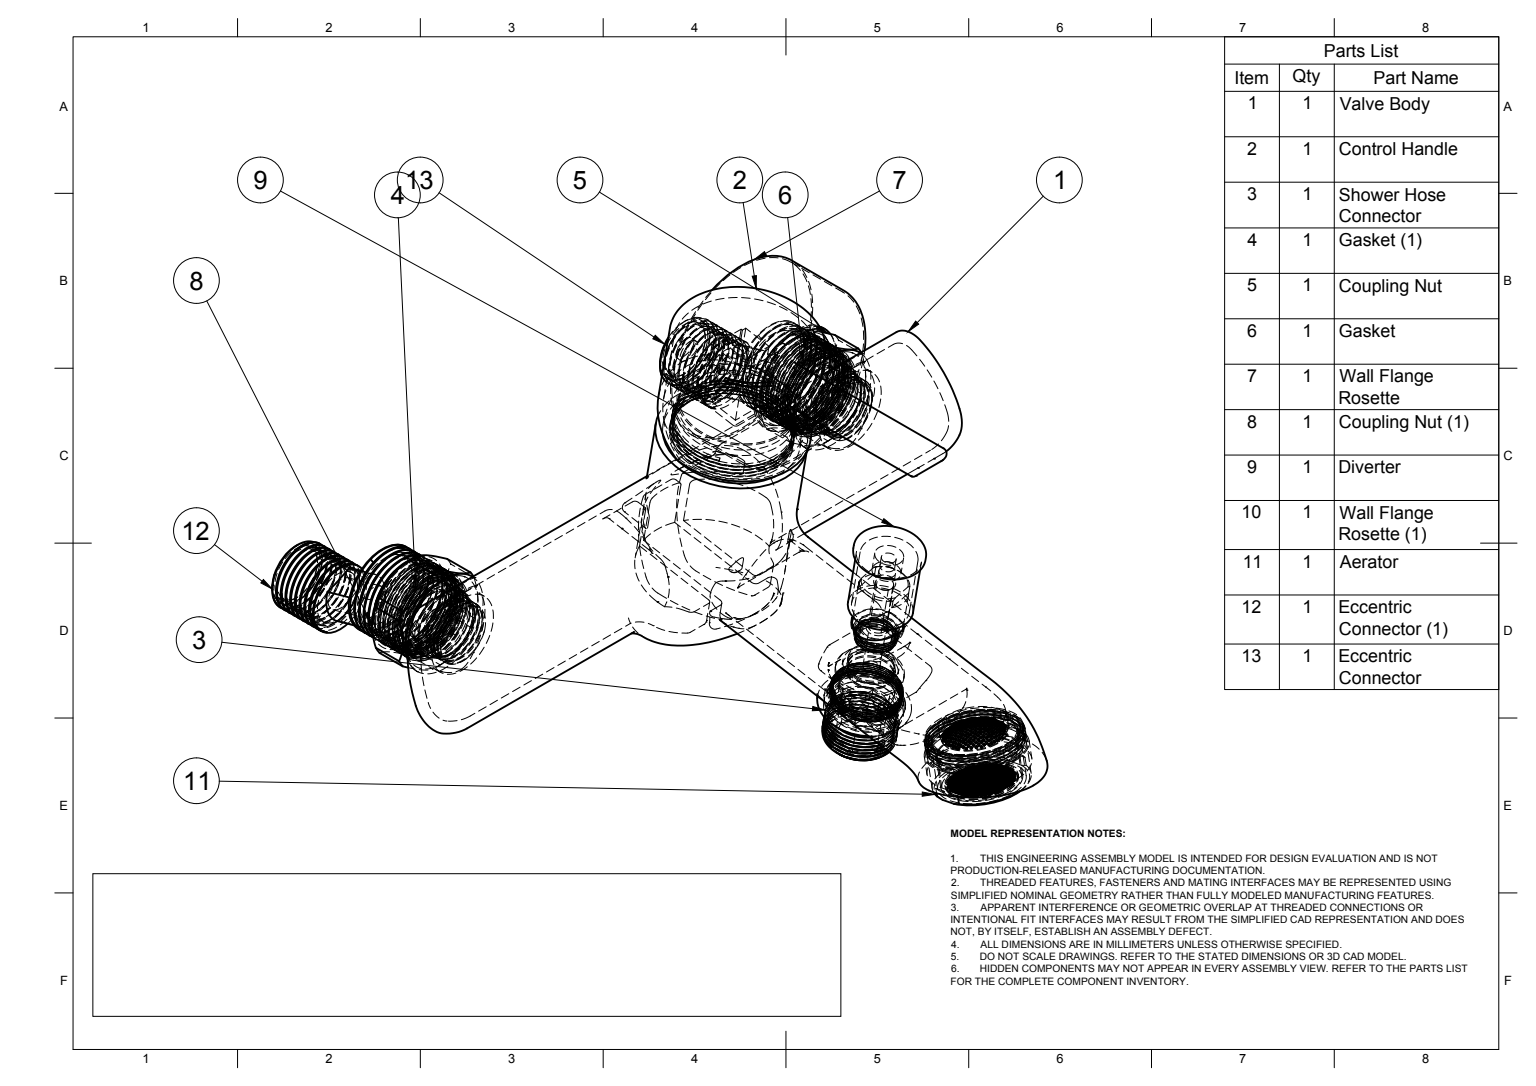
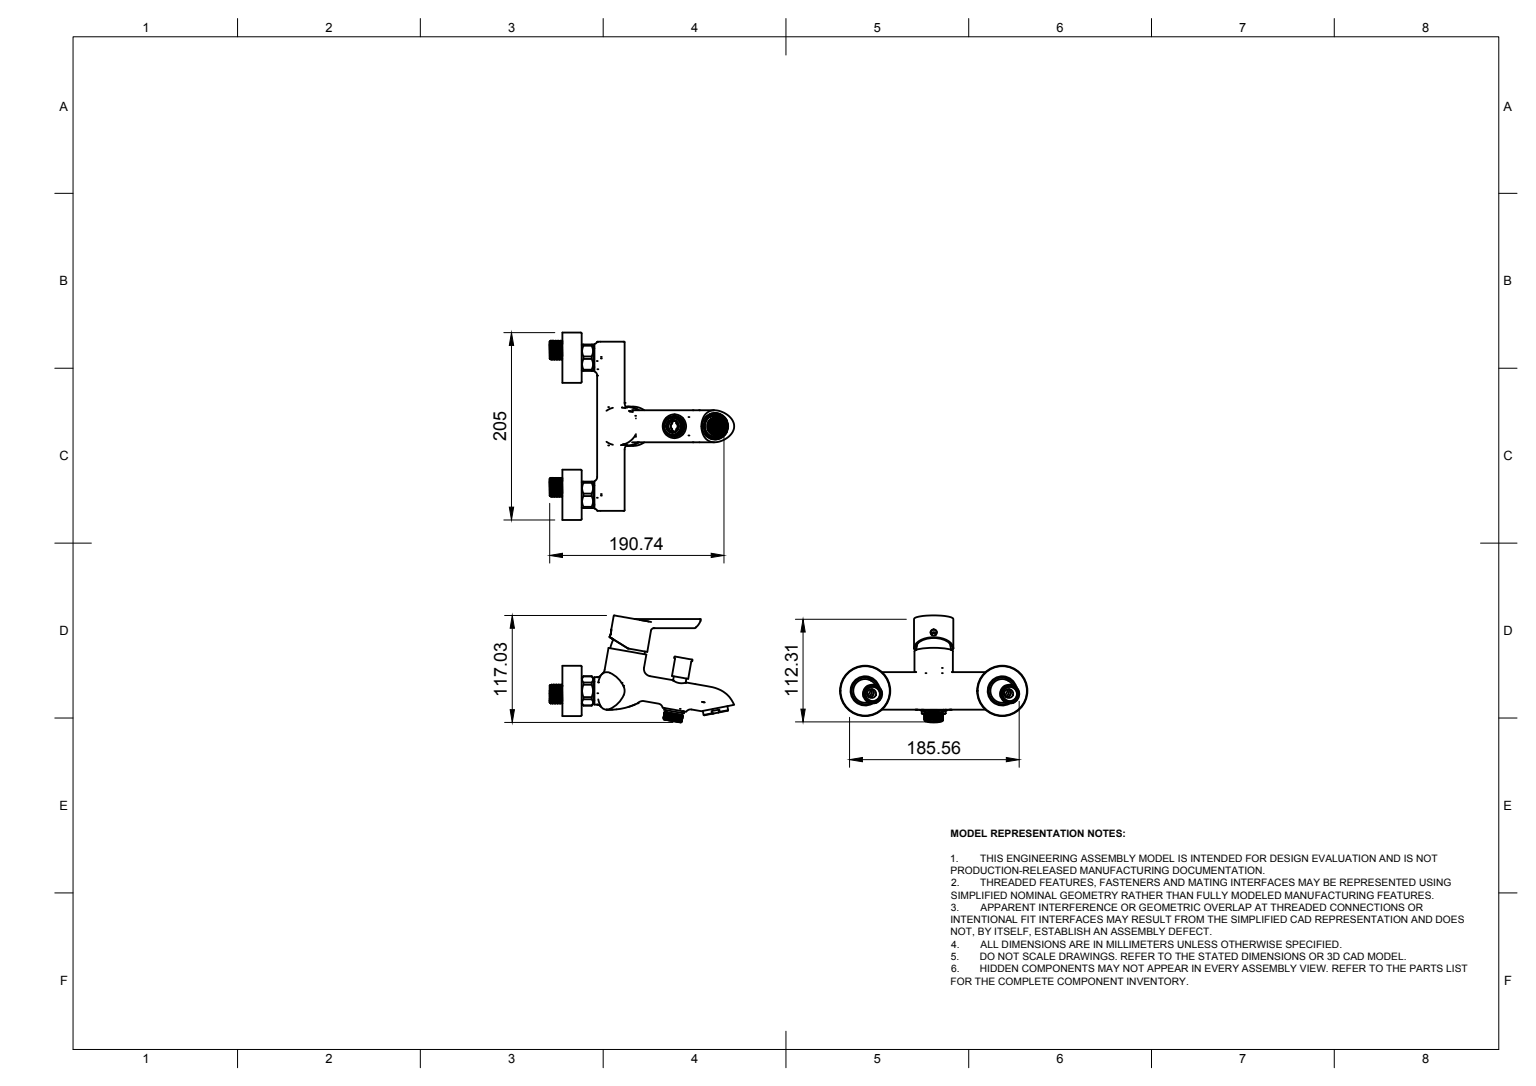
ISO-10303-21;
HEADER;
/* Generated by software containing ST-Developer
 * from STEP Tools, Inc. (www.steptools.com) 
 */

FILE_DESCRIPTION(
/* description */ ('STEP AP214'),
/* implementation_level */ '2;1');

FILE_NAME(
/* name */ 'MAS-607',
/* time_stamp */ '2026-10-05T23:18:41-07:00',
/* author */ (''),
/* organization */ (''),
/* preprocessor_version */ 'ST-DEVELOPER v20.2',
/* originating_system */ 'Autodesk Translation Framework v15.15.0.0',
/* authorisation */ '');

FILE_SCHEMA (('AUTOMOTIVE_DESIGN { 1 0 10303 214 3 1 1 }'));
ENDSEC;

DATA;
#10=MECHANICAL_DESIGN_GEOMETRIC_PRESENTATION_REPRESENTATION('',(#100,#101,
#102,#103,#104,#105,#106,#107,#108,#109,#110,#111,#112),#221662);
#11=ITEM_DEFINED_TRANSFORMATION($,$,#79483,#86151);
#12=ITEM_DEFINED_TRANSFORMATION($,$,#80379,#86152);
#13=ITEM_DEFINED_TRANSFORMATION($,$,#80522,#86153);
#14=ITEM_DEFINED_TRANSFORMATION($,$,#80620,#86154);
#15=ITEM_DEFINED_TRANSFORMATION($,$,#80667,#86155);
#16=ITEM_DEFINED_TRANSFORMATION($,$,#80719,#86156);
#17=ITEM_DEFINED_TRANSFORMATION($,$,#80766,#86157);
#18=ITEM_DEFINED_TRANSFORMATION($,$,#80796,#86158);
#19=ITEM_DEFINED_TRANSFORMATION($,$,#80848,#86159);
#20=ITEM_DEFINED_TRANSFORMATION($,$,#80951,#86160);
#21=ITEM_DEFINED_TRANSFORMATION($,$,#80981,#86161);
#22=ITEM_DEFINED_TRANSFORMATION($,$,#85967,#86162);
#23=ITEM_DEFINED_TRANSFORMATION($,$,#86059,#86163);
#24=(
REPRESENTATION_RELATIONSHIP($,$,#221709,#221708)
REPRESENTATION_RELATIONSHIP_WITH_TRANSFORMATION(#11)
SHAPE_REPRESENTATION_RELATIONSHIP()
);
#25=(
REPRESENTATION_RELATIONSHIP($,$,#221710,#221708)
REPRESENTATION_RELATIONSHIP_WITH_TRANSFORMATION(#12)
SHAPE_REPRESENTATION_RELATIONSHIP()
);
#26=(
REPRESENTATION_RELATIONSHIP($,$,#221711,#221708)
REPRESENTATION_RELATIONSHIP_WITH_TRANSFORMATION(#13)
SHAPE_REPRESENTATION_RELATIONSHIP()
);
#27=(
REPRESENTATION_RELATIONSHIP($,$,#221712,#221708)
REPRESENTATION_RELATIONSHIP_WITH_TRANSFORMATION(#14)
SHAPE_REPRESENTATION_RELATIONSHIP()
);
#28=(
REPRESENTATION_RELATIONSHIP($,$,#221713,#221708)
REPRESENTATION_RELATIONSHIP_WITH_TRANSFORMATION(#15)
SHAPE_REPRESENTATION_RELATIONSHIP()
);
#29=(
REPRESENTATION_RELATIONSHIP($,$,#221714,#221708)
REPRESENTATION_RELATIONSHIP_WITH_TRANSFORMATION(#16)
SHAPE_REPRESENTATION_RELATIONSHIP()
);
#30=(
REPRESENTATION_RELATIONSHIP($,$,#221715,#221708)
REPRESENTATION_RELATIONSHIP_WITH_TRANSFORMATION(#17)
SHAPE_REPRESENTATION_RELATIONSHIP()
);
#31=(
REPRESENTATION_RELATIONSHIP($,$,#221716,#221708)
REPRESENTATION_RELATIONSHIP_WITH_TRANSFORMATION(#18)
SHAPE_REPRESENTATION_RELATIONSHIP()
);
#32=(
REPRESENTATION_RELATIONSHIP($,$,#221717,#221708)
REPRESENTATION_RELATIONSHIP_WITH_TRANSFORMATION(#19)
SHAPE_REPRESENTATION_RELATIONSHIP()
);
#33=(
REPRESENTATION_RELATIONSHIP($,$,#221718,#221708)
REPRESENTATION_RELATIONSHIP_WITH_TRANSFORMATION(#20)
SHAPE_REPRESENTATION_RELATIONSHIP()
);
#34=(
REPRESENTATION_RELATIONSHIP($,$,#221719,#221708)
REPRESENTATION_RELATIONSHIP_WITH_TRANSFORMATION(#21)
SHAPE_REPRESENTATION_RELATIONSHIP()
);
#35=(
REPRESENTATION_RELATIONSHIP($,$,#221720,#221708)
REPRESENTATION_RELATIONSHIP_WITH_TRANSFORMATION(#22)
SHAPE_REPRESENTATION_RELATIONSHIP()
);
#36=(
REPRESENTATION_RELATIONSHIP($,$,#221721,#221708)
REPRESENTATION_RELATIONSHIP_WITH_TRANSFORMATION(#23)
SHAPE_REPRESENTATION_RELATIONSHIP()
);
#37=CONTEXT_DEPENDENT_SHAPE_REPRESENTATION(#24,#221695);
#38=CONTEXT_DEPENDENT_SHAPE_REPRESENTATION(#25,#221696);
#39=CONTEXT_DEPENDENT_SHAPE_REPRESENTATION(#26,#221697);
#40=CONTEXT_DEPENDENT_SHAPE_REPRESENTATION(#27,#221698);
#41=CONTEXT_DEPENDENT_SHAPE_REPRESENTATION(#28,#221699);
#42=CONTEXT_DEPENDENT_SHAPE_REPRESENTATION(#29,#221700);
#43=CONTEXT_DEPENDENT_SHAPE_REPRESENTATION(#30,#221701);
#44=CONTEXT_DEPENDENT_SHAPE_REPRESENTATION(#31,#221702);
#45=CONTEXT_DEPENDENT_SHAPE_REPRESENTATION(#32,#221703);
#46=CONTEXT_DEPENDENT_SHAPE_REPRESENTATION(#33,#221704);
#47=CONTEXT_DEPENDENT_SHAPE_REPRESENTATION(#34,#221705);
#48=CONTEXT_DEPENDENT_SHAPE_REPRESENTATION(#35,#221706);
#49=CONTEXT_DEPENDENT_SHAPE_REPRESENTATION(#36,#221707);
#50=NEXT_ASSEMBLY_USAGE_OCCURRENCE('Valve Body:1','Valve Body:1',
'Valve Body:1',#221723,#221724,'Valve Body:1');
#51=NEXT_ASSEMBLY_USAGE_OCCURRENCE('Control Handle:1',
'Control Handle:1','Control Handle:1',#221723,#221725,
'Control Handle:1');
#52=NEXT_ASSEMBLY_USAGE_OCCURRENCE('Shower Hose Connector:1',
'Shower Hose Connector:1','Shower Hose Connector:1',#221723,#221726,
'Shower Hose Connector:1');
#53=NEXT_ASSEMBLY_USAGE_OCCURRENCE('Gasket (1):1','Gasket (1):1',
'Gasket (1):1',#221723,#221727,'Gasket (1):1');
#54=NEXT_ASSEMBLY_USAGE_OCCURRENCE('Coupling Nut:1','Coupling Nut:1',
'Coupling Nut:1',#221723,#221728,'Coupling Nut:1');
#55=NEXT_ASSEMBLY_USAGE_OCCURRENCE('Gasket:1','Gasket:1','Gasket:1',#221723,
#221729,'Gasket:1');
#56=NEXT_ASSEMBLY_USAGE_OCCURRENCE('Wall Flange Rosette:1',
'Wall Flange Rosette:1','Wall Flange Rosette:1',#221723,#221730,
'Wall Flange Rosette:1');
#57=NEXT_ASSEMBLY_USAGE_OCCURRENCE('Coupling Nut (1):1',
'Coupling Nut (1):1','Coupling Nut (1):1',#221723,#221731,
'Coupling Nut (1):1');
#58=NEXT_ASSEMBLY_USAGE_OCCURRENCE('Diverter:1','Diverter:1',
'Diverter:1',#221723,#221732,'Diverter:1');
#59=NEXT_ASSEMBLY_USAGE_OCCURRENCE('Wall Flange Rosette (1):1',
'Wall Flange Rosette (1):1','Wall Flange Rosette (1):1',#221723,#221733,
'Wall Flange Rosette (1):1');
#60=NEXT_ASSEMBLY_USAGE_OCCURRENCE('Aerator:1','Aerator:1','Aerator:1',
#221723,#221734,'Aerator:1');
#61=NEXT_ASSEMBLY_USAGE_OCCURRENCE('Eccentric Connector (1):1',
'Eccentric Connector (1):1','Eccentric Connector (1):1',#221723,#221735,
'Eccentric Connector (1):1');
#62=NEXT_ASSEMBLY_USAGE_OCCURRENCE('Eccentric Connector:1',
'Eccentric Connector:1','Eccentric Connector:1',#221723,#221736,
'Eccentric Connector:1');
#63=MANIFOLD_SOLID_BREP('Body1',#79323);
#64=MANIFOLD_SOLID_BREP('Body1',#79324);
#65=MANIFOLD_SOLID_BREP('Body1',#79325);
#66=MANIFOLD_SOLID_BREP('Body1',#79326);
#67=MANIFOLD_SOLID_BREP('Body1',#79327);
#68=MANIFOLD_SOLID_BREP('Body1',#79328);
#69=MANIFOLD_SOLID_BREP('Body1',#79329);
#70=MANIFOLD_SOLID_BREP('Body1',#79332);
#71=MANIFOLD_SOLID_BREP('Body1',#79333);
#72=MANIFOLD_SOLID_BREP('Body1',#79334);
#73=MANIFOLD_SOLID_BREP('Body1',#79335);
#74=SHAPE_REPRESENTATION_RELATIONSHIP('SRR','None',#221709,#87);
#75=SHAPE_REPRESENTATION_RELATIONSHIP('SRR','None',#221710,#88);
#76=SHAPE_REPRESENTATION_RELATIONSHIP('SRR','None',#221711,#89);
#77=SHAPE_REPRESENTATION_RELATIONSHIP('SRR','None',#221712,#90);
#78=SHAPE_REPRESENTATION_RELATIONSHIP('SRR','None',#221713,#91);
#79=SHAPE_REPRESENTATION_RELATIONSHIP('SRR','None',#221714,#92);
#80=SHAPE_REPRESENTATION_RELATIONSHIP('SRR','None',#221715,#93);
#81=SHAPE_REPRESENTATION_RELATIONSHIP('SRR','None',#221716,#94);
#82=SHAPE_REPRESENTATION_RELATIONSHIP('SRR','None',#221717,#95);
#83=SHAPE_REPRESENTATION_RELATIONSHIP('SRR','None',#221718,#96);
#84=SHAPE_REPRESENTATION_RELATIONSHIP('SRR','None',#221719,#97);
#85=SHAPE_REPRESENTATION_RELATIONSHIP('SRR','None',#221720,#98);
#86=SHAPE_REPRESENTATION_RELATIONSHIP('SRR','None',#221721,#99);
#87=ADVANCED_BREP_SHAPE_REPRESENTATION('',(#79336),#221649);
#88=ADVANCED_BREP_SHAPE_REPRESENTATION('',(#63),#221650);
#89=ADVANCED_BREP_SHAPE_REPRESENTATION('',(#64),#221651);
#90=ADVANCED_BREP_SHAPE_REPRESENTATION('',(#65),#221652);
#91=ADVANCED_BREP_SHAPE_REPRESENTATION('',(#66),#221653);
#92=ADVANCED_BREP_SHAPE_REPRESENTATION('',(#67),#221654);
#93=ADVANCED_BREP_SHAPE_REPRESENTATION('',(#68),#221655);
#94=ADVANCED_BREP_SHAPE_REPRESENTATION('',(#69),#221656);
#95=ADVANCED_BREP_SHAPE_REPRESENTATION('',(#79337),#221657);
#96=ADVANCED_BREP_SHAPE_REPRESENTATION('',(#70),#221658);
#97=ADVANCED_BREP_SHAPE_REPRESENTATION('',(#71),#221659);
#98=ADVANCED_BREP_SHAPE_REPRESENTATION('',(#72),#221660);
#99=ADVANCED_BREP_SHAPE_REPRESENTATION('',(#73),#221661);
#100=STYLED_ITEM('',(#221783),#79336);
#101=STYLED_ITEM('',(#221783),#63);
#102=STYLED_ITEM('',(#221783),#64);
#103=STYLED_ITEM('',(#221783),#65);
#104=STYLED_ITEM('',(#221783),#66);
#105=STYLED_ITEM('',(#221783),#67);
#106=STYLED_ITEM('',(#221783),#68);
#107=STYLED_ITEM('',(#221783),#69);
#108=STYLED_ITEM('',(#221783),#79337);
#109=STYLED_ITEM('',(#221783),#70);
#110=STYLED_ITEM('',(#221783),#71);
#111=STYLED_ITEM('',(#221783),#72);
#112=STYLED_ITEM('',(#221783),#73);
#113=B_SPLINE_SURFACE_WITH_KNOTS('',3,3,((#122040,#122041,#122042,#122043,
#122044,#122045,#122046,#122047,#122048,#122049,#122050),(#122051,#122052,
#122053,#122054,#122055,#122056,#122057,#122058,#122059,#122060,#122061),
(#122062,#122063,#122064,#122065,#122066,#122067,#122068,#122069,#122070,
#122071,#122072),(#122073,#122074,#122075,#122076,#122077,#122078,#122079,
#122080,#122081,#122082,#122083)),.UNSPECIFIED.,.F.,.F.,.F.,(4,4),(4,1,
1,1,1,1,1,1,4),(0.,1.),(0.,0.125,0.249999999999986,0.374999999999913,0.499999999999809,
0.625000000000008,0.749999999999904,0.8749999999998,1.),.UNSPECIFIED.);
#114=B_SPLINE_SURFACE_WITH_KNOTS('',3,3,((#122246,#122247,#122248,#122249,
#122250,#122251,#122252,#122253,#122254,#122255,#122256),(#122257,#122258,
#122259,#122260,#122261,#122262,#122263,#122264,#122265,#122266,#122267),
(#122268,#122269,#122270,#122271,#122272,#122273,#122274,#122275,#122276,
#122277,#122278),(#122279,#122280,#122281,#122282,#122283,#122284,#122285,
#122286,#122287,#122288,#122289),(#122290,#122291,#122292,#122293,#122294,
#122295,#122296,#122297,#122298,#122299,#122300),(#122301,#122302,#122303,
#122304,#122305,#122306,#122307,#122308,#122309,#122310,#122311),(#122312,
#122313,#122314,#122315,#122316,#122317,#122318,#122319,#122320,#122321,
#122322),(#122323,#122324,#122325,#122326,#122327,#122328,#122329,#122330,
#122331,#122332,#122333),(#122334,#122335,#122336,#122337,#122338,#122339,
#122340,#122341,#122342,#122343,#122344),(#122345,#122346,#122347,#122348,
#122349,#122350,#122351,#122352,#122353,#122354,#122355)),.UNSPECIFIED.,
 .F.,.F.,.F.,(4,3,3,4),(4,1,1,1,1,1,1,1,4),(-0.01,0.,0.978175299313866,
1.),(0.,0.125000000000015,0.25000000000002,0.374999999999975,0.500000000000081,
0.625000000000188,0.750000000000041,0.875000000000148,1.),.UNSPECIFIED.);
#115=B_SPLINE_SURFACE_WITH_KNOTS('',3,3,((#122432,#122433,#122434,#122435,
#122436,#122437,#122438,#122439,#122440,#122441,#122442,#122443,#122444,
#122445,#122446,#122447,#122448,#122449,#122450),(#122451,#122452,#122453,
#122454,#122455,#122456,#122457,#122458,#122459,#122460,#122461,#122462,
#122463,#122464,#122465,#122466,#122467,#122468,#122469),(#122470,#122471,
#122472,#122473,#122474,#122475,#122476,#122477,#122478,#122479,#122480,
#122481,#122482,#122483,#122484,#122485,#122486,#122487,#122488),(#122489,
#122490,#122491,#122492,#122493,#122494,#122495,#122496,#122497,#122498,
#122499,#122500,#122501,#122502,#122503,#122504,#122505,#122506,#122507)),
 .UNSPECIFIED.,.F.,.F.,.F.,(4,4),(4,1,1,1,1,1,1,1,1,1,1,1,1,1,1,1,4),(0.,
1.),(0.,0.0625000000000019,0.12499999999999,0.187499999999977,0.249999999999904,
0.312500000000014,0.37499999999992,0.43750000000003,0.499999999999936,0.562500000000046,
0.624999999999952,0.687499999999859,0.749999999999968,0.812499999999875,
0.874999999999984,0.937499999999891,1.),.UNSPECIFIED.);
#116=B_SPLINE_SURFACE_WITH_KNOTS('',3,3,((#122509,#122510,#122511,#122512,
#122513,#122514,#122515,#122516,#122517,#122518,#122519,#122520,#122521,
#122522,#122523,#122524,#122525,#122526,#122527,#122528,#122529,#122530,
#122531,#122532,#122533,#122534,#122535,#122536,#122537,#122538,#122539,
#122540,#122541,#122542,#122543),(#122544,#122545,#122546,#122547,#122548,
#122549,#122550,#122551,#122552,#122553,#122554,#122555,#122556,#122557,
#122558,#122559,#122560,#122561,#122562,#122563,#122564,#122565,#122566,
#122567,#122568,#122569,#122570,#122571,#122572,#122573,#122574,#122575,
#122576,#122577,#122578),(#122579,#122580,#122581,#122582,#122583,#122584,
#122585,#122586,#122587,#122588,#122589,#122590,#122591,#122592,#122593,
#122594,#122595,#122596,#122597,#122598,#122599,#122600,#122601,#122602,
#122603,#122604,#122605,#122606,#122607,#122608,#122609,#122610,#122611,
#122612,#122613),(#122614,#122615,#122616,#122617,#122618,#122619,#122620,
#122621,#122622,#122623,#122624,#122625,#122626,#122627,#122628,#122629,
#122630,#122631,#122632,#122633,#122634,#122635,#122636,#122637,#122638,
#122639,#122640,#122641,#122642,#122643,#122644,#122645,#122646,#122647,
#122648)),.UNSPECIFIED.,.F.,.F.,.F.,(4,4),(4,1,1,1,1,1,1,1,1,1,1,1,1,1,
1,1,1,1,1,1,1,1,1,1,1,1,1,1,1,1,1,1,4),(0.,1.),(0.,0.031249999999986,0.0625000000000033,
0.0937499999999268,0.124999999999954,0.156249999999982,0.187499999999906,
0.218749999999933,0.249999999999961,0.281249999999885,0.312499999999912,
0.343749999999836,0.374999999999863,0.406249999999891,0.437499999999815,
0.468749999999842,0.49999999999987,0.531249999999794,0.562499999999821,
0.593749999999849,0.624999999999772,0.6562499999998,0.687499999999724,0.718749999999751,
0.749999999999779,0.781249999999703,0.81249999999973,0.843749999999758,
0.874999999999681,0.906249999999709,0.937499999999633,0.96874999999966,
1.),.UNSPECIFIED.);
#117=B_SPLINE_SURFACE_WITH_KNOTS('',3,3,((#122930,#122931,#122932,#122933,
#122934,#122935,#122936,#122937,#122938,#122939,#122940,#122941,#122942,
#122943,#122944,#122945,#122946,#122947,#122948,#122949,#122950,#122951,
#122952,#122953,#122954,#122955,#122956,#122957,#122958,#122959,#122960,
#122961,#122962,#122963,#122964),(#122965,#122966,#122967,#122968,#122969,
#122970,#122971,#122972,#122973,#122974,#122975,#122976,#122977,#122978,
#122979,#122980,#122981,#122982,#122983,#122984,#122985,#122986,#122987,
#122988,#122989,#122990,#122991,#122992,#122993,#122994,#122995,#122996,
#122997,#122998,#122999),(#123000,#123001,#123002,#123003,#123004,#123005,
#123006,#123007,#123008,#123009,#123010,#123011,#123012,#123013,#123014,
#123015,#123016,#123017,#123018,#123019,#123020,#123021,#123022,#123023,
#123024,#123025,#123026,#123027,#123028,#123029,#123030,#123031,#123032,
#123033,#123034),(#123035,#123036,#123037,#123038,#123039,#123040,#123041,
#123042,#123043,#123044,#123045,#123046,#123047,#123048,#123049,#123050,
#123051,#123052,#123053,#123054,#123055,#123056,#123057,#123058,#123059,
#123060,#123061,#123062,#123063,#123064,#123065,#123066,#123067,#123068,
#123069)),.UNSPECIFIED.,.F.,.F.,.F.,(4,4),(4,1,1,1,1,1,1,1,1,1,1,1,1,1,
1,1,1,1,1,1,1,1,1,1,1,1,1,1,1,1,1,1,4),(0.,1.),(0.,0.0312499999999875,0.0624999999999539,
0.0937500000000046,0.12499999999995,0.15625,0.187499999999946,0.218749999999891,
0.249999999999942,0.281249999999887,0.312499999999938,0.343749999999883,
0.374999999999934,0.40624999999988,0.43749999999993,0.468749999999876,0.499999999999821,
0.531249999999872,0.562499999999817,0.593749999999868,0.624999999999813,
0.656249999999864,0.687499999999809,0.71874999999986,0.749999999999805,
0.781249999999751,0.812499999999801,0.843749999999747,0.874999999999797,
0.906249999999743,0.937499999999793,0.968749999999739,1.),.UNSPECIFIED.);
#118=B_SPLINE_SURFACE_WITH_KNOTS('',3,3,((#123453,#123454,#123455,#123456,
#123457,#123458,#123459,#123460,#123461,#123462,#123463,#123464,#123465,
#123466,#123467,#123468,#123469,#123470,#123471,#123472,#123473,#123474,
#123475,#123476,#123477,#123478,#123479,#123480,#123481,#123482,#123483,
#123484,#123485),(#123486,#123487,#123488,#123489,#123490,#123491,#123492,
#123493,#123494,#123495,#123496,#123497,#123498,#123499,#123500,#123501,
#123502,#123503,#123504,#123505,#123506,#123507,#123508,#123509,#123510,
#123511,#123512,#123513,#123514,#123515,#123516,#123517,#123518),(#123519,
#123520,#123521,#123522,#123523,#123524,#123525,#123526,#123527,#123528,
#123529,#123530,#123531,#123532,#123533,#123534,#123535,#123536,#123537,
#123538,#123539,#123540,#123541,#123542,#123543,#123544,#123545,#123546,
#123547,#123548,#123549,#123550,#123551),(#123552,#123553,#123554,#123555,
#123556,#123557,#123558,#123559,#123560,#123561,#123562,#123563,#123564,
#123565,#123566,#123567,#123568,#123569,#123570,#123571,#123572,#123573,
#123574,#123575,#123576,#123577,#123578,#123579,#123580,#123581,#123582,
#123583,#123584)),.UNSPECIFIED.,.F.,.F.,.F.,(4,4),(4,1,1,1,1,1,1,1,1,1,
1,1,1,1,1,1,1,1,1,1,1,1,1,1,1,1,1,1,1,1,4),(0.,1.),(0.,0.0624999999999647,
0.0937499999999471,0.125000000000042,0.156250000000025,0.187500000000007,
0.218749999999989,0.249999999999972,0.281249999999954,0.312499999999937,
0.343750000000032,0.375000000000014,0.40625,0.437499999999979,0.468749999999961,
0.499999999999944,0.531250000000039,0.562500000000021,0.59375,0.624999999999986,
0.656249999999968,0.687499999999951,0.718749999999933,0.750000000000028,
0.781250000000011,0.8125,0.843749999999975,0.874999999999958,0.90624999999994,
0.937499999999923,1.),.UNSPECIFIED.);
#119=B_SPLINE_SURFACE_WITH_KNOTS('',3,3,((#128648,#128649,#128650,#128651,
#128652,#128653,#128654,#128655,#128656,#128657,#128658),(#128659,#128660,
#128661,#128662,#128663,#128664,#128665,#128666,#128667,#128668,#128669),
(#128670,#128671,#128672,#128673,#128674,#128675,#128676,#128677,#128678,
#128679,#128680),(#128681,#128682,#128683,#128684,#128685,#128686,#128687,
#128688,#128689,#128690,#128691)),.UNSPECIFIED.,.F.,.F.,.F.,(4,4),(4,1,
1,1,1,1,1,1,4),(0.,1.),(0.,0.125,0.249999999999986,0.374999999999913,0.499999999999809,
0.625000000000008,0.749999999999904,0.8749999999998,1.),.UNSPECIFIED.);
#120=B_SPLINE_SURFACE_WITH_KNOTS('',3,3,((#128722,#128723,#128724,#128725,
#128726,#128727,#128728,#128729,#128730,#128731,#128732,#128733,#128734,
#128735,#128736,#128737,#128738,#128739,#128740),(#128741,#128742,#128743,
#128744,#128745,#128746,#128747,#128748,#128749,#128750,#128751,#128752,
#128753,#128754,#128755,#128756,#128757,#128758,#128759),(#128760,#128761,
#128762,#128763,#128764,#128765,#128766,#128767,#128768,#128769,#128770,
#128771,#128772,#128773,#128774,#128775,#128776,#128777,#128778),(#128779,
#128780,#128781,#128782,#128783,#128784,#128785,#128786,#128787,#128788,
#128789,#128790,#128791,#128792,#128793,#128794,#128795,#128796,#128797)),
 .UNSPECIFIED.,.F.,.F.,.F.,(4,4),(4,1,1,1,1,1,1,1,1,1,1,1,1,1,1,1,4),(0.,
1.),(0.,0.0625000000000019,0.12499999999999,0.187499999999977,0.249999999999904,
0.312500000000014,0.37499999999992,0.43750000000003,0.499999999999936,0.562500000000046,
0.624999999999952,0.687499999999859,0.749999999999968,0.812499999999875,
0.874999999999984,0.937499999999891,1.),.UNSPECIFIED.);
#121=B_SPLINE_SURFACE_WITH_KNOTS('',3,3,((#128874,#128875,#128876,#128877,
#128878,#128879,#128880,#128881,#128882,#128883,#128884),(#128885,#128886,
#128887,#128888,#128889,#128890,#128891,#128892,#128893,#128894,#128895),
(#128896,#128897,#128898,#128899,#128900,#128901,#128902,#128903,#128904,
#128905,#128906),(#128907,#128908,#128909,#128910,#128911,#128912,#128913,
#128914,#128915,#128916,#128917),(#128918,#128919,#128920,#128921,#128922,
#128923,#128924,#128925,#128926,#128927,#128928),(#128929,#128930,#128931,
#128932,#128933,#128934,#128935,#128936,#128937,#128938,#128939),(#128940,
#128941,#128942,#128943,#128944,#128945,#128946,#128947,#128948,#128949,
#128950)),.UNSPECIFIED.,.F.,.F.,.F.,(4,3,4),(4,1,1,1,1,1,1,1,4),(0.,0.978284469703565,
1.),(0.,0.125000000000015,0.25000000000002,0.374999999999975,0.500000000000081,
0.625000000000188,0.750000000000041,0.875000000000148,1.),.UNSPECIFIED.);
#122=B_SPLINE_SURFACE_WITH_KNOTS('',3,3,((#128952,#128953,#128954,#128955,
#128956,#128957,#128958,#128959,#128960,#128961,#128962,#128963,#128964,
#128965,#128966,#128967,#128968,#128969,#128970,#128971,#128972,#128973,
#128974,#128975,#128976,#128977,#128978,#128979,#128980,#128981,#128982,
#128983,#128984,#128985,#128986),(#128987,#128988,#128989,#128990,#128991,
#128992,#128993,#128994,#128995,#128996,#128997,#128998,#128999,#129000,
#129001,#129002,#129003,#129004,#129005,#129006,#129007,#129008,#129009,
#129010,#129011,#129012,#129013,#129014,#129015,#129016,#129017,#129018,
#129019,#129020,#129021),(#129022,#129023,#129024,#129025,#129026,#129027,
#129028,#129029,#129030,#129031,#129032,#129033,#129034,#129035,#129036,
#129037,#129038,#129039,#129040,#129041,#129042,#129043,#129044,#129045,
#129046,#129047,#129048,#129049,#129050,#129051,#129052,#129053,#129054,
#129055,#129056),(#129057,#129058,#129059,#129060,#129061,#129062,#129063,
#129064,#129065,#129066,#129067,#129068,#129069,#129070,#129071,#129072,
#129073,#129074,#129075,#129076,#129077,#129078,#129079,#129080,#129081,
#129082,#129083,#129084,#129085,#129086,#129087,#129088,#129089,#129090,
#129091)),.UNSPECIFIED.,.F.,.F.,.F.,(4,4),(4,1,1,1,1,1,1,1,1,1,1,1,1,1,
1,1,1,1,1,1,1,1,1,1,1,1,1,1,1,1,1,1,4),(0.,1.),(0.,0.031249999999986,0.0625000000000033,
0.0937499999999268,0.124999999999954,0.156249999999982,0.187499999999906,
0.218749999999933,0.249999999999961,0.281249999999885,0.312499999999912,
0.343749999999836,0.374999999999863,0.406249999999891,0.437499999999815,
0.468749999999842,0.49999999999987,0.531249999999794,0.562499999999821,
0.593749999999849,0.624999999999772,0.6562499999998,0.687499999999724,0.718749999999751,
0.749999999999779,0.781249999999703,0.81249999999973,0.843749999999758,
0.874999999999681,0.906249999999709,0.937499999999633,0.96874999999966,
1.),.UNSPECIFIED.);
#123=B_SPLINE_SURFACE_WITH_KNOTS('',3,3,((#129371,#129372,#129373,#129374,
#129375,#129376,#129377,#129378,#129379,#129380,#129381,#129382,#129383,
#129384,#129385,#129386,#129387,#129388,#129389,#129390,#129391,#129392,
#129393,#129394,#129395,#129396,#129397,#129398,#129399,#129400,#129401,
#129402,#129403),(#129404,#129405,#129406,#129407,#129408,#129409,#129410,
#129411,#129412,#129413,#129414,#129415,#129416,#129417,#129418,#129419,
#129420,#129421,#129422,#129423,#129424,#129425,#129426,#129427,#129428,
#129429,#129430,#129431,#129432,#129433,#129434,#129435,#129436),(#129437,
#129438,#129439,#129440,#129441,#129442,#129443,#129444,#129445,#129446,
#129447,#129448,#129449,#129450,#129451,#129452,#129453,#129454,#129455,
#129456,#129457,#129458,#129459,#129460,#129461,#129462,#129463,#129464,
#129465,#129466,#129467,#129468,#129469),(#129470,#129471,#129472,#129473,
#129474,#129475,#129476,#129477,#129478,#129479,#129480,#129481,#129482,
#129483,#129484,#129485,#129486,#129487,#129488,#129489,#129490,#129491,
#129492,#129493,#129494,#129495,#129496,#129497,#129498,#129499,#129500,
#129501,#129502)),.UNSPECIFIED.,.F.,.F.,.F.,(4,4),(4,1,1,1,1,1,1,1,1,1,
1,1,1,1,1,1,1,1,1,1,1,1,1,1,1,1,1,1,1,1,4),(0.,1.),(0.,0.0624999999999647,
0.0937499999999471,0.125000000000042,0.156250000000025,0.187500000000007,
0.218749999999989,0.249999999999972,0.281249999999954,0.312499999999937,
0.343750000000032,0.375000000000014,0.40625,0.437499999999979,0.468749999999961,
0.499999999999944,0.531250000000039,0.562500000000021,0.59375,0.624999999999986,
0.656249999999968,0.687499999999951,0.718749999999933,0.750000000000028,
0.781250000000011,0.8125,0.843749999999975,0.874999999999958,0.90624999999994,
0.937499999999923,1.),.UNSPECIFIED.);
#124=B_SPLINE_SURFACE_WITH_KNOTS('',3,3,((#129824,#129825,#129826,#129827,
#129828,#129829,#129830,#129831,#129832,#129833,#129834,#129835,#129836,
#129837,#129838,#129839,#129840,#129841,#129842,#129843,#129844,#129845,
#129846,#129847,#129848,#129849,#129850,#129851,#129852,#129853,#129854,
#129855,#129856,#129857,#129858),(#129859,#129860,#129861,#129862,#129863,
#129864,#129865,#129866,#129867,#129868,#129869,#129870,#129871,#129872,
#129873,#129874,#129875,#129876,#129877,#129878,#129879,#129880,#129881,
#129882,#129883,#129884,#129885,#129886,#129887,#129888,#129889,#129890,
#129891,#129892,#129893),(#129894,#129895,#129896,#129897,#129898,#129899,
#129900,#129901,#129902,#129903,#129904,#129905,#129906,#129907,#129908,
#129909,#129910,#129911,#129912,#129913,#129914,#129915,#129916,#129917,
#129918,#129919,#129920,#129921,#129922,#129923,#129924,#129925,#129926,
#129927,#129928),(#129929,#129930,#129931,#129932,#129933,#129934,#129935,
#129936,#129937,#129938,#129939,#129940,#129941,#129942,#129943,#129944,
#129945,#129946,#129947,#129948,#129949,#129950,#129951,#129952,#129953,
#129954,#129955,#129956,#129957,#129958,#129959,#129960,#129961,#129962,
#129963)),.UNSPECIFIED.,.F.,.F.,.F.,(4,4),(4,1,1,1,1,1,1,1,1,1,1,1,1,1,
1,1,1,1,1,1,1,1,1,1,1,1,1,1,1,1,1,1,4),(0.,1.),(0.,0.0312499999999977,0.0624999999999638,
0.0937500000000142,0.124999999999959,0.15625000000001,0.187499999999955,
0.2187499999999,0.24999999999995,0.281249999999895,0.312499999999945,0.34374999999989,
0.374999999999941,0.406249999999886,0.437499999999936,0.468749999999881,
0.499999999999826,0.531249999999877,0.562499999999822,0.593749999999872,
0.624999999999817,0.656249999999867,0.687499999999812,0.718749999999863,
0.749999999999808,0.781249999999753,0.812499999999803,0.843749999999749,
0.874999999999799,0.906249999999744,0.937499999999794,0.968749999999739,
1.),.UNSPECIFIED.);
#125=B_SPLINE_SURFACE_WITH_KNOTS('',1,3,((#129975,#129976,#129977,#129978,
#129979,#129980,#129981,#129982,#129983,#129984,#129985,#129986,#129987,
#129988,#129989,#129990,#129991,#129992,#129993,#129994,#129995,#129996,
#129997,#129998,#129999,#130000,#130001,#130002,#130003,#130004,#130005,
#130006,#130007,#130008,#130009,#130010,#130011,#130012,#130013,#130014,
#130015,#130016,#130017,#130018,#130019,#130020,#130021,#130022,#130023,
#130024,#130025,#130026,#130027,#130028,#130029,#130030,#130031,#130032,
#130033,#130034,#130035,#130036,#130037,#130038,#130039,#130040,#130041,
#130042,#130043,#130044,#130045,#130046,#130047,#130048,#130049,#130050,
#130051,#130052,#130053,#130054,#130055,#130056,#130057,#130058,#130059),
(#130060,#130061,#130062,#130063,#130064,#130065,#130066,#130067,#130068,
#130069,#130070,#130071,#130072,#130073,#130074,#130075,#130076,#130077,
#130078,#130079,#130080,#130081,#130082,#130083,#130084,#130085,#130086,
#130087,#130088,#130089,#130090,#130091,#130092,#130093,#130094,#130095,
#130096,#130097,#130098,#130099,#130100,#130101,#130102,#130103,#130104,
#130105,#130106,#130107,#130108,#130109,#130110,#130111,#130112,#130113,
#130114,#130115,#130116,#130117,#130118,#130119,#130120,#130121,#130122,
#130123,#130124,#130125,#130126,#130127,#130128,#130129,#130130,#130131,
#130132,#130133,#130134,#130135,#130136,#130137,#130138,#130139,#130140,
#130141,#130142,#130143,#130144)),.UNSPECIFIED.,.F.,.F.,.F.,(2,2),(4,1,
1,1,1,1,1,1,1,1,1,1,1,1,1,1,1,1,1,1,1,1,1,1,1,1,1,1,1,1,1,1,1,1,1,1,1,1,
1,1,1,1,1,1,1,1,1,1,1,1,1,1,1,1,1,1,1,1,1,1,1,1,1,1,1,1,1,1,1,1,1,1,1,1,
1,1,1,1,1,1,1,1,4),(0.,1.),(0.,0.0122851866641497,0.0245703733282994,0.0368555599924492,
0.0491407466565989,0.0614259333207486,0.0737111199848983,0.085996306649048,
0.0982814933131977,0.110566679977347,0.122851866641497,0.135137053305647,
0.147422239969797,0.159707426633946,0.171992613298096,0.184277799962246,
0.196562986626395,0.208848173290545,0.221133359954695,0.233418546618845,
0.245703733282994,0.257988919947144,0.270274106611294,0.282559293275443,
0.294844479939593,0.307129666603743,0.319414853267893,0.331700039932042,
0.343985226596192,0.356270413260342,0.368555599924492,0.380840786588641,
0.393125973252791,0.405411159916941,0.41769634658109,0.42998153324524,0.44226671990939,
0.45455190657354,0.466837093237689,0.479122279901839,0.491407466565989,
0.503692653230138,0.515977839894288,0.528263026558438,0.540548213222588,
0.552833399886737,0.565118586550887,0.577403773215037,0.589688959879186,
0.601974146543336,0.614259333207486,0.626544519871636,0.638829706535785,
0.651114893199935,0.663400079864085,0.675685266528234,0.687970453192384,
0.700255639856534,0.712540826520684,0.724826013184833,0.737111199848983,
0.749396386513133,0.761681573177282,0.773966759841432,0.786251946505582,
0.798537133169732,0.810822319833881,0.823107506498031,0.835392693162181,
0.847677879826331,0.85996306649048,0.87224825315463,0.88453343981878,0.896818626482929,
0.909103813147079,0.921388999811229,0.933674186475379,0.945959373139528,
0.958244559803678,0.970529746467828,0.982814933131977,0.995100119796127,
1.),.UNSPECIFIED.);
#126=B_SPLINE_SURFACE_WITH_KNOTS('',1,3,((#130146,#130147,#130148,#130149,
#130150,#130151,#130152,#130153,#130154,#130155,#130156,#130157,#130158,
#130159,#130160,#130161,#130162,#130163,#130164,#130165,#130166,#130167,
#130168,#130169,#130170,#130171,#130172,#130173,#130174,#130175,#130176,
#130177,#130178,#130179,#130180,#130181,#130182,#130183,#130184,#130185,
#130186,#130187,#130188,#130189,#130190,#130191,#130192,#130193,#130194,
#130195,#130196,#130197,#130198,#130199,#130200,#130201,#130202,#130203,
#130204,#130205,#130206,#130207,#130208,#130209,#130210,#130211,#130212,
#130213,#130214,#130215,#130216,#130217,#130218,#130219,#130220,#130221,
#130222,#130223,#130224,#130225,#130226,#130227,#130228,#130229,#130230),
(#130231,#130232,#130233,#130234,#130235,#130236,#130237,#130238,#130239,
#130240,#130241,#130242,#130243,#130244,#130245,#130246,#130247,#130248,
#130249,#130250,#130251,#130252,#130253,#130254,#130255,#130256,#130257,
#130258,#130259,#130260,#130261,#130262,#130263,#130264,#130265,#130266,
#130267,#130268,#130269,#130270,#130271,#130272,#130273,#130274,#130275,
#130276,#130277,#130278,#130279,#130280,#130281,#130282,#130283,#130284,
#130285,#130286,#130287,#130288,#130289,#130290,#130291,#130292,#130293,
#130294,#130295,#130296,#130297,#130298,#130299,#130300,#130301,#130302,
#130303,#130304,#130305,#130306,#130307,#130308,#130309,#130310,#130311,
#130312,#130313,#130314,#130315)),.UNSPECIFIED.,.F.,.F.,.F.,(2,2),(4,1,
1,1,1,1,1,1,1,1,1,1,1,1,1,1,1,1,1,1,1,1,1,1,1,1,1,1,1,1,1,1,1,1,1,1,1,1,
1,1,1,1,1,1,1,1,1,1,1,1,1,1,1,1,1,1,1,1,1,1,1,1,1,1,1,1,1,1,1,1,1,1,1,1,
1,1,1,1,1,1,1,1,4),(0.,1.),(0.,0.0122851866641497,0.0245703733282994,0.0368555599924492,
0.0491407466565989,0.0614259333207486,0.0737111199848983,0.085996306649048,
0.0982814933131977,0.110566679977347,0.122851866641497,0.135137053305647,
0.147422239969797,0.159707426633946,0.171992613298096,0.184277799962246,
0.196562986626395,0.208848173290545,0.221133359954695,0.233418546618845,
0.245703733282994,0.257988919947144,0.270274106611294,0.282559293275443,
0.294844479939593,0.307129666603743,0.319414853267893,0.331700039932042,
0.343985226596192,0.356270413260342,0.368555599924492,0.380840786588641,
0.393125973252791,0.405411159916941,0.41769634658109,0.42998153324524,0.44226671990939,
0.45455190657354,0.466837093237689,0.479122279901839,0.491407466565989,
0.503692653230138,0.515977839894288,0.528263026558438,0.540548213222588,
0.552833399886737,0.565118586550887,0.577403773215037,0.589688959879186,
0.601974146543336,0.614259333207486,0.626544519871636,0.638829706535785,
0.651114893199935,0.663400079864085,0.675685266528234,0.687970453192384,
0.700255639856534,0.712540826520684,0.724826013184833,0.737111199848983,
0.749396386513133,0.761681573177282,0.773966759841432,0.786251946505582,
0.798537133169732,0.810822319833881,0.823107506498031,0.835392693162181,
0.847677879826331,0.85996306649048,0.87224825315463,0.88453343981878,0.896818626482929,
0.909103813147079,0.921388999811229,0.933674186475379,0.945959373139528,
0.958244559803678,0.970529746467828,0.982814933131977,0.995100119796127,
1.),.UNSPECIFIED.);
#127=B_SPLINE_SURFACE_WITH_KNOTS('',3,3,((#132433,#132434,#132435,#132436,
#132437,#132438,#132439,#132440,#132441),(#132442,#132443,#132444,#132445,
#132446,#132447,#132448,#132449,#132450),(#132451,#132452,#132453,#132454,
#132455,#132456,#132457,#132458,#132459),(#132460,#132461,#132462,#132463,
#132464,#132465,#132466,#132467,#132468),(#132469,#132470,#132471,#132472,
#132473,#132474,#132475,#132476,#132477),(#132478,#132479,#132480,#132481,
#132482,#132483,#132484,#132485,#132486)),.UNSPECIFIED.,.F.,.F.,.F.,(4,
2,4),(4,2,3,4),(0.,0.5,1.),(-0.00320679271163163,1.21084430265805,2.42168860531611,
6.01951071788134),.UNSPECIFIED.);
#128=B_SPLINE_SURFACE_WITH_KNOTS('',3,3,((#136533,#136534,#136535,#136536,
#136537,#136538,#136539,#136540,#136541,#136542,#136543,#136544,#136545,
#136546,#136547,#136548,#136549,#136550,#136551,#136552,#136553,#136554),
(#136555,#136556,#136557,#136558,#136559,#136560,#136561,#136562,#136563,
#136564,#136565,#136566,#136567,#136568,#136569,#136570,#136571,#136572,
#136573,#136574,#136575,#136576),(#136577,#136578,#136579,#136580,#136581,
#136582,#136583,#136584,#136585,#136586,#136587,#136588,#136589,#136590,
#136591,#136592,#136593,#136594,#136595,#136596,#136597,#136598),(#136599,
#136600,#136601,#136602,#136603,#136604,#136605,#136606,#136607,#136608,
#136609,#136610,#136611,#136612,#136613,#136614,#136615,#136616,#136617,
#136618,#136619,#136620),(#136621,#136622,#136623,#136624,#136625,#136626,
#136627,#136628,#136629,#136630,#136631,#136632,#136633,#136634,#136635,
#136636,#136637,#136638,#136639,#136640,#136641,#136642),(#136643,#136644,
#136645,#136646,#136647,#136648,#136649,#136650,#136651,#136652,#136653,
#136654,#136655,#136656,#136657,#136658,#136659,#136660,#136661,#136662,
#136663,#136664),(#136665,#136666,#136667,#136668,#136669,#136670,#136671,
#136672,#136673,#136674,#136675,#136676,#136677,#136678,#136679,#136680,
#136681,#136682,#136683,#136684,#136685,#136686),(#136687,#136688,#136689,
#136690,#136691,#136692,#136693,#136694,#136695,#136696,#136697,#136698,
#136699,#136700,#136701,#136702,#136703,#136704,#136705,#136706,#136707,
#136708),(#136709,#136710,#136711,#136712,#136713,#136714,#136715,#136716,
#136717,#136718,#136719,#136720,#136721,#136722,#136723,#136724,#136725,
#136726,#136727,#136728,#136729,#136730),(#136731,#136732,#136733,#136734,
#136735,#136736,#136737,#136738,#136739,#136740,#136741,#136742,#136743,
#136744,#136745,#136746,#136747,#136748,#136749,#136750,#136751,#136752),
(#136753,#136754,#136755,#136756,#136757,#136758,#136759,#136760,#136761,
#136762,#136763,#136764,#136765,#136766,#136767,#136768,#136769,#136770,
#136771,#136772,#136773,#136774),(#136775,#136776,#136777,#136778,#136779,
#136780,#136781,#136782,#136783,#136784,#136785,#136786,#136787,#136788,
#136789,#136790,#136791,#136792,#136793,#136794,#136795,#136796),(#136797,
#136798,#136799,#136800,#136801,#136802,#136803,#136804,#136805,#136806,
#136807,#136808,#136809,#136810,#136811,#136812,#136813,#136814,#136815,
#136816,#136817,#136818)),.UNSPECIFIED.,.F.,.F.,.F.,(4,1,1,1,1,1,1,1,1,
1,4),(4,1,1,1,1,1,1,1,1,1,1,1,1,1,1,1,1,1,1,4),(0.,0.0709766854731603,0.132271619181511,
0.254861486598212,0.377451354014914,0.500041221431615,0.622631088848316,
0.745220956265018,0.867810823681719,0.92910575739007,1.),(0.,0.13235257180777,
0.254901630119635,0.316176159275667,0.346813423853634,0.354472739998076,
0.358302398070297,0.362132056142617,0.369791372287059,0.3774506884316,0.438725217587533,
0.499999746743466,0.622548805055332,0.683823334211265,0.745097863367198,
0.80637239252323,0.867646921679163,0.928921450835096,0.990195979991028,
1.),.UNSPECIFIED.);
#129=B_SPLINE_SURFACE_WITH_KNOTS('',3,3,((#136902,#136903,#136904,#136905,
#136906,#136907,#136908,#136909,#136910,#136911,#136912,#136913,#136914,
#136915,#136916,#136917,#136918,#136919,#136920,#136921,#136922,#136923),
(#136924,#136925,#136926,#136927,#136928,#136929,#136930,#136931,#136932,
#136933,#136934,#136935,#136936,#136937,#136938,#136939,#136940,#136941,
#136942,#136943,#136944,#136945),(#136946,#136947,#136948,#136949,#136950,
#136951,#136952,#136953,#136954,#136955,#136956,#136957,#136958,#136959,
#136960,#136961,#136962,#136963,#136964,#136965,#136966,#136967),(#136968,
#136969,#136970,#136971,#136972,#136973,#136974,#136975,#136976,#136977,
#136978,#136979,#136980,#136981,#136982,#136983,#136984,#136985,#136986,
#136987,#136988,#136989),(#136990,#136991,#136992,#136993,#136994,#136995,
#136996,#136997,#136998,#136999,#137000,#137001,#137002,#137003,#137004,
#137005,#137006,#137007,#137008,#137009,#137010,#137011),(#137012,#137013,
#137014,#137015,#137016,#137017,#137018,#137019,#137020,#137021,#137022,
#137023,#137024,#137025,#137026,#137027,#137028,#137029,#137030,#137031,
#137032,#137033),(#137034,#137035,#137036,#137037,#137038,#137039,#137040,
#137041,#137042,#137043,#137044,#137045,#137046,#137047,#137048,#137049,
#137050,#137051,#137052,#137053,#137054,#137055),(#137056,#137057,#137058,
#137059,#137060,#137061,#137062,#137063,#137064,#137065,#137066,#137067,
#137068,#137069,#137070,#137071,#137072,#137073,#137074,#137075,#137076,
#137077),(#137078,#137079,#137080,#137081,#137082,#137083,#137084,#137085,
#137086,#137087,#137088,#137089,#137090,#137091,#137092,#137093,#137094,
#137095,#137096,#137097,#137098,#137099),(#137100,#137101,#137102,#137103,
#137104,#137105,#137106,#137107,#137108,#137109,#137110,#137111,#137112,
#137113,#137114,#137115,#137116,#137117,#137118,#137119,#137120,#137121),
(#137122,#137123,#137124,#137125,#137126,#137127,#137128,#137129,#137130,
#137131,#137132,#137133,#137134,#137135,#137136,#137137,#137138,#137139,
#137140,#137141,#137142,#137143),(#137144,#137145,#137146,#137147,#137148,
#137149,#137150,#137151,#137152,#137153,#137154,#137155,#137156,#137157,
#137158,#137159,#137160,#137161,#137162,#137163,#137164,#137165),(#137166,
#137167,#137168,#137169,#137170,#137171,#137172,#137173,#137174,#137175,
#137176,#137177,#137178,#137179,#137180,#137181,#137182,#137183,#137184,
#137185,#137186,#137187)),.UNSPECIFIED.,.F.,.F.,.F.,(4,1,1,1,1,1,1,1,1,
1,4),(4,1,1,1,1,1,1,1,1,1,1,1,1,1,1,1,1,1,1,4),(0.,0.0709778601999125,0.132273968651597,
0.254866185554966,0.377458402458335,0.500050619361704,0.622642836265073,
0.745235053168442,0.86782727007181,0.929123378523495,1.),(0.,0.132351844415717,
0.254900175335541,0.316174340795552,0.346811423525508,0.354470694207947,
0.358300329549167,0.362129964890486,0.369789235572925,0.377448506255464,
0.438722671715376,0.499996837175288,0.622545168095112,0.683819333555024,
0.745093499014936,0.806367664474947,0.867641829934859,0.928915995394771,
0.990190160854683,1.),.UNSPECIFIED.);
#130=B_SPLINE_SURFACE_WITH_KNOTS('',3,3,((#137610,#137611,#137612,#137613,
#137614,#137615,#137616,#137617,#137618,#137619,#137620,#137621,#137622,
#137623,#137624,#137625),(#137626,#137627,#137628,#137629,#137630,#137631,
#137632,#137633,#137634,#137635,#137636,#137637,#137638,#137639,#137640,
#137641),(#137642,#137643,#137644,#137645,#137646,#137647,#137648,#137649,
#137650,#137651,#137652,#137653,#137654,#137655,#137656,#137657),(#137658,
#137659,#137660,#137661,#137662,#137663,#137664,#137665,#137666,#137667,
#137668,#137669,#137670,#137671,#137672,#137673),(#137674,#137675,#137676,
#137677,#137678,#137679,#137680,#137681,#137682,#137683,#137684,#137685,
#137686,#137687,#137688,#137689),(#137690,#137691,#137692,#137693,#137694,
#137695,#137696,#137697,#137698,#137699,#137700,#137701,#137702,#137703,
#137704,#137705),(#137706,#137707,#137708,#137709,#137710,#137711,#137712,
#137713,#137714,#137715,#137716,#137717,#137718,#137719,#137720,#137721),
(#137722,#137723,#137724,#137725,#137726,#137727,#137728,#137729,#137730,
#137731,#137732,#137733,#137734,#137735,#137736,#137737),(#137738,#137739,
#137740,#137741,#137742,#137743,#137744,#137745,#137746,#137747,#137748,
#137749,#137750,#137751,#137752,#137753),(#137754,#137755,#137756,#137757,
#137758,#137759,#137760,#137761,#137762,#137763,#137764,#137765,#137766,
#137767,#137768,#137769),(#137770,#137771,#137772,#137773,#137774,#137775,
#137776,#137777,#137778,#137779,#137780,#137781,#137782,#137783,#137784,
#137785),(#137786,#137787,#137788,#137789,#137790,#137791,#137792,#137793,
#137794,#137795,#137796,#137797,#137798,#137799,#137800,#137801),(#137802,
#137803,#137804,#137805,#137806,#137807,#137808,#137809,#137810,#137811,
#137812,#137813,#137814,#137815,#137816,#137817),(#137818,#137819,#137820,
#137821,#137822,#137823,#137824,#137825,#137826,#137827,#137828,#137829,
#137830,#137831,#137832,#137833)),.UNSPECIFIED.,.F.,.F.,.F.,(4,1,1,1,1,
1,1,1,1,1,1,4),(4,1,1,1,1,1,1,1,1,1,1,1,1,4),(0.,0.134085205134682,0.255951223187441,
0.3778172412402,0.499683259292959,0.621549277345718,0.682482286372097,0.743415295398476,
0.804348304424856,0.865281313451235,0.926214322477615,1.),(0.,0.132446393239555,
0.193720576817934,0.254994760396314,0.316268943974693,0.377543127553072,
0.408180219342262,0.438817311131451,0.469454402920641,0.500091494709831,
0.56136567828821,0.622639861866589,0.745188229023347,1.),.UNSPECIFIED.);
#131=B_SPLINE_SURFACE_WITH_KNOTS('',3,3,((#138125,#138126,#138127,#138128,
#138129,#138130,#138131,#138132,#138133),(#138134,#138135,#138136,#138137,
#138138,#138139,#138140,#138141,#138142),(#138143,#138144,#138145,#138146,
#138147,#138148,#138149,#138150,#138151),(#138152,#138153,#138154,#138155,
#138156,#138157,#138158,#138159,#138160),(#138161,#138162,#138163,#138164,
#138165,#138166,#138167,#138168,#138169),(#138170,#138171,#138172,#138173,
#138174,#138175,#138176,#138177,#138178),(#138179,#138180,#138181,#138182,
#138183,#138184,#138185,#138186,#138187),(#138188,#138189,#138190,#138191,
#138192,#138193,#138194,#138195,#138196),(#138197,#138198,#138199,#138200,
#138201,#138202,#138203,#138204,#138205),(#138206,#138207,#138208,#138209,
#138210,#138211,#138212,#138213,#138214),(#138215,#138216,#138217,#138218,
#138219,#138220,#138221,#138222,#138223),(#138224,#138225,#138226,#138227,
#138228,#138229,#138230,#138231,#138232)),.UNSPECIFIED.,.F.,.F.,.F.,(4,
1,1,1,1,1,1,1,1,4),(4,1,1,1,1,1,4),(0.,0.133433046999215,0.194394733712586,
0.255356420425957,0.316318107139328,0.377279793852699,0.499203167279441,
0.621126540706183,0.743049914132925,1.),(0.,0.267979296737124,0.384002950769135,
0.500026604801238,0.616050258833249,0.73207391286526,1.),.UNSPECIFIED.);
#132=B_SPLINE_SURFACE_WITH_KNOTS('',3,3,((#138251,#138252,#138253,#138254,
#138255,#138256,#138257,#138258,#138259),(#138260,#138261,#138262,#138263,
#138264,#138265,#138266,#138267,#138268),(#138269,#138270,#138271,#138272,
#138273,#138274,#138275,#138276,#138277),(#138278,#138279,#138280,#138281,
#138282,#138283,#138284,#138285,#138286),(#138287,#138288,#138289,#138290,
#138291,#138292,#138293,#138294,#138295),(#138296,#138297,#138298,#138299,
#138300,#138301,#138302,#138303,#138304),(#138305,#138306,#138307,#138308,
#138309,#138310,#138311,#138312,#138313),(#138314,#138315,#138316,#138317,
#138318,#138319,#138320,#138321,#138322),(#138323,#138324,#138325,#138326,
#138327,#138328,#138329,#138330,#138331),(#138332,#138333,#138334,#138335,
#138336,#138337,#138338,#138339,#138340),(#138341,#138342,#138343,#138344,
#138345,#138346,#138347,#138348,#138349),(#138350,#138351,#138352,#138353,
#138354,#138355,#138356,#138357,#138358),(#138359,#138360,#138361,#138362,
#138363,#138364,#138365,#138366,#138367)),.UNSPECIFIED.,.F.,.F.,.F.,(4,
1,1,1,1,1,1,1,1,1,4),(4,1,1,1,1,1,4),(0.,0.133046842649236,0.255715309974117,
0.378383777298997,0.501052244623878,0.623720711948759,0.746389179273639,
0.807723412936079,0.86905764659852,0.93039188026096,1.),(0.,0.268199906405258,
0.384249094355361,0.500298282305557,0.61634747025566,0.732396658205762,
1.),.UNSPECIFIED.);
#133=B_SPLINE_SURFACE_WITH_KNOTS('',3,3,((#138412,#138413,#138414,#138415,
#138416,#138417,#138418,#138419,#138420),(#138421,#138422,#138423,#138424,
#138425,#138426,#138427,#138428,#138429),(#138430,#138431,#138432,#138433,
#138434,#138435,#138436,#138437,#138438),(#138439,#138440,#138441,#138442,
#138443,#138444,#138445,#138446,#138447),(#138448,#138449,#138450,#138451,
#138452,#138453,#138454,#138455,#138456),(#138457,#138458,#138459,#138460,
#138461,#138462,#138463,#138464,#138465),(#138466,#138467,#138468,#138469,
#138470,#138471,#138472,#138473,#138474),(#138475,#138476,#138477,#138478,
#138479,#138480,#138481,#138482,#138483),(#138484,#138485,#138486,#138487,
#138488,#138489,#138490,#138491,#138492),(#138493,#138494,#138495,#138496,
#138497,#138498,#138499,#138500,#138501),(#138502,#138503,#138504,#138505,
#138506,#138507,#138508,#138509,#138510),(#138511,#138512,#138513,#138514,
#138515,#138516,#138517,#138518,#138519),(#138520,#138521,#138522,#138523,
#138524,#138525,#138526,#138527,#138528),(#138529,#138530,#138531,#138532,
#138533,#138534,#138535,#138536,#138537),(#138538,#138539,#138540,#138541,
#138542,#138543,#138544,#138545,#138546),(#138547,#138548,#138549,#138550,
#138551,#138552,#138553,#138554,#138555)),.UNSPECIFIED.,.F.,.F.,.F.,(4,
1,1,1,1,1,1,1,1,1,1,1,1,4),(4,1,1,1,1,1,4),(0.,0.130820538487595,0.192157288159239,
0.253494037830883,0.314830787502527,0.376167537174171,0.437504286845815,
0.498841036517459,0.560177786189103,0.621514535860747,0.682851285532391,
0.744188035204036,0.866861534547324,1.),(0.,0.268122375620859,0.384109336577756,
0.500096297534654,0.616083258491645,0.732070219448542,1.),.UNSPECIFIED.);
#134=B_SPLINE_SURFACE_WITH_KNOTS('',3,3,((#138565,#138566,#138567,#138568,
#138569,#138570,#138571),(#138572,#138573,#138574,#138575,#138576,#138577,
#138578),(#138579,#138580,#138581,#138582,#138583,#138584,#138585),(#138586,
#138587,#138588,#138589,#138590,#138591,#138592),(#138593,#138594,#138595,
#138596,#138597,#138598,#138599),(#138600,#138601,#138602,#138603,#138604,
#138605,#138606),(#138607,#138608,#138609,#138610,#138611,#138612,#138613),
(#138614,#138615,#138616,#138617,#138618,#138619,#138620),(#138621,#138622,
#138623,#138624,#138625,#138626,#138627),(#138628,#138629,#138630,#138631,
#138632,#138633,#138634),(#138635,#138636,#138637,#138638,#138639,#138640,
#138641),(#138642,#138643,#138644,#138645,#138646,#138647,#138648)),
 .UNSPECIFIED.,.F.,.F.,.F.,(4,1,1,1,1,1,1,1,1,4),(4,1,1,1,4),(0.,0.25699883636701,
0.378859719476966,0.500720602586923,0.561651044141901,0.622581485696879,
0.683511927251857,0.744442368806835,0.866303251916792,1.),(0.,0.268023493710597,
0.500050957704942,0.732078421699288,1.),.UNSPECIFIED.);
#135=B_SPLINE_SURFACE_WITH_KNOTS('',3,3,((#138716,#138717,#138718,#138719,
#138720,#138721,#138722,#138723,#138724,#138725,#138726,#138727,#138728,
#138729,#138730,#138731),(#138732,#138733,#138734,#138735,#138736,#138737,
#138738,#138739,#138740,#138741,#138742,#138743,#138744,#138745,#138746,
#138747),(#138748,#138749,#138750,#138751,#138752,#138753,#138754,#138755,
#138756,#138757,#138758,#138759,#138760,#138761,#138762,#138763),(#138764,
#138765,#138766,#138767,#138768,#138769,#138770,#138771,#138772,#138773,
#138774,#138775,#138776,#138777,#138778,#138779),(#138780,#138781,#138782,
#138783,#138784,#138785,#138786,#138787,#138788,#138789,#138790,#138791,
#138792,#138793,#138794,#138795),(#138796,#138797,#138798,#138799,#138800,
#138801,#138802,#138803,#138804,#138805,#138806,#138807,#138808,#138809,
#138810,#138811),(#138812,#138813,#138814,#138815,#138816,#138817,#138818,
#138819,#138820,#138821,#138822,#138823,#138824,#138825,#138826,#138827),
(#138828,#138829,#138830,#138831,#138832,#138833,#138834,#138835,#138836,
#138837,#138838,#138839,#138840,#138841,#138842,#138843),(#138844,#138845,
#138846,#138847,#138848,#138849,#138850,#138851,#138852,#138853,#138854,
#138855,#138856,#138857,#138858,#138859),(#138860,#138861,#138862,#138863,
#138864,#138865,#138866,#138867,#138868,#138869,#138870,#138871,#138872,
#138873,#138874,#138875),(#138876,#138877,#138878,#138879,#138880,#138881,
#138882,#138883,#138884,#138885,#138886,#138887,#138888,#138889,#138890,
#138891),(#138892,#138893,#138894,#138895,#138896,#138897,#138898,#138899,
#138900,#138901,#138902,#138903,#138904,#138905,#138906,#138907),(#138908,
#138909,#138910,#138911,#138912,#138913,#138914,#138915,#138916,#138917,
#138918,#138919,#138920,#138921,#138922,#138923),(#138924,#138925,#138926,
#138927,#138928,#138929,#138930,#138931,#138932,#138933,#138934,#138935,
#138936,#138937,#138938,#138939)),.UNSPECIFIED.,.F.,.F.,.F.,(4,1,1,1,1,
1,1,1,1,1,1,4),(4,1,1,1,1,1,1,1,1,1,1,1,1,4),(0.,0.134085205130259,0.25595122318364,
0.377817241237021,0.499683259290403,0.621549277343784,0.682482286370475,
0.743415295397166,0.804348304423856,0.865281313450547,0.926214322477238,
1.),(0.,0.132425037814215,0.193700746780136,0.254976455746057,0.316252164711979,
0.3775278736779,0.40816572816086,0.438803582643821,0.469441437126781,0.500079291609742,
0.561355000575663,0.622630709541584,0.745182127473427,1.),.UNSPECIFIED.);
#136=B_SPLINE_SURFACE_WITH_KNOTS('',3,3,((#140502,#140503,#140504,#140505,
#140506,#140507),(#140508,#140509,#140510,#140511,#140512,#140513),(#140514,
#140515,#140516,#140517,#140518,#140519),(#140520,#140521,#140522,#140523,
#140524,#140525),(#140526,#140527,#140528,#140529,#140530,#140531)),
 .UNSPECIFIED.,.F.,.F.,.F.,(4,1,4),(4,1,1,4),(0.,0.369957079162583,1.),
(0.,0.342988625591935,0.659504826702446,1.),.UNSPECIFIED.);
#137=B_SPLINE_SURFACE_WITH_KNOTS('',3,3,((#141306,#141307,#141308,#141309,
#141310,#141311,#141312,#141313),(#141314,#141315,#141316,#141317,#141318,
#141319,#141320,#141321),(#141322,#141323,#141324,#141325,#141326,#141327,
#141328,#141329),(#141330,#141331,#141332,#141333,#141334,#141335,#141336,
#141337),(#141338,#141339,#141340,#141341,#141342,#141343,#141344,#141345),
(#141346,#141347,#141348,#141349,#141350,#141351,#141352,#141353),(#141354,
#141355,#141356,#141357,#141358,#141359,#141360,#141361),(#141362,#141363,
#141364,#141365,#141366,#141367,#141368,#141369),(#141370,#141371,#141372,
#141373,#141374,#141375,#141376,#141377),(#141378,#141379,#141380,#141381,
#141382,#141383,#141384,#141385),(#141386,#141387,#141388,#141389,#141390,
#141391,#141392,#141393),(#141394,#141395,#141396,#141397,#141398,#141399,
#141400,#141401)),.UNSPECIFIED.,.F.,.F.,.F.,(4,1,1,1,1,1,1,1,1,4),(4,1,
1,1,1,4),(0.,0.132237188173058,0.254692642818978,0.499603552110817,0.622059006756737,
0.744514461402656,0.805742188725616,0.866969916048576,0.928197643371536,
1.),(0.,0.368244530951745,0.72001943774428,0.807963164442414,0.895906891140547,
1.),.UNSPECIFIED.);
#138=B_SPLINE_SURFACE_WITH_KNOTS('',3,3,((#142290,#142291,#142292,#142293,
#142294,#142295,#142296,#142297,#142298,#142299,#142300,#142301,#142302,
#142303,#142304,#142305,#142306),(#142307,#142308,#142309,#142310,#142311,
#142312,#142313,#142314,#142315,#142316,#142317,#142318,#142319,#142320,
#142321,#142322,#142323),(#142324,#142325,#142326,#142327,#142328,#142329,
#142330,#142331,#142332,#142333,#142334,#142335,#142336,#142337,#142338,
#142339,#142340),(#142341,#142342,#142343,#142344,#142345,#142346,#142347,
#142348,#142349,#142350,#142351,#142352,#142353,#142354,#142355,#142356,
#142357),(#142358,#142359,#142360,#142361,#142362,#142363,#142364,#142365,
#142366,#142367,#142368,#142369,#142370,#142371,#142372,#142373,#142374),
(#142375,#142376,#142377,#142378,#142379,#142380,#142381,#142382,#142383,
#142384,#142385,#142386,#142387,#142388,#142389,#142390,#142391),(#142392,
#142393,#142394,#142395,#142396,#142397,#142398,#142399,#142400,#142401,
#142402,#142403,#142404,#142405,#142406,#142407,#142408),(#142409,#142410,
#142411,#142412,#142413,#142414,#142415,#142416,#142417,#142418,#142419,
#142420,#142421,#142422,#142423,#142424,#142425),(#142426,#142427,#142428,
#142429,#142430,#142431,#142432,#142433,#142434,#142435,#142436,#142437,
#142438,#142439,#142440,#142441,#142442),(#142443,#142444,#142445,#142446,
#142447,#142448,#142449,#142450,#142451,#142452,#142453,#142454,#142455,
#142456,#142457,#142458,#142459),(#142460,#142461,#142462,#142463,#142464,
#142465,#142466,#142467,#142468,#142469,#142470,#142471,#142472,#142473,
#142474,#142475,#142476)),.UNSPECIFIED.,.F.,.F.,.F.,(4,1,1,1,1,1,1,1,4),
(4,1,1,1,1,1,1,1,1,1,1,1,1,1,4),(0.,0.0889679837912601,0.269044155127216,
0.449120326463171,0.629196497799126,0.719234583467104,0.809272669135082,
0.899313189025203,1.),(0.,0.0299186510352439,0.0465421302688725,0.0548538698856868,
0.0631656095025011,0.0714773491193154,0.0797890887361297,0.0964125679697582,
0.113036047203387,0.146283005670644,0.212776922605158,0.279270839539673,
0.412258673408701,0.678234341146759,1.),.UNSPECIFIED.);
#139=B_SPLINE_SURFACE_WITH_KNOTS('',3,3,((#142494,#142495,#142496,#142497,
#142498,#142499,#142500,#142501,#142502,#142503,#142504,#142505,#142506,
#142507,#142508,#142509,#142510),(#142511,#142512,#142513,#142514,#142515,
#142516,#142517,#142518,#142519,#142520,#142521,#142522,#142523,#142524,
#142525,#142526,#142527),(#142528,#142529,#142530,#142531,#142532,#142533,
#142534,#142535,#142536,#142537,#142538,#142539,#142540,#142541,#142542,
#142543,#142544),(#142545,#142546,#142547,#142548,#142549,#142550,#142551,
#142552,#142553,#142554,#142555,#142556,#142557,#142558,#142559,#142560,
#142561),(#142562,#142563,#142564,#142565,#142566,#142567,#142568,#142569,
#142570,#142571,#142572,#142573,#142574,#142575,#142576,#142577,#142578),
(#142579,#142580,#142581,#142582,#142583,#142584,#142585,#142586,#142587,
#142588,#142589,#142590,#142591,#142592,#142593,#142594,#142595),(#142596,
#142597,#142598,#142599,#142600,#142601,#142602,#142603,#142604,#142605,
#142606,#142607,#142608,#142609,#142610,#142611,#142612),(#142613,#142614,
#142615,#142616,#142617,#142618,#142619,#142620,#142621,#142622,#142623,
#142624,#142625,#142626,#142627,#142628,#142629),(#142630,#142631,#142632,
#142633,#142634,#142635,#142636,#142637,#142638,#142639,#142640,#142641,
#142642,#142643,#142644,#142645,#142646),(#142647,#142648,#142649,#142650,
#142651,#142652,#142653,#142654,#142655,#142656,#142657,#142658,#142659,
#142660,#142661,#142662,#142663),(#142664,#142665,#142666,#142667,#142668,
#142669,#142670,#142671,#142672,#142673,#142674,#142675,#142676,#142677,
#142678,#142679,#142680)),.UNSPECIFIED.,.F.,.F.,.F.,(4,1,1,1,1,1,1,1,4),
(4,1,1,1,1,1,1,1,1,1,1,1,1,1,4),(0.,0.100847834071465,0.1908968616028,0.280915298912381,
0.370933736221962,0.550970610841123,0.731007485460285,0.911044360079447,
1.),(0.,0.0299179598037716,0.0465410175397665,0.054852546407764,0.0631640752757615,
0.0714756041437589,0.0797871330117564,0.0964101907477513,0.113033248483746,
0.146279363955736,0.212771594899716,0.279263825843695,0.412248287731655,
0.678217211507574,1.),.UNSPECIFIED.);
#140=B_SPLINE_SURFACE_WITH_KNOTS('',3,3,((#142692,#142693,#142694,#142695,
#142696,#142697,#142698,#142699),(#142700,#142701,#142702,#142703,#142704,
#142705,#142706,#142707),(#142708,#142709,#142710,#142711,#142712,#142713,
#142714,#142715),(#142716,#142717,#142718,#142719,#142720,#142721,#142722,
#142723),(#142724,#142725,#142726,#142727,#142728,#142729,#142730,#142731),
(#142732,#142733,#142734,#142735,#142736,#142737,#142738,#142739),(#142740,
#142741,#142742,#142743,#142744,#142745,#142746,#142747),(#142748,#142749,
#142750,#142751,#142752,#142753,#142754,#142755),(#142756,#142757,#142758,
#142759,#142760,#142761,#142762,#142763),(#142764,#142765,#142766,#142767,
#142768,#142769,#142770,#142771),(#142772,#142773,#142774,#142775,#142776,
#142777,#142778,#142779),(#142780,#142781,#142782,#142783,#142784,#142785,
#142786,#142787)),.UNSPECIFIED.,.F.,.F.,.F.,(4,1,1,1,1,1,1,1,1,4),(4,1,
1,1,1,4),(0.,0.0720826203636762,0.133291887827124,0.194500937409253,0.255709986991381,
0.378128086155638,0.500546185319895,0.745382383648409,0.867800482812665,
1.),(0.,0.368244531554185,0.720019439162548,0.807963166064639,0.895906892966729,
1.),.UNSPECIFIED.);
#141=B_SPLINE_SURFACE_WITH_KNOTS('',3,3,((#144028,#144029,#144030,#144031),
(#144032,#144033,#144034,#144035),(#144036,#144037,#144038,#144039),(#144040,
#144041,#144042,#144043),(#144044,#144045,#144046,#144047),(#144048,#144049,
#144050,#144051),(#144052,#144053,#144054,#144055)),.UNSPECIFIED.,.F.,.F.,
 .F.,(4,1,1,1,4),(4,4),(0.,0.244135329830522,0.48749215556374,0.730848981296959,
1.),(0.,1.),.UNSPECIFIED.);
#142=B_SPLINE_SURFACE_WITH_KNOTS('',3,3,((#144080,#144081,#144082,#144083),
(#144084,#144085,#144086,#144087),(#144088,#144089,#144090,#144091),(#144092,
#144093,#144094,#144095)),.UNSPECIFIED.,.F.,.F.,.F.,(4,4),(4,4),(0.,1.),
(0.,1.),.UNSPECIFIED.);
#143=B_SPLINE_SURFACE_WITH_KNOTS('',3,3,((#144143,#144144,#144145,#144146),
(#144147,#144148,#144149,#144150),(#144151,#144152,#144153,#144154),(#144155,
#144156,#144157,#144158)),.UNSPECIFIED.,.F.,.F.,.F.,(4,4),(4,4),(0.,1.),
(0.,1.),.UNSPECIFIED.);
#144=B_SPLINE_SURFACE_WITH_KNOTS('',3,3,((#144194,#144195,#144196,#144197),
(#144198,#144199,#144200,#144201),(#144202,#144203,#144204,#144205),(#144206,
#144207,#144208,#144209)),.UNSPECIFIED.,.F.,.F.,.F.,(4,4),(4,4),(0.,1.),
(0.,1.),.UNSPECIFIED.);
#145=B_SPLINE_SURFACE_WITH_KNOTS('',3,3,((#144342,#144343,#144344,#144345,
#144346,#144347),(#144348,#144349,#144350,#144351,#144352,#144353),(#144354,
#144355,#144356,#144357,#144358,#144359),(#144360,#144361,#144362,#144363,
#144364,#144365),(#144366,#144367,#144368,#144369,#144370,#144371)),
 .UNSPECIFIED.,.F.,.F.,.F.,(4,1,4),(4,1,1,4),(0.,0.697012231186303,1.),
(0.,0.257158083013883,0.500013148495854,1.),.UNSPECIFIED.);
#146=B_SPLINE_SURFACE_WITH_KNOTS('',3,3,((#144608,#144609,#144610,#144611,
#144612,#144613,#144614,#144615,#144616),(#144617,#144618,#144619,#144620,
#144621,#144622,#144623,#144624,#144625),(#144626,#144627,#144628,#144629,
#144630,#144631,#144632,#144633,#144634),(#144635,#144636,#144637,#144638,
#144639,#144640,#144641,#144642,#144643),(#144644,#144645,#144646,#144647,
#144648,#144649,#144650,#144651,#144652),(#144653,#144654,#144655,#144656,
#144657,#144658,#144659,#144660,#144661)),.UNSPECIFIED.,.F.,.F.,.F.,(4,
1,1,4),(4,1,1,1,1,1,4),(0.,0.131537245772329,0.300810603491857,1.),(0.,
0.135760677797667,0.257212789613593,0.378664901429518,0.500117013245444,
0.743021236877295,1.),.UNSPECIFIED.);
#147=B_SPLINE_SURFACE_WITH_KNOTS('',3,3,((#144666,#144667,#144668,#144669),
(#144670,#144671,#144672,#144673),(#144674,#144675,#144676,#144677),(#144678,
#144679,#144680,#144681)),.UNSPECIFIED.,.F.,.F.,.F.,(4,4),(4,4),(0.,1.),
(0.,1.),.UNSPECIFIED.);
#148=B_SPLINE_SURFACE_WITH_KNOTS('',3,3,((#144814,#144815,#144816,#144817,
#144818,#144819,#144820),(#144821,#144822,#144823,#144824,#144825,#144826,
#144827),(#144828,#144829,#144830,#144831,#144832,#144833,#144834),(#144835,
#144836,#144837,#144838,#144839,#144840,#144841),(#144842,#144843,#144844,
#144845,#144846,#144847,#144848)),.UNSPECIFIED.,.F.,.F.,.F.,(4,1,4),(4,
1,1,1,4),(0.,0.434785331173339,1.),(0.,0.317132125632511,0.510431545616903,
0.703730965601296,1.),.UNSPECIFIED.);
#149=B_SPLINE_SURFACE_WITH_KNOTS('',3,3,((#145067,#145068,#145069,#145070,
#145071,#145072,#145073),(#145074,#145075,#145076,#145077,#145078,#145079,
#145080),(#145081,#145082,#145083,#145084,#145085,#145086,#145087),(#145088,
#145089,#145090,#145091,#145092,#145093,#145094)),.UNSPECIFIED.,.F.,.F.,
 .F.,(4,4),(4,1,1,1,4),(0.,1.),(0.,0.317106921791329,0.510285028193446,
0.703322658299063,1.),.UNSPECIFIED.);
#150=B_SPLINE_SURFACE_WITH_KNOTS('',3,3,((#145106,#145107,#145108,#145109,
#145110,#145111),(#145112,#145113,#145114,#145115,#145116,#145117),(#145118,
#145119,#145120,#145121,#145122,#145123),(#145124,#145125,#145126,#145127,
#145128,#145129)),.UNSPECIFIED.,.F.,.F.,.F.,(4,4),(4,1,1,4),(0.,1.),(0.,
0.342987585047177,0.659504136375237,1.),.UNSPECIFIED.);
#151=B_SPLINE_SURFACE_WITH_KNOTS('',3,3,((#145239,#145240,#145241,#145242),
(#145243,#145244,#145245,#145246),(#145247,#145248,#145249,#145250),(#145251,
#145252,#145253,#145254)),.UNSPECIFIED.,.F.,.F.,.F.,(4,4),(4,4),(0.,1.),
(0.,1.),.UNSPECIFIED.);
#152=B_SPLINE_SURFACE_WITH_KNOTS('',3,3,((#147022,#147023,#147024,#147025,
#147026),(#147027,#147028,#147029,#147030,#147031),(#147032,#147033,#147034,
#147035,#147036),(#147037,#147038,#147039,#147040,#147041),(#147042,#147043,
#147044,#147045,#147046),(#147047,#147048,#147049,#147050,#147051),(#147052,
#147053,#147054,#147055,#147056),(#147057,#147058,#147059,#147060,#147061),
(#147062,#147063,#147064,#147065,#147066),(#147067,#147068,#147069,#147070,
#147071),(#147072,#147073,#147074,#147075,#147076),(#147077,#147078,#147079,
#147080,#147081),(#147082,#147083,#147084,#147085,#147086),(#147087,#147088,
#147089,#147090,#147091),(#147092,#147093,#147094,#147095,#147096)),
 .UNSPECIFIED.,.F.,.F.,.F.,(4,1,1,1,1,1,1,1,1,1,1,1,4),(4,1,4),(0.,0.132758396201778,
0.255171695067938,0.316378344501018,0.377584993934098,0.438791643367178,
0.499998292800258,0.561204942233338,0.622411591666418,0.683618241099498,
0.744824890532579,0.867238189398739,1.),(0.,0.579456290792951,1.),
 .UNSPECIFIED.);
#153=B_SPLINE_SURFACE_WITH_KNOTS('',3,3,((#148668,#148669,#148670,#148671,
#148672,#148673,#148674),(#148675,#148676,#148677,#148678,#148679,#148680,
#148681),(#148682,#148683,#148684,#148685,#148686,#148687,#148688),(#148689,
#148690,#148691,#148692,#148693,#148694,#148695),(#148696,#148697,#148698,
#148699,#148700,#148701,#148702),(#148703,#148704,#148705,#148706,#148707,
#148708,#148709),(#148710,#148711,#148712,#148713,#148714,#148715,#148716),
(#148717,#148718,#148719,#148720,#148721,#148722,#148723),(#148724,#148725,
#148726,#148727,#148728,#148729,#148730)),.UNSPECIFIED.,.F.,.F.,.F.,(4,
1,1,1,1,1,4),(4,1,1,1,4),(0.,0.132239664806569,0.254822586974579,0.4999884313106,
0.62257135347861,0.74515427564662,1.),(0.,0.263399375189117,0.5001298925661,
0.736860409943177,1.),.UNSPECIFIED.);
#154=B_SPLINE_SURFACE_WITH_KNOTS('',3,3,((#149012,#149013,#149014,#149015,
#149016,#149017,#149018),(#149019,#149020,#149021,#149022,#149023,#149024,
#149025),(#149026,#149027,#149028,#149029,#149030,#149031,#149032),(#149033,
#149034,#149035,#149036,#149037,#149038,#149039),(#149040,#149041,#149042,
#149043,#149044,#149045,#149046),(#149047,#149048,#149049,#149050,#149051,
#149052,#149053),(#149054,#149055,#149056,#149057,#149058,#149059,#149060),
(#149061,#149062,#149063,#149064,#149065,#149066,#149067),(#149068,#149069,
#149070,#149071,#149072,#149073,#149074),(#149075,#149076,#149077,#149078,
#149079,#149080,#149081),(#149082,#149083,#149084,#149085,#149086,#149087,
#149088),(#149089,#149090,#149091,#149092,#149093,#149094,#149095),(#149096,
#149097,#149098,#149099,#149100,#149101,#149102),(#149103,#149104,#149105,
#149106,#149107,#149108,#149109),(#149110,#149111,#149112,#149113,#149114,
#149115,#149116)),.UNSPECIFIED.,.F.,.F.,.F.,(4,1,1,1,1,1,1,1,1,1,1,1,4),
(4,1,1,1,4),(0.,0.132202892489769,0.193512430520198,0.254821968550627,0.316131506581056,
0.377441044611485,0.438750582641914,0.500060120672344,0.561369658702773,
0.622679196733201,0.74529827279406,0.867917348854918,1.),(0.,0.262289949012551,
0.500131074192934,0.737972199373412,1.),.UNSPECIFIED.);
#155=B_SPLINE_SURFACE_WITH_KNOTS('',3,3,((#149465,#149466,#149467,#149468,
#149469,#149470,#149471),(#149472,#149473,#149474,#149475,#149476,#149477,
#149478),(#149479,#149480,#149481,#149482,#149483,#149484,#149485),(#149486,
#149487,#149488,#149489,#149490,#149491,#149492),(#149493,#149494,#149495,
#149496,#149497,#149498,#149499),(#149500,#149501,#149502,#149503,#149504,
#149505,#149506),(#149507,#149508,#149509,#149510,#149511,#149512,#149513),
(#149514,#149515,#149516,#149517,#149518,#149519,#149520),(#149521,#149522,
#149523,#149524,#149525,#149526,#149527)),.UNSPECIFIED.,.F.,.F.,.F.,(4,
1,1,1,1,1,4),(4,1,1,1,4),(0.,0.132239677404676,0.254822595509748,0.499988431719892,
0.622571349824964,0.745154267930036,1.),(0.,0.263425190538822,0.500155220443197,
0.736885250347666,1.),.UNSPECIFIED.);
#156=B_SPLINE_SURFACE_WITH_KNOTS('',3,3,((#149635,#149636,#149637,#149638,
#149639,#149640,#149641),(#149642,#149643,#149644,#149645,#149646,#149647,
#149648),(#149649,#149650,#149651,#149652,#149653,#149654,#149655),(#149656,
#149657,#149658,#149659,#149660,#149661,#149662),(#149663,#149664,#149665,
#149666,#149667,#149668,#149669),(#149670,#149671,#149672,#149673,#149674,
#149675,#149676),(#149677,#149678,#149679,#149680,#149681,#149682,#149683),
(#149684,#149685,#149686,#149687,#149688,#149689,#149690),(#149691,#149692,
#149693,#149694,#149695,#149696,#149697),(#149698,#149699,#149700,#149701,
#149702,#149703,#149704),(#149705,#149706,#149707,#149708,#149709,#149710,
#149711),(#149712,#149713,#149714,#149715,#149716,#149717,#149718),(#149719,
#149720,#149721,#149722,#149723,#149724,#149725)),.UNSPECIFIED.,.F.,.F.,
 .F.,(4,1,1,1,1,1,1,1,1,1,4),(4,1,1,1,4),(0.,0.132545826215179,0.255032336533119,
0.377518846851059,0.438762102010029,0.500005357168999,0.561248612327969,
0.622491867486939,0.744978377804879,0.867464888122819,1.),(0.,0.262900516152029,
0.500175417475005,0.737450318797982,1.),.UNSPECIFIED.);
#157=B_SPLINE_SURFACE_WITH_KNOTS('',3,3,((#150344,#150345,#150346,#150347,
#150348,#150349,#150350),(#150351,#150352,#150353,#150354,#150355,#150356,
#150357),(#150358,#150359,#150360,#150361,#150362,#150363,#150364),(#150365,
#150366,#150367,#150368,#150369,#150370,#150371),(#150372,#150373,#150374,
#150375,#150376,#150377,#150378),(#150379,#150380,#150381,#150382,#150383,
#150384,#150385),(#150386,#150387,#150388,#150389,#150390,#150391,#150392),
(#150393,#150394,#150395,#150396,#150397,#150398,#150399),(#150400,#150401,
#150402,#150403,#150404,#150405,#150406)),.UNSPECIFIED.,.F.,.F.,.F.,(4,
1,1,1,1,1,4),(4,1,1,1,4),(0.,0.132239677404625,0.254822595509704,0.499988431719863,
0.622571349824942,0.745154267930021,1.),(0.,0.26342519053886,0.500155220443287,
0.736885250347713,1.),.UNSPECIFIED.);
#158=B_SPLINE_SURFACE_WITH_KNOTS('',3,3,((#150712,#150713,#150714,#150715,
#150716,#150717,#150718),(#150719,#150720,#150721,#150722,#150723,#150724,
#150725),(#150726,#150727,#150728,#150729,#150730,#150731,#150732),(#150733,
#150734,#150735,#150736,#150737,#150738,#150739),(#150740,#150741,#150742,
#150743,#150744,#150745,#150746),(#150747,#150748,#150749,#150750,#150751,
#150752,#150753),(#150754,#150755,#150756,#150757,#150758,#150759,#150760),
(#150761,#150762,#150763,#150764,#150765,#150766,#150767),(#150768,#150769,
#150770,#150771,#150772,#150773,#150774),(#150775,#150776,#150777,#150778,
#150779,#150780,#150781),(#150782,#150783,#150784,#150785,#150786,#150787,
#150788),(#150789,#150790,#150791,#150792,#150793,#150794,#150795),(#150796,
#150797,#150798,#150799,#150800,#150801,#150802)),.UNSPECIFIED.,.F.,.F.,
 .F.,(4,1,1,1,1,1,1,1,1,1,4),(4,1,1,1,4),(0.,0.132545826214933,0.255032336532908,
0.377518846850882,0.43876210200987,0.500005357168857,0.561248612327844,
0.622491867486832,0.744978377804806,0.867464888122781,1.),(0.,0.262905612958216,
0.500178847936523,0.737452082914831,1.),.UNSPECIFIED.);
#159=B_SPLINE_SURFACE_WITH_KNOTS('',3,3,((#150892,#150893,#150894,#150895,
#150896,#150897,#150898),(#150899,#150900,#150901,#150902,#150903,#150904,
#150905),(#150906,#150907,#150908,#150909,#150910,#150911,#150912),(#150913,
#150914,#150915,#150916,#150917,#150918,#150919),(#150920,#150921,#150922,
#150923,#150924,#150925,#150926),(#150927,#150928,#150929,#150930,#150931,
#150932,#150933),(#150934,#150935,#150936,#150937,#150938,#150939,#150940),
(#150941,#150942,#150943,#150944,#150945,#150946,#150947),(#150948,#150949,
#150950,#150951,#150952,#150953,#150954)),.UNSPECIFIED.,.F.,.F.,.F.,(4,
1,1,1,1,1,4),(4,1,1,1,4),(0.,0.132239664806391,0.254822586974288,0.499988431310081,
0.622571353477978,0.745154275645875,1.),(0.,0.263399375189117,0.5001298925661,
0.736860409943082,1.),.UNSPECIFIED.);
#160=B_SPLINE_SURFACE_WITH_KNOTS('',3,3,((#151226,#151227,#151228,#151229,
#151230,#151231,#151232),(#151233,#151234,#151235,#151236,#151237,#151238,
#151239),(#151240,#151241,#151242,#151243,#151244,#151245,#151246),(#151247,
#151248,#151249,#151250,#151251,#151252,#151253),(#151254,#151255,#151256,
#151257,#151258,#151259,#151260),(#151261,#151262,#151263,#151264,#151265,
#151266,#151267),(#151268,#151269,#151270,#151271,#151272,#151273,#151274),
(#151275,#151276,#151277,#151278,#151279,#151280,#151281),(#151282,#151283,
#151284,#151285,#151286,#151287,#151288),(#151289,#151290,#151291,#151292,
#151293,#151294,#151295),(#151296,#151297,#151298,#151299,#151300,#151301,
#151302),(#151303,#151304,#151305,#151306,#151307,#151308,#151309),(#151310,
#151311,#151312,#151313,#151314,#151315,#151316),(#151317,#151318,#151319,
#151320,#151321,#151322,#151323),(#151324,#151325,#151326,#151327,#151328,
#151329,#151330)),.UNSPECIFIED.,.F.,.F.,.F.,(4,1,1,1,1,1,1,1,1,1,1,1,4),
(4,1,1,1,4),(0.,0.132202892489662,0.193512430520099,0.254821968550535,0.316131506580972,
0.377441044611408,0.438750582641845,0.500060120672282,0.561369658702718,
0.622679196733155,0.745298272794028,0.867917348854901,1.),(0.,0.262289949012583,
0.500131074192996,0.737972199373408,1.),.UNSPECIFIED.);
#161=B_SPLINE_SURFACE_WITH_KNOTS('',3,3,((#151468,#151469,#151470,#151471,
#151472,#151473,#151474,#151475,#151476,#151477,#151478),(#151479,#151480,
#151481,#151482,#151483,#151484,#151485,#151486,#151487,#151488,#151489),
(#151490,#151491,#151492,#151493,#151494,#151495,#151496,#151497,#151498,
#151499,#151500),(#151501,#151502,#151503,#151504,#151505,#151506,#151507,
#151508,#151509,#151510,#151511),(#151512,#151513,#151514,#151515,#151516,
#151517,#151518,#151519,#151520,#151521,#151522),(#151523,#151524,#151525,
#151526,#151527,#151528,#151529,#151530,#151531,#151532,#151533),(#151534,
#151535,#151536,#151537,#151538,#151539,#151540,#151541,#151542,#151543,
#151544),(#151545,#151546,#151547,#151548,#151549,#151550,#151551,#151552,
#151553,#151554,#151555),(#151556,#151557,#151558,#151559,#151560,#151561,
#151562,#151563,#151564,#151565,#151566)),.UNSPECIFIED.,.F.,.F.,.F.,(4,
1,1,1,1,1,4),(4,1,1,1,1,1,1,1,4),(0.,0.254208751460181,0.499694013842769,
0.622436645034063,0.745179276225357,0.86792190741665,1.),(0.,0.138828491142032,
0.259244177039013,0.379659862935897,0.500075548832782,0.620491234729763,
0.740906920626647,0.861322606523628,1.),.UNSPECIFIED.);
#162=B_SPLINE_SURFACE_WITH_KNOTS('',3,3,((#151636,#151637,#151638,#151639,
#151640,#151641,#151642),(#151643,#151644,#151645,#151646,#151647,#151648,
#151649),(#151650,#151651,#151652,#151653,#151654,#151655,#151656),(#151657,
#151658,#151659,#151660,#151661,#151662,#151663),(#151664,#151665,#151666,
#151667,#151668,#151669,#151670),(#151671,#151672,#151673,#151674,#151675,
#151676,#151677),(#151678,#151679,#151680,#151681,#151682,#151683,#151684)),
 .UNSPECIFIED.,.F.,.F.,.F.,(4,1,1,1,4),(4,1,1,1,4),(0.,0.257623699974245,
0.499835655335243,0.742047610696241,1.),(0.,0.259937323174334,0.500055099785869,
0.740172876397403,1.),.UNSPECIFIED.);
#163=B_SPLINE_SURFACE_WITH_KNOTS('',3,3,((#151804,#151805,#151806,#151807,
#151808,#151809,#151810,#151811,#151812,#151813,#151814),(#151815,#151816,
#151817,#151818,#151819,#151820,#151821,#151822,#151823,#151824,#151825),
(#151826,#151827,#151828,#151829,#151830,#151831,#151832,#151833,#151834,
#151835,#151836),(#151837,#151838,#151839,#151840,#151841,#151842,#151843,
#151844,#151845,#151846,#151847),(#151848,#151849,#151850,#151851,#151852,
#151853,#151854,#151855,#151856,#151857,#151858),(#151859,#151860,#151861,
#151862,#151863,#151864,#151865,#151866,#151867,#151868,#151869),(#151870,
#151871,#151872,#151873,#151874,#151875,#151876,#151877,#151878,#151879,
#151880)),.UNSPECIFIED.,.F.,.F.,.F.,(4,1,1,1,4),(4,1,1,1,1,1,1,1,4),(0.,
0.258806803182955,0.500771503994781,0.742736204806219,1.),(0.,0.146126082968561,
0.264104099863688,0.382082116758815,0.500060133653942,0.618038150549069,
0.736016167444196,0.853994184339323,1.),.UNSPECIFIED.);
#164=B_SPLINE_SURFACE_WITH_KNOTS('',3,3,((#151953,#151954,#151955,#151956,
#151957,#151958,#151959),(#151960,#151961,#151962,#151963,#151964,#151965,
#151966),(#151967,#151968,#151969,#151970,#151971,#151972,#151973),(#151974,
#151975,#151976,#151977,#151978,#151979,#151980),(#151981,#151982,#151983,
#151984,#151985,#151986,#151987),(#151988,#151989,#151990,#151991,#151992,
#151993,#151994),(#151995,#151996,#151997,#151998,#151999,#152000,#152001),
(#152002,#152003,#152004,#152005,#152006,#152007,#152008),(#152009,#152010,
#152011,#152012,#152013,#152014,#152015),(#152016,#152017,#152018,#152019,
#152020,#152021,#152022),(#152023,#152024,#152025,#152026,#152027,#152028,
#152029),(#152030,#152031,#152032,#152033,#152034,#152035,#152036),(#152037,
#152038,#152039,#152040,#152041,#152042,#152043),(#152044,#152045,#152046,
#152047,#152048,#152049,#152050),(#152051,#152052,#152053,#152054,#152055,
#152056,#152057),(#152058,#152059,#152060,#152061,#152062,#152063,#152064),
(#152065,#152066,#152067,#152068,#152069,#152070,#152071),(#152072,#152073,
#152074,#152075,#152076,#152077,#152078),(#152079,#152080,#152081,#152082,
#152083,#152084,#152085),(#152086,#152087,#152088,#152089,#152090,#152091,
#152092),(#152093,#152094,#152095,#152096,#152097,#152098,#152099),(#152100,
#152101,#152102,#152103,#152104,#152105,#152106),(#152107,#152108,#152109,
#152110,#152111,#152112,#152113),(#152114,#152115,#152116,#152117,#152118,
#152119,#152120),(#152121,#152122,#152123,#152124,#152125,#152126,#152127),
(#152128,#152129,#152130,#152131,#152132,#152133,#152134),(#152135,#152136,
#152137,#152138,#152139,#152140,#152141),(#152142,#152143,#152144,#152145,
#152146,#152147,#152148),(#152149,#152150,#152151,#152152,#152153,#152154,
#152155),(#152156,#152157,#152158,#152159,#152160,#152161,#152162),(#152163,
#152164,#152165,#152166,#152167,#152168,#152169),(#152170,#152171,#152172,
#152173,#152174,#152175,#152176),(#152177,#152178,#152179,#152180,#152181,
#152182,#152183)),.UNSPECIFIED.,.F.,.F.,.F.,(4,1,1,1,1,1,1,1,1,1,1,1,1,
1,1,1,1,1,1,1,1,1,1,1,1,1,1,1,1,1,4),(4,1,1,1,4),(0.,0.0658304936520168,
0.0968410489872127,0.127851604322409,0.158862159657605,0.1898727149928,
0.220883270327996,0.251893825663192,0.313914936333584,0.34492549166878,
0.375936047003976,0.391441324671574,0.406946602339172,0.437957157674368,
0.468967713009564,0.49997826834476,0.530988823679956,0.561999379015152,
0.593009934350347,0.608515212017945,0.624020489685543,0.655031045020739,
0.686041600355935,0.748062711026327,0.779073266361523,0.810083821696719,
0.841094377031915,0.872104932367111,0.903115487702307,0.934126043037503,
1.),(0.,0.336621216511749,0.510184141880342,0.683747067249001,1.),
 .UNSPECIFIED.);
#165=B_SPLINE_SURFACE_WITH_KNOTS('',3,3,((#152443,#152444,#152445,#152446,
#152447,#152448,#152449,#152450,#152451,#152452,#152453),(#152454,#152455,
#152456,#152457,#152458,#152459,#152460,#152461,#152462,#152463,#152464),
(#152465,#152466,#152467,#152468,#152469,#152470,#152471,#152472,#152473,
#152474,#152475),(#152476,#152477,#152478,#152479,#152480,#152481,#152482,
#152483,#152484,#152485,#152486),(#152487,#152488,#152489,#152490,#152491,
#152492,#152493,#152494,#152495,#152496,#152497),(#152498,#152499,#152500,
#152501,#152502,#152503,#152504,#152505,#152506,#152507,#152508),(#152509,
#152510,#152511,#152512,#152513,#152514,#152515,#152516,#152517,#152518,
#152519),(#152520,#152521,#152522,#152523,#152524,#152525,#152526,#152527,
#152528,#152529,#152530),(#152531,#152532,#152533,#152534,#152535,#152536,
#152537,#152538,#152539,#152540,#152541),(#152542,#152543,#152544,#152545,
#152546,#152547,#152548,#152549,#152550,#152551,#152552),(#152553,#152554,
#152555,#152556,#152557,#152558,#152559,#152560,#152561,#152562,#152563),
(#152564,#152565,#152566,#152567,#152568,#152569,#152570,#152571,#152572,
#152573,#152574),(#152575,#152576,#152577,#152578,#152579,#152580,#152581,
#152582,#152583,#152584,#152585),(#152586,#152587,#152588,#152589,#152590,
#152591,#152592,#152593,#152594,#152595,#152596),(#152597,#152598,#152599,
#152600,#152601,#152602,#152603,#152604,#152605,#152606,#152607),(#152608,
#152609,#152610,#152611,#152612,#152613,#152614,#152615,#152616,#152617,
#152618),(#152619,#152620,#152621,#152622,#152623,#152624,#152625,#152626,
#152627,#152628,#152629),(#152630,#152631,#152632,#152633,#152634,#152635,
#152636,#152637,#152638,#152639,#152640),(#152641,#152642,#152643,#152644,
#152645,#152646,#152647,#152648,#152649,#152650,#152651),(#152652,#152653,
#152654,#152655,#152656,#152657,#152658,#152659,#152660,#152661,#152662)),
 .UNSPECIFIED.,.F.,.F.,.F.,(4,1,1,1,1,1,1,1,1,1,1,1,1,1,1,1,1,4),(4,1,1,
1,1,1,1,1,4),(0.,0.0708680261420804,0.132162830392948,0.254752438894683,
0.316047243145551,0.377342047396419,0.438636851647286,0.46928425377272,
0.499931655898154,0.530579058023588,0.561226460149022,0.622521264399889,
0.683816068650757,0.745110872901625,0.806405677152492,0.86770048140336,
0.928995285654228,1.),(0.,0.136846366314673,0.257938577852228,0.379030789389783,
0.500123000927338,0.621215212464893,0.742307424002448,0.863399635540003,
1.),.UNSPECIFIED.);
#166=B_SPLINE_SURFACE_WITH_KNOTS('',3,3,((#152674,#152675,#152676,#152677,
#152678,#152679,#152680,#152681,#152682,#152683,#152684),(#152685,#152686,
#152687,#152688,#152689,#152690,#152691,#152692,#152693,#152694,#152695),
(#152696,#152697,#152698,#152699,#152700,#152701,#152702,#152703,#152704,
#152705,#152706),(#152707,#152708,#152709,#152710,#152711,#152712,#152713,
#152714,#152715,#152716,#152717),(#152718,#152719,#152720,#152721,#152722,
#152723,#152724,#152725,#152726,#152727,#152728),(#152729,#152730,#152731,
#152732,#152733,#152734,#152735,#152736,#152737,#152738,#152739),(#152740,
#152741,#152742,#152743,#152744,#152745,#152746,#152747,#152748,#152749,
#152750),(#152751,#152752,#152753,#152754,#152755,#152756,#152757,#152758,
#152759,#152760,#152761),(#152762,#152763,#152764,#152765,#152766,#152767,
#152768,#152769,#152770,#152771,#152772),(#152773,#152774,#152775,#152776,
#152777,#152778,#152779,#152780,#152781,#152782,#152783)),.UNSPECIFIED.,
 .F.,.F.,.F.,(4,1,1,1,1,1,1,4),(4,1,1,1,1,1,1,1,4),(0.,0.132043267539266,
0.254787356474467,0.377531445409669,0.500275534344871,0.623019623280073,
0.745763712215274,1.),(0.,0.138828554116791,0.259244178532127,0.379659802947559,
0.500075427362895,0.620491051778231,0.740906676193567,0.861322300609,1.),
 .UNSPECIFIED.);
#167=B_SPLINE_SURFACE_WITH_KNOTS('',3,3,((#153064,#153065,#153066,#153067,
#153068,#153069,#153070,#153071,#153072),(#153073,#153074,#153075,#153076,
#153077,#153078,#153079,#153080,#153081),(#153082,#153083,#153084,#153085,
#153086,#153087,#153088,#153089,#153090),(#153091,#153092,#153093,#153094,
#153095,#153096,#153097,#153098,#153099),(#153100,#153101,#153102,#153103,
#153104,#153105,#153106,#153107,#153108),(#153109,#153110,#153111,#153112,
#153113,#153114,#153115,#153116,#153117),(#153118,#153119,#153120,#153121,
#153122,#153123,#153124,#153125,#153126)),.UNSPECIFIED.,.F.,.F.,.F.,(4,
1,1,1,4),(4,1,1,1,1,1,4),(0.,0.257122326414864,0.49891834990865,0.740714373402823,
1.),(0.,0.264098460225707,0.382080501845444,0.500062543465087,0.618044585084824,
0.736026626704467,1.),.UNSPECIFIED.);
#168=B_SPLINE_SURFACE_WITH_KNOTS('',3,3,((#153186,#153187,#153188,#153189,
#153190,#153191,#153192),(#153193,#153194,#153195,#153196,#153197,#153198,
#153199),(#153200,#153201,#153202,#153203,#153204,#153205,#153206),(#153207,
#153208,#153209,#153210,#153211,#153212,#153213),(#153214,#153215,#153216,
#153217,#153218,#153219,#153220),(#153221,#153222,#153223,#153224,#153225,
#153226,#153227),(#153228,#153229,#153230,#153231,#153232,#153233,#153234)),
 .UNSPECIFIED.,.F.,.F.,.F.,(4,1,1,1,4),(4,1,1,1,4),(0.,0.257735074161703,
0.499844908300334,0.741954742438964,1.),(0.,0.259940639367695,0.500057872218097,
0.740175105068594,1.),.UNSPECIFIED.);
#169=B_SPLINE_SURFACE_WITH_KNOTS('',3,3,((#153359,#153360,#153361,#153362,
#153363,#153364,#153365),(#153366,#153367,#153368,#153369,#153370,#153371,
#153372),(#153373,#153374,#153375,#153376,#153377,#153378,#153379),(#153380,
#153381,#153382,#153383,#153384,#153385,#153386),(#153387,#153388,#153389,
#153390,#153391,#153392,#153393),(#153394,#153395,#153396,#153397,#153398,
#153399,#153400),(#153401,#153402,#153403,#153404,#153405,#153406,#153407),
(#153408,#153409,#153410,#153411,#153412,#153413,#153414),(#153415,#153416,
#153417,#153418,#153419,#153420,#153421),(#153422,#153423,#153424,#153425,
#153426,#153427,#153428),(#153429,#153430,#153431,#153432,#153433,#153434,
#153435),(#153436,#153437,#153438,#153439,#153440,#153441,#153442)),
 .UNSPECIFIED.,.F.,.F.,.F.,(4,1,1,1,1,1,1,1,1,4),(4,1,1,1,4),(0.,0.131942207186592,
0.254618794764067,0.377295382341543,0.499971969919018,0.561310263707756,
0.622648557496493,0.745325145073969,0.868001732651444,1.),(0.,0.257681345106317,
0.499753140798927,0.741824936491634,1.),.UNSPECIFIED.);
#170=B_SPLINE_SURFACE_WITH_KNOTS('',3,3,((#153886,#153887,#153888,#153889,
#153890,#153891,#153892),(#153893,#153894,#153895,#153896,#153897,#153898,
#153899),(#153900,#153901,#153902,#153903,#153904,#153905,#153906),(#153907,
#153908,#153909,#153910,#153911,#153912,#153913),(#153914,#153915,#153916,
#153917,#153918,#153919,#153920),(#153921,#153922,#153923,#153924,#153925,
#153926,#153927),(#153928,#153929,#153930,#153931,#153932,#153933,#153934),
(#153935,#153936,#153937,#153938,#153939,#153940,#153941),(#153942,#153943,
#153944,#153945,#153946,#153947,#153948),(#153949,#153950,#153951,#153952,
#153953,#153954,#153955),(#153956,#153957,#153958,#153959,#153960,#153961,
#153962),(#153963,#153964,#153965,#153966,#153967,#153968,#153969),(#153970,
#153971,#153972,#153973,#153974,#153975,#153976),(#153977,#153978,#153979,
#153980,#153981,#153982,#153983)),.UNSPECIFIED.,.F.,.F.,.F.,(4,1,1,1,1,
1,1,1,1,1,1,4),(4,1,1,1,4),(0.,0.132195054850011,0.254794129835051,0.316093667327571,
0.377393204820091,0.438692742312611,0.499992279805131,0.561291817297652,
0.622591354790172,0.745190429775212,0.867789504760252,1.),(0.,0.261340468241408,
0.500099147644516,0.738857827047623,1.),.UNSPECIFIED.);
#171=B_SPLINE_SURFACE_WITH_KNOTS('',3,3,((#154202,#154203,#154204,#154205,
#154206),(#154207,#154208,#154209,#154210,#154211),(#154212,#154213,#154214,
#154215,#154216),(#154217,#154218,#154219,#154220,#154221)),
 .UNSPECIFIED.,.F.,.F.,.F.,(4,4),(4,1,4),(0.,1.),(0.,0.50287827766393,1.),
 .UNSPECIFIED.);
#172=B_SPLINE_SURFACE_WITH_KNOTS('',3,3,((#154416,#154417,#154418,#154419,
#154420,#154421,#154422),(#154423,#154424,#154425,#154426,#154427,#154428,
#154429),(#154430,#154431,#154432,#154433,#154434,#154435,#154436),(#154437,
#154438,#154439,#154440,#154441,#154442,#154443),(#154444,#154445,#154446,
#154447,#154448,#154449,#154450),(#154451,#154452,#154453,#154454,#154455,
#154456,#154457),(#154458,#154459,#154460,#154461,#154462,#154463,#154464),
(#154465,#154466,#154467,#154468,#154469,#154470,#154471),(#154472,#154473,
#154474,#154475,#154476,#154477,#154478),(#154479,#154480,#154481,#154482,
#154483,#154484,#154485),(#154486,#154487,#154488,#154489,#154490,#154491,
#154492),(#154493,#154494,#154495,#154496,#154497,#154498,#154499),(#154500,
#154501,#154502,#154503,#154504,#154505,#154506),(#154507,#154508,#154509,
#154510,#154511,#154512,#154513)),.UNSPECIFIED.,.F.,.F.,.F.,(4,1,1,1,1,
1,1,1,1,1,1,4),(4,1,1,1,4),(0.,0.132195054849916,0.25479412983497,0.316093667327497,
0.377393204820023,0.43869274231255,0.499992279805077,0.561291817297604,
0.622591354790131,0.745190429775184,0.867789504760238,1.),(0.,0.261340468241415,
0.50009914764452,0.738857827047626,1.),.UNSPECIFIED.);
#173=B_SPLINE_SURFACE_WITH_KNOTS('',3,3,((#154716,#154717,#154718,#154719,
#154720,#154721,#154722),(#154723,#154724,#154725,#154726,#154727,#154728,
#154729),(#154730,#154731,#154732,#154733,#154734,#154735,#154736),(#154737,
#154738,#154739,#154740,#154741,#154742,#154743),(#154744,#154745,#154746,
#154747,#154748,#154749,#154750),(#154751,#154752,#154753,#154754,#154755,
#154756,#154757),(#154758,#154759,#154760,#154761,#154762,#154763,#154764),
(#154765,#154766,#154767,#154768,#154769,#154770,#154771),(#154772,#154773,
#154774,#154775,#154776,#154777,#154778),(#154779,#154780,#154781,#154782,
#154783,#154784,#154785),(#154786,#154787,#154788,#154789,#154790,#154791,
#154792),(#154793,#154794,#154795,#154796,#154797,#154798,#154799),(#154800,
#154801,#154802,#154803,#154804,#154805,#154806)),.UNSPECIFIED.,.F.,.F.,
 .F.,(4,1,1,1,1,1,1,1,1,1,4),(4,1,1,1,4),(0.,0.132030874480919,0.19336634824744,
0.254701822013961,0.316037295780482,0.377372769547002,0.500043717080044,
0.622714664613086,0.745385612146127,0.868056559679169,1.),(0.,0.260567545092337,
0.500088901308193,0.73961025752405,1.),.UNSPECIFIED.);
#174=B_SPLINE_SURFACE_WITH_KNOTS('',3,3,((#155084,#155085,#155086,#155087),
(#155088,#155089,#155090,#155091),(#155092,#155093,#155094,#155095),(#155096,
#155097,#155098,#155099),(#155100,#155101,#155102,#155103),(#155104,#155105,
#155106,#155107),(#155108,#155109,#155110,#155111),(#155112,#155113,#155114,
#155115),(#155116,#155117,#155118,#155119),(#155120,#155121,#155122,#155123),
(#155124,#155125,#155126,#155127),(#155128,#155129,#155130,#155131),(#155132,
#155133,#155134,#155135),(#155136,#155137,#155138,#155139),(#155140,#155141,
#155142,#155143),(#155144,#155145,#155146,#155147)),.UNSPECIFIED.,.F.,.F.,
 .F.,(4,1,1,1,1,1,1,1,1,1,1,1,1,4),(4,4),(0.,0.131636988977778,0.193017807710131,
0.254398626442485,0.315779445174839,0.377160263907192,0.499921901371899,
0.561302720104253,0.622683538836606,0.68406435756896,0.745445176301313,
0.806825995033667,0.86820681376602,1.),(0.,1.),.UNSPECIFIED.);
#175=B_SPLINE_SURFACE_WITH_KNOTS('',3,3,((#155542,#155543,#155544,#155545,
#155546),(#155547,#155548,#155549,#155550,#155551),(#155552,#155553,#155554,
#155555,#155556),(#155557,#155558,#155559,#155560,#155561),(#155562,#155563,
#155564,#155565,#155566),(#155567,#155568,#155569,#155570,#155571),(#155572,
#155573,#155574,#155575,#155576),(#155577,#155578,#155579,#155580,#155581),
(#155582,#155583,#155584,#155585,#155586),(#155587,#155588,#155589,#155590,
#155591),(#155592,#155593,#155594,#155595,#155596),(#155597,#155598,#155599,
#155600,#155601),(#155602,#155603,#155604,#155605,#155606),(#155607,#155608,
#155609,#155610,#155611),(#155612,#155613,#155614,#155615,#155616)),
 .UNSPECIFIED.,.F.,.F.,.F.,(4,1,1,1,1,1,1,1,1,1,1,1,4),(4,1,4),(0.,0.132758396228893,
0.255171695213975,0.316378344706517,0.377584994199058,0.438791643691599,
0.49999829318414,0.561204942676681,0.622411592169222,0.683618241661764,
0.744824891154305,0.867238190139387,1.),(0.,0.579500129312416,1.),
 .UNSPECIFIED.);
#176=B_SPLINE_SURFACE_WITH_KNOTS('',3,3,((#159336,#159337,#159338,#159339),
(#159340,#159341,#159342,#159343),(#159344,#159345,#159346,#159347),(#159348,
#159349,#159350,#159351),(#159352,#159353,#159354,#159355),(#159356,#159357,
#159358,#159359),(#159360,#159361,#159362,#159363),(#159364,#159365,#159366,
#159367),(#159368,#159369,#159370,#159371),(#159372,#159373,#159374,#159375),
(#159376,#159377,#159378,#159379),(#159380,#159381,#159382,#159383),(#159384,
#159385,#159386,#159387),(#159388,#159389,#159390,#159391),(#159392,#159393,
#159394,#159395),(#159396,#159397,#159398,#159399)),.UNSPECIFIED.,.F.,.F.,
 .F.,(4,1,1,1,1,1,1,1,1,1,1,1,1,4),(4,4),(0.,0.0631871049823428,0.143694780613763,
0.224202456245058,0.304710131876457,0.385217807507856,0.465725483139255,
0.54623315877055,0.626740834401949,0.707248510033348,0.787756185664748,
0.868263861296042,0.948771536927442,1.),(0.,1.),.UNSPECIFIED.);
#177=B_SPLINE_SURFACE_WITH_KNOTS('',3,3,((#159424,#159425,#159426,#159427),
(#159428,#159429,#159430,#159431),(#159432,#159433,#159434,#159435),(#159436,
#159437,#159438,#159439),(#159440,#159441,#159442,#159443),(#159444,#159445,
#159446,#159447),(#159448,#159449,#159450,#159451),(#159452,#159453,#159454,
#159455),(#159456,#159457,#159458,#159459),(#159460,#159461,#159462,#159463),
(#159464,#159465,#159466,#159467),(#159468,#159469,#159470,#159471),(#159472,
#159473,#159474,#159475),(#159476,#159477,#159478,#159479),(#159480,#159481,
#159482,#159483),(#159484,#159485,#159486,#159487)),.UNSPECIFIED.,.F.,.F.,
 .F.,(4,1,1,1,1,1,1,1,1,1,1,1,1,4),(4,4),(0.,0.063187150036898,0.143694817475814,
0.224202484914604,0.304710152353498,0.385217819792393,0.465725487231287,
0.546233154670077,0.626740822108972,0.707248489547867,0.787756156986761,
0.868263824425551,0.948771491864446,1.),(0.,1.),.UNSPECIFIED.);
#178=B_SPLINE_SURFACE_WITH_KNOTS('',3,1,((#159815,#159816),(#159817,#159818),
(#159819,#159820),(#159821,#159822)),.UNSPECIFIED.,.F.,.F.,.F.,(4,4),(2,
2),(0.00340538980800498,1.),(0.,1.18214433782264),.UNSPECIFIED.);
#179=B_SPLINE_SURFACE_WITH_KNOTS('',1,3,((#174040,#174041,#174042,#174043,
#174044,#174045,#174046,#174047,#174048,#174049,#174050,#174051,#174052,
#174053,#174054,#174055,#174056,#174057,#174058,#174059,#174060,#174061,
#174062,#174063,#174064,#174065,#174066,#174067,#174068,#174069,#174070,
#174071,#174072,#174073,#174074,#174075,#174076,#174077,#174078,#174079,
#174080,#174081,#174082,#174083,#174084,#174085,#174086,#174087,#174088,
#174089,#174090,#174091,#174092,#174093,#174094,#174095,#174096,#174097,
#174098,#174099,#174100,#174101,#174102,#174103,#174104,#174105,#174106),
(#174107,#174108,#174109,#174110,#174111,#174112,#174113,#174114,#174115,
#174116,#174117,#174118,#174119,#174120,#174121,#174122,#174123,#174124,
#174125,#174126,#174127,#174128,#174129,#174130,#174131,#174132,#174133,
#174134,#174135,#174136,#174137,#174138,#174139,#174140,#174141,#174142,
#174143,#174144,#174145,#174146,#174147,#174148,#174149,#174150,#174151,
#174152,#174153,#174154,#174155,#174156,#174157,#174158,#174159,#174160,
#174161,#174162,#174163,#174164,#174165,#174166,#174167,#174168,#174169,
#174170,#174171,#174172,#174173)),.UNSPECIFIED.,.F.,.F.,.F.,(2,2),(4,1,
1,1,1,1,1,1,1,1,1,1,1,1,1,1,1,1,1,1,1,1,1,1,1,1,1,1,1,1,1,1,1,1,1,1,1,1,
1,1,1,1,1,1,1,1,1,1,1,1,1,1,1,1,1,1,1,1,1,1,1,1,1,1,4),(0.,1.),(0.,0.0157026587679609,
0.0314053175359218,0.0471079763038827,0.0628106350718436,0.0785132938398045,
0.0942159526077654,0.109918611375726,0.125621270143687,0.141323928911648,
0.157026587679609,0.17272924644757,0.188431905215531,0.204134563983492,
0.219837222751453,0.235539881519413,0.251242540287374,0.266945199055335,
0.282647857823296,0.298350516591257,0.314053175359218,0.329755834127179,
0.34545849289514,0.361161151663101,0.376863810431061,0.392566469199022,
0.408269127966983,0.423971786734944,0.439674445502905,0.455377104270866,
0.471079763038827,0.486782421806788,0.502485080574749,0.518187739342709,
0.53389039811067,0.549593056878631,0.565295715646592,0.580998374414553,
0.596701033182514,0.612403691950475,0.628106350718436,0.643809009486397,
0.659511668254358,0.675214327022318,0.690916985790279,0.70661964455824,
0.722322303326201,0.738024962094162,0.753727620862123,0.769430279630084,
0.785132938398045,0.800835597166006,0.816538255933966,0.832240914701927,
0.847943573469888,0.863646232237849,0.87934889100581,0.895051549773771,
0.910754208541732,0.926456867309693,0.942159526077654,0.957862184845615,
0.973564843613575,0.989267502381536,1.),.UNSPECIFIED.);
#180=B_SPLINE_SURFACE_WITH_KNOTS('',1,3,((#174174,#174175,#174176,#174177,
#174178,#174179,#174180,#174181,#174182,#174183,#174184,#174185,#174186,
#174187,#174188,#174189,#174190,#174191,#174192,#174193,#174194,#174195,
#174196,#174197,#174198,#174199,#174200,#174201,#174202,#174203,#174204,
#174205,#174206,#174207,#174208,#174209,#174210,#174211,#174212,#174213,
#174214,#174215,#174216,#174217,#174218,#174219,#174220,#174221,#174222,
#174223,#174224,#174225,#174226,#174227,#174228,#174229,#174230,#174231,
#174232,#174233,#174234,#174235,#174236,#174237,#174238,#174239,#174240),
(#174241,#174242,#174243,#174244,#174245,#174246,#174247,#174248,#174249,
#174250,#174251,#174252,#174253,#174254,#174255,#174256,#174257,#174258,
#174259,#174260,#174261,#174262,#174263,#174264,#174265,#174266,#174267,
#174268,#174269,#174270,#174271,#174272,#174273,#174274,#174275,#174276,
#174277,#174278,#174279,#174280,#174281,#174282,#174283,#174284,#174285,
#174286,#174287,#174288,#174289,#174290,#174291,#174292,#174293,#174294,
#174295,#174296,#174297,#174298,#174299,#174300,#174301,#174302,#174303,
#174304,#174305,#174306,#174307)),.UNSPECIFIED.,.F.,.F.,.F.,(2,2),(4,1,
1,1,1,1,1,1,1,1,1,1,1,1,1,1,1,1,1,1,1,1,1,1,1,1,1,1,1,1,1,1,1,1,1,1,1,1,
1,1,1,1,1,1,1,1,1,1,1,1,1,1,1,1,1,1,1,1,1,1,1,1,1,1,4),(0.,1.),(0.,0.0157026587679609,
0.0314053175359218,0.0471079763038827,0.0628106350718436,0.0785132938398045,
0.0942159526077654,0.109918611375726,0.125621270143687,0.141323928911648,
0.157026587679609,0.17272924644757,0.188431905215531,0.204134563983492,
0.219837222751453,0.235539881519413,0.251242540287374,0.266945199055335,
0.282647857823296,0.298350516591257,0.314053175359218,0.329755834127179,
0.34545849289514,0.361161151663101,0.376863810431061,0.392566469199022,
0.408269127966983,0.423971786734944,0.439674445502905,0.455377104270866,
0.471079763038827,0.486782421806788,0.502485080574749,0.518187739342709,
0.53389039811067,0.549593056878631,0.565295715646592,0.580998374414553,
0.596701033182514,0.612403691950475,0.628106350718436,0.643809009486397,
0.659511668254358,0.675214327022318,0.690916985790279,0.70661964455824,
0.722322303326201,0.738024962094162,0.753727620862123,0.769430279630084,
0.785132938398045,0.800835597166006,0.816538255933966,0.832240914701927,
0.847943573469888,0.863646232237849,0.87934889100581,0.895051549773771,
0.910754208541732,0.926456867309693,0.942159526077654,0.957862184845615,
0.973564843613575,0.989267502381536,1.),.UNSPECIFIED.);
#181=B_SPLINE_SURFACE_WITH_KNOTS('',1,3,((#174308,#174309,#174310,#174311,
#174312,#174313,#174314,#174315,#174316,#174317,#174318,#174319,#174320,
#174321,#174322,#174323,#174324,#174325,#174326,#174327,#174328,#174329,
#174330,#174331,#174332,#174333,#174334,#174335,#174336,#174337,#174338,
#174339,#174340,#174341,#174342,#174343,#174344,#174345,#174346,#174347,
#174348,#174349,#174350,#174351,#174352,#174353,#174354,#174355,#174356,
#174357,#174358,#174359,#174360,#174361,#174362,#174363,#174364,#174365,
#174366,#174367,#174368,#174369,#174370,#174371,#174372,#174373,#174374,
#174375,#174376,#174377,#174378,#174379,#174380,#174381,#174382,#174383,
#174384),(#174385,#174386,#174387,#174388,#174389,#174390,#174391,#174392,
#174393,#174394,#174395,#174396,#174397,#174398,#174399,#174400,#174401,
#174402,#174403,#174404,#174405,#174406,#174407,#174408,#174409,#174410,
#174411,#174412,#174413,#174414,#174415,#174416,#174417,#174418,#174419,
#174420,#174421,#174422,#174423,#174424,#174425,#174426,#174427,#174428,
#174429,#174430,#174431,#174432,#174433,#174434,#174435,#174436,#174437,
#174438,#174439,#174440,#174441,#174442,#174443,#174444,#174445,#174446,
#174447,#174448,#174449,#174450,#174451,#174452,#174453,#174454,#174455,
#174456,#174457,#174458,#174459,#174460,#174461)),.UNSPECIFIED.,.F.,.F.,
 .F.,(2,2),(4,1,1,1,1,1,1,1,1,1,1,1,1,1,1,1,1,1,1,1,1,1,1,1,1,1,1,1,1,1,
1,1,1,1,1,1,1,1,1,1,1,1,1,1,1,1,1,1,1,1,1,1,1,1,1,1,1,1,1,1,1,1,1,1,1,1,
1,1,1,1,1,1,1,1,4),(0.,1.),(0.,0.0135337770704249,0.0270675541408498,0.0406013312112747,
0.0541351082816996,0.0676688853521246,0.0812026624225494,0.0947364394929744,
0.108270216563399,0.121803993633824,0.135337770704249,0.148871547774674,
0.162405324845099,0.175939101915524,0.189472878985949,0.203006656056374,
0.216540433126799,0.230074210197223,0.243607987267648,0.257141764338073,
0.270675541408498,0.284209318478923,0.297743095549348,0.311276872619773,
0.324810649690198,0.338344426760623,0.351878203831048,0.365411980901473,
0.378945757971897,0.392479535042322,0.406013312112747,0.419547089183172,
0.433080866253597,0.446614643324022,0.460148420394447,0.473682197464872,
0.487215974535297,0.500749751605722,0.514283528676147,0.527817305746571,
0.541351082816996,0.554884859887421,0.568418636957846,0.581952414028271,
0.595486191098696,0.609019968169121,0.622553745239546,0.636087522309971,
0.649621299380396,0.663155076450821,0.676688853521245,0.69022263059167,
0.703756407662095,0.71729018473252,0.730823961802945,0.74435773887337,0.757891515943795,
0.77142529301422,0.784959070084645,0.79849284715507,0.812026624225495,0.825560401295919,
0.839094178366344,0.852627955436769,0.866161732507194,0.879695509577619,
0.893229286648044,0.906763063718469,0.920296840788894,0.933830617859319,
0.947364394929744,0.960898172000169,0.974431949070593,0.987965726141018,
1.),.UNSPECIFIED.);
#182=B_SPLINE_SURFACE_WITH_KNOTS('',1,3,((#174462,#174463,#174464,#174465,
#174466,#174467,#174468,#174469,#174470,#174471,#174472,#174473,#174474,
#174475,#174476,#174477,#174478,#174479,#174480,#174481,#174482,#174483,
#174484,#174485,#174486,#174487,#174488,#174489,#174490,#174491,#174492,
#174493,#174494,#174495,#174496,#174497,#174498,#174499,#174500,#174501,
#174502,#174503,#174504,#174505,#174506,#174507,#174508,#174509,#174510,
#174511,#174512,#174513,#174514,#174515,#174516,#174517,#174518,#174519,
#174520,#174521,#174522,#174523,#174524,#174525,#174526,#174527,#174528,
#174529,#174530,#174531,#174532,#174533,#174534,#174535,#174536,#174537,
#174538),(#174539,#174540,#174541,#174542,#174543,#174544,#174545,#174546,
#174547,#174548,#174549,#174550,#174551,#174552,#174553,#174554,#174555,
#174556,#174557,#174558,#174559,#174560,#174561,#174562,#174563,#174564,
#174565,#174566,#174567,#174568,#174569,#174570,#174571,#174572,#174573,
#174574,#174575,#174576,#174577,#174578,#174579,#174580,#174581,#174582,
#174583,#174584,#174585,#174586,#174587,#174588,#174589,#174590,#174591,
#174592,#174593,#174594,#174595,#174596,#174597,#174598,#174599,#174600,
#174601,#174602,#174603,#174604,#174605,#174606,#174607,#174608,#174609,
#174610,#174611,#174612,#174613,#174614,#174615)),.UNSPECIFIED.,.F.,.F.,
 .F.,(2,2),(4,1,1,1,1,1,1,1,1,1,1,1,1,1,1,1,1,1,1,1,1,1,1,1,1,1,1,1,1,1,
1,1,1,1,1,1,1,1,1,1,1,1,1,1,1,1,1,1,1,1,1,1,1,1,1,1,1,1,1,1,1,1,1,1,1,1,
1,1,1,1,1,1,1,1,4),(0.,1.),(0.,0.0135337770704249,0.0270675541408498,0.0406013312112747,
0.0541351082816996,0.0676688853521246,0.0812026624225494,0.0947364394929744,
0.108270216563399,0.121803993633824,0.135337770704249,0.148871547774674,
0.162405324845099,0.175939101915524,0.189472878985949,0.203006656056374,
0.216540433126799,0.230074210197223,0.243607987267648,0.257141764338073,
0.270675541408498,0.284209318478923,0.297743095549348,0.311276872619773,
0.324810649690198,0.338344426760623,0.351878203831048,0.365411980901473,
0.378945757971897,0.392479535042322,0.406013312112747,0.419547089183172,
0.433080866253597,0.446614643324022,0.460148420394447,0.473682197464872,
0.487215974535297,0.500749751605722,0.514283528676147,0.527817305746571,
0.541351082816996,0.554884859887421,0.568418636957846,0.581952414028271,
0.595486191098696,0.609019968169121,0.622553745239546,0.636087522309971,
0.649621299380396,0.663155076450821,0.676688853521245,0.69022263059167,
0.703756407662095,0.71729018473252,0.730823961802945,0.74435773887337,0.757891515943795,
0.77142529301422,0.784959070084645,0.79849284715507,0.812026624225495,0.825560401295919,
0.839094178366344,0.852627955436769,0.866161732507194,0.879695509577619,
0.893229286648044,0.906763063718469,0.920296840788894,0.933830617859319,
0.947364394929744,0.960898172000169,0.974431949070593,0.987965726141018,
1.),.UNSPECIFIED.);
#183=B_SPLINE_SURFACE_WITH_KNOTS('',3,3,((#176366,#176367,#176368,#176369,
#176370,#176371,#176372,#176373,#176374,#176375,#176376,#176377,#176378,
#176379,#176380,#176381,#176382,#176383,#176384,#176385,#176386,#176387,
#176388,#176389,#176390,#176391,#176392,#176393,#176394,#176395,#176396,
#176397,#176398,#176399,#176400),(#176401,#176402,#176403,#176404,#176405,
#176406,#176407,#176408,#176409,#176410,#176411,#176412,#176413,#176414,
#176415,#176416,#176417,#176418,#176419,#176420,#176421,#176422,#176423,
#176424,#176425,#176426,#176427,#176428,#176429,#176430,#176431,#176432,
#176433,#176434,#176435),(#176436,#176437,#176438,#176439,#176440,#176441,
#176442,#176443,#176444,#176445,#176446,#176447,#176448,#176449,#176450,
#176451,#176452,#176453,#176454,#176455,#176456,#176457,#176458,#176459,
#176460,#176461,#176462,#176463,#176464,#176465,#176466,#176467,#176468,
#176469,#176470),(#176471,#176472,#176473,#176474,#176475,#176476,#176477,
#176478,#176479,#176480,#176481,#176482,#176483,#176484,#176485,#176486,
#176487,#176488,#176489,#176490,#176491,#176492,#176493,#176494,#176495,
#176496,#176497,#176498,#176499,#176500,#176501,#176502,#176503,#176504,
#176505)),.UNSPECIFIED.,.F.,.F.,.F.,(4,4),(4,1,1,1,1,1,1,1,1,1,1,1,1,1,
1,1,1,1,1,1,1,1,1,1,1,1,1,1,1,1,1,1,4),(0.,1.),(0.,0.031249999999992,0.062499999999984,
0.0937500000001036,0.125000000000096,0.156250000000088,0.187500000000079,
0.218750000000072,0.250000000000191,0.281250000000183,0.312500000000176,
0.343750000000167,0.375000000000159,0.406250000000151,0.437500000000271,
0.468750000000263,0.500000000000255,0.531250000000247,0.562500000000239,
0.593750000000231,0.62500000000035,0.656250000000342,0.687500000000335,
0.718750000000326,0.750000000000319,0.781250000000438,0.81250000000043,
0.843750000000422,0.875000000000414,0.906250000000406,0.937500000000398,
0.968750000000518,1.),.UNSPECIFIED.);
#184=B_SPLINE_SURFACE_WITH_KNOTS('',3,3,((#176773,#176774,#176775,#176776,
#176777,#176778,#176779,#176780,#176781,#176782,#176783,#176784,#176785,
#176786,#176787,#176788,#176789,#176790,#176791,#176792,#176793,#176794,
#176795,#176796,#176797,#176798,#176799,#176800,#176801,#176802,#176803,
#176804,#176805,#176806,#176807),(#176808,#176809,#176810,#176811,#176812,
#176813,#176814,#176815,#176816,#176817,#176818,#176819,#176820,#176821,
#176822,#176823,#176824,#176825,#176826,#176827,#176828,#176829,#176830,
#176831,#176832,#176833,#176834,#176835,#176836,#176837,#176838,#176839,
#176840,#176841,#176842),(#176843,#176844,#176845,#176846,#176847,#176848,
#176849,#176850,#176851,#176852,#176853,#176854,#176855,#176856,#176857,
#176858,#176859,#176860,#176861,#176862,#176863,#176864,#176865,#176866,
#176867,#176868,#176869,#176870,#176871,#176872,#176873,#176874,#176875,
#176876,#176877),(#176878,#176879,#176880,#176881,#176882,#176883,#176884,
#176885,#176886,#176887,#176888,#176889,#176890,#176891,#176892,#176893,
#176894,#176895,#176896,#176897,#176898,#176899,#176900,#176901,#176902,
#176903,#176904,#176905,#176906,#176907,#176908,#176909,#176910,#176911,
#176912)),.UNSPECIFIED.,.F.,.F.,.F.,(4,4),(4,1,1,1,1,1,1,1,1,1,1,1,1,1,
1,1,1,1,1,1,1,1,1,1,1,1,1,1,1,1,1,1,4),(0.,1.),(0.,0.031250000000078,0.0625000000000372,
0.0937500000001152,0.125000000000074,0.156250000000034,0.187500000000111,
0.218750000000071,0.250000000000148,0.281250000000108,0.312500000000186,
0.343750000000145,0.375000000000104,0.406250000000182,0.437500000000141,
0.468750000000219,0.500000000000178,0.531250000000256,0.562500000000216,
0.593750000000175,0.625000000000253,0.656250000000212,0.68750000000029,
0.718750000000249,0.750000000000208,0.781250000000286,0.812500000000245,
0.843750000000323,0.875000000000282,0.90625000000036,0.93750000000032,0.968750000000279,
1.),.UNSPECIFIED.);
#185=B_SPLINE_SURFACE_WITH_KNOTS('',3,3,((#176995,#176996,#176997,#176998,
#176999,#177000,#177001,#177002,#177003,#177004,#177005,#177006,#177007,
#177008,#177009,#177010,#177011,#177012,#177013,#177014,#177015,#177016,
#177017,#177018,#177019,#177020,#177021,#177022,#177023,#177024,#177025,
#177026,#177027,#177028,#177029,#177030,#177031,#177032,#177033,#177034,
#177035,#177036,#177037,#177038,#177039,#177040,#177041,#177042,#177043,
#177044,#177045,#177046,#177047,#177048,#177049,#177050,#177051,#177052,
#177053,#177054,#177055,#177056,#177057,#177058,#177059,#177060,#177061),
(#177062,#177063,#177064,#177065,#177066,#177067,#177068,#177069,#177070,
#177071,#177072,#177073,#177074,#177075,#177076,#177077,#177078,#177079,
#177080,#177081,#177082,#177083,#177084,#177085,#177086,#177087,#177088,
#177089,#177090,#177091,#177092,#177093,#177094,#177095,#177096,#177097,
#177098,#177099,#177100,#177101,#177102,#177103,#177104,#177105,#177106,
#177107,#177108,#177109,#177110,#177111,#177112,#177113,#177114,#177115,
#177116,#177117,#177118,#177119,#177120,#177121,#177122,#177123,#177124,
#177125,#177126,#177127,#177128),(#177129,#177130,#177131,#177132,#177133,
#177134,#177135,#177136,#177137,#177138,#177139,#177140,#177141,#177142,
#177143,#177144,#177145,#177146,#177147,#177148,#177149,#177150,#177151,
#177152,#177153,#177154,#177155,#177156,#177157,#177158,#177159,#177160,
#177161,#177162,#177163,#177164,#177165,#177166,#177167,#177168,#177169,
#177170,#177171,#177172,#177173,#177174,#177175,#177176,#177177,#177178,
#177179,#177180,#177181,#177182,#177183,#177184,#177185,#177186,#177187,
#177188,#177189,#177190,#177191,#177192,#177193,#177194,#177195),(#177196,
#177197,#177198,#177199,#177200,#177201,#177202,#177203,#177204,#177205,
#177206,#177207,#177208,#177209,#177210,#177211,#177212,#177213,#177214,
#177215,#177216,#177217,#177218,#177219,#177220,#177221,#177222,#177223,
#177224,#177225,#177226,#177227,#177228,#177229,#177230,#177231,#177232,
#177233,#177234,#177235,#177236,#177237,#177238,#177239,#177240,#177241,
#177242,#177243,#177244,#177245,#177246,#177247,#177248,#177249,#177250,
#177251,#177252,#177253,#177254,#177255,#177256,#177257,#177258,#177259,
#177260,#177261,#177262)),.UNSPECIFIED.,.F.,.F.,.F.,(4,4),(4,1,1,1,1,1,
1,1,1,1,1,1,1,1,1,1,1,1,1,1,1,1,1,1,1,1,1,1,1,1,1,1,1,1,1,1,1,1,1,1,1,1,
1,1,1,1,1,1,1,1,1,1,1,1,1,1,1,1,1,1,1,1,1,1,4),(0.,1.),(0.,0.015625,0.03125,
0.046875,0.0625,0.078125,0.09375,0.109375,0.125,0.140625,0.15625,0.171875,
0.1875,0.203125,0.21875,0.234375,0.25,0.265625,0.28125,0.296875,0.3125,
0.328125,0.34375,0.359375,0.375,0.390625,0.40625,0.421875,0.4375,0.453125,
0.46875,0.484375,0.5,0.515625,0.53125,0.546875,0.5625,0.578125,0.59375,
0.609375,0.625,0.640625,0.65625,0.671875,0.6875,0.703125,0.71875,0.734375,
0.75,0.765625,0.78125,0.796875,0.8125,0.828125,0.84375,0.859375,0.875,0.890625,
0.90625,0.921875,0.9375,0.953125,0.96875,0.984375,1.),.UNSPECIFIED.);
#186=B_SPLINE_SURFACE_WITH_KNOTS('',3,3,((#177270,#177271,#177272,#177273,
#177274),(#177275,#177276,#177277,#177278,#177279),(#177280,#177281,#177282,
#177283,#177284),(#177285,#177286,#177287,#177288,#177289)),
 .UNSPECIFIED.,.F.,.F.,.F.,(4,4),(4,1,4),(0.,1.),(0.,0.500000000000012,
1.),.UNSPECIFIED.);
#187=B_SPLINE_SURFACE_WITH_KNOTS('',3,1,((#177348,#177349),(#177350,#177351),
(#177352,#177353),(#177354,#177355),(#177356,#177357),(#177358,#177359),
(#177360,#177361),(#177362,#177363),(#177364,#177365),(#177366,#177367),
(#177368,#177369),(#177370,#177371)),.UNSPECIFIED.,.F.,.F.,.F.,(4,2,2,2,
2,4),(2,2),(0.0140497253938099,0.25,0.5,0.75,0.875,0.987103459251385),(0.,
0.071789856256767),.UNSPECIFIED.);
#188=B_SPLINE_SURFACE_WITH_KNOTS('',3,3,((#177430,#177431,#177432,#177433,
#177434),(#177435,#177436,#177437,#177438,#177439),(#177440,#177441,#177442,
#177443,#177444),(#177445,#177446,#177447,#177448,#177449)),
 .UNSPECIFIED.,.F.,.F.,.F.,(4,4),(4,1,4),(0.,1.),(0.,0.500000000000012,
1.),.UNSPECIFIED.);
#189=B_SPLINE_SURFACE_WITH_KNOTS('',3,3,((#177456,#177457,#177458,#177459,
#177460,#177461,#177462,#177463,#177464,#177465,#177466,#177467,#177468,
#177469,#177470,#177471,#177472,#177473,#177474,#177475,#177476,#177477,
#177478,#177479,#177480,#177481,#177482,#177483,#177484,#177485,#177486,
#177487,#177488,#177489,#177490,#177491,#177492,#177493,#177494,#177495,
#177496,#177497,#177498,#177499,#177500,#177501,#177502,#177503,#177504,
#177505,#177506,#177507,#177508,#177509,#177510,#177511,#177512,#177513,
#177514,#177515,#177516,#177517,#177518,#177519,#177520,#177521,#177522),
(#177523,#177524,#177525,#177526,#177527,#177528,#177529,#177530,#177531,
#177532,#177533,#177534,#177535,#177536,#177537,#177538,#177539,#177540,
#177541,#177542,#177543,#177544,#177545,#177546,#177547,#177548,#177549,
#177550,#177551,#177552,#177553,#177554,#177555,#177556,#177557,#177558,
#177559,#177560,#177561,#177562,#177563,#177564,#177565,#177566,#177567,
#177568,#177569,#177570,#177571,#177572,#177573,#177574,#177575,#177576,
#177577,#177578,#177579,#177580,#177581,#177582,#177583,#177584,#177585,
#177586,#177587,#177588,#177589),(#177590,#177591,#177592,#177593,#177594,
#177595,#177596,#177597,#177598,#177599,#177600,#177601,#177602,#177603,
#177604,#177605,#177606,#177607,#177608,#177609,#177610,#177611,#177612,
#177613,#177614,#177615,#177616,#177617,#177618,#177619,#177620,#177621,
#177622,#177623,#177624,#177625,#177626,#177627,#177628,#177629,#177630,
#177631,#177632,#177633,#177634,#177635,#177636,#177637,#177638,#177639,
#177640,#177641,#177642,#177643,#177644,#177645,#177646,#177647,#177648,
#177649,#177650,#177651,#177652,#177653,#177654,#177655,#177656),(#177657,
#177658,#177659,#177660,#177661,#177662,#177663,#177664,#177665,#177666,
#177667,#177668,#177669,#177670,#177671,#177672,#177673,#177674,#177675,
#177676,#177677,#177678,#177679,#177680,#177681,#177682,#177683,#177684,
#177685,#177686,#177687,#177688,#177689,#177690,#177691,#177692,#177693,
#177694,#177695,#177696,#177697,#177698,#177699,#177700,#177701,#177702,
#177703,#177704,#177705,#177706,#177707,#177708,#177709,#177710,#177711,
#177712,#177713,#177714,#177715,#177716,#177717,#177718,#177719,#177720,
#177721,#177722,#177723)),.UNSPECIFIED.,.F.,.F.,.F.,(4,4),(4,1,1,1,1,1,
1,1,1,1,1,1,1,1,1,1,1,1,1,1,1,1,1,1,1,1,1,1,1,1,1,1,1,1,1,1,1,1,1,1,1,1,
1,1,1,1,1,1,1,1,1,1,1,1,1,1,1,1,1,1,1,1,1,1,4),(0.,1.),(0.,0.015625,0.03125,
0.046875,0.0625,0.078125,0.09375,0.109375,0.125,0.140625,0.15625,0.171875,
0.1875,0.203125,0.21875,0.234375,0.25,0.265625,0.28125,0.296875,0.3125,
0.328125,0.34375,0.359375,0.375,0.390625,0.40625,0.421875,0.4375,0.453125,
0.46875,0.484375,0.5,0.515625,0.53125,0.546875,0.5625,0.578125,0.59375,
0.609375,0.625,0.640625,0.65625,0.671875,0.6875,0.703125,0.71875,0.734375,
0.75,0.765625,0.78125,0.796875,0.8125,0.828125,0.84375,0.859375,0.875,0.890625,
0.90625,0.921875,0.9375,0.953125,0.96875,0.984375,1.),.UNSPECIFIED.);
#190=B_SPLINE_SURFACE_WITH_KNOTS('',3,3,((#177724,#177725,#177726,#177727,
#177728,#177729,#177730,#177731,#177732,#177733,#177734,#177735,#177736,
#177737,#177738,#177739,#177740,#177741,#177742,#177743,#177744,#177745,
#177746,#177747,#177748,#177749,#177750,#177751,#177752,#177753,#177754,
#177755,#177756,#177757,#177758),(#177759,#177760,#177761,#177762,#177763,
#177764,#177765,#177766,#177767,#177768,#177769,#177770,#177771,#177772,
#177773,#177774,#177775,#177776,#177777,#177778,#177779,#177780,#177781,
#177782,#177783,#177784,#177785,#177786,#177787,#177788,#177789,#177790,
#177791,#177792,#177793),(#177794,#177795,#177796,#177797,#177798,#177799,
#177800,#177801,#177802,#177803,#177804,#177805,#177806,#177807,#177808,
#177809,#177810,#177811,#177812,#177813,#177814,#177815,#177816,#177817,
#177818,#177819,#177820,#177821,#177822,#177823,#177824,#177825,#177826,
#177827,#177828),(#177829,#177830,#177831,#177832,#177833,#177834,#177835,
#177836,#177837,#177838,#177839,#177840,#177841,#177842,#177843,#177844,
#177845,#177846,#177847,#177848,#177849,#177850,#177851,#177852,#177853,
#177854,#177855,#177856,#177857,#177858,#177859,#177860,#177861,#177862,
#177863)),.UNSPECIFIED.,.F.,.F.,.F.,(4,4),(4,1,1,1,1,1,1,1,1,1,1,1,1,1,
1,1,1,1,1,1,1,1,1,1,1,1,1,1,1,1,1,1,4),(0.,1.),(0.,0.031250000000078,0.0625000000000372,
0.0937500000001152,0.125000000000074,0.156250000000034,0.187500000000111,
0.218750000000071,0.250000000000148,0.281250000000108,0.312500000000186,
0.343750000000145,0.375000000000104,0.406250000000182,0.437500000000141,
0.468750000000219,0.500000000000178,0.531250000000256,0.562500000000216,
0.593750000000175,0.625000000000253,0.656250000000212,0.68750000000029,
0.718750000000249,0.750000000000208,0.781250000000286,0.812500000000245,
0.843750000000323,0.875000000000282,0.90625000000036,0.93750000000032,0.968750000000279,
1.),.UNSPECIFIED.);
#191=B_SPLINE_SURFACE_WITH_KNOTS('',3,3,((#179610,#179611,#179612,#179613,
#179614,#179615,#179616,#179617,#179618,#179619,#179620,#179621,#179622,
#179623,#179624,#179625,#179626,#179627,#179628,#179629,#179630,#179631,
#179632,#179633,#179634,#179635,#179636,#179637,#179638,#179639,#179640,
#179641,#179642,#179643,#179644),(#179645,#179646,#179647,#179648,#179649,
#179650,#179651,#179652,#179653,#179654,#179655,#179656,#179657,#179658,
#179659,#179660,#179661,#179662,#179663,#179664,#179665,#179666,#179667,
#179668,#179669,#179670,#179671,#179672,#179673,#179674,#179675,#179676,
#179677,#179678,#179679),(#179680,#179681,#179682,#179683,#179684,#179685,
#179686,#179687,#179688,#179689,#179690,#179691,#179692,#179693,#179694,
#179695,#179696,#179697,#179698,#179699,#179700,#179701,#179702,#179703,
#179704,#179705,#179706,#179707,#179708,#179709,#179710,#179711,#179712,
#179713,#179714),(#179715,#179716,#179717,#179718,#179719,#179720,#179721,
#179722,#179723,#179724,#179725,#179726,#179727,#179728,#179729,#179730,
#179731,#179732,#179733,#179734,#179735,#179736,#179737,#179738,#179739,
#179740,#179741,#179742,#179743,#179744,#179745,#179746,#179747,#179748,
#179749)),.UNSPECIFIED.,.F.,.F.,.F.,(4,4),(4,1,1,1,1,1,1,1,1,1,1,1,1,1,
1,1,1,1,1,1,1,1,1,1,1,1,1,1,1,1,1,1,4),(0.,1.),(0.,0.031249999999992,0.062499999999984,
0.0937500000001036,0.125000000000096,0.156250000000088,0.187500000000079,
0.218750000000072,0.250000000000191,0.281250000000183,0.312500000000176,
0.343750000000167,0.375000000000159,0.406250000000151,0.437500000000271,
0.468750000000263,0.500000000000255,0.531250000000247,0.562500000000239,
0.593750000000231,0.62500000000035,0.656250000000342,0.687500000000335,
0.718750000000326,0.750000000000319,0.781250000000438,0.81250000000043,
0.843750000000422,0.875000000000414,0.906250000000406,0.937500000000398,
0.968750000000518,1.),.UNSPECIFIED.);
#192=B_SPLINE_SURFACE_WITH_KNOTS('',3,3,((#180017,#180018,#180019,#180020,
#180021,#180022,#180023,#180024,#180025,#180026,#180027,#180028,#180029,
#180030,#180031,#180032,#180033,#180034,#180035,#180036,#180037,#180038,
#180039,#180040,#180041,#180042,#180043,#180044,#180045,#180046,#180047,
#180048,#180049,#180050,#180051),(#180052,#180053,#180054,#180055,#180056,
#180057,#180058,#180059,#180060,#180061,#180062,#180063,#180064,#180065,
#180066,#180067,#180068,#180069,#180070,#180071,#180072,#180073,#180074,
#180075,#180076,#180077,#180078,#180079,#180080,#180081,#180082,#180083,
#180084,#180085,#180086),(#180087,#180088,#180089,#180090,#180091,#180092,
#180093,#180094,#180095,#180096,#180097,#180098,#180099,#180100,#180101,
#180102,#180103,#180104,#180105,#180106,#180107,#180108,#180109,#180110,
#180111,#180112,#180113,#180114,#180115,#180116,#180117,#180118,#180119,
#180120,#180121),(#180122,#180123,#180124,#180125,#180126,#180127,#180128,
#180129,#180130,#180131,#180132,#180133,#180134,#180135,#180136,#180137,
#180138,#180139,#180140,#180141,#180142,#180143,#180144,#180145,#180146,
#180147,#180148,#180149,#180150,#180151,#180152,#180153,#180154,#180155,
#180156)),.UNSPECIFIED.,.F.,.F.,.F.,(4,4),(4,1,1,1,1,1,1,1,1,1,1,1,1,1,
1,1,1,1,1,1,1,1,1,1,1,1,1,1,1,1,1,1,4),(0.,1.),(0.,0.031250000000078,0.0625000000000372,
0.0937500000001152,0.125000000000074,0.156250000000034,0.187500000000111,
0.218750000000071,0.250000000000148,0.281250000000108,0.312500000000186,
0.343750000000145,0.375000000000104,0.406250000000182,0.437500000000141,
0.468750000000219,0.500000000000178,0.531250000000256,0.562500000000216,
0.593750000000175,0.625000000000253,0.656250000000212,0.68750000000029,
0.718750000000249,0.750000000000208,0.781250000000286,0.812500000000245,
0.843750000000323,0.875000000000282,0.90625000000036,0.93750000000032,0.968750000000279,
1.),.UNSPECIFIED.);
#193=B_SPLINE_SURFACE_WITH_KNOTS('',3,3,((#180239,#180240,#180241,#180242,
#180243,#180244,#180245,#180246,#180247,#180248,#180249,#180250,#180251,
#180252,#180253,#180254,#180255,#180256,#180257,#180258,#180259,#180260,
#180261,#180262,#180263,#180264,#180265,#180266,#180267,#180268,#180269,
#180270,#180271,#180272,#180273,#180274,#180275,#180276,#180277,#180278,
#180279,#180280,#180281,#180282,#180283,#180284,#180285,#180286,#180287,
#180288,#180289,#180290,#180291,#180292,#180293,#180294,#180295,#180296,
#180297,#180298,#180299,#180300,#180301,#180302,#180303,#180304,#180305),
(#180306,#180307,#180308,#180309,#180310,#180311,#180312,#180313,#180314,
#180315,#180316,#180317,#180318,#180319,#180320,#180321,#180322,#180323,
#180324,#180325,#180326,#180327,#180328,#180329,#180330,#180331,#180332,
#180333,#180334,#180335,#180336,#180337,#180338,#180339,#180340,#180341,
#180342,#180343,#180344,#180345,#180346,#180347,#180348,#180349,#180350,
#180351,#180352,#180353,#180354,#180355,#180356,#180357,#180358,#180359,
#180360,#180361,#180362,#180363,#180364,#180365,#180366,#180367,#180368,
#180369,#180370,#180371,#180372),(#180373,#180374,#180375,#180376,#180377,
#180378,#180379,#180380,#180381,#180382,#180383,#180384,#180385,#180386,
#180387,#180388,#180389,#180390,#180391,#180392,#180393,#180394,#180395,
#180396,#180397,#180398,#180399,#180400,#180401,#180402,#180403,#180404,
#180405,#180406,#180407,#180408,#180409,#180410,#180411,#180412,#180413,
#180414,#180415,#180416,#180417,#180418,#180419,#180420,#180421,#180422,
#180423,#180424,#180425,#180426,#180427,#180428,#180429,#180430,#180431,
#180432,#180433,#180434,#180435,#180436,#180437,#180438,#180439),(#180440,
#180441,#180442,#180443,#180444,#180445,#180446,#180447,#180448,#180449,
#180450,#180451,#180452,#180453,#180454,#180455,#180456,#180457,#180458,
#180459,#180460,#180461,#180462,#180463,#180464,#180465,#180466,#180467,
#180468,#180469,#180470,#180471,#180472,#180473,#180474,#180475,#180476,
#180477,#180478,#180479,#180480,#180481,#180482,#180483,#180484,#180485,
#180486,#180487,#180488,#180489,#180490,#180491,#180492,#180493,#180494,
#180495,#180496,#180497,#180498,#180499,#180500,#180501,#180502,#180503,
#180504,#180505,#180506)),.UNSPECIFIED.,.F.,.F.,.F.,(4,4),(4,1,1,1,1,1,
1,1,1,1,1,1,1,1,1,1,1,1,1,1,1,1,1,1,1,1,1,1,1,1,1,1,1,1,1,1,1,1,1,1,1,1,
1,1,1,1,1,1,1,1,1,1,1,1,1,1,1,1,1,1,1,1,1,1,4),(0.,1.),(0.,0.015625,0.03125,
0.046875,0.0625,0.078125,0.09375,0.109375,0.125,0.140625,0.15625,0.171875,
0.1875,0.203125,0.21875,0.234375,0.25,0.265625,0.28125,0.296875,0.3125,
0.328125,0.34375,0.359375,0.375,0.390625,0.40625,0.421875,0.4375,0.453125,
0.46875,0.484375,0.5,0.515625,0.53125,0.546875,0.5625,0.578125,0.59375,
0.609375,0.625,0.640625,0.65625,0.671875,0.6875,0.703125,0.71875,0.734375,
0.75,0.765625,0.78125,0.796875,0.8125,0.828125,0.84375,0.859375,0.875,0.890625,
0.90625,0.921875,0.9375,0.953125,0.96875,0.984375,1.),.UNSPECIFIED.);
#194=B_SPLINE_SURFACE_WITH_KNOTS('',3,3,((#180514,#180515,#180516,#180517,
#180518),(#180519,#180520,#180521,#180522,#180523),(#180524,#180525,#180526,
#180527,#180528),(#180529,#180530,#180531,#180532,#180533)),
 .UNSPECIFIED.,.F.,.F.,.F.,(4,4),(4,1,4),(0.,1.),(0.,0.500000000000012,
1.),.UNSPECIFIED.);
#195=B_SPLINE_SURFACE_WITH_KNOTS('',3,1,((#180592,#180593),(#180594,#180595),
(#180596,#180597),(#180598,#180599),(#180600,#180601),(#180602,#180603),
(#180604,#180605),(#180606,#180607),(#180608,#180609),(#180610,#180611),
(#180612,#180613),(#180614,#180615)),.UNSPECIFIED.,.F.,.F.,.F.,(4,2,2,2,
2,4),(2,2),(0.0140497253938089,0.25,0.5,0.75,0.875,0.987103459251385),(0.,
0.0717898562567659),.UNSPECIFIED.);
#196=B_SPLINE_SURFACE_WITH_KNOTS('',3,3,((#180674,#180675,#180676,#180677,
#180678),(#180679,#180680,#180681,#180682,#180683),(#180684,#180685,#180686,
#180687,#180688),(#180689,#180690,#180691,#180692,#180693)),
 .UNSPECIFIED.,.F.,.F.,.F.,(4,4),(4,1,4),(0.,1.),(0.,0.500000000000012,
1.),.UNSPECIFIED.);
#197=B_SPLINE_SURFACE_WITH_KNOTS('',3,3,((#180700,#180701,#180702,#180703,
#180704,#180705,#180706,#180707,#180708,#180709,#180710,#180711,#180712,
#180713,#180714,#180715,#180716,#180717,#180718,#180719,#180720,#180721,
#180722,#180723,#180724,#180725,#180726,#180727,#180728,#180729,#180730,
#180731,#180732,#180733,#180734,#180735,#180736,#180737,#180738,#180739,
#180740,#180741,#180742,#180743,#180744,#180745,#180746,#180747,#180748,
#180749,#180750,#180751,#180752,#180753,#180754,#180755,#180756,#180757,
#180758,#180759,#180760,#180761,#180762,#180763,#180764,#180765,#180766),
(#180767,#180768,#180769,#180770,#180771,#180772,#180773,#180774,#180775,
#180776,#180777,#180778,#180779,#180780,#180781,#180782,#180783,#180784,
#180785,#180786,#180787,#180788,#180789,#180790,#180791,#180792,#180793,
#180794,#180795,#180796,#180797,#180798,#180799,#180800,#180801,#180802,
#180803,#180804,#180805,#180806,#180807,#180808,#180809,#180810,#180811,
#180812,#180813,#180814,#180815,#180816,#180817,#180818,#180819,#180820,
#180821,#180822,#180823,#180824,#180825,#180826,#180827,#180828,#180829,
#180830,#180831,#180832,#180833),(#180834,#180835,#180836,#180837,#180838,
#180839,#180840,#180841,#180842,#180843,#180844,#180845,#180846,#180847,
#180848,#180849,#180850,#180851,#180852,#180853,#180854,#180855,#180856,
#180857,#180858,#180859,#180860,#180861,#180862,#180863,#180864,#180865,
#180866,#180867,#180868,#180869,#180870,#180871,#180872,#180873,#180874,
#180875,#180876,#180877,#180878,#180879,#180880,#180881,#180882,#180883,
#180884,#180885,#180886,#180887,#180888,#180889,#180890,#180891,#180892,
#180893,#180894,#180895,#180896,#180897,#180898,#180899,#180900),(#180901,
#180902,#180903,#180904,#180905,#180906,#180907,#180908,#180909,#180910,
#180911,#180912,#180913,#180914,#180915,#180916,#180917,#180918,#180919,
#180920,#180921,#180922,#180923,#180924,#180925,#180926,#180927,#180928,
#180929,#180930,#180931,#180932,#180933,#180934,#180935,#180936,#180937,
#180938,#180939,#180940,#180941,#180942,#180943,#180944,#180945,#180946,
#180947,#180948,#180949,#180950,#180951,#180952,#180953,#180954,#180955,
#180956,#180957,#180958,#180959,#180960,#180961,#180962,#180963,#180964,
#180965,#180966,#180967)),.UNSPECIFIED.,.F.,.F.,.F.,(4,4),(4,1,1,1,1,1,
1,1,1,1,1,1,1,1,1,1,1,1,1,1,1,1,1,1,1,1,1,1,1,1,1,1,1,1,1,1,1,1,1,1,1,1,
1,1,1,1,1,1,1,1,1,1,1,1,1,1,1,1,1,1,1,1,1,1,4),(0.,1.),(0.,0.015625,0.03125,
0.046875,0.0625,0.078125,0.09375,0.109375,0.125,0.140625,0.15625,0.171875,
0.1875,0.203125,0.21875,0.234375,0.25,0.265625,0.28125,0.296875,0.3125,
0.328125,0.34375,0.359375,0.375,0.390625,0.40625,0.421875,0.4375,0.453125,
0.46875,0.484375,0.5,0.515625,0.53125,0.546875,0.5625,0.578125,0.59375,
0.609375,0.625,0.640625,0.65625,0.671875,0.6875,0.703125,0.71875,0.734375,
0.75,0.765625,0.78125,0.796875,0.8125,0.828125,0.84375,0.859375,0.875,0.890625,
0.90625,0.921875,0.9375,0.953125,0.96875,0.984375,1.),.UNSPECIFIED.);
#198=B_SPLINE_SURFACE_WITH_KNOTS('',3,3,((#180968,#180969,#180970,#180971,
#180972,#180973,#180974,#180975,#180976,#180977,#180978,#180979,#180980,
#180981,#180982,#180983,#180984,#180985,#180986,#180987,#180988,#180989,
#180990,#180991,#180992,#180993,#180994,#180995,#180996,#180997,#180998,
#180999,#181000,#181001,#181002),(#181003,#181004,#181005,#181006,#181007,
#181008,#181009,#181010,#181011,#181012,#181013,#181014,#181015,#181016,
#181017,#181018,#181019,#181020,#181021,#181022,#181023,#181024,#181025,
#181026,#181027,#181028,#181029,#181030,#181031,#181032,#181033,#181034,
#181035,#181036,#181037),(#181038,#181039,#181040,#181041,#181042,#181043,
#181044,#181045,#181046,#181047,#181048,#181049,#181050,#181051,#181052,
#181053,#181054,#181055,#181056,#181057,#181058,#181059,#181060,#181061,
#181062,#181063,#181064,#181065,#181066,#181067,#181068,#181069,#181070,
#181071,#181072),(#181073,#181074,#181075,#181076,#181077,#181078,#181079,
#181080,#181081,#181082,#181083,#181084,#181085,#181086,#181087,#181088,
#181089,#181090,#181091,#181092,#181093,#181094,#181095,#181096,#181097,
#181098,#181099,#181100,#181101,#181102,#181103,#181104,#181105,#181106,
#181107)),.UNSPECIFIED.,.F.,.F.,.F.,(4,4),(4,1,1,1,1,1,1,1,1,1,1,1,1,1,
1,1,1,1,1,1,1,1,1,1,1,1,1,1,1,1,1,1,4),(0.,1.),(0.,0.031250000000078,0.0625000000000372,
0.0937500000001152,0.125000000000074,0.156250000000034,0.187500000000111,
0.218750000000071,0.250000000000148,0.281250000000108,0.312500000000186,
0.343750000000145,0.375000000000104,0.406250000000182,0.437500000000141,
0.468750000000219,0.500000000000178,0.531250000000256,0.562500000000216,
0.593750000000175,0.625000000000253,0.656250000000212,0.68750000000029,
0.718750000000249,0.750000000000208,0.781250000000286,0.812500000000245,
0.843750000000323,0.875000000000282,0.90625000000036,0.93750000000032,0.968750000000279,
1.),.UNSPECIFIED.);
#199=B_SPLINE_SURFACE_WITH_KNOTS('',1,3,((#183512,#183513,#183514,#183515,
#183516,#183517,#183518,#183519,#183520,#183521,#183522,#183523,#183524,
#183525,#183526,#183527,#183528,#183529,#183530,#183531,#183532,#183533,
#183534,#183535,#183536,#183537,#183538,#183539,#183540,#183541,#183542,
#183543,#183544,#183545,#183546,#183547,#183548,#183549,#183550,#183551,
#183552,#183553,#183554,#183555,#183556,#183557,#183558,#183559,#183560,
#183561,#183562,#183563,#183564,#183565),(#183566,#183567,#183568,#183569,
#183570,#183571,#183572,#183573,#183574,#183575,#183576,#183577,#183578,
#183579,#183580,#183581,#183582,#183583,#183584,#183585,#183586,#183587,
#183588,#183589,#183590,#183591,#183592,#183593,#183594,#183595,#183596,
#183597,#183598,#183599,#183600,#183601,#183602,#183603,#183604,#183605,
#183606,#183607,#183608,#183609,#183610,#183611,#183612,#183613,#183614,
#183615,#183616,#183617,#183618,#183619)),.UNSPECIFIED.,.F.,.F.,.F.,(2,
2),(4,1,1,1,1,1,1,1,1,1,1,1,1,1,1,1,1,1,1,1,1,1,1,1,1,1,1,1,1,1,1,1,1,1,
1,1,1,1,1,1,1,1,1,1,1,1,1,1,1,1,1,4),(0.,1.),(0.,0.0198373427721521,0.0396746855443041,
0.0595120283164562,0.0793493710886083,0.0991867138607603,0.119024056632912,
0.138861399405064,0.158698742177217,0.178536084949369,0.198373427721521,
0.218210770493673,0.238048113265825,0.257885456037977,0.277722798810129,
0.297560141582281,0.317397484354433,0.337234827126585,0.357072169898737,
0.376909512670889,0.396746855443041,0.416584198215193,0.436421540987345,
0.456258883759498,0.47609622653165,0.495933569303802,0.515770912075954,
0.535608254848106,0.555445597620258,0.57528294039241,0.595120283164562,
0.614957625936714,0.634794968708866,0.654632311481018,0.67446965425317,
0.694306997025322,0.714144339797474,0.733981682569626,0.753819025341778,
0.773656368113931,0.793493710886083,0.813331053658235,0.833168396430387,
0.853005739202539,0.872843081974691,0.892680424746843,0.912517767518995,
0.932355110291147,0.952192453063299,0.972029795835451,0.991867138607603,
1.),.UNSPECIFIED.);
#200=B_SPLINE_SURFACE_WITH_KNOTS('',1,3,((#183620,#183621,#183622,#183623,
#183624,#183625,#183626,#183627,#183628,#183629,#183630,#183631,#183632,
#183633,#183634,#183635,#183636,#183637,#183638,#183639,#183640,#183641,
#183642,#183643,#183644,#183645,#183646,#183647,#183648,#183649,#183650,
#183651,#183652,#183653,#183654,#183655,#183656,#183657,#183658,#183659,
#183660,#183661,#183662,#183663,#183664,#183665,#183666,#183667,#183668,
#183669,#183670,#183671,#183672,#183673),(#183674,#183675,#183676,#183677,
#183678,#183679,#183680,#183681,#183682,#183683,#183684,#183685,#183686,
#183687,#183688,#183689,#183690,#183691,#183692,#183693,#183694,#183695,
#183696,#183697,#183698,#183699,#183700,#183701,#183702,#183703,#183704,
#183705,#183706,#183707,#183708,#183709,#183710,#183711,#183712,#183713,
#183714,#183715,#183716,#183717,#183718,#183719,#183720,#183721,#183722,
#183723,#183724,#183725,#183726,#183727)),.UNSPECIFIED.,.F.,.F.,.F.,(2,
2),(4,1,1,1,1,1,1,1,1,1,1,1,1,1,1,1,1,1,1,1,1,1,1,1,1,1,1,1,1,1,1,1,1,1,
1,1,1,1,1,1,1,1,1,1,1,1,1,1,1,1,1,4),(0.,1.),(0.,0.0198373427721521,0.0396746855443041,
0.0595120283164562,0.0793493710886083,0.0991867138607603,0.119024056632912,
0.138861399405064,0.158698742177217,0.178536084949369,0.198373427721521,
0.218210770493673,0.238048113265825,0.257885456037977,0.277722798810129,
0.297560141582281,0.317397484354433,0.337234827126585,0.357072169898737,
0.376909512670889,0.396746855443041,0.416584198215193,0.436421540987345,
0.456258883759498,0.47609622653165,0.495933569303802,0.515770912075954,
0.535608254848106,0.555445597620258,0.57528294039241,0.595120283164562,
0.614957625936714,0.634794968708866,0.654632311481018,0.67446965425317,
0.694306997025322,0.714144339797474,0.733981682569626,0.753819025341778,
0.773656368113931,0.793493710886083,0.813331053658235,0.833168396430387,
0.853005739202539,0.872843081974691,0.892680424746843,0.912517767518995,
0.932355110291147,0.952192453063299,0.972029795835451,0.991867138607603,
1.),.UNSPECIFIED.);
#201=B_SPLINE_SURFACE_WITH_KNOTS('',3,3,((#184914,#184915,#184916,#184917,
#184918,#184919,#184920,#184921,#184922,#184923,#184924,#184925,#184926,
#184927,#184928,#184929,#184930,#184931,#184932,#184933,#184934,#184935,
#184936,#184937,#184938,#184939,#184940,#184941,#184942,#184943,#184944,
#184945,#184946,#184947,#184948),(#184949,#184950,#184951,#184952,#184953,
#184954,#184955,#184956,#184957,#184958,#184959,#184960,#184961,#184962,
#184963,#184964,#184965,#184966,#184967,#184968,#184969,#184970,#184971,
#184972,#184973,#184974,#184975,#184976,#184977,#184978,#184979,#184980,
#184981,#184982,#184983),(#184984,#184985,#184986,#184987,#184988,#184989,
#184990,#184991,#184992,#184993,#184994,#184995,#184996,#184997,#184998,
#184999,#185000,#185001,#185002,#185003,#185004,#185005,#185006,#185007,
#185008,#185009,#185010,#185011,#185012,#185013,#185014,#185015,#185016,
#185017,#185018),(#185019,#185020,#185021,#185022,#185023,#185024,#185025,
#185026,#185027,#185028,#185029,#185030,#185031,#185032,#185033,#185034,
#185035,#185036,#185037,#185038,#185039,#185040,#185041,#185042,#185043,
#185044,#185045,#185046,#185047,#185048,#185049,#185050,#185051,#185052,
#185053)),.UNSPECIFIED.,.F.,.F.,.F.,(4,4),(4,1,1,1,1,1,1,1,1,1,1,1,1,1,
1,1,1,1,1,1,1,1,1,1,1,1,1,1,1,1,1,1,4),(0.,1.),(0.,0.0312500000000065,0.0625000000000025,
0.0937500000000037,0.125000000000005,0.156250000000045,0.187500000000073,
0.218749999999969,0.249999999999997,0.281250000000024,0.312500000000052,
0.343750000000079,0.374999999999975,0.40625,0.43750000000003,0.468750000000058,
0.500000000000085,0.531249999999982,0.562500000000009,0.593750000000036,
0.625000000000064,0.656250000000091,0.687499999999988,0.718750000000015,
0.750000000000043,0.78125000000007,0.812500000000097,0.84375,0.875000000000021,
0.906250000000049,0.937500000000076,0.968750000000104,1.),.UNSPECIFIED.);
#202=B_SPLINE_SURFACE_WITH_KNOTS('',3,3,((#185513,#185514,#185515,#185516,
#185517,#185518,#185519,#185520,#185521,#185522,#185523,#185524,#185525,
#185526,#185527,#185528,#185529,#185530,#185531),(#185532,#185533,#185534,
#185535,#185536,#185537,#185538,#185539,#185540,#185541,#185542,#185543,
#185544,#185545,#185546,#185547,#185548,#185549,#185550),(#185551,#185552,
#185553,#185554,#185555,#185556,#185557,#185558,#185559,#185560,#185561,
#185562,#185563,#185564,#185565,#185566,#185567,#185568,#185569),(#185570,
#185571,#185572,#185573,#185574,#185575,#185576,#185577,#185578,#185579,
#185580,#185581,#185582,#185583,#185584,#185585,#185586,#185587,#185588)),
 .UNSPECIFIED.,.F.,.F.,.F.,(4,4),(4,1,1,1,1,1,1,1,1,1,1,1,1,1,1,1,4),(0.,
1.),(0.,0.0625000000000177,0.124999999999754,0.187499999999772,0.249999999999789,
0.312499999999525,0.374999999999543,0.437499999999561,0.499999999999297,
0.562499999999315,0.624999999999332,0.687499999999069,0.749999999999086,
0.812499999998822,0.87499999999884,0.937499999998858,1.),.UNSPECIFIED.);
#203=B_SPLINE_SURFACE_WITH_KNOTS('',3,3,((#185868,#185869,#185870,#185871,
#185872,#185873,#185874,#185875,#185876,#185877,#185878,#185879,#185880,
#185881,#185882,#185883,#185884,#185885,#185886,#185887,#185888,#185889,
#185890,#185891,#185892,#185893,#185894,#185895,#185896,#185897,#185898,
#185899,#185900,#185901,#185902),(#185903,#185904,#185905,#185906,#185907,
#185908,#185909,#185910,#185911,#185912,#185913,#185914,#185915,#185916,
#185917,#185918,#185919,#185920,#185921,#185922,#185923,#185924,#185925,
#185926,#185927,#185928,#185929,#185930,#185931,#185932,#185933,#185934,
#185935,#185936,#185937),(#185938,#185939,#185940,#185941,#185942,#185943,
#185944,#185945,#185946,#185947,#185948,#185949,#185950,#185951,#185952,
#185953,#185954,#185955,#185956,#185957,#185958,#185959,#185960,#185961,
#185962,#185963,#185964,#185965,#185966,#185967,#185968,#185969,#185970,
#185971,#185972),(#185973,#185974,#185975,#185976,#185977,#185978,#185979,
#185980,#185981,#185982,#185983,#185984,#185985,#185986,#185987,#185988,
#185989,#185990,#185991,#185992,#185993,#185994,#185995,#185996,#185997,
#185998,#185999,#186000,#186001,#186002,#186003,#186004,#186005,#186006,
#186007)),.UNSPECIFIED.,.F.,.F.,.F.,(4,4),(4,1,1,1,1,1,1,1,1,1,1,1,1,1,
1,1,1,1,1,1,1,1,1,1,1,1,1,1,1,1,1,1,4),(0.,1.),(0.,0.0312499999999954,0.0624999999999932,
0.0937499999999958,0.124999999999998,0.15625,0.187500000000028,0.218750000000055,
0.249999999999961,0.281249999999988,0.312500000000014,0.343750000000041,
0.375000000000068,0.406249999999974,0.4375,0.468750000000028,0.500000000000054,
0.531250000000081,0.562499999999987,0.593750000000014,0.625000000000041,
0.656250000000068,0.687499999999974,0.71875,0.750000000000027,0.781250000000054,
0.812500000000081,0.843749999999987,0.875000000000014,0.90625000000004,
0.937500000000067,0.968750000000094,1.),.UNSPECIFIED.);
#204=B_SPLINE_SURFACE_WITH_KNOTS('',3,3,((#186635,#186636,#186637,#186638,
#186639,#186640,#186641,#186642,#186643,#186644,#186645,#186646,#186647,
#186648,#186649,#186650,#186651,#186652,#186653,#186654,#186655,#186656,
#186657,#186658,#186659,#186660,#186661,#186662,#186663,#186664,#186665,
#186666,#186667,#186668,#186669,#186670,#186671,#186672,#186673,#186674,
#186675,#186676,#186677,#186678,#186679,#186680,#186681,#186682,#186683,
#186684,#186685,#186686,#186687,#186688,#186689,#186690,#186691,#186692,
#186693,#186694,#186695,#186696,#186697,#186698,#186699,#186700,#186701),
(#186702,#186703,#186704,#186705,#186706,#186707,#186708,#186709,#186710,
#186711,#186712,#186713,#186714,#186715,#186716,#186717,#186718,#186719,
#186720,#186721,#186722,#186723,#186724,#186725,#186726,#186727,#186728,
#186729,#186730,#186731,#186732,#186733,#186734,#186735,#186736,#186737,
#186738,#186739,#186740,#186741,#186742,#186743,#186744,#186745,#186746,
#186747,#186748,#186749,#186750,#186751,#186752,#186753,#186754,#186755,
#186756,#186757,#186758,#186759,#186760,#186761,#186762,#186763,#186764,
#186765,#186766,#186767,#186768),(#186769,#186770,#186771,#186772,#186773,
#186774,#186775,#186776,#186777,#186778,#186779,#186780,#186781,#186782,
#186783,#186784,#186785,#186786,#186787,#186788,#186789,#186790,#186791,
#186792,#186793,#186794,#186795,#186796,#186797,#186798,#186799,#186800,
#186801,#186802,#186803,#186804,#186805,#186806,#186807,#186808,#186809,
#186810,#186811,#186812,#186813,#186814,#186815,#186816,#186817,#186818,
#186819,#186820,#186821,#186822,#186823,#186824,#186825,#186826,#186827,
#186828,#186829,#186830,#186831,#186832,#186833,#186834,#186835),(#186836,
#186837,#186838,#186839,#186840,#186841,#186842,#186843,#186844,#186845,
#186846,#186847,#186848,#186849,#186850,#186851,#186852,#186853,#186854,
#186855,#186856,#186857,#186858,#186859,#186860,#186861,#186862,#186863,
#186864,#186865,#186866,#186867,#186868,#186869,#186870,#186871,#186872,
#186873,#186874,#186875,#186876,#186877,#186878,#186879,#186880,#186881,
#186882,#186883,#186884,#186885,#186886,#186887,#186888,#186889,#186890,
#186891,#186892,#186893,#186894,#186895,#186896,#186897,#186898,#186899,
#186900,#186901,#186902)),.UNSPECIFIED.,.F.,.F.,.F.,(4,4),(4,1,1,1,1,1,
1,1,1,1,1,1,1,1,1,1,1,1,1,1,1,1,1,1,1,1,1,1,1,1,1,1,1,1,1,1,1,1,1,1,1,1,
1,1,1,1,1,1,1,1,1,1,1,1,1,1,1,1,1,1,1,1,1,1,4),(0.,1.),(0.,0.0156250000000016,
0.031250000000001,0.0468750000000015,0.062500000000002,0.0781250000000025,
0.093750000000003,0.109375000000004,0.125000000000004,0.140625000000026,
0.156249999999973,0.171875000000027,0.187499999999974,0.203125000000028,
0.218749999999975,0.234375000000029,0.249999999999976,0.26562500000003,
0.281249999999977,0.296875000000031,0.312499999999978,0.328125000000032,
0.343749999999979,0.359375000000033,0.37499999999998,0.390625000000034,
0.406249999999981,0.421875000000035,0.437499999999982,0.453125000000036,
0.468749999999983,0.484375000000037,0.499999999999984,0.515625000000038,
0.531249999999985,0.546875000000039,0.562499999999986,0.57812500000004,
0.593749999999987,0.609375000000041,0.624999999999988,0.640625000000042,
0.656249999999989,0.671875000000043,0.68749999999999,0.703125000000044,
0.718749999999991,0.734375000000045,0.749999999999992,0.765625000000046,
0.78125,0.796875000000047,0.8125,0.828125000000048,0.84375,0.859374999999941,
0.875,0.890624999999943,0.90625,0.921874999999943,0.9375,0.953124999999945,
0.96875,0.984374999999945,1.),.UNSPECIFIED.);
#205=B_SPLINE_SURFACE_WITH_KNOTS('',3,3,((#186905,#186906,#186907,#186908,
#186909,#186910,#186911,#186912,#186913,#186914,#186915,#186916,#186917,
#186918,#186919,#186920,#186921,#186922,#186923),(#186924,#186925,#186926,
#186927,#186928,#186929,#186930,#186931,#186932,#186933,#186934,#186935,
#186936,#186937,#186938,#186939,#186940,#186941,#186942),(#186943,#186944,
#186945,#186946,#186947,#186948,#186949,#186950,#186951,#186952,#186953,
#186954,#186955,#186956,#186957,#186958,#186959,#186960,#186961),(#186962,
#186963,#186964,#186965,#186966,#186967,#186968,#186969,#186970,#186971,
#186972,#186973,#186974,#186975,#186976,#186977,#186978,#186979,#186980)),
 .UNSPECIFIED.,.F.,.F.,.F.,(4,4),(4,1,1,1,1,1,1,1,1,1,1,1,1,1,1,1,4),(0.,
1.),(0.,0.062499999999931,0.124999999999862,0.187500000000069,0.25,0.312499999999931,
0.374999999999862,0.437499999999793,0.499999999999724,0.562499999999931,
0.624999999999862,0.687499999999793,0.749999999999724,0.812499999999656,
0.874999999999587,0.937499999999793,1.),.UNSPECIFIED.);
#206=B_SPLINE_SURFACE_WITH_KNOTS('',3,3,((#186987,#186988,#186989,#186990,
#186991,#186992,#186993,#186994,#186995,#186996,#186997,#186998,#186999,
#187000,#187001,#187002,#187003,#187004,#187005),(#187006,#187007,#187008,
#187009,#187010,#187011,#187012,#187013,#187014,#187015,#187016,#187017,
#187018,#187019,#187020,#187021,#187022,#187023,#187024),(#187025,#187026,
#187027,#187028,#187029,#187030,#187031,#187032,#187033,#187034,#187035,
#187036,#187037,#187038,#187039,#187040,#187041,#187042,#187043),(#187044,
#187045,#187046,#187047,#187048,#187049,#187050,#187051,#187052,#187053,
#187054,#187055,#187056,#187057,#187058,#187059,#187060,#187061,#187062)),
 .UNSPECIFIED.,.F.,.F.,.F.,(4,4),(4,1,1,1,1,1,1,1,1,1,1,1,1,1,1,1,4),(0.,
1.),(0.,0.0625000000000641,0.125000000000129,0.18749999999985,0.249999999999914,
0.312499999999979,0.3749999999997,0.437499999999764,0.499999999999828,0.562499999999549,
0.624999999999614,0.687499999999335,0.749999999999399,0.812499999999464,
0.874999999999185,0.937499999999249,1.),.UNSPECIFIED.);
#207=B_SPLINE_SURFACE_WITH_KNOTS('',3,3,((#208963,#208964,#208965,#208966,
#208967,#208968,#208969),(#208970,#208971,#208972,#208973,#208974,#208975,
#208976),(#208977,#208978,#208979,#208980,#208981,#208982,#208983),(#208984,
#208985,#208986,#208987,#208988,#208989,#208990)),.UNSPECIFIED.,.F.,.F.,
 .F.,(4,4),(4,1,1,1,4),(0.,1.),(0.,0.25,0.5,0.75,1.),.UNSPECIFIED.);
#208=B_SPLINE_SURFACE_WITH_KNOTS('',3,3,((#209027,#209028,#209029,#209030,
#209031,#209032,#209033,#209034,#209035,#209036,#209037,#209038,#209039,
#209040,#209041,#209042,#209043,#209044,#209045,#209046,#209047,#209048,
#209049,#209050,#209051,#209052,#209053,#209054,#209055,#209056,#209057,
#209058,#209059,#209060,#209061,#209062,#209063,#209064,#209065,#209066,
#209067,#209068,#209069,#209070,#209071,#209072,#209073,#209074,#209075,
#209076,#209077,#209078,#209079,#209080,#209081,#209082,#209083,#209084,
#209085,#209086,#209087,#209088,#209089,#209090,#209091,#209092,#209093),
(#209094,#209095,#209096,#209097,#209098,#209099,#209100,#209101,#209102,
#209103,#209104,#209105,#209106,#209107,#209108,#209109,#209110,#209111,
#209112,#209113,#209114,#209115,#209116,#209117,#209118,#209119,#209120,
#209121,#209122,#209123,#209124,#209125,#209126,#209127,#209128,#209129,
#209130,#209131,#209132,#209133,#209134,#209135,#209136,#209137,#209138,
#209139,#209140,#209141,#209142,#209143,#209144,#209145,#209146,#209147,
#209148,#209149,#209150,#209151,#209152,#209153,#209154,#209155,#209156,
#209157,#209158,#209159,#209160),(#209161,#209162,#209163,#209164,#209165,
#209166,#209167,#209168,#209169,#209170,#209171,#209172,#209173,#209174,
#209175,#209176,#209177,#209178,#209179,#209180,#209181,#209182,#209183,
#209184,#209185,#209186,#209187,#209188,#209189,#209190,#209191,#209192,
#209193,#209194,#209195,#209196,#209197,#209198,#209199,#209200,#209201,
#209202,#209203,#209204,#209205,#209206,#209207,#209208,#209209,#209210,
#209211,#209212,#209213,#209214,#209215,#209216,#209217,#209218,#209219,
#209220,#209221,#209222,#209223,#209224,#209225,#209226,#209227),(#209228,
#209229,#209230,#209231,#209232,#209233,#209234,#209235,#209236,#209237,
#209238,#209239,#209240,#209241,#209242,#209243,#209244,#209245,#209246,
#209247,#209248,#209249,#209250,#209251,#209252,#209253,#209254,#209255,
#209256,#209257,#209258,#209259,#209260,#209261,#209262,#209263,#209264,
#209265,#209266,#209267,#209268,#209269,#209270,#209271,#209272,#209273,
#209274,#209275,#209276,#209277,#209278,#209279,#209280,#209281,#209282,
#209283,#209284,#209285,#209286,#209287,#209288,#209289,#209290,#209291,
#209292,#209293,#209294)),.UNSPECIFIED.,.F.,.F.,.F.,(4,4),(4,1,1,1,1,1,
1,1,1,1,1,1,1,1,1,1,1,1,1,1,1,1,1,1,1,1,1,1,1,1,1,1,1,1,1,1,1,1,1,1,1,1,
1,1,1,1,1,1,1,1,1,1,1,1,1,1,1,1,1,1,1,1,1,1,4),(0.,1.),(0.,0.0156250000000022,
0.0312500000000006,0.0468750000000009,0.0625000000000012,0.0781250000000015,
0.0937500000000018,0.109375000000002,0.124999999999983,0.140624999999983,
0.156249999999984,0.171874999999984,0.187499999999984,0.203124999999984,
0.218749999999985,0.234374999999986,0.249999999999986,0.265624999999986,
0.281249999999986,0.296874999999986,0.312499999999987,0.328124999999987,
0.343749999999987,0.359374999999987,0.374999999999988,0.390624999999988,
0.406249999999988,0.421874999999989,0.437499999999989,0.45312499999999,
0.46874999999999,0.48437499999999,0.49999999999999,0.515624999999991,0.531249999999991,
0.546874999999991,0.562499999999992,0.578124999999992,0.593749999999992,
0.609374999999993,0.624999999999993,0.640624999999993,0.65625,0.671875,
0.6875,0.703125,0.71875,0.734375,0.75,0.765625,0.78125,0.796875,0.8125,
0.828125,0.84375,0.859375,0.875,0.890625,0.90625,0.921875,0.9375,0.953125,
0.96875,0.984375,1.),.UNSPECIFIED.);
#209=B_SPLINE_SURFACE_WITH_KNOTS('',3,3,((#209336,#209337,#209338,#209339,
#209340,#209341,#209342,#209343,#209344,#209345,#209346,#209347,#209348,
#209349,#209350,#209351,#209352,#209353,#209354,#209355,#209356,#209357,
#209358,#209359,#209360,#209361,#209362,#209363,#209364,#209365,#209366,
#209367,#209368,#209369,#209370,#209371,#209372,#209373,#209374,#209375,
#209376,#209377,#209378,#209379,#209380,#209381,#209382,#209383,#209384,
#209385,#209386,#209387,#209388,#209389,#209390,#209391,#209392,#209393,
#209394,#209395,#209396,#209397,#209398,#209399,#209400,#209401,#209402),
(#209403,#209404,#209405,#209406,#209407,#209408,#209409,#209410,#209411,
#209412,#209413,#209414,#209415,#209416,#209417,#209418,#209419,#209420,
#209421,#209422,#209423,#209424,#209425,#209426,#209427,#209428,#209429,
#209430,#209431,#209432,#209433,#209434,#209435,#209436,#209437,#209438,
#209439,#209440,#209441,#209442,#209443,#209444,#209445,#209446,#209447,
#209448,#209449,#209450,#209451,#209452,#209453,#209454,#209455,#209456,
#209457,#209458,#209459,#209460,#209461,#209462,#209463,#209464,#209465,
#209466,#209467,#209468,#209469),(#209470,#209471,#209472,#209473,#209474,
#209475,#209476,#209477,#209478,#209479,#209480,#209481,#209482,#209483,
#209484,#209485,#209486,#209487,#209488,#209489,#209490,#209491,#209492,
#209493,#209494,#209495,#209496,#209497,#209498,#209499,#209500,#209501,
#209502,#209503,#209504,#209505,#209506,#209507,#209508,#209509,#209510,
#209511,#209512,#209513,#209514,#209515,#209516,#209517,#209518,#209519,
#209520,#209521,#209522,#209523,#209524,#209525,#209526,#209527,#209528,
#209529,#209530,#209531,#209532,#209533,#209534,#209535,#209536),(#209537,
#209538,#209539,#209540,#209541,#209542,#209543,#209544,#209545,#209546,
#209547,#209548,#209549,#209550,#209551,#209552,#209553,#209554,#209555,
#209556,#209557,#209558,#209559,#209560,#209561,#209562,#209563,#209564,
#209565,#209566,#209567,#209568,#209569,#209570,#209571,#209572,#209573,
#209574,#209575,#209576,#209577,#209578,#209579,#209580,#209581,#209582,
#209583,#209584,#209585,#209586,#209587,#209588,#209589,#209590,#209591,
#209592,#209593,#209594,#209595,#209596,#209597,#209598,#209599,#209600,
#209601,#209602,#209603)),.UNSPECIFIED.,.F.,.F.,.F.,(4,4),(4,1,1,1,1,1,
1,1,1,1,1,1,1,1,1,1,1,1,1,1,1,1,1,1,1,1,1,1,1,1,1,1,1,1,1,1,1,1,1,1,1,1,
1,1,1,1,1,1,1,1,1,1,1,1,1,1,1,1,1,1,1,1,1,1,4),(0.,1.),(0.,0.0156250000000031,
0.03125,0.046875,0.0625,0.078125,0.09375,0.109375,0.124999999999992,0.140624999999992,
0.156249999999992,0.171874999999992,0.187499999999992,0.203124999999992,
0.218749999999993,0.234374999999993,0.249999999999993,0.265624999999993,
0.281249999999993,0.296874999999993,0.312499999999993,0.328124999999993,
0.343749999999994,0.359374999999994,0.374999999999994,0.390624999999994,
0.406249999999994,0.421874999999994,0.437499999999994,0.453125,0.46875,
0.484375,0.5,0.515625,0.53125,0.546875,0.5625,0.578125,0.59375,0.609375,
0.625,0.640625,0.65625,0.671875,0.6875,0.703125,0.71875,0.734375,0.75,0.765625,
0.78125,0.796875,0.8125,0.828125,0.84375,0.859375,0.875,0.890625,0.90625,
0.921875,0.9375,0.953125,0.96875,0.984375,1.),.UNSPECIFIED.);
#210=B_SPLINE_SURFACE_WITH_KNOTS('',3,3,((#209610,#209611,#209612,#209613,
#209614,#209615,#209616),(#209617,#209618,#209619,#209620,#209621,#209622,
#209623),(#209624,#209625,#209626,#209627,#209628,#209629,#209630),(#209631,
#209632,#209633,#209634,#209635,#209636,#209637)),.UNSPECIFIED.,.F.,.F.,
 .F.,(4,4),(4,1,1,1,4),(0.,1.),(0.,0.250000000000029,0.500000000000019,
0.75000000000001,1.),.UNSPECIFIED.);
#211=B_SPLINE_SURFACE_WITH_KNOTS('',3,3,((#209651,#209652,#209653,#209654,
#209655,#209656,#209657),(#209658,#209659,#209660,#209661,#209662,#209663,
#209664),(#209665,#209666,#209667,#209668,#209669,#209670,#209671),(#209672,
#209673,#209674,#209675,#209676,#209677,#209678)),.UNSPECIFIED.,.F.,.F.,
 .F.,(4,4),(4,1,1,1,4),(0.,1.),(0.,0.25,0.5,0.75,1.),.UNSPECIFIED.);
#212=B_SPLINE_SURFACE_WITH_KNOTS('',3,3,((#209685,#209686,#209687,#209688,
#209689,#209690,#209691,#209692,#209693,#209694,#209695,#209696,#209697,
#209698,#209699,#209700,#209701,#209702,#209703,#209704,#209705,#209706,
#209707,#209708,#209709,#209710,#209711,#209712,#209713,#209714,#209715,
#209716,#209717,#209718,#209719,#209720,#209721,#209722,#209723,#209724,
#209725,#209726,#209727,#209728,#209729,#209730,#209731,#209732,#209733,
#209734,#209735,#209736,#209737,#209738,#209739,#209740,#209741,#209742,
#209743,#209744,#209745,#209746,#209747,#209748,#209749,#209750,#209751),
(#209752,#209753,#209754,#209755,#209756,#209757,#209758,#209759,#209760,
#209761,#209762,#209763,#209764,#209765,#209766,#209767,#209768,#209769,
#209770,#209771,#209772,#209773,#209774,#209775,#209776,#209777,#209778,
#209779,#209780,#209781,#209782,#209783,#209784,#209785,#209786,#209787,
#209788,#209789,#209790,#209791,#209792,#209793,#209794,#209795,#209796,
#209797,#209798,#209799,#209800,#209801,#209802,#209803,#209804,#209805,
#209806,#209807,#209808,#209809,#209810,#209811,#209812,#209813,#209814,
#209815,#209816,#209817,#209818),(#209819,#209820,#209821,#209822,#209823,
#209824,#209825,#209826,#209827,#209828,#209829,#209830,#209831,#209832,
#209833,#209834,#209835,#209836,#209837,#209838,#209839,#209840,#209841,
#209842,#209843,#209844,#209845,#209846,#209847,#209848,#209849,#209850,
#209851,#209852,#209853,#209854,#209855,#209856,#209857,#209858,#209859,
#209860,#209861,#209862,#209863,#209864,#209865,#209866,#209867,#209868,
#209869,#209870,#209871,#209872,#209873,#209874,#209875,#209876,#209877,
#209878,#209879,#209880,#209881,#209882,#209883,#209884,#209885),(#209886,
#209887,#209888,#209889,#209890,#209891,#209892,#209893,#209894,#209895,
#209896,#209897,#209898,#209899,#209900,#209901,#209902,#209903,#209904,
#209905,#209906,#209907,#209908,#209909,#209910,#209911,#209912,#209913,
#209914,#209915,#209916,#209917,#209918,#209919,#209920,#209921,#209922,
#209923,#209924,#209925,#209926,#209927,#209928,#209929,#209930,#209931,
#209932,#209933,#209934,#209935,#209936,#209937,#209938,#209939,#209940,
#209941,#209942,#209943,#209944,#209945,#209946,#209947,#209948,#209949,
#209950,#209951,#209952)),.UNSPECIFIED.,.F.,.F.,.F.,(4,4),(4,1,1,1,1,1,
1,1,1,1,1,1,1,1,1,1,1,1,1,1,1,1,1,1,1,1,1,1,1,1,1,1,1,1,1,1,1,1,1,1,1,1,
1,1,1,1,1,1,1,1,1,1,1,1,1,1,1,1,1,1,1,1,1,1,4),(0.,1.),(0.,0.0156250000000031,
0.03125,0.046875,0.0625,0.078125,0.09375,0.109375,0.124999999999992,0.140624999999992,
0.156249999999992,0.171874999999992,0.187499999999992,0.203124999999992,
0.218749999999993,0.234374999999993,0.249999999999993,0.265624999999993,
0.281249999999993,0.296874999999993,0.312499999999993,0.328124999999993,
0.343749999999994,0.359374999999994,0.374999999999994,0.390624999999994,
0.406249999999994,0.421874999999994,0.437499999999994,0.453125,0.46875,
0.484375,0.5,0.515625,0.53125,0.546875,0.5625,0.578125,0.59375,0.609375,
0.625,0.640625,0.65625,0.671875,0.6875,0.703125,0.71875,0.734375,0.75,0.765625,
0.78125,0.796875,0.8125,0.828125,0.84375,0.859375,0.875,0.890625,0.90625,
0.921875,0.9375,0.953125,0.96875,0.984375,1.),.UNSPECIFIED.);
#213=B_SPLINE_SURFACE_WITH_KNOTS('',3,3,((#209954,#209955,#209956,#209957,
#209958,#209959,#209960,#209961,#209962,#209963,#209964,#209965,#209966,
#209967,#209968,#209969,#209970,#209971,#209972,#209973,#209974,#209975,
#209976,#209977,#209978,#209979,#209980,#209981,#209982,#209983,#209984,
#209985,#209986,#209987,#209988,#209989,#209990,#209991,#209992,#209993,
#209994,#209995,#209996,#209997,#209998,#209999,#210000,#210001,#210002,
#210003,#210004,#210005,#210006,#210007,#210008,#210009,#210010,#210011,
#210012,#210013,#210014,#210015,#210016,#210017,#210018,#210019,#210020),
(#210021,#210022,#210023,#210024,#210025,#210026,#210027,#210028,#210029,
#210030,#210031,#210032,#210033,#210034,#210035,#210036,#210037,#210038,
#210039,#210040,#210041,#210042,#210043,#210044,#210045,#210046,#210047,
#210048,#210049,#210050,#210051,#210052,#210053,#210054,#210055,#210056,
#210057,#210058,#210059,#210060,#210061,#210062,#210063,#210064,#210065,
#210066,#210067,#210068,#210069,#210070,#210071,#210072,#210073,#210074,
#210075,#210076,#210077,#210078,#210079,#210080,#210081,#210082,#210083,
#210084,#210085,#210086,#210087),(#210088,#210089,#210090,#210091,#210092,
#210093,#210094,#210095,#210096,#210097,#210098,#210099,#210100,#210101,
#210102,#210103,#210104,#210105,#210106,#210107,#210108,#210109,#210110,
#210111,#210112,#210113,#210114,#210115,#210116,#210117,#210118,#210119,
#210120,#210121,#210122,#210123,#210124,#210125,#210126,#210127,#210128,
#210129,#210130,#210131,#210132,#210133,#210134,#210135,#210136,#210137,
#210138,#210139,#210140,#210141,#210142,#210143,#210144,#210145,#210146,
#210147,#210148,#210149,#210150,#210151,#210152,#210153,#210154),(#210155,
#210156,#210157,#210158,#210159,#210160,#210161,#210162,#210163,#210164,
#210165,#210166,#210167,#210168,#210169,#210170,#210171,#210172,#210173,
#210174,#210175,#210176,#210177,#210178,#210179,#210180,#210181,#210182,
#210183,#210184,#210185,#210186,#210187,#210188,#210189,#210190,#210191,
#210192,#210193,#210194,#210195,#210196,#210197,#210198,#210199,#210200,
#210201,#210202,#210203,#210204,#210205,#210206,#210207,#210208,#210209,
#210210,#210211,#210212,#210213,#210214,#210215,#210216,#210217,#210218,
#210219,#210220,#210221)),.UNSPECIFIED.,.F.,.F.,.F.,(4,4),(4,1,1,1,1,1,
1,1,1,1,1,1,1,1,1,1,1,1,1,1,1,1,1,1,1,1,1,1,1,1,1,1,1,1,1,1,1,1,1,1,1,1,
1,1,1,1,1,1,1,1,1,1,1,1,1,1,1,1,1,1,1,1,1,1,4),(0.,1.),(0.,0.0156250000000022,
0.0312500000000006,0.0468750000000009,0.0625000000000012,0.0781250000000015,
0.0937500000000018,0.109375000000002,0.124999999999983,0.140624999999983,
0.156249999999984,0.171874999999984,0.187499999999984,0.203124999999984,
0.218749999999985,0.234374999999986,0.249999999999986,0.265624999999986,
0.281249999999986,0.296874999999986,0.312499999999987,0.328124999999987,
0.343749999999987,0.359374999999987,0.374999999999988,0.390624999999988,
0.406249999999988,0.421874999999989,0.437499999999989,0.45312499999999,
0.46874999999999,0.48437499999999,0.49999999999999,0.515624999999991,0.531249999999991,
0.546874999999991,0.562499999999992,0.578124999999992,0.593749999999992,
0.609374999999993,0.624999999999993,0.640624999999993,0.65625,0.671875,
0.6875,0.703125,0.71875,0.734375,0.75,0.765625,0.78125,0.796875,0.8125,
0.828125,0.84375,0.859375,0.875,0.890625,0.90625,0.921875,0.9375,0.953125,
0.96875,0.984375,1.),.UNSPECIFIED.);
#214=B_SPLINE_SURFACE_WITH_KNOTS('',3,3,((#210223,#210224,#210225,#210226,
#210227,#210228,#210229,#210230,#210231,#210232,#210233,#210234,#210235,
#210236,#210237,#210238,#210239,#210240,#210241),(#210242,#210243,#210244,
#210245,#210246,#210247,#210248,#210249,#210250,#210251,#210252,#210253,
#210254,#210255,#210256,#210257,#210258,#210259,#210260),(#210261,#210262,
#210263,#210264,#210265,#210266,#210267,#210268,#210269,#210270,#210271,
#210272,#210273,#210274,#210275,#210276,#210277,#210278,#210279),(#210280,
#210281,#210282,#210283,#210284,#210285,#210286,#210287,#210288,#210289,
#210290,#210291,#210292,#210293,#210294,#210295,#210296,#210297,#210298)),
 .UNSPECIFIED.,.F.,.F.,.F.,(4,4),(4,1,1,1,1,1,1,1,1,1,1,1,1,1,1,1,4),(0.,
1.),(0.,0.0624999999999738,0.124999999999948,0.187499999999503,0.249999999999477,
0.312499999999451,0.374999999999424,0.437499999999398,0.499999999999372,
0.562499999999346,0.62499999999932,0.687499999998875,0.749999999998849,
0.812499999998822,0.874999999998796,0.93749999999877,1.),.UNSPECIFIED.);
#215=B_SPLINE_SURFACE_WITH_KNOTS('',3,3,((#210340,#210341,#210342,#210343,
#210344,#210345,#210346),(#210347,#210348,#210349,#210350,#210351,#210352,
#210353),(#210354,#210355,#210356,#210357,#210358,#210359,#210360),(#210361,
#210362,#210363,#210364,#210365,#210366,#210367)),.UNSPECIFIED.,.F.,.F.,
 .F.,(4,4),(4,1,1,1,4),(0.,1.),(0.,0.25,0.5,0.75,1.),.UNSPECIFIED.);
#216=B_SPLINE_SURFACE_WITH_KNOTS('',3,3,((#210404,#210405,#210406,#210407,
#210408,#210409,#210410,#210411,#210412,#210413,#210414,#210415,#210416,
#210417,#210418,#210419,#210420,#210421,#210422,#210423,#210424,#210425,
#210426,#210427,#210428,#210429,#210430,#210431,#210432,#210433,#210434,
#210435,#210436,#210437,#210438),(#210439,#210440,#210441,#210442,#210443,
#210444,#210445,#210446,#210447,#210448,#210449,#210450,#210451,#210452,
#210453,#210454,#210455,#210456,#210457,#210458,#210459,#210460,#210461,
#210462,#210463,#210464,#210465,#210466,#210467,#210468,#210469,#210470,
#210471,#210472,#210473),(#210474,#210475,#210476,#210477,#210478,#210479,
#210480,#210481,#210482,#210483,#210484,#210485,#210486,#210487,#210488,
#210489,#210490,#210491,#210492,#210493,#210494,#210495,#210496,#210497,
#210498,#210499,#210500,#210501,#210502,#210503,#210504,#210505,#210506,
#210507,#210508),(#210509,#210510,#210511,#210512,#210513,#210514,#210515,
#210516,#210517,#210518,#210519,#210520,#210521,#210522,#210523,#210524,
#210525,#210526,#210527,#210528,#210529,#210530,#210531,#210532,#210533,
#210534,#210535,#210536,#210537,#210538,#210539,#210540,#210541,#210542,
#210543)),.UNSPECIFIED.,.F.,.F.,.F.,(4,4),(4,1,1,1,1,1,1,1,1,1,1,1,1,1,
1,1,1,1,1,1,1,1,1,1,1,1,1,1,1,1,1,1,4),(0.,1.),(0.,0.0312500000000088,0.0625000000000175,
0.0937500000000263,0.125000000000035,0.156250000000044,0.187500000000053,
0.218750000000062,0.25000000000007,0.281250000000078,0.312500000000087,
0.343750000000096,0.375000000000105,0.406250000000114,0.437500000000123,
0.468750000000131,0.50000000000014,0.531250000000149,0.562500000000157,
0.593750000000166,0.625000000000175,0.656250000000184,0.687500000000192,
0.718750000000201,0.75000000000021,0.781250000000079,0.812500000000087,
0.843750000000096,0.875000000000105,0.906250000000114,0.937500000000122,
0.968750000000131,1.),.UNSPECIFIED.);
#217=B_SPLINE_SURFACE_WITH_KNOTS('',3,3,((#211020,#211021,#211022,#211023,
#211024,#211025,#211026,#211027,#211028,#211029,#211030,#211031,#211032,
#211033,#211034,#211035,#211036,#211037,#211038,#211039,#211040,#211041,
#211042,#211043,#211044,#211045,#211046,#211047,#211048,#211049,#211050,
#211051,#211052,#211053,#211054,#211055,#211056,#211057,#211058,#211059,
#211060,#211061,#211062,#211063,#211064,#211065,#211066,#211067,#211068,
#211069,#211070,#211071,#211072,#211073,#211074,#211075,#211076,#211077,
#211078,#211079,#211080,#211081,#211082,#211083,#211084,#211085,#211086),
(#211087,#211088,#211089,#211090,#211091,#211092,#211093,#211094,#211095,
#211096,#211097,#211098,#211099,#211100,#211101,#211102,#211103,#211104,
#211105,#211106,#211107,#211108,#211109,#211110,#211111,#211112,#211113,
#211114,#211115,#211116,#211117,#211118,#211119,#211120,#211121,#211122,
#211123,#211124,#211125,#211126,#211127,#211128,#211129,#211130,#211131,
#211132,#211133,#211134,#211135,#211136,#211137,#211138,#211139,#211140,
#211141,#211142,#211143,#211144,#211145,#211146,#211147,#211148,#211149,
#211150,#211151,#211152,#211153),(#211154,#211155,#211156,#211157,#211158,
#211159,#211160,#211161,#211162,#211163,#211164,#211165,#211166,#211167,
#211168,#211169,#211170,#211171,#211172,#211173,#211174,#211175,#211176,
#211177,#211178,#211179,#211180,#211181,#211182,#211183,#211184,#211185,
#211186,#211187,#211188,#211189,#211190,#211191,#211192,#211193,#211194,
#211195,#211196,#211197,#211198,#211199,#211200,#211201,#211202,#211203,
#211204,#211205,#211206,#211207,#211208,#211209,#211210,#211211,#211212,
#211213,#211214,#211215,#211216,#211217,#211218,#211219,#211220),(#211221,
#211222,#211223,#211224,#211225,#211226,#211227,#211228,#211229,#211230,
#211231,#211232,#211233,#211234,#211235,#211236,#211237,#211238,#211239,
#211240,#211241,#211242,#211243,#211244,#211245,#211246,#211247,#211248,
#211249,#211250,#211251,#211252,#211253,#211254,#211255,#211256,#211257,
#211258,#211259,#211260,#211261,#211262,#211263,#211264,#211265,#211266,
#211267,#211268,#211269,#211270,#211271,#211272,#211273,#211274,#211275,
#211276,#211277,#211278,#211279,#211280,#211281,#211282,#211283,#211284,
#211285,#211286,#211287)),.UNSPECIFIED.,.F.,.F.,.F.,(4,4),(4,1,1,1,1,1,
1,1,1,1,1,1,1,1,1,1,1,1,1,1,1,1,1,1,1,1,1,1,1,1,1,1,1,1,1,1,1,1,1,1,1,1,
1,1,1,1,1,1,1,1,1,1,1,1,1,1,1,1,1,1,1,1,1,1,4),(0.,1.),(0.,0.015625,0.03125,
0.046875,0.0625,0.078125,0.09375,0.109375,0.125,0.140625,0.15625,0.171875,
0.1875,0.203125,0.21875,0.234375,0.25,0.265625,0.28125,0.296875,0.3125,
0.328125,0.34375,0.359375,0.375,0.390625,0.40625,0.421875,0.4375,0.453125,
0.46875,0.484375,0.5,0.515625,0.53125,0.546875,0.5625,0.578125,0.59375,
0.609375,0.625,0.640625,0.65625,0.671875,0.6875,0.703125,0.71875,0.734375,
0.75,0.765625,0.78125,0.796875,0.8125,0.828125,0.84375,0.859375,0.875,0.890625,
0.90625,0.921875,0.9375,0.953125,0.96875,0.984375,1.),.UNSPECIFIED.);
#218=B_SPLINE_SURFACE_WITH_KNOTS('',3,3,((#211354,#211355,#211356,#211357,
#211358,#211359,#211360),(#211361,#211362,#211363,#211364,#211365,#211366,
#211367),(#211368,#211369,#211370,#211371,#211372,#211373,#211374),(#211375,
#211376,#211377,#211378,#211379,#211380,#211381)),.UNSPECIFIED.,.F.,.F.,
 .F.,(4,4),(4,1,1,1,4),(0.,1.),(0.,0.250000000000007,0.5,0.75,1.),
 .UNSPECIFIED.);
#219=B_SPLINE_SURFACE_WITH_KNOTS('',3,3,((#211409,#211410,#211411,#211412,
#211413,#211414,#211415),(#211416,#211417,#211418,#211419,#211420,#211421,
#211422),(#211423,#211424,#211425,#211426,#211427,#211428,#211429),(#211430,
#211431,#211432,#211433,#211434,#211435,#211436)),.UNSPECIFIED.,.F.,.F.,
 .F.,(4,4),(4,1,1,1,4),(0.,1.),(0.,0.25,0.5,0.75,1.),.UNSPECIFIED.);
#220=B_SPLINE_SURFACE_WITH_KNOTS('',3,3,((#211443,#211444,#211445,#211446,
#211447,#211448,#211449,#211450,#211451,#211452,#211453,#211454,#211455,
#211456,#211457,#211458,#211459,#211460,#211461,#211462,#211463,#211464,
#211465,#211466,#211467,#211468,#211469,#211470,#211471,#211472,#211473,
#211474,#211475,#211476,#211477,#211478,#211479,#211480,#211481,#211482,
#211483,#211484,#211485,#211486,#211487,#211488,#211489,#211490,#211491,
#211492,#211493,#211494,#211495,#211496,#211497,#211498,#211499,#211500,
#211501,#211502,#211503,#211504,#211505,#211506,#211507,#211508,#211509),
(#211510,#211511,#211512,#211513,#211514,#211515,#211516,#211517,#211518,
#211519,#211520,#211521,#211522,#211523,#211524,#211525,#211526,#211527,
#211528,#211529,#211530,#211531,#211532,#211533,#211534,#211535,#211536,
#211537,#211538,#211539,#211540,#211541,#211542,#211543,#211544,#211545,
#211546,#211547,#211548,#211549,#211550,#211551,#211552,#211553,#211554,
#211555,#211556,#211557,#211558,#211559,#211560,#211561,#211562,#211563,
#211564,#211565,#211566,#211567,#211568,#211569,#211570,#211571,#211572,
#211573,#211574,#211575,#211576),(#211577,#211578,#211579,#211580,#211581,
#211582,#211583,#211584,#211585,#211586,#211587,#211588,#211589,#211590,
#211591,#211592,#211593,#211594,#211595,#211596,#211597,#211598,#211599,
#211600,#211601,#211602,#211603,#211604,#211605,#211606,#211607,#211608,
#211609,#211610,#211611,#211612,#211613,#211614,#211615,#211616,#211617,
#211618,#211619,#211620,#211621,#211622,#211623,#211624,#211625,#211626,
#211627,#211628,#211629,#211630,#211631,#211632,#211633,#211634,#211635,
#211636,#211637,#211638,#211639,#211640,#211641,#211642,#211643),(#211644,
#211645,#211646,#211647,#211648,#211649,#211650,#211651,#211652,#211653,
#211654,#211655,#211656,#211657,#211658,#211659,#211660,#211661,#211662,
#211663,#211664,#211665,#211666,#211667,#211668,#211669,#211670,#211671,
#211672,#211673,#211674,#211675,#211676,#211677,#211678,#211679,#211680,
#211681,#211682,#211683,#211684,#211685,#211686,#211687,#211688,#211689,
#211690,#211691,#211692,#211693,#211694,#211695,#211696,#211697,#211698,
#211699,#211700,#211701,#211702,#211703,#211704,#211705,#211706,#211707,
#211708,#211709,#211710)),.UNSPECIFIED.,.F.,.F.,.F.,(4,4),(4,1,1,1,1,1,
1,1,1,1,1,1,1,1,1,1,1,1,1,1,1,1,1,1,1,1,1,1,1,1,1,1,1,1,1,1,1,1,1,1,1,1,
1,1,1,1,1,1,1,1,1,1,1,1,1,1,1,1,1,1,1,1,1,1,4),(0.,1.),(0.,0.015625,0.03125,
0.046875,0.0625,0.078125,0.09375,0.109375,0.125,0.140625,0.15625,0.171875,
0.1875,0.203125,0.21875,0.234375,0.25,0.265625,0.28125,0.296875,0.3125,
0.328125,0.34375,0.359375,0.375,0.390625,0.40625,0.421875,0.4375,0.453125,
0.46875,0.484375,0.5,0.515625,0.53125,0.546875,0.5625,0.578125,0.59375,
0.609375,0.625,0.640625,0.65625,0.671875,0.6875,0.703125,0.71875,0.734375,
0.75,0.765625,0.78125,0.796875,0.8125,0.828125,0.84375,0.859375,0.875,0.890625,
0.90625,0.921875,0.9375,0.953125,0.96875,0.984375,1.),.UNSPECIFIED.);
#221=B_SPLINE_SURFACE_WITH_KNOTS('',3,3,((#211790,#211791,#211792,#211793,
#211794,#211795,#211796,#211797,#211798,#211799,#211800,#211801,#211802,
#211803,#211804,#211805,#211806,#211807,#211808,#211809,#211810,#211811,
#211812,#211813,#211814,#211815,#211816,#211817,#211818,#211819,#211820,
#211821,#211822,#211823,#211824,#211825,#211826,#211827,#211828,#211829,
#211830,#211831,#211832,#211833,#211834,#211835,#211836,#211837,#211838,
#211839,#211840,#211841,#211842,#211843,#211844,#211845,#211846,#211847,
#211848,#211849,#211850,#211851,#211852,#211853,#211854,#211855,#211856),
(#211857,#211858,#211859,#211860,#211861,#211862,#211863,#211864,#211865,
#211866,#211867,#211868,#211869,#211870,#211871,#211872,#211873,#211874,
#211875,#211876,#211877,#211878,#211879,#211880,#211881,#211882,#211883,
#211884,#211885,#211886,#211887,#211888,#211889,#211890,#211891,#211892,
#211893,#211894,#211895,#211896,#211897,#211898,#211899,#211900,#211901,
#211902,#211903,#211904,#211905,#211906,#211907,#211908,#211909,#211910,
#211911,#211912,#211913,#211914,#211915,#211916,#211917,#211918,#211919,
#211920,#211921,#211922,#211923),(#211924,#211925,#211926,#211927,#211928,
#211929,#211930,#211931,#211932,#211933,#211934,#211935,#211936,#211937,
#211938,#211939,#211940,#211941,#211942,#211943,#211944,#211945,#211946,
#211947,#211948,#211949,#211950,#211951,#211952,#211953,#211954,#211955,
#211956,#211957,#211958,#211959,#211960,#211961,#211962,#211963,#211964,
#211965,#211966,#211967,#211968,#211969,#211970,#211971,#211972,#211973,
#211974,#211975,#211976,#211977,#211978,#211979,#211980,#211981,#211982,
#211983,#211984,#211985,#211986,#211987,#211988,#211989,#211990),(#211991,
#211992,#211993,#211994,#211995,#211996,#211997,#211998,#211999,#212000,
#212001,#212002,#212003,#212004,#212005,#212006,#212007,#212008,#212009,
#212010,#212011,#212012,#212013,#212014,#212015,#212016,#212017,#212018,
#212019,#212020,#212021,#212022,#212023,#212024,#212025,#212026,#212027,
#212028,#212029,#212030,#212031,#212032,#212033,#212034,#212035,#212036,
#212037,#212038,#212039,#212040,#212041,#212042,#212043,#212044,#212045,
#212046,#212047,#212048,#212049,#212050,#212051,#212052,#212053,#212054,
#212055,#212056,#212057)),.UNSPECIFIED.,.F.,.F.,.F.,(4,4),(4,1,1,1,1,1,
1,1,1,1,1,1,1,1,1,1,1,1,1,1,1,1,1,1,1,1,1,1,1,1,1,1,1,1,1,1,1,1,1,1,1,1,
1,1,1,1,1,1,1,1,1,1,1,1,1,1,1,1,1,1,1,1,1,1,4),(0.,1.),(0.,0.015625,0.03125,
0.046875,0.0625,0.078125,0.09375,0.109375,0.125,0.140625,0.15625,0.171875,
0.1875,0.203125,0.21875,0.234375,0.25,0.265625,0.28125,0.296875,0.3125,
0.328125,0.34375,0.359375,0.375,0.390625,0.40625,0.421875,0.4375,0.453125,
0.46875,0.484375,0.5,0.515625,0.53125,0.546875,0.5625,0.578125,0.59375,
0.609375,0.625,0.640625,0.65625,0.671875,0.6875,0.703125,0.71875,0.734375,
0.75,0.765625,0.78125,0.796875,0.8125,0.828125,0.84375,0.859375,0.875,0.890625,
0.90625,0.921875,0.9375,0.953125,0.96875,0.984375,1.),.UNSPECIFIED.);
#222=B_SPLINE_SURFACE_WITH_KNOTS('',3,3,((#212059,#212060,#212061,#212062,
#212063,#212064,#212065,#212066,#212067,#212068,#212069,#212070,#212071,
#212072,#212073,#212074,#212075,#212076,#212077,#212078,#212079,#212080,
#212081,#212082,#212083,#212084,#212085,#212086,#212087,#212088,#212089,
#212090,#212091,#212092,#212093),(#212094,#212095,#212096,#212097,#212098,
#212099,#212100,#212101,#212102,#212103,#212104,#212105,#212106,#212107,
#212108,#212109,#212110,#212111,#212112,#212113,#212114,#212115,#212116,
#212117,#212118,#212119,#212120,#212121,#212122,#212123,#212124,#212125,
#212126,#212127,#212128),(#212129,#212130,#212131,#212132,#212133,#212134,
#212135,#212136,#212137,#212138,#212139,#212140,#212141,#212142,#212143,
#212144,#212145,#212146,#212147,#212148,#212149,#212150,#212151,#212152,
#212153,#212154,#212155,#212156,#212157,#212158,#212159,#212160,#212161,
#212162,#212163),(#212164,#212165,#212166,#212167,#212168,#212169,#212170,
#212171,#212172,#212173,#212174,#212175,#212176,#212177,#212178,#212179,
#212180,#212181,#212182,#212183,#212184,#212185,#212186,#212187,#212188,
#212189,#212190,#212191,#212192,#212193,#212194,#212195,#212196,#212197,
#212198)),.UNSPECIFIED.,.F.,.F.,.F.,(4,4),(4,1,1,1,1,1,1,1,1,1,1,1,1,1,
1,1,1,1,1,1,1,1,1,1,1,1,1,1,1,1,1,1,4),(0.,1.),(0.,0.0312499999999743,0.0624999999999486,
0.0937499999999229,0.125000000000034,0.156250000000008,0.187499999999983,
0.218749999999957,0.249999999999932,0.281250000000043,0.312500000000017,
0.343749999999991,0.374999999999966,0.406250000000077,0.437500000000052,
0.468750000000026,0.5,0.531249999999974,0.562500000000086,0.59375000000006,
0.625000000000034,0.656250000000009,0.687499999999983,0.718750000000095,
0.750000000000069,0.781250000000043,0.812500000000017,0.843750000000129,
0.875000000000103,0.906250000000077,0.937500000000052,0.968750000000026,
1.),.UNSPECIFIED.);
#223=B_SPLINE_SURFACE_WITH_KNOTS('',3,3,((#212211,#212212,#212213,#212214,
#212215,#212216,#212217,#212218,#212219,#212220,#212221,#212222,#212223,
#212224,#212225,#212226,#212227,#212228,#212229,#212230,#212231,#212232,
#212233,#212234,#212235,#212236,#212237,#212238,#212239,#212240,#212241,
#212242,#212243,#212244,#212245,#212246,#212247,#212248,#212249,#212250,
#212251,#212252,#212253,#212254,#212255,#212256,#212257,#212258,#212259,
#212260,#212261,#212262,#212263,#212264,#212265,#212266,#212267,#212268,
#212269,#212270,#212271,#212272,#212273,#212274,#212275,#212276,#212277),
(#212278,#212279,#212280,#212281,#212282,#212283,#212284,#212285,#212286,
#212287,#212288,#212289,#212290,#212291,#212292,#212293,#212294,#212295,
#212296,#212297,#212298,#212299,#212300,#212301,#212302,#212303,#212304,
#212305,#212306,#212307,#212308,#212309,#212310,#212311,#212312,#212313,
#212314,#212315,#212316,#212317,#212318,#212319,#212320,#212321,#212322,
#212323,#212324,#212325,#212326,#212327,#212328,#212329,#212330,#212331,
#212332,#212333,#212334,#212335,#212336,#212337,#212338,#212339,#212340,
#212341,#212342,#212343,#212344),(#212345,#212346,#212347,#212348,#212349,
#212350,#212351,#212352,#212353,#212354,#212355,#212356,#212357,#212358,
#212359,#212360,#212361,#212362,#212363,#212364,#212365,#212366,#212367,
#212368,#212369,#212370,#212371,#212372,#212373,#212374,#212375,#212376,
#212377,#212378,#212379,#212380,#212381,#212382,#212383,#212384,#212385,
#212386,#212387,#212388,#212389,#212390,#212391,#212392,#212393,#212394,
#212395,#212396,#212397,#212398,#212399,#212400,#212401,#212402,#212403,
#212404,#212405,#212406,#212407,#212408,#212409,#212410,#212411),(#212412,
#212413,#212414,#212415,#212416,#212417,#212418,#212419,#212420,#212421,
#212422,#212423,#212424,#212425,#212426,#212427,#212428,#212429,#212430,
#212431,#212432,#212433,#212434,#212435,#212436,#212437,#212438,#212439,
#212440,#212441,#212442,#212443,#212444,#212445,#212446,#212447,#212448,
#212449,#212450,#212451,#212452,#212453,#212454,#212455,#212456,#212457,
#212458,#212459,#212460,#212461,#212462,#212463,#212464,#212465,#212466,
#212467,#212468,#212469,#212470,#212471,#212472,#212473,#212474,#212475,
#212476,#212477,#212478)),.UNSPECIFIED.,.F.,.F.,.F.,(4,4),(4,1,1,1,1,1,
1,1,1,1,1,1,1,1,1,1,1,1,1,1,1,1,1,1,1,1,1,1,1,1,1,1,1,1,1,1,1,1,1,1,1,1,
1,1,1,1,1,1,1,1,1,1,1,1,1,1,1,1,1,1,1,1,1,1,4),(0.,1.),(0.,0.015625,0.03125,
0.046875,0.0625,0.078125,0.09375,0.109375,0.125,0.140625,0.15625,0.171875,
0.1875,0.203125,0.21875,0.234375,0.25,0.265625,0.28125,0.296875,0.3125,
0.328125,0.34375,0.359375,0.375,0.390625,0.40625,0.421875,0.4375,0.453125,
0.46875,0.484375,0.5,0.515625,0.53125,0.546875,0.5625,0.578125,0.59375,
0.609375,0.625,0.640625,0.65625,0.671875,0.6875,0.703125,0.71875,0.734375,
0.75,0.765625,0.78125,0.796875,0.8125,0.828125,0.84375,0.859375,0.875,0.890625,
0.90625,0.921875,0.9375,0.953125,0.96875,0.984375,1.),.UNSPECIFIED.);
#224=B_SPLINE_SURFACE_WITH_KNOTS('',3,3,((#212480,#212481,#212482,#212483,
#212484,#212485,#212486,#212487,#212488,#212489,#212490,#212491,#212492,
#212493,#212494,#212495,#212496,#212497,#212498,#212499,#212500,#212501,
#212502,#212503,#212504,#212505,#212506,#212507,#212508,#212509,#212510,
#212511,#212512,#212513,#212514),(#212515,#212516,#212517,#212518,#212519,
#212520,#212521,#212522,#212523,#212524,#212525,#212526,#212527,#212528,
#212529,#212530,#212531,#212532,#212533,#212534,#212535,#212536,#212537,
#212538,#212539,#212540,#212541,#212542,#212543,#212544,#212545,#212546,
#212547,#212548,#212549),(#212550,#212551,#212552,#212553,#212554,#212555,
#212556,#212557,#212558,#212559,#212560,#212561,#212562,#212563,#212564,
#212565,#212566,#212567,#212568,#212569,#212570,#212571,#212572,#212573,
#212574,#212575,#212576,#212577,#212578,#212579,#212580,#212581,#212582,
#212583,#212584),(#212585,#212586,#212587,#212588,#212589,#212590,#212591,
#212592,#212593,#212594,#212595,#212596,#212597,#212598,#212599,#212600,
#212601,#212602,#212603,#212604,#212605,#212606,#212607,#212608,#212609,
#212610,#212611,#212612,#212613,#212614,#212615,#212616,#212617,#212618,
#212619)),.UNSPECIFIED.,.F.,.F.,.F.,(4,4),(4,1,1,1,1,1,1,1,1,1,1,1,1,1,
1,1,1,1,1,1,1,1,1,1,1,1,1,1,1,1,1,1,4),(0.,1.),(0.,0.031249999999901,0.0624999999999529,
0.0937500000000048,0.125000000000057,0.156250000000109,0.187500000000009,
0.218750000000062,0.250000000000113,0.281250000000165,0.312500000000066,
0.343750000000118,0.37500000000017,0.406250000000221,0.437500000000123,
0.468750000000175,0.500000000000226,0.531250000000278,0.562500000000179,
0.593750000000231,0.625000000000283,0.656250000000335,0.687500000000236,
0.718750000000288,0.75000000000034,0.781250000000392,0.812500000000292,
0.843750000000344,0.875000000000396,0.906250000000448,0.937500000000349,
0.968750000000401,1.),.UNSPECIFIED.);
#225=B_SPLINE_SURFACE_WITH_KNOTS('',3,3,((#212696,#212697,#212698,#212699,
#212700,#212701,#212702,#212703,#212704,#212705,#212706,#212707,#212708,
#212709,#212710,#212711,#212712,#212713,#212714),(#212715,#212716,#212717,
#212718,#212719,#212720,#212721,#212722,#212723,#212724,#212725,#212726,
#212727,#212728,#212729,#212730,#212731,#212732,#212733),(#212734,#212735,
#212736,#212737,#212738,#212739,#212740,#212741,#212742,#212743,#212744,
#212745,#212746,#212747,#212748,#212749,#212750,#212751,#212752),(#212753,
#212754,#212755,#212756,#212757,#212758,#212759,#212760,#212761,#212762,
#212763,#212764,#212765,#212766,#212767,#212768,#212769,#212770,#212771)),
 .UNSPECIFIED.,.F.,.F.,.F.,(4,4),(4,1,1,1,1,1,1,1,1,1,1,1,1,1,1,1,4),(0.,
1.),(0.,0.0625,0.124999999999643,0.187499999999643,0.249999999999643,0.312499999999286,
0.374999999999286,0.437499999999286,0.499999999999286,0.562499999998929,
0.624999999998929,0.687499999998929,0.749999999998572,0.812499999998572,
0.874999999998572,0.937499999998572,1.),.UNSPECIFIED.);
#226=B_SPLINE_SURFACE_WITH_KNOTS('',3,3,((#217794,#217795,#217796,#217797,
#217798,#217799,#217800),(#217801,#217802,#217803,#217804,#217805,#217806,
#217807),(#217808,#217809,#217810,#217811,#217812,#217813,#217814),(#217815,
#217816,#217817,#217818,#217819,#217820,#217821)),.UNSPECIFIED.,.F.,.F.,
 .F.,(4,4),(4,1,1,1,4),(0.,1.),(0.,0.25,0.5,0.75,1.),.UNSPECIFIED.);
#227=B_SPLINE_SURFACE_WITH_KNOTS('',3,3,((#217858,#217859,#217860,#217861,
#217862,#217863,#217864,#217865,#217866,#217867,#217868,#217869,#217870,
#217871,#217872,#217873,#217874,#217875,#217876,#217877,#217878,#217879,
#217880,#217881,#217882,#217883,#217884,#217885,#217886,#217887,#217888,
#217889,#217890,#217891,#217892,#217893,#217894,#217895,#217896,#217897,
#217898,#217899,#217900,#217901,#217902,#217903,#217904,#217905,#217906,
#217907,#217908,#217909,#217910,#217911,#217912,#217913,#217914,#217915,
#217916,#217917,#217918,#217919,#217920,#217921,#217922,#217923,#217924),
(#217925,#217926,#217927,#217928,#217929,#217930,#217931,#217932,#217933,
#217934,#217935,#217936,#217937,#217938,#217939,#217940,#217941,#217942,
#217943,#217944,#217945,#217946,#217947,#217948,#217949,#217950,#217951,
#217952,#217953,#217954,#217955,#217956,#217957,#217958,#217959,#217960,
#217961,#217962,#217963,#217964,#217965,#217966,#217967,#217968,#217969,
#217970,#217971,#217972,#217973,#217974,#217975,#217976,#217977,#217978,
#217979,#217980,#217981,#217982,#217983,#217984,#217985,#217986,#217987,
#217988,#217989,#217990,#217991),(#217992,#217993,#217994,#217995,#217996,
#217997,#217998,#217999,#218000,#218001,#218002,#218003,#218004,#218005,
#218006,#218007,#218008,#218009,#218010,#218011,#218012,#218013,#218014,
#218015,#218016,#218017,#218018,#218019,#218020,#218021,#218022,#218023,
#218024,#218025,#218026,#218027,#218028,#218029,#218030,#218031,#218032,
#218033,#218034,#218035,#218036,#218037,#218038,#218039,#218040,#218041,
#218042,#218043,#218044,#218045,#218046,#218047,#218048,#218049,#218050,
#218051,#218052,#218053,#218054,#218055,#218056,#218057,#218058),(#218059,
#218060,#218061,#218062,#218063,#218064,#218065,#218066,#218067,#218068,
#218069,#218070,#218071,#218072,#218073,#218074,#218075,#218076,#218077,
#218078,#218079,#218080,#218081,#218082,#218083,#218084,#218085,#218086,
#218087,#218088,#218089,#218090,#218091,#218092,#218093,#218094,#218095,
#218096,#218097,#218098,#218099,#218100,#218101,#218102,#218103,#218104,
#218105,#218106,#218107,#218108,#218109,#218110,#218111,#218112,#218113,
#218114,#218115,#218116,#218117,#218118,#218119,#218120,#218121,#218122,
#218123,#218124,#218125)),.UNSPECIFIED.,.F.,.F.,.F.,(4,4),(4,1,1,1,1,1,
1,1,1,1,1,1,1,1,1,1,1,1,1,1,1,1,1,1,1,1,1,1,1,1,1,1,1,1,1,1,1,1,1,1,1,1,
1,1,1,1,1,1,1,1,1,1,1,1,1,1,1,1,1,1,1,1,1,1,4),(0.,1.),(0.,0.0156250000000022,
0.0312500000000006,0.0468750000000009,0.0625000000000012,0.0781250000000015,
0.0937500000000018,0.109375000000002,0.124999999999983,0.140624999999983,
0.156249999999984,0.171874999999984,0.187499999999984,0.203124999999984,
0.218749999999985,0.234374999999986,0.249999999999986,0.265624999999986,
0.281249999999986,0.296874999999986,0.312499999999987,0.328124999999987,
0.343749999999987,0.359374999999987,0.374999999999988,0.390624999999988,
0.406249999999988,0.421874999999989,0.437499999999989,0.45312499999999,
0.46874999999999,0.48437499999999,0.49999999999999,0.515624999999991,0.531249999999991,
0.546874999999991,0.562499999999992,0.578124999999992,0.593749999999992,
0.609374999999993,0.624999999999993,0.640624999999993,0.65625,0.671875,
0.6875,0.703125,0.71875,0.734375,0.75,0.765625,0.78125,0.796875,0.8125,
0.828125,0.84375,0.859375,0.875,0.890625,0.90625,0.921875,0.9375,0.953125,
0.96875,0.984375,1.),.UNSPECIFIED.);
#228=B_SPLINE_SURFACE_WITH_KNOTS('',3,3,((#218167,#218168,#218169,#218170,
#218171,#218172,#218173,#218174,#218175,#218176,#218177,#218178,#218179,
#218180,#218181,#218182,#218183,#218184,#218185,#218186,#218187,#218188,
#218189,#218190,#218191,#218192,#218193,#218194,#218195,#218196,#218197,
#218198,#218199,#218200,#218201,#218202,#218203,#218204,#218205,#218206,
#218207,#218208,#218209,#218210,#218211,#218212,#218213,#218214,#218215,
#218216,#218217,#218218,#218219,#218220,#218221,#218222,#218223,#218224,
#218225,#218226,#218227,#218228,#218229,#218230,#218231,#218232,#218233),
(#218234,#218235,#218236,#218237,#218238,#218239,#218240,#218241,#218242,
#218243,#218244,#218245,#218246,#218247,#218248,#218249,#218250,#218251,
#218252,#218253,#218254,#218255,#218256,#218257,#218258,#218259,#218260,
#218261,#218262,#218263,#218264,#218265,#218266,#218267,#218268,#218269,
#218270,#218271,#218272,#218273,#218274,#218275,#218276,#218277,#218278,
#218279,#218280,#218281,#218282,#218283,#218284,#218285,#218286,#218287,
#218288,#218289,#218290,#218291,#218292,#218293,#218294,#218295,#218296,
#218297,#218298,#218299,#218300),(#218301,#218302,#218303,#218304,#218305,
#218306,#218307,#218308,#218309,#218310,#218311,#218312,#218313,#218314,
#218315,#218316,#218317,#218318,#218319,#218320,#218321,#218322,#218323,
#218324,#218325,#218326,#218327,#218328,#218329,#218330,#218331,#218332,
#218333,#218334,#218335,#218336,#218337,#218338,#218339,#218340,#218341,
#218342,#218343,#218344,#218345,#218346,#218347,#218348,#218349,#218350,
#218351,#218352,#218353,#218354,#218355,#218356,#218357,#218358,#218359,
#218360,#218361,#218362,#218363,#218364,#218365,#218366,#218367),(#218368,
#218369,#218370,#218371,#218372,#218373,#218374,#218375,#218376,#218377,
#218378,#218379,#218380,#218381,#218382,#218383,#218384,#218385,#218386,
#218387,#218388,#218389,#218390,#218391,#218392,#218393,#218394,#218395,
#218396,#218397,#218398,#218399,#218400,#218401,#218402,#218403,#218404,
#218405,#218406,#218407,#218408,#218409,#218410,#218411,#218412,#218413,
#218414,#218415,#218416,#218417,#218418,#218419,#218420,#218421,#218422,
#218423,#218424,#218425,#218426,#218427,#218428,#218429,#218430,#218431,
#218432,#218433,#218434)),.UNSPECIFIED.,.F.,.F.,.F.,(4,4),(4,1,1,1,1,1,
1,1,1,1,1,1,1,1,1,1,1,1,1,1,1,1,1,1,1,1,1,1,1,1,1,1,1,1,1,1,1,1,1,1,1,1,
1,1,1,1,1,1,1,1,1,1,1,1,1,1,1,1,1,1,1,1,1,1,4),(0.,1.),(0.,0.0156250000000031,
0.03125,0.046875,0.0625,0.078125,0.09375,0.109375,0.124999999999992,0.140624999999992,
0.156249999999992,0.171874999999992,0.187499999999992,0.203124999999992,
0.218749999999993,0.234374999999993,0.249999999999993,0.265624999999993,
0.281249999999993,0.296874999999993,0.312499999999993,0.328124999999993,
0.343749999999994,0.359374999999994,0.374999999999994,0.390624999999994,
0.406249999999994,0.421874999999994,0.437499999999994,0.453125,0.46875,
0.484375,0.5,0.515625,0.53125,0.546875,0.5625,0.578125,0.59375,0.609375,
0.625,0.640625,0.65625,0.671875,0.6875,0.703125,0.71875,0.734375,0.75,0.765625,
0.78125,0.796875,0.8125,0.828125,0.84375,0.859375,0.875,0.890625,0.90625,
0.921875,0.9375,0.953125,0.96875,0.984375,1.),.UNSPECIFIED.);
#229=B_SPLINE_SURFACE_WITH_KNOTS('',3,3,((#218441,#218442,#218443,#218444,
#218445,#218446,#218447),(#218448,#218449,#218450,#218451,#218452,#218453,
#218454),(#218455,#218456,#218457,#218458,#218459,#218460,#218461),(#218462,
#218463,#218464,#218465,#218466,#218467,#218468)),.UNSPECIFIED.,.F.,.F.,
 .F.,(4,4),(4,1,1,1,4),(0.,1.),(0.,0.250000000000029,0.500000000000019,
0.75000000000001,1.),.UNSPECIFIED.);
#230=B_SPLINE_SURFACE_WITH_KNOTS('',3,3,((#218482,#218483,#218484,#218485,
#218486,#218487,#218488),(#218489,#218490,#218491,#218492,#218493,#218494,
#218495),(#218496,#218497,#218498,#218499,#218500,#218501,#218502),(#218503,
#218504,#218505,#218506,#218507,#218508,#218509)),.UNSPECIFIED.,.F.,.F.,
 .F.,(4,4),(4,1,1,1,4),(0.,1.),(0.,0.25,0.5,0.75,1.),.UNSPECIFIED.);
#231=B_SPLINE_SURFACE_WITH_KNOTS('',3,3,((#218516,#218517,#218518,#218519,
#218520,#218521,#218522,#218523,#218524,#218525,#218526,#218527,#218528,
#218529,#218530,#218531,#218532,#218533,#218534,#218535,#218536,#218537,
#218538,#218539,#218540,#218541,#218542,#218543,#218544,#218545,#218546,
#218547,#218548,#218549,#218550,#218551,#218552,#218553,#218554,#218555,
#218556,#218557,#218558,#218559,#218560,#218561,#218562,#218563,#218564,
#218565,#218566,#218567,#218568,#218569,#218570,#218571,#218572,#218573,
#218574,#218575,#218576,#218577,#218578,#218579,#218580,#218581,#218582),
(#218583,#218584,#218585,#218586,#218587,#218588,#218589,#218590,#218591,
#218592,#218593,#218594,#218595,#218596,#218597,#218598,#218599,#218600,
#218601,#218602,#218603,#218604,#218605,#218606,#218607,#218608,#218609,
#218610,#218611,#218612,#218613,#218614,#218615,#218616,#218617,#218618,
#218619,#218620,#218621,#218622,#218623,#218624,#218625,#218626,#218627,
#218628,#218629,#218630,#218631,#218632,#218633,#218634,#218635,#218636,
#218637,#218638,#218639,#218640,#218641,#218642,#218643,#218644,#218645,
#218646,#218647,#218648,#218649),(#218650,#218651,#218652,#218653,#218654,
#218655,#218656,#218657,#218658,#218659,#218660,#218661,#218662,#218663,
#218664,#218665,#218666,#218667,#218668,#218669,#218670,#218671,#218672,
#218673,#218674,#218675,#218676,#218677,#218678,#218679,#218680,#218681,
#218682,#218683,#218684,#218685,#218686,#218687,#218688,#218689,#218690,
#218691,#218692,#218693,#218694,#218695,#218696,#218697,#218698,#218699,
#218700,#218701,#218702,#218703,#218704,#218705,#218706,#218707,#218708,
#218709,#218710,#218711,#218712,#218713,#218714,#218715,#218716),(#218717,
#218718,#218719,#218720,#218721,#218722,#218723,#218724,#218725,#218726,
#218727,#218728,#218729,#218730,#218731,#218732,#218733,#218734,#218735,
#218736,#218737,#218738,#218739,#218740,#218741,#218742,#218743,#218744,
#218745,#218746,#218747,#218748,#218749,#218750,#218751,#218752,#218753,
#218754,#218755,#218756,#218757,#218758,#218759,#218760,#218761,#218762,
#218763,#218764,#218765,#218766,#218767,#218768,#218769,#218770,#218771,
#218772,#218773,#218774,#218775,#218776,#218777,#218778,#218779,#218780,
#218781,#218782,#218783)),.UNSPECIFIED.,.F.,.F.,.F.,(4,4),(4,1,1,1,1,1,
1,1,1,1,1,1,1,1,1,1,1,1,1,1,1,1,1,1,1,1,1,1,1,1,1,1,1,1,1,1,1,1,1,1,1,1,
1,1,1,1,1,1,1,1,1,1,1,1,1,1,1,1,1,1,1,1,1,1,4),(0.,1.),(0.,0.0156250000000031,
0.03125,0.046875,0.0625,0.078125,0.09375,0.109375,0.124999999999992,0.140624999999992,
0.156249999999992,0.171874999999992,0.187499999999992,0.203124999999992,
0.218749999999993,0.234374999999993,0.249999999999993,0.265624999999993,
0.281249999999993,0.296874999999993,0.312499999999993,0.328124999999993,
0.343749999999994,0.359374999999994,0.374999999999994,0.390624999999994,
0.406249999999994,0.421874999999994,0.437499999999994,0.453125,0.46875,
0.484375,0.5,0.515625,0.53125,0.546875,0.5625,0.578125,0.59375,0.609375,
0.625,0.640625,0.65625,0.671875,0.6875,0.703125,0.71875,0.734375,0.75,0.765625,
0.78125,0.796875,0.8125,0.828125,0.84375,0.859375,0.875,0.890625,0.90625,
0.921875,0.9375,0.953125,0.96875,0.984375,1.),.UNSPECIFIED.);
#232=B_SPLINE_SURFACE_WITH_KNOTS('',3,3,((#218785,#218786,#218787,#218788,
#218789,#218790,#218791,#218792,#218793,#218794,#218795,#218796,#218797,
#218798,#218799,#218800,#218801,#218802,#218803,#218804,#218805,#218806,
#218807,#218808,#218809,#218810,#218811,#218812,#218813,#218814,#218815,
#218816,#218817,#218818,#218819,#218820,#218821,#218822,#218823,#218824,
#218825,#218826,#218827,#218828,#218829,#218830,#218831,#218832,#218833,
#218834,#218835,#218836,#218837,#218838,#218839,#218840,#218841,#218842,
#218843,#218844,#218845,#218846,#218847,#218848,#218849,#218850,#218851),
(#218852,#218853,#218854,#218855,#218856,#218857,#218858,#218859,#218860,
#218861,#218862,#218863,#218864,#218865,#218866,#218867,#218868,#218869,
#218870,#218871,#218872,#218873,#218874,#218875,#218876,#218877,#218878,
#218879,#218880,#218881,#218882,#218883,#218884,#218885,#218886,#218887,
#218888,#218889,#218890,#218891,#218892,#218893,#218894,#218895,#218896,
#218897,#218898,#218899,#218900,#218901,#218902,#218903,#218904,#218905,
#218906,#218907,#218908,#218909,#218910,#218911,#218912,#218913,#218914,
#218915,#218916,#218917,#218918),(#218919,#218920,#218921,#218922,#218923,
#218924,#218925,#218926,#218927,#218928,#218929,#218930,#218931,#218932,
#218933,#218934,#218935,#218936,#218937,#218938,#218939,#218940,#218941,
#218942,#218943,#218944,#218945,#218946,#218947,#218948,#218949,#218950,
#218951,#218952,#218953,#218954,#218955,#218956,#218957,#218958,#218959,
#218960,#218961,#218962,#218963,#218964,#218965,#218966,#218967,#218968,
#218969,#218970,#218971,#218972,#218973,#218974,#218975,#218976,#218977,
#218978,#218979,#218980,#218981,#218982,#218983,#218984,#218985),(#218986,
#218987,#218988,#218989,#218990,#218991,#218992,#218993,#218994,#218995,
#218996,#218997,#218998,#218999,#219000,#219001,#219002,#219003,#219004,
#219005,#219006,#219007,#219008,#219009,#219010,#219011,#219012,#219013,
#219014,#219015,#219016,#219017,#219018,#219019,#219020,#219021,#219022,
#219023,#219024,#219025,#219026,#219027,#219028,#219029,#219030,#219031,
#219032,#219033,#219034,#219035,#219036,#219037,#219038,#219039,#219040,
#219041,#219042,#219043,#219044,#219045,#219046,#219047,#219048,#219049,
#219050,#219051,#219052)),.UNSPECIFIED.,.F.,.F.,.F.,(4,4),(4,1,1,1,1,1,
1,1,1,1,1,1,1,1,1,1,1,1,1,1,1,1,1,1,1,1,1,1,1,1,1,1,1,1,1,1,1,1,1,1,1,1,
1,1,1,1,1,1,1,1,1,1,1,1,1,1,1,1,1,1,1,1,1,1,4),(0.,1.),(0.,0.0156250000000022,
0.0312500000000006,0.0468750000000009,0.0625000000000012,0.0781250000000015,
0.0937500000000018,0.109375000000002,0.124999999999983,0.140624999999983,
0.156249999999984,0.171874999999984,0.187499999999984,0.203124999999984,
0.218749999999985,0.234374999999986,0.249999999999986,0.265624999999986,
0.281249999999986,0.296874999999986,0.312499999999987,0.328124999999987,
0.343749999999987,0.359374999999987,0.374999999999988,0.390624999999988,
0.406249999999988,0.421874999999989,0.437499999999989,0.45312499999999,
0.46874999999999,0.48437499999999,0.49999999999999,0.515624999999991,0.531249999999991,
0.546874999999991,0.562499999999992,0.578124999999992,0.593749999999992,
0.609374999999993,0.624999999999993,0.640624999999993,0.65625,0.671875,
0.6875,0.703125,0.71875,0.734375,0.75,0.765625,0.78125,0.796875,0.8125,
0.828125,0.84375,0.859375,0.875,0.890625,0.90625,0.921875,0.9375,0.953125,
0.96875,0.984375,1.),.UNSPECIFIED.);
#233=B_SPLINE_SURFACE_WITH_KNOTS('',3,3,((#219054,#219055,#219056,#219057,
#219058,#219059,#219060,#219061,#219062,#219063,#219064,#219065,#219066,
#219067,#219068,#219069,#219070,#219071,#219072),(#219073,#219074,#219075,
#219076,#219077,#219078,#219079,#219080,#219081,#219082,#219083,#219084,
#219085,#219086,#219087,#219088,#219089,#219090,#219091),(#219092,#219093,
#219094,#219095,#219096,#219097,#219098,#219099,#219100,#219101,#219102,
#219103,#219104,#219105,#219106,#219107,#219108,#219109,#219110),(#219111,
#219112,#219113,#219114,#219115,#219116,#219117,#219118,#219119,#219120,
#219121,#219122,#219123,#219124,#219125,#219126,#219127,#219128,#219129)),
 .UNSPECIFIED.,.F.,.F.,.F.,(4,4),(4,1,1,1,1,1,1,1,1,1,1,1,1,1,1,1,4),(0.,
1.),(0.,0.0624999999999738,0.124999999999948,0.187499999999503,0.249999999999477,
0.312499999999451,0.374999999999424,0.437499999999398,0.499999999999372,
0.562499999999346,0.62499999999932,0.687499999998875,0.749999999998849,
0.812499999998822,0.874999999998796,0.93749999999877,1.),.UNSPECIFIED.);
#234=B_SPLINE_SURFACE_WITH_KNOTS('',3,3,((#219171,#219172,#219173,#219174,
#219175,#219176,#219177),(#219178,#219179,#219180,#219181,#219182,#219183,
#219184),(#219185,#219186,#219187,#219188,#219189,#219190,#219191),(#219192,
#219193,#219194,#219195,#219196,#219197,#219198)),.UNSPECIFIED.,.F.,.F.,
 .F.,(4,4),(4,1,1,1,4),(0.,1.),(0.,0.25,0.5,0.75,1.),.UNSPECIFIED.);
#235=B_SPLINE_SURFACE_WITH_KNOTS('',3,3,((#219235,#219236,#219237,#219238,
#219239,#219240,#219241,#219242,#219243,#219244,#219245,#219246,#219247,
#219248,#219249,#219250,#219251,#219252,#219253,#219254,#219255,#219256,
#219257,#219258,#219259,#219260,#219261,#219262,#219263,#219264,#219265,
#219266,#219267,#219268,#219269),(#219270,#219271,#219272,#219273,#219274,
#219275,#219276,#219277,#219278,#219279,#219280,#219281,#219282,#219283,
#219284,#219285,#219286,#219287,#219288,#219289,#219290,#219291,#219292,
#219293,#219294,#219295,#219296,#219297,#219298,#219299,#219300,#219301,
#219302,#219303,#219304),(#219305,#219306,#219307,#219308,#219309,#219310,
#219311,#219312,#219313,#219314,#219315,#219316,#219317,#219318,#219319,
#219320,#219321,#219322,#219323,#219324,#219325,#219326,#219327,#219328,
#219329,#219330,#219331,#219332,#219333,#219334,#219335,#219336,#219337,
#219338,#219339),(#219340,#219341,#219342,#219343,#219344,#219345,#219346,
#219347,#219348,#219349,#219350,#219351,#219352,#219353,#219354,#219355,
#219356,#219357,#219358,#219359,#219360,#219361,#219362,#219363,#219364,
#219365,#219366,#219367,#219368,#219369,#219370,#219371,#219372,#219373,
#219374)),.UNSPECIFIED.,.F.,.F.,.F.,(4,4),(4,1,1,1,1,1,1,1,1,1,1,1,1,1,
1,1,1,1,1,1,1,1,1,1,1,1,1,1,1,1,1,1,4),(0.,1.),(0.,0.0312500000000088,0.0625000000000175,
0.0937500000000263,0.125000000000035,0.156250000000044,0.187500000000053,
0.218750000000062,0.25000000000007,0.281250000000078,0.312500000000087,
0.343750000000096,0.375000000000105,0.406250000000114,0.437500000000123,
0.468750000000131,0.50000000000014,0.531250000000149,0.562500000000157,
0.593750000000166,0.625000000000175,0.656250000000184,0.687500000000192,
0.718750000000201,0.75000000000021,0.781250000000079,0.812500000000087,
0.843750000000096,0.875000000000105,0.906250000000114,0.937500000000122,
0.968750000000131,1.),.UNSPECIFIED.);
#236=B_SPLINE_SURFACE_WITH_KNOTS('',3,3,((#219849,#219850,#219851,#219852,
#219853,#219854,#219855,#219856,#219857,#219858,#219859,#219860,#219861,
#219862,#219863,#219864,#219865,#219866,#219867,#219868,#219869,#219870,
#219871,#219872,#219873,#219874,#219875,#219876,#219877,#219878,#219879,
#219880,#219881,#219882,#219883,#219884,#219885,#219886,#219887,#219888,
#219889,#219890,#219891,#219892,#219893,#219894,#219895,#219896,#219897,
#219898,#219899,#219900,#219901,#219902,#219903,#219904,#219905,#219906,
#219907,#219908,#219909,#219910,#219911,#219912,#219913,#219914,#219915),
(#219916,#219917,#219918,#219919,#219920,#219921,#219922,#219923,#219924,
#219925,#219926,#219927,#219928,#219929,#219930,#219931,#219932,#219933,
#219934,#219935,#219936,#219937,#219938,#219939,#219940,#219941,#219942,
#219943,#219944,#219945,#219946,#219947,#219948,#219949,#219950,#219951,
#219952,#219953,#219954,#219955,#219956,#219957,#219958,#219959,#219960,
#219961,#219962,#219963,#219964,#219965,#219966,#219967,#219968,#219969,
#219970,#219971,#219972,#219973,#219974,#219975,#219976,#219977,#219978,
#219979,#219980,#219981,#219982),(#219983,#219984,#219985,#219986,#219987,
#219988,#219989,#219990,#219991,#219992,#219993,#219994,#219995,#219996,
#219997,#219998,#219999,#220000,#220001,#220002,#220003,#220004,#220005,
#220006,#220007,#220008,#220009,#220010,#220011,#220012,#220013,#220014,
#220015,#220016,#220017,#220018,#220019,#220020,#220021,#220022,#220023,
#220024,#220025,#220026,#220027,#220028,#220029,#220030,#220031,#220032,
#220033,#220034,#220035,#220036,#220037,#220038,#220039,#220040,#220041,
#220042,#220043,#220044,#220045,#220046,#220047,#220048,#220049),(#220050,
#220051,#220052,#220053,#220054,#220055,#220056,#220057,#220058,#220059,
#220060,#220061,#220062,#220063,#220064,#220065,#220066,#220067,#220068,
#220069,#220070,#220071,#220072,#220073,#220074,#220075,#220076,#220077,
#220078,#220079,#220080,#220081,#220082,#220083,#220084,#220085,#220086,
#220087,#220088,#220089,#220090,#220091,#220092,#220093,#220094,#220095,
#220096,#220097,#220098,#220099,#220100,#220101,#220102,#220103,#220104,
#220105,#220106,#220107,#220108,#220109,#220110,#220111,#220112,#220113,
#220114,#220115,#220116)),.UNSPECIFIED.,.F.,.F.,.F.,(4,4),(4,1,1,1,1,1,
1,1,1,1,1,1,1,1,1,1,1,1,1,1,1,1,1,1,1,1,1,1,1,1,1,1,1,1,1,1,1,1,1,1,1,1,
1,1,1,1,1,1,1,1,1,1,1,1,1,1,1,1,1,1,1,1,1,1,4),(0.,1.),(0.,0.015625,0.03125,
0.046875,0.0625,0.078125,0.09375,0.109375,0.125,0.140625,0.15625,0.171875,
0.1875,0.203125,0.21875,0.234375,0.25,0.265625,0.28125,0.296875,0.3125,
0.328125,0.34375,0.359375,0.375,0.390625,0.40625,0.421875,0.4375,0.453125,
0.46875,0.484375,0.5,0.515625,0.53125,0.546875,0.5625,0.578125,0.59375,
0.609375,0.625,0.640625,0.65625,0.671875,0.6875,0.703125,0.71875,0.734375,
0.75,0.765625,0.78125,0.796875,0.8125,0.828125,0.84375,0.859375,0.875,0.890625,
0.90625,0.921875,0.9375,0.953125,0.96875,0.984375,1.),.UNSPECIFIED.);
#237=B_SPLINE_SURFACE_WITH_KNOTS('',3,3,((#220185,#220186,#220187,#220188,
#220189,#220190,#220191),(#220192,#220193,#220194,#220195,#220196,#220197,
#220198),(#220199,#220200,#220201,#220202,#220203,#220204,#220205),(#220206,
#220207,#220208,#220209,#220210,#220211,#220212)),.UNSPECIFIED.,.F.,.F.,
 .F.,(4,4),(4,1,1,1,4),(0.,1.),(0.,0.250000000000007,0.5,0.75,1.),
 .UNSPECIFIED.);
#238=B_SPLINE_SURFACE_WITH_KNOTS('',3,3,((#220240,#220241,#220242,#220243,
#220244,#220245,#220246),(#220247,#220248,#220249,#220250,#220251,#220252,
#220253),(#220254,#220255,#220256,#220257,#220258,#220259,#220260),(#220261,
#220262,#220263,#220264,#220265,#220266,#220267)),.UNSPECIFIED.,.F.,.F.,
 .F.,(4,4),(4,1,1,1,4),(0.,1.),(0.,0.25,0.5,0.75,1.),.UNSPECIFIED.);
#239=B_SPLINE_SURFACE_WITH_KNOTS('',3,3,((#220274,#220275,#220276,#220277,
#220278,#220279,#220280,#220281,#220282,#220283,#220284,#220285,#220286,
#220287,#220288,#220289,#220290,#220291,#220292,#220293,#220294,#220295,
#220296,#220297,#220298,#220299,#220300,#220301,#220302,#220303,#220304,
#220305,#220306,#220307,#220308,#220309,#220310,#220311,#220312,#220313,
#220314,#220315,#220316,#220317,#220318,#220319,#220320,#220321,#220322,
#220323,#220324,#220325,#220326,#220327,#220328,#220329,#220330,#220331,
#220332,#220333,#220334,#220335,#220336,#220337,#220338,#220339,#220340),
(#220341,#220342,#220343,#220344,#220345,#220346,#220347,#220348,#220349,
#220350,#220351,#220352,#220353,#220354,#220355,#220356,#220357,#220358,
#220359,#220360,#220361,#220362,#220363,#220364,#220365,#220366,#220367,
#220368,#220369,#220370,#220371,#220372,#220373,#220374,#220375,#220376,
#220377,#220378,#220379,#220380,#220381,#220382,#220383,#220384,#220385,
#220386,#220387,#220388,#220389,#220390,#220391,#220392,#220393,#220394,
#220395,#220396,#220397,#220398,#220399,#220400,#220401,#220402,#220403,
#220404,#220405,#220406,#220407),(#220408,#220409,#220410,#220411,#220412,
#220413,#220414,#220415,#220416,#220417,#220418,#220419,#220420,#220421,
#220422,#220423,#220424,#220425,#220426,#220427,#220428,#220429,#220430,
#220431,#220432,#220433,#220434,#220435,#220436,#220437,#220438,#220439,
#220440,#220441,#220442,#220443,#220444,#220445,#220446,#220447,#220448,
#220449,#220450,#220451,#220452,#220453,#220454,#220455,#220456,#220457,
#220458,#220459,#220460,#220461,#220462,#220463,#220464,#220465,#220466,
#220467,#220468,#220469,#220470,#220471,#220472,#220473,#220474),(#220475,
#220476,#220477,#220478,#220479,#220480,#220481,#220482,#220483,#220484,
#220485,#220486,#220487,#220488,#220489,#220490,#220491,#220492,#220493,
#220494,#220495,#220496,#220497,#220498,#220499,#220500,#220501,#220502,
#220503,#220504,#220505,#220506,#220507,#220508,#220509,#220510,#220511,
#220512,#220513,#220514,#220515,#220516,#220517,#220518,#220519,#220520,
#220521,#220522,#220523,#220524,#220525,#220526,#220527,#220528,#220529,
#220530,#220531,#220532,#220533,#220534,#220535,#220536,#220537,#220538,
#220539,#220540,#220541)),.UNSPECIFIED.,.F.,.F.,.F.,(4,4),(4,1,1,1,1,1,
1,1,1,1,1,1,1,1,1,1,1,1,1,1,1,1,1,1,1,1,1,1,1,1,1,1,1,1,1,1,1,1,1,1,1,1,
1,1,1,1,1,1,1,1,1,1,1,1,1,1,1,1,1,1,1,1,1,1,4),(0.,1.),(0.,0.015625,0.03125,
0.046875,0.0625,0.078125,0.09375,0.109375,0.125,0.140625,0.15625,0.171875,
0.1875,0.203125,0.21875,0.234375,0.25,0.265625,0.28125,0.296875,0.3125,
0.328125,0.34375,0.359375,0.375,0.390625,0.40625,0.421875,0.4375,0.453125,
0.46875,0.484375,0.5,0.515625,0.53125,0.546875,0.5625,0.578125,0.59375,
0.609375,0.625,0.640625,0.65625,0.671875,0.6875,0.703125,0.71875,0.734375,
0.75,0.765625,0.78125,0.796875,0.8125,0.828125,0.84375,0.859375,0.875,0.890625,
0.90625,0.921875,0.9375,0.953125,0.96875,0.984375,1.),.UNSPECIFIED.);
#240=B_SPLINE_SURFACE_WITH_KNOTS('',3,3,((#220621,#220622,#220623,#220624,
#220625,#220626,#220627,#220628,#220629,#220630,#220631,#220632,#220633,
#220634,#220635,#220636,#220637,#220638,#220639,#220640,#220641,#220642,
#220643,#220644,#220645,#220646,#220647,#220648,#220649,#220650,#220651,
#220652,#220653,#220654,#220655,#220656,#220657,#220658,#220659,#220660,
#220661,#220662,#220663,#220664,#220665,#220666,#220667,#220668,#220669,
#220670,#220671,#220672,#220673,#220674,#220675,#220676,#220677,#220678,
#220679,#220680,#220681,#220682,#220683,#220684,#220685,#220686,#220687),
(#220688,#220689,#220690,#220691,#220692,#220693,#220694,#220695,#220696,
#220697,#220698,#220699,#220700,#220701,#220702,#220703,#220704,#220705,
#220706,#220707,#220708,#220709,#220710,#220711,#220712,#220713,#220714,
#220715,#220716,#220717,#220718,#220719,#220720,#220721,#220722,#220723,
#220724,#220725,#220726,#220727,#220728,#220729,#220730,#220731,#220732,
#220733,#220734,#220735,#220736,#220737,#220738,#220739,#220740,#220741,
#220742,#220743,#220744,#220745,#220746,#220747,#220748,#220749,#220750,
#220751,#220752,#220753,#220754),(#220755,#220756,#220757,#220758,#220759,
#220760,#220761,#220762,#220763,#220764,#220765,#220766,#220767,#220768,
#220769,#220770,#220771,#220772,#220773,#220774,#220775,#220776,#220777,
#220778,#220779,#220780,#220781,#220782,#220783,#220784,#220785,#220786,
#220787,#220788,#220789,#220790,#220791,#220792,#220793,#220794,#220795,
#220796,#220797,#220798,#220799,#220800,#220801,#220802,#220803,#220804,
#220805,#220806,#220807,#220808,#220809,#220810,#220811,#220812,#220813,
#220814,#220815,#220816,#220817,#220818,#220819,#220820,#220821),(#220822,
#220823,#220824,#220825,#220826,#220827,#220828,#220829,#220830,#220831,
#220832,#220833,#220834,#220835,#220836,#220837,#220838,#220839,#220840,
#220841,#220842,#220843,#220844,#220845,#220846,#220847,#220848,#220849,
#220850,#220851,#220852,#220853,#220854,#220855,#220856,#220857,#220858,
#220859,#220860,#220861,#220862,#220863,#220864,#220865,#220866,#220867,
#220868,#220869,#220870,#220871,#220872,#220873,#220874,#220875,#220876,
#220877,#220878,#220879,#220880,#220881,#220882,#220883,#220884,#220885,
#220886,#220887,#220888)),.UNSPECIFIED.,.F.,.F.,.F.,(4,4),(4,1,1,1,1,1,
1,1,1,1,1,1,1,1,1,1,1,1,1,1,1,1,1,1,1,1,1,1,1,1,1,1,1,1,1,1,1,1,1,1,1,1,
1,1,1,1,1,1,1,1,1,1,1,1,1,1,1,1,1,1,1,1,1,1,4),(0.,1.),(0.,0.015625,0.03125,
0.046875,0.0625,0.078125,0.09375,0.109375,0.125,0.140625,0.15625,0.171875,
0.1875,0.203125,0.21875,0.234375,0.25,0.265625,0.28125,0.296875,0.3125,
0.328125,0.34375,0.359375,0.375,0.390625,0.40625,0.421875,0.4375,0.453125,
0.46875,0.484375,0.5,0.515625,0.53125,0.546875,0.5625,0.578125,0.59375,
0.609375,0.625,0.640625,0.65625,0.671875,0.6875,0.703125,0.71875,0.734375,
0.75,0.765625,0.78125,0.796875,0.8125,0.828125,0.84375,0.859375,0.875,0.890625,
0.90625,0.921875,0.9375,0.953125,0.96875,0.984375,1.),.UNSPECIFIED.);
#241=B_SPLINE_SURFACE_WITH_KNOTS('',3,3,((#220890,#220891,#220892,#220893,
#220894,#220895,#220896,#220897,#220898,#220899,#220900,#220901,#220902,
#220903,#220904,#220905,#220906,#220907,#220908,#220909,#220910,#220911,
#220912,#220913,#220914,#220915,#220916,#220917,#220918,#220919,#220920,
#220921,#220922,#220923,#220924),(#220925,#220926,#220927,#220928,#220929,
#220930,#220931,#220932,#220933,#220934,#220935,#220936,#220937,#220938,
#220939,#220940,#220941,#220942,#220943,#220944,#220945,#220946,#220947,
#220948,#220949,#220950,#220951,#220952,#220953,#220954,#220955,#220956,
#220957,#220958,#220959),(#220960,#220961,#220962,#220963,#220964,#220965,
#220966,#220967,#220968,#220969,#220970,#220971,#220972,#220973,#220974,
#220975,#220976,#220977,#220978,#220979,#220980,#220981,#220982,#220983,
#220984,#220985,#220986,#220987,#220988,#220989,#220990,#220991,#220992,
#220993,#220994),(#220995,#220996,#220997,#220998,#220999,#221000,#221001,
#221002,#221003,#221004,#221005,#221006,#221007,#221008,#221009,#221010,
#221011,#221012,#221013,#221014,#221015,#221016,#221017,#221018,#221019,
#221020,#221021,#221022,#221023,#221024,#221025,#221026,#221027,#221028,
#221029)),.UNSPECIFIED.,.F.,.F.,.F.,(4,4),(4,1,1,1,1,1,1,1,1,1,1,1,1,1,
1,1,1,1,1,1,1,1,1,1,1,1,1,1,1,1,1,1,4),(0.,1.),(0.,0.0312499999999743,0.0624999999999486,
0.0937499999999229,0.125000000000034,0.156250000000008,0.187499999999983,
0.218749999999957,0.249999999999932,0.281250000000043,0.312500000000017,
0.343749999999991,0.374999999999966,0.406250000000077,0.437500000000052,
0.468750000000026,0.5,0.531249999999974,0.562500000000086,0.59375000000006,
0.625000000000034,0.656250000000009,0.687499999999983,0.718750000000095,
0.750000000000069,0.781250000000043,0.812500000000017,0.843750000000129,
0.875000000000103,0.906250000000077,0.937500000000052,0.968750000000026,
1.),.UNSPECIFIED.);
#242=B_SPLINE_SURFACE_WITH_KNOTS('',3,3,((#221042,#221043,#221044,#221045,
#221046,#221047,#221048,#221049,#221050,#221051,#221052,#221053,#221054,
#221055,#221056,#221057,#221058,#221059,#221060,#221061,#221062,#221063,
#221064,#221065,#221066,#221067,#221068,#221069,#221070,#221071,#221072,
#221073,#221074,#221075,#221076,#221077,#221078,#221079,#221080,#221081,
#221082,#221083,#221084,#221085,#221086,#221087,#221088,#221089,#221090,
#221091,#221092,#221093,#221094,#221095,#221096,#221097,#221098,#221099,
#221100,#221101,#221102,#221103,#221104,#221105,#221106,#221107,#221108),
(#221109,#221110,#221111,#221112,#221113,#221114,#221115,#221116,#221117,
#221118,#221119,#221120,#221121,#221122,#221123,#221124,#221125,#221126,
#221127,#221128,#221129,#221130,#221131,#221132,#221133,#221134,#221135,
#221136,#221137,#221138,#221139,#221140,#221141,#221142,#221143,#221144,
#221145,#221146,#221147,#221148,#221149,#221150,#221151,#221152,#221153,
#221154,#221155,#221156,#221157,#221158,#221159,#221160,#221161,#221162,
#221163,#221164,#221165,#221166,#221167,#221168,#221169,#221170,#221171,
#221172,#221173,#221174,#221175),(#221176,#221177,#221178,#221179,#221180,
#221181,#221182,#221183,#221184,#221185,#221186,#221187,#221188,#221189,
#221190,#221191,#221192,#221193,#221194,#221195,#221196,#221197,#221198,
#221199,#221200,#221201,#221202,#221203,#221204,#221205,#221206,#221207,
#221208,#221209,#221210,#221211,#221212,#221213,#221214,#221215,#221216,
#221217,#221218,#221219,#221220,#221221,#221222,#221223,#221224,#221225,
#221226,#221227,#221228,#221229,#221230,#221231,#221232,#221233,#221234,
#221235,#221236,#221237,#221238,#221239,#221240,#221241,#221242),(#221243,
#221244,#221245,#221246,#221247,#221248,#221249,#221250,#221251,#221252,
#221253,#221254,#221255,#221256,#221257,#221258,#221259,#221260,#221261,
#221262,#221263,#221264,#221265,#221266,#221267,#221268,#221269,#221270,
#221271,#221272,#221273,#221274,#221275,#221276,#221277,#221278,#221279,
#221280,#221281,#221282,#221283,#221284,#221285,#221286,#221287,#221288,
#221289,#221290,#221291,#221292,#221293,#221294,#221295,#221296,#221297,
#221298,#221299,#221300,#221301,#221302,#221303,#221304,#221305,#221306,
#221307,#221308,#221309)),.UNSPECIFIED.,.F.,.F.,.F.,(4,4),(4,1,1,1,1,1,
1,1,1,1,1,1,1,1,1,1,1,1,1,1,1,1,1,1,1,1,1,1,1,1,1,1,1,1,1,1,1,1,1,1,1,1,
1,1,1,1,1,1,1,1,1,1,1,1,1,1,1,1,1,1,1,1,1,1,4),(0.,1.),(0.,0.015625,0.03125,
0.046875,0.0625,0.078125,0.09375,0.109375,0.125,0.140625,0.15625,0.171875,
0.1875,0.203125,0.21875,0.234375,0.25,0.265625,0.28125,0.296875,0.3125,
0.328125,0.34375,0.359375,0.375,0.390625,0.40625,0.421875,0.4375,0.453125,
0.46875,0.484375,0.5,0.515625,0.53125,0.546875,0.5625,0.578125,0.59375,
0.609375,0.625,0.640625,0.65625,0.671875,0.6875,0.703125,0.71875,0.734375,
0.75,0.765625,0.78125,0.796875,0.8125,0.828125,0.84375,0.859375,0.875,0.890625,
0.90625,0.921875,0.9375,0.953125,0.96875,0.984375,1.),.UNSPECIFIED.);
#243=B_SPLINE_SURFACE_WITH_KNOTS('',3,3,((#221311,#221312,#221313,#221314,
#221315,#221316,#221317,#221318,#221319,#221320,#221321,#221322,#221323,
#221324,#221325,#221326,#221327,#221328,#221329,#221330,#221331,#221332,
#221333,#221334,#221335,#221336,#221337,#221338,#221339,#221340,#221341,
#221342,#221343,#221344,#221345),(#221346,#221347,#221348,#221349,#221350,
#221351,#221352,#221353,#221354,#221355,#221356,#221357,#221358,#221359,
#221360,#221361,#221362,#221363,#221364,#221365,#221366,#221367,#221368,
#221369,#221370,#221371,#221372,#221373,#221374,#221375,#221376,#221377,
#221378,#221379,#221380),(#221381,#221382,#221383,#221384,#221385,#221386,
#221387,#221388,#221389,#221390,#221391,#221392,#221393,#221394,#221395,
#221396,#221397,#221398,#221399,#221400,#221401,#221402,#221403,#221404,
#221405,#221406,#221407,#221408,#221409,#221410,#221411,#221412,#221413,
#221414,#221415),(#221416,#221417,#221418,#221419,#221420,#221421,#221422,
#221423,#221424,#221425,#221426,#221427,#221428,#221429,#221430,#221431,
#221432,#221433,#221434,#221435,#221436,#221437,#221438,#221439,#221440,
#221441,#221442,#221443,#221444,#221445,#221446,#221447,#221448,#221449,
#221450)),.UNSPECIFIED.,.F.,.F.,.F.,(4,4),(4,1,1,1,1,1,1,1,1,1,1,1,1,1,
1,1,1,1,1,1,1,1,1,1,1,1,1,1,1,1,1,1,4),(0.,1.),(0.,0.031249999999901,0.0624999999999529,
0.0937500000000048,0.125000000000057,0.156250000000109,0.187500000000009,
0.218750000000062,0.250000000000113,0.281250000000165,0.312500000000066,
0.343750000000118,0.37500000000017,0.406250000000221,0.437500000000123,
0.468750000000175,0.500000000000226,0.531250000000278,0.562500000000179,
0.593750000000231,0.625000000000283,0.656250000000335,0.687500000000236,
0.718750000000288,0.75000000000034,0.781250000000392,0.812500000000292,
0.843750000000344,0.875000000000396,0.906250000000448,0.937500000000349,
0.968750000000401,1.),.UNSPECIFIED.);
#244=B_SPLINE_SURFACE_WITH_KNOTS('',3,3,((#221527,#221528,#221529,#221530,
#221531,#221532,#221533,#221534,#221535,#221536,#221537,#221538,#221539,
#221540,#221541,#221542,#221543,#221544,#221545),(#221546,#221547,#221548,
#221549,#221550,#221551,#221552,#221553,#221554,#221555,#221556,#221557,
#221558,#221559,#221560,#221561,#221562,#221563,#221564),(#221565,#221566,
#221567,#221568,#221569,#221570,#221571,#221572,#221573,#221574,#221575,
#221576,#221577,#221578,#221579,#221580,#221581,#221582,#221583),(#221584,
#221585,#221586,#221587,#221588,#221589,#221590,#221591,#221592,#221593,
#221594,#221595,#221596,#221597,#221598,#221599,#221600,#221601,#221602)),
 .UNSPECIFIED.,.F.,.F.,.F.,(4,4),(4,1,1,1,1,1,1,1,1,1,1,1,1,1,1,1,4),(0.,
1.),(0.,0.0625,0.124999999999643,0.187499999999643,0.249999999999643,0.312499999999286,
0.374999999999286,0.437499999999286,0.499999999999286,0.562499999998929,
0.624999999998929,0.687499999998929,0.749999999998572,0.812499999998572,
0.874999999998572,0.937499999998572,1.),.UNSPECIFIED.);
#245=FACE_BOUND('',#23999,.T.);
#246=FACE_BOUND('',#24007,.T.);
#247=FACE_BOUND('',#24009,.T.);
#248=FACE_BOUND('',#24078,.T.);
#249=FACE_BOUND('',#24086,.T.);
#250=FACE_BOUND('',#24088,.T.);
#251=FACE_BOUND('',#24096,.T.);
#252=FACE_BOUND('',#24098,.T.);
#253=FACE_BOUND('',#24167,.T.);
#254=FACE_BOUND('',#24175,.T.);
#255=FACE_BOUND('',#24180,.T.);
#256=FACE_BOUND('',#24242,.T.);
#257=FACE_BOUND('',#24244,.T.);
#258=FACE_BOUND('',#24267,.T.);
#259=FACE_BOUND('',#24269,.T.);
#260=FACE_BOUND('',#24271,.T.);
#261=FACE_BOUND('',#24339,.T.);
#262=FACE_BOUND('',#24341,.T.);
#263=FACE_BOUND('',#24394,.T.);
#264=FACE_BOUND('',#24425,.T.);
#265=FACE_BOUND('',#24455,.T.);
#266=FACE_BOUND('',#24474,.T.);
#267=FACE_BOUND('',#24478,.T.);
#268=FACE_BOUND('',#24480,.T.);
#269=FACE_BOUND('',#24594,.T.);
#270=FACE_BOUND('',#24605,.T.);
#271=FACE_BOUND('',#24611,.T.);
#272=FACE_BOUND('',#24616,.T.);
#273=FACE_BOUND('',#24644,.T.);
#274=FACE_BOUND('',#24645,.T.);
#275=FACE_BOUND('',#24701,.T.);
#276=FACE_BOUND('',#24703,.T.);
#277=FACE_BOUND('',#24705,.T.);
#278=FACE_BOUND('',#24713,.T.);
#279=FACE_BOUND('',#24715,.T.);
#280=FACE_BOUND('',#24717,.T.);
#281=FACE_BOUND('',#24719,.T.);
#282=FACE_BOUND('',#24733,.T.);
#283=FACE_BOUND('',#24735,.T.);
#284=FACE_BOUND('',#24737,.T.);
#285=FACE_BOUND('',#24739,.T.);
#286=FACE_BOUND('',#24741,.T.);
#287=FACE_BOUND('',#24743,.T.);
#288=FACE_BOUND('',#24771,.T.);
#289=FACE_BOUND('',#24781,.T.);
#290=FACE_BOUND('',#24783,.T.);
#291=FACE_BOUND('',#24797,.T.);
#292=FACE_BOUND('',#24799,.T.);
#293=FACE_BOUND('',#24801,.T.);
#294=FACE_BOUND('',#24803,.T.);
#295=FACE_BOUND('',#24805,.T.);
#296=FACE_BOUND('',#24807,.T.);
#297=FACE_BOUND('',#24816,.T.);
#298=FACE_BOUND('',#24818,.T.);
#299=FACE_BOUND('',#24820,.T.);
#300=FACE_BOUND('',#24823,.T.);
#301=FACE_BOUND('',#24825,.T.);
#302=FACE_BOUND('',#24853,.T.);
#303=FACE_BOUND('',#24863,.T.);
#304=FACE_BOUND('',#24865,.T.);
#305=FACE_BOUND('',#24899,.T.);
#306=FACE_BOUND('',#24901,.T.);
#307=FACE_BOUND('',#24903,.T.);
#308=FACE_BOUND('',#24906,.T.);
#309=FACE_BOUND('',#24909,.T.);
#310=FACE_BOUND('',#24917,.T.);
#311=FACE_BOUND('',#24919,.T.);
#312=FACE_BOUND('',#24921,.T.);
#313=FACE_BOUND('',#24924,.T.);
#314=FACE_BOUND('',#24933,.T.);
#315=FACE_BOUND('',#24935,.T.);
#316=FACE_BOUND('',#24937,.T.);
#317=FACE_BOUND('',#24940,.T.);
#318=FACE_BOUND('',#24942,.T.);
#319=FACE_BOUND('',#24953,.T.);
#320=FACE_BOUND('',#24954,.T.);
#321=FACE_BOUND('',#24955,.T.);
#322=FACE_BOUND('',#24959,.T.);
#323=FACE_BOUND('',#24960,.T.);
#324=FACE_BOUND('',#24961,.T.);
#325=FACE_BOUND('',#24984,.T.);
#326=FACE_BOUND('',#24986,.T.);
#327=FACE_BOUND('',#24992,.T.);
#328=FACE_BOUND('',#24994,.T.);
#329=FACE_BOUND('',#24996,.T.);
#330=FACE_BOUND('',#26056,.T.);
#331=FACE_BOUND('',#27802,.T.);
#332=FACE_BOUND('',#27804,.T.);
#333=FACE_BOUND('',#27805,.T.);
#334=FACE_BOUND('',#27806,.T.);
#335=FACE_BOUND('',#27807,.T.);
#336=FACE_BOUND('',#27808,.T.);
#337=FACE_BOUND('',#27809,.T.);
#338=FACE_BOUND('',#27810,.T.);
#339=FACE_BOUND('',#27811,.T.);
#340=FACE_BOUND('',#27812,.T.);
#341=FACE_BOUND('',#27813,.T.);
#342=FACE_BOUND('',#27814,.T.);
#343=FACE_BOUND('',#27815,.T.);
#344=FACE_BOUND('',#27816,.T.);
#345=FACE_BOUND('',#27817,.T.);
#346=FACE_BOUND('',#27818,.T.);
#347=FACE_BOUND('',#27819,.T.);
#348=FACE_BOUND('',#27820,.T.);
#349=FACE_BOUND('',#27821,.T.);
#350=FACE_BOUND('',#27822,.T.);
#351=FACE_BOUND('',#27823,.T.);
#352=FACE_BOUND('',#27824,.T.);
#353=FACE_BOUND('',#27825,.T.);
#354=FACE_BOUND('',#27826,.T.);
#355=FACE_BOUND('',#27827,.T.);
#356=FACE_BOUND('',#27828,.T.);
#357=FACE_BOUND('',#27829,.T.);
#358=FACE_BOUND('',#27830,.T.);
#359=FACE_BOUND('',#27831,.T.);
#360=FACE_BOUND('',#27832,.T.);
#361=FACE_BOUND('',#27833,.T.);
#362=FACE_BOUND('',#27834,.T.);
#363=FACE_BOUND('',#27835,.T.);
#364=FACE_BOUND('',#27836,.T.);
#365=FACE_BOUND('',#27837,.T.);
#366=FACE_BOUND('',#27838,.T.);
#367=FACE_BOUND('',#27839,.T.);
#368=FACE_BOUND('',#27840,.T.);
#369=FACE_BOUND('',#27841,.T.);
#370=FACE_BOUND('',#27842,.T.);
#371=FACE_BOUND('',#27843,.T.);
#372=FACE_BOUND('',#27844,.T.);
#373=FACE_BOUND('',#27845,.T.);
#374=FACE_BOUND('',#27846,.T.);
#375=FACE_BOUND('',#27847,.T.);
#376=FACE_BOUND('',#27848,.T.);
#377=FACE_BOUND('',#27849,.T.);
#378=FACE_BOUND('',#27850,.T.);
#379=FACE_BOUND('',#27851,.T.);
#380=FACE_BOUND('',#27852,.T.);
#381=FACE_BOUND('',#27853,.T.);
#382=FACE_BOUND('',#27854,.T.);
#383=FACE_BOUND('',#27855,.T.);
#384=FACE_BOUND('',#27856,.T.);
#385=FACE_BOUND('',#27857,.T.);
#386=FACE_BOUND('',#27858,.T.);
#387=FACE_BOUND('',#27859,.T.);
#388=FACE_BOUND('',#27860,.T.);
#389=FACE_BOUND('',#27861,.T.);
#390=FACE_BOUND('',#27862,.T.);
#391=FACE_BOUND('',#27863,.T.);
#392=FACE_BOUND('',#27864,.T.);
#393=FACE_BOUND('',#27865,.T.);
#394=FACE_BOUND('',#27866,.T.);
#395=FACE_BOUND('',#27867,.T.);
#396=FACE_BOUND('',#27868,.T.);
#397=FACE_BOUND('',#27869,.T.);
#398=FACE_BOUND('',#27870,.T.);
#399=FACE_BOUND('',#27871,.T.);
#400=FACE_BOUND('',#27872,.T.);
#401=FACE_BOUND('',#27873,.T.);
#402=FACE_BOUND('',#27874,.T.);
#403=FACE_BOUND('',#27875,.T.);
#404=FACE_BOUND('',#27876,.T.);
#405=FACE_BOUND('',#27877,.T.);
#406=FACE_BOUND('',#27878,.T.);
#407=FACE_BOUND('',#27879,.T.);
#408=FACE_BOUND('',#27880,.T.);
#409=FACE_BOUND('',#27881,.T.);
#410=FACE_BOUND('',#27882,.T.);
#411=FACE_BOUND('',#27883,.T.);
#412=FACE_BOUND('',#27884,.T.);
#413=FACE_BOUND('',#27885,.T.);
#414=FACE_BOUND('',#27886,.T.);
#415=FACE_BOUND('',#27887,.T.);
#416=FACE_BOUND('',#27888,.T.);
#417=FACE_BOUND('',#27889,.T.);
#418=FACE_BOUND('',#27890,.T.);
#419=FACE_BOUND('',#27891,.T.);
#420=FACE_BOUND('',#27892,.T.);
#421=FACE_BOUND('',#27893,.T.);
#422=FACE_BOUND('',#27894,.T.);
#423=FACE_BOUND('',#27895,.T.);
#424=FACE_BOUND('',#27896,.T.);
#425=FACE_BOUND('',#27897,.T.);
#426=FACE_BOUND('',#27898,.T.);
#427=FACE_BOUND('',#27899,.T.);
#428=FACE_BOUND('',#27900,.T.);
#429=FACE_BOUND('',#27901,.T.);
#430=FACE_BOUND('',#27902,.T.);
#431=FACE_BOUND('',#27903,.T.);
#432=FACE_BOUND('',#27904,.T.);
#433=FACE_BOUND('',#27905,.T.);
#434=FACE_BOUND('',#27906,.T.);
#435=FACE_BOUND('',#27907,.T.);
#436=FACE_BOUND('',#27908,.T.);
#437=FACE_BOUND('',#27909,.T.);
#438=FACE_BOUND('',#27910,.T.);
#439=FACE_BOUND('',#27911,.T.);
#440=FACE_BOUND('',#27912,.T.);
#441=FACE_BOUND('',#27913,.T.);
#442=FACE_BOUND('',#27914,.T.);
#443=FACE_BOUND('',#27915,.T.);
#444=FACE_BOUND('',#27916,.T.);
#445=FACE_BOUND('',#27917,.T.);
#446=FACE_BOUND('',#27918,.T.);
#447=FACE_BOUND('',#27919,.T.);
#448=FACE_BOUND('',#27920,.T.);
#449=FACE_BOUND('',#27921,.T.);
#450=FACE_BOUND('',#27922,.T.);
#451=FACE_BOUND('',#27923,.T.);
#452=FACE_BOUND('',#27924,.T.);
#453=FACE_BOUND('',#27925,.T.);
#454=FACE_BOUND('',#27926,.T.);
#455=FACE_BOUND('',#27927,.T.);
#456=FACE_BOUND('',#27928,.T.);
#457=FACE_BOUND('',#27929,.T.);
#458=FACE_BOUND('',#27930,.T.);
#459=FACE_BOUND('',#27931,.T.);
#460=FACE_BOUND('',#27932,.T.);
#461=FACE_BOUND('',#27933,.T.);
#462=FACE_BOUND('',#27934,.T.);
#463=FACE_BOUND('',#27935,.T.);
#464=FACE_BOUND('',#27936,.T.);
#465=FACE_BOUND('',#27937,.T.);
#466=FACE_BOUND('',#27938,.T.);
#467=FACE_BOUND('',#27939,.T.);
#468=FACE_BOUND('',#27940,.T.);
#469=FACE_BOUND('',#27941,.T.);
#470=FACE_BOUND('',#27942,.T.);
#471=FACE_BOUND('',#27943,.T.);
#472=FACE_BOUND('',#27944,.T.);
#473=FACE_BOUND('',#27945,.T.);
#474=FACE_BOUND('',#27946,.T.);
#475=FACE_BOUND('',#27947,.T.);
#476=FACE_BOUND('',#27948,.T.);
#477=FACE_BOUND('',#27949,.T.);
#478=FACE_BOUND('',#27950,.T.);
#479=FACE_BOUND('',#27951,.T.);
#480=FACE_BOUND('',#27952,.T.);
#481=FACE_BOUND('',#27953,.T.);
#482=FACE_BOUND('',#27954,.T.);
#483=FACE_BOUND('',#27955,.T.);
#484=FACE_BOUND('',#27956,.T.);
#485=FACE_BOUND('',#27957,.T.);
#486=FACE_BOUND('',#27958,.T.);
#487=FACE_BOUND('',#27959,.T.);
#488=FACE_BOUND('',#27960,.T.);
#489=FACE_BOUND('',#27961,.T.);
#490=FACE_BOUND('',#27962,.T.);
#491=FACE_BOUND('',#27963,.T.);
#492=FACE_BOUND('',#27964,.T.);
#493=FACE_BOUND('',#27965,.T.);
#494=FACE_BOUND('',#27966,.T.);
#495=FACE_BOUND('',#27967,.T.);
#496=FACE_BOUND('',#27968,.T.);
#497=FACE_BOUND('',#27969,.T.);
#498=FACE_BOUND('',#27970,.T.);
#499=FACE_BOUND('',#27971,.T.);
#500=FACE_BOUND('',#27972,.T.);
#501=FACE_BOUND('',#27973,.T.);
#502=FACE_BOUND('',#27974,.T.);
#503=FACE_BOUND('',#27975,.T.);
#504=FACE_BOUND('',#27976,.T.);
#505=FACE_BOUND('',#27977,.T.);
#506=FACE_BOUND('',#27978,.T.);
#507=FACE_BOUND('',#27979,.T.);
#508=FACE_BOUND('',#27980,.T.);
#509=FACE_BOUND('',#27981,.T.);
#510=FACE_BOUND('',#27982,.T.);
#511=FACE_BOUND('',#27983,.T.);
#512=FACE_BOUND('',#27984,.T.);
#513=FACE_BOUND('',#27985,.T.);
#514=FACE_BOUND('',#27986,.T.);
#515=FACE_BOUND('',#27987,.T.);
#516=FACE_BOUND('',#27988,.T.);
#517=FACE_BOUND('',#27989,.T.);
#518=FACE_BOUND('',#27990,.T.);
#519=FACE_BOUND('',#27991,.T.);
#520=FACE_BOUND('',#27992,.T.);
#521=FACE_BOUND('',#27993,.T.);
#522=FACE_BOUND('',#27994,.T.);
#523=FACE_BOUND('',#27995,.T.);
#524=FACE_BOUND('',#27996,.T.);
#525=FACE_BOUND('',#27997,.T.);
#526=FACE_BOUND('',#27998,.T.);
#527=FACE_BOUND('',#27999,.T.);
#528=FACE_BOUND('',#28000,.T.);
#529=FACE_BOUND('',#28001,.T.);
#530=FACE_BOUND('',#28002,.T.);
#531=FACE_BOUND('',#28003,.T.);
#532=FACE_BOUND('',#28004,.T.);
#533=FACE_BOUND('',#28005,.T.);
#534=FACE_BOUND('',#28006,.T.);
#535=FACE_BOUND('',#28007,.T.);
#536=FACE_BOUND('',#28008,.T.);
#537=FACE_BOUND('',#28009,.T.);
#538=FACE_BOUND('',#28010,.T.);
#539=FACE_BOUND('',#28011,.T.);
#540=FACE_BOUND('',#28012,.T.);
#541=FACE_BOUND('',#28013,.T.);
#542=FACE_BOUND('',#28014,.T.);
#543=FACE_BOUND('',#28015,.T.);
#544=FACE_BOUND('',#28016,.T.);
#545=FACE_BOUND('',#28017,.T.);
#546=FACE_BOUND('',#28018,.T.);
#547=FACE_BOUND('',#28019,.T.);
#548=FACE_BOUND('',#28020,.T.);
#549=FACE_BOUND('',#28021,.T.);
#550=FACE_BOUND('',#28022,.T.);
#551=FACE_BOUND('',#28023,.T.);
#552=FACE_BOUND('',#28024,.T.);
#553=FACE_BOUND('',#28025,.T.);
#554=FACE_BOUND('',#28026,.T.);
#555=FACE_BOUND('',#28027,.T.);
#556=FACE_BOUND('',#28028,.T.);
#557=FACE_BOUND('',#28029,.T.);
#558=FACE_BOUND('',#28030,.T.);
#559=FACE_BOUND('',#28031,.T.);
#560=FACE_BOUND('',#28032,.T.);
#561=FACE_BOUND('',#28033,.T.);
#562=FACE_BOUND('',#28034,.T.);
#563=FACE_BOUND('',#28035,.T.);
#564=FACE_BOUND('',#28036,.T.);
#565=FACE_BOUND('',#28037,.T.);
#566=FACE_BOUND('',#28038,.T.);
#567=FACE_BOUND('',#28039,.T.);
#568=FACE_BOUND('',#28040,.T.);
#569=FACE_BOUND('',#28041,.T.);
#570=FACE_BOUND('',#28042,.T.);
#571=FACE_BOUND('',#28043,.T.);
#572=FACE_BOUND('',#28044,.T.);
#573=FACE_BOUND('',#28045,.T.);
#574=FACE_BOUND('',#28046,.T.);
#575=FACE_BOUND('',#28047,.T.);
#576=FACE_BOUND('',#28048,.T.);
#577=FACE_BOUND('',#28049,.T.);
#578=FACE_BOUND('',#28050,.T.);
#579=FACE_BOUND('',#28051,.T.);
#580=FACE_BOUND('',#28052,.T.);
#581=FACE_BOUND('',#28053,.T.);
#582=FACE_BOUND('',#28054,.T.);
#583=FACE_BOUND('',#28055,.T.);
#584=FACE_BOUND('',#28056,.T.);
#585=FACE_BOUND('',#28057,.T.);
#586=FACE_BOUND('',#28058,.T.);
#587=FACE_BOUND('',#28059,.T.);
#588=FACE_BOUND('',#28060,.T.);
#589=FACE_BOUND('',#28061,.T.);
#590=FACE_BOUND('',#28062,.T.);
#591=FACE_BOUND('',#28063,.T.);
#592=FACE_BOUND('',#28064,.T.);
#593=FACE_BOUND('',#28065,.T.);
#594=FACE_BOUND('',#28066,.T.);
#595=FACE_BOUND('',#28067,.T.);
#596=FACE_BOUND('',#28068,.T.);
#597=FACE_BOUND('',#28069,.T.);
#598=FACE_BOUND('',#28070,.T.);
#599=FACE_BOUND('',#28071,.T.);
#600=FACE_BOUND('',#28072,.T.);
#601=FACE_BOUND('',#28073,.T.);
#602=FACE_BOUND('',#28074,.T.);
#603=FACE_BOUND('',#28075,.T.);
#604=FACE_BOUND('',#28076,.T.);
#605=FACE_BOUND('',#28077,.T.);
#606=FACE_BOUND('',#28078,.T.);
#607=FACE_BOUND('',#28079,.T.);
#608=FACE_BOUND('',#28080,.T.);
#609=FACE_BOUND('',#28081,.T.);
#610=FACE_BOUND('',#28082,.T.);
#611=FACE_BOUND('',#28083,.T.);
#612=FACE_BOUND('',#28084,.T.);
#613=FACE_BOUND('',#28085,.T.);
#614=FACE_BOUND('',#28086,.T.);
#615=FACE_BOUND('',#28087,.T.);
#616=FACE_BOUND('',#28088,.T.);
#617=FACE_BOUND('',#28089,.T.);
#618=FACE_BOUND('',#28090,.T.);
#619=FACE_BOUND('',#28091,.T.);
#620=FACE_BOUND('',#28092,.T.);
#621=FACE_BOUND('',#28093,.T.);
#622=FACE_BOUND('',#28094,.T.);
#623=FACE_BOUND('',#28095,.T.);
#624=FACE_BOUND('',#28096,.T.);
#625=FACE_BOUND('',#28097,.T.);
#626=FACE_BOUND('',#28098,.T.);
#627=FACE_BOUND('',#28099,.T.);
#628=FACE_BOUND('',#28100,.T.);
#629=FACE_BOUND('',#28101,.T.);
#630=FACE_BOUND('',#28102,.T.);
#631=FACE_BOUND('',#28103,.T.);
#632=FACE_BOUND('',#28104,.T.);
#633=FACE_BOUND('',#28105,.T.);
#634=FACE_BOUND('',#28106,.T.);
#635=FACE_BOUND('',#28107,.T.);
#636=FACE_BOUND('',#28108,.T.);
#637=FACE_BOUND('',#28109,.T.);
#638=FACE_BOUND('',#28110,.T.);
#639=FACE_BOUND('',#28111,.T.);
#640=FACE_BOUND('',#28112,.T.);
#641=FACE_BOUND('',#28113,.T.);
#642=FACE_BOUND('',#28114,.T.);
#643=FACE_BOUND('',#28115,.T.);
#644=FACE_BOUND('',#28116,.T.);
#645=FACE_BOUND('',#28117,.T.);
#646=FACE_BOUND('',#28118,.T.);
#647=FACE_BOUND('',#28119,.T.);
#648=FACE_BOUND('',#28120,.T.);
#649=FACE_BOUND('',#28121,.T.);
#650=FACE_BOUND('',#28122,.T.);
#651=FACE_BOUND('',#28123,.T.);
#652=FACE_BOUND('',#28124,.T.);
#653=FACE_BOUND('',#28125,.T.);
#654=FACE_BOUND('',#28126,.T.);
#655=FACE_BOUND('',#28127,.T.);
#656=FACE_BOUND('',#28128,.T.);
#657=FACE_BOUND('',#28129,.T.);
#658=FACE_BOUND('',#28130,.T.);
#659=FACE_BOUND('',#28131,.T.);
#660=FACE_BOUND('',#28132,.T.);
#661=FACE_BOUND('',#28133,.T.);
#662=FACE_BOUND('',#28134,.T.);
#663=FACE_BOUND('',#28135,.T.);
#664=FACE_BOUND('',#28136,.T.);
#665=FACE_BOUND('',#28137,.T.);
#666=FACE_BOUND('',#28138,.T.);
#667=FACE_BOUND('',#28139,.T.);
#668=FACE_BOUND('',#28140,.T.);
#669=FACE_BOUND('',#28141,.T.);
#670=FACE_BOUND('',#28142,.T.);
#671=FACE_BOUND('',#28143,.T.);
#672=FACE_BOUND('',#28144,.T.);
#673=FACE_BOUND('',#28145,.T.);
#674=FACE_BOUND('',#28146,.T.);
#675=FACE_BOUND('',#28147,.T.);
#676=FACE_BOUND('',#28148,.T.);
#677=FACE_BOUND('',#28149,.T.);
#678=FACE_BOUND('',#28150,.T.);
#679=FACE_BOUND('',#28151,.T.);
#680=FACE_BOUND('',#28152,.T.);
#681=FACE_BOUND('',#28153,.T.);
#682=FACE_BOUND('',#28154,.T.);
#683=FACE_BOUND('',#28155,.T.);
#684=FACE_BOUND('',#28156,.T.);
#685=FACE_BOUND('',#28157,.T.);
#686=FACE_BOUND('',#28158,.T.);
#687=FACE_BOUND('',#28159,.T.);
#688=FACE_BOUND('',#28160,.T.);
#689=FACE_BOUND('',#28161,.T.);
#690=FACE_BOUND('',#28162,.T.);
#691=FACE_BOUND('',#28163,.T.);
#692=FACE_BOUND('',#28164,.T.);
#693=FACE_BOUND('',#28165,.T.);
#694=FACE_BOUND('',#28166,.T.);
#695=FACE_BOUND('',#28167,.T.);
#696=FACE_BOUND('',#28168,.T.);
#697=FACE_BOUND('',#28169,.T.);
#698=FACE_BOUND('',#28170,.T.);
#699=FACE_BOUND('',#28171,.T.);
#700=FACE_BOUND('',#28172,.T.);
#701=FACE_BOUND('',#28173,.T.);
#702=FACE_BOUND('',#28174,.T.);
#703=FACE_BOUND('',#28175,.T.);
#704=FACE_BOUND('',#28176,.T.);
#705=FACE_BOUND('',#28177,.T.);
#706=FACE_BOUND('',#28178,.T.);
#707=FACE_BOUND('',#28179,.T.);
#708=FACE_BOUND('',#28180,.T.);
#709=FACE_BOUND('',#28181,.T.);
#710=FACE_BOUND('',#28182,.T.);
#711=FACE_BOUND('',#28183,.T.);
#712=FACE_BOUND('',#28184,.T.);
#713=FACE_BOUND('',#28185,.T.);
#714=FACE_BOUND('',#28186,.T.);
#715=FACE_BOUND('',#28187,.T.);
#716=FACE_BOUND('',#28188,.T.);
#717=FACE_BOUND('',#28189,.T.);
#718=FACE_BOUND('',#28190,.T.);
#719=FACE_BOUND('',#28191,.T.);
#720=FACE_BOUND('',#28192,.T.);
#721=FACE_BOUND('',#28193,.T.);
#722=FACE_BOUND('',#28194,.T.);
#723=FACE_BOUND('',#28195,.T.);
#724=FACE_BOUND('',#28196,.T.);
#725=FACE_BOUND('',#28197,.T.);
#726=FACE_BOUND('',#28198,.T.);
#727=FACE_BOUND('',#28199,.T.);
#728=FACE_BOUND('',#28200,.T.);
#729=FACE_BOUND('',#28201,.T.);
#730=FACE_BOUND('',#28202,.T.);
#731=FACE_BOUND('',#28203,.T.);
#732=FACE_BOUND('',#28204,.T.);
#733=FACE_BOUND('',#28205,.T.);
#734=FACE_BOUND('',#28206,.T.);
#735=FACE_BOUND('',#28207,.T.);
#736=FACE_BOUND('',#28208,.T.);
#737=FACE_BOUND('',#28209,.T.);
#738=FACE_BOUND('',#28210,.T.);
#739=FACE_BOUND('',#28211,.T.);
#740=FACE_BOUND('',#28212,.T.);
#741=FACE_BOUND('',#28213,.T.);
#742=FACE_BOUND('',#28214,.T.);
#743=FACE_BOUND('',#28215,.T.);
#744=FACE_BOUND('',#28216,.T.);
#745=FACE_BOUND('',#28217,.T.);
#746=FACE_BOUND('',#28218,.T.);
#747=FACE_BOUND('',#28219,.T.);
#748=FACE_BOUND('',#28220,.T.);
#749=FACE_BOUND('',#28221,.T.);
#750=FACE_BOUND('',#28222,.T.);
#751=FACE_BOUND('',#28223,.T.);
#752=FACE_BOUND('',#28224,.T.);
#753=FACE_BOUND('',#28225,.T.);
#754=FACE_BOUND('',#28226,.T.);
#755=FACE_BOUND('',#28227,.T.);
#756=FACE_BOUND('',#28228,.T.);
#757=FACE_BOUND('',#28229,.T.);
#758=FACE_BOUND('',#28230,.T.);
#759=FACE_BOUND('',#28231,.T.);
#760=FACE_BOUND('',#28232,.T.);
#761=FACE_BOUND('',#28233,.T.);
#762=FACE_BOUND('',#28234,.T.);
#763=FACE_BOUND('',#28235,.T.);
#764=FACE_BOUND('',#28236,.T.);
#765=FACE_BOUND('',#28237,.T.);
#766=FACE_BOUND('',#28238,.T.);
#767=FACE_BOUND('',#28239,.T.);
#768=FACE_BOUND('',#28240,.T.);
#769=FACE_BOUND('',#28246,.T.);
#770=FACE_BOUND('',#28247,.T.);
#771=FACE_BOUND('',#28248,.T.);
#772=FACE_BOUND('',#28249,.T.);
#773=FACE_BOUND('',#28250,.T.);
#774=FACE_BOUND('',#28251,.T.);
#775=FACE_BOUND('',#28252,.T.);
#776=FACE_BOUND('',#28253,.T.);
#777=FACE_BOUND('',#28254,.T.);
#778=FACE_BOUND('',#28255,.T.);
#779=FACE_BOUND('',#28256,.T.);
#780=FACE_BOUND('',#28257,.T.);
#781=FACE_BOUND('',#28258,.T.);
#782=FACE_BOUND('',#28259,.T.);
#783=FACE_BOUND('',#28260,.T.);
#784=FACE_BOUND('',#28261,.T.);
#785=FACE_BOUND('',#28262,.T.);
#786=FACE_BOUND('',#28263,.T.);
#787=FACE_BOUND('',#28264,.T.);
#788=FACE_BOUND('',#28265,.T.);
#789=FACE_BOUND('',#28266,.T.);
#790=FACE_BOUND('',#28267,.T.);
#791=FACE_BOUND('',#28268,.T.);
#792=FACE_BOUND('',#28269,.T.);
#793=FACE_BOUND('',#28270,.T.);
#794=FACE_BOUND('',#28271,.T.);
#795=FACE_BOUND('',#28272,.T.);
#796=FACE_BOUND('',#28273,.T.);
#797=FACE_BOUND('',#28274,.T.);
#798=FACE_BOUND('',#28275,.T.);
#799=FACE_BOUND('',#28276,.T.);
#800=FACE_BOUND('',#28277,.T.);
#801=FACE_BOUND('',#28278,.T.);
#802=FACE_BOUND('',#28279,.T.);
#803=FACE_BOUND('',#28280,.T.);
#804=FACE_BOUND('',#28281,.T.);
#805=FACE_BOUND('',#28282,.T.);
#806=FACE_BOUND('',#28283,.T.);
#807=FACE_BOUND('',#28284,.T.);
#808=FACE_BOUND('',#28285,.T.);
#809=FACE_BOUND('',#28286,.T.);
#810=FACE_BOUND('',#28287,.T.);
#811=FACE_BOUND('',#28288,.T.);
#812=FACE_BOUND('',#28289,.T.);
#813=FACE_BOUND('',#28290,.T.);
#814=FACE_BOUND('',#28291,.T.);
#815=FACE_BOUND('',#28292,.T.);
#816=FACE_BOUND('',#28293,.T.);
#817=FACE_BOUND('',#28294,.T.);
#818=FACE_BOUND('',#28295,.T.);
#819=FACE_BOUND('',#28296,.T.);
#820=FACE_BOUND('',#28297,.T.);
#821=FACE_BOUND('',#28298,.T.);
#822=FACE_BOUND('',#28299,.T.);
#823=FACE_BOUND('',#28300,.T.);
#824=FACE_BOUND('',#28301,.T.);
#825=FACE_BOUND('',#28302,.T.);
#826=FACE_BOUND('',#28303,.T.);
#827=FACE_BOUND('',#28304,.T.);
#828=FACE_BOUND('',#28305,.T.);
#829=FACE_BOUND('',#28306,.T.);
#830=FACE_BOUND('',#28307,.T.);
#831=FACE_BOUND('',#28308,.T.);
#832=FACE_BOUND('',#28309,.T.);
#833=FACE_BOUND('',#28310,.T.);
#834=FACE_BOUND('',#28311,.T.);
#835=FACE_BOUND('',#28312,.T.);
#836=FACE_BOUND('',#28313,.T.);
#837=FACE_BOUND('',#28314,.T.);
#838=FACE_BOUND('',#28315,.T.);
#839=FACE_BOUND('',#28316,.T.);
#840=FACE_BOUND('',#28317,.T.);
#841=FACE_BOUND('',#28318,.T.);
#842=FACE_BOUND('',#28319,.T.);
#843=FACE_BOUND('',#28320,.T.);
#844=FACE_BOUND('',#28321,.T.);
#845=FACE_BOUND('',#28322,.T.);
#846=FACE_BOUND('',#28323,.T.);
#847=FACE_BOUND('',#28324,.T.);
#848=FACE_BOUND('',#28325,.T.);
#849=FACE_BOUND('',#28326,.T.);
#850=FACE_BOUND('',#28327,.T.);
#851=FACE_BOUND('',#28328,.T.);
#852=FACE_BOUND('',#28329,.T.);
#853=FACE_BOUND('',#28330,.T.);
#854=FACE_BOUND('',#28331,.T.);
#855=FACE_BOUND('',#28332,.T.);
#856=FACE_BOUND('',#28333,.T.);
#857=FACE_BOUND('',#28334,.T.);
#858=FACE_BOUND('',#28335,.T.);
#859=FACE_BOUND('',#28336,.T.);
#860=FACE_BOUND('',#28337,.T.);
#861=FACE_BOUND('',#28338,.T.);
#862=FACE_BOUND('',#28339,.T.);
#863=FACE_BOUND('',#28340,.T.);
#864=FACE_BOUND('',#28341,.T.);
#865=FACE_BOUND('',#28342,.T.);
#866=FACE_BOUND('',#28343,.T.);
#867=FACE_BOUND('',#28344,.T.);
#868=FACE_BOUND('',#28345,.T.);
#869=FACE_BOUND('',#28346,.T.);
#870=FACE_BOUND('',#28347,.T.);
#871=FACE_BOUND('',#28348,.T.);
#872=FACE_BOUND('',#28349,.T.);
#873=FACE_BOUND('',#28350,.T.);
#874=FACE_BOUND('',#28351,.T.);
#875=FACE_BOUND('',#28352,.T.);
#876=FACE_BOUND('',#28353,.T.);
#877=FACE_BOUND('',#28354,.T.);
#878=FACE_BOUND('',#28355,.T.);
#879=FACE_BOUND('',#28356,.T.);
#880=FACE_BOUND('',#28357,.T.);
#881=FACE_BOUND('',#28358,.T.);
#882=FACE_BOUND('',#28359,.T.);
#883=FACE_BOUND('',#28360,.T.);
#884=FACE_BOUND('',#28361,.T.);
#885=FACE_BOUND('',#28362,.T.);
#886=FACE_BOUND('',#28363,.T.);
#887=FACE_BOUND('',#28364,.T.);
#888=FACE_BOUND('',#28365,.T.);
#889=FACE_BOUND('',#28366,.T.);
#890=FACE_BOUND('',#28367,.T.);
#891=FACE_BOUND('',#28368,.T.);
#892=FACE_BOUND('',#28369,.T.);
#893=FACE_BOUND('',#28370,.T.);
#894=FACE_BOUND('',#28371,.T.);
#895=FACE_BOUND('',#28372,.T.);
#896=FACE_BOUND('',#28373,.T.);
#897=FACE_BOUND('',#28374,.T.);
#898=FACE_BOUND('',#28375,.T.);
#899=FACE_BOUND('',#28376,.T.);
#900=FACE_BOUND('',#28377,.T.);
#901=FACE_BOUND('',#28378,.T.);
#902=FACE_BOUND('',#28379,.T.);
#903=FACE_BOUND('',#28380,.T.);
#904=FACE_BOUND('',#28381,.T.);
#905=FACE_BOUND('',#28382,.T.);
#906=FACE_BOUND('',#28383,.T.);
#907=FACE_BOUND('',#28384,.T.);
#908=FACE_BOUND('',#28385,.T.);
#909=FACE_BOUND('',#28386,.T.);
#910=FACE_BOUND('',#28387,.T.);
#911=FACE_BOUND('',#28388,.T.);
#912=FACE_BOUND('',#28389,.T.);
#913=FACE_BOUND('',#28390,.T.);
#914=FACE_BOUND('',#28391,.T.);
#915=FACE_BOUND('',#28392,.T.);
#916=FACE_BOUND('',#28393,.T.);
#917=FACE_BOUND('',#28394,.T.);
#918=FACE_BOUND('',#28395,.T.);
#919=FACE_BOUND('',#28396,.T.);
#920=FACE_BOUND('',#28397,.T.);
#921=FACE_BOUND('',#28398,.T.);
#922=FACE_BOUND('',#28399,.T.);
#923=FACE_BOUND('',#28400,.T.);
#924=FACE_BOUND('',#28401,.T.);
#925=FACE_BOUND('',#28402,.T.);
#926=FACE_BOUND('',#28403,.T.);
#927=FACE_BOUND('',#28404,.T.);
#928=FACE_BOUND('',#28405,.T.);
#929=FACE_BOUND('',#28406,.T.);
#930=FACE_BOUND('',#28407,.T.);
#931=FACE_BOUND('',#28408,.T.);
#932=FACE_BOUND('',#28409,.T.);
#933=FACE_BOUND('',#28410,.T.);
#934=FACE_BOUND('',#28411,.T.);
#935=FACE_BOUND('',#28412,.T.);
#936=FACE_BOUND('',#28413,.T.);
#937=FACE_BOUND('',#28414,.T.);
#938=FACE_BOUND('',#28415,.T.);
#939=FACE_BOUND('',#28416,.T.);
#940=FACE_BOUND('',#28417,.T.);
#941=FACE_BOUND('',#28418,.T.);
#942=FACE_BOUND('',#28419,.T.);
#943=FACE_BOUND('',#28420,.T.);
#944=FACE_BOUND('',#28421,.T.);
#945=FACE_BOUND('',#28422,.T.);
#946=FACE_BOUND('',#28423,.T.);
#947=FACE_BOUND('',#28424,.T.);
#948=FACE_BOUND('',#28425,.T.);
#949=FACE_BOUND('',#28426,.T.);
#950=FACE_BOUND('',#28427,.T.);
#951=FACE_BOUND('',#28428,.T.);
#952=FACE_BOUND('',#28429,.T.);
#953=FACE_BOUND('',#28430,.T.);
#954=FACE_BOUND('',#28431,.T.);
#955=FACE_BOUND('',#28432,.T.);
#956=FACE_BOUND('',#28433,.T.);
#957=FACE_BOUND('',#28434,.T.);
#958=FACE_BOUND('',#28435,.T.);
#959=FACE_BOUND('',#28436,.T.);
#960=FACE_BOUND('',#28437,.T.);
#961=FACE_BOUND('',#28438,.T.);
#962=FACE_BOUND('',#28439,.T.);
#963=FACE_BOUND('',#28440,.T.);
#964=FACE_BOUND('',#28441,.T.);
#965=FACE_BOUND('',#28442,.T.);
#966=FACE_BOUND('',#28443,.T.);
#967=FACE_BOUND('',#28444,.T.);
#968=FACE_BOUND('',#28445,.T.);
#969=FACE_BOUND('',#28446,.T.);
#970=FACE_BOUND('',#28447,.T.);
#971=FACE_BOUND('',#28448,.T.);
#972=FACE_BOUND('',#28449,.T.);
#973=FACE_BOUND('',#28450,.T.);
#974=FACE_BOUND('',#28451,.T.);
#975=FACE_BOUND('',#28452,.T.);
#976=FACE_BOUND('',#28453,.T.);
#977=FACE_BOUND('',#28454,.T.);
#978=FACE_BOUND('',#28455,.T.);
#979=FACE_BOUND('',#28456,.T.);
#980=FACE_BOUND('',#28457,.T.);
#981=FACE_BOUND('',#28458,.T.);
#982=FACE_BOUND('',#28459,.T.);
#983=FACE_BOUND('',#28460,.T.);
#984=FACE_BOUND('',#28461,.T.);
#985=FACE_BOUND('',#28462,.T.);
#986=FACE_BOUND('',#28463,.T.);
#987=FACE_BOUND('',#28464,.T.);
#988=FACE_BOUND('',#28465,.T.);
#989=FACE_BOUND('',#28466,.T.);
#990=FACE_BOUND('',#28467,.T.);
#991=FACE_BOUND('',#28468,.T.);
#992=FACE_BOUND('',#28469,.T.);
#993=FACE_BOUND('',#28470,.T.);
#994=FACE_BOUND('',#28471,.T.);
#995=FACE_BOUND('',#28472,.T.);
#996=FACE_BOUND('',#28473,.T.);
#997=FACE_BOUND('',#28474,.T.);
#998=FACE_BOUND('',#28475,.T.);
#999=FACE_BOUND('',#28476,.T.);
#1000=FACE_BOUND('',#28477,.T.);
#1001=FACE_BOUND('',#28478,.T.);
#1002=FACE_BOUND('',#28479,.T.);
#1003=FACE_BOUND('',#28480,.T.);
#1004=FACE_BOUND('',#28481,.T.);
#1005=FACE_BOUND('',#28482,.T.);
#1006=FACE_BOUND('',#28483,.T.);
#1007=FACE_BOUND('',#28484,.T.);
#1008=FACE_BOUND('',#28485,.T.);
#1009=FACE_BOUND('',#28486,.T.);
#1010=FACE_BOUND('',#28487,.T.);
#1011=FACE_BOUND('',#28488,.T.);
#1012=FACE_BOUND('',#28489,.T.);
#1013=FACE_BOUND('',#28490,.T.);
#1014=FACE_BOUND('',#28491,.T.);
#1015=FACE_BOUND('',#28492,.T.);
#1016=FACE_BOUND('',#28493,.T.);
#1017=FACE_BOUND('',#28494,.T.);
#1018=FACE_BOUND('',#28495,.T.);
#1019=FACE_BOUND('',#28496,.T.);
#1020=FACE_BOUND('',#28497,.T.);
#1021=FACE_BOUND('',#28498,.T.);
#1022=FACE_BOUND('',#28499,.T.);
#1023=FACE_BOUND('',#28500,.T.);
#1024=FACE_BOUND('',#28501,.T.);
#1025=FACE_BOUND('',#28502,.T.);
#1026=FACE_BOUND('',#28503,.T.);
#1027=FACE_BOUND('',#28504,.T.);
#1028=FACE_BOUND('',#28505,.T.);
#1029=FACE_BOUND('',#28506,.T.);
#1030=FACE_BOUND('',#28507,.T.);
#1031=FACE_BOUND('',#28508,.T.);
#1032=FACE_BOUND('',#28509,.T.);
#1033=FACE_BOUND('',#28510,.T.);
#1034=FACE_BOUND('',#28511,.T.);
#1035=FACE_BOUND('',#28512,.T.);
#1036=FACE_BOUND('',#28513,.T.);
#1037=FACE_BOUND('',#28514,.T.);
#1038=FACE_BOUND('',#28515,.T.);
#1039=FACE_BOUND('',#28516,.T.);
#1040=FACE_BOUND('',#28517,.T.);
#1041=FACE_BOUND('',#28518,.T.);
#1042=FACE_BOUND('',#28519,.T.);
#1043=FACE_BOUND('',#28520,.T.);
#1044=FACE_BOUND('',#28521,.T.);
#1045=FACE_BOUND('',#28522,.T.);
#1046=FACE_BOUND('',#28523,.T.);
#1047=FACE_BOUND('',#28524,.T.);
#1048=FACE_BOUND('',#28525,.T.);
#1049=FACE_BOUND('',#28526,.T.);
#1050=FACE_BOUND('',#28527,.T.);
#1051=FACE_BOUND('',#28528,.T.);
#1052=FACE_BOUND('',#28529,.T.);
#1053=FACE_BOUND('',#28530,.T.);
#1054=FACE_BOUND('',#28531,.T.);
#1055=FACE_BOUND('',#28532,.T.);
#1056=FACE_BOUND('',#28533,.T.);
#1057=FACE_BOUND('',#28534,.T.);
#1058=FACE_BOUND('',#28535,.T.);
#1059=FACE_BOUND('',#28536,.T.);
#1060=FACE_BOUND('',#28537,.T.);
#1061=FACE_BOUND('',#28538,.T.);
#1062=FACE_BOUND('',#28539,.T.);
#1063=FACE_BOUND('',#28540,.T.);
#1064=FACE_BOUND('',#28541,.T.);
#1065=FACE_BOUND('',#28542,.T.);
#1066=FACE_BOUND('',#28543,.T.);
#1067=FACE_BOUND('',#28544,.T.);
#1068=FACE_BOUND('',#28545,.T.);
#1069=FACE_BOUND('',#28546,.T.);
#1070=FACE_BOUND('',#28547,.T.);
#1071=FACE_BOUND('',#28548,.T.);
#1072=FACE_BOUND('',#28549,.T.);
#1073=FACE_BOUND('',#28550,.T.);
#1074=FACE_BOUND('',#28551,.T.);
#1075=FACE_BOUND('',#28552,.T.);
#1076=FACE_BOUND('',#28553,.T.);
#1077=FACE_BOUND('',#28554,.T.);
#1078=FACE_BOUND('',#28555,.T.);
#1079=FACE_BOUND('',#28556,.T.);
#1080=FACE_BOUND('',#28557,.T.);
#1081=FACE_BOUND('',#28558,.T.);
#1082=FACE_BOUND('',#28559,.T.);
#1083=FACE_BOUND('',#28560,.T.);
#1084=FACE_BOUND('',#28561,.T.);
#1085=FACE_BOUND('',#28562,.T.);
#1086=FACE_BOUND('',#28563,.T.);
#1087=FACE_BOUND('',#28564,.T.);
#1088=FACE_BOUND('',#28565,.T.);
#1089=FACE_BOUND('',#28566,.T.);
#1090=FACE_BOUND('',#28567,.T.);
#1091=FACE_BOUND('',#28568,.T.);
#1092=FACE_BOUND('',#28569,.T.);
#1093=FACE_BOUND('',#28570,.T.);
#1094=FACE_BOUND('',#28571,.T.);
#1095=FACE_BOUND('',#28572,.T.);
#1096=FACE_BOUND('',#28573,.T.);
#1097=FACE_BOUND('',#28574,.T.);
#1098=FACE_BOUND('',#28575,.T.);
#1099=FACE_BOUND('',#28576,.T.);
#1100=FACE_BOUND('',#28577,.T.);
#1101=FACE_BOUND('',#28578,.T.);
#1102=FACE_BOUND('',#28579,.T.);
#1103=FACE_BOUND('',#28580,.T.);
#1104=FACE_BOUND('',#28581,.T.);
#1105=FACE_BOUND('',#28582,.T.);
#1106=FACE_BOUND('',#28583,.T.);
#1107=FACE_BOUND('',#28584,.T.);
#1108=FACE_BOUND('',#28585,.T.);
#1109=FACE_BOUND('',#28586,.T.);
#1110=FACE_BOUND('',#28587,.T.);
#1111=FACE_BOUND('',#28588,.T.);
#1112=FACE_BOUND('',#28589,.T.);
#1113=FACE_BOUND('',#28590,.T.);
#1114=FACE_BOUND('',#28591,.T.);
#1115=FACE_BOUND('',#28592,.T.);
#1116=FACE_BOUND('',#28593,.T.);
#1117=FACE_BOUND('',#28594,.T.);
#1118=FACE_BOUND('',#28595,.T.);
#1119=FACE_BOUND('',#28596,.T.);
#1120=FACE_BOUND('',#28597,.T.);
#1121=FACE_BOUND('',#28598,.T.);
#1122=FACE_BOUND('',#28599,.T.);
#1123=FACE_BOUND('',#28600,.T.);
#1124=FACE_BOUND('',#28601,.T.);
#1125=FACE_BOUND('',#28602,.T.);
#1126=FACE_BOUND('',#28603,.T.);
#1127=FACE_BOUND('',#28604,.T.);
#1128=FACE_BOUND('',#28605,.T.);
#1129=FACE_BOUND('',#28606,.T.);
#1130=FACE_BOUND('',#28607,.T.);
#1131=FACE_BOUND('',#28608,.T.);
#1132=FACE_BOUND('',#28609,.T.);
#1133=FACE_BOUND('',#28610,.T.);
#1134=FACE_BOUND('',#28611,.T.);
#1135=FACE_BOUND('',#28612,.T.);
#1136=FACE_BOUND('',#28613,.T.);
#1137=FACE_BOUND('',#28614,.T.);
#1138=FACE_BOUND('',#28615,.T.);
#1139=FACE_BOUND('',#28616,.T.);
#1140=FACE_BOUND('',#28617,.T.);
#1141=FACE_BOUND('',#28618,.T.);
#1142=FACE_BOUND('',#28619,.T.);
#1143=FACE_BOUND('',#28620,.T.);
#1144=FACE_BOUND('',#28621,.T.);
#1145=FACE_BOUND('',#28622,.T.);
#1146=FACE_BOUND('',#28623,.T.);
#1147=FACE_BOUND('',#28624,.T.);
#1148=FACE_BOUND('',#28625,.T.);
#1149=FACE_BOUND('',#28626,.T.);
#1150=FACE_BOUND('',#28627,.T.);
#1151=FACE_BOUND('',#28628,.T.);
#1152=FACE_BOUND('',#28629,.T.);
#1153=FACE_BOUND('',#28630,.T.);
#1154=FACE_BOUND('',#28631,.T.);
#1155=FACE_BOUND('',#28632,.T.);
#1156=FACE_BOUND('',#28633,.T.);
#1157=FACE_BOUND('',#28634,.T.);
#1158=FACE_BOUND('',#28635,.T.);
#1159=FACE_BOUND('',#28636,.T.);
#1160=FACE_BOUND('',#28637,.T.);
#1161=FACE_BOUND('',#28638,.T.);
#1162=FACE_BOUND('',#28639,.T.);
#1163=FACE_BOUND('',#28640,.T.);
#1164=FACE_BOUND('',#28641,.T.);
#1165=FACE_BOUND('',#28642,.T.);
#1166=FACE_BOUND('',#28643,.T.);
#1167=FACE_BOUND('',#28644,.T.);
#1168=FACE_BOUND('',#28645,.T.);
#1169=FACE_BOUND('',#28646,.T.);
#1170=FACE_BOUND('',#28647,.T.);
#1171=FACE_BOUND('',#28648,.T.);
#1172=FACE_BOUND('',#28649,.T.);
#1173=FACE_BOUND('',#28650,.T.);
#1174=FACE_BOUND('',#28651,.T.);
#1175=FACE_BOUND('',#28652,.T.);
#1176=FACE_BOUND('',#28653,.T.);
#1177=FACE_BOUND('',#28654,.T.);
#1178=FACE_BOUND('',#28655,.T.);
#1179=FACE_BOUND('',#28656,.T.);
#1180=FACE_BOUND('',#28657,.T.);
#1181=FACE_BOUND('',#28658,.T.);
#1182=FACE_BOUND('',#28659,.T.);
#1183=FACE_BOUND('',#28660,.T.);
#1184=FACE_BOUND('',#28661,.T.);
#1185=FACE_BOUND('',#28662,.T.);
#1186=FACE_BOUND('',#28663,.T.);
#1187=FACE_BOUND('',#28664,.T.);
#1188=FACE_BOUND('',#28665,.T.);
#1189=FACE_BOUND('',#28666,.T.);
#1190=FACE_BOUND('',#28667,.T.);
#1191=FACE_BOUND('',#28668,.T.);
#1192=FACE_BOUND('',#28669,.T.);
#1193=FACE_BOUND('',#28670,.T.);
#1194=FACE_BOUND('',#28671,.T.);
#1195=FACE_BOUND('',#28672,.T.);
#1196=FACE_BOUND('',#28673,.T.);
#1197=FACE_BOUND('',#28674,.T.);
#1198=FACE_BOUND('',#28675,.T.);
#1199=FACE_BOUND('',#28676,.T.);
#1200=FACE_BOUND('',#28677,.T.);
#1201=FACE_BOUND('',#28678,.T.);
#1202=FACE_BOUND('',#28679,.T.);
#1203=FACE_BOUND('',#28680,.T.);
#1204=FACE_BOUND('',#28681,.T.);
#1205=FACE_BOUND('',#28682,.T.);
#1206=FACE_BOUND('',#28684,.T.);
#1207=FACE_BOUND('',#28698,.T.);
#1208=FACE_BOUND('',#28700,.T.);
#1209=FACE_BOUND('',#28701,.T.);
#1210=FACE_BOUND('',#28702,.T.);
#1211=FACE_BOUND('',#28703,.T.);
#1212=FACE_BOUND('',#28704,.T.);
#1213=FACE_BOUND('',#28705,.T.);
#1214=FACE_BOUND('',#28706,.T.);
#1215=FACE_BOUND('',#28707,.T.);
#1216=FACE_BOUND('',#28708,.T.);
#1217=FACE_BOUND('',#28709,.T.);
#1218=FACE_BOUND('',#28710,.T.);
#1219=FACE_BOUND('',#28711,.T.);
#1220=FACE_BOUND('',#28712,.T.);
#1221=FACE_BOUND('',#28713,.T.);
#1222=FACE_BOUND('',#28714,.T.);
#1223=FACE_BOUND('',#28715,.T.);
#1224=FACE_BOUND('',#28716,.T.);
#1225=FACE_BOUND('',#28717,.T.);
#1226=FACE_BOUND('',#28718,.T.);
#1227=FACE_BOUND('',#28719,.T.);
#1228=FACE_BOUND('',#28720,.T.);
#1229=FACE_BOUND('',#28721,.T.);
#1230=FACE_BOUND('',#28722,.T.);
#1231=FACE_BOUND('',#28723,.T.);
#1232=FACE_BOUND('',#28724,.T.);
#1233=FACE_BOUND('',#28725,.T.);
#1234=FACE_BOUND('',#28726,.T.);
#1235=FACE_BOUND('',#28727,.T.);
#1236=FACE_BOUND('',#28728,.T.);
#1237=FACE_BOUND('',#28729,.T.);
#1238=FACE_BOUND('',#28730,.T.);
#1239=FACE_BOUND('',#28731,.T.);
#1240=FACE_BOUND('',#28732,.T.);
#1241=FACE_BOUND('',#28733,.T.);
#1242=FACE_BOUND('',#28734,.T.);
#1243=FACE_BOUND('',#28735,.T.);
#1244=FACE_BOUND('',#28736,.T.);
#1245=FACE_BOUND('',#28737,.T.);
#1246=FACE_BOUND('',#28738,.T.);
#1247=FACE_BOUND('',#28739,.T.);
#1248=FACE_BOUND('',#28740,.T.);
#1249=FACE_BOUND('',#28741,.T.);
#1250=FACE_BOUND('',#28742,.T.);
#1251=FACE_BOUND('',#28743,.T.);
#1252=FACE_BOUND('',#28744,.T.);
#1253=FACE_BOUND('',#28745,.T.);
#1254=FACE_BOUND('',#28746,.T.);
#1255=FACE_BOUND('',#28747,.T.);
#1256=FACE_BOUND('',#28748,.T.);
#1257=FACE_BOUND('',#28749,.T.);
#1258=FACE_BOUND('',#28750,.T.);
#1259=FACE_BOUND('',#28751,.T.);
#1260=FACE_BOUND('',#28752,.T.);
#1261=FACE_BOUND('',#28753,.T.);
#1262=FACE_BOUND('',#28754,.T.);
#1263=FACE_BOUND('',#28755,.T.);
#1264=FACE_BOUND('',#28756,.T.);
#1265=FACE_BOUND('',#28757,.T.);
#1266=FACE_BOUND('',#28758,.T.);
#1267=FACE_BOUND('',#28759,.T.);
#1268=FACE_BOUND('',#28760,.T.);
#1269=FACE_BOUND('',#28761,.T.);
#1270=FACE_BOUND('',#28762,.T.);
#1271=FACE_BOUND('',#28763,.T.);
#1272=FACE_BOUND('',#28764,.T.);
#1273=FACE_BOUND('',#28765,.T.);
#1274=FACE_BOUND('',#28766,.T.);
#1275=FACE_BOUND('',#28767,.T.);
#1276=FACE_BOUND('',#28768,.T.);
#1277=FACE_BOUND('',#28769,.T.);
#1278=FACE_BOUND('',#28770,.T.);
#1279=FACE_BOUND('',#28771,.T.);
#1280=FACE_BOUND('',#28772,.T.);
#1281=FACE_BOUND('',#28773,.T.);
#1282=FACE_BOUND('',#28774,.T.);
#1283=FACE_BOUND('',#28775,.T.);
#1284=FACE_BOUND('',#28776,.T.);
#1285=FACE_BOUND('',#28777,.T.);
#1286=FACE_BOUND('',#28778,.T.);
#1287=FACE_BOUND('',#28779,.T.);
#1288=FACE_BOUND('',#28780,.T.);
#1289=FACE_BOUND('',#28781,.T.);
#1290=FACE_BOUND('',#28782,.T.);
#1291=FACE_BOUND('',#28783,.T.);
#1292=FACE_BOUND('',#28784,.T.);
#1293=FACE_BOUND('',#28785,.T.);
#1294=FACE_BOUND('',#28786,.T.);
#1295=FACE_BOUND('',#28787,.T.);
#1296=FACE_BOUND('',#28788,.T.);
#1297=FACE_BOUND('',#28789,.T.);
#1298=FACE_BOUND('',#28790,.T.);
#1299=FACE_BOUND('',#28791,.T.);
#1300=FACE_BOUND('',#28792,.T.);
#1301=FACE_BOUND('',#28793,.T.);
#1302=FACE_BOUND('',#28794,.T.);
#1303=FACE_BOUND('',#28795,.T.);
#1304=FACE_BOUND('',#28796,.T.);
#1305=FACE_BOUND('',#28797,.T.);
#1306=FACE_BOUND('',#28798,.T.);
#1307=FACE_BOUND('',#28799,.T.);
#1308=FACE_BOUND('',#28800,.T.);
#1309=FACE_BOUND('',#28801,.T.);
#1310=FACE_BOUND('',#28802,.T.);
#1311=FACE_BOUND('',#28803,.T.);
#1312=FACE_BOUND('',#28804,.T.);
#1313=FACE_BOUND('',#28805,.T.);
#1314=FACE_BOUND('',#28806,.T.);
#1315=FACE_BOUND('',#28807,.T.);
#1316=FACE_BOUND('',#28808,.T.);
#1317=FACE_BOUND('',#28809,.T.);
#1318=FACE_BOUND('',#28810,.T.);
#1319=FACE_BOUND('',#28811,.T.);
#1320=FACE_BOUND('',#28812,.T.);
#1321=FACE_BOUND('',#28813,.T.);
#1322=FACE_BOUND('',#28814,.T.);
#1323=FACE_BOUND('',#28815,.T.);
#1324=FACE_BOUND('',#28816,.T.);
#1325=FACE_BOUND('',#28817,.T.);
#1326=FACE_BOUND('',#28818,.T.);
#1327=FACE_BOUND('',#28819,.T.);
#1328=FACE_BOUND('',#28820,.T.);
#1329=FACE_BOUND('',#28821,.T.);
#1330=FACE_BOUND('',#28822,.T.);
#1331=FACE_BOUND('',#28823,.T.);
#1332=FACE_BOUND('',#28824,.T.);
#1333=FACE_BOUND('',#28825,.T.);
#1334=FACE_BOUND('',#28826,.T.);
#1335=FACE_BOUND('',#28827,.T.);
#1336=FACE_BOUND('',#28828,.T.);
#1337=FACE_BOUND('',#28829,.T.);
#1338=FACE_BOUND('',#28830,.T.);
#1339=FACE_BOUND('',#28831,.T.);
#1340=FACE_BOUND('',#28832,.T.);
#1341=FACE_BOUND('',#28833,.T.);
#1342=FACE_BOUND('',#28834,.T.);
#1343=FACE_BOUND('',#28835,.T.);
#1344=FACE_BOUND('',#28836,.T.);
#1345=FACE_BOUND('',#28837,.T.);
#1346=FACE_BOUND('',#28838,.T.);
#1347=FACE_BOUND('',#28839,.T.);
#1348=FACE_BOUND('',#28840,.T.);
#1349=FACE_BOUND('',#28841,.T.);
#1350=FACE_BOUND('',#28842,.T.);
#1351=FACE_BOUND('',#28843,.T.);
#1352=FACE_BOUND('',#28844,.T.);
#1353=FACE_BOUND('',#28845,.T.);
#1354=FACE_BOUND('',#28846,.T.);
#1355=FACE_BOUND('',#28847,.T.);
#1356=FACE_BOUND('',#28848,.T.);
#1357=FACE_BOUND('',#28849,.T.);
#1358=FACE_BOUND('',#28850,.T.);
#1359=FACE_BOUND('',#28851,.T.);
#1360=FACE_BOUND('',#28852,.T.);
#1361=FACE_BOUND('',#28853,.T.);
#1362=FACE_BOUND('',#28854,.T.);
#1363=FACE_BOUND('',#28855,.T.);
#1364=FACE_BOUND('',#28856,.T.);
#1365=FACE_BOUND('',#28857,.T.);
#1366=FACE_BOUND('',#28858,.T.);
#1367=FACE_BOUND('',#28859,.T.);
#1368=FACE_BOUND('',#28860,.T.);
#1369=FACE_BOUND('',#28861,.T.);
#1370=FACE_BOUND('',#28862,.T.);
#1371=FACE_BOUND('',#28863,.T.);
#1372=FACE_BOUND('',#28864,.T.);
#1373=FACE_BOUND('',#28865,.T.);
#1374=FACE_BOUND('',#28866,.T.);
#1375=FACE_BOUND('',#28867,.T.);
#1376=FACE_BOUND('',#28868,.T.);
#1377=FACE_BOUND('',#28869,.T.);
#1378=FACE_BOUND('',#28870,.T.);
#1379=FACE_BOUND('',#28871,.T.);
#1380=FACE_BOUND('',#28872,.T.);
#1381=FACE_BOUND('',#28873,.T.);
#1382=FACE_BOUND('',#28874,.T.);
#1383=FACE_BOUND('',#28875,.T.);
#1384=FACE_BOUND('',#28876,.T.);
#1385=FACE_BOUND('',#28877,.T.);
#1386=FACE_BOUND('',#28878,.T.);
#1387=FACE_BOUND('',#28879,.T.);
#1388=FACE_BOUND('',#28880,.T.);
#1389=FACE_BOUND('',#28881,.T.);
#1390=FACE_BOUND('',#28882,.T.);
#1391=FACE_BOUND('',#28883,.T.);
#1392=FACE_BOUND('',#28884,.T.);
#1393=FACE_BOUND('',#28885,.T.);
#1394=FACE_BOUND('',#28886,.T.);
#1395=FACE_BOUND('',#28887,.T.);
#1396=FACE_BOUND('',#28888,.T.);
#1397=FACE_BOUND('',#28889,.T.);
#1398=FACE_BOUND('',#28890,.T.);
#1399=FACE_BOUND('',#28891,.T.);
#1400=FACE_BOUND('',#28892,.T.);
#1401=FACE_BOUND('',#28893,.T.);
#1402=FACE_BOUND('',#28894,.T.);
#1403=FACE_BOUND('',#28895,.T.);
#1404=FACE_BOUND('',#28896,.T.);
#1405=FACE_BOUND('',#28897,.T.);
#1406=FACE_BOUND('',#28898,.T.);
#1407=FACE_BOUND('',#28899,.T.);
#1408=FACE_BOUND('',#28900,.T.);
#1409=FACE_BOUND('',#28901,.T.);
#1410=FACE_BOUND('',#28902,.T.);
#1411=FACE_BOUND('',#28903,.T.);
#1412=FACE_BOUND('',#28904,.T.);
#1413=FACE_BOUND('',#28905,.T.);
#1414=FACE_BOUND('',#28906,.T.);
#1415=FACE_BOUND('',#28907,.T.);
#1416=FACE_BOUND('',#28908,.T.);
#1417=FACE_BOUND('',#28909,.T.);
#1418=FACE_BOUND('',#28910,.T.);
#1419=FACE_BOUND('',#28911,.T.);
#1420=FACE_BOUND('',#28912,.T.);
#1421=FACE_BOUND('',#28913,.T.);
#1422=FACE_BOUND('',#28914,.T.);
#1423=FACE_BOUND('',#28915,.T.);
#1424=FACE_BOUND('',#28916,.T.);
#1425=FACE_BOUND('',#28917,.T.);
#1426=FACE_BOUND('',#28918,.T.);
#1427=FACE_BOUND('',#28919,.T.);
#1428=FACE_BOUND('',#28920,.T.);
#1429=FACE_BOUND('',#28921,.T.);
#1430=FACE_BOUND('',#28922,.T.);
#1431=FACE_BOUND('',#28923,.T.);
#1432=FACE_BOUND('',#28924,.T.);
#1433=FACE_BOUND('',#28925,.T.);
#1434=FACE_BOUND('',#28926,.T.);
#1435=FACE_BOUND('',#28927,.T.);
#1436=FACE_BOUND('',#28928,.T.);
#1437=FACE_BOUND('',#28929,.T.);
#1438=FACE_BOUND('',#28930,.T.);
#1439=FACE_BOUND('',#28931,.T.);
#1440=FACE_BOUND('',#28932,.T.);
#1441=FACE_BOUND('',#28933,.T.);
#1442=FACE_BOUND('',#28934,.T.);
#1443=FACE_BOUND('',#28935,.T.);
#1444=FACE_BOUND('',#28936,.T.);
#1445=FACE_BOUND('',#28937,.T.);
#1446=FACE_BOUND('',#28938,.T.);
#1447=FACE_BOUND('',#28939,.T.);
#1448=FACE_BOUND('',#28940,.T.);
#1449=FACE_BOUND('',#28941,.T.);
#1450=FACE_BOUND('',#28942,.T.);
#1451=FACE_BOUND('',#28943,.T.);
#1452=FACE_BOUND('',#28944,.T.);
#1453=FACE_BOUND('',#28945,.T.);
#1454=FACE_BOUND('',#28946,.T.);
#1455=FACE_BOUND('',#28947,.T.);
#1456=FACE_BOUND('',#28948,.T.);
#1457=FACE_BOUND('',#28949,.T.);
#1458=FACE_BOUND('',#28950,.T.);
#1459=FACE_BOUND('',#28951,.T.);
#1460=FACE_BOUND('',#28952,.T.);
#1461=FACE_BOUND('',#28953,.T.);
#1462=FACE_BOUND('',#28954,.T.);
#1463=FACE_BOUND('',#28955,.T.);
#1464=FACE_BOUND('',#28961,.T.);
#1465=FACE_BOUND('',#28962,.T.);
#1466=FACE_BOUND('',#28963,.T.);
#1467=FACE_BOUND('',#28964,.T.);
#1468=FACE_BOUND('',#28965,.T.);
#1469=FACE_BOUND('',#28966,.T.);
#1470=FACE_BOUND('',#28967,.T.);
#1471=FACE_BOUND('',#28968,.T.);
#1472=FACE_BOUND('',#28969,.T.);
#1473=FACE_BOUND('',#28970,.T.);
#1474=FACE_BOUND('',#28971,.T.);
#1475=FACE_BOUND('',#28972,.T.);
#1476=FACE_BOUND('',#28973,.T.);
#1477=FACE_BOUND('',#28974,.T.);
#1478=FACE_BOUND('',#28975,.T.);
#1479=FACE_BOUND('',#28976,.T.);
#1480=FACE_BOUND('',#28977,.T.);
#1481=FACE_BOUND('',#28978,.T.);
#1482=FACE_BOUND('',#28979,.T.);
#1483=FACE_BOUND('',#28980,.T.);
#1484=FACE_BOUND('',#28981,.T.);
#1485=FACE_BOUND('',#28982,.T.);
#1486=FACE_BOUND('',#28983,.T.);
#1487=FACE_BOUND('',#28984,.T.);
#1488=FACE_BOUND('',#28985,.T.);
#1489=FACE_BOUND('',#28986,.T.);
#1490=FACE_BOUND('',#28987,.T.);
#1491=FACE_BOUND('',#28988,.T.);
#1492=FACE_BOUND('',#28989,.T.);
#1493=FACE_BOUND('',#28990,.T.);
#1494=FACE_BOUND('',#28991,.T.);
#1495=FACE_BOUND('',#28992,.T.);
#1496=FACE_BOUND('',#28993,.T.);
#1497=FACE_BOUND('',#28994,.T.);
#1498=FACE_BOUND('',#28995,.T.);
#1499=FACE_BOUND('',#28996,.T.);
#1500=FACE_BOUND('',#28997,.T.);
#1501=FACE_BOUND('',#28998,.T.);
#1502=FACE_BOUND('',#28999,.T.);
#1503=FACE_BOUND('',#29000,.T.);
#1504=FACE_BOUND('',#29001,.T.);
#1505=FACE_BOUND('',#29002,.T.);
#1506=FACE_BOUND('',#29003,.T.);
#1507=FACE_BOUND('',#29004,.T.);
#1508=FACE_BOUND('',#29005,.T.);
#1509=FACE_BOUND('',#29006,.T.);
#1510=FACE_BOUND('',#29007,.T.);
#1511=FACE_BOUND('',#29008,.T.);
#1512=FACE_BOUND('',#29009,.T.);
#1513=FACE_BOUND('',#29010,.T.);
#1514=FACE_BOUND('',#29011,.T.);
#1515=FACE_BOUND('',#29012,.T.);
#1516=FACE_BOUND('',#29013,.T.);
#1517=FACE_BOUND('',#29014,.T.);
#1518=FACE_BOUND('',#29015,.T.);
#1519=FACE_BOUND('',#29016,.T.);
#1520=FACE_BOUND('',#29017,.T.);
#1521=FACE_BOUND('',#29018,.T.);
#1522=FACE_BOUND('',#29019,.T.);
#1523=FACE_BOUND('',#29020,.T.);
#1524=FACE_BOUND('',#29021,.T.);
#1525=FACE_BOUND('',#29022,.T.);
#1526=FACE_BOUND('',#29023,.T.);
#1527=FACE_BOUND('',#29024,.T.);
#1528=FACE_BOUND('',#29025,.T.);
#1529=FACE_BOUND('',#29026,.T.);
#1530=FACE_BOUND('',#29027,.T.);
#1531=FACE_BOUND('',#29028,.T.);
#1532=FACE_BOUND('',#29029,.T.);
#1533=FACE_BOUND('',#29030,.T.);
#1534=FACE_BOUND('',#29031,.T.);
#1535=FACE_BOUND('',#29032,.T.);
#1536=FACE_BOUND('',#29033,.T.);
#1537=FACE_BOUND('',#29034,.T.);
#1538=FACE_BOUND('',#29035,.T.);
#1539=FACE_BOUND('',#29036,.T.);
#1540=FACE_BOUND('',#29037,.T.);
#1541=FACE_BOUND('',#29038,.T.);
#1542=FACE_BOUND('',#29039,.T.);
#1543=FACE_BOUND('',#29040,.T.);
#1544=FACE_BOUND('',#29041,.T.);
#1545=FACE_BOUND('',#29042,.T.);
#1546=FACE_BOUND('',#29043,.T.);
#1547=FACE_BOUND('',#29044,.T.);
#1548=FACE_BOUND('',#29045,.T.);
#1549=FACE_BOUND('',#29046,.T.);
#1550=FACE_BOUND('',#29047,.T.);
#1551=FACE_BOUND('',#29048,.T.);
#1552=FACE_BOUND('',#29049,.T.);
#1553=FACE_BOUND('',#29050,.T.);
#1554=FACE_BOUND('',#29051,.T.);
#1555=FACE_BOUND('',#29052,.T.);
#1556=FACE_BOUND('',#29053,.T.);
#1557=FACE_BOUND('',#29054,.T.);
#1558=FACE_BOUND('',#29055,.T.);
#1559=FACE_BOUND('',#29056,.T.);
#1560=FACE_BOUND('',#29057,.T.);
#1561=FACE_BOUND('',#29058,.T.);
#1562=FACE_BOUND('',#29059,.T.);
#1563=FACE_BOUND('',#29060,.T.);
#1564=FACE_BOUND('',#29061,.T.);
#1565=FACE_BOUND('',#29062,.T.);
#1566=FACE_BOUND('',#29063,.T.);
#1567=FACE_BOUND('',#29064,.T.);
#1568=FACE_BOUND('',#29065,.T.);
#1569=FACE_BOUND('',#29066,.T.);
#1570=FACE_BOUND('',#29067,.T.);
#1571=FACE_BOUND('',#29068,.T.);
#1572=FACE_BOUND('',#29069,.T.);
#1573=FACE_BOUND('',#29070,.T.);
#1574=FACE_BOUND('',#29071,.T.);
#1575=FACE_BOUND('',#29072,.T.);
#1576=FACE_BOUND('',#29073,.T.);
#1577=FACE_BOUND('',#29074,.T.);
#1578=FACE_BOUND('',#29075,.T.);
#1579=FACE_BOUND('',#29076,.T.);
#1580=FACE_BOUND('',#29077,.T.);
#1581=FACE_BOUND('',#29078,.T.);
#1582=FACE_BOUND('',#29079,.T.);
#1583=FACE_BOUND('',#29080,.T.);
#1584=FACE_BOUND('',#29081,.T.);
#1585=FACE_BOUND('',#29082,.T.);
#1586=FACE_BOUND('',#29083,.T.);
#1587=FACE_BOUND('',#29084,.T.);
#1588=FACE_BOUND('',#29085,.T.);
#1589=FACE_BOUND('',#29086,.T.);
#1590=FACE_BOUND('',#29087,.T.);
#1591=FACE_BOUND('',#29088,.T.);
#1592=FACE_BOUND('',#29089,.T.);
#1593=FACE_BOUND('',#29090,.T.);
#1594=FACE_BOUND('',#29091,.T.);
#1595=FACE_BOUND('',#29092,.T.);
#1596=FACE_BOUND('',#29093,.T.);
#1597=FACE_BOUND('',#29094,.T.);
#1598=FACE_BOUND('',#29095,.T.);
#1599=FACE_BOUND('',#29096,.T.);
#1600=FACE_BOUND('',#29097,.T.);
#1601=FACE_BOUND('',#29098,.T.);
#1602=FACE_BOUND('',#29099,.T.);
#1603=FACE_BOUND('',#29100,.T.);
#1604=FACE_BOUND('',#29101,.T.);
#1605=FACE_BOUND('',#29102,.T.);
#1606=FACE_BOUND('',#29103,.T.);
#1607=FACE_BOUND('',#29104,.T.);
#1608=FACE_BOUND('',#29105,.T.);
#1609=FACE_BOUND('',#29106,.T.);
#1610=FACE_BOUND('',#29107,.T.);
#1611=FACE_BOUND('',#29108,.T.);
#1612=FACE_BOUND('',#29109,.T.);
#1613=FACE_BOUND('',#29110,.T.);
#1614=FACE_BOUND('',#29111,.T.);
#1615=FACE_BOUND('',#29112,.T.);
#1616=FACE_BOUND('',#29113,.T.);
#1617=FACE_BOUND('',#29114,.T.);
#1618=FACE_BOUND('',#29115,.T.);
#1619=FACE_BOUND('',#29116,.T.);
#1620=FACE_BOUND('',#29117,.T.);
#1621=FACE_BOUND('',#29118,.T.);
#1622=FACE_BOUND('',#29119,.T.);
#1623=FACE_BOUND('',#29120,.T.);
#1624=FACE_BOUND('',#29121,.T.);
#1625=FACE_BOUND('',#29122,.T.);
#1626=FACE_BOUND('',#29123,.T.);
#1627=FACE_BOUND('',#29124,.T.);
#1628=FACE_BOUND('',#29125,.T.);
#1629=FACE_BOUND('',#29126,.T.);
#1630=FACE_BOUND('',#29127,.T.);
#1631=FACE_BOUND('',#29128,.T.);
#1632=FACE_BOUND('',#29129,.T.);
#1633=FACE_BOUND('',#29130,.T.);
#1634=FACE_BOUND('',#29131,.T.);
#1635=FACE_BOUND('',#29132,.T.);
#1636=FACE_BOUND('',#29133,.T.);
#1637=FACE_BOUND('',#29134,.T.);
#1638=FACE_BOUND('',#29135,.T.);
#1639=FACE_BOUND('',#29136,.T.);
#1640=FACE_BOUND('',#29137,.T.);
#1641=FACE_BOUND('',#29138,.T.);
#1642=FACE_BOUND('',#29139,.T.);
#1643=FACE_BOUND('',#29140,.T.);
#1644=FACE_BOUND('',#29141,.T.);
#1645=FACE_BOUND('',#29142,.T.);
#1646=FACE_BOUND('',#29143,.T.);
#1647=FACE_BOUND('',#29144,.T.);
#1648=FACE_BOUND('',#29145,.T.);
#1649=FACE_BOUND('',#29146,.T.);
#1650=FACE_BOUND('',#29147,.T.);
#1651=FACE_BOUND('',#29148,.T.);
#1652=FACE_BOUND('',#29149,.T.);
#1653=FACE_BOUND('',#29150,.T.);
#1654=FACE_BOUND('',#29151,.T.);
#1655=FACE_BOUND('',#29152,.T.);
#1656=FACE_BOUND('',#29153,.T.);
#1657=FACE_BOUND('',#29154,.T.);
#1658=FACE_BOUND('',#29155,.T.);
#1659=FACE_BOUND('',#29156,.T.);
#1660=FACE_BOUND('',#29157,.T.);
#1661=FACE_BOUND('',#29158,.T.);
#1662=FACE_BOUND('',#29159,.T.);
#1663=FACE_BOUND('',#29160,.T.);
#1664=FACE_BOUND('',#29161,.T.);
#1665=FACE_BOUND('',#29162,.T.);
#1666=FACE_BOUND('',#29163,.T.);
#1667=FACE_BOUND('',#29164,.T.);
#1668=FACE_BOUND('',#29165,.T.);
#1669=FACE_BOUND('',#29166,.T.);
#1670=FACE_BOUND('',#29167,.T.);
#1671=FACE_BOUND('',#29168,.T.);
#1672=FACE_BOUND('',#29169,.T.);
#1673=FACE_BOUND('',#29170,.T.);
#1674=FACE_BOUND('',#29171,.T.);
#1675=FACE_BOUND('',#29172,.T.);
#1676=FACE_BOUND('',#29173,.T.);
#1677=FACE_BOUND('',#29174,.T.);
#1678=FACE_BOUND('',#29175,.T.);
#1679=FACE_BOUND('',#29176,.T.);
#1680=FACE_BOUND('',#29177,.T.);
#1681=FACE_BOUND('',#29178,.T.);
#1682=FACE_BOUND('',#29179,.T.);
#1683=FACE_BOUND('',#29180,.T.);
#1684=FACE_BOUND('',#29181,.T.);
#1685=FACE_BOUND('',#29182,.T.);
#1686=FACE_BOUND('',#29183,.T.);
#1687=FACE_BOUND('',#29184,.T.);
#1688=FACE_BOUND('',#29185,.T.);
#1689=FACE_BOUND('',#29186,.T.);
#1690=FACE_BOUND('',#29187,.T.);
#1691=FACE_BOUND('',#29188,.T.);
#1692=FACE_BOUND('',#29189,.T.);
#1693=FACE_BOUND('',#29190,.T.);
#1694=FACE_BOUND('',#29191,.T.);
#1695=FACE_BOUND('',#29192,.T.);
#1696=FACE_BOUND('',#29193,.T.);
#1697=FACE_BOUND('',#29194,.T.);
#1698=FACE_BOUND('',#29195,.T.);
#1699=FACE_BOUND('',#29196,.T.);
#1700=FACE_BOUND('',#29197,.T.);
#1701=FACE_BOUND('',#29198,.T.);
#1702=FACE_BOUND('',#29199,.T.);
#1703=FACE_BOUND('',#29200,.T.);
#1704=FACE_BOUND('',#29201,.T.);
#1705=FACE_BOUND('',#29202,.T.);
#1706=FACE_BOUND('',#29203,.T.);
#1707=FACE_BOUND('',#29204,.T.);
#1708=FACE_BOUND('',#29205,.T.);
#1709=FACE_BOUND('',#29206,.T.);
#1710=FACE_BOUND('',#29207,.T.);
#1711=FACE_BOUND('',#29208,.T.);
#1712=FACE_BOUND('',#29209,.T.);
#1713=FACE_BOUND('',#29210,.T.);
#1714=FACE_BOUND('',#29211,.T.);
#1715=FACE_BOUND('',#29212,.T.);
#1716=FACE_BOUND('',#29213,.T.);
#1717=FACE_BOUND('',#29214,.T.);
#1718=FACE_BOUND('',#29215,.T.);
#1719=FACE_BOUND('',#29216,.T.);
#1720=FACE_BOUND('',#29218,.T.);
#1721=FACE_BOUND('',#29289,.T.);
#1722=FACE_BOUND('',#29291,.T.);
#1723=FACE_BOUND('',#29293,.T.);
#1724=FACE_BOUND('',#29297,.T.);
#1725=FACE_BOUND('',#29373,.T.);
#1726=FACE_BOUND('',#29375,.T.);
#1727=FACE_BOUND('',#29377,.T.);
#1728=FACE_BOUND('',#29381,.T.);
#1729=(
BOUNDED_CURVE()
B_SPLINE_CURVE(3,(#113475,#113476,#113477,#113478,#113479,#113480,#113481,
#113482,#113483,#113484,#113485,#113486,#113487,#113488,#113489,#113490),
 .UNSPECIFIED.,.F.,.F.)
B_SPLINE_CURVE_WITH_KNOTS((4,1,1,1,1,1,1,1,1,1,1,1,1,4),(0.,0.060042788247584,
0.141371222377395,0.225595544932924,0.308864429207092,0.38816486004432,
0.463257434984739,0.536512885135913,0.611617817006763,0.691030118817633,
0.774478150226589,0.858703197204449,0.940023204544441,1.),.UNSPECIFIED.)
CURVE()
GEOMETRIC_REPRESENTATION_ITEM()
RATIONAL_B_SPLINE_CURVE((1.00001389582334,1.00001389582334,1.00001389582334,
1.00001389582334,1.00001389582334,1.00001389582334,1.00001389582334,1.00001389582334,
1.00001389582334,1.00001389582334,1.00001389582334,1.00001389582334,1.00001389582334,
1.00001389582334,1.00001389582334,1.00001389582334))
REPRESENTATION_ITEM('')
);
#1730=(
BOUNDED_CURVE()
B_SPLINE_CURVE(3,(#113496,#113497,#113498,#113499,#113500,#113501,#113502,
#113503,#113504,#113505,#113506,#113507,#113508,#113509,#113510,#113511),
 .UNSPECIFIED.,.F.,.F.)
B_SPLINE_CURVE_WITH_KNOTS((4,1,1,1,1,1,1,1,1,1,1,1,1,4),(0.,0.0613883734612031,
0.142549216299429,0.226569566267063,0.309514053988871,0.388483661117508,
0.463334217441732,0.536400941313595,0.611266764348142,0.690361351445686,
0.773496593681541,0.857520919530913,0.93867542130663,1.),.UNSPECIFIED.)
CURVE()
GEOMETRIC_REPRESENTATION_ITEM()
RATIONAL_B_SPLINE_CURVE((1.00001399653248,1.00001399653248,1.00001399653248,
1.00001399653248,1.00001399653248,1.00001399653248,1.00001399653248,1.00001399653248,
1.00001399653248,1.00001399653248,1.00001399653248,1.00001399653248,1.00001399653248,
1.00001399653248,1.00001399653248,1.00001399653248))
REPRESENTATION_ITEM('')
);
#1731=(
BOUNDED_CURVE()
B_SPLINE_CURVE(2,(#115636,#115637,#115638),.UNSPECIFIED.,.F.,.F.)
B_SPLINE_CURVE_WITH_KNOTS((3,3),(-1.23975190889131,-0.413328514141033),
 .UNSPECIFIED.)
CURVE()
GEOMETRIC_REPRESENTATION_ITEM()
RATIONAL_B_SPLINE_CURVE((1.30231782319316,1.50378709162254,1.30231782319316))
REPRESENTATION_ITEM('')
);
#1732=(
BOUNDED_CURVE()
B_SPLINE_CURVE(2,(#115640,#115641,#115642),.UNSPECIFIED.,.F.,.F.)
B_SPLINE_CURVE_WITH_KNOTS((3,3),(-1.23975190893748,-0.413328514094878),
 .UNSPECIFIED.)
CURVE()
GEOMETRIC_REPRESENTATION_ITEM()
RATIONAL_B_SPLINE_CURVE((1.30231782317067,1.50378709164506,1.30231782317066))
REPRESENTATION_ITEM('')
);
#1733=(
BOUNDED_CURVE()
B_SPLINE_CURVE(2,(#115644,#115645,#115646),.UNSPECIFIED.,.F.,.F.)
B_SPLINE_CURVE_WITH_KNOTS((3,3),(-1.23975190893749,-0.413328514094885),
 .UNSPECIFIED.)
CURVE()
GEOMETRIC_REPRESENTATION_ITEM()
RATIONAL_B_SPLINE_CURVE((1.30231782317067,1.50378709164507,1.30231782317067))
REPRESENTATION_ITEM('')
);
#1734=(
BOUNDED_CURVE()
B_SPLINE_CURVE(2,(#115648,#115649,#115650),.UNSPECIFIED.,.F.,.F.)
B_SPLINE_CURVE_WITH_KNOTS((3,3),(0.413328514141046,0.826540211516179),
 .UNSPECIFIED.)
CURVE()
GEOMETRIC_REPRESENTATION_ITEM()
RATIONAL_B_SPLINE_CURVE((1.30231782319316,1.40305245740785,1.40305245740785))
REPRESENTATION_ITEM('')
);
#1735=(
BOUNDED_CURVE()
B_SPLINE_CURVE(2,(#115653,#115654,#115655),.UNSPECIFIED.,.F.,.F.)
B_SPLINE_CURVE_WITH_KNOTS((3,3),(0.826540211516179,1.23975190889131),
 .UNSPECIFIED.)
CURVE()
GEOMETRIC_REPRESENTATION_ITEM()
RATIONAL_B_SPLINE_CURVE((1.40305245740785,1.40305245740785,1.30231782319316))
REPRESENTATION_ITEM('')
);
#1736=(
BOUNDED_CURVE()
B_SPLINE_CURVE(2,(#115657,#115658,#115659),.UNSPECIFIED.,.F.,.F.)
B_SPLINE_CURVE_WITH_KNOTS((3,3),(0.413328514094879,1.23975190893749),
 .UNSPECIFIED.)
CURVE()
GEOMETRIC_REPRESENTATION_ITEM()
RATIONAL_B_SPLINE_CURVE((1.30231782317066,1.50378709164507,1.30231782317066))
REPRESENTATION_ITEM('')
);
#1737=(
BOUNDED_CURVE()
B_SPLINE_CURVE(2,(#115660,#115661,#115662),.UNSPECIFIED.,.F.,.F.)
B_SPLINE_CURVE_WITH_KNOTS((3,3),(0.413328514094884,1.23975190893748),
 .UNSPECIFIED.)
CURVE()
GEOMETRIC_REPRESENTATION_ITEM()
RATIONAL_B_SPLINE_CURVE((1.30231782317066,1.50378709164505,1.30231782317065))
REPRESENTATION_ITEM('')
);
#1738=(
BOUNDED_CURVE()
B_SPLINE_CURVE(3,(#116718,#116719,#116720,#116721,#116722,#116723,#116724,
#116725,#116726),.UNSPECIFIED.,.F.,.F.)
B_SPLINE_CURVE_WITH_KNOTS((4,1,1,1,1,1,4),(0.498245638802688,0.561105453430608,
0.658744313843059,0.756748145426417,0.857662812773838,0.964062246408474,
1.),.UNSPECIFIED.)
CURVE()
GEOMETRIC_REPRESENTATION_ITEM()
RATIONAL_B_SPLINE_CURVE((1.1080784066728,1.1080784066728,1.1080784066728,
1.1080784066728,1.1080784066728,1.1080784066728,1.1080784066728,1.1080784066728,
1.1080784066728))
REPRESENTATION_ITEM('')
);
#1739=(
BOUNDED_CURVE()
B_SPLINE_CURVE(2,(#116783,#116784,#116785),.UNSPECIFIED.,.F.,.F.)
B_SPLINE_CURVE_WITH_KNOTS((3,3),(-1.23975190889132,-0.413328514141037),
 .UNSPECIFIED.)
CURVE()
GEOMETRIC_REPRESENTATION_ITEM()
RATIONAL_B_SPLINE_CURVE((1.30231782319316,1.50378709162254,1.30231782319316))
REPRESENTATION_ITEM('')
);
#1740=(
BOUNDED_CURVE()
B_SPLINE_CURVE(2,(#116787,#116788,#116789),.UNSPECIFIED.,.F.,.F.)
B_SPLINE_CURVE_WITH_KNOTS((3,3),(-1.23975190893749,-0.413328514094873),
 .UNSPECIFIED.)
CURVE()
GEOMETRIC_REPRESENTATION_ITEM()
RATIONAL_B_SPLINE_CURVE((1.30231782317066,1.50378709164507,1.30231782317066))
REPRESENTATION_ITEM('')
);
#1741=(
BOUNDED_CURVE()
B_SPLINE_CURVE(2,(#116791,#116792,#116793),.UNSPECIFIED.,.F.,.F.)
B_SPLINE_CURVE_WITH_KNOTS((3,3),(-1.23975190893748,-0.413328514094879),
 .UNSPECIFIED.)
CURVE()
GEOMETRIC_REPRESENTATION_ITEM()
RATIONAL_B_SPLINE_CURVE((1.30231782317065,1.50378709164505,1.30231782317066))
REPRESENTATION_ITEM('')
);
#1742=(
BOUNDED_CURVE()
B_SPLINE_CURVE(2,(#116795,#116796,#116797),.UNSPECIFIED.,.F.,.F.)
B_SPLINE_CURVE_WITH_KNOTS((3,3),(0.413328514141045,0.826540211516179),
 .UNSPECIFIED.)
CURVE()
GEOMETRIC_REPRESENTATION_ITEM()
RATIONAL_B_SPLINE_CURVE((1.30231782319316,1.40305245740785,1.40305245740785))
REPRESENTATION_ITEM('')
);
#1743=(
BOUNDED_CURVE()
B_SPLINE_CURVE(2,(#116800,#116801,#116802),.UNSPECIFIED.,.F.,.F.)
B_SPLINE_CURVE_WITH_KNOTS((3,3),(0.826540211516179,1.23975190889132),
 .UNSPECIFIED.)
CURVE()
GEOMETRIC_REPRESENTATION_ITEM()
RATIONAL_B_SPLINE_CURVE((1.40305245740785,1.40305245740785,1.30231782319316))
REPRESENTATION_ITEM('')
);
#1744=(
BOUNDED_CURVE()
B_SPLINE_CURVE(2,(#116804,#116805,#116806),.UNSPECIFIED.,.F.,.F.)
B_SPLINE_CURVE_WITH_KNOTS((3,3),(0.41332851409488,1.23975190893749),
 .UNSPECIFIED.)
CURVE()
GEOMETRIC_REPRESENTATION_ITEM()
RATIONAL_B_SPLINE_CURVE((1.30231782317066,1.50378709164506,1.30231782317066))
REPRESENTATION_ITEM('')
);
#1745=(
BOUNDED_CURVE()
B_SPLINE_CURVE(2,(#116807,#116808,#116809),.UNSPECIFIED.,.F.,.F.)
B_SPLINE_CURVE_WITH_KNOTS((3,3),(0.413328514094886,1.23975190893748),
 .UNSPECIFIED.)
CURVE()
GEOMETRIC_REPRESENTATION_ITEM()
RATIONAL_B_SPLINE_CURVE((1.30231782317066,1.50378709164505,1.30231782317066))
REPRESENTATION_ITEM('')
);
#1746=(
BOUNDED_CURVE()
B_SPLINE_CURVE(3,(#117409,#117410,#117411,#117412,#117413,#117414,#117415,
#117416,#117417),.UNSPECIFIED.,.F.,.F.)
B_SPLINE_CURVE_WITH_KNOTS((4,1,1,1,1,1,4),(0.,0.135223490006101,0.368372760690441,
0.577807692760591,0.764911637581468,0.932796326685917,1.),.UNSPECIFIED.)
CURVE()
GEOMETRIC_REPRESENTATION_ITEM()
RATIONAL_B_SPLINE_CURVE((1.17156684956244,1.17156684956244,1.17156684956244,
1.17156684956244,1.17156684956244,1.17156684956244,1.17156684956244,1.17156684956244,
1.17156684956244))
REPRESENTATION_ITEM('')
);
#1747=(
BOUNDED_CURVE()
B_SPLINE_CURVE(3,(#117607,#117608,#117609,#117610,#117611,#117612,#117613),
 .UNSPECIFIED.,.F.,.F.)
B_SPLINE_CURVE_WITH_KNOTS((4,1,1,1,4),(0.,0.291641690547774,0.569344832932309,
0.824487948659488,0.999999966448407),.UNSPECIFIED.)
CURVE()
GEOMETRIC_REPRESENTATION_ITEM()
RATIONAL_B_SPLINE_CURVE((1.14438518125604,1.14438518125604,1.14438518125604,
1.14438518125604,1.14438518125604,1.14438518125604,1.14438518125604))
REPRESENTATION_ITEM('')
);
#1748=(
BOUNDED_CURVE()
B_SPLINE_CURVE(3,(#118540,#118541,#118542,#118543),.UNSPECIFIED.,.F.,.F.)
B_SPLINE_CURVE_WITH_KNOTS((4,4),(0.,1.),.UNSPECIFIED.)
CURVE()
GEOMETRIC_REPRESENTATION_ITEM()
RATIONAL_B_SPLINE_CURVE((1.02979156448796,0.990068747199373,0.990069478517477,
1.02979375844227))
REPRESENTATION_ITEM('')
);
#1749=(
BOUNDED_CURVE()
B_SPLINE_CURVE(3,(#120387,#120388,#120389,#120390),.UNSPECIFIED.,.F.,.F.)
B_SPLINE_CURVE_WITH_KNOTS((4,4),(0.,1.),.UNSPECIFIED.)
CURVE()
GEOMETRIC_REPRESENTATION_ITEM()
RATIONAL_B_SPLINE_CURVE((1.0350339969107,0.988321903155915,0.988322001030004,
1.03503429053297))
REPRESENTATION_ITEM('')
);
#1750=(
BOUNDED_CURVE()
B_SPLINE_CURVE(3,(#125894,#125895,#125896,#125897),.UNSPECIFIED.,.F.,.F.)
B_SPLINE_CURVE_WITH_KNOTS((4,4),(0.,1.),.UNSPECIFIED.)
CURVE()
GEOMETRIC_REPRESENTATION_ITEM()
RATIONAL_B_SPLINE_CURVE((1.1194923501161,1.03775180012471,0.997948145087754,
1.00008138500524))
REPRESENTATION_ITEM('')
);
#1751=(
BOUNDED_CURVE()
B_SPLINE_CURVE(3,(#125956,#125957,#125958,#125959,#125960,#125961),
 .UNSPECIFIED.,.F.,.F.)
B_SPLINE_CURVE_WITH_KNOTS((4,1,1,4),(0.,0.0439726678853666,0.554904538801605,
1.),.UNSPECIFIED.)
CURVE()
GEOMETRIC_REPRESENTATION_ITEM()
RATIONAL_B_SPLINE_CURVE((1.11949037511337,1.11949037511337,1.11949037511337,
1.11949037511337,1.11949037511337,1.11949037511337))
REPRESENTATION_ITEM('')
);
#1752=(
BOUNDED_CURVE()
B_SPLINE_CURVE(3,(#126614,#126615,#126616,#126617),.UNSPECIFIED.,.F.,.F.)
B_SPLINE_CURVE_WITH_KNOTS((4,4),(0.,0.999999993839391),.UNSPECIFIED.)
CURVE()
GEOMETRIC_REPRESENTATION_ITEM()
RATIONAL_B_SPLINE_CURVE((1.03503360228858,0.988322081496627,0.988322132570662,
1.03503375551068))
REPRESENTATION_ITEM('')
);
#1753=(
BOUNDED_CURVE()
B_SPLINE_CURVE(3,(#126731,#126732,#126733,#126734),.UNSPECIFIED.,.F.,.F.)
B_SPLINE_CURVE_WITH_KNOTS((4,4),(0.,1.),.UNSPECIFIED.)
CURVE()
GEOMETRIC_REPRESENTATION_ITEM()
RATIONAL_B_SPLINE_CURVE((1.03503398156237,0.988321878442041,0.988322006146192,
1.03503436467482))
REPRESENTATION_ITEM('')
);
#1754=(
BOUNDED_CURVE()
B_SPLINE_CURVE(3,(#131531,#131532,#131533,#131534),.UNSPECIFIED.,.F.,.F.)
B_SPLINE_CURVE_WITH_KNOTS((4,4),(2.53618980579517E-5,1.),.UNSPECIFIED.)
CURVE()
GEOMETRIC_REPRESENTATION_ITEM()
RATIONAL_B_SPLINE_CURVE((1.00144258776943,0.992211728886904,1.02728082050576,
1.10664986262599))
REPRESENTATION_ITEM('')
);
#1755=(
BOUNDED_CURVE()
B_SPLINE_CURVE(3,(#131667,#131668,#131669,#131670),.UNSPECIFIED.,.F.,.F.)
B_SPLINE_CURVE_WITH_KNOTS((4,4),(0.,0.99998151481627),.UNSPECIFIED.)
CURVE()
GEOMETRIC_REPRESENTATION_ITEM()
RATIONAL_B_SPLINE_CURVE((1.10666105100836,1.05697038096492,1.02464192514604,
1.00967568355171))
REPRESENTATION_ITEM('')
);
#1756=(
BOUNDED_CURVE()
B_SPLINE_CURVE(3,(#135216,#135217,#135218,#135219),.UNSPECIFIED.,.F.,.F.)
B_SPLINE_CURVE_WITH_KNOTS((4,4),(0.,1.),.UNSPECIFIED.)
CURVE()
GEOMETRIC_REPRESENTATION_ITEM()
RATIONAL_B_SPLINE_CURVE((1.1715918217896,0.942817810547867,0.942802727064813,
1.17154657134044))
REPRESENTATION_ITEM('')
);
#1757=(
BOUNDED_CURVE()
B_SPLINE_CURVE(3,(#139977,#139978,#139979,#139980),.UNSPECIFIED.,.F.,.F.)
B_SPLINE_CURVE_WITH_KNOTS((4,4),(0.,1.),.UNSPECIFIED.)
CURVE()
GEOMETRIC_REPRESENTATION_ITEM()
RATIONAL_B_SPLINE_CURVE((1.1728399592297,0.86224977517439,0.970253168357341,
1.49685013877855))
REPRESENTATION_ITEM('')
);
#1758=(
BOUNDED_CURVE()
B_SPLINE_CURVE(3,(#145857,#145858,#145859,#145860,#145861,#145862,#145863,
#145864,#145865,#145866,#145867,#145868,#145869),.UNSPECIFIED.,.F.,.F.)
B_SPLINE_CURVE_WITH_KNOTS((4,1,1,1,1,1,1,1,1,1,4),(0.,0.0361770017020252,
0.110322638446908,0.191341394631034,0.279299595253617,0.374729923390192,
0.478819817310066,0.592531700959653,0.717431194571663,0.855542845896087,
1.),.UNSPECIFIED.)
CURVE()
GEOMETRIC_REPRESENTATION_ITEM()
RATIONAL_B_SPLINE_CURVE((1.17157173846247,1.17157173846247,1.17157173846247,
1.17157173846247,1.17157173846247,1.17157173846247,1.17157173846247,1.17157173846247,
1.17157173846247,1.17157173846247,1.17157173846247,1.17157173846247,1.17157173846247))
REPRESENTATION_ITEM('')
);
#1759=(
BOUNDED_CURVE()
B_SPLINE_CURVE(3,(#146006,#146007,#146008,#146009),.UNSPECIFIED.,.F.,.F.)
B_SPLINE_CURVE_WITH_KNOTS((4,4),(0.,0.999997706678458),.UNSPECIFIED.)
CURVE()
GEOMETRIC_REPRESENTATION_ITEM()
RATIONAL_B_SPLINE_CURVE((1.17153882871445,0.942808335086217,0.942820391063934,
1.1715749966476))
REPRESENTATION_ITEM('')
);
#1760=(
BOUNDED_CURVE()
B_SPLINE_CURVE(3,(#146190,#146191,#146192,#146193),.UNSPECIFIED.,.F.,.F.)
B_SPLINE_CURVE_WITH_KNOTS((4,4),(0.,1.),.UNSPECIFIED.)
CURVE()
GEOMETRIC_REPRESENTATION_ITEM()
RATIONAL_B_SPLINE_CURVE((1.07476116149506,0.975082344906196,0.975079612909692,
1.07475296550555))
REPRESENTATION_ITEM('')
);
#1761=(
BOUNDED_CURVE()
B_SPLINE_CURVE(3,(#148249,#148250,#148251,#148252),.UNSPECIFIED.,.F.,.F.)
B_SPLINE_CURVE_WITH_KNOTS((4,4),(0.,1.),.UNSPECIFIED.)
CURVE()
GEOMETRIC_REPRESENTATION_ITEM()
RATIONAL_B_SPLINE_CURVE((1.06562254279167,0.920748224239219,1.01575223807641,
1.35063458430324))
REPRESENTATION_ITEM('')
);
#1762=(
BOUNDED_CURVE()
B_SPLINE_CURVE(3,(#155076,#155077,#155078,#155079),.UNSPECIFIED.,.F.,.F.)
B_SPLINE_CURVE_WITH_KNOTS((4,4),(0.,1.),.UNSPECIFIED.)
CURVE()
GEOMETRIC_REPRESENTATION_ITEM()
RATIONAL_B_SPLINE_CURVE((1.00307588690503,1.01543948096341,1.06507487566662,
1.15198207101464))
REPRESENTATION_ITEM('')
);
#1763=(
BOUNDED_CURVE()
B_SPLINE_CURVE(3,(#155449,#155450,#155451,#155452),.UNSPECIFIED.,.F.,.F.)
B_SPLINE_CURVE_WITH_KNOTS((4,4),(0.,1.),.UNSPECIFIED.)
CURVE()
GEOMETRIC_REPRESENTATION_ITEM()
RATIONAL_B_SPLINE_CURVE((1.02461141564327,0.991255872256879,0.991805091524064,
1.02625907344483))
REPRESENTATION_ITEM('')
);
#1764=(
BOUNDED_CURVE()
B_SPLINE_CURVE(3,(#156152,#156153,#156154,#156155),.UNSPECIFIED.,.F.,.F.)
B_SPLINE_CURVE_WITH_KNOTS((4,4),(1.38694351006516E-5,1.),.UNSPECIFIED.)
CURVE()
GEOMETRIC_REPRESENTATION_ITEM()
RATIONAL_B_SPLINE_CURVE((1.12701103586907,0.957656401969315,0.957662988299714,
1.12703079486027))
REPRESENTATION_ITEM('')
);
#1765=(
BOUNDED_CURVE()
B_SPLINE_CURVE(3,(#156811,#156812,#156813,#156814,#156815,#156816,#156817,
#156818,#156819,#156820),.UNSPECIFIED.,.F.,.F.)
B_SPLINE_CURVE_WITH_KNOTS((4,1,1,1,1,1,1,4),(0.,0.137093559948487,0.289586259168106,
0.458249167268145,0.635927168939495,0.81211997438687,0.983002488738192,
0.999999802202788),.UNSPECIFIED.)
CURVE()
GEOMETRIC_REPRESENTATION_ITEM()
RATIONAL_B_SPLINE_CURVE((1.17111220952591,1.17111220952591,1.17111220952591,
1.17111220952591,1.17111220952591,1.17111220952591,1.17111220952591,1.17111220952591,
1.17111220952591,1.17111220952591))
REPRESENTATION_ITEM('')
);
#1766=(
BOUNDED_CURVE()
B_SPLINE_CURVE(3,(#159803,#159804,#159805,#159806,#159807,#159808,#159809,
#159810,#159811,#159812,#159813),.UNSPECIFIED.,.F.,.F.)
B_SPLINE_CURVE_WITH_KNOTS((4,1,1,1,1,1,1,1,4),(0.,0.141779774422697,0.288564186808889,
0.419637721811095,0.537332459847568,0.657407795649981,0.783847578789506,
0.908572898255855,1.),.UNSPECIFIED.)
CURVE()
GEOMETRIC_REPRESENTATION_ITEM()
RATIONAL_B_SPLINE_CURVE((1.03357883859121,1.03357883859121,1.03357883859121,
1.03357883859121,1.03357883859121,1.03357883859121,1.03357883859121,1.03357883859121,
1.03357883859121,1.03357883859121,1.03357883859121))
REPRESENTATION_ITEM('')
);
#1767=(
BOUNDED_CURVE()
B_SPLINE_CURVE(3,(#159870,#159871,#159872,#159873,#159874,#159875,#159876),
 .UNSPECIFIED.,.F.,.F.)
B_SPLINE_CURVE_WITH_KNOTS((4,1,1,1,4),(0.,0.224667526957694,0.481948378364901,
0.749503179488002,1.),.UNSPECIFIED.)
CURVE()
GEOMETRIC_REPRESENTATION_ITEM()
RATIONAL_B_SPLINE_CURVE((1.24731983145218,1.24731983145218,1.24731983145218,
1.24731983145218,1.24731983145218,1.24731983145218,1.24731983145218))
REPRESENTATION_ITEM('')
);
#1768=(
BOUNDED_CURVE()
B_SPLINE_CURVE(3,(#159878,#159879,#159880,#159881,#159882,#159883,#159884,
#159885,#159886,#159887),.UNSPECIFIED.,.F.,.F.)
B_SPLINE_CURVE_WITH_KNOTS((4,1,1,1,1,1,1,4),(0.,0.122671457527971,0.275186389436719,
0.426161388513612,0.576657904418794,0.727651491077518,0.880206170558277,
1.),.UNSPECIFIED.)
CURVE()
GEOMETRIC_REPRESENTATION_ITEM()
RATIONAL_B_SPLINE_CURVE((1.26434380601904,1.26434380601904,1.26434380601904,
1.26434380601904,1.26434380601904,1.26434380601904,1.26434380601904,1.26434380601904,
1.26434380601904,1.26434380601904))
REPRESENTATION_ITEM('')
);
#1769=(
BOUNDED_CURVE()
B_SPLINE_CURVE(3,(#159888,#159889,#159890,#159891,#159892,#159893,#159894),
 .UNSPECIFIED.,.F.,.F.)
B_SPLINE_CURVE_WITH_KNOTS((4,1,1,1,4),(0.,0.253269801031687,0.52066383235046,
0.77788908313976,0.999999610731203),.UNSPECIFIED.)
CURVE()
GEOMETRIC_REPRESENTATION_ITEM()
RATIONAL_B_SPLINE_CURVE((1.24732214149726,1.24732214149726,1.24732214149726,
1.24732214149726,1.24732214149726,1.24732214149726,1.24732214149726))
REPRESENTATION_ITEM('')
);
#1770=(
BOUNDED_CURVE()
B_SPLINE_CURVE(2,(#173205,#173206,#173207),.UNSPECIFIED.,.F.,.F.)
B_SPLINE_CURVE_WITH_KNOTS((3,3),(-1.84750056124993,-0.734340623816359),
 .UNSPECIFIED.)
CURVE()
GEOMETRIC_REPRESENTATION_ITEM()
RATIONAL_B_SPLINE_CURVE((1.51230430780121,1.74625859842863,1.51230430780121))
REPRESENTATION_ITEM('')
);
#1771=(
BOUNDED_CURVE()
B_SPLINE_CURVE(2,(#173209,#173210,#173211),.UNSPECIFIED.,.F.,.F.)
B_SPLINE_CURVE_WITH_KNOTS((3,3),(-1.84750056124992,-0.734340623816352),
 .UNSPECIFIED.)
CURVE()
GEOMETRIC_REPRESENTATION_ITEM()
RATIONAL_B_SPLINE_CURVE((1.51230430780122,1.74625859842863,1.51230430780121))
REPRESENTATION_ITEM('')
);
#1772=(
BOUNDED_CURVE()
B_SPLINE_CURVE(2,(#173213,#173214,#173215),.UNSPECIFIED.,.F.,.F.)
B_SPLINE_CURVE_WITH_KNOTS((3,3),(-1.84750056124992,-0.734340623816351),
 .UNSPECIFIED.)
CURVE()
GEOMETRIC_REPRESENTATION_ITEM()
RATIONAL_B_SPLINE_CURVE((1.51230430780122,1.74625859842864,1.51230430780121))
REPRESENTATION_ITEM('')
);
#1773=(
BOUNDED_CURVE()
B_SPLINE_CURVE(2,(#173220,#173221,#173222),.UNSPECIFIED.,.F.,.F.)
B_SPLINE_CURVE_WITH_KNOTS((3,3),(0.734340623816355,1.8475005612499),
 .UNSPECIFIED.)
CURVE()
GEOMETRIC_REPRESENTATION_ITEM()
RATIONAL_B_SPLINE_CURVE((1.5123043078012,1.7462585984286,1.5123043078012))
REPRESENTATION_ITEM('')
);
#1774=(
BOUNDED_CURVE()
B_SPLINE_CURVE(2,(#173224,#173225,#173226),.UNSPECIFIED.,.F.,.F.)
B_SPLINE_CURVE_WITH_KNOTS((3,3),(0.734340623816354,1.84750056124992),
 .UNSPECIFIED.)
CURVE()
GEOMETRIC_REPRESENTATION_ITEM()
RATIONAL_B_SPLINE_CURVE((1.51230430780121,1.74625859842862,1.51230430780121))
REPRESENTATION_ITEM('')
);
#1775=(
BOUNDED_CURVE()
B_SPLINE_CURVE(2,(#173227,#173228,#173229),.UNSPECIFIED.,.F.,.F.)
B_SPLINE_CURVE_WITH_KNOTS((3,3),(0.734340623816358,1.84750056124993),
 .UNSPECIFIED.)
CURVE()
GEOMETRIC_REPRESENTATION_ITEM()
RATIONAL_B_SPLINE_CURVE((1.51230430780122,1.74625859842864,1.51230430780122))
REPRESENTATION_ITEM('')
);
#1776=(
BOUNDED_CURVE()
B_SPLINE_CURVE(2,(#176260,#176261,#176262),.UNSPECIFIED.,.F.,.F.)
B_SPLINE_CURVE_WITH_KNOTS((3,3),(1.60808462077175,3.73981215786375),
 .UNSPECIFIED.)
CURVE()
GEOMETRIC_REPRESENTATION_ITEM()
RATIONAL_B_SPLINE_CURVE((1.37704917963476,1.5195025430206,1.37704917962903))
REPRESENTATION_ITEM('')
);
#1777=(
BOUNDED_CURVE()
B_SPLINE_CURVE(2,(#176266,#176267,#176268),.UNSPECIFIED.,.F.,.F.)
B_SPLINE_CURVE_WITH_KNOTS((3,3),(1.60809643499364,3.73983031850846),
 .UNSPECIFIED.)
CURVE()
GEOMETRIC_REPRESENTATION_ITEM()
RATIONAL_B_SPLINE_CURVE((1.37705242397036,1.51950612297573,1.37705242396606))
REPRESENTATION_ITEM('')
);
#1778=(
BOUNDED_CURVE()
B_SPLINE_CURVE(2,(#176272,#176273,#176274),.UNSPECIFIED.,.F.,.F.)
B_SPLINE_CURVE_WITH_KNOTS((3,3),(-3.73983031850955,-1.60809643499435),
 .UNSPECIFIED.)
CURVE()
GEOMETRIC_REPRESENTATION_ITEM()
RATIONAL_B_SPLINE_CURVE((1.37705242396626,1.51950612297595,1.37705242397056))
REPRESENTATION_ITEM('')
);
#1779=(
BOUNDED_CURVE()
B_SPLINE_CURVE(2,(#176278,#176279,#176280),.UNSPECIFIED.,.F.,.F.)
B_SPLINE_CURVE_WITH_KNOTS((3,3),(1.60808462077176,3.73981215785305),
 .UNSPECIFIED.)
CURVE()
GEOMETRIC_REPRESENTATION_ITEM()
RATIONAL_B_SPLINE_CURVE((1.37704917963477,1.51950254301989,1.37704917963046))
REPRESENTATION_ITEM('')
);
#1780=(
BOUNDED_CURVE()
B_SPLINE_CURVE(2,(#176284,#176285,#176286),.UNSPECIFIED.,.F.,.F.)
B_SPLINE_CURVE_WITH_KNOTS((3,3),(1.6080964349947,3.73983031851011),
 .UNSPECIFIED.)
CURVE()
GEOMETRIC_REPRESENTATION_ITEM()
RATIONAL_B_SPLINE_CURVE((1.37705242397066,1.51950612297606,1.37705242396636))
REPRESENTATION_ITEM('')
);
#1781=(
BOUNDED_CURVE()
B_SPLINE_CURVE(2,(#176295,#176296,#176297),.UNSPECIFIED.,.F.,.F.)
B_SPLINE_CURVE_WITH_KNOTS((3,3),(1.60809643499431,3.73983031850951),
 .UNSPECIFIED.)
CURVE()
GEOMETRIC_REPRESENTATION_ITEM()
RATIONAL_B_SPLINE_CURVE((1.37705242397056,1.51950612297595,1.37705242396626))
REPRESENTATION_ITEM('')
);
#1782=(
BOUNDED_CURVE()
B_SPLINE_CURVE(2,(#176302,#176303,#176304),.UNSPECIFIED.,.F.,.F.)
B_SPLINE_CURVE_WITH_KNOTS((3,3),(1.76947846838518,3.98831685496983),
 .UNSPECIFIED.)
CURVE()
GEOMETRIC_REPRESENTATION_ITEM()
RATIONAL_B_SPLINE_CURVE((1.42161885175909,1.56868287088003,1.4216188517602))
REPRESENTATION_ITEM('')
);
#1783=(
BOUNDED_CURVE()
B_SPLINE_CURVE(2,(#176308,#176309,#176310),.UNSPECIFIED.,.F.,.F.)
B_SPLINE_CURVE_WITH_KNOTS((3,3),(-3.98831685495251,-1.76947846838545),
 .UNSPECIFIED.)
CURVE()
GEOMETRIC_REPRESENTATION_ITEM()
RATIONAL_B_SPLINE_CURVE((1.42161885176135,1.56868287087821,1.42161885175878))
REPRESENTATION_ITEM('')
);
#1784=(
BOUNDED_CURVE()
B_SPLINE_CURVE(2,(#176314,#176315,#176316),.UNSPECIFIED.,.F.,.F.)
B_SPLINE_CURVE_WITH_KNOTS((3,3),(1.76947846838546,3.98831685495253),
 .UNSPECIFIED.)
CURVE()
GEOMETRIC_REPRESENTATION_ITEM()
RATIONAL_B_SPLINE_CURVE((1.42161885175877,1.56868287087821,1.42161885176135))
REPRESENTATION_ITEM('')
);
#1785=(
BOUNDED_CURVE()
B_SPLINE_CURVE(2,(#176320,#176321,#176322),.UNSPECIFIED.,.F.,.F.)
B_SPLINE_CURVE_WITH_KNOTS((3,3),(1.76947846838366,3.98831685496745),
 .UNSPECIFIED.)
CURVE()
GEOMETRIC_REPRESENTATION_ITEM()
RATIONAL_B_SPLINE_CURVE((1.42161885175867,1.56868287087957,1.42161885175978))
REPRESENTATION_ITEM('')
);
#1786=(
BOUNDED_CURVE()
B_SPLINE_CURVE(2,(#176326,#176327,#176328),.UNSPECIFIED.,.F.,.F.)
B_SPLINE_CURVE_WITH_KNOTS((3,3),(-3.98831685495252,-1.76947846838541),
 .UNSPECIFIED.)
CURVE()
GEOMETRIC_REPRESENTATION_ITEM()
RATIONAL_B_SPLINE_CURVE((1.42161885176135,1.56868287087821,1.42161885175877))
REPRESENTATION_ITEM('')
);
#1787=(
BOUNDED_CURVE()
B_SPLINE_CURVE(2,(#176337,#176338,#176339),.UNSPECIFIED.,.F.,.F.)
B_SPLINE_CURVE_WITH_KNOTS((3,3),(-3.98831685495253,-1.7694784683854),
 .UNSPECIFIED.)
CURVE()
GEOMETRIC_REPRESENTATION_ITEM()
RATIONAL_B_SPLINE_CURVE((1.42161885176135,1.56868287087822,1.42161885175877))
REPRESENTATION_ITEM('')
);
#1788=(
BOUNDED_CURVE()
B_SPLINE_CURVE(2,(#179504,#179505,#179506),.UNSPECIFIED.,.F.,.F.)
B_SPLINE_CURVE_WITH_KNOTS((3,3),(1.60808462077176,3.73981215786377),
 .UNSPECIFIED.)
CURVE()
GEOMETRIC_REPRESENTATION_ITEM()
RATIONAL_B_SPLINE_CURVE((1.37704917963476,1.51950254302061,1.37704917962903))
REPRESENTATION_ITEM('')
);
#1789=(
BOUNDED_CURVE()
B_SPLINE_CURVE(2,(#179510,#179511,#179512),.UNSPECIFIED.,.F.,.F.)
B_SPLINE_CURVE_WITH_KNOTS((3,3),(1.608096434994,3.73983031850901),
 .UNSPECIFIED.)
CURVE()
GEOMETRIC_REPRESENTATION_ITEM()
RATIONAL_B_SPLINE_CURVE((1.37705242397046,1.51950612297584,1.37705242396616))
REPRESENTATION_ITEM('')
);
#1790=(
BOUNDED_CURVE()
B_SPLINE_CURVE(2,(#179516,#179517,#179518),.UNSPECIFIED.,.F.,.F.)
B_SPLINE_CURVE_WITH_KNOTS((3,3),(-3.73983031850899,-1.60809643499399),
 .UNSPECIFIED.)
CURVE()
GEOMETRIC_REPRESENTATION_ITEM()
RATIONAL_B_SPLINE_CURVE((1.37705242396616,1.51950612297584,1.37705242397046))
REPRESENTATION_ITEM('')
);
#1791=(
BOUNDED_CURVE()
B_SPLINE_CURVE(2,(#179522,#179523,#179524),.UNSPECIFIED.,.F.,.F.)
B_SPLINE_CURVE_WITH_KNOTS((3,3),(1.60808462077176,3.73981215785304),
 .UNSPECIFIED.)
CURVE()
GEOMETRIC_REPRESENTATION_ITEM()
RATIONAL_B_SPLINE_CURVE((1.37704917963476,1.51950254301988,1.37704917963046))
REPRESENTATION_ITEM('')
);
#1792=(
BOUNDED_CURVE()
B_SPLINE_CURVE(2,(#179528,#179529,#179530),.UNSPECIFIED.,.F.,.F.)
B_SPLINE_CURVE_WITH_KNOTS((3,3),(1.60809643499362,3.73983031850844),
 .UNSPECIFIED.)
CURVE()
GEOMETRIC_REPRESENTATION_ITEM()
RATIONAL_B_SPLINE_CURVE((1.37705242397036,1.51950612297573,1.37705242396606))
REPRESENTATION_ITEM('')
);
#1793=(
BOUNDED_CURVE()
B_SPLINE_CURVE(2,(#179539,#179540,#179541),.UNSPECIFIED.,.F.,.F.)
B_SPLINE_CURVE_WITH_KNOTS((3,3),(1.60809643499432,3.73983031850951),
 .UNSPECIFIED.)
CURVE()
GEOMETRIC_REPRESENTATION_ITEM()
RATIONAL_B_SPLINE_CURVE((1.37705242397056,1.51950612297595,1.37705242396626))
REPRESENTATION_ITEM('')
);
#1794=(
BOUNDED_CURVE()
B_SPLINE_CURVE(2,(#179546,#179547,#179548),.UNSPECIFIED.,.F.,.F.)
B_SPLINE_CURVE_WITH_KNOTS((3,3),(1.76947846838519,3.98831685496984),
 .UNSPECIFIED.)
CURVE()
GEOMETRIC_REPRESENTATION_ITEM()
RATIONAL_B_SPLINE_CURVE((1.4216188517591,1.56868287088004,1.4216188517602))
REPRESENTATION_ITEM('')
);
#1795=(
BOUNDED_CURVE()
B_SPLINE_CURVE(2,(#179552,#179553,#179554),.UNSPECIFIED.,.F.,.F.)
B_SPLINE_CURVE_WITH_KNOTS((3,3),(-3.98831685495251,-1.76947846838546),
 .UNSPECIFIED.)
CURVE()
GEOMETRIC_REPRESENTATION_ITEM()
RATIONAL_B_SPLINE_CURVE((1.42161885176135,1.56868287087821,1.42161885175877))
REPRESENTATION_ITEM('')
);
#1796=(
BOUNDED_CURVE()
B_SPLINE_CURVE(2,(#179558,#179559,#179560),.UNSPECIFIED.,.F.,.F.)
B_SPLINE_CURVE_WITH_KNOTS((3,3),(1.76947846838545,3.98831685495252),
 .UNSPECIFIED.)
CURVE()
GEOMETRIC_REPRESENTATION_ITEM()
RATIONAL_B_SPLINE_CURVE((1.42161885175877,1.56868287087821,1.42161885176135))
REPRESENTATION_ITEM('')
);
#1797=(
BOUNDED_CURVE()
B_SPLINE_CURVE(2,(#179564,#179565,#179566),.UNSPECIFIED.,.F.,.F.)
B_SPLINE_CURVE_WITH_KNOTS((3,3),(1.76947846838366,3.98831685496743),
 .UNSPECIFIED.)
CURVE()
GEOMETRIC_REPRESENTATION_ITEM()
RATIONAL_B_SPLINE_CURVE((1.42161885175867,1.56868287087956,1.42161885175977))
REPRESENTATION_ITEM('')
);
#1798=(
BOUNDED_CURVE()
B_SPLINE_CURVE(2,(#179570,#179571,#179572),.UNSPECIFIED.,.F.,.F.)
B_SPLINE_CURVE_WITH_KNOTS((3,3),(-3.98831685495253,-1.76947846838542),
 .UNSPECIFIED.)
CURVE()
GEOMETRIC_REPRESENTATION_ITEM()
RATIONAL_B_SPLINE_CURVE((1.42161885176134,1.56868287087821,1.42161885175876))
REPRESENTATION_ITEM('')
);
#1799=(
BOUNDED_CURVE()
B_SPLINE_CURVE(2,(#179581,#179582,#179583),.UNSPECIFIED.,.F.,.F.)
B_SPLINE_CURVE_WITH_KNOTS((3,3),(-3.98831685495253,-1.76947846838542),
 .UNSPECIFIED.)
CURVE()
GEOMETRIC_REPRESENTATION_ITEM()
RATIONAL_B_SPLINE_CURVE((1.42161885176135,1.56868287087821,1.42161885175877))
REPRESENTATION_ITEM('')
);
#1800=(
BOUNDED_CURVE()
B_SPLINE_CURVE(2,(#182624,#182625,#182626),.UNSPECIFIED.,.F.,.F.)
B_SPLINE_CURVE_WITH_KNOTS((3,3),(0.462569328702153,0.587652141350747),
 .UNSPECIFIED.)
CURVE()
GEOMETRIC_REPRESENTATION_ITEM()
RATIONAL_B_SPLINE_CURVE((1.3055338176145,1.33529904244958,1.35882091219323))
REPRESENTATION_ITEM('')
);
#1801=(
BOUNDED_CURVE()
B_SPLINE_CURVE(2,(#183748,#183749,#183750),.UNSPECIFIED.,.F.,.F.)
B_SPLINE_CURVE_WITH_KNOTS((3,3),(-1.97427612804245,-1.83367684633348),
 .UNSPECIFIED.)
CURVE()
GEOMETRIC_REPRESENTATION_ITEM()
RATIONAL_B_SPLINE_CURVE((1.43398246254344,1.46667622338746,1.49251235895387))
REPRESENTATION_ITEM('')
);
#1802=(
BOUNDED_CURVE()
B_SPLINE_CURVE(2,(#186587,#186588,#186589),.UNSPECIFIED.,.F.,.F.)
B_SPLINE_CURVE_WITH_KNOTS((3,3),(1.17484908943589,1.45283332058119),
 .UNSPECIFIED.)
CURVE()
GEOMETRIC_REPRESENTATION_ITEM()
RATIONAL_B_SPLINE_CURVE((1.26057059861676,1.27619589726591,1.28462728942758))
REPRESENTATION_ITEM('')
);
#1803=(
BOUNDED_CURVE()
B_SPLINE_CURVE(2,(#186592,#186593,#186594),.UNSPECIFIED.,.F.,.F.)
B_SPLINE_CURVE_WITH_KNOTS((3,3),(1.81320048054135,2.07306669608502),
 .UNSPECIFIED.)
CURVE()
GEOMETRIC_REPRESENTATION_ITEM()
RATIONAL_B_SPLINE_CURVE((1.22106645430084,1.21305223086313,1.19820004130138))
REPRESENTATION_ITEM('')
);
#1804=(
BOUNDED_CURVE()
B_SPLINE_CURVE(2,(#186598,#186599,#186600),.UNSPECIFIED.,.F.,.F.)
B_SPLINE_CURVE_WITH_KNOTS((3,3),(-1.45283332058118,-1.17484908943588),
 .UNSPECIFIED.)
CURVE()
GEOMETRIC_REPRESENTATION_ITEM()
RATIONAL_B_SPLINE_CURVE((1.28462728942758,1.27619589726592,1.26057059861677))
REPRESENTATION_ITEM('')
);
#1805=(
BOUNDED_CURVE()
B_SPLINE_CURVE(2,(#186604,#186605,#186606),.UNSPECIFIED.,.F.,.F.)
B_SPLINE_CURVE_WITH_KNOTS((3,3),(-2.07306669608501,-1.81320048054134),
 .UNSPECIFIED.)
CURVE()
GEOMETRIC_REPRESENTATION_ITEM()
RATIONAL_B_SPLINE_CURVE((1.19820004130138,1.21305223086313,1.22106645430084))
REPRESENTATION_ITEM('')
);
#1806=TOROIDAL_SURFACE('',#79562,11.,0.5);
#1807=TOROIDAL_SURFACE('',#79569,11.75,0.5);
#1808=TOROIDAL_SURFACE('',#79572,10.5,0.5);
#1809=TOROIDAL_SURFACE('',#79582,10.5,0.5);
#1810=TOROIDAL_SURFACE('',#79596,8.25,0.5);
#1811=TOROIDAL_SURFACE('',#79627,7.,0.5);
#1812=TOROIDAL_SURFACE('',#79657,10.,0.5);
#1813=TOROIDAL_SURFACE('',#79691,10.,0.5);
#1814=TOROIDAL_SURFACE('',#79762,26.,1.5);
#1815=TOROIDAL_SURFACE('',#79767,7.,1.5);
#1816=TOROIDAL_SURFACE('',#79770,26.,1.5);
#1817=TOROIDAL_SURFACE('',#79776,66.,1.5);
#1818=TOROIDAL_SURFACE('',#79792,4.,1.5);
#1819=TOROIDAL_SURFACE('',#79796,4.,1.5);
#1820=TOROIDAL_SURFACE('',#79803,4.,1.5);
#1821=TOROIDAL_SURFACE('',#79808,4.,1.5);
#1822=TOROIDAL_SURFACE('',#79811,36.,1.5);
#1823=TOROIDAL_SURFACE('',#79813,36.,1.5);
#1824=TOROIDAL_SURFACE('',#79817,36.,1.5);
#1825=TOROIDAL_SURFACE('',#79885,66.,1.5);
#1826=TOROIDAL_SURFACE('',#79890,26.,1.5);
#1827=TOROIDAL_SURFACE('',#79895,7.,1.5);
#1828=TOROIDAL_SURFACE('',#79898,26.,1.5);
#1829=TOROIDAL_SURFACE('',#79903,4.,1.5);
#1830=TOROIDAL_SURFACE('',#79906,36.,1.5);
#1831=TOROIDAL_SURFACE('',#79908,36.,1.5);
#1832=TOROIDAL_SURFACE('',#79910,4.,1.5);
#1833=TOROIDAL_SURFACE('',#79914,4.,1.5);
#1834=TOROIDAL_SURFACE('',#79921,4.,1.5);
#1835=TOROIDAL_SURFACE('',#79928,36.,1.5);
#1836=TOROIDAL_SURFACE('',#80002,36.5,1.);
#1837=TOROIDAL_SURFACE('',#80005,66.5,1.);
#1838=TOROIDAL_SURFACE('',#80008,4.5,1.);
#1839=TOROIDAL_SURFACE('',#80012,4.5,1.);
#1840=TOROIDAL_SURFACE('',#80022,14.,1.5);
#1841=TOROIDAL_SURFACE('',#80027,14.,1.5);
#1842=TOROIDAL_SURFACE('',#80031,8.016437378118,1.5);
#1843=TOROIDAL_SURFACE('',#80089,4.498378496899,1.);
#1844=TOROIDAL_SURFACE('',#80091,14.5,1.);
#1845=TOROIDAL_SURFACE('',#80097,14.5,1.);
#1846=TOROIDAL_SURFACE('',#80104,14.5,1.);
#1847=TOROIDAL_SURFACE('',#80111,14.5,1.);
#1848=TOROIDAL_SURFACE('',#80114,4.498378496898,1.);
#1849=TOROIDAL_SURFACE('',#80131,26.64683059909,1.);
#1850=TOROIDAL_SURFACE('',#80154,10.5,1.);
#1851=TOROIDAL_SURFACE('',#80169,10.5,1.);
#1852=TOROIDAL_SURFACE('',#80170,10.55051025722,1.);
#1853=TOROIDAL_SURFACE('',#80173,2.449489742783,1.);
#1854=TOROIDAL_SURFACE('',#80182,2.449489742783,1.);
#1855=TOROIDAL_SURFACE('',#80184,10.55051025722,1.);
#1856=TOROIDAL_SURFACE('',#80186,13.,1.5);
#1857=TOROIDAL_SURFACE('',#80197,3.998378496899,1.5);
#1858=TOROIDAL_SURFACE('',#80227,39.5,0.5);
#1859=TOROIDAL_SURFACE('',#80239,39.5,0.5);
#1860=TOROIDAL_SURFACE('',#80264,7.5,0.5);
#1861=TOROIDAL_SURFACE('',#80267,29.5,0.5);
#1862=TOROIDAL_SURFACE('',#80270,29.5,0.5);
#1863=TOROIDAL_SURFACE('',#80276,7.5,0.5);
#1864=TOROIDAL_SURFACE('',#80284,29.5,0.5);
#1865=TOROIDAL_SURFACE('',#80287,29.5,0.5);
#1866=TOROIDAL_SURFACE('',#80290,7.5,0.5);
#1867=TOROIDAL_SURFACE('',#80294,7.5,0.5);
#1868=TOROIDAL_SURFACE('',#80326,3.998378496898,1.5);
#1869=TOROIDAL_SURFACE('',#80333,13.,1.5);
#1870=TOROIDAL_SURFACE('',#80345,3.,1.5);
#1871=TOROIDAL_SURFACE('',#80355,3.,1.5);
#1872=TOROIDAL_SURFACE('',#80359,36.5,1.);
#1873=TOROIDAL_SURFACE('',#80360,66.5,1.);
#1874=TOROIDAL_SURFACE('',#80367,14.,1.5);
#1875=TOROIDAL_SURFACE('',#80370,14.,1.5);
#1876=TOROIDAL_SURFACE('',#80371,26.6468278765,1.);
#1877=TOROIDAL_SURFACE('',#80375,8.,1.5);
#1878=TOROIDAL_SURFACE('',#80380,21.,0.5);
#1879=TOROIDAL_SURFACE('',#80400,18.5,1.5);
#1880=TOROIDAL_SURFACE('',#80403,2.866784855558,1.5);
#1881=TOROIDAL_SURFACE('',#80406,2.866784855558,1.5);
#1882=TOROIDAL_SURFACE('',#80441,2.866784855558,1.5);
#1883=TOROIDAL_SURFACE('',#80446,2.866784855558,1.5);
#1884=TOROIDAL_SURFACE('',#80451,2.866784855558,1.5);
#1885=TOROIDAL_SURFACE('',#80473,2.866784855558,1.5);
#1886=TOROIDAL_SURFACE('',#80583,6.75,0.25);
#1887=TOROIDAL_SURFACE('',#80586,8.25,0.5);
#1888=TOROIDAL_SURFACE('',#80621,9.75,0.25);
#1889=TOROIDAL_SURFACE('',#80625,11.25,0.25);
#1890=TOROIDAL_SURFACE('',#80638,11.25,0.25);
#1891=TOROIDAL_SURFACE('',#80642,9.75,0.25);
#1892=TOROIDAL_SURFACE('',#80720,9.75,0.25);
#1893=TOROIDAL_SURFACE('',#80724,11.25,0.25);
#1894=TOROIDAL_SURFACE('',#80737,11.25,0.25);
#1895=TOROIDAL_SURFACE('',#80741,9.75,0.25);
#1896=TOROIDAL_SURFACE('',#80767,26.5,1.);
#1897=TOROIDAL_SURFACE('',#80779,26.5,0.5);
#1898=TOROIDAL_SURFACE('',#80902,5.84208667428926,0.959420631745662);
#1899=TOROIDAL_SURFACE('',#80915,9.5,0.5);
#1900=TOROIDAL_SURFACE('',#80918,9.5,0.5);
#1901=TOROIDAL_SURFACE('',#80921,9.5,0.5);
#1902=TOROIDAL_SURFACE('',#80926,7.5,0.5);
#1903=TOROIDAL_SURFACE('',#80952,26.5,1.);
#1904=TOROIDAL_SURFACE('',#80964,26.5,0.5);
#1905=TOROIDAL_SURFACE('',#80993,10.88886271061,0.7);
#1906=TOROIDAL_SURFACE('',#80996,12.35,1.3);
#1907=TOROIDAL_SURFACE('',#81028,10.85,0.5);
#1908=TOROIDAL_SURFACE('',#81037,12.35,1.);
#1909=TOROIDAL_SURFACE('',#81040,10.88886271061,1.);
#1910=CONICAL_SURFACE('',#79555,9.799780026165,0.785375619840672);
#1911=CONICAL_SURFACE('',#79616,13.79977495601,0.785381825805275);
#1912=CONICAL_SURFACE('',#79634,5.799851372624,0.785372339464152);
#1913=CONICAL_SURFACE('',#79652,16.375,0.21711131448682);
#1914=CONICAL_SURFACE('',#79653,17.175,0.7853981625);
#1915=CONICAL_SURFACE('',#79664,8.699805279292,0.785376526397671);
#1916=CONICAL_SURFACE('',#79681,11.25,0.7853981625);
#1917=CONICAL_SURFACE('',#79688,7.75000000000001,1.04719755);
#1918=CONICAL_SURFACE('',#79689,7.95,0.7853981625);
#1919=CONICAL_SURFACE('',#79698,8.699805279292,0.785376526397671);
#1920=CONICAL_SURFACE('',#79716,11.25,0.7853981625);
#1921=CONICAL_SURFACE('',#79723,7.75000000000001,1.04719755);
#1922=CONICAL_SURFACE('',#79724,7.95,0.7853981625);
#1923=CONICAL_SURFACE('',#80315,9.79989529474,0.785387399312301);
#1924=CONICAL_SURFACE('',#80396,20.37470056578,0.174533028825274);
#1925=CONICAL_SURFACE('',#80430,1.183506656857,0.0174532924999985);
#1926=CONICAL_SURFACE('',#80434,1.183506656857,0.0174532924999985);
#1927=CONICAL_SURFACE('',#80455,1.183506656857,0.0174532924999985);
#1928=CONICAL_SURFACE('',#80460,0.816493292676001,0.0174532924999985);
#1929=CONICAL_SURFACE('',#80464,1.189214422822,0.0174532924999985);
#1930=CONICAL_SURFACE('',#80467,1.189214422821,0.0174532924999985);
#1931=CONICAL_SURFACE('',#80476,1.183506656857,0.0174532924999985);
#1932=CONICAL_SURFACE('',#80479,0.816493289244397,0.0174532924999985);
#1933=CONICAL_SURFACE('',#80540,9.49999999999999,0.7853981625);
#1934=CONICAL_SURFACE('',#80555,7.25,1.04719755);
#1935=CONICAL_SURFACE('',#80571,10.25,1.04719755);
#1936=CONICAL_SURFACE('',#80573,9.99999999999999,1.04719755);
#1937=CONICAL_SURFACE('',#80592,9.49999999999999,0.7853981625);
#1938=CONICAL_SURFACE('',#80594,10.25,0.7853981625);
#1939=CONICAL_SURFACE('',#80684,12.750003108,0.785398266415682);
#1940=CONICAL_SURFACE('',#80686,15.,0.7853981625);
#1941=CONICAL_SURFACE('',#80695,15.,0.7853981625);
#1942=CONICAL_SURFACE('',#80785,15.31367390024,0.849141474959914);
#1943=CONICAL_SURFACE('',#80792,15.125,0.849141474959914);
#1944=CONICAL_SURFACE('',#80813,12.750003108,0.785398266415682);
#1945=CONICAL_SURFACE('',#80815,15.,0.7853981625);
#1946=CONICAL_SURFACE('',#80824,15.,0.7853981625);
#1947=CONICAL_SURFACE('',#80853,2.05,1.0297442575);
#1948=CONICAL_SURFACE('',#80859,5.5,0.7853981625);
#1949=CONICAL_SURFACE('',#80871,7.,0.7853981625);
#1950=CONICAL_SURFACE('',#80878,6.,1.04719755);
#1951=CONICAL_SURFACE('',#80890,2.55,0.7853981625);
#1952=CONICAL_SURFACE('',#80892,3.05,0.7853981625);
#1953=CONICAL_SURFACE('',#80894,5.5,0.7853981625);
#1954=CONICAL_SURFACE('',#80896,4.9,0.7853981625);
#1955=CONICAL_SURFACE('',#80948,7.,0.7853981625);
#1956=CONICAL_SURFACE('',#80970,15.31367390024,0.849141474959914);
#1957=CONICAL_SURFACE('',#80977,15.125,0.849141474959914);
#1958=CONICAL_SURFACE('',#80989,11.64412671312,0.0349065849999998);
#1959=CONICAL_SURFACE('',#81044,11.94412676881,0.0349065849999998);
#1960=CONICAL_SURFACE('',#81062,13.65,0.7853981625);
#1961=CONICAL_SURFACE('',#81068,13.45,0.7853981625);
#1962=CONICAL_SURFACE('',#81070,13.45,0.7853981625);
#1963=CONICAL_SURFACE('',#85991,12.87032685775,0.785398346845167);
#1964=CONICAL_SURFACE('',#86011,9.75000242976401,0.785398331532869);
#1965=CONICAL_SURFACE('',#86014,9.75000242976401,0.785398331532869);
#1966=CONICAL_SURFACE('',#86035,12.87032685775,0.785398346845167);
#1967=CONICAL_SURFACE('',#86042,10.75000319972,0.785398446953936);
#1968=CONICAL_SURFACE('',#86050,7.999997663262,0.785397845123046);
#1969=CONICAL_SURFACE('',#86083,12.87032685775,0.785398346845167);
#1970=CONICAL_SURFACE('',#86103,9.75000242976401,0.785398331532869);
#1971=CONICAL_SURFACE('',#86106,9.75000242976401,0.785398331532869);
#1972=CONICAL_SURFACE('',#86127,12.87032685775,0.785398346845167);
#1973=CONICAL_SURFACE('',#86134,10.75000319972,0.785398446953936);
#1974=CONICAL_SURFACE('',#86142,7.999997663262,0.785397845123046);
#1975=ORIENTED_CLOSED_SHELL('',*,#79318,.F.);
#1976=ORIENTED_CLOSED_SHELL('',*,#79319,.F.);
#1977=ORIENTED_CLOSED_SHELL('',*,#79320,.F.);
#1978=ORIENTED_CLOSED_SHELL('',*,#79321,.F.);
#1979=ORIENTED_CLOSED_SHELL('',*,#79330,.F.);
#1980=CYLINDRICAL_SURFACE('',#79490,1.5);
#1981=CYLINDRICAL_SURFACE('',#79491,20.5);
#1982=CYLINDRICAL_SURFACE('',#79498,1.5);
#1983=CYLINDRICAL_SURFACE('',#79499,20.5);
#1984=CYLINDRICAL_SURFACE('',#79500,20.5);
#1985=CYLINDRICAL_SURFACE('',#79503,1.5);
#1986=CYLINDRICAL_SURFACE('',#79507,20.5);
#1987=CYLINDRICAL_SURFACE('',#79512,1.5);
#1988=CYLINDRICAL_SURFACE('',#79515,8.4);
#1989=CYLINDRICAL_SURFACE('',#79517,8.4);
#1990=CYLINDRICAL_SURFACE('',#79518,8.4);
#1991=CYLINDRICAL_SURFACE('',#79519,8.4);
#1992=CYLINDRICAL_SURFACE('',#79521,8.4);
#1993=CYLINDRICAL_SURFACE('',#79522,8.4);
#1994=CYLINDRICAL_SURFACE('',#79524,17.);
#1995=CYLINDRICAL_SURFACE('',#79525,17.);
#1996=CYLINDRICAL_SURFACE('',#79526,17.);
#1997=CYLINDRICAL_SURFACE('',#79527,17.);
#1998=CYLINDRICAL_SURFACE('',#79528,17.);
#1999=CYLINDRICAL_SURFACE('',#79530,16.375);
#2000=CYLINDRICAL_SURFACE('',#79533,16.375);
#2001=CYLINDRICAL_SURFACE('',#79534,16.375);
#2002=CYLINDRICAL_SURFACE('',#79539,20.5);
#2003=CYLINDRICAL_SURFACE('',#79549,11.);
#2004=CYLINDRICAL_SURFACE('',#79558,10.5);
#2005=CYLINDRICAL_SURFACE('',#79565,11.25);
#2006=CYLINDRICAL_SURFACE('',#79577,11.);
#2007=CYLINDRICAL_SURFACE('',#79578,21.);
#2008=CYLINDRICAL_SURFACE('',#79586,40.);
#2009=CYLINDRICAL_SURFACE('',#79593,9.500000000001);
#2010=CYLINDRICAL_SURFACE('',#79601,7.75);
#2011=CYLINDRICAL_SURFACE('',#79603,6.5);
#2012=CYLINDRICAL_SURFACE('',#79607,9.5);
#2013=CYLINDRICAL_SURFACE('',#79612,13.5);
#2014=CYLINDRICAL_SURFACE('',#79618,14.5);
#2015=CYLINDRICAL_SURFACE('',#79621,7.25);
#2016=CYLINDRICAL_SURFACE('',#79632,6.5);
#2017=CYLINDRICAL_SURFACE('',#79638,5.5);
#2018=CYLINDRICAL_SURFACE('',#79641,9.50000000000001);
#2019=CYLINDRICAL_SURFACE('',#79644,37.5);
#2020=CYLINDRICAL_SURFACE('',#79647,16.375);
#2021=CYLINDRICAL_SURFACE('',#79648,16.);
#2022=CYLINDRICAL_SURFACE('',#79656,17.);
#2023=CYLINDRICAL_SURFACE('',#79662,9.49999999999999);
#2024=CYLINDRICAL_SURFACE('',#79666,8.4);
#2025=CYLINDRICAL_SURFACE('',#79667,12.);
#2026=CYLINDRICAL_SURFACE('',#79669,37.5);
#2027=CYLINDRICAL_SURFACE('',#79672,8.5);
#2028=CYLINDRICAL_SURFACE('',#79674,10.25);
#2029=CYLINDRICAL_SURFACE('',#79677,11.75);
#2030=CYLINDRICAL_SURFACE('',#79683,7.75000000000001);
#2031=CYLINDRICAL_SURFACE('',#79696,9.49999999999999);
#2032=CYLINDRICAL_SURFACE('',#79700,8.4);
#2033=CYLINDRICAL_SURFACE('',#79702,12.);
#2034=CYLINDRICAL_SURFACE('',#79704,37.5);
#2035=CYLINDRICAL_SURFACE('',#79707,8.5);
#2036=CYLINDRICAL_SURFACE('',#79709,10.25);
#2037=CYLINDRICAL_SURFACE('',#79712,11.75);
#2038=CYLINDRICAL_SURFACE('',#79718,7.75000000000001);
#2039=CYLINDRICAL_SURFACE('',#79735,1.5);
#2040=CYLINDRICAL_SURFACE('',#79740,18.5);
#2041=CYLINDRICAL_SURFACE('',#79748,0.999999999999999);
#2042=CYLINDRICAL_SURFACE('',#79753,1.5);
#2043=CYLINDRICAL_SURFACE('',#79755,20.5);
#2044=CYLINDRICAL_SURFACE('',#79757,0.999999999999999);
#2045=CYLINDRICAL_SURFACE('',#79775,1.5);
#2046=CYLINDRICAL_SURFACE('',#79795,27.5);
#2047=CYLINDRICAL_SURFACE('',#79806,27.5);
#2048=CYLINDRICAL_SURFACE('',#79807,67.5);
#2049=CYLINDRICAL_SURFACE('',#79812,1.5);
#2050=CYLINDRICAL_SURFACE('',#79814,5.5);
#2051=CYLINDRICAL_SURFACE('',#79815,37.5);
#2052=CYLINDRICAL_SURFACE('',#79819,37.5);
#2053=CYLINDRICAL_SURFACE('',#79820,5.5);
#2054=CYLINDRICAL_SURFACE('',#79844,1.5);
#2055=CYLINDRICAL_SURFACE('',#79848,1.);
#2056=CYLINDRICAL_SURFACE('',#79851,0.999999999999999);
#2057=CYLINDRICAL_SURFACE('',#79853,1.5);
#2058=CYLINDRICAL_SURFACE('',#79861,18.5);
#2059=CYLINDRICAL_SURFACE('',#79865,20.5);
#2060=CYLINDRICAL_SURFACE('',#79888,1.5);
#2061=CYLINDRICAL_SURFACE('',#79902,27.5);
#2062=CYLINDRICAL_SURFACE('',#79907,1.5);
#2063=CYLINDRICAL_SURFACE('',#79912,67.5);
#2064=CYLINDRICAL_SURFACE('',#79913,27.5);
#2065=CYLINDRICAL_SURFACE('',#79924,5.5);
#2066=CYLINDRICAL_SURFACE('',#79925,5.5);
#2067=CYLINDRICAL_SURFACE('',#79926,37.5);
#2068=CYLINDRICAL_SURFACE('',#79930,37.5);
#2069=CYLINDRICAL_SURFACE('',#79963,1.5);
#2070=CYLINDRICAL_SURFACE('',#79968,15.5);
#2071=CYLINDRICAL_SURFACE('',#79971,15.5);
#2072=CYLINDRICAL_SURFACE('',#79974,5.498378496899);
#2073=CYLINDRICAL_SURFACE('',#79976,5.498378496898);
#2074=CYLINDRICAL_SURFACE('',#79979,1.);
#2075=CYLINDRICAL_SURFACE('',#79981,1.);
#2076=CYLINDRICAL_SURFACE('',#79985,1.5);
#2077=CYLINDRICAL_SURFACE('',#79986,1.5);
#2078=CYLINDRICAL_SURFACE('',#80010,5.5);
#2079=CYLINDRICAL_SURFACE('',#80018,1.5);
#2080=CYLINDRICAL_SURFACE('',#80024,15.5);
#2081=CYLINDRICAL_SURFACE('',#80035,9.51643737811801);
#2082=CYLINDRICAL_SURFACE('',#80039,9.51643737811801);
#2083=CYLINDRICAL_SURFACE('',#80049,12.);
#2084=CYLINDRICAL_SURFACE('',#80053,12.);
#2085=CYLINDRICAL_SURFACE('',#80057,18.);
#2086=CYLINDRICAL_SURFACE('',#80062,18.);
#2087=CYLINDRICAL_SURFACE('',#80064,8.);
#2088=CYLINDRICAL_SURFACE('',#80066,8.);
#2089=CYLINDRICAL_SURFACE('',#80079,1.5);
#2090=CYLINDRICAL_SURFACE('',#80082,15.5);
#2091=CYLINDRICAL_SURFACE('',#80087,5.498378496899);
#2092=CYLINDRICAL_SURFACE('',#80094,0.999999999999999);
#2093=CYLINDRICAL_SURFACE('',#80100,0.999999999999999);
#2094=CYLINDRICAL_SURFACE('',#80101,1.5);
#2095=CYLINDRICAL_SURFACE('',#80108,0.999999999999999);
#2096=CYLINDRICAL_SURFACE('',#80116,5.498378496898);
#2097=CYLINDRICAL_SURFACE('',#80117,27.6468278765);
#2098=CYLINDRICAL_SURFACE('',#80122,27.64683059909);
#2099=CYLINDRICAL_SURFACE('',#80135,1.5);
#2100=CYLINDRICAL_SURFACE('',#80137,1.5);
#2101=CYLINDRICAL_SURFACE('',#80142,1.5);
#2102=CYLINDRICAL_SURFACE('',#80143,9.500000000001);
#2103=CYLINDRICAL_SURFACE('',#80159,11.5);
#2104=CYLINDRICAL_SURFACE('',#80160,11.5);
#2105=CYLINDRICAL_SURFACE('',#80162,1.);
#2106=CYLINDRICAL_SURFACE('',#80165,1.);
#2107=CYLINDRICAL_SURFACE('',#80174,1.5);
#2108=CYLINDRICAL_SURFACE('',#80176,1.);
#2109=CYLINDRICAL_SURFACE('',#80188,1.5);
#2110=CYLINDRICAL_SURFACE('',#80192,1.5);
#2111=CYLINDRICAL_SURFACE('',#80202,27.49622463646);
#2112=CYLINDRICAL_SURFACE('',#80205,1.5);
#2113=CYLINDRICAL_SURFACE('',#80206,18.5);
#2114=CYLINDRICAL_SURFACE('',#80207,18.5);
#2115=CYLINDRICAL_SURFACE('',#80219,15.);
#2116=CYLINDRICAL_SURFACE('',#80223,15.);
#2117=CYLINDRICAL_SURFACE('',#80233,40.);
#2118=CYLINDRICAL_SURFACE('',#80234,8.);
#2119=CYLINDRICAL_SURFACE('',#80237,40.);
#2120=CYLINDRICAL_SURFACE('',#80244,40.);
#2121=CYLINDRICAL_SURFACE('',#80245,8.);
#2122=CYLINDRICAL_SURFACE('',#80261,15.);
#2123=CYLINDRICAL_SURFACE('',#80262,15.);
#2124=CYLINDRICAL_SURFACE('',#80263,40.);
#2125=CYLINDRICAL_SURFACE('',#80277,30.);
#2126=CYLINDRICAL_SURFACE('',#80279,30.);
#2127=CYLINDRICAL_SURFACE('',#80281,30.);
#2128=CYLINDRICAL_SURFACE('',#80297,30.);
#2129=CYLINDRICAL_SURFACE('',#80301,30.);
#2130=CYLINDRICAL_SURFACE('',#80304,30.);
#2131=CYLINDRICAL_SURFACE('',#80310,13.);
#2132=CYLINDRICAL_SURFACE('',#80311,13.);
#2133=CYLINDRICAL_SURFACE('',#80316,1.5);
#2134=CYLINDRICAL_SURFACE('',#80331,1.5);
#2135=CYLINDRICAL_SURFACE('',#80332,1.5);
#2136=CYLINDRICAL_SURFACE('',#80334,1.5);
#2137=CYLINDRICAL_SURFACE('',#80340,1.5);
#2138=CYLINDRICAL_SURFACE('',#80341,70.);
#2139=CYLINDRICAL_SURFACE('',#80342,30.);
#2140=CYLINDRICAL_SURFACE('',#80343,1.5);
#2141=CYLINDRICAL_SURFACE('',#80347,67.5);
#2142=CYLINDRICAL_SURFACE('',#80349,1.5);
#2143=CYLINDRICAL_SURFACE('',#80352,1.5);
#2144=CYLINDRICAL_SURFACE('',#80357,1.5);
#2145=CYLINDRICAL_SURFACE('',#80361,1.5);
#2146=CYLINDRICAL_SURFACE('',#80368,1.5);
#2147=CYLINDRICAL_SURFACE('',#80369,1.5);
#2148=CYLINDRICAL_SURFACE('',#80373,0.999999999999999);
#2149=CYLINDRICAL_SURFACE('',#80378,20.5);
#2150=CYLINDRICAL_SURFACE('',#80384,21.5);
#2151=CYLINDRICAL_SURFACE('',#80388,15.00000000001);
#2152=CYLINDRICAL_SURFACE('',#80389,20.);
#2153=CYLINDRICAL_SURFACE('',#80395,3.40000000000001);
#2154=CYLINDRICAL_SURFACE('',#80409,2.15);
#2155=CYLINDRICAL_SURFACE('',#80412,19.);
#2156=CYLINDRICAL_SURFACE('',#80417,17.5);
#2157=CYLINDRICAL_SURFACE('',#80423,19.);
#2158=CYLINDRICAL_SURFACE('',#80426,17.5);
#2159=CYLINDRICAL_SURFACE('',#80438,1.50000000000001);
#2160=CYLINDRICAL_SURFACE('',#80444,1.50000000000001);
#2161=CYLINDRICAL_SURFACE('',#80449,1.50000000000001);
#2162=CYLINDRICAL_SURFACE('',#80458,1.50000000000001);
#2163=CYLINDRICAL_SURFACE('',#80469,1.50000000000001);
#2164=CYLINDRICAL_SURFACE('',#80471,1.50000000000001);
#2165=CYLINDRICAL_SURFACE('',#80500,2.50000000000001);
#2166=CYLINDRICAL_SURFACE('',#80503,2.50000000000001);
#2167=CYLINDRICAL_SURFACE('',#80507,10.);
#2168=CYLINDRICAL_SURFACE('',#80512,10.);
#2169=CYLINDRICAL_SURFACE('',#80514,4.00000000000099);
#2170=CYLINDRICAL_SURFACE('',#80523,9.35);
#2171=CYLINDRICAL_SURFACE('',#80525,9.35);
#2172=CYLINDRICAL_SURFACE('',#80526,9.35);
#2173=CYLINDRICAL_SURFACE('',#80527,9.35);
#2174=CYLINDRICAL_SURFACE('',#80528,9.35);
#2175=CYLINDRICAL_SURFACE('',#80529,9.35);
#2176=CYLINDRICAL_SURFACE('',#80530,9.35);
#2177=CYLINDRICAL_SURFACE('',#80532,9.50000000000001);
#2178=CYLINDRICAL_SURFACE('',#80534,9.50000000000001);
#2179=CYLINDRICAL_SURFACE('',#80535,9.50000000000001);
#2180=CYLINDRICAL_SURFACE('',#80536,9.50000000000001);
#2181=CYLINDRICAL_SURFACE('',#80537,9.50000000000001);
#2182=CYLINDRICAL_SURFACE('',#80538,9.50000000000001);
#2183=CYLINDRICAL_SURFACE('',#80539,9.50000000000001);
#2184=CYLINDRICAL_SURFACE('',#80542,10.);
#2185=CYLINDRICAL_SURFACE('',#80544,10.);
#2186=CYLINDRICAL_SURFACE('',#80545,10.);
#2187=CYLINDRICAL_SURFACE('',#80546,10.);
#2188=CYLINDRICAL_SURFACE('',#80547,10.);
#2189=CYLINDRICAL_SURFACE('',#80548,10.25);
#2190=CYLINDRICAL_SURFACE('',#80550,10.25);
#2191=CYLINDRICAL_SURFACE('',#80551,10.25);
#2192=CYLINDRICAL_SURFACE('',#80552,10.25);
#2193=CYLINDRICAL_SURFACE('',#80553,10.25);
#2194=CYLINDRICAL_SURFACE('',#80554,10.25);
#2195=CYLINDRICAL_SURFACE('',#80557,10.25);
#2196=CYLINDRICAL_SURFACE('',#80559,9.25);
#2197=CYLINDRICAL_SURFACE('',#80563,11.);
#2198=CYLINDRICAL_SURFACE('',#80566,9.15);
#2199=CYLINDRICAL_SURFACE('',#80569,10.);
#2200=CYLINDRICAL_SURFACE('',#80576,7.75);
#2201=CYLINDRICAL_SURFACE('',#80580,6.5);
#2202=CYLINDRICAL_SURFACE('',#80589,4.);
#2203=CYLINDRICAL_SURFACE('',#80596,9.50000000000001);
#2204=CYLINDRICAL_SURFACE('',#80597,9.35);
#2205=CYLINDRICAL_SURFACE('',#80601,4.);
#2206=CYLINDRICAL_SURFACE('',#80629,12.1);
#2207=CYLINDRICAL_SURFACE('',#80646,7.50000000000001);
#2208=CYLINDRICAL_SURFACE('',#80649,1.5);
#2209=CYLINDRICAL_SURFACE('',#80652,1.5);
#2210=CYLINDRICAL_SURFACE('',#80658,1.5);
#2211=CYLINDRICAL_SURFACE('',#80668,13.0486498132185);
#2212=CYLINDRICAL_SURFACE('',#80669,13.0486498132185);
#2213=CYLINDRICAL_SURFACE('',#80670,13.0486498132185);
#2214=CYLINDRICAL_SURFACE('',#80671,12.25);
#2215=CYLINDRICAL_SURFACE('',#80673,12.25);
#2216=CYLINDRICAL_SURFACE('',#80674,12.25);
#2217=CYLINDRICAL_SURFACE('',#80675,12.25);
#2218=CYLINDRICAL_SURFACE('',#80676,12.25);
#2219=CYLINDRICAL_SURFACE('',#80678,10.5);
#2220=CYLINDRICAL_SURFACE('',#80681,12.25);
#2221=CYLINDRICAL_SURFACE('',#80683,13.0486498132185);
#2222=CYLINDRICAL_SURFACE('',#80704,16.);
#2223=CYLINDRICAL_SURFACE('',#80708,16.);
#2224=CYLINDRICAL_SURFACE('',#80709,16.);
#2225=CYLINDRICAL_SURFACE('',#80712,16.);
#2226=CYLINDRICAL_SURFACE('',#80713,16.);
#2227=CYLINDRICAL_SURFACE('',#80714,16.);
#2228=CYLINDRICAL_SURFACE('',#80728,12.1);
#2229=CYLINDRICAL_SURFACE('',#80745,7.50000000000001);
#2230=CYLINDRICAL_SURFACE('',#80748,1.5);
#2231=CYLINDRICAL_SURFACE('',#80751,1.5);
#2232=CYLINDRICAL_SURFACE('',#80757,1.5);
#2233=CYLINDRICAL_SURFACE('',#80771,27.5);
#2234=CYLINDRICAL_SURFACE('',#80773,12.4);
#2235=CYLINDRICAL_SURFACE('',#80776,2.00000000000001);
#2236=CYLINDRICAL_SURFACE('',#80783,27.);
#2237=CYLINDRICAL_SURFACE('',#80797,13.0486498132185);
#2238=CYLINDRICAL_SURFACE('',#80798,13.0486498132185);
#2239=CYLINDRICAL_SURFACE('',#80799,13.0486498132185);
#2240=CYLINDRICAL_SURFACE('',#80800,12.25);
#2241=CYLINDRICAL_SURFACE('',#80802,12.25);
#2242=CYLINDRICAL_SURFACE('',#80803,12.25);
#2243=CYLINDRICAL_SURFACE('',#80804,12.25);
#2244=CYLINDRICAL_SURFACE('',#80805,12.25);
#2245=CYLINDRICAL_SURFACE('',#80807,10.5);
#2246=CYLINDRICAL_SURFACE('',#80810,12.25);
#2247=CYLINDRICAL_SURFACE('',#80812,13.0486498132185);
#2248=CYLINDRICAL_SURFACE('',#80833,16.);
#2249=CYLINDRICAL_SURFACE('',#80837,16.);
#2250=CYLINDRICAL_SURFACE('',#80838,16.);
#2251=CYLINDRICAL_SURFACE('',#80841,16.);
#2252=CYLINDRICAL_SURFACE('',#80842,16.);
#2253=CYLINDRICAL_SURFACE('',#80843,16.);
#2254=CYLINDRICAL_SURFACE('',#80849,2.05);
#2255=CYLINDRICAL_SURFACE('',#80855,5.5);
#2256=CYLINDRICAL_SURFACE('',#80857,5.5);
#2257=CYLINDRICAL_SURFACE('',#80858,5.5);
#2258=CYLINDRICAL_SURFACE('',#80861,6.);
#2259=CYLINDRICAL_SURFACE('',#80863,6.);
#2260=CYLINDRICAL_SURFACE('',#80864,7.);
#2261=CYLINDRICAL_SURFACE('',#80873,5.25);
#2262=CYLINDRICAL_SURFACE('',#80876,6.);
#2263=CYLINDRICAL_SURFACE('',#80881,4.4);
#2264=CYLINDRICAL_SURFACE('',#80885,2.55);
#2265=CYLINDRICAL_SURFACE('',#80898,5.5);
#2266=CYLINDRICAL_SURFACE('',#80899,6.47238979616114);
#2267=CYLINDRICAL_SURFACE('',#80905,6.47238979616113);
#2268=CYLINDRICAL_SURFACE('',#80907,9.);
#2269=CYLINDRICAL_SURFACE('',#80911,9.99999999999999);
#2270=CYLINDRICAL_SURFACE('',#80923,7.99999999999999);
#2271=CYLINDRICAL_SURFACE('',#80929,4.);
#2272=CYLINDRICAL_SURFACE('',#80932,2.30850939467147);
#2273=CYLINDRICAL_SURFACE('',#80956,27.5);
#2274=CYLINDRICAL_SURFACE('',#80958,12.4);
#2275=CYLINDRICAL_SURFACE('',#80961,2.00000000000001);
#2276=CYLINDRICAL_SURFACE('',#80968,27.);
#2277=CYLINDRICAL_SURFACE('',#80982,13.9);
#2278=CYLINDRICAL_SURFACE('',#80984,13.9);
#2279=CYLINDRICAL_SURFACE('',#80986,13.9);
#2280=CYLINDRICAL_SURFACE('',#80987,13.9);
#2281=CYLINDRICAL_SURFACE('',#80999,0.75);
#2282=CYLINDRICAL_SURFACE('',#81000,0.75);
#2283=CYLINDRICAL_SURFACE('',#81001,11.05);
#2284=CYLINDRICAL_SURFACE('',#81013,0.75);
#2285=CYLINDRICAL_SURFACE('',#81014,0.75);
#2286=CYLINDRICAL_SURFACE('',#81015,11.35);
#2287=CYLINDRICAL_SURFACE('',#81031,9.85);
#2288=CYLINDRICAL_SURFACE('',#81034,10.15);
#2289=CYLINDRICAL_SURFACE('',#81046,12.25);
#2290=CYLINDRICAL_SURFACE('',#81049,12.75);
#2291=CYLINDRICAL_SURFACE('',#81052,13.1);
#2292=CYLINDRICAL_SURFACE('',#81055,13.7);
#2293=CYLINDRICAL_SURFACE('',#81064,12.75);
#2294=CYLINDRICAL_SURFACE('',#81078,13.9);
#2295=CYLINDRICAL_SURFACE('',#85941,0.75);
#2296=CYLINDRICAL_SURFACE('',#85942,0.75);
#2297=CYLINDRICAL_SURFACE('',#85947,0.75);
#2298=CYLINDRICAL_SURFACE('',#85948,0.75);
#2299=CYLINDRICAL_SURFACE('',#85968,10.25);
#2300=CYLINDRICAL_SURFACE('',#85971,10.25);
#2301=CYLINDRICAL_SURFACE('',#85972,10.25);
#2302=CYLINDRICAL_SURFACE('',#85973,10.25);
#2303=CYLINDRICAL_SURFACE('',#85974,10.25);
#2304=CYLINDRICAL_SURFACE('',#85975,10.25);
#2305=CYLINDRICAL_SURFACE('',#85976,10.25);
#2306=CYLINDRICAL_SURFACE('',#85977,10.25);
#2307=CYLINDRICAL_SURFACE('',#85978,13.);
#2308=CYLINDRICAL_SURFACE('',#85980,13.);
#2309=CYLINDRICAL_SURFACE('',#85982,13.);
#2310=CYLINDRICAL_SURFACE('',#85983,13.);
#2311=CYLINDRICAL_SURFACE('',#85984,13.);
#2312=CYLINDRICAL_SURFACE('',#85985,13.);
#2313=CYLINDRICAL_SURFACE('',#85986,13.);
#2314=CYLINDRICAL_SURFACE('',#85987,13.);
#2315=CYLINDRICAL_SURFACE('',#85988,13.);
#2316=CYLINDRICAL_SURFACE('',#85993,9.09006752601109);
#2317=CYLINDRICAL_SURFACE('',#85994,9.09006752601109);
#2318=CYLINDRICAL_SURFACE('',#85995,9.09006752601109);
#2319=CYLINDRICAL_SURFACE('',#85996,9.09006752601109);
#2320=CYLINDRICAL_SURFACE('',#85997,9.0900675260086);
#2321=CYLINDRICAL_SURFACE('',#85998,9.0900675260086);
#2322=CYLINDRICAL_SURFACE('',#85999,9.0900675260086);
#2323=CYLINDRICAL_SURFACE('',#86000,9.0900675260086);
#2324=CYLINDRICAL_SURFACE('',#86001,9.08769033371916);
#2325=CYLINDRICAL_SURFACE('',#86003,11.8397710119949);
#2326=CYLINDRICAL_SURFACE('',#86005,11.8397710119949);
#2327=CYLINDRICAL_SURFACE('',#86006,11.8397710119949);
#2328=CYLINDRICAL_SURFACE('',#86007,11.8397710119877);
#2329=CYLINDRICAL_SURFACE('',#86008,11.8397710119877);
#2330=CYLINDRICAL_SURFACE('',#86009,11.8397710119877);
#2331=CYLINDRICAL_SURFACE('',#86010,11.8397710119877);
#2332=CYLINDRICAL_SURFACE('',#86016,4.75);
#2333=CYLINDRICAL_SURFACE('',#86019,11.8397710119877);
#2334=CYLINDRICAL_SURFACE('',#86020,11.8397710119949);
#2335=CYLINDRICAL_SURFACE('',#86022,10.3625);
#2336=CYLINDRICAL_SURFACE('',#86023,9.08769033371916);
#2337=CYLINDRICAL_SURFACE('',#86025,9.0900675260086);
#2338=CYLINDRICAL_SURFACE('',#86026,9.09006752601109);
#2339=CYLINDRICAL_SURFACE('',#86037,13.);
#2340=CYLINDRICAL_SURFACE('',#86038,10.5);
#2341=CYLINDRICAL_SURFACE('',#86048,7.75);
#2342=CYLINDRICAL_SURFACE('',#86053,10.25);
#2343=CYLINDRICAL_SURFACE('',#86058,10.3625);
#2344=CYLINDRICAL_SURFACE('',#86060,10.25);
#2345=CYLINDRICAL_SURFACE('',#86063,10.25);
#2346=CYLINDRICAL_SURFACE('',#86064,10.25);
#2347=CYLINDRICAL_SURFACE('',#86065,10.25);
#2348=CYLINDRICAL_SURFACE('',#86066,10.25);
#2349=CYLINDRICAL_SURFACE('',#86067,10.25);
#2350=CYLINDRICAL_SURFACE('',#86068,10.25);
#2351=CYLINDRICAL_SURFACE('',#86069,10.25);
#2352=CYLINDRICAL_SURFACE('',#86070,13.);
#2353=CYLINDRICAL_SURFACE('',#86072,13.);
#2354=CYLINDRICAL_SURFACE('',#86074,13.);
#2355=CYLINDRICAL_SURFACE('',#86075,13.);
#2356=CYLINDRICAL_SURFACE('',#86076,13.);
#2357=CYLINDRICAL_SURFACE('',#86077,13.);
#2358=CYLINDRICAL_SURFACE('',#86078,13.);
#2359=CYLINDRICAL_SURFACE('',#86079,13.);
#2360=CYLINDRICAL_SURFACE('',#86080,13.);
#2361=CYLINDRICAL_SURFACE('',#86085,9.09006752601109);
#2362=CYLINDRICAL_SURFACE('',#86086,9.09006752601109);
#2363=CYLINDRICAL_SURFACE('',#86087,9.09006752601109);
#2364=CYLINDRICAL_SURFACE('',#86088,9.09006752601109);
#2365=CYLINDRICAL_SURFACE('',#86089,9.0900675260086);
#2366=CYLINDRICAL_SURFACE('',#86090,9.0900675260086);
#2367=CYLINDRICAL_SURFACE('',#86091,9.0900675260086);
#2368=CYLINDRICAL_SURFACE('',#86092,9.0900675260086);
#2369=CYLINDRICAL_SURFACE('',#86093,9.08769033371916);
#2370=CYLINDRICAL_SURFACE('',#86095,11.8397710119949);
#2371=CYLINDRICAL_SURFACE('',#86097,11.8397710119949);
#2372=CYLINDRICAL_SURFACE('',#86098,11.8397710119949);
#2373=CYLINDRICAL_SURFACE('',#86099,11.8397710119877);
#2374=CYLINDRICAL_SURFACE('',#86100,11.8397710119877);
#2375=CYLINDRICAL_SURFACE('',#86101,11.8397710119877);
#2376=CYLINDRICAL_SURFACE('',#86102,11.8397710119877);
#2377=CYLINDRICAL_SURFACE('',#86108,4.75);
#2378=CYLINDRICAL_SURFACE('',#86111,11.8397710119877);
#2379=CYLINDRICAL_SURFACE('',#86112,11.8397710119949);
#2380=CYLINDRICAL_SURFACE('',#86114,10.3625);
#2381=CYLINDRICAL_SURFACE('',#86115,9.08769033371916);
#2382=CYLINDRICAL_SURFACE('',#86117,9.0900675260086);
#2383=CYLINDRICAL_SURFACE('',#86118,9.09006752601109);
#2384=CYLINDRICAL_SURFACE('',#86129,13.);
#2385=CYLINDRICAL_SURFACE('',#86130,10.5);
#2386=CYLINDRICAL_SURFACE('',#86140,7.75);
#2387=CYLINDRICAL_SURFACE('',#86145,10.25);
#2388=CYLINDRICAL_SURFACE('',#86150,10.3625);
#2389=(
BOUNDED_SURFACE()
B_SPLINE_SURFACE(3,3,((#106617,#106618,#106619,#106620,#106621,#106622,
#106623,#106624,#106625),(#106626,#106627,#106628,#106629,#106630,#106631,
#106632,#106633,#106634),(#106635,#106636,#106637,#106638,#106639,#106640,
#106641,#106642,#106643),(#106644,#106645,#106646,#106647,#106648,#106649,
#106650,#106651,#106652)),.UNSPECIFIED.,.F.,.F.,.F.)
B_SPLINE_SURFACE_WITH_KNOTS((4,4),(4,1,1,1,1,1,4),(0.,1.),(0.,0.170731713964461,
0.369331369271742,0.571283666971615,0.772321449964879,0.980780822111612,
1.),.UNSPECIFIED.)
GEOMETRIC_REPRESENTATION_ITEM()
RATIONAL_B_SPLINE_SURFACE(((1.469253866242,1.469253866242,1.469253866242,
1.469253866242,1.469253866242,1.469253866242,1.469253866242,1.469253866242,
1.469253866242),(0.843582044586,0.843582044586,0.843582044586,0.843582044586,
0.843582044586,0.843582044586,0.843582044586,0.843582044586,0.843582044586),
(0.843582044586,0.843582044586,0.843582044586,0.843582044586,0.843582044586,
0.843582044586,0.843582044586,0.843582044586,0.843582044586),(1.469253866242,
1.469253866242,1.469253866242,1.469253866242,1.469253866242,1.469253866242,
1.469253866242,1.469253866242,1.469253866242)))
REPRESENTATION_ITEM('')
SURFACE()
);
#2390=(
BOUNDED_SURFACE()
B_SPLINE_SURFACE(3,3,((#106672,#106673,#106674,#106675,#106676,#106677,
#106678,#106679,#106680,#106681,#106682,#106683,#106684,#106685,#106686,
#106687,#106688,#106689,#106690,#106691),(#106692,#106693,#106694,#106695,
#106696,#106697,#106698,#106699,#106700,#106701,#106702,#106703,#106704,
#106705,#106706,#106707,#106708,#106709,#106710,#106711),(#106712,#106713,
#106714,#106715,#106716,#106717,#106718,#106719,#106720,#106721,#106722,
#106723,#106724,#106725,#106726,#106727,#106728,#106729,#106730,#106731),
(#106732,#106733,#106734,#106735,#106736,#106737,#106738,#106739,#106740,
#106741,#106742,#106743,#106744,#106745,#106746,#106747,#106748,#106749,
#106750,#106751)),.UNSPECIFIED.,.F.,.F.,.F.)
B_SPLINE_SURFACE_WITH_KNOTS((4,4),(4,1,1,1,1,1,1,1,1,1,1,1,1,1,1,1,1,4),
(0.,1.),(0.,0.0396611801962909,0.0991280080993822,0.158967060305227,0.213500355613908,
0.265743805592041,0.31877970559442,0.372320929804579,0.42550049560743,0.477326879186013,
0.531755535132276,0.594383860510548,0.661759309442457,0.728996536779342,
0.791903310438717,0.857857310969531,0.931521029517504,1.),.UNSPECIFIED.)
GEOMETRIC_REPRESENTATION_ITEM()
RATIONAL_B_SPLINE_SURFACE(((1.186027134151,1.186027134151,1.186027134151,
1.186027134151,1.186027134151,1.186027134151,1.186027134151,1.186027134151,
1.186027134151,1.186027134151,1.186027134151,1.186027134151,1.186027134151,
1.186027134151,1.186027134151,1.186027134151,1.186027134151,1.186027134151,
1.186027134151,1.186027134151),(0.9379909552829,0.9379909552829,0.9379909552829,
0.9379909552829,0.9379909552829,0.9379909552829,0.9379909552829,0.9379909552829,
0.9379909552829,0.9379909552829,0.9379909552829,0.9379909552829,0.9379909552829,
0.9379909552829,0.9379909552829,0.9379909552829,0.9379909552829,0.9379909552829,
0.9379909552829,0.9379909552829),(0.9379909552829,0.9379909552829,0.9379909552829,
0.9379909552829,0.9379909552829,0.9379909552829,0.9379909552829,0.9379909552829,
0.9379909552829,0.9379909552829,0.9379909552829,0.9379909552829,0.9379909552829,
0.9379909552829,0.9379909552829,0.9379909552829,0.9379909552829,0.9379909552829,
0.9379909552829,0.9379909552829),(1.186027134151,1.186027134151,1.186027134151,
1.186027134151,1.186027134151,1.186027134151,1.186027134151,1.186027134151,
1.186027134151,1.186027134151,1.186027134151,1.186027134151,1.186027134151,
1.186027134151,1.186027134151,1.186027134151,1.186027134151,1.186027134151,
1.186027134151,1.186027134151)))
REPRESENTATION_ITEM('')
SURFACE()
);
#2391=(
BOUNDED_SURFACE()
B_SPLINE_SURFACE(3,3,((#106769,#106770,#106771,#106772,#106773,#106774,
#106775,#106776,#106777,#106778,#106779,#106780,#106781,#106782,#106783,
#106784,#106785,#106786,#106787,#106788),(#106789,#106790,#106791,#106792,
#106793,#106794,#106795,#106796,#106797,#106798,#106799,#106800,#106801,
#106802,#106803,#106804,#106805,#106806,#106807,#106808),(#106809,#106810,
#106811,#106812,#106813,#106814,#106815,#106816,#106817,#106818,#106819,
#106820,#106821,#106822,#106823,#106824,#106825,#106826,#106827,#106828),
(#106829,#106830,#106831,#106832,#106833,#106834,#106835,#106836,#106837,
#106838,#106839,#106840,#106841,#106842,#106843,#106844,#106845,#106846,
#106847,#106848)),.UNSPECIFIED.,.F.,.F.,.F.)
B_SPLINE_SURFACE_WITH_KNOTS((4,4),(4,1,1,1,1,1,1,1,1,1,1,1,1,1,1,1,1,4),
(0.,1.),(0.,0.0294841287779505,0.0658109628884052,0.105749498424659,0.149530724255755,
0.197388379273207,0.249559161241624,0.306281102763413,0.367810676903299,
0.434427999245631,0.506607662324375,0.585506710794748,0.670705086525465,
0.75370766324414,0.832219267034226,0.905244950763814,0.970572923362877,
1.),.UNSPECIFIED.)
GEOMETRIC_REPRESENTATION_ITEM()
RATIONAL_B_SPLINE_SURFACE(((1.204673293213,1.204673293213,1.204673293213,
1.204673293213,1.204673293213,1.204673293213,1.204673293213,1.204673293213,
1.204673293213,1.204673293213,1.204673293213,1.204673293213,1.204673293213,
1.204673293213,1.204673293213,1.204673293213,1.204673293213,1.204673293213,
1.204673293213,1.204673293213),(0.931775568929,0.931775568929,0.931775568929,
0.931775568929,0.931775568929,0.931775568929,0.931775568929,0.931775568929,
0.931775568929,0.931775568929,0.931775568929,0.931775568929,0.931775568929,
0.931775568929,0.931775568929,0.931775568929,0.931775568929,0.931775568929,
0.931775568929,0.931775568929),(0.931775568929,0.931775568929,0.931775568929,
0.931775568929,0.931775568929,0.931775568929,0.931775568929,0.931775568929,
0.931775568929,0.931775568929,0.931775568929,0.931775568929,0.931775568929,
0.931775568929,0.931775568929,0.931775568929,0.931775568929,0.931775568929,
0.931775568929,0.931775568929),(1.204673293213,1.204673293213,1.204673293213,
1.204673293213,1.204673293213,1.204673293213,1.204673293213,1.204673293213,
1.204673293213,1.204673293213,1.204673293213,1.204673293213,1.204673293213,
1.204673293213,1.204673293213,1.204673293213,1.204673293213,1.204673293213,
1.204673293213,1.204673293213)))
REPRESENTATION_ITEM('')
SURFACE()
);
#2392=(
BOUNDED_SURFACE()
B_SPLINE_SURFACE(3,3,((#106891,#106892,#106893,#106894,#106895,#106896,
#106897,#106898,#106899),(#106900,#106901,#106902,#106903,#106904,#106905,
#106906,#106907,#106908),(#106909,#106910,#106911,#106912,#106913,#106914,
#106915,#106916,#106917),(#106918,#106919,#106920,#106921,#106922,#106923,
#106924,#106925,#106926)),.UNSPECIFIED.,.F.,.F.,.F.)
B_SPLINE_SURFACE_WITH_KNOTS((4,4),(4,1,1,1,1,1,4),(0.,1.),(0.,0.0142463491922952,
0.215979712627769,0.410391612199461,0.611571691500493,0.81768157648455,
1.),.UNSPECIFIED.)
GEOMETRIC_REPRESENTATION_ITEM()
RATIONAL_B_SPLINE_SURFACE(((1.469254032395,1.469254032395,1.469254032395,
1.469254032395,1.469254032395,1.469254032395,1.469254032395,1.469254032395,
1.469254032395),(0.8435819892018,0.8435819892018,0.8435819892018,0.8435819892018,
0.8435819892018,0.8435819892018,0.8435819892018,0.8435819892018,0.8435819892018),
(0.8435819892018,0.8435819892018,0.8435819892018,0.8435819892018,0.8435819892018,
0.8435819892018,0.8435819892018,0.8435819892018,0.8435819892018),(1.469254032395,
1.469254032395,1.469254032395,1.469254032395,1.469254032395,1.469254032395,
1.469254032395,1.469254032395,1.469254032395)))
REPRESENTATION_ITEM('')
SURFACE()
);
#2393=(
BOUNDED_SURFACE()
B_SPLINE_SURFACE(3,3,((#106952,#106953,#106954,#106955,#106956,#106957,
#106958,#106959,#106960,#106961,#106962,#106963,#106964,#106965,#106966,
#106967,#106968,#106969,#106970),(#106971,#106972,#106973,#106974,#106975,
#106976,#106977,#106978,#106979,#106980,#106981,#106982,#106983,#106984,
#106985,#106986,#106987,#106988,#106989),(#106990,#106991,#106992,#106993,
#106994,#106995,#106996,#106997,#106998,#106999,#107000,#107001,#107002,
#107003,#107004,#107005,#107006,#107007,#107008),(#107009,#107010,#107011,
#107012,#107013,#107014,#107015,#107016,#107017,#107018,#107019,#107020,
#107021,#107022,#107023,#107024,#107025,#107026,#107027)),.UNSPECIFIED.,
 .F.,.F.,.F.)
B_SPLINE_SURFACE_WITH_KNOTS((4,4),(4,1,1,1,1,1,1,1,1,1,1,1,1,1,1,1,4),(0.,
1.),(0.,0.036181255324217,0.099722007940329,0.168833416481539,0.243160050304141,
0.324333552794184,0.412835986179286,0.500211138210296,0.582010035481769,
0.656172226852367,0.722805119287517,0.782471486007149,0.835893769847624,
0.883837058018828,0.927058268252567,0.966313597455318,1.),.UNSPECIFIED.)
GEOMETRIC_REPRESENTATION_ITEM()
RATIONAL_B_SPLINE_SURFACE(((1.204709660399,1.204709660399,1.204709660399,
1.204709660399,1.204709660399,1.204709660399,1.204709660399,1.204709660399,
1.204709660399,1.204709660399,1.204709660399,1.204709660399,1.204709660399,
1.204709660399,1.204709660399,1.204709660399,1.204709660399,1.204709660399,
1.204709660399),(0.9317634465338,0.9317634465338,0.9317634465338,0.9317634465338,
0.9317634465338,0.9317634465338,0.9317634465338,0.9317634465338,0.9317634465338,
0.9317634465338,0.9317634465338,0.9317634465338,0.9317634465338,0.9317634465338,
0.9317634465338,0.9317634465338,0.9317634465338,0.9317634465338,0.9317634465338),
(0.9317634465338,0.9317634465338,0.9317634465338,0.9317634465338,0.9317634465338,
0.9317634465338,0.9317634465338,0.9317634465338,0.9317634465338,0.9317634465338,
0.9317634465338,0.9317634465338,0.9317634465338,0.9317634465338,0.9317634465338,
0.9317634465338,0.9317634465338,0.9317634465338,0.9317634465338),(1.204709660399,
1.204709660399,1.204709660399,1.204709660399,1.204709660399,1.204709660399,
1.204709660399,1.204709660399,1.204709660399,1.204709660399,1.204709660399,
1.204709660399,1.204709660399,1.204709660399,1.204709660399,1.204709660399,
1.204709660399,1.204709660399,1.204709660399)))
REPRESENTATION_ITEM('')
SURFACE()
);
#2394=(
BOUNDED_SURFACE()
B_SPLINE_SURFACE(3,3,((#107055,#107056,#107057,#107058,#107059,#107060,
#107061,#107062,#107063,#107064,#107065,#107066,#107067,#107068,#107069,
#107070,#107071,#107072,#107073,#107074),(#107075,#107076,#107077,#107078,
#107079,#107080,#107081,#107082,#107083,#107084,#107085,#107086,#107087,
#107088,#107089,#107090,#107091,#107092,#107093,#107094),(#107095,#107096,
#107097,#107098,#107099,#107100,#107101,#107102,#107103,#107104,#107105,
#107106,#107107,#107108,#107109,#107110,#107111,#107112,#107113,#107114),
(#107115,#107116,#107117,#107118,#107119,#107120,#107121,#107122,#107123,
#107124,#107125,#107126,#107127,#107128,#107129,#107130,#107131,#107132,
#107133,#107134)),.UNSPECIFIED.,.F.,.F.,.F.)
B_SPLINE_SURFACE_WITH_KNOTS((4,4),(4,1,1,1,1,1,1,1,1,1,1,1,1,1,1,1,1,4),
(0.,1.),(0.,0.0634473073458767,0.137474475480583,0.203439315591922,0.266070813426101,
0.333494447777073,0.401437472430427,0.464401084256882,0.51858368764375,
0.569769560865856,0.622221496328389,0.67514181525029,0.727526446084146,
0.778774499915783,0.832231436034466,0.891640084181608,0.951727885385323,
1.),.UNSPECIFIED.)
GEOMETRIC_REPRESENTATION_ITEM()
RATIONAL_B_SPLINE_SURFACE(((1.186029185783,1.186029185783,1.186029185783,
1.186029185783,1.186029185783,1.186029185783,1.186029185783,1.186029185783,
1.186029185783,1.186029185783,1.186029185783,1.186029185783,1.186029185783,
1.186029185783,1.186029185783,1.186029185783,1.186029185783,1.186029185783,
1.186029185783,1.186029185783),(0.9379902714058,0.9379902714058,0.9379902714058,
0.9379902714058,0.9379902714058,0.9379902714058,0.9379902714058,0.9379902714058,
0.9379902714058,0.9379902714058,0.9379902714058,0.9379902714058,0.9379902714058,
0.9379902714058,0.9379902714058,0.9379902714058,0.9379902714058,0.9379902714058,
0.9379902714058,0.9379902714058),(0.9379902714058,0.9379902714058,0.9379902714058,
0.9379902714058,0.9379902714058,0.9379902714058,0.9379902714058,0.9379902714058,
0.9379902714058,0.9379902714058,0.9379902714058,0.9379902714058,0.9379902714058,
0.9379902714058,0.9379902714058,0.9379902714058,0.9379902714058,0.9379902714058,
0.9379902714058,0.9379902714058),(1.186029185783,1.186029185783,1.186029185783,
1.186029185783,1.186029185783,1.186029185783,1.186029185783,1.186029185783,
1.186029185783,1.186029185783,1.186029185783,1.186029185783,1.186029185783,
1.186029185783,1.186029185783,1.186029185783,1.186029185783,1.186029185783,
1.186029185783,1.186029185783)))
REPRESENTATION_ITEM('')
SURFACE()
);
#2395=(
BOUNDED_SURFACE()
B_SPLINE_SURFACE(3,3,((#107227,#107228,#107229,#107230,#107231,#107232,
#107233,#107234,#107235,#107236,#107237,#107238,#107239,#107240,#107241,
#107242,#107243,#107244),(#107245,#107246,#107247,#107248,#107249,#107250,
#107251,#107252,#107253,#107254,#107255,#107256,#107257,#107258,#107259,
#107260,#107261,#107262),(#107263,#107264,#107265,#107266,#107267,#107268,
#107269,#107270,#107271,#107272,#107273,#107274,#107275,#107276,#107277,
#107278,#107279,#107280),(#107281,#107282,#107283,#107284,#107285,#107286,
#107287,#107288,#107289,#107290,#107291,#107292,#107293,#107294,#107295,
#107296,#107297,#107298)),.UNSPECIFIED.,.F.,.F.,.F.)
B_SPLINE_SURFACE_WITH_KNOTS((4,4),(4,1,1,1,1,1,1,1,1,1,1,1,1,1,1,4),(0.,
1.),(0.,0.10132397085951,0.219927044777174,0.32793320705097,0.424979133082566,
0.511366209904966,0.588468326001569,0.657700207042955,0.720289724582783,
0.776922704267249,0.828179553385519,0.874662083720489,0.91698653274977,
0.955782383375446,0.991693741530312,1.),.UNSPECIFIED.)
GEOMETRIC_REPRESENTATION_ITEM()
RATIONAL_B_SPLINE_SURFACE(((1.284279766139,1.284279766139,1.284279766139,
1.284279766139,1.284279766139,1.284279766139,1.284279766139,1.284279766139,
1.284279766139,1.284279766139,1.284279766139,1.284279766139,1.284279766139,
1.284279766139,1.284279766139,1.284279766139,1.284279766139,1.284279766139),
(0.9052400779535,0.9052400779535,0.9052400779535,0.9052400779535,0.9052400779535,
0.9052400779535,0.9052400779535,0.9052400779535,0.9052400779535,0.9052400779535,
0.9052400779535,0.9052400779535,0.9052400779535,0.9052400779535,0.9052400779535,
0.9052400779535,0.9052400779535,0.9052400779535),(0.9052400779535,0.9052400779535,
0.9052400779535,0.9052400779535,0.9052400779535,0.9052400779535,0.9052400779535,
0.9052400779535,0.9052400779535,0.9052400779535,0.9052400779535,0.9052400779535,
0.9052400779535,0.9052400779535,0.9052400779535,0.9052400779535,0.9052400779535,
0.9052400779535),(1.284279766139,1.284279766139,1.284279766139,1.284279766139,
1.284279766139,1.284279766139,1.284279766139,1.284279766139,1.284279766139,
1.284279766139,1.284279766139,1.284279766139,1.284279766139,1.284279766139,
1.284279766139,1.284279766139,1.284279766139,1.284279766139)))
REPRESENTATION_ITEM('')
SURFACE()
);
#2396=(
BOUNDED_SURFACE()
B_SPLINE_SURFACE(3,3,((#107767,#107768,#107769,#107770,#107771,#107772,
#107773,#107774,#107775,#107776,#107777,#107778,#107779,#107780,#107781,
#107782,#107783,#107784,#107785,#107786,#107787,#107788,#107789,#107790,
#107791,#107792,#107793,#107794,#107795,#107796,#107797,#107798,#107799),
(#107800,#107801,#107802,#107803,#107804,#107805,#107806,#107807,#107808,
#107809,#107810,#107811,#107812,#107813,#107814,#107815,#107816,#107817,
#107818,#107819,#107820,#107821,#107822,#107823,#107824,#107825,#107826,
#107827,#107828,#107829,#107830,#107831,#107832),(#107833,#107834,#107835,
#107836,#107837,#107838,#107839,#107840,#107841,#107842,#107843,#107844,
#107845,#107846,#107847,#107848,#107849,#107850,#107851,#107852,#107853,
#107854,#107855,#107856,#107857,#107858,#107859,#107860,#107861,#107862,
#107863,#107864,#107865),(#107866,#107867,#107868,#107869,#107870,#107871,
#107872,#107873,#107874,#107875,#107876,#107877,#107878,#107879,#107880,
#107881,#107882,#107883,#107884,#107885,#107886,#107887,#107888,#107889,
#107890,#107891,#107892,#107893,#107894,#107895,#107896,#107897,#107898)),
 .UNSPECIFIED.,.F.,.F.,.F.)
B_SPLINE_SURFACE_WITH_KNOTS((4,4),(4,1,1,1,1,1,1,1,1,1,1,1,1,1,1,1,1,1,
1,1,1,1,1,1,1,1,1,1,1,1,4),(0.,1.),(0.,0.0644716348476169,0.137167075810373,
0.211054732176919,0.283781237138607,0.353003626042113,0.416381685205945,
0.471964431181103,0.521223312478128,0.565576440751156,0.605617803352698,
0.641934173237287,0.675008141068028,0.705215849646144,0.732928243655327,
0.758516244890887,0.78233549305937,0.804479039034365,0.824836899490745,
0.843461996593347,0.860503635413291,0.876112967850447,0.890506098780472,
0.904021603335236,0.917013597842901,0.930049136530003,0.944066490933434,
0.959054067042945,0.973766036233171,0.986879426257445,1.),.UNSPECIFIED.)
GEOMETRIC_REPRESENTATION_ITEM()
RATIONAL_B_SPLINE_SURFACE(((1.095545407101,1.095545407101,1.095545407101,
1.095545407101,1.095545407101,1.095545407101,1.095545407101,1.095545407101,
1.095545407101,1.095545407101,1.095545407101,1.095545407101,1.095545407101,
1.095545407101,1.095545407101,1.095545407101,1.095545407101,1.095545407101,
1.095545407101,1.095545407101,1.095545407101,1.095545407101,1.095545407101,
1.095545407101,1.095545407101,1.095545407101,1.095545407101,1.095545407101,
1.095545407101,1.095545407101,1.095545407101,1.095545407101,1.095545407101),
(0.9681515309662,0.9681515309662,0.9681515309662,0.9681515309662,0.9681515309662,
0.9681515309662,0.9681515309662,0.9681515309662,0.9681515309662,0.9681515309662,
0.9681515309662,0.9681515309662,0.9681515309662,0.9681515309662,0.9681515309662,
0.9681515309662,0.9681515309662,0.9681515309662,0.9681515309662,0.9681515309662,
0.9681515309662,0.9681515309662,0.9681515309662,0.9681515309662,0.9681515309662,
0.9681515309662,0.9681515309662,0.9681515309662,0.9681515309662,0.9681515309662,
0.9681515309662,0.9681515309662,0.9681515309662),(0.9681515309662,0.9681515309662,
0.9681515309662,0.9681515309662,0.9681515309662,0.9681515309662,0.9681515309662,
0.9681515309662,0.9681515309662,0.9681515309662,0.9681515309662,0.9681515309662,
0.9681515309662,0.9681515309662,0.9681515309662,0.9681515309662,0.9681515309662,
0.9681515309662,0.9681515309662,0.9681515309662,0.9681515309662,0.9681515309662,
0.9681515309662,0.9681515309662,0.9681515309662,0.9681515309662,0.9681515309662,
0.9681515309662,0.9681515309662,0.9681515309662,0.9681515309662,0.9681515309662,
0.9681515309662),(1.095545407101,1.095545407101,1.095545407101,1.095545407101,
1.095545407101,1.095545407101,1.095545407101,1.095545407101,1.095545407101,
1.095545407101,1.095545407101,1.095545407101,1.095545407101,1.095545407101,
1.095545407101,1.095545407101,1.095545407101,1.095545407101,1.095545407101,
1.095545407101,1.095545407101,1.095545407101,1.095545407101,1.095545407101,
1.095545407101,1.095545407101,1.095545407101,1.095545407101,1.095545407101,
1.095545407101,1.095545407101,1.095545407101,1.095545407101)))
REPRESENTATION_ITEM('')
SURFACE()
);
#2397=(
BOUNDED_SURFACE()
B_SPLINE_SURFACE(3,3,((#107915,#107916,#107917,#107918,#107919,#107920,
#107921,#107922,#107923,#107924,#107925,#107926,#107927,#107928,#107929,
#107930,#107931),(#107932,#107933,#107934,#107935,#107936,#107937,#107938,
#107939,#107940,#107941,#107942,#107943,#107944,#107945,#107946,#107947,
#107948),(#107949,#107950,#107951,#107952,#107953,#107954,#107955,#107956,
#107957,#107958,#107959,#107960,#107961,#107962,#107963,#107964,#107965),
(#107966,#107967,#107968,#107969,#107970,#107971,#107972,#107973,#107974,
#107975,#107976,#107977,#107978,#107979,#107980,#107981,#107982)),
 .UNSPECIFIED.,.F.,.F.,.F.)
B_SPLINE_SURFACE_WITH_KNOTS((4,4),(4,1,1,1,1,1,1,1,1,1,1,1,1,1,4),(0.,1.),
(0.,0.0956146431540125,0.200570336486981,0.29617085639003,0.382446369780954,
0.459533334763256,0.527981368507571,0.590340486919798,0.649866246025106,
0.709565784246277,0.769912468560832,0.830222740675431,0.890369247895391,
0.9504555950694,1.),.UNSPECIFIED.)
GEOMETRIC_REPRESENTATION_ITEM()
RATIONAL_B_SPLINE_SURFACE(((1.220899632035,1.220899632035,1.220899632035,
1.220899632035,1.220899632035,1.220899632035,1.220899632035,1.220899632035,
1.220899632035,1.220899632035,1.220899632035,1.220899632035,1.220899632035,
1.220899632035,1.220899632035,1.220899632035,1.220899632035),(0.9263667893217,
0.9263667893217,0.9263667893217,0.9263667893217,0.9263667893217,0.9263667893217,
0.9263667893217,0.9263667893217,0.9263667893217,0.9263667893217,0.9263667893217,
0.9263667893217,0.9263667893217,0.9263667893217,0.9263667893217,0.9263667893217,
0.9263667893217),(0.9263667893217,0.9263667893217,0.9263667893217,0.9263667893217,
0.9263667893217,0.9263667893217,0.9263667893217,0.9263667893217,0.9263667893217,
0.9263667893217,0.9263667893217,0.9263667893217,0.9263667893217,0.9263667893217,
0.9263667893217,0.9263667893217,0.9263667893217),(1.220899632035,1.220899632035,
1.220899632035,1.220899632035,1.220899632035,1.220899632035,1.220899632035,
1.220899632035,1.220899632035,1.220899632035,1.220899632035,1.220899632035,
1.220899632035,1.220899632035,1.220899632035,1.220899632035,1.220899632035)))
REPRESENTATION_ITEM('')
SURFACE()
);
#2398=(
BOUNDED_SURFACE()
B_SPLINE_SURFACE(3,3,((#107984,#107985,#107986,#107987,#107988,#107989,
#107990,#107991,#107992,#107993,#107994,#107995,#107996,#107997),(#107998,
#107999,#108000,#108001,#108002,#108003,#108004,#108005,#108006,#108007,
#108008,#108009,#108010,#108011),(#108012,#108013,#108014,#108015,#108016,
#108017,#108018,#108019,#108020,#108021,#108022,#108023,#108024,#108025),
(#108026,#108027,#108028,#108029,#108030,#108031,#108032,#108033,#108034,
#108035,#108036,#108037,#108038,#108039),(#108040,#108041,#108042,#108043,
#108044,#108045,#108046,#108047,#108048,#108049,#108050,#108051,#108052,
#108053),(#108054,#108055,#108056,#108057,#108058,#108059,#108060,#108061,
#108062,#108063,#108064,#108065,#108066,#108067),(#108068,#108069,#108070,
#108071,#108072,#108073,#108074,#108075,#108076,#108077,#108078,#108079,
#108080,#108081)),.UNSPECIFIED.,.F.,.F.,.F.)
B_SPLINE_SURFACE_WITH_KNOTS((4,3,4),(4,1,1,1,1,1,1,1,1,1,1,4),(0.,0.5,1.),
(0.,0.0583353807888762,0.12799724109847,0.204577536604604,0.288006073180643,
0.378737316341168,0.478075810040363,0.587386075028147,0.707620337333203,
0.838547292329974,0.975947862327006,1.),.UNSPECIFIED.)
GEOMETRIC_REPRESENTATION_ITEM()
RATIONAL_B_SPLINE_SURFACE(((1.174660538235,1.174660538235,1.174660538235,
1.174660538235,1.174660538235,1.174660538235,1.174660538235,1.174660538235,
1.174660538235,1.174660538235,1.174660538235,1.174660538235,1.174660538235,
1.174660538235),(0.9417798205884,0.9417798205884,0.9417798205884,0.9417798205884,
0.9417798205884,0.9417798205884,0.9417798205884,0.9417798205884,0.9417798205884,
0.9417798205884,0.9417798205884,0.9417798205884,0.9417798205884,0.9417798205884),
(0.9417798205884,0.9417798205884,0.9417798205884,0.9417798205884,0.9417798205884,
0.9417798205884,0.9417798205884,0.9417798205884,0.9417798205884,0.9417798205884,
0.9417798205884,0.9417798205884,0.9417798205884,0.9417798205884),(1.174660538235,
1.174660538235,1.174660538235,1.174660538235,1.174660538235,1.174660538235,
1.174660538235,1.174660538235,1.174660538235,1.174660538235,1.174660538235,
1.174660538235,1.174660538235,1.174660538235),(0.9417798205884,0.9417798205884,
0.9417798205884,0.9417798205884,0.9417798205884,0.9417798205884,0.9417798205884,
0.9417798205884,0.9417798205884,0.9417798205884,0.9417798205884,0.9417798205884,
0.9417798205884,0.9417798205884),(0.9417798205884,0.9417798205884,0.9417798205884,
0.9417798205884,0.9417798205884,0.9417798205884,0.9417798205884,0.9417798205884,
0.9417798205884,0.9417798205884,0.9417798205884,0.9417798205884,0.9417798205884,
0.9417798205884),(1.174660538235,1.174660538235,1.174660538235,1.174660538235,
1.174660538235,1.174660538235,1.174660538235,1.174660538235,1.174660538235,
1.174660538235,1.174660538235,1.174660538235,1.174660538235,1.174660538235)))
REPRESENTATION_ITEM('')
SURFACE()
);
#2399=(
BOUNDED_SURFACE()
B_SPLINE_SURFACE(3,3,((#108137,#108138,#108139,#108140,#108141,#108142,
#108143,#108144,#108145,#108146,#108147,#108148,#108149,#108150,#108151,
#108152,#108153),(#108154,#108155,#108156,#108157,#108158,#108159,#108160,
#108161,#108162,#108163,#108164,#108165,#108166,#108167,#108168,#108169,
#108170),(#108171,#108172,#108173,#108174,#108175,#108176,#108177,#108178,
#108179,#108180,#108181,#108182,#108183,#108184,#108185,#108186,#108187),
(#108188,#108189,#108190,#108191,#108192,#108193,#108194,#108195,#108196,
#108197,#108198,#108199,#108200,#108201,#108202,#108203,#108204)),
 .UNSPECIFIED.,.F.,.F.,.F.)
B_SPLINE_SURFACE_WITH_KNOTS((4,4),(4,1,1,1,1,1,1,1,1,1,1,1,1,1,4),(0.,1.),
(0.,0.0421741349720486,0.122382017207444,0.194203536901675,0.257534399271218,
0.321534135544779,0.38726227689901,0.452657895941669,0.516567929355648,
0.579748305445392,0.647421910672303,0.723873761459194,0.810175603109662,
0.905570261612151,1.),.UNSPECIFIED.)
GEOMETRIC_REPRESENTATION_ITEM()
RATIONAL_B_SPLINE_SURFACE(((1.219577374139,1.219577374139,1.219577374139,
1.219577374139,1.219577374139,1.219577374139,1.219577374139,1.219577374139,
1.219577374139,1.219577374139,1.219577374139,1.219577374139,1.219577374139,
1.219577374139,1.219577374139,1.219577374139,1.219577374139),(0.9268075419537,
0.9268075419537,0.9268075419537,0.9268075419537,0.9268075419537,0.9268075419537,
0.9268075419537,0.9268075419537,0.9268075419537,0.9268075419537,0.9268075419537,
0.9268075419537,0.9268075419537,0.9268075419537,0.9268075419537,0.9268075419537,
0.9268075419537),(0.9268075419537,0.9268075419537,0.9268075419537,0.9268075419537,
0.9268075419537,0.9268075419537,0.9268075419537,0.9268075419537,0.9268075419537,
0.9268075419537,0.9268075419537,0.9268075419537,0.9268075419537,0.9268075419537,
0.9268075419537,0.9268075419537,0.9268075419537),(1.219577374139,1.219577374139,
1.219577374139,1.219577374139,1.219577374139,1.219577374139,1.219577374139,
1.219577374139,1.219577374139,1.219577374139,1.219577374139,1.219577374139,
1.219577374139,1.219577374139,1.219577374139,1.219577374139,1.219577374139)))
REPRESENTATION_ITEM('')
SURFACE()
);
#2400=(
BOUNDED_SURFACE()
B_SPLINE_SURFACE(3,3,((#108545,#108546,#108547,#108548,#108549,#108550,
#108551,#108552,#108553,#108554,#108555,#108556,#108557,#108558,#108559,
#108560,#108561,#108562),(#108563,#108564,#108565,#108566,#108567,#108568,
#108569,#108570,#108571,#108572,#108573,#108574,#108575,#108576,#108577,
#108578,#108579,#108580),(#108581,#108582,#108583,#108584,#108585,#108586,
#108587,#108588,#108589,#108590,#108591,#108592,#108593,#108594,#108595,
#108596,#108597,#108598),(#108599,#108600,#108601,#108602,#108603,#108604,
#108605,#108606,#108607,#108608,#108609,#108610,#108611,#108612,#108613,
#108614,#108615,#108616)),.UNSPECIFIED.,.F.,.F.,.F.)
B_SPLINE_SURFACE_WITH_KNOTS((4,4),(4,1,1,1,1,1,1,1,1,1,1,1,1,1,1,4),(0.,
1.),(0.,0.00785484539651376,0.0438075231225187,0.0829336925491939,0.125798873740089,
0.172955219979332,0.224941148148525,0.282279526175794,0.345470718132813,
0.415012619574855,0.491463209282815,0.575434444650706,0.667777195884821,
0.770833971303908,0.887651863786679,1.),.UNSPECIFIED.)
GEOMETRIC_REPRESENTATION_ITEM()
RATIONAL_B_SPLINE_SURFACE(((1.284338682996,1.284338682996,1.284338682996,
1.284338682996,1.284338682996,1.284338682996,1.284338682996,1.284338682996,
1.284338682996,1.284338682996,1.284338682996,1.284338682996,1.284338682996,
1.284338682996,1.284338682996,1.284338682996,1.284338682996,1.284338682996),
(0.9052204390014,0.9052204390014,0.9052204390014,0.9052204390014,0.9052204390014,
0.9052204390014,0.9052204390014,0.9052204390014,0.9052204390014,0.9052204390014,
0.9052204390014,0.9052204390014,0.9052204390014,0.9052204390014,0.9052204390014,
0.9052204390014,0.9052204390014,0.9052204390014),(0.9052204390014,0.9052204390014,
0.9052204390014,0.9052204390014,0.9052204390014,0.9052204390014,0.9052204390014,
0.9052204390014,0.9052204390014,0.9052204390014,0.9052204390014,0.9052204390014,
0.9052204390014,0.9052204390014,0.9052204390014,0.9052204390014,0.9052204390014,
0.9052204390014),(1.284338682996,1.284338682996,1.284338682996,1.284338682996,
1.284338682996,1.284338682996,1.284338682996,1.284338682996,1.284338682996,
1.284338682996,1.284338682996,1.284338682996,1.284338682996,1.284338682996,
1.284338682996,1.284338682996,1.284338682996,1.284338682996)))
REPRESENTATION_ITEM('')
SURFACE()
);
#2401=(
BOUNDED_SURFACE()
B_SPLINE_SURFACE(3,3,((#108761,#108762,#108763,#108764,#108765,#108766,
#108767),(#108768,#108769,#108770,#108771,#108772,#108773,#108774),(#108775,
#108776,#108777,#108778,#108779,#108780,#108781),(#108782,#108783,#108784,
#108785,#108786,#108787,#108788)),.UNSPECIFIED.,.F.,.F.,.F.)
B_SPLINE_SURFACE_WITH_KNOTS((4,4),(4,1,1,1,4),(0.173609205866266,0.826397151609457),
(0.734662338499708,0.745916192959342,0.809036419626865,0.87313299624406,
0.92104874395541),.UNSPECIFIED.)
GEOMETRIC_REPRESENTATION_ITEM()
RATIONAL_B_SPLINE_SURFACE(((1.0407131654991,1.0407131654991,1.0407131654991,
1.0407131654991,1.0407131654991,1.0407131654991,1.0407131654991),(0.98642841615643,
0.98642841615643,0.98642841615643,0.98642841615643,0.98642841615643,0.98642841615643,
0.98642841615643),(0.986428944838583,0.986428944838583,0.986428944838583,
0.986428944838583,0.986428944838583,0.986428944838583,0.986428944838583),
(1.04071475154556,1.04071475154556,1.04071475154556,1.04071475154556,1.04071475154556,
1.04071475154556,1.04071475154556)))
REPRESENTATION_ITEM('')
SURFACE()
);
#2402=(
BOUNDED_SURFACE()
B_SPLINE_SURFACE(3,3,((#108828,#108829,#108830,#108831,#108832,#108833,
#108834,#108835,#108836,#108837,#108838,#108839,#108840,#108841,#108842,
#108843,#108844),(#108845,#108846,#108847,#108848,#108849,#108850,#108851,
#108852,#108853,#108854,#108855,#108856,#108857,#108858,#108859,#108860,
#108861),(#108862,#108863,#108864,#108865,#108866,#108867,#108868,#108869,
#108870,#108871,#108872,#108873,#108874,#108875,#108876,#108877,#108878),
(#108879,#108880,#108881,#108882,#108883,#108884,#108885,#108886,#108887,
#108888,#108889,#108890,#108891,#108892,#108893,#108894,#108895)),
 .UNSPECIFIED.,.F.,.F.,.F.)
B_SPLINE_SURFACE_WITH_KNOTS((4,4),(4,1,1,1,1,1,1,1,1,1,1,1,1,1,4),(0.,1.),
(0.,0.0494607190127907,0.109552090730043,0.169758737534662,0.230148354533949,
0.290560261854406,0.350306525877549,0.40987255925942,0.472274987329372,
0.540774950770296,0.617873523590501,0.704101656323432,0.799618934750072,
0.904474902078167,1.),.UNSPECIFIED.)
GEOMETRIC_REPRESENTATION_ITEM()
RATIONAL_B_SPLINE_SURFACE(((1.220899718882,1.220899718882,1.220899718882,
1.220899718882,1.220899718882,1.220899718882,1.220899718882,1.220899718882,
1.220899718882,1.220899718882,1.220899718882,1.220899718882,1.220899718882,
1.220899718882,1.220899718882,1.220899718882,1.220899718882),(0.9263667603727,
0.9263667603727,0.9263667603727,0.9263667603727,0.9263667603727,0.9263667603727,
0.9263667603727,0.9263667603727,0.9263667603727,0.9263667603727,0.9263667603727,
0.9263667603727,0.9263667603727,0.9263667603727,0.9263667603727,0.9263667603727,
0.9263667603727),(0.9263667603727,0.9263667603727,0.9263667603727,0.9263667603727,
0.9263667603727,0.9263667603727,0.9263667603727,0.9263667603727,0.9263667603727,
0.9263667603727,0.9263667603727,0.9263667603727,0.9263667603727,0.9263667603727,
0.9263667603727,0.9263667603727,0.9263667603727),(1.220899718882,1.220899718882,
1.220899718882,1.220899718882,1.220899718882,1.220899718882,1.220899718882,
1.220899718882,1.220899718882,1.220899718882,1.220899718882,1.220899718882,
1.220899718882,1.220899718882,1.220899718882,1.220899718882,1.220899718882)))
REPRESENTATION_ITEM('')
SURFACE()
);
#2403=(
BOUNDED_SURFACE()
B_SPLINE_SURFACE(3,3,((#108897,#108898,#108899,#108900,#108901,#108902,
#108903,#108904,#108905,#108906,#108907,#108908,#108909,#108910,#108911,
#108912,#108913),(#108914,#108915,#108916,#108917,#108918,#108919,#108920,
#108921,#108922,#108923,#108924,#108925,#108926,#108927,#108928,#108929,
#108930),(#108931,#108932,#108933,#108934,#108935,#108936,#108937,#108938,
#108939,#108940,#108941,#108942,#108943,#108944,#108945,#108946,#108947),
(#108948,#108949,#108950,#108951,#108952,#108953,#108954,#108955,#108956,
#108957,#108958,#108959,#108960,#108961,#108962,#108963,#108964)),
 .UNSPECIFIED.,.F.,.F.,.F.)
B_SPLINE_SURFACE_WITH_KNOTS((4,4),(4,1,1,1,1,1,1,1,1,1,1,1,1,1,4),(0.,1.),
(0.,0.0934555018707438,0.190098316562109,0.277412276927369,0.35430591142789,
0.422006518582467,0.485074288423762,0.548771616802643,0.613848873864871,
0.679223443651306,0.742843206526981,0.805944165791561,0.877524725574254,
0.957638281560363,1.),.UNSPECIFIED.)
GEOMETRIC_REPRESENTATION_ITEM()
RATIONAL_B_SPLINE_SURFACE(((1.219577491546,1.219577491546,1.219577491546,
1.219577491546,1.219577491546,1.219577491546,1.219577491546,1.219577491546,
1.219577491546,1.219577491546,1.219577491546,1.219577491546,1.219577491546,
1.219577491546,1.219577491546,1.219577491546,1.219577491546),(0.9268075028179,
0.9268075028179,0.9268075028179,0.9268075028179,0.9268075028179,0.9268075028179,
0.9268075028179,0.9268075028179,0.9268075028179,0.9268075028179,0.9268075028179,
0.9268075028179,0.9268075028179,0.9268075028179,0.9268075028179,0.9268075028179,
0.9268075028179),(0.9268075028179,0.9268075028179,0.9268075028179,0.9268075028179,
0.9268075028179,0.9268075028179,0.9268075028179,0.9268075028179,0.9268075028179,
0.9268075028179,0.9268075028179,0.9268075028179,0.9268075028179,0.9268075028179,
0.9268075028179,0.9268075028179,0.9268075028179),(1.219577491546,1.219577491546,
1.219577491546,1.219577491546,1.219577491546,1.219577491546,1.219577491546,
1.219577491546,1.219577491546,1.219577491546,1.219577491546,1.219577491546,
1.219577491546,1.219577491546,1.219577491546,1.219577491546,1.219577491546)))
REPRESENTATION_ITEM('')
SURFACE()
);
#2404=(
BOUNDED_SURFACE()
B_SPLINE_SURFACE(3,3,((#108983,#108984,#108985,#108986,#108987,#108988,
#108989,#108990,#108991,#108992,#108993,#108994,#108995,#108996),(#108997,
#108998,#108999,#109000,#109001,#109002,#109003,#109004,#109005,#109006,
#109007,#109008,#109009,#109010),(#109011,#109012,#109013,#109014,#109015,
#109016,#109017,#109018,#109019,#109020,#109021,#109022,#109023,#109024),
(#109025,#109026,#109027,#109028,#109029,#109030,#109031,#109032,#109033,
#109034,#109035,#109036,#109037,#109038),(#109039,#109040,#109041,#109042,
#109043,#109044,#109045,#109046,#109047,#109048,#109049,#109050,#109051,
#109052),(#109053,#109054,#109055,#109056,#109057,#109058,#109059,#109060,
#109061,#109062,#109063,#109064,#109065,#109066),(#109067,#109068,#109069,
#109070,#109071,#109072,#109073,#109074,#109075,#109076,#109077,#109078,
#109079,#109080)),.UNSPECIFIED.,.F.,.F.,.F.)
B_SPLINE_SURFACE_WITH_KNOTS((4,3,4),(4,1,1,1,1,1,1,1,1,1,1,4),(0.,0.5,1.),
(0.,0.0457158190500442,0.186722884538372,0.317871899774413,0.436483936855332,
0.542898565175996,0.638400280945175,0.724959173697019,0.804412779028879,
0.877341467334142,0.943792148331645,1.),.UNSPECIFIED.)
GEOMETRIC_REPRESENTATION_ITEM()
RATIONAL_B_SPLINE_SURFACE(((1.174644569129,1.174644569129,1.174644569129,
1.174644569129,1.174644569129,1.174644569129,1.174644569129,1.174644569129,
1.174644569129,1.174644569129,1.174644569129,1.174644569129,1.174644569129,
1.174644569129),(0.9417851436237,0.9417851436237,0.9417851436237,0.9417851436237,
0.9417851436237,0.9417851436237,0.9417851436237,0.9417851436237,0.9417851436237,
0.9417851436237,0.9417851436237,0.9417851436237,0.9417851436237,0.9417851436237),
(0.9417851436237,0.9417851436237,0.9417851436237,0.9417851436237,0.9417851436237,
0.9417851436237,0.9417851436237,0.9417851436237,0.9417851436237,0.9417851436237,
0.9417851436237,0.9417851436237,0.9417851436237,0.9417851436237),(1.174644569129,
1.174644569129,1.174644569129,1.174644569129,1.174644569129,1.174644569129,
1.174644569129,1.174644569129,1.174644569129,1.174644569129,1.174644569129,
1.174644569129,1.174644569129,1.174644569129),(0.9417851436237,0.9417851436237,
0.9417851436237,0.9417851436237,0.9417851436237,0.9417851436237,0.9417851436237,
0.9417851436237,0.9417851436237,0.9417851436237,0.9417851436237,0.9417851436237,
0.9417851436237,0.9417851436237),(0.9417851436237,0.9417851436237,0.9417851436237,
0.9417851436237,0.9417851436237,0.9417851436237,0.9417851436237,0.9417851436237,
0.9417851436237,0.9417851436237,0.9417851436237,0.9417851436237,0.9417851436237,
0.9417851436237),(1.174644569129,1.174644569129,1.174644569129,1.174644569129,
1.174644569129,1.174644569129,1.174644569129,1.174644569129,1.174644569129,
1.174644569129,1.174644569129,1.174644569129,1.174644569129,1.174644569129)))
REPRESENTATION_ITEM('')
SURFACE()
);
#2405=(
BOUNDED_SURFACE()
B_SPLINE_SURFACE(2,2,((#111271,#111272,#111273,#111274,#111275,#111276,
#111277,#111278,#111279),(#111280,#111281,#111282,#111283,#111284,#111285,
#111286,#111287,#111288),(#111289,#111290,#111291,#111292,#111293,#111294,
#111295,#111296,#111297)),.UNSPECIFIED.,.F.,.T.,.F.)
B_SPLINE_SURFACE_WITH_KNOTS((3,3),(3,2,2,2,3),(-0.000347234788822782,0.411138013168365),
(-3.14159265358979,-1.5707963267949,0.,1.5707963267949,3.14159265358979),
 .UNSPECIFIED.)
GEOMETRIC_REPRESENTATION_ITEM()
RATIONAL_B_SPLINE_SURFACE(((1.,0.707106781186548,1.,0.707106781186548,1.,
0.707106781186548,1.,0.707106781186548,1.),(0.978909540707877,0.692193574402748,
0.978909540707877,0.692193574402748,0.978909540707877,0.692193574402748,
0.978909540707877,0.692193574402748,0.978909540707877),(1.,0.707106781186548,
1.,0.707106781186548,1.,0.707106781186548,1.,0.707106781186548,1.)))
REPRESENTATION_ITEM('')
SURFACE()
);
#2406=(
BOUNDED_SURFACE()
B_SPLINE_SURFACE(3,3,((#116850,#116851,#116852,#116853,#116854,#116855,
#116856,#116857),(#116858,#116859,#116860,#116861,#116862,#116863,#116864,
#116865),(#116866,#116867,#116868,#116869,#116870,#116871,#116872,#116873),
(#116874,#116875,#116876,#116877,#116878,#116879,#116880,#116881)),
 .UNSPECIFIED.,.F.,.F.,.F.)
B_SPLINE_SURFACE_WITH_KNOTS((4,4),(4,1,1,1,1,4),(0.,1.),(0.,0.029644668996018,
0.295068368107701,0.594721077667762,0.933272474288206,1.),.UNSPECIFIED.)
GEOMETRIC_REPRESENTATION_ITEM()
RATIONAL_B_SPLINE_SURFACE(((1.155703625555,1.155703625555,1.155703625555,
1.155703625555,1.155703625555,1.155703625555,1.155703625555,1.155703625555),
(0.9480987914817,0.9480987914817,0.9480987914817,0.9480987914817,0.9480987914817,
0.9480987914817,0.9480987914817,0.9480987914817),(0.9480987914817,0.9480987914817,
0.9480987914817,0.9480987914817,0.9480987914817,0.9480987914817,0.9480987914817,
0.9480987914817),(1.155703625555,1.155703625555,1.155703625555,1.155703625555,
1.155703625555,1.155703625555,1.155703625555,1.155703625555)))
REPRESENTATION_ITEM('')
SURFACE()
);
#2407=(
BOUNDED_SURFACE()
B_SPLINE_SURFACE(3,3,((#116993,#116994,#116995,#116996,#116997,#116998,
#116999,#117000,#117001,#117002,#117003,#117004,#117005,#117006),(#117007,
#117008,#117009,#117010,#117011,#117012,#117013,#117014,#117015,#117016,
#117017,#117018,#117019,#117020),(#117021,#117022,#117023,#117024,#117025,
#117026,#117027,#117028,#117029,#117030,#117031,#117032,#117033,#117034),
(#117035,#117036,#117037,#117038,#117039,#117040,#117041,#117042,#117043,
#117044,#117045,#117046,#117047,#117048)),.UNSPECIFIED.,.F.,.F.,.F.)
B_SPLINE_SURFACE_WITH_KNOTS((4,4),(4,1,1,1,1,1,1,1,1,1,1,4),(0.,1.),(0.,
0.0973878961741514,0.197407551664285,0.282741541036489,0.368602466936746,
0.462528035468287,0.558082759241583,0.651875585473768,0.746019006514905,
0.842958604322709,0.945166921256564,1.),.UNSPECIFIED.)
GEOMETRIC_REPRESENTATION_ITEM()
RATIONAL_B_SPLINE_SURFACE(((1.120036296291,1.120036296291,1.120036296291,
1.120036296291,1.120036296291,1.120036296291,1.120036296291,1.120036296291,
1.120036296291,1.120036296291,1.120036296291,1.120036296291,1.120036296291,
1.120036296291),(0.9599879012363,0.9599879012363,0.9599879012363,0.9599879012363,
0.9599879012363,0.9599879012363,0.9599879012363,0.9599879012363,0.9599879012363,
0.9599879012363,0.9599879012363,0.9599879012363,0.9599879012363,0.9599879012363),
(0.9599879012363,0.9599879012363,0.9599879012363,0.9599879012363,0.9599879012363,
0.9599879012363,0.9599879012363,0.9599879012363,0.9599879012363,0.9599879012363,
0.9599879012363,0.9599879012363,0.9599879012363,0.9599879012363),(1.120036296291,
1.120036296291,1.120036296291,1.120036296291,1.120036296291,1.120036296291,
1.120036296291,1.120036296291,1.120036296291,1.120036296291,1.120036296291,
1.120036296291,1.120036296291,1.120036296291)))
REPRESENTATION_ITEM('')
SURFACE()
);
#2408=(
BOUNDED_SURFACE()
B_SPLINE_SURFACE(3,3,((#117119,#117120,#117121,#117122,#117123,#117124,
#117125,#117126,#117127,#117128,#117129,#117130,#117131),(#117132,#117133,
#117134,#117135,#117136,#117137,#117138,#117139,#117140,#117141,#117142,
#117143,#117144),(#117145,#117146,#117147,#117148,#117149,#117150,#117151,
#117152,#117153,#117154,#117155,#117156,#117157),(#117158,#117159,#117160,
#117161,#117162,#117163,#117164,#117165,#117166,#117167,#117168,#117169,
#117170)),.UNSPECIFIED.,.F.,.F.,.F.)
B_SPLINE_SURFACE_WITH_KNOTS((4,4),(4,1,1,1,1,1,1,1,1,1,4),(0.,1.),(0.,0.0998120955522525,
0.242016858642978,0.370462774661701,0.48666884032665,0.592130131858907,
0.688274163622353,0.775605045484402,0.855250354769886,0.929728823459487,
1.),.UNSPECIFIED.)
GEOMETRIC_REPRESENTATION_ITEM()
RATIONAL_B_SPLINE_SURFACE(((1.293938747545,1.293938747545,1.293938747545,
1.293938747545,1.293938747545,1.293938747545,1.293938747545,1.293938747545,
1.293938747545,1.293938747545,1.293938747545,1.293938747545,1.293938747545),
(0.9020204174849,0.9020204174849,0.9020204174849,0.9020204174849,0.9020204174849,
0.9020204174849,0.9020204174849,0.9020204174849,0.9020204174849,0.9020204174849,
0.9020204174849,0.9020204174849,0.9020204174849),(0.9020204174849,0.9020204174849,
0.9020204174849,0.9020204174849,0.9020204174849,0.9020204174849,0.9020204174849,
0.9020204174849,0.9020204174849,0.9020204174849,0.9020204174849,0.9020204174849,
0.9020204174849),(1.293938747545,1.293938747545,1.293938747545,1.293938747545,
1.293938747545,1.293938747545,1.293938747545,1.293938747545,1.293938747545,
1.293938747545,1.293938747545,1.293938747545,1.293938747545)))
REPRESENTATION_ITEM('')
SURFACE()
);
#2409=(
BOUNDED_SURFACE()
B_SPLINE_SURFACE(3,3,((#117275,#117276,#117277,#117278,#117279,#117280),
(#117281,#117282,#117283,#117284,#117285,#117286),(#117287,#117288,#117289,
#117290,#117291,#117292),(#117293,#117294,#117295,#117296,#117297,#117298)),
 .UNSPECIFIED.,.F.,.F.,.F.)
B_SPLINE_SURFACE_WITH_KNOTS((4,4),(4,1,1,4),(0.,1.),(0.,0.285815104154731,
0.750510867666097,1.),.UNSPECIFIED.)
GEOMETRIC_REPRESENTATION_ITEM()
RATIONAL_B_SPLINE_SURFACE(((1.365416124288,1.365416124288,1.365416124288,
1.365416124288,1.365416124288,1.365416124288),(0.8781946252374,0.8781946252374,
0.8781946252374,0.8781946252374,0.8781946252374,0.8781946252374),(0.8781946252374,
0.8781946252374,0.8781946252374,0.8781946252374,0.8781946252374,0.8781946252374),
(1.365416124288,1.365416124288,1.365416124288,1.365416124288,1.365416124288,
1.365416124288)))
REPRESENTATION_ITEM('')
SURFACE()
);
#2410=(
BOUNDED_SURFACE()
B_SPLINE_SURFACE(3,3,((#117370,#117371,#117372,#117373,#117374,#117375,
#117376,#117377,#117378),(#117379,#117380,#117381,#117382,#117383,#117384,
#117385,#117386,#117387),(#117388,#117389,#117390,#117391,#117392,#117393,
#117394,#117395,#117396),(#117397,#117398,#117399,#117400,#117401,#117402,
#117403,#117404,#117405)),.UNSPECIFIED.,.F.,.F.,.F.)
B_SPLINE_SURFACE_WITH_KNOTS((4,4),(4,1,1,1,1,1,4),(0.,1.),(0.,0.16964553092277,
0.380015263105082,0.568987634495723,0.737810837959708,0.889292577451102,
1.),.UNSPECIFIED.)
GEOMETRIC_REPRESENTATION_ITEM()
RATIONAL_B_SPLINE_SURFACE(((1.365402191724,1.365402191724,1.365402191724,
1.365402191724,1.365402191724,1.365402191724,1.365402191724,1.365402191724,
1.365402191724),(0.8781992694255,0.8781992694255,0.8781992694255,0.8781992694255,
0.8781992694255,0.8781992694255,0.8781992694255,0.8781992694255,0.8781992694255),
(0.8781992694255,0.8781992694255,0.8781992694255,0.8781992694255,0.8781992694255,
0.8781992694255,0.8781992694255,0.8781992694255,0.8781992694255),(1.365402191724,
1.365402191724,1.365402191724,1.365402191724,1.365402191724,1.365402191724,
1.365402191724,1.365402191724,1.365402191724)))
REPRESENTATION_ITEM('')
SURFACE()
);
#2411=(
BOUNDED_SURFACE()
B_SPLINE_SURFACE(3,3,((#117540,#117541,#117542,#117543,#117544,#117545,
#117546,#117547,#117548,#117549,#117550,#117551,#117552,#117553,#117554),
(#117555,#117556,#117557,#117558,#117559,#117560,#117561,#117562,#117563,
#117564,#117565,#117566,#117567,#117568,#117569),(#117570,#117571,#117572,
#117573,#117574,#117575,#117576,#117577,#117578,#117579,#117580,#117581,
#117582,#117583,#117584),(#117585,#117586,#117587,#117588,#117589,#117590,
#117591,#117592,#117593,#117594,#117595,#117596,#117597,#117598,#117599)),
 .UNSPECIFIED.,.F.,.F.,.F.)
B_SPLINE_SURFACE_WITH_KNOTS((4,4),(4,1,1,1,1,1,1,1,1,1,1,1,4),(0.,1.),(0.,
0.0133121513771896,0.155629666020943,0.286186478435823,0.406137126501649,
0.515333723729991,0.614145412195474,0.703320557553204,0.783598098684785,
0.855708888389128,0.920381450070005,0.978344668750669,1.),.UNSPECIFIED.)
GEOMETRIC_REPRESENTATION_ITEM()
RATIONAL_B_SPLINE_SURFACE(((1.250202018407,1.250202018407,1.250202018407,
1.250202018407,1.250202018407,1.250202018407,1.250202018407,1.250202018407,
1.250202018407,1.250202018407,1.250202018407,1.250202018407,1.250202018407,
1.250202018407,1.250202018407),(0.9165993271976,0.9165993271976,0.9165993271976,
0.9165993271976,0.9165993271976,0.9165993271976,0.9165993271976,0.9165993271976,
0.9165993271976,0.9165993271976,0.9165993271976,0.9165993271976,0.9165993271976,
0.9165993271976,0.9165993271976),(0.9165993271976,0.9165993271976,0.9165993271976,
0.9165993271976,0.9165993271976,0.9165993271976,0.9165993271976,0.9165993271976,
0.9165993271976,0.9165993271976,0.9165993271976,0.9165993271976,0.9165993271976,
0.9165993271976,0.9165993271976),(1.250202018407,1.250202018407,1.250202018407,
1.250202018407,1.250202018407,1.250202018407,1.250202018407,1.250202018407,
1.250202018407,1.250202018407,1.250202018407,1.250202018407,1.250202018407,
1.250202018407,1.250202018407)))
REPRESENTATION_ITEM('')
SURFACE()
);
#2412=(
BOUNDED_SURFACE()
B_SPLINE_SURFACE(3,3,((#117620,#117621,#117622,#117623,#117624,#117625,
#117626,#117627,#117628,#117629,#117630,#117631,#117632,#117633,#117634),
(#117635,#117636,#117637,#117638,#117639,#117640,#117641,#117642,#117643,
#117644,#117645,#117646,#117647,#117648,#117649),(#117650,#117651,#117652,
#117653,#117654,#117655,#117656,#117657,#117658,#117659,#117660,#117661,
#117662,#117663,#117664),(#117665,#117666,#117667,#117668,#117669,#117670,
#117671,#117672,#117673,#117674,#117675,#117676,#117677,#117678,#117679)),
 .UNSPECIFIED.,.F.,.F.,.F.)
B_SPLINE_SURFACE_WITH_KNOTS((4,4),(4,1,1,1,1,1,1,1,1,1,1,1,4),(0.,1.),(0.,
0.0993304258737296,0.195288926245669,0.279764193611795,0.357478306071918,
0.437884275258005,0.519144483225908,0.599505042528899,0.680729928008849,
0.764271760028651,0.850469396333162,0.939451116239952,1.),.UNSPECIFIED.)
GEOMETRIC_REPRESENTATION_ITEM()
RATIONAL_B_SPLINE_SURFACE(((1.519035604992,1.519035604992,1.519035604992,
1.519035604992,1.519035604992,1.519035604992,1.519035604992,1.519035604992,
1.519035604992,1.519035604992,1.519035604992,1.519035604992,1.519035604992,
1.519035604992,1.519035604992),(0.8269881316694,0.8269881316694,0.8269881316694,
0.8269881316694,0.8269881316694,0.8269881316694,0.8269881316694,0.8269881316694,
0.8269881316694,0.8269881316694,0.8269881316694,0.8269881316694,0.8269881316694,
0.8269881316694,0.8269881316694),(0.8269881316694,0.8269881316694,0.8269881316694,
0.8269881316694,0.8269881316694,0.8269881316694,0.8269881316694,0.8269881316694,
0.8269881316694,0.8269881316694,0.8269881316694,0.8269881316694,0.8269881316694,
0.8269881316694,0.8269881316694),(1.519035604992,1.519035604992,1.519035604992,
1.519035604992,1.519035604992,1.519035604992,1.519035604992,1.519035604992,
1.519035604992,1.519035604992,1.519035604992,1.519035604992,1.519035604992,
1.519035604992,1.519035604992)))
REPRESENTATION_ITEM('')
SURFACE()
);
#2413=(
BOUNDED_SURFACE()
B_SPLINE_SURFACE(3,3,((#117877,#117878,#117879,#117880,#117881,#117882,
#117883,#117884,#117885),(#117886,#117887,#117888,#117889,#117890,#117891,
#117892,#117893,#117894),(#117895,#117896,#117897,#117898,#117899,#117900,
#117901,#117902,#117903),(#117904,#117905,#117906,#117907,#117908,#117909,
#117910,#117911,#117912)),.UNSPECIFIED.,.F.,.F.,.F.)
B_SPLINE_SURFACE_WITH_KNOTS((4,4),(4,1,1,1,1,1,4),(0.,1.),(0.,0.192791195394506,
0.411717423884289,0.621651126749646,0.812473561049781,0.973652979997317,
1.),.UNSPECIFIED.)
GEOMETRIC_REPRESENTATION_ITEM()
RATIONAL_B_SPLINE_SURFACE(((1.365114458785,1.365114458785,1.365114458785,
1.365114458785,1.365114458785,1.365114458785,1.365114458785,1.365114458785,
1.365114458785),(0.878295180405,0.878295180405,0.878295180405,0.878295180405,
0.878295180405,0.878295180405,0.878295180405,0.878295180405,0.878295180405),
(0.878295180405,0.878295180405,0.878295180405,0.878295180405,0.878295180405,
0.878295180405,0.878295180405,0.878295180405,0.878295180405),(1.365114458785,
1.365114458785,1.365114458785,1.365114458785,1.365114458785,1.365114458785,
1.365114458785,1.365114458785,1.365114458785)))
REPRESENTATION_ITEM('')
SURFACE()
);
#2414=(
BOUNDED_SURFACE()
B_SPLINE_SURFACE(3,3,((#117949,#117950,#117951,#117952,#117953,#117954,
#117955,#117956,#117957,#117958,#117959,#117960,#117961,#117962,#117963,
#117964,#117965),(#117966,#117967,#117968,#117969,#117970,#117971,#117972,
#117973,#117974,#117975,#117976,#117977,#117978,#117979,#117980,#117981,
#117982),(#117983,#117984,#117985,#117986,#117987,#117988,#117989,#117990,
#117991,#117992,#117993,#117994,#117995,#117996,#117997,#117998,#117999),
(#118000,#118001,#118002,#118003,#118004,#118005,#118006,#118007,#118008,
#118009,#118010,#118011,#118012,#118013,#118014,#118015,#118016)),
 .UNSPECIFIED.,.F.,.F.,.F.)
B_SPLINE_SURFACE_WITH_KNOTS((4,4),(4,1,1,1,1,1,1,1,1,1,1,1,1,1,4),(0.,1.),
(0.,0.0494607190127907,0.109552090730043,0.169758737534662,0.230148354533949,
0.290560261854406,0.350306525877549,0.40987255925942,0.472274987329372,
0.540774950770296,0.617873523590501,0.704101656323432,0.799618934750072,
0.904474902078167,1.),.UNSPECIFIED.)
GEOMETRIC_REPRESENTATION_ITEM()
RATIONAL_B_SPLINE_SURFACE(((1.220899718882,1.220899718882,1.220899718882,
1.220899718882,1.220899718882,1.220899718882,1.220899718882,1.220899718882,
1.220899718882,1.220899718882,1.220899718882,1.220899718882,1.220899718882,
1.220899718882,1.220899718882,1.220899718882,1.220899718882),(0.9263667603727,
0.9263667603727,0.9263667603727,0.9263667603727,0.9263667603727,0.9263667603727,
0.9263667603727,0.9263667603727,0.9263667603727,0.9263667603727,0.9263667603727,
0.9263667603727,0.9263667603727,0.9263667603727,0.9263667603727,0.9263667603727,
0.9263667603727),(0.9263667603727,0.9263667603727,0.9263667603727,0.9263667603727,
0.9263667603727,0.9263667603727,0.9263667603727,0.9263667603727,0.9263667603727,
0.9263667603727,0.9263667603727,0.9263667603727,0.9263667603727,0.9263667603727,
0.9263667603727,0.9263667603727,0.9263667603727),(1.220899718882,1.220899718882,
1.220899718882,1.220899718882,1.220899718882,1.220899718882,1.220899718882,
1.220899718882,1.220899718882,1.220899718882,1.220899718882,1.220899718882,
1.220899718882,1.220899718882,1.220899718882,1.220899718882,1.220899718882)))
REPRESENTATION_ITEM('')
SURFACE()
);
#2415=(
BOUNDED_SURFACE()
B_SPLINE_SURFACE(3,3,((#118215,#118216,#118217,#118218,#118219,#118220),
(#118221,#118222,#118223,#118224,#118225,#118226),(#118227,#118228,#118229,
#118230,#118231,#118232),(#118233,#118234,#118235,#118236,#118237,#118238)),
 .UNSPECIFIED.,.F.,.F.,.F.)
B_SPLINE_SURFACE_WITH_KNOTS((4,4),(4,1,1,4),(0.,1.),(0.,0.447612208701937,
0.9386901437205,1.),.UNSPECIFIED.)
GEOMETRIC_REPRESENTATION_ITEM()
RATIONAL_B_SPLINE_SURFACE(((1.132184188967,1.132184188967,1.132184188967,
1.132184188967,1.132184188967,1.132184188967),(0.9559386036777,0.9559386036777,
0.9559386036777,0.9559386036777,0.9559386036777,0.9559386036777),(0.9559386036777,
0.9559386036777,0.9559386036777,0.9559386036777,0.9559386036777,0.9559386036777),
(1.132184188967,1.132184188967,1.132184188967,1.132184188967,1.132184188967,
1.132184188967)))
REPRESENTATION_ITEM('')
SURFACE()
);
#2416=(
BOUNDED_SURFACE()
B_SPLINE_SURFACE(3,3,((#118311,#118312,#118313,#118314,#118315,#118316,
#118317,#118318,#118319,#118320,#118321,#118322,#118323),(#118324,#118325,
#118326,#118327,#118328,#118329,#118330,#118331,#118332,#118333,#118334,
#118335,#118336),(#118337,#118338,#118339,#118340,#118341,#118342,#118343,
#118344,#118345,#118346,#118347,#118348,#118349),(#118350,#118351,#118352,
#118353,#118354,#118355,#118356,#118357,#118358,#118359,#118360,#118361,
#118362)),.UNSPECIFIED.,.F.,.F.,.F.)
B_SPLINE_SURFACE_WITH_KNOTS((4,4),(4,1,1,1,1,1,1,1,1,1,4),(0.,1.),(0.,0.0726579731238688,
0.165540666880435,0.265778081450179,0.365083883521996,0.460784315560169,
0.55478726880033,0.657326573221902,0.774847166279867,0.904679558230862,
1.),.UNSPECIFIED.)
GEOMETRIC_REPRESENTATION_ITEM()
RATIONAL_B_SPLINE_SURFACE(((1.132183962178,1.132183962178,1.132183962178,
1.132183962178,1.132183962178,1.132183962178,1.132183962178,1.132183962178,
1.132183962178,1.132183962178,1.132183962178,1.132183962178,1.132183962178),
(0.955938679274,0.955938679274,0.955938679274,0.955938679274,0.955938679274,
0.955938679274,0.955938679274,0.955938679274,0.955938679274,0.955938679274,
0.955938679274,0.955938679274,0.955938679274),(0.955938679274,0.955938679274,
0.955938679274,0.955938679274,0.955938679274,0.955938679274,0.955938679274,
0.955938679274,0.955938679274,0.955938679274,0.955938679274,0.955938679274,
0.955938679274),(1.132183962178,1.132183962178,1.132183962178,1.132183962178,
1.132183962178,1.132183962178,1.132183962178,1.132183962178,1.132183962178,
1.132183962178,1.132183962178,1.132183962178,1.132183962178)))
REPRESENTATION_ITEM('')
SURFACE()
);
#2417=(
BOUNDED_SURFACE()
B_SPLINE_SURFACE(3,3,((#118632,#118633,#118634,#118635,#118636,#118637,
#118638,#118639,#118640,#118641,#118642,#118643,#118644,#118645,#118646,
#118647,#118648,#118649,#118650,#118651,#118652,#118653),(#118654,#118655,
#118656,#118657,#118658,#118659,#118660,#118661,#118662,#118663,#118664,
#118665,#118666,#118667,#118668,#118669,#118670,#118671,#118672,#118673,
#118674,#118675),(#118676,#118677,#118678,#118679,#118680,#118681,#118682,
#118683,#118684,#118685,#118686,#118687,#118688,#118689,#118690,#118691,
#118692,#118693,#118694,#118695,#118696,#118697),(#118698,#118699,#118700,
#118701,#118702,#118703,#118704,#118705,#118706,#118707,#118708,#118709,
#118710,#118711,#118712,#118713,#118714,#118715,#118716,#118717,#118718,
#118719)),.UNSPECIFIED.,.F.,.F.,.F.)
B_SPLINE_SURFACE_WITH_KNOTS((4,4),(4,1,1,1,1,1,1,1,1,1,1,1,1,1,1,1,1,1,
1,4),(0.,1.),(0.,0.00179852648676455,0.0684134361341035,0.138569448512766,
0.212049560253872,0.281023409010827,0.341871044231178,0.39611355557608,
0.444140369343199,0.487339341535663,0.530585789342856,0.575339323721559,
0.620494040055896,0.664485227938823,0.706756351680787,0.752682439877936,
0.80459823145977,0.863065026247903,0.928980423200659,1.),.UNSPECIFIED.)
GEOMETRIC_REPRESENTATION_ITEM()
RATIONAL_B_SPLINE_SURFACE(((1.255321138723,1.255321138723,1.255321138723,
1.255321138723,1.255321138723,1.255321138723,1.255321138723,1.255321138723,
1.255321138723,1.255321138723,1.255321138723,1.255321138723,1.255321138723,
1.255321138723,1.255321138723,1.255321138723,1.255321138723,1.255321138723,
1.255321138723,1.255321138723,1.255321138723,1.255321138723),(0.914892953759,
0.914892953759,0.914892953759,0.914892953759,0.914892953759,0.914892953759,
0.914892953759,0.914892953759,0.914892953759,0.914892953759,0.914892953759,
0.914892953759,0.914892953759,0.914892953759,0.914892953759,0.914892953759,
0.914892953759,0.914892953759,0.914892953759,0.914892953759,0.914892953759,
0.914892953759),(0.914892953759,0.914892953759,0.914892953759,0.914892953759,
0.914892953759,0.914892953759,0.914892953759,0.914892953759,0.914892953759,
0.914892953759,0.914892953759,0.914892953759,0.914892953759,0.914892953759,
0.914892953759,0.914892953759,0.914892953759,0.914892953759,0.914892953759,
0.914892953759,0.914892953759,0.914892953759),(1.255321138723,1.255321138723,
1.255321138723,1.255321138723,1.255321138723,1.255321138723,1.255321138723,
1.255321138723,1.255321138723,1.255321138723,1.255321138723,1.255321138723,
1.255321138723,1.255321138723,1.255321138723,1.255321138723,1.255321138723,
1.255321138723,1.255321138723,1.255321138723,1.255321138723,1.255321138723)))
REPRESENTATION_ITEM('')
SURFACE()
);
#2418=(
BOUNDED_SURFACE()
B_SPLINE_SURFACE(3,3,((#118976,#118977,#118978,#118979,#118980),(#118981,
#118982,#118983,#118984,#118985),(#118986,#118987,#118988,#118989,#118990),
(#118991,#118992,#118993,#118994,#118995)),.UNSPECIFIED.,.F.,.F.,.F.)
B_SPLINE_SURFACE_WITH_KNOTS((4,4),(4,1,4),(0.,1.),(0.,0.469552763526497,
1.),.UNSPECIFIED.)
GEOMETRIC_REPRESENTATION_ITEM()
RATIONAL_B_SPLINE_SURFACE(((1.365422134914,1.365422134914,1.365422134914,
1.365422134914,1.365422134914),(0.8781926216954,0.8781926216954,0.8781926216954,
0.8781926216954,0.8781926216954),(0.8781926216954,0.8781926216954,0.8781926216954,
0.8781926216954,0.8781926216954),(1.365422134914,1.365422134914,1.365422134914,
1.365422134914,1.365422134914)))
REPRESENTATION_ITEM('')
SURFACE()
);
#2419=(
BOUNDED_SURFACE()
B_SPLINE_SURFACE(3,3,((#119003,#119004,#119005,#119006,#119007,#119008,
#119009,#119010,#119011,#119012,#119013,#119014,#119015,#119016,#119017),
(#119018,#119019,#119020,#119021,#119022,#119023,#119024,#119025,#119026,
#119027,#119028,#119029,#119030,#119031,#119032),(#119033,#119034,#119035,
#119036,#119037,#119038,#119039,#119040,#119041,#119042,#119043,#119044,
#119045,#119046,#119047),(#119048,#119049,#119050,#119051,#119052,#119053,
#119054,#119055,#119056,#119057,#119058,#119059,#119060,#119061,#119062)),
 .UNSPECIFIED.,.F.,.F.,.F.)
B_SPLINE_SURFACE_WITH_KNOTS((4,4),(4,1,1,1,1,1,1,1,1,1,1,1,4),(0.,1.),(0.,
0.0436634499300064,0.166198886318839,0.276683120299012,0.375301849455497,
0.46256216640866,0.540611125333518,0.612179050794216,0.680223368266989,
0.748962133643248,0.825081182648611,0.91081093482415,1.),.UNSPECIFIED.)
GEOMETRIC_REPRESENTATION_ITEM()
RATIONAL_B_SPLINE_SURFACE(((1.351003587175,1.351003587175,1.351003587175,
1.351003587175,1.351003587175,1.351003587175,1.351003587175,1.351003587175,
1.351003587175,1.351003587175,1.351003587175,1.351003587175,1.351003587175,
1.351003587175,1.351003587175),(0.882998804275,0.882998804275,0.882998804275,
0.882998804275,0.882998804275,0.882998804275,0.882998804275,0.882998804275,
0.882998804275,0.882998804275,0.882998804275,0.882998804275,0.882998804275,
0.882998804275,0.882998804275),(0.882998804275,0.882998804275,0.882998804275,
0.882998804275,0.882998804275,0.882998804275,0.882998804275,0.882998804275,
0.882998804275,0.882998804275,0.882998804275,0.882998804275,0.882998804275,
0.882998804275,0.882998804275),(1.351003587175,1.351003587175,1.351003587175,
1.351003587175,1.351003587175,1.351003587175,1.351003587175,1.351003587175,
1.351003587175,1.351003587175,1.351003587175,1.351003587175,1.351003587175,
1.351003587175,1.351003587175)))
REPRESENTATION_ITEM('')
SURFACE()
);
#2420=(
BOUNDED_SURFACE()
B_SPLINE_SURFACE(3,3,((#119272,#119273,#119274,#119275,#119276,#119277,
#119278,#119279,#119280,#119281,#119282,#119283,#119284,#119285,#119286,
#119287,#119288),(#119289,#119290,#119291,#119292,#119293,#119294,#119295,
#119296,#119297,#119298,#119299,#119300,#119301,#119302,#119303,#119304,
#119305),(#119306,#119307,#119308,#119309,#119310,#119311,#119312,#119313,
#119314,#119315,#119316,#119317,#119318,#119319,#119320,#119321,#119322),
(#119323,#119324,#119325,#119326,#119327,#119328,#119329,#119330,#119331,
#119332,#119333,#119334,#119335,#119336,#119337,#119338,#119339)),
 .UNSPECIFIED.,.F.,.F.,.F.)
B_SPLINE_SURFACE_WITH_KNOTS((4,4),(4,1,1,1,1,1,1,1,1,1,1,1,1,1,4),(0.,1.),
(0.,0.0934555018707438,0.190098316562109,0.277412276927369,0.35430591142789,
0.422006518582467,0.485074288423762,0.548771616802643,0.613848873864871,
0.679223443651306,0.742843206526981,0.805944165791561,0.877524725574254,
0.957638281560363,1.),.UNSPECIFIED.)
GEOMETRIC_REPRESENTATION_ITEM()
RATIONAL_B_SPLINE_SURFACE(((1.219577491546,1.219577491546,1.219577491546,
1.219577491546,1.219577491546,1.219577491546,1.219577491546,1.219577491546,
1.219577491546,1.219577491546,1.219577491546,1.219577491546,1.219577491546,
1.219577491546,1.219577491546,1.219577491546,1.219577491546),(0.9268075028179,
0.9268075028179,0.9268075028179,0.9268075028179,0.9268075028179,0.9268075028179,
0.9268075028179,0.9268075028179,0.9268075028179,0.9268075028179,0.9268075028179,
0.9268075028179,0.9268075028179,0.9268075028179,0.9268075028179,0.9268075028179,
0.9268075028179),(0.9268075028179,0.9268075028179,0.9268075028179,0.9268075028179,
0.9268075028179,0.9268075028179,0.9268075028179,0.9268075028179,0.9268075028179,
0.9268075028179,0.9268075028179,0.9268075028179,0.9268075028179,0.9268075028179,
0.9268075028179,0.9268075028179,0.9268075028179),(1.219577491546,1.219577491546,
1.219577491546,1.219577491546,1.219577491546,1.219577491546,1.219577491546,
1.219577491546,1.219577491546,1.219577491546,1.219577491546,1.219577491546,
1.219577491546,1.219577491546,1.219577491546,1.219577491546,1.219577491546)))
REPRESENTATION_ITEM('')
SURFACE()
);
#2421=(
BOUNDED_SURFACE()
B_SPLINE_SURFACE(3,3,((#119374,#119375,#119376,#119377,#119378,#119379,
#119380,#119381,#119382,#119383,#119384,#119385),(#119386,#119387,#119388,
#119389,#119390,#119391,#119392,#119393,#119394,#119395,#119396,#119397),
(#119398,#119399,#119400,#119401,#119402,#119403,#119404,#119405,#119406,
#119407,#119408,#119409),(#119410,#119411,#119412,#119413,#119414,#119415,
#119416,#119417,#119418,#119419,#119420,#119421)),.UNSPECIFIED.,.F.,.F.,
 .F.)
B_SPLINE_SURFACE_WITH_KNOTS((4,4),(4,1,1,1,1,1,1,1,1,4),(0.,1.),(0.,0.0491574788676924,
0.219592918841423,0.374383193798209,0.513141463206398,0.639408605121616,
0.757222110220193,0.870630976300795,0.983497613603143,1.),.UNSPECIFIED.)
GEOMETRIC_REPRESENTATION_ITEM()
RATIONAL_B_SPLINE_SURFACE(((1.035729017359,1.035729017359,1.035729017359,
1.035729017359,1.035729017359,1.035729017359,1.035729017359,1.035729017359,
1.035729017359,1.035729017359,1.035729017359,1.035729017359),(0.988090327547,
0.988090327547,0.988090327547,0.988090327547,0.988090327547,0.988090327547,
0.988090327547,0.988090327547,0.988090327547,0.988090327547,0.988090327547,
0.988090327547),(0.988090327547,0.988090327547,0.988090327547,0.988090327547,
0.988090327547,0.988090327547,0.988090327547,0.988090327547,0.988090327547,
0.988090327547,0.988090327547,0.988090327547),(1.035729017359,1.035729017359,
1.035729017359,1.035729017359,1.035729017359,1.035729017359,1.035729017359,
1.035729017359,1.035729017359,1.035729017359,1.035729017359,1.035729017359)))
REPRESENTATION_ITEM('')
SURFACE()
);
#2422=(
BOUNDED_SURFACE()
B_SPLINE_SURFACE(3,3,((#119834,#119835,#119836,#119837,#119838,#119839,
#119840,#119841,#119842),(#119843,#119844,#119845,#119846,#119847,#119848,
#119849,#119850,#119851),(#119852,#119853,#119854,#119855,#119856,#119857,
#119858,#119859,#119860),(#119861,#119862,#119863,#119864,#119865,#119866,
#119867,#119868,#119869)),.UNSPECIFIED.,.F.,.F.,.F.)
B_SPLINE_SURFACE_WITH_KNOTS((4,4),(4,1,1,1,1,1,4),(0.,1.),(0.,0.124217072598013,
0.310755649966071,0.499972699325182,0.689255533447521,0.875770604197989,
1.),.UNSPECIFIED.)
GEOMETRIC_REPRESENTATION_ITEM()
RATIONAL_B_SPLINE_SURFACE(((1.043303594112,1.043303594112,1.043303594112,
1.043303594112,1.043303594112,1.043303594112,1.043303594112,1.043303594112,
1.043303594112),(0.9855654686295,0.9855654686295,0.9855654686295,0.9855654686295,
0.9855654686295,0.9855654686295,0.9855654686295,0.9855654686295,0.9855654686295),
(0.9855654686295,0.9855654686295,0.9855654686295,0.9855654686295,0.9855654686295,
0.9855654686295,0.9855654686295,0.9855654686295,0.9855654686295),(1.043303594112,
1.043303594112,1.043303594112,1.043303594112,1.043303594112,1.043303594112,
1.043303594112,1.043303594112,1.043303594112)))
REPRESENTATION_ITEM('')
SURFACE()
);
#2423=(
BOUNDED_SURFACE()
B_SPLINE_SURFACE(3,3,((#119949,#119950,#119951,#119952,#119953,#119954),
(#119955,#119956,#119957,#119958,#119959,#119960),(#119961,#119962,#119963,
#119964,#119965,#119966),(#119967,#119968,#119969,#119970,#119971,#119972)),
 .UNSPECIFIED.,.F.,.F.,.F.)
B_SPLINE_SURFACE_WITH_KNOTS((4,4),(4,1,1,4),(0.,1.),(0.,0.290351630545127,
0.6856968431484,1.),.UNSPECIFIED.)
GEOMETRIC_REPRESENTATION_ITEM()
RATIONAL_B_SPLINE_SURFACE(((1.04998815347,1.04998815347,1.04998815347,1.04998815347,
1.04998815347,1.04998815347),(0.9833372821767,0.9833372821767,0.9833372821767,
0.9833372821767,0.9833372821767,0.9833372821767),(0.9833372821767,0.9833372821767,
0.9833372821767,0.9833372821767,0.9833372821767,0.9833372821767),(1.04998815347,
1.04998815347,1.04998815347,1.04998815347,1.04998815347,1.04998815347)))
REPRESENTATION_ITEM('')
SURFACE()
);
#2424=(
BOUNDED_SURFACE()
B_SPLINE_SURFACE(3,3,((#119986,#119987,#119988,#119989,#119990,#119991,
#119992,#119993,#119994,#119995,#119996,#119997,#119998,#119999,#120000,
#120001,#120002,#120003,#120004,#120005,#120006,#120007,#120008,#120009,
#120010,#120011),(#120012,#120013,#120014,#120015,#120016,#120017,#120018,
#120019,#120020,#120021,#120022,#120023,#120024,#120025,#120026,#120027,
#120028,#120029,#120030,#120031,#120032,#120033,#120034,#120035,#120036,
#120037),(#120038,#120039,#120040,#120041,#120042,#120043,#120044,#120045,
#120046,#120047,#120048,#120049,#120050,#120051,#120052,#120053,#120054,
#120055,#120056,#120057,#120058,#120059,#120060,#120061,#120062,#120063),
(#120064,#120065,#120066,#120067,#120068,#120069,#120070,#120071,#120072,
#120073,#120074,#120075,#120076,#120077,#120078,#120079,#120080,#120081,
#120082,#120083,#120084,#120085,#120086,#120087,#120088,#120089)),
 .UNSPECIFIED.,.F.,.F.,.F.)
B_SPLINE_SURFACE_WITH_KNOTS((4,4),(4,1,1,1,1,1,1,1,1,1,1,1,1,1,1,1,1,1,
1,1,1,1,1,4),(0.,1.),(0.,0.0604690860171424,0.125750773183185,0.184471262697933,
0.23763259918399,0.285727129729686,0.328587237304838,0.367339669645258,
0.404193671801395,0.441150852354512,0.478525964786371,0.515930821440246,
0.552912972270284,0.589583703038061,0.62782560752874,0.669834379167559,
0.716144402441833,0.760844285447638,0.806281350038666,0.853281683657045,
0.900484124800725,0.947112731733202,0.993172991216528,1.),.UNSPECIFIED.)
GEOMETRIC_REPRESENTATION_ITEM()
RATIONAL_B_SPLINE_SURFACE(((1.050211534691,1.050211534691,1.050211534691,
1.050211534691,1.050211534691,1.050211534691,1.050211534691,1.050211534691,
1.050211534691,1.050211534691,1.050211534691,1.050211534691,1.050211534691,
1.050211534691,1.050211534691,1.050211534691,1.050211534691,1.050211534691,
1.050211534691,1.050211534691,1.050211534691,1.050211534691,1.050211534691,
1.050211534691,1.050211534691,1.050211534691),(0.9832628217698,0.9832628217698,
0.9832628217698,0.9832628217698,0.9832628217698,0.9832628217698,0.9832628217698,
0.9832628217698,0.9832628217698,0.9832628217698,0.9832628217698,0.9832628217698,
0.9832628217698,0.9832628217698,0.9832628217698,0.9832628217698,0.9832628217698,
0.9832628217698,0.9832628217698,0.9832628217698,0.9832628217698,0.9832628217698,
0.9832628217698,0.9832628217698,0.9832628217698,0.9832628217698),(0.9832628217698,
0.9832628217698,0.9832628217698,0.9832628217698,0.9832628217698,0.9832628217698,
0.9832628217698,0.9832628217698,0.9832628217698,0.9832628217698,0.9832628217698,
0.9832628217698,0.9832628217698,0.9832628217698,0.9832628217698,0.9832628217698,
0.9832628217698,0.9832628217698,0.9832628217698,0.9832628217698,0.9832628217698,
0.9832628217698,0.9832628217698,0.9832628217698,0.9832628217698,0.9832628217698),
(1.050211534691,1.050211534691,1.050211534691,1.050211534691,1.050211534691,
1.050211534691,1.050211534691,1.050211534691,1.050211534691,1.050211534691,
1.050211534691,1.050211534691,1.050211534691,1.050211534691,1.050211534691,
1.050211534691,1.050211534691,1.050211534691,1.050211534691,1.050211534691,
1.050211534691,1.050211534691,1.050211534691,1.050211534691,1.050211534691,
1.050211534691)))
REPRESENTATION_ITEM('')
SURFACE()
);
#2425=(
BOUNDED_SURFACE()
B_SPLINE_SURFACE(3,3,((#120354,#120355,#120356,#120357,#120358,#120359,
#120360,#120361),(#120362,#120363,#120364,#120365,#120366,#120367,#120368,
#120369),(#120370,#120371,#120372,#120373,#120374,#120375,#120376,#120377),
(#120378,#120379,#120380,#120381,#120382,#120383,#120384,#120385)),
 .UNSPECIFIED.,.F.,.F.,.F.)
B_SPLINE_SURFACE_WITH_KNOTS((4,4),(4,1,1,1,1,4),(0.,1.),(0.,0.115906347737713,
0.324457197714345,0.557614394200552,0.816082473111432,1.),.UNSPECIFIED.)
GEOMETRIC_REPRESENTATION_ITEM()
RATIONAL_B_SPLINE_SURFACE(((1.04998793531,1.04998793531,1.04998793531,1.04998793531,
1.04998793531,1.04998793531,1.04998793531,1.04998793531),(0.9833373548966,
0.9833373548966,0.9833373548966,0.9833373548966,0.9833373548966,0.9833373548966,
0.9833373548966,0.9833373548966),(0.9833373548966,0.9833373548966,0.9833373548966,
0.9833373548966,0.9833373548966,0.9833373548966,0.9833373548966,0.9833373548966),
(1.04998793531,1.04998793531,1.04998793531,1.04998793531,1.04998793531,
1.04998793531,1.04998793531,1.04998793531)))
REPRESENTATION_ITEM('')
SURFACE()
);
#2426=(
BOUNDED_SURFACE()
B_SPLINE_SURFACE(3,3,((#120428,#120429,#120430,#120431,#120432,#120433),
(#120434,#120435,#120436,#120437,#120438,#120439),(#120440,#120441,#120442,
#120443,#120444,#120445),(#120446,#120447,#120448,#120449,#120450,#120451)),
 .UNSPECIFIED.,.F.,.F.,.F.)
B_SPLINE_SURFACE_WITH_KNOTS((4,4),(4,1,1,4),(0.,1.),(0.,0.261439365657105,
0.646008272416107,1.),.UNSPECIFIED.)
GEOMETRIC_REPRESENTATION_ITEM()
RATIONAL_B_SPLINE_SURFACE(((1.043303932823,1.043303932823,1.043303932823,
1.043303932823,1.043303932823,1.043303932823),(0.9855653557257,0.9855653557257,
0.9855653557257,0.9855653557257,0.9855653557257,0.9855653557257),(0.9855653557257,
0.9855653557257,0.9855653557257,0.9855653557257,0.9855653557257,0.9855653557257),
(1.043303932823,1.043303932823,1.043303932823,1.043303932823,1.043303932823,
1.043303932823)))
REPRESENTATION_ITEM('')
SURFACE()
);
#2427=(
BOUNDED_SURFACE()
B_SPLINE_SURFACE(3,3,((#120512,#120513,#120514,#120515,#120516,#120517),
(#120518,#120519,#120520,#120521,#120522,#120523),(#120524,#120525,#120526,
#120527,#120528,#120529),(#120530,#120531,#120532,#120533,#120534,#120535)),
 .UNSPECIFIED.,.F.,.F.,.F.)
B_SPLINE_SURFACE_WITH_KNOTS((4,4),(4,1,1,4),(0.,1.),(0.,0.338411219840004,
0.730847710170391,1.),.UNSPECIFIED.)
GEOMETRIC_REPRESENTATION_ITEM()
RATIONAL_B_SPLINE_SURFACE(((1.043304304122,1.043304304122,1.043304304122,
1.043304304122,1.043304304122,1.043304304122),(0.9855652319594,0.9855652319594,
0.9855652319594,0.9855652319594,0.9855652319594,0.9855652319594),(0.9855652319594,
0.9855652319594,0.9855652319594,0.9855652319594,0.9855652319594,0.9855652319594),
(1.043304304122,1.043304304122,1.043304304122,1.043304304122,1.043304304122,
1.043304304122)))
REPRESENTATION_ITEM('')
SURFACE()
);
#2428=(
BOUNDED_SURFACE()
B_SPLINE_SURFACE(3,3,((#120599,#120600,#120601,#120602,#120603,#120604,
#120605,#120606,#120607),(#120608,#120609,#120610,#120611,#120612,#120613,
#120614,#120615,#120616),(#120617,#120618,#120619,#120620,#120621,#120622,
#120623,#120624,#120625),(#120626,#120627,#120628,#120629,#120630,#120631,
#120632,#120633,#120634)),.UNSPECIFIED.,.F.,.F.,.F.)
B_SPLINE_SURFACE_WITH_KNOTS((4,4),(4,1,1,1,1,1,4),(0.,1.),(0.,0.145600865509264,
0.314399883400269,0.481396351840591,0.652048510615264,0.82890573043304,
1.),.UNSPECIFIED.)
GEOMETRIC_REPRESENTATION_ITEM()
RATIONAL_B_SPLINE_SURFACE(((1.057416537047,1.057416537047,1.057416537047,
1.057416537047,1.057416537047,1.057416537047,1.057416537047,1.057416537047,
1.057416537047),(0.9808611543175,0.9808611543175,0.9808611543175,0.9808611543175,
0.9808611543175,0.9808611543175,0.9808611543175,0.9808611543175,0.9808611543175),
(0.9808611543175,0.9808611543175,0.9808611543175,0.9808611543175,0.9808611543175,
0.9808611543175,0.9808611543175,0.9808611543175,0.9808611543175),(1.057416537047,
1.057416537047,1.057416537047,1.057416537047,1.057416537047,1.057416537047,
1.057416537047,1.057416537047,1.057416537047)))
REPRESENTATION_ITEM('')
SURFACE()
);
#2429=(
BOUNDED_SURFACE()
B_SPLINE_SURFACE(3,3,((#120749,#120750,#120751,#120752,#120753,#120754,
#120755,#120756,#120757),(#120758,#120759,#120760,#120761,#120762,#120763,
#120764,#120765,#120766),(#120767,#120768,#120769,#120770,#120771,#120772,
#120773,#120774,#120775),(#120776,#120777,#120778,#120779,#120780,#120781,
#120782,#120783,#120784)),.UNSPECIFIED.,.F.,.F.,.F.)
B_SPLINE_SURFACE_WITH_KNOTS((4,4),(4,1,1,1,1,1,4),(0.,1.),(0.,0.145967497811959,
0.326469868263455,0.503631939312401,0.67673102833901,0.85125569646002,1.),
 .UNSPECIFIED.)
GEOMETRIC_REPRESENTATION_ITEM()
RATIONAL_B_SPLINE_SURFACE(((1.057410488177,1.057410488177,1.057410488177,
1.057410488177,1.057410488177,1.057410488177,1.057410488177,1.057410488177,
1.057410488177),(0.9808631706077,0.9808631706077,0.9808631706077,0.9808631706077,
0.9808631706077,0.9808631706077,0.9808631706077,0.9808631706077,0.9808631706077),
(0.9808631706077,0.9808631706077,0.9808631706077,0.9808631706077,0.9808631706077,
0.9808631706077,0.9808631706077,0.9808631706077,0.9808631706077),(1.057410488177,
1.057410488177,1.057410488177,1.057410488177,1.057410488177,1.057410488177,
1.057410488177,1.057410488177,1.057410488177)))
REPRESENTATION_ITEM('')
SURFACE()
);
#2430=(
BOUNDED_SURFACE()
B_SPLINE_SURFACE(3,3,((#120879,#120880,#120881,#120882,#120883,#120884,
#120885,#120886,#120887,#120888),(#120889,#120890,#120891,#120892,#120893,
#120894,#120895,#120896,#120897,#120898),(#120899,#120900,#120901,#120902,
#120903,#120904,#120905,#120906,#120907,#120908),(#120909,#120910,#120911,
#120912,#120913,#120914,#120915,#120916,#120917,#120918),(#120919,#120920,
#120921,#120922,#120923,#120924,#120925,#120926,#120927,#120928),(#120929,
#120930,#120931,#120932,#120933,#120934,#120935,#120936,#120937,#120938),
(#120939,#120940,#120941,#120942,#120943,#120944,#120945,#120946,#120947,
#120948)),.UNSPECIFIED.,.F.,.F.,.F.)
B_SPLINE_SURFACE_WITH_KNOTS((4,3,4),(4,1,1,1,1,1,1,4),(0.,0.5,1.),(0.,0.161025004538591,
0.369602103221435,0.554126466977726,0.718053106645468,0.864942898489644,
0.996691241096418,1.),.UNSPECIFIED.)
GEOMETRIC_REPRESENTATION_ITEM()
RATIONAL_B_SPLINE_SURFACE(((1.201213809876,1.201213809876,1.201213809876,
1.201213809876,1.201213809876,1.201213809876,1.201213809876,1.201213809876,
1.201213809876,1.201213809876),(0.9329287300413,0.9329287300413,0.9329287300413,
0.9329287300413,0.9329287300413,0.9329287300413,0.9329287300413,0.9329287300413,
0.9329287300413,0.9329287300413),(0.9329287300413,0.9329287300413,0.9329287300413,
0.9329287300413,0.9329287300413,0.9329287300413,0.9329287300413,0.9329287300413,
0.9329287300413,0.9329287300413),(1.201213809876,1.201213809876,1.201213809876,
1.201213809876,1.201213809876,1.201213809876,1.201213809876,1.201213809876,
1.201213809876,1.201213809876),(0.9329287300413,0.9329287300413,0.9329287300413,
0.9329287300413,0.9329287300413,0.9329287300413,0.9329287300413,0.9329287300413,
0.9329287300413,0.9329287300413),(0.9329287300413,0.9329287300413,0.9329287300413,
0.9329287300413,0.9329287300413,0.9329287300413,0.9329287300413,0.9329287300413,
0.9329287300413,0.9329287300413),(1.201213809876,1.201213809876,1.201213809876,
1.201213809876,1.201213809876,1.201213809876,1.201213809876,1.201213809876,
1.201213809876,1.201213809876)))
REPRESENTATION_ITEM('')
SURFACE()
);
#2431=(
BOUNDED_SURFACE()
B_SPLINE_SURFACE(3,3,((#121035,#121036,#121037,#121038,#121039,#121040,
#121041,#121042,#121043,#121044),(#121045,#121046,#121047,#121048,#121049,
#121050,#121051,#121052,#121053,#121054),(#121055,#121056,#121057,#121058,
#121059,#121060,#121061,#121062,#121063,#121064),(#121065,#121066,#121067,
#121068,#121069,#121070,#121071,#121072,#121073,#121074),(#121075,#121076,
#121077,#121078,#121079,#121080,#121081,#121082,#121083,#121084),(#121085,
#121086,#121087,#121088,#121089,#121090,#121091,#121092,#121093,#121094),
(#121095,#121096,#121097,#121098,#121099,#121100,#121101,#121102,#121103,
#121104)),.UNSPECIFIED.,.F.,.F.,.F.)
B_SPLINE_SURFACE_WITH_KNOTS((4,3,4),(4,1,1,1,1,1,1,4),(0.,0.5,1.),(0.,0.00259132042105358,
0.133683284416713,0.278707201971115,0.438527579442401,0.616079075546092,
0.815708952652196,1.),.UNSPECIFIED.)
GEOMETRIC_REPRESENTATION_ITEM()
RATIONAL_B_SPLINE_SURFACE(((1.201171733823,1.201171733823,1.201171733823,
1.201171733823,1.201171733823,1.201171733823,1.201171733823,1.201171733823,
1.201171733823,1.201171733823),(0.9329427553922,0.9329427553922,0.9329427553922,
0.9329427553922,0.9329427553922,0.9329427553922,0.9329427553922,0.9329427553922,
0.9329427553922,0.9329427553922),(0.9329427553922,0.9329427553922,0.9329427553922,
0.9329427553922,0.9329427553922,0.9329427553922,0.9329427553922,0.9329427553922,
0.9329427553922,0.9329427553922),(1.201171733823,1.201171733823,1.201171733823,
1.201171733823,1.201171733823,1.201171733823,1.201171733823,1.201171733823,
1.201171733823,1.201171733823),(0.9329427553922,0.9329427553922,0.9329427553922,
0.9329427553922,0.9329427553922,0.9329427553922,0.9329427553922,0.9329427553922,
0.9329427553922,0.9329427553922),(0.9329427553922,0.9329427553922,0.9329427553922,
0.9329427553922,0.9329427553922,0.9329427553922,0.9329427553922,0.9329427553922,
0.9329427553922,0.9329427553922),(1.201171733823,1.201171733823,1.201171733823,
1.201171733823,1.201171733823,1.201171733823,1.201171733823,1.201171733823,
1.201171733823,1.201171733823)))
REPRESENTATION_ITEM('')
SURFACE()
);
#2432=(
BOUNDED_SURFACE()
B_SPLINE_SURFACE(3,3,((#121106,#121107,#121108,#121109,#121110,#121111,
#121112,#121113,#121114,#121115,#121116,#121117),(#121118,#121119,#121120,
#121121,#121122,#121123,#121124,#121125,#121126,#121127,#121128,#121129),
(#121130,#121131,#121132,#121133,#121134,#121135,#121136,#121137,#121138,
#121139,#121140,#121141),(#121142,#121143,#121144,#121145,#121146,#121147,
#121148,#121149,#121150,#121151,#121152,#121153),(#121154,#121155,#121156,
#121157,#121158,#121159,#121160,#121161,#121162,#121163,#121164,#121165),
(#121166,#121167,#121168,#121169,#121170,#121171,#121172,#121173,#121174,
#121175,#121176,#121177),(#121178,#121179,#121180,#121181,#121182,#121183,
#121184,#121185,#121186,#121187,#121188,#121189)),.UNSPECIFIED.,.F.,.F.,
 .F.)
B_SPLINE_SURFACE_WITH_KNOTS((4,3,4),(4,1,1,1,1,1,1,1,1,4),(0.,0.5,1.),(0.,
0.000255491591619197,0.127239783683594,0.253487500080297,0.379079641346161,
0.504106145120676,0.628664885620248,0.752853160032759,0.87675838090237,
1.),.UNSPECIFIED.)
GEOMETRIC_REPRESENTATION_ITEM()
RATIONAL_B_SPLINE_SURFACE(((1.193844362293,1.193844362293,1.193844362293,
1.193844362293,1.193844362293,1.193844362293,1.193844362293,1.193844362293,
1.193844362293,1.193844362293,1.193844362293,1.193844362293),(0.9353852125691,
0.9353852125691,0.9353852125691,0.9353852125691,0.9353852125691,0.9353852125691,
0.9353852125691,0.9353852125691,0.9353852125691,0.9353852125691,0.9353852125691,
0.9353852125691),(0.9353852125691,0.9353852125691,0.9353852125691,0.9353852125691,
0.9353852125691,0.9353852125691,0.9353852125691,0.9353852125691,0.9353852125691,
0.9353852125691,0.9353852125691,0.9353852125691),(1.193844362293,1.193844362293,
1.193844362293,1.193844362293,1.193844362293,1.193844362293,1.193844362293,
1.193844362293,1.193844362293,1.193844362293,1.193844362293,1.193844362293),
(0.9353852125691,0.9353852125691,0.9353852125691,0.9353852125691,0.9353852125691,
0.9353852125691,0.9353852125691,0.9353852125691,0.9353852125691,0.9353852125691,
0.9353852125691,0.9353852125691),(0.9353852125691,0.9353852125691,0.9353852125691,
0.9353852125691,0.9353852125691,0.9353852125691,0.9353852125691,0.9353852125691,
0.9353852125691,0.9353852125691,0.9353852125691,0.9353852125691),(1.193844362293,
1.193844362293,1.193844362293,1.193844362293,1.193844362293,1.193844362293,
1.193844362293,1.193844362293,1.193844362293,1.193844362293,1.193844362293,
1.193844362293)))
REPRESENTATION_ITEM('')
SURFACE()
);
#2433=(
BOUNDED_SURFACE()
B_SPLINE_SURFACE(3,3,((#121191,#121192,#121193,#121194,#121195,#121196,
#121197,#121198,#121199,#121200,#121201,#121202,#121203,#121204,#121205,
#121206,#121207,#121208,#121209,#121210,#121211,#121212,#121213,#121214,
#121215,#121216,#121217,#121218,#121219,#121220,#121221,#121222,#121223,
#121224),(#121225,#121226,#121227,#121228,#121229,#121230,#121231,#121232,
#121233,#121234,#121235,#121236,#121237,#121238,#121239,#121240,#121241,
#121242,#121243,#121244,#121245,#121246,#121247,#121248,#121249,#121250,
#121251,#121252,#121253,#121254,#121255,#121256,#121257,#121258),(#121259,
#121260,#121261,#121262,#121263,#121264,#121265,#121266,#121267,#121268,
#121269,#121270,#121271,#121272,#121273,#121274,#121275,#121276,#121277,
#121278,#121279,#121280,#121281,#121282,#121283,#121284,#121285,#121286,
#121287,#121288,#121289,#121290,#121291,#121292),(#121293,#121294,#121295,
#121296,#121297,#121298,#121299,#121300,#121301,#121302,#121303,#121304,
#121305,#121306,#121307,#121308,#121309,#121310,#121311,#121312,#121313,
#121314,#121315,#121316,#121317,#121318,#121319,#121320,#121321,#121322,
#121323,#121324,#121325,#121326),(#121327,#121328,#121329,#121330,#121331,
#121332,#121333,#121334,#121335,#121336,#121337,#121338,#121339,#121340,
#121341,#121342,#121343,#121344,#121345,#121346,#121347,#121348,#121349,
#121350,#121351,#121352,#121353,#121354,#121355,#121356,#121357,#121358,
#121359,#121360),(#121361,#121362,#121363,#121364,#121365,#121366,#121367,
#121368,#121369,#121370,#121371,#121372,#121373,#121374,#121375,#121376,
#121377,#121378,#121379,#121380,#121381,#121382,#121383,#121384,#121385,
#121386,#121387,#121388,#121389,#121390,#121391,#121392,#121393,#121394),
(#121395,#121396,#121397,#121398,#121399,#121400,#121401,#121402,#121403,
#121404,#121405,#121406,#121407,#121408,#121409,#121410,#121411,#121412,
#121413,#121414,#121415,#121416,#121417,#121418,#121419,#121420,#121421,
#121422,#121423,#121424,#121425,#121426,#121427,#121428)),.UNSPECIFIED.,
 .F.,.F.,.F.)
B_SPLINE_SURFACE_WITH_KNOTS((4,3,4),(4,1,1,1,1,1,1,1,1,1,1,1,1,1,1,1,1,
1,1,1,1,1,1,1,1,1,1,1,1,1,1,4),(0.,0.5,1.),(0.,0.00390411019570353,0.0280798877427953,
0.0549594760925253,0.084482057830751,0.116603170427511,0.15129817037668,
0.188488834966683,0.227507129809145,0.267411106706363,0.307272885523456,
0.346360547263377,0.385850664440005,0.42467066457681,0.461154766662463,
0.495850904898193,0.529827873260416,0.564306064772395,0.600347337077154,
0.637306063447508,0.674154674464573,0.71211198969174,0.750908172946504,
0.789490910831634,0.826793915174607,0.861784930834985,0.894042278866944,
0.923582402081779,0.950408852900018,0.974512143542049,0.995871943984923,
1.),.UNSPECIFIED.)
GEOMETRIC_REPRESENTATION_ITEM()
RATIONAL_B_SPLINE_SURFACE(((1.182964165402,1.182964165402,1.182964165402,
1.182964165402,1.182964165402,1.182964165402,1.182964165402,1.182964165402,
1.182964165402,1.182964165402,1.182964165402,1.182964165402,1.182964165402,
1.182964165402,1.182964165402,1.182964165402,1.182964165402,1.182964165402,
1.182964165402,1.182964165402,1.182964165402,1.182964165402,1.182964165402,
1.182964165402,1.182964165402,1.182964165402,1.182964165402,1.182964165402,
1.182964165402,1.182964165402,1.182964165402,1.182964165402,1.182964165402,
1.182964165402),(0.9390119448661,0.9390119448661,0.9390119448661,0.9390119448661,
0.9390119448661,0.9390119448661,0.9390119448661,0.9390119448661,0.9390119448661,
0.9390119448661,0.9390119448661,0.9390119448661,0.9390119448661,0.9390119448661,
0.9390119448661,0.9390119448661,0.9390119448661,0.9390119448661,0.9390119448661,
0.9390119448661,0.9390119448661,0.9390119448661,0.9390119448661,0.9390119448661,
0.9390119448661,0.9390119448661,0.9390119448661,0.9390119448661,0.9390119448661,
0.9390119448661,0.9390119448661,0.9390119448661,0.9390119448661,0.9390119448661),
(0.9390119448661,0.9390119448661,0.9390119448661,0.9390119448661,0.9390119448661,
0.9390119448661,0.9390119448661,0.9390119448661,0.9390119448661,0.9390119448661,
0.9390119448661,0.9390119448661,0.9390119448661,0.9390119448661,0.9390119448661,
0.9390119448661,0.9390119448661,0.9390119448661,0.9390119448661,0.9390119448661,
0.9390119448661,0.9390119448661,0.9390119448661,0.9390119448661,0.9390119448661,
0.9390119448661,0.9390119448661,0.9390119448661,0.9390119448661,0.9390119448661,
0.9390119448661,0.9390119448661,0.9390119448661,0.9390119448661),(1.182964165402,
1.182964165402,1.182964165402,1.182964165402,1.182964165402,1.182964165402,
1.182964165402,1.182964165402,1.182964165402,1.182964165402,1.182964165402,
1.182964165402,1.182964165402,1.182964165402,1.182964165402,1.182964165402,
1.182964165402,1.182964165402,1.182964165402,1.182964165402,1.182964165402,
1.182964165402,1.182964165402,1.182964165402,1.182964165402,1.182964165402,
1.182964165402,1.182964165402,1.182964165402,1.182964165402,1.182964165402,
1.182964165402,1.182964165402,1.182964165402),(0.9390119448661,0.9390119448661,
0.9390119448661,0.9390119448661,0.9390119448661,0.9390119448661,0.9390119448661,
0.9390119448661,0.9390119448661,0.9390119448661,0.9390119448661,0.9390119448661,
0.9390119448661,0.9390119448661,0.9390119448661,0.9390119448661,0.9390119448661,
0.9390119448661,0.9390119448661,0.9390119448661,0.9390119448661,0.9390119448661,
0.9390119448661,0.9390119448661,0.9390119448661,0.9390119448661,0.9390119448661,
0.9390119448661,0.9390119448661,0.9390119448661,0.9390119448661,0.9390119448661,
0.9390119448661,0.9390119448661),(0.9390119448661,0.9390119448661,0.9390119448661,
0.9390119448661,0.9390119448661,0.9390119448661,0.9390119448661,0.9390119448661,
0.9390119448661,0.9390119448661,0.9390119448661,0.9390119448661,0.9390119448661,
0.9390119448661,0.9390119448661,0.9390119448661,0.9390119448661,0.9390119448661,
0.9390119448661,0.9390119448661,0.9390119448661,0.9390119448661,0.9390119448661,
0.9390119448661,0.9390119448661,0.9390119448661,0.9390119448661,0.9390119448661,
0.9390119448661,0.9390119448661,0.9390119448661,0.9390119448661,0.9390119448661,
0.9390119448661),(1.182964165402,1.182964165402,1.182964165402,1.182964165402,
1.182964165402,1.182964165402,1.182964165402,1.182964165402,1.182964165402,
1.182964165402,1.182964165402,1.182964165402,1.182964165402,1.182964165402,
1.182964165402,1.182964165402,1.182964165402,1.182964165402,1.182964165402,
1.182964165402,1.182964165402,1.182964165402,1.182964165402,1.182964165402,
1.182964165402,1.182964165402,1.182964165402,1.182964165402,1.182964165402,
1.182964165402,1.182964165402,1.182964165402,1.182964165402,1.182964165402)))
REPRESENTATION_ITEM('')
SURFACE()
);
#2434=(
BOUNDED_SURFACE()
B_SPLINE_SURFACE(3,3,((#121430,#121431,#121432,#121433,#121434,#121435,
#121436,#121437,#121438,#121439,#121440,#121441),(#121442,#121443,#121444,
#121445,#121446,#121447,#121448,#121449,#121450,#121451,#121452,#121453),
(#121454,#121455,#121456,#121457,#121458,#121459,#121460,#121461,#121462,
#121463,#121464,#121465),(#121466,#121467,#121468,#121469,#121470,#121471,
#121472,#121473,#121474,#121475,#121476,#121477),(#121478,#121479,#121480,
#121481,#121482,#121483,#121484,#121485,#121486,#121487,#121488,#121489),
(#121490,#121491,#121492,#121493,#121494,#121495,#121496,#121497,#121498,
#121499,#121500,#121501),(#121502,#121503,#121504,#121505,#121506,#121507,
#121508,#121509,#121510,#121511,#121512,#121513)),.UNSPECIFIED.,.F.,.F.,
 .F.)
B_SPLINE_SURFACE_WITH_KNOTS((4,3,4),(4,1,1,1,1,1,1,1,1,4),(0.,0.5,1.),(0.,
0.121577744739987,0.2454785297075,0.369661120308666,0.494217098932518,0.61923924716235,
0.744819531284461,0.871051615748787,0.998028327089304,1.),.UNSPECIFIED.)
GEOMETRIC_REPRESENTATION_ITEM()
RATIONAL_B_SPLINE_SURFACE(((1.193843399739,1.193843399739,1.193843399739,
1.193843399739,1.193843399739,1.193843399739,1.193843399739,1.193843399739,
1.193843399739,1.193843399739,1.193843399739,1.193843399739),(0.9353855334202,
0.9353855334202,0.9353855334202,0.9353855334202,0.9353855334202,0.9353855334202,
0.9353855334202,0.9353855334202,0.9353855334202,0.9353855334202,0.9353855334202,
0.9353855334202),(0.9353855334202,0.9353855334202,0.9353855334202,0.9353855334202,
0.9353855334202,0.9353855334202,0.9353855334202,0.9353855334202,0.9353855334202,
0.9353855334202,0.9353855334202,0.9353855334202),(1.193843399739,1.193843399739,
1.193843399739,1.193843399739,1.193843399739,1.193843399739,1.193843399739,
1.193843399739,1.193843399739,1.193843399739,1.193843399739,1.193843399739),
(0.9353855334202,0.9353855334202,0.9353855334202,0.9353855334202,0.9353855334202,
0.9353855334202,0.9353855334202,0.9353855334202,0.9353855334202,0.9353855334202,
0.9353855334202,0.9353855334202),(0.9353855334202,0.9353855334202,0.9353855334202,
0.9353855334202,0.9353855334202,0.9353855334202,0.9353855334202,0.9353855334202,
0.9353855334202,0.9353855334202,0.9353855334202,0.9353855334202),(1.193843399739,
1.193843399739,1.193843399739,1.193843399739,1.193843399739,1.193843399739,
1.193843399739,1.193843399739,1.193843399739,1.193843399739,1.193843399739,
1.193843399739)))
REPRESENTATION_ITEM('')
SURFACE()
);
#2435=(
BOUNDED_SURFACE()
B_SPLINE_SURFACE(3,3,((#121515,#121516,#121517,#121518,#121519,#121520,
#121521,#121522,#121523,#121524),(#121525,#121526,#121527,#121528,#121529,
#121530,#121531,#121532,#121533,#121534),(#121535,#121536,#121537,#121538,
#121539,#121540,#121541,#121542,#121543,#121544),(#121545,#121546,#121547,
#121548,#121549,#121550,#121551,#121552,#121553,#121554),(#121555,#121556,
#121557,#121558,#121559,#121560,#121561,#121562,#121563,#121564),(#121565,
#121566,#121567,#121568,#121569,#121570,#121571,#121572,#121573,#121574),
(#121575,#121576,#121577,#121578,#121579,#121580,#121581,#121582,#121583,
#121584)),.UNSPECIFIED.,.F.,.F.,.F.)
B_SPLINE_SURFACE_WITH_KNOTS((4,3,4),(4,1,1,1,1,1,1,4),(0.,0.5,1.),(0.,0.213585163989469,
0.405450323624376,0.577282704132798,0.731642183256355,0.871392511498999,
0.997433055266827,1.),.UNSPECIFIED.)
GEOMETRIC_REPRESENTATION_ITEM()
RATIONAL_B_SPLINE_SURFACE(((1.201113977633,1.201113977633,1.201113977633,
1.201113977633,1.201113977633,1.201113977633,1.201113977633,1.201113977633,
1.201113977633,1.201113977633),(0.9329620074556,0.9329620074556,0.9329620074556,
0.9329620074556,0.9329620074556,0.9329620074556,0.9329620074556,0.9329620074556,
0.9329620074556,0.9329620074556),(0.9329620074556,0.9329620074556,0.9329620074556,
0.9329620074556,0.9329620074556,0.9329620074556,0.9329620074556,0.9329620074556,
0.9329620074556,0.9329620074556),(1.201113977633,1.201113977633,1.201113977633,
1.201113977633,1.201113977633,1.201113977633,1.201113977633,1.201113977633,
1.201113977633,1.201113977633),(0.9329620074556,0.9329620074556,0.9329620074556,
0.9329620074556,0.9329620074556,0.9329620074556,0.9329620074556,0.9329620074556,
0.9329620074556,0.9329620074556),(0.9329620074556,0.9329620074556,0.9329620074556,
0.9329620074556,0.9329620074556,0.9329620074556,0.9329620074556,0.9329620074556,
0.9329620074556,0.9329620074556),(1.201113977633,1.201113977633,1.201113977633,
1.201113977633,1.201113977633,1.201113977633,1.201113977633,1.201113977633,
1.201113977633,1.201113977633)))
REPRESENTATION_ITEM('')
SURFACE()
);
#2436=(
BOUNDED_SURFACE()
B_SPLINE_SURFACE(3,3,((#121603,#121604,#121605,#121606,#121607,#121608,
#121609,#121610,#121611,#121612,#121613),(#121614,#121615,#121616,#121617,
#121618,#121619,#121620,#121621,#121622,#121623,#121624),(#121625,#121626,
#121627,#121628,#121629,#121630,#121631,#121632,#121633,#121634,#121635),
(#121636,#121637,#121638,#121639,#121640,#121641,#121642,#121643,#121644,
#121645,#121646),(#121647,#121648,#121649,#121650,#121651,#121652,#121653,
#121654,#121655,#121656,#121657),(#121658,#121659,#121660,#121661,#121662,
#121663,#121664,#121665,#121666,#121667,#121668),(#121669,#121670,#121671,
#121672,#121673,#121674,#121675,#121676,#121677,#121678,#121679)),
 .UNSPECIFIED.,.F.,.F.,.F.)
B_SPLINE_SURFACE_WITH_KNOTS((4,3,4),(4,1,1,1,1,1,1,1,4),(0.,0.5,1.),(0.,
0.00181797331928698,0.105490767602339,0.219958045817536,0.345909152683817,
0.484805134723122,0.638614040911334,0.809850477822227,1.),.UNSPECIFIED.)
GEOMETRIC_REPRESENTATION_ITEM()
RATIONAL_B_SPLINE_SURFACE(((1.201132896331,1.201132896331,1.201132896331,
1.201132896331,1.201132896331,1.201132896331,1.201132896331,1.201132896331,
1.201132896331,1.201132896331,1.201132896331),(0.932955701223,0.932955701223,
0.932955701223,0.932955701223,0.932955701223,0.932955701223,0.932955701223,
0.932955701223,0.932955701223,0.932955701223,0.932955701223),(0.932955701223,
0.932955701223,0.932955701223,0.932955701223,0.932955701223,0.932955701223,
0.932955701223,0.932955701223,0.932955701223,0.932955701223,0.932955701223),
(1.201132896331,1.201132896331,1.201132896331,1.201132896331,1.201132896331,
1.201132896331,1.201132896331,1.201132896331,1.201132896331,1.201132896331,
1.201132896331),(0.932955701223,0.932955701223,0.932955701223,0.932955701223,
0.932955701223,0.932955701223,0.932955701223,0.932955701223,0.932955701223,
0.932955701223,0.932955701223),(0.932955701223,0.932955701223,0.932955701223,
0.932955701223,0.932955701223,0.932955701223,0.932955701223,0.932955701223,
0.932955701223,0.932955701223,0.932955701223),(1.201132896331,1.201132896331,
1.201132896331,1.201132896331,1.201132896331,1.201132896331,1.201132896331,
1.201132896331,1.201132896331,1.201132896331,1.201132896331)))
REPRESENTATION_ITEM('')
SURFACE()
);
#2437=(
BOUNDED_SURFACE()
B_SPLINE_SURFACE(3,3,((#121681,#121682,#121683,#121684,#121685,#121686,
#121687,#121688,#121689),(#121690,#121691,#121692,#121693,#121694,#121695,
#121696,#121697,#121698),(#121699,#121700,#121701,#121702,#121703,#121704,
#121705,#121706,#121707),(#121708,#121709,#121710,#121711,#121712,#121713,
#121714,#121715,#121716),(#121717,#121718,#121719,#121720,#121721,#121722,
#121723,#121724,#121725),(#121726,#121727,#121728,#121729,#121730,#121731,
#121732,#121733,#121734),(#121735,#121736,#121737,#121738,#121739,#121740,
#121741,#121742,#121743)),.UNSPECIFIED.,.F.,.F.,.F.)
B_SPLINE_SURFACE_WITH_KNOTS((4,3,4),(4,1,1,1,1,1,4),(0.,0.5,1.),(0.,0.146812258466779,
0.312562551467087,0.499888765632735,0.688675725217384,0.852980904228354,
1.),.UNSPECIFIED.)
GEOMETRIC_REPRESENTATION_ITEM()
RATIONAL_B_SPLINE_SURFACE(((1.193840868885,1.193840868885,1.193840868885,
1.193840868885,1.193840868885,1.193840868885,1.193840868885,1.193840868885,
1.193840868885),(0.9353863770384,0.9353863770384,0.9353863770384,0.9353863770384,
0.9353863770384,0.9353863770384,0.9353863770384,0.9353863770384,0.9353863770384),
(0.9353863770384,0.9353863770384,0.9353863770384,0.9353863770384,0.9353863770384,
0.9353863770384,0.9353863770384,0.9353863770384,0.9353863770384),(1.193840868885,
1.193840868885,1.193840868885,1.193840868885,1.193840868885,1.193840868885,
1.193840868885,1.193840868885,1.193840868885),(0.9353863770384,0.9353863770384,
0.9353863770384,0.9353863770384,0.9353863770384,0.9353863770384,0.9353863770384,
0.9353863770384,0.9353863770384),(0.9353863770384,0.9353863770384,0.9353863770384,
0.9353863770384,0.9353863770384,0.9353863770384,0.9353863770384,0.9353863770384,
0.9353863770384),(1.193840868885,1.193840868885,1.193840868885,1.193840868885,
1.193840868885,1.193840868885,1.193840868885,1.193840868885,1.193840868885)))
REPRESENTATION_ITEM('')
SURFACE()
);
#2438=(
BOUNDED_SURFACE()
B_SPLINE_SURFACE(3,3,((#121820,#121821,#121822,#121823,#121824,#121825,
#121826,#121827,#121828,#121829,#121830,#121831),(#121832,#121833,#121834,
#121835,#121836,#121837,#121838,#121839,#121840,#121841,#121842,#121843),
(#121844,#121845,#121846,#121847,#121848,#121849,#121850,#121851,#121852,
#121853,#121854,#121855),(#121856,#121857,#121858,#121859,#121860,#121861,
#121862,#121863,#121864,#121865,#121866,#121867),(#121868,#121869,#121870,
#121871,#121872,#121873,#121874,#121875,#121876,#121877,#121878,#121879),
(#121880,#121881,#121882,#121883,#121884,#121885,#121886,#121887,#121888,
#121889,#121890,#121891),(#121892,#121893,#121894,#121895,#121896,#121897,
#121898,#121899,#121900,#121901,#121902,#121903)),.UNSPECIFIED.,.F.,.F.,
 .F.)
B_SPLINE_SURFACE_WITH_KNOTS((4,3,4),(4,1,1,1,1,1,1,1,1,4),(0.,0.5,1.),(0.,
0.1150816828504,0.247731000070067,0.394496984674143,0.542441014806786,0.677432974789258,
0.797298327727755,0.903511214341264,0.999875262137635,1.),.UNSPECIFIED.)
GEOMETRIC_REPRESENTATION_ITEM()
RATIONAL_B_SPLINE_SURFACE(((1.193841606841,1.193841606841,1.193841606841,
1.193841606841,1.193841606841,1.193841606841,1.193841606841,1.193841606841,
1.193841606841,1.193841606841,1.193841606841,1.193841606841),(0.9353861310531,
0.9353861310531,0.9353861310531,0.9353861310531,0.9353861310531,0.9353861310531,
0.9353861310531,0.9353861310531,0.9353861310531,0.9353861310531,0.9353861310531,
0.9353861310531),(0.9353861310531,0.9353861310531,0.9353861310531,0.9353861310531,
0.9353861310531,0.9353861310531,0.9353861310531,0.9353861310531,0.9353861310531,
0.9353861310531,0.9353861310531,0.9353861310531),(1.193841606841,1.193841606841,
1.193841606841,1.193841606841,1.193841606841,1.193841606841,1.193841606841,
1.193841606841,1.193841606841,1.193841606841,1.193841606841,1.193841606841),
(0.9353861310531,0.9353861310531,0.9353861310531,0.9353861310531,0.9353861310531,
0.9353861310531,0.9353861310531,0.9353861310531,0.9353861310531,0.9353861310531,
0.9353861310531,0.9353861310531),(0.9353861310531,0.9353861310531,0.9353861310531,
0.9353861310531,0.9353861310531,0.9353861310531,0.9353861310531,0.9353861310531,
0.9353861310531,0.9353861310531,0.9353861310531,0.9353861310531),(1.193841606841,
1.193841606841,1.193841606841,1.193841606841,1.193841606841,1.193841606841,
1.193841606841,1.193841606841,1.193841606841,1.193841606841,1.193841606841,
1.193841606841)))
REPRESENTATION_ITEM('')
SURFACE()
);
#2439=(
BOUNDED_SURFACE()
B_SPLINE_SURFACE(3,3,((#123619,#123620,#123621,#123622,#123623,#123624,
#123625,#123626),(#123627,#123628,#123629,#123630,#123631,#123632,#123633,
#123634),(#123635,#123636,#123637,#123638,#123639,#123640,#123641,#123642),
(#123643,#123644,#123645,#123646,#123647,#123648,#123649,#123650)),
 .UNSPECIFIED.,.F.,.F.,.F.)
B_SPLINE_SURFACE_WITH_KNOTS((4,4),(4,1,1,1,1,4),(0.,1.),(0.,0.0246171264152833,
0.291238908164661,0.592562353394222,0.933298045148062,1.),.UNSPECIFIED.)
GEOMETRIC_REPRESENTATION_ITEM()
RATIONAL_B_SPLINE_SURFACE(((1.155702096291,1.155702096291,1.155702096291,
1.155702096291,1.155702096291,1.155702096291,1.155702096291,1.155702096291),
(0.9480993012362,0.9480993012362,0.9480993012362,0.9480993012362,0.9480993012362,
0.9480993012362,0.9480993012362,0.9480993012362),(0.9480993012362,0.9480993012362,
0.9480993012362,0.9480993012362,0.9480993012362,0.9480993012362,0.9480993012362,
0.9480993012362),(1.155702096291,1.155702096291,1.155702096291,1.155702096291,
1.155702096291,1.155702096291,1.155702096291,1.155702096291)))
REPRESENTATION_ITEM('')
SURFACE()
);
#2440=(
BOUNDED_SURFACE()
B_SPLINE_SURFACE(3,3,((#123749,#123750,#123751,#123752,#123753,#123754,
#123755,#123756,#123757,#123758,#123759,#123760,#123761,#123762,#123763),
(#123764,#123765,#123766,#123767,#123768,#123769,#123770,#123771,#123772,
#123773,#123774,#123775,#123776,#123777,#123778),(#123779,#123780,#123781,
#123782,#123783,#123784,#123785,#123786,#123787,#123788,#123789,#123790,
#123791,#123792,#123793),(#123794,#123795,#123796,#123797,#123798,#123799,
#123800,#123801,#123802,#123803,#123804,#123805,#123806,#123807,#123808)),
 .UNSPECIFIED.,.F.,.F.,.F.)
B_SPLINE_SURFACE_WITH_KNOTS((4,4),(4,1,1,1,1,1,1,1,1,1,1,1,4),(0.,1.),(0.,
0.0727177819492164,0.16359452595188,0.250961907386609,0.334788546033315,
0.415442620198573,0.49511203377138,0.575859115958059,0.655273963838798,
0.731996243944222,0.814480068027282,0.906324996644106,1.),.UNSPECIFIED.)
GEOMETRIC_REPRESENTATION_ITEM()
RATIONAL_B_SPLINE_SURFACE(((1.519033843966,1.519033843966,1.519033843966,
1.519033843966,1.519033843966,1.519033843966,1.519033843966,1.519033843966,
1.519033843966,1.519033843966,1.519033843966,1.519033843966,1.519033843966,
1.519033843966,1.519033843966),(0.8269887186781,0.8269887186781,0.8269887186781,
0.8269887186781,0.8269887186781,0.8269887186781,0.8269887186781,0.8269887186781,
0.8269887186781,0.8269887186781,0.8269887186781,0.8269887186781,0.8269887186781,
0.8269887186781,0.8269887186781),(0.8269887186781,0.8269887186781,0.8269887186781,
0.8269887186781,0.8269887186781,0.8269887186781,0.8269887186781,0.8269887186781,
0.8269887186781,0.8269887186781,0.8269887186781,0.8269887186781,0.8269887186781,
0.8269887186781,0.8269887186781),(1.519033843966,1.519033843966,1.519033843966,
1.519033843966,1.519033843966,1.519033843966,1.519033843966,1.519033843966,
1.519033843966,1.519033843966,1.519033843966,1.519033843966,1.519033843966,
1.519033843966,1.519033843966)))
REPRESENTATION_ITEM('')
SURFACE()
);
#2441=(
BOUNDED_SURFACE()
B_SPLINE_SURFACE(3,3,((#124103,#124104,#124105,#124106,#124107,#124108,
#124109,#124110,#124111,#124112),(#124113,#124114,#124115,#124116,#124117,
#124118,#124119,#124120,#124121,#124122),(#124123,#124124,#124125,#124126,
#124127,#124128,#124129,#124130,#124131,#124132),(#124133,#124134,#124135,
#124136,#124137,#124138,#124139,#124140,#124141,#124142)),.UNSPECIFIED.,
 .F.,.F.,.F.)
B_SPLINE_SURFACE_WITH_KNOTS((4,4),(4,1,1,1,1,1,1,4),(0.,1.),(0.,0.0442218692304281,
0.265842058411036,0.466113430548006,0.645383516910958,0.805695668205441,
0.948933238513881,1.),.UNSPECIFIED.)
GEOMETRIC_REPRESENTATION_ITEM()
RATIONAL_B_SPLINE_SURFACE(((1.365422972509,1.365422972509,1.365422972509,
1.365422972509,1.365422972509,1.365422972509,1.365422972509,1.365422972509,
1.365422972509,1.365422972509),(0.878192342497,0.878192342497,0.878192342497,
0.878192342497,0.878192342497,0.878192342497,0.878192342497,0.878192342497,
0.878192342497,0.878192342497),(0.878192342497,0.878192342497,0.878192342497,
0.878192342497,0.878192342497,0.878192342497,0.878192342497,0.878192342497,
0.878192342497,0.878192342497),(1.365422972509,1.365422972509,1.365422972509,
1.365422972509,1.365422972509,1.365422972509,1.365422972509,1.365422972509,
1.365422972509,1.365422972509)))
REPRESENTATION_ITEM('')
SURFACE()
);
#2442=(
BOUNDED_SURFACE()
B_SPLINE_SURFACE(3,3,((#124201,#124202,#124203,#124204,#124205,#124206,
#124207,#124208,#124209,#124210,#124211,#124212,#124213,#124214,#124215),
(#124216,#124217,#124218,#124219,#124220,#124221,#124222,#124223,#124224,
#124225,#124226,#124227,#124228,#124229,#124230),(#124231,#124232,#124233,
#124234,#124235,#124236,#124237,#124238,#124239,#124240,#124241,#124242,
#124243,#124244,#124245),(#124246,#124247,#124248,#124249,#124250,#124251,
#124252,#124253,#124254,#124255,#124256,#124257,#124258,#124259,#124260)),
 .UNSPECIFIED.,.F.,.F.,.F.)
B_SPLINE_SURFACE_WITH_KNOTS((4,4),(4,1,1,1,1,1,1,1,1,1,1,1,4),(0.,1.),(0.,
0.0084168370653201,0.153296921706747,0.285251477789455,0.405485980176222,
0.5143437021125,0.612495974405379,0.700795271015088,0.780077840916837,0.851172072538887,
0.914904276103888,0.972101275929351,1.),.UNSPECIFIED.)
GEOMETRIC_REPRESENTATION_ITEM()
RATIONAL_B_SPLINE_SURFACE(((1.250208738268,1.250208738268,1.250208738268,
1.250208738268,1.250208738268,1.250208738268,1.250208738268,1.250208738268,
1.250208738268,1.250208738268,1.250208738268,1.250208738268,1.250208738268,
1.250208738268,1.250208738268),(0.916597087244,0.916597087244,0.916597087244,
0.916597087244,0.916597087244,0.916597087244,0.916597087244,0.916597087244,
0.916597087244,0.916597087244,0.916597087244,0.916597087244,0.916597087244,
0.916597087244,0.916597087244),(0.916597087244,0.916597087244,0.916597087244,
0.916597087244,0.916597087244,0.916597087244,0.916597087244,0.916597087244,
0.916597087244,0.916597087244,0.916597087244,0.916597087244,0.916597087244,
0.916597087244,0.916597087244),(1.250208738268,1.250208738268,1.250208738268,
1.250208738268,1.250208738268,1.250208738268,1.250208738268,1.250208738268,
1.250208738268,1.250208738268,1.250208738268,1.250208738268,1.250208738268,
1.250208738268,1.250208738268)))
REPRESENTATION_ITEM('')
SURFACE()
);
#2443=(
BOUNDED_SURFACE()
B_SPLINE_SURFACE(3,3,((#124437,#124438,#124439,#124440,#124441,#124442),
(#124443,#124444,#124445,#124446,#124447,#124448),(#124449,#124450,#124451,
#124452,#124453,#124454),(#124455,#124456,#124457,#124458,#124459,#124460)),
 .UNSPECIFIED.,.F.,.F.,.F.)
B_SPLINE_SURFACE_WITH_KNOTS((4,4),(4,1,1,4),(0.,1.),(0.,0.0668296872169646,
0.628269522946755,1.),.UNSPECIFIED.)
GEOMETRIC_REPRESENTATION_ITEM()
RATIONAL_B_SPLINE_SURFACE(((1.365416977784,1.365416977784,1.365416977784,
1.365416977784,1.365416977784,1.365416977784),(0.8781943407385,0.8781943407385,
0.8781943407385,0.8781943407385,0.8781943407385,0.8781943407385),(0.8781943407385,
0.8781943407385,0.8781943407385,0.8781943407385,0.8781943407385,0.8781943407385),
(1.365416977784,1.365416977784,1.365416977784,1.365416977784,1.365416977784,
1.365416977784)))
REPRESENTATION_ITEM('')
SURFACE()
);
#2444=(
BOUNDED_SURFACE()
B_SPLINE_SURFACE(3,3,((#124474,#124475,#124476,#124477,#124478,#124479,
#124480,#124481,#124482,#124483,#124484,#124485,#124486,#124487,#124488),
(#124489,#124490,#124491,#124492,#124493,#124494,#124495,#124496,#124497,
#124498,#124499,#124500,#124501,#124502,#124503),(#124504,#124505,#124506,
#124507,#124508,#124509,#124510,#124511,#124512,#124513,#124514,#124515,
#124516,#124517,#124518),(#124519,#124520,#124521,#124522,#124523,#124524,
#124525,#124526,#124527,#124528,#124529,#124530,#124531,#124532,#124533)),
 .UNSPECIFIED.,.F.,.F.,.F.)
B_SPLINE_SURFACE_WITH_KNOTS((4,4),(4,1,1,1,1,1,1,1,1,1,1,1,4),(0.,1.),(0.,
0.100036646536872,0.223693703070815,0.335641994831635,0.437371524654234,
0.529770444704687,0.614003043110945,0.692082215426747,0.767474713817308,
0.84177692890213,0.916098301259391,0.991595887369207,1.),.UNSPECIFIED.)
GEOMETRIC_REPRESENTATION_ITEM()
RATIONAL_B_SPLINE_SURFACE(((1.293938210524,1.293938210524,1.293938210524,
1.293938210524,1.293938210524,1.293938210524,1.293938210524,1.293938210524,
1.293938210524,1.293938210524,1.293938210524,1.293938210524,1.293938210524,
1.293938210524,1.293938210524),(0.9020205964919,0.9020205964919,0.9020205964919,
0.9020205964919,0.9020205964919,0.9020205964919,0.9020205964919,0.9020205964919,
0.9020205964919,0.9020205964919,0.9020205964919,0.9020205964919,0.9020205964919,
0.9020205964919,0.9020205964919),(0.9020205964919,0.9020205964919,0.9020205964919,
0.9020205964919,0.9020205964919,0.9020205964919,0.9020205964919,0.9020205964919,
0.9020205964919,0.9020205964919,0.9020205964919,0.9020205964919,0.9020205964919,
0.9020205964919,0.9020205964919),(1.293938210524,1.293938210524,1.293938210524,
1.293938210524,1.293938210524,1.293938210524,1.293938210524,1.293938210524,
1.293938210524,1.293938210524,1.293938210524,1.293938210524,1.293938210524,
1.293938210524,1.293938210524)))
REPRESENTATION_ITEM('')
SURFACE()
);
#2445=(
BOUNDED_SURFACE()
B_SPLINE_SURFACE(3,3,((#124740,#124741,#124742,#124743,#124744,#124745,
#124746,#124747),(#124748,#124749,#124750,#124751,#124752,#124753,#124754,
#124755),(#124756,#124757,#124758,#124759,#124760,#124761,#124762,#124763),
(#124764,#124765,#124766,#124767,#124768,#124769,#124770,#124771)),
 .UNSPECIFIED.,.F.,.F.,.F.)
B_SPLINE_SURFACE_WITH_KNOTS((4,4),(4,1,1,1,1,4),(0.,1.),(0.,0.156651639089242,
0.358591440264207,0.564674709448518,0.789411493920748,1.),.UNSPECIFIED.)
GEOMETRIC_REPRESENTATION_ITEM()
RATIONAL_B_SPLINE_SURFACE(((1.12003765321,1.12003765321,1.12003765321,1.12003765321,
1.12003765321,1.12003765321,1.12003765321,1.12003765321),(0.9599874489302,
0.9599874489302,0.9599874489302,0.9599874489302,0.9599874489302,0.9599874489302,
0.9599874489302,0.9599874489302),(0.9599874489302,0.9599874489302,0.9599874489302,
0.9599874489302,0.9599874489302,0.9599874489302,0.9599874489302,0.9599874489302),
(1.12003765321,1.12003765321,1.12003765321,1.12003765321,1.12003765321,
1.12003765321,1.12003765321,1.12003765321)))
REPRESENTATION_ITEM('')
SURFACE()
);
#2446=(
BOUNDED_SURFACE()
B_SPLINE_SURFACE(3,3,((#124774,#124775,#124776,#124777,#124778,#124779,
#124780,#124781,#124782,#124783,#124784,#124785,#124786,#124787,#124788,
#124789,#124790),(#124791,#124792,#124793,#124794,#124795,#124796,#124797,
#124798,#124799,#124800,#124801,#124802,#124803,#124804,#124805,#124806,
#124807),(#124808,#124809,#124810,#124811,#124812,#124813,#124814,#124815,
#124816,#124817,#124818,#124819,#124820,#124821,#124822,#124823,#124824),
(#124825,#124826,#124827,#124828,#124829,#124830,#124831,#124832,#124833,
#124834,#124835,#124836,#124837,#124838,#124839,#124840,#124841)),
 .UNSPECIFIED.,.F.,.F.,.F.)
B_SPLINE_SURFACE_WITH_KNOTS((4,4),(4,1,1,1,1,1,1,1,1,1,1,1,1,1,4),(0.,1.),
(0.,0.0956146431540125,0.200570336486981,0.29617085639003,0.382446369780954,
0.459533334763256,0.527981368507571,0.590340486919798,0.649866246025106,
0.709565784246277,0.769912468560832,0.830222740675431,0.890369247895391,
0.9504555950694,1.),.UNSPECIFIED.)
GEOMETRIC_REPRESENTATION_ITEM()
RATIONAL_B_SPLINE_SURFACE(((1.220899632035,1.220899632035,1.220899632035,
1.220899632035,1.220899632035,1.220899632035,1.220899632035,1.220899632035,
1.220899632035,1.220899632035,1.220899632035,1.220899632035,1.220899632035,
1.220899632035,1.220899632035,1.220899632035,1.220899632035),(0.9263667893217,
0.9263667893217,0.9263667893217,0.9263667893217,0.9263667893217,0.9263667893217,
0.9263667893217,0.9263667893217,0.9263667893217,0.9263667893217,0.9263667893217,
0.9263667893217,0.9263667893217,0.9263667893217,0.9263667893217,0.9263667893217,
0.9263667893217),(0.9263667893217,0.9263667893217,0.9263667893217,0.9263667893217,
0.9263667893217,0.9263667893217,0.9263667893217,0.9263667893217,0.9263667893217,
0.9263667893217,0.9263667893217,0.9263667893217,0.9263667893217,0.9263667893217,
0.9263667893217,0.9263667893217,0.9263667893217),(1.220899632035,1.220899632035,
1.220899632035,1.220899632035,1.220899632035,1.220899632035,1.220899632035,
1.220899632035,1.220899632035,1.220899632035,1.220899632035,1.220899632035,
1.220899632035,1.220899632035,1.220899632035,1.220899632035,1.220899632035)))
REPRESENTATION_ITEM('')
SURFACE()
);
#2447=(
BOUNDED_SURFACE()
B_SPLINE_SURFACE(3,3,((#125007,#125008,#125009,#125010,#125011,#125012,
#125013,#125014,#125015,#125016),(#125017,#125018,#125019,#125020,#125021,
#125022,#125023,#125024,#125025,#125026),(#125027,#125028,#125029,#125030,
#125031,#125032,#125033,#125034,#125035,#125036),(#125037,#125038,#125039,
#125040,#125041,#125042,#125043,#125044,#125045,#125046)),.UNSPECIFIED.,
 .F.,.F.,.F.)
B_SPLINE_SURFACE_WITH_KNOTS((4,4),(4,1,1,1,1,1,1,4),(0.,1.),(0.,0.0291077785832009,
0.175697498314966,0.342920964150671,0.52427955765036,0.713524484672767,
0.905557751001572,1.),.UNSPECIFIED.)
GEOMETRIC_REPRESENTATION_ITEM()
RATIONAL_B_SPLINE_SURFACE(((1.365112687886,1.365112687886,1.365112687886,
1.365112687886,1.365112687886,1.365112687886,1.365112687886,1.365112687886,
1.365112687886,1.365112687886),(0.8782957707048,0.8782957707048,0.8782957707048,
0.8782957707048,0.8782957707048,0.8782957707048,0.8782957707048,0.8782957707048,
0.8782957707048,0.8782957707048),(0.8782957707048,0.8782957707048,0.8782957707048,
0.8782957707048,0.8782957707048,0.8782957707048,0.8782957707048,0.8782957707048,
0.8782957707048,0.8782957707048),(1.365112687886,1.365112687886,1.365112687886,
1.365112687886,1.365112687886,1.365112687886,1.365112687886,1.365112687886,
1.365112687886,1.365112687886)))
REPRESENTATION_ITEM('')
SURFACE()
);
#2448=(
BOUNDED_SURFACE()
B_SPLINE_SURFACE(3,3,((#125089,#125090,#125091,#125092,#125093),(#125094,
#125095,#125096,#125097,#125098),(#125099,#125100,#125101,#125102,#125103),
(#125104,#125105,#125106,#125107,#125108)),.UNSPECIFIED.,.F.,.F.,.F.)
B_SPLINE_SURFACE_WITH_KNOTS((4,4),(4,1,4),(0.,1.),(0.,0.328690768122142,
1.),.UNSPECIFIED.)
GEOMETRIC_REPRESENTATION_ITEM()
RATIONAL_B_SPLINE_SURFACE(((1.365414096237,1.365414096237,1.365414096237,
1.365414096237,1.365414096237),(0.8781953012543,0.8781953012543,0.8781953012543,
0.8781953012543,0.8781953012543),(0.8781953012543,0.8781953012543,0.8781953012543,
0.8781953012543,0.8781953012543),(1.365414096237,1.365414096237,1.365414096237,
1.365414096237,1.365414096237)))
REPRESENTATION_ITEM('')
SURFACE()
);
#2449=(
BOUNDED_SURFACE()
B_SPLINE_SURFACE(3,3,((#125118,#125119,#125120,#125121,#125122,#125123,
#125124,#125125,#125126,#125127,#125128,#125129,#125130,#125131,#125132,
#125133,#125134,#125135,#125136,#125137),(#125138,#125139,#125140,#125141,
#125142,#125143,#125144,#125145,#125146,#125147,#125148,#125149,#125150,
#125151,#125152,#125153,#125154,#125155,#125156,#125157),(#125158,#125159,
#125160,#125161,#125162,#125163,#125164,#125165,#125166,#125167,#125168,
#125169,#125170,#125171,#125172,#125173,#125174,#125175,#125176,#125177),
(#125178,#125179,#125180,#125181,#125182,#125183,#125184,#125185,#125186,
#125187,#125188,#125189,#125190,#125191,#125192,#125193,#125194,#125195,
#125196,#125197)),.UNSPECIFIED.,.F.,.F.,.F.)
B_SPLINE_SURFACE_WITH_KNOTS((4,4),(4,1,1,1,1,1,1,1,1,1,1,1,1,1,1,1,1,4),
(0.,1.),(0.,0.0437810757388625,0.14954997921505,0.246647238721872,0.335632768061324,
0.417102216875795,0.491694466527586,0.560145818346898,0.623130978563885,
0.681070799832575,0.734496942850944,0.783914635620664,0.829348379595357,
0.870873757986737,0.909008250330309,0.944496730233535,0.978199195579797,
1.),.UNSPECIFIED.)
GEOMETRIC_REPRESENTATION_ITEM()
RATIONAL_B_SPLINE_SURFACE(((1.350953897201,1.350953897201,1.350953897201,
1.350953897201,1.350953897201,1.350953897201,1.350953897201,1.350953897201,
1.350953897201,1.350953897201,1.350953897201,1.350953897201,1.350953897201,
1.350953897201,1.350953897201,1.350953897201,1.350953897201,1.350953897201,
1.350953897201,1.350953897201),(0.8830153675996,0.8830153675996,0.8830153675996,
0.8830153675996,0.8830153675996,0.8830153675996,0.8830153675996,0.8830153675996,
0.8830153675996,0.8830153675996,0.8830153675996,0.8830153675996,0.8830153675996,
0.8830153675996,0.8830153675996,0.8830153675996,0.8830153675996,0.8830153675996,
0.8830153675996,0.8830153675996),(0.8830153675996,0.8830153675996,0.8830153675996,
0.8830153675996,0.8830153675996,0.8830153675996,0.8830153675996,0.8830153675996,
0.8830153675996,0.8830153675996,0.8830153675996,0.8830153675996,0.8830153675996,
0.8830153675996,0.8830153675996,0.8830153675996,0.8830153675996,0.8830153675996,
0.8830153675996,0.8830153675996),(1.350953897201,1.350953897201,1.350953897201,
1.350953897201,1.350953897201,1.350953897201,1.350953897201,1.350953897201,
1.350953897201,1.350953897201,1.350953897201,1.350953897201,1.350953897201,
1.350953897201,1.350953897201,1.350953897201,1.350953897201,1.350953897201,
1.350953897201,1.350953897201)))
REPRESENTATION_ITEM('')
SURFACE()
);
#2450=(
BOUNDED_SURFACE()
B_SPLINE_SURFACE(3,3,((#125421,#125422,#125423,#125424,#125425,#125426,
#125427,#125428,#125429,#125430,#125431,#125432,#125433,#125434,#125435,
#125436,#125437,#125438,#125439,#125440,#125441,#125442),(#125443,#125444,
#125445,#125446,#125447,#125448,#125449,#125450,#125451,#125452,#125453,
#125454,#125455,#125456,#125457,#125458,#125459,#125460,#125461,#125462,
#125463,#125464),(#125465,#125466,#125467,#125468,#125469,#125470,#125471,
#125472,#125473,#125474,#125475,#125476,#125477,#125478,#125479,#125480,
#125481,#125482,#125483,#125484,#125485,#125486),(#125487,#125488,#125489,
#125490,#125491,#125492,#125493,#125494,#125495,#125496,#125497,#125498,
#125499,#125500,#125501,#125502,#125503,#125504,#125505,#125506,#125507,
#125508)),.UNSPECIFIED.,.F.,.F.,.F.)
B_SPLINE_SURFACE_WITH_KNOTS((4,4),(4,1,1,1,1,1,1,1,1,1,1,1,1,1,1,1,1,1,
1,4),(0.,1.),(0.,0.0711383255328258,0.137163359302248,0.195720435393546,
0.247715273019436,0.293698370802659,0.336008737306656,0.380005256943101,
0.425168878602564,0.469947554154179,0.513213820955286,0.55641075188751,
0.604436817371917,0.658671873052936,0.719515049298376,0.788488856663347,
0.862062739446009,0.932266724631227,0.998927768427254,1.),.UNSPECIFIED.)
GEOMETRIC_REPRESENTATION_ITEM()
RATIONAL_B_SPLINE_SURFACE(((1.255321345493,1.255321345493,1.255321345493,
1.255321345493,1.255321345493,1.255321345493,1.255321345493,1.255321345493,
1.255321345493,1.255321345493,1.255321345493,1.255321345493,1.255321345493,
1.255321345493,1.255321345493,1.255321345493,1.255321345493,1.255321345493,
1.255321345493,1.255321345493,1.255321345493,1.255321345493),(0.9148928848357,
0.9148928848357,0.9148928848357,0.9148928848357,0.9148928848357,0.9148928848357,
0.9148928848357,0.9148928848357,0.9148928848357,0.9148928848357,0.9148928848357,
0.9148928848357,0.9148928848357,0.9148928848357,0.9148928848357,0.9148928848357,
0.9148928848357,0.9148928848357,0.9148928848357,0.9148928848357,0.9148928848357,
0.9148928848357),(0.9148928848357,0.9148928848357,0.9148928848357,0.9148928848357,
0.9148928848357,0.9148928848357,0.9148928848357,0.9148928848357,0.9148928848357,
0.9148928848357,0.9148928848357,0.9148928848357,0.9148928848357,0.9148928848357,
0.9148928848357,0.9148928848357,0.9148928848357,0.9148928848357,0.9148928848357,
0.9148928848357,0.9148928848357,0.9148928848357),(1.255321345493,1.255321345493,
1.255321345493,1.255321345493,1.255321345493,1.255321345493,1.255321345493,
1.255321345493,1.255321345493,1.255321345493,1.255321345493,1.255321345493,
1.255321345493,1.255321345493,1.255321345493,1.255321345493,1.255321345493,
1.255321345493,1.255321345493,1.255321345493,1.255321345493,1.255321345493)))
REPRESENTATION_ITEM('')
SURFACE()
);
#2451=(
BOUNDED_SURFACE()
B_SPLINE_SURFACE(3,3,((#125841,#125842,#125843,#125844,#125845,#125846,
#125847,#125848,#125849,#125850,#125851,#125852,#125853),(#125854,#125855,
#125856,#125857,#125858,#125859,#125860,#125861,#125862,#125863,#125864,
#125865,#125866),(#125867,#125868,#125869,#125870,#125871,#125872,#125873,
#125874,#125875,#125876,#125877,#125878,#125879),(#125880,#125881,#125882,
#125883,#125884,#125885,#125886,#125887,#125888,#125889,#125890,#125891,
#125892)),.UNSPECIFIED.,.F.,.F.,.F.)
B_SPLINE_SURFACE_WITH_KNOTS((4,4),(4,1,1,1,1,1,1,1,1,1,4),(0.,1.),(0.,0.0952638051529656,
0.22509444570554,0.342634254506935,0.445180680757504,0.539182519786869,
0.634901504810863,0.734230912844932,0.834482617338388,0.927390396537817,
1.),.UNSPECIFIED.)
GEOMETRIC_REPRESENTATION_ITEM()
RATIONAL_B_SPLINE_SURFACE(((1.132183978984,1.132183978984,1.132183978984,
1.132183978984,1.132183978984,1.132183978984,1.132183978984,1.132183978984,
1.132183978984,1.132183978984,1.132183978984,1.132183978984,1.132183978984),
(0.9559386736722,0.9559386736722,0.9559386736722,0.9559386736722,0.9559386736722,
0.9559386736722,0.9559386736722,0.9559386736722,0.9559386736722,0.9559386736722,
0.9559386736722,0.9559386736722,0.9559386736722),(0.9559386736722,0.9559386736722,
0.9559386736722,0.9559386736722,0.9559386736722,0.9559386736722,0.9559386736722,
0.9559386736722,0.9559386736722,0.9559386736722,0.9559386736722,0.9559386736722,
0.9559386736722),(1.132183978984,1.132183978984,1.132183978984,1.132183978984,
1.132183978984,1.132183978984,1.132183978984,1.132183978984,1.132183978984,
1.132183978984,1.132183978984,1.132183978984,1.132183978984)))
REPRESENTATION_ITEM('')
SURFACE()
);
#2452=(
BOUNDED_SURFACE()
B_SPLINE_SURFACE(3,3,((#125932,#125933,#125934,#125935,#125936,#125937),
(#125938,#125939,#125940,#125941,#125942,#125943),(#125944,#125945,#125946,
#125947,#125948,#125949),(#125950,#125951,#125952,#125953,#125954,#125955)),
 .UNSPECIFIED.,.F.,.F.,.F.)
B_SPLINE_SURFACE_WITH_KNOTS((4,4),(4,1,1,4),(0.,1.),(0.,0.0615355941999108,
0.552403092261162,1.),.UNSPECIFIED.)
GEOMETRIC_REPRESENTATION_ITEM()
RATIONAL_B_SPLINE_SURFACE(((1.132184177625,1.132184177625,1.132184177625,
1.132184177625,1.132184177625,1.132184177625),(0.9559386074585,0.9559386074585,
0.9559386074585,0.9559386074585,0.9559386074585,0.9559386074585),(0.9559386074585,
0.9559386074585,0.9559386074585,0.9559386074585,0.9559386074585,0.9559386074585),
(1.132184177625,1.132184177625,1.132184177625,1.132184177625,1.132184177625,
1.132184177625)))
REPRESENTATION_ITEM('')
SURFACE()
);
#2453=(
BOUNDED_SURFACE()
B_SPLINE_SURFACE(3,3,((#125982,#125983,#125984,#125985,#125986,#125987,
#125988,#125989,#125990,#125991,#125992,#125993,#125994,#125995,#125996,
#125997,#125998),(#125999,#126000,#126001,#126002,#126003,#126004,#126005,
#126006,#126007,#126008,#126009,#126010,#126011,#126012,#126013,#126014,
#126015),(#126016,#126017,#126018,#126019,#126020,#126021,#126022,#126023,
#126024,#126025,#126026,#126027,#126028,#126029,#126030,#126031,#126032),
(#126033,#126034,#126035,#126036,#126037,#126038,#126039,#126040,#126041,
#126042,#126043,#126044,#126045,#126046,#126047,#126048,#126049)),
 .UNSPECIFIED.,.F.,.F.,.F.)
B_SPLINE_SURFACE_WITH_KNOTS((4,4),(4,1,1,1,1,1,1,1,1,1,1,1,1,1,4),(0.,1.),
(0.,0.0421741349720486,0.122382017207444,0.194203536901675,0.257534399271218,
0.321534135544779,0.38726227689901,0.452657895941669,0.516567929355648,
0.579748305445392,0.647421910672303,0.723873761459194,0.810175603109662,
0.905570261612151,1.),.UNSPECIFIED.)
GEOMETRIC_REPRESENTATION_ITEM()
RATIONAL_B_SPLINE_SURFACE(((1.219577374139,1.219577374139,1.219577374139,
1.219577374139,1.219577374139,1.219577374139,1.219577374139,1.219577374139,
1.219577374139,1.219577374139,1.219577374139,1.219577374139,1.219577374139,
1.219577374139,1.219577374139,1.219577374139,1.219577374139),(0.9268075419537,
0.9268075419537,0.9268075419537,0.9268075419537,0.9268075419537,0.9268075419537,
0.9268075419537,0.9268075419537,0.9268075419537,0.9268075419537,0.9268075419537,
0.9268075419537,0.9268075419537,0.9268075419537,0.9268075419537,0.9268075419537,
0.9268075419537),(0.9268075419537,0.9268075419537,0.9268075419537,0.9268075419537,
0.9268075419537,0.9268075419537,0.9268075419537,0.9268075419537,0.9268075419537,
0.9268075419537,0.9268075419537,0.9268075419537,0.9268075419537,0.9268075419537,
0.9268075419537,0.9268075419537,0.9268075419537),(1.219577374139,1.219577374139,
1.219577374139,1.219577374139,1.219577374139,1.219577374139,1.219577374139,
1.219577374139,1.219577374139,1.219577374139,1.219577374139,1.219577374139,
1.219577374139,1.219577374139,1.219577374139,1.219577374139,1.219577374139)))
REPRESENTATION_ITEM('')
SURFACE()
);
#2454=(
BOUNDED_SURFACE()
B_SPLINE_SURFACE(3,3,((#126077,#126078,#126079,#126080,#126081,#126082,
#126083,#126084,#126085,#126086,#126087,#126088),(#126089,#126090,#126091,
#126092,#126093,#126094,#126095,#126096,#126097,#126098,#126099,#126100),
(#126101,#126102,#126103,#126104,#126105,#126106,#126107,#126108,#126109,
#126110,#126111,#126112),(#126113,#126114,#126115,#126116,#126117,#126118,
#126119,#126120,#126121,#126122,#126123,#126124)),.UNSPECIFIED.,.F.,.F.,
 .F.)
B_SPLINE_SURFACE_WITH_KNOTS((4,4),(4,1,1,1,1,1,1,1,1,4),(0.,1.),(0.,0.0164345215705728,
0.129301162013314,0.242710853927909,0.360524593523248,0.486789420086521,
0.625540658542323,0.780319654457662,0.950754978076216,1.),.UNSPECIFIED.)
GEOMETRIC_REPRESENTATION_ITEM()
RATIONAL_B_SPLINE_SURFACE(((1.03572903915,1.03572903915,1.03572903915,1.03572903915,
1.03572903915,1.03572903915,1.03572903915,1.03572903915,1.03572903915,1.03572903915,
1.03572903915,1.03572903915),(0.9880903202835,0.9880903202835,0.9880903202835,
0.9880903202835,0.9880903202835,0.9880903202835,0.9880903202835,0.9880903202835,
0.9880903202835,0.9880903202835,0.9880903202835,0.9880903202835),(0.9880903202835,
0.9880903202835,0.9880903202835,0.9880903202835,0.9880903202835,0.9880903202835,
0.9880903202835,0.9880903202835,0.9880903202835,0.9880903202835,0.9880903202835,
0.9880903202835),(1.03572903915,1.03572903915,1.03572903915,1.03572903915,
1.03572903915,1.03572903915,1.03572903915,1.03572903915,1.03572903915,1.03572903915,
1.03572903915,1.03572903915)))
REPRESENTATION_ITEM('')
SURFACE()
);
#2455=(
BOUNDED_SURFACE()
B_SPLINE_SURFACE(3,3,((#126575,#126576,#126577,#126578,#126579,#126580,
#126581,#126582,#126583),(#126584,#126585,#126586,#126587,#126588,#126589,
#126590,#126591,#126592),(#126593,#126594,#126595,#126596,#126597,#126598,
#126599,#126600,#126601),(#126602,#126603,#126604,#126605,#126606,#126607,
#126608,#126609,#126610)),.UNSPECIFIED.,.F.,.F.,.F.)
B_SPLINE_SURFACE_WITH_KNOTS((4,4),(4,1,1,1,1,1,4),(0.,1.),(0.,0.124217072386526,
0.310755650559109,0.499972700734522,0.689255535673335,0.875770607228338,
1.),.UNSPECIFIED.)
GEOMETRIC_REPRESENTATION_ITEM()
RATIONAL_B_SPLINE_SURFACE(((1.04330354939,1.04330354939,1.04330354939,1.04330354939,
1.04330354939,1.04330354939,1.04330354939,1.04330354939,1.04330354939),
(0.9855654835368,0.9855654835368,0.9855654835368,0.9855654835368,0.9855654835368,
0.9855654835368,0.9855654835368,0.9855654835368,0.9855654835368),(0.9855654835368,
0.9855654835368,0.9855654835368,0.9855654835368,0.9855654835368,0.9855654835368,
0.9855654835368,0.9855654835368,0.9855654835368),(1.04330354939,1.04330354939,
1.04330354939,1.04330354939,1.04330354939,1.04330354939,1.04330354939,1.04330354939,
1.04330354939)))
REPRESENTATION_ITEM('')
SURFACE()
);
#2456=(
BOUNDED_SURFACE()
B_SPLINE_SURFACE(3,3,((#126654,#126655,#126656,#126657,#126658,#126659,
#126660,#126661,#126662,#126663,#126664,#126665,#126666,#126667,#126668,
#126669,#126670,#126671,#126672),(#126673,#126674,#126675,#126676,#126677,
#126678,#126679,#126680,#126681,#126682,#126683,#126684,#126685,#126686,
#126687,#126688,#126689,#126690,#126691),(#126692,#126693,#126694,#126695,
#126696,#126697,#126698,#126699,#126700,#126701,#126702,#126703,#126704,
#126705,#126706,#126707,#126708,#126709,#126710),(#126711,#126712,#126713,
#126714,#126715,#126716,#126717,#126718,#126719,#126720,#126721,#126722,
#126723,#126724,#126725,#126726,#126727,#126728,#126729)),.UNSPECIFIED.,
 .F.,.F.,.F.)
B_SPLINE_SURFACE_WITH_KNOTS((4,4),(4,1,1,1,1,1,1,1,1,1,1,1,1,1,1,1,4),(0.,
1.),(0.,0.0799280122799653,0.16360439135842,0.238188789720562,0.304013208895698,
0.361552441990052,0.412607959769593,0.462371825350478,0.513679071869309,
0.566147489952465,0.617336562641754,0.665597869256093,0.718768591516355,
0.778520204495205,0.846090350205214,0.922943284356756,1.),.UNSPECIFIED.)
GEOMETRIC_REPRESENTATION_ITEM()
RATIONAL_B_SPLINE_SURFACE(((1.057421706335,1.057421706335,1.057421706335,
1.057421706335,1.057421706335,1.057421706335,1.057421706335,1.057421706335,
1.057421706335,1.057421706335,1.057421706335,1.057421706335,1.057421706335,
1.057421706335,1.057421706335,1.057421706335,1.057421706335,1.057421706335,
1.057421706335),(0.9808594312216,0.9808594312216,0.9808594312216,0.9808594312216,
0.9808594312216,0.9808594312216,0.9808594312216,0.9808594312216,0.9808594312216,
0.9808594312216,0.9808594312216,0.9808594312216,0.9808594312216,0.9808594312216,
0.9808594312216,0.9808594312216,0.9808594312216,0.9808594312216,0.9808594312216),
(0.9808594312216,0.9808594312216,0.9808594312216,0.9808594312216,0.9808594312216,
0.9808594312216,0.9808594312216,0.9808594312216,0.9808594312216,0.9808594312216,
0.9808594312216,0.9808594312216,0.9808594312216,0.9808594312216,0.9808594312216,
0.9808594312216,0.9808594312216,0.9808594312216,0.9808594312216),(1.057421706335,
1.057421706335,1.057421706335,1.057421706335,1.057421706335,1.057421706335,
1.057421706335,1.057421706335,1.057421706335,1.057421706335,1.057421706335,
1.057421706335,1.057421706335,1.057421706335,1.057421706335,1.057421706335,
1.057421706335,1.057421706335,1.057421706335)))
REPRESENTATION_ITEM('')
SURFACE()
);
#2457=(
BOUNDED_SURFACE()
B_SPLINE_SURFACE(3,3,((#126949,#126950,#126951,#126952,#126953,#126954),
(#126955,#126956,#126957,#126958,#126959,#126960),(#126961,#126962,#126963,
#126964,#126965,#126966),(#126967,#126968,#126969,#126970,#126971,#126972)),
 .UNSPECIFIED.,.F.,.F.,.F.)
B_SPLINE_SURFACE_WITH_KNOTS((4,4),(4,1,1,4),(0.,1.),(0.,0.261439365399046,
0.646008272605236,1.),.UNSPECIFIED.)
GEOMETRIC_REPRESENTATION_ITEM()
RATIONAL_B_SPLINE_SURFACE(((1.043303915571,1.043303915571,1.043303915571,
1.043303915571,1.043303915571,1.043303915571),(0.9855653614763,0.9855653614763,
0.9855653614763,0.9855653614763,0.9855653614763,0.9855653614763),(0.9855653614763,
0.9855653614763,0.9855653614763,0.9855653614763,0.9855653614763,0.9855653614763),
(1.043303915571,1.043303915571,1.043303915571,1.043303915571,1.043303915571,
1.043303915571)))
REPRESENTATION_ITEM('')
SURFACE()
);
#2458=(
BOUNDED_SURFACE()
B_SPLINE_SURFACE(3,3,((#127033,#127034,#127035,#127036,#127037,#127038),
(#127039,#127040,#127041,#127042,#127043,#127044),(#127045,#127046,#127047,
#127048,#127049,#127050),(#127051,#127052,#127053,#127054,#127055,#127056)),
 .UNSPECIFIED.,.F.,.F.,.F.)
B_SPLINE_SURFACE_WITH_KNOTS((4,4),(4,1,1,4),(0.,1.),(0.,0.338411218706876,
0.730847706276313,1.),.UNSPECIFIED.)
GEOMETRIC_REPRESENTATION_ITEM()
RATIONAL_B_SPLINE_SURFACE(((1.043304339832,1.043304339832,1.043304339832,
1.043304339832,1.043304339832,1.043304339832),(0.9855652200561,0.9855652200561,
0.9855652200561,0.9855652200561,0.9855652200561,0.9855652200561),(0.9855652200561,
0.9855652200561,0.9855652200561,0.9855652200561,0.9855652200561,0.9855652200561),
(1.043304339832,1.043304339832,1.043304339832,1.043304339832,1.043304339832,
1.043304339832)))
REPRESENTATION_ITEM('')
SURFACE()
);
#2459=(
BOUNDED_SURFACE()
B_SPLINE_SURFACE(3,3,((#127120,#127121,#127122,#127123,#127124,#127125),
(#127126,#127127,#127128,#127129,#127130,#127131),(#127132,#127133,#127134,
#127135,#127136,#127137),(#127138,#127139,#127140,#127141,#127142,#127143)),
 .UNSPECIFIED.,.F.,.F.,.F.)
B_SPLINE_SURFACE_WITH_KNOTS((4,4),(4,1,1,4),(0.,1.),(0.,0.29605416480998,
0.688995950644091,1.),.UNSPECIFIED.)
GEOMETRIC_REPRESENTATION_ITEM()
RATIONAL_B_SPLINE_SURFACE(((1.049988055972,1.049988055972,1.049988055972,
1.049988055972,1.049988055972,1.049988055972),(0.983337314676,0.983337314676,
0.983337314676,0.983337314676,0.983337314676,0.983337314676),(0.983337314676,
0.983337314676,0.983337314676,0.983337314676,0.983337314676,0.983337314676),
(1.049988055972,1.049988055972,1.049988055972,1.049988055972,1.049988055972,
1.049988055972)))
REPRESENTATION_ITEM('')
SURFACE()
);
#2460=(
BOUNDED_SURFACE()
B_SPLINE_SURFACE(3,3,((#127157,#127158,#127159,#127160,#127161,#127162,
#127163,#127164,#127165,#127166,#127167,#127168),(#127169,#127170,#127171,
#127172,#127173,#127174,#127175,#127176,#127177,#127178,#127179,#127180),
(#127181,#127182,#127183,#127184,#127185,#127186,#127187,#127188,#127189,
#127190,#127191,#127192),(#127193,#127194,#127195,#127196,#127197,#127198,
#127199,#127200,#127201,#127202,#127203,#127204)),.UNSPECIFIED.,.F.,.F.,
 .F.)
B_SPLINE_SURFACE_WITH_KNOTS((4,4),(4,1,1,1,1,1,1,1,1,4),(0.,1.),(0.,0.0415070947502971,
0.154210972284995,0.269286157242448,0.38315843713789,0.490653949298758,
0.603397292452659,0.728418373951416,0.867462240539534,1.),.UNSPECIFIED.)
GEOMETRIC_REPRESENTATION_ITEM()
RATIONAL_B_SPLINE_SURFACE(((1.050209251113,1.050209251113,1.050209251113,
1.050209251113,1.050209251113,1.050209251113,1.050209251113,1.050209251113,
1.050209251113,1.050209251113,1.050209251113,1.050209251113),(0.9832635829624,
0.9832635829624,0.9832635829624,0.9832635829624,0.9832635829624,0.9832635829624,
0.9832635829624,0.9832635829624,0.9832635829624,0.9832635829624,0.9832635829624,
0.9832635829624),(0.9832635829624,0.9832635829624,0.9832635829624,0.9832635829624,
0.9832635829624,0.9832635829624,0.9832635829624,0.9832635829624,0.9832635829624,
0.9832635829624,0.9832635829624,0.9832635829624),(1.050209251113,1.050209251113,
1.050209251113,1.050209251113,1.050209251113,1.050209251113,1.050209251113,
1.050209251113,1.050209251113,1.050209251113,1.050209251113,1.050209251113)))
REPRESENTATION_ITEM('')
SURFACE()
);
#2461=(
BOUNDED_SURFACE()
B_SPLINE_SURFACE(3,3,((#127358,#127359,#127360,#127361,#127362,#127363,
#127364,#127365),(#127366,#127367,#127368,#127369,#127370,#127371,#127372,
#127373),(#127374,#127375,#127376,#127377,#127378,#127379,#127380,#127381),
(#127382,#127383,#127384,#127385,#127386,#127387,#127388,#127389)),
 .UNSPECIFIED.,.F.,.F.,.F.)
B_SPLINE_SURFACE_WITH_KNOTS((4,4),(4,1,1,1,1,4),(0.,1.),(0.,0.20131167769844,
0.447511967106375,0.696970531427775,0.944927146503993,1.),.UNSPECIFIED.)
GEOMETRIC_REPRESENTATION_ITEM()
RATIONAL_B_SPLINE_SURFACE(((1.050193937179,1.050193937179,1.050193937179,
1.050193937179,1.050193937179,1.050193937179,1.050193937179,1.050193937179),
(0.9832686876072,0.9832686876072,0.9832686876072,0.9832686876072,0.9832686876071,
0.9832686876072,0.9832686876072,0.9832686876072),(0.9832686876072,0.9832686876072,
0.9832686876072,0.9832686876072,0.9832686876071,0.9832686876072,0.9832686876072,
0.9832686876072),(1.050193937179,1.050193937179,1.050193937179,1.050193937179,
1.050193937179,1.050193937179,1.050193937179,1.050193937179)))
REPRESENTATION_ITEM('')
SURFACE()
);
#2462=(
BOUNDED_SURFACE()
B_SPLINE_SURFACE(3,3,((#127425,#127426,#127427,#127428,#127429,#127430),
(#127431,#127432,#127433,#127434,#127435,#127436),(#127437,#127438,#127439,
#127440,#127441,#127442),(#127443,#127444,#127445,#127446,#127447,#127448)),
 .UNSPECIFIED.,.F.,.F.,.F.)
B_SPLINE_SURFACE_WITH_KNOTS((4,4),(4,1,1,4),(0.,1.),(0.,0.314367621060507,
0.711949844500348,1.),.UNSPECIFIED.)
GEOMETRIC_REPRESENTATION_ITEM()
RATIONAL_B_SPLINE_SURFACE(((1.049987137241,1.049987137241,1.049987137241,
1.049987137241,1.049987137241,1.049987137241),(0.9833376209197,0.9833376209197,
0.9833376209197,0.9833376209197,0.9833376209197,0.9833376209197),(0.9833376209197,
0.9833376209197,0.9833376209197,0.9833376209197,0.9833376209197,0.9833376209197),
(1.049987137241,1.049987137241,1.049987137241,1.049987137241,1.049987137241,
1.049987137241)))
REPRESENTATION_ITEM('')
SURFACE()
);
#2463=(
BOUNDED_SURFACE()
B_SPLINE_SURFACE(3,3,((#127489,#127490,#127491,#127492,#127493,#127494,
#127495,#127496,#127497,#127498),(#127499,#127500,#127501,#127502,#127503,
#127504,#127505,#127506,#127507,#127508),(#127509,#127510,#127511,#127512,
#127513,#127514,#127515,#127516,#127517,#127518),(#127519,#127520,#127521,
#127522,#127523,#127524,#127525,#127526,#127527,#127528),(#127529,#127530,
#127531,#127532,#127533,#127534,#127535,#127536,#127537,#127538),(#127539,
#127540,#127541,#127542,#127543,#127544,#127545,#127546,#127547,#127548),
(#127549,#127550,#127551,#127552,#127553,#127554,#127555,#127556,#127557,
#127558)),.UNSPECIFIED.,.F.,.F.,.F.)
B_SPLINE_SURFACE_WITH_KNOTS((4,3,4),(4,1,1,1,1,1,1,4),(0.,0.5,1.),(0.,0.161024836461119,
0.369601718395748,0.554125890569757,0.718052359943506,0.864941999117123,
0.996690204747089,1.),.UNSPECIFIED.)
GEOMETRIC_REPRESENTATION_ITEM()
RATIONAL_B_SPLINE_SURFACE(((1.201213809875,1.201213809875,1.201213809875,
1.201213809875,1.201213809875,1.201213809875,1.201213809875,1.201213809875,
1.201213809875,1.201213809875),(0.9329287300417,0.9329287300417,0.9329287300417,
0.9329287300417,0.9329287300417,0.9329287300417,0.9329287300417,0.9329287300417,
0.9329287300417,0.9329287300417),(0.9329287300417,0.9329287300417,0.9329287300417,
0.9329287300417,0.9329287300417,0.9329287300417,0.9329287300417,0.9329287300417,
0.9329287300417,0.9329287300417),(1.201213809875,1.201213809875,1.201213809875,
1.201213809875,1.201213809875,1.201213809875,1.201213809875,1.201213809875,
1.201213809875,1.201213809875),(0.9329287300417,0.9329287300417,0.9329287300417,
0.9329287300417,0.9329287300417,0.9329287300417,0.9329287300417,0.9329287300417,
0.9329287300417,0.9329287300417),(0.9329287300417,0.9329287300417,0.9329287300417,
0.9329287300417,0.9329287300417,0.9329287300417,0.9329287300417,0.9329287300417,
0.9329287300417,0.9329287300417),(1.201213809875,1.201213809875,1.201213809875,
1.201213809875,1.201213809875,1.201213809875,1.201213809875,1.201213809875,
1.201213809875,1.201213809875)))
REPRESENTATION_ITEM('')
SURFACE()
);
#2464=(
BOUNDED_SURFACE()
B_SPLINE_SURFACE(3,3,((#127645,#127646,#127647,#127648,#127649,#127650,
#127651,#127652,#127653,#127654),(#127655,#127656,#127657,#127658,#127659,
#127660,#127661,#127662,#127663,#127664),(#127665,#127666,#127667,#127668,
#127669,#127670,#127671,#127672,#127673,#127674),(#127675,#127676,#127677,
#127678,#127679,#127680,#127681,#127682,#127683,#127684),(#127685,#127686,
#127687,#127688,#127689,#127690,#127691,#127692,#127693,#127694),(#127695,
#127696,#127697,#127698,#127699,#127700,#127701,#127702,#127703,#127704),
(#127705,#127706,#127707,#127708,#127709,#127710,#127711,#127712,#127713,
#127714)),.UNSPECIFIED.,.F.,.F.,.F.)
B_SPLINE_SURFACE_WITH_KNOTS((4,3,4),(4,1,1,1,1,1,1,4),(0.,0.5,1.),(0.,0.0025907538636228,
0.133682793303005,0.278706793926935,0.438527262608492,0.616078859653579,
0.815708849792895,1.),.UNSPECIFIED.)
GEOMETRIC_REPRESENTATION_ITEM()
RATIONAL_B_SPLINE_SURFACE(((1.201171733822,1.201171733822,1.201171733822,
1.201171733822,1.201171733822,1.201171733822,1.201171733822,1.201171733822,
1.201171733822,1.201171733822),(0.9329427553926,0.9329427553926,0.9329427553926,
0.9329427553926,0.9329427553926,0.9329427553926,0.9329427553926,0.9329427553926,
0.9329427553926,0.9329427553926),(0.9329427553926,0.9329427553926,0.9329427553926,
0.9329427553926,0.9329427553926,0.9329427553926,0.9329427553926,0.9329427553926,
0.9329427553926,0.9329427553926),(1.201171733822,1.201171733822,1.201171733822,
1.201171733822,1.201171733822,1.201171733822,1.201171733822,1.201171733822,
1.201171733822,1.201171733822),(0.9329427553926,0.9329427553926,0.9329427553926,
0.9329427553926,0.9329427553926,0.9329427553926,0.9329427553926,0.9329427553926,
0.9329427553926,0.9329427553926),(0.9329427553926,0.9329427553926,0.9329427553926,
0.9329427553926,0.9329427553926,0.9329427553926,0.9329427553926,0.9329427553926,
0.9329427553926,0.9329427553926),(1.201171733822,1.201171733822,1.201171733822,
1.201171733822,1.201171733822,1.201171733822,1.201171733822,1.201171733822,
1.201171733822,1.201171733822)))
REPRESENTATION_ITEM('')
SURFACE()
);
#2465=(
BOUNDED_SURFACE()
B_SPLINE_SURFACE(3,3,((#127716,#127717,#127718,#127719,#127720,#127721,
#127722,#127723,#127724,#127725,#127726,#127727,#127728,#127729,#127730,
#127731,#127732,#127733,#127734,#127735,#127736,#127737,#127738,#127739,
#127740,#127741),(#127742,#127743,#127744,#127745,#127746,#127747,#127748,
#127749,#127750,#127751,#127752,#127753,#127754,#127755,#127756,#127757,
#127758,#127759,#127760,#127761,#127762,#127763,#127764,#127765,#127766,
#127767),(#127768,#127769,#127770,#127771,#127772,#127773,#127774,#127775,
#127776,#127777,#127778,#127779,#127780,#127781,#127782,#127783,#127784,
#127785,#127786,#127787,#127788,#127789,#127790,#127791,#127792,#127793),
(#127794,#127795,#127796,#127797,#127798,#127799,#127800,#127801,#127802,
#127803,#127804,#127805,#127806,#127807,#127808,#127809,#127810,#127811,
#127812,#127813,#127814,#127815,#127816,#127817,#127818,#127819),(#127820,
#127821,#127822,#127823,#127824,#127825,#127826,#127827,#127828,#127829,
#127830,#127831,#127832,#127833,#127834,#127835,#127836,#127837,#127838,
#127839,#127840,#127841,#127842,#127843,#127844,#127845),(#127846,#127847,
#127848,#127849,#127850,#127851,#127852,#127853,#127854,#127855,#127856,
#127857,#127858,#127859,#127860,#127861,#127862,#127863,#127864,#127865,
#127866,#127867,#127868,#127869,#127870,#127871),(#127872,#127873,#127874,
#127875,#127876,#127877,#127878,#127879,#127880,#127881,#127882,#127883,
#127884,#127885,#127886,#127887,#127888,#127889,#127890,#127891,#127892,
#127893,#127894,#127895,#127896,#127897)),.UNSPECIFIED.,.F.,.F.,.F.)
B_SPLINE_SURFACE_WITH_KNOTS((4,3,4),(4,1,1,1,1,1,1,1,1,1,1,1,1,1,1,1,1,
1,1,1,1,1,1,4),(0.,0.5,1.),(0.,0.00338709104151123,0.0292031644766076,0.0596169482905785,
0.0941190289168756,0.132291998012268,0.173832504660512,0.218910698019246,
0.268547982014753,0.323764747156882,0.385760267159764,0.456177213623959,
0.530980523979295,0.603593295594907,0.667945269850854,0.724945053578612,
0.775984643286146,0.822177899369198,0.864653703764676,0.903649038429262,
0.93888404941214,0.969960836451304,0.99638734008221,1.),.UNSPECIFIED.)
GEOMETRIC_REPRESENTATION_ITEM()
RATIONAL_B_SPLINE_SURFACE(((1.193841844068,1.193841844068,1.193841844068,
1.193841844068,1.193841844068,1.193841844068,1.193841844068,1.193841844068,
1.193841844068,1.193841844068,1.193841844068,1.193841844068,1.193841844068,
1.193841844068,1.193841844068,1.193841844068,1.193841844068,1.193841844068,
1.193841844068,1.193841844068,1.193841844068,1.193841844068,1.193841844068,
1.193841844068,1.193841844068,1.193841844068),(0.9353860519774,0.9353860519774,
0.9353860519774,0.9353860519774,0.9353860519774,0.9353860519774,0.9353860519774,
0.9353860519774,0.9353860519774,0.9353860519774,0.9353860519774,0.9353860519774,
0.9353860519774,0.9353860519774,0.9353860519774,0.9353860519774,0.9353860519774,
0.9353860519774,0.9353860519774,0.9353860519774,0.9353860519774,0.9353860519774,
0.9353860519774,0.9353860519774,0.9353860519774,0.9353860519774),(0.9353860519774,
0.9353860519774,0.9353860519774,0.9353860519774,0.9353860519774,0.9353860519774,
0.9353860519774,0.9353860519774,0.9353860519774,0.9353860519774,0.9353860519774,
0.9353860519774,0.9353860519774,0.9353860519774,0.9353860519774,0.9353860519774,
0.9353860519774,0.9353860519774,0.9353860519774,0.9353860519774,0.9353860519774,
0.9353860519774,0.9353860519774,0.9353860519774,0.9353860519774,0.9353860519774),
(1.193841844068,1.193841844068,1.193841844068,1.193841844068,1.193841844068,
1.193841844068,1.193841844068,1.193841844068,1.193841844068,1.193841844068,
1.193841844068,1.193841844068,1.193841844068,1.193841844068,1.193841844068,
1.193841844068,1.193841844068,1.193841844068,1.193841844068,1.193841844068,
1.193841844068,1.193841844068,1.193841844068,1.193841844068,1.193841844068,
1.193841844068),(0.9353860519774,0.9353860519774,0.9353860519774,0.9353860519774,
0.9353860519774,0.9353860519774,0.9353860519774,0.9353860519774,0.9353860519774,
0.9353860519774,0.9353860519774,0.9353860519774,0.9353860519774,0.9353860519774,
0.9353860519774,0.9353860519774,0.9353860519774,0.9353860519774,0.9353860519774,
0.9353860519774,0.9353860519774,0.9353860519774,0.9353860519774,0.9353860519774,
0.9353860519774,0.9353860519774),(0.9353860519774,0.9353860519774,0.9353860519774,
0.9353860519774,0.9353860519774,0.9353860519774,0.9353860519774,0.9353860519774,
0.9353860519774,0.9353860519774,0.9353860519774,0.9353860519774,0.9353860519774,
0.9353860519774,0.9353860519774,0.9353860519774,0.9353860519774,0.9353860519774,
0.9353860519774,0.9353860519774,0.9353860519774,0.9353860519774,0.9353860519774,
0.9353860519774,0.9353860519774,0.9353860519774),(1.193841844068,1.193841844068,
1.193841844068,1.193841844068,1.193841844068,1.193841844068,1.193841844068,
1.193841844068,1.193841844068,1.193841844068,1.193841844068,1.193841844068,
1.193841844068,1.193841844068,1.193841844068,1.193841844068,1.193841844068,
1.193841844068,1.193841844068,1.193841844068,1.193841844068,1.193841844068,
1.193841844068,1.193841844068,1.193841844068,1.193841844068)))
REPRESENTATION_ITEM('')
SURFACE()
);
#2466=(
BOUNDED_SURFACE()
B_SPLINE_SURFACE(3,3,((#127899,#127900,#127901,#127902,#127903,#127904,
#127905,#127906,#127907,#127908),(#127909,#127910,#127911,#127912,#127913,
#127914,#127915,#127916,#127917,#127918),(#127919,#127920,#127921,#127922,
#127923,#127924,#127925,#127926,#127927,#127928),(#127929,#127930,#127931,
#127932,#127933,#127934,#127935,#127936,#127937,#127938),(#127939,#127940,
#127941,#127942,#127943,#127944,#127945,#127946,#127947,#127948),(#127949,
#127950,#127951,#127952,#127953,#127954,#127955,#127956,#127957,#127958),
(#127959,#127960,#127961,#127962,#127963,#127964,#127965,#127966,#127967,
#127968)),.UNSPECIFIED.,.F.,.F.,.F.)
B_SPLINE_SURFACE_WITH_KNOTS((4,3,4),(4,1,1,1,1,1,1,4),(0.,0.5,1.),(0.,0.213585283551531,
0.4054505508447,0.577283027769576,0.731642593504136,0.871393000159704,0.997433614646813,
1.),.UNSPECIFIED.)
GEOMETRIC_REPRESENTATION_ITEM()
RATIONAL_B_SPLINE_SURFACE(((1.201113977633,1.201113977633,1.201113977633,
1.201113977633,1.201113977633,1.201113977633,1.201113977633,1.201113977633,
1.201113977633,1.201113977633),(0.9329620074556,0.9329620074556,0.9329620074556,
0.9329620074556,0.9329620074556,0.9329620074556,0.9329620074556,0.9329620074556,
0.9329620074556,0.9329620074556),(0.9329620074556,0.9329620074556,0.9329620074556,
0.9329620074556,0.9329620074556,0.9329620074556,0.9329620074556,0.9329620074556,
0.9329620074556,0.9329620074556),(1.201113977633,1.201113977633,1.201113977633,
1.201113977633,1.201113977633,1.201113977633,1.201113977633,1.201113977633,
1.201113977633,1.201113977633),(0.9329620074556,0.9329620074556,0.9329620074556,
0.9329620074556,0.9329620074556,0.9329620074556,0.9329620074556,0.9329620074556,
0.9329620074556,0.9329620074556),(0.9329620074556,0.9329620074556,0.9329620074556,
0.9329620074556,0.9329620074556,0.9329620074556,0.9329620074556,0.9329620074556,
0.9329620074556,0.9329620074556),(1.201113977633,1.201113977633,1.201113977633,
1.201113977633,1.201113977633,1.201113977633,1.201113977633,1.201113977633,
1.201113977633,1.201113977633)))
REPRESENTATION_ITEM('')
SURFACE()
);
#2467=(
BOUNDED_SURFACE()
B_SPLINE_SURFACE(3,3,((#127987,#127988,#127989,#127990,#127991,#127992,
#127993,#127994,#127995,#127996,#127997),(#127998,#127999,#128000,#128001,
#128002,#128003,#128004,#128005,#128006,#128007,#128008),(#128009,#128010,
#128011,#128012,#128013,#128014,#128015,#128016,#128017,#128018,#128019),
(#128020,#128021,#128022,#128023,#128024,#128025,#128026,#128027,#128028,
#128029,#128030),(#128031,#128032,#128033,#128034,#128035,#128036,#128037,
#128038,#128039,#128040,#128041),(#128042,#128043,#128044,#128045,#128046,
#128047,#128048,#128049,#128050,#128051,#128052),(#128053,#128054,#128055,
#128056,#128057,#128058,#128059,#128060,#128061,#128062,#128063)),
 .UNSPECIFIED.,.F.,.F.,.F.)
B_SPLINE_SURFACE_WITH_KNOTS((4,3,4),(4,1,1,1,1,1,1,1,4),(0.,0.5,1.),(0.,
0.00181835876594797,0.105491111993237,0.219958345253759,0.345909403004321,
0.484805331232095,0.638614178236773,0.80985054968314,1.),.UNSPECIFIED.)
GEOMETRIC_REPRESENTATION_ITEM()
RATIONAL_B_SPLINE_SURFACE(((1.201132896331,1.201132896331,1.201132896331,
1.201132896331,1.201132896331,1.201132896331,1.201132896331,1.201132896331,
1.201132896331,1.201132896331,1.201132896331),(0.9329557012229,0.9329557012229,
0.9329557012229,0.9329557012229,0.9329557012229,0.9329557012229,0.9329557012229,
0.9329557012229,0.9329557012229,0.9329557012229,0.9329557012229),(0.9329557012229,
0.9329557012229,0.9329557012229,0.9329557012229,0.9329557012229,0.9329557012229,
0.9329557012229,0.9329557012229,0.9329557012229,0.9329557012229,0.9329557012229),
(1.201132896331,1.201132896331,1.201132896331,1.201132896331,1.201132896331,
1.201132896331,1.201132896331,1.201132896331,1.201132896331,1.201132896331,
1.201132896331),(0.9329557012229,0.9329557012229,0.9329557012229,0.9329557012229,
0.9329557012229,0.9329557012229,0.9329557012229,0.9329557012229,0.9329557012229,
0.9329557012229,0.9329557012229),(0.9329557012229,0.9329557012229,0.9329557012229,
0.9329557012229,0.9329557012229,0.9329557012229,0.9329557012229,0.9329557012229,
0.9329557012229,0.9329557012229,0.9329557012229),(1.201132896331,1.201132896331,
1.201132896331,1.201132896331,1.201132896331,1.201132896331,1.201132896331,
1.201132896331,1.201132896331,1.201132896331,1.201132896331)))
REPRESENTATION_ITEM('')
SURFACE()
);
#2468=(
BOUNDED_SURFACE()
B_SPLINE_SURFACE(3,3,((#128065,#128066,#128067,#128068,#128069,#128070,
#128071,#128072,#128073,#128074,#128075,#128076),(#128077,#128078,#128079,
#128080,#128081,#128082,#128083,#128084,#128085,#128086,#128087,#128088),
(#128089,#128090,#128091,#128092,#128093,#128094,#128095,#128096,#128097,
#128098,#128099,#128100),(#128101,#128102,#128103,#128104,#128105,#128106,
#128107,#128108,#128109,#128110,#128111,#128112),(#128113,#128114,#128115,
#128116,#128117,#128118,#128119,#128120,#128121,#128122,#128123,#128124),
(#128125,#128126,#128127,#128128,#128129,#128130,#128131,#128132,#128133,
#128134,#128135,#128136),(#128137,#128138,#128139,#128140,#128141,#128142,
#128143,#128144,#128145,#128146,#128147,#128148)),.UNSPECIFIED.,.F.,.F.,
 .F.)
B_SPLINE_SURFACE_WITH_KNOTS((4,3,4),(4,1,1,1,1,1,1,1,1,4),(0.,0.5,1.),(0.,
0.000255346721705583,0.127238168179912,0.25348490093621,0.379076505598381,
0.504103162940652,0.628662748636027,0.752852442580265,0.876759085909055,
1.),.UNSPECIFIED.)
GEOMETRIC_REPRESENTATION_ITEM()
RATIONAL_B_SPLINE_SURFACE(((1.193842470635,1.193842470635,1.193842470635,
1.193842470635,1.193842470635,1.193842470635,1.193842470635,1.193842470635,
1.193842470635,1.193842470635,1.193842470635,1.193842470635),(0.9353858431218,
0.9353858431218,0.9353858431218,0.9353858431218,0.9353858431218,0.9353858431218,
0.9353858431218,0.9353858431218,0.9353858431218,0.9353858431218,0.9353858431218,
0.9353858431218),(0.9353858431218,0.9353858431218,0.9353858431218,0.9353858431218,
0.9353858431218,0.9353858431218,0.9353858431218,0.9353858431218,0.9353858431218,
0.9353858431218,0.9353858431218,0.9353858431218),(1.193842470635,1.193842470635,
1.193842470635,1.193842470635,1.193842470635,1.193842470635,1.193842470635,
1.193842470635,1.193842470635,1.193842470635,1.193842470635,1.193842470635),
(0.9353858431218,0.9353858431218,0.9353858431218,0.9353858431218,0.9353858431218,
0.9353858431218,0.9353858431218,0.9353858431218,0.9353858431218,0.9353858431218,
0.9353858431218,0.9353858431218),(0.9353858431218,0.9353858431218,0.9353858431218,
0.9353858431218,0.9353858431218,0.9353858431218,0.9353858431218,0.9353858431218,
0.9353858431218,0.9353858431218,0.9353858431218,0.9353858431218),(1.193842470635,
1.193842470635,1.193842470635,1.193842470635,1.193842470635,1.193842470635,
1.193842470635,1.193842470635,1.193842470635,1.193842470635,1.193842470635,
1.193842470635)))
REPRESENTATION_ITEM('')
SURFACE()
);
#2469=(
BOUNDED_SURFACE()
B_SPLINE_SURFACE(3,3,((#128150,#128151,#128152,#128153,#128154,#128155,
#128156,#128157,#128158,#128159,#128160,#128161,#128162,#128163,#128164,
#128165,#128166,#128167,#128168,#128169),(#128170,#128171,#128172,#128173,
#128174,#128175,#128176,#128177,#128178,#128179,#128180,#128181,#128182,
#128183,#128184,#128185,#128186,#128187,#128188,#128189),(#128190,#128191,
#128192,#128193,#128194,#128195,#128196,#128197,#128198,#128199,#128200,
#128201,#128202,#128203,#128204,#128205,#128206,#128207,#128208,#128209),
(#128210,#128211,#128212,#128213,#128214,#128215,#128216,#128217,#128218,
#128219,#128220,#128221,#128222,#128223,#128224,#128225,#128226,#128227,
#128228,#128229),(#128230,#128231,#128232,#128233,#128234,#128235,#128236,
#128237,#128238,#128239,#128240,#128241,#128242,#128243,#128244,#128245,
#128246,#128247,#128248,#128249),(#128250,#128251,#128252,#128253,#128254,
#128255,#128256,#128257,#128258,#128259,#128260,#128261,#128262,#128263,
#128264,#128265,#128266,#128267,#128268,#128269),(#128270,#128271,#128272,
#128273,#128274,#128275,#128276,#128277,#128278,#128279,#128280,#128281,
#128282,#128283,#128284,#128285,#128286,#128287,#128288,#128289)),
 .UNSPECIFIED.,.F.,.F.,.F.)
B_SPLINE_SURFACE_WITH_KNOTS((4,3,4),(4,1,1,1,1,1,1,1,1,1,1,1,1,1,1,1,1,
4),(0.,0.5,1.),(0.,0.0489590947384862,0.106545697307053,0.169926417435894,
0.240019733012254,0.317744348497442,0.399711066482656,0.479868307731546,
0.557020357792415,0.630152704112907,0.698243580475678,0.760671732039233,
0.81767991258728,0.869583135240796,0.916669699502804,0.959206322109519,
0.997448988846953,1.),.UNSPECIFIED.)
GEOMETRIC_REPRESENTATION_ITEM()
RATIONAL_B_SPLINE_SURFACE(((1.182965384822,1.182965384822,1.182965384822,
1.182965384822,1.182965384822,1.182965384822,1.182965384822,1.182965384822,
1.182965384822,1.182965384822,1.182965384822,1.182965384822,1.182965384822,
1.182965384822,1.182965384822,1.182965384822,1.182965384822,1.182965384822,
1.182965384822,1.182965384822),(0.9390115383926,0.9390115383926,0.9390115383926,
0.9390115383926,0.9390115383926,0.9390115383926,0.9390115383926,0.9390115383926,
0.9390115383926,0.9390115383926,0.9390115383926,0.9390115383926,0.9390115383926,
0.9390115383926,0.9390115383926,0.9390115383926,0.9390115383926,0.9390115383926,
0.9390115383926,0.9390115383926),(0.9390115383926,0.9390115383926,0.9390115383926,
0.9390115383926,0.9390115383926,0.9390115383926,0.9390115383926,0.9390115383926,
0.9390115383926,0.9390115383926,0.9390115383926,0.9390115383926,0.9390115383926,
0.9390115383926,0.9390115383926,0.9390115383926,0.9390115383926,0.9390115383926,
0.9390115383926,0.9390115383926),(1.182965384822,1.182965384822,1.182965384822,
1.182965384822,1.182965384822,1.182965384822,1.182965384822,1.182965384822,
1.182965384822,1.182965384822,1.182965384822,1.182965384822,1.182965384822,
1.182965384822,1.182965384822,1.182965384822,1.182965384822,1.182965384822,
1.182965384822,1.182965384822),(0.9390115383926,0.9390115383926,0.9390115383926,
0.9390115383926,0.9390115383926,0.9390115383926,0.9390115383926,0.9390115383926,
0.9390115383926,0.9390115383926,0.9390115383926,0.9390115383926,0.9390115383926,
0.9390115383926,0.9390115383926,0.9390115383926,0.9390115383926,0.9390115383926,
0.9390115383926,0.9390115383926),(0.9390115383926,0.9390115383926,0.9390115383926,
0.9390115383926,0.9390115383926,0.9390115383926,0.9390115383926,0.9390115383926,
0.9390115383926,0.9390115383926,0.9390115383926,0.9390115383926,0.9390115383926,
0.9390115383926,0.9390115383926,0.9390115383926,0.9390115383926,0.9390115383926,
0.9390115383926,0.9390115383926),(1.182965384822,1.182965384822,1.182965384822,
1.182965384822,1.182965384822,1.182965384822,1.182965384822,1.182965384822,
1.182965384822,1.182965384822,1.182965384822,1.182965384822,1.182965384822,
1.182965384822,1.182965384822,1.182965384822,1.182965384822,1.182965384822,
1.182965384822,1.182965384822)))
REPRESENTATION_ITEM('')
SURFACE()
);
#2470=(
BOUNDED_SURFACE()
B_SPLINE_SURFACE(3,3,((#128308,#128309,#128310,#128311,#128312,#128313,
#128314,#128315,#128316,#128317,#128318,#128319,#128320,#128321,#128322,
#128323,#128324,#128325,#128326),(#128327,#128328,#128329,#128330,#128331,
#128332,#128333,#128334,#128335,#128336,#128337,#128338,#128339,#128340,
#128341,#128342,#128343,#128344,#128345),(#128346,#128347,#128348,#128349,
#128350,#128351,#128352,#128353,#128354,#128355,#128356,#128357,#128358,
#128359,#128360,#128361,#128362,#128363,#128364),(#128365,#128366,#128367,
#128368,#128369,#128370,#128371,#128372,#128373,#128374,#128375,#128376,
#128377,#128378,#128379,#128380,#128381,#128382,#128383),(#128384,#128385,
#128386,#128387,#128388,#128389,#128390,#128391,#128392,#128393,#128394,
#128395,#128396,#128397,#128398,#128399,#128400,#128401,#128402),(#128403,
#128404,#128405,#128406,#128407,#128408,#128409,#128410,#128411,#128412,
#128413,#128414,#128415,#128416,#128417,#128418,#128419,#128420,#128421),
(#128422,#128423,#128424,#128425,#128426,#128427,#128428,#128429,#128430,
#128431,#128432,#128433,#128434,#128435,#128436,#128437,#128438,#128439,
#128440)),.UNSPECIFIED.,.F.,.F.,.F.)
B_SPLINE_SURFACE_WITH_KNOTS((4,3,4),(4,1,1,1,1,1,1,1,1,1,1,1,1,1,1,1,4),
(0.,0.5,1.),(0.,0.00198169918793633,0.0506821482100691,0.105488478666356,
0.16376961522165,0.222938538024466,0.281407831568016,0.339150728322178,
0.397207423178538,0.457726780737408,0.522920886388937,0.594978378611854,
0.675924491902483,0.762809530116442,0.849642958155992,0.931396381678324,
1.),.UNSPECIFIED.)
GEOMETRIC_REPRESENTATION_ITEM()
RATIONAL_B_SPLINE_SURFACE(((1.18298561069,1.18298561069,1.18298561069,1.18298561069,
1.18298561069,1.18298561069,1.18298561069,1.18298561069,1.18298561069,1.18298561069,
1.18298561069,1.18298561069,1.18298561069,1.18298561069,1.18298561069,1.18298561069,
1.18298561069,1.18298561069,1.18298561069),(0.9390047964366,0.9390047964366,
0.9390047964366,0.9390047964366,0.9390047964366,0.9390047964366,0.9390047964366,
0.9390047964366,0.9390047964366,0.9390047964366,0.9390047964366,0.9390047964366,
0.9390047964366,0.9390047964366,0.9390047964366,0.9390047964366,0.9390047964366,
0.9390047964366,0.9390047964366),(0.9390047964366,0.9390047964366,0.9390047964366,
0.9390047964366,0.9390047964366,0.9390047964366,0.9390047964366,0.9390047964366,
0.9390047964366,0.9390047964366,0.9390047964366,0.9390047964366,0.9390047964366,
0.9390047964366,0.9390047964366,0.9390047964366,0.9390047964366,0.9390047964366,
0.9390047964366),(1.18298561069,1.18298561069,1.18298561069,1.18298561069,
1.18298561069,1.18298561069,1.18298561069,1.18298561069,1.18298561069,1.18298561069,
1.18298561069,1.18298561069,1.18298561069,1.18298561069,1.18298561069,1.18298561069,
1.18298561069,1.18298561069,1.18298561069),(0.9390047964366,0.9390047964366,
0.9390047964366,0.9390047964366,0.9390047964366,0.9390047964366,0.9390047964366,
0.9390047964366,0.9390047964366,0.9390047964366,0.9390047964366,0.9390047964366,
0.9390047964366,0.9390047964366,0.9390047964366,0.9390047964366,0.9390047964366,
0.9390047964366,0.9390047964366),(0.9390047964366,0.9390047964366,0.9390047964366,
0.9390047964366,0.9390047964366,0.9390047964366,0.9390047964366,0.9390047964366,
0.9390047964366,0.9390047964366,0.9390047964366,0.9390047964366,0.9390047964366,
0.9390047964366,0.9390047964366,0.9390047964366,0.9390047964366,0.9390047964366,
0.9390047964366),(1.18298561069,1.18298561069,1.18298561069,1.18298561069,
1.18298561069,1.18298561069,1.18298561069,1.18298561069,1.18298561069,1.18298561069,
1.18298561069,1.18298561069,1.18298561069,1.18298561069,1.18298561069,1.18298561069,
1.18298561069,1.18298561069,1.18298561069)))
REPRESENTATION_ITEM('')
SURFACE()
);
#2471=(
BOUNDED_SURFACE()
B_SPLINE_SURFACE(3,3,((#128523,#128524,#128525,#128526,#128527,#128528,
#128529,#128530,#128531,#128532,#128533,#128534),(#128535,#128536,#128537,
#128538,#128539,#128540,#128541,#128542,#128543,#128544,#128545,#128546),
(#128547,#128548,#128549,#128550,#128551,#128552,#128553,#128554,#128555,
#128556,#128557,#128558),(#128559,#128560,#128561,#128562,#128563,#128564,
#128565,#128566,#128567,#128568,#128569,#128570),(#128571,#128572,#128573,
#128574,#128575,#128576,#128577,#128578,#128579,#128580,#128581,#128582),
(#128583,#128584,#128585,#128586,#128587,#128588,#128589,#128590,#128591,
#128592,#128593,#128594),(#128595,#128596,#128597,#128598,#128599,#128600,
#128601,#128602,#128603,#128604,#128605,#128606)),.UNSPECIFIED.,.F.,.F.,
 .F.)
B_SPLINE_SURFACE_WITH_KNOTS((4,3,4),(4,1,1,1,1,1,1,1,1,4),(0.,0.5,1.),(0.,
0.121564102375813,0.245468926981195,0.369653809053026,0.494206194236183,
0.619223276452004,0.744802842314215,0.871034840780298,0.998000117655881,
1.),.UNSPECIFIED.)
GEOMETRIC_REPRESENTATION_ITEM()
RATIONAL_B_SPLINE_SURFACE(((1.193853494575,1.193853494575,1.193853494575,
1.193853494575,1.193853494575,1.193853494575,1.193853494575,1.193853494575,
1.193853494575,1.193853494575,1.193853494575,1.193853494575),(0.9353821684751,
0.9353821684751,0.9353821684751,0.9353821684751,0.9353821684751,0.9353821684751,
0.9353821684751,0.9353821684751,0.9353821684751,0.9353821684751,0.9353821684751,
0.9353821684751),(0.9353821684751,0.9353821684751,0.9353821684751,0.9353821684751,
0.9353821684751,0.9353821684751,0.9353821684751,0.9353821684751,0.9353821684751,
0.9353821684751,0.9353821684751,0.9353821684751),(1.193853494575,1.193853494575,
1.193853494575,1.193853494575,1.193853494575,1.193853494575,1.193853494575,
1.193853494575,1.193853494575,1.193853494575,1.193853494575,1.193853494575),
(0.9353821684751,0.9353821684751,0.9353821684751,0.9353821684751,0.9353821684751,
0.9353821684751,0.9353821684751,0.9353821684751,0.9353821684751,0.9353821684751,
0.9353821684751,0.9353821684751),(0.9353821684751,0.9353821684751,0.9353821684751,
0.9353821684751,0.9353821684751,0.9353821684751,0.9353821684751,0.9353821684751,
0.9353821684751,0.9353821684751,0.9353821684751,0.9353821684751),(1.193853494575,
1.193853494575,1.193853494575,1.193853494575,1.193853494575,1.193853494575,
1.193853494575,1.193853494575,1.193853494575,1.193853494575,1.193853494575,
1.193853494575)))
REPRESENTATION_ITEM('')
SURFACE()
);
#2472=(
BOUNDED_SURFACE()
B_SPLINE_SURFACE(3,3,((#130378,#130379,#130380,#130381,#130382),(#130383,
#130384,#130385,#130386,#130387),(#130388,#130389,#130390,#130391,#130392),
(#130393,#130394,#130395,#130396,#130397)),.UNSPECIFIED.,.F.,.F.,.F.)
B_SPLINE_SURFACE_WITH_KNOTS((4,4),(4,1,4),(0.,1.),(0.,0.0723197122150453,
1.),.UNSPECIFIED.)
GEOMETRIC_REPRESENTATION_ITEM()
RATIONAL_B_SPLINE_SURFACE(((1.229651833258,1.229651833258,1.229651833258,
1.229651833258,1.229651833258),(0.9234493889141,0.9234493889141,0.9234493889141,
0.9234493889141,0.9234493889141),(0.9234493889141,0.9234493889141,0.9234493889141,
0.9234493889141,0.9234493889141),(1.229651833258,1.229651833258,1.229651833258,
1.229651833258,1.229651833258)))
REPRESENTATION_ITEM('')
SURFACE()
);
#2473=(
BOUNDED_SURFACE()
B_SPLINE_SURFACE(3,3,((#130463,#130464,#130465,#130466,#130467,#130468,
#130469,#130470,#130471,#130472,#130473,#130474,#130475,#130476,#130477,
#130478,#130479,#130480,#130481,#130482),(#130483,#130484,#130485,#130486,
#130487,#130488,#130489,#130490,#130491,#130492,#130493,#130494,#130495,
#130496,#130497,#130498,#130499,#130500,#130501,#130502),(#130503,#130504,
#130505,#130506,#130507,#130508,#130509,#130510,#130511,#130512,#130513,
#130514,#130515,#130516,#130517,#130518,#130519,#130520,#130521,#130522),
(#130523,#130524,#130525,#130526,#130527,#130528,#130529,#130530,#130531,
#130532,#130533,#130534,#130535,#130536,#130537,#130538,#130539,#130540,
#130541,#130542)),.UNSPECIFIED.,.F.,.F.,.F.)
B_SPLINE_SURFACE_WITH_KNOTS((4,4),(4,1,1,1,1,1,1,1,1,1,1,1,1,1,1,1,1,4),
(0.,1.),(0.,0.0396611801962909,0.0991280080993822,0.158967060305227,0.213500355613908,
0.265743805592041,0.31877970559442,0.372320929804579,0.42550049560743,0.477326879186013,
0.531755535132276,0.594383860510548,0.661759309442457,0.728996536779342,
0.791903310438717,0.857857310969531,0.931521029517504,1.),.UNSPECIFIED.)
GEOMETRIC_REPRESENTATION_ITEM()
RATIONAL_B_SPLINE_SURFACE(((1.186027134151,1.186027134151,1.186027134151,
1.186027134151,1.186027134151,1.186027134151,1.186027134151,1.186027134151,
1.186027134151,1.186027134151,1.186027134151,1.186027134151,1.186027134151,
1.186027134151,1.186027134151,1.186027134151,1.186027134151,1.186027134151,
1.186027134151,1.186027134151),(0.9379909552829,0.9379909552829,0.9379909552829,
0.9379909552829,0.9379909552829,0.9379909552829,0.9379909552829,0.9379909552829,
0.9379909552829,0.9379909552829,0.9379909552829,0.9379909552829,0.9379909552829,
0.9379909552829,0.9379909552829,0.9379909552829,0.9379909552829,0.9379909552829,
0.9379909552829,0.9379909552829),(0.9379909552829,0.9379909552829,0.9379909552829,
0.9379909552829,0.9379909552829,0.9379909552829,0.9379909552829,0.9379909552829,
0.9379909552829,0.9379909552829,0.9379909552829,0.9379909552829,0.9379909552829,
0.9379909552829,0.9379909552829,0.9379909552829,0.9379909552829,0.9379909552829,
0.9379909552829,0.9379909552829),(1.186027134151,1.186027134151,1.186027134151,
1.186027134151,1.186027134151,1.186027134151,1.186027134151,1.186027134151,
1.186027134151,1.186027134151,1.186027134151,1.186027134151,1.186027134151,
1.186027134151,1.186027134151,1.186027134151,1.186027134151,1.186027134151,
1.186027134151,1.186027134151)))
REPRESENTATION_ITEM('')
SURFACE()
);
#2474=(
BOUNDED_SURFACE()
B_SPLINE_SURFACE(3,3,((#131452,#131453,#131454,#131455,#131456,#131457,
#131458,#131459,#131460,#131461,#131462,#131463,#131464,#131465,#131466,
#131467,#131468,#131469),(#131470,#131471,#131472,#131473,#131474,#131475,
#131476,#131477,#131478,#131479,#131480,#131481,#131482,#131483,#131484,
#131485,#131486,#131487),(#131488,#131489,#131490,#131491,#131492,#131493,
#131494,#131495,#131496,#131497,#131498,#131499,#131500,#131501,#131502,
#131503,#131504,#131505),(#131506,#131507,#131508,#131509,#131510,#131511,
#131512,#131513,#131514,#131515,#131516,#131517,#131518,#131519,#131520,
#131521,#131522,#131523)),.UNSPECIFIED.,.F.,.F.,.F.)
B_SPLINE_SURFACE_WITH_KNOTS((4,4),(4,1,1,1,1,1,1,1,1,1,1,1,1,1,1,4),(0.,
1.),(0.,0.0565664707614419,0.138737193301063,0.216966583065079,0.292764930742884,
0.367550058790166,0.442396912571936,0.51714275336354,0.591290850026512,
0.664372024038177,0.735878178033487,0.805267355840292,0.8719728304485,0.935407611159442,
0.994981558271123,1.),.UNSPECIFIED.)
GEOMETRIC_REPRESENTATION_ITEM()
RATIONAL_B_SPLINE_SURFACE(((1.117361802752,1.117361802752,1.117361802752,
1.117361802752,1.117361802752,1.117361802752,1.117361802752,1.117361802752,
1.117361802752,1.117361802752,1.117361802752,1.117361802752,1.117361802752,
1.117361802752,1.117361802752,1.117361802752,1.117361802752,1.117361802752),
(0.9608793990826,0.9608793990826,0.9608793990826,0.9608793990826,0.9608793990826,
0.9608793990826,0.9608793990826,0.9608793990826,0.9608793990826,0.9608793990826,
0.9608793990826,0.9608793990826,0.9608793990826,0.9608793990826,0.9608793990826,
0.9608793990826,0.9608793990826,0.9608793990826),(0.9608793990826,0.9608793990826,
0.9608793990826,0.9608793990826,0.9608793990826,0.9608793990826,0.9608793990826,
0.9608793990826,0.9608793990826,0.9608793990826,0.9608793990826,0.9608793990826,
0.9608793990826,0.9608793990826,0.9608793990826,0.9608793990826,0.9608793990826,
0.9608793990826),(1.117361802752,1.117361802752,1.117361802752,1.117361802752,
1.117361802752,1.117361802752,1.117361802752,1.117361802752,1.117361802752,
1.117361802752,1.117361802752,1.117361802752,1.117361802752,1.117361802752,
1.117361802752,1.117361802752,1.117361802752,1.117361802752)))
REPRESENTATION_ITEM('')
SURFACE()
);
#2475=(
BOUNDED_SURFACE()
B_SPLINE_SURFACE(3,3,((#131671,#131672,#131673,#131674,#131675,#131676,
#131677,#131678,#131679,#131680,#131681,#131682,#131683,#131684,#131685),
(#131686,#131687,#131688,#131689,#131690,#131691,#131692,#131693,#131694,
#131695,#131696,#131697,#131698,#131699,#131700),(#131701,#131702,#131703,
#131704,#131705,#131706,#131707,#131708,#131709,#131710,#131711,#131712,
#131713,#131714,#131715),(#131716,#131717,#131718,#131719,#131720,#131721,
#131722,#131723,#131724,#131725,#131726,#131727,#131728,#131729,#131730)),
 .UNSPECIFIED.,.F.,.F.,.F.)
B_SPLINE_SURFACE_WITH_KNOTS((4,4),(4,1,1,1,1,1,1,1,1,1,1,1,4),(0.,1.),(0.,
0.00433344281298221,0.0666934882632817,0.132801776489929,0.205016366496403,
0.284357715917161,0.370665202265106,0.46484948769096,0.568277692564041,
0.682614773264253,0.810064514841178,0.952973196107536,1.),.UNSPECIFIED.)
GEOMETRIC_REPRESENTATION_ITEM()
RATIONAL_B_SPLINE_SURFACE(((1.116717554521,1.116717554521,1.116717554521,
1.116717554521,1.116717554521,1.116717554521,1.116717554521,1.116717554521,
1.116717554521,1.116717554521,1.116717554521,1.116717554521,1.116717554521,
1.116717554521,1.116717554521),(0.9610941484931,0.9610941484931,0.9610941484931,
0.9610941484931,0.9610941484931,0.9610941484931,0.9610941484931,0.9610941484931,
0.9610941484931,0.9610941484931,0.9610941484931,0.9610941484931,0.9610941484931,
0.9610941484931,0.9610941484931),(0.9610941484931,0.9610941484931,0.9610941484931,
0.9610941484931,0.9610941484931,0.9610941484931,0.9610941484931,0.9610941484931,
0.9610941484931,0.9610941484931,0.9610941484931,0.9610941484931,0.9610941484931,
0.9610941484931,0.9610941484931),(1.116717554521,1.116717554521,1.116717554521,
1.116717554521,1.116717554521,1.116717554521,1.116717554521,1.116717554521,
1.116717554521,1.116717554521,1.116717554521,1.116717554521,1.116717554521,
1.116717554521,1.116717554521)))
REPRESENTATION_ITEM('')
SURFACE()
);
#2476=(
BOUNDED_SURFACE()
B_SPLINE_SURFACE(3,3,((#131768,#131769,#131770,#131771),(#131772,#131773,
#131774,#131775),(#131776,#131777,#131778,#131779),(#131780,#131781,#131782,
#131783)),.UNSPECIFIED.,.F.,.F.,.F.)
B_SPLINE_SURFACE_WITH_KNOTS((4,4),(4,4),(0.,1.),(0.,1.),.UNSPECIFIED.)
GEOMETRIC_REPRESENTATION_ITEM()
RATIONAL_B_SPLINE_SURFACE(((1.1173473569,1.1173473569,1.1173473569,1.1173473569),
(0.9608842143667,0.9608842143667,0.9608842143667,0.9608842143667),(0.9608842143667,
0.9608842143667,0.9608842143667,0.9608842143667),(1.1173473569,1.1173473569,
1.1173473569,1.1173473569)))
REPRESENTATION_ITEM('')
SURFACE()
);
#2477=(
BOUNDED_SURFACE()
B_SPLINE_SURFACE(3,3,((#131784,#131785,#131786,#131787,#131788,#131789,
#131790,#131791,#131792,#131793,#131794,#131795,#131796,#131797,#131798,
#131799,#131800,#131801,#131802,#131803),(#131804,#131805,#131806,#131807,
#131808,#131809,#131810,#131811,#131812,#131813,#131814,#131815,#131816,
#131817,#131818,#131819,#131820,#131821,#131822,#131823),(#131824,#131825,
#131826,#131827,#131828,#131829,#131830,#131831,#131832,#131833,#131834,
#131835,#131836,#131837,#131838,#131839,#131840,#131841,#131842,#131843),
(#131844,#131845,#131846,#131847,#131848,#131849,#131850,#131851,#131852,
#131853,#131854,#131855,#131856,#131857,#131858,#131859,#131860,#131861,
#131862,#131863)),.UNSPECIFIED.,.F.,.F.,.F.)
B_SPLINE_SURFACE_WITH_KNOTS((4,4),(4,1,1,1,1,1,1,1,1,1,1,1,1,1,1,1,1,4),
(0.,1.),(0.,0.0634473073458767,0.137474475480583,0.203439315591922,0.266070813426101,
0.333494447777073,0.401437472430427,0.464401084256882,0.51858368764375,
0.569769560865856,0.622221496328389,0.67514181525029,0.727526446084146,
0.778774499915783,0.832231436034466,0.891640084181608,0.951727885385323,
1.),.UNSPECIFIED.)
GEOMETRIC_REPRESENTATION_ITEM()
RATIONAL_B_SPLINE_SURFACE(((1.186029185783,1.186029185783,1.186029185783,
1.186029185783,1.186029185783,1.186029185783,1.186029185783,1.186029185783,
1.186029185783,1.186029185783,1.186029185783,1.186029185783,1.186029185783,
1.186029185783,1.186029185783,1.186029185783,1.186029185783,1.186029185783,
1.186029185783,1.186029185783),(0.9379902714058,0.9379902714058,0.9379902714058,
0.9379902714058,0.9379902714058,0.9379902714058,0.9379902714058,0.9379902714058,
0.9379902714058,0.9379902714058,0.9379902714058,0.9379902714058,0.9379902714058,
0.9379902714058,0.9379902714058,0.9379902714058,0.9379902714058,0.9379902714058,
0.9379902714058,0.9379902714058),(0.9379902714058,0.9379902714058,0.9379902714058,
0.9379902714058,0.9379902714058,0.9379902714058,0.9379902714058,0.9379902714058,
0.9379902714058,0.9379902714058,0.9379902714058,0.9379902714058,0.9379902714058,
0.9379902714058,0.9379902714058,0.9379902714058,0.9379902714058,0.9379902714058,
0.9379902714058,0.9379902714058),(1.186029185783,1.186029185783,1.186029185783,
1.186029185783,1.186029185783,1.186029185783,1.186029185783,1.186029185783,
1.186029185783,1.186029185783,1.186029185783,1.186029185783,1.186029185783,
1.186029185783,1.186029185783,1.186029185783,1.186029185783,1.186029185783,
1.186029185783,1.186029185783)))
REPRESENTATION_ITEM('')
SURFACE()
);
#2478=(
BOUNDED_SURFACE()
B_SPLINE_SURFACE(3,3,((#131894,#131895,#131896,#131897,#131898,#131899,
#131900,#131901,#131902,#131903,#131904,#131905,#131906,#131907),(#131908,
#131909,#131910,#131911,#131912,#131913,#131914,#131915,#131916,#131917,
#131918,#131919,#131920,#131921),(#131922,#131923,#131924,#131925,#131926,
#131927,#131928,#131929,#131930,#131931,#131932,#131933,#131934,#131935),
(#131936,#131937,#131938,#131939,#131940,#131941,#131942,#131943,#131944,
#131945,#131946,#131947,#131948,#131949)),.UNSPECIFIED.,.F.,.F.,.F.)
B_SPLINE_SURFACE_WITH_KNOTS((4,4),(4,1,1,1,1,1,1,1,1,1,1,4),(0.,1.),(0.,
0.025958376473271,0.179859171762141,0.318182203672271,0.441108132212019,
0.551634708740777,0.651710515506557,0.743010369069283,0.826230829945666,
0.901572688650554,0.970015580606343,1.),.UNSPECIFIED.)
GEOMETRIC_REPRESENTATION_ITEM()
RATIONAL_B_SPLINE_SURFACE(((1.116719050321,1.116719050321,1.116719050321,
1.116719050321,1.116719050321,1.116719050321,1.116719050321,1.116719050321,
1.116719050321,1.116719050321,1.116719050321,1.116719050321,1.116719050321,
1.116719050321),(0.961093649893,0.961093649893,0.961093649893,0.961093649893,
0.961093649893,0.961093649893,0.961093649893,0.961093649893,0.961093649893,
0.961093649893,0.961093649893,0.961093649893,0.961093649893,0.961093649893),
(0.961093649893,0.961093649893,0.961093649893,0.961093649893,0.961093649893,
0.961093649893,0.961093649893,0.961093649893,0.961093649893,0.961093649893,
0.961093649893,0.961093649893,0.961093649893,0.961093649893),(1.116719050321,
1.116719050321,1.116719050321,1.116719050321,1.116719050321,1.116719050321,
1.116719050321,1.116719050321,1.116719050321,1.116719050321,1.116719050321,
1.116719050321,1.116719050321,1.116719050321)))
REPRESENTATION_ITEM('')
SURFACE()
);
#2479=(
BOUNDED_SURFACE()
B_SPLINE_SURFACE(3,3,((#131951,#131952,#131953,#131954),(#131955,#131956,
#131957,#131958),(#131959,#131960,#131961,#131962),(#131963,#131964,#131965,
#131966)),.UNSPECIFIED.,.F.,.F.,.F.)
B_SPLINE_SURFACE_WITH_KNOTS((4,4),(4,4),(0.,1.),(0.,1.),.UNSPECIFIED.)
GEOMETRIC_REPRESENTATION_ITEM()
RATIONAL_B_SPLINE_SURFACE(((1.117354081969,1.117354081969,1.117354081969,
1.117354081969),(0.9608819726769,0.9608819726769,0.9608819726769,0.9608819726769),
(0.9608819726769,0.9608819726769,0.9608819726769,0.9608819726769),(1.117354081969,
1.117354081969,1.117354081969,1.117354081969)))
REPRESENTATION_ITEM('')
SURFACE()
);
#2480=(
BOUNDED_SURFACE()
B_SPLINE_SURFACE(3,3,((#131977,#131978,#131979,#131980,#131981,#131982,
#131983,#131984,#131985,#131986,#131987,#131988,#131989,#131990,#131991,
#131992,#131993,#131994),(#131995,#131996,#131997,#131998,#131999,#132000,
#132001,#132002,#132003,#132004,#132005,#132006,#132007,#132008,#132009,
#132010,#132011,#132012),(#132013,#132014,#132015,#132016,#132017,#132018,
#132019,#132020,#132021,#132022,#132023,#132024,#132025,#132026,#132027,
#132028,#132029,#132030),(#132031,#132032,#132033,#132034,#132035,#132036,
#132037,#132038,#132039,#132040,#132041,#132042,#132043,#132044,#132045,
#132046,#132047,#132048)),.UNSPECIFIED.,.F.,.F.,.F.)
B_SPLINE_SURFACE_WITH_KNOTS((4,4),(4,1,1,1,1,1,1,1,1,1,1,1,1,1,1,4),(0.,
1.),(0.,0.000242963129974397,0.0605980029967337,0.126012042753347,0.195352701343378,
0.267486808827858,0.341302963992409,0.415716209072041,0.489674476326956,
0.56246465276733,0.634611827570827,0.706994977225878,0.780514441156784,
0.856110535001656,0.934799701636564,1.),.UNSPECIFIED.)
GEOMETRIC_REPRESENTATION_ITEM()
RATIONAL_B_SPLINE_SURFACE(((1.117353920691,1.117353920691,1.117353920691,
1.117353920691,1.117353920691,1.117353920691,1.117353920691,1.117353920691,
1.117353920691,1.117353920691,1.117353920691,1.117353920691,1.117353920691,
1.117353920691,1.117353920691,1.117353920691,1.117353920691,1.117353920691),
(0.9608820264364,0.9608820264364,0.9608820264364,0.9608820264364,0.9608820264364,
0.9608820264364,0.9608820264364,0.9608820264364,0.9608820264364,0.9608820264364,
0.9608820264364,0.9608820264364,0.9608820264364,0.9608820264364,0.9608820264364,
0.9608820264364,0.9608820264364,0.9608820264364),(0.9608820264364,0.9608820264364,
0.9608820264364,0.9608820264364,0.9608820264364,0.9608820264364,0.9608820264364,
0.9608820264364,0.9608820264364,0.9608820264364,0.9608820264364,0.9608820264364,
0.9608820264364,0.9608820264364,0.9608820264364,0.9608820264364,0.9608820264364,
0.9608820264364),(1.117353920691,1.117353920691,1.117353920691,1.117353920691,
1.117353920691,1.117353920691,1.117353920691,1.117353920691,1.117353920691,
1.117353920691,1.117353920691,1.117353920691,1.117353920691,1.117353920691,
1.117353920691,1.117353920691,1.117353920691,1.117353920691)))
REPRESENTATION_ITEM('')
SURFACE()
);
#2481=(
BOUNDED_SURFACE()
B_SPLINE_SURFACE(3,3,((#132299,#132300,#132301,#132302,#132303,#132304,
#132305,#132306),(#132307,#132308,#132309,#132310,#132311,#132312,#132313,
#132314),(#132315,#132316,#132317,#132318,#132319,#132320,#132321,#132322),
(#132323,#132324,#132325,#132326,#132327,#132328,#132329,#132330)),
 .UNSPECIFIED.,.F.,.F.,.F.)
B_SPLINE_SURFACE_WITH_KNOTS((4,4),(4,1,1,1,1,4),(0.,1.),(0.,0.120712626123964,
0.331920437096621,0.562126515133101,0.816265604424358,1.),.UNSPECIFIED.)
GEOMETRIC_REPRESENTATION_ITEM()
RATIONAL_B_SPLINE_SURFACE(((1.229639485543,1.229639485543,1.229639485543,
1.229639485543,1.229639485543,1.229639485543,1.229639485543,1.229639485543),
(0.9234535048188,0.9234535048188,0.9234535048188,0.9234535048188,0.9234535048188,
0.9234535048188,0.9234535048188,0.9234535048188),(0.9234535048188,0.9234535048188,
0.9234535048188,0.9234535048188,0.9234535048188,0.9234535048188,0.9234535048188,
0.9234535048188),(1.229639485543,1.229639485543,1.229639485543,1.229639485543,
1.229639485543,1.229639485543,1.229639485543,1.229639485543)))
REPRESENTATION_ITEM('')
SURFACE()
);
#2482=(
BOUNDED_SURFACE()
B_SPLINE_SURFACE(3,3,((#132549,#132550,#132551,#132552,#132553,#132554,
#132555,#132556,#132557),(#132558,#132559,#132560,#132561,#132562,#132563,
#132564,#132565,#132566),(#132567,#132568,#132569,#132570,#132571,#132572,
#132573,#132574,#132575),(#132576,#132577,#132578,#132579,#132580,#132581,
#132582,#132583,#132584)),.UNSPECIFIED.,.F.,.F.,.F.)
B_SPLINE_SURFACE_WITH_KNOTS((4,4),(4,1,1,1,1,1,4),(0.,1.),(0.,0.0837316477041681,
0.294311209377657,0.486443539434301,0.667285087674737,0.84576890430481,
1.),.UNSPECIFIED.)
GEOMETRIC_REPRESENTATION_ITEM()
RATIONAL_B_SPLINE_SURFACE(((1.00893514375611,1.00893514375611,1.00893514375611,
1.00893514375611,1.00893514375611,1.00893514375611,1.00893514375611,1.00893514375611,
1.00893514375611),(1.01179069517864,1.01179069517864,1.01179069517864,1.01179069517864,
1.01179069517864,1.01179069517864,1.01179069517864,1.01179069517864,1.01179069517864),
(1.01533069338925,1.01533069338925,1.01533069338925,1.01533069338925,1.01533069338925,
1.01533069338925,1.01533069338925,1.01533069338925,1.01533069338925),(1.01955513838796,
1.01955513838796,1.01955513838796,1.01955513838796,1.01955513838796,1.01955513838796,
1.01955513838796,1.01955513838796,1.01955513838796)))
REPRESENTATION_ITEM('')
SURFACE()
);
#2483=(
BOUNDED_SURFACE()
B_SPLINE_SURFACE(3,3,((#132594,#132595,#132596,#132597,#132598,#132599,
#132600,#132601,#132602),(#132603,#132604,#132605,#132606,#132607,#132608,
#132609,#132610,#132611),(#132612,#132613,#132614,#132615,#132616,#132617,
#132618,#132619,#132620),(#132621,#132622,#132623,#132624,#132625,#132626,
#132627,#132628,#132629)),.UNSPECIFIED.,.F.,.F.,.F.)
B_SPLINE_SURFACE_WITH_KNOTS((4,4),(4,1,1,1,1,1,4),(0.,1.),(0.,0.0837316477041681,
0.294311209377657,0.486443539434301,0.667285087674737,0.84576890430481,
1.),.UNSPECIFIED.)
GEOMETRIC_REPRESENTATION_ITEM()
RATIONAL_B_SPLINE_SURFACE(((1.01955513838796,1.01955513838796,1.01955513838796,
1.01955513838796,1.01955513838796,1.01955513838796,1.01955513838796,1.01955513838796,
1.01955513838796),(1.03766231011378,1.03766231011378,1.03766231011378,1.03766231011378,
1.03766231011378,1.03766231011378,1.03766231011378,1.03766231011378,1.03766231011378),
(1.06834429701362,1.06834429701362,1.06834429701362,1.06834429701362,1.06834429701362,
1.06834429701362,1.06834429701362,1.06834429701362,1.06834429701362),(1.11160109908747,
1.11160109908747,1.11160109908747,1.11160109908747,1.11160109908747,1.11160109908747,
1.11160109908747,1.11160109908747,1.11160109908747)))
REPRESENTATION_ITEM('')
SURFACE()
);
#2484=(
BOUNDED_SURFACE()
B_SPLINE_SURFACE(3,3,((#132643,#132644,#132645,#132646,#132647,#132648,
#132649,#132650,#132651,#132652,#132653,#132654,#132655,#132656,#132657,
#132658,#132659,#132660,#132661,#132662,#132663),(#132664,#132665,#132666,
#132667,#132668,#132669,#132670,#132671,#132672,#132673,#132674,#132675,
#132676,#132677,#132678,#132679,#132680,#132681,#132682,#132683,#132684),
(#132685,#132686,#132687,#132688,#132689,#132690,#132691,#132692,#132693,
#132694,#132695,#132696,#132697,#132698,#132699,#132700,#132701,#132702,
#132703,#132704,#132705),(#132706,#132707,#132708,#132709,#132710,#132711,
#132712,#132713,#132714,#132715,#132716,#132717,#132718,#132719,#132720,
#132721,#132722,#132723,#132724,#132725,#132726)),.UNSPECIFIED.,.F.,.F.,
 .F.)
B_SPLINE_SURFACE_WITH_KNOTS((4,4),(4,1,1,1,1,1,1,1,1,1,1,1,1,1,1,1,1,1,
4),(0.,1.),(0.,0.0546624749950295,0.160757685575355,0.256729617165409,0.343735196321369,
0.422731592898268,0.494638559250071,0.560248549174547,0.620252323655667,
0.6753431121518,0.726138185608107,0.772911121896331,0.815853204906754,0.855219379345603,
0.891312858927466,0.92449329904142,0.955123399607878,0.983429063756098,
1.),.UNSPECIFIED.)
GEOMETRIC_REPRESENTATION_ITEM()
RATIONAL_B_SPLINE_SURFACE(((1.11300250285163,1.11300250285163,1.11300250285163,
1.11300250285163,1.11300250285163,1.11300250285163,1.11300250285163,1.11300250285163,
1.11300250285163,1.11300250285163,1.11300250285163,1.11300250285163,1.11300250285163,
1.11300250285163,1.11300250285163,1.11300250285163,1.11300250285163,1.11300250285163,
1.11300250285163,1.11300250285163,1.11300250285163),(1.04579493402343,1.04579493402343,
1.04579493402343,1.04579493402343,1.04579493402343,1.04579493402343,1.04579493402343,
1.04579493402343,1.04579493402343,1.04579493402343,1.04579493402343,1.04579493402343,
1.04579493402343,1.04579493402343,1.04579493402343,1.04579493402343,1.04579493402343,
1.04579493402343,1.04579493402343,1.04579493402343,1.04579493402343),(1.00856584262147,
1.00856584262147,1.00856584262147,1.00856584262147,1.00856584262147,1.00856584262147,
1.00856584262147,1.00856584262147,1.00856584262147,1.00856584262147,1.00856584262147,
1.00856584262147,1.00856584262147,1.00856584262147,1.00856584262147,1.00856584262147,
1.00856584262147,1.00856584262147,1.00856584262147,1.00856584262147,1.00856584262147),
(1.00131522864575,1.00131522864575,1.00131522864575,1.00131522864575,1.00131522864575,
1.00131522864575,1.00131522864575,1.00131522864575,1.00131522864575,1.00131522864575,
1.00131522864575,1.00131522864575,1.00131522864575,1.00131522864575,1.00131522864575,
1.00131522864575,1.00131522864575,1.00131522864575,1.00131522864575,1.00131522864575,
1.00131522864575)))
REPRESENTATION_ITEM('')
SURFACE()
);
#2485=(
BOUNDED_SURFACE()
B_SPLINE_SURFACE(3,3,((#132823,#132824,#132825,#132826,#132827,#132828),
(#132829,#132830,#132831,#132832,#132833,#132834),(#132835,#132836,#132837,
#132838,#132839,#132840),(#132841,#132842,#132843,#132844,#132845,#132846)),
 .UNSPECIFIED.,.F.,.F.,.F.)
B_SPLINE_SURFACE_WITH_KNOTS((4,4),(4,1,1,4),(0.,1.),(0.,0.0270381251289528,
0.669758370381433,1.),.UNSPECIFIED.)
GEOMETRIC_REPRESENTATION_ITEM()
RATIONAL_B_SPLINE_SURFACE(((1.02521912049085,1.02521912049085,1.02521912049085,
1.02521912049085,1.02521912049085,1.02521912049085),(1.01907532458687,1.01907532458687,
1.01907532458687,1.01907532458687,1.01907532458687,1.01907532458687),(1.0140540765962,
1.0140540765962,1.0140540765962,1.0140540765962,1.0140540765962,1.0140540765962),
(1.01015537651883,1.01015537651883,1.01015537651883,1.01015537651883,1.01015537651883,
1.01015537651883)))
REPRESENTATION_ITEM('')
SURFACE()
);
#2486=(
BOUNDED_SURFACE()
B_SPLINE_SURFACE(3,3,((#132883,#132884,#132885,#132886,#132887,#132888,
#132889,#132890),(#132891,#132892,#132893,#132894,#132895,#132896,#132897,
#132898),(#132899,#132900,#132901,#132902,#132903,#132904,#132905,#132906),
(#132907,#132908,#132909,#132910,#132911,#132912,#132913,#132914)),
 .UNSPECIFIED.,.F.,.F.,.F.)
B_SPLINE_SURFACE_WITH_KNOTS((4,4),(4,1,1,1,1,4),(0.,1.),(0.,0.105738953419075,
0.324437351992926,0.56483220773929,0.829287264033599,1.),.UNSPECIFIED.)
GEOMETRIC_REPRESENTATION_ITEM()
RATIONAL_B_SPLINE_SURFACE(((1.01015537651883,1.01015537651883,1.01015537651883,
1.01015537651883,1.01015537651883,1.01015537651883,1.01015537651883,1.01015537651883),
(1.00780920781131,1.00780920781131,1.00780920781131,1.00780920781131,1.00780920781131,
1.00780920781131,1.00780920781131,1.00780920781131),(1.00586956078178,1.00586956078178,
1.00586956078178,1.00586956078178,1.00586956078178,1.00586956078178,1.00586956078178,
1.00586956078178),(1.00433643543025,1.00433643543025,1.00433643543025,1.00433643543025,
1.00433643543025,1.00433643543025,1.00433643543025,1.00433643543025)))
REPRESENTATION_ITEM('')
SURFACE()
);
#2487=(
BOUNDED_SURFACE()
B_SPLINE_SURFACE(3,3,((#132933,#132934,#132935,#132936,#132937,#132938,
#132939,#132940),(#132941,#132942,#132943,#132944,#132945,#132946,#132947,
#132948),(#132949,#132950,#132951,#132952,#132953,#132954,#132955,#132956),
(#132957,#132958,#132959,#132960,#132961,#132962,#132963,#132964)),
 .UNSPECIFIED.,.F.,.F.,.F.)
B_SPLINE_SURFACE_WITH_KNOTS((4,4),(4,1,1,1,1,4),(0.,1.),(0.,0.105738953419075,
0.324437351992926,0.56483220773929,0.829287264033599,1.),.UNSPECIFIED.)
GEOMETRIC_REPRESENTATION_ITEM()
RATIONAL_B_SPLINE_SURFACE(((1.02521912049085,1.02521912049085,1.02521912049085,
1.02521912049085,1.02521912049085,1.02521912049085,1.02521912049085,1.02521912049085),
(1.01907532458687,1.01907532458687,1.01907532458687,1.01907532458687,1.01907532458687,
1.01907532458687,1.01907532458687,1.01907532458687),(1.0140540765962,1.0140540765962,
1.0140540765962,1.0140540765962,1.0140540765962,1.0140540765962,1.0140540765962,
1.0140540765962),(1.01015537651883,1.01015537651883,1.01015537651883,1.01015537651883,
1.01015537651883,1.01015537651883,1.01015537651883,1.01015537651883)))
REPRESENTATION_ITEM('')
SURFACE()
);
#2488=(
BOUNDED_SURFACE()
B_SPLINE_SURFACE(3,3,((#132996,#132997,#132998,#132999,#133000,#133001,
#133002,#133003,#133004,#133005,#133006,#133007,#133008,#133009,#133010,
#133011),(#133012,#133013,#133014,#133015,#133016,#133017,#133018,#133019,
#133020,#133021,#133022,#133023,#133024,#133025,#133026,#133027),(#133028,
#133029,#133030,#133031,#133032,#133033,#133034,#133035,#133036,#133037,
#133038,#133039,#133040,#133041,#133042,#133043),(#133044,#133045,#133046,
#133047,#133048,#133049,#133050,#133051,#133052,#133053,#133054,#133055,
#133056,#133057,#133058,#133059)),.UNSPECIFIED.,.F.,.F.,.F.)
B_SPLINE_SURFACE_WITH_KNOTS((4,4),(4,1,1,1,1,1,1,1,1,1,1,1,1,4),(0.,1.),
(0.,0.0186503236401621,0.0681861826858635,0.122274864726643,0.181134794327188,
0.244976288689619,0.314185121458223,0.389489559305443,0.47162927932211,
0.561313355930194,0.659220518921088,0.766025144246682,0.882569333512905,
1.),.UNSPECIFIED.)
GEOMETRIC_REPRESENTATION_ITEM()
RATIONAL_B_SPLINE_SURFACE(((1.00001053115096,1.00001053115096,1.00001053115096,
1.00001053115096,1.00001053115096,1.00001053115096,1.00001053115096,1.00001053115096,
1.00001053115096,1.00001053115096,1.00001053115096,1.00001053115096,1.00001053115096,
1.00001053115096,1.00001053115096,1.00001053115096),(0.999657107718199,
0.999657107718199,0.999657107718199,0.999657107718199,0.999657107718199,
0.999657107718199,0.999657107718199,0.999657107718199,0.999657107718199,
0.999657107718199,0.999657107718199,0.999657107718199,0.999657107718199,
0.999657107718199,0.999657107718199,0.999657107718199),(1.0081993019117,
1.0081993019117,1.0081993019117,1.0081993019117,1.0081993019117,1.0081993019117,
1.0081993019117,1.0081993019117,1.0081993019117,1.0081993019117,1.0081993019117,
1.0081993019117,1.0081993019117,1.0081993019117,1.0081993019117,1.0081993019117),
(1.02563711373146,1.02563711373146,1.02563711373146,1.02563711373146,1.02563711373146,
1.02563711373146,1.02563711373146,1.02563711373146,1.02563711373146,1.02563711373146,
1.02563711373146,1.02563711373146,1.02563711373146,1.02563711373146,1.02563711373146,
1.02563711373146)))
REPRESENTATION_ITEM('')
SURFACE()
);
#2489=(
BOUNDED_SURFACE()
B_SPLINE_SURFACE(3,3,((#133129,#133130,#133131,#133132,#133133,#133134),
(#133135,#133136,#133137,#133138,#133139,#133140),(#133141,#133142,#133143,
#133144,#133145,#133146),(#133147,#133148,#133149,#133150,#133151,#133152)),
 .UNSPECIFIED.,.F.,.F.,.F.)
B_SPLINE_SURFACE_WITH_KNOTS((4,4),(4,1,1,4),(0.,1.),(0.,0.0271721067421099,
0.646141430958428,1.),.UNSPECIFIED.)
GEOMETRIC_REPRESENTATION_ITEM()
RATIONAL_B_SPLINE_SURFACE(((1.00945321541545,1.00945321541545,1.00945321541545,
1.00945321541545,1.00945321541545,1.00945321541545),(1.01344341494481,1.01344341494481,
1.01344341494481,1.01344341494481,1.01344341494481,1.01344341494481),(1.01869681103622,
1.01869681103622,1.01869681103622,1.01869681103622,1.01869681103622,1.01869681103622),
(1.02521340368968,1.02521340368968,1.02521340368968,1.02521340368968,1.02521340368968,
1.02521340368968)))
REPRESENTATION_ITEM('')
SURFACE()
);
#2490=(
BOUNDED_SURFACE()
B_SPLINE_SURFACE(3,3,((#133174,#133175,#133176,#133177,#133178,#133179,
#133180,#133181),(#133182,#133183,#133184,#133185,#133186,#133187,#133188,
#133189),(#133190,#133191,#133192,#133193,#133194,#133195,#133196,#133197),
(#133198,#133199,#133200,#133201,#133202,#133203,#133204,#133205)),
 .UNSPECIFIED.,.F.,.F.,.F.)
B_SPLINE_SURFACE_WITH_KNOTS((4,4),(4,1,1,1,1,4),(0.,1.),(-0.00146608837293589,
0.0970814361513046,0.317736262577814,0.559494757859586,0.822645521844187,
1.00146608855681),.UNSPECIFIED.)
GEOMETRIC_REPRESENTATION_ITEM()
RATIONAL_B_SPLINE_SURFACE(((1.00945321541545,1.00945321541545,1.00945321541545,
1.00945321541545,1.00945321541545,1.00945321541545,1.00945321541545,1.00945321541545),
(1.01344341494481,1.01344341494481,1.01344341494481,1.01344341494481,1.01344341494481,
1.01344341494481,1.01344341494481,1.01344341494481),(1.01869681103622,1.01869681103622,
1.01869681103622,1.01869681103622,1.01869681103622,1.01869681103622,1.01869681103622,
1.01869681103622),(1.02521340368968,1.02521340368968,1.02521340368968,1.02521340368968,
1.02521340368968,1.02521340368968,1.02521340368968,1.02521340368968)))
REPRESENTATION_ITEM('')
SURFACE()
);
#2491=(
BOUNDED_SURFACE()
B_SPLINE_SURFACE(3,3,((#133216,#133217,#133218,#133219,#133220,#133221,
#133222,#133223),(#133224,#133225,#133226,#133227,#133228,#133229,#133230,
#133231),(#133232,#133233,#133234,#133235,#133236,#133237,#133238,#133239),
(#133240,#133241,#133242,#133243,#133244,#133245,#133246,#133247)),
 .UNSPECIFIED.,.F.,.F.,.F.)
B_SPLINE_SURFACE_WITH_KNOTS((4,4),(4,1,1,1,1,4),(0.,1.),(0.,0.0970814361513046,
0.317736262577814,0.559494757859586,0.822645521844187,1.),.UNSPECIFIED.)
GEOMETRIC_REPRESENTATION_ITEM()
RATIONAL_B_SPLINE_SURFACE(((1.00417423477067,1.00417423477067,1.00417423477067,
1.00417423477067,1.00417423477067,1.00417423477067,1.00417423477067,1.00417423477067),
(1.00557922143849,1.00557922143849,1.00557922143849,1.00557922143849,1.00557922143849,
1.00557922143849,1.00557922143849,1.00557922143849),(1.00733888165342,1.00733888165342,
1.00733888165342,1.00733888165342,1.00733888165342,1.00733888165342,1.00733888165342,
1.00733888165342),(1.00945321541545,1.00945321541545,1.00945321541545,1.00945321541545,
1.00945321541545,1.00945321541545,1.00945321541545,1.00945321541545)))
REPRESENTATION_ITEM('')
SURFACE()
);
#2492=(
BOUNDED_SURFACE()
B_SPLINE_SURFACE(3,3,((#133254,#133255,#133256,#133257,#133258,#133259,
#133260,#133261,#133262,#133263,#133264,#133265,#133266,#133267,#133268,
#133269,#133270),(#133271,#133272,#133273,#133274,#133275,#133276,#133277,
#133278,#133279,#133280,#133281,#133282,#133283,#133284,#133285,#133286,
#133287),(#133288,#133289,#133290,#133291,#133292,#133293,#133294,#133295,
#133296,#133297,#133298,#133299,#133300,#133301,#133302,#133303,#133304),
(#133305,#133306,#133307,#133308,#133309,#133310,#133311,#133312,#133313,
#133314,#133315,#133316,#133317,#133318,#133319,#133320,#133321)),
 .UNSPECIFIED.,.F.,.F.,.F.)
B_SPLINE_SURFACE_WITH_KNOTS((4,4),(4,1,1,1,1,1,1,1,1,1,1,1,1,1,4),(0.,1.),
(0.,0.0169119460810613,0.0654242130848353,0.118166345404895,0.175802236516308,
0.238929210760529,0.307690566088615,0.381894800562219,0.461375561007429,
0.546721723948187,0.639112945312709,0.739719346812922,0.849650913359874,
0.96995594614347,1.),.UNSPECIFIED.)
GEOMETRIC_REPRESENTATION_ITEM()
RATIONAL_B_SPLINE_SURFACE(((1.00000962163611,1.00000962163611,1.00000962163611,
1.00000962163611,1.00000962163611,1.00000962163611,1.00000962163611,1.00000962163611,
1.00000962163611,1.00000962163611,1.00000962163611,1.00000962163611,1.00000962163611,
1.00000962163611,1.00000962163611,1.00000962163611,1.00000962163611),(1.00033430815833,
1.00033430815833,1.00033430815833,1.00033430815833,1.00033430815833,1.00033430815833,
1.00033430815833,1.00033430815833,1.00033430815833,1.00033430815833,1.00033430815833,
1.00033430815833,1.00033430815833,1.00033430815833,1.00033430815833,1.00033430815833,
1.00033430815833),(1.00887651633456,1.00887651633456,1.00887651633456,1.00887651633456,
1.00887651633456,1.00887651633456,1.00887651633456,1.00887651633456,1.00887651633456,
1.00887651633456,1.00887651633456,1.00887651633456,1.00887651633456,1.00887651633456,
1.00887651633456,1.00887651633456,1.00887651633456),(1.02563624616481,1.02563624616481,
1.02563624616481,1.02563624616481,1.02563624616481,1.02563624616481,1.02563624616481,
1.02563624616481,1.02563624616481,1.02563624616481,1.02563624616481,1.02563624616481,
1.02563624616481,1.02563624616481,1.02563624616481,1.02563624616481,1.02563624616481)))
REPRESENTATION_ITEM('')
SURFACE()
);
#2493=(
BOUNDED_SURFACE()
B_SPLINE_SURFACE(3,3,((#133528,#133529,#133530,#133531,#133532,#133533,
#133534,#133535,#133536,#133537,#133538,#133539,#133540,#133541,#133542,
#133543,#133544,#133545,#133546,#133547),(#133548,#133549,#133550,#133551,
#133552,#133553,#133554,#133555,#133556,#133557,#133558,#133559,#133560,
#133561,#133562,#133563,#133564,#133565,#133566,#133567),(#133568,#133569,
#133570,#133571,#133572,#133573,#133574,#133575,#133576,#133577,#133578,
#133579,#133580,#133581,#133582,#133583,#133584,#133585,#133586,#133587),
(#133588,#133589,#133590,#133591,#133592,#133593,#133594,#133595,#133596,
#133597,#133598,#133599,#133600,#133601,#133602,#133603,#133604,#133605,
#133606,#133607)),.UNSPECIFIED.,.F.,.F.,.F.)
B_SPLINE_SURFACE_WITH_KNOTS((4,4),(4,1,1,1,1,1,1,1,1,1,1,1,1,1,1,1,1,4),
(0.,1.),(0.,0.0396611801962909,0.0991280080993822,0.158967060305227,0.213500355613908,
0.265743805592041,0.31877970559442,0.372320929804579,0.42550049560743,0.477326879186013,
0.531755535132276,0.594383860510548,0.661759309442457,0.728996536779342,
0.791903310438717,0.857857310969531,0.931521029517504,1.),.UNSPECIFIED.)
GEOMETRIC_REPRESENTATION_ITEM()
RATIONAL_B_SPLINE_SURFACE(((1.186027134151,1.186027134151,1.186027134151,
1.186027134151,1.186027134151,1.186027134151,1.186027134151,1.186027134151,
1.186027134151,1.186027134151,1.186027134151,1.186027134151,1.186027134151,
1.186027134151,1.186027134151,1.186027134151,1.186027134151,1.186027134151,
1.186027134151,1.186027134151),(0.9379909552829,0.9379909552829,0.9379909552829,
0.9379909552829,0.9379909552829,0.9379909552829,0.9379909552829,0.9379909552829,
0.9379909552829,0.9379909552829,0.9379909552829,0.9379909552829,0.9379909552829,
0.9379909552829,0.9379909552829,0.9379909552829,0.9379909552829,0.9379909552829,
0.9379909552829,0.9379909552829),(0.9379909552829,0.9379909552829,0.9379909552829,
0.9379909552829,0.9379909552829,0.9379909552829,0.9379909552829,0.9379909552829,
0.9379909552829,0.9379909552829,0.9379909552829,0.9379909552829,0.9379909552829,
0.9379909552829,0.9379909552829,0.9379909552829,0.9379909552829,0.9379909552829,
0.9379909552829,0.9379909552829),(1.186027134151,1.186027134151,1.186027134151,
1.186027134151,1.186027134151,1.186027134151,1.186027134151,1.186027134151,
1.186027134151,1.186027134151,1.186027134151,1.186027134151,1.186027134151,
1.186027134151,1.186027134151,1.186027134151,1.186027134151,1.186027134151,
1.186027134151,1.186027134151)))
REPRESENTATION_ITEM('')
SURFACE()
);
#2494=(
BOUNDED_SURFACE()
B_SPLINE_SURFACE(3,3,((#133731,#133732,#133733,#133734,#133735,#133736,
#133737,#133738,#133739,#133740),(#133741,#133742,#133743,#133744,#133745,
#133746,#133747,#133748,#133749,#133750),(#133751,#133752,#133753,#133754,
#133755,#133756,#133757,#133758,#133759,#133760),(#133761,#133762,#133763,
#133764,#133765,#133766,#133767,#133768,#133769,#133770)),.UNSPECIFIED.,
 .F.,.F.,.F.)
B_SPLINE_SURFACE_WITH_KNOTS((4,4),(4,1,1,1,1,1,1,4),(0.,1.),(0.,0.180483144409011,
0.376627636825192,0.555380925262604,0.717719202974124,0.864187978201653,
0.995189047099047,1.),.UNSPECIFIED.)
GEOMETRIC_REPRESENTATION_ITEM()
RATIONAL_B_SPLINE_SURFACE(((1.543563279584,1.543563279584,1.543563279584,
1.543563279584,1.543563279584,1.543563279584,1.543563279584,1.543563279584,
1.543563279584,1.543563279584),(0.8188122401388,0.8188122401388,0.8188122401388,
0.8188122401388,0.8188122401388,0.8188122401388,0.8188122401388,0.8188122401388,
0.8188122401388,0.8188122401388),(0.8188122401388,0.8188122401388,0.8188122401388,
0.8188122401388,0.8188122401388,0.8188122401388,0.8188122401388,0.8188122401388,
0.8188122401388,0.8188122401388),(1.543563279584,1.543563279584,1.543563279584,
1.543563279584,1.543563279584,1.543563279584,1.543563279584,1.543563279584,
1.543563279584,1.543563279584)))
REPRESENTATION_ITEM('')
SURFACE()
);
#2495=(
BOUNDED_SURFACE()
B_SPLINE_SURFACE(3,3,((#134090,#134091,#134092,#134093,#134094,#134095,
#134096,#134097,#134098,#134099),(#134100,#134101,#134102,#134103,#134104,
#134105,#134106,#134107,#134108,#134109),(#134110,#134111,#134112,#134113,
#134114,#134115,#134116,#134117,#134118,#134119),(#134120,#134121,#134122,
#134123,#134124,#134125,#134126,#134127,#134128,#134129)),.UNSPECIFIED.,
 .F.,.F.,.F.)
B_SPLINE_SURFACE_WITH_KNOTS((4,4),(4,1,1,1,1,1,1,4),(0.,1.),(0.,0.0801033777080447,
0.269947183593058,0.444907444701882,0.606049850917101,0.757247797830559,
0.903019663307709,1.),.UNSPECIFIED.)
GEOMETRIC_REPRESENTATION_ITEM()
RATIONAL_B_SPLINE_SURFACE(((1.289190167752,1.289190167752,1.289190167752,
1.289190167752,1.289190167752,1.289190167752,1.289190167752,1.289190167752,
1.289190167752,1.289190167752),(0.9036032774159,0.9036032774159,0.9036032774159,
0.9036032774159,0.9036032774159,0.9036032774159,0.9036032774159,0.9036032774159,
0.9036032774159,0.9036032774159),(0.9036032774159,0.9036032774159,0.9036032774159,
0.9036032774159,0.9036032774159,0.9036032774159,0.9036032774159,0.9036032774159,
0.9036032774159,0.9036032774159),(1.289190167752,1.289190167752,1.289190167752,
1.289190167752,1.289190167752,1.289190167752,1.289190167752,1.289190167752,
1.289190167752,1.289190167752)))
REPRESENTATION_ITEM('')
SURFACE()
);
#2496=(
BOUNDED_SURFACE()
B_SPLINE_SURFACE(3,3,((#134254,#134255,#134256,#134257,#134258,#134259,
#134260,#134261,#134262,#134263,#134264,#134265,#134266,#134267,#134268,
#134269,#134270,#134271,#134272,#134273,#134274,#134275,#134276),(#134277,
#134278,#134279,#134280,#134281,#134282,#134283,#134284,#134285,#134286,
#134287,#134288,#134289,#134290,#134291,#134292,#134293,#134294,#134295,
#134296,#134297,#134298,#134299),(#134300,#134301,#134302,#134303,#134304,
#134305,#134306,#134307,#134308,#134309,#134310,#134311,#134312,#134313,
#134314,#134315,#134316,#134317,#134318,#134319,#134320,#134321,#134322),
(#134323,#134324,#134325,#134326,#134327,#134328,#134329,#134330,#134331,
#134332,#134333,#134334,#134335,#134336,#134337,#134338,#134339,#134340,
#134341,#134342,#134343,#134344,#134345)),.UNSPECIFIED.,.F.,.F.,.F.)
B_SPLINE_SURFACE_WITH_KNOTS((4,4),(4,3,1,1,1,1,1,1,1,1,1,1,1,1,1,1,1,1,
4),(0.,1.),(-0.0877127999650316,0.,0.0438526529104932,0.0936371717010089,
0.147143943539872,0.203180298908346,0.261023062007613,0.320175420604179,
0.380280116633112,0.441075199270649,0.502372544364654,0.564033875272927,
0.62595494019857,0.68805881886387,0.75029079479597,0.812614800050668,0.875010812287183,
0.937472218801071,1.),.UNSPECIFIED.)
GEOMETRIC_REPRESENTATION_ITEM()
RATIONAL_B_SPLINE_SURFACE(((1.,1.,1.,1.,1.,1.,1.,1.,1.,1.,1.,1.,1.,1.,1.,
1.,1.,1.,1.,1.,1.,1.,1.),(0.776946963780595,0.776946963780595,0.776946963780595,
0.776946963780595,0.776946963780595,0.776946963780595,0.776946963780595,
0.776946963780595,0.776946963780595,0.776946963780595,0.776946963780596,
0.776946963780595,0.776946963780595,0.776946963780595,0.776946963780595,
0.776946963780595,0.776946963780595,0.776946963780595,0.776946963780595,
0.776946963780595,0.776946963780595,0.776946963780595,0.776946963780595),
(0.776946963780595,0.776946963780595,0.776946963780595,0.776946963780595,
0.776946963780595,0.776946963780595,0.776946963780595,0.776946963780595,
0.776946963780595,0.776946963780595,0.776946963780596,0.776946963780595,
0.776946963780595,0.776946963780595,0.776946963780595,0.776946963780595,
0.776946963780595,0.776946963780595,0.776946963780595,0.776946963780595,
0.776946963780595,0.776946963780595,0.776946963780595),(1.,1.,1.,1.,1.,
1.,1.,1.,1.,1.,1.,1.,1.,1.,1.,1.,1.,1.,1.,1.,1.,1.,1.)))
REPRESENTATION_ITEM('')
SURFACE()
);
#2497=(
BOUNDED_SURFACE()
B_SPLINE_SURFACE(3,3,((#134718,#134719,#134720,#134721,#134722,#134723),
(#134724,#134725,#134726,#134727,#134728,#134729),(#134730,#134731,#134732,
#134733,#134734,#134735),(#134736,#134737,#134738,#134739,#134740,#134741)),
 .UNSPECIFIED.,.F.,.F.,.F.)
B_SPLINE_SURFACE_WITH_KNOTS((4,4),(4,1,1,4),(0.,1.),(0.,0.291618855427959,
0.679839163052527,1.),.UNSPECIFIED.)
GEOMETRIC_REPRESENTATION_ITEM()
RATIONAL_B_SPLINE_SURFACE(((1.268105254047,1.268105254047,1.268105254047,
1.268105254047,1.268105254047,1.268105254047),(0.9106315819844,0.9106315819844,
0.9106315819844,0.9106315819844,0.9106315819844,0.9106315819844),(0.9106315819844,
0.9106315819844,0.9106315819844,0.9106315819844,0.9106315819844,0.9106315819844),
(1.268105254047,1.268105254047,1.268105254047,1.268105254047,1.268105254047,
1.268105254047)))
REPRESENTATION_ITEM('')
SURFACE()
);
#2498=(
BOUNDED_SURFACE()
B_SPLINE_SURFACE(3,3,((#134864,#134865,#134866,#134867,#134868,#134869,
#134870,#134871,#134872,#134873),(#134874,#134875,#134876,#134877,#134878,
#134879,#134880,#134881,#134882,#134883),(#134884,#134885,#134886,#134887,
#134888,#134889,#134890,#134891,#134892,#134893),(#134894,#134895,#134896,
#134897,#134898,#134899,#134900,#134901,#134902,#134903)),.UNSPECIFIED.,
 .F.,.F.,.F.)
B_SPLINE_SURFACE_WITH_KNOTS((4,4),(4,1,1,1,1,1,1,4),(0.,1.),(0.,0.0598844757860275,
0.21530560800185,0.388152655537293,0.569077055547832,0.736795344088362,
0.884453290136092,1.),.UNSPECIFIED.)
GEOMETRIC_REPRESENTATION_ITEM()
RATIONAL_B_SPLINE_SURFACE(((1.625548306272,1.625548306272,1.625548306272,
1.625548306272,1.625548306272,1.625548306272,1.625548306272,1.625548306272,
1.625548306272,1.625548306272),(0.7914838979093,0.7914838979093,0.7914838979093,
0.7914838979093,0.7914838979093,0.7914838979093,0.7914838979093,0.7914838979093,
0.7914838979093,0.7914838979093),(0.7914838979093,0.7914838979093,0.7914838979093,
0.7914838979093,0.7914838979093,0.7914838979093,0.7914838979093,0.7914838979093,
0.7914838979093,0.7914838979093),(1.625548306272,1.625548306272,1.625548306272,
1.625548306272,1.625548306272,1.625548306272,1.625548306272,1.625548306272,
1.625548306272,1.625548306272)))
REPRESENTATION_ITEM('')
SURFACE()
);
#2499=(
BOUNDED_SURFACE()
B_SPLINE_SURFACE(3,3,((#134994,#134995,#134996,#134997,#134998,#134999,
#135000,#135001,#135002,#135003),(#135004,#135005,#135006,#135007,#135008,
#135009,#135010,#135011,#135012,#135013),(#135014,#135015,#135016,#135017,
#135018,#135019,#135020,#135021,#135022,#135023),(#135024,#135025,#135026,
#135027,#135028,#135029,#135030,#135031,#135032,#135033)),.UNSPECIFIED.,
 .F.,.F.,.F.)
B_SPLINE_SURFACE_WITH_KNOTS((4,4),(4,1,1,1,1,1,1,4),(0.,1.),(0.,0.118544207568657,
0.266810022823391,0.435219131927487,0.616475909576636,0.78883439689268,
0.943447617027774,1.),.UNSPECIFIED.)
GEOMETRIC_REPRESENTATION_ITEM()
RATIONAL_B_SPLINE_SURFACE(((1.62577582512,1.62577582512,1.62577582512,1.62577582512,
1.62577582512,1.62577582512,1.62577582512,1.62577582512,1.62577582512,1.62577582512),
(0.7914080582935,0.7914080582935,0.7914080582935,0.7914080582935,0.7914080582935,
0.7914080582935,0.7914080582935,0.7914080582935,0.7914080582935,0.7914080582935),
(0.7914080582935,0.7914080582935,0.7914080582935,0.7914080582935,0.7914080582935,
0.7914080582935,0.7914080582935,0.7914080582935,0.7914080582935,0.7914080582935),
(1.62577582512,1.62577582512,1.62577582512,1.62577582512,1.62577582512,
1.62577582512,1.62577582512,1.62577582512,1.62577582512,1.62577582512)))
REPRESENTATION_ITEM('')
SURFACE()
);
#2500=(
BOUNDED_SURFACE()
B_SPLINE_SURFACE(3,3,((#135155,#135156,#135157,#135158,#135159,#135160,
#135161,#135162,#135163,#135164,#135165,#135166,#135167,#135168,#135169),
(#135170,#135171,#135172,#135173,#135174,#135175,#135176,#135177,#135178,
#135179,#135180,#135181,#135182,#135183,#135184),(#135185,#135186,#135187,
#135188,#135189,#135190,#135191,#135192,#135193,#135194,#135195,#135196,
#135197,#135198,#135199),(#135200,#135201,#135202,#135203,#135204,#135205,
#135206,#135207,#135208,#135209,#135210,#135211,#135212,#135213,#135214)),
 .UNSPECIFIED.,.F.,.F.,.F.)
B_SPLINE_SURFACE_WITH_KNOTS((4,4),(4,1,1,1,1,1,1,1,1,1,1,1,4),(0.,1.),(0.,
0.0167135648045114,0.156510702717728,0.290602098832967,0.41291935039186,
0.522243745128064,0.620141294857168,0.708532612403636,0.788779269412781,
0.861957662054057,0.928247897390154,0.98772116750503,1.),.UNSPECIFIED.)
GEOMETRIC_REPRESENTATION_ITEM()
RATIONAL_B_SPLINE_SURFACE(((1.289190114461,1.289190114461,1.289190114461,
1.289190114461,1.289190114461,1.289190114461,1.289190114461,1.289190114461,
1.289190114461,1.289190114461,1.289190114461,1.289190114461,1.289190114461,
1.289190114461,1.289190114461),(0.9036032951798,0.9036032951798,0.9036032951798,
0.9036032951798,0.9036032951798,0.9036032951798,0.9036032951798,0.9036032951798,
0.9036032951798,0.9036032951798,0.9036032951798,0.9036032951798,0.9036032951798,
0.9036032951798,0.9036032951798),(0.9036032951798,0.9036032951798,0.9036032951798,
0.9036032951798,0.9036032951798,0.9036032951798,0.9036032951798,0.9036032951798,
0.9036032951798,0.9036032951798,0.9036032951798,0.9036032951798,0.9036032951798,
0.9036032951798,0.9036032951798),(1.289190114461,1.289190114461,1.289190114461,
1.289190114461,1.289190114461,1.289190114461,1.289190114461,1.289190114461,
1.289190114461,1.289190114461,1.289190114461,1.289190114461,1.289190114461,
1.289190114461,1.289190114461)))
REPRESENTATION_ITEM('')
SURFACE()
);
#2501=(
BOUNDED_SURFACE()
B_SPLINE_SURFACE(3,3,((#135581,#135582,#135583,#135584,#135585,#135586),
(#135587,#135588,#135589,#135590,#135591,#135592),(#135593,#135594,#135595,
#135596,#135597,#135598),(#135599,#135600,#135601,#135602,#135603,#135604)),
 .UNSPECIFIED.,.F.,.F.,.F.)
B_SPLINE_SURFACE_WITH_KNOTS((4,4),(4,1,1,4),(0.,1.),(0.,0.235053155447178,
0.807846173326003,1.),.UNSPECIFIED.)
GEOMETRIC_REPRESENTATION_ITEM()
RATIONAL_B_SPLINE_SURFACE(((1.190144115645,1.190144115645,1.190144115645,
1.190144115645,1.190144115645,1.190144115645),(0.9366186281184,0.9366186281184,
0.9366186281184,0.9366186281184,0.9366186281184,0.9366186281184),(0.9366186281184,
0.9366186281184,0.9366186281184,0.9366186281184,0.9366186281184,0.9366186281184),
(1.190144115645,1.190144115645,1.190144115645,1.190144115645,1.190144115645,
1.190144115645)))
REPRESENTATION_ITEM('')
SURFACE()
);
#2502=(
BOUNDED_SURFACE()
B_SPLINE_SURFACE(3,3,((#135839,#135840,#135841,#135842,#135843,#135844,
#135845,#135846,#135847,#135848,#135849,#135850,#135851,#135852,#135853,
#135854),(#135855,#135856,#135857,#135858,#135859,#135860,#135861,#135862,
#135863,#135864,#135865,#135866,#135867,#135868,#135869,#135870),(#135871,
#135872,#135873,#135874,#135875,#135876,#135877,#135878,#135879,#135880,
#135881,#135882,#135883,#135884,#135885,#135886),(#135887,#135888,#135889,
#135890,#135891,#135892,#135893,#135894,#135895,#135896,#135897,#135898,
#135899,#135900,#135901,#135902),(#135903,#135904,#135905,#135906,#135907,
#135908,#135909,#135910,#135911,#135912,#135913,#135914,#135915,#135916,
#135917,#135918),(#135919,#135920,#135921,#135922,#135923,#135924,#135925,
#135926,#135927,#135928,#135929,#135930,#135931,#135932,#135933,#135934),
(#135935,#135936,#135937,#135938,#135939,#135940,#135941,#135942,#135943,
#135944,#135945,#135946,#135947,#135948,#135949,#135950)),.UNSPECIFIED.,
 .F.,.F.,.F.)
B_SPLINE_SURFACE_WITH_KNOTS((4,3,4),(4,1,1,1,1,1,1,1,1,1,1,1,1,4),(0.,0.5,
1.),(0.,0.0687092176565791,0.148436322486723,0.231002296681117,0.312631644850041,
0.390370677084989,0.463984704679376,0.535797779848878,0.609423921069924,
0.687272621576965,0.769077589534318,0.851644273887414,0.931363117848373,
1.),.UNSPECIFIED.)
GEOMETRIC_REPRESENTATION_ITEM()
RATIONAL_B_SPLINE_SURFACE(((1.308864936088,1.308864936088,1.308864936088,
1.308864936088,1.308864936088,1.308864936088,1.308864936088,1.308864936088,
1.308864936088,1.308864936088,1.308864936088,1.308864936088,1.308864936088,
1.308864936088,1.308864936088,1.308864936088),(0.8970450213041,0.8970450213041,
0.8970450213041,0.8970450213041,0.8970450213041,0.8970450213041,0.8970450213041,
0.8970450213041,0.8970450213041,0.8970450213041,0.8970450213041,0.8970450213041,
0.8970450213041,0.8970450213041,0.8970450213041,0.8970450213041),(0.8970450213041,
0.8970450213041,0.8970450213041,0.8970450213041,0.8970450213041,0.8970450213041,
0.8970450213041,0.8970450213041,0.8970450213041,0.8970450213041,0.8970450213041,
0.8970450213041,0.8970450213041,0.8970450213041,0.8970450213041,0.8970450213041),
(1.308864936088,1.308864936088,1.308864936088,1.308864936088,1.308864936088,
1.308864936088,1.308864936088,1.308864936088,1.308864936088,1.308864936088,
1.308864936088,1.308864936088,1.308864936088,1.308864936088,1.308864936088,
1.308864936088),(0.8970450213041,0.8970450213041,0.8970450213041,0.8970450213041,
0.8970450213041,0.8970450213041,0.8970450213041,0.8970450213041,0.8970450213041,
0.8970450213041,0.8970450213041,0.8970450213041,0.8970450213041,0.8970450213041,
0.8970450213041,0.8970450213041),(0.8970450213041,0.8970450213041,0.8970450213041,
0.8970450213041,0.8970450213041,0.8970450213041,0.8970450213041,0.8970450213041,
0.8970450213041,0.8970450213041,0.8970450213041,0.8970450213041,0.8970450213041,
0.8970450213041,0.8970450213041,0.8970450213041),(1.308864936088,1.308864936088,
1.308864936088,1.308864936088,1.308864936088,1.308864936088,1.308864936088,
1.308864936088,1.308864936088,1.308864936088,1.308864936088,1.308864936088,
1.308864936088,1.308864936088,1.308864936088,1.308864936088)))
REPRESENTATION_ITEM('')
SURFACE()
);
#2503=(
BOUNDED_SURFACE()
B_SPLINE_SURFACE(3,3,((#135952,#135953,#135954,#135955,#135956,#135957),
(#135958,#135959,#135960,#135961,#135962,#135963),(#135964,#135965,#135966,
#135967,#135968,#135969),(#135970,#135971,#135972,#135973,#135974,#135975)),
 .UNSPECIFIED.,.F.,.F.,.F.)
B_SPLINE_SURFACE_WITH_KNOTS((4,4),(4,1,1,4),(0.,1.),(0.,0.0809027375127101,
0.709349370148383,1.),.UNSPECIFIED.)
GEOMETRIC_REPRESENTATION_ITEM()
RATIONAL_B_SPLINE_SURFACE(((1.190145701779,1.190145701779,1.190145701779,
1.190145701779,1.190145701779,1.190145701779),(0.936618099407,0.936618099407,
0.936618099407,0.936618099407,0.936618099407,0.936618099407),(0.936618099407,
0.936618099407,0.936618099407,0.936618099407,0.936618099407,0.936618099407),
(1.190145701779,1.190145701779,1.190145701779,1.190145701779,1.190145701779,
1.190145701779)))
REPRESENTATION_ITEM('')
SURFACE()
);
#2504=(
BOUNDED_SURFACE()
B_SPLINE_SURFACE(3,3,((#135977,#135978,#135979,#135980,#135981,#135982),
(#135983,#135984,#135985,#135986,#135987,#135988),(#135989,#135990,#135991,
#135992,#135993,#135994),(#135995,#135996,#135997,#135998,#135999,#136000),
(#136001,#136002,#136003,#136004,#136005,#136006),(#136007,#136008,#136009,
#136010,#136011,#136012),(#136013,#136014,#136015,#136016,#136017,#136018)),
 .UNSPECIFIED.,.F.,.F.,.F.)
B_SPLINE_SURFACE_WITH_KNOTS((4,3,4),(4,1,1,4),(0.,0.5,1.),(0.,0.274607544356056,
0.733821408099398,1.),.UNSPECIFIED.)
GEOMETRIC_REPRESENTATION_ITEM()
RATIONAL_B_SPLINE_SURFACE(((1.232615246856,1.232615246856,1.232615246856,
1.232615246856,1.232615246856,1.232615246856),(0.9224615843814,0.9224615843814,
0.9224615843814,0.9224615843814,0.9224615843814,0.9224615843814),(0.9224615843814,
0.9224615843814,0.9224615843814,0.9224615843814,0.9224615843814,0.9224615843814),
(1.232615246856,1.232615246856,1.232615246856,1.232615246856,1.232615246856,
1.232615246856),(0.9224615843814,0.9224615843814,0.9224615843814,0.9224615843814,
0.9224615843814,0.9224615843814),(0.9224615843814,0.9224615843814,0.9224615843814,
0.9224615843814,0.9224615843814,0.9224615843814),(1.232615246856,1.232615246856,
1.232615246856,1.232615246856,1.232615246856,1.232615246856)))
REPRESENTATION_ITEM('')
SURFACE()
);
#2505=(
BOUNDED_SURFACE()
B_SPLINE_SURFACE(3,3,((#136020,#136021,#136022,#136023,#136024,#136025),
(#136026,#136027,#136028,#136029,#136030,#136031),(#136032,#136033,#136034,
#136035,#136036,#136037),(#136038,#136039,#136040,#136041,#136042,#136043)),
 .UNSPECIFIED.,.F.,.F.,.F.)
B_SPLINE_SURFACE_WITH_KNOTS((4,4),(4,1,1,4),(0.,1.),(0.,0.0915158091820991,
0.730870545365667,1.),.UNSPECIFIED.)
GEOMETRIC_REPRESENTATION_ITEM()
RATIONAL_B_SPLINE_SURFACE(((1.190145739571,1.190145739571,1.190145739571,
1.190145739571,1.190145739571,1.190145739571),(0.9366180868096,0.9366180868096,
0.9366180868096,0.9366180868096,0.9366180868096,0.9366180868096),(0.9366180868096,
0.9366180868096,0.9366180868096,0.9366180868096,0.9366180868096,0.9366180868096),
(1.190145739571,1.190145739571,1.190145739571,1.190145739571,1.190145739571,
1.190145739571)))
REPRESENTATION_ITEM('')
SURFACE()
);
#2506=(
BOUNDED_SURFACE()
B_SPLINE_SURFACE(3,3,((#136045,#136046,#136047,#136048,#136049,#136050,
#136051,#136052,#136053,#136054,#136055,#136056,#136057,#136058,#136059,
#136060),(#136061,#136062,#136063,#136064,#136065,#136066,#136067,#136068,
#136069,#136070,#136071,#136072,#136073,#136074,#136075,#136076),(#136077,
#136078,#136079,#136080,#136081,#136082,#136083,#136084,#136085,#136086,
#136087,#136088,#136089,#136090,#136091,#136092),(#136093,#136094,#136095,
#136096,#136097,#136098,#136099,#136100,#136101,#136102,#136103,#136104,
#136105,#136106,#136107,#136108),(#136109,#136110,#136111,#136112,#136113,
#136114,#136115,#136116,#136117,#136118,#136119,#136120,#136121,#136122,
#136123,#136124),(#136125,#136126,#136127,#136128,#136129,#136130,#136131,
#136132,#136133,#136134,#136135,#136136,#136137,#136138,#136139,#136140),
(#136141,#136142,#136143,#136144,#136145,#136146,#136147,#136148,#136149,
#136150,#136151,#136152,#136153,#136154,#136155,#136156)),.UNSPECIFIED.,
 .F.,.F.,.F.)
B_SPLINE_SURFACE_WITH_KNOTS((4,3,4),(4,1,1,1,1,1,1,1,1,1,1,1,1,4),(0.,0.5,
1.),(0.,0.0700282448367935,0.149591065260121,0.231957090335842,0.31326843643496,
0.39068316564619,0.464059946408323,0.535688017619035,0.609079764496469,
0.686617012874269,0.768115357612328,0.85048528028637,0.930041884500008,
1.),.UNSPECIFIED.)
GEOMETRIC_REPRESENTATION_ITEM()
RATIONAL_B_SPLINE_SURFACE(((1.308862041161,1.308862041161,1.308862041161,
1.308862041161,1.308862041161,1.308862041161,1.308862041161,1.308862041161,
1.308862041161,1.308862041161,1.308862041161,1.308862041161,1.308862041161,
1.308862041161,1.308862041161,1.308862041161),(0.8970459862798,0.8970459862798,
0.8970459862798,0.8970459862798,0.8970459862798,0.8970459862798,0.8970459862798,
0.8970459862798,0.8970459862798,0.8970459862798,0.8970459862798,0.8970459862798,
0.8970459862798,0.8970459862798,0.8970459862798,0.8970459862798),(0.8970459862798,
0.8970459862798,0.8970459862798,0.8970459862798,0.8970459862798,0.8970459862798,
0.8970459862798,0.8970459862798,0.8970459862798,0.8970459862798,0.8970459862798,
0.8970459862798,0.8970459862798,0.8970459862798,0.8970459862798,0.8970459862798),
(1.308862041161,1.308862041161,1.308862041161,1.308862041161,1.308862041161,
1.308862041161,1.308862041161,1.308862041161,1.308862041161,1.308862041161,
1.308862041161,1.308862041161,1.308862041161,1.308862041161,1.308862041161,
1.308862041161),(0.8970459862798,0.8970459862798,0.8970459862798,0.8970459862798,
0.8970459862798,0.8970459862798,0.8970459862798,0.8970459862798,0.8970459862798,
0.8970459862798,0.8970459862798,0.8970459862798,0.8970459862798,0.8970459862798,
0.8970459862798,0.8970459862798),(0.8970459862798,0.8970459862798,0.8970459862798,
0.8970459862798,0.8970459862798,0.8970459862798,0.8970459862798,0.8970459862798,
0.8970459862798,0.8970459862798,0.8970459862798,0.8970459862798,0.8970459862798,
0.8970459862798,0.8970459862798,0.8970459862798),(1.308862041161,1.308862041161,
1.308862041161,1.308862041161,1.308862041161,1.308862041161,1.308862041161,
1.308862041161,1.308862041161,1.308862041161,1.308862041161,1.308862041161,
1.308862041161,1.308862041161,1.308862041161,1.308862041161)))
REPRESENTATION_ITEM('')
SURFACE()
);
#2507=(
BOUNDED_SURFACE()
B_SPLINE_SURFACE(3,3,((#138377,#138378,#138379,#138380),(#138381,#138382,
#138383,#138384),(#138385,#138386,#138387,#138388),(#138389,#138390,#138391,
#138392)),.UNSPECIFIED.,.F.,.F.,.F.)
B_SPLINE_SURFACE_WITH_KNOTS((4,4),(4,4),(0.,1.),(0.,1.),.UNSPECIFIED.)
GEOMETRIC_REPRESENTATION_ITEM()
RATIONAL_B_SPLINE_SURFACE(((1.008822121122,0.8033151890331,0.8032831812337,
1.008726097724),(1.008912249556,0.8013058203417,0.8012734855446,1.008815245165),
(1.008912321853,0.8013042085275,0.8012718734681,1.008815316675),(1.008822107526,
0.8033154921495,0.8032834843994,1.008726084276)))
REPRESENTATION_ITEM('')
SURFACE()
);
#2508=(
BOUNDED_SURFACE()
B_SPLINE_SURFACE(3,3,((#139238,#139239,#139240,#139241,#139242,#139243,
#139244,#139245,#139246,#139247,#139248,#139249,#139250,#139251,#139252,
#139253,#139254,#139255,#139256,#139257,#139258,#139259,#139260,#139261,
#139262,#139263,#139264,#139265,#139266,#139267,#139268,#139269,#139270,
#139271,#139272,#139273,#139274,#139275,#139276,#139277,#139278,#139279,
#139280,#139281,#139282,#139283,#139284,#139285,#139286,#139287,#139288,
#139289,#139290,#139291,#139292,#139293,#139294),(#139295,#139296,#139297,
#139298,#139299,#139300,#139301,#139302,#139303,#139304,#139305,#139306,
#139307,#139308,#139309,#139310,#139311,#139312,#139313,#139314,#139315,
#139316,#139317,#139318,#139319,#139320,#139321,#139322,#139323,#139324,
#139325,#139326,#139327,#139328,#139329,#139330,#139331,#139332,#139333,
#139334,#139335,#139336,#139337,#139338,#139339,#139340,#139341,#139342,
#139343,#139344,#139345,#139346,#139347,#139348,#139349,#139350,#139351),
(#139352,#139353,#139354,#139355,#139356,#139357,#139358,#139359,#139360,
#139361,#139362,#139363,#139364,#139365,#139366,#139367,#139368,#139369,
#139370,#139371,#139372,#139373,#139374,#139375,#139376,#139377,#139378,
#139379,#139380,#139381,#139382,#139383,#139384,#139385,#139386,#139387,
#139388,#139389,#139390,#139391,#139392,#139393,#139394,#139395,#139396,
#139397,#139398,#139399,#139400,#139401,#139402,#139403,#139404,#139405,
#139406,#139407,#139408),(#139409,#139410,#139411,#139412,#139413,#139414,
#139415,#139416,#139417,#139418,#139419,#139420,#139421,#139422,#139423,
#139424,#139425,#139426,#139427,#139428,#139429,#139430,#139431,#139432,
#139433,#139434,#139435,#139436,#139437,#139438,#139439,#139440,#139441,
#139442,#139443,#139444,#139445,#139446,#139447,#139448,#139449,#139450,
#139451,#139452,#139453,#139454,#139455,#139456,#139457,#139458,#139459,
#139460,#139461,#139462,#139463,#139464,#139465)),.UNSPECIFIED.,.F.,.F.,
 .F.)
B_SPLINE_SURFACE_WITH_KNOTS((4,4),(4,1,1,1,1,1,1,1,1,1,1,1,1,1,1,1,1,1,
1,1,1,1,1,1,1,1,1,1,1,1,1,1,1,1,1,1,1,1,1,1,1,1,1,1,1,1,1,1,1,1,1,1,1,1,
4),(0.,1.),(0.,0.00436594588687658,0.0182600210166181,0.0336361494826213,
0.0506183732771892,0.0693310885947867,0.0898968700401271,0.112502721901119,
0.137670869409112,0.166010055644541,0.197488961679859,0.231803117837838,
0.269453903656424,0.310997004277211,0.356845197598653,0.407613486217267,
0.459741003658159,0.507079603017427,0.548859184651959,0.586033851963287,
0.619338629530692,0.649347424630681,0.676440228532917,0.701038763414989,
0.723416730015481,0.743823676714273,0.762471787524201,0.779541489745329,
0.795189394601638,0.809554049025702,0.822746458983589,0.834875103495141,
0.846051713912006,0.856380231241817,0.865896925803063,0.874602749195169,
0.88252206935229,0.889825047977363,0.896737634924824,0.903485575835366,
0.910246440119728,0.917100212565293,0.923938121747363,0.930419691089745,
0.936750575754955,0.94324323866504,0.949721357335021,0.955738934700183,
0.961744884998761,0.96808108564707,0.974379967180707,0.981030794925491,
0.98771333105686,0.994327233714889,1.),.UNSPECIFIED.)
GEOMETRIC_REPRESENTATION_ITEM()
RATIONAL_B_SPLINE_SURFACE(((1.753204797659,1.753204797659,1.753204797659,
1.753204797659,1.753204797659,1.753204797659,1.753204797659,1.753204797659,
1.753204797659,1.753204797659,1.753204797659,1.753204797659,1.753204797659,
1.753204797659,1.753204797659,1.753204797659,1.753204797659,1.753204797659,
1.753204797659,1.753204797659,1.753204797659,1.753204797659,1.753204797659,
1.753204797659,1.753204797659,1.753204797659,1.753204797659,1.753204797659,
1.753204797659,1.753204797659,1.753204797659,1.753204797659,1.753204797659,
1.753204797659,1.753204797659,1.753204797659,1.753204797659,1.753204797659,
1.753204797659,1.753204797659,1.753204797659,1.753204797659,1.753204797659,
1.753204797659,1.753204797659,1.753204797659,1.753204797659,1.753204797659,
1.753204797659,1.753204797659,1.753204797659,1.753204797659,1.753204797659,
1.753204797659,1.753204797659,1.753204797659,1.753204797659),(0.7489317341138,
0.7489317341138,0.7489317341138,0.7489317341138,0.7489317341138,0.7489317341138,
0.7489317341138,0.7489317341138,0.7489317341138,0.7489317341138,0.7489317341138,
0.7489317341138,0.7489317341138,0.7489317341138,0.7489317341138,0.7489317341138,
0.7489317341138,0.7489317341138,0.7489317341138,0.7489317341138,0.7489317341138,
0.7489317341138,0.7489317341138,0.7489317341138,0.7489317341138,0.7489317341138,
0.7489317341138,0.7489317341138,0.7489317341138,0.7489317341138,0.7489317341138,
0.7489317341138,0.7489317341138,0.7489317341138,0.7489317341138,0.7489317341138,
0.7489317341138,0.7489317341138,0.7489317341138,0.7489317341138,0.7489317341138,
0.7489317341138,0.7489317341138,0.7489317341138,0.7489317341138,0.7489317341138,
0.7489317341138,0.7489317341138,0.7489317341138,0.7489317341138,0.7489317341138,
0.7489317341138,0.7489317341138,0.7489317341138,0.7489317341138,0.7489317341138,
0.7489317341138),(0.7489317341138,0.7489317341138,0.7489317341138,0.7489317341138,
0.7489317341138,0.7489317341138,0.7489317341138,0.7489317341138,0.7489317341138,
0.7489317341138,0.7489317341138,0.7489317341138,0.7489317341138,0.7489317341138,
0.7489317341138,0.7489317341138,0.7489317341138,0.7489317341138,0.7489317341138,
0.7489317341138,0.7489317341138,0.7489317341138,0.7489317341138,0.7489317341138,
0.7489317341138,0.7489317341138,0.7489317341138,0.7489317341138,0.7489317341138,
0.7489317341138,0.7489317341138,0.7489317341138,0.7489317341138,0.7489317341138,
0.7489317341138,0.7489317341138,0.7489317341138,0.7489317341138,0.7489317341138,
0.7489317341138,0.7489317341138,0.7489317341138,0.7489317341138,0.7489317341138,
0.7489317341138,0.7489317341138,0.7489317341138,0.7489317341138,0.7489317341138,
0.7489317341138,0.7489317341138,0.7489317341138,0.7489317341138,0.7489317341138,
0.7489317341138,0.7489317341138,0.7489317341138),(1.753204797659,1.753204797659,
1.753204797659,1.753204797659,1.753204797659,1.753204797659,1.753204797659,
1.753204797659,1.753204797659,1.753204797659,1.753204797659,1.753204797659,
1.753204797659,1.753204797659,1.753204797659,1.753204797659,1.753204797659,
1.753204797659,1.753204797659,1.753204797659,1.753204797659,1.753204797659,
1.753204797659,1.753204797659,1.753204797659,1.753204797659,1.753204797659,
1.753204797659,1.753204797659,1.753204797659,1.753204797659,1.753204797659,
1.753204797659,1.753204797659,1.753204797659,1.753204797659,1.753204797659,
1.753204797659,1.753204797659,1.753204797659,1.753204797659,1.753204797659,
1.753204797659,1.753204797659,1.753204797659,1.753204797659,1.753204797659,
1.753204797659,1.753204797659,1.753204797659,1.753204797659,1.753204797659,
1.753204797659,1.753204797659,1.753204797659,1.753204797659,1.753204797659)))
REPRESENTATION_ITEM('')
SURFACE()
);
#2509=(
BOUNDED_SURFACE()
B_SPLINE_SURFACE(3,3,((#139981,#139982,#139983,#139984,#139985,#139986,
#139987,#139988,#139989,#139990,#139991,#139992,#139993,#139994,#139995,
#139996,#139997),(#139998,#139999,#140000,#140001,#140002,#140003,#140004,
#140005,#140006,#140007,#140008,#140009,#140010,#140011,#140012,#140013,
#140014),(#140015,#140016,#140017,#140018,#140019,#140020,#140021,#140022,
#140023,#140024,#140025,#140026,#140027,#140028,#140029,#140030,#140031),
(#140032,#140033,#140034,#140035,#140036,#140037,#140038,#140039,#140040,
#140041,#140042,#140043,#140044,#140045,#140046,#140047,#140048)),
 .UNSPECIFIED.,.F.,.F.,.F.)
B_SPLINE_SURFACE_WITH_KNOTS((4,4),(4,1,1,1,1,1,1,1,1,1,1,1,1,1,4),(0.,1.),
(0.,0.0309106984649458,0.0767351380515422,0.126422877856924,0.180395940015139,
0.239061834418011,0.302825261448321,0.372125224244129,0.447415877060644,
0.529151218103455,0.61776396940816,0.713738372609746,0.817824498173652,
0.93084881910144,1.),.UNSPECIFIED.)
GEOMETRIC_REPRESENTATION_ITEM()
RATIONAL_B_SPLINE_SURFACE(((1.477765587143,1.477765587143,1.477765587143,
1.477765587143,1.477765587143,1.477765587143,1.477765587143,1.477765587143,
1.477765587143,1.477765587143,1.477765587143,1.477765587143,1.477765587143,
1.477765587143,1.477765587143,1.477765587143,1.477765587143),(0.8407448042857,
0.8407448042857,0.8407448042857,0.8407448042857,0.8407448042857,0.8407448042857,
0.8407448042857,0.8407448042857,0.8407448042857,0.8407448042857,0.8407448042857,
0.8407448042857,0.8407448042857,0.8407448042857,0.8407448042857,0.8407448042857,
0.8407448042857),(0.8407448042857,0.8407448042857,0.8407448042857,0.8407448042857,
0.8407448042857,0.8407448042857,0.8407448042857,0.8407448042857,0.8407448042857,
0.8407448042857,0.8407448042857,0.8407448042857,0.8407448042857,0.8407448042857,
0.8407448042857,0.8407448042857,0.8407448042857),(1.477765587143,1.477765587143,
1.477765587143,1.477765587143,1.477765587143,1.477765587143,1.477765587143,
1.477765587143,1.477765587143,1.477765587143,1.477765587143,1.477765587143,
1.477765587143,1.477765587143,1.477765587143,1.477765587143,1.477765587143)))
REPRESENTATION_ITEM('')
SURFACE()
);
#2510=(
BOUNDED_SURFACE()
B_SPLINE_SURFACE(3,3,((#140136,#140137,#140138,#140139,#140140,#140141,
#140142,#140143,#140144,#140145),(#140146,#140147,#140148,#140149,#140150,
#140151,#140152,#140153,#140154,#140155),(#140156,#140157,#140158,#140159,
#140160,#140161,#140162,#140163,#140164,#140165),(#140166,#140167,#140168,
#140169,#140170,#140171,#140172,#140173,#140174,#140175)),.UNSPECIFIED.,
 .F.,.F.,.F.)
B_SPLINE_SURFACE_WITH_KNOTS((4,4),(4,1,1,1,1,1,1,4),(0.,1.),(0.,0.128230369083995,
0.280285083819611,0.448824676206344,0.626406055676366,0.804550055721658,
0.977970892840894,1.),.UNSPECIFIED.)
GEOMETRIC_REPRESENTATION_ITEM()
RATIONAL_B_SPLINE_SURFACE(((1.391693969077,1.391693969077,1.391693969077,
1.391693969077,1.391693969077,1.391693969077,1.391693969077,1.391693969077,
1.391693969077,1.391693969077),(0.8694353436408,0.8694353436408,0.8694353436408,
0.8694353436408,0.8694353436408,0.8694353436408,0.8694353436408,0.8694353436408,
0.8694353436408,0.8694353436408),(0.8694353436408,0.8694353436408,0.8694353436408,
0.8694353436408,0.8694353436408,0.8694353436408,0.8694353436408,0.8694353436408,
0.8694353436408,0.8694353436408),(1.391693969077,1.391693969077,1.391693969077,
1.391693969077,1.391693969077,1.391693969077,1.391693969077,1.391693969077,
1.391693969077,1.391693969077)))
REPRESENTATION_ITEM('')
SURFACE()
);
#2511=(
BOUNDED_SURFACE()
B_SPLINE_SURFACE(3,3,((#140424,#140425,#140426,#140427),(#140428,#140429,
#140430,#140431),(#140432,#140433,#140434,#140435),(#140436,#140437,#140438,
#140439)),.UNSPECIFIED.,.F.,.F.,.F.)
B_SPLINE_SURFACE_WITH_KNOTS((4,4),(4,4),(0.,1.),(0.,1.),.UNSPECIFIED.)
GEOMETRIC_REPRESENTATION_ITEM()
RATIONAL_B_SPLINE_SURFACE(((1.292957414843,1.292957414843,1.292957414843,
1.292957414843),(0.9023475283856,0.9023475283856,0.9023475283856,0.9023475283856),
(0.9023475283856,0.9023475283856,0.9023475283856,0.9023475283856),(1.292957414843,
1.292957414843,1.292957414843,1.292957414843)))
REPRESENTATION_ITEM('')
SURFACE()
);
#2512=(
BOUNDED_SURFACE()
B_SPLINE_SURFACE(3,3,((#140565,#140566,#140567,#140568,#140569,#140570,
#140571),(#140572,#140573,#140574,#140575,#140576,#140577,#140578),(#140579,
#140580,#140581,#140582,#140583,#140584,#140585),(#140586,#140587,#140588,
#140589,#140590,#140591,#140592)),.UNSPECIFIED.,.F.,.F.,.F.)
B_SPLINE_SURFACE_WITH_KNOTS((4,4),(4,1,1,1,4),(0.,1.),(0.,0.222752526718504,
0.482252641961039,0.73941984056398,1.),.UNSPECIFIED.)
GEOMETRIC_REPRESENTATION_ITEM()
RATIONAL_B_SPLINE_SURFACE(((1.400806786583,1.400806786583,1.400806786583,
1.400806786583,1.400806786583,1.400806786583,1.400806786583),(0.8663977378056,
0.8663977378056,0.8663977378056,0.8663977378056,0.8663977378056,0.8663977378056,
0.8663977378056),(0.8663977378056,0.8663977378056,0.8663977378056,0.8663977378056,
0.8663977378056,0.8663977378056,0.8663977378056),(1.400806786583,1.400806786583,
1.400806786583,1.400806786583,1.400806786583,1.400806786583,1.400806786583)))
REPRESENTATION_ITEM('')
SURFACE()
);
#2513=(
BOUNDED_SURFACE()
B_SPLINE_SURFACE(3,3,((#141054,#141055,#141056,#141057,#141058,#141059,
#141060,#141061,#141062,#141063),(#141064,#141065,#141066,#141067,#141068,
#141069,#141070,#141071,#141072,#141073),(#141074,#141075,#141076,#141077,
#141078,#141079,#141080,#141081,#141082,#141083),(#141084,#141085,#141086,
#141087,#141088,#141089,#141090,#141091,#141092,#141093)),.UNSPECIFIED.,
 .F.,.F.,.F.)
B_SPLINE_SURFACE_WITH_KNOTS((4,4),(4,1,1,1,1,1,1,4),(0.,1.),(0.,0.0210781168668079,
0.19449715108835,0.372688328304436,0.550339588756535,0.718994260976883,
0.87136168298915,1.),.UNSPECIFIED.)
GEOMETRIC_REPRESENTATION_ITEM()
RATIONAL_B_SPLINE_SURFACE(((1.391693714632,1.391693714632,1.391693714632,
1.391693714632,1.391693714632,1.391693714632,1.391693714632,1.391693714632,
1.391693714632,1.391693714632),(0.8694354284561,0.8694354284561,0.8694354284561,
0.8694354284561,0.8694354284561,0.8694354284561,0.8694354284561,0.8694354284561,
0.8694354284561,0.8694354284561),(0.8694354284561,0.8694354284561,0.8694354284561,
0.8694354284561,0.8694354284561,0.8694354284561,0.8694354284561,0.8694354284561,
0.8694354284561,0.8694354284561),(1.391693714632,1.391693714632,1.391693714632,
1.391693714632,1.391693714632,1.391693714632,1.391693714632,1.391693714632,
1.391693714632,1.391693714632)))
REPRESENTATION_ITEM('')
SURFACE()
);
#2514=(
BOUNDED_SURFACE()
B_SPLINE_SURFACE(3,3,((#141536,#141537,#141538,#141539,#141540,#141541,
#141542,#141543,#141544,#141545,#141546,#141547,#141548,#141549,#141550,
#141551,#141552),(#141553,#141554,#141555,#141556,#141557,#141558,#141559,
#141560,#141561,#141562,#141563,#141564,#141565,#141566,#141567,#141568,
#141569),(#141570,#141571,#141572,#141573,#141574,#141575,#141576,#141577,
#141578,#141579,#141580,#141581,#141582,#141583,#141584,#141585,#141586),
(#141587,#141588,#141589,#141590,#141591,#141592,#141593,#141594,#141595,
#141596,#141597,#141598,#141599,#141600,#141601,#141602,#141603)),
 .UNSPECIFIED.,.F.,.F.,.F.)
B_SPLINE_SURFACE_WITH_KNOTS((4,4),(4,1,1,1,1,1,1,1,1,1,1,1,1,1,4),(0.,1.),
(0.,0.069890317865961,0.183519863377166,0.288095357886999,0.384463811683335,
0.473385027678461,0.555345635364338,0.630785683183373,0.700166793190766,
0.763949567937318,0.82257831309593,0.876462900672047,0.926018168114661,
0.971673401817449,1.),.UNSPECIFIED.)
GEOMETRIC_REPRESENTATION_ITEM()
RATIONAL_B_SPLINE_SURFACE(((1.47776666642,1.47776666642,1.47776666642,1.47776666642,
1.47776666642,1.47776666642,1.47776666642,1.47776666642,1.47776666642,1.47776666642,
1.47776666642,1.47776666642,1.47776666642,1.47776666642,1.47776666642,1.47776666642,
1.47776666642),(0.8407444445268,0.8407444445268,0.8407444445268,0.8407444445268,
0.8407444445268,0.8407444445268,0.8407444445268,0.8407444445268,0.8407444445268,
0.8407444445268,0.8407444445268,0.8407444445268,0.8407444445268,0.8407444445268,
0.8407444445268,0.8407444445268,0.8407444445268),(0.8407444445268,0.8407444445268,
0.8407444445268,0.8407444445268,0.8407444445268,0.8407444445268,0.8407444445268,
0.8407444445268,0.8407444445268,0.8407444445268,0.8407444445268,0.8407444445268,
0.8407444445268,0.8407444445268,0.8407444445268,0.8407444445268,0.8407444445268),
(1.47776666642,1.47776666642,1.47776666642,1.47776666642,1.47776666642,
1.47776666642,1.47776666642,1.47776666642,1.47776666642,1.47776666642,1.47776666642,
1.47776666642,1.47776666642,1.47776666642,1.47776666642,1.47776666642,1.47776666642)))
REPRESENTATION_ITEM('')
SURFACE()
);
#2515=(
BOUNDED_SURFACE()
B_SPLINE_SURFACE(3,3,((#141677,#141678,#141679,#141680,#141681,#141682,
#141683,#141684,#141685,#141686,#141687,#141688,#141689,#141690,#141691,
#141692,#141693,#141694,#141695,#141696,#141697,#141698,#141699,#141700,
#141701,#141702,#141703,#141704,#141705,#141706,#141707,#141708,#141709,
#141710,#141711,#141712,#141713,#141714,#141715,#141716,#141717,#141718,
#141719,#141720,#141721,#141722,#141723,#141724,#141725,#141726,#141727,
#141728,#141729,#141730,#141731,#141732,#141733),(#141734,#141735,#141736,
#141737,#141738,#141739,#141740,#141741,#141742,#141743,#141744,#141745,
#141746,#141747,#141748,#141749,#141750,#141751,#141752,#141753,#141754,
#141755,#141756,#141757,#141758,#141759,#141760,#141761,#141762,#141763,
#141764,#141765,#141766,#141767,#141768,#141769,#141770,#141771,#141772,
#141773,#141774,#141775,#141776,#141777,#141778,#141779,#141780,#141781,
#141782,#141783,#141784,#141785,#141786,#141787,#141788,#141789,#141790),
(#141791,#141792,#141793,#141794,#141795,#141796,#141797,#141798,#141799,
#141800,#141801,#141802,#141803,#141804,#141805,#141806,#141807,#141808,
#141809,#141810,#141811,#141812,#141813,#141814,#141815,#141816,#141817,
#141818,#141819,#141820,#141821,#141822,#141823,#141824,#141825,#141826,
#141827,#141828,#141829,#141830,#141831,#141832,#141833,#141834,#141835,
#141836,#141837,#141838,#141839,#141840,#141841,#141842,#141843,#141844,
#141845,#141846,#141847),(#141848,#141849,#141850,#141851,#141852,#141853,
#141854,#141855,#141856,#141857,#141858,#141859,#141860,#141861,#141862,
#141863,#141864,#141865,#141866,#141867,#141868,#141869,#141870,#141871,
#141872,#141873,#141874,#141875,#141876,#141877,#141878,#141879,#141880,
#141881,#141882,#141883,#141884,#141885,#141886,#141887,#141888,#141889,
#141890,#141891,#141892,#141893,#141894,#141895,#141896,#141897,#141898,
#141899,#141900,#141901,#141902,#141903,#141904)),.UNSPECIFIED.,.F.,.F.,
 .F.)
B_SPLINE_SURFACE_WITH_KNOTS((4,4),(4,1,1,1,1,1,1,1,1,1,1,1,1,1,1,1,1,1,
1,1,1,1,1,1,1,1,1,1,1,1,1,1,1,1,1,1,1,1,1,1,1,1,1,1,1,1,1,1,1,1,1,1,1,1,
4),(0.,1.),(0.,0.00102850105811001,0.00759318438410793,0.0139342463721671,
0.0202721319015908,0.0267573495732106,0.0334153340449433,0.0399168198355134,
0.045663172318244,0.0517104759733391,0.0580362016986109,0.0643601149605132,
0.0709346866883761,0.078010969765109,0.0857264910323804,0.0941395929016807,
0.103307185168012,0.113276381440939,0.124079872938569,0.135753629220017,
0.148375964850575,0.162042755872641,0.176849244103508,0.192893057298682,
0.210287271282822,0.229156444467865,0.249639202539587,0.271887793018783,
0.296073149179171,0.322391880247146,0.351041060424109,0.382305717422001,
0.416405241220516,0.453678246748928,0.494467807818825,0.539245592433777,
0.5885590237456,0.638055262903253,0.681623741762806,0.720070723334701,0.754284171425329,
0.784974928394346,0.812861516420407,0.838339911838843,0.861378440096615,
0.882356404231104,0.901543934509106,0.919072351149281,0.935063242320242,
0.949632381127728,0.962891435925974,0.974950552369462,0.985929151039583,
0.995930274056731,1.),.UNSPECIFIED.)
GEOMETRIC_REPRESENTATION_ITEM()
RATIONAL_B_SPLINE_SURFACE(((1.753204347239,1.753204347239,1.753204347239,
1.753204347239,1.753204347239,1.753204347239,1.753204347239,1.753204347239,
1.753204347239,1.753204347239,1.753204347239,1.753204347239,1.753204347239,
1.753204347239,1.753204347239,1.753204347239,1.753204347239,1.753204347239,
1.753204347239,1.753204347239,1.753204347239,1.753204347239,1.753204347239,
1.753204347239,1.753204347239,1.753204347239,1.753204347239,1.753204347239,
1.753204347239,1.753204347239,1.753204347239,1.753204347239,1.753204347239,
1.753204347239,1.753204347239,1.753204347239,1.753204347239,1.753204347239,
1.753204347239,1.753204347239,1.753204347239,1.753204347239,1.753204347239,
1.753204347239,1.753204347239,1.753204347239,1.753204347239,1.753204347239,
1.753204347239,1.753204347239,1.753204347239,1.753204347239,1.753204347239,
1.753204347239,1.753204347239,1.753204347239,1.753204347239),(0.7489318842535,
0.7489318842535,0.7489318842535,0.7489318842535,0.7489318842535,0.7489318842535,
0.7489318842535,0.7489318842535,0.7489318842535,0.7489318842535,0.7489318842535,
0.7489318842535,0.7489318842535,0.7489318842535,0.7489318842535,0.7489318842535,
0.7489318842535,0.7489318842535,0.7489318842535,0.7489318842535,0.7489318842535,
0.7489318842535,0.7489318842535,0.7489318842535,0.7489318842535,0.7489318842535,
0.7489318842535,0.7489318842535,0.7489318842535,0.7489318842535,0.7489318842535,
0.7489318842535,0.7489318842535,0.7489318842535,0.7489318842535,0.7489318842535,
0.7489318842535,0.7489318842535,0.7489318842535,0.7489318842535,0.7489318842535,
0.7489318842535,0.7489318842535,0.7489318842535,0.7489318842535,0.7489318842535,
0.7489318842535,0.7489318842535,0.7489318842535,0.7489318842535,0.7489318842535,
0.7489318842535,0.7489318842535,0.7489318842535,0.7489318842535,0.7489318842535,
0.7489318842535),(0.7489318842535,0.7489318842535,0.7489318842535,0.7489318842535,
0.7489318842535,0.7489318842535,0.7489318842535,0.7489318842535,0.7489318842535,
0.7489318842535,0.7489318842535,0.7489318842535,0.7489318842535,0.7489318842535,
0.7489318842535,0.7489318842535,0.7489318842535,0.7489318842535,0.7489318842535,
0.7489318842535,0.7489318842535,0.7489318842535,0.7489318842535,0.7489318842535,
0.7489318842535,0.7489318842535,0.7489318842535,0.7489318842535,0.7489318842535,
0.7489318842535,0.7489318842535,0.7489318842535,0.7489318842535,0.7489318842535,
0.7489318842535,0.7489318842535,0.7489318842535,0.7489318842535,0.7489318842535,
0.7489318842535,0.7489318842535,0.7489318842535,0.7489318842535,0.7489318842535,
0.7489318842535,0.7489318842535,0.7489318842535,0.7489318842535,0.7489318842535,
0.7489318842535,0.7489318842535,0.7489318842535,0.7489318842535,0.7489318842535,
0.7489318842535,0.7489318842535,0.7489318842535),(1.753204347239,1.753204347239,
1.753204347239,1.753204347239,1.753204347239,1.753204347239,1.753204347239,
1.753204347239,1.753204347239,1.753204347239,1.753204347239,1.753204347239,
1.753204347239,1.753204347239,1.753204347239,1.753204347239,1.753204347239,
1.753204347239,1.753204347239,1.753204347239,1.753204347239,1.753204347239,
1.753204347239,1.753204347239,1.753204347239,1.753204347239,1.753204347239,
1.753204347239,1.753204347239,1.753204347239,1.753204347239,1.753204347239,
1.753204347239,1.753204347239,1.753204347239,1.753204347239,1.753204347239,
1.753204347239,1.753204347239,1.753204347239,1.753204347239,1.753204347239,
1.753204347239,1.753204347239,1.753204347239,1.753204347239,1.753204347239,
1.753204347239,1.753204347239,1.753204347239,1.753204347239,1.753204347239,
1.753204347239,1.753204347239,1.753204347239,1.753204347239,1.753204347239)))
REPRESENTATION_ITEM('')
SURFACE()
);
#2516=(
BOUNDED_SURFACE()
B_SPLINE_SURFACE(3,3,((#143029,#143030,#143031,#143032,#143033,#143034),
(#143035,#143036,#143037,#143038,#143039,#143040),(#143041,#143042,#143043,
#143044,#143045,#143046),(#143047,#143048,#143049,#143050,#143051,#143052)),
 .UNSPECIFIED.,.F.,.F.,.F.)
B_SPLINE_SURFACE_WITH_KNOTS((4,4),(4,1,1,4),(0.,1.),(0.,0.431751876033485,
0.936198433808859,1.),.UNSPECIFIED.)
GEOMETRIC_REPRESENTATION_ITEM()
RATIONAL_B_SPLINE_SURFACE(((1.289342975298,1.289342975298,1.289342975298,
1.289342975298,1.289342975298,1.289342975298),(0.9035523415674,0.9035523415674,
0.9035523415674,0.9035523415674,0.9035523415674,0.9035523415674),(0.9035523415674,
0.9035523415674,0.9035523415674,0.9035523415674,0.9035523415674,0.9035523415674),
(1.289342975298,1.289342975298,1.289342975298,1.289342975298,1.289342975298,
1.289342975298)))
REPRESENTATION_ITEM('')
SURFACE()
);
#2517=(
BOUNDED_SURFACE()
B_SPLINE_SURFACE(3,3,((#143070,#143071,#143072,#143073,#143074,#143075,
#143076,#143077,#143078,#143079),(#143080,#143081,#143082,#143083,#143084,
#143085,#143086,#143087,#143088,#143089),(#143090,#143091,#143092,#143093,
#143094,#143095,#143096,#143097,#143098,#143099),(#143100,#143101,#143102,
#143103,#143104,#143105,#143106,#143107,#143108,#143109)),.UNSPECIFIED.,
 .F.,.F.,.F.)
B_SPLINE_SURFACE_WITH_KNOTS((4,4),(4,1,1,1,1,1,1,4),(0.,1.),(0.,0.0532774375645769,
0.208329877010428,0.378436697484889,0.575701395918878,0.790211251619391,
0.990473980866038,1.),.UNSPECIFIED.)
GEOMETRIC_REPRESENTATION_ITEM()
RATIONAL_B_SPLINE_SURFACE(((1.478656999093,1.478656999093,1.478656999093,
1.478656999093,1.478656999093,1.478656999093,1.478656999093,1.478656999093,
1.478656999093,1.478656999093),(0.8404476669691,0.8404476669691,0.8404476669691,
0.8404476669691,0.8404476669691,0.8404476669691,0.8404476669691,0.8404476669691,
0.8404476669691,0.8404476669691),(0.8404476669691,0.8404476669691,0.8404476669691,
0.8404476669691,0.8404476669691,0.8404476669691,0.8404476669691,0.8404476669691,
0.8404476669691,0.8404476669691),(1.478656999093,1.478656999093,1.478656999093,
1.478656999093,1.478656999093,1.478656999093,1.478656999093,1.478656999093,
1.478656999093,1.478656999093)))
REPRESENTATION_ITEM('')
SURFACE()
);
#2518=(
BOUNDED_SURFACE()
B_SPLINE_SURFACE(3,3,((#143313,#143314,#143315,#143316,#143317,#143318,
#143319,#143320,#143321,#143322),(#143323,#143324,#143325,#143326,#143327,
#143328,#143329,#143330,#143331,#143332),(#143333,#143334,#143335,#143336,
#143337,#143338,#143339,#143340,#143341,#143342),(#143343,#143344,#143345,
#143346,#143347,#143348,#143349,#143350,#143351,#143352)),.UNSPECIFIED.,
 .F.,.F.,.F.)
B_SPLINE_SURFACE_WITH_KNOTS((4,4),(4,1,1,1,1,1,1,4),(0.,1.),(0.,0.0779252083993214,
0.243678133170507,0.415917299399803,0.596243537777757,0.781438784892872,
0.967855482654964,1.),.UNSPECIFIED.)
GEOMETRIC_REPRESENTATION_ITEM()
RATIONAL_B_SPLINE_SURFACE(((1.474156190063,1.474156190063,1.474156190063,
1.474156190063,1.474156190063,1.474156190063,1.474156190063,1.474156190063,
1.474156190063,1.474156190063),(0.8419479366457,0.8419479366457,0.8419479366457,
0.8419479366457,0.8419479366457,0.8419479366457,0.8419479366457,0.8419479366457,
0.8419479366457,0.8419479366457),(0.8419479366457,0.8419479366457,0.8419479366457,
0.8419479366457,0.8419479366457,0.8419479366457,0.8419479366457,0.8419479366457,
0.8419479366457,0.8419479366457),(1.474156190063,1.474156190063,1.474156190063,
1.474156190063,1.474156190063,1.474156190063,1.474156190063,1.474156190063,
1.474156190063,1.474156190063)))
REPRESENTATION_ITEM('')
SURFACE()
);
#2519=(
BOUNDED_SURFACE()
B_SPLINE_SURFACE(3,3,((#143483,#143484,#143485,#143486,#143487,#143488,
#143489,#143490,#143491,#143492),(#143493,#143494,#143495,#143496,#143497,
#143498,#143499,#143500,#143501,#143502),(#143503,#143504,#143505,#143506,
#143507,#143508,#143509,#143510,#143511,#143512),(#143513,#143514,#143515,
#143516,#143517,#143518,#143519,#143520,#143521,#143522)),.UNSPECIFIED.,
 .F.,.F.,.F.)
B_SPLINE_SURFACE_WITH_KNOTS((4,4),(4,1,1,1,1,1,1,4),(0.,1.),(0.,0.0147775451285446,
0.185822509142439,0.356344875612291,0.525759183537156,0.694014694357844,
0.861570783923705,1.),.UNSPECIFIED.)
GEOMETRIC_REPRESENTATION_ITEM()
RATIONAL_B_SPLINE_SURFACE(((1.474127146691,1.474127146691,1.474127146691,
1.474127146691,1.474127146691,1.474127146691,1.474127146691,1.474127146691,
1.474127146691,1.474127146691),(0.8419576177696,0.8419576177696,0.8419576177696,
0.8419576177696,0.8419576177696,0.8419576177696,0.8419576177696,0.8419576177696,
0.8419576177696,0.8419576177696),(0.8419576177696,0.8419576177696,0.8419576177696,
0.8419576177696,0.8419576177696,0.8419576177696,0.8419576177696,0.8419576177696,
0.8419576177696,0.8419576177696),(1.474127146691,1.474127146691,1.474127146691,
1.474127146691,1.474127146691,1.474127146691,1.474127146691,1.474127146691,
1.474127146691,1.474127146691)))
REPRESENTATION_ITEM('')
SURFACE()
);
#2520=(
BOUNDED_SURFACE()
B_SPLINE_SURFACE(3,3,((#143587,#143588,#143589,#143590,#143591,#143592,
#143593,#143594,#143595),(#143596,#143597,#143598,#143599,#143600,#143601,
#143602,#143603,#143604),(#143605,#143606,#143607,#143608,#143609,#143610,
#143611,#143612,#143613),(#143614,#143615,#143616,#143617,#143618,#143619,
#143620,#143621,#143622)),.UNSPECIFIED.,.F.,.F.,.F.)
B_SPLINE_SURFACE_WITH_KNOTS((4,4),(4,1,1,1,1,1,4),(0.,1.),(0.,0.125272810862783,
0.299863569490546,0.48106636157826,0.670112397030726,0.863600947542818,
1.),.UNSPECIFIED.)
GEOMETRIC_REPRESENTATION_ITEM()
RATIONAL_B_SPLINE_SURFACE(((1.30708297461,1.30708297461,1.30708297461,1.30708297461,
1.30708297461,1.30708297461,1.30708297461,1.30708297461,1.30708297461),
(0.8976390084633,0.8976390084633,0.8976390084633,0.8976390084633,0.8976390084633,
0.8976390084633,0.8976390084633,0.8976390084633,0.8976390084633),(0.8976390084633,
0.8976390084633,0.8976390084633,0.8976390084633,0.8976390084633,0.8976390084633,
0.8976390084633,0.8976390084633,0.8976390084633),(1.30708297461,1.30708297461,
1.30708297461,1.30708297461,1.30708297461,1.30708297461,1.30708297461,1.30708297461,
1.30708297461)))
REPRESENTATION_ITEM('')
SURFACE()
);
#2521=(
BOUNDED_SURFACE()
B_SPLINE_SURFACE(3,3,((#143655,#143656,#143657,#143658,#143659,#143660,
#143661,#143662),(#143663,#143664,#143665,#143666,#143667,#143668,#143669,
#143670),(#143671,#143672,#143673,#143674,#143675,#143676,#143677,#143678),
(#143679,#143680,#143681,#143682,#143683,#143684,#143685,#143686)),
 .UNSPECIFIED.,.F.,.F.,.F.)
B_SPLINE_SURFACE_WITH_KNOTS((4,4),(4,1,1,1,1,4),(0.,1.),(0.,0.0104550154603523,
0.283607455569876,0.586586557478444,0.907836751474964,1.),.UNSPECIFIED.)
GEOMETRIC_REPRESENTATION_ITEM()
RATIONAL_B_SPLINE_SURFACE(((1.053280938608,1.053280938608,1.053280938608,
1.053280938608,1.053280938608,1.053280938608,1.053280938608,1.053280938608),
(0.9822396871305,0.9822396871305,0.9822396871305,0.9822396871305,0.9822396871305,
0.9822396871305,0.9822396871305,0.9822396871305),(0.9822396871305,0.9822396871305,
0.9822396871305,0.9822396871305,0.9822396871305,0.9822396871305,0.9822396871305,
0.9822396871305),(1.053280938608,1.053280938608,1.053280938608,1.053280938608,
1.053280938608,1.053280938608,1.053280938608,1.053280938608)))
REPRESENTATION_ITEM('')
SURFACE()
);
#2522=(
BOUNDED_SURFACE()
B_SPLINE_SURFACE(3,3,((#143709,#143710,#143711,#143712,#143713,#143714,
#143715,#143716,#143717),(#143718,#143719,#143720,#143721,#143722,#143723,
#143724,#143725,#143726),(#143727,#143728,#143729,#143730,#143731,#143732,
#143733,#143734,#143735),(#143736,#143737,#143738,#143739,#143740,#143741,
#143742,#143743,#143744)),.UNSPECIFIED.,.F.,.F.,.F.)
B_SPLINE_SURFACE_WITH_KNOTS((4,4),(4,1,1,1,1,1,4),(0.,1.),(0.,0.142766734134771,
0.334374398032124,0.521585124423469,0.701026212149163,0.873921879053949,
1.),.UNSPECIFIED.)
GEOMETRIC_REPRESENTATION_ITEM()
RATIONAL_B_SPLINE_SURFACE(((1.307082945987,1.307082945987,1.307082945987,
1.307082945987,1.307082945987,1.307082945987,1.307082945987,1.307082945987,
1.307082945987),(0.8976390180043,0.8976390180043,0.8976390180043,0.8976390180043,
0.8976390180043,0.8976390180043,0.8976390180043,0.8976390180043,0.8976390180043),
(0.8976390180043,0.8976390180043,0.8976390180043,0.8976390180043,0.8976390180043,
0.8976390180043,0.8976390180043,0.8976390180043,0.8976390180043),(1.307082945987,
1.307082945987,1.307082945987,1.307082945987,1.307082945987,1.307082945987,
1.307082945987,1.307082945987,1.307082945987)))
REPRESENTATION_ITEM('')
SURFACE()
);
#2523=(
BOUNDED_SURFACE()
B_SPLINE_SURFACE(3,3,((#143751,#143752,#143753,#143754,#143755,#143756,
#143757,#143758,#143759,#143760),(#143761,#143762,#143763,#143764,#143765,
#143766,#143767,#143768,#143769,#143770),(#143771,#143772,#143773,#143774,
#143775,#143776,#143777,#143778,#143779,#143780),(#143781,#143782,#143783,
#143784,#143785,#143786,#143787,#143788,#143789,#143790)),.UNSPECIFIED.,
 .F.,.F.,.F.)
B_SPLINE_SURFACE_WITH_KNOTS((4,4),(4,1,1,1,1,1,1,4),(0.,1.),(0.,0.140512983352509,
0.308388853051919,0.476969773176465,0.646706159656357,0.81755755850554,
0.988926783135651,1.),.UNSPECIFIED.)
GEOMETRIC_REPRESENTATION_ITEM()
RATIONAL_B_SPLINE_SURFACE(((1.474127154187,1.474127154187,1.474127154187,
1.474127154187,1.474127154187,1.474127154187,1.474127154187,1.474127154187,
1.474127154187,1.474127154187),(0.8419576152711,0.8419576152711,0.8419576152711,
0.8419576152711,0.8419576152711,0.8419576152711,0.8419576152711,0.8419576152711,
0.8419576152711,0.8419576152711),(0.8419576152711,0.8419576152711,0.8419576152711,
0.8419576152711,0.8419576152711,0.8419576152711,0.8419576152711,0.8419576152711,
0.8419576152711,0.8419576152711),(1.474127154187,1.474127154187,1.474127154187,
1.474127154187,1.474127154187,1.474127154187,1.474127154187,1.474127154187,
1.474127154187,1.474127154187)))
REPRESENTATION_ITEM('')
SURFACE()
);
#2524=(
BOUNDED_SURFACE()
B_SPLINE_SURFACE(3,3,((#143855,#143856,#143857,#143858,#143859,#143860,
#143861,#143862,#143863,#143864),(#143865,#143866,#143867,#143868,#143869,
#143870,#143871,#143872,#143873,#143874),(#143875,#143876,#143877,#143878,
#143879,#143880,#143881,#143882,#143883,#143884),(#143885,#143886,#143887,
#143888,#143889,#143890,#143891,#143892,#143893,#143894)),.UNSPECIFIED.,
 .F.,.F.,.F.)
B_SPLINE_SURFACE_WITH_KNOTS((4,4),(4,1,1,1,1,1,1,4),(0.,1.),(0.,0.0339830500431831,
0.220389385504102,0.405800841682597,0.58634133762222,0.758214941734974,
0.924667979715977,1.),.UNSPECIFIED.)
GEOMETRIC_REPRESENTATION_ITEM()
RATIONAL_B_SPLINE_SURFACE(((1.474147508313,1.474147508313,1.474147508313,
1.474147508313,1.474147508313,1.474147508313,1.474147508313,1.474147508313,
1.474147508313,1.474147508313),(0.8419508305625,0.8419508305625,0.8419508305625,
0.8419508305625,0.8419508305625,0.8419508305625,0.8419508305625,0.8419508305625,
0.8419508305625,0.8419508305625),(0.8419508305625,0.8419508305625,0.8419508305625,
0.8419508305625,0.8419508305625,0.8419508305625,0.8419508305625,0.8419508305625,
0.8419508305625,0.8419508305625),(1.474147508313,1.474147508313,1.474147508313,
1.474147508313,1.474147508313,1.474147508313,1.474147508313,1.474147508313,
1.474147508313,1.474147508313)))
REPRESENTATION_ITEM('')
SURFACE()
);
#2525=(
BOUNDED_SURFACE()
B_SPLINE_SURFACE(3,3,((#144431,#144432,#144433,#144434,#144435,#144436,
#144437,#144438,#144439,#144440,#144441,#144442),(#144443,#144444,#144445,
#144446,#144447,#144448,#144449,#144450,#144451,#144452,#144453,#144454),
(#144455,#144456,#144457,#144458,#144459,#144460,#144461,#144462,#144463,
#144464,#144465,#144466),(#144467,#144468,#144469,#144470,#144471,#144472,
#144473,#144474,#144475,#144476,#144477,#144478)),.UNSPECIFIED.,.F.,.F.,
 .F.)
B_SPLINE_SURFACE_WITH_KNOTS((4,4),(4,1,1,1,1,1,1,1,1,4),(0.,1.),(0.,0.138818488903363,
0.265940452688414,0.381533804843745,0.48830798531101,0.587709442370304,
0.691765681012883,0.798051585674866,0.902466958148731,1.),.UNSPECIFIED.)
GEOMETRIC_REPRESENTATION_ITEM()
RATIONAL_B_SPLINE_SURFACE(((1.438707812053,1.438707812053,1.438707812053,
1.438707812053,1.438707812053,1.438707812053,1.438707812053,1.438707812053,
1.438707812053,1.438707812053,1.438707812053,1.438707812053),(0.853764062649,
0.853764062649,0.853764062649,0.853764062649,0.853764062649,0.853764062649,
0.853764062649,0.853764062649,0.853764062649,0.853764062649,0.853764062649,
0.853764062649),(0.853764062649,0.853764062649,0.853764062649,0.853764062649,
0.853764062649,0.853764062649,0.853764062649,0.853764062649,0.853764062649,
0.853764062649,0.853764062649,0.853764062649),(1.438707812053,1.438707812053,
1.438707812053,1.438707812053,1.438707812053,1.438707812053,1.438707812053,
1.438707812053,1.438707812053,1.438707812053,1.438707812053,1.438707812053)))
REPRESENTATION_ITEM('')
SURFACE()
);
#2526=(
BOUNDED_SURFACE()
B_SPLINE_SURFACE(3,3,((#144481,#144482,#144483,#144484,#144485,#144486,
#144487,#144488,#144489,#144490,#144491,#144492,#144493,#144494,#144495,
#144496),(#144497,#144498,#144499,#144500,#144501,#144502,#144503,#144504,
#144505,#144506,#144507,#144508,#144509,#144510,#144511,#144512),(#144513,
#144514,#144515,#144516,#144517,#144518,#144519,#144520,#144521,#144522,
#144523,#144524,#144525,#144526,#144527,#144528),(#144529,#144530,#144531,
#144532,#144533,#144534,#144535,#144536,#144537,#144538,#144539,#144540,
#144541,#144542,#144543,#144544)),.UNSPECIFIED.,.F.,.F.,.F.)
B_SPLINE_SURFACE_WITH_KNOTS((4,4),(4,1,1,1,1,1,1,1,1,1,1,1,1,4),(0.,1.),
(0.,0.0400287123538256,0.085970757690431,0.136438109413432,0.191920076265951,
0.252892665741402,0.319816049166386,0.393195571222119,0.473564327244262,
0.561361330336151,0.656626165655672,0.760754425605914,0.875598191304292,
1.),.UNSPECIFIED.)
GEOMETRIC_REPRESENTATION_ITEM()
RATIONAL_B_SPLINE_SURFACE(((1.438707901845,1.438707901845,1.438707901845,
1.438707901845,1.438707901845,1.438707901845,1.438707901845,1.438707901845,
1.438707901845,1.438707901845,1.438707901845,1.438707901845,1.438707901845,
1.438707901845,1.438707901845,1.438707901845),(0.8537640327185,0.8537640327185,
0.8537640327185,0.8537640327185,0.8537640327185,0.8537640327185,0.8537640327185,
0.8537640327185,0.8537640327185,0.8537640327185,0.8537640327185,0.8537640327185,
0.8537640327185,0.8537640327185,0.8537640327185,0.8537640327185),(0.8537640327185,
0.8537640327185,0.8537640327185,0.8537640327185,0.8537640327185,0.8537640327185,
0.8537640327185,0.8537640327185,0.8537640327185,0.8537640327185,0.8537640327185,
0.8537640327185,0.8537640327185,0.8537640327185,0.8537640327185,0.8537640327185),
(1.438707901845,1.438707901845,1.438707901845,1.438707901845,1.438707901845,
1.438707901845,1.438707901845,1.438707901845,1.438707901845,1.438707901845,
1.438707901845,1.438707901845,1.438707901845,1.438707901845,1.438707901845,
1.438707901845)))
REPRESENTATION_ITEM('')
SURFACE()
);
#2527=(
BOUNDED_SURFACE()
B_SPLINE_SURFACE(3,3,((#144697,#144698,#144699,#144700,#144701,#144702,
#144703),(#144704,#144705,#144706,#144707,#144708,#144709,#144710),(#144711,
#144712,#144713,#144714,#144715,#144716,#144717),(#144718,#144719,#144720,
#144721,#144722,#144723,#144724)),.UNSPECIFIED.,.F.,.F.,.F.)
B_SPLINE_SURFACE_WITH_KNOTS((4,4),(4,1,1,1,4),(0.,1.),(0.,0.0527467299113482,
0.354834542652793,0.677277799939644,1.),.UNSPECIFIED.)
GEOMETRIC_REPRESENTATION_ITEM()
RATIONAL_B_SPLINE_SURFACE(((1.416282589503,1.416282589503,1.416282589503,
1.416282589503,1.416282589503,1.416282589503,1.416282589503),(0.8612391368322,
0.8612391368322,0.8612391368322,0.8612391368322,0.8612391368322,0.8612391368322,
0.8612391368322),(0.8612391368322,0.8612391368322,0.8612391368322,0.8612391368322,
0.8612391368322,0.8612391368322,0.8612391368322),(1.416282589503,1.416282589503,
1.416282589503,1.416282589503,1.416282589503,1.416282589503,1.416282589503)))
REPRESENTATION_ITEM('')
SURFACE()
);
#2528=(
BOUNDED_SURFACE()
B_SPLINE_SURFACE(3,3,((#144726,#144727,#144728,#144729,#144730,#144731,
#144732,#144733,#144734,#144735,#144736,#144737),(#144738,#144739,#144740,
#144741,#144742,#144743,#144744,#144745,#144746,#144747,#144748,#144749),
(#144750,#144751,#144752,#144753,#144754,#144755,#144756,#144757,#144758,
#144759,#144760,#144761),(#144762,#144763,#144764,#144765,#144766,#144767,
#144768,#144769,#144770,#144771,#144772,#144773)),.UNSPECIFIED.,.F.,.F.,
 .F.)
B_SPLINE_SURFACE_WITH_KNOTS((4,4),(4,1,1,1,1,1,1,1,1,4),(0.,1.),(0.,0.113647120730493,
0.219125808734348,0.329468109271596,0.439978777291567,0.551628244914102,
0.666572223899566,0.781504772087705,0.893407203154914,1.),.UNSPECIFIED.)
GEOMETRIC_REPRESENTATION_ITEM()
RATIONAL_B_SPLINE_SURFACE(((1.411871186478,1.411871186478,1.411871186478,
1.411871186478,1.411871186478,1.411871186478,1.411871186478,1.411871186478,
1.411871186478,1.411871186478,1.411871186478,1.411871186478),(0.8627096045073,
0.8627096045073,0.8627096045073,0.8627096045073,0.8627096045073,0.8627096045073,
0.8627096045073,0.8627096045073,0.8627096045073,0.8627096045073,0.8627096045073,
0.8627096045073),(0.8627096045073,0.8627096045073,0.8627096045073,0.8627096045073,
0.8627096045073,0.8627096045073,0.8627096045073,0.8627096045073,0.8627096045073,
0.8627096045073,0.8627096045073,0.8627096045073),(1.411871186478,1.411871186478,
1.411871186478,1.411871186478,1.411871186478,1.411871186478,1.411871186478,
1.411871186478,1.411871186478,1.411871186478,1.411871186478,1.411871186478)))
REPRESENTATION_ITEM('')
SURFACE()
);
#2529=(
BOUNDED_SURFACE()
B_SPLINE_SURFACE(3,3,((#144849,#144850,#144851,#144852,#144853,#144854),
(#144855,#144856,#144857,#144858,#144859,#144860),(#144861,#144862,#144863,
#144864,#144865,#144866),(#144867,#144868,#144869,#144870,#144871,#144872)),
 .UNSPECIFIED.,.F.,.F.,.F.)
B_SPLINE_SURFACE_WITH_KNOTS((4,4),(4,1,1,4),(0.,1.),(0.,0.373237854628505,
0.718584603248465,1.),.UNSPECIFIED.)
GEOMETRIC_REPRESENTATION_ITEM()
RATIONAL_B_SPLINE_SURFACE(((1.416338033926,1.416338033926,1.416338033926,
1.416338033926,1.416338033926,1.416338033926),(0.861220655358,0.861220655358,
0.861220655358,0.861220655358,0.861220655358,0.861220655358),(0.861220655358,
0.861220655358,0.861220655358,0.861220655358,0.861220655358,0.861220655358),
(1.416338033926,1.416338033926,1.416338033926,1.416338033926,1.416338033926,
1.416338033926)))
REPRESENTATION_ITEM('')
SURFACE()
);
#2530=(
BOUNDED_SURFACE()
B_SPLINE_SURFACE(3,3,((#144894,#144895,#144896,#144897,#144898,#144899,
#144900,#144901,#144902,#144903,#144904,#144905,#144906,#144907),(#144908,
#144909,#144910,#144911,#144912,#144913,#144914,#144915,#144916,#144917,
#144918,#144919,#144920,#144921),(#144922,#144923,#144924,#144925,#144926,
#144927,#144928,#144929,#144930,#144931,#144932,#144933,#144934,#144935),
(#144936,#144937,#144938,#144939,#144940,#144941,#144942,#144943,#144944,
#144945,#144946,#144947,#144948,#144949)),.UNSPECIFIED.,.F.,.F.,.F.)
B_SPLINE_SURFACE_WITH_KNOTS((4,4),(4,1,1,1,1,1,1,1,1,1,1,4),(0.,1.),(0.,
0.0189196969648684,0.123026245101233,0.22799245863482,0.333423755560677,
0.4381783971276,0.543725879883426,0.653238579359784,0.762171136752647,0.869991259904252,
0.976017729140831,1.),.UNSPECIFIED.)
GEOMETRIC_REPRESENTATION_ITEM()
RATIONAL_B_SPLINE_SURFACE(((1.411894266579,1.411894266579,1.411894266579,
1.411894266579,1.411894266579,1.411894266579,1.411894266579,1.411894266579,
1.411894266579,1.411894266579,1.411894266579,1.411894266579,1.411894266579,
1.411894266579),(0.8627019111402,0.8627019111402,0.8627019111402,0.8627019111402,
0.8627019111402,0.8627019111402,0.8627019111402,0.8627019111402,0.8627019111402,
0.8627019111402,0.8627019111402,0.8627019111402,0.8627019111402,0.8627019111402),
(0.8627019111402,0.8627019111402,0.8627019111402,0.8627019111402,0.8627019111402,
0.8627019111402,0.8627019111402,0.8627019111402,0.8627019111402,0.8627019111402,
0.8627019111402,0.8627019111402,0.8627019111402,0.8627019111402),(1.411894266579,
1.411894266579,1.411894266579,1.411894266579,1.411894266579,1.411894266579,
1.411894266579,1.411894266579,1.411894266579,1.411894266579,1.411894266579,
1.411894266579,1.411894266579,1.411894266579)))
REPRESENTATION_ITEM('')
SURFACE()
);
#2531=(
BOUNDED_SURFACE()
B_SPLINE_SURFACE(3,3,((#145190,#145191,#145192,#145193,#145194,#145195,
#145196,#145197),(#145198,#145199,#145200,#145201,#145202,#145203,#145204,
#145205),(#145206,#145207,#145208,#145209,#145210,#145211,#145212,#145213),
(#145214,#145215,#145216,#145217,#145218,#145219,#145220,#145221)),
 .UNSPECIFIED.,.F.,.F.,.F.)
B_SPLINE_SURFACE_WITH_KNOTS((4,4),(4,1,1,1,1,4),(0.,1.),(0.,0.0014184679519637,
0.26748144230672,0.529910202206513,0.793736319541623,1.),.UNSPECIFIED.)
GEOMETRIC_REPRESENTATION_ITEM()
RATIONAL_B_SPLINE_SURFACE(((1.400814311523,1.400814311523,1.400814311523,
1.400814311523,1.400814311523,1.400814311523,1.400814311523,1.400814311523),
(0.8663952294922,0.8663952294922,0.8663952294922,0.8663952294922,0.8663952294922,
0.8663952294922,0.8663952294922,0.8663952294922),(0.8663952294922,0.8663952294922,
0.8663952294922,0.8663952294922,0.8663952294922,0.8663952294922,0.8663952294922,
0.8663952294922),(1.400814311523,1.400814311523,1.400814311523,1.400814311523,
1.400814311523,1.400814311523,1.400814311523,1.400814311523)))
REPRESENTATION_ITEM('')
SURFACE()
);
#2532=(
BOUNDED_SURFACE()
B_SPLINE_SURFACE(3,3,((#145223,#145224,#145225,#145226),(#145227,#145228,
#145229,#145230),(#145231,#145232,#145233,#145234),(#145235,#145236,#145237,
#145238)),.UNSPECIFIED.,.F.,.F.,.F.)
B_SPLINE_SURFACE_WITH_KNOTS((4,4),(4,4),(0.,1.),(0.,1.),.UNSPECIFIED.)
GEOMETRIC_REPRESENTATION_ITEM()
RATIONAL_B_SPLINE_SURFACE(((1.292992000439,1.292992000439,1.292992000439,
1.292992000439),(0.9023359998537,0.9023359998537,0.9023359998537,0.9023359998537),
(0.9023359998537,0.9023359998537,0.9023359998537,0.9023359998537),(1.292992000439,
1.292992000439,1.292992000439,1.292992000439)))
REPRESENTATION_ITEM('')
SURFACE()
);
#2533=(
BOUNDED_SURFACE()
B_SPLINE_SURFACE(3,3,((#145638,#145639,#145640,#145641,#145642,#145643,
#145644,#145645,#145646,#145647,#145648,#145649,#145650,#145651,#145652,
#145653),(#145654,#145655,#145656,#145657,#145658,#145659,#145660,#145661,
#145662,#145663,#145664,#145665,#145666,#145667,#145668,#145669),(#145670,
#145671,#145672,#145673,#145674,#145675,#145676,#145677,#145678,#145679,
#145680,#145681,#145682,#145683,#145684,#145685),(#145686,#145687,#145688,
#145689,#145690,#145691,#145692,#145693,#145694,#145695,#145696,#145697,
#145698,#145699,#145700,#145701)),.UNSPECIFIED.,.F.,.F.,.F.)
B_SPLINE_SURFACE_WITH_KNOTS((4,4),(4,1,1,1,1,1,1,1,1,1,1,1,1,4),(0.,1.),
(0.,0.0559219040610143,0.119566494393519,0.185306102594679,0.252047391027673,
0.319960693178036,0.38890975610616,0.458498614355498,0.530499085950225,
0.608940039864404,0.696077429834816,0.792156237533156,0.898636382678449,
1.),.UNSPECIFIED.)
GEOMETRIC_REPRESENTATION_ITEM()
RATIONAL_B_SPLINE_SURFACE(((1.307002971129,1.307002971129,1.307002971129,
1.307002971129,1.307002971129,1.307002971129,1.307002971129,1.307002971129,
1.307002971129,1.307002971129,1.307002971129,1.307002971129,1.307002971129,
1.307002971129,1.307002971129,1.307002971129),(0.8976656762905,0.8976656762905,
0.8976656762905,0.8976656762905,0.8976656762905,0.8976656762905,0.8976656762905,
0.8976656762905,0.8976656762905,0.8976656762905,0.8976656762905,0.8976656762905,
0.8976656762905,0.8976656762905,0.8976656762905,0.8976656762905),(0.8976656762905,
0.8976656762905,0.8976656762905,0.8976656762905,0.8976656762905,0.8976656762905,
0.8976656762905,0.8976656762905,0.8976656762905,0.8976656762905,0.8976656762905,
0.8976656762905,0.8976656762905,0.8976656762905,0.8976656762905,0.8976656762905),
(1.307002971129,1.307002971129,1.307002971129,1.307002971129,1.307002971129,
1.307002971129,1.307002971129,1.307002971129,1.307002971129,1.307002971129,
1.307002971129,1.307002971129,1.307002971129,1.307002971129,1.307002971129,
1.307002971129)))
REPRESENTATION_ITEM('')
SURFACE()
);
#2534=(
BOUNDED_SURFACE()
B_SPLINE_SURFACE(3,3,((#145952,#145953,#145954,#145955,#145956,#145957,
#145958,#145959,#145960,#145961,#145962,#145963,#145964),(#145965,#145966,
#145967,#145968,#145969,#145970,#145971,#145972,#145973,#145974,#145975,
#145976,#145977),(#145978,#145979,#145980,#145981,#145982,#145983,#145984,
#145985,#145986,#145987,#145988,#145989,#145990),(#145991,#145992,#145993,
#145994,#145995,#145996,#145997,#145998,#145999,#146000,#146001,#146002,
#146003)),.UNSPECIFIED.,.F.,.F.,.F.)
B_SPLINE_SURFACE_WITH_KNOTS((4,4),(4,1,1,1,1,1,1,1,1,1,4),(0.,1.),(0.,0.0361770017020252,
0.110322638446908,0.191341394631034,0.279299595253617,0.374729923390192,
0.478819817310066,0.592531700959653,0.717431194571663,0.855542845896087,
1.),.UNSPECIFIED.)
GEOMETRIC_REPRESENTATION_ITEM()
RATIONAL_B_SPLINE_SURFACE(((1.17157330090261,1.17157330090261,1.17157330090261,
1.17157330090261,1.17157330090261,1.17157330090261,1.17157330090261,1.17157330090261,
1.17157330090261,1.17157330090261,1.17157330090261,1.17157330090261,1.17157330090261),
(0.942808938970757,0.942808938970757,0.942808938970757,0.942808938970757,
0.942808938970757,0.942808938970757,0.942808938970757,0.942808938970757,
0.942808938970757,0.942808938970757,0.942808938970757,0.942808938970757,
0.942808938970757),(0.942808899699103,0.942808899699103,0.942808899699103,
0.942808899699103,0.942808899699103,0.942808899699103,0.942808899699103,
0.942808899699103,0.942808899699103,0.942808899699103,0.942808899699103,
0.942808899699103,0.942808899699103),(1.17157318308765,1.17157318308765,
1.17157318308765,1.17157318308765,1.17157318308765,1.17157318308765,1.17157318308765,
1.17157318308765,1.17157318308765,1.17157318308765,1.17157318308765,1.17157318308765,
1.17157318308765)))
REPRESENTATION_ITEM('')
SURFACE()
);
#2535=(
BOUNDED_SURFACE()
B_SPLINE_SURFACE(3,3,((#146010,#146011,#146012,#146013,#146014,#146015),
(#146016,#146017,#146018,#146019,#146020,#146021),(#146022,#146023,#146024,
#146025,#146026,#146027),(#146028,#146029,#146030,#146031,#146032,#146033)),
 .UNSPECIFIED.,.F.,.F.,.F.)
B_SPLINE_SURFACE_WITH_KNOTS((4,4),(4,1,1,4),(0.,1.),(0.,0.143192077928725,
0.593387555486125,1.),.UNSPECIFIED.)
GEOMETRIC_REPRESENTATION_ITEM()
RATIONAL_B_SPLINE_SURFACE(((1.365448016002,1.365448016002,1.365448016002,
1.365448016002,1.365448016002,1.365448016002),(0.878183994666,0.878183994666,
0.878183994666,0.878183994666,0.878183994666,0.878183994666),(0.878183994666,
0.878183994666,0.878183994666,0.878183994666,0.878183994666,0.878183994666),
(1.365448016002,1.365448016002,1.365448016002,1.365448016002,1.365448016002,
1.365448016002)))
REPRESENTATION_ITEM('')
SURFACE()
);
#2536=(
BOUNDED_SURFACE()
B_SPLINE_SURFACE(3,3,((#146131,#146132,#146133,#146134,#146135,#146136,
#146137,#146138,#146139),(#146140,#146141,#146142,#146143,#146144,#146145,
#146146,#146147,#146148),(#146149,#146150,#146151,#146152,#146153,#146154,
#146155,#146156,#146157),(#146158,#146159,#146160,#146161,#146162,#146163,
#146164,#146165,#146166)),.UNSPECIFIED.,.F.,.F.,.F.)
B_SPLINE_SURFACE_WITH_KNOTS((4,4),(4,1,1,1,1,1,4),(0.,1.),(0.,0.210945365171019,
0.440528327664717,0.642835784013808,0.823409899665082,0.985793689031676,
1.),.UNSPECIFIED.)
GEOMETRIC_REPRESENTATION_ITEM()
RATIONAL_B_SPLINE_SURFACE(((1.289189279229,1.289189279229,1.289189279229,
1.289189279229,1.289189279229,1.289189279229,1.289189279229,1.289189279229,
1.289189279229),(0.9036035735905,0.9036035735905,0.9036035735905,0.9036035735905,
0.9036035735905,0.9036035735905,0.9036035735905,0.9036035735905,0.9036035735905),
(0.9036035735905,0.9036035735905,0.9036035735905,0.9036035735905,0.9036035735905,
0.9036035735905,0.9036035735905,0.9036035735905,0.9036035735905),(1.289189279229,
1.289189279229,1.289189279229,1.289189279229,1.289189279229,1.289189279229,
1.289189279229,1.289189279229,1.289189279229)))
REPRESENTATION_ITEM('')
SURFACE()
);
#2537=(
BOUNDED_SURFACE()
B_SPLINE_SURFACE(3,3,((#146194,#146195,#146196,#146197,#146198,#146199,
#146200,#146201),(#146202,#146203,#146204,#146205,#146206,#146207,#146208,
#146209),(#146210,#146211,#146212,#146213,#146214,#146215,#146216,#146217),
(#146218,#146219,#146220,#146221,#146222,#146223,#146224,#146225)),
 .UNSPECIFIED.,.F.,.F.,.F.)
B_SPLINE_SURFACE_WITH_KNOTS((4,4),(4,1,1,1,1,4),(0.,1.),(0.,0.0487760373381725,
0.313271775641559,0.605696041835668,0.929388134239699,1.),.UNSPECIFIED.)
GEOMETRIC_REPRESENTATION_ITEM()
RATIONAL_B_SPLINE_SURFACE(((1.19718919652,1.19718919652,1.19718919652,1.19718919652,
1.19718919652,1.19718919652,1.19718919652,1.19718919652),(0.9342702678265,
0.9342702678265,0.9342702678265,0.9342702678265,0.9342702678265,0.9342702678265,
0.9342702678265,0.9342702678265),(0.9342702678265,0.9342702678265,0.9342702678265,
0.9342702678265,0.9342702678265,0.9342702678265,0.9342702678265,0.9342702678265),
(1.19718919652,1.19718919652,1.19718919652,1.19718919652,1.19718919652,
1.19718919652,1.19718919652,1.19718919652)))
REPRESENTATION_ITEM('')
SURFACE()
);
#2538=(
BOUNDED_SURFACE()
B_SPLINE_SURFACE(3,3,((#146429,#146430,#146431,#146432,#146433,#146434,
#146435,#146436),(#146437,#146438,#146439,#146440,#146441,#146442,#146443,
#146444),(#146445,#146446,#146447,#146448,#146449,#146450,#146451,#146452),
(#146453,#146454,#146455,#146456,#146457,#146458,#146459,#146460)),
 .UNSPECIFIED.,.F.,.F.,.F.)
B_SPLINE_SURFACE_WITH_KNOTS((4,4),(4,1,1,1,1,4),(0.,1.),(0.,0.218953851268331,
0.474954346235349,0.702206697993898,0.905113568673651,1.),.UNSPECIFIED.)
GEOMETRIC_REPRESENTATION_ITEM()
RATIONAL_B_SPLINE_SURFACE(((1.289211918215,1.289211918215,1.289211918215,
1.289211918215,1.289211918215,1.289211918215,1.289211918215,1.289211918215),
(0.9035960272617,0.9035960272617,0.9035960272617,0.9035960272617,0.9035960272617,
0.9035960272617,0.9035960272617,0.9035960272617),(0.9035960272617,0.9035960272617,
0.9035960272617,0.9035960272617,0.9035960272617,0.9035960272617,0.9035960272617,
0.9035960272617),(1.289211918215,1.289211918215,1.289211918215,1.289211918215,
1.289211918215,1.289211918215,1.289211918215,1.289211918215)))
REPRESENTATION_ITEM('')
SURFACE()
);
#2539=(
BOUNDED_SURFACE()
B_SPLINE_SURFACE(3,3,((#146696,#146697,#146698,#146699,#146700,#146701,
#146702,#146703,#146704,#146705,#146706,#146707,#146708),(#146709,#146710,
#146711,#146712,#146713,#146714,#146715,#146716,#146717,#146718,#146719,
#146720,#146721),(#146722,#146723,#146724,#146725,#146726,#146727,#146728,
#146729,#146730,#146731,#146732,#146733,#146734),(#146735,#146736,#146737,
#146738,#146739,#146740,#146741,#146742,#146743,#146744,#146745,#146746,
#146747)),.UNSPECIFIED.,.F.,.F.,.F.)
B_SPLINE_SURFACE_WITH_KNOTS((4,4),(4,1,1,1,1,1,1,1,1,1,4),(0.,1.),(0.,0.0617308889043711,
0.222967927738356,0.364574399931382,0.491340784341846,0.605251267138888,
0.708180598151713,0.801277211250371,0.885526519088398,0.96089518018748,
1.),.UNSPECIFIED.)
GEOMETRIC_REPRESENTATION_ITEM()
RATIONAL_B_SPLINE_SURFACE(((1.225181244217,1.225181244217,1.225181244217,
1.225181244217,1.225181244217,1.225181244217,1.225181244217,1.225181244217,
1.225181244217,1.225181244217,1.225181244217,1.225181244217,1.225181244217),
(0.9249395852609,0.9249395852609,0.9249395852609,0.9249395852609,0.9249395852609,
0.9249395852609,0.9249395852609,0.9249395852609,0.9249395852609,0.9249395852609,
0.9249395852609,0.9249395852609,0.9249395852609),(0.9249395852609,0.9249395852609,
0.9249395852609,0.9249395852609,0.9249395852609,0.9249395852609,0.9249395852609,
0.9249395852609,0.9249395852609,0.9249395852609,0.9249395852609,0.9249395852609,
0.9249395852609),(1.225181244217,1.225181244217,1.225181244217,1.225181244217,
1.225181244217,1.225181244217,1.225181244217,1.225181244217,1.225181244217,
1.225181244217,1.225181244217,1.225181244217,1.225181244217)))
REPRESENTATION_ITEM('')
SURFACE()
);
#2540=(
BOUNDED_SURFACE()
B_SPLINE_SURFACE(3,3,((#146837,#146838,#146839,#146840,#146841,#146842,
#146843,#146844,#146845,#146846,#146847,#146848,#146849,#146850,#146851,
#146852,#146853),(#146854,#146855,#146856,#146857,#146858,#146859,#146860,
#146861,#146862,#146863,#146864,#146865,#146866,#146867,#146868,#146869,
#146870),(#146871,#146872,#146873,#146874,#146875,#146876,#146877,#146878,
#146879,#146880,#146881,#146882,#146883,#146884,#146885,#146886,#146887),
(#146888,#146889,#146890,#146891,#146892,#146893,#146894,#146895,#146896,
#146897,#146898,#146899,#146900,#146901,#146902,#146903,#146904)),
 .UNSPECIFIED.,.F.,.F.,.F.)
B_SPLINE_SURFACE_WITH_KNOTS((4,4),(4,1,1,1,1,1,1,1,1,1,1,1,1,1,4),(0.,1.),
(0.,0.0169119460810613,0.0654242130848353,0.118166345404895,0.175802236516308,
0.238929210760529,0.307690566088615,0.381894800562219,0.461375561007429,
0.546721723948187,0.639112945312709,0.739719346812922,0.849650913359874,
0.96995594614347,1.),.UNSPECIFIED.)
GEOMETRIC_REPRESENTATION_ITEM()
RATIONAL_B_SPLINE_SURFACE(((1.02563715093864,1.02563715093864,1.02563715093864,
1.02563715093864,1.02563715093864,1.02563715093864,1.02563715093864,1.02563715093864,
1.02563715093864,1.02563715093864,1.02563715093864,1.02563715093864,1.02563715093864,
1.02563715093864,1.02563715093864,1.02563715093864,1.02563715093864),(1.00821461019054,
1.00821461019054,1.00821461019054,1.00821461019054,1.00821461019054,1.00821461019054,
1.00821461019054,1.00821461019054,1.00821461019054,1.00821461019054,1.00821461019054,
1.00821461019054,1.00821461019054,1.00821461019054,1.00821461019054,1.00821461019054,
1.00821461019054),(0.999672100423032,0.999672100423032,0.999672100423032,
0.999672100423032,0.999672100423032,0.999672100423032,0.999672100423032,
0.999672100423032,0.999672100423032,0.999672100423032,0.999672100423032,
0.999672100423032,0.999672100423032,0.999672100423032,0.999672100423032,
0.999672100423032,0.999672100423032),(1.00000962163611,1.00000962163611,
1.00000962163611,1.00000962163611,1.00000962163611,1.00000962163611,1.00000962163611,
1.00000962163611,1.00000962163611,1.00000962163611,1.00000962163611,1.00000962163611,
1.00000962163611,1.00000962163611,1.00000962163611,1.00000962163611,1.00000962163611)))
REPRESENTATION_ITEM('')
SURFACE()
);
#2541=(
BOUNDED_SURFACE()
B_SPLINE_SURFACE(3,3,((#146935,#146936,#146937,#146938,#146939,#146940),
(#146941,#146942,#146943,#146944,#146945,#146946),(#146947,#146948,#146949,
#146950,#146951,#146952),(#146953,#146954,#146955,#146956,#146957,#146958)),
 .UNSPECIFIED.,.F.,.F.,.F.)
B_SPLINE_SURFACE_WITH_KNOTS((4,4),(4,1,1,4),(0.,1.),(0.,0.330743299833935,
0.694013975265241,1.),.UNSPECIFIED.)
GEOMETRIC_REPRESENTATION_ITEM()
RATIONAL_B_SPLINE_SURFACE(((1.289433315103,1.289433315103,1.289433315103,
1.289433315103,1.289433315103,1.289433315103),(0.9035222282991,0.9035222282991,
0.9035222282991,0.9035222282991,0.9035222282991,0.9035222282991),(0.9035222282991,
0.9035222282991,0.9035222282991,0.9035222282991,0.9035222282991,0.9035222282991),
(1.289433315103,1.289433315103,1.289433315103,1.289433315103,1.289433315103,
1.289433315103)))
REPRESENTATION_ITEM('')
SURFACE()
);
#2542=(
BOUNDED_SURFACE()
B_SPLINE_SURFACE(3,3,((#147219,#147220,#147221,#147222,#147223,#147224,
#147225,#147226,#147227,#147228,#147229),(#147230,#147231,#147232,#147233,
#147234,#147235,#147236,#147237,#147238,#147239,#147240),(#147241,#147242,
#147243,#147244,#147245,#147246,#147247,#147248,#147249,#147250,#147251),
(#147252,#147253,#147254,#147255,#147256,#147257,#147258,#147259,#147260,
#147261,#147262)),.UNSPECIFIED.,.F.,.F.,.F.)
B_SPLINE_SURFACE_WITH_KNOTS((4,4),(4,1,1,1,1,1,1,1,4),(0.,1.),(0.,0.09718625494397,
0.209222889679937,0.33412363069135,0.473952091224752,0.627037941696765,
0.768578301480889,0.892964492195342,1.),.UNSPECIFIED.)
GEOMETRIC_REPRESENTATION_ITEM()
RATIONAL_B_SPLINE_SURFACE(((1.155039452605,1.155039452605,1.155039452605,
1.155039452605,1.155039452605,1.155039452605,1.155039452605,1.155039452605,
1.155039452605,1.155039452605,1.155039452605),(0.9483201824649,0.9483201824649,
0.9483201824649,0.9483201824649,0.9483201824649,0.9483201824649,0.9483201824649,
0.9483201824649,0.9483201824649,0.9483201824649,0.9483201824649),(0.9483201824649,
0.9483201824649,0.9483201824649,0.9483201824649,0.9483201824649,0.9483201824649,
0.9483201824649,0.9483201824649,0.9483201824649,0.9483201824649,0.9483201824649),
(1.155039452605,1.155039452605,1.155039452605,1.155039452605,1.155039452605,
1.155039452605,1.155039452605,1.155039452605,1.155039452605,1.155039452605,
1.155039452605)))
REPRESENTATION_ITEM('')
SURFACE()
);
#2543=(
BOUNDED_SURFACE()
B_SPLINE_SURFACE(3,3,((#147376,#147377,#147378,#147379,#147380,#147381),
(#147382,#147383,#147384,#147385,#147386,#147387),(#147388,#147389,#147390,
#147391,#147392,#147393),(#147394,#147395,#147396,#147397,#147398,#147399)),
 .UNSPECIFIED.,.F.,.F.,.F.)
B_SPLINE_SURFACE_WITH_KNOTS((4,4),(4,1,1,4),(0.,1.),(0.,0.335198257973395,
0.677912136352372,1.),.UNSPECIFIED.)
GEOMETRIC_REPRESENTATION_ITEM()
RATIONAL_B_SPLINE_SURFACE(((1.097833560248,1.097833560248,1.097833560248,
1.097833560248,1.097833560248,1.097833560248),(0.9673888132507,0.9673888132507,
0.9673888132507,0.9673888132507,0.9673888132507,0.9673888132507),(0.9673888132507,
0.9673888132507,0.9673888132507,0.9673888132507,0.9673888132507,0.9673888132507),
(1.097833560248,1.097833560248,1.097833560248,1.097833560248,1.097833560248,
1.097833560248)))
REPRESENTATION_ITEM('')
SURFACE()
);
#2544=(
BOUNDED_SURFACE()
B_SPLINE_SURFACE(3,3,((#147427,#147428,#147429,#147430),(#147431,#147432,
#147433,#147434),(#147435,#147436,#147437,#147438),(#147439,#147440,#147441,
#147442)),.UNSPECIFIED.,.F.,.F.,.F.)
B_SPLINE_SURFACE_WITH_KNOTS((4,4),(4,4),(0.,1.),(0.,1.),.UNSPECIFIED.)
GEOMETRIC_REPRESENTATION_ITEM()
RATIONAL_B_SPLINE_SURFACE(((1.007258252712,0.8716678894048,0.857683274695,
0.9653044085823),(1.006827278554,0.879287880805,0.8661336322704,0.9673645329503),
(1.00640304118,0.8867887601249,0.8744518978764,0.9693924544342),(1.006012840932,
0.8936878339527,0.882102778005,0.971257673089)))
REPRESENTATION_ITEM('')
SURFACE()
);
#2545=(
BOUNDED_SURFACE()
B_SPLINE_SURFACE(3,3,((#147485,#147486,#147487,#147488,#147489,#147490,
#147491,#147492,#147493,#147494,#147495,#147496,#147497,#147498,#147499,
#147500,#147501,#147502,#147503,#147504,#147505,#147506),(#147507,#147508,
#147509,#147510,#147511,#147512,#147513,#147514,#147515,#147516,#147517,
#147518,#147519,#147520,#147521,#147522,#147523,#147524,#147525,#147526,
#147527,#147528),(#147529,#147530,#147531,#147532,#147533,#147534,#147535,
#147536,#147537,#147538,#147539,#147540,#147541,#147542,#147543,#147544,
#147545,#147546,#147547,#147548,#147549,#147550),(#147551,#147552,#147553,
#147554,#147555,#147556,#147557,#147558,#147559,#147560,#147561,#147562,
#147563,#147564,#147565,#147566,#147567,#147568,#147569,#147570,#147571,
#147572)),.UNSPECIFIED.,.F.,.F.,.F.)
B_SPLINE_SURFACE_WITH_KNOTS((4,4),(4,1,1,1,1,1,1,1,1,1,1,1,1,1,1,1,1,1,
1,4),(0.,1.),(0.,0.0711383255328258,0.137163359302248,0.195720435393546,
0.247715273019436,0.293698370802659,0.336008737306656,0.380005256943101,
0.425168878602564,0.469947554154179,0.513213820955286,0.55641075188751,
0.604436817371917,0.658671873052936,0.719515049298376,0.788488856663347,
0.862062739446009,0.932266724631227,0.998927768427254,1.),.UNSPECIFIED.)
GEOMETRIC_REPRESENTATION_ITEM()
RATIONAL_B_SPLINE_SURFACE(((1.255321345493,1.255321345493,1.255321345493,
1.255321345493,1.255321345493,1.255321345493,1.255321345493,1.255321345493,
1.255321345493,1.255321345493,1.255321345493,1.255321345493,1.255321345493,
1.255321345493,1.255321345493,1.255321345493,1.255321345493,1.255321345493,
1.255321345493,1.255321345493,1.255321345493,1.255321345493),(0.9148928848357,
0.9148928848357,0.9148928848357,0.9148928848357,0.9148928848357,0.9148928848357,
0.9148928848357,0.9148928848357,0.9148928848357,0.9148928848357,0.9148928848357,
0.9148928848357,0.9148928848357,0.9148928848357,0.9148928848357,0.9148928848357,
0.9148928848357,0.9148928848357,0.9148928848357,0.9148928848357,0.9148928848357,
0.9148928848357),(0.9148928848357,0.9148928848357,0.9148928848357,0.9148928848357,
0.9148928848357,0.9148928848357,0.9148928848357,0.9148928848357,0.9148928848357,
0.9148928848357,0.9148928848357,0.9148928848357,0.9148928848357,0.9148928848357,
0.9148928848357,0.9148928848357,0.9148928848357,0.9148928848357,0.9148928848357,
0.9148928848357,0.9148928848357,0.9148928848357),(1.255321345493,1.255321345493,
1.255321345493,1.255321345493,1.255321345493,1.255321345493,1.255321345493,
1.255321345493,1.255321345493,1.255321345493,1.255321345493,1.255321345493,
1.255321345493,1.255321345493,1.255321345493,1.255321345493,1.255321345493,
1.255321345493,1.255321345493,1.255321345493,1.255321345493,1.255321345493)))
REPRESENTATION_ITEM('')
SURFACE()
);
#2546=(
BOUNDED_SURFACE()
B_SPLINE_SURFACE(3,3,((#147722,#147723,#147724,#147725,#147726,#147727,
#147728,#147729,#147730,#147731,#147732,#147733,#147734,#147735,#147736),
(#147737,#147738,#147739,#147740,#147741,#147742,#147743,#147744,#147745,
#147746,#147747,#147748,#147749,#147750,#147751),(#147752,#147753,#147754,
#147755,#147756,#147757,#147758,#147759,#147760,#147761,#147762,#147763,
#147764,#147765,#147766),(#147767,#147768,#147769,#147770,#147771,#147772,
#147773,#147774,#147775,#147776,#147777,#147778,#147779,#147780,#147781)),
 .UNSPECIFIED.,.F.,.F.,.F.)
B_SPLINE_SURFACE_WITH_KNOTS((4,4),(4,1,1,1,1,1,1,1,1,1,1,1,4),(0.,1.),(0.,
0.00433344281298221,0.0666934882632817,0.132801776489929,0.205016366496403,
0.284357715917161,0.370665202265106,0.46484948769096,0.568277692564041,
0.682614773264253,0.810064514841178,0.952973196107536,1.),.UNSPECIFIED.)
GEOMETRIC_REPRESENTATION_ITEM()
RATIONAL_B_SPLINE_SURFACE(((1.116717554521,1.116717554521,1.116717554521,
1.116717554521,1.116717554521,1.116717554521,1.116717554521,1.116717554521,
1.116717554521,1.116717554521,1.116717554521,1.116717554521,1.116717554521,
1.116717554521,1.116717554521),(0.9610941484931,0.9610941484931,0.9610941484931,
0.9610941484931,0.9610941484931,0.9610941484931,0.9610941484931,0.9610941484931,
0.9610941484931,0.9610941484931,0.9610941484931,0.9610941484931,0.9610941484931,
0.9610941484931,0.9610941484931),(0.9610941484931,0.9610941484931,0.9610941484931,
0.9610941484931,0.9610941484931,0.9610941484931,0.9610941484931,0.9610941484931,
0.9610941484931,0.9610941484931,0.9610941484931,0.9610941484931,0.9610941484931,
0.9610941484931,0.9610941484931),(1.116717554521,1.116717554521,1.116717554521,
1.116717554521,1.116717554521,1.116717554521,1.116717554521,1.116717554521,
1.116717554521,1.116717554521,1.116717554521,1.116717554521,1.116717554521,
1.116717554521,1.116717554521)))
REPRESENTATION_ITEM('')
SURFACE()
);
#2547=(
BOUNDED_SURFACE()
B_SPLINE_SURFACE(3,3,((#147835,#147836,#147837,#147838,#147839,#147840,
#147841,#147842,#147843,#147844,#147845,#147846,#147847,#147848,#147849,
#147850,#147851,#147852,#147853,#147854,#147855,#147856,#147857,#147858,
#147859,#147860,#147861,#147862,#147863,#147864,#147865,#147866),(#147867,
#147868,#147869,#147870,#147871,#147872,#147873,#147874,#147875,#147876,
#147877,#147878,#147879,#147880,#147881,#147882,#147883,#147884,#147885,
#147886,#147887,#147888,#147889,#147890,#147891,#147892,#147893,#147894,
#147895,#147896,#147897,#147898),(#147899,#147900,#147901,#147902,#147903,
#147904,#147905,#147906,#147907,#147908,#147909,#147910,#147911,#147912,
#147913,#147914,#147915,#147916,#147917,#147918,#147919,#147920,#147921,
#147922,#147923,#147924,#147925,#147926,#147927,#147928,#147929,#147930),
(#147931,#147932,#147933,#147934,#147935,#147936,#147937,#147938,#147939,
#147940,#147941,#147942,#147943,#147944,#147945,#147946,#147947,#147948,
#147949,#147950,#147951,#147952,#147953,#147954,#147955,#147956,#147957,
#147958,#147959,#147960,#147961,#147962)),.UNSPECIFIED.,.F.,.F.,.F.)
B_SPLINE_SURFACE_WITH_KNOTS((4,4),(4,1,1,1,1,1,1,1,1,1,1,1,1,1,1,1,1,1,
1,1,1,1,1,1,1,1,1,1,1,4),(0.,1.),(0.,0.00739679806268109,0.0171434919654321,
0.0278671486052808,0.0396906394914082,0.0527364856978208,0.0671005283054457,
0.0828041080432213,0.09991535616353,0.118571172417619,0.13891405612076,
0.161058401251212,0.185059763604759,0.211052408434658,0.23922330365136,
0.269821407003499,0.303084978001006,0.338803301575319,0.377356136968251,
0.419277131157154,0.465109562725025,0.515198516585569,0.569694099550452,
0.628581626647206,0.692308097186769,0.762043150357223,0.838144940217723,
0.913367566845421,0.976864842465518,1.),.UNSPECIFIED.)
GEOMETRIC_REPRESENTATION_ITEM()
RATIONAL_B_SPLINE_SURFACE(((1.778014213746,1.778014213746,1.778014213746,
1.778014213746,1.778014213746,1.778014213746,1.778014213746,1.778014213746,
1.778014213746,1.778014213746,1.778014213746,1.778014213746,1.778014213746,
1.778014213746,1.778014213746,1.778014213746,1.778014213746,1.778014213746,
1.778014213746,1.778014213746,1.778014213746,1.778014213746,1.778014213746,
1.778014213746,1.778014213746,1.778014213746,1.778014213746,1.778014213746,
1.778014213746,1.778014213746,1.778014213746,1.778014213746),(0.7406619287514,
0.7406619287514,0.7406619287514,0.7406619287514,0.7406619287514,0.7406619287514,
0.7406619287514,0.7406619287514,0.7406619287514,0.7406619287514,0.7406619287514,
0.7406619287514,0.7406619287514,0.7406619287514,0.7406619287514,0.7406619287514,
0.7406619287514,0.7406619287514,0.7406619287514,0.7406619287514,0.7406619287514,
0.7406619287514,0.7406619287514,0.7406619287514,0.7406619287514,0.7406619287514,
0.7406619287514,0.7406619287514,0.7406619287514,0.7406619287514,0.7406619287514,
0.7406619287514),(0.7406619287514,0.7406619287514,0.7406619287514,0.7406619287514,
0.7406619287514,0.7406619287514,0.7406619287514,0.7406619287514,0.7406619287514,
0.7406619287514,0.7406619287514,0.7406619287514,0.7406619287514,0.7406619287514,
0.7406619287514,0.7406619287514,0.7406619287514,0.7406619287514,0.7406619287514,
0.7406619287514,0.7406619287514,0.7406619287514,0.7406619287514,0.7406619287514,
0.7406619287514,0.7406619287514,0.7406619287514,0.7406619287514,0.7406619287514,
0.7406619287514,0.7406619287514,0.7406619287514),(1.778014213746,1.778014213746,
1.778014213746,1.778014213746,1.778014213746,1.778014213746,1.778014213746,
1.778014213746,1.778014213746,1.778014213746,1.778014213746,1.778014213746,
1.778014213746,1.778014213746,1.778014213746,1.778014213746,1.778014213746,
1.778014213746,1.778014213746,1.778014213746,1.778014213746,1.778014213746,
1.778014213746,1.778014213746,1.778014213746,1.778014213746,1.778014213746,
1.778014213746,1.778014213746,1.778014213746,1.778014213746,1.778014213746)))
REPRESENTATION_ITEM('')
SURFACE()
);
#2548=(
BOUNDED_SURFACE()
B_SPLINE_SURFACE(3,3,((#147977,#147978,#147979,#147980),(#147981,#147982,
#147983,#147984),(#147985,#147986,#147987,#147988),(#147989,#147990,#147991,
#147992)),.UNSPECIFIED.,.F.,.F.,.F.)
B_SPLINE_SURFACE_WITH_KNOTS((4,4),(4,4),(0.,1.),(0.,1.),.UNSPECIFIED.)
GEOMETRIC_REPRESENTATION_ITEM()
RATIONAL_B_SPLINE_SURFACE(((1.1173473569,1.1173473569,1.1173473569,1.1173473569),
(0.9608842143667,0.9608842143667,0.9608842143667,0.9608842143667),(0.9608842143667,
0.9608842143667,0.9608842143667,0.9608842143667),(1.1173473569,1.1173473569,
1.1173473569,1.1173473569)))
REPRESENTATION_ITEM('')
SURFACE()
);
#2549=(
BOUNDED_SURFACE()
B_SPLINE_SURFACE(3,3,((#147999,#148000,#148001,#148002,#148003,#148004,
#148005,#148006,#148007,#148008,#148009,#148010,#148011,#148012,#148013,
#148014,#148015,#148016,#148017,#148018),(#148019,#148020,#148021,#148022,
#148023,#148024,#148025,#148026,#148027,#148028,#148029,#148030,#148031,
#148032,#148033,#148034,#148035,#148036,#148037,#148038),(#148039,#148040,
#148041,#148042,#148043,#148044,#148045,#148046,#148047,#148048,#148049,
#148050,#148051,#148052,#148053,#148054,#148055,#148056,#148057,#148058),
(#148059,#148060,#148061,#148062,#148063,#148064,#148065,#148066,#148067,
#148068,#148069,#148070,#148071,#148072,#148073,#148074,#148075,#148076,
#148077,#148078)),.UNSPECIFIED.,.F.,.F.,.F.)
B_SPLINE_SURFACE_WITH_KNOTS((4,4),(4,1,1,1,1,1,1,1,1,1,1,1,1,1,1,1,1,4),
(0.,1.),(0.,0.0634473073458767,0.137474475480583,0.203439315591922,0.266070813426101,
0.333494447777073,0.401437472430427,0.464401084256882,0.51858368764375,
0.569769560865856,0.622221496328389,0.67514181525029,0.727526446084146,
0.778774499915783,0.832231436034466,0.891640084181608,0.951727885385323,
1.),.UNSPECIFIED.)
GEOMETRIC_REPRESENTATION_ITEM()
RATIONAL_B_SPLINE_SURFACE(((1.186029185783,1.186029185783,1.186029185783,
1.186029185783,1.186029185783,1.186029185783,1.186029185783,1.186029185783,
1.186029185783,1.186029185783,1.186029185783,1.186029185783,1.186029185783,
1.186029185783,1.186029185783,1.186029185783,1.186029185783,1.186029185783,
1.186029185783,1.186029185783),(0.9379902714058,0.9379902714058,0.9379902714058,
0.9379902714058,0.9379902714058,0.9379902714058,0.9379902714058,0.9379902714058,
0.9379902714058,0.9379902714058,0.9379902714058,0.9379902714058,0.9379902714058,
0.9379902714058,0.9379902714058,0.9379902714058,0.9379902714058,0.9379902714058,
0.9379902714058,0.9379902714058),(0.9379902714058,0.9379902714058,0.9379902714058,
0.9379902714058,0.9379902714058,0.9379902714058,0.9379902714058,0.9379902714058,
0.9379902714058,0.9379902714058,0.9379902714058,0.9379902714058,0.9379902714058,
0.9379902714058,0.9379902714058,0.9379902714058,0.9379902714058,0.9379902714058,
0.9379902714058,0.9379902714058),(1.186029185783,1.186029185783,1.186029185783,
1.186029185783,1.186029185783,1.186029185783,1.186029185783,1.186029185783,
1.186029185783,1.186029185783,1.186029185783,1.186029185783,1.186029185783,
1.186029185783,1.186029185783,1.186029185783,1.186029185783,1.186029185783,
1.186029185783,1.186029185783)))
REPRESENTATION_ITEM('')
SURFACE()
);
#2550=(
BOUNDED_SURFACE()
B_SPLINE_SURFACE(3,3,((#148208,#148209,#148210,#148211,#148212,#148213,
#148214,#148215,#148216,#148217),(#148218,#148219,#148220,#148221,#148222,
#148223,#148224,#148225,#148226,#148227),(#148228,#148229,#148230,#148231,
#148232,#148233,#148234,#148235,#148236,#148237),(#148238,#148239,#148240,
#148241,#148242,#148243,#148244,#148245,#148246,#148247)),.UNSPECIFIED.,
 .F.,.F.,.F.)
B_SPLINE_SURFACE_WITH_KNOTS((4,4),(4,1,1,1,1,1,1,4),(0.,1.),(0.,0.00515718315225492,
0.135375072417774,0.281251016648657,0.443276496267116,0.622074124477441,
0.818604636422717,1.),.UNSPECIFIED.)
GEOMETRIC_REPRESENTATION_ITEM()
RATIONAL_B_SPLINE_SURFACE(((1.54356298079,1.54356298079,1.54356298079,1.54356298079,
1.54356298079,1.54356298079,1.54356298079,1.54356298079,1.54356298079,1.54356298079),
(0.8188123397367,0.8188123397367,0.8188123397367,0.8188123397367,0.8188123397367,
0.8188123397367,0.8188123397367,0.8188123397367,0.8188123397367,0.8188123397367),
(0.8188123397367,0.8188123397367,0.8188123397367,0.8188123397367,0.8188123397367,
0.8188123397367,0.8188123397367,0.8188123397367,0.8188123397367,0.8188123397367),
(1.54356298079,1.54356298079,1.54356298079,1.54356298079,1.54356298079,
1.54356298079,1.54356298079,1.54356298079,1.54356298079,1.54356298079)))
REPRESENTATION_ITEM('')
SURFACE()
);
#2551=(
BOUNDED_SURFACE()
B_SPLINE_SURFACE(3,3,((#148418,#148419,#148420,#148421,#148422,#148423,
#148424,#148425),(#148426,#148427,#148428,#148429,#148430,#148431,#148432,
#148433),(#148434,#148435,#148436,#148437,#148438,#148439,#148440,#148441),
(#148442,#148443,#148444,#148445,#148446,#148447,#148448,#148449)),
 .UNSPECIFIED.,.F.,.F.,.F.)
B_SPLINE_SURFACE_WITH_KNOTS((4,4),(4,1,1,1,1,4),(0.,1.),(0.,0.018056873287542,
0.345151041851993,0.669351068431515,0.992791000152672,1.),.UNSPECIFIED.)
GEOMETRIC_REPRESENTATION_ITEM()
RATIONAL_B_SPLINE_SURFACE(((1.546274274408,1.546274274408,1.546274274408,
1.546274274408,1.546274274408,1.546274274408,1.546274274408,1.546274274408),
(0.8179085751973,0.8179085751973,0.8179085751973,0.8179085751973,0.8179085751973,
0.8179085751973,0.8179085751973,0.8179085751973),(0.8179085751973,0.8179085751973,
0.8179085751973,0.8179085751973,0.8179085751973,0.8179085751973,0.8179085751973,
0.8179085751973),(1.546274274408,1.546274274408,1.546274274408,1.546274274408,
1.546274274408,1.546274274408,1.546274274408,1.546274274408)))
REPRESENTATION_ITEM('')
SURFACE()
);
#2552=(
BOUNDED_SURFACE()
B_SPLINE_SURFACE(3,3,((#148459,#148460,#148461,#148462,#148463,#148464),
(#148465,#148466,#148467,#148468,#148469,#148470),(#148471,#148472,#148473,
#148474,#148475,#148476),(#148477,#148478,#148479,#148480,#148481,#148482)),
 .UNSPECIFIED.,.F.,.F.,.F.)
B_SPLINE_SURFACE_WITH_KNOTS((4,4),(4,1,1,4),(0.,1.),(0.,0.31080225069139,
0.761591972733954,1.),.UNSPECIFIED.)
GEOMETRIC_REPRESENTATION_ITEM()
RATIONAL_B_SPLINE_SURFACE(((1.187262794735,1.187262794735,1.187262794735,
1.187262794735,1.187262794735,1.187262794735),(0.9375790684218,0.9375790684218,
0.9375790684218,0.9375790684218,0.9375790684218,0.9375790684218),(0.9375790684218,
0.9375790684218,0.9375790684218,0.9375790684218,0.9375790684218,0.9375790684218),
(1.187262794735,1.187262794735,1.187262794735,1.187262794735,1.187262794735,
1.187262794735)))
REPRESENTATION_ITEM('')
SURFACE()
);
#2553=(
BOUNDED_SURFACE()
B_SPLINE_SURFACE(3,3,((#148542,#148543,#148544,#148545),(#148546,#148547,
#148548,#148549),(#148550,#148551,#148552,#148553),(#148554,#148555,#148556,
#148557)),.UNSPECIFIED.,.F.,.F.,.F.)
B_SPLINE_SURFACE_WITH_KNOTS((4,4),(4,4),(0.,1.),(0.,1.),.UNSPECIFIED.)
GEOMETRIC_REPRESENTATION_ITEM()
RATIONAL_B_SPLINE_SURFACE(((1.011180720188,0.8618966200521,0.8618556159516,
1.011057707886),(1.011640235655,0.8562207209891,0.8561780316645,1.011512167682),
(1.01213768218,0.8500763004794,0.8500317868227,1.01200414121),(1.012657343954,
0.8436574789567,0.8436110594958,1.012518085571)))
REPRESENTATION_ITEM('')
SURFACE()
);
#2554=(
BOUNDED_SURFACE()
B_SPLINE_SURFACE(3,3,((#148566,#148567,#148568,#148569),(#148570,#148571,
#148572,#148573),(#148574,#148575,#148576,#148577),(#148578,#148579,#148580,
#148581)),.UNSPECIFIED.,.F.,.F.,.F.)
B_SPLINE_SURFACE_WITH_KNOTS((4,4),(4,4),(0.,1.),(0.,1.),.UNSPECIFIED.)
GEOMETRIC_REPRESENTATION_ITEM()
RATIONAL_B_SPLINE_SURFACE(((1.010409839248,0.8769632993351,0.8769431939423,
1.010349523069),(1.01120923021,0.8675150817268,0.8674934324034,1.01114428224),
(1.012237722807,0.8553590500252,0.8553354142881,1.012166815596),(1.013244124764,
0.8434641135782,0.8434385340929,1.013167386308)))
REPRESENTATION_ITEM('')
SURFACE()
);
#2555=(
BOUNDED_SURFACE()
B_SPLINE_SURFACE(3,3,((#148995,#148996,#148997,#148998),(#148999,#149000,
#149001,#149002),(#149003,#149004,#149005,#149006),(#149007,#149008,#149009,
#149010)),.UNSPECIFIED.,.F.,.F.,.F.)
B_SPLINE_SURFACE_WITH_KNOTS((4,4),(4,4),(0.,1.),(0.,1.),.UNSPECIFIED.)
GEOMETRIC_REPRESENTATION_ITEM()
RATIONAL_B_SPLINE_SURFACE(((1.013235612141,0.8434362301637,0.8434372659622,
1.013238719536),(1.012229953762,0.8553321413794,0.8553330984767,1.012232825054),
(1.011193573923,0.867591456086,0.8675923320778,1.011196201899),(1.010402717632,
0.8769464780539,0.8769472921545,1.010405159934)))
REPRESENTATION_ITEM('')
SURFACE()
);
#2556=(
BOUNDED_SURFACE()
B_SPLINE_SURFACE(3,3,((#149118,#149119,#149120,#149121),(#149122,#149123,
#149124,#149125),(#149126,#149127,#149128,#149129),(#149130,#149131,#149132,
#149133)),.UNSPECIFIED.,.F.,.F.,.F.)
B_SPLINE_SURFACE_WITH_KNOTS((4,4),(4,4),(0.,1.),(0.,1.),.UNSPECIFIED.)
GEOMETRIC_REPRESENTATION_ITEM()
RATIONAL_B_SPLINE_SURFACE(((1.010400602958,0.8769605371814,0.8769497680482,
1.010368295558),(1.011189967337,0.8676223315438,0.8676107450762,1.011155207934),
(1.012219596932,0.8554417807797,0.8554291281992,1.012181639191),(1.01323329396,
0.8434497127943,0.8434360105978,1.013192187371)))
REPRESENTATION_ITEM('')
SURFACE()
);
#2557=(
BOUNDED_SURFACE()
B_SPLINE_SURFACE(3,3,((#149564,#149565,#149566,#149567),(#149568,#149569,
#149570,#149571),(#149572,#149573,#149574,#149575),(#149576,#149577,#149578,
#149579)),.UNSPECIFIED.,.F.,.F.,.F.)
B_SPLINE_SURFACE_WITH_KNOTS((4,4),(4,4),(0.,1.),(0.,1.),.UNSPECIFIED.)
GEOMETRIC_REPRESENTATION_ITEM()
RATIONAL_B_SPLINE_SURFACE(((1.013249647536,0.8434881174035,0.8434387387947,
1.01310151171),(1.012238397043,0.8554335459903,0.8553879360963,1.012101567361),
(1.0112206302,0.8674559491715,0.8674141322774,1.011095179517),(1.01041429526,
0.8769808062689,0.876941994413,1.010297859693)))
REPRESENTATION_ITEM('')
SURFACE()
);
#2558=(
BOUNDED_SURFACE()
B_SPLINE_SURFACE(3,3,((#149607,#149608,#149609,#149610),(#149611,#149612,
#149613,#149614),(#149615,#149616,#149617,#149618),(#149619,#149620,#149621,
#149622)),.UNSPECIFIED.,.F.,.F.,.F.)
B_SPLINE_SURFACE_WITH_KNOTS((4,4),(4,4),(0.,1.),(0.,1.),.UNSPECIFIED.)
GEOMETRIC_REPRESENTATION_ITEM()
RATIONAL_B_SPLINE_SURFACE(((1.012658416243,0.843652975638,0.8436063190053,
1.012518446345),(1.012143467457,0.850013227104,0.8499684684794,1.012009191583),
(1.011645124798,0.8561683724535,0.8561254506298,1.011516359326),(1.011180895029,
0.8619021816099,0.8618609708532,1.011057262759)))
REPRESENTATION_ITEM('')
SURFACE()
);
#2559=(
BOUNDED_SURFACE()
B_SPLINE_SURFACE(3,3,((#150260,#150261,#150262,#150263),(#150264,#150265,
#150266,#150267),(#150268,#150269,#150270,#150271),(#150272,#150273,#150274,
#150275)),.UNSPECIFIED.,.F.,.F.,.F.)
B_SPLINE_SURFACE_WITH_KNOTS((4,4),(4,4),(0.,1.),(0.,1.),.UNSPECIFIED.)
GEOMETRIC_REPRESENTATION_ITEM()
RATIONAL_B_SPLINE_SURFACE(((1.013249647536,0.8434881174035,0.8434387387948,
1.01310151171),(1.012238397043,0.8554335459903,0.8553879360964,1.012101567361),
(1.0112206302,0.8674559491716,0.8674141322775,1.011095179517),(1.01041429526,
0.876980806269,0.8769419944131,1.010297859693)))
REPRESENTATION_ITEM('')
SURFACE()
);
#2560=(
BOUNDED_SURFACE()
B_SPLINE_SURFACE(3,3,((#150602,#150603,#150604,#150605),(#150606,#150607,
#150608,#150609),(#150610,#150611,#150612,#150613),(#150614,#150615,#150616,
#150617)),.UNSPECIFIED.,.F.,.F.,.F.)
B_SPLINE_SURFACE_WITH_KNOTS((4,4),(4,4),(0.,1.),(0.,1.),.UNSPECIFIED.)
GEOMETRIC_REPRESENTATION_ITEM()
RATIONAL_B_SPLINE_SURFACE(((1.010400602958,0.8769605371815,0.8769497680483,
1.010368295558),(1.011189967337,0.8676223315439,0.8676107450763,1.011155207934),
(1.012219596932,0.8554417807799,0.8554291281992,1.01218163919),(1.01323329396,
0.8434497127945,0.8434360105979,1.01319218737)))
REPRESENTATION_ITEM('')
SURFACE()
);
#2561=(
BOUNDED_SURFACE()
B_SPLINE_SURFACE(3,3,((#150690,#150691,#150692,#150693),(#150694,#150695,
#150696,#150697),(#150698,#150699,#150700,#150701),(#150702,#150703,#150704,
#150705)),.UNSPECIFIED.,.F.,.F.,.F.)
B_SPLINE_SURFACE_WITH_KNOTS((4,4),(4,4),(0.,1.),(0.,1.),.UNSPECIFIED.)
GEOMETRIC_REPRESENTATION_ITEM()
RATIONAL_B_SPLINE_SURFACE(((1.011180720188,0.8618966200521,0.8618556159514,
1.011057707886),(1.011640235656,0.8562207209891,0.8561780316643,1.011512167682),
(1.012137682181,0.8500763004794,0.8500317868225,1.01200414121),(1.012657343955,
0.8436574789567,0.8436110594956,1.012518085571)))
REPRESENTATION_ITEM('')
SURFACE()
);
#2562=(
BOUNDED_SURFACE()
B_SPLINE_SURFACE(3,3,((#150815,#150816,#150817,#150818),(#150819,#150820,
#150821,#150822),(#150823,#150824,#150825,#150826),(#150827,#150828,#150829,
#150830)),.UNSPECIFIED.,.F.,.F.,.F.)
B_SPLINE_SURFACE_WITH_KNOTS((4,4),(4,4),(0.,1.),(0.,1.),.UNSPECIFIED.)
GEOMETRIC_REPRESENTATION_ITEM()
RATIONAL_B_SPLINE_SURFACE(((1.012658416244,0.8436529756379,0.843606319005,
1.012518446345),(1.012143467457,0.850013227104,0.8499684684792,1.012009191583),
(1.011645124798,0.8561683724535,0.8561254506296,1.011516359326),(1.011180895029,
0.8619021816099,0.861860970853,1.011057262759)))
REPRESENTATION_ITEM('')
SURFACE()
);
#2563=(
BOUNDED_SURFACE()
B_SPLINE_SURFACE(3,3,((#150837,#150838,#150839,#150840),(#150841,#150842,
#150843,#150844),(#150845,#150846,#150847,#150848),(#150849,#150850,#150851,
#150852)),.UNSPECIFIED.,.F.,.F.,.F.)
B_SPLINE_SURFACE_WITH_KNOTS((4,4),(4,4),(0.,1.),(0.,1.),.UNSPECIFIED.)
GEOMETRIC_REPRESENTATION_ITEM()
RATIONAL_B_SPLINE_SURFACE(((1.01323561214,0.8434362301639,0.8434372659623,
1.013238719536),(1.012229953762,0.8553321413796,0.8553330984767,1.012232825053),
(1.011193573923,0.8675914560862,0.8675923320778,1.011196201898),(1.010402717632,
0.8769464780541,0.8769472921545,1.010405159933)))
REPRESENTATION_ITEM('')
SURFACE()
);
#2564=(
BOUNDED_SURFACE()
B_SPLINE_SURFACE(3,3,((#151147,#151148,#151149,#151150),(#151151,#151152,
#151153,#151154),(#151155,#151156,#151157,#151158),(#151159,#151160,#151161,
#151162)),.UNSPECIFIED.,.F.,.F.,.F.)
B_SPLINE_SURFACE_WITH_KNOTS((4,4),(4,4),(0.,1.),(0.,1.),.UNSPECIFIED.)
GEOMETRIC_REPRESENTATION_ITEM()
RATIONAL_B_SPLINE_SURFACE(((1.010409839247,0.8769632993348,0.8769431939425,
1.01034952307),(1.011209230209,0.8675150817265,0.8674934324036,1.01114428224),
(1.012237722807,0.8553590500249,0.8553354142882,1.012166815597),(1.013244124763,
0.8434641135779,0.8434385340931,1.013167386309)))
REPRESENTATION_ITEM('')
SURFACE()
);
#2565=(
BOUNDED_SURFACE()
B_SPLINE_SURFACE(3,3,((#151686,#151687,#151688,#151689),(#151690,#151691,
#151692,#151693),(#151694,#151695,#151696,#151697),(#151698,#151699,#151700,
#151701)),.UNSPECIFIED.,.F.,.F.,.F.)
B_SPLINE_SURFACE_WITH_KNOTS((4,4),(4,4),(0.,1.),(0.,1.),.UNSPECIFIED.)
GEOMETRIC_REPRESENTATION_ITEM()
RATIONAL_B_SPLINE_SURFACE(((1.010417420083,0.8327746891999,0.8327405236387,
1.0103149234),(1.008972082557,0.855975924729,0.8559464993787,1.008883806506),
(1.007744072525,0.8756885174588,0.8756631195597,1.007667878827),(1.007061933964,
0.8866385254159,0.8866153646972,1.006992451808)))
REPRESENTATION_ITEM('')
SURFACE()
);
#2566=(
BOUNDED_SURFACE()
B_SPLINE_SURFACE(3,3,((#151933,#151934,#151935,#151936),(#151937,#151938,
#151939,#151940),(#151941,#151942,#151943,#151944),(#151945,#151946,#151947,
#151948)),.UNSPECIFIED.,.F.,.F.,.F.)
B_SPLINE_SURFACE_WITH_KNOTS((4,4),(4,4),(0.,1.),(0.,1.),.UNSPECIFIED.)
GEOMETRIC_REPRESENTATION_ITEM()
RATIONAL_B_SPLINE_SURFACE(((1.,1.,1.,1.),(0.9999761823555,1.000244831856,
1.000245109353,0.9999770148458),(1.001594007107,0.9836145123668,0.983595940764,
1.001538292299),(1.005023743582,0.9483587695743,0.9483002384861,1.004848150317)))
REPRESENTATION_ITEM('')
SURFACE()
);
#2567=(
BOUNDED_SURFACE()
B_SPLINE_SURFACE(3,3,((#153169,#153170,#153171,#153172),(#153173,#153174,
#153175,#153176),(#153177,#153178,#153179,#153180),(#153181,#153182,#153183,
#153184)),.UNSPECIFIED.,.F.,.F.,.F.)
B_SPLINE_SURFACE_WITH_KNOTS((4,4),(4,4),(0.,1.),(0.,1.),.UNSPECIFIED.)
GEOMETRIC_REPRESENTATION_ITEM()
RATIONAL_B_SPLINE_SURFACE(((1.007042941756,0.8866336160624,0.8866223630418,
1.007009182694),(1.00772434029,0.8756655162888,0.8756531745481,1.007687315068),
(1.008958893915,0.8557935813658,0.8557792670889,1.008915951085),(1.010389488669,
0.832766079544,0.8327494795017,1.010339688542)))
REPRESENTATION_ITEM('')
SURFACE()
);
#2568=(
BOUNDED_SURFACE()
B_SPLINE_SURFACE(3,3,((#153235,#153236,#153237,#153238),(#153239,#153240,
#153241,#153242),(#153243,#153244,#153245,#153246),(#153247,#153248,#153249,
#153250)),.UNSPECIFIED.,.F.,.F.,.F.)
B_SPLINE_SURFACE_WITH_KNOTS((4,4),(4,4),(0.,1.),(0.,1.),.UNSPECIFIED.)
GEOMETRIC_REPRESENTATION_ITEM()
RATIONAL_B_SPLINE_SURFACE(((1.,1.,1.,1.),(0.9999865607556,1.000144735869,
1.000144432799,0.999985651546),(1.001528719443,0.9835362368208,0.9835707111406,
1.001632142403),(1.004804655344,0.9482555755455,0.9483639258552,1.005129706273)))
REPRESENTATION_ITEM('')
SURFACE()
);
#2569=(
BOUNDED_SURFACE()
B_SPLINE_SURFACE(3,3,((#153265,#153266,#153267,#153268),(#153269,#153270,
#153271,#153272),(#153273,#153274,#153275,#153276),(#153277,#153278,#153279,
#153280)),.UNSPECIFIED.,.F.,.F.,.F.)
B_SPLINE_SURFACE_WITH_KNOTS((4,4),(4,4),(0.,1.),(0.,1.),.UNSPECIFIED.)
GEOMETRIC_REPRESENTATION_ITEM()
RATIONAL_B_SPLINE_SURFACE(((1.007751232385,0.8441927077371,0.8441759670975,
1.007701010467),(1.007532711944,0.8485851806412,0.8485689119488,1.007483905867),
(1.00730599456,0.8531424200671,0.8531266410251,1.007258657434),(1.00707431254,
0.8577994534751,0.8577841748059,1.007028476532)))
REPRESENTATION_ITEM('')
SURFACE()
);
#2570=(
BOUNDED_SURFACE()
B_SPLINE_SURFACE(3,3,((#153653,#153654,#153655,#153656),(#153657,#153658,
#153659,#153660),(#153661,#153662,#153663,#153664),(#153665,#153666,#153667,
#153668)),.UNSPECIFIED.,.F.,.F.,.F.)
B_SPLINE_SURFACE_WITH_KNOTS((4,4),(4,4),(0.,1.),(0.,1.),.UNSPECIFIED.)
GEOMETRIC_REPRESENTATION_ITEM()
RATIONAL_B_SPLINE_SURFACE(((1.007074258056,0.8577963970444,0.8577811874664,
1.007028629322),(1.007304418006,0.8531698236429,0.8531541192235,1.007257304748),
(1.007532328373,0.8485884703757,0.8485722759515,1.0074837451),(1.007750873574,
0.8441953715068,0.8441787072129,1.007700880692)))
REPRESENTATION_ITEM('')
SURFACE()
);
#2571=(
BOUNDED_SURFACE()
B_SPLINE_SURFACE(3,3,((#153847,#153848,#153849,#153850),(#153851,#153852,
#153853,#153854),(#153855,#153856,#153857,#153858),(#153859,#153860,#153861,
#153862)),.UNSPECIFIED.,.F.,.F.,.F.)
B_SPLINE_SURFACE_WITH_KNOTS((4,4),(4,4),(0.,1.),(0.,1.),.UNSPECIFIED.)
GEOMETRIC_REPRESENTATION_ITEM()
RATIONAL_B_SPLINE_SURFACE(((1.008509940924,0.8799663128153,0.8799421151717,
1.008437347994),(1.009061509065,0.8721863812946,0.8721606152913,1.008984211055),
(1.009661139189,0.8637285300159,0.8637010589907,1.009578726113),(1.010270334951,
0.8551357543165,0.8551065510698,1.010182725211)))
REPRESENTATION_ITEM('')
SURFACE()
);
#2572=(
BOUNDED_SURFACE()
B_SPLINE_SURFACE(3,3,((#154082,#154083,#154084,#154085),(#154086,#154087,
#154088,#154089),(#154090,#154091,#154092,#154093),(#154094,#154095,#154096,
#154097)),.UNSPECIFIED.,.F.,.F.,.F.)
B_SPLINE_SURFACE_WITH_KNOTS((4,4),(4,4),(0.,1.),(0.,1.),.UNSPECIFIED.)
GEOMETRIC_REPRESENTATION_ITEM()
RATIONAL_B_SPLINE_SURFACE(((1.010270521476,0.855133113183,0.8551039195422,
1.010182940553),(1.009662767308,0.863705555624,0.8636780895057,1.009580368953),
(1.009062759899,0.8721687291531,0.8721429685373,1.008985478052),(1.008509452897,
0.8799731880642,0.8799490002066,1.008436889324)))
REPRESENTATION_ITEM('')
SURFACE()
);
#2573=(
BOUNDED_SURFACE()
B_SPLINE_SURFACE(3,3,((#154178,#154179,#154180,#154181),(#154182,#154183,
#154184,#154185),(#154186,#154187,#154188,#154189),(#154190,#154191,#154192,
#154193)),.UNSPECIFIED.,.F.,.F.,.F.)
B_SPLINE_SURFACE_WITH_KNOTS((4,4),(4,4),(0.,1.),(0.,1.),.UNSPECIFIED.)
GEOMETRIC_REPRESENTATION_ITEM()
RATIONAL_B_SPLINE_SURFACE(((1.010390527686,0.8555764834497,0.8555484358643,
1.01030638493),(1.009638708354,0.8660264235414,0.8660004053733,1.009560653849),
(1.008824865687,0.8773384592094,0.8773146378808,1.008753401701),(1.008356067081,
0.8838545424531,0.8838319865722,1.008288399438)))
REPRESENTATION_ITEM('')
SURFACE()
);
#2574=(
BOUNDED_SURFACE()
B_SPLINE_SURFACE(3,3,((#154234,#154235,#154236,#154237),(#154238,#154239,
#154240,#154241),(#154242,#154243,#154244,#154245),(#154246,#154247,#154248,
#154249)),.UNSPECIFIED.,.F.,.F.,.F.)
B_SPLINE_SURFACE_WITH_KNOTS((4,4),(4,4),(0.,1.),(0.,1.),.UNSPECIFIED.)
GEOMETRIC_REPRESENTATION_ITEM()
RATIONAL_B_SPLINE_SURFACE(((1.008132395777,0.8893233508291,0.8892957763681,
1.008049672393),(1.008118961572,0.8895061816728,0.889478652763,1.008036374842),
(1.008279269408,0.8873244956603,0.8872964231958,1.008195052014),(1.008608872932,
0.8828388047798,0.8828096147308,1.008521302784)))
REPRESENTATION_ITEM('')
SURFACE()
);
#2575=(
BOUNDED_SURFACE()
B_SPLINE_SURFACE(3,3,((#154315,#154316,#154317,#154318),(#154319,#154320,
#154321,#154322),(#154323,#154324,#154325,#154326),(#154327,#154328,#154329,
#154330)),.UNSPECIFIED.,.F.,.F.,.F.)
B_SPLINE_SURFACE_WITH_KNOTS((4,4),(4,4),(0.,1.),(0.,1.),.UNSPECIFIED.)
GEOMETRIC_REPRESENTATION_ITEM()
RATIONAL_B_SPLINE_SURFACE(((1.008356913351,0.8838612339881,0.8838315240827,
1.008267783634),(1.008831957538,0.8772593890908,0.877227990342,1.008737761292),
(1.009633148898,0.8661249699641,0.8660907228766,1.009530407636),(1.010391558546,
0.8555851023152,0.8555481589836,1.010280728551)))
REPRESENTATION_ITEM('')
SURFACE()
);
#2576=(
BOUNDED_SURFACE()
B_SPLINE_SURFACE(3,3,((#154388,#154389,#154390,#154391),(#154392,#154393,
#154394,#154395),(#154396,#154397,#154398,#154399),(#154400,#154401,#154402,
#154403)),.UNSPECIFIED.,.F.,.F.,.F.)
B_SPLINE_SURFACE_WITH_KNOTS((4,4),(4,4),(0.,1.),(0.,1.),.UNSPECIFIED.)
GEOMETRIC_REPRESENTATION_ITEM()
RATIONAL_B_SPLINE_SURFACE(((1.008509940924,0.8799663128153,0.8799421151718,
1.008437347994),(1.009061509065,0.8721863812947,0.8721606152913,1.008984211055),
(1.009661139189,0.863728530016,0.8637010589907,1.009578726113),(1.010270334951,
0.8551357543165,0.8551065510698,1.010182725211)))
REPRESENTATION_ITEM('')
SURFACE()
);
#2577=(
BOUNDED_SURFACE()
B_SPLINE_SURFACE(3,3,((#154612,#154613,#154614,#154615),(#154616,#154617,
#154618,#154619),(#154620,#154621,#154622,#154623),(#154624,#154625,#154626,
#154627)),.UNSPECIFIED.,.F.,.F.,.F.)
B_SPLINE_SURFACE_WITH_KNOTS((4,4),(4,4),(0.,1.),(0.,1.),.UNSPECIFIED.)
GEOMETRIC_REPRESENTATION_ITEM()
RATIONAL_B_SPLINE_SURFACE(((1.010270521476,0.8551331131831,0.8551039195422,
1.010182940553),(1.009662767308,0.863705555624,0.8636780895057,1.009580368953),
(1.009062759899,0.8721687291531,0.8721429685373,1.008985478051),(1.008509452897,
0.8799731880642,0.8799490002065,1.008436889324)))
REPRESENTATION_ITEM('')
SURFACE()
);
#2578=(
BOUNDED_SURFACE()
B_SPLINE_SURFACE(3,3,((#154979,#154980,#154981,#154982,#154983,#154984),
(#154985,#154986,#154987,#154988,#154989,#154990),(#154991,#154992,#154993,
#154994,#154995,#154996),(#154997,#154998,#154999,#155000,#155001,#155002)),
 .UNSPECIFIED.,.F.,.F.,.F.)
B_SPLINE_SURFACE_WITH_KNOTS((4,4),(4,1,1,4),(0.,1.),(0.,0.380343625085213,
0.838543336801836,1.),.UNSPECIFIED.)
GEOMETRIC_REPRESENTATION_ITEM()
RATIONAL_B_SPLINE_SURFACE(((1.097838297065,1.097838297065,1.097838297065,
1.097838297065,1.097838297065,1.097838297065),(0.9673872343117,0.9673872343117,
0.9673872343117,0.9673872343117,0.9673872343117,0.9673872343117),(0.9673872343117,
0.9673872343117,0.9673872343117,0.9673872343117,0.9673872343117,0.9673872343117),
(1.097838297065,1.097838297065,1.097838297065,1.097838297065,1.097838297065,
1.097838297065)))
REPRESENTATION_ITEM('')
SURFACE()
);
#2579=(
BOUNDED_SURFACE()
B_SPLINE_SURFACE(3,3,((#155006,#155007,#155008,#155009),(#155010,#155011,
#155012,#155013),(#155014,#155015,#155016,#155017),(#155018,#155019,#155020,
#155021)),.UNSPECIFIED.,.F.,.F.,.F.)
B_SPLINE_SURFACE_WITH_KNOTS((4,4),(4,4),(0.,1.),(0.,1.),.UNSPECIFIED.)
GEOMETRIC_REPRESENTATION_ITEM()
RATIONAL_B_SPLINE_SURFACE(((1.,0.8932355607724,0.8836489357959,0.9712401250704),
(1.,0.8866507841162,0.8764728968729,0.9694663382699),(1.,0.8795406937193,
0.868724375078,0.9675510440761),(1.,0.8723221998445,0.8608577160073,0.9656065484883)))
REPRESENTATION_ITEM('')
SURFACE()
);
#2580=(
BOUNDED_SURFACE()
B_SPLINE_SURFACE(3,3,((#155029,#155030,#155031,#155032,#155033,#155034),
(#155035,#155036,#155037,#155038,#155039,#155040),(#155041,#155042,#155043,
#155044,#155045,#155046),(#155047,#155048,#155049,#155050,#155051,#155052)),
 .UNSPECIFIED.,.F.,.F.,.F.)
B_SPLINE_SURFACE_WITH_KNOTS((4,4),(4,1,1,4),(0.,1.),(0.,0.048792228532537,
0.607299349828058,1.),.UNSPECIFIED.)
GEOMETRIC_REPRESENTATION_ITEM()
RATIONAL_B_SPLINE_SURFACE(((1.227394348186,1.227394348186,1.227394348186,
1.227394348186,1.227394348186,1.227394348186),(0.9242018839379,0.9242018839379,
0.9242018839379,0.9242018839379,0.9242018839379,0.9242018839379),(0.9242018839379,
0.9242018839379,0.9242018839379,0.9242018839379,0.9242018839379,0.9242018839379),
(1.227394348186,1.227394348186,1.227394348186,1.227394348186,1.227394348186,
1.227394348186)))
REPRESENTATION_ITEM('')
SURFACE()
);
#2581=(
BOUNDED_SURFACE()
B_SPLINE_SURFACE(3,3,((#155055,#155056,#155057,#155058,#155059),(#155060,
#155061,#155062,#155063,#155064),(#155065,#155066,#155067,#155068,#155069),
(#155070,#155071,#155072,#155073,#155074)),.UNSPECIFIED.,.F.,.F.,.F.)
B_SPLINE_SURFACE_WITH_KNOTS((4,4),(4,1,4),(0.,1.),(0.,0.724305737931071,
1.),.UNSPECIFIED.)
GEOMETRIC_REPRESENTATION_ITEM()
RATIONAL_B_SPLINE_SURFACE(((1.071521449038,1.071521449038,1.071521449038,
1.071521449038,1.071521449038),(0.9761595169872,0.9761595169872,0.9761595169872,
0.9761595169872,0.9761595169872),(0.9761595169872,0.9761595169872,0.9761595169872,
0.9761595169872,0.9761595169872),(1.071521449038,1.071521449038,1.071521449038,
1.071521449038,1.071521449038)))
REPRESENTATION_ITEM('')
SURFACE()
);
#2582=(
BOUNDED_SURFACE()
B_SPLINE_SURFACE(3,3,((#155429,#155430,#155431,#155432,#155433),(#155434,
#155435,#155436,#155437,#155438),(#155439,#155440,#155441,#155442,#155443),
(#155444,#155445,#155446,#155447,#155448)),.UNSPECIFIED.,.F.,.F.,.F.)
B_SPLINE_SURFACE_WITH_KNOTS((4,4),(4,1,4),(0.,1.),(0.,0.294824597653245,
1.),.UNSPECIFIED.)
GEOMETRIC_REPRESENTATION_ITEM()
RATIONAL_B_SPLINE_SURFACE(((1.071512049094,1.071512049094,1.071512049094,
1.071512049094,1.071512049094),(0.9761626503021,0.9761626503021,0.9761626503021,
0.9761626503021,0.9761626503021),(0.9761626503021,0.9761626503021,0.9761626503021,
0.9761626503021,0.9761626503021),(1.071512049094,1.071512049094,1.071512049094,
1.071512049094,1.071512049094)))
REPRESENTATION_ITEM('')
SURFACE()
);
#2583=(
BOUNDED_SURFACE()
B_SPLINE_SURFACE(3,3,((#155459,#155460,#155461,#155462,#155463,#155464),
(#155465,#155466,#155467,#155468,#155469,#155470),(#155471,#155472,#155473,
#155474,#155475,#155476),(#155477,#155478,#155479,#155480,#155481,#155482)),
 .UNSPECIFIED.,.F.,.F.,.F.)
B_SPLINE_SURFACE_WITH_KNOTS((4,4),(4,1,1,4),(0.,1.),(0.,0.313954312956168,
0.656504260785239,1.),.UNSPECIFIED.)
GEOMETRIC_REPRESENTATION_ITEM()
RATIONAL_B_SPLINE_SURFACE(((1.097834676065,1.097834676065,1.097834676065,
1.097834676065,1.097834676065,1.097834676065),(0.9673884413118,0.9673884413118,
0.9673884413118,0.9673884413118,0.9673884413118,0.9673884413118),(0.9673884413118,
0.9673884413118,0.9673884413118,0.9673884413118,0.9673884413118,0.9673884413118),
(1.097834676065,1.097834676065,1.097834676065,1.097834676065,1.097834676065,
1.097834676065)))
REPRESENTATION_ITEM('')
SURFACE()
);
#2584=(
BOUNDED_SURFACE()
B_SPLINE_SURFACE(3,3,((#155501,#155502,#155503,#155504),(#155505,#155506,
#155507,#155508),(#155509,#155510,#155511,#155512),(#155513,#155514,#155515,
#155516)),.UNSPECIFIED.,.F.,.F.,.F.)
B_SPLINE_SURFACE_WITH_KNOTS((4,4),(4,4),(0.,1.),(0.,1.),.UNSPECIFIED.)
GEOMETRIC_REPRESENTATION_ITEM()
RATIONAL_B_SPLINE_SURFACE(((1.006012832044,0.8936858019092,0.8821005665622,
0.9712571260029),(1.006404088946,0.8867679030724,0.87442881276,0.9693868180087),
(1.00682837482,0.8792660117647,0.866109427854,0.9673586230877),(1.00725810598,
0.8716678411682,0.8576832719446,0.9653043983088)))
REPRESENTATION_ITEM('')
SURFACE()
);
#2585=(
BOUNDED_SURFACE()
B_SPLINE_SURFACE(3,3,((#155742,#155743,#155744,#155745,#155746,#155747),
(#155748,#155749,#155750,#155751,#155752,#155753),(#155754,#155755,#155756,
#155757,#155758,#155759),(#155760,#155761,#155762,#155763,#155764,#155765)),
 .UNSPECIFIED.,.F.,.F.,.F.)
B_SPLINE_SURFACE_WITH_KNOTS((4,4),(4,1,1,4),(0.,1.),(0.,0.305886131949221,
0.66938588399328,1.),.UNSPECIFIED.)
GEOMETRIC_REPRESENTATION_ITEM()
RATIONAL_B_SPLINE_SURFACE(((1.289432719618,1.289432719618,1.289432719618,
1.289432719618,1.289432719618,1.289432719618),(0.9035224267941,0.9035224267941,
0.9035224267941,0.9035224267941,0.9035224267941,0.9035224267941),(0.9035224267941,
0.9035224267941,0.9035224267941,0.9035224267941,0.9035224267941,0.9035224267941),
(1.289432719618,1.289432719618,1.289432719618,1.289432719618,1.289432719618,
1.289432719618)))
REPRESENTATION_ITEM('')
SURFACE()
);
#2586=(
BOUNDED_SURFACE()
B_SPLINE_SURFACE(3,3,((#155940,#155941,#155942,#155943,#155944,#155945,
#155946,#155947,#155948,#155949),(#155950,#155951,#155952,#155953,#155954,
#155955,#155956,#155957,#155958,#155959),(#155960,#155961,#155962,#155963,
#155964,#155965,#155966,#155967,#155968,#155969),(#155970,#155971,#155972,
#155973,#155974,#155975,#155976,#155977,#155978,#155979)),.UNSPECIFIED.,
 .F.,.F.,.F.)
B_SPLINE_SURFACE_WITH_KNOTS((4,4),(4,1,1,1,1,1,1,4),(0.,1.),(0.,0.00407814944862078,
0.20628932018066,0.424188287120768,0.621485607426675,0.792206769446229,
0.94764413919974,1.),.UNSPECIFIED.)
GEOMETRIC_REPRESENTATION_ITEM()
RATIONAL_B_SPLINE_SURFACE(((1.478660809567,1.478660809567,1.478660809567,
1.478660809567,1.478660809567,1.478660809567,1.478660809567,1.478660809567,
1.478660809567,1.478660809567),(0.840446396811,0.840446396811,0.840446396811,
0.840446396811,0.840446396811,0.840446396811,0.840446396811,0.840446396811,
0.840446396811,0.840446396811),(0.840446396811,0.840446396811,0.840446396811,
0.840446396811,0.840446396811,0.840446396811,0.840446396811,0.840446396811,
0.840446396811,0.840446396811),(1.478660809567,1.478660809567,1.478660809567,
1.478660809567,1.478660809567,1.478660809567,1.478660809567,1.478660809567,
1.478660809567,1.478660809567)))
REPRESENTATION_ITEM('')
SURFACE()
);
#2587=(
BOUNDED_SURFACE()
B_SPLINE_SURFACE(3,3,((#156025,#156026,#156027,#156028,#156029,#156030),
(#156031,#156032,#156033,#156034,#156035,#156036),(#156037,#156038,#156039,
#156040,#156041,#156042),(#156043,#156044,#156045,#156046,#156047,#156048)),
 .UNSPECIFIED.,.F.,.F.,.F.)
B_SPLINE_SURFACE_WITH_KNOTS((4,4),(4,1,1,4),(0.,1.),(0.,0.0564405642465865,
0.555415182027201,1.),.UNSPECIFIED.)
GEOMETRIC_REPRESENTATION_ITEM()
RATIONAL_B_SPLINE_SURFACE(((1.289342804764,1.289342804764,1.289342804764,
1.289342804764,1.289342804764,1.289342804764),(0.9035523984119,0.9035523984119,
0.9035523984119,0.9035523984119,0.9035523984119,0.9035523984119),(0.9035523984119,
0.9035523984119,0.9035523984119,0.9035523984119,0.9035523984119,0.9035523984119),
(1.289342804764,1.289342804764,1.289342804764,1.289342804764,1.289342804764,
1.289342804764)))
REPRESENTATION_ITEM('')
SURFACE()
);
#2588=(
BOUNDED_SURFACE()
B_SPLINE_SURFACE(3,3,((#156100,#156101,#156102,#156103,#156104,#156105,
#156106,#156107,#156108,#156109,#156110,#156111,#156112),(#156113,#156114,
#156115,#156116,#156117,#156118,#156119,#156120,#156121,#156122,#156123,
#156124,#156125),(#156126,#156127,#156128,#156129,#156130,#156131,#156132,
#156133,#156134,#156135,#156136,#156137,#156138),(#156139,#156140,#156141,
#156142,#156143,#156144,#156145,#156146,#156147,#156148,#156149,#156150,
#156151)),.UNSPECIFIED.,.F.,.F.,.F.)
B_SPLINE_SURFACE_WITH_KNOTS((4,4),(4,1,1,1,1,1,1,1,1,1,4),(0.,1.),(0.,0.0392950764212505,
0.11457615782262,0.1986935009597,0.291671866982471,0.394461000807193,0.508210508879651,
0.634800597831141,0.77592091339028,0.937113831440419,1.),.UNSPECIFIED.)
GEOMETRIC_REPRESENTATION_ITEM()
RATIONAL_B_SPLINE_SURFACE(((1.225183392518,1.225183392518,1.225183392518,
1.225183392518,1.225183392518,1.225183392518,1.225183392518,1.225183392518,
1.225183392518,1.225183392518,1.225183392518,1.225183392518,1.225183392518),
(0.9249388691606,0.9249388691606,0.9249388691606,0.9249388691606,0.9249388691606,
0.9249388691606,0.9249388691606,0.9249388691606,0.9249388691606,0.9249388691606,
0.9249388691606,0.9249388691606,0.9249388691606),(0.9249388691606,0.9249388691606,
0.9249388691606,0.9249388691606,0.9249388691606,0.9249388691606,0.9249388691606,
0.9249388691606,0.9249388691606,0.9249388691606,0.9249388691606,0.9249388691606,
0.9249388691606),(1.225183392518,1.225183392518,1.225183392518,1.225183392518,
1.225183392518,1.225183392518,1.225183392518,1.225183392518,1.225183392518,
1.225183392518,1.225183392518,1.225183392518,1.225183392518)))
REPRESENTATION_ITEM('')
SURFACE()
);
#2589=(
BOUNDED_SURFACE()
B_SPLINE_SURFACE(3,3,((#156160,#156161,#156162,#156163,#156164,#156165,
#156166,#156167,#156168,#156169,#156170,#156171,#156172,#156173,#156174,
#156175),(#156176,#156177,#156178,#156179,#156180,#156181,#156182,#156183,
#156184,#156185,#156186,#156187,#156188,#156189,#156190,#156191),(#156192,
#156193,#156194,#156195,#156196,#156197,#156198,#156199,#156200,#156201,
#156202,#156203,#156204,#156205,#156206,#156207),(#156208,#156209,#156210,
#156211,#156212,#156213,#156214,#156215,#156216,#156217,#156218,#156219,
#156220,#156221,#156222,#156223)),.UNSPECIFIED.,.F.,.F.,.F.)
B_SPLINE_SURFACE_WITH_KNOTS((4,4),(4,1,1,1,1,1,1,1,1,1,1,1,1,4),(0.,1.),
(0.,0.0186503236401621,0.0681861826858635,0.122274864726643,0.181134794327188,
0.244976288689619,0.314185121458223,0.389489559305443,0.47162927932211,
0.561313355930194,0.659220518921088,0.766025144246682,0.882569333512905,
1.),.UNSPECIFIED.)
GEOMETRIC_REPRESENTATION_ITEM()
RATIONAL_B_SPLINE_SURFACE(((1.02563369563202,1.02563369563202,1.02563369563202,
1.02563369563202,1.02563369563202,1.02563369563202,1.02563369563202,1.02563369563202,
1.02563369563202,1.02563369563202,1.02563369563202,1.02563369563202,1.02563369563202,
1.02563369563202,1.02563369563202,1.02563369563202),(1.00889094478308,1.00889094478308,
1.00889094478308,1.00889094478308,1.00889094478308,1.00889094478308,1.00889094478308,
1.00889094478308,1.00889094478308,1.00889094478308,1.00889094478308,1.00889094478308,
1.00889094478308,1.00889094478308,1.00889094478308,1.00889094478308),(1.00034988995606,
1.00034988995606,1.00034988995606,1.00034988995606,1.00034988995606,1.00034988995606,
1.00034988995606,1.00034988995606,1.00034988995606,1.00034988995606,1.00034988995606,
1.00034988995606,1.00034988995606,1.00034988995606,1.00034988995606,1.00034988995606),
(1.00001053115096,1.00001053115096,1.00001053115096,1.00001053115096,1.00001053115096,
1.00001053115096,1.00001053115096,1.00001053115096,1.00001053115096,1.00001053115096,
1.00001053115096,1.00001053115096,1.00001053115096,1.00001053115096,1.00001053115096,
1.00001053115096)))
REPRESENTATION_ITEM('')
SURFACE()
);
#2590=(
BOUNDED_SURFACE()
B_SPLINE_SURFACE(3,3,((#156226,#156227,#156228,#156229,#156230,#156231),
(#156232,#156233,#156234,#156235,#156236,#156237),(#156238,#156239,#156240,
#156241,#156242,#156243),(#156244,#156245,#156246,#156247,#156248,#156249)),
 .UNSPECIFIED.,.F.,.F.,.F.)
B_SPLINE_SURFACE_WITH_KNOTS((4,4),(4,1,1,4),(0.,1.),(0.,0.422272978047247,
0.965778076451582,1.),.UNSPECIFIED.)
GEOMETRIC_REPRESENTATION_ITEM()
RATIONAL_B_SPLINE_SURFACE(((1.227394458612,1.227394458612,1.227394458612,
1.227394458612,1.227394458612,1.227394458612),(0.9242018471293,0.9242018471293,
0.9242018471293,0.9242018471293,0.9242018471293,0.9242018471293),(0.9242018471293,
0.9242018471293,0.9242018471293,0.9242018471293,0.9242018471293,0.9242018471293),
(1.227394458612,1.227394458612,1.227394458612,1.227394458612,1.227394458612,
1.227394458612)))
REPRESENTATION_ITEM('')
SURFACE()
);
#2591=(
BOUNDED_SURFACE()
B_SPLINE_SURFACE(3,3,((#156259,#156260,#156261,#156262),(#156263,#156264,
#156265,#156266),(#156267,#156268,#156269,#156270),(#156271,#156272,#156273,
#156274)),.UNSPECIFIED.,.F.,.F.,.F.)
B_SPLINE_SURFACE_WITH_KNOTS((4,4),(4,4),(0.,1.),(0.,1.),.UNSPECIFIED.)
GEOMETRIC_REPRESENTATION_ITEM()
RATIONAL_B_SPLINE_SURFACE(((1.,0.8723221998447,0.8608577160075,0.9656065484883),
(1.,0.8795681296753,0.8687542745717,0.9675584346892),(1.,0.8866850345386,
0.8765102227196,0.9694755645429),(1.,0.8932587951734,0.8836742564673,0.9712463838817)))
REPRESENTATION_ITEM('')
SURFACE()
);
#2592=(
BOUNDED_SURFACE()
B_SPLINE_SURFACE(3,3,((#156276,#156277,#156278,#156279,#156280,#156281),
(#156282,#156283,#156284,#156285,#156286,#156287),(#156288,#156289,#156290,
#156291,#156292,#156293),(#156294,#156295,#156296,#156297,#156298,#156299)),
 .UNSPECIFIED.,.F.,.F.,.F.)
B_SPLINE_SURFACE_WITH_KNOTS((4,4),(4,1,1,4),(0.,1.),(0.,0.148909102857252,
0.594712811487906,1.),.UNSPECIFIED.)
GEOMETRIC_REPRESENTATION_ITEM()
RATIONAL_B_SPLINE_SURFACE(((1.097837209174,1.097837209174,1.097837209174,
1.097837209174,1.097837209174,1.097837209174),(0.9673875969419,0.9673875969419,
0.9673875969419,0.9673875969419,0.9673875969419,0.9673875969419),(0.9673875969419,
0.9673875969419,0.9673875969419,0.9673875969419,0.9673875969419,0.9673875969419),
(1.097837209174,1.097837209174,1.097837209174,1.097837209174,1.097837209174,
1.097837209174)))
REPRESENTATION_ITEM('')
SURFACE()
);
#2593=(
BOUNDED_SURFACE()
B_SPLINE_SURFACE(3,3,((#156303,#156304,#156305,#156306,#156307,#156308,
#156309,#156310,#156311,#156312,#156313),(#156314,#156315,#156316,#156317,
#156318,#156319,#156320,#156321,#156322,#156323,#156324),(#156325,#156326,
#156327,#156328,#156329,#156330,#156331,#156332,#156333,#156334,#156335),
(#156336,#156337,#156338,#156339,#156340,#156341,#156342,#156343,#156344,
#156345,#156346)),.UNSPECIFIED.,.F.,.F.,.F.)
B_SPLINE_SURFACE_WITH_KNOTS((4,4),(4,1,1,1,1,1,1,1,4),(0.,1.),(0.,0.0971862194548168,
0.209222881559132,0.334123661442517,0.473952177526924,0.627038064857414,
0.768578420172363,0.89296459914939,1.),.UNSPECIFIED.)
GEOMETRIC_REPRESENTATION_ITEM()
RATIONAL_B_SPLINE_SURFACE(((1.155039451457,1.155039451457,1.155039451457,
1.155039451457,1.155039451457,1.155039451457,1.155039451457,1.155039451457,
1.155039451457,1.155039451457,1.155039451457),(0.9483201828478,0.9483201828478,
0.9483201828478,0.9483201828478,0.9483201828478,0.9483201828478,0.9483201828478,
0.9483201828478,0.9483201828478,0.9483201828478,0.9483201828478),(0.9483201828478,
0.9483201828478,0.9483201828478,0.9483201828478,0.9483201828478,0.9483201828478,
0.9483201828478,0.9483201828478,0.9483201828478,0.9483201828478,0.9483201828478),
(1.155039451457,1.155039451457,1.155039451457,1.155039451457,1.155039451457,
1.155039451457,1.155039451457,1.155039451457,1.155039451457,1.155039451457,
1.155039451457)))
REPRESENTATION_ITEM('')
SURFACE()
);
#2594=(
BOUNDED_SURFACE()
B_SPLINE_SURFACE(3,3,((#156347,#156348,#156349,#156350,#156351,#156352,
#156353,#156354,#156355,#156356,#156357,#156358,#156359,#156360,#156361,
#156362,#156363,#156364,#156365,#156366,#156367,#156368,#156369,#156370,
#156371,#156372,#156373),(#156374,#156375,#156376,#156377,#156378,#156379,
#156380,#156381,#156382,#156383,#156384,#156385,#156386,#156387,#156388,
#156389,#156390,#156391,#156392,#156393,#156394,#156395,#156396,#156397,
#156398,#156399,#156400),(#156401,#156402,#156403,#156404,#156405,#156406,
#156407,#156408,#156409,#156410,#156411,#156412,#156413,#156414,#156415,
#156416,#156417,#156418,#156419,#156420,#156421,#156422,#156423,#156424,
#156425,#156426,#156427),(#156428,#156429,#156430,#156431,#156432,#156433,
#156434,#156435,#156436,#156437,#156438,#156439,#156440,#156441,#156442,
#156443,#156444,#156445,#156446,#156447,#156448,#156449,#156450,#156451,
#156452,#156453,#156454)),.UNSPECIFIED.,.F.,.F.,.F.)
B_SPLINE_SURFACE_WITH_KNOTS((4,4),(4,1,1,1,1,1,1,1,1,1,1,1,1,1,1,1,1,1,
1,1,1,1,1,1,4),(0.,1.),(0.,0.0133790708609555,0.0453329796627258,0.0807388003454147,
0.119840389730795,0.163002464189262,0.208524978632734,0.255893607883244,
0.304895617468101,0.352488053627177,0.399297953204769,0.44670582741306,
0.495059060800077,0.544318051162291,0.593648529667453,0.642243067504499,
0.69097472016604,0.740534478000938,0.788178737579007,0.834198656035311,
0.878796199450591,0.918860483820039,0.954457386043452,0.986512936409789,
1.),.UNSPECIFIED.)
GEOMETRIC_REPRESENTATION_ITEM()
RATIONAL_B_SPLINE_SURFACE(((1.261104736243,1.261104736243,1.261104736243,
1.261104736243,1.261104736243,1.261104736243,1.261104736243,1.261104736243,
1.261104736243,1.261104736243,1.261104736243,1.261104736243,1.261104736243,
1.261104736243,1.261104736243,1.261104736243,1.261104736243,1.261104736243,
1.261104736243,1.261104736243,1.261104736243,1.261104736243,1.261104736243,
1.261104736243,1.261104736243,1.261104736243,1.261104736243),(0.912965087919,
0.912965087919,0.912965087919,0.912965087919,0.912965087919,0.912965087919,
0.912965087919,0.912965087919,0.912965087919,0.912965087919,0.912965087919,
0.912965087919,0.912965087919,0.912965087919,0.912965087919,0.912965087919,
0.912965087919,0.912965087919,0.912965087919,0.912965087919,0.912965087919,
0.912965087919,0.912965087919,0.912965087919,0.912965087919,0.912965087919,
0.912965087919),(0.912965087919,0.912965087919,0.912965087919,0.912965087919,
0.912965087919,0.912965087919,0.912965087919,0.912965087919,0.912965087919,
0.912965087919,0.912965087919,0.912965087919,0.912965087919,0.912965087919,
0.912965087919,0.912965087919,0.912965087919,0.912965087919,0.912965087919,
0.912965087919,0.912965087919,0.912965087919,0.912965087919,0.912965087919,
0.912965087919,0.912965087919,0.912965087919),(1.261104736243,1.261104736243,
1.261104736243,1.261104736243,1.261104736243,1.261104736243,1.261104736243,
1.261104736243,1.261104736243,1.261104736243,1.261104736243,1.261104736243,
1.261104736243,1.261104736243,1.261104736243,1.261104736243,1.261104736243,
1.261104736243,1.261104736243,1.261104736243,1.261104736243,1.261104736243,
1.261104736243,1.261104736243,1.261104736243,1.261104736243,1.261104736243)))
REPRESENTATION_ITEM('')
SURFACE()
);
#2595=(
BOUNDED_SURFACE()
B_SPLINE_SURFACE(3,3,((#156684,#156685,#156686,#156687,#156688,#156689,
#156690,#156691,#156692,#156693,#156694,#156695,#156696,#156697,#156698,
#156699,#156700,#156701,#156702,#156703,#156704,#156705),(#156706,#156707,
#156708,#156709,#156710,#156711,#156712,#156713,#156714,#156715,#156716,
#156717,#156718,#156719,#156720,#156721,#156722,#156723,#156724,#156725,
#156726,#156727),(#156728,#156729,#156730,#156731,#156732,#156733,#156734,
#156735,#156736,#156737,#156738,#156739,#156740,#156741,#156742,#156743,
#156744,#156745,#156746,#156747,#156748,#156749),(#156750,#156751,#156752,
#156753,#156754,#156755,#156756,#156757,#156758,#156759,#156760,#156761,
#156762,#156763,#156764,#156765,#156766,#156767,#156768,#156769,#156770,
#156771)),.UNSPECIFIED.,.F.,.F.,.F.)
B_SPLINE_SURFACE_WITH_KNOTS((4,4),(4,1,1,1,1,1,1,1,1,1,1,1,1,1,1,1,1,1,
1,4),(0.,1.),(0.,0.00179852648676455,0.0684134361341035,0.138569448512766,
0.212049560253872,0.281023409010827,0.341871044231178,0.39611355557608,
0.444140369343199,0.487339341535663,0.530585789342856,0.575339323721559,
0.620494040055896,0.664485227938823,0.706756351680787,0.752682439877936,
0.80459823145977,0.863065026247903,0.928980423200659,1.),.UNSPECIFIED.)
GEOMETRIC_REPRESENTATION_ITEM()
RATIONAL_B_SPLINE_SURFACE(((1.255321138723,1.255321138723,1.255321138723,
1.255321138723,1.255321138723,1.255321138723,1.255321138723,1.255321138723,
1.255321138723,1.255321138723,1.255321138723,1.255321138723,1.255321138723,
1.255321138723,1.255321138723,1.255321138723,1.255321138723,1.255321138723,
1.255321138723,1.255321138723,1.255321138723,1.255321138723),(0.914892953759,
0.914892953759,0.914892953759,0.914892953759,0.914892953759,0.914892953759,
0.914892953759,0.914892953759,0.914892953759,0.914892953759,0.914892953759,
0.914892953759,0.914892953759,0.914892953759,0.914892953759,0.914892953759,
0.914892953759,0.914892953759,0.914892953759,0.914892953759,0.914892953759,
0.914892953759),(0.914892953759,0.914892953759,0.914892953759,0.914892953759,
0.914892953759,0.914892953759,0.914892953759,0.914892953759,0.914892953759,
0.914892953759,0.914892953759,0.914892953759,0.914892953759,0.914892953759,
0.914892953759,0.914892953759,0.914892953759,0.914892953759,0.914892953759,
0.914892953759,0.914892953759,0.914892953759),(1.255321138723,1.255321138723,
1.255321138723,1.255321138723,1.255321138723,1.255321138723,1.255321138723,
1.255321138723,1.255321138723,1.255321138723,1.255321138723,1.255321138723,
1.255321138723,1.255321138723,1.255321138723,1.255321138723,1.255321138723,
1.255321138723,1.255321138723,1.255321138723,1.255321138723,1.255321138723)))
REPRESENTATION_ITEM('')
SURFACE()
);
#2596=(
BOUNDED_SURFACE()
B_SPLINE_SURFACE(3,3,((#156821,#156822,#156823,#156824,#156825,#156826,
#156827,#156828,#156829,#156830,#156831),(#156832,#156833,#156834,#156835,
#156836,#156837,#156838,#156839,#156840,#156841,#156842),(#156843,#156844,
#156845,#156846,#156847,#156848,#156849,#156850,#156851,#156852,#156853),
(#156854,#156855,#156856,#156857,#156858,#156859,#156860,#156861,#156862,
#156863,#156864)),.UNSPECIFIED.,.F.,.F.,.F.)
B_SPLINE_SURFACE_WITH_KNOTS((4,4),(4,1,1,1,1,1,1,1,4),(0.,1.),(0.,0.0185293626863753,
0.146534230162969,0.288917342557819,0.446398650999111,0.612297392457084,
0.77680939958634,0.936363164269577,1.),.UNSPECIFIED.)
GEOMETRIC_REPRESENTATION_ITEM()
RATIONAL_B_SPLINE_SURFACE(((1.366220667592,1.366220667592,1.366220667592,
1.366220667592,1.366220667592,1.366220667592,1.366220667592,1.366220667592,
1.366220667592,1.366220667592,1.366220667592),(0.8779264441361,0.8779264441361,
0.8779264441361,0.8779264441361,0.8779264441361,0.8779264441361,0.8779264441361,
0.8779264441361,0.8779264441361,0.8779264441361,0.8779264441361),(0.8779264441361,
0.8779264441361,0.8779264441361,0.8779264441361,0.8779264441361,0.8779264441361,
0.8779264441361,0.8779264441361,0.8779264441361,0.8779264441361,0.8779264441361),
(1.366220667592,1.366220667592,1.366220667592,1.366220667592,1.366220667592,
1.366220667592,1.366220667592,1.366220667592,1.366220667592,1.366220667592,
1.366220667592)))
REPRESENTATION_ITEM('')
SURFACE()
);
#2597=(
BOUNDED_SURFACE()
B_SPLINE_SURFACE(2,2,((#157031,#157032,#157033),(#157034,#157035,#157036),
(#157037,#157038,#157039),(#157040,#157041,#157042),(#157043,#157044,#157045)),
 .UNSPECIFIED.,.F.,.F.,.F.)
B_SPLINE_SURFACE_WITH_KNOTS((3,2,3),(3,3),(5.17583184338056E-13,0.78540290201525,
1.57080580402998),(-0.715662500296765,0.715662500296765),.UNSPECIFIED.)
GEOMETRIC_REPRESENTATION_ITEM()
RATIONAL_B_SPLINE_SURFACE(((1.,0.754658728802486,1.),(0.923878625813598,
0.697213069324277,0.923878625813598),(1.,0.754658728802486,1.),(0.923878625813414,
0.697213069324138,0.923878625813414),(1.,0.754658728802486,1.)))
REPRESENTATION_ITEM('')
SURFACE()
);
#2598=(
BOUNDED_SURFACE()
B_SPLINE_SURFACE(3,3,((#157065,#157066,#157067,#157068,#157069,#157070,
#157071,#157072,#157073,#157074),(#157075,#157076,#157077,#157078,#157079,
#157080,#157081,#157082,#157083,#157084),(#157085,#157086,#157087,#157088,
#157089,#157090,#157091,#157092,#157093,#157094),(#157095,#157096,#157097,
#157098,#157099,#157100,#157101,#157102,#157103,#157104)),.UNSPECIFIED.,
 .F.,.F.,.F.)
B_SPLINE_SURFACE_WITH_KNOTS((4,4),(4,1,1,1,1,1,1,4),(0.,1.),(0.,0.0918892366120133,
0.277217977594551,0.468937582524931,0.657129296434973,0.829336528589428,
0.981429132764797,1.),.UNSPECIFIED.)
GEOMETRIC_REPRESENTATION_ITEM()
RATIONAL_B_SPLINE_SURFACE(((1.367123648823,1.367123648823,1.367123648823,
1.367123648823,1.367123648823,1.367123648823,1.367123648823,1.367123648823,
1.367123648823,1.367123648823),(0.8776254503924,0.8776254503924,0.8776254503924,
0.8776254503924,0.8776254503924,0.8776254503924,0.8776254503924,0.8776254503924,
0.8776254503924,0.8776254503924),(0.8776254503924,0.8776254503924,0.8776254503924,
0.8776254503924,0.8776254503924,0.8776254503924,0.8776254503924,0.8776254503924,
0.8776254503924,0.8776254503924),(1.367123648823,1.367123648823,1.367123648823,
1.367123648823,1.367123648823,1.367123648823,1.367123648823,1.367123648823,
1.367123648823,1.367123648823)))
REPRESENTATION_ITEM('')
SURFACE()
);
#2599=(
BOUNDED_SURFACE()
B_SPLINE_SURFACE(2,2,((#157106,#157107,#157108),(#157109,#157110,#157111),
(#157112,#157113,#157114),(#157115,#157116,#157117),(#157118,#157119,#157120)),
 .UNSPECIFIED.,.F.,.F.,.F.)
B_SPLINE_SURFACE_WITH_KNOTS((3,2,3),(3,3),(-1.57080581687637,-0.785402908437997,
3.76899203758591E-13),(-0.715662500299626,0.715662500299626),
 .UNSPECIFIED.)
GEOMETRIC_REPRESENTATION_ITEM()
RATIONAL_B_SPLINE_SURFACE(((1.,0.754658728800609,1.),(0.923878624584496,
0.69721306839499,0.923878624584496),(1.,0.754658728800609,1.),(0.923878624584344,
0.697213068394876,0.923878624584344),(1.,0.754658728800609,1.)))
REPRESENTATION_ITEM('')
SURFACE()
);
#2600=(
BOUNDED_SURFACE()
B_SPLINE_SURFACE(3,3,((#157126,#157127,#157128,#157129,#157130,#157131,
#157132,#157133,#157134,#157135,#157136,#157137,#157138,#157139,#157140,
#157141,#157142,#157143,#157144,#157145,#157146,#157147,#157148,#157149,
#157150,#157151,#157152,#157153,#157154,#157155,#157156,#157157),(#157158,
#157159,#157160,#157161,#157162,#157163,#157164,#157165,#157166,#157167,
#157168,#157169,#157170,#157171,#157172,#157173,#157174,#157175,#157176,
#157177,#157178,#157179,#157180,#157181,#157182,#157183,#157184,#157185,
#157186,#157187,#157188,#157189),(#157190,#157191,#157192,#157193,#157194,
#157195,#157196,#157197,#157198,#157199,#157200,#157201,#157202,#157203,
#157204,#157205,#157206,#157207,#157208,#157209,#157210,#157211,#157212,
#157213,#157214,#157215,#157216,#157217,#157218,#157219,#157220,#157221),
(#157222,#157223,#157224,#157225,#157226,#157227,#157228,#157229,#157230,
#157231,#157232,#157233,#157234,#157235,#157236,#157237,#157238,#157239,
#157240,#157241,#157242,#157243,#157244,#157245,#157246,#157247,#157248,
#157249,#157250,#157251,#157252,#157253)),.UNSPECIFIED.,.F.,.F.,.F.)
B_SPLINE_SURFACE_WITH_KNOTS((4,4),(4,1,1,1,1,1,1,1,1,1,1,1,1,1,1,1,1,1,
1,1,1,1,1,1,1,1,1,1,1,4),(0.,1.),(0.,0.022976135501356,0.0695598229222624,
0.121692586326365,0.178900115493456,0.240694690781884,0.30610330870727,
0.373471747186216,0.440686754218971,0.501942919989092,0.555359583174251,
0.602908392139393,0.6457512695131,0.684704926133708,0.720523567288128,0.753147804956652,
0.782813392672435,0.809944931270991,0.834840676715807,0.857737986813372,
0.878754366287739,0.898008224113769,0.915646640643435,0.931806303451426,
0.946546912483728,0.959896478233652,0.971957268367346,0.982857205461103,
0.992730071740333,1.),.UNSPECIFIED.)
GEOMETRIC_REPRESENTATION_ITEM()
RATIONAL_B_SPLINE_SURFACE(((1.777949029729,1.777949029729,1.777949029729,
1.777949029729,1.777949029729,1.777949029729,1.777949029729,1.777949029729,
1.777949029729,1.777949029729,1.777949029729,1.777949029729,1.777949029729,
1.777949029729,1.777949029729,1.777949029729,1.777949029729,1.777949029729,
1.777949029729,1.777949029729,1.777949029729,1.777949029729,1.777949029729,
1.777949029729,1.777949029729,1.777949029729,1.777949029729,1.777949029729,
1.777949029729,1.777949029729,1.777949029729,1.777949029729),(0.740683656757,
0.740683656757,0.740683656757,0.740683656757,0.740683656757,0.740683656757,
0.740683656757,0.740683656757,0.740683656757,0.740683656757,0.740683656757,
0.740683656757,0.740683656757,0.740683656757,0.740683656757,0.740683656757,
0.740683656757,0.740683656757,0.740683656757,0.740683656757,0.740683656757,
0.740683656757,0.740683656757,0.740683656757,0.740683656757,0.740683656757,
0.740683656757,0.740683656757,0.740683656757,0.740683656757,0.740683656757,
0.740683656757),(0.740683656757,0.740683656757,0.740683656757,0.740683656757,
0.740683656757,0.740683656757,0.740683656757,0.740683656757,0.740683656757,
0.740683656757,0.740683656757,0.740683656757,0.740683656757,0.740683656757,
0.740683656757,0.740683656757,0.740683656757,0.740683656757,0.740683656757,
0.740683656757,0.740683656757,0.740683656757,0.740683656757,0.740683656757,
0.740683656757,0.740683656757,0.740683656757,0.740683656757,0.740683656757,
0.740683656757,0.740683656757,0.740683656757),(1.777949029729,1.777949029729,
1.777949029729,1.777949029729,1.777949029729,1.777949029729,1.777949029729,
1.777949029729,1.777949029729,1.777949029729,1.777949029729,1.777949029729,
1.777949029729,1.777949029729,1.777949029729,1.777949029729,1.777949029729,
1.777949029729,1.777949029729,1.777949029729,1.777949029729,1.777949029729,
1.777949029729,1.777949029729,1.777949029729,1.777949029729,1.777949029729,
1.777949029729,1.777949029729,1.777949029729,1.777949029729,1.777949029729)))
REPRESENTATION_ITEM('')
SURFACE()
);
#2601=(
BOUNDED_SURFACE()
B_SPLINE_SURFACE(3,3,((#157306,#157307,#157308,#157309,#157310,#157311,
#157312,#157313,#157314,#157315,#157316,#157317,#157318,#157319),(#157320,
#157321,#157322,#157323,#157324,#157325,#157326,#157327,#157328,#157329,
#157330,#157331,#157332,#157333),(#157334,#157335,#157336,#157337,#157338,
#157339,#157340,#157341,#157342,#157343,#157344,#157345,#157346,#157347),
(#157348,#157349,#157350,#157351,#157352,#157353,#157354,#157355,#157356,
#157357,#157358,#157359,#157360,#157361)),.UNSPECIFIED.,.F.,.F.,.F.)
B_SPLINE_SURFACE_WITH_KNOTS((4,4),(4,1,1,1,1,1,1,1,1,1,1,4),(0.,1.),(0.,
0.025958376473271,0.179859171762141,0.318182203672271,0.441108132212019,
0.551634708740777,0.651710515506557,0.743010369069283,0.826230829945666,
0.901572688650554,0.970015580606343,1.),.UNSPECIFIED.)
GEOMETRIC_REPRESENTATION_ITEM()
RATIONAL_B_SPLINE_SURFACE(((1.116719050321,1.116719050321,1.116719050321,
1.116719050321,1.116719050321,1.116719050321,1.116719050321,1.116719050321,
1.116719050321,1.116719050321,1.116719050321,1.116719050321,1.116719050321,
1.116719050321),(0.961093649893,0.961093649893,0.961093649893,0.961093649893,
0.961093649893,0.961093649893,0.961093649893,0.961093649893,0.961093649893,
0.961093649893,0.961093649893,0.961093649893,0.961093649893,0.961093649893),
(0.961093649893,0.961093649893,0.961093649893,0.961093649893,0.961093649893,
0.961093649893,0.961093649893,0.961093649893,0.961093649893,0.961093649893,
0.961093649893,0.961093649893,0.961093649893,0.961093649893),(1.116719050321,
1.116719050321,1.116719050321,1.116719050321,1.116719050321,1.116719050321,
1.116719050321,1.116719050321,1.116719050321,1.116719050321,1.116719050321,
1.116719050321,1.116719050321,1.116719050321)))
REPRESENTATION_ITEM('')
SURFACE()
);
#2602=(
BOUNDED_SURFACE()
B_SPLINE_SURFACE(3,3,((#157370,#157371,#157372,#157373),(#157374,#157375,
#157376,#157377),(#157378,#157379,#157380,#157381),(#157382,#157383,#157384,
#157385)),.UNSPECIFIED.,.F.,.F.,.F.)
B_SPLINE_SURFACE_WITH_KNOTS((4,4),(4,4),(0.,1.),(0.,1.),.UNSPECIFIED.)
GEOMETRIC_REPRESENTATION_ITEM()
RATIONAL_B_SPLINE_SURFACE(((1.117354081969,1.117354081969,1.117354081969,
1.117354081969),(0.9608819726769,0.9608819726769,0.9608819726769,0.9608819726769),
(0.9608819726769,0.9608819726769,0.9608819726769,0.9608819726769),(1.117354081969,
1.117354081969,1.117354081969,1.117354081969)))
REPRESENTATION_ITEM('')
SURFACE()
);
#2603=(
BOUNDED_SURFACE()
B_SPLINE_SURFACE(3,3,((#157392,#157393,#157394,#157395,#157396,#157397),
(#157398,#157399,#157400,#157401,#157402,#157403),(#157404,#157405,#157406,
#157407,#157408,#157409),(#157410,#157411,#157412,#157413,#157414,#157415)),
 .UNSPECIFIED.,.F.,.F.,.F.)
B_SPLINE_SURFACE_WITH_KNOTS((4,4),(4,1,1,4),(0.,1.),(0.,0.131075263192113,
0.624369556415442,1.),.UNSPECIFIED.)
GEOMETRIC_REPRESENTATION_ITEM()
RATIONAL_B_SPLINE_SURFACE(((1.187262830589,1.187262830589,1.187262830589,
1.187262830589,1.187262830589,1.187262830589),(0.9375790564704,0.9375790564704,
0.9375790564704,0.9375790564704,0.9375790564704,0.9375790564704),(0.9375790564704,
0.9375790564704,0.9375790564704,0.9375790564704,0.9375790564704,0.9375790564704),
(1.187262830589,1.187262830589,1.187262830589,1.187262830589,1.187262830589,
1.187262830589)))
REPRESENTATION_ITEM('')
SURFACE()
);
#2604=(
BOUNDED_SURFACE()
B_SPLINE_SURFACE(3,3,((#157417,#157418,#157419,#157420,#157421,#157422,
#157423,#157424),(#157425,#157426,#157427,#157428,#157429,#157430,#157431,
#157432),(#157433,#157434,#157435,#157436,#157437,#157438,#157439,#157440),
(#157441,#157442,#157443,#157444,#157445,#157446,#157447,#157448)),
 .UNSPECIFIED.,.F.,.F.,.F.)
B_SPLINE_SURFACE_WITH_KNOTS((4,4),(4,1,1,1,1,4),(0.,1.),(0.,0.0123570293092027,
0.272651924312037,0.542654748910529,0.824134468225905,1.),.UNSPECIFIED.)
GEOMETRIC_REPRESENTATION_ITEM()
RATIONAL_B_SPLINE_SURFACE(((1.546267699181,1.546267699181,1.546267699181,
1.546267699181,1.546267699181,1.546267699181,1.546267699181,1.546267699181),
(0.8179107669398,0.8179107669398,0.8179107669398,0.8179107669398,0.8179107669398,
0.8179107669398,0.8179107669398,0.8179107669398),(0.8179107669398,0.8179107669398,
0.8179107669398,0.8179107669398,0.8179107669398,0.8179107669398,0.8179107669398,
0.8179107669398),(1.546267699181,1.546267699181,1.546267699181,1.546267699181,
1.546267699181,1.546267699181,1.546267699181,1.546267699181)))
REPRESENTATION_ITEM('')
SURFACE()
);
#2605=(
BOUNDED_SURFACE()
B_SPLINE_SURFACE(3,3,((#157456,#157457,#157458,#157459,#157460,#157461,
#157462,#157463,#157464,#157465),(#157466,#157467,#157468,#157469,#157470,
#157471,#157472,#157473,#157474,#157475),(#157476,#157477,#157478,#157479,
#157480,#157481,#157482,#157483,#157484,#157485),(#157486,#157487,#157488,
#157489,#157490,#157491,#157492,#157493,#157494,#157495)),.UNSPECIFIED.,
 .F.,.F.,.F.)
B_SPLINE_SURFACE_WITH_KNOTS((4,4),(4,1,1,1,1,1,1,4),(0.,1.),(0.,0.0912471898348692,
0.237776614561094,0.390267328672513,0.55260360700317,0.728899321816043,
0.920187339345513,1.),.UNSPECIFIED.)
GEOMETRIC_REPRESENTATION_ITEM()
RATIONAL_B_SPLINE_SURFACE(((1.289680320997,1.289680320997,1.289680320997,
1.289680320997,1.289680320997,1.289680320997,1.289680320997,1.289680320997,
1.289680320997,1.289680320997),(0.9034398930009,0.9034398930009,0.9034398930009,
0.9034398930009,0.9034398930009,0.9034398930009,0.9034398930009,0.9034398930009,
0.9034398930009,0.9034398930009),(0.9034398930009,0.9034398930009,0.9034398930009,
0.9034398930009,0.9034398930009,0.9034398930009,0.9034398930009,0.9034398930009,
0.9034398930009,0.9034398930009),(1.289680320997,1.289680320997,1.289680320997,
1.289680320997,1.289680320997,1.289680320997,1.289680320997,1.289680320997,
1.289680320997,1.289680320997)))
REPRESENTATION_ITEM('')
SURFACE()
);
#2606=(
BOUNDED_SURFACE()
B_SPLINE_SURFACE(3,3,((#157621,#157622,#157623,#157624,#157625,#157626,
#157627,#157628,#157629,#157630,#157631,#157632,#157633,#157634,#157635,
#157636,#157637,#157638,#157639,#157640,#157641),(#157642,#157643,#157644,
#157645,#157646,#157647,#157648,#157649,#157650,#157651,#157652,#157653,
#157654,#157655,#157656,#157657,#157658,#157659,#157660,#157661,#157662),
(#157663,#157664,#157665,#157666,#157667,#157668,#157669,#157670,#157671,
#157672,#157673,#157674,#157675,#157676,#157677,#157678,#157679,#157680,
#157681,#157682,#157683),(#157684,#157685,#157686,#157687,#157688,#157689,
#157690,#157691,#157692,#157693,#157694,#157695,#157696,#157697,#157698,
#157699,#157700,#157701,#157702,#157703,#157704)),.UNSPECIFIED.,.F.,.F.,
 .F.)
B_SPLINE_SURFACE_WITH_KNOTS((4,4),(4,1,1,1,1,1,1,1,1,1,1,1,1,1,1,1,1,1,
4),(0.,1.),(0.,0.0546624749950295,0.160757685575355,0.256729617165409,0.343735196321369,
0.422731592898268,0.494638559250071,0.560248549174547,0.620252323655667,
0.6753431121518,0.726138185608107,0.772911121896331,0.815853204906754,0.855219379345603,
0.891312858927466,0.92449329904142,0.955123399607878,0.983429063756098,
1.),.UNSPECIFIED.)
GEOMETRIC_REPRESENTATION_ITEM()
RATIONAL_B_SPLINE_SURFACE(((1.00131522864575,1.00131522864575,1.00131522864575,
1.00131522864575,1.00131522864575,1.00131522864575,1.00131522864575,1.00131522864575,
1.00131522864575,1.00131522864575,1.00131522864575,1.00131522864575,1.00131522864575,
1.00131522864575,1.00131522864575,1.00131522864575,1.00131522864575,1.00131522864575,
1.00131522864575,1.00131522864575,1.00131522864575),(0.992301531113087,
0.992301531113087,0.992301531113087,0.992301531113087,0.992301531113087,
0.992301531113087,0.992301531113087,0.992301531113087,0.992301531113087,
0.992301531113087,0.992301531113087,0.992301531113087,0.992301531113087,
0.992301531113087,0.992301531113087,0.992301531113087,0.992301531113087,
0.992301531113087,0.992301531113087,0.992301531113087,0.992301531113087),
(1.02961822457532,1.02961822457532,1.02961822457532,1.02961822457532,1.02961822457532,
1.02961822457532,1.02961822457532,1.02961822457532,1.02961822457532,1.02961822457532,
1.02961822457532,1.02961822457532,1.02961822457532,1.02961822457532,1.02961822457532,
1.02961822457532,1.02961822457532,1.02961822457532,1.02961822457532,1.02961822457532,
1.02961822457532),(1.11326530903245,1.11326530903245,1.11326530903245,1.11326530903245,
1.11326530903245,1.11326530903245,1.11326530903245,1.11326530903245,1.11326530903245,
1.11326530903245,1.11326530903245,1.11326530903245,1.11326530903245,1.11326530903245,
1.11326530903245,1.11326530903245,1.11326530903245,1.11326530903245,1.11326530903245,
1.11326530903245,1.11326530903245)))
REPRESENTATION_ITEM('')
SURFACE()
);
#2607=(
BOUNDED_SURFACE()
B_SPLINE_SURFACE(3,3,((#157707,#157708,#157709,#157710,#157711,#157712,
#157713,#157714,#157715,#157716),(#157717,#157718,#157719,#157720,#157721,
#157722,#157723,#157724,#157725,#157726),(#157727,#157728,#157729,#157730,
#157731,#157732,#157733,#157734,#157735,#157736),(#157737,#157738,#157739,
#157740,#157741,#157742,#157743,#157744,#157745,#157746)),.UNSPECIFIED.,
 .F.,.F.,.F.)
B_SPLINE_SURFACE_WITH_KNOTS((4,4),(4,1,1,1,1,1,1,4),(0.,1.),(0.,0.100889583131889,
0.31750308787695,0.513050576898124,0.689879175955297,0.85048492065676,0.997565294800237,
1.),.UNSPECIFIED.)
GEOMETRIC_REPRESENTATION_ITEM()
RATIONAL_B_SPLINE_SURFACE(((1.365423084219,1.365423084219,1.365423084219,
1.365423084219,1.365423084219,1.365423084219,1.365423084219,1.365423084219,
1.365423084219,1.365423084219),(0.8781923052603,0.8781923052603,0.8781923052603,
0.8781923052603,0.8781923052603,0.8781923052603,0.8781923052603,0.8781923052603,
0.8781923052603,0.8781923052603),(0.8781923052603,0.8781923052603,0.8781923052603,
0.8781923052603,0.8781923052603,0.8781923052603,0.8781923052603,0.8781923052603,
0.8781923052603,0.8781923052603),(1.365423084219,1.365423084219,1.365423084219,
1.365423084219,1.365423084219,1.365423084219,1.365423084219,1.365423084219,
1.365423084219,1.365423084219)))
REPRESENTATION_ITEM('')
SURFACE()
);
#2608=(
BOUNDED_SURFACE()
B_SPLINE_SURFACE(3,3,((#157765,#157766,#157767,#157768,#157769,#157770,
#157771,#157772),(#157773,#157774,#157775,#157776,#157777,#157778,#157779,
#157780),(#157781,#157782,#157783,#157784,#157785,#157786,#157787,#157788),
(#157789,#157790,#157791,#157792,#157793,#157794,#157795,#157796)),
 .UNSPECIFIED.,.F.,.F.,.F.)
B_SPLINE_SURFACE_WITH_KNOTS((4,4),(4,1,1,1,1,4),(0.,1.),(0.,0.157697040801397,
0.393079047435905,0.650027565804429,0.931370132469644,1.),.UNSPECIFIED.)
GEOMETRIC_REPRESENTATION_ITEM()
RATIONAL_B_SPLINE_SURFACE(((1.197148182303,1.197148182303,1.197148182303,
1.197148182303,1.197148182303,1.197148182303,1.197148182303,1.197148182303),
(0.9342839392322,0.9342839392322,0.9342839392322,0.9342839392322,0.9342839392322,
0.9342839392322,0.9342839392322,0.9342839392322),(0.9342839392322,0.9342839392322,
0.9342839392322,0.9342839392322,0.9342839392322,0.9342839392322,0.9342839392322,
0.9342839392322),(1.197148182303,1.197148182303,1.197148182303,1.197148182303,
1.197148182303,1.197148182303,1.197148182303,1.197148182303)))
REPRESENTATION_ITEM('')
SURFACE()
);
#2609=(
BOUNDED_SURFACE()
B_SPLINE_SURFACE(3,3,((#157809,#157810,#157811,#157812,#157813,#157814,
#157815,#157816),(#157817,#157818,#157819,#157820,#157821,#157822,#157823,
#157824),(#157825,#157826,#157827,#157828,#157829,#157830,#157831,#157832),
(#157833,#157834,#157835,#157836,#157837,#157838,#157839,#157840)),
 .UNSPECIFIED.,.F.,.F.,.F.)
B_SPLINE_SURFACE_WITH_KNOTS((4,4),(4,1,1,1,1,4),(0.,1.),(0.,0.245592378959836,
0.46830203940624,0.669594909978842,0.852727601618965,1.),.UNSPECIFIED.)
GEOMETRIC_REPRESENTATION_ITEM()
RATIONAL_B_SPLINE_SURFACE(((1.57495749403,1.57495749403,1.57495749403,1.57495749403,
1.57495749403,1.57495749403,1.57495749403,1.57495749403),(0.80834750199,
0.80834750199,0.80834750199,0.80834750199,0.80834750199,0.80834750199,0.80834750199,
0.80834750199),(0.80834750199,0.80834750199,0.80834750199,0.80834750199,
0.80834750199,0.80834750199,0.80834750199,0.80834750199),(1.57495749403,
1.57495749403,1.57495749403,1.57495749403,1.57495749403,1.57495749403,1.57495749403,
1.57495749403)))
REPRESENTATION_ITEM('')
SURFACE()
);
#2610=(
BOUNDED_SURFACE()
B_SPLINE_SURFACE(3,3,((#157908,#157909,#157910,#157911,#157912,#157913),
(#157914,#157915,#157916,#157917,#157918,#157919),(#157920,#157921,#157922,
#157923,#157924,#157925),(#157926,#157927,#157928,#157929,#157930,#157931)),
 .UNSPECIFIED.,.F.,.F.,.F.)
B_SPLINE_SURFACE_WITH_KNOTS((4,4),(4,1,1,4),(0.,1.),(0.,0.315996242763536,
0.651612786416777,1.),.UNSPECIFIED.)
GEOMETRIC_REPRESENTATION_ITEM()
RATIONAL_B_SPLINE_SURFACE(((1.618973394811,1.618973394811,1.618973394811,
1.618973394811,1.618973394811,1.618973394811),(0.7936755350628,0.7936755350628,
0.7936755350628,0.7936755350628,0.7936755350628,0.7936755350628),(0.7936755350628,
0.7936755350628,0.7936755350628,0.7936755350628,0.7936755350628,0.7936755350628),
(1.618973394811,1.618973394811,1.618973394811,1.618973394811,1.618973394811,
1.618973394811)))
REPRESENTATION_ITEM('')
SURFACE()
);
#2611=(
BOUNDED_SURFACE()
B_SPLINE_SURFACE(3,3,((#157933,#157934,#157935,#157936,#157937,#157938),
(#157939,#157940,#157941,#157942,#157943,#157944),(#157945,#157946,#157947,
#157948,#157949,#157950),(#157951,#157952,#157953,#157954,#157955,#157956)),
 .UNSPECIFIED.,.F.,.F.,.F.)
B_SPLINE_SURFACE_WITH_KNOTS((4,4),(4,1,1,4),(0.,1.),(0.,0.353278343182746,
0.688996150200427,1.),.UNSPECIFIED.)
GEOMETRIC_REPRESENTATION_ITEM()
RATIONAL_B_SPLINE_SURFACE(((1.61897754235,1.61897754235,1.61897754235,1.61897754235,
1.61897754235,1.61897754235),(0.7936741525501,0.7936741525501,0.7936741525501,
0.7936741525501,0.7936741525501,0.7936741525501),(0.7936741525501,0.7936741525501,
0.7936741525501,0.7936741525501,0.7936741525501,0.7936741525501),(1.61897754235,
1.61897754235,1.61897754235,1.61897754235,1.61897754235,1.61897754235)))
REPRESENTATION_ITEM('')
SURFACE()
);
#2612=(
BOUNDED_SURFACE()
B_SPLINE_SURFACE(3,3,((#158024,#158025,#158026,#158027,#158028,#158029,
#158030),(#158031,#158032,#158033,#158034,#158035,#158036,#158037),(#158038,
#158039,#158040,#158041,#158042,#158043,#158044),(#158045,#158046,#158047,
#158048,#158049,#158050,#158051)),.UNSPECIFIED.,.F.,.F.,.F.)
B_SPLINE_SURFACE_WITH_KNOTS((4,4),(4,1,1,1,4),(0.,1.),(0.,0.238209296182581,
0.514853671561738,0.773063557579565,1.),.UNSPECIFIED.)
GEOMETRIC_REPRESENTATION_ITEM()
RATIONAL_B_SPLINE_SURFACE(((1.574963454954,1.574963454954,1.574963454954,
1.574963454954,1.574963454954,1.574963454954,1.574963454954),(0.8083455150155,
0.8083455150155,0.8083455150155,0.8083455150155,0.8083455150155,0.8083455150155,
0.8083455150155),(0.8083455150155,0.8083455150155,0.8083455150155,0.8083455150155,
0.8083455150155,0.8083455150155,0.8083455150155),(1.574963454954,1.574963454954,
1.574963454954,1.574963454954,1.574963454954,1.574963454954,1.574963454954)))
REPRESENTATION_ITEM('')
SURFACE()
);
#2613=(
BOUNDED_SURFACE()
B_SPLINE_SURFACE(3,3,((#158059,#158060,#158061,#158062,#158063,#158064,
#158065,#158066),(#158067,#158068,#158069,#158070,#158071,#158072,#158073,
#158074),(#158075,#158076,#158077,#158078,#158079,#158080,#158081,#158082),
(#158083,#158084,#158085,#158086,#158087,#158088,#158089,#158090)),
 .UNSPECIFIED.,.F.,.F.,.F.)
B_SPLINE_SURFACE_WITH_KNOTS((4,4),(4,1,1,1,1,4),(0.,1.),(0.,0.0910089094295778,
0.411981715642662,0.714695138546929,0.987601458405524,1.),.UNSPECIFIED.)
GEOMETRIC_REPRESENTATION_ITEM()
RATIONAL_B_SPLINE_SURFACE(((1.053281584436,1.053281584436,1.053281584436,
1.053281584436,1.053281584436,1.053281584436,1.053281584436,1.053281584436),
(0.9822394718546,0.9822394718546,0.9822394718546,0.9822394718546,0.9822394718546,
0.9822394718546,0.9822394718546,0.9822394718546),(0.9822394718546,0.9822394718546,
0.9822394718546,0.9822394718546,0.9822394718546,0.9822394718546,0.9822394718546,
0.9822394718546),(1.053281584436,1.053281584436,1.053281584436,1.053281584436,
1.053281584436,1.053281584436,1.053281584436,1.053281584436)))
REPRESENTATION_ITEM('')
SURFACE()
);
#2614=(
BOUNDED_SURFACE()
B_SPLINE_SURFACE(3,3,((#158092,#158093,#158094,#158095,#158096,#158097,
#158098,#158099,#158100,#158101,#158102,#158103,#158104,#158105,#158106),
(#158107,#158108,#158109,#158110,#158111,#158112,#158113,#158114,#158115,
#158116,#158117,#158118,#158119,#158120,#158121),(#158122,#158123,#158124,
#158125,#158126,#158127,#158128,#158129,#158130,#158131,#158132,#158133,
#158134,#158135,#158136),(#158137,#158138,#158139,#158140,#158141,#158142,
#158143,#158144,#158145,#158146,#158147,#158148,#158149,#158150,#158151)),
 .UNSPECIFIED.,.F.,.F.,.F.)
B_SPLINE_SURFACE_WITH_KNOTS((4,4),(4,1,1,1,1,1,1,1,1,1,1,1,4),(0.,1.),(0.,
0.0156422110548145,0.0753559354221289,0.141207904238176,0.214058894202432,
0.294186759104291,0.382332029305939,0.47906197419899,0.584630248561368,
0.699064662214264,0.825987217014722,0.963692456243815,1.),.UNSPECIFIED.)
GEOMETRIC_REPRESENTATION_ITEM()
RATIONAL_B_SPLINE_SURFACE(((1.289195161833,1.289195161833,1.289195161833,
1.289195161833,1.289195161833,1.289195161833,1.289195161833,1.289195161833,
1.289195161833,1.289195161833,1.289195161833,1.289195161833,1.289195161833,
1.289195161833,1.289195161833),(0.9036016127224,0.9036016127224,0.9036016127224,
0.9036016127224,0.9036016127224,0.9036016127224,0.9036016127224,0.9036016127224,
0.9036016127224,0.9036016127224,0.9036016127224,0.9036016127224,0.9036016127224,
0.9036016127224,0.9036016127224),(0.9036016127224,0.9036016127224,0.9036016127224,
0.9036016127224,0.9036016127224,0.9036016127224,0.9036016127224,0.9036016127224,
0.9036016127224,0.9036016127224,0.9036016127224,0.9036016127224,0.9036016127224,
0.9036016127224,0.9036016127224),(1.289195161833,1.289195161833,1.289195161833,
1.289195161833,1.289195161833,1.289195161833,1.289195161833,1.289195161833,
1.289195161833,1.289195161833,1.289195161833,1.289195161833,1.289195161833,
1.289195161833,1.289195161833)))
REPRESENTATION_ITEM('')
SURFACE()
);
#2615=(
BOUNDED_SURFACE()
B_SPLINE_SURFACE(3,3,((#159279,#159280,#159281,#159282,#159283,#159284,
#159285,#159286,#159287,#159288,#159289,#159290,#159291),(#159292,#159293,
#159294,#159295,#159296,#159297,#159298,#159299,#159300,#159301,#159302,
#159303,#159304),(#159305,#159306,#159307,#159308,#159309,#159310,#159311,
#159312,#159313,#159314,#159315,#159316,#159317),(#159318,#159319,#159320,
#159321,#159322,#159323,#159324,#159325,#159326,#159327,#159328,#159329,
#159330)),.UNSPECIFIED.,.F.,.F.,.F.)
B_SPLINE_SURFACE_WITH_KNOTS((4,4),(4,1,1,1,1,1,1,1,1,1,4),(0.,1.),(0.,0.0348134269562723,
0.158608211677217,0.280646015430893,0.400635489137686,0.518375328151176,
0.633927632286859,0.74698660160379,0.85748053072882,0.966231997819705,1.),
 .UNSPECIFIED.)
GEOMETRIC_REPRESENTATION_ITEM()
RATIONAL_B_SPLINE_SURFACE(((1.216775993711,1.216775993711,1.216775993711,
1.216775993711,1.216775993711,1.216775993711,1.216775993711,1.216775993711,
1.216775993711,1.216775993711,1.216775993711,1.216775993711,1.216775993711),
(0.9277413354296,0.9277413354296,0.9277413354296,0.9277413354296,0.9277413354296,
0.9277413354296,0.9277413354296,0.9277413354296,0.9277413354296,0.9277413354296,
0.9277413354296,0.9277413354296,0.9277413354296),(0.9277413354296,0.9277413354296,
0.9277413354296,0.9277413354296,0.9277413354296,0.9277413354296,0.9277413354296,
0.9277413354296,0.9277413354296,0.9277413354296,0.9277413354296,0.9277413354296,
0.9277413354296),(1.216775993711,1.216775993711,1.216775993711,1.216775993711,
1.216775993711,1.216775993711,1.216775993711,1.216775993711,1.216775993711,
1.216775993711,1.216775993711,1.216775993711,1.216775993711)))
REPRESENTATION_ITEM('')
SURFACE()
);
#2616=(
BOUNDED_SURFACE()
B_SPLINE_SURFACE(3,3,((#159523,#159524,#159525,#159526,#159527,#159528,
#159529,#159530,#159531,#159532,#159533,#159534,#159535),(#159536,#159537,
#159538,#159539,#159540,#159541,#159542,#159543,#159544,#159545,#159546,
#159547,#159548),(#159549,#159550,#159551,#159552,#159553,#159554,#159555,
#159556,#159557,#159558,#159559,#159560,#159561),(#159562,#159563,#159564,
#159565,#159566,#159567,#159568,#159569,#159570,#159571,#159572,#159573,
#159574)),.UNSPECIFIED.,.F.,.F.,.F.)
B_SPLINE_SURFACE_WITH_KNOTS((4,4),(4,1,1,1,1,1,1,1,1,1,4),(0.,1.),(0.,0.0348134437205886,
0.158607302135055,0.280647732326047,0.400637496360499,0.518378147625292,
0.633929635661477,0.746988357647408,0.857493579740769,0.966231987897078,
1.),.UNSPECIFIED.)
GEOMETRIC_REPRESENTATION_ITEM()
RATIONAL_B_SPLINE_SURFACE(((1.216775996933,1.216775996933,1.216775996933,
1.216775996933,1.216775996933,1.216775996933,1.216775996933,1.216775996933,
1.216775996933,1.216775996933,1.216775996933,1.216775996933,1.216775996933),
(0.9277413343557,0.9277413343557,0.9277413343557,0.9277413343557,0.9277413343557,
0.9277413343557,0.9277413343557,0.9277413343557,0.9277413343557,0.9277413343557,
0.9277413343557,0.9277413343557,0.9277413343557),(0.9277413343557,0.9277413343557,
0.9277413343557,0.9277413343557,0.9277413343557,0.9277413343557,0.9277413343557,
0.9277413343557,0.9277413343557,0.9277413343557,0.9277413343557,0.9277413343557,
0.9277413343557),(1.216775996933,1.216775996933,1.216775996933,1.216775996933,
1.216775996933,1.216775996933,1.216775996933,1.216775996933,1.216775996933,
1.216775996933,1.216775996933,1.216775996933,1.216775996933)))
REPRESENTATION_ITEM('')
SURFACE()
);
#2617=(
BOUNDED_SURFACE()
B_SPLINE_SURFACE(3,3,((#159756,#159757,#159758,#159759,#159760,#159761,
#159762,#159763,#159764,#159765,#159766),(#159767,#159768,#159769,#159770,
#159771,#159772,#159773,#159774,#159775,#159776,#159777),(#159778,#159779,
#159780,#159781,#159782,#159783,#159784,#159785,#159786,#159787,#159788),
(#159789,#159790,#159791,#159792,#159793,#159794,#159795,#159796,#159797,
#159798,#159799)),.UNSPECIFIED.,.F.,.F.,.F.)
B_SPLINE_SURFACE_WITH_KNOTS((4,4),(4,1,1,1,1,1,1,1,4),(0.,1.),(0.,0.148763869419657,
0.292686130252006,0.421203860344306,0.536603666842246,0.654337651793038,
0.778311983622731,0.900605282133238,1.),.UNSPECIFIED.)
GEOMETRIC_REPRESENTATION_ITEM()
RATIONAL_B_SPLINE_SURFACE(((1.068703746667,1.068703746667,1.068703746667,
1.068703746667,1.068703746667,1.068703746667,1.068703746667,1.068703746667,
1.068703746667,1.068703746667,1.068703746667),(0.9770987511109,0.9770987511109,
0.9770987511109,0.9770987511109,0.9770987511109,0.9770987511109,0.9770987511109,
0.9770987511109,0.9770987511109,0.9770987511109,0.9770987511109),(0.9770987511109,
0.9770987511109,0.9770987511109,0.9770987511109,0.9770987511109,0.9770987511109,
0.9770987511109,0.9770987511109,0.9770987511109,0.9770987511109,0.9770987511109),
(1.068703746667,1.068703746667,1.068703746667,1.068703746667,1.068703746667,
1.068703746667,1.068703746667,1.068703746667,1.068703746667,1.068703746667,
1.068703746667)))
REPRESENTATION_ITEM('')
SURFACE()
);
#2618=(
BOUNDED_SURFACE()
B_SPLINE_SURFACE(3,3,((#159895,#159896,#159897,#159898,#159899,#159900,
#159901,#159902,#159903,#159904),(#159905,#159906,#159907,#159908,#159909,
#159910,#159911,#159912,#159913,#159914),(#159915,#159916,#159917,#159918,
#159919,#159920,#159921,#159922,#159923,#159924),(#159925,#159926,#159927,
#159928,#159929,#159930,#159931,#159932,#159933,#159934)),.UNSPECIFIED.,
 .F.,.F.,.F.)
B_SPLINE_SURFACE_WITH_KNOTS((4,4),(4,1,1,1,1,1,1,4),(0.,1.),(0.,0.0982957502815311,
0.222717520122402,0.361997328765986,0.517413543628817,0.685998740299415,
0.858955544446863,1.),.UNSPECIFIED.)
GEOMETRIC_REPRESENTATION_ITEM()
RATIONAL_B_SPLINE_SURFACE(((1.298412003099,1.298412003099,1.298412003099,
1.298412003099,1.298412003099,1.298412003099,1.298412003099,1.298412003099,
1.298412003099,1.298412003099),(0.9005293323002,0.9005293323002,0.9005293323002,
0.9005293323002,0.9005293323002,0.9005293323002,0.9005293323002,0.9005293323002,
0.9005293323002,0.9005293323002),(0.9005293323002,0.9005293323002,0.9005293323002,
0.9005293323002,0.9005293323002,0.9005293323002,0.9005293323002,0.9005293323002,
0.9005293323002,0.9005293323002),(1.298412003099,1.298412003099,1.298412003099,
1.298412003099,1.298412003099,1.298412003099,1.298412003099,1.298412003099,
1.298412003099,1.298412003099)))
REPRESENTATION_ITEM('')
SURFACE()
);
#2619=(
BOUNDED_SURFACE()
B_SPLINE_SURFACE(3,3,((#160037,#160038,#160039,#160040,#160041,#160042,
#160043,#160044,#160045,#160046,#160047),(#160048,#160049,#160050,#160051,
#160052,#160053,#160054,#160055,#160056,#160057,#160058),(#160059,#160060,
#160061,#160062,#160063,#160064,#160065,#160066,#160067,#160068,#160069),
(#160070,#160071,#160072,#160073,#160074,#160075,#160076,#160077,#160078,
#160079,#160080)),.UNSPECIFIED.,.F.,.F.,.F.)
B_SPLINE_SURFACE_WITH_KNOTS((4,4),(4,1,1,1,1,1,1,1,4),(0.,1.),(0.,0.113847052245463,
0.256880770340595,0.393447274181346,0.529715276691642,0.664740251429543,
0.79675578013572,0.925830065497239,1.),.UNSPECIFIED.)
GEOMETRIC_REPRESENTATION_ITEM()
RATIONAL_B_SPLINE_SURFACE(((1.14428616678,1.14428616678,1.14428616678,1.14428616678,
1.14428616678,1.14428616678,1.14428616678,1.14428616678,1.14428616678,1.14428616678,
1.14428616678),(0.9519046110735,0.9519046110735,0.9519046110735,0.9519046110735,
0.9519046110735,0.9519046110735,0.9519046110735,0.9519046110735,0.9519046110735,
0.9519046110735,0.9519046110735),(0.9519046110735,0.9519046110735,0.9519046110735,
0.9519046110735,0.9519046110735,0.9519046110735,0.9519046110735,0.9519046110735,
0.9519046110735,0.9519046110735,0.9519046110735),(1.14428616678,1.14428616678,
1.14428616678,1.14428616678,1.14428616678,1.14428616678,1.14428616678,1.14428616678,
1.14428616678,1.14428616678,1.14428616678)))
REPRESENTATION_ITEM('')
SURFACE()
);
#2620=(
BOUNDED_SURFACE()
B_SPLINE_SURFACE(3,3,((#160180,#160181,#160182,#160183,#160184,#160185,
#160186,#160187,#160188,#160189,#160190),(#160191,#160192,#160193,#160194,
#160195,#160196,#160197,#160198,#160199,#160200,#160201),(#160202,#160203,
#160204,#160205,#160206,#160207,#160208,#160209,#160210,#160211,#160212),
(#160213,#160214,#160215,#160216,#160217,#160218,#160219,#160220,#160221,
#160222,#160223)),.UNSPECIFIED.,.F.,.F.,.F.)
B_SPLINE_SURFACE_WITH_KNOTS((4,4),(4,1,1,1,1,1,1,1,4),(0.,1.),(0.,0.0944145406001002,
0.22382893510453,0.356121659603939,0.491296333098967,0.627233999913856,
0.763922934472171,0.907653635910875,1.),.UNSPECIFIED.)
GEOMETRIC_REPRESENTATION_ITEM()
RATIONAL_B_SPLINE_SURFACE(((1.144284885867,1.144284885867,1.144284885867,
1.144284885867,1.144284885867,1.144284885867,1.144284885867,1.144284885867,
1.144284885867,1.144284885867,1.144284885867),(0.9519050380443,0.9519050380443,
0.9519050380443,0.9519050380443,0.9519050380443,0.9519050380443,0.9519050380443,
0.9519050380443,0.9519050380443,0.9519050380443,0.9519050380443),(0.9519050380443,
0.9519050380443,0.9519050380443,0.9519050380443,0.9519050380443,0.9519050380443,
0.9519050380443,0.9519050380443,0.9519050380443,0.9519050380443,0.9519050380443),
(1.144284885867,1.144284885867,1.144284885867,1.144284885867,1.144284885867,
1.144284885867,1.144284885867,1.144284885867,1.144284885867,1.144284885867,
1.144284885867)))
REPRESENTATION_ITEM('')
SURFACE()
);
#2621=(
BOUNDED_SURFACE()
B_SPLINE_SURFACE(3,3,((#160430,#160431,#160432,#160433,#160434,#160435,
#160436,#160437,#160438,#160439),(#160440,#160441,#160442,#160443,#160444,
#160445,#160446,#160447,#160448,#160449),(#160450,#160451,#160452,#160453,
#160454,#160455,#160456,#160457,#160458,#160459),(#160460,#160461,#160462,
#160463,#160464,#160465,#160466,#160467,#160468,#160469)),.UNSPECIFIED.,
 .F.,.F.,.F.)
B_SPLINE_SURFACE_WITH_KNOTS((4,4),(4,1,1,1,1,1,1,4),(0.,1.),(0.,0.146101495488384,
0.319452627218425,0.487967212214235,0.642996851728068,0.781791002263477,
0.905806643913708,1.),.UNSPECIFIED.)
GEOMETRIC_REPRESENTATION_ITEM()
RATIONAL_B_SPLINE_SURFACE(((1.298413325381,1.298413325381,1.298413325381,
1.298413325381,1.298413325381,1.298413325381,1.298413325381,1.298413325381,
1.298413325381,1.298413325381),(0.9005288915396,0.9005288915396,0.9005288915396,
0.9005288915396,0.9005288915396,0.9005288915396,0.9005288915396,0.9005288915396,
0.9005288915396,0.9005288915396),(0.9005288915396,0.9005288915396,0.9005288915396,
0.9005288915396,0.9005288915396,0.9005288915396,0.9005288915396,0.9005288915396,
0.9005288915396,0.9005288915396),(1.298413325381,1.298413325381,1.298413325381,
1.298413325381,1.298413325381,1.298413325381,1.298413325381,1.298413325381,
1.298413325381,1.298413325381)))
REPRESENTATION_ITEM('')
SURFACE()
);
#2622=(
BOUNDED_SURFACE()
B_SPLINE_SURFACE(3,3,((#160471,#160472,#160473,#160474,#160475,#160476,
#160477),(#160478,#160479,#160480,#160481,#160482,#160483,#160484),(#160485,
#160486,#160487,#160488,#160489,#160490,#160491),(#160492,#160493,#160494,
#160495,#160496,#160497,#160498)),.UNSPECIFIED.,.F.,.F.,.F.)
B_SPLINE_SURFACE_WITH_KNOTS((4,4),(4,1,1,1,4),(0.,1.),(0.,0.230593160213399,
0.482348490956705,0.744157121798399,1.),.UNSPECIFIED.)
GEOMETRIC_REPRESENTATION_ITEM()
RATIONAL_B_SPLINE_SURFACE(((1.353838625123,1.353838625123,1.353838625123,
1.353838625123,1.353838625123,1.353838625123,1.353838625123),(0.8820537916258,
0.8820537916258,0.8820537916258,0.8820537916258,0.8820537916258,0.8820537916258,
0.8820537916258),(0.8820537916258,0.8820537916258,0.8820537916258,0.8820537916258,
0.8820537916258,0.8820537916258,0.8820537916258),(1.353838625123,1.353838625123,
1.353838625123,1.353838625123,1.353838625123,1.353838625123,1.353838625123)))
REPRESENTATION_ITEM('')
SURFACE()
);
#2623=(
BOUNDED_SURFACE()
B_SPLINE_SURFACE(3,3,((#160516,#160517,#160518,#160519,#160520,#160521,
#160522,#160523,#160524,#160525),(#160526,#160527,#160528,#160529,#160530,
#160531,#160532,#160533,#160534,#160535),(#160536,#160537,#160538,#160539,
#160540,#160541,#160542,#160543,#160544,#160545),(#160546,#160547,#160548,
#160549,#160550,#160551,#160552,#160553,#160554,#160555)),.UNSPECIFIED.,
 .F.,.F.,.F.)
B_SPLINE_SURFACE_WITH_KNOTS((4,4),(4,1,1,1,1,1,1,4),(0.,1.),(0.,0.13457163316798,
0.282274649724905,0.428486319030034,0.574234601524777,0.720464271965091,
0.868205782040083,1.),.UNSPECIFIED.)
GEOMETRIC_REPRESENTATION_ITEM()
RATIONAL_B_SPLINE_SURFACE(((1.375941287385,1.375941287385,1.375941287385,
1.375941287385,1.375941287385,1.375941287385,1.375941287385,1.375941287385,
1.375941287385,1.375941287385),(0.8746862375382,0.8746862375382,0.8746862375382,
0.8746862375382,0.8746862375382,0.8746862375382,0.8746862375382,0.8746862375382,
0.8746862375382,0.8746862375382),(0.8746862375382,0.8746862375382,0.8746862375382,
0.8746862375382,0.8746862375382,0.8746862375382,0.8746862375382,0.8746862375382,
0.8746862375382,0.8746862375382),(1.375941287385,1.375941287385,1.375941287385,
1.375941287385,1.375941287385,1.375941287385,1.375941287385,1.375941287385,
1.375941287385,1.375941287385)))
REPRESENTATION_ITEM('')
SURFACE()
);
#2624=(
BOUNDED_SURFACE()
B_SPLINE_SURFACE(3,3,((#160619,#160620,#160621,#160622,#160623,#160624,
#160625),(#160626,#160627,#160628,#160629,#160630,#160631,#160632),(#160633,
#160634,#160635,#160636,#160637,#160638,#160639),(#160640,#160641,#160642,
#160643,#160644,#160645,#160646)),.UNSPECIFIED.,.F.,.F.,.F.)
B_SPLINE_SURFACE_WITH_KNOTS((4,4),(4,1,1,1,4),(0.,1.),(0.,0.266221048065604,
0.525168076403688,0.774267556960161,1.),.UNSPECIFIED.)
GEOMETRIC_REPRESENTATION_ITEM()
RATIONAL_B_SPLINE_SURFACE(((1.35383923737,1.35383923737,1.35383923737,1.35383923737,
1.35383923737,1.35383923737,1.35383923737),(0.8820535875433,0.8820535875433,
0.8820535875433,0.8820535875433,0.8820535875433,0.8820535875433,0.8820535875433),
(0.8820535875433,0.8820535875433,0.8820535875433,0.8820535875433,0.8820535875433,
0.8820535875433,0.8820535875433),(1.35383923737,1.35383923737,1.35383923737,
1.35383923737,1.35383923737,1.35383923737,1.35383923737)))
REPRESENTATION_ITEM('')
SURFACE()
);
#2625=(
BOUNDED_SURFACE()
B_SPLINE_SURFACE(3,3,((#160766,#160767,#160768,#160769,#160770,#160771),
(#160772,#160773,#160774,#160775,#160776,#160777),(#160778,#160779,#160780,
#160781,#160782,#160783),(#160784,#160785,#160786,#160787,#160788,#160789)),
 .UNSPECIFIED.,.F.,.F.,.F.)
B_SPLINE_SURFACE_WITH_KNOTS((4,4),(4,1,1,4),(0.,1.),(0.,0.343001553297945,
0.735822721578711,1.),.UNSPECIFIED.)
GEOMETRIC_REPRESENTATION_ITEM()
RATIONAL_B_SPLINE_SURFACE(((1.133911518843,1.133911518843,1.133911518843,
1.133911518843,1.133911518843,1.133911518843),(0.9553628270522,0.9553628270522,
0.9553628270522,0.9553628270522,0.9553628270522,0.9553628270522),(0.9553628270522,
0.9553628270522,0.9553628270522,0.9553628270522,0.9553628270522,0.9553628270522),
(1.133911518843,1.133911518843,1.133911518843,1.133911518843,1.133911518843,
1.133911518843)))
REPRESENTATION_ITEM('')
SURFACE()
);
#2626=(
BOUNDED_SURFACE()
B_SPLINE_SURFACE(3,3,((#160791,#160792,#160793,#160794,#160795,#160796),
(#160797,#160798,#160799,#160800,#160801,#160802),(#160803,#160804,#160805,
#160806,#160807,#160808),(#160809,#160810,#160811,#160812,#160813,#160814)),
 .UNSPECIFIED.,.F.,.F.,.F.)
B_SPLINE_SURFACE_WITH_KNOTS((4,4),(4,1,1,4),(0.,1.),(0.,0.326783840018485,
0.677637015410791,1.),.UNSPECIFIED.)
GEOMETRIC_REPRESENTATION_ITEM()
RATIONAL_B_SPLINE_SURFACE(((1.154127816646,1.154127816646,1.154127816646,
1.154127816646,1.154127816646,1.154127816646),(0.948624061118,0.948624061118,
0.948624061118,0.948624061118,0.948624061118,0.948624061118),(0.948624061118,
0.948624061118,0.948624061118,0.948624061118,0.948624061118,0.948624061118),
(1.154127816646,1.154127816646,1.154127816646,1.154127816646,1.154127816646,
1.154127816646)))
REPRESENTATION_ITEM('')
SURFACE()
);
#2627=(
BOUNDED_SURFACE()
B_SPLINE_SURFACE(3,3,((#160816,#160817,#160818,#160819,#160820,#160821),
(#160822,#160823,#160824,#160825,#160826,#160827),(#160828,#160829,#160830,
#160831,#160832,#160833),(#160834,#160835,#160836,#160837,#160838,#160839)),
 .UNSPECIFIED.,.F.,.F.,.F.)
B_SPLINE_SURFACE_WITH_KNOTS((4,4),(4,1,1,4),(0.,1.),(0.,0.325921012985495,
0.684444108359778,1.),.UNSPECIFIED.)
GEOMETRIC_REPRESENTATION_ITEM()
RATIONAL_B_SPLINE_SURFACE(((1.154128041374,1.154128041374,1.154128041374,
1.154128041374,1.154128041374,1.154128041374),(0.9486239862088,0.9486239862088,
0.9486239862088,0.9486239862088,0.9486239862088,0.9486239862088),(0.9486239862088,
0.9486239862088,0.9486239862088,0.9486239862088,0.9486239862088,0.9486239862088),
(1.154128041374,1.154128041374,1.154128041374,1.154128041374,1.154128041374,
1.154128041374)))
REPRESENTATION_ITEM('')
SURFACE()
);
#2628=(
BOUNDED_SURFACE()
B_SPLINE_SURFACE(3,3,((#160840,#160841,#160842,#160843,#160844,#160845),
(#160846,#160847,#160848,#160849,#160850,#160851),(#160852,#160853,#160854,
#160855,#160856,#160857),(#160858,#160859,#160860,#160861,#160862,#160863)),
 .UNSPECIFIED.,.F.,.F.,.F.)
B_SPLINE_SURFACE_WITH_KNOTS((4,4),(4,1,1,4),(0.,1.),(0.,0.298212289448515,
0.67415586424402,1.),.UNSPECIFIED.)
GEOMETRIC_REPRESENTATION_ITEM()
RATIONAL_B_SPLINE_SURFACE(((1.133911518295,1.133911518295,1.133911518295,
1.133911518295,1.133911518295,1.133911518295),(0.955362827235,0.955362827235,
0.955362827235,0.955362827235,0.955362827235,0.955362827235),(0.955362827235,
0.955362827235,0.955362827235,0.955362827235,0.955362827235,0.955362827235),
(1.133911518295,1.133911518295,1.133911518295,1.133911518295,1.133911518295,
1.133911518295)))
REPRESENTATION_ITEM('')
SURFACE()
);
#2629=(
BOUNDED_SURFACE()
B_SPLINE_SURFACE(3,3,((#161268,#161269,#161270,#161271,#161272,#161273,
#161274,#161275,#161276,#161277,#161278,#161279,#161280,#161281,#161282,
#161283,#161284,#161285,#161286,#161287,#161288,#161289,#161290,#161291,
#161292,#161293,#161294,#161295,#161296,#161297,#161298,#161299,#161300,
#161301,#161302,#161303,#161304,#161305,#161306,#161307),(#161308,#161309,
#161310,#161311,#161312,#161313,#161314,#161315,#161316,#161317,#161318,
#161319,#161320,#161321,#161322,#161323,#161324,#161325,#161326,#161327,
#161328,#161329,#161330,#161331,#161332,#161333,#161334,#161335,#161336,
#161337,#161338,#161339,#161340,#161341,#161342,#161343,#161344,#161345,
#161346,#161347),(#161348,#161349,#161350,#161351,#161352,#161353,#161354,
#161355,#161356,#161357,#161358,#161359,#161360,#161361,#161362,#161363,
#161364,#161365,#161366,#161367,#161368,#161369,#161370,#161371,#161372,
#161373,#161374,#161375,#161376,#161377,#161378,#161379,#161380,#161381,
#161382,#161383,#161384,#161385,#161386,#161387),(#161388,#161389,#161390,
#161391,#161392,#161393,#161394,#161395,#161396,#161397,#161398,#161399,
#161400,#161401,#161402,#161403,#161404,#161405,#161406,#161407,#161408,
#161409,#161410,#161411,#161412,#161413,#161414,#161415,#161416,#161417,
#161418,#161419,#161420,#161421,#161422,#161423,#161424,#161425,#161426,
#161427)),.UNSPECIFIED.,.F.,.F.,.F.)
B_SPLINE_SURFACE_WITH_KNOTS((4,4),(4,1,1,1,1,1,1,1,1,1,1,1,1,1,1,1,1,1,
1,1,1,1,1,1,1,1,1,1,1,1,1,1,1,1,1,1,1,4),(0.,1.),(0.,0.0080855657193485,
0.0596218558242468,0.106852501388389,0.150184164955898,0.19003235366263,
0.226816246755187,0.260884487830858,0.292377213220895,0.321411667226958,
0.348115402080392,0.372633477126632,0.395157121664735,0.415908415220206,
0.434997267820443,0.452409696784467,0.468313480733662,0.482712550753752,
0.495419214437213,0.507133333503985,0.519448003687265,0.533357648922,0.548832281415337,
0.566241232560042,0.585544933168279,0.606300542403394,0.628001557637231,
0.650281261920833,0.673235965567153,0.698456243264167,0.725991202217506,
0.755882932612454,0.78864738633083,0.824762418308521,0.864558914403212,
0.908348167961349,0.956921864249176,1.),.UNSPECIFIED.)
GEOMETRIC_REPRESENTATION_ITEM()
RATIONAL_B_SPLINE_SURFACE(((1.046091568931,1.046091568931,1.046091568931,
1.046091568931,1.046091568931,1.046091568931,1.046091568931,1.046091568931,
1.046091568931,1.046091568931,1.046091568931,1.046091568931,1.046091568931,
1.046091568931,1.046091568931,1.046091568931,1.046091568931,1.046091568931,
1.046091568931,1.046091568931,1.046091568931,1.046091568931,1.046091568931,
1.046091568931,1.046091568931,1.046091568931,1.046091568931,1.046091568931,
1.046091568931,1.046091568931,1.046091568931,1.046091568931,1.046091568931,
1.046091568931,1.046091568931,1.046091568931,1.046091568931,1.046091568931,
1.046091568931,1.046091568931),(0.9846361436895,0.9846361436895,0.9846361436895,
0.9846361436895,0.9846361436895,0.9846361436895,0.9846361436895,0.9846361436895,
0.9846361436895,0.9846361436895,0.9846361436895,0.9846361436895,0.9846361436895,
0.9846361436895,0.9846361436895,0.9846361436895,0.9846361436895,0.9846361436895,
0.9846361436895,0.9846361436895,0.9846361436895,0.9846361436895,0.9846361436895,
0.9846361436895,0.9846361436895,0.9846361436895,0.9846361436895,0.9846361436895,
0.9846361436895,0.9846361436895,0.9846361436895,0.9846361436895,0.9846361436895,
0.9846361436895,0.9846361436895,0.9846361436895,0.9846361436895,0.9846361436895,
0.9846361436895,0.9846361436895),(0.9846361436895,0.9846361436895,0.9846361436895,
0.9846361436895,0.9846361436895,0.9846361436895,0.9846361436895,0.9846361436895,
0.9846361436895,0.9846361436895,0.9846361436895,0.9846361436895,0.9846361436895,
0.9846361436895,0.9846361436895,0.9846361436895,0.9846361436895,0.9846361436895,
0.9846361436895,0.9846361436895,0.9846361436895,0.9846361436895,0.9846361436895,
0.9846361436895,0.9846361436895,0.9846361436895,0.9846361436895,0.9846361436895,
0.9846361436895,0.9846361436895,0.9846361436895,0.9846361436895,0.9846361436895,
0.9846361436895,0.9846361436895,0.9846361436895,0.9846361436895,0.9846361436895,
0.9846361436895,0.9846361436895),(1.046091568931,1.046091568931,1.046091568931,
1.046091568931,1.046091568931,1.046091568931,1.046091568931,1.046091568931,
1.046091568931,1.046091568931,1.046091568931,1.046091568931,1.046091568931,
1.046091568931,1.046091568931,1.046091568931,1.046091568931,1.046091568931,
1.046091568931,1.046091568931,1.046091568931,1.046091568931,1.046091568931,
1.046091568931,1.046091568931,1.046091568931,1.046091568931,1.046091568931,
1.046091568931,1.046091568931,1.046091568931,1.046091568931,1.046091568931,
1.046091568931,1.046091568931,1.046091568931,1.046091568931,1.046091568931,
1.046091568931,1.046091568931)))
REPRESENTATION_ITEM('')
SURFACE()
);
#2630=(
BOUNDED_SURFACE()
B_SPLINE_SURFACE(3,3,((#161772,#161773,#161774,#161775,#161776,#161777),
(#161778,#161779,#161780,#161781,#161782,#161783),(#161784,#161785,#161786,
#161787,#161788,#161789),(#161790,#161791,#161792,#161793,#161794,#161795)),
 .UNSPECIFIED.,.F.,.F.,.F.)
B_SPLINE_SURFACE_WITH_KNOTS((4,4),(4,1,1,4),(0.,1.),(0.,0.297847735602895,
0.685768611894679,1.),.UNSPECIFIED.)
GEOMETRIC_REPRESENTATION_ITEM()
RATIONAL_B_SPLINE_SURFACE(((1.064510917442,1.064510917442,1.064510917442,
1.064510917442,1.064510917442,1.064510917442),(0.9784963608528,0.9784963608528,
0.9784963608528,0.9784963608528,0.9784963608528,0.9784963608528),(0.9784963608528,
0.9784963608528,0.9784963608528,0.9784963608528,0.9784963608528,0.9784963608528),
(1.064510917442,1.064510917442,1.064510917442,1.064510917442,1.064510917442,
1.064510917442)))
REPRESENTATION_ITEM('')
SURFACE()
);
#2631=(
BOUNDED_SURFACE()
B_SPLINE_SURFACE(3,3,((#161798,#161799,#161800,#161801,#161802,#161803,
#161804,#161805,#161806,#161807,#161808,#161809,#161810,#161811),(#161812,
#161813,#161814,#161815,#161816,#161817,#161818,#161819,#161820,#161821,
#161822,#161823,#161824,#161825),(#161826,#161827,#161828,#161829,#161830,
#161831,#161832,#161833,#161834,#161835,#161836,#161837,#161838,#161839),
(#161840,#161841,#161842,#161843,#161844,#161845,#161846,#161847,#161848,
#161849,#161850,#161851,#161852,#161853)),.UNSPECIFIED.,.F.,.F.,.F.)
B_SPLINE_SURFACE_WITH_KNOTS((4,4),(4,1,1,1,1,1,1,1,1,1,1,4),(0.,1.),(0.,
0.0507109297548065,0.123516716092259,0.193792769620065,0.266862729149513,
0.34659901892772,0.435171212264714,0.53358024119019,0.644372653483454,0.767724369233791,
0.895033447798833,1.),.UNSPECIFIED.)
GEOMETRIC_REPRESENTATION_ITEM()
RATIONAL_B_SPLINE_SURFACE(((1.133915806589,1.133915806589,1.133915806589,
1.133915806589,1.133915806589,1.133915806589,1.133915806589,1.133915806589,
1.133915806589,1.133915806589,1.133915806589,1.133915806589,1.133915806589,
1.133915806589),(0.9553613978037,0.9553613978037,0.9553613978037,0.9553613978037,
0.9553613978037,0.9553613978037,0.9553613978037,0.9553613978037,0.9553613978037,
0.9553613978037,0.9553613978037,0.9553613978037,0.9553613978037,0.9553613978037),
(0.9553613978037,0.9553613978037,0.9553613978037,0.9553613978037,0.9553613978037,
0.9553613978037,0.9553613978037,0.9553613978037,0.9553613978037,0.9553613978037,
0.9553613978037,0.9553613978037,0.9553613978037,0.9553613978037),(1.133915806589,
1.133915806589,1.133915806589,1.133915806589,1.133915806589,1.133915806589,
1.133915806589,1.133915806589,1.133915806589,1.133915806589,1.133915806589,
1.133915806589,1.133915806589,1.133915806589)))
REPRESENTATION_ITEM('')
SURFACE()
);
#2632=(
BOUNDED_SURFACE()
B_SPLINE_SURFACE(3,3,((#161854,#161855,#161856,#161857,#161858,#161859,
#161860,#161861,#161862,#161863,#161864,#161865,#161866,#161867),(#161868,
#161869,#161870,#161871,#161872,#161873,#161874,#161875,#161876,#161877,
#161878,#161879,#161880,#161881),(#161882,#161883,#161884,#161885,#161886,
#161887,#161888,#161889,#161890,#161891,#161892,#161893,#161894,#161895),
(#161896,#161897,#161898,#161899,#161900,#161901,#161902,#161903,#161904,
#161905,#161906,#161907,#161908,#161909)),.UNSPECIFIED.,.F.,.F.,.F.)
B_SPLINE_SURFACE_WITH_KNOTS((4,4),(4,1,1,1,1,1,1,1,1,1,1,4),(0.,1.),(0.,
0.104814911231639,0.230943732857245,0.351656664711374,0.461900769684698,
0.561079572404948,0.649863357676646,0.729556548498204,0.802369461782467,
0.872320141269624,0.94477376676948,1.),.UNSPECIFIED.)
GEOMETRIC_REPRESENTATION_ITEM()
RATIONAL_B_SPLINE_SURFACE(((1.133915819794,1.133915819794,1.133915819794,
1.133915819794,1.133915819794,1.133915819794,1.133915819794,1.133915819794,
1.133915819794,1.133915819794,1.133915819794,1.133915819794,1.133915819794,
1.133915819794),(0.955361393402,0.955361393402,0.955361393402,0.955361393402,
0.955361393402,0.955361393402,0.955361393402,0.955361393402,0.955361393402,
0.955361393402,0.955361393402,0.955361393402,0.955361393402,0.955361393402),
(0.955361393402,0.955361393402,0.955361393402,0.955361393402,0.955361393402,
0.955361393402,0.955361393402,0.955361393402,0.955361393402,0.955361393402,
0.955361393402,0.955361393402,0.955361393402,0.955361393402),(1.133915819794,
1.133915819794,1.133915819794,1.133915819794,1.133915819794,1.133915819794,
1.133915819794,1.133915819794,1.133915819794,1.133915819794,1.133915819794,
1.133915819794,1.133915819794,1.133915819794)))
REPRESENTATION_ITEM('')
SURFACE()
);
#2633=(
BOUNDED_SURFACE()
B_SPLINE_SURFACE(3,3,((#161911,#161912,#161913,#161914,#161915,#161916),
(#161917,#161918,#161919,#161920,#161921,#161922),(#161923,#161924,#161925,
#161926,#161927,#161928),(#161929,#161930,#161931,#161932,#161933,#161934)),
 .UNSPECIFIED.,.F.,.F.,.F.)
B_SPLINE_SURFACE_WITH_KNOTS((4,4),(4,1,1,4),(0.,1.),(0.,0.325174256189807,
0.72869537342957,1.),.UNSPECIFIED.)
GEOMETRIC_REPRESENTATION_ITEM()
RATIONAL_B_SPLINE_SURFACE(((1.064511164288,1.064511164288,1.064511164288,
1.064511164288,1.064511164288,1.064511164288),(0.9784962785707,0.9784962785707,
0.9784962785707,0.9784962785707,0.9784962785707,0.9784962785707),(0.9784962785707,
0.9784962785707,0.9784962785707,0.9784962785707,0.9784962785707,0.9784962785707),
(1.064511164288,1.064511164288,1.064511164288,1.064511164288,1.064511164288,
1.064511164288)))
REPRESENTATION_ITEM('')
SURFACE()
);
#2634=ELLIPSE('',#79489,7.3350975987285,0.32648194728831);
#2635=ELLIPSE('',#79497,7.83636103876833,0.373161200194601);
#2636=ELLIPSE('',#79579,12.7157342481197,10.9354621733428);
#2637=ELLIPSE('',#79581,12.7157342481197,10.9354621733428);
#2638=ELLIPSE('',#79623,8.41787972385908,7.11051334783377);
#2639=ELLIPSE('',#79624,9.74678054815318,7.6569975264341);
#2640=ELLIPSE('',#79625,8.32808509851651,7.07191618373715);
#2641=ELLIPSE('',#79626,9.18146121407547,7.43010531309855);
#2642=ELLIPSE('',#79642,14.1342891289832,8.17227711305746);
#2643=ELLIPSE('',#79746,0.448239149373515,0.327540749333151);
#2644=ELLIPSE('',#79856,0.537354784288396,0.471561563563283);
#2645=ELLIPSE('',#79960,3.55794038290777,3.09770950143825);
#2646=ELLIPSE('',#79962,3.55430359086793,3.0925288495517);
#2647=ELLIPSE('',#79989,0.230877359575232,0.0439685216321683);
#2648=ELLIPSE('',#79992,0.999999440004323,0.999956206655532);
#2649=ELLIPSE('',#79993,0.58212397125333,0.288222735668278);
#2650=ELLIPSE('',#79994,1.00000913814908,1.00000372087532);
#2651=ELLIPSE('',#79996,0.99999751649857,0.999949952913826);
#2652=ELLIPSE('',#79997,0.461878026571497,0.20445740323273);
#2653=ELLIPSE('',#79999,0.570625652506482,0.279442134038595);
#2654=ELLIPSE('',#80000,1.00000820510229,1.00000324016541);
#2655=ELLIPSE('',#80036,5.77975652153566,1.73376523826803);
#2656=ELLIPSE('',#80037,5.77975702315866,1.73376510670019);
#2657=ELLIPSE('',#80040,7.98766575140942,6.54138279610246);
#2658=ELLIPSE('',#80041,7.89479656652042,6.50286203782701);
#2659=ELLIPSE('',#80048,6.68093268230233,6.48391619812492);
#2660=ELLIPSE('',#80050,17.8204676442288,10.8665310134287);
#2661=ELLIPSE('',#80054,17.8216755759407,10.8669283569276);
#2662=ELLIPSE('',#80055,13.7004973761119,10.3996515308452);
#2663=ELLIPSE('',#80056,17.8213078488318,10.8675975589238);
#2664=ELLIPSE('',#80058,0.300578905254033,0.300169332845296);
#2665=ELLIPSE('',#80061,0.300501638187859,0.300145087153444);
#2666=ELLIPSE('',#80063,26.0448166050072,22.5188326364935);
#2667=ELLIPSE('',#80067,26.0445282577398,22.5188288456468);
#2668=ELLIPSE('',#80075,1.16678567996192,0.984956908240673);
#2669=ELLIPSE('',#80080,2.02790772505133,1.32306037298937);
#2670=ELLIPSE('',#80086,1.50087549620214,1.50024072486622);
#2671=ELLIPSE('',#80109,1.00000429582904,0.999959765461321);
#2672=ELLIPSE('',#80119,7.36743767248193,6.31153366741115);
#2673=ELLIPSE('',#80120,7.3643766184232,6.30732810291296);
#2674=ELLIPSE('',#80121,7.36683820377045,6.30652372661992);
#2675=ELLIPSE('',#80198,6.01936442072139,4.02510096151128);
#2676=ELLIPSE('',#80199,1.50007989461004,1.49835565329252);
#2677=ELLIPSE('',#80201,7.45835235668087,6.38816819337483);
#2678=ELLIPSE('',#80203,14.4207325249774,8.05921542126747);
#2679=ELLIPSE('',#80210,7.92572203798161,6.57522559953783);
#2680=ELLIPSE('',#80324,1.50007991586928,1.49835521240408);
#2681=ELLIPSE('',#80325,6.01990921502876,4.02545539685083);
#2682=ELLIPSE('',#80364,7.9772978335424,6.59922188838911);
#2683=ELLIPSE('',#80385,23.1884969675686,21.5);
#2684=ELLIPSE('',#80387,23.1884969675686,21.5);
#2685=ELLIPSE('',#80391,21.5706948535507,20.0000000000001);
#2686=ELLIPSE('',#80394,21.5706948535507,20.0000000000001);
#2687=ELLIPSE('',#80397,22.4931093186433,20.8022577124141);
#2688=ELLIPSE('',#80399,22.4931093186513,20.8022577124259);
#2689=ELLIPSE('',#80461,1.38995187870583,0.982694699824574);
#2690=ELLIPSE('',#80465,1.42205238917504,1.00538969185979);
#2691=ELLIPSE('',#80468,1.42205238916912,1.00538969185822);
#2692=ELLIPSE('',#80480,1.38995186236733,0.982694649787225);
#2693=ELLIPSE('',#80508,57.0184616553497,7.46584982016915);
#2694=ELLIPSE('',#80513,64.4723561020752,8.58068888240209);
#2695=ELLIPSE('',#80518,60.7406503949971,10.3416271531119);
#2696=ELLIPSE('',#80520,62.3232622923384,10.641597160497);
#2697=ELLIPSE('',#86017,4.91756185694802,4.75000000000025);
#2698=ELLIPSE('',#86018,4.91756185694662,4.74999999999883);
#2699=ELLIPSE('',#86109,4.91756185694817,4.75000000000039);
#2700=ELLIPSE('',#86110,4.91756185694847,4.75000000000065);
#2701=LINE('',#106613,#9768);
#2702=LINE('',#106615,#9769);
#2703=LINE('',#106950,#9770);
#2704=LINE('',#106951,#9771);
#2705=LINE('',#107207,#9772);
#2706=LINE('',#107758,#9773);
#2707=LINE('',#107759,#9774);
#2708=LINE('',#108267,#9775);
#2709=LINE('',#108825,#9776);
#2710=LINE('',#108827,#9777);
#2711=LINE('',#109125,#9778);
#2712=LINE('',#109254,#9779);
#2713=LINE('',#109326,#9780);
#2714=LINE('',#109441,#9781);
#2715=LINE('',#109491,#9782);
#2716=LINE('',#109604,#9783);
#2717=LINE('',#109681,#9784);
#2718=LINE('',#109724,#9785);
#2719=LINE('',#109768,#9786);
#2720=LINE('',#109996,#9787);
#2721=LINE('',#110222,#9788);
#2722=LINE('',#110454,#9789);
#2723=LINE('',#110486,#9790);
#2724=LINE('',#110567,#9791);
#2725=LINE('',#110648,#9792);
#2726=LINE('',#110787,#9793);
#2727=LINE('',#111047,#9794);
#2728=LINE('',#111463,#9795);
#2729=LINE('',#111492,#9796);
#2730=LINE('',#111578,#9797);
#2731=LINE('',#111581,#9798);
#2732=LINE('',#111587,#9799);
#2733=LINE('',#111599,#9800);
#2734=LINE('',#111650,#9801);
#2735=LINE('',#111651,#9802);
#2736=LINE('',#112256,#9803);
#2737=LINE('',#113128,#9804);
#2738=LINE('',#113325,#9805);
#2739=LINE('',#113362,#9806);
#2740=LINE('',#113388,#9807);
#2741=LINE('',#113394,#9808);
#2742=LINE('',#113431,#9809);
#2743=LINE('',#113453,#9810);
#2744=LINE('',#113459,#9811);
#2745=LINE('',#113465,#9812);
#2746=LINE('',#113471,#9813);
#2747=LINE('',#113524,#9814);
#2748=LINE('',#113530,#9815);
#2749=LINE('',#113538,#9816);
#2750=LINE('',#113664,#9817);
#2751=LINE('',#113667,#9818);
#2752=LINE('',#113930,#9819);
#2753=LINE('',#113934,#9820);
#2754=LINE('',#113960,#9821);
#2755=LINE('',#114235,#9822);
#2756=LINE('',#114914,#9823);
#2757=LINE('',#115280,#9824);
#2758=LINE('',#115284,#9825);
#2759=LINE('',#115455,#9826);
#2760=LINE('',#115461,#9827);
#2761=LINE('',#115604,#9828);
#2762=LINE('',#115609,#9829);
#2763=LINE('',#115616,#9830);
#2764=LINE('',#115621,#9831);
#2765=LINE('',#115628,#9832);
#2766=LINE('',#115651,#9833);
#2767=LINE('',#115665,#9834);
#2768=LINE('',#115678,#9835);
#2769=LINE('',#116093,#9836);
#2770=LINE('',#116707,#9837);
#2771=LINE('',#116711,#9838);
#2772=LINE('',#116714,#9839);
#2773=LINE('',#116748,#9840);
#2774=LINE('',#116751,#9841);
#2775=LINE('',#116756,#9842);
#2776=LINE('',#116763,#9843);
#2777=LINE('',#116768,#9844);
#2778=LINE('',#116775,#9845);
#2779=LINE('',#116798,#9846);
#2780=LINE('',#116812,#9847);
#2781=LINE('',#116817,#9848);
#2782=LINE('',#116819,#9849);
#2783=LINE('',#116821,#9850);
#2784=LINE('',#116823,#9851);
#2785=LINE('',#116825,#9852);
#2786=LINE('',#116826,#9853);
#2787=LINE('',#116828,#9854);
#2788=LINE('',#116829,#9855);
#2789=LINE('',#116831,#9856);
#2790=LINE('',#116833,#9857);
#2791=LINE('',#116835,#9858);
#2792=LINE('',#116837,#9859);
#2793=LINE('',#116844,#9860);
#2794=LINE('',#116848,#9861);
#2795=LINE('',#117113,#9862);
#2796=LINE('',#117115,#9863);
#2797=LINE('',#117118,#9864);
#2798=LINE('',#117357,#9865);
#2799=LINE('',#117369,#9866);
#2800=LINE('',#117504,#9867);
#2801=LINE('',#117507,#9868);
#2802=LINE('',#117509,#9869);
#2803=LINE('',#117618,#9870);
#2804=LINE('',#117619,#9871);
#2805=LINE('',#118955,#9872);
#2806=LINE('',#118971,#9873);
#2807=LINE('',#119357,#9874);
#2808=LINE('',#119373,#9875);
#2809=LINE('',#119490,#9876);
#2810=LINE('',#119623,#9877);
#2811=LINE('',#119803,#9878);
#2812=LINE('',#122245,#9879);
#2813=LINE('',#122357,#9880);
#2814=LINE('',#122508,#9881);
#2815=LINE('',#123595,#9882);
#2816=LINE('',#123597,#9883);
#2817=LINE('',#123599,#9884);
#2818=LINE('',#123601,#9885);
#2819=LINE('',#123603,#9886);
#2820=LINE('',#123604,#9887);
#2821=LINE('',#123606,#9888);
#2822=LINE('',#123607,#9889);
#2823=LINE('',#123609,#9890);
#2824=LINE('',#123611,#9891);
#2825=LINE('',#123613,#9892);
#2826=LINE('',#123615,#9893);
#2827=LINE('',#123743,#9894);
#2828=LINE('',#123747,#9895);
#2829=LINE('',#124100,#9896);
#2830=LINE('',#124102,#9897);
#2831=LINE('',#124362,#9898);
#2832=LINE('',#124433,#9899);
#2833=LINE('',#124436,#9900);
#2834=LINE('',#124472,#9901);
#2835=LINE('',#124473,#9902);
#2836=LINE('',#124716,#9903);
#2837=LINE('',#124739,#9904);
#2838=LINE('',#125405,#9905);
#2839=LINE('',#125420,#9906);
#2840=LINE('',#125981,#9907);
#2841=LINE('',#126076,#9908);
#2842=LINE('',#126214,#9909);
#2843=LINE('',#126231,#9910);
#2844=LINE('',#126387,#9911);
#2845=LINE('',#128721,#9912);
#2846=LINE('',#128799,#9913);
#2847=LINE('',#128951,#9914);
#2848=LINE('',#130145,#9915);
#2849=LINE('',#130316,#9916);
#2850=LINE('',#130323,#9917);
#2851=LINE('',#130325,#9918);
#2852=LINE('',#130327,#9919);
#2853=LINE('',#130329,#9920);
#2854=LINE('',#130342,#9921);
#2855=LINE('',#130344,#9922);
#2856=LINE('',#130346,#9923);
#2857=LINE('',#130357,#9924);
#2858=LINE('',#130360,#9925);
#2859=LINE('',#130362,#9926);
#2860=LINE('',#130366,#9927);
#2861=LINE('',#130368,#9928);
#2862=LINE('',#130376,#9929);
#2863=LINE('',#130405,#9930);
#2864=LINE('',#130459,#9931);
#2865=LINE('',#130461,#9932);
#2866=LINE('',#130462,#9933);
#2867=LINE('',#130599,#9934);
#2868=LINE('',#130809,#9935);
#2869=LINE('',#131031,#9936);
#2870=LINE('',#131158,#9937);
#2871=LINE('',#131190,#9938);
#2872=LINE('',#131323,#9939);
#2873=LINE('',#131351,#9940);
#2874=LINE('',#131878,#9941);
#2875=LINE('',#131892,#9942);
#2876=LINE('',#132386,#9943);
#2877=LINE('',#133459,#9944);
#2878=LINE('',#133466,#9945);
#2879=LINE('',#133470,#9946);
#2880=LINE('',#133472,#9947);
#2881=LINE('',#133473,#9948);
#2882=LINE('',#133475,#9949);
#2883=LINE('',#134436,#9950);
#2884=LINE('',#134583,#9951);
#2885=LINE('',#134694,#9952);
#2886=LINE('',#134712,#9953);
#2887=LINE('',#135396,#9954);
#2888=LINE('',#135398,#9955);
#2889=LINE('',#135577,#9956);
#2890=LINE('',#135578,#9957);
#2891=LINE('',#135614,#9958);
#2892=LINE('',#135619,#9959);
#2893=LINE('',#135625,#9960);
#2894=LINE('',#135629,#9961);
#2895=LINE('',#135644,#9962);
#2896=LINE('',#136522,#9963);
#2897=LINE('',#137848,#9964);
#2898=LINE('',#137895,#9965);
#2899=LINE('',#137934,#9966);
#2900=LINE('',#138666,#9967);
#2901=LINE('',#138705,#9968);
#2902=LINE('',#139066,#9969);
#2903=LINE('',#141026,#9970);
#2904=LINE('',#142940,#9971);
#2905=LINE('',#143028,#9972);
#2906=LINE('',#143481,#9973);
#2907=LINE('',#143689,#9974);
#2908=LINE('',#143853,#9975);
#2909=LINE('',#144373,#9976);
#2910=LINE('',#145397,#9977);
#2911=LINE('',#145399,#9978);
#2912=LINE('',#145401,#9979);
#2913=LINE('',#145402,#9980);
#2914=LINE('',#145404,#9981);
#2915=LINE('',#145411,#9982);
#2916=LINE('',#145415,#9983);
#2917=LINE('',#145500,#9984);
#2918=LINE('',#145576,#9985);
#2919=LINE('',#145595,#9986);
#2920=LINE('',#145631,#9987);
#2921=LINE('',#145831,#9988);
#2922=LINE('',#145834,#9989);
#2923=LINE('',#145881,#9990);
#2924=LINE('',#145883,#9991);
#2925=LINE('',#145885,#9992);
#2926=LINE('',#145948,#9993);
#2927=LINE('',#146296,#9994);
#2928=LINE('',#146299,#9995);
#2929=LINE('',#146333,#9996);
#2930=LINE('',#146364,#9997);
#2931=LINE('',#146366,#9998);
#2932=LINE('',#146367,#9999);
#2933=LINE('',#146906,#10000);
#2934=LINE('',#146909,#10001);
#2935=LINE('',#146910,#10002);
#2936=LINE('',#146914,#10003);
#2937=LINE('',#146916,#10004);
#2938=LINE('',#146917,#10005);
#2939=LINE('',#147574,#10006);
#2940=LINE('',#147714,#10007);
#2941=LINE('',#147721,#10008);
#2942=LINE('',#149827,#10009);
#2943=LINE('',#149867,#10010);
#2944=LINE('',#149954,#10011);
#2945=LINE('',#149957,#10012);
#2946=LINE('',#150111,#10013);
#2947=LINE('',#150150,#10014);
#2948=LINE('',#150202,#10015);
#2949=LINE('',#150257,#10016);
#2950=LINE('',#150259,#10017);
#2951=LINE('',#154828,#10018);
#2952=LINE('',#154832,#10019);
#2953=LINE('',#154966,#10020);
#2954=LINE('',#156808,#10021);
#2955=LINE('',#156999,#10022);
#2956=LINE('',#158442,#10023);
#2957=LINE('',#158463,#10024);
#2958=LINE('',#158665,#10025);
#2959=LINE('',#158710,#10026);
#2960=LINE('',#158718,#10027);
#2961=LINE('',#158739,#10028);
#2962=LINE('',#158764,#10029);
#2963=LINE('',#159026,#10030);
#2964=LINE('',#159059,#10031);
#2965=LINE('',#159061,#10032);
#2966=LINE('',#159063,#10033);
#2967=LINE('',#159064,#10034);
#2968=LINE('',#159070,#10035);
#2969=LINE('',#159074,#10036);
#2970=LINE('',#159078,#10037);
#2971=LINE('',#159080,#10038);
#2972=LINE('',#159086,#10039);
#2973=LINE('',#159089,#10040);
#2974=LINE('',#159092,#10041);
#2975=LINE('',#159094,#10042);
#2976=LINE('',#159098,#10043);
#2977=LINE('',#159099,#10044);
#2978=LINE('',#159102,#10045);
#2979=LINE('',#159105,#10046);
#2980=LINE('',#159109,#10047);
#2981=LINE('',#159111,#10048);
#2982=LINE('',#159113,#10049);
#2983=LINE('',#159114,#10050);
#2984=LINE('',#159119,#10051);
#2985=LINE('',#159123,#10052);
#2986=LINE('',#159125,#10053);
#2987=LINE('',#159126,#10054);
#2988=LINE('',#159131,#10055);
#2989=LINE('',#159135,#10056);
#2990=LINE('',#159137,#10057);
#2991=LINE('',#159138,#10058);
#2992=LINE('',#159144,#10059);
#2993=LINE('',#159152,#10060);
#2994=LINE('',#159160,#10061);
#2995=LINE('',#159169,#10062);
#2996=LINE('',#159173,#10063);
#2997=LINE('',#159175,#10064);
#2998=LINE('',#159176,#10065);
#2999=LINE('',#159334,#10066);
#3000=LINE('',#159510,#10067);
#3001=LINE('',#159512,#10068);
#3002=LINE('',#159516,#10069);
#3003=LINE('',#159517,#10070);
#3004=LINE('',#159518,#10071);
#3005=LINE('',#159522,#10072);
#3006=LINE('',#159685,#10073);
#3007=LINE('',#159692,#10074);
#3008=LINE('',#159695,#10075);
#3009=LINE('',#159696,#10076);
#3010=LINE('',#159700,#10077);
#3011=LINE('',#159704,#10078);
#3012=LINE('',#159706,#10079);
#3013=LINE('',#159708,#10080);
#3014=LINE('',#159710,#10081);
#3015=LINE('',#159712,#10082);
#3016=LINE('',#159714,#10083);
#3017=LINE('',#159716,#10084);
#3018=LINE('',#159717,#10085);
#3019=LINE('',#159720,#10086);
#3020=LINE('',#159722,#10087);
#3021=LINE('',#159723,#10088);
#3022=LINE('',#159726,#10089);
#3023=LINE('',#159727,#10090);
#3024=LINE('',#159730,#10091);
#3025=LINE('',#159731,#10092);
#3026=LINE('',#159734,#10093);
#3027=LINE('',#159735,#10094);
#3028=LINE('',#159738,#10095);
#3029=LINE('',#159739,#10096);
#3030=LINE('',#159742,#10097);
#3031=LINE('',#159743,#10098);
#3032=LINE('',#159746,#10099);
#3033=LINE('',#159747,#10100);
#3034=LINE('',#159749,#10101);
#3035=LINE('',#159753,#10102);
#3036=LINE('',#159754,#10103);
#3037=LINE('',#160179,#10104);
#3038=LINE('',#160332,#10105);
#3039=LINE('',#160675,#10106);
#3040=LINE('',#160980,#10107);
#3041=LINE('',#161941,#10108);
#3042=LINE('',#162330,#10109);
#3043=LINE('',#162956,#10110);
#3044=LINE('',#163166,#10111);
#3045=LINE('',#163572,#10112);
#3046=LINE('',#163993,#10113);
#3047=LINE('',#164421,#10114);
#3048=LINE('',#164833,#10115);
#3049=LINE('',#165106,#10116);
#3050=LINE('',#165636,#10117);
#3051=LINE('',#166150,#10118);
#3052=LINE('',#166686,#10119);
#3053=LINE('',#167210,#10120);
#3054=LINE('',#167730,#10121);
#3055=LINE('',#168256,#10122);
#3056=LINE('',#168283,#10123);
#3057=LINE('',#168630,#10124);
#3058=LINE('',#169158,#10125);
#3059=LINE('',#169674,#10126);
#3060=LINE('',#170192,#10127);
#3061=LINE('',#170718,#10128);
#3062=LINE('',#171017,#10129);
#3063=LINE('',#171447,#10130);
#3064=LINE('',#171891,#10131);
#3065=LINE('',#172549,#10132);
#3066=LINE('',#172769,#10133);
#3067=LINE('',#173217,#10134);
#3068=LINE('',#173296,#10135);
#3069=LINE('',#173304,#10136);
#3070=LINE('',#173310,#10137);
#3071=LINE('',#173726,#10138);
#3072=LINE('',#173793,#10139);
#3073=LINE('',#173799,#10140);
#3074=LINE('',#173806,#10141);
#3075=LINE('',#173821,#10142);
#3076=LINE('',#173824,#10143);
#3077=LINE('',#173948,#10144);
#3078=LINE('',#174618,#10145);
#3079=LINE('',#174620,#10146);
#3080=LINE('',#174621,#10147);
#3081=LINE('',#174624,#10148);
#3082=LINE('',#174626,#10149);
#3083=LINE('',#174627,#10150);
#3084=LINE('',#174630,#10151);
#3085=LINE('',#174632,#10152);
#3086=LINE('',#174633,#10153);
#3087=LINE('',#174638,#10154);
#3088=LINE('',#174642,#10155);
#3089=LINE('',#174644,#10156);
#3090=LINE('',#174645,#10157);
#3091=LINE('',#174648,#10158);
#3092=LINE('',#174650,#10159);
#3093=LINE('',#174651,#10160);
#3094=LINE('',#174653,#10161);
#3095=LINE('',#174654,#10162);
#3096=LINE('',#174660,#10163);
#3097=LINE('',#174662,#10164);
#3098=LINE('',#174664,#10165);
#3099=LINE('',#174666,#10166);
#3100=LINE('',#174668,#10167);
#3101=LINE('',#174669,#10168);
#3102=LINE('',#174671,#10169);
#3103=LINE('',#174672,#10170);
#3104=LINE('',#174674,#10171);
#3105=LINE('',#174676,#10172);
#3106=LINE('',#174678,#10173);
#3107=LINE('',#174680,#10174);
#3108=LINE('',#174703,#10175);
#3109=LINE('',#174707,#10176);
#3110=LINE('',#174711,#10177);
#3111=LINE('',#174715,#10178);
#3112=LINE('',#174719,#10179);
#3113=LINE('',#174723,#10180);
#3114=LINE('',#174727,#10181);
#3115=LINE('',#174745,#10182);
#3116=LINE('',#174769,#10183);
#3117=LINE('',#174847,#10184);
#3118=LINE('',#174927,#10185);
#3119=LINE('',#175093,#10186);
#3120=LINE('',#175123,#10187);
#3121=LINE('',#175188,#10188);
#3122=LINE('',#175253,#10189);
#3123=LINE('',#175334,#10190);
#3124=LINE('',#175494,#10191);
#3125=LINE('',#175659,#10192);
#3126=LINE('',#175816,#10193);
#3127=LINE('',#175831,#10194);
#3128=LINE('',#176150,#10195);
#3129=LINE('',#176290,#10196);
#3130=LINE('',#176332,#10197);
#3131=LINE('',#176342,#10198);
#3132=LINE('',#176343,#10199);
#3133=LINE('',#176345,#10200);
#3134=LINE('',#176346,#10201);
#3135=LINE('',#176348,#10202);
#3136=LINE('',#176350,#10203);
#3137=LINE('',#176352,#10204);
#3138=LINE('',#176354,#10205);
#3139=LINE('',#176356,#10206);
#3140=LINE('',#176358,#10207);
#3141=LINE('',#176359,#10208);
#3142=LINE('',#176362,#10209);
#3143=LINE('',#176772,#10210);
#3144=LINE('',#177269,#10211);
#3145=LINE('',#177883,#10212);
#3146=LINE('',#177887,#10213);
#3147=LINE('',#177891,#10214);
#3148=LINE('',#177895,#10215);
#3149=LINE('',#177899,#10216);
#3150=LINE('',#177903,#10217);
#3151=LINE('',#177907,#10218);
#3152=LINE('',#177925,#10219);
#3153=LINE('',#177954,#10220);
#3154=LINE('',#177961,#10221);
#3155=LINE('',#177964,#10222);
#3156=LINE('',#177977,#10223);
#3157=LINE('',#177982,#10224);
#3158=LINE('',#177991,#10225);
#3159=LINE('',#177999,#10226);
#3160=LINE('',#178079,#10227);
#3161=LINE('',#178155,#10228);
#3162=LINE('',#178321,#10229);
#3163=LINE('',#178351,#10230);
#3164=LINE('',#178420,#10231);
#3165=LINE('',#178487,#10232);
#3166=LINE('',#178570,#10233);
#3167=LINE('',#178736,#10234);
#3168=LINE('',#178905,#10235);
#3169=LINE('',#179064,#10236);
#3170=LINE('',#179079,#10237);
#3171=LINE('',#179394,#10238);
#3172=LINE('',#179534,#10239);
#3173=LINE('',#179576,#10240);
#3174=LINE('',#179586,#10241);
#3175=LINE('',#179587,#10242);
#3176=LINE('',#179589,#10243);
#3177=LINE('',#179590,#10244);
#3178=LINE('',#179592,#10245);
#3179=LINE('',#179594,#10246);
#3180=LINE('',#179596,#10247);
#3181=LINE('',#179598,#10248);
#3182=LINE('',#179600,#10249);
#3183=LINE('',#179602,#10250);
#3184=LINE('',#179603,#10251);
#3185=LINE('',#179606,#10252);
#3186=LINE('',#180016,#10253);
#3187=LINE('',#180513,#10254);
#3188=LINE('',#181115,#10255);
#3189=LINE('',#181121,#10256);
#3190=LINE('',#181126,#10257);
#3191=LINE('',#181319,#10258);
#3192=LINE('',#181683,#10259);
#3193=LINE('',#182045,#10260);
#3194=LINE('',#182068,#10261);
#3195=LINE('',#182209,#10262);
#3196=LINE('',#182592,#10263);
#3197=LINE('',#182596,#10264);
#3198=LINE('',#182600,#10265);
#3199=LINE('',#182604,#10266);
#3200=LINE('',#182608,#10267);
#3201=LINE('',#182631,#10268);
#3202=LINE('',#183011,#10269);
#3203=LINE('',#183017,#10270);
#3204=LINE('',#183027,#10271);
#3205=LINE('',#183032,#10272);
#3206=LINE('',#183043,#10273);
#3207=LINE('',#183054,#10274);
#3208=LINE('',#183187,#10275);
#3209=LINE('',#183448,#10276);
#3210=LINE('',#183456,#10277);
#3211=LINE('',#183463,#10278);
#3212=LINE('',#183470,#10279);
#3213=LINE('',#183488,#10280);
#3214=LINE('',#183498,#10281);
#3215=LINE('',#183504,#10282);
#3216=LINE('',#183729,#10283);
#3217=LINE('',#183742,#10284);
#3218=LINE('',#183744,#10285);
#3219=LINE('',#183747,#10286);
#3220=LINE('',#183766,#10287);
#3221=LINE('',#183773,#10288);
#3222=LINE('',#183776,#10289);
#3223=LINE('',#183789,#10290);
#3224=LINE('',#183794,#10291);
#3225=LINE('',#183803,#10292);
#3226=LINE('',#183811,#10293);
#3227=LINE('',#183825,#10294);
#3228=LINE('',#183967,#10295);
#3229=LINE('',#184165,#10296);
#3230=LINE('',#184353,#10297);
#3231=LINE('',#184386,#10298);
#3232=LINE('',#184406,#10299);
#3233=LINE('',#184429,#10300);
#3234=LINE('',#184449,#10301);
#3235=LINE('',#184452,#10302);
#3236=LINE('',#184478,#10303);
#3237=LINE('',#184612,#10304);
#3238=LINE('',#184613,#10305);
#3239=LINE('',#184616,#10306);
#3240=LINE('',#184636,#10307);
#3241=LINE('',#184641,#10308);
#3242=LINE('',#184667,#10309);
#3243=LINE('',#184748,#10310);
#3244=LINE('',#184754,#10311);
#3245=LINE('',#184769,#10312);
#3246=LINE('',#184774,#10313);
#3247=LINE('',#184780,#10314);
#3248=LINE('',#184786,#10315);
#3249=LINE('',#184793,#10316);
#3250=LINE('',#184797,#10317);
#3251=LINE('',#184801,#10318);
#3252=LINE('',#184805,#10319);
#3253=LINE('',#184809,#10320);
#3254=LINE('',#184912,#10321);
#3255=LINE('',#185512,#10322);
#3256=LINE('',#185590,#10323);
#3257=LINE('',#186590,#10324);
#3258=LINE('',#186595,#10325);
#3259=LINE('',#186609,#10326);
#3260=LINE('',#186610,#10327);
#3261=LINE('',#186903,#10328);
#3262=LINE('',#187082,#10329);
#3263=LINE('',#187084,#10330);
#3264=LINE('',#187085,#10331);
#3265=LINE('',#187088,#10332);
#3266=LINE('',#187092,#10333);
#3267=LINE('',#187099,#10334);
#3268=LINE('',#187104,#10335);
#3269=LINE('',#187112,#10336);
#3270=LINE('',#187114,#10337);
#3271=LINE('',#187115,#10338);
#3272=LINE('',#187121,#10339);
#3273=LINE('',#187123,#10340);
#3274=LINE('',#187129,#10341);
#3275=LINE('',#187134,#10342);
#3276=LINE('',#187140,#10343);
#3277=LINE('',#187144,#10344);
#3278=LINE('',#187149,#10345);
#3279=LINE('',#187150,#10346);
#3280=LINE('',#187155,#10347);
#3281=LINE('',#187156,#10348);
#3282=LINE('',#187161,#10349);
#3283=LINE('',#187168,#10350);
#3284=LINE('',#187172,#10351);
#3285=LINE('',#187177,#10352);
#3286=LINE('',#187183,#10353);
#3287=LINE('',#187192,#10354);
#3288=LINE('',#187196,#10355);
#3289=LINE('',#187201,#10356);
#3290=LINE('',#187207,#10357);
#3291=LINE('',#187216,#10358);
#3292=LINE('',#187220,#10359);
#3293=LINE('',#187225,#10360);
#3294=LINE('',#187231,#10361);
#3295=LINE('',#187240,#10362);
#3296=LINE('',#187244,#10363);
#3297=LINE('',#187249,#10364);
#3298=LINE('',#187255,#10365);
#3299=LINE('',#187266,#10366);
#3300=LINE('',#187268,#10367);
#3301=LINE('',#187269,#10368);
#3302=LINE('',#187275,#10369);
#3303=LINE('',#187277,#10370);
#3304=LINE('',#187283,#10371);
#3305=LINE('',#187288,#10372);
#3306=LINE('',#187294,#10373);
#3307=LINE('',#187298,#10374);
#3308=LINE('',#187303,#10375);
#3309=LINE('',#187305,#10376);
#3310=LINE('',#187311,#10377);
#3311=LINE('',#187312,#10378);
#3312=LINE('',#187317,#10379);
#3313=LINE('',#187324,#10380);
#3314=LINE('',#187328,#10381);
#3315=LINE('',#187333,#10382);
#3316=LINE('',#187335,#10383);
#3317=LINE('',#187341,#10384);
#3318=LINE('',#187342,#10385);
#3319=LINE('',#187347,#10386);
#3320=LINE('',#187354,#10387);
#3321=LINE('',#187358,#10388);
#3322=LINE('',#187363,#10389);
#3323=LINE('',#187369,#10390);
#3324=LINE('',#187371,#10391);
#3325=LINE('',#187377,#10392);
#3326=LINE('',#187384,#10393);
#3327=LINE('',#187388,#10394);
#3328=LINE('',#187393,#10395);
#3329=LINE('',#187399,#10396);
#3330=LINE('',#187408,#10397);
#3331=LINE('',#187412,#10398);
#3332=LINE('',#187417,#10399);
#3333=LINE('',#187419,#10400);
#3334=LINE('',#187425,#10401);
#3335=LINE('',#187426,#10402);
#3336=LINE('',#187431,#10403);
#3337=LINE('',#187438,#10404);
#3338=LINE('',#187442,#10405);
#3339=LINE('',#187447,#10406);
#3340=LINE('',#187449,#10407);
#3341=LINE('',#187455,#10408);
#3342=LINE('',#187456,#10409);
#3343=LINE('',#187461,#10410);
#3344=LINE('',#187468,#10411);
#3345=LINE('',#187472,#10412);
#3346=LINE('',#187477,#10413);
#3347=LINE('',#187479,#10414);
#3348=LINE('',#187485,#10415);
#3349=LINE('',#187486,#10416);
#3350=LINE('',#187491,#10417);
#3351=LINE('',#187498,#10418);
#3352=LINE('',#187502,#10419);
#3353=LINE('',#187507,#10420);
#3354=LINE('',#187509,#10421);
#3355=LINE('',#187515,#10422);
#3356=LINE('',#187516,#10423);
#3357=LINE('',#187521,#10424);
#3358=LINE('',#187528,#10425);
#3359=LINE('',#187532,#10426);
#3360=LINE('',#187537,#10427);
#3361=LINE('',#187543,#10428);
#3362=LINE('',#187552,#10429);
#3363=LINE('',#187556,#10430);
#3364=LINE('',#187561,#10431);
#3365=LINE('',#187567,#10432);
#3366=LINE('',#187576,#10433);
#3367=LINE('',#187580,#10434);
#3368=LINE('',#187585,#10435);
#3369=LINE('',#187591,#10436);
#3370=LINE('',#187600,#10437);
#3371=LINE('',#187604,#10438);
#3372=LINE('',#187609,#10439);
#3373=LINE('',#187615,#10440);
#3374=LINE('',#187624,#10441);
#3375=LINE('',#187628,#10442);
#3376=LINE('',#187633,#10443);
#3377=LINE('',#187639,#10444);
#3378=LINE('',#187648,#10445);
#3379=LINE('',#187652,#10446);
#3380=LINE('',#187657,#10447);
#3381=LINE('',#187663,#10448);
#3382=LINE('',#187674,#10449);
#3383=LINE('',#187677,#10450);
#3384=LINE('',#187682,#10451);
#3385=LINE('',#187687,#10452);
#3386=LINE('',#187691,#10453);
#3387=LINE('',#187696,#10454);
#3388=LINE('',#187702,#10455);
#3389=LINE('',#187706,#10456);
#3390=LINE('',#187711,#10457);
#3391=LINE('',#187713,#10458);
#3392=LINE('',#187719,#10459);
#3393=LINE('',#187720,#10460);
#3394=LINE('',#187725,#10461);
#3395=LINE('',#187732,#10462);
#3396=LINE('',#187736,#10463);
#3397=LINE('',#187741,#10464);
#3398=LINE('',#187747,#10465);
#3399=LINE('',#187756,#10466);
#3400=LINE('',#187760,#10467);
#3401=LINE('',#187765,#10468);
#3402=LINE('',#187771,#10469);
#3403=LINE('',#187780,#10470);
#3404=LINE('',#187784,#10471);
#3405=LINE('',#187789,#10472);
#3406=LINE('',#187795,#10473);
#3407=LINE('',#187804,#10474);
#3408=LINE('',#187808,#10475);
#3409=LINE('',#187813,#10476);
#3410=LINE('',#187819,#10477);
#3411=LINE('',#187828,#10478);
#3412=LINE('',#187832,#10479);
#3413=LINE('',#187837,#10480);
#3414=LINE('',#187843,#10481);
#3415=LINE('',#187852,#10482);
#3416=LINE('',#187856,#10483);
#3417=LINE('',#187861,#10484);
#3418=LINE('',#187867,#10485);
#3419=LINE('',#187876,#10486);
#3420=LINE('',#187880,#10487);
#3421=LINE('',#187885,#10488);
#3422=LINE('',#187891,#10489);
#3423=LINE('',#187900,#10490);
#3424=LINE('',#187904,#10491);
#3425=LINE('',#187909,#10492);
#3426=LINE('',#187915,#10493);
#3427=LINE('',#187924,#10494);
#3428=LINE('',#187928,#10495);
#3429=LINE('',#187933,#10496);
#3430=LINE('',#187935,#10497);
#3431=LINE('',#187941,#10498);
#3432=LINE('',#187942,#10499);
#3433=LINE('',#187947,#10500);
#3434=LINE('',#187954,#10501);
#3435=LINE('',#187958,#10502);
#3436=LINE('',#187963,#10503);
#3437=LINE('',#187965,#10504);
#3438=LINE('',#187971,#10505);
#3439=LINE('',#187972,#10506);
#3440=LINE('',#187977,#10507);
#3441=LINE('',#187984,#10508);
#3442=LINE('',#187988,#10509);
#3443=LINE('',#187993,#10510);
#3444=LINE('',#187999,#10511);
#3445=LINE('',#188008,#10512);
#3446=LINE('',#188012,#10513);
#3447=LINE('',#188017,#10514);
#3448=LINE('',#188023,#10515);
#3449=LINE('',#188032,#10516);
#3450=LINE('',#188036,#10517);
#3451=LINE('',#188041,#10518);
#3452=LINE('',#188047,#10519);
#3453=LINE('',#188056,#10520);
#3454=LINE('',#188060,#10521);
#3455=LINE('',#188065,#10522);
#3456=LINE('',#188071,#10523);
#3457=LINE('',#188080,#10524);
#3458=LINE('',#188084,#10525);
#3459=LINE('',#188089,#10526);
#3460=LINE('',#188095,#10527);
#3461=LINE('',#188104,#10528);
#3462=LINE('',#188108,#10529);
#3463=LINE('',#188113,#10530);
#3464=LINE('',#188119,#10531);
#3465=LINE('',#188128,#10532);
#3466=LINE('',#188132,#10533);
#3467=LINE('',#188137,#10534);
#3468=LINE('',#188143,#10535);
#3469=LINE('',#188152,#10536);
#3470=LINE('',#188156,#10537);
#3471=LINE('',#188161,#10538);
#3472=LINE('',#188167,#10539);
#3473=LINE('',#188176,#10540);
#3474=LINE('',#188180,#10541);
#3475=LINE('',#188185,#10542);
#3476=LINE('',#188191,#10543);
#3477=LINE('',#188200,#10544);
#3478=LINE('',#188204,#10545);
#3479=LINE('',#188209,#10546);
#3480=LINE('',#188215,#10547);
#3481=LINE('',#188224,#10548);
#3482=LINE('',#188226,#10549);
#3483=LINE('',#188231,#10550);
#3484=LINE('',#188235,#10551);
#3485=LINE('',#188240,#10552);
#3486=LINE('',#188245,#10553);
#3487=LINE('',#188254,#10554);
#3488=LINE('',#188258,#10555);
#3489=LINE('',#188263,#10556);
#3490=LINE('',#188269,#10557);
#3491=LINE('',#188278,#10558);
#3492=LINE('',#188282,#10559);
#3493=LINE('',#188287,#10560);
#3494=LINE('',#188293,#10561);
#3495=LINE('',#188302,#10562);
#3496=LINE('',#188306,#10563);
#3497=LINE('',#188311,#10564);
#3498=LINE('',#188317,#10565);
#3499=LINE('',#188326,#10566);
#3500=LINE('',#188330,#10567);
#3501=LINE('',#188335,#10568);
#3502=LINE('',#188341,#10569);
#3503=LINE('',#188350,#10570);
#3504=LINE('',#188354,#10571);
#3505=LINE('',#188359,#10572);
#3506=LINE('',#188365,#10573);
#3507=LINE('',#188374,#10574);
#3508=LINE('',#188378,#10575);
#3509=LINE('',#188383,#10576);
#3510=LINE('',#188389,#10577);
#3511=LINE('',#188398,#10578);
#3512=LINE('',#188402,#10579);
#3513=LINE('',#188407,#10580);
#3514=LINE('',#188413,#10581);
#3515=LINE('',#188422,#10582);
#3516=LINE('',#188426,#10583);
#3517=LINE('',#188431,#10584);
#3518=LINE('',#188437,#10585);
#3519=LINE('',#188446,#10586);
#3520=LINE('',#188450,#10587);
#3521=LINE('',#188455,#10588);
#3522=LINE('',#188461,#10589);
#3523=LINE('',#188470,#10590);
#3524=LINE('',#188474,#10591);
#3525=LINE('',#188479,#10592);
#3526=LINE('',#188485,#10593);
#3527=LINE('',#188494,#10594);
#3528=LINE('',#188498,#10595);
#3529=LINE('',#188503,#10596);
#3530=LINE('',#188509,#10597);
#3531=LINE('',#188511,#10598);
#3532=LINE('',#188517,#10599);
#3533=LINE('',#188524,#10600);
#3534=LINE('',#188528,#10601);
#3535=LINE('',#188533,#10602);
#3536=LINE('',#188539,#10603);
#3537=LINE('',#188541,#10604);
#3538=LINE('',#188547,#10605);
#3539=LINE('',#188554,#10606);
#3540=LINE('',#188558,#10607);
#3541=LINE('',#188563,#10608);
#3542=LINE('',#188569,#10609);
#3543=LINE('',#188578,#10610);
#3544=LINE('',#188582,#10611);
#3545=LINE('',#188587,#10612);
#3546=LINE('',#188593,#10613);
#3547=LINE('',#188602,#10614);
#3548=LINE('',#188606,#10615);
#3549=LINE('',#188611,#10616);
#3550=LINE('',#188617,#10617);
#3551=LINE('',#188626,#10618);
#3552=LINE('',#188630,#10619);
#3553=LINE('',#188635,#10620);
#3554=LINE('',#188641,#10621);
#3555=LINE('',#188650,#10622);
#3556=LINE('',#188654,#10623);
#3557=LINE('',#188659,#10624);
#3558=LINE('',#188665,#10625);
#3559=LINE('',#188674,#10626);
#3560=LINE('',#188678,#10627);
#3561=LINE('',#188683,#10628);
#3562=LINE('',#188689,#10629);
#3563=LINE('',#188698,#10630);
#3564=LINE('',#188702,#10631);
#3565=LINE('',#188707,#10632);
#3566=LINE('',#188713,#10633);
#3567=LINE('',#188722,#10634);
#3568=LINE('',#188726,#10635);
#3569=LINE('',#188731,#10636);
#3570=LINE('',#188737,#10637);
#3571=LINE('',#188746,#10638);
#3572=LINE('',#188750,#10639);
#3573=LINE('',#188755,#10640);
#3574=LINE('',#188761,#10641);
#3575=LINE('',#188770,#10642);
#3576=LINE('',#188774,#10643);
#3577=LINE('',#188779,#10644);
#3578=LINE('',#188785,#10645);
#3579=LINE('',#188794,#10646);
#3580=LINE('',#188798,#10647);
#3581=LINE('',#188803,#10648);
#3582=LINE('',#188809,#10649);
#3583=LINE('',#188818,#10650);
#3584=LINE('',#188822,#10651);
#3585=LINE('',#188827,#10652);
#3586=LINE('',#188833,#10653);
#3587=LINE('',#188842,#10654);
#3588=LINE('',#188846,#10655);
#3589=LINE('',#188851,#10656);
#3590=LINE('',#188857,#10657);
#3591=LINE('',#188866,#10658);
#3592=LINE('',#188870,#10659);
#3593=LINE('',#188875,#10660);
#3594=LINE('',#188881,#10661);
#3595=LINE('',#188890,#10662);
#3596=LINE('',#188894,#10663);
#3597=LINE('',#188899,#10664);
#3598=LINE('',#188905,#10665);
#3599=LINE('',#188914,#10666);
#3600=LINE('',#188918,#10667);
#3601=LINE('',#188923,#10668);
#3602=LINE('',#188929,#10669);
#3603=LINE('',#188938,#10670);
#3604=LINE('',#188942,#10671);
#3605=LINE('',#188947,#10672);
#3606=LINE('',#188953,#10673);
#3607=LINE('',#188962,#10674);
#3608=LINE('',#188966,#10675);
#3609=LINE('',#188971,#10676);
#3610=LINE('',#188977,#10677);
#3611=LINE('',#188986,#10678);
#3612=LINE('',#188990,#10679);
#3613=LINE('',#188995,#10680);
#3614=LINE('',#189001,#10681);
#3615=LINE('',#189010,#10682);
#3616=LINE('',#189014,#10683);
#3617=LINE('',#189019,#10684);
#3618=LINE('',#189025,#10685);
#3619=LINE('',#189034,#10686);
#3620=LINE('',#189038,#10687);
#3621=LINE('',#189043,#10688);
#3622=LINE('',#189049,#10689);
#3623=LINE('',#189058,#10690);
#3624=LINE('',#189062,#10691);
#3625=LINE('',#189067,#10692);
#3626=LINE('',#189073,#10693);
#3627=LINE('',#189082,#10694);
#3628=LINE('',#189086,#10695);
#3629=LINE('',#189091,#10696);
#3630=LINE('',#189097,#10697);
#3631=LINE('',#189106,#10698);
#3632=LINE('',#189110,#10699);
#3633=LINE('',#189115,#10700);
#3634=LINE('',#189121,#10701);
#3635=LINE('',#189130,#10702);
#3636=LINE('',#189134,#10703);
#3637=LINE('',#189139,#10704);
#3638=LINE('',#189145,#10705);
#3639=LINE('',#189154,#10706);
#3640=LINE('',#189158,#10707);
#3641=LINE('',#189163,#10708);
#3642=LINE('',#189169,#10709);
#3643=LINE('',#189178,#10710);
#3644=LINE('',#189182,#10711);
#3645=LINE('',#189187,#10712);
#3646=LINE('',#189193,#10713);
#3647=LINE('',#189202,#10714);
#3648=LINE('',#189206,#10715);
#3649=LINE('',#189211,#10716);
#3650=LINE('',#189217,#10717);
#3651=LINE('',#189226,#10718);
#3652=LINE('',#189230,#10719);
#3653=LINE('',#189235,#10720);
#3654=LINE('',#189241,#10721);
#3655=LINE('',#189250,#10722);
#3656=LINE('',#189254,#10723);
#3657=LINE('',#189259,#10724);
#3658=LINE('',#189265,#10725);
#3659=LINE('',#189274,#10726);
#3660=LINE('',#189278,#10727);
#3661=LINE('',#189283,#10728);
#3662=LINE('',#189289,#10729);
#3663=LINE('',#189298,#10730);
#3664=LINE('',#189302,#10731);
#3665=LINE('',#189307,#10732);
#3666=LINE('',#189313,#10733);
#3667=LINE('',#189322,#10734);
#3668=LINE('',#189326,#10735);
#3669=LINE('',#189331,#10736);
#3670=LINE('',#189337,#10737);
#3671=LINE('',#189346,#10738);
#3672=LINE('',#189350,#10739);
#3673=LINE('',#189355,#10740);
#3674=LINE('',#189361,#10741);
#3675=LINE('',#189370,#10742);
#3676=LINE('',#189374,#10743);
#3677=LINE('',#189379,#10744);
#3678=LINE('',#189385,#10745);
#3679=LINE('',#189394,#10746);
#3680=LINE('',#189398,#10747);
#3681=LINE('',#189403,#10748);
#3682=LINE('',#189409,#10749);
#3683=LINE('',#189418,#10750);
#3684=LINE('',#189422,#10751);
#3685=LINE('',#189427,#10752);
#3686=LINE('',#189433,#10753);
#3687=LINE('',#189442,#10754);
#3688=LINE('',#189446,#10755);
#3689=LINE('',#189451,#10756);
#3690=LINE('',#189457,#10757);
#3691=LINE('',#189466,#10758);
#3692=LINE('',#189470,#10759);
#3693=LINE('',#189475,#10760);
#3694=LINE('',#189481,#10761);
#3695=LINE('',#189490,#10762);
#3696=LINE('',#189494,#10763);
#3697=LINE('',#189499,#10764);
#3698=LINE('',#189505,#10765);
#3699=LINE('',#189514,#10766);
#3700=LINE('',#189518,#10767);
#3701=LINE('',#189523,#10768);
#3702=LINE('',#189529,#10769);
#3703=LINE('',#189538,#10770);
#3704=LINE('',#189542,#10771);
#3705=LINE('',#189547,#10772);
#3706=LINE('',#189553,#10773);
#3707=LINE('',#189562,#10774);
#3708=LINE('',#189566,#10775);
#3709=LINE('',#189571,#10776);
#3710=LINE('',#189577,#10777);
#3711=LINE('',#189586,#10778);
#3712=LINE('',#189590,#10779);
#3713=LINE('',#189595,#10780);
#3714=LINE('',#189601,#10781);
#3715=LINE('',#189610,#10782);
#3716=LINE('',#189614,#10783);
#3717=LINE('',#189619,#10784);
#3718=LINE('',#189625,#10785);
#3719=LINE('',#189634,#10786);
#3720=LINE('',#189638,#10787);
#3721=LINE('',#189643,#10788);
#3722=LINE('',#189649,#10789);
#3723=LINE('',#189658,#10790);
#3724=LINE('',#189662,#10791);
#3725=LINE('',#189667,#10792);
#3726=LINE('',#189673,#10793);
#3727=LINE('',#189682,#10794);
#3728=LINE('',#189686,#10795);
#3729=LINE('',#189691,#10796);
#3730=LINE('',#189697,#10797);
#3731=LINE('',#189706,#10798);
#3732=LINE('',#189710,#10799);
#3733=LINE('',#189715,#10800);
#3734=LINE('',#189721,#10801);
#3735=LINE('',#189730,#10802);
#3736=LINE('',#189734,#10803);
#3737=LINE('',#189739,#10804);
#3738=LINE('',#189745,#10805);
#3739=LINE('',#189754,#10806);
#3740=LINE('',#189758,#10807);
#3741=LINE('',#189763,#10808);
#3742=LINE('',#189769,#10809);
#3743=LINE('',#189778,#10810);
#3744=LINE('',#189782,#10811);
#3745=LINE('',#189787,#10812);
#3746=LINE('',#189793,#10813);
#3747=LINE('',#189802,#10814);
#3748=LINE('',#189806,#10815);
#3749=LINE('',#189811,#10816);
#3750=LINE('',#189817,#10817);
#3751=LINE('',#189826,#10818);
#3752=LINE('',#189830,#10819);
#3753=LINE('',#189835,#10820);
#3754=LINE('',#189841,#10821);
#3755=LINE('',#189850,#10822);
#3756=LINE('',#189854,#10823);
#3757=LINE('',#189859,#10824);
#3758=LINE('',#189865,#10825);
#3759=LINE('',#189874,#10826);
#3760=LINE('',#189878,#10827);
#3761=LINE('',#189883,#10828);
#3762=LINE('',#189889,#10829);
#3763=LINE('',#189898,#10830);
#3764=LINE('',#189902,#10831);
#3765=LINE('',#189907,#10832);
#3766=LINE('',#189913,#10833);
#3767=LINE('',#189922,#10834);
#3768=LINE('',#189926,#10835);
#3769=LINE('',#189931,#10836);
#3770=LINE('',#189937,#10837);
#3771=LINE('',#189946,#10838);
#3772=LINE('',#189950,#10839);
#3773=LINE('',#189955,#10840);
#3774=LINE('',#189961,#10841);
#3775=LINE('',#189970,#10842);
#3776=LINE('',#189974,#10843);
#3777=LINE('',#189979,#10844);
#3778=LINE('',#189985,#10845);
#3779=LINE('',#189994,#10846);
#3780=LINE('',#189998,#10847);
#3781=LINE('',#190003,#10848);
#3782=LINE('',#190009,#10849);
#3783=LINE('',#190018,#10850);
#3784=LINE('',#190022,#10851);
#3785=LINE('',#190027,#10852);
#3786=LINE('',#190033,#10853);
#3787=LINE('',#190042,#10854);
#3788=LINE('',#190046,#10855);
#3789=LINE('',#190051,#10856);
#3790=LINE('',#190057,#10857);
#3791=LINE('',#190066,#10858);
#3792=LINE('',#190070,#10859);
#3793=LINE('',#190075,#10860);
#3794=LINE('',#190081,#10861);
#3795=LINE('',#190090,#10862);
#3796=LINE('',#190094,#10863);
#3797=LINE('',#190099,#10864);
#3798=LINE('',#190105,#10865);
#3799=LINE('',#190114,#10866);
#3800=LINE('',#190118,#10867);
#3801=LINE('',#190123,#10868);
#3802=LINE('',#190129,#10869);
#3803=LINE('',#190138,#10870);
#3804=LINE('',#190142,#10871);
#3805=LINE('',#190147,#10872);
#3806=LINE('',#190153,#10873);
#3807=LINE('',#190162,#10874);
#3808=LINE('',#190166,#10875);
#3809=LINE('',#190171,#10876);
#3810=LINE('',#190177,#10877);
#3811=LINE('',#190186,#10878);
#3812=LINE('',#190190,#10879);
#3813=LINE('',#190195,#10880);
#3814=LINE('',#190201,#10881);
#3815=LINE('',#190210,#10882);
#3816=LINE('',#190214,#10883);
#3817=LINE('',#190219,#10884);
#3818=LINE('',#190225,#10885);
#3819=LINE('',#190234,#10886);
#3820=LINE('',#190238,#10887);
#3821=LINE('',#190243,#10888);
#3822=LINE('',#190245,#10889);
#3823=LINE('',#190251,#10890);
#3824=LINE('',#190252,#10891);
#3825=LINE('',#190255,#10892);
#3826=LINE('',#190262,#10893);
#3827=LINE('',#190266,#10894);
#3828=LINE('',#190271,#10895);
#3829=LINE('',#190273,#10896);
#3830=LINE('',#190279,#10897);
#3831=LINE('',#190280,#10898);
#3832=LINE('',#190285,#10899);
#3833=LINE('',#190292,#10900);
#3834=LINE('',#190296,#10901);
#3835=LINE('',#190301,#10902);
#3836=LINE('',#190303,#10903);
#3837=LINE('',#190309,#10904);
#3838=LINE('',#190310,#10905);
#3839=LINE('',#190315,#10906);
#3840=LINE('',#190322,#10907);
#3841=LINE('',#190326,#10908);
#3842=LINE('',#190331,#10909);
#3843=LINE('',#190333,#10910);
#3844=LINE('',#190339,#10911);
#3845=LINE('',#190340,#10912);
#3846=LINE('',#190345,#10913);
#3847=LINE('',#190352,#10914);
#3848=LINE('',#190356,#10915);
#3849=LINE('',#190361,#10916);
#3850=LINE('',#190363,#10917);
#3851=LINE('',#190369,#10918);
#3852=LINE('',#190370,#10919);
#3853=LINE('',#190375,#10920);
#3854=LINE('',#190382,#10921);
#3855=LINE('',#190384,#10922);
#3856=LINE('',#190388,#10923);
#3857=LINE('',#190393,#10924);
#3858=LINE('',#190394,#10925);
#3859=LINE('',#190399,#10926);
#3860=LINE('',#190400,#10927);
#3861=LINE('',#190405,#10928);
#3862=LINE('',#190412,#10929);
#3863=LINE('',#190414,#10930);
#3864=LINE('',#190418,#10931);
#3865=LINE('',#190423,#10932);
#3866=LINE('',#190424,#10933);
#3867=LINE('',#190429,#10934);
#3868=LINE('',#190430,#10935);
#3869=LINE('',#190435,#10936);
#3870=LINE('',#190442,#10937);
#3871=LINE('',#190446,#10938);
#3872=LINE('',#190451,#10939);
#3873=LINE('',#190453,#10940);
#3874=LINE('',#190459,#10941);
#3875=LINE('',#190460,#10942);
#3876=LINE('',#190465,#10943);
#3877=LINE('',#190472,#10944);
#3878=LINE('',#190476,#10945);
#3879=LINE('',#190481,#10946);
#3880=LINE('',#190483,#10947);
#3881=LINE('',#190489,#10948);
#3882=LINE('',#190490,#10949);
#3883=LINE('',#190495,#10950);
#3884=LINE('',#190502,#10951);
#3885=LINE('',#190506,#10952);
#3886=LINE('',#190511,#10953);
#3887=LINE('',#190513,#10954);
#3888=LINE('',#190519,#10955);
#3889=LINE('',#190520,#10956);
#3890=LINE('',#190525,#10957);
#3891=LINE('',#190532,#10958);
#3892=LINE('',#190536,#10959);
#3893=LINE('',#190541,#10960);
#3894=LINE('',#190547,#10961);
#3895=LINE('',#190556,#10962);
#3896=LINE('',#190560,#10963);
#3897=LINE('',#190565,#10964);
#3898=LINE('',#190571,#10965);
#3899=LINE('',#190580,#10966);
#3900=LINE('',#190584,#10967);
#3901=LINE('',#190589,#10968);
#3902=LINE('',#190595,#10969);
#3903=LINE('',#190604,#10970);
#3904=LINE('',#190608,#10971);
#3905=LINE('',#190613,#10972);
#3906=LINE('',#190619,#10973);
#3907=LINE('',#190628,#10974);
#3908=LINE('',#190632,#10975);
#3909=LINE('',#190637,#10976);
#3910=LINE('',#190643,#10977);
#3911=LINE('',#190652,#10978);
#3912=LINE('',#190656,#10979);
#3913=LINE('',#190661,#10980);
#3914=LINE('',#190667,#10981);
#3915=LINE('',#190676,#10982);
#3916=LINE('',#190680,#10983);
#3917=LINE('',#190685,#10984);
#3918=LINE('',#190691,#10985);
#3919=LINE('',#190700,#10986);
#3920=LINE('',#190704,#10987);
#3921=LINE('',#190709,#10988);
#3922=LINE('',#190715,#10989);
#3923=LINE('',#190724,#10990);
#3924=LINE('',#190726,#10991);
#3925=LINE('',#190730,#10992);
#3926=LINE('',#190735,#10993);
#3927=LINE('',#190736,#10994);
#3928=LINE('',#190741,#10995);
#3929=LINE('',#190742,#10996);
#3930=LINE('',#190747,#10997);
#3931=LINE('',#190754,#10998);
#3932=LINE('',#190756,#10999);
#3933=LINE('',#190760,#11000);
#3934=LINE('',#190765,#11001);
#3935=LINE('',#190766,#11002);
#3936=LINE('',#190771,#11003);
#3937=LINE('',#190772,#11004);
#3938=LINE('',#190777,#11005);
#3939=LINE('',#190784,#11006);
#3940=LINE('',#190788,#11007);
#3941=LINE('',#190793,#11008);
#3942=LINE('',#190799,#11009);
#3943=LINE('',#190808,#11010);
#3944=LINE('',#190812,#11011);
#3945=LINE('',#190817,#11012);
#3946=LINE('',#190823,#11013);
#3947=LINE('',#190832,#11014);
#3948=LINE('',#190836,#11015);
#3949=LINE('',#190841,#11016);
#3950=LINE('',#190847,#11017);
#3951=LINE('',#190856,#11018);
#3952=LINE('',#190860,#11019);
#3953=LINE('',#190865,#11020);
#3954=LINE('',#190871,#11021);
#3955=LINE('',#190880,#11022);
#3956=LINE('',#190884,#11023);
#3957=LINE('',#190889,#11024);
#3958=LINE('',#190895,#11025);
#3959=LINE('',#190897,#11026);
#3960=LINE('',#190903,#11027);
#3961=LINE('',#190910,#11028);
#3962=LINE('',#190914,#11029);
#3963=LINE('',#190919,#11030);
#3964=LINE('',#190921,#11031);
#3965=LINE('',#190927,#11032);
#3966=LINE('',#190928,#11033);
#3967=LINE('',#190933,#11034);
#3968=LINE('',#190940,#11035);
#3969=LINE('',#190944,#11036);
#3970=LINE('',#190949,#11037);
#3971=LINE('',#190951,#11038);
#3972=LINE('',#190957,#11039);
#3973=LINE('',#190958,#11040);
#3974=LINE('',#190963,#11041);
#3975=LINE('',#190970,#11042);
#3976=LINE('',#190974,#11043);
#3977=LINE('',#190979,#11044);
#3978=LINE('',#190985,#11045);
#3979=LINE('',#190987,#11046);
#3980=LINE('',#190993,#11047);
#3981=LINE('',#191000,#11048);
#3982=LINE('',#191004,#11049);
#3983=LINE('',#191009,#11050);
#3984=LINE('',#191015,#11051);
#3985=LINE('',#191024,#11052);
#3986=LINE('',#191028,#11053);
#3987=LINE('',#191033,#11054);
#3988=LINE('',#191039,#11055);
#3989=LINE('',#191048,#11056);
#3990=LINE('',#191052,#11057);
#3991=LINE('',#191057,#11058);
#3992=LINE('',#191063,#11059);
#3993=LINE('',#191072,#11060);
#3994=LINE('',#191076,#11061);
#3995=LINE('',#191081,#11062);
#3996=LINE('',#191087,#11063);
#3997=LINE('',#191096,#11064);
#3998=LINE('',#191100,#11065);
#3999=LINE('',#191105,#11066);
#4000=LINE('',#191111,#11067);
#4001=LINE('',#191120,#11068);
#4002=LINE('',#191124,#11069);
#4003=LINE('',#191129,#11070);
#4004=LINE('',#191135,#11071);
#4005=LINE('',#191144,#11072);
#4006=LINE('',#191148,#11073);
#4007=LINE('',#191153,#11074);
#4008=LINE('',#191159,#11075);
#4009=LINE('',#191168,#11076);
#4010=LINE('',#191172,#11077);
#4011=LINE('',#191177,#11078);
#4012=LINE('',#191183,#11079);
#4013=LINE('',#191192,#11080);
#4014=LINE('',#191196,#11081);
#4015=LINE('',#191201,#11082);
#4016=LINE('',#191207,#11083);
#4017=LINE('',#191216,#11084);
#4018=LINE('',#191220,#11085);
#4019=LINE('',#191225,#11086);
#4020=LINE('',#191231,#11087);
#4021=LINE('',#191240,#11088);
#4022=LINE('',#191244,#11089);
#4023=LINE('',#191249,#11090);
#4024=LINE('',#191255,#11091);
#4025=LINE('',#191257,#11092);
#4026=LINE('',#191263,#11093);
#4027=LINE('',#191270,#11094);
#4028=LINE('',#191274,#11095);
#4029=LINE('',#191279,#11096);
#4030=LINE('',#191285,#11097);
#4031=LINE('',#191287,#11098);
#4032=LINE('',#191293,#11099);
#4033=LINE('',#191300,#11100);
#4034=LINE('',#191304,#11101);
#4035=LINE('',#191309,#11102);
#4036=LINE('',#191315,#11103);
#4037=LINE('',#191324,#11104);
#4038=LINE('',#191328,#11105);
#4039=LINE('',#191333,#11106);
#4040=LINE('',#191339,#11107);
#4041=LINE('',#191348,#11108);
#4042=LINE('',#191352,#11109);
#4043=LINE('',#191357,#11110);
#4044=LINE('',#191363,#11111);
#4045=LINE('',#191372,#11112);
#4046=LINE('',#191376,#11113);
#4047=LINE('',#191381,#11114);
#4048=LINE('',#191387,#11115);
#4049=LINE('',#191396,#11116);
#4050=LINE('',#191400,#11117);
#4051=LINE('',#191405,#11118);
#4052=LINE('',#191411,#11119);
#4053=LINE('',#191420,#11120);
#4054=LINE('',#191424,#11121);
#4055=LINE('',#191429,#11122);
#4056=LINE('',#191435,#11123);
#4057=LINE('',#191444,#11124);
#4058=LINE('',#191448,#11125);
#4059=LINE('',#191453,#11126);
#4060=LINE('',#191459,#11127);
#4061=LINE('',#191468,#11128);
#4062=LINE('',#191472,#11129);
#4063=LINE('',#191477,#11130);
#4064=LINE('',#191483,#11131);
#4065=LINE('',#191492,#11132);
#4066=LINE('',#191496,#11133);
#4067=LINE('',#191501,#11134);
#4068=LINE('',#191507,#11135);
#4069=LINE('',#191516,#11136);
#4070=LINE('',#191520,#11137);
#4071=LINE('',#191525,#11138);
#4072=LINE('',#191527,#11139);
#4073=LINE('',#191533,#11140);
#4074=LINE('',#191534,#11141);
#4075=LINE('',#191539,#11142);
#4076=LINE('',#191546,#11143);
#4077=LINE('',#191550,#11144);
#4078=LINE('',#191555,#11145);
#4079=LINE('',#191561,#11146);
#4080=LINE('',#191563,#11147);
#4081=LINE('',#191569,#11148);
#4082=LINE('',#191576,#11149);
#4083=LINE('',#191580,#11150);
#4084=LINE('',#191585,#11151);
#4085=LINE('',#191591,#11152);
#4086=LINE('',#191600,#11153);
#4087=LINE('',#191604,#11154);
#4088=LINE('',#191609,#11155);
#4089=LINE('',#191615,#11156);
#4090=LINE('',#191624,#11157);
#4091=LINE('',#191628,#11158);
#4092=LINE('',#191633,#11159);
#4093=LINE('',#191639,#11160);
#4094=LINE('',#191648,#11161);
#4095=LINE('',#191652,#11162);
#4096=LINE('',#191657,#11163);
#4097=LINE('',#191663,#11164);
#4098=LINE('',#191672,#11165);
#4099=LINE('',#191676,#11166);
#4100=LINE('',#191681,#11167);
#4101=LINE('',#191687,#11168);
#4102=LINE('',#191696,#11169);
#4103=LINE('',#191700,#11170);
#4104=LINE('',#191705,#11171);
#4105=LINE('',#191711,#11172);
#4106=LINE('',#191720,#11173);
#4107=LINE('',#191724,#11174);
#4108=LINE('',#191729,#11175);
#4109=LINE('',#191735,#11176);
#4110=LINE('',#191744,#11177);
#4111=LINE('',#191748,#11178);
#4112=LINE('',#191753,#11179);
#4113=LINE('',#191759,#11180);
#4114=LINE('',#191768,#11181);
#4115=LINE('',#191772,#11182);
#4116=LINE('',#191777,#11183);
#4117=LINE('',#191783,#11184);
#4118=LINE('',#191792,#11185);
#4119=LINE('',#191796,#11186);
#4120=LINE('',#191801,#11187);
#4121=LINE('',#191807,#11188);
#4122=LINE('',#191816,#11189);
#4123=LINE('',#191820,#11190);
#4124=LINE('',#191825,#11191);
#4125=LINE('',#191831,#11192);
#4126=LINE('',#191840,#11193);
#4127=LINE('',#191844,#11194);
#4128=LINE('',#191849,#11195);
#4129=LINE('',#191855,#11196);
#4130=LINE('',#191864,#11197);
#4131=LINE('',#191868,#11198);
#4132=LINE('',#191873,#11199);
#4133=LINE('',#191879,#11200);
#4134=LINE('',#191888,#11201);
#4135=LINE('',#191892,#11202);
#4136=LINE('',#191897,#11203);
#4137=LINE('',#191903,#11204);
#4138=LINE('',#191912,#11205);
#4139=LINE('',#191916,#11206);
#4140=LINE('',#191921,#11207);
#4141=LINE('',#191927,#11208);
#4142=LINE('',#191936,#11209);
#4143=LINE('',#191940,#11210);
#4144=LINE('',#191945,#11211);
#4145=LINE('',#191951,#11212);
#4146=LINE('',#191960,#11213);
#4147=LINE('',#191964,#11214);
#4148=LINE('',#191969,#11215);
#4149=LINE('',#191975,#11216);
#4150=LINE('',#191984,#11217);
#4151=LINE('',#191988,#11218);
#4152=LINE('',#191993,#11219);
#4153=LINE('',#191999,#11220);
#4154=LINE('',#192008,#11221);
#4155=LINE('',#192012,#11222);
#4156=LINE('',#192017,#11223);
#4157=LINE('',#192023,#11224);
#4158=LINE('',#192032,#11225);
#4159=LINE('',#192036,#11226);
#4160=LINE('',#192041,#11227);
#4161=LINE('',#192047,#11228);
#4162=LINE('',#192056,#11229);
#4163=LINE('',#192060,#11230);
#4164=LINE('',#192065,#11231);
#4165=LINE('',#192071,#11232);
#4166=LINE('',#192080,#11233);
#4167=LINE('',#192084,#11234);
#4168=LINE('',#192089,#11235);
#4169=LINE('',#192095,#11236);
#4170=LINE('',#192104,#11237);
#4171=LINE('',#192108,#11238);
#4172=LINE('',#192113,#11239);
#4173=LINE('',#192119,#11240);
#4174=LINE('',#192128,#11241);
#4175=LINE('',#192132,#11242);
#4176=LINE('',#192137,#11243);
#4177=LINE('',#192143,#11244);
#4178=LINE('',#192152,#11245);
#4179=LINE('',#192156,#11246);
#4180=LINE('',#192161,#11247);
#4181=LINE('',#192167,#11248);
#4182=LINE('',#192176,#11249);
#4183=LINE('',#192180,#11250);
#4184=LINE('',#192185,#11251);
#4185=LINE('',#192191,#11252);
#4186=LINE('',#192200,#11253);
#4187=LINE('',#192204,#11254);
#4188=LINE('',#192209,#11255);
#4189=LINE('',#192215,#11256);
#4190=LINE('',#192224,#11257);
#4191=LINE('',#192228,#11258);
#4192=LINE('',#192233,#11259);
#4193=LINE('',#192239,#11260);
#4194=LINE('',#192248,#11261);
#4195=LINE('',#192252,#11262);
#4196=LINE('',#192257,#11263);
#4197=LINE('',#192263,#11264);
#4198=LINE('',#192272,#11265);
#4199=LINE('',#192276,#11266);
#4200=LINE('',#192281,#11267);
#4201=LINE('',#192287,#11268);
#4202=LINE('',#192296,#11269);
#4203=LINE('',#192300,#11270);
#4204=LINE('',#192305,#11271);
#4205=LINE('',#192311,#11272);
#4206=LINE('',#192320,#11273);
#4207=LINE('',#192324,#11274);
#4208=LINE('',#192329,#11275);
#4209=LINE('',#192335,#11276);
#4210=LINE('',#192344,#11277);
#4211=LINE('',#192348,#11278);
#4212=LINE('',#192353,#11279);
#4213=LINE('',#192359,#11280);
#4214=LINE('',#192368,#11281);
#4215=LINE('',#192372,#11282);
#4216=LINE('',#192377,#11283);
#4217=LINE('',#192383,#11284);
#4218=LINE('',#192392,#11285);
#4219=LINE('',#192396,#11286);
#4220=LINE('',#192401,#11287);
#4221=LINE('',#192407,#11288);
#4222=LINE('',#192416,#11289);
#4223=LINE('',#192420,#11290);
#4224=LINE('',#192425,#11291);
#4225=LINE('',#192431,#11292);
#4226=LINE('',#192440,#11293);
#4227=LINE('',#192444,#11294);
#4228=LINE('',#192449,#11295);
#4229=LINE('',#192455,#11296);
#4230=LINE('',#192464,#11297);
#4231=LINE('',#192468,#11298);
#4232=LINE('',#192473,#11299);
#4233=LINE('',#192479,#11300);
#4234=LINE('',#192488,#11301);
#4235=LINE('',#192492,#11302);
#4236=LINE('',#192497,#11303);
#4237=LINE('',#192503,#11304);
#4238=LINE('',#192512,#11305);
#4239=LINE('',#192516,#11306);
#4240=LINE('',#192521,#11307);
#4241=LINE('',#192527,#11308);
#4242=LINE('',#192536,#11309);
#4243=LINE('',#192540,#11310);
#4244=LINE('',#192545,#11311);
#4245=LINE('',#192551,#11312);
#4246=LINE('',#192560,#11313);
#4247=LINE('',#192564,#11314);
#4248=LINE('',#192569,#11315);
#4249=LINE('',#192575,#11316);
#4250=LINE('',#192584,#11317);
#4251=LINE('',#192588,#11318);
#4252=LINE('',#192593,#11319);
#4253=LINE('',#192599,#11320);
#4254=LINE('',#192608,#11321);
#4255=LINE('',#192612,#11322);
#4256=LINE('',#192617,#11323);
#4257=LINE('',#192623,#11324);
#4258=LINE('',#192632,#11325);
#4259=LINE('',#192636,#11326);
#4260=LINE('',#192641,#11327);
#4261=LINE('',#192647,#11328);
#4262=LINE('',#192656,#11329);
#4263=LINE('',#192660,#11330);
#4264=LINE('',#192665,#11331);
#4265=LINE('',#192671,#11332);
#4266=LINE('',#192680,#11333);
#4267=LINE('',#192684,#11334);
#4268=LINE('',#192689,#11335);
#4269=LINE('',#192695,#11336);
#4270=LINE('',#192704,#11337);
#4271=LINE('',#192708,#11338);
#4272=LINE('',#192713,#11339);
#4273=LINE('',#192719,#11340);
#4274=LINE('',#192728,#11341);
#4275=LINE('',#192732,#11342);
#4276=LINE('',#192737,#11343);
#4277=LINE('',#192743,#11344);
#4278=LINE('',#192752,#11345);
#4279=LINE('',#192756,#11346);
#4280=LINE('',#192761,#11347);
#4281=LINE('',#192767,#11348);
#4282=LINE('',#192776,#11349);
#4283=LINE('',#192780,#11350);
#4284=LINE('',#192785,#11351);
#4285=LINE('',#192791,#11352);
#4286=LINE('',#192800,#11353);
#4287=LINE('',#192804,#11354);
#4288=LINE('',#192809,#11355);
#4289=LINE('',#192815,#11356);
#4290=LINE('',#192824,#11357);
#4291=LINE('',#192828,#11358);
#4292=LINE('',#192833,#11359);
#4293=LINE('',#192839,#11360);
#4294=LINE('',#192848,#11361);
#4295=LINE('',#192852,#11362);
#4296=LINE('',#192857,#11363);
#4297=LINE('',#192863,#11364);
#4298=LINE('',#192872,#11365);
#4299=LINE('',#192876,#11366);
#4300=LINE('',#192881,#11367);
#4301=LINE('',#192887,#11368);
#4302=LINE('',#192896,#11369);
#4303=LINE('',#192900,#11370);
#4304=LINE('',#192905,#11371);
#4305=LINE('',#192911,#11372);
#4306=LINE('',#192920,#11373);
#4307=LINE('',#192924,#11374);
#4308=LINE('',#192929,#11375);
#4309=LINE('',#192935,#11376);
#4310=LINE('',#192944,#11377);
#4311=LINE('',#192948,#11378);
#4312=LINE('',#192953,#11379);
#4313=LINE('',#192959,#11380);
#4314=LINE('',#192968,#11381);
#4315=LINE('',#192972,#11382);
#4316=LINE('',#192977,#11383);
#4317=LINE('',#192983,#11384);
#4318=LINE('',#192992,#11385);
#4319=LINE('',#192996,#11386);
#4320=LINE('',#193001,#11387);
#4321=LINE('',#193007,#11388);
#4322=LINE('',#193016,#11389);
#4323=LINE('',#193020,#11390);
#4324=LINE('',#193025,#11391);
#4325=LINE('',#193031,#11392);
#4326=LINE('',#193040,#11393);
#4327=LINE('',#193044,#11394);
#4328=LINE('',#193049,#11395);
#4329=LINE('',#193055,#11396);
#4330=LINE('',#193064,#11397);
#4331=LINE('',#193068,#11398);
#4332=LINE('',#193073,#11399);
#4333=LINE('',#193079,#11400);
#4334=LINE('',#193088,#11401);
#4335=LINE('',#193092,#11402);
#4336=LINE('',#193097,#11403);
#4337=LINE('',#193103,#11404);
#4338=LINE('',#193112,#11405);
#4339=LINE('',#193116,#11406);
#4340=LINE('',#193121,#11407);
#4341=LINE('',#193127,#11408);
#4342=LINE('',#193136,#11409);
#4343=LINE('',#193140,#11410);
#4344=LINE('',#193145,#11411);
#4345=LINE('',#193151,#11412);
#4346=LINE('',#193160,#11413);
#4347=LINE('',#193164,#11414);
#4348=LINE('',#193169,#11415);
#4349=LINE('',#193175,#11416);
#4350=LINE('',#193184,#11417);
#4351=LINE('',#193188,#11418);
#4352=LINE('',#193193,#11419);
#4353=LINE('',#193199,#11420);
#4354=LINE('',#193208,#11421);
#4355=LINE('',#193212,#11422);
#4356=LINE('',#193217,#11423);
#4357=LINE('',#193223,#11424);
#4358=LINE('',#193232,#11425);
#4359=LINE('',#193236,#11426);
#4360=LINE('',#193241,#11427);
#4361=LINE('',#193247,#11428);
#4362=LINE('',#193256,#11429);
#4363=LINE('',#193260,#11430);
#4364=LINE('',#193265,#11431);
#4365=LINE('',#193271,#11432);
#4366=LINE('',#193280,#11433);
#4367=LINE('',#193284,#11434);
#4368=LINE('',#193289,#11435);
#4369=LINE('',#193295,#11436);
#4370=LINE('',#193304,#11437);
#4371=LINE('',#193308,#11438);
#4372=LINE('',#193313,#11439);
#4373=LINE('',#193319,#11440);
#4374=LINE('',#193328,#11441);
#4375=LINE('',#193332,#11442);
#4376=LINE('',#193337,#11443);
#4377=LINE('',#193343,#11444);
#4378=LINE('',#193352,#11445);
#4379=LINE('',#193356,#11446);
#4380=LINE('',#193361,#11447);
#4381=LINE('',#193367,#11448);
#4382=LINE('',#193376,#11449);
#4383=LINE('',#193380,#11450);
#4384=LINE('',#193385,#11451);
#4385=LINE('',#193391,#11452);
#4386=LINE('',#193400,#11453);
#4387=LINE('',#193404,#11454);
#4388=LINE('',#193409,#11455);
#4389=LINE('',#193415,#11456);
#4390=LINE('',#193425,#11457);
#4391=LINE('',#193427,#11458);
#4392=LINE('',#193429,#11459);
#4393=LINE('',#193430,#11460);
#4394=LINE('',#193434,#11461);
#4395=LINE('',#193435,#11462);
#4396=LINE('',#193436,#11463);
#4397=LINE('',#193440,#11464);
#4398=LINE('',#193441,#11465);
#4399=LINE('',#193442,#11466);
#4400=LINE('',#193444,#11467);
#4401=LINE('',#193445,#11468);
#4402=LINE('',#193449,#11469);
#4403=LINE('',#193451,#11470);
#4404=LINE('',#193453,#11471);
#4405=LINE('',#193454,#11472);
#4406=LINE('',#193458,#11473);
#4407=LINE('',#193459,#11474);
#4408=LINE('',#193460,#11475);
#4409=LINE('',#193464,#11476);
#4410=LINE('',#193465,#11477);
#4411=LINE('',#193466,#11478);
#4412=LINE('',#193468,#11479);
#4413=LINE('',#193469,#11480);
#4414=LINE('',#193473,#11481);
#4415=LINE('',#193475,#11482);
#4416=LINE('',#193477,#11483);
#4417=LINE('',#193478,#11484);
#4418=LINE('',#193482,#11485);
#4419=LINE('',#193483,#11486);
#4420=LINE('',#193484,#11487);
#4421=LINE('',#193488,#11488);
#4422=LINE('',#193489,#11489);
#4423=LINE('',#193490,#11490);
#4424=LINE('',#193492,#11491);
#4425=LINE('',#193493,#11492);
#4426=LINE('',#193497,#11493);
#4427=LINE('',#193499,#11494);
#4428=LINE('',#193501,#11495);
#4429=LINE('',#193502,#11496);
#4430=LINE('',#193506,#11497);
#4431=LINE('',#193507,#11498);
#4432=LINE('',#193508,#11499);
#4433=LINE('',#193512,#11500);
#4434=LINE('',#193513,#11501);
#4435=LINE('',#193514,#11502);
#4436=LINE('',#193516,#11503);
#4437=LINE('',#193517,#11504);
#4438=LINE('',#193521,#11505);
#4439=LINE('',#193523,#11506);
#4440=LINE('',#193525,#11507);
#4441=LINE('',#193526,#11508);
#4442=LINE('',#193530,#11509);
#4443=LINE('',#193531,#11510);
#4444=LINE('',#193532,#11511);
#4445=LINE('',#193536,#11512);
#4446=LINE('',#193537,#11513);
#4447=LINE('',#193538,#11514);
#4448=LINE('',#193540,#11515);
#4449=LINE('',#193541,#11516);
#4450=LINE('',#193545,#11517);
#4451=LINE('',#193547,#11518);
#4452=LINE('',#193549,#11519);
#4453=LINE('',#193550,#11520);
#4454=LINE('',#193554,#11521);
#4455=LINE('',#193555,#11522);
#4456=LINE('',#193556,#11523);
#4457=LINE('',#193560,#11524);
#4458=LINE('',#193561,#11525);
#4459=LINE('',#193562,#11526);
#4460=LINE('',#193564,#11527);
#4461=LINE('',#193565,#11528);
#4462=LINE('',#193569,#11529);
#4463=LINE('',#193571,#11530);
#4464=LINE('',#193573,#11531);
#4465=LINE('',#193574,#11532);
#4466=LINE('',#193578,#11533);
#4467=LINE('',#193579,#11534);
#4468=LINE('',#193580,#11535);
#4469=LINE('',#193584,#11536);
#4470=LINE('',#193585,#11537);
#4471=LINE('',#193586,#11538);
#4472=LINE('',#193588,#11539);
#4473=LINE('',#193589,#11540);
#4474=LINE('',#193593,#11541);
#4475=LINE('',#193595,#11542);
#4476=LINE('',#193597,#11543);
#4477=LINE('',#193598,#11544);
#4478=LINE('',#193602,#11545);
#4479=LINE('',#193603,#11546);
#4480=LINE('',#193604,#11547);
#4481=LINE('',#193608,#11548);
#4482=LINE('',#193609,#11549);
#4483=LINE('',#193610,#11550);
#4484=LINE('',#193612,#11551);
#4485=LINE('',#193613,#11552);
#4486=LINE('',#193617,#11553);
#4487=LINE('',#193619,#11554);
#4488=LINE('',#193621,#11555);
#4489=LINE('',#193622,#11556);
#4490=LINE('',#193626,#11557);
#4491=LINE('',#193627,#11558);
#4492=LINE('',#193628,#11559);
#4493=LINE('',#193632,#11560);
#4494=LINE('',#193633,#11561);
#4495=LINE('',#193634,#11562);
#4496=LINE('',#193636,#11563);
#4497=LINE('',#193637,#11564);
#4498=LINE('',#193641,#11565);
#4499=LINE('',#193643,#11566);
#4500=LINE('',#193645,#11567);
#4501=LINE('',#193646,#11568);
#4502=LINE('',#193650,#11569);
#4503=LINE('',#193651,#11570);
#4504=LINE('',#193652,#11571);
#4505=LINE('',#193656,#11572);
#4506=LINE('',#193657,#11573);
#4507=LINE('',#193658,#11574);
#4508=LINE('',#193660,#11575);
#4509=LINE('',#193661,#11576);
#4510=LINE('',#193665,#11577);
#4511=LINE('',#193667,#11578);
#4512=LINE('',#193669,#11579);
#4513=LINE('',#193670,#11580);
#4514=LINE('',#193674,#11581);
#4515=LINE('',#193675,#11582);
#4516=LINE('',#193676,#11583);
#4517=LINE('',#193680,#11584);
#4518=LINE('',#193681,#11585);
#4519=LINE('',#193682,#11586);
#4520=LINE('',#193684,#11587);
#4521=LINE('',#193685,#11588);
#4522=LINE('',#193689,#11589);
#4523=LINE('',#193691,#11590);
#4524=LINE('',#193693,#11591);
#4525=LINE('',#193694,#11592);
#4526=LINE('',#193698,#11593);
#4527=LINE('',#193699,#11594);
#4528=LINE('',#193700,#11595);
#4529=LINE('',#193704,#11596);
#4530=LINE('',#193705,#11597);
#4531=LINE('',#193706,#11598);
#4532=LINE('',#193708,#11599);
#4533=LINE('',#193709,#11600);
#4534=LINE('',#193713,#11601);
#4535=LINE('',#193715,#11602);
#4536=LINE('',#193717,#11603);
#4537=LINE('',#193718,#11604);
#4538=LINE('',#193722,#11605);
#4539=LINE('',#193723,#11606);
#4540=LINE('',#193724,#11607);
#4541=LINE('',#193728,#11608);
#4542=LINE('',#193729,#11609);
#4543=LINE('',#193730,#11610);
#4544=LINE('',#193732,#11611);
#4545=LINE('',#193733,#11612);
#4546=LINE('',#193737,#11613);
#4547=LINE('',#193739,#11614);
#4548=LINE('',#193741,#11615);
#4549=LINE('',#193742,#11616);
#4550=LINE('',#193746,#11617);
#4551=LINE('',#193747,#11618);
#4552=LINE('',#193748,#11619);
#4553=LINE('',#193752,#11620);
#4554=LINE('',#193753,#11621);
#4555=LINE('',#193754,#11622);
#4556=LINE('',#193756,#11623);
#4557=LINE('',#193757,#11624);
#4558=LINE('',#193761,#11625);
#4559=LINE('',#193763,#11626);
#4560=LINE('',#193765,#11627);
#4561=LINE('',#193766,#11628);
#4562=LINE('',#193770,#11629);
#4563=LINE('',#193771,#11630);
#4564=LINE('',#193772,#11631);
#4565=LINE('',#193776,#11632);
#4566=LINE('',#193777,#11633);
#4567=LINE('',#193778,#11634);
#4568=LINE('',#193780,#11635);
#4569=LINE('',#193781,#11636);
#4570=LINE('',#193785,#11637);
#4571=LINE('',#193787,#11638);
#4572=LINE('',#193789,#11639);
#4573=LINE('',#193790,#11640);
#4574=LINE('',#193794,#11641);
#4575=LINE('',#193795,#11642);
#4576=LINE('',#193796,#11643);
#4577=LINE('',#193800,#11644);
#4578=LINE('',#193801,#11645);
#4579=LINE('',#193802,#11646);
#4580=LINE('',#193804,#11647);
#4581=LINE('',#193805,#11648);
#4582=LINE('',#193809,#11649);
#4583=LINE('',#193811,#11650);
#4584=LINE('',#193813,#11651);
#4585=LINE('',#193814,#11652);
#4586=LINE('',#193818,#11653);
#4587=LINE('',#193819,#11654);
#4588=LINE('',#193820,#11655);
#4589=LINE('',#193824,#11656);
#4590=LINE('',#193825,#11657);
#4591=LINE('',#193826,#11658);
#4592=LINE('',#193828,#11659);
#4593=LINE('',#193829,#11660);
#4594=LINE('',#193833,#11661);
#4595=LINE('',#193835,#11662);
#4596=LINE('',#193837,#11663);
#4597=LINE('',#193838,#11664);
#4598=LINE('',#193842,#11665);
#4599=LINE('',#193843,#11666);
#4600=LINE('',#193844,#11667);
#4601=LINE('',#193848,#11668);
#4602=LINE('',#193849,#11669);
#4603=LINE('',#193850,#11670);
#4604=LINE('',#193852,#11671);
#4605=LINE('',#193853,#11672);
#4606=LINE('',#193857,#11673);
#4607=LINE('',#193859,#11674);
#4608=LINE('',#193861,#11675);
#4609=LINE('',#193862,#11676);
#4610=LINE('',#193866,#11677);
#4611=LINE('',#193867,#11678);
#4612=LINE('',#193868,#11679);
#4613=LINE('',#193872,#11680);
#4614=LINE('',#193873,#11681);
#4615=LINE('',#193874,#11682);
#4616=LINE('',#193876,#11683);
#4617=LINE('',#193877,#11684);
#4618=LINE('',#193881,#11685);
#4619=LINE('',#193883,#11686);
#4620=LINE('',#193885,#11687);
#4621=LINE('',#193886,#11688);
#4622=LINE('',#193890,#11689);
#4623=LINE('',#193891,#11690);
#4624=LINE('',#193892,#11691);
#4625=LINE('',#193896,#11692);
#4626=LINE('',#193897,#11693);
#4627=LINE('',#193898,#11694);
#4628=LINE('',#193900,#11695);
#4629=LINE('',#193901,#11696);
#4630=LINE('',#193905,#11697);
#4631=LINE('',#193907,#11698);
#4632=LINE('',#193909,#11699);
#4633=LINE('',#193910,#11700);
#4634=LINE('',#193914,#11701);
#4635=LINE('',#193915,#11702);
#4636=LINE('',#193916,#11703);
#4637=LINE('',#193920,#11704);
#4638=LINE('',#193921,#11705);
#4639=LINE('',#193922,#11706);
#4640=LINE('',#193924,#11707);
#4641=LINE('',#193925,#11708);
#4642=LINE('',#193929,#11709);
#4643=LINE('',#193931,#11710);
#4644=LINE('',#193933,#11711);
#4645=LINE('',#193934,#11712);
#4646=LINE('',#193938,#11713);
#4647=LINE('',#193939,#11714);
#4648=LINE('',#193940,#11715);
#4649=LINE('',#193944,#11716);
#4650=LINE('',#193945,#11717);
#4651=LINE('',#193946,#11718);
#4652=LINE('',#193948,#11719);
#4653=LINE('',#193949,#11720);
#4654=LINE('',#193953,#11721);
#4655=LINE('',#193955,#11722);
#4656=LINE('',#193957,#11723);
#4657=LINE('',#193958,#11724);
#4658=LINE('',#193962,#11725);
#4659=LINE('',#193963,#11726);
#4660=LINE('',#193964,#11727);
#4661=LINE('',#193968,#11728);
#4662=LINE('',#193969,#11729);
#4663=LINE('',#193970,#11730);
#4664=LINE('',#193972,#11731);
#4665=LINE('',#193973,#11732);
#4666=LINE('',#193977,#11733);
#4667=LINE('',#193979,#11734);
#4668=LINE('',#193981,#11735);
#4669=LINE('',#193982,#11736);
#4670=LINE('',#193986,#11737);
#4671=LINE('',#193987,#11738);
#4672=LINE('',#193988,#11739);
#4673=LINE('',#193992,#11740);
#4674=LINE('',#193993,#11741);
#4675=LINE('',#193994,#11742);
#4676=LINE('',#193996,#11743);
#4677=LINE('',#193997,#11744);
#4678=LINE('',#194001,#11745);
#4679=LINE('',#194003,#11746);
#4680=LINE('',#194005,#11747);
#4681=LINE('',#194006,#11748);
#4682=LINE('',#194010,#11749);
#4683=LINE('',#194011,#11750);
#4684=LINE('',#194012,#11751);
#4685=LINE('',#194016,#11752);
#4686=LINE('',#194017,#11753);
#4687=LINE('',#194018,#11754);
#4688=LINE('',#194020,#11755);
#4689=LINE('',#194021,#11756);
#4690=LINE('',#194025,#11757);
#4691=LINE('',#194027,#11758);
#4692=LINE('',#194029,#11759);
#4693=LINE('',#194030,#11760);
#4694=LINE('',#194034,#11761);
#4695=LINE('',#194035,#11762);
#4696=LINE('',#194036,#11763);
#4697=LINE('',#194040,#11764);
#4698=LINE('',#194041,#11765);
#4699=LINE('',#194042,#11766);
#4700=LINE('',#194044,#11767);
#4701=LINE('',#194045,#11768);
#4702=LINE('',#194049,#11769);
#4703=LINE('',#194051,#11770);
#4704=LINE('',#194053,#11771);
#4705=LINE('',#194054,#11772);
#4706=LINE('',#194058,#11773);
#4707=LINE('',#194059,#11774);
#4708=LINE('',#194060,#11775);
#4709=LINE('',#194064,#11776);
#4710=LINE('',#194065,#11777);
#4711=LINE('',#194066,#11778);
#4712=LINE('',#194068,#11779);
#4713=LINE('',#194069,#11780);
#4714=LINE('',#194073,#11781);
#4715=LINE('',#194075,#11782);
#4716=LINE('',#194077,#11783);
#4717=LINE('',#194078,#11784);
#4718=LINE('',#194082,#11785);
#4719=LINE('',#194083,#11786);
#4720=LINE('',#194084,#11787);
#4721=LINE('',#194088,#11788);
#4722=LINE('',#194089,#11789);
#4723=LINE('',#194090,#11790);
#4724=LINE('',#194092,#11791);
#4725=LINE('',#194093,#11792);
#4726=LINE('',#194097,#11793);
#4727=LINE('',#194099,#11794);
#4728=LINE('',#194101,#11795);
#4729=LINE('',#194102,#11796);
#4730=LINE('',#194106,#11797);
#4731=LINE('',#194107,#11798);
#4732=LINE('',#194108,#11799);
#4733=LINE('',#194112,#11800);
#4734=LINE('',#194113,#11801);
#4735=LINE('',#194114,#11802);
#4736=LINE('',#194116,#11803);
#4737=LINE('',#194117,#11804);
#4738=LINE('',#194121,#11805);
#4739=LINE('',#194123,#11806);
#4740=LINE('',#194125,#11807);
#4741=LINE('',#194126,#11808);
#4742=LINE('',#194130,#11809);
#4743=LINE('',#194131,#11810);
#4744=LINE('',#194132,#11811);
#4745=LINE('',#194136,#11812);
#4746=LINE('',#194137,#11813);
#4747=LINE('',#194138,#11814);
#4748=LINE('',#194140,#11815);
#4749=LINE('',#194141,#11816);
#4750=LINE('',#194145,#11817);
#4751=LINE('',#194147,#11818);
#4752=LINE('',#194149,#11819);
#4753=LINE('',#194150,#11820);
#4754=LINE('',#194154,#11821);
#4755=LINE('',#194155,#11822);
#4756=LINE('',#194156,#11823);
#4757=LINE('',#194160,#11824);
#4758=LINE('',#194161,#11825);
#4759=LINE('',#194162,#11826);
#4760=LINE('',#194164,#11827);
#4761=LINE('',#194165,#11828);
#4762=LINE('',#194169,#11829);
#4763=LINE('',#194171,#11830);
#4764=LINE('',#194173,#11831);
#4765=LINE('',#194174,#11832);
#4766=LINE('',#194178,#11833);
#4767=LINE('',#194179,#11834);
#4768=LINE('',#194180,#11835);
#4769=LINE('',#194184,#11836);
#4770=LINE('',#194185,#11837);
#4771=LINE('',#194186,#11838);
#4772=LINE('',#194188,#11839);
#4773=LINE('',#194189,#11840);
#4774=LINE('',#194193,#11841);
#4775=LINE('',#194195,#11842);
#4776=LINE('',#194197,#11843);
#4777=LINE('',#194198,#11844);
#4778=LINE('',#194202,#11845);
#4779=LINE('',#194203,#11846);
#4780=LINE('',#194204,#11847);
#4781=LINE('',#194208,#11848);
#4782=LINE('',#194209,#11849);
#4783=LINE('',#194210,#11850);
#4784=LINE('',#194212,#11851);
#4785=LINE('',#194213,#11852);
#4786=LINE('',#194217,#11853);
#4787=LINE('',#194219,#11854);
#4788=LINE('',#194221,#11855);
#4789=LINE('',#194222,#11856);
#4790=LINE('',#194226,#11857);
#4791=LINE('',#194227,#11858);
#4792=LINE('',#194228,#11859);
#4793=LINE('',#194232,#11860);
#4794=LINE('',#194233,#11861);
#4795=LINE('',#194234,#11862);
#4796=LINE('',#194236,#11863);
#4797=LINE('',#194237,#11864);
#4798=LINE('',#194241,#11865);
#4799=LINE('',#194243,#11866);
#4800=LINE('',#194245,#11867);
#4801=LINE('',#194246,#11868);
#4802=LINE('',#194250,#11869);
#4803=LINE('',#194251,#11870);
#4804=LINE('',#194252,#11871);
#4805=LINE('',#194256,#11872);
#4806=LINE('',#194257,#11873);
#4807=LINE('',#194258,#11874);
#4808=LINE('',#194260,#11875);
#4809=LINE('',#194261,#11876);
#4810=LINE('',#194265,#11877);
#4811=LINE('',#194267,#11878);
#4812=LINE('',#194269,#11879);
#4813=LINE('',#194270,#11880);
#4814=LINE('',#194274,#11881);
#4815=LINE('',#194275,#11882);
#4816=LINE('',#194276,#11883);
#4817=LINE('',#194280,#11884);
#4818=LINE('',#194281,#11885);
#4819=LINE('',#194282,#11886);
#4820=LINE('',#194284,#11887);
#4821=LINE('',#194285,#11888);
#4822=LINE('',#194289,#11889);
#4823=LINE('',#194291,#11890);
#4824=LINE('',#194293,#11891);
#4825=LINE('',#194294,#11892);
#4826=LINE('',#194298,#11893);
#4827=LINE('',#194299,#11894);
#4828=LINE('',#194300,#11895);
#4829=LINE('',#194304,#11896);
#4830=LINE('',#194305,#11897);
#4831=LINE('',#194306,#11898);
#4832=LINE('',#194308,#11899);
#4833=LINE('',#194309,#11900);
#4834=LINE('',#194313,#11901);
#4835=LINE('',#194315,#11902);
#4836=LINE('',#194317,#11903);
#4837=LINE('',#194318,#11904);
#4838=LINE('',#194322,#11905);
#4839=LINE('',#194323,#11906);
#4840=LINE('',#194324,#11907);
#4841=LINE('',#194328,#11908);
#4842=LINE('',#194329,#11909);
#4843=LINE('',#194330,#11910);
#4844=LINE('',#194332,#11911);
#4845=LINE('',#194333,#11912);
#4846=LINE('',#194337,#11913);
#4847=LINE('',#194339,#11914);
#4848=LINE('',#194341,#11915);
#4849=LINE('',#194342,#11916);
#4850=LINE('',#194346,#11917);
#4851=LINE('',#194347,#11918);
#4852=LINE('',#194348,#11919);
#4853=LINE('',#194352,#11920);
#4854=LINE('',#194353,#11921);
#4855=LINE('',#194354,#11922);
#4856=LINE('',#194356,#11923);
#4857=LINE('',#194357,#11924);
#4858=LINE('',#194361,#11925);
#4859=LINE('',#194363,#11926);
#4860=LINE('',#194365,#11927);
#4861=LINE('',#194366,#11928);
#4862=LINE('',#194370,#11929);
#4863=LINE('',#194371,#11930);
#4864=LINE('',#194372,#11931);
#4865=LINE('',#194376,#11932);
#4866=LINE('',#194377,#11933);
#4867=LINE('',#194378,#11934);
#4868=LINE('',#194380,#11935);
#4869=LINE('',#194381,#11936);
#4870=LINE('',#194385,#11937);
#4871=LINE('',#194387,#11938);
#4872=LINE('',#194389,#11939);
#4873=LINE('',#194390,#11940);
#4874=LINE('',#194394,#11941);
#4875=LINE('',#194395,#11942);
#4876=LINE('',#194396,#11943);
#4877=LINE('',#194400,#11944);
#4878=LINE('',#194401,#11945);
#4879=LINE('',#194402,#11946);
#4880=LINE('',#194404,#11947);
#4881=LINE('',#194405,#11948);
#4882=LINE('',#194409,#11949);
#4883=LINE('',#194411,#11950);
#4884=LINE('',#194413,#11951);
#4885=LINE('',#194414,#11952);
#4886=LINE('',#194418,#11953);
#4887=LINE('',#194419,#11954);
#4888=LINE('',#194420,#11955);
#4889=LINE('',#194424,#11956);
#4890=LINE('',#194425,#11957);
#4891=LINE('',#194426,#11958);
#4892=LINE('',#194428,#11959);
#4893=LINE('',#194429,#11960);
#4894=LINE('',#194433,#11961);
#4895=LINE('',#194435,#11962);
#4896=LINE('',#194437,#11963);
#4897=LINE('',#194438,#11964);
#4898=LINE('',#194442,#11965);
#4899=LINE('',#194443,#11966);
#4900=LINE('',#194444,#11967);
#4901=LINE('',#194448,#11968);
#4902=LINE('',#194449,#11969);
#4903=LINE('',#194450,#11970);
#4904=LINE('',#194452,#11971);
#4905=LINE('',#194453,#11972);
#4906=LINE('',#194457,#11973);
#4907=LINE('',#194459,#11974);
#4908=LINE('',#194461,#11975);
#4909=LINE('',#194462,#11976);
#4910=LINE('',#194466,#11977);
#4911=LINE('',#194467,#11978);
#4912=LINE('',#194468,#11979);
#4913=LINE('',#194472,#11980);
#4914=LINE('',#194473,#11981);
#4915=LINE('',#194474,#11982);
#4916=LINE('',#194476,#11983);
#4917=LINE('',#194477,#11984);
#4918=LINE('',#194481,#11985);
#4919=LINE('',#194483,#11986);
#4920=LINE('',#194485,#11987);
#4921=LINE('',#194486,#11988);
#4922=LINE('',#194490,#11989);
#4923=LINE('',#194491,#11990);
#4924=LINE('',#194492,#11991);
#4925=LINE('',#194496,#11992);
#4926=LINE('',#194497,#11993);
#4927=LINE('',#194498,#11994);
#4928=LINE('',#194500,#11995);
#4929=LINE('',#194501,#11996);
#4930=LINE('',#194505,#11997);
#4931=LINE('',#194507,#11998);
#4932=LINE('',#194509,#11999);
#4933=LINE('',#194510,#12000);
#4934=LINE('',#194514,#12001);
#4935=LINE('',#194515,#12002);
#4936=LINE('',#194516,#12003);
#4937=LINE('',#194520,#12004);
#4938=LINE('',#194521,#12005);
#4939=LINE('',#194522,#12006);
#4940=LINE('',#194524,#12007);
#4941=LINE('',#194525,#12008);
#4942=LINE('',#194529,#12009);
#4943=LINE('',#194531,#12010);
#4944=LINE('',#194533,#12011);
#4945=LINE('',#194534,#12012);
#4946=LINE('',#194538,#12013);
#4947=LINE('',#194539,#12014);
#4948=LINE('',#194540,#12015);
#4949=LINE('',#194544,#12016);
#4950=LINE('',#194545,#12017);
#4951=LINE('',#194546,#12018);
#4952=LINE('',#194548,#12019);
#4953=LINE('',#194549,#12020);
#4954=LINE('',#194553,#12021);
#4955=LINE('',#194555,#12022);
#4956=LINE('',#194557,#12023);
#4957=LINE('',#194558,#12024);
#4958=LINE('',#194562,#12025);
#4959=LINE('',#194563,#12026);
#4960=LINE('',#194564,#12027);
#4961=LINE('',#194568,#12028);
#4962=LINE('',#194569,#12029);
#4963=LINE('',#194570,#12030);
#4964=LINE('',#194572,#12031);
#4965=LINE('',#194573,#12032);
#4966=LINE('',#194577,#12033);
#4967=LINE('',#194579,#12034);
#4968=LINE('',#194581,#12035);
#4969=LINE('',#194582,#12036);
#4970=LINE('',#194586,#12037);
#4971=LINE('',#194587,#12038);
#4972=LINE('',#194588,#12039);
#4973=LINE('',#194592,#12040);
#4974=LINE('',#194593,#12041);
#4975=LINE('',#194594,#12042);
#4976=LINE('',#194596,#12043);
#4977=LINE('',#194597,#12044);
#4978=LINE('',#194601,#12045);
#4979=LINE('',#194603,#12046);
#4980=LINE('',#194605,#12047);
#4981=LINE('',#194606,#12048);
#4982=LINE('',#194610,#12049);
#4983=LINE('',#194611,#12050);
#4984=LINE('',#194612,#12051);
#4985=LINE('',#194616,#12052);
#4986=LINE('',#194617,#12053);
#4987=LINE('',#194618,#12054);
#4988=LINE('',#194620,#12055);
#4989=LINE('',#194621,#12056);
#4990=LINE('',#194625,#12057);
#4991=LINE('',#194627,#12058);
#4992=LINE('',#194629,#12059);
#4993=LINE('',#194630,#12060);
#4994=LINE('',#194634,#12061);
#4995=LINE('',#194635,#12062);
#4996=LINE('',#194636,#12063);
#4997=LINE('',#194640,#12064);
#4998=LINE('',#194641,#12065);
#4999=LINE('',#194642,#12066);
#5000=LINE('',#194644,#12067);
#5001=LINE('',#194645,#12068);
#5002=LINE('',#194649,#12069);
#5003=LINE('',#194651,#12070);
#5004=LINE('',#194653,#12071);
#5005=LINE('',#194654,#12072);
#5006=LINE('',#194658,#12073);
#5007=LINE('',#194659,#12074);
#5008=LINE('',#194660,#12075);
#5009=LINE('',#194664,#12076);
#5010=LINE('',#194665,#12077);
#5011=LINE('',#194666,#12078);
#5012=LINE('',#194668,#12079);
#5013=LINE('',#194669,#12080);
#5014=LINE('',#194673,#12081);
#5015=LINE('',#194675,#12082);
#5016=LINE('',#194677,#12083);
#5017=LINE('',#194678,#12084);
#5018=LINE('',#194682,#12085);
#5019=LINE('',#194683,#12086);
#5020=LINE('',#194684,#12087);
#5021=LINE('',#194688,#12088);
#5022=LINE('',#194689,#12089);
#5023=LINE('',#194690,#12090);
#5024=LINE('',#194692,#12091);
#5025=LINE('',#194693,#12092);
#5026=LINE('',#194697,#12093);
#5027=LINE('',#194699,#12094);
#5028=LINE('',#194701,#12095);
#5029=LINE('',#194702,#12096);
#5030=LINE('',#194706,#12097);
#5031=LINE('',#194707,#12098);
#5032=LINE('',#194708,#12099);
#5033=LINE('',#194712,#12100);
#5034=LINE('',#194713,#12101);
#5035=LINE('',#194714,#12102);
#5036=LINE('',#194716,#12103);
#5037=LINE('',#194717,#12104);
#5038=LINE('',#194721,#12105);
#5039=LINE('',#194723,#12106);
#5040=LINE('',#194725,#12107);
#5041=LINE('',#194726,#12108);
#5042=LINE('',#194730,#12109);
#5043=LINE('',#194731,#12110);
#5044=LINE('',#194732,#12111);
#5045=LINE('',#194736,#12112);
#5046=LINE('',#194737,#12113);
#5047=LINE('',#194738,#12114);
#5048=LINE('',#194740,#12115);
#5049=LINE('',#194741,#12116);
#5050=LINE('',#194745,#12117);
#5051=LINE('',#194747,#12118);
#5052=LINE('',#194749,#12119);
#5053=LINE('',#194750,#12120);
#5054=LINE('',#194754,#12121);
#5055=LINE('',#194755,#12122);
#5056=LINE('',#194756,#12123);
#5057=LINE('',#194760,#12124);
#5058=LINE('',#194761,#12125);
#5059=LINE('',#194762,#12126);
#5060=LINE('',#194764,#12127);
#5061=LINE('',#194765,#12128);
#5062=LINE('',#194769,#12129);
#5063=LINE('',#194771,#12130);
#5064=LINE('',#194773,#12131);
#5065=LINE('',#194774,#12132);
#5066=LINE('',#194778,#12133);
#5067=LINE('',#194779,#12134);
#5068=LINE('',#194780,#12135);
#5069=LINE('',#194784,#12136);
#5070=LINE('',#194785,#12137);
#5071=LINE('',#194786,#12138);
#5072=LINE('',#194788,#12139);
#5073=LINE('',#194789,#12140);
#5074=LINE('',#194793,#12141);
#5075=LINE('',#194795,#12142);
#5076=LINE('',#194797,#12143);
#5077=LINE('',#194798,#12144);
#5078=LINE('',#194802,#12145);
#5079=LINE('',#194803,#12146);
#5080=LINE('',#194804,#12147);
#5081=LINE('',#194808,#12148);
#5082=LINE('',#194809,#12149);
#5083=LINE('',#194810,#12150);
#5084=LINE('',#194812,#12151);
#5085=LINE('',#194813,#12152);
#5086=LINE('',#194817,#12153);
#5087=LINE('',#194819,#12154);
#5088=LINE('',#194821,#12155);
#5089=LINE('',#194822,#12156);
#5090=LINE('',#194826,#12157);
#5091=LINE('',#194827,#12158);
#5092=LINE('',#194828,#12159);
#5093=LINE('',#194832,#12160);
#5094=LINE('',#194833,#12161);
#5095=LINE('',#194834,#12162);
#5096=LINE('',#194836,#12163);
#5097=LINE('',#194837,#12164);
#5098=LINE('',#194841,#12165);
#5099=LINE('',#194843,#12166);
#5100=LINE('',#194845,#12167);
#5101=LINE('',#194846,#12168);
#5102=LINE('',#194850,#12169);
#5103=LINE('',#194851,#12170);
#5104=LINE('',#194852,#12171);
#5105=LINE('',#194856,#12172);
#5106=LINE('',#194857,#12173);
#5107=LINE('',#194858,#12174);
#5108=LINE('',#194860,#12175);
#5109=LINE('',#194861,#12176);
#5110=LINE('',#194865,#12177);
#5111=LINE('',#194867,#12178);
#5112=LINE('',#194869,#12179);
#5113=LINE('',#194870,#12180);
#5114=LINE('',#194874,#12181);
#5115=LINE('',#194875,#12182);
#5116=LINE('',#194876,#12183);
#5117=LINE('',#194880,#12184);
#5118=LINE('',#194881,#12185);
#5119=LINE('',#194882,#12186);
#5120=LINE('',#194884,#12187);
#5121=LINE('',#194885,#12188);
#5122=LINE('',#194889,#12189);
#5123=LINE('',#194891,#12190);
#5124=LINE('',#194893,#12191);
#5125=LINE('',#194894,#12192);
#5126=LINE('',#194898,#12193);
#5127=LINE('',#194899,#12194);
#5128=LINE('',#194900,#12195);
#5129=LINE('',#194904,#12196);
#5130=LINE('',#194905,#12197);
#5131=LINE('',#194906,#12198);
#5132=LINE('',#194908,#12199);
#5133=LINE('',#194909,#12200);
#5134=LINE('',#194913,#12201);
#5135=LINE('',#194915,#12202);
#5136=LINE('',#194917,#12203);
#5137=LINE('',#194918,#12204);
#5138=LINE('',#194922,#12205);
#5139=LINE('',#194923,#12206);
#5140=LINE('',#194924,#12207);
#5141=LINE('',#194928,#12208);
#5142=LINE('',#194929,#12209);
#5143=LINE('',#194930,#12210);
#5144=LINE('',#194932,#12211);
#5145=LINE('',#194933,#12212);
#5146=LINE('',#194937,#12213);
#5147=LINE('',#194939,#12214);
#5148=LINE('',#194941,#12215);
#5149=LINE('',#194942,#12216);
#5150=LINE('',#194946,#12217);
#5151=LINE('',#194947,#12218);
#5152=LINE('',#194948,#12219);
#5153=LINE('',#194952,#12220);
#5154=LINE('',#194953,#12221);
#5155=LINE('',#194954,#12222);
#5156=LINE('',#194956,#12223);
#5157=LINE('',#194957,#12224);
#5158=LINE('',#194961,#12225);
#5159=LINE('',#194963,#12226);
#5160=LINE('',#194965,#12227);
#5161=LINE('',#194966,#12228);
#5162=LINE('',#194970,#12229);
#5163=LINE('',#194971,#12230);
#5164=LINE('',#194972,#12231);
#5165=LINE('',#194976,#12232);
#5166=LINE('',#194977,#12233);
#5167=LINE('',#194978,#12234);
#5168=LINE('',#194980,#12235);
#5169=LINE('',#194981,#12236);
#5170=LINE('',#194985,#12237);
#5171=LINE('',#194987,#12238);
#5172=LINE('',#194989,#12239);
#5173=LINE('',#194990,#12240);
#5174=LINE('',#194994,#12241);
#5175=LINE('',#194995,#12242);
#5176=LINE('',#194996,#12243);
#5177=LINE('',#195000,#12244);
#5178=LINE('',#195001,#12245);
#5179=LINE('',#195002,#12246);
#5180=LINE('',#195004,#12247);
#5181=LINE('',#195005,#12248);
#5182=LINE('',#195009,#12249);
#5183=LINE('',#195011,#12250);
#5184=LINE('',#195013,#12251);
#5185=LINE('',#195014,#12252);
#5186=LINE('',#195018,#12253);
#5187=LINE('',#195019,#12254);
#5188=LINE('',#195020,#12255);
#5189=LINE('',#195024,#12256);
#5190=LINE('',#195025,#12257);
#5191=LINE('',#195026,#12258);
#5192=LINE('',#195028,#12259);
#5193=LINE('',#195029,#12260);
#5194=LINE('',#195033,#12261);
#5195=LINE('',#195035,#12262);
#5196=LINE('',#195037,#12263);
#5197=LINE('',#195038,#12264);
#5198=LINE('',#195042,#12265);
#5199=LINE('',#195043,#12266);
#5200=LINE('',#195044,#12267);
#5201=LINE('',#195048,#12268);
#5202=LINE('',#195049,#12269);
#5203=LINE('',#195050,#12270);
#5204=LINE('',#195052,#12271);
#5205=LINE('',#195053,#12272);
#5206=LINE('',#195057,#12273);
#5207=LINE('',#195059,#12274);
#5208=LINE('',#195061,#12275);
#5209=LINE('',#195062,#12276);
#5210=LINE('',#195066,#12277);
#5211=LINE('',#195067,#12278);
#5212=LINE('',#195068,#12279);
#5213=LINE('',#195072,#12280);
#5214=LINE('',#195073,#12281);
#5215=LINE('',#195074,#12282);
#5216=LINE('',#195076,#12283);
#5217=LINE('',#195077,#12284);
#5218=LINE('',#195081,#12285);
#5219=LINE('',#195083,#12286);
#5220=LINE('',#195085,#12287);
#5221=LINE('',#195086,#12288);
#5222=LINE('',#195090,#12289);
#5223=LINE('',#195091,#12290);
#5224=LINE('',#195092,#12291);
#5225=LINE('',#195096,#12292);
#5226=LINE('',#195097,#12293);
#5227=LINE('',#195098,#12294);
#5228=LINE('',#195100,#12295);
#5229=LINE('',#195101,#12296);
#5230=LINE('',#195105,#12297);
#5231=LINE('',#195107,#12298);
#5232=LINE('',#195109,#12299);
#5233=LINE('',#195110,#12300);
#5234=LINE('',#195114,#12301);
#5235=LINE('',#195115,#12302);
#5236=LINE('',#195116,#12303);
#5237=LINE('',#195120,#12304);
#5238=LINE('',#195121,#12305);
#5239=LINE('',#195122,#12306);
#5240=LINE('',#195124,#12307);
#5241=LINE('',#195125,#12308);
#5242=LINE('',#195129,#12309);
#5243=LINE('',#195131,#12310);
#5244=LINE('',#195133,#12311);
#5245=LINE('',#195134,#12312);
#5246=LINE('',#195138,#12313);
#5247=LINE('',#195139,#12314);
#5248=LINE('',#195140,#12315);
#5249=LINE('',#195144,#12316);
#5250=LINE('',#195145,#12317);
#5251=LINE('',#195146,#12318);
#5252=LINE('',#195148,#12319);
#5253=LINE('',#195149,#12320);
#5254=LINE('',#195153,#12321);
#5255=LINE('',#195155,#12322);
#5256=LINE('',#195157,#12323);
#5257=LINE('',#195158,#12324);
#5258=LINE('',#195162,#12325);
#5259=LINE('',#195163,#12326);
#5260=LINE('',#195164,#12327);
#5261=LINE('',#195168,#12328);
#5262=LINE('',#195169,#12329);
#5263=LINE('',#195170,#12330);
#5264=LINE('',#195172,#12331);
#5265=LINE('',#195173,#12332);
#5266=LINE('',#195177,#12333);
#5267=LINE('',#195179,#12334);
#5268=LINE('',#195181,#12335);
#5269=LINE('',#195182,#12336);
#5270=LINE('',#195186,#12337);
#5271=LINE('',#195187,#12338);
#5272=LINE('',#195188,#12339);
#5273=LINE('',#195192,#12340);
#5274=LINE('',#195193,#12341);
#5275=LINE('',#195194,#12342);
#5276=LINE('',#195196,#12343);
#5277=LINE('',#195197,#12344);
#5278=LINE('',#195201,#12345);
#5279=LINE('',#195203,#12346);
#5280=LINE('',#195205,#12347);
#5281=LINE('',#195206,#12348);
#5282=LINE('',#195210,#12349);
#5283=LINE('',#195211,#12350);
#5284=LINE('',#195212,#12351);
#5285=LINE('',#195216,#12352);
#5286=LINE('',#195217,#12353);
#5287=LINE('',#195218,#12354);
#5288=LINE('',#195220,#12355);
#5289=LINE('',#195221,#12356);
#5290=LINE('',#195225,#12357);
#5291=LINE('',#195227,#12358);
#5292=LINE('',#195229,#12359);
#5293=LINE('',#195230,#12360);
#5294=LINE('',#195234,#12361);
#5295=LINE('',#195235,#12362);
#5296=LINE('',#195236,#12363);
#5297=LINE('',#195240,#12364);
#5298=LINE('',#195241,#12365);
#5299=LINE('',#195242,#12366);
#5300=LINE('',#195244,#12367);
#5301=LINE('',#195245,#12368);
#5302=LINE('',#195249,#12369);
#5303=LINE('',#195251,#12370);
#5304=LINE('',#195253,#12371);
#5305=LINE('',#195254,#12372);
#5306=LINE('',#195258,#12373);
#5307=LINE('',#195259,#12374);
#5308=LINE('',#195260,#12375);
#5309=LINE('',#195264,#12376);
#5310=LINE('',#195265,#12377);
#5311=LINE('',#195266,#12378);
#5312=LINE('',#195268,#12379);
#5313=LINE('',#195269,#12380);
#5314=LINE('',#195273,#12381);
#5315=LINE('',#195275,#12382);
#5316=LINE('',#195277,#12383);
#5317=LINE('',#195278,#12384);
#5318=LINE('',#195282,#12385);
#5319=LINE('',#195283,#12386);
#5320=LINE('',#195284,#12387);
#5321=LINE('',#195288,#12388);
#5322=LINE('',#195289,#12389);
#5323=LINE('',#195290,#12390);
#5324=LINE('',#195292,#12391);
#5325=LINE('',#195293,#12392);
#5326=LINE('',#195297,#12393);
#5327=LINE('',#195299,#12394);
#5328=LINE('',#195301,#12395);
#5329=LINE('',#195302,#12396);
#5330=LINE('',#195306,#12397);
#5331=LINE('',#195307,#12398);
#5332=LINE('',#195308,#12399);
#5333=LINE('',#195312,#12400);
#5334=LINE('',#195313,#12401);
#5335=LINE('',#195314,#12402);
#5336=LINE('',#195316,#12403);
#5337=LINE('',#195317,#12404);
#5338=LINE('',#195321,#12405);
#5339=LINE('',#195323,#12406);
#5340=LINE('',#195325,#12407);
#5341=LINE('',#195326,#12408);
#5342=LINE('',#195330,#12409);
#5343=LINE('',#195331,#12410);
#5344=LINE('',#195332,#12411);
#5345=LINE('',#195336,#12412);
#5346=LINE('',#195337,#12413);
#5347=LINE('',#195338,#12414);
#5348=LINE('',#195340,#12415);
#5349=LINE('',#195341,#12416);
#5350=LINE('',#195345,#12417);
#5351=LINE('',#195347,#12418);
#5352=LINE('',#195349,#12419);
#5353=LINE('',#195350,#12420);
#5354=LINE('',#195354,#12421);
#5355=LINE('',#195355,#12422);
#5356=LINE('',#195356,#12423);
#5357=LINE('',#195360,#12424);
#5358=LINE('',#195361,#12425);
#5359=LINE('',#195362,#12426);
#5360=LINE('',#195364,#12427);
#5361=LINE('',#195365,#12428);
#5362=LINE('',#195369,#12429);
#5363=LINE('',#195371,#12430);
#5364=LINE('',#195373,#12431);
#5365=LINE('',#195374,#12432);
#5366=LINE('',#195378,#12433);
#5367=LINE('',#195379,#12434);
#5368=LINE('',#195380,#12435);
#5369=LINE('',#195384,#12436);
#5370=LINE('',#195385,#12437);
#5371=LINE('',#195386,#12438);
#5372=LINE('',#195388,#12439);
#5373=LINE('',#195389,#12440);
#5374=LINE('',#195393,#12441);
#5375=LINE('',#195395,#12442);
#5376=LINE('',#195397,#12443);
#5377=LINE('',#195398,#12444);
#5378=LINE('',#195402,#12445);
#5379=LINE('',#195403,#12446);
#5380=LINE('',#195404,#12447);
#5381=LINE('',#195408,#12448);
#5382=LINE('',#195409,#12449);
#5383=LINE('',#195410,#12450);
#5384=LINE('',#195412,#12451);
#5385=LINE('',#195413,#12452);
#5386=LINE('',#195417,#12453);
#5387=LINE('',#195419,#12454);
#5388=LINE('',#195421,#12455);
#5389=LINE('',#195422,#12456);
#5390=LINE('',#195426,#12457);
#5391=LINE('',#195427,#12458);
#5392=LINE('',#195428,#12459);
#5393=LINE('',#195432,#12460);
#5394=LINE('',#195433,#12461);
#5395=LINE('',#195434,#12462);
#5396=LINE('',#195436,#12463);
#5397=LINE('',#195437,#12464);
#5398=LINE('',#195441,#12465);
#5399=LINE('',#195443,#12466);
#5400=LINE('',#195445,#12467);
#5401=LINE('',#195446,#12468);
#5402=LINE('',#195450,#12469);
#5403=LINE('',#195451,#12470);
#5404=LINE('',#195452,#12471);
#5405=LINE('',#195456,#12472);
#5406=LINE('',#195457,#12473);
#5407=LINE('',#195458,#12474);
#5408=LINE('',#195460,#12475);
#5409=LINE('',#195461,#12476);
#5410=LINE('',#195465,#12477);
#5411=LINE('',#195467,#12478);
#5412=LINE('',#195469,#12479);
#5413=LINE('',#195470,#12480);
#5414=LINE('',#195474,#12481);
#5415=LINE('',#195475,#12482);
#5416=LINE('',#195476,#12483);
#5417=LINE('',#195480,#12484);
#5418=LINE('',#195481,#12485);
#5419=LINE('',#195482,#12486);
#5420=LINE('',#195484,#12487);
#5421=LINE('',#195485,#12488);
#5422=LINE('',#195489,#12489);
#5423=LINE('',#195491,#12490);
#5424=LINE('',#195493,#12491);
#5425=LINE('',#195494,#12492);
#5426=LINE('',#195498,#12493);
#5427=LINE('',#195499,#12494);
#5428=LINE('',#195500,#12495);
#5429=LINE('',#195504,#12496);
#5430=LINE('',#195505,#12497);
#5431=LINE('',#195506,#12498);
#5432=LINE('',#195508,#12499);
#5433=LINE('',#195509,#12500);
#5434=LINE('',#195513,#12501);
#5435=LINE('',#195515,#12502);
#5436=LINE('',#195517,#12503);
#5437=LINE('',#195518,#12504);
#5438=LINE('',#195522,#12505);
#5439=LINE('',#195523,#12506);
#5440=LINE('',#195524,#12507);
#5441=LINE('',#195528,#12508);
#5442=LINE('',#195529,#12509);
#5443=LINE('',#195530,#12510);
#5444=LINE('',#195532,#12511);
#5445=LINE('',#195533,#12512);
#5446=LINE('',#195537,#12513);
#5447=LINE('',#195539,#12514);
#5448=LINE('',#195541,#12515);
#5449=LINE('',#195542,#12516);
#5450=LINE('',#195546,#12517);
#5451=LINE('',#195547,#12518);
#5452=LINE('',#195548,#12519);
#5453=LINE('',#195552,#12520);
#5454=LINE('',#195553,#12521);
#5455=LINE('',#195554,#12522);
#5456=LINE('',#195556,#12523);
#5457=LINE('',#195557,#12524);
#5458=LINE('',#195561,#12525);
#5459=LINE('',#195563,#12526);
#5460=LINE('',#195565,#12527);
#5461=LINE('',#195566,#12528);
#5462=LINE('',#195570,#12529);
#5463=LINE('',#195571,#12530);
#5464=LINE('',#195572,#12531);
#5465=LINE('',#195576,#12532);
#5466=LINE('',#195577,#12533);
#5467=LINE('',#195578,#12534);
#5468=LINE('',#195580,#12535);
#5469=LINE('',#195581,#12536);
#5470=LINE('',#195585,#12537);
#5471=LINE('',#195587,#12538);
#5472=LINE('',#195589,#12539);
#5473=LINE('',#195590,#12540);
#5474=LINE('',#195594,#12541);
#5475=LINE('',#195595,#12542);
#5476=LINE('',#195596,#12543);
#5477=LINE('',#195600,#12544);
#5478=LINE('',#195601,#12545);
#5479=LINE('',#195602,#12546);
#5480=LINE('',#195604,#12547);
#5481=LINE('',#195605,#12548);
#5482=LINE('',#195609,#12549);
#5483=LINE('',#195611,#12550);
#5484=LINE('',#195613,#12551);
#5485=LINE('',#195614,#12552);
#5486=LINE('',#195618,#12553);
#5487=LINE('',#195619,#12554);
#5488=LINE('',#195620,#12555);
#5489=LINE('',#195624,#12556);
#5490=LINE('',#195625,#12557);
#5491=LINE('',#195626,#12558);
#5492=LINE('',#195628,#12559);
#5493=LINE('',#195629,#12560);
#5494=LINE('',#195633,#12561);
#5495=LINE('',#195635,#12562);
#5496=LINE('',#195637,#12563);
#5497=LINE('',#195638,#12564);
#5498=LINE('',#195642,#12565);
#5499=LINE('',#195643,#12566);
#5500=LINE('',#195644,#12567);
#5501=LINE('',#195648,#12568);
#5502=LINE('',#195649,#12569);
#5503=LINE('',#195650,#12570);
#5504=LINE('',#195652,#12571);
#5505=LINE('',#195653,#12572);
#5506=LINE('',#195657,#12573);
#5507=LINE('',#195659,#12574);
#5508=LINE('',#195661,#12575);
#5509=LINE('',#195662,#12576);
#5510=LINE('',#195666,#12577);
#5511=LINE('',#195667,#12578);
#5512=LINE('',#195668,#12579);
#5513=LINE('',#195672,#12580);
#5514=LINE('',#195673,#12581);
#5515=LINE('',#195674,#12582);
#5516=LINE('',#195676,#12583);
#5517=LINE('',#195677,#12584);
#5518=LINE('',#195681,#12585);
#5519=LINE('',#195683,#12586);
#5520=LINE('',#195685,#12587);
#5521=LINE('',#195686,#12588);
#5522=LINE('',#195690,#12589);
#5523=LINE('',#195691,#12590);
#5524=LINE('',#195692,#12591);
#5525=LINE('',#195696,#12592);
#5526=LINE('',#195697,#12593);
#5527=LINE('',#195698,#12594);
#5528=LINE('',#195700,#12595);
#5529=LINE('',#195701,#12596);
#5530=LINE('',#195705,#12597);
#5531=LINE('',#195707,#12598);
#5532=LINE('',#195709,#12599);
#5533=LINE('',#195710,#12600);
#5534=LINE('',#195714,#12601);
#5535=LINE('',#195715,#12602);
#5536=LINE('',#195716,#12603);
#5537=LINE('',#195720,#12604);
#5538=LINE('',#195721,#12605);
#5539=LINE('',#195722,#12606);
#5540=LINE('',#195724,#12607);
#5541=LINE('',#195725,#12608);
#5542=LINE('',#195729,#12609);
#5543=LINE('',#195731,#12610);
#5544=LINE('',#195733,#12611);
#5545=LINE('',#195734,#12612);
#5546=LINE('',#195738,#12613);
#5547=LINE('',#195739,#12614);
#5548=LINE('',#195740,#12615);
#5549=LINE('',#195744,#12616);
#5550=LINE('',#195745,#12617);
#5551=LINE('',#195746,#12618);
#5552=LINE('',#195748,#12619);
#5553=LINE('',#195749,#12620);
#5554=LINE('',#195753,#12621);
#5555=LINE('',#195755,#12622);
#5556=LINE('',#195757,#12623);
#5557=LINE('',#195758,#12624);
#5558=LINE('',#195762,#12625);
#5559=LINE('',#195763,#12626);
#5560=LINE('',#195764,#12627);
#5561=LINE('',#195768,#12628);
#5562=LINE('',#195769,#12629);
#5563=LINE('',#195770,#12630);
#5564=LINE('',#195772,#12631);
#5565=LINE('',#195773,#12632);
#5566=LINE('',#195777,#12633);
#5567=LINE('',#195779,#12634);
#5568=LINE('',#195781,#12635);
#5569=LINE('',#195782,#12636);
#5570=LINE('',#195786,#12637);
#5571=LINE('',#195787,#12638);
#5572=LINE('',#195788,#12639);
#5573=LINE('',#195792,#12640);
#5574=LINE('',#195793,#12641);
#5575=LINE('',#195794,#12642);
#5576=LINE('',#195796,#12643);
#5577=LINE('',#195797,#12644);
#5578=LINE('',#195801,#12645);
#5579=LINE('',#195803,#12646);
#5580=LINE('',#195805,#12647);
#5581=LINE('',#195806,#12648);
#5582=LINE('',#195810,#12649);
#5583=LINE('',#195811,#12650);
#5584=LINE('',#195812,#12651);
#5585=LINE('',#195816,#12652);
#5586=LINE('',#195817,#12653);
#5587=LINE('',#195818,#12654);
#5588=LINE('',#195820,#12655);
#5589=LINE('',#195821,#12656);
#5590=LINE('',#195825,#12657);
#5591=LINE('',#195827,#12658);
#5592=LINE('',#195829,#12659);
#5593=LINE('',#195830,#12660);
#5594=LINE('',#195834,#12661);
#5595=LINE('',#195835,#12662);
#5596=LINE('',#195836,#12663);
#5597=LINE('',#195840,#12664);
#5598=LINE('',#195841,#12665);
#5599=LINE('',#195842,#12666);
#5600=LINE('',#195844,#12667);
#5601=LINE('',#195845,#12668);
#5602=LINE('',#195849,#12669);
#5603=LINE('',#195851,#12670);
#5604=LINE('',#195853,#12671);
#5605=LINE('',#195854,#12672);
#5606=LINE('',#195858,#12673);
#5607=LINE('',#195859,#12674);
#5608=LINE('',#195860,#12675);
#5609=LINE('',#195864,#12676);
#5610=LINE('',#195865,#12677);
#5611=LINE('',#195866,#12678);
#5612=LINE('',#195868,#12679);
#5613=LINE('',#195869,#12680);
#5614=LINE('',#195873,#12681);
#5615=LINE('',#195875,#12682);
#5616=LINE('',#195877,#12683);
#5617=LINE('',#195878,#12684);
#5618=LINE('',#195882,#12685);
#5619=LINE('',#195883,#12686);
#5620=LINE('',#195884,#12687);
#5621=LINE('',#195888,#12688);
#5622=LINE('',#195889,#12689);
#5623=LINE('',#195890,#12690);
#5624=LINE('',#195892,#12691);
#5625=LINE('',#195893,#12692);
#5626=LINE('',#195897,#12693);
#5627=LINE('',#195899,#12694);
#5628=LINE('',#195901,#12695);
#5629=LINE('',#195902,#12696);
#5630=LINE('',#195906,#12697);
#5631=LINE('',#195907,#12698);
#5632=LINE('',#195908,#12699);
#5633=LINE('',#195912,#12700);
#5634=LINE('',#195913,#12701);
#5635=LINE('',#195914,#12702);
#5636=LINE('',#195916,#12703);
#5637=LINE('',#195917,#12704);
#5638=LINE('',#195921,#12705);
#5639=LINE('',#195923,#12706);
#5640=LINE('',#195925,#12707);
#5641=LINE('',#195926,#12708);
#5642=LINE('',#195930,#12709);
#5643=LINE('',#195931,#12710);
#5644=LINE('',#195932,#12711);
#5645=LINE('',#195936,#12712);
#5646=LINE('',#195937,#12713);
#5647=LINE('',#195938,#12714);
#5648=LINE('',#195940,#12715);
#5649=LINE('',#195941,#12716);
#5650=LINE('',#195945,#12717);
#5651=LINE('',#195947,#12718);
#5652=LINE('',#195949,#12719);
#5653=LINE('',#195950,#12720);
#5654=LINE('',#195954,#12721);
#5655=LINE('',#195955,#12722);
#5656=LINE('',#195956,#12723);
#5657=LINE('',#195960,#12724);
#5658=LINE('',#195961,#12725);
#5659=LINE('',#195962,#12726);
#5660=LINE('',#195964,#12727);
#5661=LINE('',#195965,#12728);
#5662=LINE('',#195969,#12729);
#5663=LINE('',#195971,#12730);
#5664=LINE('',#195973,#12731);
#5665=LINE('',#195974,#12732);
#5666=LINE('',#195978,#12733);
#5667=LINE('',#195979,#12734);
#5668=LINE('',#195980,#12735);
#5669=LINE('',#195984,#12736);
#5670=LINE('',#195985,#12737);
#5671=LINE('',#195986,#12738);
#5672=LINE('',#195988,#12739);
#5673=LINE('',#195989,#12740);
#5674=LINE('',#195993,#12741);
#5675=LINE('',#195995,#12742);
#5676=LINE('',#195997,#12743);
#5677=LINE('',#195998,#12744);
#5678=LINE('',#196002,#12745);
#5679=LINE('',#196003,#12746);
#5680=LINE('',#196004,#12747);
#5681=LINE('',#196008,#12748);
#5682=LINE('',#196009,#12749);
#5683=LINE('',#196010,#12750);
#5684=LINE('',#196012,#12751);
#5685=LINE('',#196013,#12752);
#5686=LINE('',#196017,#12753);
#5687=LINE('',#196019,#12754);
#5688=LINE('',#196021,#12755);
#5689=LINE('',#196022,#12756);
#5690=LINE('',#196026,#12757);
#5691=LINE('',#196027,#12758);
#5692=LINE('',#196028,#12759);
#5693=LINE('',#196032,#12760);
#5694=LINE('',#196033,#12761);
#5695=LINE('',#196034,#12762);
#5696=LINE('',#196036,#12763);
#5697=LINE('',#196037,#12764);
#5698=LINE('',#196041,#12765);
#5699=LINE('',#196043,#12766);
#5700=LINE('',#196045,#12767);
#5701=LINE('',#196046,#12768);
#5702=LINE('',#196050,#12769);
#5703=LINE('',#196051,#12770);
#5704=LINE('',#196052,#12771);
#5705=LINE('',#196056,#12772);
#5706=LINE('',#196057,#12773);
#5707=LINE('',#196058,#12774);
#5708=LINE('',#196060,#12775);
#5709=LINE('',#196061,#12776);
#5710=LINE('',#196065,#12777);
#5711=LINE('',#196067,#12778);
#5712=LINE('',#196069,#12779);
#5713=LINE('',#196070,#12780);
#5714=LINE('',#196074,#12781);
#5715=LINE('',#196075,#12782);
#5716=LINE('',#196076,#12783);
#5717=LINE('',#196080,#12784);
#5718=LINE('',#196081,#12785);
#5719=LINE('',#196082,#12786);
#5720=LINE('',#196084,#12787);
#5721=LINE('',#196085,#12788);
#5722=LINE('',#196089,#12789);
#5723=LINE('',#196091,#12790);
#5724=LINE('',#196093,#12791);
#5725=LINE('',#196094,#12792);
#5726=LINE('',#196098,#12793);
#5727=LINE('',#196099,#12794);
#5728=LINE('',#196100,#12795);
#5729=LINE('',#196104,#12796);
#5730=LINE('',#196105,#12797);
#5731=LINE('',#196106,#12798);
#5732=LINE('',#196108,#12799);
#5733=LINE('',#196109,#12800);
#5734=LINE('',#196113,#12801);
#5735=LINE('',#196115,#12802);
#5736=LINE('',#196117,#12803);
#5737=LINE('',#196118,#12804);
#5738=LINE('',#196122,#12805);
#5739=LINE('',#196123,#12806);
#5740=LINE('',#196124,#12807);
#5741=LINE('',#196128,#12808);
#5742=LINE('',#196129,#12809);
#5743=LINE('',#196130,#12810);
#5744=LINE('',#196132,#12811);
#5745=LINE('',#196133,#12812);
#5746=LINE('',#196137,#12813);
#5747=LINE('',#196139,#12814);
#5748=LINE('',#196141,#12815);
#5749=LINE('',#196142,#12816);
#5750=LINE('',#196146,#12817);
#5751=LINE('',#196147,#12818);
#5752=LINE('',#196148,#12819);
#5753=LINE('',#196152,#12820);
#5754=LINE('',#196153,#12821);
#5755=LINE('',#196154,#12822);
#5756=LINE('',#196156,#12823);
#5757=LINE('',#196157,#12824);
#5758=LINE('',#196161,#12825);
#5759=LINE('',#196163,#12826);
#5760=LINE('',#196165,#12827);
#5761=LINE('',#196166,#12828);
#5762=LINE('',#196170,#12829);
#5763=LINE('',#196171,#12830);
#5764=LINE('',#196172,#12831);
#5765=LINE('',#196176,#12832);
#5766=LINE('',#196177,#12833);
#5767=LINE('',#196178,#12834);
#5768=LINE('',#196180,#12835);
#5769=LINE('',#196181,#12836);
#5770=LINE('',#196185,#12837);
#5771=LINE('',#196187,#12838);
#5772=LINE('',#196189,#12839);
#5773=LINE('',#196190,#12840);
#5774=LINE('',#196194,#12841);
#5775=LINE('',#196195,#12842);
#5776=LINE('',#196196,#12843);
#5777=LINE('',#196200,#12844);
#5778=LINE('',#196201,#12845);
#5779=LINE('',#196202,#12846);
#5780=LINE('',#196204,#12847);
#5781=LINE('',#196205,#12848);
#5782=LINE('',#196209,#12849);
#5783=LINE('',#196211,#12850);
#5784=LINE('',#196213,#12851);
#5785=LINE('',#196214,#12852);
#5786=LINE('',#196218,#12853);
#5787=LINE('',#196219,#12854);
#5788=LINE('',#196220,#12855);
#5789=LINE('',#196224,#12856);
#5790=LINE('',#196225,#12857);
#5791=LINE('',#196226,#12858);
#5792=LINE('',#196228,#12859);
#5793=LINE('',#196229,#12860);
#5794=LINE('',#196233,#12861);
#5795=LINE('',#196235,#12862);
#5796=LINE('',#196237,#12863);
#5797=LINE('',#196238,#12864);
#5798=LINE('',#196242,#12865);
#5799=LINE('',#196243,#12866);
#5800=LINE('',#196244,#12867);
#5801=LINE('',#196248,#12868);
#5802=LINE('',#196249,#12869);
#5803=LINE('',#196250,#12870);
#5804=LINE('',#196252,#12871);
#5805=LINE('',#196253,#12872);
#5806=LINE('',#196257,#12873);
#5807=LINE('',#196259,#12874);
#5808=LINE('',#196261,#12875);
#5809=LINE('',#196262,#12876);
#5810=LINE('',#196266,#12877);
#5811=LINE('',#196267,#12878);
#5812=LINE('',#196268,#12879);
#5813=LINE('',#196272,#12880);
#5814=LINE('',#196273,#12881);
#5815=LINE('',#196274,#12882);
#5816=LINE('',#196276,#12883);
#5817=LINE('',#196277,#12884);
#5818=LINE('',#196281,#12885);
#5819=LINE('',#196283,#12886);
#5820=LINE('',#196285,#12887);
#5821=LINE('',#196286,#12888);
#5822=LINE('',#196290,#12889);
#5823=LINE('',#196291,#12890);
#5824=LINE('',#196292,#12891);
#5825=LINE('',#196296,#12892);
#5826=LINE('',#196297,#12893);
#5827=LINE('',#196298,#12894);
#5828=LINE('',#196300,#12895);
#5829=LINE('',#196301,#12896);
#5830=LINE('',#196305,#12897);
#5831=LINE('',#196307,#12898);
#5832=LINE('',#196309,#12899);
#5833=LINE('',#196310,#12900);
#5834=LINE('',#196314,#12901);
#5835=LINE('',#196315,#12902);
#5836=LINE('',#196316,#12903);
#5837=LINE('',#196320,#12904);
#5838=LINE('',#196321,#12905);
#5839=LINE('',#196322,#12906);
#5840=LINE('',#196324,#12907);
#5841=LINE('',#196325,#12908);
#5842=LINE('',#196329,#12909);
#5843=LINE('',#196331,#12910);
#5844=LINE('',#196333,#12911);
#5845=LINE('',#196334,#12912);
#5846=LINE('',#196338,#12913);
#5847=LINE('',#196339,#12914);
#5848=LINE('',#196340,#12915);
#5849=LINE('',#196344,#12916);
#5850=LINE('',#196345,#12917);
#5851=LINE('',#196346,#12918);
#5852=LINE('',#196348,#12919);
#5853=LINE('',#196349,#12920);
#5854=LINE('',#196353,#12921);
#5855=LINE('',#196355,#12922);
#5856=LINE('',#196357,#12923);
#5857=LINE('',#196358,#12924);
#5858=LINE('',#196362,#12925);
#5859=LINE('',#196363,#12926);
#5860=LINE('',#196364,#12927);
#5861=LINE('',#196368,#12928);
#5862=LINE('',#196369,#12929);
#5863=LINE('',#196370,#12930);
#5864=LINE('',#196372,#12931);
#5865=LINE('',#196373,#12932);
#5866=LINE('',#196377,#12933);
#5867=LINE('',#196379,#12934);
#5868=LINE('',#196381,#12935);
#5869=LINE('',#196382,#12936);
#5870=LINE('',#196386,#12937);
#5871=LINE('',#196387,#12938);
#5872=LINE('',#196388,#12939);
#5873=LINE('',#196392,#12940);
#5874=LINE('',#196393,#12941);
#5875=LINE('',#196394,#12942);
#5876=LINE('',#196396,#12943);
#5877=LINE('',#196397,#12944);
#5878=LINE('',#196401,#12945);
#5879=LINE('',#196403,#12946);
#5880=LINE('',#196405,#12947);
#5881=LINE('',#196406,#12948);
#5882=LINE('',#196410,#12949);
#5883=LINE('',#196411,#12950);
#5884=LINE('',#196412,#12951);
#5885=LINE('',#196416,#12952);
#5886=LINE('',#196417,#12953);
#5887=LINE('',#196418,#12954);
#5888=LINE('',#196420,#12955);
#5889=LINE('',#196421,#12956);
#5890=LINE('',#196425,#12957);
#5891=LINE('',#196427,#12958);
#5892=LINE('',#196429,#12959);
#5893=LINE('',#196430,#12960);
#5894=LINE('',#196434,#12961);
#5895=LINE('',#196435,#12962);
#5896=LINE('',#196436,#12963);
#5897=LINE('',#196440,#12964);
#5898=LINE('',#196441,#12965);
#5899=LINE('',#196442,#12966);
#5900=LINE('',#196444,#12967);
#5901=LINE('',#196445,#12968);
#5902=LINE('',#196449,#12969);
#5903=LINE('',#196451,#12970);
#5904=LINE('',#196453,#12971);
#5905=LINE('',#196454,#12972);
#5906=LINE('',#196458,#12973);
#5907=LINE('',#196459,#12974);
#5908=LINE('',#196460,#12975);
#5909=LINE('',#196464,#12976);
#5910=LINE('',#196465,#12977);
#5911=LINE('',#196466,#12978);
#5912=LINE('',#196468,#12979);
#5913=LINE('',#196469,#12980);
#5914=LINE('',#196473,#12981);
#5915=LINE('',#196475,#12982);
#5916=LINE('',#196477,#12983);
#5917=LINE('',#196478,#12984);
#5918=LINE('',#196482,#12985);
#5919=LINE('',#196483,#12986);
#5920=LINE('',#196484,#12987);
#5921=LINE('',#196488,#12988);
#5922=LINE('',#196489,#12989);
#5923=LINE('',#196490,#12990);
#5924=LINE('',#196492,#12991);
#5925=LINE('',#196493,#12992);
#5926=LINE('',#196497,#12993);
#5927=LINE('',#196499,#12994);
#5928=LINE('',#196501,#12995);
#5929=LINE('',#196502,#12996);
#5930=LINE('',#196506,#12997);
#5931=LINE('',#196507,#12998);
#5932=LINE('',#196508,#12999);
#5933=LINE('',#196512,#13000);
#5934=LINE('',#196513,#13001);
#5935=LINE('',#196514,#13002);
#5936=LINE('',#196516,#13003);
#5937=LINE('',#196517,#13004);
#5938=LINE('',#196521,#13005);
#5939=LINE('',#196523,#13006);
#5940=LINE('',#196525,#13007);
#5941=LINE('',#196526,#13008);
#5942=LINE('',#196530,#13009);
#5943=LINE('',#196531,#13010);
#5944=LINE('',#196532,#13011);
#5945=LINE('',#196536,#13012);
#5946=LINE('',#196537,#13013);
#5947=LINE('',#196538,#13014);
#5948=LINE('',#196540,#13015);
#5949=LINE('',#196541,#13016);
#5950=LINE('',#196545,#13017);
#5951=LINE('',#196547,#13018);
#5952=LINE('',#196549,#13019);
#5953=LINE('',#196550,#13020);
#5954=LINE('',#196554,#13021);
#5955=LINE('',#196555,#13022);
#5956=LINE('',#196556,#13023);
#5957=LINE('',#196560,#13024);
#5958=LINE('',#196561,#13025);
#5959=LINE('',#196562,#13026);
#5960=LINE('',#196564,#13027);
#5961=LINE('',#196565,#13028);
#5962=LINE('',#196569,#13029);
#5963=LINE('',#196571,#13030);
#5964=LINE('',#196573,#13031);
#5965=LINE('',#196574,#13032);
#5966=LINE('',#196578,#13033);
#5967=LINE('',#196579,#13034);
#5968=LINE('',#196580,#13035);
#5969=LINE('',#196584,#13036);
#5970=LINE('',#196585,#13037);
#5971=LINE('',#196586,#13038);
#5972=LINE('',#196588,#13039);
#5973=LINE('',#196589,#13040);
#5974=LINE('',#196593,#13041);
#5975=LINE('',#196595,#13042);
#5976=LINE('',#196597,#13043);
#5977=LINE('',#196598,#13044);
#5978=LINE('',#196602,#13045);
#5979=LINE('',#196603,#13046);
#5980=LINE('',#196604,#13047);
#5981=LINE('',#196608,#13048);
#5982=LINE('',#196609,#13049);
#5983=LINE('',#196610,#13050);
#5984=LINE('',#196612,#13051);
#5985=LINE('',#196613,#13052);
#5986=LINE('',#196617,#13053);
#5987=LINE('',#196619,#13054);
#5988=LINE('',#196621,#13055);
#5989=LINE('',#196622,#13056);
#5990=LINE('',#196626,#13057);
#5991=LINE('',#196627,#13058);
#5992=LINE('',#196628,#13059);
#5993=LINE('',#196632,#13060);
#5994=LINE('',#196633,#13061);
#5995=LINE('',#196634,#13062);
#5996=LINE('',#196636,#13063);
#5997=LINE('',#196637,#13064);
#5998=LINE('',#196641,#13065);
#5999=LINE('',#196643,#13066);
#6000=LINE('',#196645,#13067);
#6001=LINE('',#196646,#13068);
#6002=LINE('',#196650,#13069);
#6003=LINE('',#196651,#13070);
#6004=LINE('',#196652,#13071);
#6005=LINE('',#196656,#13072);
#6006=LINE('',#196657,#13073);
#6007=LINE('',#196658,#13074);
#6008=LINE('',#196660,#13075);
#6009=LINE('',#196661,#13076);
#6010=LINE('',#196665,#13077);
#6011=LINE('',#196667,#13078);
#6012=LINE('',#196669,#13079);
#6013=LINE('',#196670,#13080);
#6014=LINE('',#196674,#13081);
#6015=LINE('',#196675,#13082);
#6016=LINE('',#196676,#13083);
#6017=LINE('',#196680,#13084);
#6018=LINE('',#196681,#13085);
#6019=LINE('',#196682,#13086);
#6020=LINE('',#196684,#13087);
#6021=LINE('',#196685,#13088);
#6022=LINE('',#196689,#13089);
#6023=LINE('',#196691,#13090);
#6024=LINE('',#196693,#13091);
#6025=LINE('',#196694,#13092);
#6026=LINE('',#196698,#13093);
#6027=LINE('',#196699,#13094);
#6028=LINE('',#196700,#13095);
#6029=LINE('',#196704,#13096);
#6030=LINE('',#196705,#13097);
#6031=LINE('',#196706,#13098);
#6032=LINE('',#196708,#13099);
#6033=LINE('',#196709,#13100);
#6034=LINE('',#196713,#13101);
#6035=LINE('',#196715,#13102);
#6036=LINE('',#196717,#13103);
#6037=LINE('',#196718,#13104);
#6038=LINE('',#196722,#13105);
#6039=LINE('',#196723,#13106);
#6040=LINE('',#196724,#13107);
#6041=LINE('',#196728,#13108);
#6042=LINE('',#196729,#13109);
#6043=LINE('',#196730,#13110);
#6044=LINE('',#196732,#13111);
#6045=LINE('',#196733,#13112);
#6046=LINE('',#196737,#13113);
#6047=LINE('',#196739,#13114);
#6048=LINE('',#196741,#13115);
#6049=LINE('',#196742,#13116);
#6050=LINE('',#196746,#13117);
#6051=LINE('',#196747,#13118);
#6052=LINE('',#196748,#13119);
#6053=LINE('',#196752,#13120);
#6054=LINE('',#196753,#13121);
#6055=LINE('',#196754,#13122);
#6056=LINE('',#196756,#13123);
#6057=LINE('',#196757,#13124);
#6058=LINE('',#196761,#13125);
#6059=LINE('',#196763,#13126);
#6060=LINE('',#196765,#13127);
#6061=LINE('',#196766,#13128);
#6062=LINE('',#196770,#13129);
#6063=LINE('',#196771,#13130);
#6064=LINE('',#196772,#13131);
#6065=LINE('',#196776,#13132);
#6066=LINE('',#196777,#13133);
#6067=LINE('',#196778,#13134);
#6068=LINE('',#196780,#13135);
#6069=LINE('',#196781,#13136);
#6070=LINE('',#196785,#13137);
#6071=LINE('',#196787,#13138);
#6072=LINE('',#196789,#13139);
#6073=LINE('',#196790,#13140);
#6074=LINE('',#196794,#13141);
#6075=LINE('',#196795,#13142);
#6076=LINE('',#196796,#13143);
#6077=LINE('',#196800,#13144);
#6078=LINE('',#196801,#13145);
#6079=LINE('',#196802,#13146);
#6080=LINE('',#196804,#13147);
#6081=LINE('',#196805,#13148);
#6082=LINE('',#196809,#13149);
#6083=LINE('',#196811,#13150);
#6084=LINE('',#196813,#13151);
#6085=LINE('',#196814,#13152);
#6086=LINE('',#196818,#13153);
#6087=LINE('',#196819,#13154);
#6088=LINE('',#196820,#13155);
#6089=LINE('',#196824,#13156);
#6090=LINE('',#196825,#13157);
#6091=LINE('',#196826,#13158);
#6092=LINE('',#196828,#13159);
#6093=LINE('',#196829,#13160);
#6094=LINE('',#196833,#13161);
#6095=LINE('',#196835,#13162);
#6096=LINE('',#196837,#13163);
#6097=LINE('',#196838,#13164);
#6098=LINE('',#196842,#13165);
#6099=LINE('',#196843,#13166);
#6100=LINE('',#196844,#13167);
#6101=LINE('',#196848,#13168);
#6102=LINE('',#196849,#13169);
#6103=LINE('',#196850,#13170);
#6104=LINE('',#196852,#13171);
#6105=LINE('',#196853,#13172);
#6106=LINE('',#196857,#13173);
#6107=LINE('',#196859,#13174);
#6108=LINE('',#196861,#13175);
#6109=LINE('',#196862,#13176);
#6110=LINE('',#196866,#13177);
#6111=LINE('',#196867,#13178);
#6112=LINE('',#196868,#13179);
#6113=LINE('',#196872,#13180);
#6114=LINE('',#196873,#13181);
#6115=LINE('',#196874,#13182);
#6116=LINE('',#196876,#13183);
#6117=LINE('',#196877,#13184);
#6118=LINE('',#196881,#13185);
#6119=LINE('',#196883,#13186);
#6120=LINE('',#196885,#13187);
#6121=LINE('',#196886,#13188);
#6122=LINE('',#196890,#13189);
#6123=LINE('',#196891,#13190);
#6124=LINE('',#196892,#13191);
#6125=LINE('',#196896,#13192);
#6126=LINE('',#196897,#13193);
#6127=LINE('',#196898,#13194);
#6128=LINE('',#196900,#13195);
#6129=LINE('',#196901,#13196);
#6130=LINE('',#196905,#13197);
#6131=LINE('',#196907,#13198);
#6132=LINE('',#196909,#13199);
#6133=LINE('',#196910,#13200);
#6134=LINE('',#196914,#13201);
#6135=LINE('',#196915,#13202);
#6136=LINE('',#196916,#13203);
#6137=LINE('',#196920,#13204);
#6138=LINE('',#196921,#13205);
#6139=LINE('',#196922,#13206);
#6140=LINE('',#196924,#13207);
#6141=LINE('',#196925,#13208);
#6142=LINE('',#196929,#13209);
#6143=LINE('',#196931,#13210);
#6144=LINE('',#196933,#13211);
#6145=LINE('',#196934,#13212);
#6146=LINE('',#196938,#13213);
#6147=LINE('',#196939,#13214);
#6148=LINE('',#196940,#13215);
#6149=LINE('',#196944,#13216);
#6150=LINE('',#196945,#13217);
#6151=LINE('',#196946,#13218);
#6152=LINE('',#196948,#13219);
#6153=LINE('',#196949,#13220);
#6154=LINE('',#196953,#13221);
#6155=LINE('',#196955,#13222);
#6156=LINE('',#196957,#13223);
#6157=LINE('',#196958,#13224);
#6158=LINE('',#196962,#13225);
#6159=LINE('',#196963,#13226);
#6160=LINE('',#196964,#13227);
#6161=LINE('',#196968,#13228);
#6162=LINE('',#196969,#13229);
#6163=LINE('',#196970,#13230);
#6164=LINE('',#196972,#13231);
#6165=LINE('',#196973,#13232);
#6166=LINE('',#196977,#13233);
#6167=LINE('',#196979,#13234);
#6168=LINE('',#196981,#13235);
#6169=LINE('',#196982,#13236);
#6170=LINE('',#196986,#13237);
#6171=LINE('',#196987,#13238);
#6172=LINE('',#196988,#13239);
#6173=LINE('',#196992,#13240);
#6174=LINE('',#196993,#13241);
#6175=LINE('',#196994,#13242);
#6176=LINE('',#196996,#13243);
#6177=LINE('',#196997,#13244);
#6178=LINE('',#197001,#13245);
#6179=LINE('',#197003,#13246);
#6180=LINE('',#197005,#13247);
#6181=LINE('',#197006,#13248);
#6182=LINE('',#197010,#13249);
#6183=LINE('',#197011,#13250);
#6184=LINE('',#197012,#13251);
#6185=LINE('',#197016,#13252);
#6186=LINE('',#197017,#13253);
#6187=LINE('',#197018,#13254);
#6188=LINE('',#197020,#13255);
#6189=LINE('',#197021,#13256);
#6190=LINE('',#197025,#13257);
#6191=LINE('',#197027,#13258);
#6192=LINE('',#197029,#13259);
#6193=LINE('',#197030,#13260);
#6194=LINE('',#197034,#13261);
#6195=LINE('',#197035,#13262);
#6196=LINE('',#197036,#13263);
#6197=LINE('',#197040,#13264);
#6198=LINE('',#197041,#13265);
#6199=LINE('',#197042,#13266);
#6200=LINE('',#197044,#13267);
#6201=LINE('',#197045,#13268);
#6202=LINE('',#197049,#13269);
#6203=LINE('',#197051,#13270);
#6204=LINE('',#197053,#13271);
#6205=LINE('',#197054,#13272);
#6206=LINE('',#197058,#13273);
#6207=LINE('',#197059,#13274);
#6208=LINE('',#197060,#13275);
#6209=LINE('',#197064,#13276);
#6210=LINE('',#197065,#13277);
#6211=LINE('',#197066,#13278);
#6212=LINE('',#197068,#13279);
#6213=LINE('',#197069,#13280);
#6214=LINE('',#197073,#13281);
#6215=LINE('',#197075,#13282);
#6216=LINE('',#197077,#13283);
#6217=LINE('',#197078,#13284);
#6218=LINE('',#197082,#13285);
#6219=LINE('',#197083,#13286);
#6220=LINE('',#197084,#13287);
#6221=LINE('',#197088,#13288);
#6222=LINE('',#197089,#13289);
#6223=LINE('',#197090,#13290);
#6224=LINE('',#197092,#13291);
#6225=LINE('',#197093,#13292);
#6226=LINE('',#197097,#13293);
#6227=LINE('',#197099,#13294);
#6228=LINE('',#197101,#13295);
#6229=LINE('',#197102,#13296);
#6230=LINE('',#197106,#13297);
#6231=LINE('',#197107,#13298);
#6232=LINE('',#197108,#13299);
#6233=LINE('',#197112,#13300);
#6234=LINE('',#197113,#13301);
#6235=LINE('',#197114,#13302);
#6236=LINE('',#197116,#13303);
#6237=LINE('',#197117,#13304);
#6238=LINE('',#197121,#13305);
#6239=LINE('',#197123,#13306);
#6240=LINE('',#197125,#13307);
#6241=LINE('',#197126,#13308);
#6242=LINE('',#197130,#13309);
#6243=LINE('',#197131,#13310);
#6244=LINE('',#197132,#13311);
#6245=LINE('',#197136,#13312);
#6246=LINE('',#197137,#13313);
#6247=LINE('',#197138,#13314);
#6248=LINE('',#197140,#13315);
#6249=LINE('',#197141,#13316);
#6250=LINE('',#197145,#13317);
#6251=LINE('',#197147,#13318);
#6252=LINE('',#197149,#13319);
#6253=LINE('',#197150,#13320);
#6254=LINE('',#197154,#13321);
#6255=LINE('',#197155,#13322);
#6256=LINE('',#197156,#13323);
#6257=LINE('',#197160,#13324);
#6258=LINE('',#197161,#13325);
#6259=LINE('',#197162,#13326);
#6260=LINE('',#197164,#13327);
#6261=LINE('',#197165,#13328);
#6262=LINE('',#197169,#13329);
#6263=LINE('',#197171,#13330);
#6264=LINE('',#197173,#13331);
#6265=LINE('',#197174,#13332);
#6266=LINE('',#197178,#13333);
#6267=LINE('',#197179,#13334);
#6268=LINE('',#197180,#13335);
#6269=LINE('',#197184,#13336);
#6270=LINE('',#197185,#13337);
#6271=LINE('',#197186,#13338);
#6272=LINE('',#197188,#13339);
#6273=LINE('',#197189,#13340);
#6274=LINE('',#197193,#13341);
#6275=LINE('',#197195,#13342);
#6276=LINE('',#197197,#13343);
#6277=LINE('',#197198,#13344);
#6278=LINE('',#197202,#13345);
#6279=LINE('',#197203,#13346);
#6280=LINE('',#197204,#13347);
#6281=LINE('',#197208,#13348);
#6282=LINE('',#197209,#13349);
#6283=LINE('',#197210,#13350);
#6284=LINE('',#197212,#13351);
#6285=LINE('',#197213,#13352);
#6286=LINE('',#197217,#13353);
#6287=LINE('',#197219,#13354);
#6288=LINE('',#197221,#13355);
#6289=LINE('',#197222,#13356);
#6290=LINE('',#197226,#13357);
#6291=LINE('',#197227,#13358);
#6292=LINE('',#197228,#13359);
#6293=LINE('',#197232,#13360);
#6294=LINE('',#197233,#13361);
#6295=LINE('',#197234,#13362);
#6296=LINE('',#197236,#13363);
#6297=LINE('',#197237,#13364);
#6298=LINE('',#197241,#13365);
#6299=LINE('',#197243,#13366);
#6300=LINE('',#197245,#13367);
#6301=LINE('',#197246,#13368);
#6302=LINE('',#197250,#13369);
#6303=LINE('',#197251,#13370);
#6304=LINE('',#197252,#13371);
#6305=LINE('',#197256,#13372);
#6306=LINE('',#197257,#13373);
#6307=LINE('',#197258,#13374);
#6308=LINE('',#197260,#13375);
#6309=LINE('',#197261,#13376);
#6310=LINE('',#197265,#13377);
#6311=LINE('',#197267,#13378);
#6312=LINE('',#197269,#13379);
#6313=LINE('',#197270,#13380);
#6314=LINE('',#197274,#13381);
#6315=LINE('',#197275,#13382);
#6316=LINE('',#197276,#13383);
#6317=LINE('',#197280,#13384);
#6318=LINE('',#197281,#13385);
#6319=LINE('',#197282,#13386);
#6320=LINE('',#197284,#13387);
#6321=LINE('',#197285,#13388);
#6322=LINE('',#197289,#13389);
#6323=LINE('',#197291,#13390);
#6324=LINE('',#197293,#13391);
#6325=LINE('',#197294,#13392);
#6326=LINE('',#197298,#13393);
#6327=LINE('',#197299,#13394);
#6328=LINE('',#197300,#13395);
#6329=LINE('',#197304,#13396);
#6330=LINE('',#197305,#13397);
#6331=LINE('',#197306,#13398);
#6332=LINE('',#197308,#13399);
#6333=LINE('',#197309,#13400);
#6334=LINE('',#197313,#13401);
#6335=LINE('',#197315,#13402);
#6336=LINE('',#197317,#13403);
#6337=LINE('',#197318,#13404);
#6338=LINE('',#197322,#13405);
#6339=LINE('',#197323,#13406);
#6340=LINE('',#197324,#13407);
#6341=LINE('',#197328,#13408);
#6342=LINE('',#197329,#13409);
#6343=LINE('',#197330,#13410);
#6344=LINE('',#197332,#13411);
#6345=LINE('',#197333,#13412);
#6346=LINE('',#197337,#13413);
#6347=LINE('',#197339,#13414);
#6348=LINE('',#197341,#13415);
#6349=LINE('',#197342,#13416);
#6350=LINE('',#197346,#13417);
#6351=LINE('',#197347,#13418);
#6352=LINE('',#197348,#13419);
#6353=LINE('',#197352,#13420);
#6354=LINE('',#197353,#13421);
#6355=LINE('',#197354,#13422);
#6356=LINE('',#197356,#13423);
#6357=LINE('',#197357,#13424);
#6358=LINE('',#197361,#13425);
#6359=LINE('',#197363,#13426);
#6360=LINE('',#197365,#13427);
#6361=LINE('',#197366,#13428);
#6362=LINE('',#197370,#13429);
#6363=LINE('',#197371,#13430);
#6364=LINE('',#197372,#13431);
#6365=LINE('',#197376,#13432);
#6366=LINE('',#197377,#13433);
#6367=LINE('',#197378,#13434);
#6368=LINE('',#197380,#13435);
#6369=LINE('',#197381,#13436);
#6370=LINE('',#197385,#13437);
#6371=LINE('',#197387,#13438);
#6372=LINE('',#197389,#13439);
#6373=LINE('',#197390,#13440);
#6374=LINE('',#197394,#13441);
#6375=LINE('',#197395,#13442);
#6376=LINE('',#197396,#13443);
#6377=LINE('',#197400,#13444);
#6378=LINE('',#197401,#13445);
#6379=LINE('',#197402,#13446);
#6380=LINE('',#197404,#13447);
#6381=LINE('',#197405,#13448);
#6382=LINE('',#197409,#13449);
#6383=LINE('',#197411,#13450);
#6384=LINE('',#197413,#13451);
#6385=LINE('',#197414,#13452);
#6386=LINE('',#197418,#13453);
#6387=LINE('',#197419,#13454);
#6388=LINE('',#197420,#13455);
#6389=LINE('',#197424,#13456);
#6390=LINE('',#197425,#13457);
#6391=LINE('',#197426,#13458);
#6392=LINE('',#197428,#13459);
#6393=LINE('',#197429,#13460);
#6394=LINE('',#197433,#13461);
#6395=LINE('',#197435,#13462);
#6396=LINE('',#197437,#13463);
#6397=LINE('',#197438,#13464);
#6398=LINE('',#197442,#13465);
#6399=LINE('',#197443,#13466);
#6400=LINE('',#197444,#13467);
#6401=LINE('',#197448,#13468);
#6402=LINE('',#197449,#13469);
#6403=LINE('',#197450,#13470);
#6404=LINE('',#197452,#13471);
#6405=LINE('',#197453,#13472);
#6406=LINE('',#197457,#13473);
#6407=LINE('',#197459,#13474);
#6408=LINE('',#197461,#13475);
#6409=LINE('',#197462,#13476);
#6410=LINE('',#197466,#13477);
#6411=LINE('',#197467,#13478);
#6412=LINE('',#197468,#13479);
#6413=LINE('',#197472,#13480);
#6414=LINE('',#197473,#13481);
#6415=LINE('',#197474,#13482);
#6416=LINE('',#197476,#13483);
#6417=LINE('',#197477,#13484);
#6418=LINE('',#197481,#13485);
#6419=LINE('',#197483,#13486);
#6420=LINE('',#197485,#13487);
#6421=LINE('',#197486,#13488);
#6422=LINE('',#197490,#13489);
#6423=LINE('',#197491,#13490);
#6424=LINE('',#197492,#13491);
#6425=LINE('',#197496,#13492);
#6426=LINE('',#197497,#13493);
#6427=LINE('',#197498,#13494);
#6428=LINE('',#197500,#13495);
#6429=LINE('',#197501,#13496);
#6430=LINE('',#197505,#13497);
#6431=LINE('',#197507,#13498);
#6432=LINE('',#197509,#13499);
#6433=LINE('',#197510,#13500);
#6434=LINE('',#197514,#13501);
#6435=LINE('',#197515,#13502);
#6436=LINE('',#197516,#13503);
#6437=LINE('',#197520,#13504);
#6438=LINE('',#197521,#13505);
#6439=LINE('',#197522,#13506);
#6440=LINE('',#197524,#13507);
#6441=LINE('',#197525,#13508);
#6442=LINE('',#197529,#13509);
#6443=LINE('',#197531,#13510);
#6444=LINE('',#197533,#13511);
#6445=LINE('',#197534,#13512);
#6446=LINE('',#197538,#13513);
#6447=LINE('',#197539,#13514);
#6448=LINE('',#197540,#13515);
#6449=LINE('',#197544,#13516);
#6450=LINE('',#197545,#13517);
#6451=LINE('',#197546,#13518);
#6452=LINE('',#197548,#13519);
#6453=LINE('',#197549,#13520);
#6454=LINE('',#197553,#13521);
#6455=LINE('',#197555,#13522);
#6456=LINE('',#197557,#13523);
#6457=LINE('',#197558,#13524);
#6458=LINE('',#197562,#13525);
#6459=LINE('',#197563,#13526);
#6460=LINE('',#197564,#13527);
#6461=LINE('',#197568,#13528);
#6462=LINE('',#197569,#13529);
#6463=LINE('',#197570,#13530);
#6464=LINE('',#197572,#13531);
#6465=LINE('',#197573,#13532);
#6466=LINE('',#197577,#13533);
#6467=LINE('',#197579,#13534);
#6468=LINE('',#197581,#13535);
#6469=LINE('',#197582,#13536);
#6470=LINE('',#197586,#13537);
#6471=LINE('',#197587,#13538);
#6472=LINE('',#197588,#13539);
#6473=LINE('',#197592,#13540);
#6474=LINE('',#197593,#13541);
#6475=LINE('',#197594,#13542);
#6476=LINE('',#197596,#13543);
#6477=LINE('',#197597,#13544);
#6478=LINE('',#197601,#13545);
#6479=LINE('',#197603,#13546);
#6480=LINE('',#197605,#13547);
#6481=LINE('',#197606,#13548);
#6482=LINE('',#197610,#13549);
#6483=LINE('',#197611,#13550);
#6484=LINE('',#197612,#13551);
#6485=LINE('',#197616,#13552);
#6486=LINE('',#197617,#13553);
#6487=LINE('',#197618,#13554);
#6488=LINE('',#197620,#13555);
#6489=LINE('',#197621,#13556);
#6490=LINE('',#197625,#13557);
#6491=LINE('',#197627,#13558);
#6492=LINE('',#197629,#13559);
#6493=LINE('',#197630,#13560);
#6494=LINE('',#197634,#13561);
#6495=LINE('',#197635,#13562);
#6496=LINE('',#197636,#13563);
#6497=LINE('',#197640,#13564);
#6498=LINE('',#197641,#13565);
#6499=LINE('',#197642,#13566);
#6500=LINE('',#197644,#13567);
#6501=LINE('',#197645,#13568);
#6502=LINE('',#197649,#13569);
#6503=LINE('',#197651,#13570);
#6504=LINE('',#197653,#13571);
#6505=LINE('',#197654,#13572);
#6506=LINE('',#197658,#13573);
#6507=LINE('',#197659,#13574);
#6508=LINE('',#197660,#13575);
#6509=LINE('',#197664,#13576);
#6510=LINE('',#197665,#13577);
#6511=LINE('',#197666,#13578);
#6512=LINE('',#197668,#13579);
#6513=LINE('',#197669,#13580);
#6514=LINE('',#197673,#13581);
#6515=LINE('',#197675,#13582);
#6516=LINE('',#197677,#13583);
#6517=LINE('',#197678,#13584);
#6518=LINE('',#197682,#13585);
#6519=LINE('',#197683,#13586);
#6520=LINE('',#197684,#13587);
#6521=LINE('',#197688,#13588);
#6522=LINE('',#197689,#13589);
#6523=LINE('',#197690,#13590);
#6524=LINE('',#197692,#13591);
#6525=LINE('',#197693,#13592);
#6526=LINE('',#197697,#13593);
#6527=LINE('',#197699,#13594);
#6528=LINE('',#197701,#13595);
#6529=LINE('',#197702,#13596);
#6530=LINE('',#197706,#13597);
#6531=LINE('',#197707,#13598);
#6532=LINE('',#197708,#13599);
#6533=LINE('',#197712,#13600);
#6534=LINE('',#197713,#13601);
#6535=LINE('',#197714,#13602);
#6536=LINE('',#197716,#13603);
#6537=LINE('',#197717,#13604);
#6538=LINE('',#197721,#13605);
#6539=LINE('',#197723,#13606);
#6540=LINE('',#197725,#13607);
#6541=LINE('',#197726,#13608);
#6542=LINE('',#197730,#13609);
#6543=LINE('',#197731,#13610);
#6544=LINE('',#197732,#13611);
#6545=LINE('',#197736,#13612);
#6546=LINE('',#197737,#13613);
#6547=LINE('',#197738,#13614);
#6548=LINE('',#197740,#13615);
#6549=LINE('',#197741,#13616);
#6550=LINE('',#197745,#13617);
#6551=LINE('',#197747,#13618);
#6552=LINE('',#197749,#13619);
#6553=LINE('',#197750,#13620);
#6554=LINE('',#197754,#13621);
#6555=LINE('',#197755,#13622);
#6556=LINE('',#197756,#13623);
#6557=LINE('',#197760,#13624);
#6558=LINE('',#197761,#13625);
#6559=LINE('',#197762,#13626);
#6560=LINE('',#197764,#13627);
#6561=LINE('',#197765,#13628);
#6562=LINE('',#197769,#13629);
#6563=LINE('',#197771,#13630);
#6564=LINE('',#197773,#13631);
#6565=LINE('',#197774,#13632);
#6566=LINE('',#197778,#13633);
#6567=LINE('',#197779,#13634);
#6568=LINE('',#197780,#13635);
#6569=LINE('',#197784,#13636);
#6570=LINE('',#197785,#13637);
#6571=LINE('',#197786,#13638);
#6572=LINE('',#197788,#13639);
#6573=LINE('',#197789,#13640);
#6574=LINE('',#197793,#13641);
#6575=LINE('',#197795,#13642);
#6576=LINE('',#197797,#13643);
#6577=LINE('',#197798,#13644);
#6578=LINE('',#197802,#13645);
#6579=LINE('',#197803,#13646);
#6580=LINE('',#197804,#13647);
#6581=LINE('',#197808,#13648);
#6582=LINE('',#197809,#13649);
#6583=LINE('',#197810,#13650);
#6584=LINE('',#197812,#13651);
#6585=LINE('',#197813,#13652);
#6586=LINE('',#197817,#13653);
#6587=LINE('',#197819,#13654);
#6588=LINE('',#197821,#13655);
#6589=LINE('',#197822,#13656);
#6590=LINE('',#197826,#13657);
#6591=LINE('',#197827,#13658);
#6592=LINE('',#197828,#13659);
#6593=LINE('',#197832,#13660);
#6594=LINE('',#197833,#13661);
#6595=LINE('',#197834,#13662);
#6596=LINE('',#197836,#13663);
#6597=LINE('',#197837,#13664);
#6598=LINE('',#197841,#13665);
#6599=LINE('',#197843,#13666);
#6600=LINE('',#197845,#13667);
#6601=LINE('',#197846,#13668);
#6602=LINE('',#197850,#13669);
#6603=LINE('',#197851,#13670);
#6604=LINE('',#197852,#13671);
#6605=LINE('',#197856,#13672);
#6606=LINE('',#197857,#13673);
#6607=LINE('',#197858,#13674);
#6608=LINE('',#197860,#13675);
#6609=LINE('',#197861,#13676);
#6610=LINE('',#197865,#13677);
#6611=LINE('',#197867,#13678);
#6612=LINE('',#197869,#13679);
#6613=LINE('',#197870,#13680);
#6614=LINE('',#197874,#13681);
#6615=LINE('',#197875,#13682);
#6616=LINE('',#197876,#13683);
#6617=LINE('',#197880,#13684);
#6618=LINE('',#197881,#13685);
#6619=LINE('',#197882,#13686);
#6620=LINE('',#197884,#13687);
#6621=LINE('',#197885,#13688);
#6622=LINE('',#197889,#13689);
#6623=LINE('',#197891,#13690);
#6624=LINE('',#197893,#13691);
#6625=LINE('',#197894,#13692);
#6626=LINE('',#197898,#13693);
#6627=LINE('',#197899,#13694);
#6628=LINE('',#197900,#13695);
#6629=LINE('',#197904,#13696);
#6630=LINE('',#197905,#13697);
#6631=LINE('',#197906,#13698);
#6632=LINE('',#197908,#13699);
#6633=LINE('',#197909,#13700);
#6634=LINE('',#197913,#13701);
#6635=LINE('',#197915,#13702);
#6636=LINE('',#197917,#13703);
#6637=LINE('',#197918,#13704);
#6638=LINE('',#197922,#13705);
#6639=LINE('',#197923,#13706);
#6640=LINE('',#197924,#13707);
#6641=LINE('',#197928,#13708);
#6642=LINE('',#197929,#13709);
#6643=LINE('',#197930,#13710);
#6644=LINE('',#197932,#13711);
#6645=LINE('',#197933,#13712);
#6646=LINE('',#197937,#13713);
#6647=LINE('',#197939,#13714);
#6648=LINE('',#197941,#13715);
#6649=LINE('',#197942,#13716);
#6650=LINE('',#197946,#13717);
#6651=LINE('',#197947,#13718);
#6652=LINE('',#197948,#13719);
#6653=LINE('',#197952,#13720);
#6654=LINE('',#197953,#13721);
#6655=LINE('',#197954,#13722);
#6656=LINE('',#197956,#13723);
#6657=LINE('',#197957,#13724);
#6658=LINE('',#197961,#13725);
#6659=LINE('',#197963,#13726);
#6660=LINE('',#197965,#13727);
#6661=LINE('',#197966,#13728);
#6662=LINE('',#197970,#13729);
#6663=LINE('',#197971,#13730);
#6664=LINE('',#197972,#13731);
#6665=LINE('',#197976,#13732);
#6666=LINE('',#197977,#13733);
#6667=LINE('',#197978,#13734);
#6668=LINE('',#197980,#13735);
#6669=LINE('',#197981,#13736);
#6670=LINE('',#197985,#13737);
#6671=LINE('',#197987,#13738);
#6672=LINE('',#197989,#13739);
#6673=LINE('',#197990,#13740);
#6674=LINE('',#197994,#13741);
#6675=LINE('',#197995,#13742);
#6676=LINE('',#197996,#13743);
#6677=LINE('',#198000,#13744);
#6678=LINE('',#198001,#13745);
#6679=LINE('',#198002,#13746);
#6680=LINE('',#198004,#13747);
#6681=LINE('',#198005,#13748);
#6682=LINE('',#198009,#13749);
#6683=LINE('',#198011,#13750);
#6684=LINE('',#198013,#13751);
#6685=LINE('',#198014,#13752);
#6686=LINE('',#198018,#13753);
#6687=LINE('',#198019,#13754);
#6688=LINE('',#198020,#13755);
#6689=LINE('',#198024,#13756);
#6690=LINE('',#198025,#13757);
#6691=LINE('',#198026,#13758);
#6692=LINE('',#198028,#13759);
#6693=LINE('',#198029,#13760);
#6694=LINE('',#198033,#13761);
#6695=LINE('',#198035,#13762);
#6696=LINE('',#198037,#13763);
#6697=LINE('',#198038,#13764);
#6698=LINE('',#198042,#13765);
#6699=LINE('',#198043,#13766);
#6700=LINE('',#198044,#13767);
#6701=LINE('',#198048,#13768);
#6702=LINE('',#198049,#13769);
#6703=LINE('',#198050,#13770);
#6704=LINE('',#198052,#13771);
#6705=LINE('',#198053,#13772);
#6706=LINE('',#198057,#13773);
#6707=LINE('',#198059,#13774);
#6708=LINE('',#198061,#13775);
#6709=LINE('',#198062,#13776);
#6710=LINE('',#198066,#13777);
#6711=LINE('',#198067,#13778);
#6712=LINE('',#198068,#13779);
#6713=LINE('',#198072,#13780);
#6714=LINE('',#198073,#13781);
#6715=LINE('',#198074,#13782);
#6716=LINE('',#198076,#13783);
#6717=LINE('',#198077,#13784);
#6718=LINE('',#198081,#13785);
#6719=LINE('',#198083,#13786);
#6720=LINE('',#198085,#13787);
#6721=LINE('',#198086,#13788);
#6722=LINE('',#198090,#13789);
#6723=LINE('',#198091,#13790);
#6724=LINE('',#198092,#13791);
#6725=LINE('',#198096,#13792);
#6726=LINE('',#198097,#13793);
#6727=LINE('',#198098,#13794);
#6728=LINE('',#198100,#13795);
#6729=LINE('',#198101,#13796);
#6730=LINE('',#198105,#13797);
#6731=LINE('',#198107,#13798);
#6732=LINE('',#198109,#13799);
#6733=LINE('',#198110,#13800);
#6734=LINE('',#198114,#13801);
#6735=LINE('',#198115,#13802);
#6736=LINE('',#198116,#13803);
#6737=LINE('',#198120,#13804);
#6738=LINE('',#198121,#13805);
#6739=LINE('',#198122,#13806);
#6740=LINE('',#198124,#13807);
#6741=LINE('',#198125,#13808);
#6742=LINE('',#198129,#13809);
#6743=LINE('',#198131,#13810);
#6744=LINE('',#198133,#13811);
#6745=LINE('',#198134,#13812);
#6746=LINE('',#198138,#13813);
#6747=LINE('',#198139,#13814);
#6748=LINE('',#198140,#13815);
#6749=LINE('',#198144,#13816);
#6750=LINE('',#198145,#13817);
#6751=LINE('',#198146,#13818);
#6752=LINE('',#198148,#13819);
#6753=LINE('',#198149,#13820);
#6754=LINE('',#198153,#13821);
#6755=LINE('',#198155,#13822);
#6756=LINE('',#198157,#13823);
#6757=LINE('',#198158,#13824);
#6758=LINE('',#198162,#13825);
#6759=LINE('',#198163,#13826);
#6760=LINE('',#198164,#13827);
#6761=LINE('',#198168,#13828);
#6762=LINE('',#198169,#13829);
#6763=LINE('',#198170,#13830);
#6764=LINE('',#198172,#13831);
#6765=LINE('',#198173,#13832);
#6766=LINE('',#198177,#13833);
#6767=LINE('',#198179,#13834);
#6768=LINE('',#198181,#13835);
#6769=LINE('',#198182,#13836);
#6770=LINE('',#198186,#13837);
#6771=LINE('',#198187,#13838);
#6772=LINE('',#198188,#13839);
#6773=LINE('',#198192,#13840);
#6774=LINE('',#198193,#13841);
#6775=LINE('',#198194,#13842);
#6776=LINE('',#198196,#13843);
#6777=LINE('',#198197,#13844);
#6778=LINE('',#198201,#13845);
#6779=LINE('',#198203,#13846);
#6780=LINE('',#198205,#13847);
#6781=LINE('',#198206,#13848);
#6782=LINE('',#198210,#13849);
#6783=LINE('',#198211,#13850);
#6784=LINE('',#198212,#13851);
#6785=LINE('',#198216,#13852);
#6786=LINE('',#198217,#13853);
#6787=LINE('',#198218,#13854);
#6788=LINE('',#198220,#13855);
#6789=LINE('',#198221,#13856);
#6790=LINE('',#198225,#13857);
#6791=LINE('',#198227,#13858);
#6792=LINE('',#198229,#13859);
#6793=LINE('',#198230,#13860);
#6794=LINE('',#198234,#13861);
#6795=LINE('',#198235,#13862);
#6796=LINE('',#198236,#13863);
#6797=LINE('',#198240,#13864);
#6798=LINE('',#198241,#13865);
#6799=LINE('',#198242,#13866);
#6800=LINE('',#198244,#13867);
#6801=LINE('',#198245,#13868);
#6802=LINE('',#198249,#13869);
#6803=LINE('',#198251,#13870);
#6804=LINE('',#198253,#13871);
#6805=LINE('',#198254,#13872);
#6806=LINE('',#198258,#13873);
#6807=LINE('',#198259,#13874);
#6808=LINE('',#198260,#13875);
#6809=LINE('',#198264,#13876);
#6810=LINE('',#198265,#13877);
#6811=LINE('',#198266,#13878);
#6812=LINE('',#198268,#13879);
#6813=LINE('',#198269,#13880);
#6814=LINE('',#198273,#13881);
#6815=LINE('',#198275,#13882);
#6816=LINE('',#198277,#13883);
#6817=LINE('',#198278,#13884);
#6818=LINE('',#198282,#13885);
#6819=LINE('',#198283,#13886);
#6820=LINE('',#198284,#13887);
#6821=LINE('',#198288,#13888);
#6822=LINE('',#198289,#13889);
#6823=LINE('',#198290,#13890);
#6824=LINE('',#198292,#13891);
#6825=LINE('',#198293,#13892);
#6826=LINE('',#198297,#13893);
#6827=LINE('',#198299,#13894);
#6828=LINE('',#198301,#13895);
#6829=LINE('',#198302,#13896);
#6830=LINE('',#198306,#13897);
#6831=LINE('',#198307,#13898);
#6832=LINE('',#198308,#13899);
#6833=LINE('',#198312,#13900);
#6834=LINE('',#198313,#13901);
#6835=LINE('',#198314,#13902);
#6836=LINE('',#198316,#13903);
#6837=LINE('',#198317,#13904);
#6838=LINE('',#198321,#13905);
#6839=LINE('',#198323,#13906);
#6840=LINE('',#198325,#13907);
#6841=LINE('',#198326,#13908);
#6842=LINE('',#198330,#13909);
#6843=LINE('',#198331,#13910);
#6844=LINE('',#198332,#13911);
#6845=LINE('',#198336,#13912);
#6846=LINE('',#198337,#13913);
#6847=LINE('',#198338,#13914);
#6848=LINE('',#198340,#13915);
#6849=LINE('',#198341,#13916);
#6850=LINE('',#198345,#13917);
#6851=LINE('',#198347,#13918);
#6852=LINE('',#198349,#13919);
#6853=LINE('',#198350,#13920);
#6854=LINE('',#198354,#13921);
#6855=LINE('',#198355,#13922);
#6856=LINE('',#198356,#13923);
#6857=LINE('',#198360,#13924);
#6858=LINE('',#198361,#13925);
#6859=LINE('',#198362,#13926);
#6860=LINE('',#198364,#13927);
#6861=LINE('',#198365,#13928);
#6862=LINE('',#198369,#13929);
#6863=LINE('',#198371,#13930);
#6864=LINE('',#198373,#13931);
#6865=LINE('',#198374,#13932);
#6866=LINE('',#198378,#13933);
#6867=LINE('',#198379,#13934);
#6868=LINE('',#198380,#13935);
#6869=LINE('',#198384,#13936);
#6870=LINE('',#198385,#13937);
#6871=LINE('',#198386,#13938);
#6872=LINE('',#198388,#13939);
#6873=LINE('',#198389,#13940);
#6874=LINE('',#198393,#13941);
#6875=LINE('',#198395,#13942);
#6876=LINE('',#198397,#13943);
#6877=LINE('',#198398,#13944);
#6878=LINE('',#198402,#13945);
#6879=LINE('',#198403,#13946);
#6880=LINE('',#198404,#13947);
#6881=LINE('',#198408,#13948);
#6882=LINE('',#198409,#13949);
#6883=LINE('',#198410,#13950);
#6884=LINE('',#198412,#13951);
#6885=LINE('',#198413,#13952);
#6886=LINE('',#198417,#13953);
#6887=LINE('',#198419,#13954);
#6888=LINE('',#198421,#13955);
#6889=LINE('',#198422,#13956);
#6890=LINE('',#198426,#13957);
#6891=LINE('',#198427,#13958);
#6892=LINE('',#198428,#13959);
#6893=LINE('',#198432,#13960);
#6894=LINE('',#198433,#13961);
#6895=LINE('',#198434,#13962);
#6896=LINE('',#198436,#13963);
#6897=LINE('',#198437,#13964);
#6898=LINE('',#198441,#13965);
#6899=LINE('',#198443,#13966);
#6900=LINE('',#198445,#13967);
#6901=LINE('',#198446,#13968);
#6902=LINE('',#198450,#13969);
#6903=LINE('',#198451,#13970);
#6904=LINE('',#198452,#13971);
#6905=LINE('',#198456,#13972);
#6906=LINE('',#198457,#13973);
#6907=LINE('',#198458,#13974);
#6908=LINE('',#198460,#13975);
#6909=LINE('',#198461,#13976);
#6910=LINE('',#198465,#13977);
#6911=LINE('',#198467,#13978);
#6912=LINE('',#198469,#13979);
#6913=LINE('',#198470,#13980);
#6914=LINE('',#198474,#13981);
#6915=LINE('',#198475,#13982);
#6916=LINE('',#198476,#13983);
#6917=LINE('',#198480,#13984);
#6918=LINE('',#198481,#13985);
#6919=LINE('',#198482,#13986);
#6920=LINE('',#198484,#13987);
#6921=LINE('',#198485,#13988);
#6922=LINE('',#198489,#13989);
#6923=LINE('',#198491,#13990);
#6924=LINE('',#198493,#13991);
#6925=LINE('',#198494,#13992);
#6926=LINE('',#198498,#13993);
#6927=LINE('',#198499,#13994);
#6928=LINE('',#198500,#13995);
#6929=LINE('',#198504,#13996);
#6930=LINE('',#198505,#13997);
#6931=LINE('',#198506,#13998);
#6932=LINE('',#198508,#13999);
#6933=LINE('',#198509,#14000);
#6934=LINE('',#198513,#14001);
#6935=LINE('',#198515,#14002);
#6936=LINE('',#198517,#14003);
#6937=LINE('',#198518,#14004);
#6938=LINE('',#198522,#14005);
#6939=LINE('',#198523,#14006);
#6940=LINE('',#198524,#14007);
#6941=LINE('',#198528,#14008);
#6942=LINE('',#198529,#14009);
#6943=LINE('',#198530,#14010);
#6944=LINE('',#198532,#14011);
#6945=LINE('',#198533,#14012);
#6946=LINE('',#198537,#14013);
#6947=LINE('',#198539,#14014);
#6948=LINE('',#198541,#14015);
#6949=LINE('',#198542,#14016);
#6950=LINE('',#198546,#14017);
#6951=LINE('',#198547,#14018);
#6952=LINE('',#198548,#14019);
#6953=LINE('',#198552,#14020);
#6954=LINE('',#198553,#14021);
#6955=LINE('',#198554,#14022);
#6956=LINE('',#198556,#14023);
#6957=LINE('',#198557,#14024);
#6958=LINE('',#198561,#14025);
#6959=LINE('',#198563,#14026);
#6960=LINE('',#198565,#14027);
#6961=LINE('',#198566,#14028);
#6962=LINE('',#198570,#14029);
#6963=LINE('',#198571,#14030);
#6964=LINE('',#198572,#14031);
#6965=LINE('',#198576,#14032);
#6966=LINE('',#198577,#14033);
#6967=LINE('',#198578,#14034);
#6968=LINE('',#198580,#14035);
#6969=LINE('',#198581,#14036);
#6970=LINE('',#198585,#14037);
#6971=LINE('',#198587,#14038);
#6972=LINE('',#198589,#14039);
#6973=LINE('',#198590,#14040);
#6974=LINE('',#198594,#14041);
#6975=LINE('',#198595,#14042);
#6976=LINE('',#198596,#14043);
#6977=LINE('',#198600,#14044);
#6978=LINE('',#198601,#14045);
#6979=LINE('',#198602,#14046);
#6980=LINE('',#198604,#14047);
#6981=LINE('',#198605,#14048);
#6982=LINE('',#198609,#14049);
#6983=LINE('',#198611,#14050);
#6984=LINE('',#198613,#14051);
#6985=LINE('',#198614,#14052);
#6986=LINE('',#198618,#14053);
#6987=LINE('',#198619,#14054);
#6988=LINE('',#198620,#14055);
#6989=LINE('',#198624,#14056);
#6990=LINE('',#198625,#14057);
#6991=LINE('',#198626,#14058);
#6992=LINE('',#198628,#14059);
#6993=LINE('',#198629,#14060);
#6994=LINE('',#198633,#14061);
#6995=LINE('',#198635,#14062);
#6996=LINE('',#198637,#14063);
#6997=LINE('',#198638,#14064);
#6998=LINE('',#198642,#14065);
#6999=LINE('',#198643,#14066);
#7000=LINE('',#198644,#14067);
#7001=LINE('',#198648,#14068);
#7002=LINE('',#198649,#14069);
#7003=LINE('',#198650,#14070);
#7004=LINE('',#198652,#14071);
#7005=LINE('',#198653,#14072);
#7006=LINE('',#198657,#14073);
#7007=LINE('',#198659,#14074);
#7008=LINE('',#198661,#14075);
#7009=LINE('',#198662,#14076);
#7010=LINE('',#198666,#14077);
#7011=LINE('',#198667,#14078);
#7012=LINE('',#198668,#14079);
#7013=LINE('',#198672,#14080);
#7014=LINE('',#198673,#14081);
#7015=LINE('',#198674,#14082);
#7016=LINE('',#198676,#14083);
#7017=LINE('',#198677,#14084);
#7018=LINE('',#198681,#14085);
#7019=LINE('',#198683,#14086);
#7020=LINE('',#198685,#14087);
#7021=LINE('',#198686,#14088);
#7022=LINE('',#198690,#14089);
#7023=LINE('',#198691,#14090);
#7024=LINE('',#198692,#14091);
#7025=LINE('',#198696,#14092);
#7026=LINE('',#198697,#14093);
#7027=LINE('',#198698,#14094);
#7028=LINE('',#198700,#14095);
#7029=LINE('',#198701,#14096);
#7030=LINE('',#198705,#14097);
#7031=LINE('',#198707,#14098);
#7032=LINE('',#198709,#14099);
#7033=LINE('',#198710,#14100);
#7034=LINE('',#198714,#14101);
#7035=LINE('',#198715,#14102);
#7036=LINE('',#198716,#14103);
#7037=LINE('',#198720,#14104);
#7038=LINE('',#198721,#14105);
#7039=LINE('',#198722,#14106);
#7040=LINE('',#198724,#14107);
#7041=LINE('',#198725,#14108);
#7042=LINE('',#198729,#14109);
#7043=LINE('',#198731,#14110);
#7044=LINE('',#198733,#14111);
#7045=LINE('',#198734,#14112);
#7046=LINE('',#198738,#14113);
#7047=LINE('',#198739,#14114);
#7048=LINE('',#198740,#14115);
#7049=LINE('',#198744,#14116);
#7050=LINE('',#198745,#14117);
#7051=LINE('',#198746,#14118);
#7052=LINE('',#198748,#14119);
#7053=LINE('',#198749,#14120);
#7054=LINE('',#198753,#14121);
#7055=LINE('',#198755,#14122);
#7056=LINE('',#198757,#14123);
#7057=LINE('',#198758,#14124);
#7058=LINE('',#198762,#14125);
#7059=LINE('',#198763,#14126);
#7060=LINE('',#198764,#14127);
#7061=LINE('',#198768,#14128);
#7062=LINE('',#198769,#14129);
#7063=LINE('',#198770,#14130);
#7064=LINE('',#198772,#14131);
#7065=LINE('',#198773,#14132);
#7066=LINE('',#198777,#14133);
#7067=LINE('',#198779,#14134);
#7068=LINE('',#198781,#14135);
#7069=LINE('',#198782,#14136);
#7070=LINE('',#198786,#14137);
#7071=LINE('',#198787,#14138);
#7072=LINE('',#198788,#14139);
#7073=LINE('',#198792,#14140);
#7074=LINE('',#198793,#14141);
#7075=LINE('',#198794,#14142);
#7076=LINE('',#198796,#14143);
#7077=LINE('',#198797,#14144);
#7078=LINE('',#198801,#14145);
#7079=LINE('',#198803,#14146);
#7080=LINE('',#198805,#14147);
#7081=LINE('',#198806,#14148);
#7082=LINE('',#198810,#14149);
#7083=LINE('',#198811,#14150);
#7084=LINE('',#198812,#14151);
#7085=LINE('',#198816,#14152);
#7086=LINE('',#198817,#14153);
#7087=LINE('',#198818,#14154);
#7088=LINE('',#198820,#14155);
#7089=LINE('',#198821,#14156);
#7090=LINE('',#198825,#14157);
#7091=LINE('',#198827,#14158);
#7092=LINE('',#198829,#14159);
#7093=LINE('',#198830,#14160);
#7094=LINE('',#198834,#14161);
#7095=LINE('',#198835,#14162);
#7096=LINE('',#198836,#14163);
#7097=LINE('',#198840,#14164);
#7098=LINE('',#198841,#14165);
#7099=LINE('',#198842,#14166);
#7100=LINE('',#198844,#14167);
#7101=LINE('',#198845,#14168);
#7102=LINE('',#198849,#14169);
#7103=LINE('',#198851,#14170);
#7104=LINE('',#198853,#14171);
#7105=LINE('',#198854,#14172);
#7106=LINE('',#198858,#14173);
#7107=LINE('',#198859,#14174);
#7108=LINE('',#198860,#14175);
#7109=LINE('',#198864,#14176);
#7110=LINE('',#198865,#14177);
#7111=LINE('',#198866,#14178);
#7112=LINE('',#198868,#14179);
#7113=LINE('',#198869,#14180);
#7114=LINE('',#198873,#14181);
#7115=LINE('',#198875,#14182);
#7116=LINE('',#198877,#14183);
#7117=LINE('',#198878,#14184);
#7118=LINE('',#198882,#14185);
#7119=LINE('',#198883,#14186);
#7120=LINE('',#198884,#14187);
#7121=LINE('',#198888,#14188);
#7122=LINE('',#198889,#14189);
#7123=LINE('',#198890,#14190);
#7124=LINE('',#198892,#14191);
#7125=LINE('',#198893,#14192);
#7126=LINE('',#198897,#14193);
#7127=LINE('',#198899,#14194);
#7128=LINE('',#198901,#14195);
#7129=LINE('',#198902,#14196);
#7130=LINE('',#198906,#14197);
#7131=LINE('',#198907,#14198);
#7132=LINE('',#198908,#14199);
#7133=LINE('',#198912,#14200);
#7134=LINE('',#198913,#14201);
#7135=LINE('',#198914,#14202);
#7136=LINE('',#198916,#14203);
#7137=LINE('',#198917,#14204);
#7138=LINE('',#198921,#14205);
#7139=LINE('',#198923,#14206);
#7140=LINE('',#198925,#14207);
#7141=LINE('',#198926,#14208);
#7142=LINE('',#198930,#14209);
#7143=LINE('',#198931,#14210);
#7144=LINE('',#198932,#14211);
#7145=LINE('',#198936,#14212);
#7146=LINE('',#198937,#14213);
#7147=LINE('',#198938,#14214);
#7148=LINE('',#198940,#14215);
#7149=LINE('',#198941,#14216);
#7150=LINE('',#198945,#14217);
#7151=LINE('',#198947,#14218);
#7152=LINE('',#198949,#14219);
#7153=LINE('',#198950,#14220);
#7154=LINE('',#198954,#14221);
#7155=LINE('',#198955,#14222);
#7156=LINE('',#198956,#14223);
#7157=LINE('',#198960,#14224);
#7158=LINE('',#198961,#14225);
#7159=LINE('',#198962,#14226);
#7160=LINE('',#198964,#14227);
#7161=LINE('',#198965,#14228);
#7162=LINE('',#198969,#14229);
#7163=LINE('',#198971,#14230);
#7164=LINE('',#198973,#14231);
#7165=LINE('',#198974,#14232);
#7166=LINE('',#198978,#14233);
#7167=LINE('',#198979,#14234);
#7168=LINE('',#198980,#14235);
#7169=LINE('',#198984,#14236);
#7170=LINE('',#198985,#14237);
#7171=LINE('',#198986,#14238);
#7172=LINE('',#198988,#14239);
#7173=LINE('',#198989,#14240);
#7174=LINE('',#198993,#14241);
#7175=LINE('',#198995,#14242);
#7176=LINE('',#198997,#14243);
#7177=LINE('',#198998,#14244);
#7178=LINE('',#199002,#14245);
#7179=LINE('',#199003,#14246);
#7180=LINE('',#199004,#14247);
#7181=LINE('',#199008,#14248);
#7182=LINE('',#199009,#14249);
#7183=LINE('',#199010,#14250);
#7184=LINE('',#199012,#14251);
#7185=LINE('',#199013,#14252);
#7186=LINE('',#199017,#14253);
#7187=LINE('',#199019,#14254);
#7188=LINE('',#199021,#14255);
#7189=LINE('',#199022,#14256);
#7190=LINE('',#199026,#14257);
#7191=LINE('',#199027,#14258);
#7192=LINE('',#199028,#14259);
#7193=LINE('',#199032,#14260);
#7194=LINE('',#199033,#14261);
#7195=LINE('',#199034,#14262);
#7196=LINE('',#199036,#14263);
#7197=LINE('',#199037,#14264);
#7198=LINE('',#199041,#14265);
#7199=LINE('',#199043,#14266);
#7200=LINE('',#199045,#14267);
#7201=LINE('',#199046,#14268);
#7202=LINE('',#199050,#14269);
#7203=LINE('',#199051,#14270);
#7204=LINE('',#199052,#14271);
#7205=LINE('',#199056,#14272);
#7206=LINE('',#199057,#14273);
#7207=LINE('',#199058,#14274);
#7208=LINE('',#199060,#14275);
#7209=LINE('',#199061,#14276);
#7210=LINE('',#199065,#14277);
#7211=LINE('',#199067,#14278);
#7212=LINE('',#199069,#14279);
#7213=LINE('',#199070,#14280);
#7214=LINE('',#199074,#14281);
#7215=LINE('',#199075,#14282);
#7216=LINE('',#199076,#14283);
#7217=LINE('',#199080,#14284);
#7218=LINE('',#199081,#14285);
#7219=LINE('',#199082,#14286);
#7220=LINE('',#199084,#14287);
#7221=LINE('',#199085,#14288);
#7222=LINE('',#199089,#14289);
#7223=LINE('',#199091,#14290);
#7224=LINE('',#199093,#14291);
#7225=LINE('',#199094,#14292);
#7226=LINE('',#199098,#14293);
#7227=LINE('',#199099,#14294);
#7228=LINE('',#199100,#14295);
#7229=LINE('',#199104,#14296);
#7230=LINE('',#199105,#14297);
#7231=LINE('',#199106,#14298);
#7232=LINE('',#199108,#14299);
#7233=LINE('',#199109,#14300);
#7234=LINE('',#199113,#14301);
#7235=LINE('',#199115,#14302);
#7236=LINE('',#199117,#14303);
#7237=LINE('',#199118,#14304);
#7238=LINE('',#199122,#14305);
#7239=LINE('',#199123,#14306);
#7240=LINE('',#199124,#14307);
#7241=LINE('',#199128,#14308);
#7242=LINE('',#199129,#14309);
#7243=LINE('',#199130,#14310);
#7244=LINE('',#199132,#14311);
#7245=LINE('',#199133,#14312);
#7246=LINE('',#199137,#14313);
#7247=LINE('',#199139,#14314);
#7248=LINE('',#199141,#14315);
#7249=LINE('',#199142,#14316);
#7250=LINE('',#199146,#14317);
#7251=LINE('',#199147,#14318);
#7252=LINE('',#199148,#14319);
#7253=LINE('',#199152,#14320);
#7254=LINE('',#199153,#14321);
#7255=LINE('',#199154,#14322);
#7256=LINE('',#199156,#14323);
#7257=LINE('',#199157,#14324);
#7258=LINE('',#199161,#14325);
#7259=LINE('',#199163,#14326);
#7260=LINE('',#199165,#14327);
#7261=LINE('',#199166,#14328);
#7262=LINE('',#199170,#14329);
#7263=LINE('',#199171,#14330);
#7264=LINE('',#199172,#14331);
#7265=LINE('',#199176,#14332);
#7266=LINE('',#199177,#14333);
#7267=LINE('',#199178,#14334);
#7268=LINE('',#199180,#14335);
#7269=LINE('',#199181,#14336);
#7270=LINE('',#199185,#14337);
#7271=LINE('',#199187,#14338);
#7272=LINE('',#199189,#14339);
#7273=LINE('',#199190,#14340);
#7274=LINE('',#199194,#14341);
#7275=LINE('',#199195,#14342);
#7276=LINE('',#199196,#14343);
#7277=LINE('',#199200,#14344);
#7278=LINE('',#199201,#14345);
#7279=LINE('',#199202,#14346);
#7280=LINE('',#199204,#14347);
#7281=LINE('',#199205,#14348);
#7282=LINE('',#199209,#14349);
#7283=LINE('',#199211,#14350);
#7284=LINE('',#199213,#14351);
#7285=LINE('',#199214,#14352);
#7286=LINE('',#199218,#14353);
#7287=LINE('',#199219,#14354);
#7288=LINE('',#199220,#14355);
#7289=LINE('',#199224,#14356);
#7290=LINE('',#199225,#14357);
#7291=LINE('',#199226,#14358);
#7292=LINE('',#199228,#14359);
#7293=LINE('',#199229,#14360);
#7294=LINE('',#199233,#14361);
#7295=LINE('',#199235,#14362);
#7296=LINE('',#199237,#14363);
#7297=LINE('',#199238,#14364);
#7298=LINE('',#199242,#14365);
#7299=LINE('',#199243,#14366);
#7300=LINE('',#199244,#14367);
#7301=LINE('',#199248,#14368);
#7302=LINE('',#199249,#14369);
#7303=LINE('',#199250,#14370);
#7304=LINE('',#199252,#14371);
#7305=LINE('',#199253,#14372);
#7306=LINE('',#199257,#14373);
#7307=LINE('',#199259,#14374);
#7308=LINE('',#199261,#14375);
#7309=LINE('',#199262,#14376);
#7310=LINE('',#199266,#14377);
#7311=LINE('',#199267,#14378);
#7312=LINE('',#199268,#14379);
#7313=LINE('',#199272,#14380);
#7314=LINE('',#199273,#14381);
#7315=LINE('',#199274,#14382);
#7316=LINE('',#199276,#14383);
#7317=LINE('',#199277,#14384);
#7318=LINE('',#199281,#14385);
#7319=LINE('',#199283,#14386);
#7320=LINE('',#199285,#14387);
#7321=LINE('',#199286,#14388);
#7322=LINE('',#199290,#14389);
#7323=LINE('',#199291,#14390);
#7324=LINE('',#199292,#14391);
#7325=LINE('',#199296,#14392);
#7326=LINE('',#199297,#14393);
#7327=LINE('',#199298,#14394);
#7328=LINE('',#199300,#14395);
#7329=LINE('',#199301,#14396);
#7330=LINE('',#199305,#14397);
#7331=LINE('',#199307,#14398);
#7332=LINE('',#199309,#14399);
#7333=LINE('',#199310,#14400);
#7334=LINE('',#199314,#14401);
#7335=LINE('',#199315,#14402);
#7336=LINE('',#199316,#14403);
#7337=LINE('',#199320,#14404);
#7338=LINE('',#199321,#14405);
#7339=LINE('',#199322,#14406);
#7340=LINE('',#199324,#14407);
#7341=LINE('',#199325,#14408);
#7342=LINE('',#199329,#14409);
#7343=LINE('',#199331,#14410);
#7344=LINE('',#199333,#14411);
#7345=LINE('',#199334,#14412);
#7346=LINE('',#199338,#14413);
#7347=LINE('',#199339,#14414);
#7348=LINE('',#199340,#14415);
#7349=LINE('',#199344,#14416);
#7350=LINE('',#199345,#14417);
#7351=LINE('',#199346,#14418);
#7352=LINE('',#199348,#14419);
#7353=LINE('',#199349,#14420);
#7354=LINE('',#199353,#14421);
#7355=LINE('',#199355,#14422);
#7356=LINE('',#199357,#14423);
#7357=LINE('',#199358,#14424);
#7358=LINE('',#199362,#14425);
#7359=LINE('',#199363,#14426);
#7360=LINE('',#199364,#14427);
#7361=LINE('',#199368,#14428);
#7362=LINE('',#199369,#14429);
#7363=LINE('',#199370,#14430);
#7364=LINE('',#199372,#14431);
#7365=LINE('',#199373,#14432);
#7366=LINE('',#199377,#14433);
#7367=LINE('',#199379,#14434);
#7368=LINE('',#199381,#14435);
#7369=LINE('',#199382,#14436);
#7370=LINE('',#199386,#14437);
#7371=LINE('',#199387,#14438);
#7372=LINE('',#199388,#14439);
#7373=LINE('',#199392,#14440);
#7374=LINE('',#199393,#14441);
#7375=LINE('',#199394,#14442);
#7376=LINE('',#199396,#14443);
#7377=LINE('',#199397,#14444);
#7378=LINE('',#199401,#14445);
#7379=LINE('',#199403,#14446);
#7380=LINE('',#199405,#14447);
#7381=LINE('',#199406,#14448);
#7382=LINE('',#199410,#14449);
#7383=LINE('',#199411,#14450);
#7384=LINE('',#199412,#14451);
#7385=LINE('',#199416,#14452);
#7386=LINE('',#199417,#14453);
#7387=LINE('',#199418,#14454);
#7388=LINE('',#199420,#14455);
#7389=LINE('',#199421,#14456);
#7390=LINE('',#199425,#14457);
#7391=LINE('',#199427,#14458);
#7392=LINE('',#199429,#14459);
#7393=LINE('',#199430,#14460);
#7394=LINE('',#199434,#14461);
#7395=LINE('',#199435,#14462);
#7396=LINE('',#199436,#14463);
#7397=LINE('',#199440,#14464);
#7398=LINE('',#199441,#14465);
#7399=LINE('',#199442,#14466);
#7400=LINE('',#199444,#14467);
#7401=LINE('',#199445,#14468);
#7402=LINE('',#199449,#14469);
#7403=LINE('',#199451,#14470);
#7404=LINE('',#199453,#14471);
#7405=LINE('',#199454,#14472);
#7406=LINE('',#199458,#14473);
#7407=LINE('',#199459,#14474);
#7408=LINE('',#199460,#14475);
#7409=LINE('',#199464,#14476);
#7410=LINE('',#199465,#14477);
#7411=LINE('',#199466,#14478);
#7412=LINE('',#199468,#14479);
#7413=LINE('',#199469,#14480);
#7414=LINE('',#199473,#14481);
#7415=LINE('',#199475,#14482);
#7416=LINE('',#199477,#14483);
#7417=LINE('',#199478,#14484);
#7418=LINE('',#199482,#14485);
#7419=LINE('',#199483,#14486);
#7420=LINE('',#199484,#14487);
#7421=LINE('',#199488,#14488);
#7422=LINE('',#199489,#14489);
#7423=LINE('',#199490,#14490);
#7424=LINE('',#199492,#14491);
#7425=LINE('',#199493,#14492);
#7426=LINE('',#199497,#14493);
#7427=LINE('',#199499,#14494);
#7428=LINE('',#199501,#14495);
#7429=LINE('',#199502,#14496);
#7430=LINE('',#199506,#14497);
#7431=LINE('',#199507,#14498);
#7432=LINE('',#199508,#14499);
#7433=LINE('',#199512,#14500);
#7434=LINE('',#199513,#14501);
#7435=LINE('',#199514,#14502);
#7436=LINE('',#199516,#14503);
#7437=LINE('',#199517,#14504);
#7438=LINE('',#199521,#14505);
#7439=LINE('',#199523,#14506);
#7440=LINE('',#199525,#14507);
#7441=LINE('',#199526,#14508);
#7442=LINE('',#199530,#14509);
#7443=LINE('',#199531,#14510);
#7444=LINE('',#199532,#14511);
#7445=LINE('',#199536,#14512);
#7446=LINE('',#199537,#14513);
#7447=LINE('',#199538,#14514);
#7448=LINE('',#199540,#14515);
#7449=LINE('',#199541,#14516);
#7450=LINE('',#199545,#14517);
#7451=LINE('',#199547,#14518);
#7452=LINE('',#199549,#14519);
#7453=LINE('',#199550,#14520);
#7454=LINE('',#199554,#14521);
#7455=LINE('',#199555,#14522);
#7456=LINE('',#199556,#14523);
#7457=LINE('',#199560,#14524);
#7458=LINE('',#199561,#14525);
#7459=LINE('',#199562,#14526);
#7460=LINE('',#199564,#14527);
#7461=LINE('',#199565,#14528);
#7462=LINE('',#199569,#14529);
#7463=LINE('',#199571,#14530);
#7464=LINE('',#199573,#14531);
#7465=LINE('',#199574,#14532);
#7466=LINE('',#199578,#14533);
#7467=LINE('',#199579,#14534);
#7468=LINE('',#199580,#14535);
#7469=LINE('',#199584,#14536);
#7470=LINE('',#199585,#14537);
#7471=LINE('',#199586,#14538);
#7472=LINE('',#199588,#14539);
#7473=LINE('',#199589,#14540);
#7474=LINE('',#199593,#14541);
#7475=LINE('',#199595,#14542);
#7476=LINE('',#199597,#14543);
#7477=LINE('',#199598,#14544);
#7478=LINE('',#199602,#14545);
#7479=LINE('',#199603,#14546);
#7480=LINE('',#199604,#14547);
#7481=LINE('',#199608,#14548);
#7482=LINE('',#199609,#14549);
#7483=LINE('',#199610,#14550);
#7484=LINE('',#199612,#14551);
#7485=LINE('',#199613,#14552);
#7486=LINE('',#199617,#14553);
#7487=LINE('',#199619,#14554);
#7488=LINE('',#199621,#14555);
#7489=LINE('',#199622,#14556);
#7490=LINE('',#199626,#14557);
#7491=LINE('',#199627,#14558);
#7492=LINE('',#199628,#14559);
#7493=LINE('',#199632,#14560);
#7494=LINE('',#199633,#14561);
#7495=LINE('',#199634,#14562);
#7496=LINE('',#199636,#14563);
#7497=LINE('',#199637,#14564);
#7498=LINE('',#199641,#14565);
#7499=LINE('',#199643,#14566);
#7500=LINE('',#199645,#14567);
#7501=LINE('',#199646,#14568);
#7502=LINE('',#199650,#14569);
#7503=LINE('',#199651,#14570);
#7504=LINE('',#199652,#14571);
#7505=LINE('',#199656,#14572);
#7506=LINE('',#199657,#14573);
#7507=LINE('',#199658,#14574);
#7508=LINE('',#199660,#14575);
#7509=LINE('',#199661,#14576);
#7510=LINE('',#199665,#14577);
#7511=LINE('',#199667,#14578);
#7512=LINE('',#199669,#14579);
#7513=LINE('',#199670,#14580);
#7514=LINE('',#199674,#14581);
#7515=LINE('',#199675,#14582);
#7516=LINE('',#199676,#14583);
#7517=LINE('',#199680,#14584);
#7518=LINE('',#199681,#14585);
#7519=LINE('',#199682,#14586);
#7520=LINE('',#199684,#14587);
#7521=LINE('',#199685,#14588);
#7522=LINE('',#199689,#14589);
#7523=LINE('',#199691,#14590);
#7524=LINE('',#199693,#14591);
#7525=LINE('',#199694,#14592);
#7526=LINE('',#199698,#14593);
#7527=LINE('',#199699,#14594);
#7528=LINE('',#199700,#14595);
#7529=LINE('',#199704,#14596);
#7530=LINE('',#199705,#14597);
#7531=LINE('',#199706,#14598);
#7532=LINE('',#199708,#14599);
#7533=LINE('',#199709,#14600);
#7534=LINE('',#199713,#14601);
#7535=LINE('',#199715,#14602);
#7536=LINE('',#199717,#14603);
#7537=LINE('',#199718,#14604);
#7538=LINE('',#199722,#14605);
#7539=LINE('',#199723,#14606);
#7540=LINE('',#199724,#14607);
#7541=LINE('',#199728,#14608);
#7542=LINE('',#199729,#14609);
#7543=LINE('',#199730,#14610);
#7544=LINE('',#199732,#14611);
#7545=LINE('',#199733,#14612);
#7546=LINE('',#199737,#14613);
#7547=LINE('',#199739,#14614);
#7548=LINE('',#199741,#14615);
#7549=LINE('',#199742,#14616);
#7550=LINE('',#199746,#14617);
#7551=LINE('',#199747,#14618);
#7552=LINE('',#199748,#14619);
#7553=LINE('',#199752,#14620);
#7554=LINE('',#199753,#14621);
#7555=LINE('',#199754,#14622);
#7556=LINE('',#199756,#14623);
#7557=LINE('',#199757,#14624);
#7558=LINE('',#199761,#14625);
#7559=LINE('',#199763,#14626);
#7560=LINE('',#199765,#14627);
#7561=LINE('',#199766,#14628);
#7562=LINE('',#199770,#14629);
#7563=LINE('',#199771,#14630);
#7564=LINE('',#199772,#14631);
#7565=LINE('',#199776,#14632);
#7566=LINE('',#199777,#14633);
#7567=LINE('',#199778,#14634);
#7568=LINE('',#199780,#14635);
#7569=LINE('',#199781,#14636);
#7570=LINE('',#199785,#14637);
#7571=LINE('',#199787,#14638);
#7572=LINE('',#199789,#14639);
#7573=LINE('',#199790,#14640);
#7574=LINE('',#199794,#14641);
#7575=LINE('',#199795,#14642);
#7576=LINE('',#199796,#14643);
#7577=LINE('',#199800,#14644);
#7578=LINE('',#199801,#14645);
#7579=LINE('',#199802,#14646);
#7580=LINE('',#199804,#14647);
#7581=LINE('',#199805,#14648);
#7582=LINE('',#199809,#14649);
#7583=LINE('',#199811,#14650);
#7584=LINE('',#199813,#14651);
#7585=LINE('',#199814,#14652);
#7586=LINE('',#199818,#14653);
#7587=LINE('',#199819,#14654);
#7588=LINE('',#199820,#14655);
#7589=LINE('',#199824,#14656);
#7590=LINE('',#199825,#14657);
#7591=LINE('',#199826,#14658);
#7592=LINE('',#199828,#14659);
#7593=LINE('',#199829,#14660);
#7594=LINE('',#199833,#14661);
#7595=LINE('',#199835,#14662);
#7596=LINE('',#199837,#14663);
#7597=LINE('',#199838,#14664);
#7598=LINE('',#199842,#14665);
#7599=LINE('',#199843,#14666);
#7600=LINE('',#199844,#14667);
#7601=LINE('',#199848,#14668);
#7602=LINE('',#199849,#14669);
#7603=LINE('',#199850,#14670);
#7604=LINE('',#199852,#14671);
#7605=LINE('',#199853,#14672);
#7606=LINE('',#199857,#14673);
#7607=LINE('',#199859,#14674);
#7608=LINE('',#199861,#14675);
#7609=LINE('',#199862,#14676);
#7610=LINE('',#199866,#14677);
#7611=LINE('',#199867,#14678);
#7612=LINE('',#199868,#14679);
#7613=LINE('',#199872,#14680);
#7614=LINE('',#199873,#14681);
#7615=LINE('',#199874,#14682);
#7616=LINE('',#199876,#14683);
#7617=LINE('',#199877,#14684);
#7618=LINE('',#199881,#14685);
#7619=LINE('',#199883,#14686);
#7620=LINE('',#199885,#14687);
#7621=LINE('',#199886,#14688);
#7622=LINE('',#199890,#14689);
#7623=LINE('',#199891,#14690);
#7624=LINE('',#199892,#14691);
#7625=LINE('',#199896,#14692);
#7626=LINE('',#199897,#14693);
#7627=LINE('',#199898,#14694);
#7628=LINE('',#199900,#14695);
#7629=LINE('',#199901,#14696);
#7630=LINE('',#199905,#14697);
#7631=LINE('',#199907,#14698);
#7632=LINE('',#199909,#14699);
#7633=LINE('',#199910,#14700);
#7634=LINE('',#199914,#14701);
#7635=LINE('',#199915,#14702);
#7636=LINE('',#199916,#14703);
#7637=LINE('',#199920,#14704);
#7638=LINE('',#199921,#14705);
#7639=LINE('',#199922,#14706);
#7640=LINE('',#199924,#14707);
#7641=LINE('',#199925,#14708);
#7642=LINE('',#199929,#14709);
#7643=LINE('',#199931,#14710);
#7644=LINE('',#199933,#14711);
#7645=LINE('',#199934,#14712);
#7646=LINE('',#199938,#14713);
#7647=LINE('',#199939,#14714);
#7648=LINE('',#199940,#14715);
#7649=LINE('',#199944,#14716);
#7650=LINE('',#199945,#14717);
#7651=LINE('',#199946,#14718);
#7652=LINE('',#199948,#14719);
#7653=LINE('',#199949,#14720);
#7654=LINE('',#199953,#14721);
#7655=LINE('',#199955,#14722);
#7656=LINE('',#199957,#14723);
#7657=LINE('',#199958,#14724);
#7658=LINE('',#199962,#14725);
#7659=LINE('',#199963,#14726);
#7660=LINE('',#199964,#14727);
#7661=LINE('',#199968,#14728);
#7662=LINE('',#199969,#14729);
#7663=LINE('',#199970,#14730);
#7664=LINE('',#199972,#14731);
#7665=LINE('',#199973,#14732);
#7666=LINE('',#199977,#14733);
#7667=LINE('',#199979,#14734);
#7668=LINE('',#199981,#14735);
#7669=LINE('',#199982,#14736);
#7670=LINE('',#199986,#14737);
#7671=LINE('',#199987,#14738);
#7672=LINE('',#199988,#14739);
#7673=LINE('',#199992,#14740);
#7674=LINE('',#199993,#14741);
#7675=LINE('',#199994,#14742);
#7676=LINE('',#199996,#14743);
#7677=LINE('',#199997,#14744);
#7678=LINE('',#200001,#14745);
#7679=LINE('',#200003,#14746);
#7680=LINE('',#200005,#14747);
#7681=LINE('',#200006,#14748);
#7682=LINE('',#200010,#14749);
#7683=LINE('',#200011,#14750);
#7684=LINE('',#200012,#14751);
#7685=LINE('',#200016,#14752);
#7686=LINE('',#200017,#14753);
#7687=LINE('',#200018,#14754);
#7688=LINE('',#200020,#14755);
#7689=LINE('',#200021,#14756);
#7690=LINE('',#200025,#14757);
#7691=LINE('',#200027,#14758);
#7692=LINE('',#200029,#14759);
#7693=LINE('',#200030,#14760);
#7694=LINE('',#200034,#14761);
#7695=LINE('',#200035,#14762);
#7696=LINE('',#200036,#14763);
#7697=LINE('',#200040,#14764);
#7698=LINE('',#200041,#14765);
#7699=LINE('',#200042,#14766);
#7700=LINE('',#200044,#14767);
#7701=LINE('',#200045,#14768);
#7702=LINE('',#200049,#14769);
#7703=LINE('',#200051,#14770);
#7704=LINE('',#200053,#14771);
#7705=LINE('',#200054,#14772);
#7706=LINE('',#200058,#14773);
#7707=LINE('',#200059,#14774);
#7708=LINE('',#200060,#14775);
#7709=LINE('',#200064,#14776);
#7710=LINE('',#200065,#14777);
#7711=LINE('',#200066,#14778);
#7712=LINE('',#200068,#14779);
#7713=LINE('',#200069,#14780);
#7714=LINE('',#200073,#14781);
#7715=LINE('',#200075,#14782);
#7716=LINE('',#200077,#14783);
#7717=LINE('',#200078,#14784);
#7718=LINE('',#200082,#14785);
#7719=LINE('',#200083,#14786);
#7720=LINE('',#200084,#14787);
#7721=LINE('',#200088,#14788);
#7722=LINE('',#200089,#14789);
#7723=LINE('',#200090,#14790);
#7724=LINE('',#200092,#14791);
#7725=LINE('',#200093,#14792);
#7726=LINE('',#200097,#14793);
#7727=LINE('',#200099,#14794);
#7728=LINE('',#200101,#14795);
#7729=LINE('',#200102,#14796);
#7730=LINE('',#200106,#14797);
#7731=LINE('',#200107,#14798);
#7732=LINE('',#200108,#14799);
#7733=LINE('',#200112,#14800);
#7734=LINE('',#200113,#14801);
#7735=LINE('',#200114,#14802);
#7736=LINE('',#200116,#14803);
#7737=LINE('',#200117,#14804);
#7738=LINE('',#200121,#14805);
#7739=LINE('',#200123,#14806);
#7740=LINE('',#200125,#14807);
#7741=LINE('',#200126,#14808);
#7742=LINE('',#200130,#14809);
#7743=LINE('',#200131,#14810);
#7744=LINE('',#200132,#14811);
#7745=LINE('',#200136,#14812);
#7746=LINE('',#200137,#14813);
#7747=LINE('',#200138,#14814);
#7748=LINE('',#200140,#14815);
#7749=LINE('',#200141,#14816);
#7750=LINE('',#200145,#14817);
#7751=LINE('',#200147,#14818);
#7752=LINE('',#200149,#14819);
#7753=LINE('',#200150,#14820);
#7754=LINE('',#200154,#14821);
#7755=LINE('',#200155,#14822);
#7756=LINE('',#200156,#14823);
#7757=LINE('',#200160,#14824);
#7758=LINE('',#200161,#14825);
#7759=LINE('',#200162,#14826);
#7760=LINE('',#200164,#14827);
#7761=LINE('',#200165,#14828);
#7762=LINE('',#200169,#14829);
#7763=LINE('',#200171,#14830);
#7764=LINE('',#200173,#14831);
#7765=LINE('',#200174,#14832);
#7766=LINE('',#200178,#14833);
#7767=LINE('',#200179,#14834);
#7768=LINE('',#200180,#14835);
#7769=LINE('',#200184,#14836);
#7770=LINE('',#200185,#14837);
#7771=LINE('',#200186,#14838);
#7772=LINE('',#200188,#14839);
#7773=LINE('',#200189,#14840);
#7774=LINE('',#200193,#14841);
#7775=LINE('',#200195,#14842);
#7776=LINE('',#200197,#14843);
#7777=LINE('',#200198,#14844);
#7778=LINE('',#200202,#14845);
#7779=LINE('',#200203,#14846);
#7780=LINE('',#200204,#14847);
#7781=LINE('',#200208,#14848);
#7782=LINE('',#200209,#14849);
#7783=LINE('',#200210,#14850);
#7784=LINE('',#200212,#14851);
#7785=LINE('',#200213,#14852);
#7786=LINE('',#200217,#14853);
#7787=LINE('',#200219,#14854);
#7788=LINE('',#200221,#14855);
#7789=LINE('',#200222,#14856);
#7790=LINE('',#200226,#14857);
#7791=LINE('',#200227,#14858);
#7792=LINE('',#200228,#14859);
#7793=LINE('',#200232,#14860);
#7794=LINE('',#200233,#14861);
#7795=LINE('',#200234,#14862);
#7796=LINE('',#200236,#14863);
#7797=LINE('',#200237,#14864);
#7798=LINE('',#200241,#14865);
#7799=LINE('',#200243,#14866);
#7800=LINE('',#200245,#14867);
#7801=LINE('',#200246,#14868);
#7802=LINE('',#200250,#14869);
#7803=LINE('',#200251,#14870);
#7804=LINE('',#200252,#14871);
#7805=LINE('',#200256,#14872);
#7806=LINE('',#200257,#14873);
#7807=LINE('',#200258,#14874);
#7808=LINE('',#200260,#14875);
#7809=LINE('',#200261,#14876);
#7810=LINE('',#200265,#14877);
#7811=LINE('',#200267,#14878);
#7812=LINE('',#200269,#14879);
#7813=LINE('',#200270,#14880);
#7814=LINE('',#200274,#14881);
#7815=LINE('',#200275,#14882);
#7816=LINE('',#200276,#14883);
#7817=LINE('',#200280,#14884);
#7818=LINE('',#200281,#14885);
#7819=LINE('',#200282,#14886);
#7820=LINE('',#200284,#14887);
#7821=LINE('',#200285,#14888);
#7822=LINE('',#200289,#14889);
#7823=LINE('',#200291,#14890);
#7824=LINE('',#200293,#14891);
#7825=LINE('',#200294,#14892);
#7826=LINE('',#200298,#14893);
#7827=LINE('',#200299,#14894);
#7828=LINE('',#200300,#14895);
#7829=LINE('',#200304,#14896);
#7830=LINE('',#200305,#14897);
#7831=LINE('',#200306,#14898);
#7832=LINE('',#200308,#14899);
#7833=LINE('',#200309,#14900);
#7834=LINE('',#200313,#14901);
#7835=LINE('',#200315,#14902);
#7836=LINE('',#200317,#14903);
#7837=LINE('',#200318,#14904);
#7838=LINE('',#200322,#14905);
#7839=LINE('',#200323,#14906);
#7840=LINE('',#200324,#14907);
#7841=LINE('',#200328,#14908);
#7842=LINE('',#200329,#14909);
#7843=LINE('',#200330,#14910);
#7844=LINE('',#200332,#14911);
#7845=LINE('',#200333,#14912);
#7846=LINE('',#200337,#14913);
#7847=LINE('',#200339,#14914);
#7848=LINE('',#200341,#14915);
#7849=LINE('',#200342,#14916);
#7850=LINE('',#200346,#14917);
#7851=LINE('',#200347,#14918);
#7852=LINE('',#200348,#14919);
#7853=LINE('',#200352,#14920);
#7854=LINE('',#200353,#14921);
#7855=LINE('',#200354,#14922);
#7856=LINE('',#200356,#14923);
#7857=LINE('',#200357,#14924);
#7858=LINE('',#200361,#14925);
#7859=LINE('',#200363,#14926);
#7860=LINE('',#200365,#14927);
#7861=LINE('',#200366,#14928);
#7862=LINE('',#200370,#14929);
#7863=LINE('',#200371,#14930);
#7864=LINE('',#200372,#14931);
#7865=LINE('',#200376,#14932);
#7866=LINE('',#200377,#14933);
#7867=LINE('',#200378,#14934);
#7868=LINE('',#200380,#14935);
#7869=LINE('',#200381,#14936);
#7870=LINE('',#200385,#14937);
#7871=LINE('',#200387,#14938);
#7872=LINE('',#200389,#14939);
#7873=LINE('',#200390,#14940);
#7874=LINE('',#200394,#14941);
#7875=LINE('',#200395,#14942);
#7876=LINE('',#200396,#14943);
#7877=LINE('',#200400,#14944);
#7878=LINE('',#200401,#14945);
#7879=LINE('',#200402,#14946);
#7880=LINE('',#200404,#14947);
#7881=LINE('',#200405,#14948);
#7882=LINE('',#200409,#14949);
#7883=LINE('',#200411,#14950);
#7884=LINE('',#200413,#14951);
#7885=LINE('',#200414,#14952);
#7886=LINE('',#200418,#14953);
#7887=LINE('',#200419,#14954);
#7888=LINE('',#200420,#14955);
#7889=LINE('',#200424,#14956);
#7890=LINE('',#200425,#14957);
#7891=LINE('',#200426,#14958);
#7892=LINE('',#200428,#14959);
#7893=LINE('',#200429,#14960);
#7894=LINE('',#200433,#14961);
#7895=LINE('',#200435,#14962);
#7896=LINE('',#200437,#14963);
#7897=LINE('',#200438,#14964);
#7898=LINE('',#200442,#14965);
#7899=LINE('',#200443,#14966);
#7900=LINE('',#200444,#14967);
#7901=LINE('',#200448,#14968);
#7902=LINE('',#200449,#14969);
#7903=LINE('',#200450,#14970);
#7904=LINE('',#200452,#14971);
#7905=LINE('',#200453,#14972);
#7906=LINE('',#200457,#14973);
#7907=LINE('',#200459,#14974);
#7908=LINE('',#200461,#14975);
#7909=LINE('',#200462,#14976);
#7910=LINE('',#200466,#14977);
#7911=LINE('',#200467,#14978);
#7912=LINE('',#200468,#14979);
#7913=LINE('',#200472,#14980);
#7914=LINE('',#200473,#14981);
#7915=LINE('',#200474,#14982);
#7916=LINE('',#200476,#14983);
#7917=LINE('',#200477,#14984);
#7918=LINE('',#200481,#14985);
#7919=LINE('',#200483,#14986);
#7920=LINE('',#200485,#14987);
#7921=LINE('',#200486,#14988);
#7922=LINE('',#200490,#14989);
#7923=LINE('',#200491,#14990);
#7924=LINE('',#200492,#14991);
#7925=LINE('',#200496,#14992);
#7926=LINE('',#200497,#14993);
#7927=LINE('',#200498,#14994);
#7928=LINE('',#200500,#14995);
#7929=LINE('',#200501,#14996);
#7930=LINE('',#200505,#14997);
#7931=LINE('',#200507,#14998);
#7932=LINE('',#200509,#14999);
#7933=LINE('',#200510,#15000);
#7934=LINE('',#200514,#15001);
#7935=LINE('',#200515,#15002);
#7936=LINE('',#200516,#15003);
#7937=LINE('',#200520,#15004);
#7938=LINE('',#200521,#15005);
#7939=LINE('',#200522,#15006);
#7940=LINE('',#200524,#15007);
#7941=LINE('',#200525,#15008);
#7942=LINE('',#200529,#15009);
#7943=LINE('',#200531,#15010);
#7944=LINE('',#200533,#15011);
#7945=LINE('',#200534,#15012);
#7946=LINE('',#200538,#15013);
#7947=LINE('',#200539,#15014);
#7948=LINE('',#200540,#15015);
#7949=LINE('',#200544,#15016);
#7950=LINE('',#200545,#15017);
#7951=LINE('',#200546,#15018);
#7952=LINE('',#200548,#15019);
#7953=LINE('',#200549,#15020);
#7954=LINE('',#200553,#15021);
#7955=LINE('',#200555,#15022);
#7956=LINE('',#200557,#15023);
#7957=LINE('',#200558,#15024);
#7958=LINE('',#200562,#15025);
#7959=LINE('',#200563,#15026);
#7960=LINE('',#200564,#15027);
#7961=LINE('',#200568,#15028);
#7962=LINE('',#200569,#15029);
#7963=LINE('',#200570,#15030);
#7964=LINE('',#200572,#15031);
#7965=LINE('',#200573,#15032);
#7966=LINE('',#200577,#15033);
#7967=LINE('',#200579,#15034);
#7968=LINE('',#200581,#15035);
#7969=LINE('',#200582,#15036);
#7970=LINE('',#200586,#15037);
#7971=LINE('',#200587,#15038);
#7972=LINE('',#200588,#15039);
#7973=LINE('',#200592,#15040);
#7974=LINE('',#200593,#15041);
#7975=LINE('',#200594,#15042);
#7976=LINE('',#200596,#15043);
#7977=LINE('',#200597,#15044);
#7978=LINE('',#200601,#15045);
#7979=LINE('',#200603,#15046);
#7980=LINE('',#200605,#15047);
#7981=LINE('',#200606,#15048);
#7982=LINE('',#200610,#15049);
#7983=LINE('',#200611,#15050);
#7984=LINE('',#200612,#15051);
#7985=LINE('',#200616,#15052);
#7986=LINE('',#200617,#15053);
#7987=LINE('',#200618,#15054);
#7988=LINE('',#200620,#15055);
#7989=LINE('',#200621,#15056);
#7990=LINE('',#200625,#15057);
#7991=LINE('',#200627,#15058);
#7992=LINE('',#200629,#15059);
#7993=LINE('',#200630,#15060);
#7994=LINE('',#200634,#15061);
#7995=LINE('',#200635,#15062);
#7996=LINE('',#200636,#15063);
#7997=LINE('',#200640,#15064);
#7998=LINE('',#200641,#15065);
#7999=LINE('',#200642,#15066);
#8000=LINE('',#200644,#15067);
#8001=LINE('',#200645,#15068);
#8002=LINE('',#200649,#15069);
#8003=LINE('',#200651,#15070);
#8004=LINE('',#200653,#15071);
#8005=LINE('',#200654,#15072);
#8006=LINE('',#200658,#15073);
#8007=LINE('',#200659,#15074);
#8008=LINE('',#200660,#15075);
#8009=LINE('',#200664,#15076);
#8010=LINE('',#200665,#15077);
#8011=LINE('',#200666,#15078);
#8012=LINE('',#200668,#15079);
#8013=LINE('',#200669,#15080);
#8014=LINE('',#200673,#15081);
#8015=LINE('',#200675,#15082);
#8016=LINE('',#200677,#15083);
#8017=LINE('',#200678,#15084);
#8018=LINE('',#200682,#15085);
#8019=LINE('',#200683,#15086);
#8020=LINE('',#200684,#15087);
#8021=LINE('',#200688,#15088);
#8022=LINE('',#200689,#15089);
#8023=LINE('',#200690,#15090);
#8024=LINE('',#200692,#15091);
#8025=LINE('',#200693,#15092);
#8026=LINE('',#200697,#15093);
#8027=LINE('',#200699,#15094);
#8028=LINE('',#200701,#15095);
#8029=LINE('',#200702,#15096);
#8030=LINE('',#200706,#15097);
#8031=LINE('',#200707,#15098);
#8032=LINE('',#200708,#15099);
#8033=LINE('',#200712,#15100);
#8034=LINE('',#200713,#15101);
#8035=LINE('',#200714,#15102);
#8036=LINE('',#200716,#15103);
#8037=LINE('',#200717,#15104);
#8038=LINE('',#200721,#15105);
#8039=LINE('',#200723,#15106);
#8040=LINE('',#200725,#15107);
#8041=LINE('',#200726,#15108);
#8042=LINE('',#200730,#15109);
#8043=LINE('',#200731,#15110);
#8044=LINE('',#200732,#15111);
#8045=LINE('',#200736,#15112);
#8046=LINE('',#200737,#15113);
#8047=LINE('',#200738,#15114);
#8048=LINE('',#200740,#15115);
#8049=LINE('',#200741,#15116);
#8050=LINE('',#200745,#15117);
#8051=LINE('',#200747,#15118);
#8052=LINE('',#200749,#15119);
#8053=LINE('',#200750,#15120);
#8054=LINE('',#200754,#15121);
#8055=LINE('',#200755,#15122);
#8056=LINE('',#200756,#15123);
#8057=LINE('',#200760,#15124);
#8058=LINE('',#200761,#15125);
#8059=LINE('',#200762,#15126);
#8060=LINE('',#200764,#15127);
#8061=LINE('',#200765,#15128);
#8062=LINE('',#200769,#15129);
#8063=LINE('',#200771,#15130);
#8064=LINE('',#200773,#15131);
#8065=LINE('',#200774,#15132);
#8066=LINE('',#200778,#15133);
#8067=LINE('',#200779,#15134);
#8068=LINE('',#200780,#15135);
#8069=LINE('',#200784,#15136);
#8070=LINE('',#200785,#15137);
#8071=LINE('',#200786,#15138);
#8072=LINE('',#200788,#15139);
#8073=LINE('',#200789,#15140);
#8074=LINE('',#200793,#15141);
#8075=LINE('',#200795,#15142);
#8076=LINE('',#200797,#15143);
#8077=LINE('',#200798,#15144);
#8078=LINE('',#200802,#15145);
#8079=LINE('',#200803,#15146);
#8080=LINE('',#200804,#15147);
#8081=LINE('',#200808,#15148);
#8082=LINE('',#200809,#15149);
#8083=LINE('',#200810,#15150);
#8084=LINE('',#200812,#15151);
#8085=LINE('',#200813,#15152);
#8086=LINE('',#200817,#15153);
#8087=LINE('',#200819,#15154);
#8088=LINE('',#200821,#15155);
#8089=LINE('',#200822,#15156);
#8090=LINE('',#200826,#15157);
#8091=LINE('',#200827,#15158);
#8092=LINE('',#200828,#15159);
#8093=LINE('',#200832,#15160);
#8094=LINE('',#200833,#15161);
#8095=LINE('',#200834,#15162);
#8096=LINE('',#200836,#15163);
#8097=LINE('',#200837,#15164);
#8098=LINE('',#200841,#15165);
#8099=LINE('',#200843,#15166);
#8100=LINE('',#200845,#15167);
#8101=LINE('',#200846,#15168);
#8102=LINE('',#200850,#15169);
#8103=LINE('',#200851,#15170);
#8104=LINE('',#200852,#15171);
#8105=LINE('',#200856,#15172);
#8106=LINE('',#200857,#15173);
#8107=LINE('',#200858,#15174);
#8108=LINE('',#200860,#15175);
#8109=LINE('',#200861,#15176);
#8110=LINE('',#200865,#15177);
#8111=LINE('',#200867,#15178);
#8112=LINE('',#200869,#15179);
#8113=LINE('',#200870,#15180);
#8114=LINE('',#200874,#15181);
#8115=LINE('',#200875,#15182);
#8116=LINE('',#200876,#15183);
#8117=LINE('',#200880,#15184);
#8118=LINE('',#200881,#15185);
#8119=LINE('',#200882,#15186);
#8120=LINE('',#200884,#15187);
#8121=LINE('',#200885,#15188);
#8122=LINE('',#200889,#15189);
#8123=LINE('',#200891,#15190);
#8124=LINE('',#200893,#15191);
#8125=LINE('',#200894,#15192);
#8126=LINE('',#200898,#15193);
#8127=LINE('',#200899,#15194);
#8128=LINE('',#200900,#15195);
#8129=LINE('',#200904,#15196);
#8130=LINE('',#200905,#15197);
#8131=LINE('',#200906,#15198);
#8132=LINE('',#200908,#15199);
#8133=LINE('',#200909,#15200);
#8134=LINE('',#200913,#15201);
#8135=LINE('',#200915,#15202);
#8136=LINE('',#200917,#15203);
#8137=LINE('',#200918,#15204);
#8138=LINE('',#200922,#15205);
#8139=LINE('',#200923,#15206);
#8140=LINE('',#200924,#15207);
#8141=LINE('',#200928,#15208);
#8142=LINE('',#200929,#15209);
#8143=LINE('',#200930,#15210);
#8144=LINE('',#200932,#15211);
#8145=LINE('',#200933,#15212);
#8146=LINE('',#200937,#15213);
#8147=LINE('',#200939,#15214);
#8148=LINE('',#200941,#15215);
#8149=LINE('',#200942,#15216);
#8150=LINE('',#200946,#15217);
#8151=LINE('',#200947,#15218);
#8152=LINE('',#200948,#15219);
#8153=LINE('',#200952,#15220);
#8154=LINE('',#200953,#15221);
#8155=LINE('',#200954,#15222);
#8156=LINE('',#200956,#15223);
#8157=LINE('',#200957,#15224);
#8158=LINE('',#200961,#15225);
#8159=LINE('',#200963,#15226);
#8160=LINE('',#200965,#15227);
#8161=LINE('',#200966,#15228);
#8162=LINE('',#200970,#15229);
#8163=LINE('',#200971,#15230);
#8164=LINE('',#200972,#15231);
#8165=LINE('',#200976,#15232);
#8166=LINE('',#200977,#15233);
#8167=LINE('',#200978,#15234);
#8168=LINE('',#200980,#15235);
#8169=LINE('',#200981,#15236);
#8170=LINE('',#200985,#15237);
#8171=LINE('',#200987,#15238);
#8172=LINE('',#200989,#15239);
#8173=LINE('',#200990,#15240);
#8174=LINE('',#200994,#15241);
#8175=LINE('',#200995,#15242);
#8176=LINE('',#200996,#15243);
#8177=LINE('',#201000,#15244);
#8178=LINE('',#201001,#15245);
#8179=LINE('',#201002,#15246);
#8180=LINE('',#201004,#15247);
#8181=LINE('',#201005,#15248);
#8182=LINE('',#201009,#15249);
#8183=LINE('',#201011,#15250);
#8184=LINE('',#201013,#15251);
#8185=LINE('',#201014,#15252);
#8186=LINE('',#201018,#15253);
#8187=LINE('',#201019,#15254);
#8188=LINE('',#201020,#15255);
#8189=LINE('',#201024,#15256);
#8190=LINE('',#201025,#15257);
#8191=LINE('',#201026,#15258);
#8192=LINE('',#201028,#15259);
#8193=LINE('',#201029,#15260);
#8194=LINE('',#201033,#15261);
#8195=LINE('',#201035,#15262);
#8196=LINE('',#201037,#15263);
#8197=LINE('',#201038,#15264);
#8198=LINE('',#201042,#15265);
#8199=LINE('',#201043,#15266);
#8200=LINE('',#201044,#15267);
#8201=LINE('',#201048,#15268);
#8202=LINE('',#201049,#15269);
#8203=LINE('',#201050,#15270);
#8204=LINE('',#201052,#15271);
#8205=LINE('',#201053,#15272);
#8206=LINE('',#201057,#15273);
#8207=LINE('',#201059,#15274);
#8208=LINE('',#201061,#15275);
#8209=LINE('',#201062,#15276);
#8210=LINE('',#201066,#15277);
#8211=LINE('',#201067,#15278);
#8212=LINE('',#201068,#15279);
#8213=LINE('',#201072,#15280);
#8214=LINE('',#201073,#15281);
#8215=LINE('',#201074,#15282);
#8216=LINE('',#201076,#15283);
#8217=LINE('',#201077,#15284);
#8218=LINE('',#201081,#15285);
#8219=LINE('',#201083,#15286);
#8220=LINE('',#201085,#15287);
#8221=LINE('',#201086,#15288);
#8222=LINE('',#201090,#15289);
#8223=LINE('',#201091,#15290);
#8224=LINE('',#201092,#15291);
#8225=LINE('',#201096,#15292);
#8226=LINE('',#201097,#15293);
#8227=LINE('',#201098,#15294);
#8228=LINE('',#201100,#15295);
#8229=LINE('',#201101,#15296);
#8230=LINE('',#201105,#15297);
#8231=LINE('',#201107,#15298);
#8232=LINE('',#201109,#15299);
#8233=LINE('',#201110,#15300);
#8234=LINE('',#201114,#15301);
#8235=LINE('',#201115,#15302);
#8236=LINE('',#201116,#15303);
#8237=LINE('',#201120,#15304);
#8238=LINE('',#201121,#15305);
#8239=LINE('',#201122,#15306);
#8240=LINE('',#201124,#15307);
#8241=LINE('',#201125,#15308);
#8242=LINE('',#201129,#15309);
#8243=LINE('',#201131,#15310);
#8244=LINE('',#201133,#15311);
#8245=LINE('',#201134,#15312);
#8246=LINE('',#201138,#15313);
#8247=LINE('',#201139,#15314);
#8248=LINE('',#201140,#15315);
#8249=LINE('',#201144,#15316);
#8250=LINE('',#201145,#15317);
#8251=LINE('',#201146,#15318);
#8252=LINE('',#201148,#15319);
#8253=LINE('',#201149,#15320);
#8254=LINE('',#201153,#15321);
#8255=LINE('',#201155,#15322);
#8256=LINE('',#201157,#15323);
#8257=LINE('',#201158,#15324);
#8258=LINE('',#201162,#15325);
#8259=LINE('',#201163,#15326);
#8260=LINE('',#201164,#15327);
#8261=LINE('',#201168,#15328);
#8262=LINE('',#201169,#15329);
#8263=LINE('',#201170,#15330);
#8264=LINE('',#201172,#15331);
#8265=LINE('',#201173,#15332);
#8266=LINE('',#201177,#15333);
#8267=LINE('',#201179,#15334);
#8268=LINE('',#201181,#15335);
#8269=LINE('',#201182,#15336);
#8270=LINE('',#201186,#15337);
#8271=LINE('',#201187,#15338);
#8272=LINE('',#201188,#15339);
#8273=LINE('',#201192,#15340);
#8274=LINE('',#201193,#15341);
#8275=LINE('',#201194,#15342);
#8276=LINE('',#201196,#15343);
#8277=LINE('',#201197,#15344);
#8278=LINE('',#201201,#15345);
#8279=LINE('',#201203,#15346);
#8280=LINE('',#201205,#15347);
#8281=LINE('',#201206,#15348);
#8282=LINE('',#201210,#15349);
#8283=LINE('',#201211,#15350);
#8284=LINE('',#201212,#15351);
#8285=LINE('',#201216,#15352);
#8286=LINE('',#201217,#15353);
#8287=LINE('',#201218,#15354);
#8288=LINE('',#201220,#15355);
#8289=LINE('',#201221,#15356);
#8290=LINE('',#201225,#15357);
#8291=LINE('',#201227,#15358);
#8292=LINE('',#201229,#15359);
#8293=LINE('',#201230,#15360);
#8294=LINE('',#201234,#15361);
#8295=LINE('',#201235,#15362);
#8296=LINE('',#201236,#15363);
#8297=LINE('',#201240,#15364);
#8298=LINE('',#201241,#15365);
#8299=LINE('',#201242,#15366);
#8300=LINE('',#201244,#15367);
#8301=LINE('',#201245,#15368);
#8302=LINE('',#201249,#15369);
#8303=LINE('',#201251,#15370);
#8304=LINE('',#201253,#15371);
#8305=LINE('',#201254,#15372);
#8306=LINE('',#201258,#15373);
#8307=LINE('',#201259,#15374);
#8308=LINE('',#201260,#15375);
#8309=LINE('',#201264,#15376);
#8310=LINE('',#201265,#15377);
#8311=LINE('',#201266,#15378);
#8312=LINE('',#201268,#15379);
#8313=LINE('',#201269,#15380);
#8314=LINE('',#201273,#15381);
#8315=LINE('',#201275,#15382);
#8316=LINE('',#201277,#15383);
#8317=LINE('',#201278,#15384);
#8318=LINE('',#201282,#15385);
#8319=LINE('',#201283,#15386);
#8320=LINE('',#201284,#15387);
#8321=LINE('',#201288,#15388);
#8322=LINE('',#201289,#15389);
#8323=LINE('',#201290,#15390);
#8324=LINE('',#201292,#15391);
#8325=LINE('',#201293,#15392);
#8326=LINE('',#201297,#15393);
#8327=LINE('',#201299,#15394);
#8328=LINE('',#201301,#15395);
#8329=LINE('',#201302,#15396);
#8330=LINE('',#201306,#15397);
#8331=LINE('',#201307,#15398);
#8332=LINE('',#201308,#15399);
#8333=LINE('',#201312,#15400);
#8334=LINE('',#201313,#15401);
#8335=LINE('',#201314,#15402);
#8336=LINE('',#201316,#15403);
#8337=LINE('',#201317,#15404);
#8338=LINE('',#201321,#15405);
#8339=LINE('',#201323,#15406);
#8340=LINE('',#201325,#15407);
#8341=LINE('',#201326,#15408);
#8342=LINE('',#201330,#15409);
#8343=LINE('',#201331,#15410);
#8344=LINE('',#201332,#15411);
#8345=LINE('',#201336,#15412);
#8346=LINE('',#201337,#15413);
#8347=LINE('',#201338,#15414);
#8348=LINE('',#201340,#15415);
#8349=LINE('',#201341,#15416);
#8350=LINE('',#201345,#15417);
#8351=LINE('',#201347,#15418);
#8352=LINE('',#201349,#15419);
#8353=LINE('',#201350,#15420);
#8354=LINE('',#201354,#15421);
#8355=LINE('',#201355,#15422);
#8356=LINE('',#201356,#15423);
#8357=LINE('',#201360,#15424);
#8358=LINE('',#201361,#15425);
#8359=LINE('',#201362,#15426);
#8360=LINE('',#201364,#15427);
#8361=LINE('',#201365,#15428);
#8362=LINE('',#201369,#15429);
#8363=LINE('',#201371,#15430);
#8364=LINE('',#201373,#15431);
#8365=LINE('',#201374,#15432);
#8366=LINE('',#201378,#15433);
#8367=LINE('',#201379,#15434);
#8368=LINE('',#201380,#15435);
#8369=LINE('',#201384,#15436);
#8370=LINE('',#201385,#15437);
#8371=LINE('',#201386,#15438);
#8372=LINE('',#201388,#15439);
#8373=LINE('',#201389,#15440);
#8374=LINE('',#201393,#15441);
#8375=LINE('',#201395,#15442);
#8376=LINE('',#201397,#15443);
#8377=LINE('',#201398,#15444);
#8378=LINE('',#201402,#15445);
#8379=LINE('',#201403,#15446);
#8380=LINE('',#201404,#15447);
#8381=LINE('',#201408,#15448);
#8382=LINE('',#201409,#15449);
#8383=LINE('',#201410,#15450);
#8384=LINE('',#201412,#15451);
#8385=LINE('',#201413,#15452);
#8386=LINE('',#201417,#15453);
#8387=LINE('',#201419,#15454);
#8388=LINE('',#201421,#15455);
#8389=LINE('',#201422,#15456);
#8390=LINE('',#201426,#15457);
#8391=LINE('',#201427,#15458);
#8392=LINE('',#201428,#15459);
#8393=LINE('',#201432,#15460);
#8394=LINE('',#201433,#15461);
#8395=LINE('',#201434,#15462);
#8396=LINE('',#201436,#15463);
#8397=LINE('',#201437,#15464);
#8398=LINE('',#201441,#15465);
#8399=LINE('',#201443,#15466);
#8400=LINE('',#201445,#15467);
#8401=LINE('',#201446,#15468);
#8402=LINE('',#201450,#15469);
#8403=LINE('',#201451,#15470);
#8404=LINE('',#201452,#15471);
#8405=LINE('',#201456,#15472);
#8406=LINE('',#201457,#15473);
#8407=LINE('',#201458,#15474);
#8408=LINE('',#201460,#15475);
#8409=LINE('',#201461,#15476);
#8410=LINE('',#201465,#15477);
#8411=LINE('',#201467,#15478);
#8412=LINE('',#201469,#15479);
#8413=LINE('',#201470,#15480);
#8414=LINE('',#201474,#15481);
#8415=LINE('',#201475,#15482);
#8416=LINE('',#201476,#15483);
#8417=LINE('',#201480,#15484);
#8418=LINE('',#201481,#15485);
#8419=LINE('',#201482,#15486);
#8420=LINE('',#201484,#15487);
#8421=LINE('',#201485,#15488);
#8422=LINE('',#201489,#15489);
#8423=LINE('',#201491,#15490);
#8424=LINE('',#201493,#15491);
#8425=LINE('',#201494,#15492);
#8426=LINE('',#201498,#15493);
#8427=LINE('',#201499,#15494);
#8428=LINE('',#201500,#15495);
#8429=LINE('',#201504,#15496);
#8430=LINE('',#201505,#15497);
#8431=LINE('',#201506,#15498);
#8432=LINE('',#201508,#15499);
#8433=LINE('',#201509,#15500);
#8434=LINE('',#201513,#15501);
#8435=LINE('',#201515,#15502);
#8436=LINE('',#201517,#15503);
#8437=LINE('',#201518,#15504);
#8438=LINE('',#201522,#15505);
#8439=LINE('',#201523,#15506);
#8440=LINE('',#201524,#15507);
#8441=LINE('',#201528,#15508);
#8442=LINE('',#201529,#15509);
#8443=LINE('',#201530,#15510);
#8444=LINE('',#201532,#15511);
#8445=LINE('',#201533,#15512);
#8446=LINE('',#201537,#15513);
#8447=LINE('',#201539,#15514);
#8448=LINE('',#201541,#15515);
#8449=LINE('',#201542,#15516);
#8450=LINE('',#201546,#15517);
#8451=LINE('',#201547,#15518);
#8452=LINE('',#201548,#15519);
#8453=LINE('',#201552,#15520);
#8454=LINE('',#201553,#15521);
#8455=LINE('',#201554,#15522);
#8456=LINE('',#201556,#15523);
#8457=LINE('',#201557,#15524);
#8458=LINE('',#201561,#15525);
#8459=LINE('',#201563,#15526);
#8460=LINE('',#201565,#15527);
#8461=LINE('',#201566,#15528);
#8462=LINE('',#201570,#15529);
#8463=LINE('',#201571,#15530);
#8464=LINE('',#201572,#15531);
#8465=LINE('',#201576,#15532);
#8466=LINE('',#201577,#15533);
#8467=LINE('',#201578,#15534);
#8468=LINE('',#201580,#15535);
#8469=LINE('',#201581,#15536);
#8470=LINE('',#201585,#15537);
#8471=LINE('',#201587,#15538);
#8472=LINE('',#201589,#15539);
#8473=LINE('',#201590,#15540);
#8474=LINE('',#201594,#15541);
#8475=LINE('',#201595,#15542);
#8476=LINE('',#201596,#15543);
#8477=LINE('',#201600,#15544);
#8478=LINE('',#201601,#15545);
#8479=LINE('',#201602,#15546);
#8480=LINE('',#201604,#15547);
#8481=LINE('',#201605,#15548);
#8482=LINE('',#201609,#15549);
#8483=LINE('',#201611,#15550);
#8484=LINE('',#201613,#15551);
#8485=LINE('',#201614,#15552);
#8486=LINE('',#201618,#15553);
#8487=LINE('',#201619,#15554);
#8488=LINE('',#201620,#15555);
#8489=LINE('',#201624,#15556);
#8490=LINE('',#201625,#15557);
#8491=LINE('',#201626,#15558);
#8492=LINE('',#201628,#15559);
#8493=LINE('',#201629,#15560);
#8494=LINE('',#201633,#15561);
#8495=LINE('',#201635,#15562);
#8496=LINE('',#201637,#15563);
#8497=LINE('',#201638,#15564);
#8498=LINE('',#201642,#15565);
#8499=LINE('',#201643,#15566);
#8500=LINE('',#201644,#15567);
#8501=LINE('',#201648,#15568);
#8502=LINE('',#201649,#15569);
#8503=LINE('',#201650,#15570);
#8504=LINE('',#201652,#15571);
#8505=LINE('',#201653,#15572);
#8506=LINE('',#201657,#15573);
#8507=LINE('',#201659,#15574);
#8508=LINE('',#201661,#15575);
#8509=LINE('',#201662,#15576);
#8510=LINE('',#201666,#15577);
#8511=LINE('',#201667,#15578);
#8512=LINE('',#201668,#15579);
#8513=LINE('',#201672,#15580);
#8514=LINE('',#201673,#15581);
#8515=LINE('',#201674,#15582);
#8516=LINE('',#201676,#15583);
#8517=LINE('',#201677,#15584);
#8518=LINE('',#201681,#15585);
#8519=LINE('',#201683,#15586);
#8520=LINE('',#201685,#15587);
#8521=LINE('',#201686,#15588);
#8522=LINE('',#201690,#15589);
#8523=LINE('',#201691,#15590);
#8524=LINE('',#201692,#15591);
#8525=LINE('',#201696,#15592);
#8526=LINE('',#201697,#15593);
#8527=LINE('',#201698,#15594);
#8528=LINE('',#201700,#15595);
#8529=LINE('',#201701,#15596);
#8530=LINE('',#201705,#15597);
#8531=LINE('',#201707,#15598);
#8532=LINE('',#201709,#15599);
#8533=LINE('',#201710,#15600);
#8534=LINE('',#201714,#15601);
#8535=LINE('',#201715,#15602);
#8536=LINE('',#201716,#15603);
#8537=LINE('',#201720,#15604);
#8538=LINE('',#201721,#15605);
#8539=LINE('',#201722,#15606);
#8540=LINE('',#201724,#15607);
#8541=LINE('',#201725,#15608);
#8542=LINE('',#201729,#15609);
#8543=LINE('',#201731,#15610);
#8544=LINE('',#201733,#15611);
#8545=LINE('',#201734,#15612);
#8546=LINE('',#201738,#15613);
#8547=LINE('',#201739,#15614);
#8548=LINE('',#201740,#15615);
#8549=LINE('',#201744,#15616);
#8550=LINE('',#201745,#15617);
#8551=LINE('',#201746,#15618);
#8552=LINE('',#201748,#15619);
#8553=LINE('',#201749,#15620);
#8554=LINE('',#201753,#15621);
#8555=LINE('',#201755,#15622);
#8556=LINE('',#201757,#15623);
#8557=LINE('',#201758,#15624);
#8558=LINE('',#201762,#15625);
#8559=LINE('',#201763,#15626);
#8560=LINE('',#201764,#15627);
#8561=LINE('',#201768,#15628);
#8562=LINE('',#201769,#15629);
#8563=LINE('',#201770,#15630);
#8564=LINE('',#201772,#15631);
#8565=LINE('',#201773,#15632);
#8566=LINE('',#201777,#15633);
#8567=LINE('',#201779,#15634);
#8568=LINE('',#201781,#15635);
#8569=LINE('',#201782,#15636);
#8570=LINE('',#201786,#15637);
#8571=LINE('',#201787,#15638);
#8572=LINE('',#201788,#15639);
#8573=LINE('',#201792,#15640);
#8574=LINE('',#201793,#15641);
#8575=LINE('',#201794,#15642);
#8576=LINE('',#201796,#15643);
#8577=LINE('',#201797,#15644);
#8578=LINE('',#201801,#15645);
#8579=LINE('',#201803,#15646);
#8580=LINE('',#201805,#15647);
#8581=LINE('',#201806,#15648);
#8582=LINE('',#201810,#15649);
#8583=LINE('',#201811,#15650);
#8584=LINE('',#201812,#15651);
#8585=LINE('',#201816,#15652);
#8586=LINE('',#201817,#15653);
#8587=LINE('',#201818,#15654);
#8588=LINE('',#201820,#15655);
#8589=LINE('',#201821,#15656);
#8590=LINE('',#201825,#15657);
#8591=LINE('',#201827,#15658);
#8592=LINE('',#201829,#15659);
#8593=LINE('',#201830,#15660);
#8594=LINE('',#201834,#15661);
#8595=LINE('',#201835,#15662);
#8596=LINE('',#201836,#15663);
#8597=LINE('',#201840,#15664);
#8598=LINE('',#201841,#15665);
#8599=LINE('',#201842,#15666);
#8600=LINE('',#201844,#15667);
#8601=LINE('',#201845,#15668);
#8602=LINE('',#201849,#15669);
#8603=LINE('',#201851,#15670);
#8604=LINE('',#201853,#15671);
#8605=LINE('',#201854,#15672);
#8606=LINE('',#201858,#15673);
#8607=LINE('',#201859,#15674);
#8608=LINE('',#201860,#15675);
#8609=LINE('',#201864,#15676);
#8610=LINE('',#201865,#15677);
#8611=LINE('',#201866,#15678);
#8612=LINE('',#201868,#15679);
#8613=LINE('',#201869,#15680);
#8614=LINE('',#201873,#15681);
#8615=LINE('',#201875,#15682);
#8616=LINE('',#201877,#15683);
#8617=LINE('',#201878,#15684);
#8618=LINE('',#201882,#15685);
#8619=LINE('',#201883,#15686);
#8620=LINE('',#201884,#15687);
#8621=LINE('',#201888,#15688);
#8622=LINE('',#201889,#15689);
#8623=LINE('',#201890,#15690);
#8624=LINE('',#201892,#15691);
#8625=LINE('',#201893,#15692);
#8626=LINE('',#201897,#15693);
#8627=LINE('',#201899,#15694);
#8628=LINE('',#201901,#15695);
#8629=LINE('',#201902,#15696);
#8630=LINE('',#201906,#15697);
#8631=LINE('',#201907,#15698);
#8632=LINE('',#201908,#15699);
#8633=LINE('',#201912,#15700);
#8634=LINE('',#201913,#15701);
#8635=LINE('',#201914,#15702);
#8636=LINE('',#201916,#15703);
#8637=LINE('',#201917,#15704);
#8638=LINE('',#201921,#15705);
#8639=LINE('',#201923,#15706);
#8640=LINE('',#201925,#15707);
#8641=LINE('',#201926,#15708);
#8642=LINE('',#201930,#15709);
#8643=LINE('',#201931,#15710);
#8644=LINE('',#201932,#15711);
#8645=LINE('',#201936,#15712);
#8646=LINE('',#201937,#15713);
#8647=LINE('',#201938,#15714);
#8648=LINE('',#201940,#15715);
#8649=LINE('',#201941,#15716);
#8650=LINE('',#201945,#15717);
#8651=LINE('',#201947,#15718);
#8652=LINE('',#201949,#15719);
#8653=LINE('',#201950,#15720);
#8654=LINE('',#201954,#15721);
#8655=LINE('',#201955,#15722);
#8656=LINE('',#201956,#15723);
#8657=LINE('',#201960,#15724);
#8658=LINE('',#201961,#15725);
#8659=LINE('',#201962,#15726);
#8660=LINE('',#201964,#15727);
#8661=LINE('',#201965,#15728);
#8662=LINE('',#201969,#15729);
#8663=LINE('',#201971,#15730);
#8664=LINE('',#201973,#15731);
#8665=LINE('',#201974,#15732);
#8666=LINE('',#201978,#15733);
#8667=LINE('',#201979,#15734);
#8668=LINE('',#201980,#15735);
#8669=LINE('',#201984,#15736);
#8670=LINE('',#201985,#15737);
#8671=LINE('',#201986,#15738);
#8672=LINE('',#201988,#15739);
#8673=LINE('',#201989,#15740);
#8674=LINE('',#201993,#15741);
#8675=LINE('',#201995,#15742);
#8676=LINE('',#201997,#15743);
#8677=LINE('',#201998,#15744);
#8678=LINE('',#202002,#15745);
#8679=LINE('',#202003,#15746);
#8680=LINE('',#202004,#15747);
#8681=LINE('',#202008,#15748);
#8682=LINE('',#202009,#15749);
#8683=LINE('',#202010,#15750);
#8684=LINE('',#202012,#15751);
#8685=LINE('',#202013,#15752);
#8686=LINE('',#202017,#15753);
#8687=LINE('',#202019,#15754);
#8688=LINE('',#202021,#15755);
#8689=LINE('',#202022,#15756);
#8690=LINE('',#202026,#15757);
#8691=LINE('',#202027,#15758);
#8692=LINE('',#202028,#15759);
#8693=LINE('',#202032,#15760);
#8694=LINE('',#202033,#15761);
#8695=LINE('',#202034,#15762);
#8696=LINE('',#202036,#15763);
#8697=LINE('',#202037,#15764);
#8698=LINE('',#202041,#15765);
#8699=LINE('',#202043,#15766);
#8700=LINE('',#202045,#15767);
#8701=LINE('',#202046,#15768);
#8702=LINE('',#202050,#15769);
#8703=LINE('',#202051,#15770);
#8704=LINE('',#202052,#15771);
#8705=LINE('',#202056,#15772);
#8706=LINE('',#202057,#15773);
#8707=LINE('',#202058,#15774);
#8708=LINE('',#202060,#15775);
#8709=LINE('',#202061,#15776);
#8710=LINE('',#202065,#15777);
#8711=LINE('',#202067,#15778);
#8712=LINE('',#202069,#15779);
#8713=LINE('',#202070,#15780);
#8714=LINE('',#202074,#15781);
#8715=LINE('',#202075,#15782);
#8716=LINE('',#202076,#15783);
#8717=LINE('',#202080,#15784);
#8718=LINE('',#202081,#15785);
#8719=LINE('',#202082,#15786);
#8720=LINE('',#202084,#15787);
#8721=LINE('',#202085,#15788);
#8722=LINE('',#202089,#15789);
#8723=LINE('',#202091,#15790);
#8724=LINE('',#202093,#15791);
#8725=LINE('',#202094,#15792);
#8726=LINE('',#202098,#15793);
#8727=LINE('',#202099,#15794);
#8728=LINE('',#202100,#15795);
#8729=LINE('',#202104,#15796);
#8730=LINE('',#202105,#15797);
#8731=LINE('',#202106,#15798);
#8732=LINE('',#202108,#15799);
#8733=LINE('',#202109,#15800);
#8734=LINE('',#202113,#15801);
#8735=LINE('',#202115,#15802);
#8736=LINE('',#202117,#15803);
#8737=LINE('',#202118,#15804);
#8738=LINE('',#202122,#15805);
#8739=LINE('',#202123,#15806);
#8740=LINE('',#202124,#15807);
#8741=LINE('',#202128,#15808);
#8742=LINE('',#202129,#15809);
#8743=LINE('',#202130,#15810);
#8744=LINE('',#202132,#15811);
#8745=LINE('',#202133,#15812);
#8746=LINE('',#202137,#15813);
#8747=LINE('',#202139,#15814);
#8748=LINE('',#202141,#15815);
#8749=LINE('',#202142,#15816);
#8750=LINE('',#202146,#15817);
#8751=LINE('',#202147,#15818);
#8752=LINE('',#202148,#15819);
#8753=LINE('',#202152,#15820);
#8754=LINE('',#202153,#15821);
#8755=LINE('',#202154,#15822);
#8756=LINE('',#202156,#15823);
#8757=LINE('',#202157,#15824);
#8758=LINE('',#202161,#15825);
#8759=LINE('',#202163,#15826);
#8760=LINE('',#202165,#15827);
#8761=LINE('',#202166,#15828);
#8762=LINE('',#202170,#15829);
#8763=LINE('',#202171,#15830);
#8764=LINE('',#202172,#15831);
#8765=LINE('',#202176,#15832);
#8766=LINE('',#202177,#15833);
#8767=LINE('',#202178,#15834);
#8768=LINE('',#202180,#15835);
#8769=LINE('',#202181,#15836);
#8770=LINE('',#202185,#15837);
#8771=LINE('',#202187,#15838);
#8772=LINE('',#202189,#15839);
#8773=LINE('',#202190,#15840);
#8774=LINE('',#202194,#15841);
#8775=LINE('',#202195,#15842);
#8776=LINE('',#202196,#15843);
#8777=LINE('',#202200,#15844);
#8778=LINE('',#202201,#15845);
#8779=LINE('',#202202,#15846);
#8780=LINE('',#202204,#15847);
#8781=LINE('',#202205,#15848);
#8782=LINE('',#202209,#15849);
#8783=LINE('',#202211,#15850);
#8784=LINE('',#202213,#15851);
#8785=LINE('',#202214,#15852);
#8786=LINE('',#202218,#15853);
#8787=LINE('',#202219,#15854);
#8788=LINE('',#202220,#15855);
#8789=LINE('',#202224,#15856);
#8790=LINE('',#202225,#15857);
#8791=LINE('',#202226,#15858);
#8792=LINE('',#202228,#15859);
#8793=LINE('',#202229,#15860);
#8794=LINE('',#202233,#15861);
#8795=LINE('',#202235,#15862);
#8796=LINE('',#202237,#15863);
#8797=LINE('',#202238,#15864);
#8798=LINE('',#202242,#15865);
#8799=LINE('',#202243,#15866);
#8800=LINE('',#202244,#15867);
#8801=LINE('',#202248,#15868);
#8802=LINE('',#202249,#15869);
#8803=LINE('',#202250,#15870);
#8804=LINE('',#202252,#15871);
#8805=LINE('',#202253,#15872);
#8806=LINE('',#202257,#15873);
#8807=LINE('',#202259,#15874);
#8808=LINE('',#202261,#15875);
#8809=LINE('',#202262,#15876);
#8810=LINE('',#202266,#15877);
#8811=LINE('',#202267,#15878);
#8812=LINE('',#202268,#15879);
#8813=LINE('',#202272,#15880);
#8814=LINE('',#202273,#15881);
#8815=LINE('',#202274,#15882);
#8816=LINE('',#202276,#15883);
#8817=LINE('',#202277,#15884);
#8818=LINE('',#202281,#15885);
#8819=LINE('',#202283,#15886);
#8820=LINE('',#202285,#15887);
#8821=LINE('',#202286,#15888);
#8822=LINE('',#202290,#15889);
#8823=LINE('',#202291,#15890);
#8824=LINE('',#202292,#15891);
#8825=LINE('',#202296,#15892);
#8826=LINE('',#202297,#15893);
#8827=LINE('',#202298,#15894);
#8828=LINE('',#202300,#15895);
#8829=LINE('',#202301,#15896);
#8830=LINE('',#202305,#15897);
#8831=LINE('',#202307,#15898);
#8832=LINE('',#202309,#15899);
#8833=LINE('',#202310,#15900);
#8834=LINE('',#202314,#15901);
#8835=LINE('',#202315,#15902);
#8836=LINE('',#202316,#15903);
#8837=LINE('',#202320,#15904);
#8838=LINE('',#202321,#15905);
#8839=LINE('',#202322,#15906);
#8840=LINE('',#202324,#15907);
#8841=LINE('',#202325,#15908);
#8842=LINE('',#202329,#15909);
#8843=LINE('',#202331,#15910);
#8844=LINE('',#202333,#15911);
#8845=LINE('',#202334,#15912);
#8846=LINE('',#202338,#15913);
#8847=LINE('',#202339,#15914);
#8848=LINE('',#202340,#15915);
#8849=LINE('',#202344,#15916);
#8850=LINE('',#202345,#15917);
#8851=LINE('',#202346,#15918);
#8852=LINE('',#202348,#15919);
#8853=LINE('',#202349,#15920);
#8854=LINE('',#202353,#15921);
#8855=LINE('',#202355,#15922);
#8856=LINE('',#202357,#15923);
#8857=LINE('',#202358,#15924);
#8858=LINE('',#202362,#15925);
#8859=LINE('',#202363,#15926);
#8860=LINE('',#202364,#15927);
#8861=LINE('',#202368,#15928);
#8862=LINE('',#202369,#15929);
#8863=LINE('',#202370,#15930);
#8864=LINE('',#202372,#15931);
#8865=LINE('',#202373,#15932);
#8866=LINE('',#202377,#15933);
#8867=LINE('',#202379,#15934);
#8868=LINE('',#202381,#15935);
#8869=LINE('',#202382,#15936);
#8870=LINE('',#202386,#15937);
#8871=LINE('',#202387,#15938);
#8872=LINE('',#202388,#15939);
#8873=LINE('',#202392,#15940);
#8874=LINE('',#202393,#15941);
#8875=LINE('',#202394,#15942);
#8876=LINE('',#202396,#15943);
#8877=LINE('',#202397,#15944);
#8878=LINE('',#202401,#15945);
#8879=LINE('',#202403,#15946);
#8880=LINE('',#202405,#15947);
#8881=LINE('',#202406,#15948);
#8882=LINE('',#202410,#15949);
#8883=LINE('',#202411,#15950);
#8884=LINE('',#202412,#15951);
#8885=LINE('',#202416,#15952);
#8886=LINE('',#202417,#15953);
#8887=LINE('',#202418,#15954);
#8888=LINE('',#202420,#15955);
#8889=LINE('',#202421,#15956);
#8890=LINE('',#202425,#15957);
#8891=LINE('',#202427,#15958);
#8892=LINE('',#202429,#15959);
#8893=LINE('',#202430,#15960);
#8894=LINE('',#202434,#15961);
#8895=LINE('',#202435,#15962);
#8896=LINE('',#202436,#15963);
#8897=LINE('',#202440,#15964);
#8898=LINE('',#202441,#15965);
#8899=LINE('',#202442,#15966);
#8900=LINE('',#202444,#15967);
#8901=LINE('',#202445,#15968);
#8902=LINE('',#202449,#15969);
#8903=LINE('',#202451,#15970);
#8904=LINE('',#202453,#15971);
#8905=LINE('',#202454,#15972);
#8906=LINE('',#202458,#15973);
#8907=LINE('',#202459,#15974);
#8908=LINE('',#202460,#15975);
#8909=LINE('',#202464,#15976);
#8910=LINE('',#202465,#15977);
#8911=LINE('',#202466,#15978);
#8912=LINE('',#202468,#15979);
#8913=LINE('',#202469,#15980);
#8914=LINE('',#202473,#15981);
#8915=LINE('',#202475,#15982);
#8916=LINE('',#202477,#15983);
#8917=LINE('',#202478,#15984);
#8918=LINE('',#202482,#15985);
#8919=LINE('',#202483,#15986);
#8920=LINE('',#202484,#15987);
#8921=LINE('',#202488,#15988);
#8922=LINE('',#202489,#15989);
#8923=LINE('',#202490,#15990);
#8924=LINE('',#202492,#15991);
#8925=LINE('',#202493,#15992);
#8926=LINE('',#202497,#15993);
#8927=LINE('',#202499,#15994);
#8928=LINE('',#202501,#15995);
#8929=LINE('',#202502,#15996);
#8930=LINE('',#202506,#15997);
#8931=LINE('',#202507,#15998);
#8932=LINE('',#202508,#15999);
#8933=LINE('',#202512,#16000);
#8934=LINE('',#202513,#16001);
#8935=LINE('',#202514,#16002);
#8936=LINE('',#202516,#16003);
#8937=LINE('',#202517,#16004);
#8938=LINE('',#202521,#16005);
#8939=LINE('',#202523,#16006);
#8940=LINE('',#202525,#16007);
#8941=LINE('',#202526,#16008);
#8942=LINE('',#202530,#16009);
#8943=LINE('',#202531,#16010);
#8944=LINE('',#202532,#16011);
#8945=LINE('',#202536,#16012);
#8946=LINE('',#202537,#16013);
#8947=LINE('',#202538,#16014);
#8948=LINE('',#202540,#16015);
#8949=LINE('',#202541,#16016);
#8950=LINE('',#202545,#16017);
#8951=LINE('',#202547,#16018);
#8952=LINE('',#202549,#16019);
#8953=LINE('',#202550,#16020);
#8954=LINE('',#202554,#16021);
#8955=LINE('',#202555,#16022);
#8956=LINE('',#202556,#16023);
#8957=LINE('',#202560,#16024);
#8958=LINE('',#202561,#16025);
#8959=LINE('',#202562,#16026);
#8960=LINE('',#202564,#16027);
#8961=LINE('',#202565,#16028);
#8962=LINE('',#202569,#16029);
#8963=LINE('',#202571,#16030);
#8964=LINE('',#202573,#16031);
#8965=LINE('',#202574,#16032);
#8966=LINE('',#202578,#16033);
#8967=LINE('',#202579,#16034);
#8968=LINE('',#202580,#16035);
#8969=LINE('',#202584,#16036);
#8970=LINE('',#202585,#16037);
#8971=LINE('',#202586,#16038);
#8972=LINE('',#202588,#16039);
#8973=LINE('',#202589,#16040);
#8974=LINE('',#202593,#16041);
#8975=LINE('',#202595,#16042);
#8976=LINE('',#202597,#16043);
#8977=LINE('',#202598,#16044);
#8978=LINE('',#202602,#16045);
#8979=LINE('',#202603,#16046);
#8980=LINE('',#202604,#16047);
#8981=LINE('',#202608,#16048);
#8982=LINE('',#202609,#16049);
#8983=LINE('',#202610,#16050);
#8984=LINE('',#202612,#16051);
#8985=LINE('',#202613,#16052);
#8986=LINE('',#202617,#16053);
#8987=LINE('',#202619,#16054);
#8988=LINE('',#202621,#16055);
#8989=LINE('',#202622,#16056);
#8990=LINE('',#202626,#16057);
#8991=LINE('',#202627,#16058);
#8992=LINE('',#202628,#16059);
#8993=LINE('',#202632,#16060);
#8994=LINE('',#202633,#16061);
#8995=LINE('',#202634,#16062);
#8996=LINE('',#202636,#16063);
#8997=LINE('',#202637,#16064);
#8998=LINE('',#202641,#16065);
#8999=LINE('',#202643,#16066);
#9000=LINE('',#202645,#16067);
#9001=LINE('',#202646,#16068);
#9002=LINE('',#202650,#16069);
#9003=LINE('',#202651,#16070);
#9004=LINE('',#202652,#16071);
#9005=LINE('',#202656,#16072);
#9006=LINE('',#202657,#16073);
#9007=LINE('',#202658,#16074);
#9008=LINE('',#202660,#16075);
#9009=LINE('',#202661,#16076);
#9010=LINE('',#202665,#16077);
#9011=LINE('',#202667,#16078);
#9012=LINE('',#202669,#16079);
#9013=LINE('',#202670,#16080);
#9014=LINE('',#202674,#16081);
#9015=LINE('',#202675,#16082);
#9016=LINE('',#202676,#16083);
#9017=LINE('',#202680,#16084);
#9018=LINE('',#202681,#16085);
#9019=LINE('',#202682,#16086);
#9020=LINE('',#202684,#16087);
#9021=LINE('',#202685,#16088);
#9022=LINE('',#202689,#16089);
#9023=LINE('',#202691,#16090);
#9024=LINE('',#202693,#16091);
#9025=LINE('',#202694,#16092);
#9026=LINE('',#202698,#16093);
#9027=LINE('',#202699,#16094);
#9028=LINE('',#202700,#16095);
#9029=LINE('',#202704,#16096);
#9030=LINE('',#202705,#16097);
#9031=LINE('',#202706,#16098);
#9032=LINE('',#202708,#16099);
#9033=LINE('',#202709,#16100);
#9034=LINE('',#202713,#16101);
#9035=LINE('',#202715,#16102);
#9036=LINE('',#202717,#16103);
#9037=LINE('',#202718,#16104);
#9038=LINE('',#202722,#16105);
#9039=LINE('',#202723,#16106);
#9040=LINE('',#202724,#16107);
#9041=LINE('',#202728,#16108);
#9042=LINE('',#202729,#16109);
#9043=LINE('',#202730,#16110);
#9044=LINE('',#202732,#16111);
#9045=LINE('',#202733,#16112);
#9046=LINE('',#202737,#16113);
#9047=LINE('',#202739,#16114);
#9048=LINE('',#202741,#16115);
#9049=LINE('',#202742,#16116);
#9050=LINE('',#202746,#16117);
#9051=LINE('',#202747,#16118);
#9052=LINE('',#202748,#16119);
#9053=LINE('',#202752,#16120);
#9054=LINE('',#202753,#16121);
#9055=LINE('',#202754,#16122);
#9056=LINE('',#202756,#16123);
#9057=LINE('',#202757,#16124);
#9058=LINE('',#202761,#16125);
#9059=LINE('',#202763,#16126);
#9060=LINE('',#202765,#16127);
#9061=LINE('',#202766,#16128);
#9062=LINE('',#202770,#16129);
#9063=LINE('',#202771,#16130);
#9064=LINE('',#202772,#16131);
#9065=LINE('',#202776,#16132);
#9066=LINE('',#202777,#16133);
#9067=LINE('',#202778,#16134);
#9068=LINE('',#202780,#16135);
#9069=LINE('',#202781,#16136);
#9070=LINE('',#202785,#16137);
#9071=LINE('',#202787,#16138);
#9072=LINE('',#202789,#16139);
#9073=LINE('',#202790,#16140);
#9074=LINE('',#202794,#16141);
#9075=LINE('',#202795,#16142);
#9076=LINE('',#202796,#16143);
#9077=LINE('',#202800,#16144);
#9078=LINE('',#202801,#16145);
#9079=LINE('',#202802,#16146);
#9080=LINE('',#202804,#16147);
#9081=LINE('',#202805,#16148);
#9082=LINE('',#202809,#16149);
#9083=LINE('',#202811,#16150);
#9084=LINE('',#202813,#16151);
#9085=LINE('',#202814,#16152);
#9086=LINE('',#202818,#16153);
#9087=LINE('',#202819,#16154);
#9088=LINE('',#202820,#16155);
#9089=LINE('',#202824,#16156);
#9090=LINE('',#202825,#16157);
#9091=LINE('',#202826,#16158);
#9092=LINE('',#202828,#16159);
#9093=LINE('',#202829,#16160);
#9094=LINE('',#202833,#16161);
#9095=LINE('',#202835,#16162);
#9096=LINE('',#202837,#16163);
#9097=LINE('',#202838,#16164);
#9098=LINE('',#202842,#16165);
#9099=LINE('',#202843,#16166);
#9100=LINE('',#202844,#16167);
#9101=LINE('',#202848,#16168);
#9102=LINE('',#202849,#16169);
#9103=LINE('',#202850,#16170);
#9104=LINE('',#202852,#16171);
#9105=LINE('',#202853,#16172);
#9106=LINE('',#202857,#16173);
#9107=LINE('',#202859,#16174);
#9108=LINE('',#202861,#16175);
#9109=LINE('',#202862,#16176);
#9110=LINE('',#202866,#16177);
#9111=LINE('',#202867,#16178);
#9112=LINE('',#202868,#16179);
#9113=LINE('',#202872,#16180);
#9114=LINE('',#202873,#16181);
#9115=LINE('',#202874,#16182);
#9116=LINE('',#202876,#16183);
#9117=LINE('',#202877,#16184);
#9118=LINE('',#202881,#16185);
#9119=LINE('',#202883,#16186);
#9120=LINE('',#202885,#16187);
#9121=LINE('',#202886,#16188);
#9122=LINE('',#202890,#16189);
#9123=LINE('',#202891,#16190);
#9124=LINE('',#202892,#16191);
#9125=LINE('',#202896,#16192);
#9126=LINE('',#202897,#16193);
#9127=LINE('',#202898,#16194);
#9128=LINE('',#202900,#16195);
#9129=LINE('',#202901,#16196);
#9130=LINE('',#202905,#16197);
#9131=LINE('',#202907,#16198);
#9132=LINE('',#202909,#16199);
#9133=LINE('',#202910,#16200);
#9134=LINE('',#202914,#16201);
#9135=LINE('',#202915,#16202);
#9136=LINE('',#202916,#16203);
#9137=LINE('',#202920,#16204);
#9138=LINE('',#202921,#16205);
#9139=LINE('',#202922,#16206);
#9140=LINE('',#202924,#16207);
#9141=LINE('',#202925,#16208);
#9142=LINE('',#202929,#16209);
#9143=LINE('',#202931,#16210);
#9144=LINE('',#202933,#16211);
#9145=LINE('',#202934,#16212);
#9146=LINE('',#202938,#16213);
#9147=LINE('',#202939,#16214);
#9148=LINE('',#202940,#16215);
#9149=LINE('',#202944,#16216);
#9150=LINE('',#202945,#16217);
#9151=LINE('',#202946,#16218);
#9152=LINE('',#202948,#16219);
#9153=LINE('',#202949,#16220);
#9154=LINE('',#202953,#16221);
#9155=LINE('',#202955,#16222);
#9156=LINE('',#202957,#16223);
#9157=LINE('',#202958,#16224);
#9158=LINE('',#202962,#16225);
#9159=LINE('',#202963,#16226);
#9160=LINE('',#202964,#16227);
#9161=LINE('',#202968,#16228);
#9162=LINE('',#202969,#16229);
#9163=LINE('',#202970,#16230);
#9164=LINE('',#202972,#16231);
#9165=LINE('',#202973,#16232);
#9166=LINE('',#202977,#16233);
#9167=LINE('',#202979,#16234);
#9168=LINE('',#202981,#16235);
#9169=LINE('',#202982,#16236);
#9170=LINE('',#202986,#16237);
#9171=LINE('',#202987,#16238);
#9172=LINE('',#202988,#16239);
#9173=LINE('',#202992,#16240);
#9174=LINE('',#202993,#16241);
#9175=LINE('',#202994,#16242);
#9176=LINE('',#202996,#16243);
#9177=LINE('',#202997,#16244);
#9178=LINE('',#203001,#16245);
#9179=LINE('',#203003,#16246);
#9180=LINE('',#203005,#16247);
#9181=LINE('',#203006,#16248);
#9182=LINE('',#203010,#16249);
#9183=LINE('',#203011,#16250);
#9184=LINE('',#203012,#16251);
#9185=LINE('',#203016,#16252);
#9186=LINE('',#203017,#16253);
#9187=LINE('',#203018,#16254);
#9188=LINE('',#203020,#16255);
#9189=LINE('',#203021,#16256);
#9190=LINE('',#203025,#16257);
#9191=LINE('',#203027,#16258);
#9192=LINE('',#203029,#16259);
#9193=LINE('',#203030,#16260);
#9194=LINE('',#203034,#16261);
#9195=LINE('',#203035,#16262);
#9196=LINE('',#203036,#16263);
#9197=LINE('',#203040,#16264);
#9198=LINE('',#203041,#16265);
#9199=LINE('',#203042,#16266);
#9200=LINE('',#203044,#16267);
#9201=LINE('',#203045,#16268);
#9202=LINE('',#203049,#16269);
#9203=LINE('',#203051,#16270);
#9204=LINE('',#203053,#16271);
#9205=LINE('',#203054,#16272);
#9206=LINE('',#203058,#16273);
#9207=LINE('',#203059,#16274);
#9208=LINE('',#203060,#16275);
#9209=LINE('',#203064,#16276);
#9210=LINE('',#203065,#16277);
#9211=LINE('',#203066,#16278);
#9212=LINE('',#203068,#16279);
#9213=LINE('',#203069,#16280);
#9214=LINE('',#203073,#16281);
#9215=LINE('',#203075,#16282);
#9216=LINE('',#203077,#16283);
#9217=LINE('',#203078,#16284);
#9218=LINE('',#203082,#16285);
#9219=LINE('',#203083,#16286);
#9220=LINE('',#203084,#16287);
#9221=LINE('',#203088,#16288);
#9222=LINE('',#203089,#16289);
#9223=LINE('',#203090,#16290);
#9224=LINE('',#203092,#16291);
#9225=LINE('',#203093,#16292);
#9226=LINE('',#203097,#16293);
#9227=LINE('',#203099,#16294);
#9228=LINE('',#203101,#16295);
#9229=LINE('',#203102,#16296);
#9230=LINE('',#203106,#16297);
#9231=LINE('',#203107,#16298);
#9232=LINE('',#203108,#16299);
#9233=LINE('',#203112,#16300);
#9234=LINE('',#203113,#16301);
#9235=LINE('',#203114,#16302);
#9236=LINE('',#203116,#16303);
#9237=LINE('',#203117,#16304);
#9238=LINE('',#203121,#16305);
#9239=LINE('',#203123,#16306);
#9240=LINE('',#203125,#16307);
#9241=LINE('',#203126,#16308);
#9242=LINE('',#203130,#16309);
#9243=LINE('',#203131,#16310);
#9244=LINE('',#203132,#16311);
#9245=LINE('',#203136,#16312);
#9246=LINE('',#203137,#16313);
#9247=LINE('',#203138,#16314);
#9248=LINE('',#203140,#16315);
#9249=LINE('',#203141,#16316);
#9250=LINE('',#203145,#16317);
#9251=LINE('',#203147,#16318);
#9252=LINE('',#203149,#16319);
#9253=LINE('',#203150,#16320);
#9254=LINE('',#203154,#16321);
#9255=LINE('',#203155,#16322);
#9256=LINE('',#203156,#16323);
#9257=LINE('',#203160,#16324);
#9258=LINE('',#203161,#16325);
#9259=LINE('',#203162,#16326);
#9260=LINE('',#203164,#16327);
#9261=LINE('',#203165,#16328);
#9262=LINE('',#203169,#16329);
#9263=LINE('',#203171,#16330);
#9264=LINE('',#203173,#16331);
#9265=LINE('',#203174,#16332);
#9266=LINE('',#203178,#16333);
#9267=LINE('',#203179,#16334);
#9268=LINE('',#203180,#16335);
#9269=LINE('',#203184,#16336);
#9270=LINE('',#203185,#16337);
#9271=LINE('',#203186,#16338);
#9272=LINE('',#203188,#16339);
#9273=LINE('',#203189,#16340);
#9274=LINE('',#203193,#16341);
#9275=LINE('',#203195,#16342);
#9276=LINE('',#203197,#16343);
#9277=LINE('',#203198,#16344);
#9278=LINE('',#203202,#16345);
#9279=LINE('',#203203,#16346);
#9280=LINE('',#203204,#16347);
#9281=LINE('',#203208,#16348);
#9282=LINE('',#203209,#16349);
#9283=LINE('',#203210,#16350);
#9284=LINE('',#203212,#16351);
#9285=LINE('',#203213,#16352);
#9286=LINE('',#203217,#16353);
#9287=LINE('',#203219,#16354);
#9288=LINE('',#203221,#16355);
#9289=LINE('',#203222,#16356);
#9290=LINE('',#203226,#16357);
#9291=LINE('',#203227,#16358);
#9292=LINE('',#203228,#16359);
#9293=LINE('',#203232,#16360);
#9294=LINE('',#203233,#16361);
#9295=LINE('',#203234,#16362);
#9296=LINE('',#203236,#16363);
#9297=LINE('',#203237,#16364);
#9298=LINE('',#203241,#16365);
#9299=LINE('',#203243,#16366);
#9300=LINE('',#203245,#16367);
#9301=LINE('',#203246,#16368);
#9302=LINE('',#203250,#16369);
#9303=LINE('',#203251,#16370);
#9304=LINE('',#203252,#16371);
#9305=LINE('',#203256,#16372);
#9306=LINE('',#203257,#16373);
#9307=LINE('',#203258,#16374);
#9308=LINE('',#203260,#16375);
#9309=LINE('',#203261,#16376);
#9310=LINE('',#203265,#16377);
#9311=LINE('',#203267,#16378);
#9312=LINE('',#203269,#16379);
#9313=LINE('',#203270,#16380);
#9314=LINE('',#203274,#16381);
#9315=LINE('',#203275,#16382);
#9316=LINE('',#203276,#16383);
#9317=LINE('',#203280,#16384);
#9318=LINE('',#203281,#16385);
#9319=LINE('',#203282,#16386);
#9320=LINE('',#203284,#16387);
#9321=LINE('',#203285,#16388);
#9322=LINE('',#203289,#16389);
#9323=LINE('',#203291,#16390);
#9324=LINE('',#203293,#16391);
#9325=LINE('',#203294,#16392);
#9326=LINE('',#203298,#16393);
#9327=LINE('',#203299,#16394);
#9328=LINE('',#203300,#16395);
#9329=LINE('',#203304,#16396);
#9330=LINE('',#203305,#16397);
#9331=LINE('',#203306,#16398);
#9332=LINE('',#203308,#16399);
#9333=LINE('',#203309,#16400);
#9334=LINE('',#203313,#16401);
#9335=LINE('',#203315,#16402);
#9336=LINE('',#203317,#16403);
#9337=LINE('',#203318,#16404);
#9338=LINE('',#203322,#16405);
#9339=LINE('',#203323,#16406);
#9340=LINE('',#203324,#16407);
#9341=LINE('',#203328,#16408);
#9342=LINE('',#203329,#16409);
#9343=LINE('',#203330,#16410);
#9344=LINE('',#203332,#16411);
#9345=LINE('',#203333,#16412);
#9346=LINE('',#203337,#16413);
#9347=LINE('',#203339,#16414);
#9348=LINE('',#203341,#16415);
#9349=LINE('',#203342,#16416);
#9350=LINE('',#203346,#16417);
#9351=LINE('',#203347,#16418);
#9352=LINE('',#203348,#16419);
#9353=LINE('',#203352,#16420);
#9354=LINE('',#203353,#16421);
#9355=LINE('',#203354,#16422);
#9356=LINE('',#203356,#16423);
#9357=LINE('',#203357,#16424);
#9358=LINE('',#203361,#16425);
#9359=LINE('',#203363,#16426);
#9360=LINE('',#203365,#16427);
#9361=LINE('',#203366,#16428);
#9362=LINE('',#203370,#16429);
#9363=LINE('',#203371,#16430);
#9364=LINE('',#203372,#16431);
#9365=LINE('',#203376,#16432);
#9366=LINE('',#203377,#16433);
#9367=LINE('',#203378,#16434);
#9368=LINE('',#203380,#16435);
#9369=LINE('',#203381,#16436);
#9370=LINE('',#203385,#16437);
#9371=LINE('',#203387,#16438);
#9372=LINE('',#203389,#16439);
#9373=LINE('',#203390,#16440);
#9374=LINE('',#203394,#16441);
#9375=LINE('',#203395,#16442);
#9376=LINE('',#203396,#16443);
#9377=LINE('',#203400,#16444);
#9378=LINE('',#203401,#16445);
#9379=LINE('',#203402,#16446);
#9380=LINE('',#203404,#16447);
#9381=LINE('',#203405,#16448);
#9382=LINE('',#203409,#16449);
#9383=LINE('',#203411,#16450);
#9384=LINE('',#203413,#16451);
#9385=LINE('',#203414,#16452);
#9386=LINE('',#203418,#16453);
#9387=LINE('',#203419,#16454);
#9388=LINE('',#203420,#16455);
#9389=LINE('',#203424,#16456);
#9390=LINE('',#203425,#16457);
#9391=LINE('',#203426,#16458);
#9392=LINE('',#203428,#16459);
#9393=LINE('',#203429,#16460);
#9394=LINE('',#203433,#16461);
#9395=LINE('',#203435,#16462);
#9396=LINE('',#203437,#16463);
#9397=LINE('',#203438,#16464);
#9398=LINE('',#203442,#16465);
#9399=LINE('',#203443,#16466);
#9400=LINE('',#203444,#16467);
#9401=LINE('',#203448,#16468);
#9402=LINE('',#203449,#16469);
#9403=LINE('',#203450,#16470);
#9404=LINE('',#203452,#16471);
#9405=LINE('',#203453,#16472);
#9406=LINE('',#203457,#16473);
#9407=LINE('',#203459,#16474);
#9408=LINE('',#203461,#16475);
#9409=LINE('',#203462,#16476);
#9410=LINE('',#203466,#16477);
#9411=LINE('',#203467,#16478);
#9412=LINE('',#203468,#16479);
#9413=LINE('',#203472,#16480);
#9414=LINE('',#203473,#16481);
#9415=LINE('',#203474,#16482);
#9416=LINE('',#203476,#16483);
#9417=LINE('',#203477,#16484);
#9418=LINE('',#203481,#16485);
#9419=LINE('',#203483,#16486);
#9420=LINE('',#203485,#16487);
#9421=LINE('',#203486,#16488);
#9422=LINE('',#203490,#16489);
#9423=LINE('',#203491,#16490);
#9424=LINE('',#203492,#16491);
#9425=LINE('',#203496,#16492);
#9426=LINE('',#203497,#16493);
#9427=LINE('',#203498,#16494);
#9428=LINE('',#203500,#16495);
#9429=LINE('',#203501,#16496);
#9430=LINE('',#203505,#16497);
#9431=LINE('',#203507,#16498);
#9432=LINE('',#203509,#16499);
#9433=LINE('',#203510,#16500);
#9434=LINE('',#203514,#16501);
#9435=LINE('',#203515,#16502);
#9436=LINE('',#203516,#16503);
#9437=LINE('',#203520,#16504);
#9438=LINE('',#203521,#16505);
#9439=LINE('',#203522,#16506);
#9440=LINE('',#203524,#16507);
#9441=LINE('',#203525,#16508);
#9442=LINE('',#203529,#16509);
#9443=LINE('',#203531,#16510);
#9444=LINE('',#203533,#16511);
#9445=LINE('',#203534,#16512);
#9446=LINE('',#203538,#16513);
#9447=LINE('',#203539,#16514);
#9448=LINE('',#203540,#16515);
#9449=LINE('',#203544,#16516);
#9450=LINE('',#203545,#16517);
#9451=LINE('',#203546,#16518);
#9452=LINE('',#203548,#16519);
#9453=LINE('',#203549,#16520);
#9454=LINE('',#203553,#16521);
#9455=LINE('',#203555,#16522);
#9456=LINE('',#203557,#16523);
#9457=LINE('',#203558,#16524);
#9458=LINE('',#203562,#16525);
#9459=LINE('',#203563,#16526);
#9460=LINE('',#203564,#16527);
#9461=LINE('',#203568,#16528);
#9462=LINE('',#203569,#16529);
#9463=LINE('',#203570,#16530);
#9464=LINE('',#203572,#16531);
#9465=LINE('',#203573,#16532);
#9466=LINE('',#203577,#16533);
#9467=LINE('',#203579,#16534);
#9468=LINE('',#203581,#16535);
#9469=LINE('',#203582,#16536);
#9470=LINE('',#203586,#16537);
#9471=LINE('',#203587,#16538);
#9472=LINE('',#203588,#16539);
#9473=LINE('',#203592,#16540);
#9474=LINE('',#203593,#16541);
#9475=LINE('',#203594,#16542);
#9476=LINE('',#203596,#16543);
#9477=LINE('',#203597,#16544);
#9478=LINE('',#203601,#16545);
#9479=LINE('',#203603,#16546);
#9480=LINE('',#203605,#16547);
#9481=LINE('',#203606,#16548);
#9482=LINE('',#203610,#16549);
#9483=LINE('',#203611,#16550);
#9484=LINE('',#203612,#16551);
#9485=LINE('',#203616,#16552);
#9486=LINE('',#203617,#16553);
#9487=LINE('',#203618,#16554);
#9488=LINE('',#203620,#16555);
#9489=LINE('',#203621,#16556);
#9490=LINE('',#203625,#16557);
#9491=LINE('',#203627,#16558);
#9492=LINE('',#203629,#16559);
#9493=LINE('',#203630,#16560);
#9494=LINE('',#203634,#16561);
#9495=LINE('',#203635,#16562);
#9496=LINE('',#203636,#16563);
#9497=LINE('',#203640,#16564);
#9498=LINE('',#203641,#16565);
#9499=LINE('',#203642,#16566);
#9500=LINE('',#203644,#16567);
#9501=LINE('',#203645,#16568);
#9502=LINE('',#203649,#16569);
#9503=LINE('',#203651,#16570);
#9504=LINE('',#203653,#16571);
#9505=LINE('',#203654,#16572);
#9506=LINE('',#203658,#16573);
#9507=LINE('',#203659,#16574);
#9508=LINE('',#203660,#16575);
#9509=LINE('',#203664,#16576);
#9510=LINE('',#203665,#16577);
#9511=LINE('',#203666,#16578);
#9512=LINE('',#203668,#16579);
#9513=LINE('',#203669,#16580);
#9514=LINE('',#203673,#16581);
#9515=LINE('',#203675,#16582);
#9516=LINE('',#203677,#16583);
#9517=LINE('',#203678,#16584);
#9518=LINE('',#203682,#16585);
#9519=LINE('',#203683,#16586);
#9520=LINE('',#203684,#16587);
#9521=LINE('',#203688,#16588);
#9522=LINE('',#203689,#16589);
#9523=LINE('',#203690,#16590);
#9524=LINE('',#203692,#16591);
#9525=LINE('',#203693,#16592);
#9526=LINE('',#203697,#16593);
#9527=LINE('',#203699,#16594);
#9528=LINE('',#203701,#16595);
#9529=LINE('',#203702,#16596);
#9530=LINE('',#203706,#16597);
#9531=LINE('',#203707,#16598);
#9532=LINE('',#203708,#16599);
#9533=LINE('',#203712,#16600);
#9534=LINE('',#203713,#16601);
#9535=LINE('',#203714,#16602);
#9536=LINE('',#203716,#16603);
#9537=LINE('',#203717,#16604);
#9538=LINE('',#203721,#16605);
#9539=LINE('',#203723,#16606);
#9540=LINE('',#203725,#16607);
#9541=LINE('',#203726,#16608);
#9542=LINE('',#203730,#16609);
#9543=LINE('',#203731,#16610);
#9544=LINE('',#203732,#16611);
#9545=LINE('',#203736,#16612);
#9546=LINE('',#203737,#16613);
#9547=LINE('',#203738,#16614);
#9548=LINE('',#203740,#16615);
#9549=LINE('',#203741,#16616);
#9550=LINE('',#203745,#16617);
#9551=LINE('',#203747,#16618);
#9552=LINE('',#203749,#16619);
#9553=LINE('',#203750,#16620);
#9554=LINE('',#203754,#16621);
#9555=LINE('',#203755,#16622);
#9556=LINE('',#203756,#16623);
#9557=LINE('',#203760,#16624);
#9558=LINE('',#203761,#16625);
#9559=LINE('',#203762,#16626);
#9560=LINE('',#203764,#16627);
#9561=LINE('',#203765,#16628);
#9562=LINE('',#203769,#16629);
#9563=LINE('',#203771,#16630);
#9564=LINE('',#203773,#16631);
#9565=LINE('',#203774,#16632);
#9566=LINE('',#203778,#16633);
#9567=LINE('',#203779,#16634);
#9568=LINE('',#203780,#16635);
#9569=LINE('',#203784,#16636);
#9570=LINE('',#203785,#16637);
#9571=LINE('',#203786,#16638);
#9572=LINE('',#203788,#16639);
#9573=LINE('',#203789,#16640);
#9574=LINE('',#203793,#16641);
#9575=LINE('',#203795,#16642);
#9576=LINE('',#203797,#16643);
#9577=LINE('',#203798,#16644);
#9578=LINE('',#203802,#16645);
#9579=LINE('',#203803,#16646);
#9580=LINE('',#203804,#16647);
#9581=LINE('',#203808,#16648);
#9582=LINE('',#203809,#16649);
#9583=LINE('',#203810,#16650);
#9584=LINE('',#203812,#16651);
#9585=LINE('',#203813,#16652);
#9586=LINE('',#203817,#16653);
#9587=LINE('',#203819,#16654);
#9588=LINE('',#203821,#16655);
#9589=LINE('',#203822,#16656);
#9590=LINE('',#203826,#16657);
#9591=LINE('',#203827,#16658);
#9592=LINE('',#203828,#16659);
#9593=LINE('',#203832,#16660);
#9594=LINE('',#203833,#16661);
#9595=LINE('',#203834,#16662);
#9596=LINE('',#203836,#16663);
#9597=LINE('',#203837,#16664);
#9598=LINE('',#203841,#16665);
#9599=LINE('',#203843,#16666);
#9600=LINE('',#203845,#16667);
#9601=LINE('',#203846,#16668);
#9602=LINE('',#203850,#16669);
#9603=LINE('',#203851,#16670);
#9604=LINE('',#203852,#16671);
#9605=LINE('',#203856,#16672);
#9606=LINE('',#203857,#16673);
#9607=LINE('',#203858,#16674);
#9608=LINE('',#203860,#16675);
#9609=LINE('',#203861,#16676);
#9610=LINE('',#203865,#16677);
#9611=LINE('',#203867,#16678);
#9612=LINE('',#203869,#16679);
#9613=LINE('',#203870,#16680);
#9614=LINE('',#203874,#16681);
#9615=LINE('',#203875,#16682);
#9616=LINE('',#203876,#16683);
#9617=LINE('',#203880,#16684);
#9618=LINE('',#203881,#16685);
#9619=LINE('',#203882,#16686);
#9620=LINE('',#203884,#16687);
#9621=LINE('',#203885,#16688);
#9622=LINE('',#203890,#16689);
#9623=LINE('',#203892,#16690);
#9624=LINE('',#203894,#16691);
#9625=LINE('',#203895,#16692);
#9626=LINE('',#203898,#16693);
#9627=LINE('',#203900,#16694);
#9628=LINE('',#203901,#16695);
#9629=LINE('',#203904,#16696);
#9630=LINE('',#203905,#16697);
#9631=LINE('',#203908,#16698);
#9632=LINE('',#203909,#16699);
#9633=LINE('',#203911,#16700);
#9634=LINE('',#203915,#16701);
#9635=LINE('',#203917,#16702);
#9636=LINE('',#203919,#16703);
#9637=LINE('',#203921,#16704);
#9638=LINE('',#203925,#16705);
#9639=LINE('',#203927,#16706);
#9640=LINE('',#203929,#16707);
#9641=LINE('',#203931,#16708);
#9642=LINE('',#203948,#16709);
#9643=LINE('',#203950,#16710);
#9644=LINE('',#203954,#16711);
#9645=LINE('',#203958,#16712);
#9646=LINE('',#203970,#16713);
#9647=LINE('',#204037,#16714);
#9648=LINE('',#204089,#16715);
#9649=LINE('',#204141,#16716);
#9650=LINE('',#204283,#16717);
#9651=LINE('',#204417,#16718);
#9652=LINE('',#204554,#16719);
#9653=LINE('',#204693,#16720);
#9654=LINE('',#204831,#16721);
#9655=LINE('',#204967,#16722);
#9656=LINE('',#205096,#16723);
#9657=LINE('',#205110,#16724);
#9658=LINE('',#205244,#16725);
#9659=LINE('',#205387,#16726);
#9660=LINE('',#205552,#16727);
#9661=LINE('',#205712,#16728);
#9662=LINE('',#205879,#16729);
#9663=LINE('',#206044,#16730);
#9664=LINE('',#206207,#16731);
#9665=LINE('',#206216,#16732);
#9666=LINE('',#206225,#16733);
#9667=LINE('',#206303,#16734);
#9668=LINE('',#206419,#16735);
#9669=LINE('',#206439,#16736);
#9670=LINE('',#206521,#16737);
#9671=LINE('',#206589,#16738);
#9672=LINE('',#206737,#16739);
#9673=LINE('',#206881,#16740);
#9674=LINE('',#206897,#16741);
#9675=LINE('',#206975,#16742);
#9676=LINE('',#207043,#16743);
#9677=LINE('',#207171,#16744);
#9678=LINE('',#207317,#16745);
#9679=LINE('',#207334,#16746);
#9680=LINE('',#207487,#16747);
#9681=LINE('',#207645,#16748);
#9682=LINE('',#207803,#16749);
#9683=LINE('',#207835,#16750);
#9684=LINE('',#207937,#16751);
#9685=LINE('',#208019,#16752);
#9686=LINE('',#208181,#16753);
#9687=LINE('',#208339,#16754);
#9688=LINE('',#208471,#16755);
#9689=LINE('',#208573,#16756);
#9690=LINE('',#208591,#16757);
#9691=LINE('',#209012,#16758);
#9692=LINE('',#209296,#16759);
#9693=LINE('',#209335,#16760);
#9694=LINE('',#209953,#16761);
#9695=LINE('',#210222,#16762);
#9696=LINE('',#210314,#16763);
#9697=LINE('',#210389,#16764);
#9698=LINE('',#211295,#16765);
#9699=LINE('',#211789,#16766);
#9700=LINE('',#212058,#16767);
#9701=LINE('',#212479,#16768);
#9702=LINE('',#212636,#16769);
#9703=LINE('',#212641,#16770);
#9704=LINE('',#212650,#16771);
#9705=LINE('',#212654,#16772);
#9706=LINE('',#212787,#16773);
#9707=LINE('',#212793,#16774);
#9708=LINE('',#212860,#16775);
#9709=LINE('',#212912,#16776);
#9710=LINE('',#212962,#16777);
#9711=LINE('',#213102,#16778);
#9712=LINE('',#213238,#16779);
#9713=LINE('',#213381,#16780);
#9714=LINE('',#213518,#16781);
#9715=LINE('',#213654,#16782);
#9716=LINE('',#213790,#16783);
#9717=LINE('',#213917,#16784);
#9718=LINE('',#213931,#16785);
#9719=LINE('',#214065,#16786);
#9720=LINE('',#214206,#16787);
#9721=LINE('',#214371,#16788);
#9722=LINE('',#214529,#16789);
#9723=LINE('',#214696,#16790);
#9724=LINE('',#214861,#16791);
#9725=LINE('',#215024,#16792);
#9726=LINE('',#215033,#16793);
#9727=LINE('',#215042,#16794);
#9728=LINE('',#215120,#16795);
#9729=LINE('',#215236,#16796);
#9730=LINE('',#215256,#16797);
#9731=LINE('',#215342,#16798);
#9732=LINE('',#215414,#16799);
#9733=LINE('',#215564,#16800);
#9734=LINE('',#215710,#16801);
#9735=LINE('',#215726,#16802);
#9736=LINE('',#215804,#16803);
#9737=LINE('',#215878,#16804);
#9738=LINE('',#216014,#16805);
#9739=LINE('',#216152,#16806);
#9740=LINE('',#216169,#16807);
#9741=LINE('',#216322,#16808);
#9742=LINE('',#216480,#16809);
#9743=LINE('',#216638,#16810);
#9744=LINE('',#216670,#16811);
#9745=LINE('',#216774,#16812);
#9746=LINE('',#216856,#16813);
#9747=LINE('',#217016,#16814);
#9748=LINE('',#217176,#16815);
#9749=LINE('',#217308,#16816);
#9750=LINE('',#217410,#16817);
#9751=LINE('',#217428,#16818);
#9752=LINE('',#217843,#16819);
#9753=LINE('',#218127,#16820);
#9754=LINE('',#218166,#16821);
#9755=LINE('',#218784,#16822);
#9756=LINE('',#219053,#16823);
#9757=LINE('',#219145,#16824);
#9758=LINE('',#219220,#16825);
#9759=LINE('',#220124,#16826);
#9760=LINE('',#220620,#16827);
#9761=LINE('',#220889,#16828);
#9762=LINE('',#221310,#16829);
#9763=LINE('',#221467,#16830);
#9764=LINE('',#221472,#16831);
#9765=LINE('',#221481,#16832);
#9766=LINE('',#221485,#16833);
#9767=LINE('',#221618,#16834);
#9768=VECTOR('',#86178,1000.);
#9769=VECTOR('',#86179,1000.);
#9770=VECTOR('',#86198,1000.);
#9771=VECTOR('',#86199,1000.);
#9772=VECTOR('',#86208,1000.);
#9773=VECTOR('',#86213,1000.);
#9774=VECTOR('',#86214,1000.);
#9775=VECTOR('',#86225,1000.);
#9776=VECTOR('',#86232,1000.);
#9777=VECTOR('',#86235,1000.);
#9778=VECTOR('',#86242,8.4);
#9779=VECTOR('',#86247,8.4);
#9780=VECTOR('',#86250,8.4);
#9781=VECTOR('',#86253,8.4);
#9782=VECTOR('',#86258,8.4);
#9783=VECTOR('',#86261,8.4);
#9784=VECTOR('',#86266,17.);
#9785=VECTOR('',#86267,1000.);
#9786=VECTOR('',#86270,17.);
#9787=VECTOR('',#86273,17.);
#9788=VECTOR('',#86276,17.);
#9789=VECTOR('',#86279,17.);
#9790=VECTOR('',#86284,16.375);
#9791=VECTOR('',#86285,1000.);
#9792=VECTOR('',#86286,16.375);
#9793=VECTOR('',#86293,16.375);
#9794=VECTOR('',#86296,16.375);
#9795=VECTOR('',#86329,1000.);
#9796=VECTOR('',#86330,1000.);
#9797=VECTOR('',#86343,10.);
#9798=VECTOR('',#86346,10.);
#9799=VECTOR('',#86351,10.5);
#9800=VECTOR('',#86366,11.25);
#9801=VECTOR('',#86389,1000.);
#9802=VECTOR('',#86390,1000.);
#9803=VECTOR('',#86395,21.);
#9804=VECTOR('',#86410,1000.);
#9805=VECTOR('',#86411,1000.);
#9806=VECTOR('',#86428,9.500000000001);
#9807=VECTOR('',#86443,7.75);
#9808=VECTOR('',#86450,6.5);
#9809=VECTOR('',#86461,9.5);
#9810=VECTOR('',#86470,13.5);
#9811=VECTOR('',#86477,13.79977495601);
#9812=VECTOR('',#86484,14.5);
#9813=VECTOR('',#86491,7.25000000000001);
#9814=VECTOR('',#86514,6.5);
#9815=VECTOR('',#86519,5.799851372624);
#9816=VECTOR('',#86530,5.5);
#9817=VECTOR('',#86541,1000.);
#9818=VECTOR('',#86544,1000.);
#9819=VECTOR('',#86551,16.);
#9820=VECTOR('',#86558,16.375);
#9821=VECTOR('',#86563,17.175);
#9822=VECTOR('',#86580,9.49999999999999);
#9823=VECTOR('',#86591,12.);
#9824=VECTOR('',#86598,1000.);
#9825=VECTOR('',#86601,1000.);
#9826=VECTOR('',#86602,1000.);
#9827=VECTOR('',#86607,1000.);
#9828=VECTOR('',#86608,1000.);
#9829=VECTOR('',#86613,10.25);
#9830=VECTOR('',#86620,11.75);
#9831=VECTOR('',#86627,11.25);
#9832=VECTOR('',#86634,7.75000000000001);
#9833=VECTOR('',#86643,7.75000000000001);
#9834=VECTOR('',#86646,7.95);
#9835=VECTOR('',#86663,9.49999999999999);
#9836=VECTOR('',#86674,12.);
#9837=VECTOR('',#86679,1000.);
#9838=VECTOR('',#86682,1000.);
#9839=VECTOR('',#86685,1000.);
#9840=VECTOR('',#86688,1000.);
#9841=VECTOR('',#86691,1000.);
#9842=VECTOR('',#86696,10.25);
#9843=VECTOR('',#86703,11.75);
#9844=VECTOR('',#86710,11.25);
#9845=VECTOR('',#86717,7.75000000000001);
#9846=VECTOR('',#86726,7.75000000000001);
#9847=VECTOR('',#86729,7.95);
#9848=VECTOR('',#86734,1000.);
#9849=VECTOR('',#86735,1000.);
#9850=VECTOR('',#86736,1000.);
#9851=VECTOR('',#86737,1000.);
#9852=VECTOR('',#86738,1000.);
#9853=VECTOR('',#86739,1000.);
#9854=VECTOR('',#86742,1000.);
#9855=VECTOR('',#86743,1000.);
#9856=VECTOR('',#86746,1000.);
#9857=VECTOR('',#86749,1000.);
#9858=VECTOR('',#86752,1000.);
#9859=VECTOR('',#86755,1000.);
#9860=VECTOR('',#86764,1000.);
#9861=VECTOR('',#86767,1000.);
#9862=VECTOR('',#86786,1000.);
#9863=VECTOR('',#86787,1000.);
#9864=VECTOR('',#86790,1000.);
#9865=VECTOR('',#86795,1000.);
#9866=VECTOR('',#86802,1000.);
#9867=VECTOR('',#86807,1000.);
#9868=VECTOR('',#86810,1000.);
#9869=VECTOR('',#86813,1000.);
#9870=VECTOR('',#86820,1000.);
#9871=VECTOR('',#86821,1000.);
#9872=VECTOR('',#86856,1000.);
#9873=VECTOR('',#86879,1000.);
#9874=VECTOR('',#86898,10.);
#9875=VECTOR('',#86921,10.);
#9876=VECTOR('',#86924,1000.);
#9877=VECTOR('',#86939,1000.);
#9878=VECTOR('',#86950,1000.);
#9879=VECTOR('',#86979,10.);
#9880=VECTOR('',#86980,10.);
#9881=VECTOR('',#86981,10.);
#9882=VECTOR('',#86986,1000.);
#9883=VECTOR('',#86987,1000.);
#9884=VECTOR('',#86988,1000.);
#9885=VECTOR('',#86989,1000.);
#9886=VECTOR('',#86990,1000.);
#9887=VECTOR('',#86991,1000.);
#9888=VECTOR('',#86994,1000.);
#9889=VECTOR('',#86995,1000.);
#9890=VECTOR('',#86998,1000.);
#9891=VECTOR('',#87001,1000.);
#9892=VECTOR('',#87004,1000.);
#9893=VECTOR('',#87007,1000.);
#9894=VECTOR('',#87016,1000.);
#9895=VECTOR('',#87019,1000.);
#9896=VECTOR('',#87028,1000.);
#9897=VECTOR('',#87031,1000.);
#9898=VECTOR('',#87034,1000.);
#9899=VECTOR('',#87039,1000.);
#9900=VECTOR('',#87042,1000.);
#9901=VECTOR('',#87049,1000.);
#9902=VECTOR('',#87050,1000.);
#9903=VECTOR('',#87065,1000.);
#9904=VECTOR('',#87070,1000.);
#9905=VECTOR('',#87093,1000.);
#9906=VECTOR('',#87116,1000.);
#9907=VECTOR('',#87145,10.);
#9908=VECTOR('',#87166,1000.);
#9909=VECTOR('',#87169,10.);
#9910=VECTOR('',#87192,1000.);
#9911=VECTOR('',#87195,1000.);
#9912=VECTOR('',#87230,10.);
#9913=VECTOR('',#87231,10.);
#9914=VECTOR('',#87232,10.);
#9915=VECTOR('',#87235,10.);
#9916=VECTOR('',#87236,10.);
#9917=VECTOR('',#87245,1000.);
#9918=VECTOR('',#87246,1000.);
#9919=VECTOR('',#87247,1000.);
#9920=VECTOR('',#87248,1000.);
#9921=VECTOR('',#87261,1000.);
#9922=VECTOR('',#87262,1000.);
#9923=VECTOR('',#87263,1000.);
#9924=VECTOR('',#87274,1000.);
#9925=VECTOR('',#87277,1000.);
#9926=VECTOR('',#87278,1000.);
#9927=VECTOR('',#87283,1000.);
#9928=VECTOR('',#87284,1000.);
#9929=VECTOR('',#87293,10.);
#9930=VECTOR('',#87298,1000.);
#9931=VECTOR('',#87299,10.);
#9932=VECTOR('',#87300,1000.);
#9933=VECTOR('',#87301,1000.);
#9934=VECTOR('',#87306,10.);
#9935=VECTOR('',#87309,1000.);
#9936=VECTOR('',#87314,10.);
#9937=VECTOR('',#87319,1000.);
#9938=VECTOR('',#87322,10.);
#9939=VECTOR('',#87325,10.);
#9940=VECTOR('',#87328,1000.);
#9941=VECTOR('',#87335,1000.);
#9942=VECTOR('',#87338,1000.);
#9943=VECTOR('',#87351,1000.);
#9944=VECTOR('',#87398,1000.);
#9945=VECTOR('',#87411,1000.);
#9946=VECTOR('',#87414,1000.);
#9947=VECTOR('',#87415,1000.);
#9948=VECTOR('',#87416,1000.);
#9949=VECTOR('',#87417,1000.);
#9950=VECTOR('',#87434,1000.);
#9951=VECTOR('',#87437,1000.);
#9952=VECTOR('',#87438,1000.);
#9953=VECTOR('',#87461,1000.);
#9954=VECTOR('',#87472,1000.);
#9955=VECTOR('',#87473,1000.);
#9956=VECTOR('',#87476,1000.);
#9957=VECTOR('',#87477,1000.);
#9958=VECTOR('',#87492,1000.);
#9959=VECTOR('',#87497,1000.);
#9960=VECTOR('',#87502,1000.);
#9961=VECTOR('',#87505,1000.);
#9962=VECTOR('',#87510,1000.);
#9963=VECTOR('',#87521,1000.);
#9964=VECTOR('',#87522,1000.);
#9965=VECTOR('',#87527,1000.);
#9966=VECTOR('',#87528,1000.);
#9967=VECTOR('',#87533,1000.);
#9968=VECTOR('',#87534,1000.);
#9969=VECTOR('',#87545,1000.);
#9970=VECTOR('',#87560,1000.);
#9971=VECTOR('',#87571,1000.);
#9972=VECTOR('',#87574,1000.);
#9973=VECTOR('',#87595,1000.);
#9974=VECTOR('',#87610,1000.);
#9975=VECTOR('',#87625,1000.);
#9976=VECTOR('',#87656,1000.);
#9977=VECTOR('',#87679,1000.);
#9978=VECTOR('',#87682,1000.);
#9979=VECTOR('',#87685,1000.);
#9980=VECTOR('',#87686,1000.);
#9981=VECTOR('',#87689,1000.);
#9982=VECTOR('',#87698,1000.);
#9983=VECTOR('',#87701,1000.);
#9984=VECTOR('',#87702,1000.);
#9985=VECTOR('',#87703,1000.);
#9986=VECTOR('',#87712,1000.);
#9987=VECTOR('',#87727,1000.);
#9988=VECTOR('',#87740,10.);
#9989=VECTOR('',#87743,10.);
#9990=VECTOR('',#87748,1000.);
#9991=VECTOR('',#87751,1000.);
#9992=VECTOR('',#87754,1000.);
#9993=VECTOR('',#87755,1000.);
#9994=VECTOR('',#87776,1000.);
#9995=VECTOR('',#87779,1000.);
#9996=VECTOR('',#87780,1000.);
#9997=VECTOR('',#87781,1000.);
#9998=VECTOR('',#87782,1000.);
#9999=VECTOR('',#87783,1000.);
#10000=VECTOR('',#87810,1000.);
#10001=VECTOR('',#87813,1000.);
#10002=VECTOR('',#87814,1000.);
#10003=VECTOR('',#87817,1000.);
#10004=VECTOR('',#87818,1000.);
#10005=VECTOR('',#87819,1000.);
#10006=VECTOR('',#87844,10.);
#10007=VECTOR('',#87855,10.);
#10008=VECTOR('',#87856,1000.);
#10009=VECTOR('',#87909,1000.);
#10010=VECTOR('',#87914,1000.);
#10011=VECTOR('',#87915,1000.);
#10012=VECTOR('',#87918,1000.);
#10013=VECTOR('',#87935,1000.);
#10014=VECTOR('',#87940,1000.);
#10015=VECTOR('',#87941,1000.);
#10016=VECTOR('',#87942,1000.);
#10017=VECTOR('',#87945,1000.);
#10018=VECTOR('',#88084,1000.);
#10019=VECTOR('',#88089,1000.);
#10020=VECTOR('',#88092,1000.);
#10021=VECTOR('',#88141,1000.);
#10022=VECTOR('',#88150,1000.);
#10023=VECTOR('',#88225,21.5);
#10024=VECTOR('',#88226,21.5);
#10025=VECTOR('',#88235,10.);
#10026=VECTOR('',#88236,10.);
#10027=VECTOR('',#88243,20.);
#10028=VECTOR('',#88244,20.);
#10029=VECTOR('',#88253,3.40000000000001);
#10030=VECTOR('',#88282,2.15);
#10031=VECTOR('',#88287,1000.);
#10032=VECTOR('',#88288,1000.);
#10033=VECTOR('',#88289,1000.);
#10034=VECTOR('',#88290,1000.);
#10035=VECTOR('',#88297,1000.);
#10036=VECTOR('',#88302,1000.);
#10037=VECTOR('',#88307,1000.);
#10038=VECTOR('',#88310,1000.);
#10039=VECTOR('',#88315,1000.);
#10040=VECTOR('',#88318,1000.);
#10041=VECTOR('',#88321,1000.);
#10042=VECTOR('',#88322,1000.);
#10043=VECTOR('',#88327,1000.);
#10044=VECTOR('',#88328,1000.);
#10045=VECTOR('',#88331,1000.);
#10046=VECTOR('',#88336,1000.);
#10047=VECTOR('',#88339,1000.);
#10048=VECTOR('',#88340,1000.);
#10049=VECTOR('',#88341,1000.);
#10050=VECTOR('',#88342,1000.);
#10051=VECTOR('',#88347,1000.);
#10052=VECTOR('',#88352,1000.);
#10053=VECTOR('',#88353,1000.);
#10054=VECTOR('',#88354,1000.);
#10055=VECTOR('',#88359,1000.);
#10056=VECTOR('',#88364,1000.);
#10057=VECTOR('',#88365,1000.);
#10058=VECTOR('',#88366,1000.);
#10059=VECTOR('',#88373,1000.);
#10060=VECTOR('',#88384,1000.);
#10061=VECTOR('',#88395,1000.);
#10062=VECTOR('',#88406,1000.);
#10063=VECTOR('',#88411,1000.);
#10064=VECTOR('',#88412,1000.);
#10065=VECTOR('',#88413,1000.);
#10066=VECTOR('',#88420,1000.);
#10067=VECTOR('',#88429,1000.);
#10068=VECTOR('',#88430,1000.);
#10069=VECTOR('',#88435,1000.);
#10070=VECTOR('',#88436,1000.);
#10071=VECTOR('',#88437,1000.);
#10072=VECTOR('',#88444,1000.);
#10073=VECTOR('',#88451,1000.);
#10074=VECTOR('',#88462,1000.);
#10075=VECTOR('',#88465,1000.);
#10076=VECTOR('',#88466,1000.);
#10077=VECTOR('',#88473,1000.);
#10078=VECTOR('',#88476,1000.);
#10079=VECTOR('',#88477,1000.);
#10080=VECTOR('',#88478,1000.);
#10081=VECTOR('',#88479,1000.);
#10082=VECTOR('',#88480,1000.);
#10083=VECTOR('',#88481,1000.);
#10084=VECTOR('',#88482,1000.);
#10085=VECTOR('',#88483,1000.);
#10086=VECTOR('',#88486,1000.);
#10087=VECTOR('',#88487,1000.);
#10088=VECTOR('',#88488,1000.);
#10089=VECTOR('',#88491,1000.);
#10090=VECTOR('',#88492,1000.);
#10091=VECTOR('',#88495,1000.);
#10092=VECTOR('',#88496,1000.);
#10093=VECTOR('',#88499,1000.);
#10094=VECTOR('',#88500,1000.);
#10095=VECTOR('',#88503,1000.);
#10096=VECTOR('',#88504,1000.);
#10097=VECTOR('',#88507,1000.);
#10098=VECTOR('',#88508,1000.);
#10099=VECTOR('',#88511,1000.);
#10100=VECTOR('',#88512,1000.);
#10101=VECTOR('',#88515,1000.);
#10102=VECTOR('',#88522,1000.);
#10103=VECTOR('',#88523,1000.);
#10104=VECTOR('',#88538,1000.);
#10105=VECTOR('',#88545,1000.);
#10106=VECTOR('',#88554,1000.);
#10107=VECTOR('',#88567,1000.);
#10108=VECTOR('',#88588,9.35000000000001);
#10109=VECTOR('',#88593,9.35000000000001);
#10110=VECTOR('',#88596,9.35000000000001);
#10111=VECTOR('',#88599,9.35000000000001);
#10112=VECTOR('',#88602,9.35000000000001);
#10113=VECTOR('',#88605,9.35000000000001);
#10114=VECTOR('',#88608,9.35000000000001);
#10115=VECTOR('',#88613,9.50000000000001);
#10116=VECTOR('',#88618,9.50000000000001);
#10117=VECTOR('',#88621,9.50000000000001);
#10118=VECTOR('',#88624,9.50000000000001);
#10119=VECTOR('',#88627,9.50000000000001);
#10120=VECTOR('',#88630,9.50000000000001);
#10121=VECTOR('',#88633,9.50000000000001);
#10122=VECTOR('',#88636,9.5);
#10123=VECTOR('',#88641,10.);
#10124=VECTOR('',#88646,10.);
#10125=VECTOR('',#88649,10.);
#10126=VECTOR('',#88652,10.);
#10127=VECTOR('',#88655,10.);
#10128=VECTOR('',#88658,10.25);
#10129=VECTOR('',#88663,10.25);
#10130=VECTOR('',#88666,10.25);
#10131=VECTOR('',#88669,10.25);
#10132=VECTOR('',#88672,10.25);
#10133=VECTOR('',#88675,10.25);
#10134=VECTOR('',#88678,7.25);
#10135=VECTOR('',#88689,9.25000000000001);
#10136=VECTOR('',#88698,11.);
#10137=VECTOR('',#88705,9.15);
#10138=VECTOR('',#88716,10.25);
#10139=VECTOR('',#88723,9.99999999999999);
#10140=VECTOR('',#88728,7.75);
#10141=VECTOR('',#88737,6.5);
#10142=VECTOR('',#88756,1000.);
#10143=VECTOR('',#88759,1000.);
#10144=VECTOR('',#88766,10.25);
#10145=VECTOR('',#88775,1000.);
#10146=VECTOR('',#88776,1000.);
#10147=VECTOR('',#88777,1000.);
#10148=VECTOR('',#88780,1000.);
#10149=VECTOR('',#88781,1000.);
#10150=VECTOR('',#88782,1000.);
#10151=VECTOR('',#88785,1000.);
#10152=VECTOR('',#88786,1000.);
#10153=VECTOR('',#88787,1000.);
#10154=VECTOR('',#88792,1000.);
#10155=VECTOR('',#88797,1000.);
#10156=VECTOR('',#88798,1000.);
#10157=VECTOR('',#88799,1000.);
#10158=VECTOR('',#88802,1000.);
#10159=VECTOR('',#88803,1000.);
#10160=VECTOR('',#88804,1000.);
#10161=VECTOR('',#88807,1000.);
#10162=VECTOR('',#88808,1000.);
#10163=VECTOR('',#88815,1000.);
#10164=VECTOR('',#88816,1000.);
#10165=VECTOR('',#88817,1000.);
#10166=VECTOR('',#88818,1000.);
#10167=VECTOR('',#88819,1000.);
#10168=VECTOR('',#88820,1000.);
#10169=VECTOR('',#88823,1000.);
#10170=VECTOR('',#88824,1000.);
#10171=VECTOR('',#88827,1000.);
#10172=VECTOR('',#88830,1000.);
#10173=VECTOR('',#88833,1000.);
#10174=VECTOR('',#88836,1000.);
#10175=VECTOR('',#88869,12.1);
#10176=VECTOR('',#88872,1000.);
#10177=VECTOR('',#88875,1000.);
#10178=VECTOR('',#88878,1000.);
#10179=VECTOR('',#88881,1000.);
#10180=VECTOR('',#88884,1000.);
#10181=VECTOR('',#88887,1000.);
#10182=VECTOR('',#88910,7.50000000000001);
#10183=VECTOR('',#88953,13.0486498132185);
#10184=VECTOR('',#88954,10.);
#10185=VECTOR('',#88957,13.0486498132185);
#10186=VECTOR('',#88960,13.0486498132185);
#10187=VECTOR('',#88963,12.25);
#10188=VECTOR('',#88964,10.);
#10189=VECTOR('',#88965,12.25);
#10190=VECTOR('',#88970,12.25);
#10191=VECTOR('',#88973,12.25);
#10192=VECTOR('',#88976,12.25);
#10193=VECTOR('',#88979,12.25);
#10194=VECTOR('',#88986,10.5);
#10195=VECTOR('',#88997,12.750003108);
#10196=VECTOR('',#89012,15.);
#10197=VECTOR('',#89031,15.);
#10198=VECTOR('',#89040,1000.);
#10199=VECTOR('',#89041,1000.);
#10200=VECTOR('',#89044,1000.);
#10201=VECTOR('',#89045,1000.);
#10202=VECTOR('',#89048,1000.);
#10203=VECTOR('',#89051,1000.);
#10204=VECTOR('',#89054,1000.);
#10205=VECTOR('',#89057,1000.);
#10206=VECTOR('',#89060,1000.);
#10207=VECTOR('',#89063,1000.);
#10208=VECTOR('',#89064,1000.);
#10209=VECTOR('',#89069,1000.);
#10210=VECTOR('',#89076,10.);
#10211=VECTOR('',#89077,10.);
#10212=VECTOR('',#89104,12.1);
#10213=VECTOR('',#89107,1000.);
#10214=VECTOR('',#89110,1000.);
#10215=VECTOR('',#89113,1000.);
#10216=VECTOR('',#89116,1000.);
#10217=VECTOR('',#89119,1000.);
#10218=VECTOR('',#89122,1000.);
#10219=VECTOR('',#89145,7.50000000000001);
#10220=VECTOR('',#89196,27.5);
#10221=VECTOR('',#89203,1000.);
#10222=VECTOR('',#89206,1000.);
#10223=VECTOR('',#89225,27.);
#10224=VECTOR('',#89230,15.31367390024);
#10225=VECTOR('',#89243,15.125);
#10226=VECTOR('',#89254,13.0486498132185);
#10227=VECTOR('',#89255,10.);
#10228=VECTOR('',#89258,13.0486498132185);
#10229=VECTOR('',#89261,13.0486498132185);
#10230=VECTOR('',#89264,12.25);
#10231=VECTOR('',#89265,10.);
#10232=VECTOR('',#89266,12.25);
#10233=VECTOR('',#89271,12.25);
#10234=VECTOR('',#89274,12.25);
#10235=VECTOR('',#89277,12.25);
#10236=VECTOR('',#89280,12.25);
#10237=VECTOR('',#89287,10.5);
#10238=VECTOR('',#89298,12.750003108);
#10239=VECTOR('',#89313,15.);
#10240=VECTOR('',#89332,15.);
#10241=VECTOR('',#89341,1000.);
#10242=VECTOR('',#89342,1000.);
#10243=VECTOR('',#89345,1000.);
#10244=VECTOR('',#89346,1000.);
#10245=VECTOR('',#89349,1000.);
#10246=VECTOR('',#89352,1000.);
#10247=VECTOR('',#89355,1000.);
#10248=VECTOR('',#89358,1000.);
#10249=VECTOR('',#89361,1000.);
#10250=VECTOR('',#89364,1000.);
#10251=VECTOR('',#89365,1000.);
#10252=VECTOR('',#89370,1000.);
#10253=VECTOR('',#89377,10.);
#10254=VECTOR('',#89378,10.);
#10255=VECTOR('',#89389,2.05);
#10256=VECTOR('',#89396,2.05);
#10257=VECTOR('',#89401,5.5);
#10258=VECTOR('',#89406,5.5);
#10259=VECTOR('',#89409,5.5);
#10260=VECTOR('',#89412,5.5);
#10261=VECTOR('',#89417,6.);
#10262=VECTOR('',#89422,6.);
#10263=VECTOR('',#89427,7.);
#10264=VECTOR('',#89430,1000.);
#10265=VECTOR('',#89433,1000.);
#10266=VECTOR('',#89436,1000.);
#10267=VECTOR('',#89439,1000.);
#10268=VECTOR('',#89450,5.25);
#10269=VECTOR('',#89463,6.);
#10270=VECTOR('',#89468,4.4);
#10271=VECTOR('',#89479,1000.);
#10272=VECTOR('',#89484,1000.);
#10273=VECTOR('',#89487,2.55);
#10274=VECTOR('',#89492,3.05);
#10275=VECTOR('',#89501,4.9);
#10276=VECTOR('',#89510,6.47238979616114);
#10277=VECTOR('',#89521,6.47238979616113);
#10278=VECTOR('',#89528,9.);
#10279=VECTOR('',#89537,9.99999999999999);
#10280=VECTOR('',#89562,8.);
#10281=VECTOR('',#89575,4.);
#10282=VECTOR('',#89582,2.30850939467147);
#10283=VECTOR('',#89599,1000.);
#10284=VECTOR('',#89602,1000.);
#10285=VECTOR('',#89605,1000.);
#10286=VECTOR('',#89608,1000.);
#10287=VECTOR('',#89633,27.5);
#10288=VECTOR('',#89640,1000.);
#10289=VECTOR('',#89643,1000.);
#10290=VECTOR('',#89662,27.);
#10291=VECTOR('',#89667,15.31367390024);
#10292=VECTOR('',#89680,15.125);
#10293=VECTOR('',#89691,13.9);
#10294=VECTOR('',#89696,13.9);
#10295=VECTOR('',#89701,13.9);
#10296=VECTOR('',#89704,13.9);
#10297=VECTOR('',#89711,11.64412671312);
#10298=VECTOR('',#89730,1000.);
#10299=VECTOR('',#89731,1000.);
#10300=VECTOR('',#89734,1000.);
#10301=VECTOR('',#89735,1000.);
#10302=VECTOR('',#89738,11.05);
#10303=VECTOR('',#89743,11.05);
#10304=VECTOR('',#89764,1000.);
#10305=VECTOR('',#89765,1000.);
#10306=VECTOR('',#89768,1000.);
#10307=VECTOR('',#89769,1000.);
#10308=VECTOR('',#89774,11.35);
#10309=VECTOR('',#89779,11.35);
#10310=VECTOR('',#89808,9.85);
#10311=VECTOR('',#89815,10.15);
#10312=VECTOR('',#89836,11.94412676881);
#10313=VECTOR('',#89841,12.25);
#10314=VECTOR('',#89848,12.75);
#10315=VECTOR('',#89855,13.1);
#10316=VECTOR('',#89862,1000.);
#10317=VECTOR('',#89865,1000.);
#10318=VECTOR('',#89868,1000.);
#10319=VECTOR('',#89871,13.7);
#10320=VECTOR('',#89876,1000.);
#10321=VECTOR('',#89885,12.75);
#10322=VECTOR('',#89888,10.);
#10323=VECTOR('',#89889,10.);
#10324=VECTOR('',#89892,1000.);
#10325=VECTOR('',#89893,1000.);
#10326=VECTOR('',#89904,1000.);
#10327=VECTOR('',#89905,1000.);
#10328=VECTOR('',#89916,10.);
#10329=VECTOR('',#89929,1000.);
#10330=VECTOR('',#89930,1000.);
#10331=VECTOR('',#89931,1000.);
#10332=VECTOR('',#89934,1000.);
#10333=VECTOR('',#89937,1000.);
#10334=VECTOR('',#89946,1000.);
#10335=VECTOR('',#89953,1000.);
#10336=VECTOR('',#89962,1000.);
#10337=VECTOR('',#89963,1000.);
#10338=VECTOR('',#89964,1000.);
#10339=VECTOR('',#89969,1000.);
#10340=VECTOR('',#89972,1000.);
#10341=VECTOR('',#89979,1000.);
#10342=VECTOR('',#89986,1000.);
#10343=VECTOR('',#89993,1000.);
#10344=VECTOR('',#89996,1000.);
#10345=VECTOR('',#90001,1000.);
#10346=VECTOR('',#90002,1000.);
#10347=VECTOR('',#90007,1000.);
#10348=VECTOR('',#90008,1000.);
#10349=VECTOR('',#90015,1000.);
#10350=VECTOR('',#90024,1000.);
#10351=VECTOR('',#90027,1000.);
#10352=VECTOR('',#90032,1000.);
#10353=VECTOR('',#90039,1000.);
#10354=VECTOR('',#90052,1000.);
#10355=VECTOR('',#90055,1000.);
#10356=VECTOR('',#90060,1000.);
#10357=VECTOR('',#90067,1000.);
#10358=VECTOR('',#90080,1000.);
#10359=VECTOR('',#90083,1000.);
#10360=VECTOR('',#90088,1000.);
#10361=VECTOR('',#90095,1000.);
#10362=VECTOR('',#90108,1000.);
#10363=VECTOR('',#90111,1000.);
#10364=VECTOR('',#90116,1000.);
#10365=VECTOR('',#90123,1000.);
#10366=VECTOR('',#90138,1000.);
#10367=VECTOR('',#90139,1000.);
#10368=VECTOR('',#90140,1000.);
#10369=VECTOR('',#90145,1000.);
#10370=VECTOR('',#90148,1000.);
#10371=VECTOR('',#90155,1000.);
#10372=VECTOR('',#90162,1000.);
#10373=VECTOR('',#90169,1000.);
#10374=VECTOR('',#90172,1000.);
#10375=VECTOR('',#90177,1000.);
#10376=VECTOR('',#90178,1000.);
#10377=VECTOR('',#90185,1000.);
#10378=VECTOR('',#90186,1000.);
#10379=VECTOR('',#90193,1000.);
#10380=VECTOR('',#90202,1000.);
#10381=VECTOR('',#90205,1000.);
#10382=VECTOR('',#90210,1000.);
#10383=VECTOR('',#90211,1000.);
#10384=VECTOR('',#90218,1000.);
#10385=VECTOR('',#90219,1000.);
#10386=VECTOR('',#90226,1000.);
#10387=VECTOR('',#90235,1000.);
#10388=VECTOR('',#90238,1000.);
#10389=VECTOR('',#90243,1000.);
#10390=VECTOR('',#90250,1000.);
#10391=VECTOR('',#90251,1000.);
#10392=VECTOR('',#90260,1000.);
#10393=VECTOR('',#90269,1000.);
#10394=VECTOR('',#90272,1000.);
#10395=VECTOR('',#90277,1000.);
#10396=VECTOR('',#90284,1000.);
#10397=VECTOR('',#90297,1000.);
#10398=VECTOR('',#90300,1000.);
#10399=VECTOR('',#90305,1000.);
#10400=VECTOR('',#90306,1000.);
#10401=VECTOR('',#90313,1000.);
#10402=VECTOR('',#90314,1000.);
#10403=VECTOR('',#90321,1000.);
#10404=VECTOR('',#90330,1000.);
#10405=VECTOR('',#90333,1000.);
#10406=VECTOR('',#90338,1000.);
#10407=VECTOR('',#90339,1000.);
#10408=VECTOR('',#90346,1000.);
#10409=VECTOR('',#90347,1000.);
#10410=VECTOR('',#90354,1000.);
#10411=VECTOR('',#90363,1000.);
#10412=VECTOR('',#90366,1000.);
#10413=VECTOR('',#90371,1000.);
#10414=VECTOR('',#90372,1000.);
#10415=VECTOR('',#90379,1000.);
#10416=VECTOR('',#90380,1000.);
#10417=VECTOR('',#90387,1000.);
#10418=VECTOR('',#90396,1000.);
#10419=VECTOR('',#90399,1000.);
#10420=VECTOR('',#90404,1000.);
#10421=VECTOR('',#90405,1000.);
#10422=VECTOR('',#90412,1000.);
#10423=VECTOR('',#90413,1000.);
#10424=VECTOR('',#90420,1000.);
#10425=VECTOR('',#90429,1000.);
#10426=VECTOR('',#90432,1000.);
#10427=VECTOR('',#90437,1000.);
#10428=VECTOR('',#90444,1000.);
#10429=VECTOR('',#90457,1000.);
#10430=VECTOR('',#90460,1000.);
#10431=VECTOR('',#90465,1000.);
#10432=VECTOR('',#90472,1000.);
#10433=VECTOR('',#90485,1000.);
#10434=VECTOR('',#90488,1000.);
#10435=VECTOR('',#90493,1000.);
#10436=VECTOR('',#90500,1000.);
#10437=VECTOR('',#90513,1000.);
#10438=VECTOR('',#90516,1000.);
#10439=VECTOR('',#90521,1000.);
#10440=VECTOR('',#90528,1000.);
#10441=VECTOR('',#90541,1000.);
#10442=VECTOR('',#90544,1000.);
#10443=VECTOR('',#90549,1000.);
#10444=VECTOR('',#90556,1000.);
#10445=VECTOR('',#90569,1000.);
#10446=VECTOR('',#90572,1000.);
#10447=VECTOR('',#90577,1000.);
#10448=VECTOR('',#90584,1000.);
#10449=VECTOR('',#90599,1000.);
#10450=VECTOR('',#90602,1000.);
#10451=VECTOR('',#90607,1000.);
#10452=VECTOR('',#90612,1000.);
#10453=VECTOR('',#90617,1000.);
#10454=VECTOR('',#90624,1000.);
#10455=VECTOR('',#90631,1000.);
#10456=VECTOR('',#90634,1000.);
#10457=VECTOR('',#90639,1000.);
#10458=VECTOR('',#90640,1000.);
#10459=VECTOR('',#90647,1000.);
#10460=VECTOR('',#90648,1000.);
#10461=VECTOR('',#90655,1000.);
#10462=VECTOR('',#90664,1000.);
#10463=VECTOR('',#90667,1000.);
#10464=VECTOR('',#90672,1000.);
#10465=VECTOR('',#90679,1000.);
#10466=VECTOR('',#90692,1000.);
#10467=VECTOR('',#90695,1000.);
#10468=VECTOR('',#90700,1000.);
#10469=VECTOR('',#90707,1000.);
#10470=VECTOR('',#90720,1000.);
#10471=VECTOR('',#90723,1000.);
#10472=VECTOR('',#90728,1000.);
#10473=VECTOR('',#90735,1000.);
#10474=VECTOR('',#90748,1000.);
#10475=VECTOR('',#90751,1000.);
#10476=VECTOR('',#90756,1000.);
#10477=VECTOR('',#90763,1000.);
#10478=VECTOR('',#90776,1000.);
#10479=VECTOR('',#90779,1000.);
#10480=VECTOR('',#90784,1000.);
#10481=VECTOR('',#90791,1000.);
#10482=VECTOR('',#90804,1000.);
#10483=VECTOR('',#90807,1000.);
#10484=VECTOR('',#90812,1000.);
#10485=VECTOR('',#90819,1000.);
#10486=VECTOR('',#90832,1000.);
#10487=VECTOR('',#90835,1000.);
#10488=VECTOR('',#90840,1000.);
#10489=VECTOR('',#90847,1000.);
#10490=VECTOR('',#90860,1000.);
#10491=VECTOR('',#90863,1000.);
#10492=VECTOR('',#90868,1000.);
#10493=VECTOR('',#90875,1000.);
#10494=VECTOR('',#90888,1000.);
#10495=VECTOR('',#90891,1000.);
#10496=VECTOR('',#90896,1000.);
#10497=VECTOR('',#90897,1000.);
#10498=VECTOR('',#90904,1000.);
#10499=VECTOR('',#90905,1000.);
#10500=VECTOR('',#90912,1000.);
#10501=VECTOR('',#90921,1000.);
#10502=VECTOR('',#90924,1000.);
#10503=VECTOR('',#90929,1000.);
#10504=VECTOR('',#90930,1000.);
#10505=VECTOR('',#90937,1000.);
#10506=VECTOR('',#90938,1000.);
#10507=VECTOR('',#90945,1000.);
#10508=VECTOR('',#90954,1000.);
#10509=VECTOR('',#90957,1000.);
#10510=VECTOR('',#90962,1000.);
#10511=VECTOR('',#90969,1000.);
#10512=VECTOR('',#90982,1000.);
#10513=VECTOR('',#90985,1000.);
#10514=VECTOR('',#90990,1000.);
#10515=VECTOR('',#90997,1000.);
#10516=VECTOR('',#91010,1000.);
#10517=VECTOR('',#91013,1000.);
#10518=VECTOR('',#91018,1000.);
#10519=VECTOR('',#91025,1000.);
#10520=VECTOR('',#91038,1000.);
#10521=VECTOR('',#91041,1000.);
#10522=VECTOR('',#91046,1000.);
#10523=VECTOR('',#91053,1000.);
#10524=VECTOR('',#91066,1000.);
#10525=VECTOR('',#91069,1000.);
#10526=VECTOR('',#91074,1000.);
#10527=VECTOR('',#91081,1000.);
#10528=VECTOR('',#91094,1000.);
#10529=VECTOR('',#91097,1000.);
#10530=VECTOR('',#91102,1000.);
#10531=VECTOR('',#91109,1000.);
#10532=VECTOR('',#91122,1000.);
#10533=VECTOR('',#91125,1000.);
#10534=VECTOR('',#91130,1000.);
#10535=VECTOR('',#91137,1000.);
#10536=VECTOR('',#91150,1000.);
#10537=VECTOR('',#91153,1000.);
#10538=VECTOR('',#91158,1000.);
#10539=VECTOR('',#91165,1000.);
#10540=VECTOR('',#91178,1000.);
#10541=VECTOR('',#91181,1000.);
#10542=VECTOR('',#91186,1000.);
#10543=VECTOR('',#91193,1000.);
#10544=VECTOR('',#91206,1000.);
#10545=VECTOR('',#91209,1000.);
#10546=VECTOR('',#91214,1000.);
#10547=VECTOR('',#91221,1000.);
#10548=VECTOR('',#91234,1000.);
#10549=VECTOR('',#91235,1000.);
#10550=VECTOR('',#91240,1000.);
#10551=VECTOR('',#91243,1000.);
#10552=VECTOR('',#91248,1000.);
#10553=VECTOR('',#91255,1000.);
#10554=VECTOR('',#91268,1000.);
#10555=VECTOR('',#91271,1000.);
#10556=VECTOR('',#91276,1000.);
#10557=VECTOR('',#91283,1000.);
#10558=VECTOR('',#91296,1000.);
#10559=VECTOR('',#91299,1000.);
#10560=VECTOR('',#91304,1000.);
#10561=VECTOR('',#91311,1000.);
#10562=VECTOR('',#91324,1000.);
#10563=VECTOR('',#91327,1000.);
#10564=VECTOR('',#91332,1000.);
#10565=VECTOR('',#91339,1000.);
#10566=VECTOR('',#91352,1000.);
#10567=VECTOR('',#91355,1000.);
#10568=VECTOR('',#91360,1000.);
#10569=VECTOR('',#91367,1000.);
#10570=VECTOR('',#91380,1000.);
#10571=VECTOR('',#91383,1000.);
#10572=VECTOR('',#91388,1000.);
#10573=VECTOR('',#91395,1000.);
#10574=VECTOR('',#91408,1000.);
#10575=VECTOR('',#91411,1000.);
#10576=VECTOR('',#91416,1000.);
#10577=VECTOR('',#91423,1000.);
#10578=VECTOR('',#91436,1000.);
#10579=VECTOR('',#91439,1000.);
#10580=VECTOR('',#91444,1000.);
#10581=VECTOR('',#91451,1000.);
#10582=VECTOR('',#91464,1000.);
#10583=VECTOR('',#91467,1000.);
#10584=VECTOR('',#91472,1000.);
#10585=VECTOR('',#91479,1000.);
#10586=VECTOR('',#91492,1000.);
#10587=VECTOR('',#91495,1000.);
#10588=VECTOR('',#91500,1000.);
#10589=VECTOR('',#91507,1000.);
#10590=VECTOR('',#91520,1000.);
#10591=VECTOR('',#91523,1000.);
#10592=VECTOR('',#91528,1000.);
#10593=VECTOR('',#91535,1000.);
#10594=VECTOR('',#91548,1000.);
#10595=VECTOR('',#91551,1000.);
#10596=VECTOR('',#91556,1000.);
#10597=VECTOR('',#91563,1000.);
#10598=VECTOR('',#91564,1000.);
#10599=VECTOR('',#91573,1000.);
#10600=VECTOR('',#91582,1000.);
#10601=VECTOR('',#91585,1000.);
#10602=VECTOR('',#91590,1000.);
#10603=VECTOR('',#91597,1000.);
#10604=VECTOR('',#91598,1000.);
#10605=VECTOR('',#91607,1000.);
#10606=VECTOR('',#91616,1000.);
#10607=VECTOR('',#91619,1000.);
#10608=VECTOR('',#91624,1000.);
#10609=VECTOR('',#91631,1000.);
#10610=VECTOR('',#91644,1000.);
#10611=VECTOR('',#91647,1000.);
#10612=VECTOR('',#91652,1000.);
#10613=VECTOR('',#91659,1000.);
#10614=VECTOR('',#91672,1000.);
#10615=VECTOR('',#91675,1000.);
#10616=VECTOR('',#91680,1000.);
#10617=VECTOR('',#91687,1000.);
#10618=VECTOR('',#91700,1000.);
#10619=VECTOR('',#91703,1000.);
#10620=VECTOR('',#91708,1000.);
#10621=VECTOR('',#91715,1000.);
#10622=VECTOR('',#91728,1000.);
#10623=VECTOR('',#91731,1000.);
#10624=VECTOR('',#91736,1000.);
#10625=VECTOR('',#91743,1000.);
#10626=VECTOR('',#91756,1000.);
#10627=VECTOR('',#91759,1000.);
#10628=VECTOR('',#91764,1000.);
#10629=VECTOR('',#91771,1000.);
#10630=VECTOR('',#91784,1000.);
#10631=VECTOR('',#91787,1000.);
#10632=VECTOR('',#91792,1000.);
#10633=VECTOR('',#91799,1000.);
#10634=VECTOR('',#91812,1000.);
#10635=VECTOR('',#91815,1000.);
#10636=VECTOR('',#91820,1000.);
#10637=VECTOR('',#91827,1000.);
#10638=VECTOR('',#91840,1000.);
#10639=VECTOR('',#91843,1000.);
#10640=VECTOR('',#91848,1000.);
#10641=VECTOR('',#91855,1000.);
#10642=VECTOR('',#91868,1000.);
#10643=VECTOR('',#91871,1000.);
#10644=VECTOR('',#91876,1000.);
#10645=VECTOR('',#91883,1000.);
#10646=VECTOR('',#91896,1000.);
#10647=VECTOR('',#91899,1000.);
#10648=VECTOR('',#91904,1000.);
#10649=VECTOR('',#91911,1000.);
#10650=VECTOR('',#91924,1000.);
#10651=VECTOR('',#91927,1000.);
#10652=VECTOR('',#91932,1000.);
#10653=VECTOR('',#91939,1000.);
#10654=VECTOR('',#91952,1000.);
#10655=VECTOR('',#91955,1000.);
#10656=VECTOR('',#91960,1000.);
#10657=VECTOR('',#91967,1000.);
#10658=VECTOR('',#91980,1000.);
#10659=VECTOR('',#91983,1000.);
#10660=VECTOR('',#91988,1000.);
#10661=VECTOR('',#91995,1000.);
#10662=VECTOR('',#92008,1000.);
#10663=VECTOR('',#92011,1000.);
#10664=VECTOR('',#92016,1000.);
#10665=VECTOR('',#92023,1000.);
#10666=VECTOR('',#92036,1000.);
#10667=VECTOR('',#92039,1000.);
#10668=VECTOR('',#92044,1000.);
#10669=VECTOR('',#92051,1000.);
#10670=VECTOR('',#92064,1000.);
#10671=VECTOR('',#92067,1000.);
#10672=VECTOR('',#92072,1000.);
#10673=VECTOR('',#92079,1000.);
#10674=VECTOR('',#92092,1000.);
#10675=VECTOR('',#92095,1000.);
#10676=VECTOR('',#92100,1000.);
#10677=VECTOR('',#92107,1000.);
#10678=VECTOR('',#92120,1000.);
#10679=VECTOR('',#92123,1000.);
#10680=VECTOR('',#92128,1000.);
#10681=VECTOR('',#92135,1000.);
#10682=VECTOR('',#92148,1000.);
#10683=VECTOR('',#92151,1000.);
#10684=VECTOR('',#92156,1000.);
#10685=VECTOR('',#92163,1000.);
#10686=VECTOR('',#92176,1000.);
#10687=VECTOR('',#92179,1000.);
#10688=VECTOR('',#92184,1000.);
#10689=VECTOR('',#92191,1000.);
#10690=VECTOR('',#92204,1000.);
#10691=VECTOR('',#92207,1000.);
#10692=VECTOR('',#92212,1000.);
#10693=VECTOR('',#92219,1000.);
#10694=VECTOR('',#92232,1000.);
#10695=VECTOR('',#92235,1000.);
#10696=VECTOR('',#92240,1000.);
#10697=VECTOR('',#92247,1000.);
#10698=VECTOR('',#92260,1000.);
#10699=VECTOR('',#92263,1000.);
#10700=VECTOR('',#92268,1000.);
#10701=VECTOR('',#92275,1000.);
#10702=VECTOR('',#92288,1000.);
#10703=VECTOR('',#92291,1000.);
#10704=VECTOR('',#92296,1000.);
#10705=VECTOR('',#92303,1000.);
#10706=VECTOR('',#92316,1000.);
#10707=VECTOR('',#92319,1000.);
#10708=VECTOR('',#92324,1000.);
#10709=VECTOR('',#92331,1000.);
#10710=VECTOR('',#92344,1000.);
#10711=VECTOR('',#92347,1000.);
#10712=VECTOR('',#92352,1000.);
#10713=VECTOR('',#92359,1000.);
#10714=VECTOR('',#92372,1000.);
#10715=VECTOR('',#92375,1000.);
#10716=VECTOR('',#92380,1000.);
#10717=VECTOR('',#92387,1000.);
#10718=VECTOR('',#92400,1000.);
#10719=VECTOR('',#92403,1000.);
#10720=VECTOR('',#92408,1000.);
#10721=VECTOR('',#92415,1000.);
#10722=VECTOR('',#92428,1000.);
#10723=VECTOR('',#92431,1000.);
#10724=VECTOR('',#92436,1000.);
#10725=VECTOR('',#92443,1000.);
#10726=VECTOR('',#92456,1000.);
#10727=VECTOR('',#92459,1000.);
#10728=VECTOR('',#92464,1000.);
#10729=VECTOR('',#92471,1000.);
#10730=VECTOR('',#92484,1000.);
#10731=VECTOR('',#92487,1000.);
#10732=VECTOR('',#92492,1000.);
#10733=VECTOR('',#92499,1000.);
#10734=VECTOR('',#92512,1000.);
#10735=VECTOR('',#92515,1000.);
#10736=VECTOR('',#92520,1000.);
#10737=VECTOR('',#92527,1000.);
#10738=VECTOR('',#92540,1000.);
#10739=VECTOR('',#92543,1000.);
#10740=VECTOR('',#92548,1000.);
#10741=VECTOR('',#92555,1000.);
#10742=VECTOR('',#92568,1000.);
#10743=VECTOR('',#92571,1000.);
#10744=VECTOR('',#92576,1000.);
#10745=VECTOR('',#92583,1000.);
#10746=VECTOR('',#92596,1000.);
#10747=VECTOR('',#92599,1000.);
#10748=VECTOR('',#92604,1000.);
#10749=VECTOR('',#92611,1000.);
#10750=VECTOR('',#92624,1000.);
#10751=VECTOR('',#92627,1000.);
#10752=VECTOR('',#92632,1000.);
#10753=VECTOR('',#92639,1000.);
#10754=VECTOR('',#92652,1000.);
#10755=VECTOR('',#92655,1000.);
#10756=VECTOR('',#92660,1000.);
#10757=VECTOR('',#92667,1000.);
#10758=VECTOR('',#92680,1000.);
#10759=VECTOR('',#92683,1000.);
#10760=VECTOR('',#92688,1000.);
#10761=VECTOR('',#92695,1000.);
#10762=VECTOR('',#92708,1000.);
#10763=VECTOR('',#92711,1000.);
#10764=VECTOR('',#92716,1000.);
#10765=VECTOR('',#92723,1000.);
#10766=VECTOR('',#92736,1000.);
#10767=VECTOR('',#92739,1000.);
#10768=VECTOR('',#92744,1000.);
#10769=VECTOR('',#92751,1000.);
#10770=VECTOR('',#92764,1000.);
#10771=VECTOR('',#92767,1000.);
#10772=VECTOR('',#92772,1000.);
#10773=VECTOR('',#92779,1000.);
#10774=VECTOR('',#92792,1000.);
#10775=VECTOR('',#92795,1000.);
#10776=VECTOR('',#92800,1000.);
#10777=VECTOR('',#92807,1000.);
#10778=VECTOR('',#92820,1000.);
#10779=VECTOR('',#92823,1000.);
#10780=VECTOR('',#92828,1000.);
#10781=VECTOR('',#92835,1000.);
#10782=VECTOR('',#92848,1000.);
#10783=VECTOR('',#92851,1000.);
#10784=VECTOR('',#92856,1000.);
#10785=VECTOR('',#92863,1000.);
#10786=VECTOR('',#92876,1000.);
#10787=VECTOR('',#92879,1000.);
#10788=VECTOR('',#92884,1000.);
#10789=VECTOR('',#92891,1000.);
#10790=VECTOR('',#92904,1000.);
#10791=VECTOR('',#92907,1000.);
#10792=VECTOR('',#92912,1000.);
#10793=VECTOR('',#92919,1000.);
#10794=VECTOR('',#92932,1000.);
#10795=VECTOR('',#92935,1000.);
#10796=VECTOR('',#92940,1000.);
#10797=VECTOR('',#92947,1000.);
#10798=VECTOR('',#92960,1000.);
#10799=VECTOR('',#92963,1000.);
#10800=VECTOR('',#92968,1000.);
#10801=VECTOR('',#92975,1000.);
#10802=VECTOR('',#92988,1000.);
#10803=VECTOR('',#92991,1000.);
#10804=VECTOR('',#92996,1000.);
#10805=VECTOR('',#93003,1000.);
#10806=VECTOR('',#93016,1000.);
#10807=VECTOR('',#93019,1000.);
#10808=VECTOR('',#93024,1000.);
#10809=VECTOR('',#93031,1000.);
#10810=VECTOR('',#93044,1000.);
#10811=VECTOR('',#93047,1000.);
#10812=VECTOR('',#93052,1000.);
#10813=VECTOR('',#93059,1000.);
#10814=VECTOR('',#93072,1000.);
#10815=VECTOR('',#93075,1000.);
#10816=VECTOR('',#93080,1000.);
#10817=VECTOR('',#93087,1000.);
#10818=VECTOR('',#93100,1000.);
#10819=VECTOR('',#93103,1000.);
#10820=VECTOR('',#93108,1000.);
#10821=VECTOR('',#93115,1000.);
#10822=VECTOR('',#93128,1000.);
#10823=VECTOR('',#93131,1000.);
#10824=VECTOR('',#93136,1000.);
#10825=VECTOR('',#93143,1000.);
#10826=VECTOR('',#93156,1000.);
#10827=VECTOR('',#93159,1000.);
#10828=VECTOR('',#93164,1000.);
#10829=VECTOR('',#93171,1000.);
#10830=VECTOR('',#93184,1000.);
#10831=VECTOR('',#93187,1000.);
#10832=VECTOR('',#93192,1000.);
#10833=VECTOR('',#93199,1000.);
#10834=VECTOR('',#93212,1000.);
#10835=VECTOR('',#93215,1000.);
#10836=VECTOR('',#93220,1000.);
#10837=VECTOR('',#93227,1000.);
#10838=VECTOR('',#93240,1000.);
#10839=VECTOR('',#93243,1000.);
#10840=VECTOR('',#93248,1000.);
#10841=VECTOR('',#93255,1000.);
#10842=VECTOR('',#93268,1000.);
#10843=VECTOR('',#93271,1000.);
#10844=VECTOR('',#93276,1000.);
#10845=VECTOR('',#93283,1000.);
#10846=VECTOR('',#93296,1000.);
#10847=VECTOR('',#93299,1000.);
#10848=VECTOR('',#93304,1000.);
#10849=VECTOR('',#93311,1000.);
#10850=VECTOR('',#93324,1000.);
#10851=VECTOR('',#93327,1000.);
#10852=VECTOR('',#93332,1000.);
#10853=VECTOR('',#93339,1000.);
#10854=VECTOR('',#93352,1000.);
#10855=VECTOR('',#93355,1000.);
#10856=VECTOR('',#93360,1000.);
#10857=VECTOR('',#93367,1000.);
#10858=VECTOR('',#93380,1000.);
#10859=VECTOR('',#93383,1000.);
#10860=VECTOR('',#93388,1000.);
#10861=VECTOR('',#93395,1000.);
#10862=VECTOR('',#93408,1000.);
#10863=VECTOR('',#93411,1000.);
#10864=VECTOR('',#93416,1000.);
#10865=VECTOR('',#93423,1000.);
#10866=VECTOR('',#93436,1000.);
#10867=VECTOR('',#93439,1000.);
#10868=VECTOR('',#93444,1000.);
#10869=VECTOR('',#93451,1000.);
#10870=VECTOR('',#93464,1000.);
#10871=VECTOR('',#93467,1000.);
#10872=VECTOR('',#93472,1000.);
#10873=VECTOR('',#93479,1000.);
#10874=VECTOR('',#93492,1000.);
#10875=VECTOR('',#93495,1000.);
#10876=VECTOR('',#93500,1000.);
#10877=VECTOR('',#93507,1000.);
#10878=VECTOR('',#93520,1000.);
#10879=VECTOR('',#93523,1000.);
#10880=VECTOR('',#93528,1000.);
#10881=VECTOR('',#93535,1000.);
#10882=VECTOR('',#93548,1000.);
#10883=VECTOR('',#93551,1000.);
#10884=VECTOR('',#93556,1000.);
#10885=VECTOR('',#93563,1000.);
#10886=VECTOR('',#93576,1000.);
#10887=VECTOR('',#93579,1000.);
#10888=VECTOR('',#93584,1000.);
#10889=VECTOR('',#93585,1000.);
#10890=VECTOR('',#93592,1000.);
#10891=VECTOR('',#93593,1000.);
#10892=VECTOR('',#93598,1000.);
#10893=VECTOR('',#93607,1000.);
#10894=VECTOR('',#93610,1000.);
#10895=VECTOR('',#93615,1000.);
#10896=VECTOR('',#93616,1000.);
#10897=VECTOR('',#93623,1000.);
#10898=VECTOR('',#93624,1000.);
#10899=VECTOR('',#93631,1000.);
#10900=VECTOR('',#93640,1000.);
#10901=VECTOR('',#93643,1000.);
#10902=VECTOR('',#93648,1000.);
#10903=VECTOR('',#93649,1000.);
#10904=VECTOR('',#93656,1000.);
#10905=VECTOR('',#93657,1000.);
#10906=VECTOR('',#93664,1000.);
#10907=VECTOR('',#93673,1000.);
#10908=VECTOR('',#93676,1000.);
#10909=VECTOR('',#93681,1000.);
#10910=VECTOR('',#93682,1000.);
#10911=VECTOR('',#93689,1000.);
#10912=VECTOR('',#93690,1000.);
#10913=VECTOR('',#93697,1000.);
#10914=VECTOR('',#93706,1000.);
#10915=VECTOR('',#93709,1000.);
#10916=VECTOR('',#93714,1000.);
#10917=VECTOR('',#93715,1000.);
#10918=VECTOR('',#93722,1000.);
#10919=VECTOR('',#93723,1000.);
#10920=VECTOR('',#93730,1000.);
#10921=VECTOR('',#93739,1000.);
#10922=VECTOR('',#93740,1000.);
#10923=VECTOR('',#93743,1000.);
#10924=VECTOR('',#93748,1000.);
#10925=VECTOR('',#93749,1000.);
#10926=VECTOR('',#93754,1000.);
#10927=VECTOR('',#93755,1000.);
#10928=VECTOR('',#93762,1000.);
#10929=VECTOR('',#93771,1000.);
#10930=VECTOR('',#93772,1000.);
#10931=VECTOR('',#93775,1000.);
#10932=VECTOR('',#93780,1000.);
#10933=VECTOR('',#93781,1000.);
#10934=VECTOR('',#93786,1000.);
#10935=VECTOR('',#93787,1000.);
#10936=VECTOR('',#93794,1000.);
#10937=VECTOR('',#93803,1000.);
#10938=VECTOR('',#93806,1000.);
#10939=VECTOR('',#93811,1000.);
#10940=VECTOR('',#93812,1000.);
#10941=VECTOR('',#93819,1000.);
#10942=VECTOR('',#93820,1000.);
#10943=VECTOR('',#93827,1000.);
#10944=VECTOR('',#93836,1000.);
#10945=VECTOR('',#93839,1000.);
#10946=VECTOR('',#93844,1000.);
#10947=VECTOR('',#93845,1000.);
#10948=VECTOR('',#93852,1000.);
#10949=VECTOR('',#93853,1000.);
#10950=VECTOR('',#93860,1000.);
#10951=VECTOR('',#93869,1000.);
#10952=VECTOR('',#93872,1000.);
#10953=VECTOR('',#93877,1000.);
#10954=VECTOR('',#93878,1000.);
#10955=VECTOR('',#93885,1000.);
#10956=VECTOR('',#93886,1000.);
#10957=VECTOR('',#93893,1000.);
#10958=VECTOR('',#93902,1000.);
#10959=VECTOR('',#93905,1000.);
#10960=VECTOR('',#93910,1000.);
#10961=VECTOR('',#93917,1000.);
#10962=VECTOR('',#93930,1000.);
#10963=VECTOR('',#93933,1000.);
#10964=VECTOR('',#93938,1000.);
#10965=VECTOR('',#93945,1000.);
#10966=VECTOR('',#93958,1000.);
#10967=VECTOR('',#93961,1000.);
#10968=VECTOR('',#93966,1000.);
#10969=VECTOR('',#93973,1000.);
#10970=VECTOR('',#93986,1000.);
#10971=VECTOR('',#93989,1000.);
#10972=VECTOR('',#93994,1000.);
#10973=VECTOR('',#94001,1000.);
#10974=VECTOR('',#94014,1000.);
#10975=VECTOR('',#94017,1000.);
#10976=VECTOR('',#94022,1000.);
#10977=VECTOR('',#94029,1000.);
#10978=VECTOR('',#94042,1000.);
#10979=VECTOR('',#94045,1000.);
#10980=VECTOR('',#94050,1000.);
#10981=VECTOR('',#94057,1000.);
#10982=VECTOR('',#94070,1000.);
#10983=VECTOR('',#94073,1000.);
#10984=VECTOR('',#94078,1000.);
#10985=VECTOR('',#94085,1000.);
#10986=VECTOR('',#94098,1000.);
#10987=VECTOR('',#94101,1000.);
#10988=VECTOR('',#94106,1000.);
#10989=VECTOR('',#94113,1000.);
#10990=VECTOR('',#94126,1000.);
#10991=VECTOR('',#94127,1000.);
#10992=VECTOR('',#94130,1000.);
#10993=VECTOR('',#94135,1000.);
#10994=VECTOR('',#94136,1000.);
#10995=VECTOR('',#94141,1000.);
#10996=VECTOR('',#94142,1000.);
#10997=VECTOR('',#94149,1000.);
#10998=VECTOR('',#94158,1000.);
#10999=VECTOR('',#94159,1000.);
#11000=VECTOR('',#94162,1000.);
#11001=VECTOR('',#94167,1000.);
#11002=VECTOR('',#94168,1000.);
#11003=VECTOR('',#94173,1000.);
#11004=VECTOR('',#94174,1000.);
#11005=VECTOR('',#94181,1000.);
#11006=VECTOR('',#94190,1000.);
#11007=VECTOR('',#94193,1000.);
#11008=VECTOR('',#94198,1000.);
#11009=VECTOR('',#94205,1000.);
#11010=VECTOR('',#94218,1000.);
#11011=VECTOR('',#94221,1000.);
#11012=VECTOR('',#94226,1000.);
#11013=VECTOR('',#94233,1000.);
#11014=VECTOR('',#94246,1000.);
#11015=VECTOR('',#94249,1000.);
#11016=VECTOR('',#94254,1000.);
#11017=VECTOR('',#94261,1000.);
#11018=VECTOR('',#94274,1000.);
#11019=VECTOR('',#94277,1000.);
#11020=VECTOR('',#94282,1000.);
#11021=VECTOR('',#94289,1000.);
#11022=VECTOR('',#94302,1000.);
#11023=VECTOR('',#94305,1000.);
#11024=VECTOR('',#94310,1000.);
#11025=VECTOR('',#94317,1000.);
#11026=VECTOR('',#94318,1000.);
#11027=VECTOR('',#94327,1000.);
#11028=VECTOR('',#94336,1000.);
#11029=VECTOR('',#94339,1000.);
#11030=VECTOR('',#94344,1000.);
#11031=VECTOR('',#94345,1000.);
#11032=VECTOR('',#94352,1000.);
#11033=VECTOR('',#94353,1000.);
#11034=VECTOR('',#94360,1000.);
#11035=VECTOR('',#94369,1000.);
#11036=VECTOR('',#94372,1000.);
#11037=VECTOR('',#94377,1000.);
#11038=VECTOR('',#94378,1000.);
#11039=VECTOR('',#94385,1000.);
#11040=VECTOR('',#94386,1000.);
#11041=VECTOR('',#94393,1000.);
#11042=VECTOR('',#94402,1000.);
#11043=VECTOR('',#94405,1000.);
#11044=VECTOR('',#94410,1000.);
#11045=VECTOR('',#94417,1000.);
#11046=VECTOR('',#94418,1000.);
#11047=VECTOR('',#94427,1000.);
#11048=VECTOR('',#94436,1000.);
#11049=VECTOR('',#94439,1000.);
#11050=VECTOR('',#94444,1000.);
#11051=VECTOR('',#94451,1000.);
#11052=VECTOR('',#94464,1000.);
#11053=VECTOR('',#94467,1000.);
#11054=VECTOR('',#94472,1000.);
#11055=VECTOR('',#94479,1000.);
#11056=VECTOR('',#94492,1000.);
#11057=VECTOR('',#94495,1000.);
#11058=VECTOR('',#94500,1000.);
#11059=VECTOR('',#94507,1000.);
#11060=VECTOR('',#94520,1000.);
#11061=VECTOR('',#94523,1000.);
#11062=VECTOR('',#94528,1000.);
#11063=VECTOR('',#94535,1000.);
#11064=VECTOR('',#94548,1000.);
#11065=VECTOR('',#94551,1000.);
#11066=VECTOR('',#94556,1000.);
#11067=VECTOR('',#94563,1000.);
#11068=VECTOR('',#94576,1000.);
#11069=VECTOR('',#94579,1000.);
#11070=VECTOR('',#94584,1000.);
#11071=VECTOR('',#94591,1000.);
#11072=VECTOR('',#94604,1000.);
#11073=VECTOR('',#94607,1000.);
#11074=VECTOR('',#94612,1000.);
#11075=VECTOR('',#94619,1000.);
#11076=VECTOR('',#94632,1000.);
#11077=VECTOR('',#94635,1000.);
#11078=VECTOR('',#94640,1000.);
#11079=VECTOR('',#94647,1000.);
#11080=VECTOR('',#94660,1000.);
#11081=VECTOR('',#94663,1000.);
#11082=VECTOR('',#94668,1000.);
#11083=VECTOR('',#94675,1000.);
#11084=VECTOR('',#94688,1000.);
#11085=VECTOR('',#94691,1000.);
#11086=VECTOR('',#94696,1000.);
#11087=VECTOR('',#94703,1000.);
#11088=VECTOR('',#94716,1000.);
#11089=VECTOR('',#94719,1000.);
#11090=VECTOR('',#94724,1000.);
#11091=VECTOR('',#94731,1000.);
#11092=VECTOR('',#94732,1000.);
#11093=VECTOR('',#94741,1000.);
#11094=VECTOR('',#94750,1000.);
#11095=VECTOR('',#94753,1000.);
#11096=VECTOR('',#94758,1000.);
#11097=VECTOR('',#94765,1000.);
#11098=VECTOR('',#94766,1000.);
#11099=VECTOR('',#94775,1000.);
#11100=VECTOR('',#94784,1000.);
#11101=VECTOR('',#94787,1000.);
#11102=VECTOR('',#94792,1000.);
#11103=VECTOR('',#94799,1000.);
#11104=VECTOR('',#94812,1000.);
#11105=VECTOR('',#94815,1000.);
#11106=VECTOR('',#94820,1000.);
#11107=VECTOR('',#94827,1000.);
#11108=VECTOR('',#94840,1000.);
#11109=VECTOR('',#94843,1000.);
#11110=VECTOR('',#94848,1000.);
#11111=VECTOR('',#94855,1000.);
#11112=VECTOR('',#94868,1000.);
#11113=VECTOR('',#94871,1000.);
#11114=VECTOR('',#94876,1000.);
#11115=VECTOR('',#94883,1000.);
#11116=VECTOR('',#94896,1000.);
#11117=VECTOR('',#94899,1000.);
#11118=VECTOR('',#94904,1000.);
#11119=VECTOR('',#94911,1000.);
#11120=VECTOR('',#94924,1000.);
#11121=VECTOR('',#94927,1000.);
#11122=VECTOR('',#94932,1000.);
#11123=VECTOR('',#94939,1000.);
#11124=VECTOR('',#94952,1000.);
#11125=VECTOR('',#94955,1000.);
#11126=VECTOR('',#94960,1000.);
#11127=VECTOR('',#94967,1000.);
#11128=VECTOR('',#94980,1000.);
#11129=VECTOR('',#94983,1000.);
#11130=VECTOR('',#94988,1000.);
#11131=VECTOR('',#94995,1000.);
#11132=VECTOR('',#95008,1000.);
#11133=VECTOR('',#95011,1000.);
#11134=VECTOR('',#95016,1000.);
#11135=VECTOR('',#95023,1000.);
#11136=VECTOR('',#95036,1000.);
#11137=VECTOR('',#95039,1000.);
#11138=VECTOR('',#95044,1000.);
#11139=VECTOR('',#95045,1000.);
#11140=VECTOR('',#95052,1000.);
#11141=VECTOR('',#95053,1000.);
#11142=VECTOR('',#95060,1000.);
#11143=VECTOR('',#95069,1000.);
#11144=VECTOR('',#95072,1000.);
#11145=VECTOR('',#95077,1000.);
#11146=VECTOR('',#95084,1000.);
#11147=VECTOR('',#95085,1000.);
#11148=VECTOR('',#95094,1000.);
#11149=VECTOR('',#95103,1000.);
#11150=VECTOR('',#95106,1000.);
#11151=VECTOR('',#95111,1000.);
#11152=VECTOR('',#95118,1000.);
#11153=VECTOR('',#95131,1000.);
#11154=VECTOR('',#95134,1000.);
#11155=VECTOR('',#95139,1000.);
#11156=VECTOR('',#95146,1000.);
#11157=VECTOR('',#95159,1000.);
#11158=VECTOR('',#95162,1000.);
#11159=VECTOR('',#95167,1000.);
#11160=VECTOR('',#95174,1000.);
#11161=VECTOR('',#95187,1000.);
#11162=VECTOR('',#95190,1000.);
#11163=VECTOR('',#95195,1000.);
#11164=VECTOR('',#95202,1000.);
#11165=VECTOR('',#95215,1000.);
#11166=VECTOR('',#95218,1000.);
#11167=VECTOR('',#95223,1000.);
#11168=VECTOR('',#95230,1000.);
#11169=VECTOR('',#95243,1000.);
#11170=VECTOR('',#95246,1000.);
#11171=VECTOR('',#95251,1000.);
#11172=VECTOR('',#95258,1000.);
#11173=VECTOR('',#95271,1000.);
#11174=VECTOR('',#95274,1000.);
#11175=VECTOR('',#95279,1000.);
#11176=VECTOR('',#95286,1000.);
#11177=VECTOR('',#95299,1000.);
#11178=VECTOR('',#95302,1000.);
#11179=VECTOR('',#95307,1000.);
#11180=VECTOR('',#95314,1000.);
#11181=VECTOR('',#95327,1000.);
#11182=VECTOR('',#95330,1000.);
#11183=VECTOR('',#95335,1000.);
#11184=VECTOR('',#95342,1000.);
#11185=VECTOR('',#95355,1000.);
#11186=VECTOR('',#95358,1000.);
#11187=VECTOR('',#95363,1000.);
#11188=VECTOR('',#95370,1000.);
#11189=VECTOR('',#95383,1000.);
#11190=VECTOR('',#95386,1000.);
#11191=VECTOR('',#95391,1000.);
#11192=VECTOR('',#95398,1000.);
#11193=VECTOR('',#95411,1000.);
#11194=VECTOR('',#95414,1000.);
#11195=VECTOR('',#95419,1000.);
#11196=VECTOR('',#95426,1000.);
#11197=VECTOR('',#95439,1000.);
#11198=VECTOR('',#95442,1000.);
#11199=VECTOR('',#95447,1000.);
#11200=VECTOR('',#95454,1000.);
#11201=VECTOR('',#95467,1000.);
#11202=VECTOR('',#95470,1000.);
#11203=VECTOR('',#95475,1000.);
#11204=VECTOR('',#95482,1000.);
#11205=VECTOR('',#95495,1000.);
#11206=VECTOR('',#95498,1000.);
#11207=VECTOR('',#95503,1000.);
#11208=VECTOR('',#95510,1000.);
#11209=VECTOR('',#95523,1000.);
#11210=VECTOR('',#95526,1000.);
#11211=VECTOR('',#95531,1000.);
#11212=VECTOR('',#95538,1000.);
#11213=VECTOR('',#95551,1000.);
#11214=VECTOR('',#95554,1000.);
#11215=VECTOR('',#95559,1000.);
#11216=VECTOR('',#95566,1000.);
#11217=VECTOR('',#95579,1000.);
#11218=VECTOR('',#95582,1000.);
#11219=VECTOR('',#95587,1000.);
#11220=VECTOR('',#95594,1000.);
#11221=VECTOR('',#95607,1000.);
#11222=VECTOR('',#95610,1000.);
#11223=VECTOR('',#95615,1000.);
#11224=VECTOR('',#95622,1000.);
#11225=VECTOR('',#95635,1000.);
#11226=VECTOR('',#95638,1000.);
#11227=VECTOR('',#95643,1000.);
#11228=VECTOR('',#95650,1000.);
#11229=VECTOR('',#95663,1000.);
#11230=VECTOR('',#95666,1000.);
#11231=VECTOR('',#95671,1000.);
#11232=VECTOR('',#95678,1000.);
#11233=VECTOR('',#95691,1000.);
#11234=VECTOR('',#95694,1000.);
#11235=VECTOR('',#95699,1000.);
#11236=VECTOR('',#95706,1000.);
#11237=VECTOR('',#95719,1000.);
#11238=VECTOR('',#95722,1000.);
#11239=VECTOR('',#95727,1000.);
#11240=VECTOR('',#95734,1000.);
#11241=VECTOR('',#95747,1000.);
#11242=VECTOR('',#95750,1000.);
#11243=VECTOR('',#95755,1000.);
#11244=VECTOR('',#95762,1000.);
#11245=VECTOR('',#95775,1000.);
#11246=VECTOR('',#95778,1000.);
#11247=VECTOR('',#95783,1000.);
#11248=VECTOR('',#95790,1000.);
#11249=VECTOR('',#95803,1000.);
#11250=VECTOR('',#95806,1000.);
#11251=VECTOR('',#95811,1000.);
#11252=VECTOR('',#95818,1000.);
#11253=VECTOR('',#95831,1000.);
#11254=VECTOR('',#95834,1000.);
#11255=VECTOR('',#95839,1000.);
#11256=VECTOR('',#95846,1000.);
#11257=VECTOR('',#95859,1000.);
#11258=VECTOR('',#95862,1000.);
#11259=VECTOR('',#95867,1000.);
#11260=VECTOR('',#95874,1000.);
#11261=VECTOR('',#95887,1000.);
#11262=VECTOR('',#95890,1000.);
#11263=VECTOR('',#95895,1000.);
#11264=VECTOR('',#95902,1000.);
#11265=VECTOR('',#95915,1000.);
#11266=VECTOR('',#95918,1000.);
#11267=VECTOR('',#95923,1000.);
#11268=VECTOR('',#95930,1000.);
#11269=VECTOR('',#95943,1000.);
#11270=VECTOR('',#95946,1000.);
#11271=VECTOR('',#95951,1000.);
#11272=VECTOR('',#95958,1000.);
#11273=VECTOR('',#95971,1000.);
#11274=VECTOR('',#95974,1000.);
#11275=VECTOR('',#95979,1000.);
#11276=VECTOR('',#95986,1000.);
#11277=VECTOR('',#95999,1000.);
#11278=VECTOR('',#96002,1000.);
#11279=VECTOR('',#96007,1000.);
#11280=VECTOR('',#96014,1000.);
#11281=VECTOR('',#96027,1000.);
#11282=VECTOR('',#96030,1000.);
#11283=VECTOR('',#96035,1000.);
#11284=VECTOR('',#96042,1000.);
#11285=VECTOR('',#96055,1000.);
#11286=VECTOR('',#96058,1000.);
#11287=VECTOR('',#96063,1000.);
#11288=VECTOR('',#96070,1000.);
#11289=VECTOR('',#96083,1000.);
#11290=VECTOR('',#96086,1000.);
#11291=VECTOR('',#96091,1000.);
#11292=VECTOR('',#96098,1000.);
#11293=VECTOR('',#96111,1000.);
#11294=VECTOR('',#96114,1000.);
#11295=VECTOR('',#96119,1000.);
#11296=VECTOR('',#96126,1000.);
#11297=VECTOR('',#96139,1000.);
#11298=VECTOR('',#96142,1000.);
#11299=VECTOR('',#96147,1000.);
#11300=VECTOR('',#96154,1000.);
#11301=VECTOR('',#96167,1000.);
#11302=VECTOR('',#96170,1000.);
#11303=VECTOR('',#96175,1000.);
#11304=VECTOR('',#96182,1000.);
#11305=VECTOR('',#96195,1000.);
#11306=VECTOR('',#96198,1000.);
#11307=VECTOR('',#96203,1000.);
#11308=VECTOR('',#96210,1000.);
#11309=VECTOR('',#96223,1000.);
#11310=VECTOR('',#96226,1000.);
#11311=VECTOR('',#96231,1000.);
#11312=VECTOR('',#96238,1000.);
#11313=VECTOR('',#96251,1000.);
#11314=VECTOR('',#96254,1000.);
#11315=VECTOR('',#96259,1000.);
#11316=VECTOR('',#96266,1000.);
#11317=VECTOR('',#96279,1000.);
#11318=VECTOR('',#96282,1000.);
#11319=VECTOR('',#96287,1000.);
#11320=VECTOR('',#96294,1000.);
#11321=VECTOR('',#96307,1000.);
#11322=VECTOR('',#96310,1000.);
#11323=VECTOR('',#96315,1000.);
#11324=VECTOR('',#96322,1000.);
#11325=VECTOR('',#96335,1000.);
#11326=VECTOR('',#96338,1000.);
#11327=VECTOR('',#96343,1000.);
#11328=VECTOR('',#96350,1000.);
#11329=VECTOR('',#96363,1000.);
#11330=VECTOR('',#96366,1000.);
#11331=VECTOR('',#96371,1000.);
#11332=VECTOR('',#96378,1000.);
#11333=VECTOR('',#96391,1000.);
#11334=VECTOR('',#96394,1000.);
#11335=VECTOR('',#96399,1000.);
#11336=VECTOR('',#96406,1000.);
#11337=VECTOR('',#96419,1000.);
#11338=VECTOR('',#96422,1000.);
#11339=VECTOR('',#96427,1000.);
#11340=VECTOR('',#96434,1000.);
#11341=VECTOR('',#96447,1000.);
#11342=VECTOR('',#96450,1000.);
#11343=VECTOR('',#96455,1000.);
#11344=VECTOR('',#96462,1000.);
#11345=VECTOR('',#96475,1000.);
#11346=VECTOR('',#96478,1000.);
#11347=VECTOR('',#96483,1000.);
#11348=VECTOR('',#96490,1000.);
#11349=VECTOR('',#96503,1000.);
#11350=VECTOR('',#96506,1000.);
#11351=VECTOR('',#96511,1000.);
#11352=VECTOR('',#96518,1000.);
#11353=VECTOR('',#96531,1000.);
#11354=VECTOR('',#96534,1000.);
#11355=VECTOR('',#96539,1000.);
#11356=VECTOR('',#96546,1000.);
#11357=VECTOR('',#96559,1000.);
#11358=VECTOR('',#96562,1000.);
#11359=VECTOR('',#96567,1000.);
#11360=VECTOR('',#96574,1000.);
#11361=VECTOR('',#96587,1000.);
#11362=VECTOR('',#96590,1000.);
#11363=VECTOR('',#96595,1000.);
#11364=VECTOR('',#96602,1000.);
#11365=VECTOR('',#96615,1000.);
#11366=VECTOR('',#96618,1000.);
#11367=VECTOR('',#96623,1000.);
#11368=VECTOR('',#96630,1000.);
#11369=VECTOR('',#96643,1000.);
#11370=VECTOR('',#96646,1000.);
#11371=VECTOR('',#96651,1000.);
#11372=VECTOR('',#96658,1000.);
#11373=VECTOR('',#96671,1000.);
#11374=VECTOR('',#96674,1000.);
#11375=VECTOR('',#96679,1000.);
#11376=VECTOR('',#96686,1000.);
#11377=VECTOR('',#96699,1000.);
#11378=VECTOR('',#96702,1000.);
#11379=VECTOR('',#96707,1000.);
#11380=VECTOR('',#96714,1000.);
#11381=VECTOR('',#96727,1000.);
#11382=VECTOR('',#96730,1000.);
#11383=VECTOR('',#96735,1000.);
#11384=VECTOR('',#96742,1000.);
#11385=VECTOR('',#96755,1000.);
#11386=VECTOR('',#96758,1000.);
#11387=VECTOR('',#96763,1000.);
#11388=VECTOR('',#96770,1000.);
#11389=VECTOR('',#96783,1000.);
#11390=VECTOR('',#96786,1000.);
#11391=VECTOR('',#96791,1000.);
#11392=VECTOR('',#96798,1000.);
#11393=VECTOR('',#96811,1000.);
#11394=VECTOR('',#96814,1000.);
#11395=VECTOR('',#96819,1000.);
#11396=VECTOR('',#96826,1000.);
#11397=VECTOR('',#96839,1000.);
#11398=VECTOR('',#96842,1000.);
#11399=VECTOR('',#96847,1000.);
#11400=VECTOR('',#96854,1000.);
#11401=VECTOR('',#96867,1000.);
#11402=VECTOR('',#96870,1000.);
#11403=VECTOR('',#96875,1000.);
#11404=VECTOR('',#96882,1000.);
#11405=VECTOR('',#96895,1000.);
#11406=VECTOR('',#96898,1000.);
#11407=VECTOR('',#96903,1000.);
#11408=VECTOR('',#96910,1000.);
#11409=VECTOR('',#96923,1000.);
#11410=VECTOR('',#96926,1000.);
#11411=VECTOR('',#96931,1000.);
#11412=VECTOR('',#96938,1000.);
#11413=VECTOR('',#96951,1000.);
#11414=VECTOR('',#96954,1000.);
#11415=VECTOR('',#96959,1000.);
#11416=VECTOR('',#96966,1000.);
#11417=VECTOR('',#96979,1000.);
#11418=VECTOR('',#96982,1000.);
#11419=VECTOR('',#96987,1000.);
#11420=VECTOR('',#96994,1000.);
#11421=VECTOR('',#97007,1000.);
#11422=VECTOR('',#97010,1000.);
#11423=VECTOR('',#97015,1000.);
#11424=VECTOR('',#97022,1000.);
#11425=VECTOR('',#97035,1000.);
#11426=VECTOR('',#97038,1000.);
#11427=VECTOR('',#97043,1000.);
#11428=VECTOR('',#97050,1000.);
#11429=VECTOR('',#97063,1000.);
#11430=VECTOR('',#97066,1000.);
#11431=VECTOR('',#97071,1000.);
#11432=VECTOR('',#97078,1000.);
#11433=VECTOR('',#97091,1000.);
#11434=VECTOR('',#97094,1000.);
#11435=VECTOR('',#97099,1000.);
#11436=VECTOR('',#97106,1000.);
#11437=VECTOR('',#97119,1000.);
#11438=VECTOR('',#97122,1000.);
#11439=VECTOR('',#97127,1000.);
#11440=VECTOR('',#97134,1000.);
#11441=VECTOR('',#97147,1000.);
#11442=VECTOR('',#97150,1000.);
#11443=VECTOR('',#97155,1000.);
#11444=VECTOR('',#97162,1000.);
#11445=VECTOR('',#97175,1000.);
#11446=VECTOR('',#97178,1000.);
#11447=VECTOR('',#97183,1000.);
#11448=VECTOR('',#97190,1000.);
#11449=VECTOR('',#97203,1000.);
#11450=VECTOR('',#97206,1000.);
#11451=VECTOR('',#97211,1000.);
#11452=VECTOR('',#97218,1000.);
#11453=VECTOR('',#97231,1000.);
#11454=VECTOR('',#97234,1000.);
#11455=VECTOR('',#97239,1000.);
#11456=VECTOR('',#97246,1000.);
#11457=VECTOR('',#97261,1000.);
#11458=VECTOR('',#97262,1000.);
#11459=VECTOR('',#97263,1000.);
#11460=VECTOR('',#97264,1000.);
#11461=VECTOR('',#97267,1000.);
#11462=VECTOR('',#97268,1000.);
#11463=VECTOR('',#97269,1000.);
#11464=VECTOR('',#97272,1000.);
#11465=VECTOR('',#97273,1000.);
#11466=VECTOR('',#97274,1000.);
#11467=VECTOR('',#97277,1000.);
#11468=VECTOR('',#97278,1000.);
#11469=VECTOR('',#97281,1000.);
#11470=VECTOR('',#97282,1000.);
#11471=VECTOR('',#97283,1000.);
#11472=VECTOR('',#97284,1000.);
#11473=VECTOR('',#97287,1000.);
#11474=VECTOR('',#97288,1000.);
#11475=VECTOR('',#97289,1000.);
#11476=VECTOR('',#97292,1000.);
#11477=VECTOR('',#97293,1000.);
#11478=VECTOR('',#97294,1000.);
#11479=VECTOR('',#97297,1000.);
#11480=VECTOR('',#97298,1000.);
#11481=VECTOR('',#97301,1000.);
#11482=VECTOR('',#97302,1000.);
#11483=VECTOR('',#97303,1000.);
#11484=VECTOR('',#97304,1000.);
#11485=VECTOR('',#97307,1000.);
#11486=VECTOR('',#97308,1000.);
#11487=VECTOR('',#97309,1000.);
#11488=VECTOR('',#97312,1000.);
#11489=VECTOR('',#97313,1000.);
#11490=VECTOR('',#97314,1000.);
#11491=VECTOR('',#97317,1000.);
#11492=VECTOR('',#97318,1000.);
#11493=VECTOR('',#97321,1000.);
#11494=VECTOR('',#97322,1000.);
#11495=VECTOR('',#97323,1000.);
#11496=VECTOR('',#97324,1000.);
#11497=VECTOR('',#97327,1000.);
#11498=VECTOR('',#97328,1000.);
#11499=VECTOR('',#97329,1000.);
#11500=VECTOR('',#97332,1000.);
#11501=VECTOR('',#97333,1000.);
#11502=VECTOR('',#97334,1000.);
#11503=VECTOR('',#97337,1000.);
#11504=VECTOR('',#97338,1000.);
#11505=VECTOR('',#97341,1000.);
#11506=VECTOR('',#97342,1000.);
#11507=VECTOR('',#97343,1000.);
#11508=VECTOR('',#97344,1000.);
#11509=VECTOR('',#97347,1000.);
#11510=VECTOR('',#97348,1000.);
#11511=VECTOR('',#97349,1000.);
#11512=VECTOR('',#97352,1000.);
#11513=VECTOR('',#97353,1000.);
#11514=VECTOR('',#97354,1000.);
#11515=VECTOR('',#97357,1000.);
#11516=VECTOR('',#97358,1000.);
#11517=VECTOR('',#97361,1000.);
#11518=VECTOR('',#97362,1000.);
#11519=VECTOR('',#97363,1000.);
#11520=VECTOR('',#97364,1000.);
#11521=VECTOR('',#97367,1000.);
#11522=VECTOR('',#97368,1000.);
#11523=VECTOR('',#97369,1000.);
#11524=VECTOR('',#97372,1000.);
#11525=VECTOR('',#97373,1000.);
#11526=VECTOR('',#97374,1000.);
#11527=VECTOR('',#97377,1000.);
#11528=VECTOR('',#97378,1000.);
#11529=VECTOR('',#97381,1000.);
#11530=VECTOR('',#97382,1000.);
#11531=VECTOR('',#97383,1000.);
#11532=VECTOR('',#97384,1000.);
#11533=VECTOR('',#97387,1000.);
#11534=VECTOR('',#97388,1000.);
#11535=VECTOR('',#97389,1000.);
#11536=VECTOR('',#97392,1000.);
#11537=VECTOR('',#97393,1000.);
#11538=VECTOR('',#97394,1000.);
#11539=VECTOR('',#97397,1000.);
#11540=VECTOR('',#97398,1000.);
#11541=VECTOR('',#97401,1000.);
#11542=VECTOR('',#97402,1000.);
#11543=VECTOR('',#97403,1000.);
#11544=VECTOR('',#97404,1000.);
#11545=VECTOR('',#97407,1000.);
#11546=VECTOR('',#97408,1000.);
#11547=VECTOR('',#97409,1000.);
#11548=VECTOR('',#97412,1000.);
#11549=VECTOR('',#97413,1000.);
#11550=VECTOR('',#97414,1000.);
#11551=VECTOR('',#97417,1000.);
#11552=VECTOR('',#97418,1000.);
#11553=VECTOR('',#97421,1000.);
#11554=VECTOR('',#97422,1000.);
#11555=VECTOR('',#97423,1000.);
#11556=VECTOR('',#97424,1000.);
#11557=VECTOR('',#97427,1000.);
#11558=VECTOR('',#97428,1000.);
#11559=VECTOR('',#97429,1000.);
#11560=VECTOR('',#97432,1000.);
#11561=VECTOR('',#97433,1000.);
#11562=VECTOR('',#97434,1000.);
#11563=VECTOR('',#97437,1000.);
#11564=VECTOR('',#97438,1000.);
#11565=VECTOR('',#97441,1000.);
#11566=VECTOR('',#97442,1000.);
#11567=VECTOR('',#97443,1000.);
#11568=VECTOR('',#97444,1000.);
#11569=VECTOR('',#97447,1000.);
#11570=VECTOR('',#97448,1000.);
#11571=VECTOR('',#97449,1000.);
#11572=VECTOR('',#97452,1000.);
#11573=VECTOR('',#97453,1000.);
#11574=VECTOR('',#97454,1000.);
#11575=VECTOR('',#97457,1000.);
#11576=VECTOR('',#97458,1000.);
#11577=VECTOR('',#97461,1000.);
#11578=VECTOR('',#97462,1000.);
#11579=VECTOR('',#97463,1000.);
#11580=VECTOR('',#97464,1000.);
#11581=VECTOR('',#97467,1000.);
#11582=VECTOR('',#97468,1000.);
#11583=VECTOR('',#97469,1000.);
#11584=VECTOR('',#97472,1000.);
#11585=VECTOR('',#97473,1000.);
#11586=VECTOR('',#97474,1000.);
#11587=VECTOR('',#97477,1000.);
#11588=VECTOR('',#97478,1000.);
#11589=VECTOR('',#97481,1000.);
#11590=VECTOR('',#97482,1000.);
#11591=VECTOR('',#97483,1000.);
#11592=VECTOR('',#97484,1000.);
#11593=VECTOR('',#97487,1000.);
#11594=VECTOR('',#97488,1000.);
#11595=VECTOR('',#97489,1000.);
#11596=VECTOR('',#97492,1000.);
#11597=VECTOR('',#97493,1000.);
#11598=VECTOR('',#97494,1000.);
#11599=VECTOR('',#97497,1000.);
#11600=VECTOR('',#97498,1000.);
#11601=VECTOR('',#97501,1000.);
#11602=VECTOR('',#97502,1000.);
#11603=VECTOR('',#97503,1000.);
#11604=VECTOR('',#97504,1000.);
#11605=VECTOR('',#97507,1000.);
#11606=VECTOR('',#97508,1000.);
#11607=VECTOR('',#97509,1000.);
#11608=VECTOR('',#97512,1000.);
#11609=VECTOR('',#97513,1000.);
#11610=VECTOR('',#97514,1000.);
#11611=VECTOR('',#97517,1000.);
#11612=VECTOR('',#97518,1000.);
#11613=VECTOR('',#97521,1000.);
#11614=VECTOR('',#97522,1000.);
#11615=VECTOR('',#97523,1000.);
#11616=VECTOR('',#97524,1000.);
#11617=VECTOR('',#97527,1000.);
#11618=VECTOR('',#97528,1000.);
#11619=VECTOR('',#97529,1000.);
#11620=VECTOR('',#97532,1000.);
#11621=VECTOR('',#97533,1000.);
#11622=VECTOR('',#97534,1000.);
#11623=VECTOR('',#97537,1000.);
#11624=VECTOR('',#97538,1000.);
#11625=VECTOR('',#97541,1000.);
#11626=VECTOR('',#97542,1000.);
#11627=VECTOR('',#97543,1000.);
#11628=VECTOR('',#97544,1000.);
#11629=VECTOR('',#97547,1000.);
#11630=VECTOR('',#97548,1000.);
#11631=VECTOR('',#97549,1000.);
#11632=VECTOR('',#97552,1000.);
#11633=VECTOR('',#97553,1000.);
#11634=VECTOR('',#97554,1000.);
#11635=VECTOR('',#97557,1000.);
#11636=VECTOR('',#97558,1000.);
#11637=VECTOR('',#97561,1000.);
#11638=VECTOR('',#97562,1000.);
#11639=VECTOR('',#97563,1000.);
#11640=VECTOR('',#97564,1000.);
#11641=VECTOR('',#97567,1000.);
#11642=VECTOR('',#97568,1000.);
#11643=VECTOR('',#97569,1000.);
#11644=VECTOR('',#97572,1000.);
#11645=VECTOR('',#97573,1000.);
#11646=VECTOR('',#97574,1000.);
#11647=VECTOR('',#97577,1000.);
#11648=VECTOR('',#97578,1000.);
#11649=VECTOR('',#97581,1000.);
#11650=VECTOR('',#97582,1000.);
#11651=VECTOR('',#97583,1000.);
#11652=VECTOR('',#97584,1000.);
#11653=VECTOR('',#97587,1000.);
#11654=VECTOR('',#97588,1000.);
#11655=VECTOR('',#97589,1000.);
#11656=VECTOR('',#97592,1000.);
#11657=VECTOR('',#97593,1000.);
#11658=VECTOR('',#97594,1000.);
#11659=VECTOR('',#97597,1000.);
#11660=VECTOR('',#97598,1000.);
#11661=VECTOR('',#97601,1000.);
#11662=VECTOR('',#97602,1000.);
#11663=VECTOR('',#97603,1000.);
#11664=VECTOR('',#97604,1000.);
#11665=VECTOR('',#97607,1000.);
#11666=VECTOR('',#97608,1000.);
#11667=VECTOR('',#97609,1000.);
#11668=VECTOR('',#97612,1000.);
#11669=VECTOR('',#97613,1000.);
#11670=VECTOR('',#97614,1000.);
#11671=VECTOR('',#97617,1000.);
#11672=VECTOR('',#97618,1000.);
#11673=VECTOR('',#97621,1000.);
#11674=VECTOR('',#97622,1000.);
#11675=VECTOR('',#97623,1000.);
#11676=VECTOR('',#97624,1000.);
#11677=VECTOR('',#97627,1000.);
#11678=VECTOR('',#97628,1000.);
#11679=VECTOR('',#97629,1000.);
#11680=VECTOR('',#97632,1000.);
#11681=VECTOR('',#97633,1000.);
#11682=VECTOR('',#97634,1000.);
#11683=VECTOR('',#97637,1000.);
#11684=VECTOR('',#97638,1000.);
#11685=VECTOR('',#97641,1000.);
#11686=VECTOR('',#97642,1000.);
#11687=VECTOR('',#97643,1000.);
#11688=VECTOR('',#97644,1000.);
#11689=VECTOR('',#97647,1000.);
#11690=VECTOR('',#97648,1000.);
#11691=VECTOR('',#97649,1000.);
#11692=VECTOR('',#97652,1000.);
#11693=VECTOR('',#97653,1000.);
#11694=VECTOR('',#97654,1000.);
#11695=VECTOR('',#97657,1000.);
#11696=VECTOR('',#97658,1000.);
#11697=VECTOR('',#97661,1000.);
#11698=VECTOR('',#97662,1000.);
#11699=VECTOR('',#97663,1000.);
#11700=VECTOR('',#97664,1000.);
#11701=VECTOR('',#97667,1000.);
#11702=VECTOR('',#97668,1000.);
#11703=VECTOR('',#97669,1000.);
#11704=VECTOR('',#97672,1000.);
#11705=VECTOR('',#97673,1000.);
#11706=VECTOR('',#97674,1000.);
#11707=VECTOR('',#97677,1000.);
#11708=VECTOR('',#97678,1000.);
#11709=VECTOR('',#97681,1000.);
#11710=VECTOR('',#97682,1000.);
#11711=VECTOR('',#97683,1000.);
#11712=VECTOR('',#97684,1000.);
#11713=VECTOR('',#97687,1000.);
#11714=VECTOR('',#97688,1000.);
#11715=VECTOR('',#97689,1000.);
#11716=VECTOR('',#97692,1000.);
#11717=VECTOR('',#97693,1000.);
#11718=VECTOR('',#97694,1000.);
#11719=VECTOR('',#97697,1000.);
#11720=VECTOR('',#97698,1000.);
#11721=VECTOR('',#97701,1000.);
#11722=VECTOR('',#97702,1000.);
#11723=VECTOR('',#97703,1000.);
#11724=VECTOR('',#97704,1000.);
#11725=VECTOR('',#97707,1000.);
#11726=VECTOR('',#97708,1000.);
#11727=VECTOR('',#97709,1000.);
#11728=VECTOR('',#97712,1000.);
#11729=VECTOR('',#97713,1000.);
#11730=VECTOR('',#97714,1000.);
#11731=VECTOR('',#97717,1000.);
#11732=VECTOR('',#97718,1000.);
#11733=VECTOR('',#97721,1000.);
#11734=VECTOR('',#97722,1000.);
#11735=VECTOR('',#97723,1000.);
#11736=VECTOR('',#97724,1000.);
#11737=VECTOR('',#97727,1000.);
#11738=VECTOR('',#97728,1000.);
#11739=VECTOR('',#97729,1000.);
#11740=VECTOR('',#97732,1000.);
#11741=VECTOR('',#97733,1000.);
#11742=VECTOR('',#97734,1000.);
#11743=VECTOR('',#97737,1000.);
#11744=VECTOR('',#97738,1000.);
#11745=VECTOR('',#97741,1000.);
#11746=VECTOR('',#97742,1000.);
#11747=VECTOR('',#97743,1000.);
#11748=VECTOR('',#97744,1000.);
#11749=VECTOR('',#97747,1000.);
#11750=VECTOR('',#97748,1000.);
#11751=VECTOR('',#97749,1000.);
#11752=VECTOR('',#97752,1000.);
#11753=VECTOR('',#97753,1000.);
#11754=VECTOR('',#97754,1000.);
#11755=VECTOR('',#97757,1000.);
#11756=VECTOR('',#97758,1000.);
#11757=VECTOR('',#97761,1000.);
#11758=VECTOR('',#97762,1000.);
#11759=VECTOR('',#97763,1000.);
#11760=VECTOR('',#97764,1000.);
#11761=VECTOR('',#97767,1000.);
#11762=VECTOR('',#97768,1000.);
#11763=VECTOR('',#97769,1000.);
#11764=VECTOR('',#97772,1000.);
#11765=VECTOR('',#97773,1000.);
#11766=VECTOR('',#97774,1000.);
#11767=VECTOR('',#97777,1000.);
#11768=VECTOR('',#97778,1000.);
#11769=VECTOR('',#97781,1000.);
#11770=VECTOR('',#97782,1000.);
#11771=VECTOR('',#97783,1000.);
#11772=VECTOR('',#97784,1000.);
#11773=VECTOR('',#97787,1000.);
#11774=VECTOR('',#97788,1000.);
#11775=VECTOR('',#97789,1000.);
#11776=VECTOR('',#97792,1000.);
#11777=VECTOR('',#97793,1000.);
#11778=VECTOR('',#97794,1000.);
#11779=VECTOR('',#97797,1000.);
#11780=VECTOR('',#97798,1000.);
#11781=VECTOR('',#97801,1000.);
#11782=VECTOR('',#97802,1000.);
#11783=VECTOR('',#97803,1000.);
#11784=VECTOR('',#97804,1000.);
#11785=VECTOR('',#97807,1000.);
#11786=VECTOR('',#97808,1000.);
#11787=VECTOR('',#97809,1000.);
#11788=VECTOR('',#97812,1000.);
#11789=VECTOR('',#97813,1000.);
#11790=VECTOR('',#97814,1000.);
#11791=VECTOR('',#97817,1000.);
#11792=VECTOR('',#97818,1000.);
#11793=VECTOR('',#97821,1000.);
#11794=VECTOR('',#97822,1000.);
#11795=VECTOR('',#97823,1000.);
#11796=VECTOR('',#97824,1000.);
#11797=VECTOR('',#97827,1000.);
#11798=VECTOR('',#97828,1000.);
#11799=VECTOR('',#97829,1000.);
#11800=VECTOR('',#97832,1000.);
#11801=VECTOR('',#97833,1000.);
#11802=VECTOR('',#97834,1000.);
#11803=VECTOR('',#97837,1000.);
#11804=VECTOR('',#97838,1000.);
#11805=VECTOR('',#97841,1000.);
#11806=VECTOR('',#97842,1000.);
#11807=VECTOR('',#97843,1000.);
#11808=VECTOR('',#97844,1000.);
#11809=VECTOR('',#97847,1000.);
#11810=VECTOR('',#97848,1000.);
#11811=VECTOR('',#97849,1000.);
#11812=VECTOR('',#97852,1000.);
#11813=VECTOR('',#97853,1000.);
#11814=VECTOR('',#97854,1000.);
#11815=VECTOR('',#97857,1000.);
#11816=VECTOR('',#97858,1000.);
#11817=VECTOR('',#97861,1000.);
#11818=VECTOR('',#97862,1000.);
#11819=VECTOR('',#97863,1000.);
#11820=VECTOR('',#97864,1000.);
#11821=VECTOR('',#97867,1000.);
#11822=VECTOR('',#97868,1000.);
#11823=VECTOR('',#97869,1000.);
#11824=VECTOR('',#97872,1000.);
#11825=VECTOR('',#97873,1000.);
#11826=VECTOR('',#97874,1000.);
#11827=VECTOR('',#97877,1000.);
#11828=VECTOR('',#97878,1000.);
#11829=VECTOR('',#97881,1000.);
#11830=VECTOR('',#97882,1000.);
#11831=VECTOR('',#97883,1000.);
#11832=VECTOR('',#97884,1000.);
#11833=VECTOR('',#97887,1000.);
#11834=VECTOR('',#97888,1000.);
#11835=VECTOR('',#97889,1000.);
#11836=VECTOR('',#97892,1000.);
#11837=VECTOR('',#97893,1000.);
#11838=VECTOR('',#97894,1000.);
#11839=VECTOR('',#97897,1000.);
#11840=VECTOR('',#97898,1000.);
#11841=VECTOR('',#97901,1000.);
#11842=VECTOR('',#97902,1000.);
#11843=VECTOR('',#97903,1000.);
#11844=VECTOR('',#97904,1000.);
#11845=VECTOR('',#97907,1000.);
#11846=VECTOR('',#97908,1000.);
#11847=VECTOR('',#97909,1000.);
#11848=VECTOR('',#97912,1000.);
#11849=VECTOR('',#97913,1000.);
#11850=VECTOR('',#97914,1000.);
#11851=VECTOR('',#97917,1000.);
#11852=VECTOR('',#97918,1000.);
#11853=VECTOR('',#97921,1000.);
#11854=VECTOR('',#97922,1000.);
#11855=VECTOR('',#97923,1000.);
#11856=VECTOR('',#97924,1000.);
#11857=VECTOR('',#97927,1000.);
#11858=VECTOR('',#97928,1000.);
#11859=VECTOR('',#97929,1000.);
#11860=VECTOR('',#97932,1000.);
#11861=VECTOR('',#97933,1000.);
#11862=VECTOR('',#97934,1000.);
#11863=VECTOR('',#97937,1000.);
#11864=VECTOR('',#97938,1000.);
#11865=VECTOR('',#97941,1000.);
#11866=VECTOR('',#97942,1000.);
#11867=VECTOR('',#97943,1000.);
#11868=VECTOR('',#97944,1000.);
#11869=VECTOR('',#97947,1000.);
#11870=VECTOR('',#97948,1000.);
#11871=VECTOR('',#97949,1000.);
#11872=VECTOR('',#97952,1000.);
#11873=VECTOR('',#97953,1000.);
#11874=VECTOR('',#97954,1000.);
#11875=VECTOR('',#97957,1000.);
#11876=VECTOR('',#97958,1000.);
#11877=VECTOR('',#97961,1000.);
#11878=VECTOR('',#97962,1000.);
#11879=VECTOR('',#97963,1000.);
#11880=VECTOR('',#97964,1000.);
#11881=VECTOR('',#97967,1000.);
#11882=VECTOR('',#97968,1000.);
#11883=VECTOR('',#97969,1000.);
#11884=VECTOR('',#97972,1000.);
#11885=VECTOR('',#97973,1000.);
#11886=VECTOR('',#97974,1000.);
#11887=VECTOR('',#97977,1000.);
#11888=VECTOR('',#97978,1000.);
#11889=VECTOR('',#97981,1000.);
#11890=VECTOR('',#97982,1000.);
#11891=VECTOR('',#97983,1000.);
#11892=VECTOR('',#97984,1000.);
#11893=VECTOR('',#97987,1000.);
#11894=VECTOR('',#97988,1000.);
#11895=VECTOR('',#97989,1000.);
#11896=VECTOR('',#97992,1000.);
#11897=VECTOR('',#97993,1000.);
#11898=VECTOR('',#97994,1000.);
#11899=VECTOR('',#97997,1000.);
#11900=VECTOR('',#97998,1000.);
#11901=VECTOR('',#98001,1000.);
#11902=VECTOR('',#98002,1000.);
#11903=VECTOR('',#98003,1000.);
#11904=VECTOR('',#98004,1000.);
#11905=VECTOR('',#98007,1000.);
#11906=VECTOR('',#98008,1000.);
#11907=VECTOR('',#98009,1000.);
#11908=VECTOR('',#98012,1000.);
#11909=VECTOR('',#98013,1000.);
#11910=VECTOR('',#98014,1000.);
#11911=VECTOR('',#98017,1000.);
#11912=VECTOR('',#98018,1000.);
#11913=VECTOR('',#98021,1000.);
#11914=VECTOR('',#98022,1000.);
#11915=VECTOR('',#98023,1000.);
#11916=VECTOR('',#98024,1000.);
#11917=VECTOR('',#98027,1000.);
#11918=VECTOR('',#98028,1000.);
#11919=VECTOR('',#98029,1000.);
#11920=VECTOR('',#98032,1000.);
#11921=VECTOR('',#98033,1000.);
#11922=VECTOR('',#98034,1000.);
#11923=VECTOR('',#98037,1000.);
#11924=VECTOR('',#98038,1000.);
#11925=VECTOR('',#98041,1000.);
#11926=VECTOR('',#98042,1000.);
#11927=VECTOR('',#98043,1000.);
#11928=VECTOR('',#98044,1000.);
#11929=VECTOR('',#98047,1000.);
#11930=VECTOR('',#98048,1000.);
#11931=VECTOR('',#98049,1000.);
#11932=VECTOR('',#98052,1000.);
#11933=VECTOR('',#98053,1000.);
#11934=VECTOR('',#98054,1000.);
#11935=VECTOR('',#98057,1000.);
#11936=VECTOR('',#98058,1000.);
#11937=VECTOR('',#98061,1000.);
#11938=VECTOR('',#98062,1000.);
#11939=VECTOR('',#98063,1000.);
#11940=VECTOR('',#98064,1000.);
#11941=VECTOR('',#98067,1000.);
#11942=VECTOR('',#98068,1000.);
#11943=VECTOR('',#98069,1000.);
#11944=VECTOR('',#98072,1000.);
#11945=VECTOR('',#98073,1000.);
#11946=VECTOR('',#98074,1000.);
#11947=VECTOR('',#98077,1000.);
#11948=VECTOR('',#98078,1000.);
#11949=VECTOR('',#98081,1000.);
#11950=VECTOR('',#98082,1000.);
#11951=VECTOR('',#98083,1000.);
#11952=VECTOR('',#98084,1000.);
#11953=VECTOR('',#98087,1000.);
#11954=VECTOR('',#98088,1000.);
#11955=VECTOR('',#98089,1000.);
#11956=VECTOR('',#98092,1000.);
#11957=VECTOR('',#98093,1000.);
#11958=VECTOR('',#98094,1000.);
#11959=VECTOR('',#98097,1000.);
#11960=VECTOR('',#98098,1000.);
#11961=VECTOR('',#98101,1000.);
#11962=VECTOR('',#98102,1000.);
#11963=VECTOR('',#98103,1000.);
#11964=VECTOR('',#98104,1000.);
#11965=VECTOR('',#98107,1000.);
#11966=VECTOR('',#98108,1000.);
#11967=VECTOR('',#98109,1000.);
#11968=VECTOR('',#98112,1000.);
#11969=VECTOR('',#98113,1000.);
#11970=VECTOR('',#98114,1000.);
#11971=VECTOR('',#98117,1000.);
#11972=VECTOR('',#98118,1000.);
#11973=VECTOR('',#98121,1000.);
#11974=VECTOR('',#98122,1000.);
#11975=VECTOR('',#98123,1000.);
#11976=VECTOR('',#98124,1000.);
#11977=VECTOR('',#98127,1000.);
#11978=VECTOR('',#98128,1000.);
#11979=VECTOR('',#98129,1000.);
#11980=VECTOR('',#98132,1000.);
#11981=VECTOR('',#98133,1000.);
#11982=VECTOR('',#98134,1000.);
#11983=VECTOR('',#98137,1000.);
#11984=VECTOR('',#98138,1000.);
#11985=VECTOR('',#98141,1000.);
#11986=VECTOR('',#98142,1000.);
#11987=VECTOR('',#98143,1000.);
#11988=VECTOR('',#98144,1000.);
#11989=VECTOR('',#98147,1000.);
#11990=VECTOR('',#98148,1000.);
#11991=VECTOR('',#98149,1000.);
#11992=VECTOR('',#98152,1000.);
#11993=VECTOR('',#98153,1000.);
#11994=VECTOR('',#98154,1000.);
#11995=VECTOR('',#98157,1000.);
#11996=VECTOR('',#98158,1000.);
#11997=VECTOR('',#98161,1000.);
#11998=VECTOR('',#98162,1000.);
#11999=VECTOR('',#98163,1000.);
#12000=VECTOR('',#98164,1000.);
#12001=VECTOR('',#98167,1000.);
#12002=VECTOR('',#98168,1000.);
#12003=VECTOR('',#98169,1000.);
#12004=VECTOR('',#98172,1000.);
#12005=VECTOR('',#98173,1000.);
#12006=VECTOR('',#98174,1000.);
#12007=VECTOR('',#98177,1000.);
#12008=VECTOR('',#98178,1000.);
#12009=VECTOR('',#98181,1000.);
#12010=VECTOR('',#98182,1000.);
#12011=VECTOR('',#98183,1000.);
#12012=VECTOR('',#98184,1000.);
#12013=VECTOR('',#98187,1000.);
#12014=VECTOR('',#98188,1000.);
#12015=VECTOR('',#98189,1000.);
#12016=VECTOR('',#98192,1000.);
#12017=VECTOR('',#98193,1000.);
#12018=VECTOR('',#98194,1000.);
#12019=VECTOR('',#98197,1000.);
#12020=VECTOR('',#98198,1000.);
#12021=VECTOR('',#98201,1000.);
#12022=VECTOR('',#98202,1000.);
#12023=VECTOR('',#98203,1000.);
#12024=VECTOR('',#98204,1000.);
#12025=VECTOR('',#98207,1000.);
#12026=VECTOR('',#98208,1000.);
#12027=VECTOR('',#98209,1000.);
#12028=VECTOR('',#98212,1000.);
#12029=VECTOR('',#98213,1000.);
#12030=VECTOR('',#98214,1000.);
#12031=VECTOR('',#98217,1000.);
#12032=VECTOR('',#98218,1000.);
#12033=VECTOR('',#98221,1000.);
#12034=VECTOR('',#98222,1000.);
#12035=VECTOR('',#98223,1000.);
#12036=VECTOR('',#98224,1000.);
#12037=VECTOR('',#98227,1000.);
#12038=VECTOR('',#98228,1000.);
#12039=VECTOR('',#98229,1000.);
#12040=VECTOR('',#98232,1000.);
#12041=VECTOR('',#98233,1000.);
#12042=VECTOR('',#98234,1000.);
#12043=VECTOR('',#98237,1000.);
#12044=VECTOR('',#98238,1000.);
#12045=VECTOR('',#98241,1000.);
#12046=VECTOR('',#98242,1000.);
#12047=VECTOR('',#98243,1000.);
#12048=VECTOR('',#98244,1000.);
#12049=VECTOR('',#98247,1000.);
#12050=VECTOR('',#98248,1000.);
#12051=VECTOR('',#98249,1000.);
#12052=VECTOR('',#98252,1000.);
#12053=VECTOR('',#98253,1000.);
#12054=VECTOR('',#98254,1000.);
#12055=VECTOR('',#98257,1000.);
#12056=VECTOR('',#98258,1000.);
#12057=VECTOR('',#98261,1000.);
#12058=VECTOR('',#98262,1000.);
#12059=VECTOR('',#98263,1000.);
#12060=VECTOR('',#98264,1000.);
#12061=VECTOR('',#98267,1000.);
#12062=VECTOR('',#98268,1000.);
#12063=VECTOR('',#98269,1000.);
#12064=VECTOR('',#98272,1000.);
#12065=VECTOR('',#98273,1000.);
#12066=VECTOR('',#98274,1000.);
#12067=VECTOR('',#98277,1000.);
#12068=VECTOR('',#98278,1000.);
#12069=VECTOR('',#98281,1000.);
#12070=VECTOR('',#98282,1000.);
#12071=VECTOR('',#98283,1000.);
#12072=VECTOR('',#98284,1000.);
#12073=VECTOR('',#98287,1000.);
#12074=VECTOR('',#98288,1000.);
#12075=VECTOR('',#98289,1000.);
#12076=VECTOR('',#98292,1000.);
#12077=VECTOR('',#98293,1000.);
#12078=VECTOR('',#98294,1000.);
#12079=VECTOR('',#98297,1000.);
#12080=VECTOR('',#98298,1000.);
#12081=VECTOR('',#98301,1000.);
#12082=VECTOR('',#98302,1000.);
#12083=VECTOR('',#98303,1000.);
#12084=VECTOR('',#98304,1000.);
#12085=VECTOR('',#98307,1000.);
#12086=VECTOR('',#98308,1000.);
#12087=VECTOR('',#98309,1000.);
#12088=VECTOR('',#98312,1000.);
#12089=VECTOR('',#98313,1000.);
#12090=VECTOR('',#98314,1000.);
#12091=VECTOR('',#98317,1000.);
#12092=VECTOR('',#98318,1000.);
#12093=VECTOR('',#98321,1000.);
#12094=VECTOR('',#98322,1000.);
#12095=VECTOR('',#98323,1000.);
#12096=VECTOR('',#98324,1000.);
#12097=VECTOR('',#98327,1000.);
#12098=VECTOR('',#98328,1000.);
#12099=VECTOR('',#98329,1000.);
#12100=VECTOR('',#98332,1000.);
#12101=VECTOR('',#98333,1000.);
#12102=VECTOR('',#98334,1000.);
#12103=VECTOR('',#98337,1000.);
#12104=VECTOR('',#98338,1000.);
#12105=VECTOR('',#98341,1000.);
#12106=VECTOR('',#98342,1000.);
#12107=VECTOR('',#98343,1000.);
#12108=VECTOR('',#98344,1000.);
#12109=VECTOR('',#98347,1000.);
#12110=VECTOR('',#98348,1000.);
#12111=VECTOR('',#98349,1000.);
#12112=VECTOR('',#98352,1000.);
#12113=VECTOR('',#98353,1000.);
#12114=VECTOR('',#98354,1000.);
#12115=VECTOR('',#98357,1000.);
#12116=VECTOR('',#98358,1000.);
#12117=VECTOR('',#98361,1000.);
#12118=VECTOR('',#98362,1000.);
#12119=VECTOR('',#98363,1000.);
#12120=VECTOR('',#98364,1000.);
#12121=VECTOR('',#98367,1000.);
#12122=VECTOR('',#98368,1000.);
#12123=VECTOR('',#98369,1000.);
#12124=VECTOR('',#98372,1000.);
#12125=VECTOR('',#98373,1000.);
#12126=VECTOR('',#98374,1000.);
#12127=VECTOR('',#98377,1000.);
#12128=VECTOR('',#98378,1000.);
#12129=VECTOR('',#98381,1000.);
#12130=VECTOR('',#98382,1000.);
#12131=VECTOR('',#98383,1000.);
#12132=VECTOR('',#98384,1000.);
#12133=VECTOR('',#98387,1000.);
#12134=VECTOR('',#98388,1000.);
#12135=VECTOR('',#98389,1000.);
#12136=VECTOR('',#98392,1000.);
#12137=VECTOR('',#98393,1000.);
#12138=VECTOR('',#98394,1000.);
#12139=VECTOR('',#98397,1000.);
#12140=VECTOR('',#98398,1000.);
#12141=VECTOR('',#98401,1000.);
#12142=VECTOR('',#98402,1000.);
#12143=VECTOR('',#98403,1000.);
#12144=VECTOR('',#98404,1000.);
#12145=VECTOR('',#98407,1000.);
#12146=VECTOR('',#98408,1000.);
#12147=VECTOR('',#98409,1000.);
#12148=VECTOR('',#98412,1000.);
#12149=VECTOR('',#98413,1000.);
#12150=VECTOR('',#98414,1000.);
#12151=VECTOR('',#98417,1000.);
#12152=VECTOR('',#98418,1000.);
#12153=VECTOR('',#98421,1000.);
#12154=VECTOR('',#98422,1000.);
#12155=VECTOR('',#98423,1000.);
#12156=VECTOR('',#98424,1000.);
#12157=VECTOR('',#98427,1000.);
#12158=VECTOR('',#98428,1000.);
#12159=VECTOR('',#98429,1000.);
#12160=VECTOR('',#98432,1000.);
#12161=VECTOR('',#98433,1000.);
#12162=VECTOR('',#98434,1000.);
#12163=VECTOR('',#98437,1000.);
#12164=VECTOR('',#98438,1000.);
#12165=VECTOR('',#98441,1000.);
#12166=VECTOR('',#98442,1000.);
#12167=VECTOR('',#98443,1000.);
#12168=VECTOR('',#98444,1000.);
#12169=VECTOR('',#98447,1000.);
#12170=VECTOR('',#98448,1000.);
#12171=VECTOR('',#98449,1000.);
#12172=VECTOR('',#98452,1000.);
#12173=VECTOR('',#98453,1000.);
#12174=VECTOR('',#98454,1000.);
#12175=VECTOR('',#98457,1000.);
#12176=VECTOR('',#98458,1000.);
#12177=VECTOR('',#98461,1000.);
#12178=VECTOR('',#98462,1000.);
#12179=VECTOR('',#98463,1000.);
#12180=VECTOR('',#98464,1000.);
#12181=VECTOR('',#98467,1000.);
#12182=VECTOR('',#98468,1000.);
#12183=VECTOR('',#98469,1000.);
#12184=VECTOR('',#98472,1000.);
#12185=VECTOR('',#98473,1000.);
#12186=VECTOR('',#98474,1000.);
#12187=VECTOR('',#98477,1000.);
#12188=VECTOR('',#98478,1000.);
#12189=VECTOR('',#98481,1000.);
#12190=VECTOR('',#98482,1000.);
#12191=VECTOR('',#98483,1000.);
#12192=VECTOR('',#98484,1000.);
#12193=VECTOR('',#98487,1000.);
#12194=VECTOR('',#98488,1000.);
#12195=VECTOR('',#98489,1000.);
#12196=VECTOR('',#98492,1000.);
#12197=VECTOR('',#98493,1000.);
#12198=VECTOR('',#98494,1000.);
#12199=VECTOR('',#98497,1000.);
#12200=VECTOR('',#98498,1000.);
#12201=VECTOR('',#98501,1000.);
#12202=VECTOR('',#98502,1000.);
#12203=VECTOR('',#98503,1000.);
#12204=VECTOR('',#98504,1000.);
#12205=VECTOR('',#98507,1000.);
#12206=VECTOR('',#98508,1000.);
#12207=VECTOR('',#98509,1000.);
#12208=VECTOR('',#98512,1000.);
#12209=VECTOR('',#98513,1000.);
#12210=VECTOR('',#98514,1000.);
#12211=VECTOR('',#98517,1000.);
#12212=VECTOR('',#98518,1000.);
#12213=VECTOR('',#98521,1000.);
#12214=VECTOR('',#98522,1000.);
#12215=VECTOR('',#98523,1000.);
#12216=VECTOR('',#98524,1000.);
#12217=VECTOR('',#98527,1000.);
#12218=VECTOR('',#98528,1000.);
#12219=VECTOR('',#98529,1000.);
#12220=VECTOR('',#98532,1000.);
#12221=VECTOR('',#98533,1000.);
#12222=VECTOR('',#98534,1000.);
#12223=VECTOR('',#98537,1000.);
#12224=VECTOR('',#98538,1000.);
#12225=VECTOR('',#98541,1000.);
#12226=VECTOR('',#98542,1000.);
#12227=VECTOR('',#98543,1000.);
#12228=VECTOR('',#98544,1000.);
#12229=VECTOR('',#98547,1000.);
#12230=VECTOR('',#98548,1000.);
#12231=VECTOR('',#98549,1000.);
#12232=VECTOR('',#98552,1000.);
#12233=VECTOR('',#98553,1000.);
#12234=VECTOR('',#98554,1000.);
#12235=VECTOR('',#98557,1000.);
#12236=VECTOR('',#98558,1000.);
#12237=VECTOR('',#98561,1000.);
#12238=VECTOR('',#98562,1000.);
#12239=VECTOR('',#98563,1000.);
#12240=VECTOR('',#98564,1000.);
#12241=VECTOR('',#98567,1000.);
#12242=VECTOR('',#98568,1000.);
#12243=VECTOR('',#98569,1000.);
#12244=VECTOR('',#98572,1000.);
#12245=VECTOR('',#98573,1000.);
#12246=VECTOR('',#98574,1000.);
#12247=VECTOR('',#98577,1000.);
#12248=VECTOR('',#98578,1000.);
#12249=VECTOR('',#98581,1000.);
#12250=VECTOR('',#98582,1000.);
#12251=VECTOR('',#98583,1000.);
#12252=VECTOR('',#98584,1000.);
#12253=VECTOR('',#98587,1000.);
#12254=VECTOR('',#98588,1000.);
#12255=VECTOR('',#98589,1000.);
#12256=VECTOR('',#98592,1000.);
#12257=VECTOR('',#98593,1000.);
#12258=VECTOR('',#98594,1000.);
#12259=VECTOR('',#98597,1000.);
#12260=VECTOR('',#98598,1000.);
#12261=VECTOR('',#98601,1000.);
#12262=VECTOR('',#98602,1000.);
#12263=VECTOR('',#98603,1000.);
#12264=VECTOR('',#98604,1000.);
#12265=VECTOR('',#98607,1000.);
#12266=VECTOR('',#98608,1000.);
#12267=VECTOR('',#98609,1000.);
#12268=VECTOR('',#98612,1000.);
#12269=VECTOR('',#98613,1000.);
#12270=VECTOR('',#98614,1000.);
#12271=VECTOR('',#98617,1000.);
#12272=VECTOR('',#98618,1000.);
#12273=VECTOR('',#98621,1000.);
#12274=VECTOR('',#98622,1000.);
#12275=VECTOR('',#98623,1000.);
#12276=VECTOR('',#98624,1000.);
#12277=VECTOR('',#98627,1000.);
#12278=VECTOR('',#98628,1000.);
#12279=VECTOR('',#98629,1000.);
#12280=VECTOR('',#98632,1000.);
#12281=VECTOR('',#98633,1000.);
#12282=VECTOR('',#98634,1000.);
#12283=VECTOR('',#98637,1000.);
#12284=VECTOR('',#98638,1000.);
#12285=VECTOR('',#98641,1000.);
#12286=VECTOR('',#98642,1000.);
#12287=VECTOR('',#98643,1000.);
#12288=VECTOR('',#98644,1000.);
#12289=VECTOR('',#98647,1000.);
#12290=VECTOR('',#98648,1000.);
#12291=VECTOR('',#98649,1000.);
#12292=VECTOR('',#98652,1000.);
#12293=VECTOR('',#98653,1000.);
#12294=VECTOR('',#98654,1000.);
#12295=VECTOR('',#98657,1000.);
#12296=VECTOR('',#98658,1000.);
#12297=VECTOR('',#98661,1000.);
#12298=VECTOR('',#98662,1000.);
#12299=VECTOR('',#98663,1000.);
#12300=VECTOR('',#98664,1000.);
#12301=VECTOR('',#98667,1000.);
#12302=VECTOR('',#98668,1000.);
#12303=VECTOR('',#98669,1000.);
#12304=VECTOR('',#98672,1000.);
#12305=VECTOR('',#98673,1000.);
#12306=VECTOR('',#98674,1000.);
#12307=VECTOR('',#98677,1000.);
#12308=VECTOR('',#98678,1000.);
#12309=VECTOR('',#98681,1000.);
#12310=VECTOR('',#98682,1000.);
#12311=VECTOR('',#98683,1000.);
#12312=VECTOR('',#98684,1000.);
#12313=VECTOR('',#98687,1000.);
#12314=VECTOR('',#98688,1000.);
#12315=VECTOR('',#98689,1000.);
#12316=VECTOR('',#98692,1000.);
#12317=VECTOR('',#98693,1000.);
#12318=VECTOR('',#98694,1000.);
#12319=VECTOR('',#98697,1000.);
#12320=VECTOR('',#98698,1000.);
#12321=VECTOR('',#98701,1000.);
#12322=VECTOR('',#98702,1000.);
#12323=VECTOR('',#98703,1000.);
#12324=VECTOR('',#98704,1000.);
#12325=VECTOR('',#98707,1000.);
#12326=VECTOR('',#98708,1000.);
#12327=VECTOR('',#98709,1000.);
#12328=VECTOR('',#98712,1000.);
#12329=VECTOR('',#98713,1000.);
#12330=VECTOR('',#98714,1000.);
#12331=VECTOR('',#98717,1000.);
#12332=VECTOR('',#98718,1000.);
#12333=VECTOR('',#98721,1000.);
#12334=VECTOR('',#98722,1000.);
#12335=VECTOR('',#98723,1000.);
#12336=VECTOR('',#98724,1000.);
#12337=VECTOR('',#98727,1000.);
#12338=VECTOR('',#98728,1000.);
#12339=VECTOR('',#98729,1000.);
#12340=VECTOR('',#98732,1000.);
#12341=VECTOR('',#98733,1000.);
#12342=VECTOR('',#98734,1000.);
#12343=VECTOR('',#98737,1000.);
#12344=VECTOR('',#98738,1000.);
#12345=VECTOR('',#98741,1000.);
#12346=VECTOR('',#98742,1000.);
#12347=VECTOR('',#98743,1000.);
#12348=VECTOR('',#98744,1000.);
#12349=VECTOR('',#98747,1000.);
#12350=VECTOR('',#98748,1000.);
#12351=VECTOR('',#98749,1000.);
#12352=VECTOR('',#98752,1000.);
#12353=VECTOR('',#98753,1000.);
#12354=VECTOR('',#98754,1000.);
#12355=VECTOR('',#98757,1000.);
#12356=VECTOR('',#98758,1000.);
#12357=VECTOR('',#98761,1000.);
#12358=VECTOR('',#98762,1000.);
#12359=VECTOR('',#98763,1000.);
#12360=VECTOR('',#98764,1000.);
#12361=VECTOR('',#98767,1000.);
#12362=VECTOR('',#98768,1000.);
#12363=VECTOR('',#98769,1000.);
#12364=VECTOR('',#98772,1000.);
#12365=VECTOR('',#98773,1000.);
#12366=VECTOR('',#98774,1000.);
#12367=VECTOR('',#98777,1000.);
#12368=VECTOR('',#98778,1000.);
#12369=VECTOR('',#98781,1000.);
#12370=VECTOR('',#98782,1000.);
#12371=VECTOR('',#98783,1000.);
#12372=VECTOR('',#98784,1000.);
#12373=VECTOR('',#98787,1000.);
#12374=VECTOR('',#98788,1000.);
#12375=VECTOR('',#98789,1000.);
#12376=VECTOR('',#98792,1000.);
#12377=VECTOR('',#98793,1000.);
#12378=VECTOR('',#98794,1000.);
#12379=VECTOR('',#98797,1000.);
#12380=VECTOR('',#98798,1000.);
#12381=VECTOR('',#98801,1000.);
#12382=VECTOR('',#98802,1000.);
#12383=VECTOR('',#98803,1000.);
#12384=VECTOR('',#98804,1000.);
#12385=VECTOR('',#98807,1000.);
#12386=VECTOR('',#98808,1000.);
#12387=VECTOR('',#98809,1000.);
#12388=VECTOR('',#98812,1000.);
#12389=VECTOR('',#98813,1000.);
#12390=VECTOR('',#98814,1000.);
#12391=VECTOR('',#98817,1000.);
#12392=VECTOR('',#98818,1000.);
#12393=VECTOR('',#98821,1000.);
#12394=VECTOR('',#98822,1000.);
#12395=VECTOR('',#98823,1000.);
#12396=VECTOR('',#98824,1000.);
#12397=VECTOR('',#98827,1000.);
#12398=VECTOR('',#98828,1000.);
#12399=VECTOR('',#98829,1000.);
#12400=VECTOR('',#98832,1000.);
#12401=VECTOR('',#98833,1000.);
#12402=VECTOR('',#98834,1000.);
#12403=VECTOR('',#98837,1000.);
#12404=VECTOR('',#98838,1000.);
#12405=VECTOR('',#98841,1000.);
#12406=VECTOR('',#98842,1000.);
#12407=VECTOR('',#98843,1000.);
#12408=VECTOR('',#98844,1000.);
#12409=VECTOR('',#98847,1000.);
#12410=VECTOR('',#98848,1000.);
#12411=VECTOR('',#98849,1000.);
#12412=VECTOR('',#98852,1000.);
#12413=VECTOR('',#98853,1000.);
#12414=VECTOR('',#98854,1000.);
#12415=VECTOR('',#98857,1000.);
#12416=VECTOR('',#98858,1000.);
#12417=VECTOR('',#98861,1000.);
#12418=VECTOR('',#98862,1000.);
#12419=VECTOR('',#98863,1000.);
#12420=VECTOR('',#98864,1000.);
#12421=VECTOR('',#98867,1000.);
#12422=VECTOR('',#98868,1000.);
#12423=VECTOR('',#98869,1000.);
#12424=VECTOR('',#98872,1000.);
#12425=VECTOR('',#98873,1000.);
#12426=VECTOR('',#98874,1000.);
#12427=VECTOR('',#98877,1000.);
#12428=VECTOR('',#98878,1000.);
#12429=VECTOR('',#98881,1000.);
#12430=VECTOR('',#98882,1000.);
#12431=VECTOR('',#98883,1000.);
#12432=VECTOR('',#98884,1000.);
#12433=VECTOR('',#98887,1000.);
#12434=VECTOR('',#98888,1000.);
#12435=VECTOR('',#98889,1000.);
#12436=VECTOR('',#98892,1000.);
#12437=VECTOR('',#98893,1000.);
#12438=VECTOR('',#98894,1000.);
#12439=VECTOR('',#98897,1000.);
#12440=VECTOR('',#98898,1000.);
#12441=VECTOR('',#98901,1000.);
#12442=VECTOR('',#98902,1000.);
#12443=VECTOR('',#98903,1000.);
#12444=VECTOR('',#98904,1000.);
#12445=VECTOR('',#98907,1000.);
#12446=VECTOR('',#98908,1000.);
#12447=VECTOR('',#98909,1000.);
#12448=VECTOR('',#98912,1000.);
#12449=VECTOR('',#98913,1000.);
#12450=VECTOR('',#98914,1000.);
#12451=VECTOR('',#98917,1000.);
#12452=VECTOR('',#98918,1000.);
#12453=VECTOR('',#98921,1000.);
#12454=VECTOR('',#98922,1000.);
#12455=VECTOR('',#98923,1000.);
#12456=VECTOR('',#98924,1000.);
#12457=VECTOR('',#98927,1000.);
#12458=VECTOR('',#98928,1000.);
#12459=VECTOR('',#98929,1000.);
#12460=VECTOR('',#98932,1000.);
#12461=VECTOR('',#98933,1000.);
#12462=VECTOR('',#98934,1000.);
#12463=VECTOR('',#98937,1000.);
#12464=VECTOR('',#98938,1000.);
#12465=VECTOR('',#98941,1000.);
#12466=VECTOR('',#98942,1000.);
#12467=VECTOR('',#98943,1000.);
#12468=VECTOR('',#98944,1000.);
#12469=VECTOR('',#98947,1000.);
#12470=VECTOR('',#98948,1000.);
#12471=VECTOR('',#98949,1000.);
#12472=VECTOR('',#98952,1000.);
#12473=VECTOR('',#98953,1000.);
#12474=VECTOR('',#98954,1000.);
#12475=VECTOR('',#98957,1000.);
#12476=VECTOR('',#98958,1000.);
#12477=VECTOR('',#98961,1000.);
#12478=VECTOR('',#98962,1000.);
#12479=VECTOR('',#98963,1000.);
#12480=VECTOR('',#98964,1000.);
#12481=VECTOR('',#98967,1000.);
#12482=VECTOR('',#98968,1000.);
#12483=VECTOR('',#98969,1000.);
#12484=VECTOR('',#98972,1000.);
#12485=VECTOR('',#98973,1000.);
#12486=VECTOR('',#98974,1000.);
#12487=VECTOR('',#98977,1000.);
#12488=VECTOR('',#98978,1000.);
#12489=VECTOR('',#98981,1000.);
#12490=VECTOR('',#98982,1000.);
#12491=VECTOR('',#98983,1000.);
#12492=VECTOR('',#98984,1000.);
#12493=VECTOR('',#98987,1000.);
#12494=VECTOR('',#98988,1000.);
#12495=VECTOR('',#98989,1000.);
#12496=VECTOR('',#98992,1000.);
#12497=VECTOR('',#98993,1000.);
#12498=VECTOR('',#98994,1000.);
#12499=VECTOR('',#98997,1000.);
#12500=VECTOR('',#98998,1000.);
#12501=VECTOR('',#99001,1000.);
#12502=VECTOR('',#99002,1000.);
#12503=VECTOR('',#99003,1000.);
#12504=VECTOR('',#99004,1000.);
#12505=VECTOR('',#99007,1000.);
#12506=VECTOR('',#99008,1000.);
#12507=VECTOR('',#99009,1000.);
#12508=VECTOR('',#99012,1000.);
#12509=VECTOR('',#99013,1000.);
#12510=VECTOR('',#99014,1000.);
#12511=VECTOR('',#99017,1000.);
#12512=VECTOR('',#99018,1000.);
#12513=VECTOR('',#99021,1000.);
#12514=VECTOR('',#99022,1000.);
#12515=VECTOR('',#99023,1000.);
#12516=VECTOR('',#99024,1000.);
#12517=VECTOR('',#99027,1000.);
#12518=VECTOR('',#99028,1000.);
#12519=VECTOR('',#99029,1000.);
#12520=VECTOR('',#99032,1000.);
#12521=VECTOR('',#99033,1000.);
#12522=VECTOR('',#99034,1000.);
#12523=VECTOR('',#99037,1000.);
#12524=VECTOR('',#99038,1000.);
#12525=VECTOR('',#99041,1000.);
#12526=VECTOR('',#99042,1000.);
#12527=VECTOR('',#99043,1000.);
#12528=VECTOR('',#99044,1000.);
#12529=VECTOR('',#99047,1000.);
#12530=VECTOR('',#99048,1000.);
#12531=VECTOR('',#99049,1000.);
#12532=VECTOR('',#99052,1000.);
#12533=VECTOR('',#99053,1000.);
#12534=VECTOR('',#99054,1000.);
#12535=VECTOR('',#99057,1000.);
#12536=VECTOR('',#99058,1000.);
#12537=VECTOR('',#99061,1000.);
#12538=VECTOR('',#99062,1000.);
#12539=VECTOR('',#99063,1000.);
#12540=VECTOR('',#99064,1000.);
#12541=VECTOR('',#99067,1000.);
#12542=VECTOR('',#99068,1000.);
#12543=VECTOR('',#99069,1000.);
#12544=VECTOR('',#99072,1000.);
#12545=VECTOR('',#99073,1000.);
#12546=VECTOR('',#99074,1000.);
#12547=VECTOR('',#99077,1000.);
#12548=VECTOR('',#99078,1000.);
#12549=VECTOR('',#99081,1000.);
#12550=VECTOR('',#99082,1000.);
#12551=VECTOR('',#99083,1000.);
#12552=VECTOR('',#99084,1000.);
#12553=VECTOR('',#99087,1000.);
#12554=VECTOR('',#99088,1000.);
#12555=VECTOR('',#99089,1000.);
#12556=VECTOR('',#99092,1000.);
#12557=VECTOR('',#99093,1000.);
#12558=VECTOR('',#99094,1000.);
#12559=VECTOR('',#99097,1000.);
#12560=VECTOR('',#99098,1000.);
#12561=VECTOR('',#99101,1000.);
#12562=VECTOR('',#99102,1000.);
#12563=VECTOR('',#99103,1000.);
#12564=VECTOR('',#99104,1000.);
#12565=VECTOR('',#99107,1000.);
#12566=VECTOR('',#99108,1000.);
#12567=VECTOR('',#99109,1000.);
#12568=VECTOR('',#99112,1000.);
#12569=VECTOR('',#99113,1000.);
#12570=VECTOR('',#99114,1000.);
#12571=VECTOR('',#99117,1000.);
#12572=VECTOR('',#99118,1000.);
#12573=VECTOR('',#99121,1000.);
#12574=VECTOR('',#99122,1000.);
#12575=VECTOR('',#99123,1000.);
#12576=VECTOR('',#99124,1000.);
#12577=VECTOR('',#99127,1000.);
#12578=VECTOR('',#99128,1000.);
#12579=VECTOR('',#99129,1000.);
#12580=VECTOR('',#99132,1000.);
#12581=VECTOR('',#99133,1000.);
#12582=VECTOR('',#99134,1000.);
#12583=VECTOR('',#99137,1000.);
#12584=VECTOR('',#99138,1000.);
#12585=VECTOR('',#99141,1000.);
#12586=VECTOR('',#99142,1000.);
#12587=VECTOR('',#99143,1000.);
#12588=VECTOR('',#99144,1000.);
#12589=VECTOR('',#99147,1000.);
#12590=VECTOR('',#99148,1000.);
#12591=VECTOR('',#99149,1000.);
#12592=VECTOR('',#99152,1000.);
#12593=VECTOR('',#99153,1000.);
#12594=VECTOR('',#99154,1000.);
#12595=VECTOR('',#99157,1000.);
#12596=VECTOR('',#99158,1000.);
#12597=VECTOR('',#99161,1000.);
#12598=VECTOR('',#99162,1000.);
#12599=VECTOR('',#99163,1000.);
#12600=VECTOR('',#99164,1000.);
#12601=VECTOR('',#99167,1000.);
#12602=VECTOR('',#99168,1000.);
#12603=VECTOR('',#99169,1000.);
#12604=VECTOR('',#99172,1000.);
#12605=VECTOR('',#99173,1000.);
#12606=VECTOR('',#99174,1000.);
#12607=VECTOR('',#99177,1000.);
#12608=VECTOR('',#99178,1000.);
#12609=VECTOR('',#99181,1000.);
#12610=VECTOR('',#99182,1000.);
#12611=VECTOR('',#99183,1000.);
#12612=VECTOR('',#99184,1000.);
#12613=VECTOR('',#99187,1000.);
#12614=VECTOR('',#99188,1000.);
#12615=VECTOR('',#99189,1000.);
#12616=VECTOR('',#99192,1000.);
#12617=VECTOR('',#99193,1000.);
#12618=VECTOR('',#99194,1000.);
#12619=VECTOR('',#99197,1000.);
#12620=VECTOR('',#99198,1000.);
#12621=VECTOR('',#99201,1000.);
#12622=VECTOR('',#99202,1000.);
#12623=VECTOR('',#99203,1000.);
#12624=VECTOR('',#99204,1000.);
#12625=VECTOR('',#99207,1000.);
#12626=VECTOR('',#99208,1000.);
#12627=VECTOR('',#99209,1000.);
#12628=VECTOR('',#99212,1000.);
#12629=VECTOR('',#99213,1000.);
#12630=VECTOR('',#99214,1000.);
#12631=VECTOR('',#99217,1000.);
#12632=VECTOR('',#99218,1000.);
#12633=VECTOR('',#99221,1000.);
#12634=VECTOR('',#99222,1000.);
#12635=VECTOR('',#99223,1000.);
#12636=VECTOR('',#99224,1000.);
#12637=VECTOR('',#99227,1000.);
#12638=VECTOR('',#99228,1000.);
#12639=VECTOR('',#99229,1000.);
#12640=VECTOR('',#99232,1000.);
#12641=VECTOR('',#99233,1000.);
#12642=VECTOR('',#99234,1000.);
#12643=VECTOR('',#99237,1000.);
#12644=VECTOR('',#99238,1000.);
#12645=VECTOR('',#99241,1000.);
#12646=VECTOR('',#99242,1000.);
#12647=VECTOR('',#99243,1000.);
#12648=VECTOR('',#99244,1000.);
#12649=VECTOR('',#99247,1000.);
#12650=VECTOR('',#99248,1000.);
#12651=VECTOR('',#99249,1000.);
#12652=VECTOR('',#99252,1000.);
#12653=VECTOR('',#99253,1000.);
#12654=VECTOR('',#99254,1000.);
#12655=VECTOR('',#99257,1000.);
#12656=VECTOR('',#99258,1000.);
#12657=VECTOR('',#99261,1000.);
#12658=VECTOR('',#99262,1000.);
#12659=VECTOR('',#99263,1000.);
#12660=VECTOR('',#99264,1000.);
#12661=VECTOR('',#99267,1000.);
#12662=VECTOR('',#99268,1000.);
#12663=VECTOR('',#99269,1000.);
#12664=VECTOR('',#99272,1000.);
#12665=VECTOR('',#99273,1000.);
#12666=VECTOR('',#99274,1000.);
#12667=VECTOR('',#99277,1000.);
#12668=VECTOR('',#99278,1000.);
#12669=VECTOR('',#99281,1000.);
#12670=VECTOR('',#99282,1000.);
#12671=VECTOR('',#99283,1000.);
#12672=VECTOR('',#99284,1000.);
#12673=VECTOR('',#99287,1000.);
#12674=VECTOR('',#99288,1000.);
#12675=VECTOR('',#99289,1000.);
#12676=VECTOR('',#99292,1000.);
#12677=VECTOR('',#99293,1000.);
#12678=VECTOR('',#99294,1000.);
#12679=VECTOR('',#99297,1000.);
#12680=VECTOR('',#99298,1000.);
#12681=VECTOR('',#99301,1000.);
#12682=VECTOR('',#99302,1000.);
#12683=VECTOR('',#99303,1000.);
#12684=VECTOR('',#99304,1000.);
#12685=VECTOR('',#99307,1000.);
#12686=VECTOR('',#99308,1000.);
#12687=VECTOR('',#99309,1000.);
#12688=VECTOR('',#99312,1000.);
#12689=VECTOR('',#99313,1000.);
#12690=VECTOR('',#99314,1000.);
#12691=VECTOR('',#99317,1000.);
#12692=VECTOR('',#99318,1000.);
#12693=VECTOR('',#99321,1000.);
#12694=VECTOR('',#99322,1000.);
#12695=VECTOR('',#99323,1000.);
#12696=VECTOR('',#99324,1000.);
#12697=VECTOR('',#99327,1000.);
#12698=VECTOR('',#99328,1000.);
#12699=VECTOR('',#99329,1000.);
#12700=VECTOR('',#99332,1000.);
#12701=VECTOR('',#99333,1000.);
#12702=VECTOR('',#99334,1000.);
#12703=VECTOR('',#99337,1000.);
#12704=VECTOR('',#99338,1000.);
#12705=VECTOR('',#99341,1000.);
#12706=VECTOR('',#99342,1000.);
#12707=VECTOR('',#99343,1000.);
#12708=VECTOR('',#99344,1000.);
#12709=VECTOR('',#99347,1000.);
#12710=VECTOR('',#99348,1000.);
#12711=VECTOR('',#99349,1000.);
#12712=VECTOR('',#99352,1000.);
#12713=VECTOR('',#99353,1000.);
#12714=VECTOR('',#99354,1000.);
#12715=VECTOR('',#99357,1000.);
#12716=VECTOR('',#99358,1000.);
#12717=VECTOR('',#99361,1000.);
#12718=VECTOR('',#99362,1000.);
#12719=VECTOR('',#99363,1000.);
#12720=VECTOR('',#99364,1000.);
#12721=VECTOR('',#99367,1000.);
#12722=VECTOR('',#99368,1000.);
#12723=VECTOR('',#99369,1000.);
#12724=VECTOR('',#99372,1000.);
#12725=VECTOR('',#99373,1000.);
#12726=VECTOR('',#99374,1000.);
#12727=VECTOR('',#99377,1000.);
#12728=VECTOR('',#99378,1000.);
#12729=VECTOR('',#99381,1000.);
#12730=VECTOR('',#99382,1000.);
#12731=VECTOR('',#99383,1000.);
#12732=VECTOR('',#99384,1000.);
#12733=VECTOR('',#99387,1000.);
#12734=VECTOR('',#99388,1000.);
#12735=VECTOR('',#99389,1000.);
#12736=VECTOR('',#99392,1000.);
#12737=VECTOR('',#99393,1000.);
#12738=VECTOR('',#99394,1000.);
#12739=VECTOR('',#99397,1000.);
#12740=VECTOR('',#99398,1000.);
#12741=VECTOR('',#99401,1000.);
#12742=VECTOR('',#99402,1000.);
#12743=VECTOR('',#99403,1000.);
#12744=VECTOR('',#99404,1000.);
#12745=VECTOR('',#99407,1000.);
#12746=VECTOR('',#99408,1000.);
#12747=VECTOR('',#99409,1000.);
#12748=VECTOR('',#99412,1000.);
#12749=VECTOR('',#99413,1000.);
#12750=VECTOR('',#99414,1000.);
#12751=VECTOR('',#99417,1000.);
#12752=VECTOR('',#99418,1000.);
#12753=VECTOR('',#99421,1000.);
#12754=VECTOR('',#99422,1000.);
#12755=VECTOR('',#99423,1000.);
#12756=VECTOR('',#99424,1000.);
#12757=VECTOR('',#99427,1000.);
#12758=VECTOR('',#99428,1000.);
#12759=VECTOR('',#99429,1000.);
#12760=VECTOR('',#99432,1000.);
#12761=VECTOR('',#99433,1000.);
#12762=VECTOR('',#99434,1000.);
#12763=VECTOR('',#99437,1000.);
#12764=VECTOR('',#99438,1000.);
#12765=VECTOR('',#99441,1000.);
#12766=VECTOR('',#99442,1000.);
#12767=VECTOR('',#99443,1000.);
#12768=VECTOR('',#99444,1000.);
#12769=VECTOR('',#99447,1000.);
#12770=VECTOR('',#99448,1000.);
#12771=VECTOR('',#99449,1000.);
#12772=VECTOR('',#99452,1000.);
#12773=VECTOR('',#99453,1000.);
#12774=VECTOR('',#99454,1000.);
#12775=VECTOR('',#99457,1000.);
#12776=VECTOR('',#99458,1000.);
#12777=VECTOR('',#99461,1000.);
#12778=VECTOR('',#99462,1000.);
#12779=VECTOR('',#99463,1000.);
#12780=VECTOR('',#99464,1000.);
#12781=VECTOR('',#99467,1000.);
#12782=VECTOR('',#99468,1000.);
#12783=VECTOR('',#99469,1000.);
#12784=VECTOR('',#99472,1000.);
#12785=VECTOR('',#99473,1000.);
#12786=VECTOR('',#99474,1000.);
#12787=VECTOR('',#99477,1000.);
#12788=VECTOR('',#99478,1000.);
#12789=VECTOR('',#99481,1000.);
#12790=VECTOR('',#99482,1000.);
#12791=VECTOR('',#99483,1000.);
#12792=VECTOR('',#99484,1000.);
#12793=VECTOR('',#99487,1000.);
#12794=VECTOR('',#99488,1000.);
#12795=VECTOR('',#99489,1000.);
#12796=VECTOR('',#99492,1000.);
#12797=VECTOR('',#99493,1000.);
#12798=VECTOR('',#99494,1000.);
#12799=VECTOR('',#99497,1000.);
#12800=VECTOR('',#99498,1000.);
#12801=VECTOR('',#99501,1000.);
#12802=VECTOR('',#99502,1000.);
#12803=VECTOR('',#99503,1000.);
#12804=VECTOR('',#99504,1000.);
#12805=VECTOR('',#99507,1000.);
#12806=VECTOR('',#99508,1000.);
#12807=VECTOR('',#99509,1000.);
#12808=VECTOR('',#99512,1000.);
#12809=VECTOR('',#99513,1000.);
#12810=VECTOR('',#99514,1000.);
#12811=VECTOR('',#99517,1000.);
#12812=VECTOR('',#99518,1000.);
#12813=VECTOR('',#99521,1000.);
#12814=VECTOR('',#99522,1000.);
#12815=VECTOR('',#99523,1000.);
#12816=VECTOR('',#99524,1000.);
#12817=VECTOR('',#99527,1000.);
#12818=VECTOR('',#99528,1000.);
#12819=VECTOR('',#99529,1000.);
#12820=VECTOR('',#99532,1000.);
#12821=VECTOR('',#99533,1000.);
#12822=VECTOR('',#99534,1000.);
#12823=VECTOR('',#99537,1000.);
#12824=VECTOR('',#99538,1000.);
#12825=VECTOR('',#99541,1000.);
#12826=VECTOR('',#99542,1000.);
#12827=VECTOR('',#99543,1000.);
#12828=VECTOR('',#99544,1000.);
#12829=VECTOR('',#99547,1000.);
#12830=VECTOR('',#99548,1000.);
#12831=VECTOR('',#99549,1000.);
#12832=VECTOR('',#99552,1000.);
#12833=VECTOR('',#99553,1000.);
#12834=VECTOR('',#99554,1000.);
#12835=VECTOR('',#99557,1000.);
#12836=VECTOR('',#99558,1000.);
#12837=VECTOR('',#99561,1000.);
#12838=VECTOR('',#99562,1000.);
#12839=VECTOR('',#99563,1000.);
#12840=VECTOR('',#99564,1000.);
#12841=VECTOR('',#99567,1000.);
#12842=VECTOR('',#99568,1000.);
#12843=VECTOR('',#99569,1000.);
#12844=VECTOR('',#99572,1000.);
#12845=VECTOR('',#99573,1000.);
#12846=VECTOR('',#99574,1000.);
#12847=VECTOR('',#99577,1000.);
#12848=VECTOR('',#99578,1000.);
#12849=VECTOR('',#99581,1000.);
#12850=VECTOR('',#99582,1000.);
#12851=VECTOR('',#99583,1000.);
#12852=VECTOR('',#99584,1000.);
#12853=VECTOR('',#99587,1000.);
#12854=VECTOR('',#99588,1000.);
#12855=VECTOR('',#99589,1000.);
#12856=VECTOR('',#99592,1000.);
#12857=VECTOR('',#99593,1000.);
#12858=VECTOR('',#99594,1000.);
#12859=VECTOR('',#99597,1000.);
#12860=VECTOR('',#99598,1000.);
#12861=VECTOR('',#99601,1000.);
#12862=VECTOR('',#99602,1000.);
#12863=VECTOR('',#99603,1000.);
#12864=VECTOR('',#99604,1000.);
#12865=VECTOR('',#99607,1000.);
#12866=VECTOR('',#99608,1000.);
#12867=VECTOR('',#99609,1000.);
#12868=VECTOR('',#99612,1000.);
#12869=VECTOR('',#99613,1000.);
#12870=VECTOR('',#99614,1000.);
#12871=VECTOR('',#99617,1000.);
#12872=VECTOR('',#99618,1000.);
#12873=VECTOR('',#99621,1000.);
#12874=VECTOR('',#99622,1000.);
#12875=VECTOR('',#99623,1000.);
#12876=VECTOR('',#99624,1000.);
#12877=VECTOR('',#99627,1000.);
#12878=VECTOR('',#99628,1000.);
#12879=VECTOR('',#99629,1000.);
#12880=VECTOR('',#99632,1000.);
#12881=VECTOR('',#99633,1000.);
#12882=VECTOR('',#99634,1000.);
#12883=VECTOR('',#99637,1000.);
#12884=VECTOR('',#99638,1000.);
#12885=VECTOR('',#99641,1000.);
#12886=VECTOR('',#99642,1000.);
#12887=VECTOR('',#99643,1000.);
#12888=VECTOR('',#99644,1000.);
#12889=VECTOR('',#99647,1000.);
#12890=VECTOR('',#99648,1000.);
#12891=VECTOR('',#99649,1000.);
#12892=VECTOR('',#99652,1000.);
#12893=VECTOR('',#99653,1000.);
#12894=VECTOR('',#99654,1000.);
#12895=VECTOR('',#99657,1000.);
#12896=VECTOR('',#99658,1000.);
#12897=VECTOR('',#99661,1000.);
#12898=VECTOR('',#99662,1000.);
#12899=VECTOR('',#99663,1000.);
#12900=VECTOR('',#99664,1000.);
#12901=VECTOR('',#99667,1000.);
#12902=VECTOR('',#99668,1000.);
#12903=VECTOR('',#99669,1000.);
#12904=VECTOR('',#99672,1000.);
#12905=VECTOR('',#99673,1000.);
#12906=VECTOR('',#99674,1000.);
#12907=VECTOR('',#99677,1000.);
#12908=VECTOR('',#99678,1000.);
#12909=VECTOR('',#99681,1000.);
#12910=VECTOR('',#99682,1000.);
#12911=VECTOR('',#99683,1000.);
#12912=VECTOR('',#99684,1000.);
#12913=VECTOR('',#99687,1000.);
#12914=VECTOR('',#99688,1000.);
#12915=VECTOR('',#99689,1000.);
#12916=VECTOR('',#99692,1000.);
#12917=VECTOR('',#99693,1000.);
#12918=VECTOR('',#99694,1000.);
#12919=VECTOR('',#99697,1000.);
#12920=VECTOR('',#99698,1000.);
#12921=VECTOR('',#99701,1000.);
#12922=VECTOR('',#99702,1000.);
#12923=VECTOR('',#99703,1000.);
#12924=VECTOR('',#99704,1000.);
#12925=VECTOR('',#99707,1000.);
#12926=VECTOR('',#99708,1000.);
#12927=VECTOR('',#99709,1000.);
#12928=VECTOR('',#99712,1000.);
#12929=VECTOR('',#99713,1000.);
#12930=VECTOR('',#99714,1000.);
#12931=VECTOR('',#99717,1000.);
#12932=VECTOR('',#99718,1000.);
#12933=VECTOR('',#99721,1000.);
#12934=VECTOR('',#99722,1000.);
#12935=VECTOR('',#99723,1000.);
#12936=VECTOR('',#99724,1000.);
#12937=VECTOR('',#99727,1000.);
#12938=VECTOR('',#99728,1000.);
#12939=VECTOR('',#99729,1000.);
#12940=VECTOR('',#99732,1000.);
#12941=VECTOR('',#99733,1000.);
#12942=VECTOR('',#99734,1000.);
#12943=VECTOR('',#99737,1000.);
#12944=VECTOR('',#99738,1000.);
#12945=VECTOR('',#99741,1000.);
#12946=VECTOR('',#99742,1000.);
#12947=VECTOR('',#99743,1000.);
#12948=VECTOR('',#99744,1000.);
#12949=VECTOR('',#99747,1000.);
#12950=VECTOR('',#99748,1000.);
#12951=VECTOR('',#99749,1000.);
#12952=VECTOR('',#99752,1000.);
#12953=VECTOR('',#99753,1000.);
#12954=VECTOR('',#99754,1000.);
#12955=VECTOR('',#99757,1000.);
#12956=VECTOR('',#99758,1000.);
#12957=VECTOR('',#99761,1000.);
#12958=VECTOR('',#99762,1000.);
#12959=VECTOR('',#99763,1000.);
#12960=VECTOR('',#99764,1000.);
#12961=VECTOR('',#99767,1000.);
#12962=VECTOR('',#99768,1000.);
#12963=VECTOR('',#99769,1000.);
#12964=VECTOR('',#99772,1000.);
#12965=VECTOR('',#99773,1000.);
#12966=VECTOR('',#99774,1000.);
#12967=VECTOR('',#99777,1000.);
#12968=VECTOR('',#99778,1000.);
#12969=VECTOR('',#99781,1000.);
#12970=VECTOR('',#99782,1000.);
#12971=VECTOR('',#99783,1000.);
#12972=VECTOR('',#99784,1000.);
#12973=VECTOR('',#99787,1000.);
#12974=VECTOR('',#99788,1000.);
#12975=VECTOR('',#99789,1000.);
#12976=VECTOR('',#99792,1000.);
#12977=VECTOR('',#99793,1000.);
#12978=VECTOR('',#99794,1000.);
#12979=VECTOR('',#99797,1000.);
#12980=VECTOR('',#99798,1000.);
#12981=VECTOR('',#99801,1000.);
#12982=VECTOR('',#99802,1000.);
#12983=VECTOR('',#99803,1000.);
#12984=VECTOR('',#99804,1000.);
#12985=VECTOR('',#99807,1000.);
#12986=VECTOR('',#99808,1000.);
#12987=VECTOR('',#99809,1000.);
#12988=VECTOR('',#99812,1000.);
#12989=VECTOR('',#99813,1000.);
#12990=VECTOR('',#99814,1000.);
#12991=VECTOR('',#99817,1000.);
#12992=VECTOR('',#99818,1000.);
#12993=VECTOR('',#99821,1000.);
#12994=VECTOR('',#99822,1000.);
#12995=VECTOR('',#99823,1000.);
#12996=VECTOR('',#99824,1000.);
#12997=VECTOR('',#99827,1000.);
#12998=VECTOR('',#99828,1000.);
#12999=VECTOR('',#99829,1000.);
#13000=VECTOR('',#99832,1000.);
#13001=VECTOR('',#99833,1000.);
#13002=VECTOR('',#99834,1000.);
#13003=VECTOR('',#99837,1000.);
#13004=VECTOR('',#99838,1000.);
#13005=VECTOR('',#99841,1000.);
#13006=VECTOR('',#99842,1000.);
#13007=VECTOR('',#99843,1000.);
#13008=VECTOR('',#99844,1000.);
#13009=VECTOR('',#99847,1000.);
#13010=VECTOR('',#99848,1000.);
#13011=VECTOR('',#99849,1000.);
#13012=VECTOR('',#99852,1000.);
#13013=VECTOR('',#99853,1000.);
#13014=VECTOR('',#99854,1000.);
#13015=VECTOR('',#99857,1000.);
#13016=VECTOR('',#99858,1000.);
#13017=VECTOR('',#99861,1000.);
#13018=VECTOR('',#99862,1000.);
#13019=VECTOR('',#99863,1000.);
#13020=VECTOR('',#99864,1000.);
#13021=VECTOR('',#99867,1000.);
#13022=VECTOR('',#99868,1000.);
#13023=VECTOR('',#99869,1000.);
#13024=VECTOR('',#99872,1000.);
#13025=VECTOR('',#99873,1000.);
#13026=VECTOR('',#99874,1000.);
#13027=VECTOR('',#99877,1000.);
#13028=VECTOR('',#99878,1000.);
#13029=VECTOR('',#99881,1000.);
#13030=VECTOR('',#99882,1000.);
#13031=VECTOR('',#99883,1000.);
#13032=VECTOR('',#99884,1000.);
#13033=VECTOR('',#99887,1000.);
#13034=VECTOR('',#99888,1000.);
#13035=VECTOR('',#99889,1000.);
#13036=VECTOR('',#99892,1000.);
#13037=VECTOR('',#99893,1000.);
#13038=VECTOR('',#99894,1000.);
#13039=VECTOR('',#99897,1000.);
#13040=VECTOR('',#99898,1000.);
#13041=VECTOR('',#99901,1000.);
#13042=VECTOR('',#99902,1000.);
#13043=VECTOR('',#99903,1000.);
#13044=VECTOR('',#99904,1000.);
#13045=VECTOR('',#99907,1000.);
#13046=VECTOR('',#99908,1000.);
#13047=VECTOR('',#99909,1000.);
#13048=VECTOR('',#99912,1000.);
#13049=VECTOR('',#99913,1000.);
#13050=VECTOR('',#99914,1000.);
#13051=VECTOR('',#99917,1000.);
#13052=VECTOR('',#99918,1000.);
#13053=VECTOR('',#99921,1000.);
#13054=VECTOR('',#99922,1000.);
#13055=VECTOR('',#99923,1000.);
#13056=VECTOR('',#99924,1000.);
#13057=VECTOR('',#99927,1000.);
#13058=VECTOR('',#99928,1000.);
#13059=VECTOR('',#99929,1000.);
#13060=VECTOR('',#99932,1000.);
#13061=VECTOR('',#99933,1000.);
#13062=VECTOR('',#99934,1000.);
#13063=VECTOR('',#99937,1000.);
#13064=VECTOR('',#99938,1000.);
#13065=VECTOR('',#99941,1000.);
#13066=VECTOR('',#99942,1000.);
#13067=VECTOR('',#99943,1000.);
#13068=VECTOR('',#99944,1000.);
#13069=VECTOR('',#99947,1000.);
#13070=VECTOR('',#99948,1000.);
#13071=VECTOR('',#99949,1000.);
#13072=VECTOR('',#99952,1000.);
#13073=VECTOR('',#99953,1000.);
#13074=VECTOR('',#99954,1000.);
#13075=VECTOR('',#99957,1000.);
#13076=VECTOR('',#99958,1000.);
#13077=VECTOR('',#99961,1000.);
#13078=VECTOR('',#99962,1000.);
#13079=VECTOR('',#99963,1000.);
#13080=VECTOR('',#99964,1000.);
#13081=VECTOR('',#99967,1000.);
#13082=VECTOR('',#99968,1000.);
#13083=VECTOR('',#99969,1000.);
#13084=VECTOR('',#99972,1000.);
#13085=VECTOR('',#99973,1000.);
#13086=VECTOR('',#99974,1000.);
#13087=VECTOR('',#99977,1000.);
#13088=VECTOR('',#99978,1000.);
#13089=VECTOR('',#99981,1000.);
#13090=VECTOR('',#99982,1000.);
#13091=VECTOR('',#99983,1000.);
#13092=VECTOR('',#99984,1000.);
#13093=VECTOR('',#99987,1000.);
#13094=VECTOR('',#99988,1000.);
#13095=VECTOR('',#99989,1000.);
#13096=VECTOR('',#99992,1000.);
#13097=VECTOR('',#99993,1000.);
#13098=VECTOR('',#99994,1000.);
#13099=VECTOR('',#99997,1000.);
#13100=VECTOR('',#99998,1000.);
#13101=VECTOR('',#100001,1000.);
#13102=VECTOR('',#100002,1000.);
#13103=VECTOR('',#100003,1000.);
#13104=VECTOR('',#100004,1000.);
#13105=VECTOR('',#100007,1000.);
#13106=VECTOR('',#100008,1000.);
#13107=VECTOR('',#100009,1000.);
#13108=VECTOR('',#100012,1000.);
#13109=VECTOR('',#100013,1000.);
#13110=VECTOR('',#100014,1000.);
#13111=VECTOR('',#100017,1000.);
#13112=VECTOR('',#100018,1000.);
#13113=VECTOR('',#100021,1000.);
#13114=VECTOR('',#100022,1000.);
#13115=VECTOR('',#100023,1000.);
#13116=VECTOR('',#100024,1000.);
#13117=VECTOR('',#100027,1000.);
#13118=VECTOR('',#100028,1000.);
#13119=VECTOR('',#100029,1000.);
#13120=VECTOR('',#100032,1000.);
#13121=VECTOR('',#100033,1000.);
#13122=VECTOR('',#100034,1000.);
#13123=VECTOR('',#100037,1000.);
#13124=VECTOR('',#100038,1000.);
#13125=VECTOR('',#100041,1000.);
#13126=VECTOR('',#100042,1000.);
#13127=VECTOR('',#100043,1000.);
#13128=VECTOR('',#100044,1000.);
#13129=VECTOR('',#100047,1000.);
#13130=VECTOR('',#100048,1000.);
#13131=VECTOR('',#100049,1000.);
#13132=VECTOR('',#100052,1000.);
#13133=VECTOR('',#100053,1000.);
#13134=VECTOR('',#100054,1000.);
#13135=VECTOR('',#100057,1000.);
#13136=VECTOR('',#100058,1000.);
#13137=VECTOR('',#100061,1000.);
#13138=VECTOR('',#100062,1000.);
#13139=VECTOR('',#100063,1000.);
#13140=VECTOR('',#100064,1000.);
#13141=VECTOR('',#100067,1000.);
#13142=VECTOR('',#100068,1000.);
#13143=VECTOR('',#100069,1000.);
#13144=VECTOR('',#100072,1000.);
#13145=VECTOR('',#100073,1000.);
#13146=VECTOR('',#100074,1000.);
#13147=VECTOR('',#100077,1000.);
#13148=VECTOR('',#100078,1000.);
#13149=VECTOR('',#100081,1000.);
#13150=VECTOR('',#100082,1000.);
#13151=VECTOR('',#100083,1000.);
#13152=VECTOR('',#100084,1000.);
#13153=VECTOR('',#100087,1000.);
#13154=VECTOR('',#100088,1000.);
#13155=VECTOR('',#100089,1000.);
#13156=VECTOR('',#100092,1000.);
#13157=VECTOR('',#100093,1000.);
#13158=VECTOR('',#100094,1000.);
#13159=VECTOR('',#100097,1000.);
#13160=VECTOR('',#100098,1000.);
#13161=VECTOR('',#100101,1000.);
#13162=VECTOR('',#100102,1000.);
#13163=VECTOR('',#100103,1000.);
#13164=VECTOR('',#100104,1000.);
#13165=VECTOR('',#100107,1000.);
#13166=VECTOR('',#100108,1000.);
#13167=VECTOR('',#100109,1000.);
#13168=VECTOR('',#100112,1000.);
#13169=VECTOR('',#100113,1000.);
#13170=VECTOR('',#100114,1000.);
#13171=VECTOR('',#100117,1000.);
#13172=VECTOR('',#100118,1000.);
#13173=VECTOR('',#100121,1000.);
#13174=VECTOR('',#100122,1000.);
#13175=VECTOR('',#100123,1000.);
#13176=VECTOR('',#100124,1000.);
#13177=VECTOR('',#100127,1000.);
#13178=VECTOR('',#100128,1000.);
#13179=VECTOR('',#100129,1000.);
#13180=VECTOR('',#100132,1000.);
#13181=VECTOR('',#100133,1000.);
#13182=VECTOR('',#100134,1000.);
#13183=VECTOR('',#100137,1000.);
#13184=VECTOR('',#100138,1000.);
#13185=VECTOR('',#100141,1000.);
#13186=VECTOR('',#100142,1000.);
#13187=VECTOR('',#100143,1000.);
#13188=VECTOR('',#100144,1000.);
#13189=VECTOR('',#100147,1000.);
#13190=VECTOR('',#100148,1000.);
#13191=VECTOR('',#100149,1000.);
#13192=VECTOR('',#100152,1000.);
#13193=VECTOR('',#100153,1000.);
#13194=VECTOR('',#100154,1000.);
#13195=VECTOR('',#100157,1000.);
#13196=VECTOR('',#100158,1000.);
#13197=VECTOR('',#100161,1000.);
#13198=VECTOR('',#100162,1000.);
#13199=VECTOR('',#100163,1000.);
#13200=VECTOR('',#100164,1000.);
#13201=VECTOR('',#100167,1000.);
#13202=VECTOR('',#100168,1000.);
#13203=VECTOR('',#100169,1000.);
#13204=VECTOR('',#100172,1000.);
#13205=VECTOR('',#100173,1000.);
#13206=VECTOR('',#100174,1000.);
#13207=VECTOR('',#100177,1000.);
#13208=VECTOR('',#100178,1000.);
#13209=VECTOR('',#100181,1000.);
#13210=VECTOR('',#100182,1000.);
#13211=VECTOR('',#100183,1000.);
#13212=VECTOR('',#100184,1000.);
#13213=VECTOR('',#100187,1000.);
#13214=VECTOR('',#100188,1000.);
#13215=VECTOR('',#100189,1000.);
#13216=VECTOR('',#100192,1000.);
#13217=VECTOR('',#100193,1000.);
#13218=VECTOR('',#100194,1000.);
#13219=VECTOR('',#100197,1000.);
#13220=VECTOR('',#100198,1000.);
#13221=VECTOR('',#100201,1000.);
#13222=VECTOR('',#100202,1000.);
#13223=VECTOR('',#100203,1000.);
#13224=VECTOR('',#100204,1000.);
#13225=VECTOR('',#100207,1000.);
#13226=VECTOR('',#100208,1000.);
#13227=VECTOR('',#100209,1000.);
#13228=VECTOR('',#100212,1000.);
#13229=VECTOR('',#100213,1000.);
#13230=VECTOR('',#100214,1000.);
#13231=VECTOR('',#100217,1000.);
#13232=VECTOR('',#100218,1000.);
#13233=VECTOR('',#100221,1000.);
#13234=VECTOR('',#100222,1000.);
#13235=VECTOR('',#100223,1000.);
#13236=VECTOR('',#100224,1000.);
#13237=VECTOR('',#100227,1000.);
#13238=VECTOR('',#100228,1000.);
#13239=VECTOR('',#100229,1000.);
#13240=VECTOR('',#100232,1000.);
#13241=VECTOR('',#100233,1000.);
#13242=VECTOR('',#100234,1000.);
#13243=VECTOR('',#100237,1000.);
#13244=VECTOR('',#100238,1000.);
#13245=VECTOR('',#100241,1000.);
#13246=VECTOR('',#100242,1000.);
#13247=VECTOR('',#100243,1000.);
#13248=VECTOR('',#100244,1000.);
#13249=VECTOR('',#100247,1000.);
#13250=VECTOR('',#100248,1000.);
#13251=VECTOR('',#100249,1000.);
#13252=VECTOR('',#100252,1000.);
#13253=VECTOR('',#100253,1000.);
#13254=VECTOR('',#100254,1000.);
#13255=VECTOR('',#100257,1000.);
#13256=VECTOR('',#100258,1000.);
#13257=VECTOR('',#100261,1000.);
#13258=VECTOR('',#100262,1000.);
#13259=VECTOR('',#100263,1000.);
#13260=VECTOR('',#100264,1000.);
#13261=VECTOR('',#100267,1000.);
#13262=VECTOR('',#100268,1000.);
#13263=VECTOR('',#100269,1000.);
#13264=VECTOR('',#100272,1000.);
#13265=VECTOR('',#100273,1000.);
#13266=VECTOR('',#100274,1000.);
#13267=VECTOR('',#100277,1000.);
#13268=VECTOR('',#100278,1000.);
#13269=VECTOR('',#100281,1000.);
#13270=VECTOR('',#100282,1000.);
#13271=VECTOR('',#100283,1000.);
#13272=VECTOR('',#100284,1000.);
#13273=VECTOR('',#100287,1000.);
#13274=VECTOR('',#100288,1000.);
#13275=VECTOR('',#100289,1000.);
#13276=VECTOR('',#100292,1000.);
#13277=VECTOR('',#100293,1000.);
#13278=VECTOR('',#100294,1000.);
#13279=VECTOR('',#100297,1000.);
#13280=VECTOR('',#100298,1000.);
#13281=VECTOR('',#100301,1000.);
#13282=VECTOR('',#100302,1000.);
#13283=VECTOR('',#100303,1000.);
#13284=VECTOR('',#100304,1000.);
#13285=VECTOR('',#100307,1000.);
#13286=VECTOR('',#100308,1000.);
#13287=VECTOR('',#100309,1000.);
#13288=VECTOR('',#100312,1000.);
#13289=VECTOR('',#100313,1000.);
#13290=VECTOR('',#100314,1000.);
#13291=VECTOR('',#100317,1000.);
#13292=VECTOR('',#100318,1000.);
#13293=VECTOR('',#100321,1000.);
#13294=VECTOR('',#100322,1000.);
#13295=VECTOR('',#100323,1000.);
#13296=VECTOR('',#100324,1000.);
#13297=VECTOR('',#100327,1000.);
#13298=VECTOR('',#100328,1000.);
#13299=VECTOR('',#100329,1000.);
#13300=VECTOR('',#100332,1000.);
#13301=VECTOR('',#100333,1000.);
#13302=VECTOR('',#100334,1000.);
#13303=VECTOR('',#100337,1000.);
#13304=VECTOR('',#100338,1000.);
#13305=VECTOR('',#100341,1000.);
#13306=VECTOR('',#100342,1000.);
#13307=VECTOR('',#100343,1000.);
#13308=VECTOR('',#100344,1000.);
#13309=VECTOR('',#100347,1000.);
#13310=VECTOR('',#100348,1000.);
#13311=VECTOR('',#100349,1000.);
#13312=VECTOR('',#100352,1000.);
#13313=VECTOR('',#100353,1000.);
#13314=VECTOR('',#100354,1000.);
#13315=VECTOR('',#100357,1000.);
#13316=VECTOR('',#100358,1000.);
#13317=VECTOR('',#100361,1000.);
#13318=VECTOR('',#100362,1000.);
#13319=VECTOR('',#100363,1000.);
#13320=VECTOR('',#100364,1000.);
#13321=VECTOR('',#100367,1000.);
#13322=VECTOR('',#100368,1000.);
#13323=VECTOR('',#100369,1000.);
#13324=VECTOR('',#100372,1000.);
#13325=VECTOR('',#100373,1000.);
#13326=VECTOR('',#100374,1000.);
#13327=VECTOR('',#100377,1000.);
#13328=VECTOR('',#100378,1000.);
#13329=VECTOR('',#100381,1000.);
#13330=VECTOR('',#100382,1000.);
#13331=VECTOR('',#100383,1000.);
#13332=VECTOR('',#100384,1000.);
#13333=VECTOR('',#100387,1000.);
#13334=VECTOR('',#100388,1000.);
#13335=VECTOR('',#100389,1000.);
#13336=VECTOR('',#100392,1000.);
#13337=VECTOR('',#100393,1000.);
#13338=VECTOR('',#100394,1000.);
#13339=VECTOR('',#100397,1000.);
#13340=VECTOR('',#100398,1000.);
#13341=VECTOR('',#100401,1000.);
#13342=VECTOR('',#100402,1000.);
#13343=VECTOR('',#100403,1000.);
#13344=VECTOR('',#100404,1000.);
#13345=VECTOR('',#100407,1000.);
#13346=VECTOR('',#100408,1000.);
#13347=VECTOR('',#100409,1000.);
#13348=VECTOR('',#100412,1000.);
#13349=VECTOR('',#100413,1000.);
#13350=VECTOR('',#100414,1000.);
#13351=VECTOR('',#100417,1000.);
#13352=VECTOR('',#100418,1000.);
#13353=VECTOR('',#100421,1000.);
#13354=VECTOR('',#100422,1000.);
#13355=VECTOR('',#100423,1000.);
#13356=VECTOR('',#100424,1000.);
#13357=VECTOR('',#100427,1000.);
#13358=VECTOR('',#100428,1000.);
#13359=VECTOR('',#100429,1000.);
#13360=VECTOR('',#100432,1000.);
#13361=VECTOR('',#100433,1000.);
#13362=VECTOR('',#100434,1000.);
#13363=VECTOR('',#100437,1000.);
#13364=VECTOR('',#100438,1000.);
#13365=VECTOR('',#100441,1000.);
#13366=VECTOR('',#100442,1000.);
#13367=VECTOR('',#100443,1000.);
#13368=VECTOR('',#100444,1000.);
#13369=VECTOR('',#100447,1000.);
#13370=VECTOR('',#100448,1000.);
#13371=VECTOR('',#100449,1000.);
#13372=VECTOR('',#100452,1000.);
#13373=VECTOR('',#100453,1000.);
#13374=VECTOR('',#100454,1000.);
#13375=VECTOR('',#100457,1000.);
#13376=VECTOR('',#100458,1000.);
#13377=VECTOR('',#100461,1000.);
#13378=VECTOR('',#100462,1000.);
#13379=VECTOR('',#100463,1000.);
#13380=VECTOR('',#100464,1000.);
#13381=VECTOR('',#100467,1000.);
#13382=VECTOR('',#100468,1000.);
#13383=VECTOR('',#100469,1000.);
#13384=VECTOR('',#100472,1000.);
#13385=VECTOR('',#100473,1000.);
#13386=VECTOR('',#100474,1000.);
#13387=VECTOR('',#100477,1000.);
#13388=VECTOR('',#100478,1000.);
#13389=VECTOR('',#100481,1000.);
#13390=VECTOR('',#100482,1000.);
#13391=VECTOR('',#100483,1000.);
#13392=VECTOR('',#100484,1000.);
#13393=VECTOR('',#100487,1000.);
#13394=VECTOR('',#100488,1000.);
#13395=VECTOR('',#100489,1000.);
#13396=VECTOR('',#100492,1000.);
#13397=VECTOR('',#100493,1000.);
#13398=VECTOR('',#100494,1000.);
#13399=VECTOR('',#100497,1000.);
#13400=VECTOR('',#100498,1000.);
#13401=VECTOR('',#100501,1000.);
#13402=VECTOR('',#100502,1000.);
#13403=VECTOR('',#100503,1000.);
#13404=VECTOR('',#100504,1000.);
#13405=VECTOR('',#100507,1000.);
#13406=VECTOR('',#100508,1000.);
#13407=VECTOR('',#100509,1000.);
#13408=VECTOR('',#100512,1000.);
#13409=VECTOR('',#100513,1000.);
#13410=VECTOR('',#100514,1000.);
#13411=VECTOR('',#100517,1000.);
#13412=VECTOR('',#100518,1000.);
#13413=VECTOR('',#100521,1000.);
#13414=VECTOR('',#100522,1000.);
#13415=VECTOR('',#100523,1000.);
#13416=VECTOR('',#100524,1000.);
#13417=VECTOR('',#100527,1000.);
#13418=VECTOR('',#100528,1000.);
#13419=VECTOR('',#100529,1000.);
#13420=VECTOR('',#100532,1000.);
#13421=VECTOR('',#100533,1000.);
#13422=VECTOR('',#100534,1000.);
#13423=VECTOR('',#100537,1000.);
#13424=VECTOR('',#100538,1000.);
#13425=VECTOR('',#100541,1000.);
#13426=VECTOR('',#100542,1000.);
#13427=VECTOR('',#100543,1000.);
#13428=VECTOR('',#100544,1000.);
#13429=VECTOR('',#100547,1000.);
#13430=VECTOR('',#100548,1000.);
#13431=VECTOR('',#100549,1000.);
#13432=VECTOR('',#100552,1000.);
#13433=VECTOR('',#100553,1000.);
#13434=VECTOR('',#100554,1000.);
#13435=VECTOR('',#100557,1000.);
#13436=VECTOR('',#100558,1000.);
#13437=VECTOR('',#100561,1000.);
#13438=VECTOR('',#100562,1000.);
#13439=VECTOR('',#100563,1000.);
#13440=VECTOR('',#100564,1000.);
#13441=VECTOR('',#100567,1000.);
#13442=VECTOR('',#100568,1000.);
#13443=VECTOR('',#100569,1000.);
#13444=VECTOR('',#100572,1000.);
#13445=VECTOR('',#100573,1000.);
#13446=VECTOR('',#100574,1000.);
#13447=VECTOR('',#100577,1000.);
#13448=VECTOR('',#100578,1000.);
#13449=VECTOR('',#100581,1000.);
#13450=VECTOR('',#100582,1000.);
#13451=VECTOR('',#100583,1000.);
#13452=VECTOR('',#100584,1000.);
#13453=VECTOR('',#100587,1000.);
#13454=VECTOR('',#100588,1000.);
#13455=VECTOR('',#100589,1000.);
#13456=VECTOR('',#100592,1000.);
#13457=VECTOR('',#100593,1000.);
#13458=VECTOR('',#100594,1000.);
#13459=VECTOR('',#100597,1000.);
#13460=VECTOR('',#100598,1000.);
#13461=VECTOR('',#100601,1000.);
#13462=VECTOR('',#100602,1000.);
#13463=VECTOR('',#100603,1000.);
#13464=VECTOR('',#100604,1000.);
#13465=VECTOR('',#100607,1000.);
#13466=VECTOR('',#100608,1000.);
#13467=VECTOR('',#100609,1000.);
#13468=VECTOR('',#100612,1000.);
#13469=VECTOR('',#100613,1000.);
#13470=VECTOR('',#100614,1000.);
#13471=VECTOR('',#100617,1000.);
#13472=VECTOR('',#100618,1000.);
#13473=VECTOR('',#100621,1000.);
#13474=VECTOR('',#100622,1000.);
#13475=VECTOR('',#100623,1000.);
#13476=VECTOR('',#100624,1000.);
#13477=VECTOR('',#100627,1000.);
#13478=VECTOR('',#100628,1000.);
#13479=VECTOR('',#100629,1000.);
#13480=VECTOR('',#100632,1000.);
#13481=VECTOR('',#100633,1000.);
#13482=VECTOR('',#100634,1000.);
#13483=VECTOR('',#100637,1000.);
#13484=VECTOR('',#100638,1000.);
#13485=VECTOR('',#100641,1000.);
#13486=VECTOR('',#100642,1000.);
#13487=VECTOR('',#100643,1000.);
#13488=VECTOR('',#100644,1000.);
#13489=VECTOR('',#100647,1000.);
#13490=VECTOR('',#100648,1000.);
#13491=VECTOR('',#100649,1000.);
#13492=VECTOR('',#100652,1000.);
#13493=VECTOR('',#100653,1000.);
#13494=VECTOR('',#100654,1000.);
#13495=VECTOR('',#100657,1000.);
#13496=VECTOR('',#100658,1000.);
#13497=VECTOR('',#100661,1000.);
#13498=VECTOR('',#100662,1000.);
#13499=VECTOR('',#100663,1000.);
#13500=VECTOR('',#100664,1000.);
#13501=VECTOR('',#100667,1000.);
#13502=VECTOR('',#100668,1000.);
#13503=VECTOR('',#100669,1000.);
#13504=VECTOR('',#100672,1000.);
#13505=VECTOR('',#100673,1000.);
#13506=VECTOR('',#100674,1000.);
#13507=VECTOR('',#100677,1000.);
#13508=VECTOR('',#100678,1000.);
#13509=VECTOR('',#100681,1000.);
#13510=VECTOR('',#100682,1000.);
#13511=VECTOR('',#100683,1000.);
#13512=VECTOR('',#100684,1000.);
#13513=VECTOR('',#100687,1000.);
#13514=VECTOR('',#100688,1000.);
#13515=VECTOR('',#100689,1000.);
#13516=VECTOR('',#100692,1000.);
#13517=VECTOR('',#100693,1000.);
#13518=VECTOR('',#100694,1000.);
#13519=VECTOR('',#100697,1000.);
#13520=VECTOR('',#100698,1000.);
#13521=VECTOR('',#100701,1000.);
#13522=VECTOR('',#100702,1000.);
#13523=VECTOR('',#100703,1000.);
#13524=VECTOR('',#100704,1000.);
#13525=VECTOR('',#100707,1000.);
#13526=VECTOR('',#100708,1000.);
#13527=VECTOR('',#100709,1000.);
#13528=VECTOR('',#100712,1000.);
#13529=VECTOR('',#100713,1000.);
#13530=VECTOR('',#100714,1000.);
#13531=VECTOR('',#100717,1000.);
#13532=VECTOR('',#100718,1000.);
#13533=VECTOR('',#100721,1000.);
#13534=VECTOR('',#100722,1000.);
#13535=VECTOR('',#100723,1000.);
#13536=VECTOR('',#100724,1000.);
#13537=VECTOR('',#100727,1000.);
#13538=VECTOR('',#100728,1000.);
#13539=VECTOR('',#100729,1000.);
#13540=VECTOR('',#100732,1000.);
#13541=VECTOR('',#100733,1000.);
#13542=VECTOR('',#100734,1000.);
#13543=VECTOR('',#100737,1000.);
#13544=VECTOR('',#100738,1000.);
#13545=VECTOR('',#100741,1000.);
#13546=VECTOR('',#100742,1000.);
#13547=VECTOR('',#100743,1000.);
#13548=VECTOR('',#100744,1000.);
#13549=VECTOR('',#100747,1000.);
#13550=VECTOR('',#100748,1000.);
#13551=VECTOR('',#100749,1000.);
#13552=VECTOR('',#100752,1000.);
#13553=VECTOR('',#100753,1000.);
#13554=VECTOR('',#100754,1000.);
#13555=VECTOR('',#100757,1000.);
#13556=VECTOR('',#100758,1000.);
#13557=VECTOR('',#100761,1000.);
#13558=VECTOR('',#100762,1000.);
#13559=VECTOR('',#100763,1000.);
#13560=VECTOR('',#100764,1000.);
#13561=VECTOR('',#100767,1000.);
#13562=VECTOR('',#100768,1000.);
#13563=VECTOR('',#100769,1000.);
#13564=VECTOR('',#100772,1000.);
#13565=VECTOR('',#100773,1000.);
#13566=VECTOR('',#100774,1000.);
#13567=VECTOR('',#100777,1000.);
#13568=VECTOR('',#100778,1000.);
#13569=VECTOR('',#100781,1000.);
#13570=VECTOR('',#100782,1000.);
#13571=VECTOR('',#100783,1000.);
#13572=VECTOR('',#100784,1000.);
#13573=VECTOR('',#100787,1000.);
#13574=VECTOR('',#100788,1000.);
#13575=VECTOR('',#100789,1000.);
#13576=VECTOR('',#100792,1000.);
#13577=VECTOR('',#100793,1000.);
#13578=VECTOR('',#100794,1000.);
#13579=VECTOR('',#100797,1000.);
#13580=VECTOR('',#100798,1000.);
#13581=VECTOR('',#100801,1000.);
#13582=VECTOR('',#100802,1000.);
#13583=VECTOR('',#100803,1000.);
#13584=VECTOR('',#100804,1000.);
#13585=VECTOR('',#100807,1000.);
#13586=VECTOR('',#100808,1000.);
#13587=VECTOR('',#100809,1000.);
#13588=VECTOR('',#100812,1000.);
#13589=VECTOR('',#100813,1000.);
#13590=VECTOR('',#100814,1000.);
#13591=VECTOR('',#100817,1000.);
#13592=VECTOR('',#100818,1000.);
#13593=VECTOR('',#100821,1000.);
#13594=VECTOR('',#100822,1000.);
#13595=VECTOR('',#100823,1000.);
#13596=VECTOR('',#100824,1000.);
#13597=VECTOR('',#100827,1000.);
#13598=VECTOR('',#100828,1000.);
#13599=VECTOR('',#100829,1000.);
#13600=VECTOR('',#100832,1000.);
#13601=VECTOR('',#100833,1000.);
#13602=VECTOR('',#100834,1000.);
#13603=VECTOR('',#100837,1000.);
#13604=VECTOR('',#100838,1000.);
#13605=VECTOR('',#100841,1000.);
#13606=VECTOR('',#100842,1000.);
#13607=VECTOR('',#100843,1000.);
#13608=VECTOR('',#100844,1000.);
#13609=VECTOR('',#100847,1000.);
#13610=VECTOR('',#100848,1000.);
#13611=VECTOR('',#100849,1000.);
#13612=VECTOR('',#100852,1000.);
#13613=VECTOR('',#100853,1000.);
#13614=VECTOR('',#100854,1000.);
#13615=VECTOR('',#100857,1000.);
#13616=VECTOR('',#100858,1000.);
#13617=VECTOR('',#100861,1000.);
#13618=VECTOR('',#100862,1000.);
#13619=VECTOR('',#100863,1000.);
#13620=VECTOR('',#100864,1000.);
#13621=VECTOR('',#100867,1000.);
#13622=VECTOR('',#100868,1000.);
#13623=VECTOR('',#100869,1000.);
#13624=VECTOR('',#100872,1000.);
#13625=VECTOR('',#100873,1000.);
#13626=VECTOR('',#100874,1000.);
#13627=VECTOR('',#100877,1000.);
#13628=VECTOR('',#100878,1000.);
#13629=VECTOR('',#100881,1000.);
#13630=VECTOR('',#100882,1000.);
#13631=VECTOR('',#100883,1000.);
#13632=VECTOR('',#100884,1000.);
#13633=VECTOR('',#100887,1000.);
#13634=VECTOR('',#100888,1000.);
#13635=VECTOR('',#100889,1000.);
#13636=VECTOR('',#100892,1000.);
#13637=VECTOR('',#100893,1000.);
#13638=VECTOR('',#100894,1000.);
#13639=VECTOR('',#100897,1000.);
#13640=VECTOR('',#100898,1000.);
#13641=VECTOR('',#100901,1000.);
#13642=VECTOR('',#100902,1000.);
#13643=VECTOR('',#100903,1000.);
#13644=VECTOR('',#100904,1000.);
#13645=VECTOR('',#100907,1000.);
#13646=VECTOR('',#100908,1000.);
#13647=VECTOR('',#100909,1000.);
#13648=VECTOR('',#100912,1000.);
#13649=VECTOR('',#100913,1000.);
#13650=VECTOR('',#100914,1000.);
#13651=VECTOR('',#100917,1000.);
#13652=VECTOR('',#100918,1000.);
#13653=VECTOR('',#100921,1000.);
#13654=VECTOR('',#100922,1000.);
#13655=VECTOR('',#100923,1000.);
#13656=VECTOR('',#100924,1000.);
#13657=VECTOR('',#100927,1000.);
#13658=VECTOR('',#100928,1000.);
#13659=VECTOR('',#100929,1000.);
#13660=VECTOR('',#100932,1000.);
#13661=VECTOR('',#100933,1000.);
#13662=VECTOR('',#100934,1000.);
#13663=VECTOR('',#100937,1000.);
#13664=VECTOR('',#100938,1000.);
#13665=VECTOR('',#100941,1000.);
#13666=VECTOR('',#100942,1000.);
#13667=VECTOR('',#100943,1000.);
#13668=VECTOR('',#100944,1000.);
#13669=VECTOR('',#100947,1000.);
#13670=VECTOR('',#100948,1000.);
#13671=VECTOR('',#100949,1000.);
#13672=VECTOR('',#100952,1000.);
#13673=VECTOR('',#100953,1000.);
#13674=VECTOR('',#100954,1000.);
#13675=VECTOR('',#100957,1000.);
#13676=VECTOR('',#100958,1000.);
#13677=VECTOR('',#100961,1000.);
#13678=VECTOR('',#100962,1000.);
#13679=VECTOR('',#100963,1000.);
#13680=VECTOR('',#100964,1000.);
#13681=VECTOR('',#100967,1000.);
#13682=VECTOR('',#100968,1000.);
#13683=VECTOR('',#100969,1000.);
#13684=VECTOR('',#100972,1000.);
#13685=VECTOR('',#100973,1000.);
#13686=VECTOR('',#100974,1000.);
#13687=VECTOR('',#100977,1000.);
#13688=VECTOR('',#100978,1000.);
#13689=VECTOR('',#100981,1000.);
#13690=VECTOR('',#100982,1000.);
#13691=VECTOR('',#100983,1000.);
#13692=VECTOR('',#100984,1000.);
#13693=VECTOR('',#100987,1000.);
#13694=VECTOR('',#100988,1000.);
#13695=VECTOR('',#100989,1000.);
#13696=VECTOR('',#100992,1000.);
#13697=VECTOR('',#100993,1000.);
#13698=VECTOR('',#100994,1000.);
#13699=VECTOR('',#100997,1000.);
#13700=VECTOR('',#100998,1000.);
#13701=VECTOR('',#101001,1000.);
#13702=VECTOR('',#101002,1000.);
#13703=VECTOR('',#101003,1000.);
#13704=VECTOR('',#101004,1000.);
#13705=VECTOR('',#101007,1000.);
#13706=VECTOR('',#101008,1000.);
#13707=VECTOR('',#101009,1000.);
#13708=VECTOR('',#101012,1000.);
#13709=VECTOR('',#101013,1000.);
#13710=VECTOR('',#101014,1000.);
#13711=VECTOR('',#101017,1000.);
#13712=VECTOR('',#101018,1000.);
#13713=VECTOR('',#101021,1000.);
#13714=VECTOR('',#101022,1000.);
#13715=VECTOR('',#101023,1000.);
#13716=VECTOR('',#101024,1000.);
#13717=VECTOR('',#101027,1000.);
#13718=VECTOR('',#101028,1000.);
#13719=VECTOR('',#101029,1000.);
#13720=VECTOR('',#101032,1000.);
#13721=VECTOR('',#101033,1000.);
#13722=VECTOR('',#101034,1000.);
#13723=VECTOR('',#101037,1000.);
#13724=VECTOR('',#101038,1000.);
#13725=VECTOR('',#101041,1000.);
#13726=VECTOR('',#101042,1000.);
#13727=VECTOR('',#101043,1000.);
#13728=VECTOR('',#101044,1000.);
#13729=VECTOR('',#101047,1000.);
#13730=VECTOR('',#101048,1000.);
#13731=VECTOR('',#101049,1000.);
#13732=VECTOR('',#101052,1000.);
#13733=VECTOR('',#101053,1000.);
#13734=VECTOR('',#101054,1000.);
#13735=VECTOR('',#101057,1000.);
#13736=VECTOR('',#101058,1000.);
#13737=VECTOR('',#101061,1000.);
#13738=VECTOR('',#101062,1000.);
#13739=VECTOR('',#101063,1000.);
#13740=VECTOR('',#101064,1000.);
#13741=VECTOR('',#101067,1000.);
#13742=VECTOR('',#101068,1000.);
#13743=VECTOR('',#101069,1000.);
#13744=VECTOR('',#101072,1000.);
#13745=VECTOR('',#101073,1000.);
#13746=VECTOR('',#101074,1000.);
#13747=VECTOR('',#101077,1000.);
#13748=VECTOR('',#101078,1000.);
#13749=VECTOR('',#101081,1000.);
#13750=VECTOR('',#101082,1000.);
#13751=VECTOR('',#101083,1000.);
#13752=VECTOR('',#101084,1000.);
#13753=VECTOR('',#101087,1000.);
#13754=VECTOR('',#101088,1000.);
#13755=VECTOR('',#101089,1000.);
#13756=VECTOR('',#101092,1000.);
#13757=VECTOR('',#101093,1000.);
#13758=VECTOR('',#101094,1000.);
#13759=VECTOR('',#101097,1000.);
#13760=VECTOR('',#101098,1000.);
#13761=VECTOR('',#101101,1000.);
#13762=VECTOR('',#101102,1000.);
#13763=VECTOR('',#101103,1000.);
#13764=VECTOR('',#101104,1000.);
#13765=VECTOR('',#101107,1000.);
#13766=VECTOR('',#101108,1000.);
#13767=VECTOR('',#101109,1000.);
#13768=VECTOR('',#101112,1000.);
#13769=VECTOR('',#101113,1000.);
#13770=VECTOR('',#101114,1000.);
#13771=VECTOR('',#101117,1000.);
#13772=VECTOR('',#101118,1000.);
#13773=VECTOR('',#101121,1000.);
#13774=VECTOR('',#101122,1000.);
#13775=VECTOR('',#101123,1000.);
#13776=VECTOR('',#101124,1000.);
#13777=VECTOR('',#101127,1000.);
#13778=VECTOR('',#101128,1000.);
#13779=VECTOR('',#101129,1000.);
#13780=VECTOR('',#101132,1000.);
#13781=VECTOR('',#101133,1000.);
#13782=VECTOR('',#101134,1000.);
#13783=VECTOR('',#101137,1000.);
#13784=VECTOR('',#101138,1000.);
#13785=VECTOR('',#101141,1000.);
#13786=VECTOR('',#101142,1000.);
#13787=VECTOR('',#101143,1000.);
#13788=VECTOR('',#101144,1000.);
#13789=VECTOR('',#101147,1000.);
#13790=VECTOR('',#101148,1000.);
#13791=VECTOR('',#101149,1000.);
#13792=VECTOR('',#101152,1000.);
#13793=VECTOR('',#101153,1000.);
#13794=VECTOR('',#101154,1000.);
#13795=VECTOR('',#101157,1000.);
#13796=VECTOR('',#101158,1000.);
#13797=VECTOR('',#101161,1000.);
#13798=VECTOR('',#101162,1000.);
#13799=VECTOR('',#101163,1000.);
#13800=VECTOR('',#101164,1000.);
#13801=VECTOR('',#101167,1000.);
#13802=VECTOR('',#101168,1000.);
#13803=VECTOR('',#101169,1000.);
#13804=VECTOR('',#101172,1000.);
#13805=VECTOR('',#101173,1000.);
#13806=VECTOR('',#101174,1000.);
#13807=VECTOR('',#101177,1000.);
#13808=VECTOR('',#101178,1000.);
#13809=VECTOR('',#101181,1000.);
#13810=VECTOR('',#101182,1000.);
#13811=VECTOR('',#101183,1000.);
#13812=VECTOR('',#101184,1000.);
#13813=VECTOR('',#101187,1000.);
#13814=VECTOR('',#101188,1000.);
#13815=VECTOR('',#101189,1000.);
#13816=VECTOR('',#101192,1000.);
#13817=VECTOR('',#101193,1000.);
#13818=VECTOR('',#101194,1000.);
#13819=VECTOR('',#101197,1000.);
#13820=VECTOR('',#101198,1000.);
#13821=VECTOR('',#101201,1000.);
#13822=VECTOR('',#101202,1000.);
#13823=VECTOR('',#101203,1000.);
#13824=VECTOR('',#101204,1000.);
#13825=VECTOR('',#101207,1000.);
#13826=VECTOR('',#101208,1000.);
#13827=VECTOR('',#101209,1000.);
#13828=VECTOR('',#101212,1000.);
#13829=VECTOR('',#101213,1000.);
#13830=VECTOR('',#101214,1000.);
#13831=VECTOR('',#101217,1000.);
#13832=VECTOR('',#101218,1000.);
#13833=VECTOR('',#101221,1000.);
#13834=VECTOR('',#101222,1000.);
#13835=VECTOR('',#101223,1000.);
#13836=VECTOR('',#101224,1000.);
#13837=VECTOR('',#101227,1000.);
#13838=VECTOR('',#101228,1000.);
#13839=VECTOR('',#101229,1000.);
#13840=VECTOR('',#101232,1000.);
#13841=VECTOR('',#101233,1000.);
#13842=VECTOR('',#101234,1000.);
#13843=VECTOR('',#101237,1000.);
#13844=VECTOR('',#101238,1000.);
#13845=VECTOR('',#101241,1000.);
#13846=VECTOR('',#101242,1000.);
#13847=VECTOR('',#101243,1000.);
#13848=VECTOR('',#101244,1000.);
#13849=VECTOR('',#101247,1000.);
#13850=VECTOR('',#101248,1000.);
#13851=VECTOR('',#101249,1000.);
#13852=VECTOR('',#101252,1000.);
#13853=VECTOR('',#101253,1000.);
#13854=VECTOR('',#101254,1000.);
#13855=VECTOR('',#101257,1000.);
#13856=VECTOR('',#101258,1000.);
#13857=VECTOR('',#101261,1000.);
#13858=VECTOR('',#101262,1000.);
#13859=VECTOR('',#101263,1000.);
#13860=VECTOR('',#101264,1000.);
#13861=VECTOR('',#101267,1000.);
#13862=VECTOR('',#101268,1000.);
#13863=VECTOR('',#101269,1000.);
#13864=VECTOR('',#101272,1000.);
#13865=VECTOR('',#101273,1000.);
#13866=VECTOR('',#101274,1000.);
#13867=VECTOR('',#101277,1000.);
#13868=VECTOR('',#101278,1000.);
#13869=VECTOR('',#101281,1000.);
#13870=VECTOR('',#101282,1000.);
#13871=VECTOR('',#101283,1000.);
#13872=VECTOR('',#101284,1000.);
#13873=VECTOR('',#101287,1000.);
#13874=VECTOR('',#101288,1000.);
#13875=VECTOR('',#101289,1000.);
#13876=VECTOR('',#101292,1000.);
#13877=VECTOR('',#101293,1000.);
#13878=VECTOR('',#101294,1000.);
#13879=VECTOR('',#101297,1000.);
#13880=VECTOR('',#101298,1000.);
#13881=VECTOR('',#101301,1000.);
#13882=VECTOR('',#101302,1000.);
#13883=VECTOR('',#101303,1000.);
#13884=VECTOR('',#101304,1000.);
#13885=VECTOR('',#101307,1000.);
#13886=VECTOR('',#101308,1000.);
#13887=VECTOR('',#101309,1000.);
#13888=VECTOR('',#101312,1000.);
#13889=VECTOR('',#101313,1000.);
#13890=VECTOR('',#101314,1000.);
#13891=VECTOR('',#101317,1000.);
#13892=VECTOR('',#101318,1000.);
#13893=VECTOR('',#101321,1000.);
#13894=VECTOR('',#101322,1000.);
#13895=VECTOR('',#101323,1000.);
#13896=VECTOR('',#101324,1000.);
#13897=VECTOR('',#101327,1000.);
#13898=VECTOR('',#101328,1000.);
#13899=VECTOR('',#101329,1000.);
#13900=VECTOR('',#101332,1000.);
#13901=VECTOR('',#101333,1000.);
#13902=VECTOR('',#101334,1000.);
#13903=VECTOR('',#101337,1000.);
#13904=VECTOR('',#101338,1000.);
#13905=VECTOR('',#101341,1000.);
#13906=VECTOR('',#101342,1000.);
#13907=VECTOR('',#101343,1000.);
#13908=VECTOR('',#101344,1000.);
#13909=VECTOR('',#101347,1000.);
#13910=VECTOR('',#101348,1000.);
#13911=VECTOR('',#101349,1000.);
#13912=VECTOR('',#101352,1000.);
#13913=VECTOR('',#101353,1000.);
#13914=VECTOR('',#101354,1000.);
#13915=VECTOR('',#101357,1000.);
#13916=VECTOR('',#101358,1000.);
#13917=VECTOR('',#101361,1000.);
#13918=VECTOR('',#101362,1000.);
#13919=VECTOR('',#101363,1000.);
#13920=VECTOR('',#101364,1000.);
#13921=VECTOR('',#101367,1000.);
#13922=VECTOR('',#101368,1000.);
#13923=VECTOR('',#101369,1000.);
#13924=VECTOR('',#101372,1000.);
#13925=VECTOR('',#101373,1000.);
#13926=VECTOR('',#101374,1000.);
#13927=VECTOR('',#101377,1000.);
#13928=VECTOR('',#101378,1000.);
#13929=VECTOR('',#101381,1000.);
#13930=VECTOR('',#101382,1000.);
#13931=VECTOR('',#101383,1000.);
#13932=VECTOR('',#101384,1000.);
#13933=VECTOR('',#101387,1000.);
#13934=VECTOR('',#101388,1000.);
#13935=VECTOR('',#101389,1000.);
#13936=VECTOR('',#101392,1000.);
#13937=VECTOR('',#101393,1000.);
#13938=VECTOR('',#101394,1000.);
#13939=VECTOR('',#101397,1000.);
#13940=VECTOR('',#101398,1000.);
#13941=VECTOR('',#101401,1000.);
#13942=VECTOR('',#101402,1000.);
#13943=VECTOR('',#101403,1000.);
#13944=VECTOR('',#101404,1000.);
#13945=VECTOR('',#101407,1000.);
#13946=VECTOR('',#101408,1000.);
#13947=VECTOR('',#101409,1000.);
#13948=VECTOR('',#101412,1000.);
#13949=VECTOR('',#101413,1000.);
#13950=VECTOR('',#101414,1000.);
#13951=VECTOR('',#101417,1000.);
#13952=VECTOR('',#101418,1000.);
#13953=VECTOR('',#101421,1000.);
#13954=VECTOR('',#101422,1000.);
#13955=VECTOR('',#101423,1000.);
#13956=VECTOR('',#101424,1000.);
#13957=VECTOR('',#101427,1000.);
#13958=VECTOR('',#101428,1000.);
#13959=VECTOR('',#101429,1000.);
#13960=VECTOR('',#101432,1000.);
#13961=VECTOR('',#101433,1000.);
#13962=VECTOR('',#101434,1000.);
#13963=VECTOR('',#101437,1000.);
#13964=VECTOR('',#101438,1000.);
#13965=VECTOR('',#101441,1000.);
#13966=VECTOR('',#101442,1000.);
#13967=VECTOR('',#101443,1000.);
#13968=VECTOR('',#101444,1000.);
#13969=VECTOR('',#101447,1000.);
#13970=VECTOR('',#101448,1000.);
#13971=VECTOR('',#101449,1000.);
#13972=VECTOR('',#101452,1000.);
#13973=VECTOR('',#101453,1000.);
#13974=VECTOR('',#101454,1000.);
#13975=VECTOR('',#101457,1000.);
#13976=VECTOR('',#101458,1000.);
#13977=VECTOR('',#101461,1000.);
#13978=VECTOR('',#101462,1000.);
#13979=VECTOR('',#101463,1000.);
#13980=VECTOR('',#101464,1000.);
#13981=VECTOR('',#101467,1000.);
#13982=VECTOR('',#101468,1000.);
#13983=VECTOR('',#101469,1000.);
#13984=VECTOR('',#101472,1000.);
#13985=VECTOR('',#101473,1000.);
#13986=VECTOR('',#101474,1000.);
#13987=VECTOR('',#101477,1000.);
#13988=VECTOR('',#101478,1000.);
#13989=VECTOR('',#101481,1000.);
#13990=VECTOR('',#101482,1000.);
#13991=VECTOR('',#101483,1000.);
#13992=VECTOR('',#101484,1000.);
#13993=VECTOR('',#101487,1000.);
#13994=VECTOR('',#101488,1000.);
#13995=VECTOR('',#101489,1000.);
#13996=VECTOR('',#101492,1000.);
#13997=VECTOR('',#101493,1000.);
#13998=VECTOR('',#101494,1000.);
#13999=VECTOR('',#101497,1000.);
#14000=VECTOR('',#101498,1000.);
#14001=VECTOR('',#101501,1000.);
#14002=VECTOR('',#101502,1000.);
#14003=VECTOR('',#101503,1000.);
#14004=VECTOR('',#101504,1000.);
#14005=VECTOR('',#101507,1000.);
#14006=VECTOR('',#101508,1000.);
#14007=VECTOR('',#101509,1000.);
#14008=VECTOR('',#101512,1000.);
#14009=VECTOR('',#101513,1000.);
#14010=VECTOR('',#101514,1000.);
#14011=VECTOR('',#101517,1000.);
#14012=VECTOR('',#101518,1000.);
#14013=VECTOR('',#101521,1000.);
#14014=VECTOR('',#101522,1000.);
#14015=VECTOR('',#101523,1000.);
#14016=VECTOR('',#101524,1000.);
#14017=VECTOR('',#101527,1000.);
#14018=VECTOR('',#101528,1000.);
#14019=VECTOR('',#101529,1000.);
#14020=VECTOR('',#101532,1000.);
#14021=VECTOR('',#101533,1000.);
#14022=VECTOR('',#101534,1000.);
#14023=VECTOR('',#101537,1000.);
#14024=VECTOR('',#101538,1000.);
#14025=VECTOR('',#101541,1000.);
#14026=VECTOR('',#101542,1000.);
#14027=VECTOR('',#101543,1000.);
#14028=VECTOR('',#101544,1000.);
#14029=VECTOR('',#101547,1000.);
#14030=VECTOR('',#101548,1000.);
#14031=VECTOR('',#101549,1000.);
#14032=VECTOR('',#101552,1000.);
#14033=VECTOR('',#101553,1000.);
#14034=VECTOR('',#101554,1000.);
#14035=VECTOR('',#101557,1000.);
#14036=VECTOR('',#101558,1000.);
#14037=VECTOR('',#101561,1000.);
#14038=VECTOR('',#101562,1000.);
#14039=VECTOR('',#101563,1000.);
#14040=VECTOR('',#101564,1000.);
#14041=VECTOR('',#101567,1000.);
#14042=VECTOR('',#101568,1000.);
#14043=VECTOR('',#101569,1000.);
#14044=VECTOR('',#101572,1000.);
#14045=VECTOR('',#101573,1000.);
#14046=VECTOR('',#101574,1000.);
#14047=VECTOR('',#101577,1000.);
#14048=VECTOR('',#101578,1000.);
#14049=VECTOR('',#101581,1000.);
#14050=VECTOR('',#101582,1000.);
#14051=VECTOR('',#101583,1000.);
#14052=VECTOR('',#101584,1000.);
#14053=VECTOR('',#101587,1000.);
#14054=VECTOR('',#101588,1000.);
#14055=VECTOR('',#101589,1000.);
#14056=VECTOR('',#101592,1000.);
#14057=VECTOR('',#101593,1000.);
#14058=VECTOR('',#101594,1000.);
#14059=VECTOR('',#101597,1000.);
#14060=VECTOR('',#101598,1000.);
#14061=VECTOR('',#101601,1000.);
#14062=VECTOR('',#101602,1000.);
#14063=VECTOR('',#101603,1000.);
#14064=VECTOR('',#101604,1000.);
#14065=VECTOR('',#101607,1000.);
#14066=VECTOR('',#101608,1000.);
#14067=VECTOR('',#101609,1000.);
#14068=VECTOR('',#101612,1000.);
#14069=VECTOR('',#101613,1000.);
#14070=VECTOR('',#101614,1000.);
#14071=VECTOR('',#101617,1000.);
#14072=VECTOR('',#101618,1000.);
#14073=VECTOR('',#101621,1000.);
#14074=VECTOR('',#101622,1000.);
#14075=VECTOR('',#101623,1000.);
#14076=VECTOR('',#101624,1000.);
#14077=VECTOR('',#101627,1000.);
#14078=VECTOR('',#101628,1000.);
#14079=VECTOR('',#101629,1000.);
#14080=VECTOR('',#101632,1000.);
#14081=VECTOR('',#101633,1000.);
#14082=VECTOR('',#101634,1000.);
#14083=VECTOR('',#101637,1000.);
#14084=VECTOR('',#101638,1000.);
#14085=VECTOR('',#101641,1000.);
#14086=VECTOR('',#101642,1000.);
#14087=VECTOR('',#101643,1000.);
#14088=VECTOR('',#101644,1000.);
#14089=VECTOR('',#101647,1000.);
#14090=VECTOR('',#101648,1000.);
#14091=VECTOR('',#101649,1000.);
#14092=VECTOR('',#101652,1000.);
#14093=VECTOR('',#101653,1000.);
#14094=VECTOR('',#101654,1000.);
#14095=VECTOR('',#101657,1000.);
#14096=VECTOR('',#101658,1000.);
#14097=VECTOR('',#101661,1000.);
#14098=VECTOR('',#101662,1000.);
#14099=VECTOR('',#101663,1000.);
#14100=VECTOR('',#101664,1000.);
#14101=VECTOR('',#101667,1000.);
#14102=VECTOR('',#101668,1000.);
#14103=VECTOR('',#101669,1000.);
#14104=VECTOR('',#101672,1000.);
#14105=VECTOR('',#101673,1000.);
#14106=VECTOR('',#101674,1000.);
#14107=VECTOR('',#101677,1000.);
#14108=VECTOR('',#101678,1000.);
#14109=VECTOR('',#101681,1000.);
#14110=VECTOR('',#101682,1000.);
#14111=VECTOR('',#101683,1000.);
#14112=VECTOR('',#101684,1000.);
#14113=VECTOR('',#101687,1000.);
#14114=VECTOR('',#101688,1000.);
#14115=VECTOR('',#101689,1000.);
#14116=VECTOR('',#101692,1000.);
#14117=VECTOR('',#101693,1000.);
#14118=VECTOR('',#101694,1000.);
#14119=VECTOR('',#101697,1000.);
#14120=VECTOR('',#101698,1000.);
#14121=VECTOR('',#101701,1000.);
#14122=VECTOR('',#101702,1000.);
#14123=VECTOR('',#101703,1000.);
#14124=VECTOR('',#101704,1000.);
#14125=VECTOR('',#101707,1000.);
#14126=VECTOR('',#101708,1000.);
#14127=VECTOR('',#101709,1000.);
#14128=VECTOR('',#101712,1000.);
#14129=VECTOR('',#101713,1000.);
#14130=VECTOR('',#101714,1000.);
#14131=VECTOR('',#101717,1000.);
#14132=VECTOR('',#101718,1000.);
#14133=VECTOR('',#101721,1000.);
#14134=VECTOR('',#101722,1000.);
#14135=VECTOR('',#101723,1000.);
#14136=VECTOR('',#101724,1000.);
#14137=VECTOR('',#101727,1000.);
#14138=VECTOR('',#101728,1000.);
#14139=VECTOR('',#101729,1000.);
#14140=VECTOR('',#101732,1000.);
#14141=VECTOR('',#101733,1000.);
#14142=VECTOR('',#101734,1000.);
#14143=VECTOR('',#101737,1000.);
#14144=VECTOR('',#101738,1000.);
#14145=VECTOR('',#101741,1000.);
#14146=VECTOR('',#101742,1000.);
#14147=VECTOR('',#101743,1000.);
#14148=VECTOR('',#101744,1000.);
#14149=VECTOR('',#101747,1000.);
#14150=VECTOR('',#101748,1000.);
#14151=VECTOR('',#101749,1000.);
#14152=VECTOR('',#101752,1000.);
#14153=VECTOR('',#101753,1000.);
#14154=VECTOR('',#101754,1000.);
#14155=VECTOR('',#101757,1000.);
#14156=VECTOR('',#101758,1000.);
#14157=VECTOR('',#101761,1000.);
#14158=VECTOR('',#101762,1000.);
#14159=VECTOR('',#101763,1000.);
#14160=VECTOR('',#101764,1000.);
#14161=VECTOR('',#101767,1000.);
#14162=VECTOR('',#101768,1000.);
#14163=VECTOR('',#101769,1000.);
#14164=VECTOR('',#101772,1000.);
#14165=VECTOR('',#101773,1000.);
#14166=VECTOR('',#101774,1000.);
#14167=VECTOR('',#101777,1000.);
#14168=VECTOR('',#101778,1000.);
#14169=VECTOR('',#101781,1000.);
#14170=VECTOR('',#101782,1000.);
#14171=VECTOR('',#101783,1000.);
#14172=VECTOR('',#101784,1000.);
#14173=VECTOR('',#101787,1000.);
#14174=VECTOR('',#101788,1000.);
#14175=VECTOR('',#101789,1000.);
#14176=VECTOR('',#101792,1000.);
#14177=VECTOR('',#101793,1000.);
#14178=VECTOR('',#101794,1000.);
#14179=VECTOR('',#101797,1000.);
#14180=VECTOR('',#101798,1000.);
#14181=VECTOR('',#101801,1000.);
#14182=VECTOR('',#101802,1000.);
#14183=VECTOR('',#101803,1000.);
#14184=VECTOR('',#101804,1000.);
#14185=VECTOR('',#101807,1000.);
#14186=VECTOR('',#101808,1000.);
#14187=VECTOR('',#101809,1000.);
#14188=VECTOR('',#101812,1000.);
#14189=VECTOR('',#101813,1000.);
#14190=VECTOR('',#101814,1000.);
#14191=VECTOR('',#101817,1000.);
#14192=VECTOR('',#101818,1000.);
#14193=VECTOR('',#101821,1000.);
#14194=VECTOR('',#101822,1000.);
#14195=VECTOR('',#101823,1000.);
#14196=VECTOR('',#101824,1000.);
#14197=VECTOR('',#101827,1000.);
#14198=VECTOR('',#101828,1000.);
#14199=VECTOR('',#101829,1000.);
#14200=VECTOR('',#101832,1000.);
#14201=VECTOR('',#101833,1000.);
#14202=VECTOR('',#101834,1000.);
#14203=VECTOR('',#101837,1000.);
#14204=VECTOR('',#101838,1000.);
#14205=VECTOR('',#101841,1000.);
#14206=VECTOR('',#101842,1000.);
#14207=VECTOR('',#101843,1000.);
#14208=VECTOR('',#101844,1000.);
#14209=VECTOR('',#101847,1000.);
#14210=VECTOR('',#101848,1000.);
#14211=VECTOR('',#101849,1000.);
#14212=VECTOR('',#101852,1000.);
#14213=VECTOR('',#101853,1000.);
#14214=VECTOR('',#101854,1000.);
#14215=VECTOR('',#101857,1000.);
#14216=VECTOR('',#101858,1000.);
#14217=VECTOR('',#101861,1000.);
#14218=VECTOR('',#101862,1000.);
#14219=VECTOR('',#101863,1000.);
#14220=VECTOR('',#101864,1000.);
#14221=VECTOR('',#101867,1000.);
#14222=VECTOR('',#101868,1000.);
#14223=VECTOR('',#101869,1000.);
#14224=VECTOR('',#101872,1000.);
#14225=VECTOR('',#101873,1000.);
#14226=VECTOR('',#101874,1000.);
#14227=VECTOR('',#101877,1000.);
#14228=VECTOR('',#101878,1000.);
#14229=VECTOR('',#101881,1000.);
#14230=VECTOR('',#101882,1000.);
#14231=VECTOR('',#101883,1000.);
#14232=VECTOR('',#101884,1000.);
#14233=VECTOR('',#101887,1000.);
#14234=VECTOR('',#101888,1000.);
#14235=VECTOR('',#101889,1000.);
#14236=VECTOR('',#101892,1000.);
#14237=VECTOR('',#101893,1000.);
#14238=VECTOR('',#101894,1000.);
#14239=VECTOR('',#101897,1000.);
#14240=VECTOR('',#101898,1000.);
#14241=VECTOR('',#101901,1000.);
#14242=VECTOR('',#101902,1000.);
#14243=VECTOR('',#101903,1000.);
#14244=VECTOR('',#101904,1000.);
#14245=VECTOR('',#101907,1000.);
#14246=VECTOR('',#101908,1000.);
#14247=VECTOR('',#101909,1000.);
#14248=VECTOR('',#101912,1000.);
#14249=VECTOR('',#101913,1000.);
#14250=VECTOR('',#101914,1000.);
#14251=VECTOR('',#101917,1000.);
#14252=VECTOR('',#101918,1000.);
#14253=VECTOR('',#101921,1000.);
#14254=VECTOR('',#101922,1000.);
#14255=VECTOR('',#101923,1000.);
#14256=VECTOR('',#101924,1000.);
#14257=VECTOR('',#101927,1000.);
#14258=VECTOR('',#101928,1000.);
#14259=VECTOR('',#101929,1000.);
#14260=VECTOR('',#101932,1000.);
#14261=VECTOR('',#101933,1000.);
#14262=VECTOR('',#101934,1000.);
#14263=VECTOR('',#101937,1000.);
#14264=VECTOR('',#101938,1000.);
#14265=VECTOR('',#101941,1000.);
#14266=VECTOR('',#101942,1000.);
#14267=VECTOR('',#101943,1000.);
#14268=VECTOR('',#101944,1000.);
#14269=VECTOR('',#101947,1000.);
#14270=VECTOR('',#101948,1000.);
#14271=VECTOR('',#101949,1000.);
#14272=VECTOR('',#101952,1000.);
#14273=VECTOR('',#101953,1000.);
#14274=VECTOR('',#101954,1000.);
#14275=VECTOR('',#101957,1000.);
#14276=VECTOR('',#101958,1000.);
#14277=VECTOR('',#101961,1000.);
#14278=VECTOR('',#101962,1000.);
#14279=VECTOR('',#101963,1000.);
#14280=VECTOR('',#101964,1000.);
#14281=VECTOR('',#101967,1000.);
#14282=VECTOR('',#101968,1000.);
#14283=VECTOR('',#101969,1000.);
#14284=VECTOR('',#101972,1000.);
#14285=VECTOR('',#101973,1000.);
#14286=VECTOR('',#101974,1000.);
#14287=VECTOR('',#101977,1000.);
#14288=VECTOR('',#101978,1000.);
#14289=VECTOR('',#101981,1000.);
#14290=VECTOR('',#101982,1000.);
#14291=VECTOR('',#101983,1000.);
#14292=VECTOR('',#101984,1000.);
#14293=VECTOR('',#101987,1000.);
#14294=VECTOR('',#101988,1000.);
#14295=VECTOR('',#101989,1000.);
#14296=VECTOR('',#101992,1000.);
#14297=VECTOR('',#101993,1000.);
#14298=VECTOR('',#101994,1000.);
#14299=VECTOR('',#101997,1000.);
#14300=VECTOR('',#101998,1000.);
#14301=VECTOR('',#102001,1000.);
#14302=VECTOR('',#102002,1000.);
#14303=VECTOR('',#102003,1000.);
#14304=VECTOR('',#102004,1000.);
#14305=VECTOR('',#102007,1000.);
#14306=VECTOR('',#102008,1000.);
#14307=VECTOR('',#102009,1000.);
#14308=VECTOR('',#102012,1000.);
#14309=VECTOR('',#102013,1000.);
#14310=VECTOR('',#102014,1000.);
#14311=VECTOR('',#102017,1000.);
#14312=VECTOR('',#102018,1000.);
#14313=VECTOR('',#102021,1000.);
#14314=VECTOR('',#102022,1000.);
#14315=VECTOR('',#102023,1000.);
#14316=VECTOR('',#102024,1000.);
#14317=VECTOR('',#102027,1000.);
#14318=VECTOR('',#102028,1000.);
#14319=VECTOR('',#102029,1000.);
#14320=VECTOR('',#102032,1000.);
#14321=VECTOR('',#102033,1000.);
#14322=VECTOR('',#102034,1000.);
#14323=VECTOR('',#102037,1000.);
#14324=VECTOR('',#102038,1000.);
#14325=VECTOR('',#102041,1000.);
#14326=VECTOR('',#102042,1000.);
#14327=VECTOR('',#102043,1000.);
#14328=VECTOR('',#102044,1000.);
#14329=VECTOR('',#102047,1000.);
#14330=VECTOR('',#102048,1000.);
#14331=VECTOR('',#102049,1000.);
#14332=VECTOR('',#102052,1000.);
#14333=VECTOR('',#102053,1000.);
#14334=VECTOR('',#102054,1000.);
#14335=VECTOR('',#102057,1000.);
#14336=VECTOR('',#102058,1000.);
#14337=VECTOR('',#102061,1000.);
#14338=VECTOR('',#102062,1000.);
#14339=VECTOR('',#102063,1000.);
#14340=VECTOR('',#102064,1000.);
#14341=VECTOR('',#102067,1000.);
#14342=VECTOR('',#102068,1000.);
#14343=VECTOR('',#102069,1000.);
#14344=VECTOR('',#102072,1000.);
#14345=VECTOR('',#102073,1000.);
#14346=VECTOR('',#102074,1000.);
#14347=VECTOR('',#102077,1000.);
#14348=VECTOR('',#102078,1000.);
#14349=VECTOR('',#102081,1000.);
#14350=VECTOR('',#102082,1000.);
#14351=VECTOR('',#102083,1000.);
#14352=VECTOR('',#102084,1000.);
#14353=VECTOR('',#102087,1000.);
#14354=VECTOR('',#102088,1000.);
#14355=VECTOR('',#102089,1000.);
#14356=VECTOR('',#102092,1000.);
#14357=VECTOR('',#102093,1000.);
#14358=VECTOR('',#102094,1000.);
#14359=VECTOR('',#102097,1000.);
#14360=VECTOR('',#102098,1000.);
#14361=VECTOR('',#102101,1000.);
#14362=VECTOR('',#102102,1000.);
#14363=VECTOR('',#102103,1000.);
#14364=VECTOR('',#102104,1000.);
#14365=VECTOR('',#102107,1000.);
#14366=VECTOR('',#102108,1000.);
#14367=VECTOR('',#102109,1000.);
#14368=VECTOR('',#102112,1000.);
#14369=VECTOR('',#102113,1000.);
#14370=VECTOR('',#102114,1000.);
#14371=VECTOR('',#102117,1000.);
#14372=VECTOR('',#102118,1000.);
#14373=VECTOR('',#102121,1000.);
#14374=VECTOR('',#102122,1000.);
#14375=VECTOR('',#102123,1000.);
#14376=VECTOR('',#102124,1000.);
#14377=VECTOR('',#102127,1000.);
#14378=VECTOR('',#102128,1000.);
#14379=VECTOR('',#102129,1000.);
#14380=VECTOR('',#102132,1000.);
#14381=VECTOR('',#102133,1000.);
#14382=VECTOR('',#102134,1000.);
#14383=VECTOR('',#102137,1000.);
#14384=VECTOR('',#102138,1000.);
#14385=VECTOR('',#102141,1000.);
#14386=VECTOR('',#102142,1000.);
#14387=VECTOR('',#102143,1000.);
#14388=VECTOR('',#102144,1000.);
#14389=VECTOR('',#102147,1000.);
#14390=VECTOR('',#102148,1000.);
#14391=VECTOR('',#102149,1000.);
#14392=VECTOR('',#102152,1000.);
#14393=VECTOR('',#102153,1000.);
#14394=VECTOR('',#102154,1000.);
#14395=VECTOR('',#102157,1000.);
#14396=VECTOR('',#102158,1000.);
#14397=VECTOR('',#102161,1000.);
#14398=VECTOR('',#102162,1000.);
#14399=VECTOR('',#102163,1000.);
#14400=VECTOR('',#102164,1000.);
#14401=VECTOR('',#102167,1000.);
#14402=VECTOR('',#102168,1000.);
#14403=VECTOR('',#102169,1000.);
#14404=VECTOR('',#102172,1000.);
#14405=VECTOR('',#102173,1000.);
#14406=VECTOR('',#102174,1000.);
#14407=VECTOR('',#102177,1000.);
#14408=VECTOR('',#102178,1000.);
#14409=VECTOR('',#102181,1000.);
#14410=VECTOR('',#102182,1000.);
#14411=VECTOR('',#102183,1000.);
#14412=VECTOR('',#102184,1000.);
#14413=VECTOR('',#102187,1000.);
#14414=VECTOR('',#102188,1000.);
#14415=VECTOR('',#102189,1000.);
#14416=VECTOR('',#102192,1000.);
#14417=VECTOR('',#102193,1000.);
#14418=VECTOR('',#102194,1000.);
#14419=VECTOR('',#102197,1000.);
#14420=VECTOR('',#102198,1000.);
#14421=VECTOR('',#102201,1000.);
#14422=VECTOR('',#102202,1000.);
#14423=VECTOR('',#102203,1000.);
#14424=VECTOR('',#102204,1000.);
#14425=VECTOR('',#102207,1000.);
#14426=VECTOR('',#102208,1000.);
#14427=VECTOR('',#102209,1000.);
#14428=VECTOR('',#102212,1000.);
#14429=VECTOR('',#102213,1000.);
#14430=VECTOR('',#102214,1000.);
#14431=VECTOR('',#102217,1000.);
#14432=VECTOR('',#102218,1000.);
#14433=VECTOR('',#102221,1000.);
#14434=VECTOR('',#102222,1000.);
#14435=VECTOR('',#102223,1000.);
#14436=VECTOR('',#102224,1000.);
#14437=VECTOR('',#102227,1000.);
#14438=VECTOR('',#102228,1000.);
#14439=VECTOR('',#102229,1000.);
#14440=VECTOR('',#102232,1000.);
#14441=VECTOR('',#102233,1000.);
#14442=VECTOR('',#102234,1000.);
#14443=VECTOR('',#102237,1000.);
#14444=VECTOR('',#102238,1000.);
#14445=VECTOR('',#102241,1000.);
#14446=VECTOR('',#102242,1000.);
#14447=VECTOR('',#102243,1000.);
#14448=VECTOR('',#102244,1000.);
#14449=VECTOR('',#102247,1000.);
#14450=VECTOR('',#102248,1000.);
#14451=VECTOR('',#102249,1000.);
#14452=VECTOR('',#102252,1000.);
#14453=VECTOR('',#102253,1000.);
#14454=VECTOR('',#102254,1000.);
#14455=VECTOR('',#102257,1000.);
#14456=VECTOR('',#102258,1000.);
#14457=VECTOR('',#102261,1000.);
#14458=VECTOR('',#102262,1000.);
#14459=VECTOR('',#102263,1000.);
#14460=VECTOR('',#102264,1000.);
#14461=VECTOR('',#102267,1000.);
#14462=VECTOR('',#102268,1000.);
#14463=VECTOR('',#102269,1000.);
#14464=VECTOR('',#102272,1000.);
#14465=VECTOR('',#102273,1000.);
#14466=VECTOR('',#102274,1000.);
#14467=VECTOR('',#102277,1000.);
#14468=VECTOR('',#102278,1000.);
#14469=VECTOR('',#102281,1000.);
#14470=VECTOR('',#102282,1000.);
#14471=VECTOR('',#102283,1000.);
#14472=VECTOR('',#102284,1000.);
#14473=VECTOR('',#102287,1000.);
#14474=VECTOR('',#102288,1000.);
#14475=VECTOR('',#102289,1000.);
#14476=VECTOR('',#102292,1000.);
#14477=VECTOR('',#102293,1000.);
#14478=VECTOR('',#102294,1000.);
#14479=VECTOR('',#102297,1000.);
#14480=VECTOR('',#102298,1000.);
#14481=VECTOR('',#102301,1000.);
#14482=VECTOR('',#102302,1000.);
#14483=VECTOR('',#102303,1000.);
#14484=VECTOR('',#102304,1000.);
#14485=VECTOR('',#102307,1000.);
#14486=VECTOR('',#102308,1000.);
#14487=VECTOR('',#102309,1000.);
#14488=VECTOR('',#102312,1000.);
#14489=VECTOR('',#102313,1000.);
#14490=VECTOR('',#102314,1000.);
#14491=VECTOR('',#102317,1000.);
#14492=VECTOR('',#102318,1000.);
#14493=VECTOR('',#102321,1000.);
#14494=VECTOR('',#102322,1000.);
#14495=VECTOR('',#102323,1000.);
#14496=VECTOR('',#102324,1000.);
#14497=VECTOR('',#102327,1000.);
#14498=VECTOR('',#102328,1000.);
#14499=VECTOR('',#102329,1000.);
#14500=VECTOR('',#102332,1000.);
#14501=VECTOR('',#102333,1000.);
#14502=VECTOR('',#102334,1000.);
#14503=VECTOR('',#102337,1000.);
#14504=VECTOR('',#102338,1000.);
#14505=VECTOR('',#102341,1000.);
#14506=VECTOR('',#102342,1000.);
#14507=VECTOR('',#102343,1000.);
#14508=VECTOR('',#102344,1000.);
#14509=VECTOR('',#102347,1000.);
#14510=VECTOR('',#102348,1000.);
#14511=VECTOR('',#102349,1000.);
#14512=VECTOR('',#102352,1000.);
#14513=VECTOR('',#102353,1000.);
#14514=VECTOR('',#102354,1000.);
#14515=VECTOR('',#102357,1000.);
#14516=VECTOR('',#102358,1000.);
#14517=VECTOR('',#102361,1000.);
#14518=VECTOR('',#102362,1000.);
#14519=VECTOR('',#102363,1000.);
#14520=VECTOR('',#102364,1000.);
#14521=VECTOR('',#102367,1000.);
#14522=VECTOR('',#102368,1000.);
#14523=VECTOR('',#102369,1000.);
#14524=VECTOR('',#102372,1000.);
#14525=VECTOR('',#102373,1000.);
#14526=VECTOR('',#102374,1000.);
#14527=VECTOR('',#102377,1000.);
#14528=VECTOR('',#102378,1000.);
#14529=VECTOR('',#102381,1000.);
#14530=VECTOR('',#102382,1000.);
#14531=VECTOR('',#102383,1000.);
#14532=VECTOR('',#102384,1000.);
#14533=VECTOR('',#102387,1000.);
#14534=VECTOR('',#102388,1000.);
#14535=VECTOR('',#102389,1000.);
#14536=VECTOR('',#102392,1000.);
#14537=VECTOR('',#102393,1000.);
#14538=VECTOR('',#102394,1000.);
#14539=VECTOR('',#102397,1000.);
#14540=VECTOR('',#102398,1000.);
#14541=VECTOR('',#102401,1000.);
#14542=VECTOR('',#102402,1000.);
#14543=VECTOR('',#102403,1000.);
#14544=VECTOR('',#102404,1000.);
#14545=VECTOR('',#102407,1000.);
#14546=VECTOR('',#102408,1000.);
#14547=VECTOR('',#102409,1000.);
#14548=VECTOR('',#102412,1000.);
#14549=VECTOR('',#102413,1000.);
#14550=VECTOR('',#102414,1000.);
#14551=VECTOR('',#102417,1000.);
#14552=VECTOR('',#102418,1000.);
#14553=VECTOR('',#102421,1000.);
#14554=VECTOR('',#102422,1000.);
#14555=VECTOR('',#102423,1000.);
#14556=VECTOR('',#102424,1000.);
#14557=VECTOR('',#102427,1000.);
#14558=VECTOR('',#102428,1000.);
#14559=VECTOR('',#102429,1000.);
#14560=VECTOR('',#102432,1000.);
#14561=VECTOR('',#102433,1000.);
#14562=VECTOR('',#102434,1000.);
#14563=VECTOR('',#102437,1000.);
#14564=VECTOR('',#102438,1000.);
#14565=VECTOR('',#102441,1000.);
#14566=VECTOR('',#102442,1000.);
#14567=VECTOR('',#102443,1000.);
#14568=VECTOR('',#102444,1000.);
#14569=VECTOR('',#102447,1000.);
#14570=VECTOR('',#102448,1000.);
#14571=VECTOR('',#102449,1000.);
#14572=VECTOR('',#102452,1000.);
#14573=VECTOR('',#102453,1000.);
#14574=VECTOR('',#102454,1000.);
#14575=VECTOR('',#102457,1000.);
#14576=VECTOR('',#102458,1000.);
#14577=VECTOR('',#102461,1000.);
#14578=VECTOR('',#102462,1000.);
#14579=VECTOR('',#102463,1000.);
#14580=VECTOR('',#102464,1000.);
#14581=VECTOR('',#102467,1000.);
#14582=VECTOR('',#102468,1000.);
#14583=VECTOR('',#102469,1000.);
#14584=VECTOR('',#102472,1000.);
#14585=VECTOR('',#102473,1000.);
#14586=VECTOR('',#102474,1000.);
#14587=VECTOR('',#102477,1000.);
#14588=VECTOR('',#102478,1000.);
#14589=VECTOR('',#102481,1000.);
#14590=VECTOR('',#102482,1000.);
#14591=VECTOR('',#102483,1000.);
#14592=VECTOR('',#102484,1000.);
#14593=VECTOR('',#102487,1000.);
#14594=VECTOR('',#102488,1000.);
#14595=VECTOR('',#102489,1000.);
#14596=VECTOR('',#102492,1000.);
#14597=VECTOR('',#102493,1000.);
#14598=VECTOR('',#102494,1000.);
#14599=VECTOR('',#102497,1000.);
#14600=VECTOR('',#102498,1000.);
#14601=VECTOR('',#102501,1000.);
#14602=VECTOR('',#102502,1000.);
#14603=VECTOR('',#102503,1000.);
#14604=VECTOR('',#102504,1000.);
#14605=VECTOR('',#102507,1000.);
#14606=VECTOR('',#102508,1000.);
#14607=VECTOR('',#102509,1000.);
#14608=VECTOR('',#102512,1000.);
#14609=VECTOR('',#102513,1000.);
#14610=VECTOR('',#102514,1000.);
#14611=VECTOR('',#102517,1000.);
#14612=VECTOR('',#102518,1000.);
#14613=VECTOR('',#102521,1000.);
#14614=VECTOR('',#102522,1000.);
#14615=VECTOR('',#102523,1000.);
#14616=VECTOR('',#102524,1000.);
#14617=VECTOR('',#102527,1000.);
#14618=VECTOR('',#102528,1000.);
#14619=VECTOR('',#102529,1000.);
#14620=VECTOR('',#102532,1000.);
#14621=VECTOR('',#102533,1000.);
#14622=VECTOR('',#102534,1000.);
#14623=VECTOR('',#102537,1000.);
#14624=VECTOR('',#102538,1000.);
#14625=VECTOR('',#102541,1000.);
#14626=VECTOR('',#102542,1000.);
#14627=VECTOR('',#102543,1000.);
#14628=VECTOR('',#102544,1000.);
#14629=VECTOR('',#102547,1000.);
#14630=VECTOR('',#102548,1000.);
#14631=VECTOR('',#102549,1000.);
#14632=VECTOR('',#102552,1000.);
#14633=VECTOR('',#102553,1000.);
#14634=VECTOR('',#102554,1000.);
#14635=VECTOR('',#102557,1000.);
#14636=VECTOR('',#102558,1000.);
#14637=VECTOR('',#102561,1000.);
#14638=VECTOR('',#102562,1000.);
#14639=VECTOR('',#102563,1000.);
#14640=VECTOR('',#102564,1000.);
#14641=VECTOR('',#102567,1000.);
#14642=VECTOR('',#102568,1000.);
#14643=VECTOR('',#102569,1000.);
#14644=VECTOR('',#102572,1000.);
#14645=VECTOR('',#102573,1000.);
#14646=VECTOR('',#102574,1000.);
#14647=VECTOR('',#102577,1000.);
#14648=VECTOR('',#102578,1000.);
#14649=VECTOR('',#102581,1000.);
#14650=VECTOR('',#102582,1000.);
#14651=VECTOR('',#102583,1000.);
#14652=VECTOR('',#102584,1000.);
#14653=VECTOR('',#102587,1000.);
#14654=VECTOR('',#102588,1000.);
#14655=VECTOR('',#102589,1000.);
#14656=VECTOR('',#102592,1000.);
#14657=VECTOR('',#102593,1000.);
#14658=VECTOR('',#102594,1000.);
#14659=VECTOR('',#102597,1000.);
#14660=VECTOR('',#102598,1000.);
#14661=VECTOR('',#102601,1000.);
#14662=VECTOR('',#102602,1000.);
#14663=VECTOR('',#102603,1000.);
#14664=VECTOR('',#102604,1000.);
#14665=VECTOR('',#102607,1000.);
#14666=VECTOR('',#102608,1000.);
#14667=VECTOR('',#102609,1000.);
#14668=VECTOR('',#102612,1000.);
#14669=VECTOR('',#102613,1000.);
#14670=VECTOR('',#102614,1000.);
#14671=VECTOR('',#102617,1000.);
#14672=VECTOR('',#102618,1000.);
#14673=VECTOR('',#102621,1000.);
#14674=VECTOR('',#102622,1000.);
#14675=VECTOR('',#102623,1000.);
#14676=VECTOR('',#102624,1000.);
#14677=VECTOR('',#102627,1000.);
#14678=VECTOR('',#102628,1000.);
#14679=VECTOR('',#102629,1000.);
#14680=VECTOR('',#102632,1000.);
#14681=VECTOR('',#102633,1000.);
#14682=VECTOR('',#102634,1000.);
#14683=VECTOR('',#102637,1000.);
#14684=VECTOR('',#102638,1000.);
#14685=VECTOR('',#102641,1000.);
#14686=VECTOR('',#102642,1000.);
#14687=VECTOR('',#102643,1000.);
#14688=VECTOR('',#102644,1000.);
#14689=VECTOR('',#102647,1000.);
#14690=VECTOR('',#102648,1000.);
#14691=VECTOR('',#102649,1000.);
#14692=VECTOR('',#102652,1000.);
#14693=VECTOR('',#102653,1000.);
#14694=VECTOR('',#102654,1000.);
#14695=VECTOR('',#102657,1000.);
#14696=VECTOR('',#102658,1000.);
#14697=VECTOR('',#102661,1000.);
#14698=VECTOR('',#102662,1000.);
#14699=VECTOR('',#102663,1000.);
#14700=VECTOR('',#102664,1000.);
#14701=VECTOR('',#102667,1000.);
#14702=VECTOR('',#102668,1000.);
#14703=VECTOR('',#102669,1000.);
#14704=VECTOR('',#102672,1000.);
#14705=VECTOR('',#102673,1000.);
#14706=VECTOR('',#102674,1000.);
#14707=VECTOR('',#102677,1000.);
#14708=VECTOR('',#102678,1000.);
#14709=VECTOR('',#102681,1000.);
#14710=VECTOR('',#102682,1000.);
#14711=VECTOR('',#102683,1000.);
#14712=VECTOR('',#102684,1000.);
#14713=VECTOR('',#102687,1000.);
#14714=VECTOR('',#102688,1000.);
#14715=VECTOR('',#102689,1000.);
#14716=VECTOR('',#102692,1000.);
#14717=VECTOR('',#102693,1000.);
#14718=VECTOR('',#102694,1000.);
#14719=VECTOR('',#102697,1000.);
#14720=VECTOR('',#102698,1000.);
#14721=VECTOR('',#102701,1000.);
#14722=VECTOR('',#102702,1000.);
#14723=VECTOR('',#102703,1000.);
#14724=VECTOR('',#102704,1000.);
#14725=VECTOR('',#102707,1000.);
#14726=VECTOR('',#102708,1000.);
#14727=VECTOR('',#102709,1000.);
#14728=VECTOR('',#102712,1000.);
#14729=VECTOR('',#102713,1000.);
#14730=VECTOR('',#102714,1000.);
#14731=VECTOR('',#102717,1000.);
#14732=VECTOR('',#102718,1000.);
#14733=VECTOR('',#102721,1000.);
#14734=VECTOR('',#102722,1000.);
#14735=VECTOR('',#102723,1000.);
#14736=VECTOR('',#102724,1000.);
#14737=VECTOR('',#102727,1000.);
#14738=VECTOR('',#102728,1000.);
#14739=VECTOR('',#102729,1000.);
#14740=VECTOR('',#102732,1000.);
#14741=VECTOR('',#102733,1000.);
#14742=VECTOR('',#102734,1000.);
#14743=VECTOR('',#102737,1000.);
#14744=VECTOR('',#102738,1000.);
#14745=VECTOR('',#102741,1000.);
#14746=VECTOR('',#102742,1000.);
#14747=VECTOR('',#102743,1000.);
#14748=VECTOR('',#102744,1000.);
#14749=VECTOR('',#102747,1000.);
#14750=VECTOR('',#102748,1000.);
#14751=VECTOR('',#102749,1000.);
#14752=VECTOR('',#102752,1000.);
#14753=VECTOR('',#102753,1000.);
#14754=VECTOR('',#102754,1000.);
#14755=VECTOR('',#102757,1000.);
#14756=VECTOR('',#102758,1000.);
#14757=VECTOR('',#102761,1000.);
#14758=VECTOR('',#102762,1000.);
#14759=VECTOR('',#102763,1000.);
#14760=VECTOR('',#102764,1000.);
#14761=VECTOR('',#102767,1000.);
#14762=VECTOR('',#102768,1000.);
#14763=VECTOR('',#102769,1000.);
#14764=VECTOR('',#102772,1000.);
#14765=VECTOR('',#102773,1000.);
#14766=VECTOR('',#102774,1000.);
#14767=VECTOR('',#102777,1000.);
#14768=VECTOR('',#102778,1000.);
#14769=VECTOR('',#102781,1000.);
#14770=VECTOR('',#102782,1000.);
#14771=VECTOR('',#102783,1000.);
#14772=VECTOR('',#102784,1000.);
#14773=VECTOR('',#102787,1000.);
#14774=VECTOR('',#102788,1000.);
#14775=VECTOR('',#102789,1000.);
#14776=VECTOR('',#102792,1000.);
#14777=VECTOR('',#102793,1000.);
#14778=VECTOR('',#102794,1000.);
#14779=VECTOR('',#102797,1000.);
#14780=VECTOR('',#102798,1000.);
#14781=VECTOR('',#102801,1000.);
#14782=VECTOR('',#102802,1000.);
#14783=VECTOR('',#102803,1000.);
#14784=VECTOR('',#102804,1000.);
#14785=VECTOR('',#102807,1000.);
#14786=VECTOR('',#102808,1000.);
#14787=VECTOR('',#102809,1000.);
#14788=VECTOR('',#102812,1000.);
#14789=VECTOR('',#102813,1000.);
#14790=VECTOR('',#102814,1000.);
#14791=VECTOR('',#102817,1000.);
#14792=VECTOR('',#102818,1000.);
#14793=VECTOR('',#102821,1000.);
#14794=VECTOR('',#102822,1000.);
#14795=VECTOR('',#102823,1000.);
#14796=VECTOR('',#102824,1000.);
#14797=VECTOR('',#102827,1000.);
#14798=VECTOR('',#102828,1000.);
#14799=VECTOR('',#102829,1000.);
#14800=VECTOR('',#102832,1000.);
#14801=VECTOR('',#102833,1000.);
#14802=VECTOR('',#102834,1000.);
#14803=VECTOR('',#102837,1000.);
#14804=VECTOR('',#102838,1000.);
#14805=VECTOR('',#102841,1000.);
#14806=VECTOR('',#102842,1000.);
#14807=VECTOR('',#102843,1000.);
#14808=VECTOR('',#102844,1000.);
#14809=VECTOR('',#102847,1000.);
#14810=VECTOR('',#102848,1000.);
#14811=VECTOR('',#102849,1000.);
#14812=VECTOR('',#102852,1000.);
#14813=VECTOR('',#102853,1000.);
#14814=VECTOR('',#102854,1000.);
#14815=VECTOR('',#102857,1000.);
#14816=VECTOR('',#102858,1000.);
#14817=VECTOR('',#102861,1000.);
#14818=VECTOR('',#102862,1000.);
#14819=VECTOR('',#102863,1000.);
#14820=VECTOR('',#102864,1000.);
#14821=VECTOR('',#102867,1000.);
#14822=VECTOR('',#102868,1000.);
#14823=VECTOR('',#102869,1000.);
#14824=VECTOR('',#102872,1000.);
#14825=VECTOR('',#102873,1000.);
#14826=VECTOR('',#102874,1000.);
#14827=VECTOR('',#102877,1000.);
#14828=VECTOR('',#102878,1000.);
#14829=VECTOR('',#102881,1000.);
#14830=VECTOR('',#102882,1000.);
#14831=VECTOR('',#102883,1000.);
#14832=VECTOR('',#102884,1000.);
#14833=VECTOR('',#102887,1000.);
#14834=VECTOR('',#102888,1000.);
#14835=VECTOR('',#102889,1000.);
#14836=VECTOR('',#102892,1000.);
#14837=VECTOR('',#102893,1000.);
#14838=VECTOR('',#102894,1000.);
#14839=VECTOR('',#102897,1000.);
#14840=VECTOR('',#102898,1000.);
#14841=VECTOR('',#102901,1000.);
#14842=VECTOR('',#102902,1000.);
#14843=VECTOR('',#102903,1000.);
#14844=VECTOR('',#102904,1000.);
#14845=VECTOR('',#102907,1000.);
#14846=VECTOR('',#102908,1000.);
#14847=VECTOR('',#102909,1000.);
#14848=VECTOR('',#102912,1000.);
#14849=VECTOR('',#102913,1000.);
#14850=VECTOR('',#102914,1000.);
#14851=VECTOR('',#102917,1000.);
#14852=VECTOR('',#102918,1000.);
#14853=VECTOR('',#102921,1000.);
#14854=VECTOR('',#102922,1000.);
#14855=VECTOR('',#102923,1000.);
#14856=VECTOR('',#102924,1000.);
#14857=VECTOR('',#102927,1000.);
#14858=VECTOR('',#102928,1000.);
#14859=VECTOR('',#102929,1000.);
#14860=VECTOR('',#102932,1000.);
#14861=VECTOR('',#102933,1000.);
#14862=VECTOR('',#102934,1000.);
#14863=VECTOR('',#102937,1000.);
#14864=VECTOR('',#102938,1000.);
#14865=VECTOR('',#102941,1000.);
#14866=VECTOR('',#102942,1000.);
#14867=VECTOR('',#102943,1000.);
#14868=VECTOR('',#102944,1000.);
#14869=VECTOR('',#102947,1000.);
#14870=VECTOR('',#102948,1000.);
#14871=VECTOR('',#102949,1000.);
#14872=VECTOR('',#102952,1000.);
#14873=VECTOR('',#102953,1000.);
#14874=VECTOR('',#102954,1000.);
#14875=VECTOR('',#102957,1000.);
#14876=VECTOR('',#102958,1000.);
#14877=VECTOR('',#102961,1000.);
#14878=VECTOR('',#102962,1000.);
#14879=VECTOR('',#102963,1000.);
#14880=VECTOR('',#102964,1000.);
#14881=VECTOR('',#102967,1000.);
#14882=VECTOR('',#102968,1000.);
#14883=VECTOR('',#102969,1000.);
#14884=VECTOR('',#102972,1000.);
#14885=VECTOR('',#102973,1000.);
#14886=VECTOR('',#102974,1000.);
#14887=VECTOR('',#102977,1000.);
#14888=VECTOR('',#102978,1000.);
#14889=VECTOR('',#102981,1000.);
#14890=VECTOR('',#102982,1000.);
#14891=VECTOR('',#102983,1000.);
#14892=VECTOR('',#102984,1000.);
#14893=VECTOR('',#102987,1000.);
#14894=VECTOR('',#102988,1000.);
#14895=VECTOR('',#102989,1000.);
#14896=VECTOR('',#102992,1000.);
#14897=VECTOR('',#102993,1000.);
#14898=VECTOR('',#102994,1000.);
#14899=VECTOR('',#102997,1000.);
#14900=VECTOR('',#102998,1000.);
#14901=VECTOR('',#103001,1000.);
#14902=VECTOR('',#103002,1000.);
#14903=VECTOR('',#103003,1000.);
#14904=VECTOR('',#103004,1000.);
#14905=VECTOR('',#103007,1000.);
#14906=VECTOR('',#103008,1000.);
#14907=VECTOR('',#103009,1000.);
#14908=VECTOR('',#103012,1000.);
#14909=VECTOR('',#103013,1000.);
#14910=VECTOR('',#103014,1000.);
#14911=VECTOR('',#103017,1000.);
#14912=VECTOR('',#103018,1000.);
#14913=VECTOR('',#103021,1000.);
#14914=VECTOR('',#103022,1000.);
#14915=VECTOR('',#103023,1000.);
#14916=VECTOR('',#103024,1000.);
#14917=VECTOR('',#103027,1000.);
#14918=VECTOR('',#103028,1000.);
#14919=VECTOR('',#103029,1000.);
#14920=VECTOR('',#103032,1000.);
#14921=VECTOR('',#103033,1000.);
#14922=VECTOR('',#103034,1000.);
#14923=VECTOR('',#103037,1000.);
#14924=VECTOR('',#103038,1000.);
#14925=VECTOR('',#103041,1000.);
#14926=VECTOR('',#103042,1000.);
#14927=VECTOR('',#103043,1000.);
#14928=VECTOR('',#103044,1000.);
#14929=VECTOR('',#103047,1000.);
#14930=VECTOR('',#103048,1000.);
#14931=VECTOR('',#103049,1000.);
#14932=VECTOR('',#103052,1000.);
#14933=VECTOR('',#103053,1000.);
#14934=VECTOR('',#103054,1000.);
#14935=VECTOR('',#103057,1000.);
#14936=VECTOR('',#103058,1000.);
#14937=VECTOR('',#103061,1000.);
#14938=VECTOR('',#103062,1000.);
#14939=VECTOR('',#103063,1000.);
#14940=VECTOR('',#103064,1000.);
#14941=VECTOR('',#103067,1000.);
#14942=VECTOR('',#103068,1000.);
#14943=VECTOR('',#103069,1000.);
#14944=VECTOR('',#103072,1000.);
#14945=VECTOR('',#103073,1000.);
#14946=VECTOR('',#103074,1000.);
#14947=VECTOR('',#103077,1000.);
#14948=VECTOR('',#103078,1000.);
#14949=VECTOR('',#103081,1000.);
#14950=VECTOR('',#103082,1000.);
#14951=VECTOR('',#103083,1000.);
#14952=VECTOR('',#103084,1000.);
#14953=VECTOR('',#103087,1000.);
#14954=VECTOR('',#103088,1000.);
#14955=VECTOR('',#103089,1000.);
#14956=VECTOR('',#103092,1000.);
#14957=VECTOR('',#103093,1000.);
#14958=VECTOR('',#103094,1000.);
#14959=VECTOR('',#103097,1000.);
#14960=VECTOR('',#103098,1000.);
#14961=VECTOR('',#103101,1000.);
#14962=VECTOR('',#103102,1000.);
#14963=VECTOR('',#103103,1000.);
#14964=VECTOR('',#103104,1000.);
#14965=VECTOR('',#103107,1000.);
#14966=VECTOR('',#103108,1000.);
#14967=VECTOR('',#103109,1000.);
#14968=VECTOR('',#103112,1000.);
#14969=VECTOR('',#103113,1000.);
#14970=VECTOR('',#103114,1000.);
#14971=VECTOR('',#103117,1000.);
#14972=VECTOR('',#103118,1000.);
#14973=VECTOR('',#103121,1000.);
#14974=VECTOR('',#103122,1000.);
#14975=VECTOR('',#103123,1000.);
#14976=VECTOR('',#103124,1000.);
#14977=VECTOR('',#103127,1000.);
#14978=VECTOR('',#103128,1000.);
#14979=VECTOR('',#103129,1000.);
#14980=VECTOR('',#103132,1000.);
#14981=VECTOR('',#103133,1000.);
#14982=VECTOR('',#103134,1000.);
#14983=VECTOR('',#103137,1000.);
#14984=VECTOR('',#103138,1000.);
#14985=VECTOR('',#103141,1000.);
#14986=VECTOR('',#103142,1000.);
#14987=VECTOR('',#103143,1000.);
#14988=VECTOR('',#103144,1000.);
#14989=VECTOR('',#103147,1000.);
#14990=VECTOR('',#103148,1000.);
#14991=VECTOR('',#103149,1000.);
#14992=VECTOR('',#103152,1000.);
#14993=VECTOR('',#103153,1000.);
#14994=VECTOR('',#103154,1000.);
#14995=VECTOR('',#103157,1000.);
#14996=VECTOR('',#103158,1000.);
#14997=VECTOR('',#103161,1000.);
#14998=VECTOR('',#103162,1000.);
#14999=VECTOR('',#103163,1000.);
#15000=VECTOR('',#103164,1000.);
#15001=VECTOR('',#103167,1000.);
#15002=VECTOR('',#103168,1000.);
#15003=VECTOR('',#103169,1000.);
#15004=VECTOR('',#103172,1000.);
#15005=VECTOR('',#103173,1000.);
#15006=VECTOR('',#103174,1000.);
#15007=VECTOR('',#103177,1000.);
#15008=VECTOR('',#103178,1000.);
#15009=VECTOR('',#103181,1000.);
#15010=VECTOR('',#103182,1000.);
#15011=VECTOR('',#103183,1000.);
#15012=VECTOR('',#103184,1000.);
#15013=VECTOR('',#103187,1000.);
#15014=VECTOR('',#103188,1000.);
#15015=VECTOR('',#103189,1000.);
#15016=VECTOR('',#103192,1000.);
#15017=VECTOR('',#103193,1000.);
#15018=VECTOR('',#103194,1000.);
#15019=VECTOR('',#103197,1000.);
#15020=VECTOR('',#103198,1000.);
#15021=VECTOR('',#103201,1000.);
#15022=VECTOR('',#103202,1000.);
#15023=VECTOR('',#103203,1000.);
#15024=VECTOR('',#103204,1000.);
#15025=VECTOR('',#103207,1000.);
#15026=VECTOR('',#103208,1000.);
#15027=VECTOR('',#103209,1000.);
#15028=VECTOR('',#103212,1000.);
#15029=VECTOR('',#103213,1000.);
#15030=VECTOR('',#103214,1000.);
#15031=VECTOR('',#103217,1000.);
#15032=VECTOR('',#103218,1000.);
#15033=VECTOR('',#103221,1000.);
#15034=VECTOR('',#103222,1000.);
#15035=VECTOR('',#103223,1000.);
#15036=VECTOR('',#103224,1000.);
#15037=VECTOR('',#103227,1000.);
#15038=VECTOR('',#103228,1000.);
#15039=VECTOR('',#103229,1000.);
#15040=VECTOR('',#103232,1000.);
#15041=VECTOR('',#103233,1000.);
#15042=VECTOR('',#103234,1000.);
#15043=VECTOR('',#103237,1000.);
#15044=VECTOR('',#103238,1000.);
#15045=VECTOR('',#103241,1000.);
#15046=VECTOR('',#103242,1000.);
#15047=VECTOR('',#103243,1000.);
#15048=VECTOR('',#103244,1000.);
#15049=VECTOR('',#103247,1000.);
#15050=VECTOR('',#103248,1000.);
#15051=VECTOR('',#103249,1000.);
#15052=VECTOR('',#103252,1000.);
#15053=VECTOR('',#103253,1000.);
#15054=VECTOR('',#103254,1000.);
#15055=VECTOR('',#103257,1000.);
#15056=VECTOR('',#103258,1000.);
#15057=VECTOR('',#103261,1000.);
#15058=VECTOR('',#103262,1000.);
#15059=VECTOR('',#103263,1000.);
#15060=VECTOR('',#103264,1000.);
#15061=VECTOR('',#103267,1000.);
#15062=VECTOR('',#103268,1000.);
#15063=VECTOR('',#103269,1000.);
#15064=VECTOR('',#103272,1000.);
#15065=VECTOR('',#103273,1000.);
#15066=VECTOR('',#103274,1000.);
#15067=VECTOR('',#103277,1000.);
#15068=VECTOR('',#103278,1000.);
#15069=VECTOR('',#103281,1000.);
#15070=VECTOR('',#103282,1000.);
#15071=VECTOR('',#103283,1000.);
#15072=VECTOR('',#103284,1000.);
#15073=VECTOR('',#103287,1000.);
#15074=VECTOR('',#103288,1000.);
#15075=VECTOR('',#103289,1000.);
#15076=VECTOR('',#103292,1000.);
#15077=VECTOR('',#103293,1000.);
#15078=VECTOR('',#103294,1000.);
#15079=VECTOR('',#103297,1000.);
#15080=VECTOR('',#103298,1000.);
#15081=VECTOR('',#103301,1000.);
#15082=VECTOR('',#103302,1000.);
#15083=VECTOR('',#103303,1000.);
#15084=VECTOR('',#103304,1000.);
#15085=VECTOR('',#103307,1000.);
#15086=VECTOR('',#103308,1000.);
#15087=VECTOR('',#103309,1000.);
#15088=VECTOR('',#103312,1000.);
#15089=VECTOR('',#103313,1000.);
#15090=VECTOR('',#103314,1000.);
#15091=VECTOR('',#103317,1000.);
#15092=VECTOR('',#103318,1000.);
#15093=VECTOR('',#103321,1000.);
#15094=VECTOR('',#103322,1000.);
#15095=VECTOR('',#103323,1000.);
#15096=VECTOR('',#103324,1000.);
#15097=VECTOR('',#103327,1000.);
#15098=VECTOR('',#103328,1000.);
#15099=VECTOR('',#103329,1000.);
#15100=VECTOR('',#103332,1000.);
#15101=VECTOR('',#103333,1000.);
#15102=VECTOR('',#103334,1000.);
#15103=VECTOR('',#103337,1000.);
#15104=VECTOR('',#103338,1000.);
#15105=VECTOR('',#103341,1000.);
#15106=VECTOR('',#103342,1000.);
#15107=VECTOR('',#103343,1000.);
#15108=VECTOR('',#103344,1000.);
#15109=VECTOR('',#103347,1000.);
#15110=VECTOR('',#103348,1000.);
#15111=VECTOR('',#103349,1000.);
#15112=VECTOR('',#103352,1000.);
#15113=VECTOR('',#103353,1000.);
#15114=VECTOR('',#103354,1000.);
#15115=VECTOR('',#103357,1000.);
#15116=VECTOR('',#103358,1000.);
#15117=VECTOR('',#103361,1000.);
#15118=VECTOR('',#103362,1000.);
#15119=VECTOR('',#103363,1000.);
#15120=VECTOR('',#103364,1000.);
#15121=VECTOR('',#103367,1000.);
#15122=VECTOR('',#103368,1000.);
#15123=VECTOR('',#103369,1000.);
#15124=VECTOR('',#103372,1000.);
#15125=VECTOR('',#103373,1000.);
#15126=VECTOR('',#103374,1000.);
#15127=VECTOR('',#103377,1000.);
#15128=VECTOR('',#103378,1000.);
#15129=VECTOR('',#103381,1000.);
#15130=VECTOR('',#103382,1000.);
#15131=VECTOR('',#103383,1000.);
#15132=VECTOR('',#103384,1000.);
#15133=VECTOR('',#103387,1000.);
#15134=VECTOR('',#103388,1000.);
#15135=VECTOR('',#103389,1000.);
#15136=VECTOR('',#103392,1000.);
#15137=VECTOR('',#103393,1000.);
#15138=VECTOR('',#103394,1000.);
#15139=VECTOR('',#103397,1000.);
#15140=VECTOR('',#103398,1000.);
#15141=VECTOR('',#103401,1000.);
#15142=VECTOR('',#103402,1000.);
#15143=VECTOR('',#103403,1000.);
#15144=VECTOR('',#103404,1000.);
#15145=VECTOR('',#103407,1000.);
#15146=VECTOR('',#103408,1000.);
#15147=VECTOR('',#103409,1000.);
#15148=VECTOR('',#103412,1000.);
#15149=VECTOR('',#103413,1000.);
#15150=VECTOR('',#103414,1000.);
#15151=VECTOR('',#103417,1000.);
#15152=VECTOR('',#103418,1000.);
#15153=VECTOR('',#103421,1000.);
#15154=VECTOR('',#103422,1000.);
#15155=VECTOR('',#103423,1000.);
#15156=VECTOR('',#103424,1000.);
#15157=VECTOR('',#103427,1000.);
#15158=VECTOR('',#103428,1000.);
#15159=VECTOR('',#103429,1000.);
#15160=VECTOR('',#103432,1000.);
#15161=VECTOR('',#103433,1000.);
#15162=VECTOR('',#103434,1000.);
#15163=VECTOR('',#103437,1000.);
#15164=VECTOR('',#103438,1000.);
#15165=VECTOR('',#103441,1000.);
#15166=VECTOR('',#103442,1000.);
#15167=VECTOR('',#103443,1000.);
#15168=VECTOR('',#103444,1000.);
#15169=VECTOR('',#103447,1000.);
#15170=VECTOR('',#103448,1000.);
#15171=VECTOR('',#103449,1000.);
#15172=VECTOR('',#103452,1000.);
#15173=VECTOR('',#103453,1000.);
#15174=VECTOR('',#103454,1000.);
#15175=VECTOR('',#103457,1000.);
#15176=VECTOR('',#103458,1000.);
#15177=VECTOR('',#103461,1000.);
#15178=VECTOR('',#103462,1000.);
#15179=VECTOR('',#103463,1000.);
#15180=VECTOR('',#103464,1000.);
#15181=VECTOR('',#103467,1000.);
#15182=VECTOR('',#103468,1000.);
#15183=VECTOR('',#103469,1000.);
#15184=VECTOR('',#103472,1000.);
#15185=VECTOR('',#103473,1000.);
#15186=VECTOR('',#103474,1000.);
#15187=VECTOR('',#103477,1000.);
#15188=VECTOR('',#103478,1000.);
#15189=VECTOR('',#103481,1000.);
#15190=VECTOR('',#103482,1000.);
#15191=VECTOR('',#103483,1000.);
#15192=VECTOR('',#103484,1000.);
#15193=VECTOR('',#103487,1000.);
#15194=VECTOR('',#103488,1000.);
#15195=VECTOR('',#103489,1000.);
#15196=VECTOR('',#103492,1000.);
#15197=VECTOR('',#103493,1000.);
#15198=VECTOR('',#103494,1000.);
#15199=VECTOR('',#103497,1000.);
#15200=VECTOR('',#103498,1000.);
#15201=VECTOR('',#103501,1000.);
#15202=VECTOR('',#103502,1000.);
#15203=VECTOR('',#103503,1000.);
#15204=VECTOR('',#103504,1000.);
#15205=VECTOR('',#103507,1000.);
#15206=VECTOR('',#103508,1000.);
#15207=VECTOR('',#103509,1000.);
#15208=VECTOR('',#103512,1000.);
#15209=VECTOR('',#103513,1000.);
#15210=VECTOR('',#103514,1000.);
#15211=VECTOR('',#103517,1000.);
#15212=VECTOR('',#103518,1000.);
#15213=VECTOR('',#103521,1000.);
#15214=VECTOR('',#103522,1000.);
#15215=VECTOR('',#103523,1000.);
#15216=VECTOR('',#103524,1000.);
#15217=VECTOR('',#103527,1000.);
#15218=VECTOR('',#103528,1000.);
#15219=VECTOR('',#103529,1000.);
#15220=VECTOR('',#103532,1000.);
#15221=VECTOR('',#103533,1000.);
#15222=VECTOR('',#103534,1000.);
#15223=VECTOR('',#103537,1000.);
#15224=VECTOR('',#103538,1000.);
#15225=VECTOR('',#103541,1000.);
#15226=VECTOR('',#103542,1000.);
#15227=VECTOR('',#103543,1000.);
#15228=VECTOR('',#103544,1000.);
#15229=VECTOR('',#103547,1000.);
#15230=VECTOR('',#103548,1000.);
#15231=VECTOR('',#103549,1000.);
#15232=VECTOR('',#103552,1000.);
#15233=VECTOR('',#103553,1000.);
#15234=VECTOR('',#103554,1000.);
#15235=VECTOR('',#103557,1000.);
#15236=VECTOR('',#103558,1000.);
#15237=VECTOR('',#103561,1000.);
#15238=VECTOR('',#103562,1000.);
#15239=VECTOR('',#103563,1000.);
#15240=VECTOR('',#103564,1000.);
#15241=VECTOR('',#103567,1000.);
#15242=VECTOR('',#103568,1000.);
#15243=VECTOR('',#103569,1000.);
#15244=VECTOR('',#103572,1000.);
#15245=VECTOR('',#103573,1000.);
#15246=VECTOR('',#103574,1000.);
#15247=VECTOR('',#103577,1000.);
#15248=VECTOR('',#103578,1000.);
#15249=VECTOR('',#103581,1000.);
#15250=VECTOR('',#103582,1000.);
#15251=VECTOR('',#103583,1000.);
#15252=VECTOR('',#103584,1000.);
#15253=VECTOR('',#103587,1000.);
#15254=VECTOR('',#103588,1000.);
#15255=VECTOR('',#103589,1000.);
#15256=VECTOR('',#103592,1000.);
#15257=VECTOR('',#103593,1000.);
#15258=VECTOR('',#103594,1000.);
#15259=VECTOR('',#103597,1000.);
#15260=VECTOR('',#103598,1000.);
#15261=VECTOR('',#103601,1000.);
#15262=VECTOR('',#103602,1000.);
#15263=VECTOR('',#103603,1000.);
#15264=VECTOR('',#103604,1000.);
#15265=VECTOR('',#103607,1000.);
#15266=VECTOR('',#103608,1000.);
#15267=VECTOR('',#103609,1000.);
#15268=VECTOR('',#103612,1000.);
#15269=VECTOR('',#103613,1000.);
#15270=VECTOR('',#103614,1000.);
#15271=VECTOR('',#103617,1000.);
#15272=VECTOR('',#103618,1000.);
#15273=VECTOR('',#103621,1000.);
#15274=VECTOR('',#103622,1000.);
#15275=VECTOR('',#103623,1000.);
#15276=VECTOR('',#103624,1000.);
#15277=VECTOR('',#103627,1000.);
#15278=VECTOR('',#103628,1000.);
#15279=VECTOR('',#103629,1000.);
#15280=VECTOR('',#103632,1000.);
#15281=VECTOR('',#103633,1000.);
#15282=VECTOR('',#103634,1000.);
#15283=VECTOR('',#103637,1000.);
#15284=VECTOR('',#103638,1000.);
#15285=VECTOR('',#103641,1000.);
#15286=VECTOR('',#103642,1000.);
#15287=VECTOR('',#103643,1000.);
#15288=VECTOR('',#103644,1000.);
#15289=VECTOR('',#103647,1000.);
#15290=VECTOR('',#103648,1000.);
#15291=VECTOR('',#103649,1000.);
#15292=VECTOR('',#103652,1000.);
#15293=VECTOR('',#103653,1000.);
#15294=VECTOR('',#103654,1000.);
#15295=VECTOR('',#103657,1000.);
#15296=VECTOR('',#103658,1000.);
#15297=VECTOR('',#103661,1000.);
#15298=VECTOR('',#103662,1000.);
#15299=VECTOR('',#103663,1000.);
#15300=VECTOR('',#103664,1000.);
#15301=VECTOR('',#103667,1000.);
#15302=VECTOR('',#103668,1000.);
#15303=VECTOR('',#103669,1000.);
#15304=VECTOR('',#103672,1000.);
#15305=VECTOR('',#103673,1000.);
#15306=VECTOR('',#103674,1000.);
#15307=VECTOR('',#103677,1000.);
#15308=VECTOR('',#103678,1000.);
#15309=VECTOR('',#103681,1000.);
#15310=VECTOR('',#103682,1000.);
#15311=VECTOR('',#103683,1000.);
#15312=VECTOR('',#103684,1000.);
#15313=VECTOR('',#103687,1000.);
#15314=VECTOR('',#103688,1000.);
#15315=VECTOR('',#103689,1000.);
#15316=VECTOR('',#103692,1000.);
#15317=VECTOR('',#103693,1000.);
#15318=VECTOR('',#103694,1000.);
#15319=VECTOR('',#103697,1000.);
#15320=VECTOR('',#103698,1000.);
#15321=VECTOR('',#103701,1000.);
#15322=VECTOR('',#103702,1000.);
#15323=VECTOR('',#103703,1000.);
#15324=VECTOR('',#103704,1000.);
#15325=VECTOR('',#103707,1000.);
#15326=VECTOR('',#103708,1000.);
#15327=VECTOR('',#103709,1000.);
#15328=VECTOR('',#103712,1000.);
#15329=VECTOR('',#103713,1000.);
#15330=VECTOR('',#103714,1000.);
#15331=VECTOR('',#103717,1000.);
#15332=VECTOR('',#103718,1000.);
#15333=VECTOR('',#103721,1000.);
#15334=VECTOR('',#103722,1000.);
#15335=VECTOR('',#103723,1000.);
#15336=VECTOR('',#103724,1000.);
#15337=VECTOR('',#103727,1000.);
#15338=VECTOR('',#103728,1000.);
#15339=VECTOR('',#103729,1000.);
#15340=VECTOR('',#103732,1000.);
#15341=VECTOR('',#103733,1000.);
#15342=VECTOR('',#103734,1000.);
#15343=VECTOR('',#103737,1000.);
#15344=VECTOR('',#103738,1000.);
#15345=VECTOR('',#103741,1000.);
#15346=VECTOR('',#103742,1000.);
#15347=VECTOR('',#103743,1000.);
#15348=VECTOR('',#103744,1000.);
#15349=VECTOR('',#103747,1000.);
#15350=VECTOR('',#103748,1000.);
#15351=VECTOR('',#103749,1000.);
#15352=VECTOR('',#103752,1000.);
#15353=VECTOR('',#103753,1000.);
#15354=VECTOR('',#103754,1000.);
#15355=VECTOR('',#103757,1000.);
#15356=VECTOR('',#103758,1000.);
#15357=VECTOR('',#103761,1000.);
#15358=VECTOR('',#103762,1000.);
#15359=VECTOR('',#103763,1000.);
#15360=VECTOR('',#103764,1000.);
#15361=VECTOR('',#103767,1000.);
#15362=VECTOR('',#103768,1000.);
#15363=VECTOR('',#103769,1000.);
#15364=VECTOR('',#103772,1000.);
#15365=VECTOR('',#103773,1000.);
#15366=VECTOR('',#103774,1000.);
#15367=VECTOR('',#103777,1000.);
#15368=VECTOR('',#103778,1000.);
#15369=VECTOR('',#103781,1000.);
#15370=VECTOR('',#103782,1000.);
#15371=VECTOR('',#103783,1000.);
#15372=VECTOR('',#103784,1000.);
#15373=VECTOR('',#103787,1000.);
#15374=VECTOR('',#103788,1000.);
#15375=VECTOR('',#103789,1000.);
#15376=VECTOR('',#103792,1000.);
#15377=VECTOR('',#103793,1000.);
#15378=VECTOR('',#103794,1000.);
#15379=VECTOR('',#103797,1000.);
#15380=VECTOR('',#103798,1000.);
#15381=VECTOR('',#103801,1000.);
#15382=VECTOR('',#103802,1000.);
#15383=VECTOR('',#103803,1000.);
#15384=VECTOR('',#103804,1000.);
#15385=VECTOR('',#103807,1000.);
#15386=VECTOR('',#103808,1000.);
#15387=VECTOR('',#103809,1000.);
#15388=VECTOR('',#103812,1000.);
#15389=VECTOR('',#103813,1000.);
#15390=VECTOR('',#103814,1000.);
#15391=VECTOR('',#103817,1000.);
#15392=VECTOR('',#103818,1000.);
#15393=VECTOR('',#103821,1000.);
#15394=VECTOR('',#103822,1000.);
#15395=VECTOR('',#103823,1000.);
#15396=VECTOR('',#103824,1000.);
#15397=VECTOR('',#103827,1000.);
#15398=VECTOR('',#103828,1000.);
#15399=VECTOR('',#103829,1000.);
#15400=VECTOR('',#103832,1000.);
#15401=VECTOR('',#103833,1000.);
#15402=VECTOR('',#103834,1000.);
#15403=VECTOR('',#103837,1000.);
#15404=VECTOR('',#103838,1000.);
#15405=VECTOR('',#103841,1000.);
#15406=VECTOR('',#103842,1000.);
#15407=VECTOR('',#103843,1000.);
#15408=VECTOR('',#103844,1000.);
#15409=VECTOR('',#103847,1000.);
#15410=VECTOR('',#103848,1000.);
#15411=VECTOR('',#103849,1000.);
#15412=VECTOR('',#103852,1000.);
#15413=VECTOR('',#103853,1000.);
#15414=VECTOR('',#103854,1000.);
#15415=VECTOR('',#103857,1000.);
#15416=VECTOR('',#103858,1000.);
#15417=VECTOR('',#103861,1000.);
#15418=VECTOR('',#103862,1000.);
#15419=VECTOR('',#103863,1000.);
#15420=VECTOR('',#103864,1000.);
#15421=VECTOR('',#103867,1000.);
#15422=VECTOR('',#103868,1000.);
#15423=VECTOR('',#103869,1000.);
#15424=VECTOR('',#103872,1000.);
#15425=VECTOR('',#103873,1000.);
#15426=VECTOR('',#103874,1000.);
#15427=VECTOR('',#103877,1000.);
#15428=VECTOR('',#103878,1000.);
#15429=VECTOR('',#103881,1000.);
#15430=VECTOR('',#103882,1000.);
#15431=VECTOR('',#103883,1000.);
#15432=VECTOR('',#103884,1000.);
#15433=VECTOR('',#103887,1000.);
#15434=VECTOR('',#103888,1000.);
#15435=VECTOR('',#103889,1000.);
#15436=VECTOR('',#103892,1000.);
#15437=VECTOR('',#103893,1000.);
#15438=VECTOR('',#103894,1000.);
#15439=VECTOR('',#103897,1000.);
#15440=VECTOR('',#103898,1000.);
#15441=VECTOR('',#103901,1000.);
#15442=VECTOR('',#103902,1000.);
#15443=VECTOR('',#103903,1000.);
#15444=VECTOR('',#103904,1000.);
#15445=VECTOR('',#103907,1000.);
#15446=VECTOR('',#103908,1000.);
#15447=VECTOR('',#103909,1000.);
#15448=VECTOR('',#103912,1000.);
#15449=VECTOR('',#103913,1000.);
#15450=VECTOR('',#103914,1000.);
#15451=VECTOR('',#103917,1000.);
#15452=VECTOR('',#103918,1000.);
#15453=VECTOR('',#103921,1000.);
#15454=VECTOR('',#103922,1000.);
#15455=VECTOR('',#103923,1000.);
#15456=VECTOR('',#103924,1000.);
#15457=VECTOR('',#103927,1000.);
#15458=VECTOR('',#103928,1000.);
#15459=VECTOR('',#103929,1000.);
#15460=VECTOR('',#103932,1000.);
#15461=VECTOR('',#103933,1000.);
#15462=VECTOR('',#103934,1000.);
#15463=VECTOR('',#103937,1000.);
#15464=VECTOR('',#103938,1000.);
#15465=VECTOR('',#103941,1000.);
#15466=VECTOR('',#103942,1000.);
#15467=VECTOR('',#103943,1000.);
#15468=VECTOR('',#103944,1000.);
#15469=VECTOR('',#103947,1000.);
#15470=VECTOR('',#103948,1000.);
#15471=VECTOR('',#103949,1000.);
#15472=VECTOR('',#103952,1000.);
#15473=VECTOR('',#103953,1000.);
#15474=VECTOR('',#103954,1000.);
#15475=VECTOR('',#103957,1000.);
#15476=VECTOR('',#103958,1000.);
#15477=VECTOR('',#103961,1000.);
#15478=VECTOR('',#103962,1000.);
#15479=VECTOR('',#103963,1000.);
#15480=VECTOR('',#103964,1000.);
#15481=VECTOR('',#103967,1000.);
#15482=VECTOR('',#103968,1000.);
#15483=VECTOR('',#103969,1000.);
#15484=VECTOR('',#103972,1000.);
#15485=VECTOR('',#103973,1000.);
#15486=VECTOR('',#103974,1000.);
#15487=VECTOR('',#103977,1000.);
#15488=VECTOR('',#103978,1000.);
#15489=VECTOR('',#103981,1000.);
#15490=VECTOR('',#103982,1000.);
#15491=VECTOR('',#103983,1000.);
#15492=VECTOR('',#103984,1000.);
#15493=VECTOR('',#103987,1000.);
#15494=VECTOR('',#103988,1000.);
#15495=VECTOR('',#103989,1000.);
#15496=VECTOR('',#103992,1000.);
#15497=VECTOR('',#103993,1000.);
#15498=VECTOR('',#103994,1000.);
#15499=VECTOR('',#103997,1000.);
#15500=VECTOR('',#103998,1000.);
#15501=VECTOR('',#104001,1000.);
#15502=VECTOR('',#104002,1000.);
#15503=VECTOR('',#104003,1000.);
#15504=VECTOR('',#104004,1000.);
#15505=VECTOR('',#104007,1000.);
#15506=VECTOR('',#104008,1000.);
#15507=VECTOR('',#104009,1000.);
#15508=VECTOR('',#104012,1000.);
#15509=VECTOR('',#104013,1000.);
#15510=VECTOR('',#104014,1000.);
#15511=VECTOR('',#104017,1000.);
#15512=VECTOR('',#104018,1000.);
#15513=VECTOR('',#104021,1000.);
#15514=VECTOR('',#104022,1000.);
#15515=VECTOR('',#104023,1000.);
#15516=VECTOR('',#104024,1000.);
#15517=VECTOR('',#104027,1000.);
#15518=VECTOR('',#104028,1000.);
#15519=VECTOR('',#104029,1000.);
#15520=VECTOR('',#104032,1000.);
#15521=VECTOR('',#104033,1000.);
#15522=VECTOR('',#104034,1000.);
#15523=VECTOR('',#104037,1000.);
#15524=VECTOR('',#104038,1000.);
#15525=VECTOR('',#104041,1000.);
#15526=VECTOR('',#104042,1000.);
#15527=VECTOR('',#104043,1000.);
#15528=VECTOR('',#104044,1000.);
#15529=VECTOR('',#104047,1000.);
#15530=VECTOR('',#104048,1000.);
#15531=VECTOR('',#104049,1000.);
#15532=VECTOR('',#104052,1000.);
#15533=VECTOR('',#104053,1000.);
#15534=VECTOR('',#104054,1000.);
#15535=VECTOR('',#104057,1000.);
#15536=VECTOR('',#104058,1000.);
#15537=VECTOR('',#104061,1000.);
#15538=VECTOR('',#104062,1000.);
#15539=VECTOR('',#104063,1000.);
#15540=VECTOR('',#104064,1000.);
#15541=VECTOR('',#104067,1000.);
#15542=VECTOR('',#104068,1000.);
#15543=VECTOR('',#104069,1000.);
#15544=VECTOR('',#104072,1000.);
#15545=VECTOR('',#104073,1000.);
#15546=VECTOR('',#104074,1000.);
#15547=VECTOR('',#104077,1000.);
#15548=VECTOR('',#104078,1000.);
#15549=VECTOR('',#104081,1000.);
#15550=VECTOR('',#104082,1000.);
#15551=VECTOR('',#104083,1000.);
#15552=VECTOR('',#104084,1000.);
#15553=VECTOR('',#104087,1000.);
#15554=VECTOR('',#104088,1000.);
#15555=VECTOR('',#104089,1000.);
#15556=VECTOR('',#104092,1000.);
#15557=VECTOR('',#104093,1000.);
#15558=VECTOR('',#104094,1000.);
#15559=VECTOR('',#104097,1000.);
#15560=VECTOR('',#104098,1000.);
#15561=VECTOR('',#104101,1000.);
#15562=VECTOR('',#104102,1000.);
#15563=VECTOR('',#104103,1000.);
#15564=VECTOR('',#104104,1000.);
#15565=VECTOR('',#104107,1000.);
#15566=VECTOR('',#104108,1000.);
#15567=VECTOR('',#104109,1000.);
#15568=VECTOR('',#104112,1000.);
#15569=VECTOR('',#104113,1000.);
#15570=VECTOR('',#104114,1000.);
#15571=VECTOR('',#104117,1000.);
#15572=VECTOR('',#104118,1000.);
#15573=VECTOR('',#104121,1000.);
#15574=VECTOR('',#104122,1000.);
#15575=VECTOR('',#104123,1000.);
#15576=VECTOR('',#104124,1000.);
#15577=VECTOR('',#104127,1000.);
#15578=VECTOR('',#104128,1000.);
#15579=VECTOR('',#104129,1000.);
#15580=VECTOR('',#104132,1000.);
#15581=VECTOR('',#104133,1000.);
#15582=VECTOR('',#104134,1000.);
#15583=VECTOR('',#104137,1000.);
#15584=VECTOR('',#104138,1000.);
#15585=VECTOR('',#104141,1000.);
#15586=VECTOR('',#104142,1000.);
#15587=VECTOR('',#104143,1000.);
#15588=VECTOR('',#104144,1000.);
#15589=VECTOR('',#104147,1000.);
#15590=VECTOR('',#104148,1000.);
#15591=VECTOR('',#104149,1000.);
#15592=VECTOR('',#104152,1000.);
#15593=VECTOR('',#104153,1000.);
#15594=VECTOR('',#104154,1000.);
#15595=VECTOR('',#104157,1000.);
#15596=VECTOR('',#104158,1000.);
#15597=VECTOR('',#104161,1000.);
#15598=VECTOR('',#104162,1000.);
#15599=VECTOR('',#104163,1000.);
#15600=VECTOR('',#104164,1000.);
#15601=VECTOR('',#104167,1000.);
#15602=VECTOR('',#104168,1000.);
#15603=VECTOR('',#104169,1000.);
#15604=VECTOR('',#104172,1000.);
#15605=VECTOR('',#104173,1000.);
#15606=VECTOR('',#104174,1000.);
#15607=VECTOR('',#104177,1000.);
#15608=VECTOR('',#104178,1000.);
#15609=VECTOR('',#104181,1000.);
#15610=VECTOR('',#104182,1000.);
#15611=VECTOR('',#104183,1000.);
#15612=VECTOR('',#104184,1000.);
#15613=VECTOR('',#104187,1000.);
#15614=VECTOR('',#104188,1000.);
#15615=VECTOR('',#104189,1000.);
#15616=VECTOR('',#104192,1000.);
#15617=VECTOR('',#104193,1000.);
#15618=VECTOR('',#104194,1000.);
#15619=VECTOR('',#104197,1000.);
#15620=VECTOR('',#104198,1000.);
#15621=VECTOR('',#104201,1000.);
#15622=VECTOR('',#104202,1000.);
#15623=VECTOR('',#104203,1000.);
#15624=VECTOR('',#104204,1000.);
#15625=VECTOR('',#104207,1000.);
#15626=VECTOR('',#104208,1000.);
#15627=VECTOR('',#104209,1000.);
#15628=VECTOR('',#104212,1000.);
#15629=VECTOR('',#104213,1000.);
#15630=VECTOR('',#104214,1000.);
#15631=VECTOR('',#104217,1000.);
#15632=VECTOR('',#104218,1000.);
#15633=VECTOR('',#104221,1000.);
#15634=VECTOR('',#104222,1000.);
#15635=VECTOR('',#104223,1000.);
#15636=VECTOR('',#104224,1000.);
#15637=VECTOR('',#104227,1000.);
#15638=VECTOR('',#104228,1000.);
#15639=VECTOR('',#104229,1000.);
#15640=VECTOR('',#104232,1000.);
#15641=VECTOR('',#104233,1000.);
#15642=VECTOR('',#104234,1000.);
#15643=VECTOR('',#104237,1000.);
#15644=VECTOR('',#104238,1000.);
#15645=VECTOR('',#104241,1000.);
#15646=VECTOR('',#104242,1000.);
#15647=VECTOR('',#104243,1000.);
#15648=VECTOR('',#104244,1000.);
#15649=VECTOR('',#104247,1000.);
#15650=VECTOR('',#104248,1000.);
#15651=VECTOR('',#104249,1000.);
#15652=VECTOR('',#104252,1000.);
#15653=VECTOR('',#104253,1000.);
#15654=VECTOR('',#104254,1000.);
#15655=VECTOR('',#104257,1000.);
#15656=VECTOR('',#104258,1000.);
#15657=VECTOR('',#104261,1000.);
#15658=VECTOR('',#104262,1000.);
#15659=VECTOR('',#104263,1000.);
#15660=VECTOR('',#104264,1000.);
#15661=VECTOR('',#104267,1000.);
#15662=VECTOR('',#104268,1000.);
#15663=VECTOR('',#104269,1000.);
#15664=VECTOR('',#104272,1000.);
#15665=VECTOR('',#104273,1000.);
#15666=VECTOR('',#104274,1000.);
#15667=VECTOR('',#104277,1000.);
#15668=VECTOR('',#104278,1000.);
#15669=VECTOR('',#104281,1000.);
#15670=VECTOR('',#104282,1000.);
#15671=VECTOR('',#104283,1000.);
#15672=VECTOR('',#104284,1000.);
#15673=VECTOR('',#104287,1000.);
#15674=VECTOR('',#104288,1000.);
#15675=VECTOR('',#104289,1000.);
#15676=VECTOR('',#104292,1000.);
#15677=VECTOR('',#104293,1000.);
#15678=VECTOR('',#104294,1000.);
#15679=VECTOR('',#104297,1000.);
#15680=VECTOR('',#104298,1000.);
#15681=VECTOR('',#104301,1000.);
#15682=VECTOR('',#104302,1000.);
#15683=VECTOR('',#104303,1000.);
#15684=VECTOR('',#104304,1000.);
#15685=VECTOR('',#104307,1000.);
#15686=VECTOR('',#104308,1000.);
#15687=VECTOR('',#104309,1000.);
#15688=VECTOR('',#104312,1000.);
#15689=VECTOR('',#104313,1000.);
#15690=VECTOR('',#104314,1000.);
#15691=VECTOR('',#104317,1000.);
#15692=VECTOR('',#104318,1000.);
#15693=VECTOR('',#104321,1000.);
#15694=VECTOR('',#104322,1000.);
#15695=VECTOR('',#104323,1000.);
#15696=VECTOR('',#104324,1000.);
#15697=VECTOR('',#104327,1000.);
#15698=VECTOR('',#104328,1000.);
#15699=VECTOR('',#104329,1000.);
#15700=VECTOR('',#104332,1000.);
#15701=VECTOR('',#104333,1000.);
#15702=VECTOR('',#104334,1000.);
#15703=VECTOR('',#104337,1000.);
#15704=VECTOR('',#104338,1000.);
#15705=VECTOR('',#104341,1000.);
#15706=VECTOR('',#104342,1000.);
#15707=VECTOR('',#104343,1000.);
#15708=VECTOR('',#104344,1000.);
#15709=VECTOR('',#104347,1000.);
#15710=VECTOR('',#104348,1000.);
#15711=VECTOR('',#104349,1000.);
#15712=VECTOR('',#104352,1000.);
#15713=VECTOR('',#104353,1000.);
#15714=VECTOR('',#104354,1000.);
#15715=VECTOR('',#104357,1000.);
#15716=VECTOR('',#104358,1000.);
#15717=VECTOR('',#104361,1000.);
#15718=VECTOR('',#104362,1000.);
#15719=VECTOR('',#104363,1000.);
#15720=VECTOR('',#104364,1000.);
#15721=VECTOR('',#104367,1000.);
#15722=VECTOR('',#104368,1000.);
#15723=VECTOR('',#104369,1000.);
#15724=VECTOR('',#104372,1000.);
#15725=VECTOR('',#104373,1000.);
#15726=VECTOR('',#104374,1000.);
#15727=VECTOR('',#104377,1000.);
#15728=VECTOR('',#104378,1000.);
#15729=VECTOR('',#104381,1000.);
#15730=VECTOR('',#104382,1000.);
#15731=VECTOR('',#104383,1000.);
#15732=VECTOR('',#104384,1000.);
#15733=VECTOR('',#104387,1000.);
#15734=VECTOR('',#104388,1000.);
#15735=VECTOR('',#104389,1000.);
#15736=VECTOR('',#104392,1000.);
#15737=VECTOR('',#104393,1000.);
#15738=VECTOR('',#104394,1000.);
#15739=VECTOR('',#104397,1000.);
#15740=VECTOR('',#104398,1000.);
#15741=VECTOR('',#104401,1000.);
#15742=VECTOR('',#104402,1000.);
#15743=VECTOR('',#104403,1000.);
#15744=VECTOR('',#104404,1000.);
#15745=VECTOR('',#104407,1000.);
#15746=VECTOR('',#104408,1000.);
#15747=VECTOR('',#104409,1000.);
#15748=VECTOR('',#104412,1000.);
#15749=VECTOR('',#104413,1000.);
#15750=VECTOR('',#104414,1000.);
#15751=VECTOR('',#104417,1000.);
#15752=VECTOR('',#104418,1000.);
#15753=VECTOR('',#104421,1000.);
#15754=VECTOR('',#104422,1000.);
#15755=VECTOR('',#104423,1000.);
#15756=VECTOR('',#104424,1000.);
#15757=VECTOR('',#104427,1000.);
#15758=VECTOR('',#104428,1000.);
#15759=VECTOR('',#104429,1000.);
#15760=VECTOR('',#104432,1000.);
#15761=VECTOR('',#104433,1000.);
#15762=VECTOR('',#104434,1000.);
#15763=VECTOR('',#104437,1000.);
#15764=VECTOR('',#104438,1000.);
#15765=VECTOR('',#104441,1000.);
#15766=VECTOR('',#104442,1000.);
#15767=VECTOR('',#104443,1000.);
#15768=VECTOR('',#104444,1000.);
#15769=VECTOR('',#104447,1000.);
#15770=VECTOR('',#104448,1000.);
#15771=VECTOR('',#104449,1000.);
#15772=VECTOR('',#104452,1000.);
#15773=VECTOR('',#104453,1000.);
#15774=VECTOR('',#104454,1000.);
#15775=VECTOR('',#104457,1000.);
#15776=VECTOR('',#104458,1000.);
#15777=VECTOR('',#104461,1000.);
#15778=VECTOR('',#104462,1000.);
#15779=VECTOR('',#104463,1000.);
#15780=VECTOR('',#104464,1000.);
#15781=VECTOR('',#104467,1000.);
#15782=VECTOR('',#104468,1000.);
#15783=VECTOR('',#104469,1000.);
#15784=VECTOR('',#104472,1000.);
#15785=VECTOR('',#104473,1000.);
#15786=VECTOR('',#104474,1000.);
#15787=VECTOR('',#104477,1000.);
#15788=VECTOR('',#104478,1000.);
#15789=VECTOR('',#104481,1000.);
#15790=VECTOR('',#104482,1000.);
#15791=VECTOR('',#104483,1000.);
#15792=VECTOR('',#104484,1000.);
#15793=VECTOR('',#104487,1000.);
#15794=VECTOR('',#104488,1000.);
#15795=VECTOR('',#104489,1000.);
#15796=VECTOR('',#104492,1000.);
#15797=VECTOR('',#104493,1000.);
#15798=VECTOR('',#104494,1000.);
#15799=VECTOR('',#104497,1000.);
#15800=VECTOR('',#104498,1000.);
#15801=VECTOR('',#104501,1000.);
#15802=VECTOR('',#104502,1000.);
#15803=VECTOR('',#104503,1000.);
#15804=VECTOR('',#104504,1000.);
#15805=VECTOR('',#104507,1000.);
#15806=VECTOR('',#104508,1000.);
#15807=VECTOR('',#104509,1000.);
#15808=VECTOR('',#104512,1000.);
#15809=VECTOR('',#104513,1000.);
#15810=VECTOR('',#104514,1000.);
#15811=VECTOR('',#104517,1000.);
#15812=VECTOR('',#104518,1000.);
#15813=VECTOR('',#104521,1000.);
#15814=VECTOR('',#104522,1000.);
#15815=VECTOR('',#104523,1000.);
#15816=VECTOR('',#104524,1000.);
#15817=VECTOR('',#104527,1000.);
#15818=VECTOR('',#104528,1000.);
#15819=VECTOR('',#104529,1000.);
#15820=VECTOR('',#104532,1000.);
#15821=VECTOR('',#104533,1000.);
#15822=VECTOR('',#104534,1000.);
#15823=VECTOR('',#104537,1000.);
#15824=VECTOR('',#104538,1000.);
#15825=VECTOR('',#104541,1000.);
#15826=VECTOR('',#104542,1000.);
#15827=VECTOR('',#104543,1000.);
#15828=VECTOR('',#104544,1000.);
#15829=VECTOR('',#104547,1000.);
#15830=VECTOR('',#104548,1000.);
#15831=VECTOR('',#104549,1000.);
#15832=VECTOR('',#104552,1000.);
#15833=VECTOR('',#104553,1000.);
#15834=VECTOR('',#104554,1000.);
#15835=VECTOR('',#104557,1000.);
#15836=VECTOR('',#104558,1000.);
#15837=VECTOR('',#104561,1000.);
#15838=VECTOR('',#104562,1000.);
#15839=VECTOR('',#104563,1000.);
#15840=VECTOR('',#104564,1000.);
#15841=VECTOR('',#104567,1000.);
#15842=VECTOR('',#104568,1000.);
#15843=VECTOR('',#104569,1000.);
#15844=VECTOR('',#104572,1000.);
#15845=VECTOR('',#104573,1000.);
#15846=VECTOR('',#104574,1000.);
#15847=VECTOR('',#104577,1000.);
#15848=VECTOR('',#104578,1000.);
#15849=VECTOR('',#104581,1000.);
#15850=VECTOR('',#104582,1000.);
#15851=VECTOR('',#104583,1000.);
#15852=VECTOR('',#104584,1000.);
#15853=VECTOR('',#104587,1000.);
#15854=VECTOR('',#104588,1000.);
#15855=VECTOR('',#104589,1000.);
#15856=VECTOR('',#104592,1000.);
#15857=VECTOR('',#104593,1000.);
#15858=VECTOR('',#104594,1000.);
#15859=VECTOR('',#104597,1000.);
#15860=VECTOR('',#104598,1000.);
#15861=VECTOR('',#104601,1000.);
#15862=VECTOR('',#104602,1000.);
#15863=VECTOR('',#104603,1000.);
#15864=VECTOR('',#104604,1000.);
#15865=VECTOR('',#104607,1000.);
#15866=VECTOR('',#104608,1000.);
#15867=VECTOR('',#104609,1000.);
#15868=VECTOR('',#104612,1000.);
#15869=VECTOR('',#104613,1000.);
#15870=VECTOR('',#104614,1000.);
#15871=VECTOR('',#104617,1000.);
#15872=VECTOR('',#104618,1000.);
#15873=VECTOR('',#104621,1000.);
#15874=VECTOR('',#104622,1000.);
#15875=VECTOR('',#104623,1000.);
#15876=VECTOR('',#104624,1000.);
#15877=VECTOR('',#104627,1000.);
#15878=VECTOR('',#104628,1000.);
#15879=VECTOR('',#104629,1000.);
#15880=VECTOR('',#104632,1000.);
#15881=VECTOR('',#104633,1000.);
#15882=VECTOR('',#104634,1000.);
#15883=VECTOR('',#104637,1000.);
#15884=VECTOR('',#104638,1000.);
#15885=VECTOR('',#104641,1000.);
#15886=VECTOR('',#104642,1000.);
#15887=VECTOR('',#104643,1000.);
#15888=VECTOR('',#104644,1000.);
#15889=VECTOR('',#104647,1000.);
#15890=VECTOR('',#104648,1000.);
#15891=VECTOR('',#104649,1000.);
#15892=VECTOR('',#104652,1000.);
#15893=VECTOR('',#104653,1000.);
#15894=VECTOR('',#104654,1000.);
#15895=VECTOR('',#104657,1000.);
#15896=VECTOR('',#104658,1000.);
#15897=VECTOR('',#104661,1000.);
#15898=VECTOR('',#104662,1000.);
#15899=VECTOR('',#104663,1000.);
#15900=VECTOR('',#104664,1000.);
#15901=VECTOR('',#104667,1000.);
#15902=VECTOR('',#104668,1000.);
#15903=VECTOR('',#104669,1000.);
#15904=VECTOR('',#104672,1000.);
#15905=VECTOR('',#104673,1000.);
#15906=VECTOR('',#104674,1000.);
#15907=VECTOR('',#104677,1000.);
#15908=VECTOR('',#104678,1000.);
#15909=VECTOR('',#104681,1000.);
#15910=VECTOR('',#104682,1000.);
#15911=VECTOR('',#104683,1000.);
#15912=VECTOR('',#104684,1000.);
#15913=VECTOR('',#104687,1000.);
#15914=VECTOR('',#104688,1000.);
#15915=VECTOR('',#104689,1000.);
#15916=VECTOR('',#104692,1000.);
#15917=VECTOR('',#104693,1000.);
#15918=VECTOR('',#104694,1000.);
#15919=VECTOR('',#104697,1000.);
#15920=VECTOR('',#104698,1000.);
#15921=VECTOR('',#104701,1000.);
#15922=VECTOR('',#104702,1000.);
#15923=VECTOR('',#104703,1000.);
#15924=VECTOR('',#104704,1000.);
#15925=VECTOR('',#104707,1000.);
#15926=VECTOR('',#104708,1000.);
#15927=VECTOR('',#104709,1000.);
#15928=VECTOR('',#104712,1000.);
#15929=VECTOR('',#104713,1000.);
#15930=VECTOR('',#104714,1000.);
#15931=VECTOR('',#104717,1000.);
#15932=VECTOR('',#104718,1000.);
#15933=VECTOR('',#104721,1000.);
#15934=VECTOR('',#104722,1000.);
#15935=VECTOR('',#104723,1000.);
#15936=VECTOR('',#104724,1000.);
#15937=VECTOR('',#104727,1000.);
#15938=VECTOR('',#104728,1000.);
#15939=VECTOR('',#104729,1000.);
#15940=VECTOR('',#104732,1000.);
#15941=VECTOR('',#104733,1000.);
#15942=VECTOR('',#104734,1000.);
#15943=VECTOR('',#104737,1000.);
#15944=VECTOR('',#104738,1000.);
#15945=VECTOR('',#104741,1000.);
#15946=VECTOR('',#104742,1000.);
#15947=VECTOR('',#104743,1000.);
#15948=VECTOR('',#104744,1000.);
#15949=VECTOR('',#104747,1000.);
#15950=VECTOR('',#104748,1000.);
#15951=VECTOR('',#104749,1000.);
#15952=VECTOR('',#104752,1000.);
#15953=VECTOR('',#104753,1000.);
#15954=VECTOR('',#104754,1000.);
#15955=VECTOR('',#104757,1000.);
#15956=VECTOR('',#104758,1000.);
#15957=VECTOR('',#104761,1000.);
#15958=VECTOR('',#104762,1000.);
#15959=VECTOR('',#104763,1000.);
#15960=VECTOR('',#104764,1000.);
#15961=VECTOR('',#104767,1000.);
#15962=VECTOR('',#104768,1000.);
#15963=VECTOR('',#104769,1000.);
#15964=VECTOR('',#104772,1000.);
#15965=VECTOR('',#104773,1000.);
#15966=VECTOR('',#104774,1000.);
#15967=VECTOR('',#104777,1000.);
#15968=VECTOR('',#104778,1000.);
#15969=VECTOR('',#104781,1000.);
#15970=VECTOR('',#104782,1000.);
#15971=VECTOR('',#104783,1000.);
#15972=VECTOR('',#104784,1000.);
#15973=VECTOR('',#104787,1000.);
#15974=VECTOR('',#104788,1000.);
#15975=VECTOR('',#104789,1000.);
#15976=VECTOR('',#104792,1000.);
#15977=VECTOR('',#104793,1000.);
#15978=VECTOR('',#104794,1000.);
#15979=VECTOR('',#104797,1000.);
#15980=VECTOR('',#104798,1000.);
#15981=VECTOR('',#104801,1000.);
#15982=VECTOR('',#104802,1000.);
#15983=VECTOR('',#104803,1000.);
#15984=VECTOR('',#104804,1000.);
#15985=VECTOR('',#104807,1000.);
#15986=VECTOR('',#104808,1000.);
#15987=VECTOR('',#104809,1000.);
#15988=VECTOR('',#104812,1000.);
#15989=VECTOR('',#104813,1000.);
#15990=VECTOR('',#104814,1000.);
#15991=VECTOR('',#104817,1000.);
#15992=VECTOR('',#104818,1000.);
#15993=VECTOR('',#104821,1000.);
#15994=VECTOR('',#104822,1000.);
#15995=VECTOR('',#104823,1000.);
#15996=VECTOR('',#104824,1000.);
#15997=VECTOR('',#104827,1000.);
#15998=VECTOR('',#104828,1000.);
#15999=VECTOR('',#104829,1000.);
#16000=VECTOR('',#104832,1000.);
#16001=VECTOR('',#104833,1000.);
#16002=VECTOR('',#104834,1000.);
#16003=VECTOR('',#104837,1000.);
#16004=VECTOR('',#104838,1000.);
#16005=VECTOR('',#104841,1000.);
#16006=VECTOR('',#104842,1000.);
#16007=VECTOR('',#104843,1000.);
#16008=VECTOR('',#104844,1000.);
#16009=VECTOR('',#104847,1000.);
#16010=VECTOR('',#104848,1000.);
#16011=VECTOR('',#104849,1000.);
#16012=VECTOR('',#104852,1000.);
#16013=VECTOR('',#104853,1000.);
#16014=VECTOR('',#104854,1000.);
#16015=VECTOR('',#104857,1000.);
#16016=VECTOR('',#104858,1000.);
#16017=VECTOR('',#104861,1000.);
#16018=VECTOR('',#104862,1000.);
#16019=VECTOR('',#104863,1000.);
#16020=VECTOR('',#104864,1000.);
#16021=VECTOR('',#104867,1000.);
#16022=VECTOR('',#104868,1000.);
#16023=VECTOR('',#104869,1000.);
#16024=VECTOR('',#104872,1000.);
#16025=VECTOR('',#104873,1000.);
#16026=VECTOR('',#104874,1000.);
#16027=VECTOR('',#104877,1000.);
#16028=VECTOR('',#104878,1000.);
#16029=VECTOR('',#104881,1000.);
#16030=VECTOR('',#104882,1000.);
#16031=VECTOR('',#104883,1000.);
#16032=VECTOR('',#104884,1000.);
#16033=VECTOR('',#104887,1000.);
#16034=VECTOR('',#104888,1000.);
#16035=VECTOR('',#104889,1000.);
#16036=VECTOR('',#104892,1000.);
#16037=VECTOR('',#104893,1000.);
#16038=VECTOR('',#104894,1000.);
#16039=VECTOR('',#104897,1000.);
#16040=VECTOR('',#104898,1000.);
#16041=VECTOR('',#104901,1000.);
#16042=VECTOR('',#104902,1000.);
#16043=VECTOR('',#104903,1000.);
#16044=VECTOR('',#104904,1000.);
#16045=VECTOR('',#104907,1000.);
#16046=VECTOR('',#104908,1000.);
#16047=VECTOR('',#104909,1000.);
#16048=VECTOR('',#104912,1000.);
#16049=VECTOR('',#104913,1000.);
#16050=VECTOR('',#104914,1000.);
#16051=VECTOR('',#104917,1000.);
#16052=VECTOR('',#104918,1000.);
#16053=VECTOR('',#104921,1000.);
#16054=VECTOR('',#104922,1000.);
#16055=VECTOR('',#104923,1000.);
#16056=VECTOR('',#104924,1000.);
#16057=VECTOR('',#104927,1000.);
#16058=VECTOR('',#104928,1000.);
#16059=VECTOR('',#104929,1000.);
#16060=VECTOR('',#104932,1000.);
#16061=VECTOR('',#104933,1000.);
#16062=VECTOR('',#104934,1000.);
#16063=VECTOR('',#104937,1000.);
#16064=VECTOR('',#104938,1000.);
#16065=VECTOR('',#104941,1000.);
#16066=VECTOR('',#104942,1000.);
#16067=VECTOR('',#104943,1000.);
#16068=VECTOR('',#104944,1000.);
#16069=VECTOR('',#104947,1000.);
#16070=VECTOR('',#104948,1000.);
#16071=VECTOR('',#104949,1000.);
#16072=VECTOR('',#104952,1000.);
#16073=VECTOR('',#104953,1000.);
#16074=VECTOR('',#104954,1000.);
#16075=VECTOR('',#104957,1000.);
#16076=VECTOR('',#104958,1000.);
#16077=VECTOR('',#104961,1000.);
#16078=VECTOR('',#104962,1000.);
#16079=VECTOR('',#104963,1000.);
#16080=VECTOR('',#104964,1000.);
#16081=VECTOR('',#104967,1000.);
#16082=VECTOR('',#104968,1000.);
#16083=VECTOR('',#104969,1000.);
#16084=VECTOR('',#104972,1000.);
#16085=VECTOR('',#104973,1000.);
#16086=VECTOR('',#104974,1000.);
#16087=VECTOR('',#104977,1000.);
#16088=VECTOR('',#104978,1000.);
#16089=VECTOR('',#104981,1000.);
#16090=VECTOR('',#104982,1000.);
#16091=VECTOR('',#104983,1000.);
#16092=VECTOR('',#104984,1000.);
#16093=VECTOR('',#104987,1000.);
#16094=VECTOR('',#104988,1000.);
#16095=VECTOR('',#104989,1000.);
#16096=VECTOR('',#104992,1000.);
#16097=VECTOR('',#104993,1000.);
#16098=VECTOR('',#104994,1000.);
#16099=VECTOR('',#104997,1000.);
#16100=VECTOR('',#104998,1000.);
#16101=VECTOR('',#105001,1000.);
#16102=VECTOR('',#105002,1000.);
#16103=VECTOR('',#105003,1000.);
#16104=VECTOR('',#105004,1000.);
#16105=VECTOR('',#105007,1000.);
#16106=VECTOR('',#105008,1000.);
#16107=VECTOR('',#105009,1000.);
#16108=VECTOR('',#105012,1000.);
#16109=VECTOR('',#105013,1000.);
#16110=VECTOR('',#105014,1000.);
#16111=VECTOR('',#105017,1000.);
#16112=VECTOR('',#105018,1000.);
#16113=VECTOR('',#105021,1000.);
#16114=VECTOR('',#105022,1000.);
#16115=VECTOR('',#105023,1000.);
#16116=VECTOR('',#105024,1000.);
#16117=VECTOR('',#105027,1000.);
#16118=VECTOR('',#105028,1000.);
#16119=VECTOR('',#105029,1000.);
#16120=VECTOR('',#105032,1000.);
#16121=VECTOR('',#105033,1000.);
#16122=VECTOR('',#105034,1000.);
#16123=VECTOR('',#105037,1000.);
#16124=VECTOR('',#105038,1000.);
#16125=VECTOR('',#105041,1000.);
#16126=VECTOR('',#105042,1000.);
#16127=VECTOR('',#105043,1000.);
#16128=VECTOR('',#105044,1000.);
#16129=VECTOR('',#105047,1000.);
#16130=VECTOR('',#105048,1000.);
#16131=VECTOR('',#105049,1000.);
#16132=VECTOR('',#105052,1000.);
#16133=VECTOR('',#105053,1000.);
#16134=VECTOR('',#105054,1000.);
#16135=VECTOR('',#105057,1000.);
#16136=VECTOR('',#105058,1000.);
#16137=VECTOR('',#105061,1000.);
#16138=VECTOR('',#105062,1000.);
#16139=VECTOR('',#105063,1000.);
#16140=VECTOR('',#105064,1000.);
#16141=VECTOR('',#105067,1000.);
#16142=VECTOR('',#105068,1000.);
#16143=VECTOR('',#105069,1000.);
#16144=VECTOR('',#105072,1000.);
#16145=VECTOR('',#105073,1000.);
#16146=VECTOR('',#105074,1000.);
#16147=VECTOR('',#105077,1000.);
#16148=VECTOR('',#105078,1000.);
#16149=VECTOR('',#105081,1000.);
#16150=VECTOR('',#105082,1000.);
#16151=VECTOR('',#105083,1000.);
#16152=VECTOR('',#105084,1000.);
#16153=VECTOR('',#105087,1000.);
#16154=VECTOR('',#105088,1000.);
#16155=VECTOR('',#105089,1000.);
#16156=VECTOR('',#105092,1000.);
#16157=VECTOR('',#105093,1000.);
#16158=VECTOR('',#105094,1000.);
#16159=VECTOR('',#105097,1000.);
#16160=VECTOR('',#105098,1000.);
#16161=VECTOR('',#105101,1000.);
#16162=VECTOR('',#105102,1000.);
#16163=VECTOR('',#105103,1000.);
#16164=VECTOR('',#105104,1000.);
#16165=VECTOR('',#105107,1000.);
#16166=VECTOR('',#105108,1000.);
#16167=VECTOR('',#105109,1000.);
#16168=VECTOR('',#105112,1000.);
#16169=VECTOR('',#105113,1000.);
#16170=VECTOR('',#105114,1000.);
#16171=VECTOR('',#105117,1000.);
#16172=VECTOR('',#105118,1000.);
#16173=VECTOR('',#105121,1000.);
#16174=VECTOR('',#105122,1000.);
#16175=VECTOR('',#105123,1000.);
#16176=VECTOR('',#105124,1000.);
#16177=VECTOR('',#105127,1000.);
#16178=VECTOR('',#105128,1000.);
#16179=VECTOR('',#105129,1000.);
#16180=VECTOR('',#105132,1000.);
#16181=VECTOR('',#105133,1000.);
#16182=VECTOR('',#105134,1000.);
#16183=VECTOR('',#105137,1000.);
#16184=VECTOR('',#105138,1000.);
#16185=VECTOR('',#105141,1000.);
#16186=VECTOR('',#105142,1000.);
#16187=VECTOR('',#105143,1000.);
#16188=VECTOR('',#105144,1000.);
#16189=VECTOR('',#105147,1000.);
#16190=VECTOR('',#105148,1000.);
#16191=VECTOR('',#105149,1000.);
#16192=VECTOR('',#105152,1000.);
#16193=VECTOR('',#105153,1000.);
#16194=VECTOR('',#105154,1000.);
#16195=VECTOR('',#105157,1000.);
#16196=VECTOR('',#105158,1000.);
#16197=VECTOR('',#105161,1000.);
#16198=VECTOR('',#105162,1000.);
#16199=VECTOR('',#105163,1000.);
#16200=VECTOR('',#105164,1000.);
#16201=VECTOR('',#105167,1000.);
#16202=VECTOR('',#105168,1000.);
#16203=VECTOR('',#105169,1000.);
#16204=VECTOR('',#105172,1000.);
#16205=VECTOR('',#105173,1000.);
#16206=VECTOR('',#105174,1000.);
#16207=VECTOR('',#105177,1000.);
#16208=VECTOR('',#105178,1000.);
#16209=VECTOR('',#105181,1000.);
#16210=VECTOR('',#105182,1000.);
#16211=VECTOR('',#105183,1000.);
#16212=VECTOR('',#105184,1000.);
#16213=VECTOR('',#105187,1000.);
#16214=VECTOR('',#105188,1000.);
#16215=VECTOR('',#105189,1000.);
#16216=VECTOR('',#105192,1000.);
#16217=VECTOR('',#105193,1000.);
#16218=VECTOR('',#105194,1000.);
#16219=VECTOR('',#105197,1000.);
#16220=VECTOR('',#105198,1000.);
#16221=VECTOR('',#105201,1000.);
#16222=VECTOR('',#105202,1000.);
#16223=VECTOR('',#105203,1000.);
#16224=VECTOR('',#105204,1000.);
#16225=VECTOR('',#105207,1000.);
#16226=VECTOR('',#105208,1000.);
#16227=VECTOR('',#105209,1000.);
#16228=VECTOR('',#105212,1000.);
#16229=VECTOR('',#105213,1000.);
#16230=VECTOR('',#105214,1000.);
#16231=VECTOR('',#105217,1000.);
#16232=VECTOR('',#105218,1000.);
#16233=VECTOR('',#105221,1000.);
#16234=VECTOR('',#105222,1000.);
#16235=VECTOR('',#105223,1000.);
#16236=VECTOR('',#105224,1000.);
#16237=VECTOR('',#105227,1000.);
#16238=VECTOR('',#105228,1000.);
#16239=VECTOR('',#105229,1000.);
#16240=VECTOR('',#105232,1000.);
#16241=VECTOR('',#105233,1000.);
#16242=VECTOR('',#105234,1000.);
#16243=VECTOR('',#105237,1000.);
#16244=VECTOR('',#105238,1000.);
#16245=VECTOR('',#105241,1000.);
#16246=VECTOR('',#105242,1000.);
#16247=VECTOR('',#105243,1000.);
#16248=VECTOR('',#105244,1000.);
#16249=VECTOR('',#105247,1000.);
#16250=VECTOR('',#105248,1000.);
#16251=VECTOR('',#105249,1000.);
#16252=VECTOR('',#105252,1000.);
#16253=VECTOR('',#105253,1000.);
#16254=VECTOR('',#105254,1000.);
#16255=VECTOR('',#105257,1000.);
#16256=VECTOR('',#105258,1000.);
#16257=VECTOR('',#105261,1000.);
#16258=VECTOR('',#105262,1000.);
#16259=VECTOR('',#105263,1000.);
#16260=VECTOR('',#105264,1000.);
#16261=VECTOR('',#105267,1000.);
#16262=VECTOR('',#105268,1000.);
#16263=VECTOR('',#105269,1000.);
#16264=VECTOR('',#105272,1000.);
#16265=VECTOR('',#105273,1000.);
#16266=VECTOR('',#105274,1000.);
#16267=VECTOR('',#105277,1000.);
#16268=VECTOR('',#105278,1000.);
#16269=VECTOR('',#105281,1000.);
#16270=VECTOR('',#105282,1000.);
#16271=VECTOR('',#105283,1000.);
#16272=VECTOR('',#105284,1000.);
#16273=VECTOR('',#105287,1000.);
#16274=VECTOR('',#105288,1000.);
#16275=VECTOR('',#105289,1000.);
#16276=VECTOR('',#105292,1000.);
#16277=VECTOR('',#105293,1000.);
#16278=VECTOR('',#105294,1000.);
#16279=VECTOR('',#105297,1000.);
#16280=VECTOR('',#105298,1000.);
#16281=VECTOR('',#105301,1000.);
#16282=VECTOR('',#105302,1000.);
#16283=VECTOR('',#105303,1000.);
#16284=VECTOR('',#105304,1000.);
#16285=VECTOR('',#105307,1000.);
#16286=VECTOR('',#105308,1000.);
#16287=VECTOR('',#105309,1000.);
#16288=VECTOR('',#105312,1000.);
#16289=VECTOR('',#105313,1000.);
#16290=VECTOR('',#105314,1000.);
#16291=VECTOR('',#105317,1000.);
#16292=VECTOR('',#105318,1000.);
#16293=VECTOR('',#105321,1000.);
#16294=VECTOR('',#105322,1000.);
#16295=VECTOR('',#105323,1000.);
#16296=VECTOR('',#105324,1000.);
#16297=VECTOR('',#105327,1000.);
#16298=VECTOR('',#105328,1000.);
#16299=VECTOR('',#105329,1000.);
#16300=VECTOR('',#105332,1000.);
#16301=VECTOR('',#105333,1000.);
#16302=VECTOR('',#105334,1000.);
#16303=VECTOR('',#105337,1000.);
#16304=VECTOR('',#105338,1000.);
#16305=VECTOR('',#105341,1000.);
#16306=VECTOR('',#105342,1000.);
#16307=VECTOR('',#105343,1000.);
#16308=VECTOR('',#105344,1000.);
#16309=VECTOR('',#105347,1000.);
#16310=VECTOR('',#105348,1000.);
#16311=VECTOR('',#105349,1000.);
#16312=VECTOR('',#105352,1000.);
#16313=VECTOR('',#105353,1000.);
#16314=VECTOR('',#105354,1000.);
#16315=VECTOR('',#105357,1000.);
#16316=VECTOR('',#105358,1000.);
#16317=VECTOR('',#105361,1000.);
#16318=VECTOR('',#105362,1000.);
#16319=VECTOR('',#105363,1000.);
#16320=VECTOR('',#105364,1000.);
#16321=VECTOR('',#105367,1000.);
#16322=VECTOR('',#105368,1000.);
#16323=VECTOR('',#105369,1000.);
#16324=VECTOR('',#105372,1000.);
#16325=VECTOR('',#105373,1000.);
#16326=VECTOR('',#105374,1000.);
#16327=VECTOR('',#105377,1000.);
#16328=VECTOR('',#105378,1000.);
#16329=VECTOR('',#105381,1000.);
#16330=VECTOR('',#105382,1000.);
#16331=VECTOR('',#105383,1000.);
#16332=VECTOR('',#105384,1000.);
#16333=VECTOR('',#105387,1000.);
#16334=VECTOR('',#105388,1000.);
#16335=VECTOR('',#105389,1000.);
#16336=VECTOR('',#105392,1000.);
#16337=VECTOR('',#105393,1000.);
#16338=VECTOR('',#105394,1000.);
#16339=VECTOR('',#105397,1000.);
#16340=VECTOR('',#105398,1000.);
#16341=VECTOR('',#105401,1000.);
#16342=VECTOR('',#105402,1000.);
#16343=VECTOR('',#105403,1000.);
#16344=VECTOR('',#105404,1000.);
#16345=VECTOR('',#105407,1000.);
#16346=VECTOR('',#105408,1000.);
#16347=VECTOR('',#105409,1000.);
#16348=VECTOR('',#105412,1000.);
#16349=VECTOR('',#105413,1000.);
#16350=VECTOR('',#105414,1000.);
#16351=VECTOR('',#105417,1000.);
#16352=VECTOR('',#105418,1000.);
#16353=VECTOR('',#105421,1000.);
#16354=VECTOR('',#105422,1000.);
#16355=VECTOR('',#105423,1000.);
#16356=VECTOR('',#105424,1000.);
#16357=VECTOR('',#105427,1000.);
#16358=VECTOR('',#105428,1000.);
#16359=VECTOR('',#105429,1000.);
#16360=VECTOR('',#105432,1000.);
#16361=VECTOR('',#105433,1000.);
#16362=VECTOR('',#105434,1000.);
#16363=VECTOR('',#105437,1000.);
#16364=VECTOR('',#105438,1000.);
#16365=VECTOR('',#105441,1000.);
#16366=VECTOR('',#105442,1000.);
#16367=VECTOR('',#105443,1000.);
#16368=VECTOR('',#105444,1000.);
#16369=VECTOR('',#105447,1000.);
#16370=VECTOR('',#105448,1000.);
#16371=VECTOR('',#105449,1000.);
#16372=VECTOR('',#105452,1000.);
#16373=VECTOR('',#105453,1000.);
#16374=VECTOR('',#105454,1000.);
#16375=VECTOR('',#105457,1000.);
#16376=VECTOR('',#105458,1000.);
#16377=VECTOR('',#105461,1000.);
#16378=VECTOR('',#105462,1000.);
#16379=VECTOR('',#105463,1000.);
#16380=VECTOR('',#105464,1000.);
#16381=VECTOR('',#105467,1000.);
#16382=VECTOR('',#105468,1000.);
#16383=VECTOR('',#105469,1000.);
#16384=VECTOR('',#105472,1000.);
#16385=VECTOR('',#105473,1000.);
#16386=VECTOR('',#105474,1000.);
#16387=VECTOR('',#105477,1000.);
#16388=VECTOR('',#105478,1000.);
#16389=VECTOR('',#105481,1000.);
#16390=VECTOR('',#105482,1000.);
#16391=VECTOR('',#105483,1000.);
#16392=VECTOR('',#105484,1000.);
#16393=VECTOR('',#105487,1000.);
#16394=VECTOR('',#105488,1000.);
#16395=VECTOR('',#105489,1000.);
#16396=VECTOR('',#105492,1000.);
#16397=VECTOR('',#105493,1000.);
#16398=VECTOR('',#105494,1000.);
#16399=VECTOR('',#105497,1000.);
#16400=VECTOR('',#105498,1000.);
#16401=VECTOR('',#105501,1000.);
#16402=VECTOR('',#105502,1000.);
#16403=VECTOR('',#105503,1000.);
#16404=VECTOR('',#105504,1000.);
#16405=VECTOR('',#105507,1000.);
#16406=VECTOR('',#105508,1000.);
#16407=VECTOR('',#105509,1000.);
#16408=VECTOR('',#105512,1000.);
#16409=VECTOR('',#105513,1000.);
#16410=VECTOR('',#105514,1000.);
#16411=VECTOR('',#105517,1000.);
#16412=VECTOR('',#105518,1000.);
#16413=VECTOR('',#105521,1000.);
#16414=VECTOR('',#105522,1000.);
#16415=VECTOR('',#105523,1000.);
#16416=VECTOR('',#105524,1000.);
#16417=VECTOR('',#105527,1000.);
#16418=VECTOR('',#105528,1000.);
#16419=VECTOR('',#105529,1000.);
#16420=VECTOR('',#105532,1000.);
#16421=VECTOR('',#105533,1000.);
#16422=VECTOR('',#105534,1000.);
#16423=VECTOR('',#105537,1000.);
#16424=VECTOR('',#105538,1000.);
#16425=VECTOR('',#105541,1000.);
#16426=VECTOR('',#105542,1000.);
#16427=VECTOR('',#105543,1000.);
#16428=VECTOR('',#105544,1000.);
#16429=VECTOR('',#105547,1000.);
#16430=VECTOR('',#105548,1000.);
#16431=VECTOR('',#105549,1000.);
#16432=VECTOR('',#105552,1000.);
#16433=VECTOR('',#105553,1000.);
#16434=VECTOR('',#105554,1000.);
#16435=VECTOR('',#105557,1000.);
#16436=VECTOR('',#105558,1000.);
#16437=VECTOR('',#105561,1000.);
#16438=VECTOR('',#105562,1000.);
#16439=VECTOR('',#105563,1000.);
#16440=VECTOR('',#105564,1000.);
#16441=VECTOR('',#105567,1000.);
#16442=VECTOR('',#105568,1000.);
#16443=VECTOR('',#105569,1000.);
#16444=VECTOR('',#105572,1000.);
#16445=VECTOR('',#105573,1000.);
#16446=VECTOR('',#105574,1000.);
#16447=VECTOR('',#105577,1000.);
#16448=VECTOR('',#105578,1000.);
#16449=VECTOR('',#105581,1000.);
#16450=VECTOR('',#105582,1000.);
#16451=VECTOR('',#105583,1000.);
#16452=VECTOR('',#105584,1000.);
#16453=VECTOR('',#105587,1000.);
#16454=VECTOR('',#105588,1000.);
#16455=VECTOR('',#105589,1000.);
#16456=VECTOR('',#105592,1000.);
#16457=VECTOR('',#105593,1000.);
#16458=VECTOR('',#105594,1000.);
#16459=VECTOR('',#105597,1000.);
#16460=VECTOR('',#105598,1000.);
#16461=VECTOR('',#105601,1000.);
#16462=VECTOR('',#105602,1000.);
#16463=VECTOR('',#105603,1000.);
#16464=VECTOR('',#105604,1000.);
#16465=VECTOR('',#105607,1000.);
#16466=VECTOR('',#105608,1000.);
#16467=VECTOR('',#105609,1000.);
#16468=VECTOR('',#105612,1000.);
#16469=VECTOR('',#105613,1000.);
#16470=VECTOR('',#105614,1000.);
#16471=VECTOR('',#105617,1000.);
#16472=VECTOR('',#105618,1000.);
#16473=VECTOR('',#105621,1000.);
#16474=VECTOR('',#105622,1000.);
#16475=VECTOR('',#105623,1000.);
#16476=VECTOR('',#105624,1000.);
#16477=VECTOR('',#105627,1000.);
#16478=VECTOR('',#105628,1000.);
#16479=VECTOR('',#105629,1000.);
#16480=VECTOR('',#105632,1000.);
#16481=VECTOR('',#105633,1000.);
#16482=VECTOR('',#105634,1000.);
#16483=VECTOR('',#105637,1000.);
#16484=VECTOR('',#105638,1000.);
#16485=VECTOR('',#105641,1000.);
#16486=VECTOR('',#105642,1000.);
#16487=VECTOR('',#105643,1000.);
#16488=VECTOR('',#105644,1000.);
#16489=VECTOR('',#105647,1000.);
#16490=VECTOR('',#105648,1000.);
#16491=VECTOR('',#105649,1000.);
#16492=VECTOR('',#105652,1000.);
#16493=VECTOR('',#105653,1000.);
#16494=VECTOR('',#105654,1000.);
#16495=VECTOR('',#105657,1000.);
#16496=VECTOR('',#105658,1000.);
#16497=VECTOR('',#105661,1000.);
#16498=VECTOR('',#105662,1000.);
#16499=VECTOR('',#105663,1000.);
#16500=VECTOR('',#105664,1000.);
#16501=VECTOR('',#105667,1000.);
#16502=VECTOR('',#105668,1000.);
#16503=VECTOR('',#105669,1000.);
#16504=VECTOR('',#105672,1000.);
#16505=VECTOR('',#105673,1000.);
#16506=VECTOR('',#105674,1000.);
#16507=VECTOR('',#105677,1000.);
#16508=VECTOR('',#105678,1000.);
#16509=VECTOR('',#105681,1000.);
#16510=VECTOR('',#105682,1000.);
#16511=VECTOR('',#105683,1000.);
#16512=VECTOR('',#105684,1000.);
#16513=VECTOR('',#105687,1000.);
#16514=VECTOR('',#105688,1000.);
#16515=VECTOR('',#105689,1000.);
#16516=VECTOR('',#105692,1000.);
#16517=VECTOR('',#105693,1000.);
#16518=VECTOR('',#105694,1000.);
#16519=VECTOR('',#105697,1000.);
#16520=VECTOR('',#105698,1000.);
#16521=VECTOR('',#105701,1000.);
#16522=VECTOR('',#105702,1000.);
#16523=VECTOR('',#105703,1000.);
#16524=VECTOR('',#105704,1000.);
#16525=VECTOR('',#105707,1000.);
#16526=VECTOR('',#105708,1000.);
#16527=VECTOR('',#105709,1000.);
#16528=VECTOR('',#105712,1000.);
#16529=VECTOR('',#105713,1000.);
#16530=VECTOR('',#105714,1000.);
#16531=VECTOR('',#105717,1000.);
#16532=VECTOR('',#105718,1000.);
#16533=VECTOR('',#105721,1000.);
#16534=VECTOR('',#105722,1000.);
#16535=VECTOR('',#105723,1000.);
#16536=VECTOR('',#105724,1000.);
#16537=VECTOR('',#105727,1000.);
#16538=VECTOR('',#105728,1000.);
#16539=VECTOR('',#105729,1000.);
#16540=VECTOR('',#105732,1000.);
#16541=VECTOR('',#105733,1000.);
#16542=VECTOR('',#105734,1000.);
#16543=VECTOR('',#105737,1000.);
#16544=VECTOR('',#105738,1000.);
#16545=VECTOR('',#105741,1000.);
#16546=VECTOR('',#105742,1000.);
#16547=VECTOR('',#105743,1000.);
#16548=VECTOR('',#105744,1000.);
#16549=VECTOR('',#105747,1000.);
#16550=VECTOR('',#105748,1000.);
#16551=VECTOR('',#105749,1000.);
#16552=VECTOR('',#105752,1000.);
#16553=VECTOR('',#105753,1000.);
#16554=VECTOR('',#105754,1000.);
#16555=VECTOR('',#105757,1000.);
#16556=VECTOR('',#105758,1000.);
#16557=VECTOR('',#105761,1000.);
#16558=VECTOR('',#105762,1000.);
#16559=VECTOR('',#105763,1000.);
#16560=VECTOR('',#105764,1000.);
#16561=VECTOR('',#105767,1000.);
#16562=VECTOR('',#105768,1000.);
#16563=VECTOR('',#105769,1000.);
#16564=VECTOR('',#105772,1000.);
#16565=VECTOR('',#105773,1000.);
#16566=VECTOR('',#105774,1000.);
#16567=VECTOR('',#105777,1000.);
#16568=VECTOR('',#105778,1000.);
#16569=VECTOR('',#105781,1000.);
#16570=VECTOR('',#105782,1000.);
#16571=VECTOR('',#105783,1000.);
#16572=VECTOR('',#105784,1000.);
#16573=VECTOR('',#105787,1000.);
#16574=VECTOR('',#105788,1000.);
#16575=VECTOR('',#105789,1000.);
#16576=VECTOR('',#105792,1000.);
#16577=VECTOR('',#105793,1000.);
#16578=VECTOR('',#105794,1000.);
#16579=VECTOR('',#105797,1000.);
#16580=VECTOR('',#105798,1000.);
#16581=VECTOR('',#105801,1000.);
#16582=VECTOR('',#105802,1000.);
#16583=VECTOR('',#105803,1000.);
#16584=VECTOR('',#105804,1000.);
#16585=VECTOR('',#105807,1000.);
#16586=VECTOR('',#105808,1000.);
#16587=VECTOR('',#105809,1000.);
#16588=VECTOR('',#105812,1000.);
#16589=VECTOR('',#105813,1000.);
#16590=VECTOR('',#105814,1000.);
#16591=VECTOR('',#105817,1000.);
#16592=VECTOR('',#105818,1000.);
#16593=VECTOR('',#105821,1000.);
#16594=VECTOR('',#105822,1000.);
#16595=VECTOR('',#105823,1000.);
#16596=VECTOR('',#105824,1000.);
#16597=VECTOR('',#105827,1000.);
#16598=VECTOR('',#105828,1000.);
#16599=VECTOR('',#105829,1000.);
#16600=VECTOR('',#105832,1000.);
#16601=VECTOR('',#105833,1000.);
#16602=VECTOR('',#105834,1000.);
#16603=VECTOR('',#105837,1000.);
#16604=VECTOR('',#105838,1000.);
#16605=VECTOR('',#105841,1000.);
#16606=VECTOR('',#105842,1000.);
#16607=VECTOR('',#105843,1000.);
#16608=VECTOR('',#105844,1000.);
#16609=VECTOR('',#105847,1000.);
#16610=VECTOR('',#105848,1000.);
#16611=VECTOR('',#105849,1000.);
#16612=VECTOR('',#105852,1000.);
#16613=VECTOR('',#105853,1000.);
#16614=VECTOR('',#105854,1000.);
#16615=VECTOR('',#105857,1000.);
#16616=VECTOR('',#105858,1000.);
#16617=VECTOR('',#105861,1000.);
#16618=VECTOR('',#105862,1000.);
#16619=VECTOR('',#105863,1000.);
#16620=VECTOR('',#105864,1000.);
#16621=VECTOR('',#105867,1000.);
#16622=VECTOR('',#105868,1000.);
#16623=VECTOR('',#105869,1000.);
#16624=VECTOR('',#105872,1000.);
#16625=VECTOR('',#105873,1000.);
#16626=VECTOR('',#105874,1000.);
#16627=VECTOR('',#105877,1000.);
#16628=VECTOR('',#105878,1000.);
#16629=VECTOR('',#105881,1000.);
#16630=VECTOR('',#105882,1000.);
#16631=VECTOR('',#105883,1000.);
#16632=VECTOR('',#105884,1000.);
#16633=VECTOR('',#105887,1000.);
#16634=VECTOR('',#105888,1000.);
#16635=VECTOR('',#105889,1000.);
#16636=VECTOR('',#105892,1000.);
#16637=VECTOR('',#105893,1000.);
#16638=VECTOR('',#105894,1000.);
#16639=VECTOR('',#105897,1000.);
#16640=VECTOR('',#105898,1000.);
#16641=VECTOR('',#105901,1000.);
#16642=VECTOR('',#105902,1000.);
#16643=VECTOR('',#105903,1000.);
#16644=VECTOR('',#105904,1000.);
#16645=VECTOR('',#105907,1000.);
#16646=VECTOR('',#105908,1000.);
#16647=VECTOR('',#105909,1000.);
#16648=VECTOR('',#105912,1000.);
#16649=VECTOR('',#105913,1000.);
#16650=VECTOR('',#105914,1000.);
#16651=VECTOR('',#105917,1000.);
#16652=VECTOR('',#105918,1000.);
#16653=VECTOR('',#105921,1000.);
#16654=VECTOR('',#105922,1000.);
#16655=VECTOR('',#105923,1000.);
#16656=VECTOR('',#105924,1000.);
#16657=VECTOR('',#105927,1000.);
#16658=VECTOR('',#105928,1000.);
#16659=VECTOR('',#105929,1000.);
#16660=VECTOR('',#105932,1000.);
#16661=VECTOR('',#105933,1000.);
#16662=VECTOR('',#105934,1000.);
#16663=VECTOR('',#105937,1000.);
#16664=VECTOR('',#105938,1000.);
#16665=VECTOR('',#105941,1000.);
#16666=VECTOR('',#105942,1000.);
#16667=VECTOR('',#105943,1000.);
#16668=VECTOR('',#105944,1000.);
#16669=VECTOR('',#105947,1000.);
#16670=VECTOR('',#105948,1000.);
#16671=VECTOR('',#105949,1000.);
#16672=VECTOR('',#105952,1000.);
#16673=VECTOR('',#105953,1000.);
#16674=VECTOR('',#105954,1000.);
#16675=VECTOR('',#105957,1000.);
#16676=VECTOR('',#105958,1000.);
#16677=VECTOR('',#105961,1000.);
#16678=VECTOR('',#105962,1000.);
#16679=VECTOR('',#105963,1000.);
#16680=VECTOR('',#105964,1000.);
#16681=VECTOR('',#105967,1000.);
#16682=VECTOR('',#105968,1000.);
#16683=VECTOR('',#105969,1000.);
#16684=VECTOR('',#105972,1000.);
#16685=VECTOR('',#105973,1000.);
#16686=VECTOR('',#105974,1000.);
#16687=VECTOR('',#105977,1000.);
#16688=VECTOR('',#105978,1000.);
#16689=VECTOR('',#105983,1000.);
#16690=VECTOR('',#105984,1000.);
#16691=VECTOR('',#105985,1000.);
#16692=VECTOR('',#105986,1000.);
#16693=VECTOR('',#105989,1000.);
#16694=VECTOR('',#105990,1000.);
#16695=VECTOR('',#105991,1000.);
#16696=VECTOR('',#105994,1000.);
#16697=VECTOR('',#105995,1000.);
#16698=VECTOR('',#105998,1000.);
#16699=VECTOR('',#105999,1000.);
#16700=VECTOR('',#106002,1000.);
#16701=VECTOR('',#106009,1000.);
#16702=VECTOR('',#106012,1000.);
#16703=VECTOR('',#106015,1000.);
#16704=VECTOR('',#106018,1000.);
#16705=VECTOR('',#106025,1000.);
#16706=VECTOR('',#106028,1000.);
#16707=VECTOR('',#106031,1000.);
#16708=VECTOR('',#106034,1000.);
#16709=VECTOR('',#106055,1000.);
#16710=VECTOR('',#106056,1000.);
#16711=VECTOR('',#106061,1000.);
#16712=VECTOR('',#106066,1000.);
#16713=VECTOR('',#106083,10.25);
#16714=VECTOR('',#106084,10.25);
#16715=VECTOR('',#106089,1000.);
#16716=VECTOR('',#106092,10.25);
#16717=VECTOR('',#106095,10.25);
#16718=VECTOR('',#106098,10.25);
#16719=VECTOR('',#106101,10.25);
#16720=VECTOR('',#106104,10.25);
#16721=VECTOR('',#106107,10.25);
#16722=VECTOR('',#106110,10.25);
#16723=VECTOR('',#106113,13.);
#16724=VECTOR('',#106118,13.);
#16725=VECTOR('',#106123,13.);
#16726=VECTOR('',#106126,13.);
#16727=VECTOR('',#106129,13.);
#16728=VECTOR('',#106132,13.);
#16729=VECTOR('',#106135,13.);
#16730=VECTOR('',#106138,13.);
#16731=VECTOR('',#106145,13.);
#16732=VECTOR('',#106146,1000.);
#16733=VECTOR('',#106147,13.);
#16734=VECTOR('',#106150,12.87032685775);
#16735=VECTOR('',#106155,9.09006752601109);
#16736=VECTOR('',#106156,10.);
#16737=VECTOR('',#106159,9.09006752601109);
#16738=VECTOR('',#106162,9.09006752601109);
#16739=VECTOR('',#106165,9.09006752601109);
#16740=VECTOR('',#106168,9.0900675260086);
#16741=VECTOR('',#106169,10.);
#16742=VECTOR('',#106172,9.0900675260086);
#16743=VECTOR('',#106175,9.0900675260086);
#16744=VECTOR('',#106178,9.0900675260086);
#16745=VECTOR('',#106181,9.08769033371916);
#16746=VECTOR('',#106186,11.8397710119949);
#16747=VECTOR('',#106191,11.8397710119949);
#16748=VECTOR('',#106194,11.8397710119949);
#16749=VECTOR('',#106197,11.8397710119877);
#16750=VECTOR('',#106198,10.);
#16751=VECTOR('',#106201,11.8397710119877);
#16752=VECTOR('',#106204,11.8397710119877);
#16753=VECTOR('',#106207,11.8397710119877);
#16754=VECTOR('',#106210,9.75000242976401);
#16755=VECTOR('',#106223,4.75);
#16756=VECTOR('',#106234,1000.);
#16757=VECTOR('',#106235,1000.);
#16758=VECTOR('',#106244,1000.);
#16759=VECTOR('',#106245,10.);
#16760=VECTOR('',#106246,10.);
#16761=VECTOR('',#106249,10.);
#16762=VECTOR('',#106250,10.);
#16763=VECTOR('',#106253,1000.);
#16764=VECTOR('',#106268,1000.);
#16765=VECTOR('',#106269,10.);
#16766=VECTOR('',#106272,10.);
#16767=VECTOR('',#106273,10.);
#16768=VECTOR('',#106276,10.);
#16769=VECTOR('',#106281,10.5);
#16770=VECTOR('',#106288,10.75000319972);
#16771=VECTOR('',#106301,7.75);
#16772=VECTOR('',#106306,7.999997663262);
#16773=VECTOR('',#106321,1000.);
#16774=VECTOR('',#106328,10.25);
#16775=VECTOR('',#106329,10.25);
#16776=VECTOR('',#106334,1000.);
#16777=VECTOR('',#106337,10.25);
#16778=VECTOR('',#106340,10.25);
#16779=VECTOR('',#106343,10.25);
#16780=VECTOR('',#106346,10.25);
#16781=VECTOR('',#106349,10.25);
#16782=VECTOR('',#106352,10.25);
#16783=VECTOR('',#106355,10.25);
#16784=VECTOR('',#106358,13.);
#16785=VECTOR('',#106363,13.);
#16786=VECTOR('',#106368,13.);
#16787=VECTOR('',#106371,13.);
#16788=VECTOR('',#106374,13.);
#16789=VECTOR('',#106377,13.);
#16790=VECTOR('',#106380,13.);
#16791=VECTOR('',#106383,13.);
#16792=VECTOR('',#106390,13.);
#16793=VECTOR('',#106391,1000.);
#16794=VECTOR('',#106392,13.);
#16795=VECTOR('',#106395,12.87032685775);
#16796=VECTOR('',#106400,9.09006752601109);
#16797=VECTOR('',#106401,10.);
#16798=VECTOR('',#106404,9.09006752601109);
#16799=VECTOR('',#106407,9.09006752601109);
#16800=VECTOR('',#106410,9.09006752601109);
#16801=VECTOR('',#106413,9.0900675260086);
#16802=VECTOR('',#106414,10.);
#16803=VECTOR('',#106417,9.0900675260086);
#16804=VECTOR('',#106420,9.0900675260086);
#16805=VECTOR('',#106423,9.0900675260086);
#16806=VECTOR('',#106426,9.08769033371916);
#16807=VECTOR('',#106431,11.8397710119949);
#16808=VECTOR('',#106436,11.8397710119949);
#16809=VECTOR('',#106439,11.8397710119949);
#16810=VECTOR('',#106442,11.8397710119877);
#16811=VECTOR('',#106443,10.);
#16812=VECTOR('',#106446,11.8397710119877);
#16813=VECTOR('',#106449,11.8397710119877);
#16814=VECTOR('',#106452,11.8397710119877);
#16815=VECTOR('',#106455,9.75000242976401);
#16816=VECTOR('',#106468,4.75);
#16817=VECTOR('',#106479,1000.);
#16818=VECTOR('',#106480,1000.);
#16819=VECTOR('',#106489,1000.);
#16820=VECTOR('',#106490,10.);
#16821=VECTOR('',#106491,10.);
#16822=VECTOR('',#106494,10.);
#16823=VECTOR('',#106495,10.);
#16824=VECTOR('',#106498,1000.);
#16825=VECTOR('',#106513,1000.);
#16826=VECTOR('',#106514,10.);
#16827=VECTOR('',#106517,10.);
#16828=VECTOR('',#106518,10.);
#16829=VECTOR('',#106521,10.);
#16830=VECTOR('',#106526,10.5);
#16831=VECTOR('',#106533,10.75000319972);
#16832=VECTOR('',#106546,7.75);
#16833=VECTOR('',#106551,7.999997663262);
#16834=VECTOR('',#106566,1000.);
#16835=PLANE('',#79488);
#16836=PLANE('',#79496);
#16837=PLANE('',#79504);
#16838=PLANE('',#79506);
#16839=PLANE('',#79511);
#16840=PLANE('',#79514);
#16841=PLANE('',#79726);
#16842=PLANE('',#79727);
#16843=PLANE('',#79728);
#16844=PLANE('',#79729);
#16845=PLANE('',#79730);
#16846=PLANE('',#79731);
#16847=PLANE('',#79732);
#16848=PLANE('',#79733);
#16849=PLANE('',#79734);
#16850=PLANE('',#79745);
#16851=PLANE('',#79750);
#16852=PLANE('',#79780);
#16853=PLANE('',#79786);
#16854=PLANE('',#79789);
#16855=PLANE('',#79800);
#16856=PLANE('',#79833);
#16857=PLANE('',#79834);
#16858=PLANE('',#79835);
#16859=PLANE('',#79836);
#16860=PLANE('',#79837);
#16861=PLANE('',#79838);
#16862=PLANE('',#79839);
#16863=PLANE('',#79840);
#16864=PLANE('',#79841);
#16865=PLANE('',#79842);
#16866=PLANE('',#79843);
#16867=PLANE('',#79857);
#16868=PLANE('',#79863);
#16869=PLANE('',#79874);
#16870=PLANE('',#79877);
#16871=PLANE('',#79881);
#16872=PLANE('',#79918);
#16873=PLANE('',#79942);
#16874=PLANE('',#79943);
#16875=PLANE('',#79944);
#16876=PLANE('',#79945);
#16877=PLANE('',#79946);
#16878=PLANE('',#79947);
#16879=PLANE('',#79953);
#16880=PLANE('',#79959);
#16881=PLANE('',#79961);
#16882=PLANE('',#79967);
#16883=PLANE('',#80015);
#16884=PLANE('',#80017);
#16885=PLANE('',#80042);
#16886=PLANE('',#80044);
#16887=PLANE('',#80045);
#16888=PLANE('',#80068);
#16889=PLANE('',#80069);
#16890=PLANE('',#80070);
#16891=PLANE('',#80071);
#16892=PLANE('',#80072);
#16893=PLANE('',#80078);
#16894=PLANE('',#80133);
#16895=PLANE('',#80136);
#16896=PLANE('',#80138);
#16897=PLANE('',#80139);
#16898=PLANE('',#80140);
#16899=PLANE('',#80146);
#16900=PLANE('',#80150);
#16901=PLANE('',#80163);
#16902=PLANE('',#80175);
#16903=PLANE('',#80189);
#16904=PLANE('',#80190);
#16905=PLANE('',#80212);
#16906=PLANE('',#80258);
#16907=PLANE('',#80274);
#16908=PLANE('',#80292);
#16909=PLANE('',#80295);
#16910=PLANE('',#80307);
#16911=PLANE('',#80312);
#16912=PLANE('',#80313);
#16913=PLANE('',#80319);
#16914=PLANE('',#80365);
#16915=PLANE('',#80376);
#16916=PLANE('',#80411);
#16917=PLANE('',#80415);
#16918=PLANE('',#80419);
#16919=PLANE('',#80420);
#16920=PLANE('',#80425);
#16921=PLANE('',#80428);
#16922=PLANE('',#80429);
#16923=PLANE('',#80433);
#16924=PLANE('',#80437);
#16925=PLANE('',#80457);
#16926=PLANE('',#80466);
#16927=PLANE('',#80478);
#16928=PLANE('',#80481);
#16929=PLANE('',#80482);
#16930=PLANE('',#80483);
#16931=PLANE('',#80484);
#16932=PLANE('',#80485);
#16933=PLANE('',#80486);
#16934=PLANE('',#80487);
#16935=PLANE('',#80488);
#16936=PLANE('',#80489);
#16937=PLANE('',#80490);
#16938=PLANE('',#80491);
#16939=PLANE('',#80492);
#16940=PLANE('',#80493);
#16941=PLANE('',#80494);
#16942=PLANE('',#80521);
#16943=PLANE('',#80598);
#16944=PLANE('',#80599);
#16945=PLANE('',#80600);
#16946=PLANE('',#80604);
#16947=PLANE('',#80605);
#16948=PLANE('',#80606);
#16949=PLANE('',#80607);
#16950=PLANE('',#80608);
#16951=PLANE('',#80609);
#16952=PLANE('',#80610);
#16953=PLANE('',#80611);
#16954=PLANE('',#80612);
#16955=PLANE('',#80613);
#16956=PLANE('',#80614);
#16957=PLANE('',#80615);
#16958=PLANE('',#80616);
#16959=PLANE('',#80617);
#16960=PLANE('',#80618);
#16961=PLANE('',#80619);
#16962=PLANE('',#80655);
#16963=PLANE('',#80656);
#16964=PLANE('',#80660);
#16965=PLANE('',#80661);
#16966=PLANE('',#80662);
#16967=PLANE('',#80663);
#16968=PLANE('',#80664);
#16969=PLANE('',#80665);
#16970=PLANE('',#80666);
#16971=PLANE('',#80705);
#16972=PLANE('',#80706);
#16973=PLANE('',#80707);
#16974=PLANE('',#80710);
#16975=PLANE('',#80711);
#16976=PLANE('',#80715);
#16977=PLANE('',#80716);
#16978=PLANE('',#80717);
#16979=PLANE('',#80718);
#16980=PLANE('',#80754);
#16981=PLANE('',#80755);
#16982=PLANE('',#80759);
#16983=PLANE('',#80760);
#16984=PLANE('',#80761);
#16985=PLANE('',#80762);
#16986=PLANE('',#80763);
#16987=PLANE('',#80764);
#16988=PLANE('',#80765);
#16989=PLANE('',#80788);
#16990=PLANE('',#80789);
#16991=PLANE('',#80790);
#16992=PLANE('',#80794);
#16993=PLANE('',#80795);
#16994=PLANE('',#80834);
#16995=PLANE('',#80835);
#16996=PLANE('',#80836);
#16997=PLANE('',#80839);
#16998=PLANE('',#80840);
#16999=PLANE('',#80844);
#17000=PLANE('',#80845);
#17001=PLANE('',#80846);
#17002=PLANE('',#80847);
#17003=PLANE('',#80854);
#17004=PLANE('',#80935);
#17005=PLANE('',#80936);
#17006=PLANE('',#80937);
#17007=PLANE('',#80938);
#17008=PLANE('',#80939);
#17009=PLANE('',#80940);
#17010=PLANE('',#80941);
#17011=PLANE('',#80942);
#17012=PLANE('',#80943);
#17013=PLANE('',#80944);
#17014=PLANE('',#80945);
#17015=PLANE('',#80946);
#17016=PLANE('',#80947);
#17017=PLANE('',#80950);
#17018=PLANE('',#80973);
#17019=PLANE('',#80974);
#17020=PLANE('',#80975);
#17021=PLANE('',#80979);
#17022=PLANE('',#80980);
#17023=PLANE('',#81067);
#17024=PLANE('',#81072);
#17025=PLANE('',#81073);
#17026=PLANE('',#81074);
#17027=PLANE('',#81075);
#17028=PLANE('',#81076);
#17029=PLANE('',#81079);
#17030=PLANE('',#81080);
#17031=PLANE('',#81081);
#17032=PLANE('',#81082);
#17033=PLANE('',#81084);
#17034=PLANE('',#81087);
#17035=PLANE('',#81090);
#17036=PLANE('',#81093);
#17037=PLANE('',#81095);
#17038=PLANE('',#81097);
#17039=PLANE('',#81100);
#17040=PLANE('',#81103);
#17041=PLANE('',#81106);
#17042=PLANE('',#81108);
#17043=PLANE('',#81111);
#17044=PLANE('',#81113);
#17045=PLANE('',#81115);
#17046=PLANE('',#81118);
#17047=PLANE('',#81120);
#17048=PLANE('',#81123);
#17049=PLANE('',#81126);
#17050=PLANE('',#81129);
#17051=PLANE('',#81132);
#17052=PLANE('',#81135);
#17053=PLANE('',#81138);
#17054=PLANE('',#81141);
#17055=PLANE('',#81144);
#17056=PLANE('',#81147);
#17057=PLANE('',#81150);
#17058=PLANE('',#81153);
#17059=PLANE('',#81156);
#17060=PLANE('',#81159);
#17061=PLANE('',#81162);
#17062=PLANE('',#81165);
#17063=PLANE('',#81168);
#17064=PLANE('',#81170);
#17065=PLANE('',#81173);
#17066=PLANE('',#81176);
#17067=PLANE('',#81179);
#17068=PLANE('',#81181);
#17069=PLANE('',#81184);
#17070=PLANE('',#81187);
#17071=PLANE('',#81189);
#17072=PLANE('',#81192);
#17073=PLANE('',#81194);
#17074=PLANE('',#81197);
#17075=PLANE('',#81200);
#17076=PLANE('',#81202);
#17077=PLANE('',#81205);
#17078=PLANE('',#81207);
#17079=PLANE('',#81210);
#17080=PLANE('',#81213);
#17081=PLANE('',#81216);
#17082=PLANE('',#81219);
#17083=PLANE('',#81221);
#17084=PLANE('',#81224);
#17085=PLANE('',#81227);
#17086=PLANE('',#81230);
#17087=PLANE('',#81233);
#17088=PLANE('',#81236);
#17089=PLANE('',#81239);
#17090=PLANE('',#81241);
#17091=PLANE('',#81244);
#17092=PLANE('',#81246);
#17093=PLANE('',#81249);
#17094=PLANE('',#81252);
#17095=PLANE('',#81254);
#17096=PLANE('',#81257);
#17097=PLANE('',#81259);
#17098=PLANE('',#81262);
#17099=PLANE('',#81265);
#17100=PLANE('',#81267);
#17101=PLANE('',#81270);
#17102=PLANE('',#81272);
#17103=PLANE('',#81275);
#17104=PLANE('',#81278);
#17105=PLANE('',#81280);
#17106=PLANE('',#81283);
#17107=PLANE('',#81285);
#17108=PLANE('',#81288);
#17109=PLANE('',#81291);
#17110=PLANE('',#81294);
#17111=PLANE('',#81297);
#17112=PLANE('',#81300);
#17113=PLANE('',#81303);
#17114=PLANE('',#81306);
#17115=PLANE('',#81309);
#17116=PLANE('',#81312);
#17117=PLANE('',#81315);
#17118=PLANE('',#81318);
#17119=PLANE('',#81321);
#17120=PLANE('',#81324);
#17121=PLANE('',#81327);
#17122=PLANE('',#81330);
#17123=PLANE('',#81333);
#17124=PLANE('',#81336);
#17125=PLANE('',#81339);
#17126=PLANE('',#81342);
#17127=PLANE('',#81345);
#17128=PLANE('',#81348);
#17129=PLANE('',#81351);
#17130=PLANE('',#81354);
#17131=PLANE('',#81357);
#17132=PLANE('',#81360);
#17133=PLANE('',#81363);
#17134=PLANE('',#81366);
#17135=PLANE('',#81369);
#17136=PLANE('',#81371);
#17137=PLANE('',#81374);
#17138=PLANE('',#81377);
#17139=PLANE('',#81379);
#17140=PLANE('',#81382);
#17141=PLANE('',#81384);
#17142=PLANE('',#81387);
#17143=PLANE('',#81390);
#17144=PLANE('',#81393);
#17145=PLANE('',#81396);
#17146=PLANE('',#81399);
#17147=PLANE('',#81402);
#17148=PLANE('',#81405);
#17149=PLANE('',#81408);
#17150=PLANE('',#81411);
#17151=PLANE('',#81414);
#17152=PLANE('',#81417);
#17153=PLANE('',#81420);
#17154=PLANE('',#81423);
#17155=PLANE('',#81426);
#17156=PLANE('',#81429);
#17157=PLANE('',#81432);
#17158=PLANE('',#81435);
#17159=PLANE('',#81438);
#17160=PLANE('',#81441);
#17161=PLANE('',#81444);
#17162=PLANE('',#81447);
#17163=PLANE('',#81450);
#17164=PLANE('',#81453);
#17165=PLANE('',#81456);
#17166=PLANE('',#81459);
#17167=PLANE('',#81462);
#17168=PLANE('',#81465);
#17169=PLANE('',#81468);
#17170=PLANE('',#81471);
#17171=PLANE('',#81474);
#17172=PLANE('',#81477);
#17173=PLANE('',#81480);
#17174=PLANE('',#81483);
#17175=PLANE('',#81486);
#17176=PLANE('',#81488);
#17177=PLANE('',#81491);
#17178=PLANE('',#81493);
#17179=PLANE('',#81496);
#17180=PLANE('',#81499);
#17181=PLANE('',#81501);
#17182=PLANE('',#81504);
#17183=PLANE('',#81506);
#17184=PLANE('',#81509);
#17185=PLANE('',#81512);
#17186=PLANE('',#81515);
#17187=PLANE('',#81518);
#17188=PLANE('',#81521);
#17189=PLANE('',#81524);
#17190=PLANE('',#81527);
#17191=PLANE('',#81530);
#17192=PLANE('',#81533);
#17193=PLANE('',#81536);
#17194=PLANE('',#81539);
#17195=PLANE('',#81542);
#17196=PLANE('',#81545);
#17197=PLANE('',#81548);
#17198=PLANE('',#81551);
#17199=PLANE('',#81554);
#17200=PLANE('',#81557);
#17201=PLANE('',#81560);
#17202=PLANE('',#81563);
#17203=PLANE('',#81566);
#17204=PLANE('',#81569);
#17205=PLANE('',#81572);
#17206=PLANE('',#81575);
#17207=PLANE('',#81578);
#17208=PLANE('',#81581);
#17209=PLANE('',#81584);
#17210=PLANE('',#81587);
#17211=PLANE('',#81590);
#17212=PLANE('',#81593);
#17213=PLANE('',#81596);
#17214=PLANE('',#81599);
#17215=PLANE('',#81602);
#17216=PLANE('',#81605);
#17217=PLANE('',#81608);
#17218=PLANE('',#81611);
#17219=PLANE('',#81614);
#17220=PLANE('',#81617);
#17221=PLANE('',#81620);
#17222=PLANE('',#81623);
#17223=PLANE('',#81626);
#17224=PLANE('',#81628);
#17225=PLANE('',#81631);
#17226=PLANE('',#81634);
#17227=PLANE('',#81637);
#17228=PLANE('',#81640);
#17229=PLANE('',#81643);
#17230=PLANE('',#81646);
#17231=PLANE('',#81649);
#17232=PLANE('',#81652);
#17233=PLANE('',#81655);
#17234=PLANE('',#81658);
#17235=PLANE('',#81661);
#17236=PLANE('',#81664);
#17237=PLANE('',#81667);
#17238=PLANE('',#81670);
#17239=PLANE('',#81673);
#17240=PLANE('',#81676);
#17241=PLANE('',#81679);
#17242=PLANE('',#81682);
#17243=PLANE('',#81685);
#17244=PLANE('',#81688);
#17245=PLANE('',#81691);
#17246=PLANE('',#81694);
#17247=PLANE('',#81697);
#17248=PLANE('',#81700);
#17249=PLANE('',#81703);
#17250=PLANE('',#81706);
#17251=PLANE('',#81709);
#17252=PLANE('',#81712);
#17253=PLANE('',#81715);
#17254=PLANE('',#81718);
#17255=PLANE('',#81721);
#17256=PLANE('',#81724);
#17257=PLANE('',#81727);
#17258=PLANE('',#81730);
#17259=PLANE('',#81733);
#17260=PLANE('',#81736);
#17261=PLANE('',#81739);
#17262=PLANE('',#81742);
#17263=PLANE('',#81745);
#17264=PLANE('',#81748);
#17265=PLANE('',#81751);
#17266=PLANE('',#81754);
#17267=PLANE('',#81757);
#17268=PLANE('',#81760);
#17269=PLANE('',#81763);
#17270=PLANE('',#81766);
#17271=PLANE('',#81769);
#17272=PLANE('',#81772);
#17273=PLANE('',#81774);
#17274=PLANE('',#81777);
#17275=PLANE('',#81780);
#17276=PLANE('',#81783);
#17277=PLANE('',#81786);
#17278=PLANE('',#81788);
#17279=PLANE('',#81791);
#17280=PLANE('',#81794);
#17281=PLANE('',#81797);
#17282=PLANE('',#81800);
#17283=PLANE('',#81803);
#17284=PLANE('',#81806);
#17285=PLANE('',#81809);
#17286=PLANE('',#81812);
#17287=PLANE('',#81815);
#17288=PLANE('',#81818);
#17289=PLANE('',#81821);
#17290=PLANE('',#81824);
#17291=PLANE('',#81827);
#17292=PLANE('',#81830);
#17293=PLANE('',#81833);
#17294=PLANE('',#81836);
#17295=PLANE('',#81839);
#17296=PLANE('',#81842);
#17297=PLANE('',#81845);
#17298=PLANE('',#81848);
#17299=PLANE('',#81851);
#17300=PLANE('',#81854);
#17301=PLANE('',#81857);
#17302=PLANE('',#81860);
#17303=PLANE('',#81863);
#17304=PLANE('',#81866);
#17305=PLANE('',#81869);
#17306=PLANE('',#81872);
#17307=PLANE('',#81875);
#17308=PLANE('',#81878);
#17309=PLANE('',#81881);
#17310=PLANE('',#81884);
#17311=PLANE('',#81887);
#17312=PLANE('',#81890);
#17313=PLANE('',#81893);
#17314=PLANE('',#81896);
#17315=PLANE('',#81899);
#17316=PLANE('',#81902);
#17317=PLANE('',#81905);
#17318=PLANE('',#81908);
#17319=PLANE('',#81911);
#17320=PLANE('',#81914);
#17321=PLANE('',#81917);
#17322=PLANE('',#81920);
#17323=PLANE('',#81923);
#17324=PLANE('',#81926);
#17325=PLANE('',#81929);
#17326=PLANE('',#81932);
#17327=PLANE('',#81935);
#17328=PLANE('',#81938);
#17329=PLANE('',#81941);
#17330=PLANE('',#81944);
#17331=PLANE('',#81947);
#17332=PLANE('',#81950);
#17333=PLANE('',#81953);
#17334=PLANE('',#81956);
#17335=PLANE('',#81959);
#17336=PLANE('',#81962);
#17337=PLANE('',#81965);
#17338=PLANE('',#81968);
#17339=PLANE('',#81971);
#17340=PLANE('',#81974);
#17341=PLANE('',#81977);
#17342=PLANE('',#81980);
#17343=PLANE('',#81983);
#17344=PLANE('',#81986);
#17345=PLANE('',#81989);
#17346=PLANE('',#81992);
#17347=PLANE('',#81995);
#17348=PLANE('',#81998);
#17349=PLANE('',#82001);
#17350=PLANE('',#82004);
#17351=PLANE('',#82007);
#17352=PLANE('',#82010);
#17353=PLANE('',#82013);
#17354=PLANE('',#82016);
#17355=PLANE('',#82019);
#17356=PLANE('',#82022);
#17357=PLANE('',#82025);
#17358=PLANE('',#82028);
#17359=PLANE('',#82031);
#17360=PLANE('',#82034);
#17361=PLANE('',#82037);
#17362=PLANE('',#82040);
#17363=PLANE('',#82043);
#17364=PLANE('',#82046);
#17365=PLANE('',#82049);
#17366=PLANE('',#82052);
#17367=PLANE('',#82055);
#17368=PLANE('',#82058);
#17369=PLANE('',#82061);
#17370=PLANE('',#82064);
#17371=PLANE('',#82067);
#17372=PLANE('',#82070);
#17373=PLANE('',#82073);
#17374=PLANE('',#82076);
#17375=PLANE('',#82079);
#17376=PLANE('',#82082);
#17377=PLANE('',#82085);
#17378=PLANE('',#82088);
#17379=PLANE('',#82091);
#17380=PLANE('',#82094);
#17381=PLANE('',#82097);
#17382=PLANE('',#82100);
#17383=PLANE('',#82103);
#17384=PLANE('',#82106);
#17385=PLANE('',#82109);
#17386=PLANE('',#82112);
#17387=PLANE('',#82115);
#17388=PLANE('',#82118);
#17389=PLANE('',#82121);
#17390=PLANE('',#82124);
#17391=PLANE('',#82127);
#17392=PLANE('',#82130);
#17393=PLANE('',#82133);
#17394=PLANE('',#82136);
#17395=PLANE('',#82139);
#17396=PLANE('',#82142);
#17397=PLANE('',#82145);
#17398=PLANE('',#82148);
#17399=PLANE('',#82151);
#17400=PLANE('',#82154);
#17401=PLANE('',#82157);
#17402=PLANE('',#82160);
#17403=PLANE('',#82163);
#17404=PLANE('',#82166);
#17405=PLANE('',#82169);
#17406=PLANE('',#82172);
#17407=PLANE('',#82175);
#17408=PLANE('',#82178);
#17409=PLANE('',#82181);
#17410=PLANE('',#82184);
#17411=PLANE('',#82187);
#17412=PLANE('',#82190);
#17413=PLANE('',#82193);
#17414=PLANE('',#82196);
#17415=PLANE('',#82199);
#17416=PLANE('',#82202);
#17417=PLANE('',#82205);
#17418=PLANE('',#82208);
#17419=PLANE('',#82211);
#17420=PLANE('',#82214);
#17421=PLANE('',#82217);
#17422=PLANE('',#82220);
#17423=PLANE('',#82223);
#17424=PLANE('',#82226);
#17425=PLANE('',#82229);
#17426=PLANE('',#82232);
#17427=PLANE('',#82235);
#17428=PLANE('',#82238);
#17429=PLANE('',#82241);
#17430=PLANE('',#82244);
#17431=PLANE('',#82247);
#17432=PLANE('',#82250);
#17433=PLANE('',#82253);
#17434=PLANE('',#82256);
#17435=PLANE('',#82259);
#17436=PLANE('',#82262);
#17437=PLANE('',#82265);
#17438=PLANE('',#82268);
#17439=PLANE('',#82271);
#17440=PLANE('',#82274);
#17441=PLANE('',#82277);
#17442=PLANE('',#82280);
#17443=PLANE('',#82283);
#17444=PLANE('',#82286);
#17445=PLANE('',#82289);
#17446=PLANE('',#82292);
#17447=PLANE('',#82295);
#17448=PLANE('',#82298);
#17449=PLANE('',#82301);
#17450=PLANE('',#82304);
#17451=PLANE('',#82307);
#17452=PLANE('',#82310);
#17453=PLANE('',#82313);
#17454=PLANE('',#82316);
#17455=PLANE('',#82319);
#17456=PLANE('',#82322);
#17457=PLANE('',#82325);
#17458=PLANE('',#82328);
#17459=PLANE('',#82331);
#17460=PLANE('',#82334);
#17461=PLANE('',#82337);
#17462=PLANE('',#82340);
#17463=PLANE('',#82343);
#17464=PLANE('',#82346);
#17465=PLANE('',#82349);
#17466=PLANE('',#82352);
#17467=PLANE('',#82355);
#17468=PLANE('',#82358);
#17469=PLANE('',#82361);
#17470=PLANE('',#82364);
#17471=PLANE('',#82367);
#17472=PLANE('',#82370);
#17473=PLANE('',#82373);
#17474=PLANE('',#82376);
#17475=PLANE('',#82379);
#17476=PLANE('',#82382);
#17477=PLANE('',#82385);
#17478=PLANE('',#82388);
#17479=PLANE('',#82391);
#17480=PLANE('',#82394);
#17481=PLANE('',#82397);
#17482=PLANE('',#82400);
#17483=PLANE('',#82403);
#17484=PLANE('',#82406);
#17485=PLANE('',#82409);
#17486=PLANE('',#82412);
#17487=PLANE('',#82415);
#17488=PLANE('',#82418);
#17489=PLANE('',#82421);
#17490=PLANE('',#82424);
#17491=PLANE('',#82427);
#17492=PLANE('',#82430);
#17493=PLANE('',#82433);
#17494=PLANE('',#82436);
#17495=PLANE('',#82439);
#17496=PLANE('',#82442);
#17497=PLANE('',#82445);
#17498=PLANE('',#82448);
#17499=PLANE('',#82451);
#17500=PLANE('',#82454);
#17501=PLANE('',#82457);
#17502=PLANE('',#82460);
#17503=PLANE('',#82463);
#17504=PLANE('',#82466);
#17505=PLANE('',#82469);
#17506=PLANE('',#82472);
#17507=PLANE('',#82475);
#17508=PLANE('',#82478);
#17509=PLANE('',#82481);
#17510=PLANE('',#82484);
#17511=PLANE('',#82487);
#17512=PLANE('',#82490);
#17513=PLANE('',#82493);
#17514=PLANE('',#82496);
#17515=PLANE('',#82499);
#17516=PLANE('',#82502);
#17517=PLANE('',#82505);
#17518=PLANE('',#82508);
#17519=PLANE('',#82511);
#17520=PLANE('',#82514);
#17521=PLANE('',#82517);
#17522=PLANE('',#82520);
#17523=PLANE('',#82523);
#17524=PLANE('',#82526);
#17525=PLANE('',#82529);
#17526=PLANE('',#82532);
#17527=PLANE('',#82535);
#17528=PLANE('',#82538);
#17529=PLANE('',#82541);
#17530=PLANE('',#82544);
#17531=PLANE('',#82547);
#17532=PLANE('',#82550);
#17533=PLANE('',#82553);
#17534=PLANE('',#82556);
#17535=PLANE('',#82559);
#17536=PLANE('',#82562);
#17537=PLANE('',#82565);
#17538=PLANE('',#82568);
#17539=PLANE('',#82571);
#17540=PLANE('',#82574);
#17541=PLANE('',#82577);
#17542=PLANE('',#82580);
#17543=PLANE('',#82583);
#17544=PLANE('',#82586);
#17545=PLANE('',#82589);
#17546=PLANE('',#82592);
#17547=PLANE('',#82595);
#17548=PLANE('',#82598);
#17549=PLANE('',#82601);
#17550=PLANE('',#82604);
#17551=PLANE('',#82607);
#17552=PLANE('',#82610);
#17553=PLANE('',#82613);
#17554=PLANE('',#82616);
#17555=PLANE('',#82619);
#17556=PLANE('',#82622);
#17557=PLANE('',#82625);
#17558=PLANE('',#82628);
#17559=PLANE('',#82631);
#17560=PLANE('',#82634);
#17561=PLANE('',#82636);
#17562=PLANE('',#82638);
#17563=PLANE('',#82640);
#17564=PLANE('',#82643);
#17565=PLANE('',#82646);
#17566=PLANE('',#82648);
#17567=PLANE('',#82651);
#17568=PLANE('',#82653);
#17569=PLANE('',#82656);
#17570=PLANE('',#82659);
#17571=PLANE('',#82661);
#17572=PLANE('',#82664);
#17573=PLANE('',#82666);
#17574=PLANE('',#82669);
#17575=PLANE('',#82672);
#17576=PLANE('',#82674);
#17577=PLANE('',#82677);
#17578=PLANE('',#82679);
#17579=PLANE('',#82682);
#17580=PLANE('',#82685);
#17581=PLANE('',#82687);
#17582=PLANE('',#82690);
#17583=PLANE('',#82692);
#17584=PLANE('',#82695);
#17585=PLANE('',#82697);
#17586=PLANE('',#82699);
#17587=PLANE('',#82702);
#17588=PLANE('',#82704);
#17589=PLANE('',#82707);
#17590=PLANE('',#82709);
#17591=PLANE('',#82711);
#17592=PLANE('',#82714);
#17593=PLANE('',#82716);
#17594=PLANE('',#82719);
#17595=PLANE('',#82722);
#17596=PLANE('',#82724);
#17597=PLANE('',#82727);
#17598=PLANE('',#82729);
#17599=PLANE('',#82732);
#17600=PLANE('',#82735);
#17601=PLANE('',#82737);
#17602=PLANE('',#82740);
#17603=PLANE('',#82742);
#17604=PLANE('',#82745);
#17605=PLANE('',#82748);
#17606=PLANE('',#82750);
#17607=PLANE('',#82753);
#17608=PLANE('',#82755);
#17609=PLANE('',#82758);
#17610=PLANE('',#82761);
#17611=PLANE('',#82764);
#17612=PLANE('',#82767);
#17613=PLANE('',#82770);
#17614=PLANE('',#82773);
#17615=PLANE('',#82776);
#17616=PLANE('',#82779);
#17617=PLANE('',#82782);
#17618=PLANE('',#82785);
#17619=PLANE('',#82788);
#17620=PLANE('',#82791);
#17621=PLANE('',#82794);
#17622=PLANE('',#82797);
#17623=PLANE('',#82800);
#17624=PLANE('',#82803);
#17625=PLANE('',#82806);
#17626=PLANE('',#82809);
#17627=PLANE('',#82812);
#17628=PLANE('',#82815);
#17629=PLANE('',#82818);
#17630=PLANE('',#82821);
#17631=PLANE('',#82824);
#17632=PLANE('',#82827);
#17633=PLANE('',#82830);
#17634=PLANE('',#82833);
#17635=PLANE('',#82836);
#17636=PLANE('',#82839);
#17637=PLANE('',#82842);
#17638=PLANE('',#82845);
#17639=PLANE('',#82848);
#17640=PLANE('',#82851);
#17641=PLANE('',#82854);
#17642=PLANE('',#82856);
#17643=PLANE('',#82858);
#17644=PLANE('',#82861);
#17645=PLANE('',#82863);
#17646=PLANE('',#82866);
#17647=PLANE('',#82868);
#17648=PLANE('',#82870);
#17649=PLANE('',#82873);
#17650=PLANE('',#82875);
#17651=PLANE('',#82878);
#17652=PLANE('',#82881);
#17653=PLANE('',#82884);
#17654=PLANE('',#82887);
#17655=PLANE('',#82890);
#17656=PLANE('',#82893);
#17657=PLANE('',#82896);
#17658=PLANE('',#82899);
#17659=PLANE('',#82902);
#17660=PLANE('',#82905);
#17661=PLANE('',#82908);
#17662=PLANE('',#82911);
#17663=PLANE('',#82914);
#17664=PLANE('',#82917);
#17665=PLANE('',#82920);
#17666=PLANE('',#82923);
#17667=PLANE('',#82926);
#17668=PLANE('',#82929);
#17669=PLANE('',#82932);
#17670=PLANE('',#82935);
#17671=PLANE('',#82937);
#17672=PLANE('',#82940);
#17673=PLANE('',#82943);
#17674=PLANE('',#82945);
#17675=PLANE('',#82948);
#17676=PLANE('',#82950);
#17677=PLANE('',#82953);
#17678=PLANE('',#82956);
#17679=PLANE('',#82958);
#17680=PLANE('',#82961);
#17681=PLANE('',#82963);
#17682=PLANE('',#82966);
#17683=PLANE('',#82969);
#17684=PLANE('',#82972);
#17685=PLANE('',#82975);
#17686=PLANE('',#82977);
#17687=PLANE('',#82980);
#17688=PLANE('',#82983);
#17689=PLANE('',#82986);
#17690=PLANE('',#82989);
#17691=PLANE('',#82992);
#17692=PLANE('',#82995);
#17693=PLANE('',#82998);
#17694=PLANE('',#83001);
#17695=PLANE('',#83004);
#17696=PLANE('',#83007);
#17697=PLANE('',#83010);
#17698=PLANE('',#83013);
#17699=PLANE('',#83016);
#17700=PLANE('',#83019);
#17701=PLANE('',#83022);
#17702=PLANE('',#83025);
#17703=PLANE('',#83028);
#17704=PLANE('',#83031);
#17705=PLANE('',#83034);
#17706=PLANE('',#83037);
#17707=PLANE('',#83040);
#17708=PLANE('',#83043);
#17709=PLANE('',#83046);
#17710=PLANE('',#83049);
#17711=PLANE('',#83052);
#17712=PLANE('',#83055);
#17713=PLANE('',#83058);
#17714=PLANE('',#83061);
#17715=PLANE('',#83064);
#17716=PLANE('',#83067);
#17717=PLANE('',#83070);
#17718=PLANE('',#83073);
#17719=PLANE('',#83076);
#17720=PLANE('',#83079);
#17721=PLANE('',#83082);
#17722=PLANE('',#83085);
#17723=PLANE('',#83088);
#17724=PLANE('',#83091);
#17725=PLANE('',#83094);
#17726=PLANE('',#83097);
#17727=PLANE('',#83100);
#17728=PLANE('',#83103);
#17729=PLANE('',#83106);
#17730=PLANE('',#83109);
#17731=PLANE('',#83111);
#17732=PLANE('',#83114);
#17733=PLANE('',#83117);
#17734=PLANE('',#83120);
#17735=PLANE('',#83123);
#17736=PLANE('',#83125);
#17737=PLANE('',#83128);
#17738=PLANE('',#83131);
#17739=PLANE('',#83134);
#17740=PLANE('',#83137);
#17741=PLANE('',#83140);
#17742=PLANE('',#83143);
#17743=PLANE('',#83146);
#17744=PLANE('',#83149);
#17745=PLANE('',#83152);
#17746=PLANE('',#83155);
#17747=PLANE('',#83158);
#17748=PLANE('',#83161);
#17749=PLANE('',#83164);
#17750=PLANE('',#83167);
#17751=PLANE('',#83170);
#17752=PLANE('',#83173);
#17753=PLANE('',#83176);
#17754=PLANE('',#83179);
#17755=PLANE('',#83182);
#17756=PLANE('',#83185);
#17757=PLANE('',#83188);
#17758=PLANE('',#83191);
#17759=PLANE('',#83194);
#17760=PLANE('',#83197);
#17761=PLANE('',#83200);
#17762=PLANE('',#83203);
#17763=PLANE('',#83206);
#17764=PLANE('',#83209);
#17765=PLANE('',#83212);
#17766=PLANE('',#83215);
#17767=PLANE('',#83218);
#17768=PLANE('',#83221);
#17769=PLANE('',#83224);
#17770=PLANE('',#83227);
#17771=PLANE('',#83230);
#17772=PLANE('',#83233);
#17773=PLANE('',#83236);
#17774=PLANE('',#83239);
#17775=PLANE('',#83241);
#17776=PLANE('',#83244);
#17777=PLANE('',#83246);
#17778=PLANE('',#83249);
#17779=PLANE('',#83252);
#17780=PLANE('',#83255);
#17781=PLANE('',#83258);
#17782=PLANE('',#83260);
#17783=PLANE('',#83263);
#17784=PLANE('',#83266);
#17785=PLANE('',#83269);
#17786=PLANE('',#83272);
#17787=PLANE('',#83275);
#17788=PLANE('',#83278);
#17789=PLANE('',#83281);
#17790=PLANE('',#83284);
#17791=PLANE('',#83287);
#17792=PLANE('',#83290);
#17793=PLANE('',#83293);
#17794=PLANE('',#83296);
#17795=PLANE('',#83299);
#17796=PLANE('',#83302);
#17797=PLANE('',#83305);
#17798=PLANE('',#83308);
#17799=PLANE('',#83311);
#17800=PLANE('',#83314);
#17801=PLANE('',#83317);
#17802=PLANE('',#83320);
#17803=PLANE('',#83323);
#17804=PLANE('',#83326);
#17805=PLANE('',#83329);
#17806=PLANE('',#83332);
#17807=PLANE('',#83335);
#17808=PLANE('',#83338);
#17809=PLANE('',#83341);
#17810=PLANE('',#83344);
#17811=PLANE('',#83347);
#17812=PLANE('',#83350);
#17813=PLANE('',#83353);
#17814=PLANE('',#83356);
#17815=PLANE('',#83359);
#17816=PLANE('',#83362);
#17817=PLANE('',#83365);
#17818=PLANE('',#83368);
#17819=PLANE('',#83371);
#17820=PLANE('',#83374);
#17821=PLANE('',#83377);
#17822=PLANE('',#83380);
#17823=PLANE('',#83383);
#17824=PLANE('',#83386);
#17825=PLANE('',#83389);
#17826=PLANE('',#83392);
#17827=PLANE('',#83395);
#17828=PLANE('',#83398);
#17829=PLANE('',#83401);
#17830=PLANE('',#83404);
#17831=PLANE('',#83407);
#17832=PLANE('',#83410);
#17833=PLANE('',#83413);
#17834=PLANE('',#83416);
#17835=PLANE('',#83419);
#17836=PLANE('',#83422);
#17837=PLANE('',#83425);
#17838=PLANE('',#83428);
#17839=PLANE('',#83431);
#17840=PLANE('',#83434);
#17841=PLANE('',#83437);
#17842=PLANE('',#83440);
#17843=PLANE('',#83443);
#17844=PLANE('',#83446);
#17845=PLANE('',#83449);
#17846=PLANE('',#83452);
#17847=PLANE('',#83455);
#17848=PLANE('',#83458);
#17849=PLANE('',#83461);
#17850=PLANE('',#83464);
#17851=PLANE('',#83467);
#17852=PLANE('',#83470);
#17853=PLANE('',#83473);
#17854=PLANE('',#83476);
#17855=PLANE('',#83479);
#17856=PLANE('',#83482);
#17857=PLANE('',#83485);
#17858=PLANE('',#83488);
#17859=PLANE('',#83491);
#17860=PLANE('',#83494);
#17861=PLANE('',#83497);
#17862=PLANE('',#83500);
#17863=PLANE('',#83503);
#17864=PLANE('',#83506);
#17865=PLANE('',#83509);
#17866=PLANE('',#83512);
#17867=PLANE('',#83515);
#17868=PLANE('',#83518);
#17869=PLANE('',#83521);
#17870=PLANE('',#83524);
#17871=PLANE('',#83527);
#17872=PLANE('',#83530);
#17873=PLANE('',#83533);
#17874=PLANE('',#83536);
#17875=PLANE('',#83539);
#17876=PLANE('',#83542);
#17877=PLANE('',#83545);
#17878=PLANE('',#83548);
#17879=PLANE('',#83551);
#17880=PLANE('',#83554);
#17881=PLANE('',#83557);
#17882=PLANE('',#83560);
#17883=PLANE('',#83563);
#17884=PLANE('',#83566);
#17885=PLANE('',#83569);
#17886=PLANE('',#83572);
#17887=PLANE('',#83575);
#17888=PLANE('',#83578);
#17889=PLANE('',#83581);
#17890=PLANE('',#83584);
#17891=PLANE('',#83587);
#17892=PLANE('',#83590);
#17893=PLANE('',#83593);
#17894=PLANE('',#83596);
#17895=PLANE('',#83599);
#17896=PLANE('',#83602);
#17897=PLANE('',#83605);
#17898=PLANE('',#83608);
#17899=PLANE('',#83611);
#17900=PLANE('',#83614);
#17901=PLANE('',#83617);
#17902=PLANE('',#83620);
#17903=PLANE('',#83623);
#17904=PLANE('',#83626);
#17905=PLANE('',#83629);
#17906=PLANE('',#83632);
#17907=PLANE('',#83635);
#17908=PLANE('',#83638);
#17909=PLANE('',#83641);
#17910=PLANE('',#83644);
#17911=PLANE('',#83647);
#17912=PLANE('',#83650);
#17913=PLANE('',#83653);
#17914=PLANE('',#83656);
#17915=PLANE('',#83659);
#17916=PLANE('',#83662);
#17917=PLANE('',#83665);
#17918=PLANE('',#83668);
#17919=PLANE('',#83671);
#17920=PLANE('',#83674);
#17921=PLANE('',#83677);
#17922=PLANE('',#83680);
#17923=PLANE('',#83683);
#17924=PLANE('',#83686);
#17925=PLANE('',#83689);
#17926=PLANE('',#83692);
#17927=PLANE('',#83695);
#17928=PLANE('',#83698);
#17929=PLANE('',#83701);
#17930=PLANE('',#83704);
#17931=PLANE('',#83707);
#17932=PLANE('',#83710);
#17933=PLANE('',#83713);
#17934=PLANE('',#83716);
#17935=PLANE('',#83719);
#17936=PLANE('',#83722);
#17937=PLANE('',#83725);
#17938=PLANE('',#83728);
#17939=PLANE('',#83731);
#17940=PLANE('',#83734);
#17941=PLANE('',#83737);
#17942=PLANE('',#83740);
#17943=PLANE('',#83743);
#17944=PLANE('',#83746);
#17945=PLANE('',#83749);
#17946=PLANE('',#83752);
#17947=PLANE('',#83755);
#17948=PLANE('',#83758);
#17949=PLANE('',#83761);
#17950=PLANE('',#83764);
#17951=PLANE('',#83767);
#17952=PLANE('',#83770);
#17953=PLANE('',#83773);
#17954=PLANE('',#83776);
#17955=PLANE('',#83779);
#17956=PLANE('',#83782);
#17957=PLANE('',#83785);
#17958=PLANE('',#83788);
#17959=PLANE('',#83791);
#17960=PLANE('',#83794);
#17961=PLANE('',#83797);
#17962=PLANE('',#83800);
#17963=PLANE('',#83803);
#17964=PLANE('',#83806);
#17965=PLANE('',#83809);
#17966=PLANE('',#83812);
#17967=PLANE('',#83815);
#17968=PLANE('',#83818);
#17969=PLANE('',#83821);
#17970=PLANE('',#83824);
#17971=PLANE('',#83827);
#17972=PLANE('',#83830);
#17973=PLANE('',#83833);
#17974=PLANE('',#83836);
#17975=PLANE('',#83839);
#17976=PLANE('',#83842);
#17977=PLANE('',#83845);
#17978=PLANE('',#83848);
#17979=PLANE('',#83851);
#17980=PLANE('',#83854);
#17981=PLANE('',#83857);
#17982=PLANE('',#83860);
#17983=PLANE('',#83863);
#17984=PLANE('',#83866);
#17985=PLANE('',#83869);
#17986=PLANE('',#83872);
#17987=PLANE('',#83875);
#17988=PLANE('',#83878);
#17989=PLANE('',#83881);
#17990=PLANE('',#83884);
#17991=PLANE('',#83887);
#17992=PLANE('',#83890);
#17993=PLANE('',#83893);
#17994=PLANE('',#83896);
#17995=PLANE('',#83899);
#17996=PLANE('',#83902);
#17997=PLANE('',#83905);
#17998=PLANE('',#83908);
#17999=PLANE('',#83911);
#18000=PLANE('',#83914);
#18001=PLANE('',#83917);
#18002=PLANE('',#83920);
#18003=PLANE('',#83923);
#18004=PLANE('',#83926);
#18005=PLANE('',#83929);
#18006=PLANE('',#83932);
#18007=PLANE('',#83935);
#18008=PLANE('',#83938);
#18009=PLANE('',#83941);
#18010=PLANE('',#83944);
#18011=PLANE('',#83947);
#18012=PLANE('',#83950);
#18013=PLANE('',#83953);
#18014=PLANE('',#83956);
#18015=PLANE('',#83959);
#18016=PLANE('',#83962);
#18017=PLANE('',#83965);
#18018=PLANE('',#83968);
#18019=PLANE('',#83971);
#18020=PLANE('',#83974);
#18021=PLANE('',#83977);
#18022=PLANE('',#83980);
#18023=PLANE('',#83983);
#18024=PLANE('',#83986);
#18025=PLANE('',#83989);
#18026=PLANE('',#83992);
#18027=PLANE('',#83995);
#18028=PLANE('',#83998);
#18029=PLANE('',#84001);
#18030=PLANE('',#84004);
#18031=PLANE('',#84007);
#18032=PLANE('',#84010);
#18033=PLANE('',#84013);
#18034=PLANE('',#84016);
#18035=PLANE('',#84019);
#18036=PLANE('',#84022);
#18037=PLANE('',#84025);
#18038=PLANE('',#84028);
#18039=PLANE('',#84031);
#18040=PLANE('',#84034);
#18041=PLANE('',#84037);
#18042=PLANE('',#84040);
#18043=PLANE('',#84043);
#18044=PLANE('',#84046);
#18045=PLANE('',#84049);
#18046=PLANE('',#84052);
#18047=PLANE('',#84055);
#18048=PLANE('',#84058);
#18049=PLANE('',#84061);
#18050=PLANE('',#84064);
#18051=PLANE('',#84067);
#18052=PLANE('',#84070);
#18053=PLANE('',#84073);
#18054=PLANE('',#84076);
#18055=PLANE('',#84079);
#18056=PLANE('',#84082);
#18057=PLANE('',#84085);
#18058=PLANE('',#84088);
#18059=PLANE('',#84091);
#18060=PLANE('',#84094);
#18061=PLANE('',#84097);
#18062=PLANE('',#84100);
#18063=PLANE('',#84103);
#18064=PLANE('',#84106);
#18065=PLANE('',#84109);
#18066=PLANE('',#84112);
#18067=PLANE('',#84115);
#18068=PLANE('',#84118);
#18069=PLANE('',#84121);
#18070=PLANE('',#84124);
#18071=PLANE('',#84127);
#18072=PLANE('',#84130);
#18073=PLANE('',#84133);
#18074=PLANE('',#84136);
#18075=PLANE('',#84139);
#18076=PLANE('',#84142);
#18077=PLANE('',#84145);
#18078=PLANE('',#84148);
#18079=PLANE('',#84151);
#18080=PLANE('',#84154);
#18081=PLANE('',#84157);
#18082=PLANE('',#84160);
#18083=PLANE('',#84163);
#18084=PLANE('',#84166);
#18085=PLANE('',#84169);
#18086=PLANE('',#84172);
#18087=PLANE('',#84175);
#18088=PLANE('',#84178);
#18089=PLANE('',#84181);
#18090=PLANE('',#84184);
#18091=PLANE('',#84185);
#18092=PLANE('',#84186);
#18093=PLANE('',#84187);
#18094=PLANE('',#84188);
#18095=PLANE('',#84189);
#18096=PLANE('',#84190);
#18097=PLANE('',#84191);
#18098=PLANE('',#84192);
#18099=PLANE('',#84193);
#18100=PLANE('',#84194);
#18101=PLANE('',#84195);
#18102=PLANE('',#84196);
#18103=PLANE('',#84197);
#18104=PLANE('',#84198);
#18105=PLANE('',#84199);
#18106=PLANE('',#84200);
#18107=PLANE('',#84201);
#18108=PLANE('',#84202);
#18109=PLANE('',#84203);
#18110=PLANE('',#84204);
#18111=PLANE('',#84205);
#18112=PLANE('',#84206);
#18113=PLANE('',#84207);
#18114=PLANE('',#84208);
#18115=PLANE('',#84209);
#18116=PLANE('',#84210);
#18117=PLANE('',#84211);
#18118=PLANE('',#84212);
#18119=PLANE('',#84213);
#18120=PLANE('',#84214);
#18121=PLANE('',#84215);
#18122=PLANE('',#84216);
#18123=PLANE('',#84217);
#18124=PLANE('',#84218);
#18125=PLANE('',#84219);
#18126=PLANE('',#84220);
#18127=PLANE('',#84221);
#18128=PLANE('',#84222);
#18129=PLANE('',#84223);
#18130=PLANE('',#84224);
#18131=PLANE('',#84225);
#18132=PLANE('',#84226);
#18133=PLANE('',#84227);
#18134=PLANE('',#84228);
#18135=PLANE('',#84229);
#18136=PLANE('',#84230);
#18137=PLANE('',#84231);
#18138=PLANE('',#84232);
#18139=PLANE('',#84233);
#18140=PLANE('',#84234);
#18141=PLANE('',#84235);
#18142=PLANE('',#84236);
#18143=PLANE('',#84237);
#18144=PLANE('',#84238);
#18145=PLANE('',#84239);
#18146=PLANE('',#84240);
#18147=PLANE('',#84241);
#18148=PLANE('',#84242);
#18149=PLANE('',#84243);
#18150=PLANE('',#84244);
#18151=PLANE('',#84245);
#18152=PLANE('',#84246);
#18153=PLANE('',#84247);
#18154=PLANE('',#84248);
#18155=PLANE('',#84249);
#18156=PLANE('',#84250);
#18157=PLANE('',#84251);
#18158=PLANE('',#84252);
#18159=PLANE('',#84253);
#18160=PLANE('',#84254);
#18161=PLANE('',#84255);
#18162=PLANE('',#84256);
#18163=PLANE('',#84257);
#18164=PLANE('',#84258);
#18165=PLANE('',#84259);
#18166=PLANE('',#84260);
#18167=PLANE('',#84261);
#18168=PLANE('',#84262);
#18169=PLANE('',#84263);
#18170=PLANE('',#84264);
#18171=PLANE('',#84265);
#18172=PLANE('',#84266);
#18173=PLANE('',#84267);
#18174=PLANE('',#84268);
#18175=PLANE('',#84269);
#18176=PLANE('',#84270);
#18177=PLANE('',#84271);
#18178=PLANE('',#84272);
#18179=PLANE('',#84273);
#18180=PLANE('',#84274);
#18181=PLANE('',#84275);
#18182=PLANE('',#84276);
#18183=PLANE('',#84277);
#18184=PLANE('',#84278);
#18185=PLANE('',#84279);
#18186=PLANE('',#84280);
#18187=PLANE('',#84281);
#18188=PLANE('',#84282);
#18189=PLANE('',#84283);
#18190=PLANE('',#84284);
#18191=PLANE('',#84285);
#18192=PLANE('',#84286);
#18193=PLANE('',#84287);
#18194=PLANE('',#84288);
#18195=PLANE('',#84289);
#18196=PLANE('',#84290);
#18197=PLANE('',#84291);
#18198=PLANE('',#84292);
#18199=PLANE('',#84293);
#18200=PLANE('',#84294);
#18201=PLANE('',#84295);
#18202=PLANE('',#84296);
#18203=PLANE('',#84297);
#18204=PLANE('',#84298);
#18205=PLANE('',#84299);
#18206=PLANE('',#84300);
#18207=PLANE('',#84301);
#18208=PLANE('',#84302);
#18209=PLANE('',#84303);
#18210=PLANE('',#84304);
#18211=PLANE('',#84305);
#18212=PLANE('',#84306);
#18213=PLANE('',#84307);
#18214=PLANE('',#84308);
#18215=PLANE('',#84309);
#18216=PLANE('',#84310);
#18217=PLANE('',#84311);
#18218=PLANE('',#84312);
#18219=PLANE('',#84313);
#18220=PLANE('',#84314);
#18221=PLANE('',#84315);
#18222=PLANE('',#84316);
#18223=PLANE('',#84317);
#18224=PLANE('',#84318);
#18225=PLANE('',#84319);
#18226=PLANE('',#84320);
#18227=PLANE('',#84321);
#18228=PLANE('',#84322);
#18229=PLANE('',#84323);
#18230=PLANE('',#84324);
#18231=PLANE('',#84325);
#18232=PLANE('',#84326);
#18233=PLANE('',#84327);
#18234=PLANE('',#84328);
#18235=PLANE('',#84329);
#18236=PLANE('',#84330);
#18237=PLANE('',#84331);
#18238=PLANE('',#84332);
#18239=PLANE('',#84333);
#18240=PLANE('',#84334);
#18241=PLANE('',#84335);
#18242=PLANE('',#84336);
#18243=PLANE('',#84337);
#18244=PLANE('',#84338);
#18245=PLANE('',#84339);
#18246=PLANE('',#84340);
#18247=PLANE('',#84341);
#18248=PLANE('',#84342);
#18249=PLANE('',#84343);
#18250=PLANE('',#84344);
#18251=PLANE('',#84345);
#18252=PLANE('',#84346);
#18253=PLANE('',#84347);
#18254=PLANE('',#84348);
#18255=PLANE('',#84349);
#18256=PLANE('',#84350);
#18257=PLANE('',#84351);
#18258=PLANE('',#84352);
#18259=PLANE('',#84353);
#18260=PLANE('',#84354);
#18261=PLANE('',#84355);
#18262=PLANE('',#84356);
#18263=PLANE('',#84357);
#18264=PLANE('',#84358);
#18265=PLANE('',#84359);
#18266=PLANE('',#84360);
#18267=PLANE('',#84361);
#18268=PLANE('',#84362);
#18269=PLANE('',#84363);
#18270=PLANE('',#84364);
#18271=PLANE('',#84365);
#18272=PLANE('',#84366);
#18273=PLANE('',#84367);
#18274=PLANE('',#84368);
#18275=PLANE('',#84369);
#18276=PLANE('',#84370);
#18277=PLANE('',#84371);
#18278=PLANE('',#84372);
#18279=PLANE('',#84373);
#18280=PLANE('',#84374);
#18281=PLANE('',#84375);
#18282=PLANE('',#84376);
#18283=PLANE('',#84377);
#18284=PLANE('',#84378);
#18285=PLANE('',#84379);
#18286=PLANE('',#84380);
#18287=PLANE('',#84381);
#18288=PLANE('',#84382);
#18289=PLANE('',#84383);
#18290=PLANE('',#84384);
#18291=PLANE('',#84385);
#18292=PLANE('',#84386);
#18293=PLANE('',#84387);
#18294=PLANE('',#84388);
#18295=PLANE('',#84389);
#18296=PLANE('',#84390);
#18297=PLANE('',#84391);
#18298=PLANE('',#84392);
#18299=PLANE('',#84393);
#18300=PLANE('',#84394);
#18301=PLANE('',#84395);
#18302=PLANE('',#84396);
#18303=PLANE('',#84397);
#18304=PLANE('',#84398);
#18305=PLANE('',#84399);
#18306=PLANE('',#84400);
#18307=PLANE('',#84401);
#18308=PLANE('',#84402);
#18309=PLANE('',#84403);
#18310=PLANE('',#84404);
#18311=PLANE('',#84405);
#18312=PLANE('',#84406);
#18313=PLANE('',#84407);
#18314=PLANE('',#84408);
#18315=PLANE('',#84409);
#18316=PLANE('',#84410);
#18317=PLANE('',#84411);
#18318=PLANE('',#84412);
#18319=PLANE('',#84413);
#18320=PLANE('',#84414);
#18321=PLANE('',#84415);
#18322=PLANE('',#84416);
#18323=PLANE('',#84417);
#18324=PLANE('',#84418);
#18325=PLANE('',#84419);
#18326=PLANE('',#84420);
#18327=PLANE('',#84421);
#18328=PLANE('',#84422);
#18329=PLANE('',#84423);
#18330=PLANE('',#84424);
#18331=PLANE('',#84425);
#18332=PLANE('',#84426);
#18333=PLANE('',#84427);
#18334=PLANE('',#84428);
#18335=PLANE('',#84429);
#18336=PLANE('',#84430);
#18337=PLANE('',#84431);
#18338=PLANE('',#84432);
#18339=PLANE('',#84433);
#18340=PLANE('',#84434);
#18341=PLANE('',#84435);
#18342=PLANE('',#84436);
#18343=PLANE('',#84437);
#18344=PLANE('',#84438);
#18345=PLANE('',#84439);
#18346=PLANE('',#84440);
#18347=PLANE('',#84441);
#18348=PLANE('',#84442);
#18349=PLANE('',#84443);
#18350=PLANE('',#84444);
#18351=PLANE('',#84445);
#18352=PLANE('',#84446);
#18353=PLANE('',#84447);
#18354=PLANE('',#84448);
#18355=PLANE('',#84449);
#18356=PLANE('',#84450);
#18357=PLANE('',#84451);
#18358=PLANE('',#84452);
#18359=PLANE('',#84453);
#18360=PLANE('',#84454);
#18361=PLANE('',#84455);
#18362=PLANE('',#84456);
#18363=PLANE('',#84457);
#18364=PLANE('',#84458);
#18365=PLANE('',#84459);
#18366=PLANE('',#84460);
#18367=PLANE('',#84461);
#18368=PLANE('',#84462);
#18369=PLANE('',#84463);
#18370=PLANE('',#84464);
#18371=PLANE('',#84465);
#18372=PLANE('',#84466);
#18373=PLANE('',#84467);
#18374=PLANE('',#84468);
#18375=PLANE('',#84469);
#18376=PLANE('',#84470);
#18377=PLANE('',#84471);
#18378=PLANE('',#84472);
#18379=PLANE('',#84473);
#18380=PLANE('',#84474);
#18381=PLANE('',#84475);
#18382=PLANE('',#84476);
#18383=PLANE('',#84477);
#18384=PLANE('',#84478);
#18385=PLANE('',#84479);
#18386=PLANE('',#84480);
#18387=PLANE('',#84481);
#18388=PLANE('',#84482);
#18389=PLANE('',#84483);
#18390=PLANE('',#84484);
#18391=PLANE('',#84485);
#18392=PLANE('',#84486);
#18393=PLANE('',#84487);
#18394=PLANE('',#84488);
#18395=PLANE('',#84489);
#18396=PLANE('',#84490);
#18397=PLANE('',#84491);
#18398=PLANE('',#84492);
#18399=PLANE('',#84493);
#18400=PLANE('',#84494);
#18401=PLANE('',#84495);
#18402=PLANE('',#84496);
#18403=PLANE('',#84497);
#18404=PLANE('',#84498);
#18405=PLANE('',#84499);
#18406=PLANE('',#84500);
#18407=PLANE('',#84501);
#18408=PLANE('',#84502);
#18409=PLANE('',#84503);
#18410=PLANE('',#84504);
#18411=PLANE('',#84505);
#18412=PLANE('',#84506);
#18413=PLANE('',#84507);
#18414=PLANE('',#84508);
#18415=PLANE('',#84509);
#18416=PLANE('',#84510);
#18417=PLANE('',#84511);
#18418=PLANE('',#84512);
#18419=PLANE('',#84513);
#18420=PLANE('',#84514);
#18421=PLANE('',#84515);
#18422=PLANE('',#84516);
#18423=PLANE('',#84517);
#18424=PLANE('',#84518);
#18425=PLANE('',#84519);
#18426=PLANE('',#84520);
#18427=PLANE('',#84521);
#18428=PLANE('',#84522);
#18429=PLANE('',#84523);
#18430=PLANE('',#84524);
#18431=PLANE('',#84525);
#18432=PLANE('',#84526);
#18433=PLANE('',#84527);
#18434=PLANE('',#84528);
#18435=PLANE('',#84529);
#18436=PLANE('',#84530);
#18437=PLANE('',#84531);
#18438=PLANE('',#84532);
#18439=PLANE('',#84533);
#18440=PLANE('',#84534);
#18441=PLANE('',#84535);
#18442=PLANE('',#84536);
#18443=PLANE('',#84537);
#18444=PLANE('',#84538);
#18445=PLANE('',#84539);
#18446=PLANE('',#84540);
#18447=PLANE('',#84541);
#18448=PLANE('',#84542);
#18449=PLANE('',#84543);
#18450=PLANE('',#84544);
#18451=PLANE('',#84545);
#18452=PLANE('',#84546);
#18453=PLANE('',#84547);
#18454=PLANE('',#84548);
#18455=PLANE('',#84549);
#18456=PLANE('',#84550);
#18457=PLANE('',#84551);
#18458=PLANE('',#84552);
#18459=PLANE('',#84553);
#18460=PLANE('',#84554);
#18461=PLANE('',#84555);
#18462=PLANE('',#84556);
#18463=PLANE('',#84557);
#18464=PLANE('',#84558);
#18465=PLANE('',#84559);
#18466=PLANE('',#84560);
#18467=PLANE('',#84561);
#18468=PLANE('',#84562);
#18469=PLANE('',#84563);
#18470=PLANE('',#84564);
#18471=PLANE('',#84565);
#18472=PLANE('',#84566);
#18473=PLANE('',#84567);
#18474=PLANE('',#84568);
#18475=PLANE('',#84569);
#18476=PLANE('',#84570);
#18477=PLANE('',#84571);
#18478=PLANE('',#84572);
#18479=PLANE('',#84573);
#18480=PLANE('',#84574);
#18481=PLANE('',#84575);
#18482=PLANE('',#84576);
#18483=PLANE('',#84577);
#18484=PLANE('',#84578);
#18485=PLANE('',#84579);
#18486=PLANE('',#84580);
#18487=PLANE('',#84581);
#18488=PLANE('',#84582);
#18489=PLANE('',#84583);
#18490=PLANE('',#84584);
#18491=PLANE('',#84585);
#18492=PLANE('',#84586);
#18493=PLANE('',#84587);
#18494=PLANE('',#84588);
#18495=PLANE('',#84589);
#18496=PLANE('',#84590);
#18497=PLANE('',#84591);
#18498=PLANE('',#84592);
#18499=PLANE('',#84593);
#18500=PLANE('',#84594);
#18501=PLANE('',#84595);
#18502=PLANE('',#84596);
#18503=PLANE('',#84597);
#18504=PLANE('',#84598);
#18505=PLANE('',#84599);
#18506=PLANE('',#84600);
#18507=PLANE('',#84601);
#18508=PLANE('',#84602);
#18509=PLANE('',#84603);
#18510=PLANE('',#84604);
#18511=PLANE('',#84605);
#18512=PLANE('',#84606);
#18513=PLANE('',#84607);
#18514=PLANE('',#84608);
#18515=PLANE('',#84609);
#18516=PLANE('',#84610);
#18517=PLANE('',#84611);
#18518=PLANE('',#84612);
#18519=PLANE('',#84613);
#18520=PLANE('',#84614);
#18521=PLANE('',#84615);
#18522=PLANE('',#84616);
#18523=PLANE('',#84617);
#18524=PLANE('',#84618);
#18525=PLANE('',#84619);
#18526=PLANE('',#84620);
#18527=PLANE('',#84621);
#18528=PLANE('',#84622);
#18529=PLANE('',#84623);
#18530=PLANE('',#84624);
#18531=PLANE('',#84625);
#18532=PLANE('',#84626);
#18533=PLANE('',#84627);
#18534=PLANE('',#84628);
#18535=PLANE('',#84629);
#18536=PLANE('',#84630);
#18537=PLANE('',#84631);
#18538=PLANE('',#84632);
#18539=PLANE('',#84633);
#18540=PLANE('',#84634);
#18541=PLANE('',#84635);
#18542=PLANE('',#84636);
#18543=PLANE('',#84637);
#18544=PLANE('',#84638);
#18545=PLANE('',#84639);
#18546=PLANE('',#84640);
#18547=PLANE('',#84641);
#18548=PLANE('',#84642);
#18549=PLANE('',#84643);
#18550=PLANE('',#84644);
#18551=PLANE('',#84645);
#18552=PLANE('',#84646);
#18553=PLANE('',#84647);
#18554=PLANE('',#84648);
#18555=PLANE('',#84649);
#18556=PLANE('',#84650);
#18557=PLANE('',#84651);
#18558=PLANE('',#84652);
#18559=PLANE('',#84653);
#18560=PLANE('',#84654);
#18561=PLANE('',#84655);
#18562=PLANE('',#84656);
#18563=PLANE('',#84657);
#18564=PLANE('',#84658);
#18565=PLANE('',#84659);
#18566=PLANE('',#84660);
#18567=PLANE('',#84661);
#18568=PLANE('',#84662);
#18569=PLANE('',#84663);
#18570=PLANE('',#84664);
#18571=PLANE('',#84665);
#18572=PLANE('',#84666);
#18573=PLANE('',#84667);
#18574=PLANE('',#84668);
#18575=PLANE('',#84669);
#18576=PLANE('',#84670);
#18577=PLANE('',#84671);
#18578=PLANE('',#84672);
#18579=PLANE('',#84673);
#18580=PLANE('',#84674);
#18581=PLANE('',#84675);
#18582=PLANE('',#84676);
#18583=PLANE('',#84677);
#18584=PLANE('',#84678);
#18585=PLANE('',#84679);
#18586=PLANE('',#84680);
#18587=PLANE('',#84681);
#18588=PLANE('',#84682);
#18589=PLANE('',#84683);
#18590=PLANE('',#84684);
#18591=PLANE('',#84685);
#18592=PLANE('',#84686);
#18593=PLANE('',#84687);
#18594=PLANE('',#84688);
#18595=PLANE('',#84689);
#18596=PLANE('',#84690);
#18597=PLANE('',#84691);
#18598=PLANE('',#84692);
#18599=PLANE('',#84693);
#18600=PLANE('',#84694);
#18601=PLANE('',#84695);
#18602=PLANE('',#84696);
#18603=PLANE('',#84697);
#18604=PLANE('',#84698);
#18605=PLANE('',#84699);
#18606=PLANE('',#84700);
#18607=PLANE('',#84701);
#18608=PLANE('',#84702);
#18609=PLANE('',#84703);
#18610=PLANE('',#84704);
#18611=PLANE('',#84705);
#18612=PLANE('',#84706);
#18613=PLANE('',#84707);
#18614=PLANE('',#84708);
#18615=PLANE('',#84709);
#18616=PLANE('',#84710);
#18617=PLANE('',#84711);
#18618=PLANE('',#84712);
#18619=PLANE('',#84713);
#18620=PLANE('',#84714);
#18621=PLANE('',#84715);
#18622=PLANE('',#84716);
#18623=PLANE('',#84717);
#18624=PLANE('',#84718);
#18625=PLANE('',#84719);
#18626=PLANE('',#84720);
#18627=PLANE('',#84721);
#18628=PLANE('',#84722);
#18629=PLANE('',#84723);
#18630=PLANE('',#84724);
#18631=PLANE('',#84725);
#18632=PLANE('',#84726);
#18633=PLANE('',#84727);
#18634=PLANE('',#84728);
#18635=PLANE('',#84729);
#18636=PLANE('',#84730);
#18637=PLANE('',#84731);
#18638=PLANE('',#84732);
#18639=PLANE('',#84733);
#18640=PLANE('',#84734);
#18641=PLANE('',#84735);
#18642=PLANE('',#84736);
#18643=PLANE('',#84737);
#18644=PLANE('',#84738);
#18645=PLANE('',#84739);
#18646=PLANE('',#84740);
#18647=PLANE('',#84741);
#18648=PLANE('',#84742);
#18649=PLANE('',#84743);
#18650=PLANE('',#84744);
#18651=PLANE('',#84745);
#18652=PLANE('',#84746);
#18653=PLANE('',#84747);
#18654=PLANE('',#84748);
#18655=PLANE('',#84749);
#18656=PLANE('',#84750);
#18657=PLANE('',#84751);
#18658=PLANE('',#84752);
#18659=PLANE('',#84753);
#18660=PLANE('',#84754);
#18661=PLANE('',#84755);
#18662=PLANE('',#84756);
#18663=PLANE('',#84757);
#18664=PLANE('',#84758);
#18665=PLANE('',#84759);
#18666=PLANE('',#84760);
#18667=PLANE('',#84761);
#18668=PLANE('',#84762);
#18669=PLANE('',#84763);
#18670=PLANE('',#84764);
#18671=PLANE('',#84765);
#18672=PLANE('',#84766);
#18673=PLANE('',#84767);
#18674=PLANE('',#84768);
#18675=PLANE('',#84769);
#18676=PLANE('',#84770);
#18677=PLANE('',#84771);
#18678=PLANE('',#84772);
#18679=PLANE('',#84773);
#18680=PLANE('',#84774);
#18681=PLANE('',#84775);
#18682=PLANE('',#84776);
#18683=PLANE('',#84777);
#18684=PLANE('',#84778);
#18685=PLANE('',#84779);
#18686=PLANE('',#84780);
#18687=PLANE('',#84781);
#18688=PLANE('',#84782);
#18689=PLANE('',#84783);
#18690=PLANE('',#84784);
#18691=PLANE('',#84785);
#18692=PLANE('',#84786);
#18693=PLANE('',#84787);
#18694=PLANE('',#84788);
#18695=PLANE('',#84789);
#18696=PLANE('',#84790);
#18697=PLANE('',#84791);
#18698=PLANE('',#84792);
#18699=PLANE('',#84793);
#18700=PLANE('',#84794);
#18701=PLANE('',#84795);
#18702=PLANE('',#84796);
#18703=PLANE('',#84797);
#18704=PLANE('',#84798);
#18705=PLANE('',#84799);
#18706=PLANE('',#84800);
#18707=PLANE('',#84801);
#18708=PLANE('',#84802);
#18709=PLANE('',#84803);
#18710=PLANE('',#84804);
#18711=PLANE('',#84805);
#18712=PLANE('',#84806);
#18713=PLANE('',#84807);
#18714=PLANE('',#84808);
#18715=PLANE('',#84809);
#18716=PLANE('',#84810);
#18717=PLANE('',#84811);
#18718=PLANE('',#84812);
#18719=PLANE('',#84813);
#18720=PLANE('',#84814);
#18721=PLANE('',#84815);
#18722=PLANE('',#84816);
#18723=PLANE('',#84817);
#18724=PLANE('',#84818);
#18725=PLANE('',#84819);
#18726=PLANE('',#84820);
#18727=PLANE('',#84821);
#18728=PLANE('',#84822);
#18729=PLANE('',#84823);
#18730=PLANE('',#84824);
#18731=PLANE('',#84825);
#18732=PLANE('',#84826);
#18733=PLANE('',#84827);
#18734=PLANE('',#84828);
#18735=PLANE('',#84829);
#18736=PLANE('',#84830);
#18737=PLANE('',#84831);
#18738=PLANE('',#84832);
#18739=PLANE('',#84833);
#18740=PLANE('',#84834);
#18741=PLANE('',#84835);
#18742=PLANE('',#84836);
#18743=PLANE('',#84837);
#18744=PLANE('',#84838);
#18745=PLANE('',#84839);
#18746=PLANE('',#84840);
#18747=PLANE('',#84841);
#18748=PLANE('',#84842);
#18749=PLANE('',#84843);
#18750=PLANE('',#84844);
#18751=PLANE('',#84845);
#18752=PLANE('',#84846);
#18753=PLANE('',#84847);
#18754=PLANE('',#84848);
#18755=PLANE('',#84849);
#18756=PLANE('',#84850);
#18757=PLANE('',#84851);
#18758=PLANE('',#84852);
#18759=PLANE('',#84853);
#18760=PLANE('',#84854);
#18761=PLANE('',#84855);
#18762=PLANE('',#84856);
#18763=PLANE('',#84857);
#18764=PLANE('',#84858);
#18765=PLANE('',#84859);
#18766=PLANE('',#84860);
#18767=PLANE('',#84861);
#18768=PLANE('',#84862);
#18769=PLANE('',#84863);
#18770=PLANE('',#84864);
#18771=PLANE('',#84865);
#18772=PLANE('',#84866);
#18773=PLANE('',#84867);
#18774=PLANE('',#84868);
#18775=PLANE('',#84869);
#18776=PLANE('',#84870);
#18777=PLANE('',#84871);
#18778=PLANE('',#84872);
#18779=PLANE('',#84873);
#18780=PLANE('',#84874);
#18781=PLANE('',#84875);
#18782=PLANE('',#84876);
#18783=PLANE('',#84877);
#18784=PLANE('',#84878);
#18785=PLANE('',#84879);
#18786=PLANE('',#84880);
#18787=PLANE('',#84881);
#18788=PLANE('',#84882);
#18789=PLANE('',#84883);
#18790=PLANE('',#84884);
#18791=PLANE('',#84885);
#18792=PLANE('',#84886);
#18793=PLANE('',#84887);
#18794=PLANE('',#84888);
#18795=PLANE('',#84889);
#18796=PLANE('',#84890);
#18797=PLANE('',#84891);
#18798=PLANE('',#84892);
#18799=PLANE('',#84893);
#18800=PLANE('',#84894);
#18801=PLANE('',#84895);
#18802=PLANE('',#84896);
#18803=PLANE('',#84897);
#18804=PLANE('',#84898);
#18805=PLANE('',#84899);
#18806=PLANE('',#84900);
#18807=PLANE('',#84901);
#18808=PLANE('',#84902);
#18809=PLANE('',#84903);
#18810=PLANE('',#84904);
#18811=PLANE('',#84905);
#18812=PLANE('',#84906);
#18813=PLANE('',#84907);
#18814=PLANE('',#84908);
#18815=PLANE('',#84909);
#18816=PLANE('',#84910);
#18817=PLANE('',#84911);
#18818=PLANE('',#84912);
#18819=PLANE('',#84913);
#18820=PLANE('',#84914);
#18821=PLANE('',#84915);
#18822=PLANE('',#84916);
#18823=PLANE('',#84917);
#18824=PLANE('',#84918);
#18825=PLANE('',#84919);
#18826=PLANE('',#84920);
#18827=PLANE('',#84921);
#18828=PLANE('',#84922);
#18829=PLANE('',#84923);
#18830=PLANE('',#84924);
#18831=PLANE('',#84925);
#18832=PLANE('',#84926);
#18833=PLANE('',#84927);
#18834=PLANE('',#84928);
#18835=PLANE('',#84929);
#18836=PLANE('',#84930);
#18837=PLANE('',#84931);
#18838=PLANE('',#84932);
#18839=PLANE('',#84933);
#18840=PLANE('',#84934);
#18841=PLANE('',#84935);
#18842=PLANE('',#84936);
#18843=PLANE('',#84937);
#18844=PLANE('',#84938);
#18845=PLANE('',#84939);
#18846=PLANE('',#84940);
#18847=PLANE('',#84941);
#18848=PLANE('',#84942);
#18849=PLANE('',#84943);
#18850=PLANE('',#84944);
#18851=PLANE('',#84945);
#18852=PLANE('',#84946);
#18853=PLANE('',#84947);
#18854=PLANE('',#84948);
#18855=PLANE('',#84949);
#18856=PLANE('',#84950);
#18857=PLANE('',#84951);
#18858=PLANE('',#84952);
#18859=PLANE('',#84953);
#18860=PLANE('',#84954);
#18861=PLANE('',#84955);
#18862=PLANE('',#84956);
#18863=PLANE('',#84957);
#18864=PLANE('',#84958);
#18865=PLANE('',#84959);
#18866=PLANE('',#84960);
#18867=PLANE('',#84961);
#18868=PLANE('',#84962);
#18869=PLANE('',#84963);
#18870=PLANE('',#84964);
#18871=PLANE('',#84965);
#18872=PLANE('',#84966);
#18873=PLANE('',#84967);
#18874=PLANE('',#84968);
#18875=PLANE('',#84969);
#18876=PLANE('',#84970);
#18877=PLANE('',#84971);
#18878=PLANE('',#84972);
#18879=PLANE('',#84973);
#18880=PLANE('',#84974);
#18881=PLANE('',#84975);
#18882=PLANE('',#84976);
#18883=PLANE('',#84977);
#18884=PLANE('',#84978);
#18885=PLANE('',#84979);
#18886=PLANE('',#84980);
#18887=PLANE('',#84981);
#18888=PLANE('',#84982);
#18889=PLANE('',#84983);
#18890=PLANE('',#84984);
#18891=PLANE('',#84985);
#18892=PLANE('',#84986);
#18893=PLANE('',#84987);
#18894=PLANE('',#84988);
#18895=PLANE('',#84989);
#18896=PLANE('',#84990);
#18897=PLANE('',#84991);
#18898=PLANE('',#84992);
#18899=PLANE('',#84993);
#18900=PLANE('',#84994);
#18901=PLANE('',#84995);
#18902=PLANE('',#84996);
#18903=PLANE('',#84997);
#18904=PLANE('',#84998);
#18905=PLANE('',#84999);
#18906=PLANE('',#85000);
#18907=PLANE('',#85001);
#18908=PLANE('',#85002);
#18909=PLANE('',#85003);
#18910=PLANE('',#85004);
#18911=PLANE('',#85005);
#18912=PLANE('',#85006);
#18913=PLANE('',#85007);
#18914=PLANE('',#85008);
#18915=PLANE('',#85009);
#18916=PLANE('',#85010);
#18917=PLANE('',#85011);
#18918=PLANE('',#85012);
#18919=PLANE('',#85013);
#18920=PLANE('',#85014);
#18921=PLANE('',#85015);
#18922=PLANE('',#85016);
#18923=PLANE('',#85017);
#18924=PLANE('',#85018);
#18925=PLANE('',#85019);
#18926=PLANE('',#85020);
#18927=PLANE('',#85021);
#18928=PLANE('',#85022);
#18929=PLANE('',#85023);
#18930=PLANE('',#85024);
#18931=PLANE('',#85025);
#18932=PLANE('',#85026);
#18933=PLANE('',#85027);
#18934=PLANE('',#85028);
#18935=PLANE('',#85029);
#18936=PLANE('',#85030);
#18937=PLANE('',#85031);
#18938=PLANE('',#85032);
#18939=PLANE('',#85033);
#18940=PLANE('',#85034);
#18941=PLANE('',#85035);
#18942=PLANE('',#85036);
#18943=PLANE('',#85037);
#18944=PLANE('',#85038);
#18945=PLANE('',#85039);
#18946=PLANE('',#85040);
#18947=PLANE('',#85041);
#18948=PLANE('',#85042);
#18949=PLANE('',#85043);
#18950=PLANE('',#85044);
#18951=PLANE('',#85045);
#18952=PLANE('',#85046);
#18953=PLANE('',#85047);
#18954=PLANE('',#85048);
#18955=PLANE('',#85049);
#18956=PLANE('',#85050);
#18957=PLANE('',#85051);
#18958=PLANE('',#85052);
#18959=PLANE('',#85053);
#18960=PLANE('',#85054);
#18961=PLANE('',#85055);
#18962=PLANE('',#85056);
#18963=PLANE('',#85057);
#18964=PLANE('',#85058);
#18965=PLANE('',#85059);
#18966=PLANE('',#85060);
#18967=PLANE('',#85061);
#18968=PLANE('',#85062);
#18969=PLANE('',#85063);
#18970=PLANE('',#85064);
#18971=PLANE('',#85065);
#18972=PLANE('',#85066);
#18973=PLANE('',#85067);
#18974=PLANE('',#85068);
#18975=PLANE('',#85069);
#18976=PLANE('',#85070);
#18977=PLANE('',#85071);
#18978=PLANE('',#85072);
#18979=PLANE('',#85073);
#18980=PLANE('',#85074);
#18981=PLANE('',#85075);
#18982=PLANE('',#85076);
#18983=PLANE('',#85077);
#18984=PLANE('',#85078);
#18985=PLANE('',#85079);
#18986=PLANE('',#85080);
#18987=PLANE('',#85081);
#18988=PLANE('',#85082);
#18989=PLANE('',#85083);
#18990=PLANE('',#85084);
#18991=PLANE('',#85085);
#18992=PLANE('',#85086);
#18993=PLANE('',#85087);
#18994=PLANE('',#85088);
#18995=PLANE('',#85089);
#18996=PLANE('',#85090);
#18997=PLANE('',#85091);
#18998=PLANE('',#85092);
#18999=PLANE('',#85093);
#19000=PLANE('',#85094);
#19001=PLANE('',#85095);
#19002=PLANE('',#85096);
#19003=PLANE('',#85097);
#19004=PLANE('',#85098);
#19005=PLANE('',#85099);
#19006=PLANE('',#85100);
#19007=PLANE('',#85101);
#19008=PLANE('',#85102);
#19009=PLANE('',#85103);
#19010=PLANE('',#85104);
#19011=PLANE('',#85105);
#19012=PLANE('',#85106);
#19013=PLANE('',#85107);
#19014=PLANE('',#85108);
#19015=PLANE('',#85109);
#19016=PLANE('',#85110);
#19017=PLANE('',#85111);
#19018=PLANE('',#85112);
#19019=PLANE('',#85113);
#19020=PLANE('',#85114);
#19021=PLANE('',#85115);
#19022=PLANE('',#85116);
#19023=PLANE('',#85117);
#19024=PLANE('',#85118);
#19025=PLANE('',#85119);
#19026=PLANE('',#85120);
#19027=PLANE('',#85121);
#19028=PLANE('',#85122);
#19029=PLANE('',#85123);
#19030=PLANE('',#85124);
#19031=PLANE('',#85125);
#19032=PLANE('',#85126);
#19033=PLANE('',#85127);
#19034=PLANE('',#85128);
#19035=PLANE('',#85129);
#19036=PLANE('',#85130);
#19037=PLANE('',#85131);
#19038=PLANE('',#85132);
#19039=PLANE('',#85133);
#19040=PLANE('',#85134);
#19041=PLANE('',#85135);
#19042=PLANE('',#85136);
#19043=PLANE('',#85137);
#19044=PLANE('',#85138);
#19045=PLANE('',#85139);
#19046=PLANE('',#85140);
#19047=PLANE('',#85141);
#19048=PLANE('',#85142);
#19049=PLANE('',#85143);
#19050=PLANE('',#85144);
#19051=PLANE('',#85145);
#19052=PLANE('',#85146);
#19053=PLANE('',#85147);
#19054=PLANE('',#85148);
#19055=PLANE('',#85149);
#19056=PLANE('',#85150);
#19057=PLANE('',#85151);
#19058=PLANE('',#85152);
#19059=PLANE('',#85153);
#19060=PLANE('',#85154);
#19061=PLANE('',#85155);
#19062=PLANE('',#85156);
#19063=PLANE('',#85157);
#19064=PLANE('',#85158);
#19065=PLANE('',#85159);
#19066=PLANE('',#85160);
#19067=PLANE('',#85161);
#19068=PLANE('',#85162);
#19069=PLANE('',#85163);
#19070=PLANE('',#85164);
#19071=PLANE('',#85165);
#19072=PLANE('',#85166);
#19073=PLANE('',#85167);
#19074=PLANE('',#85168);
#19075=PLANE('',#85169);
#19076=PLANE('',#85170);
#19077=PLANE('',#85171);
#19078=PLANE('',#85172);
#19079=PLANE('',#85173);
#19080=PLANE('',#85174);
#19081=PLANE('',#85175);
#19082=PLANE('',#85176);
#19083=PLANE('',#85177);
#19084=PLANE('',#85178);
#19085=PLANE('',#85179);
#19086=PLANE('',#85180);
#19087=PLANE('',#85181);
#19088=PLANE('',#85182);
#19089=PLANE('',#85183);
#19090=PLANE('',#85184);
#19091=PLANE('',#85185);
#19092=PLANE('',#85186);
#19093=PLANE('',#85187);
#19094=PLANE('',#85188);
#19095=PLANE('',#85189);
#19096=PLANE('',#85190);
#19097=PLANE('',#85191);
#19098=PLANE('',#85192);
#19099=PLANE('',#85193);
#19100=PLANE('',#85194);
#19101=PLANE('',#85195);
#19102=PLANE('',#85196);
#19103=PLANE('',#85197);
#19104=PLANE('',#85198);
#19105=PLANE('',#85199);
#19106=PLANE('',#85200);
#19107=PLANE('',#85201);
#19108=PLANE('',#85202);
#19109=PLANE('',#85203);
#19110=PLANE('',#85204);
#19111=PLANE('',#85205);
#19112=PLANE('',#85206);
#19113=PLANE('',#85207);
#19114=PLANE('',#85208);
#19115=PLANE('',#85209);
#19116=PLANE('',#85210);
#19117=PLANE('',#85211);
#19118=PLANE('',#85212);
#19119=PLANE('',#85213);
#19120=PLANE('',#85214);
#19121=PLANE('',#85215);
#19122=PLANE('',#85216);
#19123=PLANE('',#85217);
#19124=PLANE('',#85218);
#19125=PLANE('',#85219);
#19126=PLANE('',#85220);
#19127=PLANE('',#85221);
#19128=PLANE('',#85222);
#19129=PLANE('',#85223);
#19130=PLANE('',#85224);
#19131=PLANE('',#85225);
#19132=PLANE('',#85226);
#19133=PLANE('',#85227);
#19134=PLANE('',#85228);
#19135=PLANE('',#85229);
#19136=PLANE('',#85230);
#19137=PLANE('',#85231);
#19138=PLANE('',#85232);
#19139=PLANE('',#85233);
#19140=PLANE('',#85234);
#19141=PLANE('',#85235);
#19142=PLANE('',#85236);
#19143=PLANE('',#85237);
#19144=PLANE('',#85238);
#19145=PLANE('',#85239);
#19146=PLANE('',#85240);
#19147=PLANE('',#85241);
#19148=PLANE('',#85242);
#19149=PLANE('',#85243);
#19150=PLANE('',#85244);
#19151=PLANE('',#85245);
#19152=PLANE('',#85246);
#19153=PLANE('',#85247);
#19154=PLANE('',#85248);
#19155=PLANE('',#85249);
#19156=PLANE('',#85250);
#19157=PLANE('',#85251);
#19158=PLANE('',#85252);
#19159=PLANE('',#85253);
#19160=PLANE('',#85254);
#19161=PLANE('',#85255);
#19162=PLANE('',#85256);
#19163=PLANE('',#85257);
#19164=PLANE('',#85258);
#19165=PLANE('',#85259);
#19166=PLANE('',#85260);
#19167=PLANE('',#85261);
#19168=PLANE('',#85262);
#19169=PLANE('',#85263);
#19170=PLANE('',#85264);
#19171=PLANE('',#85265);
#19172=PLANE('',#85266);
#19173=PLANE('',#85267);
#19174=PLANE('',#85268);
#19175=PLANE('',#85269);
#19176=PLANE('',#85270);
#19177=PLANE('',#85271);
#19178=PLANE('',#85272);
#19179=PLANE('',#85273);
#19180=PLANE('',#85274);
#19181=PLANE('',#85275);
#19182=PLANE('',#85276);
#19183=PLANE('',#85277);
#19184=PLANE('',#85278);
#19185=PLANE('',#85279);
#19186=PLANE('',#85280);
#19187=PLANE('',#85281);
#19188=PLANE('',#85282);
#19189=PLANE('',#85283);
#19190=PLANE('',#85284);
#19191=PLANE('',#85285);
#19192=PLANE('',#85286);
#19193=PLANE('',#85287);
#19194=PLANE('',#85288);
#19195=PLANE('',#85289);
#19196=PLANE('',#85290);
#19197=PLANE('',#85291);
#19198=PLANE('',#85292);
#19199=PLANE('',#85293);
#19200=PLANE('',#85294);
#19201=PLANE('',#85295);
#19202=PLANE('',#85296);
#19203=PLANE('',#85297);
#19204=PLANE('',#85298);
#19205=PLANE('',#85299);
#19206=PLANE('',#85300);
#19207=PLANE('',#85301);
#19208=PLANE('',#85302);
#19209=PLANE('',#85303);
#19210=PLANE('',#85304);
#19211=PLANE('',#85305);
#19212=PLANE('',#85306);
#19213=PLANE('',#85307);
#19214=PLANE('',#85308);
#19215=PLANE('',#85309);
#19216=PLANE('',#85310);
#19217=PLANE('',#85311);
#19218=PLANE('',#85312);
#19219=PLANE('',#85313);
#19220=PLANE('',#85314);
#19221=PLANE('',#85315);
#19222=PLANE('',#85316);
#19223=PLANE('',#85317);
#19224=PLANE('',#85318);
#19225=PLANE('',#85319);
#19226=PLANE('',#85320);
#19227=PLANE('',#85321);
#19228=PLANE('',#85322);
#19229=PLANE('',#85323);
#19230=PLANE('',#85324);
#19231=PLANE('',#85325);
#19232=PLANE('',#85326);
#19233=PLANE('',#85327);
#19234=PLANE('',#85328);
#19235=PLANE('',#85329);
#19236=PLANE('',#85330);
#19237=PLANE('',#85331);
#19238=PLANE('',#85332);
#19239=PLANE('',#85333);
#19240=PLANE('',#85334);
#19241=PLANE('',#85335);
#19242=PLANE('',#85336);
#19243=PLANE('',#85337);
#19244=PLANE('',#85338);
#19245=PLANE('',#85339);
#19246=PLANE('',#85340);
#19247=PLANE('',#85341);
#19248=PLANE('',#85342);
#19249=PLANE('',#85343);
#19250=PLANE('',#85344);
#19251=PLANE('',#85345);
#19252=PLANE('',#85346);
#19253=PLANE('',#85347);
#19254=PLANE('',#85348);
#19255=PLANE('',#85349);
#19256=PLANE('',#85350);
#19257=PLANE('',#85351);
#19258=PLANE('',#85352);
#19259=PLANE('',#85353);
#19260=PLANE('',#85354);
#19261=PLANE('',#85355);
#19262=PLANE('',#85356);
#19263=PLANE('',#85357);
#19264=PLANE('',#85358);
#19265=PLANE('',#85359);
#19266=PLANE('',#85360);
#19267=PLANE('',#85361);
#19268=PLANE('',#85362);
#19269=PLANE('',#85363);
#19270=PLANE('',#85364);
#19271=PLANE('',#85365);
#19272=PLANE('',#85366);
#19273=PLANE('',#85367);
#19274=PLANE('',#85368);
#19275=PLANE('',#85369);
#19276=PLANE('',#85370);
#19277=PLANE('',#85371);
#19278=PLANE('',#85372);
#19279=PLANE('',#85373);
#19280=PLANE('',#85374);
#19281=PLANE('',#85375);
#19282=PLANE('',#85376);
#19283=PLANE('',#85377);
#19284=PLANE('',#85378);
#19285=PLANE('',#85379);
#19286=PLANE('',#85380);
#19287=PLANE('',#85381);
#19288=PLANE('',#85382);
#19289=PLANE('',#85383);
#19290=PLANE('',#85384);
#19291=PLANE('',#85385);
#19292=PLANE('',#85386);
#19293=PLANE('',#85387);
#19294=PLANE('',#85388);
#19295=PLANE('',#85389);
#19296=PLANE('',#85390);
#19297=PLANE('',#85391);
#19298=PLANE('',#85392);
#19299=PLANE('',#85393);
#19300=PLANE('',#85394);
#19301=PLANE('',#85395);
#19302=PLANE('',#85396);
#19303=PLANE('',#85397);
#19304=PLANE('',#85398);
#19305=PLANE('',#85399);
#19306=PLANE('',#85400);
#19307=PLANE('',#85401);
#19308=PLANE('',#85402);
#19309=PLANE('',#85403);
#19310=PLANE('',#85404);
#19311=PLANE('',#85405);
#19312=PLANE('',#85406);
#19313=PLANE('',#85407);
#19314=PLANE('',#85408);
#19315=PLANE('',#85409);
#19316=PLANE('',#85410);
#19317=PLANE('',#85411);
#19318=PLANE('',#85412);
#19319=PLANE('',#85413);
#19320=PLANE('',#85414);
#19321=PLANE('',#85415);
#19322=PLANE('',#85416);
#19323=PLANE('',#85417);
#19324=PLANE('',#85418);
#19325=PLANE('',#85419);
#19326=PLANE('',#85420);
#19327=PLANE('',#85421);
#19328=PLANE('',#85422);
#19329=PLANE('',#85423);
#19330=PLANE('',#85424);
#19331=PLANE('',#85425);
#19332=PLANE('',#85426);
#19333=PLANE('',#85427);
#19334=PLANE('',#85428);
#19335=PLANE('',#85429);
#19336=PLANE('',#85430);
#19337=PLANE('',#85431);
#19338=PLANE('',#85432);
#19339=PLANE('',#85433);
#19340=PLANE('',#85434);
#19341=PLANE('',#85435);
#19342=PLANE('',#85436);
#19343=PLANE('',#85437);
#19344=PLANE('',#85438);
#19345=PLANE('',#85439);
#19346=PLANE('',#85440);
#19347=PLANE('',#85441);
#19348=PLANE('',#85442);
#19349=PLANE('',#85443);
#19350=PLANE('',#85444);
#19351=PLANE('',#85445);
#19352=PLANE('',#85446);
#19353=PLANE('',#85447);
#19354=PLANE('',#85448);
#19355=PLANE('',#85449);
#19356=PLANE('',#85450);
#19357=PLANE('',#85451);
#19358=PLANE('',#85452);
#19359=PLANE('',#85453);
#19360=PLANE('',#85454);
#19361=PLANE('',#85455);
#19362=PLANE('',#85456);
#19363=PLANE('',#85457);
#19364=PLANE('',#85458);
#19365=PLANE('',#85459);
#19366=PLANE('',#85460);
#19367=PLANE('',#85461);
#19368=PLANE('',#85462);
#19369=PLANE('',#85463);
#19370=PLANE('',#85464);
#19371=PLANE('',#85465);
#19372=PLANE('',#85466);
#19373=PLANE('',#85467);
#19374=PLANE('',#85468);
#19375=PLANE('',#85469);
#19376=PLANE('',#85470);
#19377=PLANE('',#85471);
#19378=PLANE('',#85472);
#19379=PLANE('',#85473);
#19380=PLANE('',#85474);
#19381=PLANE('',#85475);
#19382=PLANE('',#85476);
#19383=PLANE('',#85477);
#19384=PLANE('',#85478);
#19385=PLANE('',#85479);
#19386=PLANE('',#85480);
#19387=PLANE('',#85481);
#19388=PLANE('',#85482);
#19389=PLANE('',#85483);
#19390=PLANE('',#85484);
#19391=PLANE('',#85485);
#19392=PLANE('',#85486);
#19393=PLANE('',#85487);
#19394=PLANE('',#85488);
#19395=PLANE('',#85489);
#19396=PLANE('',#85490);
#19397=PLANE('',#85491);
#19398=PLANE('',#85492);
#19399=PLANE('',#85493);
#19400=PLANE('',#85494);
#19401=PLANE('',#85495);
#19402=PLANE('',#85496);
#19403=PLANE('',#85497);
#19404=PLANE('',#85498);
#19405=PLANE('',#85499);
#19406=PLANE('',#85500);
#19407=PLANE('',#85501);
#19408=PLANE('',#85502);
#19409=PLANE('',#85503);
#19410=PLANE('',#85504);
#19411=PLANE('',#85505);
#19412=PLANE('',#85506);
#19413=PLANE('',#85507);
#19414=PLANE('',#85508);
#19415=PLANE('',#85509);
#19416=PLANE('',#85510);
#19417=PLANE('',#85511);
#19418=PLANE('',#85512);
#19419=PLANE('',#85513);
#19420=PLANE('',#85514);
#19421=PLANE('',#85515);
#19422=PLANE('',#85516);
#19423=PLANE('',#85517);
#19424=PLANE('',#85518);
#19425=PLANE('',#85519);
#19426=PLANE('',#85520);
#19427=PLANE('',#85521);
#19428=PLANE('',#85522);
#19429=PLANE('',#85523);
#19430=PLANE('',#85524);
#19431=PLANE('',#85525);
#19432=PLANE('',#85526);
#19433=PLANE('',#85527);
#19434=PLANE('',#85528);
#19435=PLANE('',#85529);
#19436=PLANE('',#85530);
#19437=PLANE('',#85531);
#19438=PLANE('',#85532);
#19439=PLANE('',#85533);
#19440=PLANE('',#85534);
#19441=PLANE('',#85535);
#19442=PLANE('',#85536);
#19443=PLANE('',#85537);
#19444=PLANE('',#85538);
#19445=PLANE('',#85539);
#19446=PLANE('',#85540);
#19447=PLANE('',#85541);
#19448=PLANE('',#85542);
#19449=PLANE('',#85543);
#19450=PLANE('',#85544);
#19451=PLANE('',#85545);
#19452=PLANE('',#85546);
#19453=PLANE('',#85547);
#19454=PLANE('',#85548);
#19455=PLANE('',#85549);
#19456=PLANE('',#85550);
#19457=PLANE('',#85551);
#19458=PLANE('',#85552);
#19459=PLANE('',#85553);
#19460=PLANE('',#85554);
#19461=PLANE('',#85555);
#19462=PLANE('',#85556);
#19463=PLANE('',#85557);
#19464=PLANE('',#85558);
#19465=PLANE('',#85559);
#19466=PLANE('',#85560);
#19467=PLANE('',#85561);
#19468=PLANE('',#85562);
#19469=PLANE('',#85563);
#19470=PLANE('',#85564);
#19471=PLANE('',#85565);
#19472=PLANE('',#85566);
#19473=PLANE('',#85567);
#19474=PLANE('',#85568);
#19475=PLANE('',#85569);
#19476=PLANE('',#85570);
#19477=PLANE('',#85571);
#19478=PLANE('',#85572);
#19479=PLANE('',#85573);
#19480=PLANE('',#85574);
#19481=PLANE('',#85575);
#19482=PLANE('',#85576);
#19483=PLANE('',#85577);
#19484=PLANE('',#85578);
#19485=PLANE('',#85579);
#19486=PLANE('',#85580);
#19487=PLANE('',#85581);
#19488=PLANE('',#85582);
#19489=PLANE('',#85583);
#19490=PLANE('',#85584);
#19491=PLANE('',#85585);
#19492=PLANE('',#85586);
#19493=PLANE('',#85587);
#19494=PLANE('',#85588);
#19495=PLANE('',#85589);
#19496=PLANE('',#85590);
#19497=PLANE('',#85591);
#19498=PLANE('',#85592);
#19499=PLANE('',#85593);
#19500=PLANE('',#85594);
#19501=PLANE('',#85595);
#19502=PLANE('',#85596);
#19503=PLANE('',#85597);
#19504=PLANE('',#85598);
#19505=PLANE('',#85599);
#19506=PLANE('',#85600);
#19507=PLANE('',#85601);
#19508=PLANE('',#85602);
#19509=PLANE('',#85603);
#19510=PLANE('',#85604);
#19511=PLANE('',#85605);
#19512=PLANE('',#85606);
#19513=PLANE('',#85607);
#19514=PLANE('',#85608);
#19515=PLANE('',#85609);
#19516=PLANE('',#85610);
#19517=PLANE('',#85611);
#19518=PLANE('',#85612);
#19519=PLANE('',#85613);
#19520=PLANE('',#85614);
#19521=PLANE('',#85615);
#19522=PLANE('',#85616);
#19523=PLANE('',#85617);
#19524=PLANE('',#85618);
#19525=PLANE('',#85619);
#19526=PLANE('',#85620);
#19527=PLANE('',#85621);
#19528=PLANE('',#85622);
#19529=PLANE('',#85623);
#19530=PLANE('',#85624);
#19531=PLANE('',#85625);
#19532=PLANE('',#85626);
#19533=PLANE('',#85627);
#19534=PLANE('',#85628);
#19535=PLANE('',#85629);
#19536=PLANE('',#85630);
#19537=PLANE('',#85631);
#19538=PLANE('',#85632);
#19539=PLANE('',#85633);
#19540=PLANE('',#85634);
#19541=PLANE('',#85635);
#19542=PLANE('',#85636);
#19543=PLANE('',#85637);
#19544=PLANE('',#85638);
#19545=PLANE('',#85639);
#19546=PLANE('',#85640);
#19547=PLANE('',#85641);
#19548=PLANE('',#85642);
#19549=PLANE('',#85643);
#19550=PLANE('',#85644);
#19551=PLANE('',#85645);
#19552=PLANE('',#85646);
#19553=PLANE('',#85647);
#19554=PLANE('',#85648);
#19555=PLANE('',#85649);
#19556=PLANE('',#85650);
#19557=PLANE('',#85651);
#19558=PLANE('',#85652);
#19559=PLANE('',#85653);
#19560=PLANE('',#85654);
#19561=PLANE('',#85655);
#19562=PLANE('',#85656);
#19563=PLANE('',#85657);
#19564=PLANE('',#85658);
#19565=PLANE('',#85659);
#19566=PLANE('',#85660);
#19567=PLANE('',#85661);
#19568=PLANE('',#85662);
#19569=PLANE('',#85663);
#19570=PLANE('',#85664);
#19571=PLANE('',#85665);
#19572=PLANE('',#85666);
#19573=PLANE('',#85667);
#19574=PLANE('',#85668);
#19575=PLANE('',#85669);
#19576=PLANE('',#85670);
#19577=PLANE('',#85671);
#19578=PLANE('',#85672);
#19579=PLANE('',#85673);
#19580=PLANE('',#85674);
#19581=PLANE('',#85675);
#19582=PLANE('',#85676);
#19583=PLANE('',#85677);
#19584=PLANE('',#85678);
#19585=PLANE('',#85679);
#19586=PLANE('',#85680);
#19587=PLANE('',#85681);
#19588=PLANE('',#85682);
#19589=PLANE('',#85683);
#19590=PLANE('',#85684);
#19591=PLANE('',#85685);
#19592=PLANE('',#85686);
#19593=PLANE('',#85687);
#19594=PLANE('',#85688);
#19595=PLANE('',#85689);
#19596=PLANE('',#85690);
#19597=PLANE('',#85691);
#19598=PLANE('',#85692);
#19599=PLANE('',#85693);
#19600=PLANE('',#85694);
#19601=PLANE('',#85695);
#19602=PLANE('',#85696);
#19603=PLANE('',#85697);
#19604=PLANE('',#85698);
#19605=PLANE('',#85699);
#19606=PLANE('',#85700);
#19607=PLANE('',#85701);
#19608=PLANE('',#85702);
#19609=PLANE('',#85703);
#19610=PLANE('',#85704);
#19611=PLANE('',#85705);
#19612=PLANE('',#85706);
#19613=PLANE('',#85707);
#19614=PLANE('',#85708);
#19615=PLANE('',#85709);
#19616=PLANE('',#85710);
#19617=PLANE('',#85711);
#19618=PLANE('',#85712);
#19619=PLANE('',#85713);
#19620=PLANE('',#85714);
#19621=PLANE('',#85715);
#19622=PLANE('',#85716);
#19623=PLANE('',#85717);
#19624=PLANE('',#85718);
#19625=PLANE('',#85719);
#19626=PLANE('',#85720);
#19627=PLANE('',#85721);
#19628=PLANE('',#85722);
#19629=PLANE('',#85723);
#19630=PLANE('',#85724);
#19631=PLANE('',#85725);
#19632=PLANE('',#85726);
#19633=PLANE('',#85727);
#19634=PLANE('',#85728);
#19635=PLANE('',#85729);
#19636=PLANE('',#85730);
#19637=PLANE('',#85731);
#19638=PLANE('',#85732);
#19639=PLANE('',#85733);
#19640=PLANE('',#85734);
#19641=PLANE('',#85735);
#19642=PLANE('',#85736);
#19643=PLANE('',#85737);
#19644=PLANE('',#85738);
#19645=PLANE('',#85739);
#19646=PLANE('',#85740);
#19647=PLANE('',#85741);
#19648=PLANE('',#85742);
#19649=PLANE('',#85743);
#19650=PLANE('',#85744);
#19651=PLANE('',#85745);
#19652=PLANE('',#85746);
#19653=PLANE('',#85747);
#19654=PLANE('',#85748);
#19655=PLANE('',#85749);
#19656=PLANE('',#85750);
#19657=PLANE('',#85751);
#19658=PLANE('',#85752);
#19659=PLANE('',#85753);
#19660=PLANE('',#85754);
#19661=PLANE('',#85755);
#19662=PLANE('',#85756);
#19663=PLANE('',#85757);
#19664=PLANE('',#85758);
#19665=PLANE('',#85759);
#19666=PLANE('',#85760);
#19667=PLANE('',#85761);
#19668=PLANE('',#85762);
#19669=PLANE('',#85763);
#19670=PLANE('',#85764);
#19671=PLANE('',#85765);
#19672=PLANE('',#85766);
#19673=PLANE('',#85767);
#19674=PLANE('',#85768);
#19675=PLANE('',#85769);
#19676=PLANE('',#85770);
#19677=PLANE('',#85771);
#19678=PLANE('',#85772);
#19679=PLANE('',#85773);
#19680=PLANE('',#85774);
#19681=PLANE('',#85775);
#19682=PLANE('',#85776);
#19683=PLANE('',#85777);
#19684=PLANE('',#85778);
#19685=PLANE('',#85779);
#19686=PLANE('',#85780);
#19687=PLANE('',#85781);
#19688=PLANE('',#85782);
#19689=PLANE('',#85783);
#19690=PLANE('',#85784);
#19691=PLANE('',#85785);
#19692=PLANE('',#85786);
#19693=PLANE('',#85787);
#19694=PLANE('',#85788);
#19695=PLANE('',#85789);
#19696=PLANE('',#85790);
#19697=PLANE('',#85791);
#19698=PLANE('',#85792);
#19699=PLANE('',#85793);
#19700=PLANE('',#85794);
#19701=PLANE('',#85795);
#19702=PLANE('',#85796);
#19703=PLANE('',#85797);
#19704=PLANE('',#85798);
#19705=PLANE('',#85799);
#19706=PLANE('',#85800);
#19707=PLANE('',#85801);
#19708=PLANE('',#85802);
#19709=PLANE('',#85803);
#19710=PLANE('',#85804);
#19711=PLANE('',#85805);
#19712=PLANE('',#85806);
#19713=PLANE('',#85807);
#19714=PLANE('',#85808);
#19715=PLANE('',#85809);
#19716=PLANE('',#85810);
#19717=PLANE('',#85811);
#19718=PLANE('',#85812);
#19719=PLANE('',#85813);
#19720=PLANE('',#85814);
#19721=PLANE('',#85815);
#19722=PLANE('',#85816);
#19723=PLANE('',#85817);
#19724=PLANE('',#85818);
#19725=PLANE('',#85819);
#19726=PLANE('',#85820);
#19727=PLANE('',#85821);
#19728=PLANE('',#85822);
#19729=PLANE('',#85823);
#19730=PLANE('',#85824);
#19731=PLANE('',#85825);
#19732=PLANE('',#85826);
#19733=PLANE('',#85827);
#19734=PLANE('',#85828);
#19735=PLANE('',#85829);
#19736=PLANE('',#85830);
#19737=PLANE('',#85831);
#19738=PLANE('',#85832);
#19739=PLANE('',#85833);
#19740=PLANE('',#85834);
#19741=PLANE('',#85835);
#19742=PLANE('',#85836);
#19743=PLANE('',#85837);
#19744=PLANE('',#85838);
#19745=PLANE('',#85839);
#19746=PLANE('',#85840);
#19747=PLANE('',#85841);
#19748=PLANE('',#85842);
#19749=PLANE('',#85843);
#19750=PLANE('',#85844);
#19751=PLANE('',#85845);
#19752=PLANE('',#85846);
#19753=PLANE('',#85847);
#19754=PLANE('',#85848);
#19755=PLANE('',#85849);
#19756=PLANE('',#85850);
#19757=PLANE('',#85851);
#19758=PLANE('',#85852);
#19759=PLANE('',#85853);
#19760=PLANE('',#85854);
#19761=PLANE('',#85855);
#19762=PLANE('',#85856);
#19763=PLANE('',#85857);
#19764=PLANE('',#85858);
#19765=PLANE('',#85859);
#19766=PLANE('',#85860);
#19767=PLANE('',#85861);
#19768=PLANE('',#85862);
#19769=PLANE('',#85863);
#19770=PLANE('',#85864);
#19771=PLANE('',#85865);
#19772=PLANE('',#85866);
#19773=PLANE('',#85867);
#19774=PLANE('',#85868);
#19775=PLANE('',#85869);
#19776=PLANE('',#85870);
#19777=PLANE('',#85871);
#19778=PLANE('',#85872);
#19779=PLANE('',#85873);
#19780=PLANE('',#85874);
#19781=PLANE('',#85875);
#19782=PLANE('',#85876);
#19783=PLANE('',#85877);
#19784=PLANE('',#85878);
#19785=PLANE('',#85879);
#19786=PLANE('',#85880);
#19787=PLANE('',#85881);
#19788=PLANE('',#85882);
#19789=PLANE('',#85883);
#19790=PLANE('',#85884);
#19791=PLANE('',#85885);
#19792=PLANE('',#85886);
#19793=PLANE('',#85887);
#19794=PLANE('',#85888);
#19795=PLANE('',#85889);
#19796=PLANE('',#85890);
#19797=PLANE('',#85891);
#19798=PLANE('',#85892);
#19799=PLANE('',#85893);
#19800=PLANE('',#85894);
#19801=PLANE('',#85895);
#19802=PLANE('',#85896);
#19803=PLANE('',#85897);
#19804=PLANE('',#85898);
#19805=PLANE('',#85899);
#19806=PLANE('',#85900);
#19807=PLANE('',#85901);
#19808=PLANE('',#85902);
#19809=PLANE('',#85903);
#19810=PLANE('',#85904);
#19811=PLANE('',#85905);
#19812=PLANE('',#85906);
#19813=PLANE('',#85907);
#19814=PLANE('',#85908);
#19815=PLANE('',#85909);
#19816=PLANE('',#85910);
#19817=PLANE('',#85911);
#19818=PLANE('',#85912);
#19819=PLANE('',#85913);
#19820=PLANE('',#85914);
#19821=PLANE('',#85915);
#19822=PLANE('',#85916);
#19823=PLANE('',#85917);
#19824=PLANE('',#85918);
#19825=PLANE('',#85919);
#19826=PLANE('',#85920);
#19827=PLANE('',#85921);
#19828=PLANE('',#85922);
#19829=PLANE('',#85923);
#19830=PLANE('',#85924);
#19831=PLANE('',#85925);
#19832=PLANE('',#85926);
#19833=PLANE('',#85927);
#19834=PLANE('',#85928);
#19835=PLANE('',#85929);
#19836=PLANE('',#85930);
#19837=PLANE('',#85931);
#19838=PLANE('',#85932);
#19839=PLANE('',#85933);
#19840=PLANE('',#85934);
#19841=PLANE('',#85935);
#19842=PLANE('',#85936);
#19843=PLANE('',#85937);
#19844=PLANE('',#85938);
#19845=PLANE('',#85939);
#19846=PLANE('',#85940);
#19847=PLANE('',#85943);
#19848=PLANE('',#85944);
#19849=PLANE('',#85945);
#19850=PLANE('',#85946);
#19851=PLANE('',#85949);
#19852=PLANE('',#85956);
#19853=PLANE('',#85958);
#19854=PLANE('',#85960);
#19855=PLANE('',#85962);
#19856=PLANE('',#85966);
#19857=PLANE('',#86027);
#19858=PLANE('',#86028);
#19859=PLANE('',#86036);
#19860=PLANE('',#86044);
#19861=PLANE('',#86045);
#19862=PLANE('',#86046);
#19863=PLANE('',#86052);
#19864=PLANE('',#86057);
#19865=PLANE('',#86119);
#19866=PLANE('',#86120);
#19867=PLANE('',#86128);
#19868=PLANE('',#86136);
#19869=PLANE('',#86137);
#19870=PLANE('',#86138);
#19871=PLANE('',#86144);
#19872=PLANE('',#86149);
#19873=FACE_OUTER_BOUND('',#23888,.T.);
#19874=FACE_OUTER_BOUND('',#23889,.T.);
#19875=FACE_OUTER_BOUND('',#23890,.T.);
#19876=FACE_OUTER_BOUND('',#23891,.T.);
#19877=FACE_OUTER_BOUND('',#23892,.T.);
#19878=FACE_OUTER_BOUND('',#23893,.T.);
#19879=FACE_OUTER_BOUND('',#23894,.T.);
#19880=FACE_OUTER_BOUND('',#23895,.T.);
#19881=FACE_OUTER_BOUND('',#23896,.T.);
#19882=FACE_OUTER_BOUND('',#23897,.T.);
#19883=FACE_OUTER_BOUND('',#23898,.T.);
#19884=FACE_OUTER_BOUND('',#23899,.T.);
#19885=FACE_OUTER_BOUND('',#23900,.T.);
#19886=FACE_OUTER_BOUND('',#23901,.T.);
#19887=FACE_OUTER_BOUND('',#23902,.T.);
#19888=FACE_OUTER_BOUND('',#23903,.T.);
#19889=FACE_OUTER_BOUND('',#23904,.T.);
#19890=FACE_OUTER_BOUND('',#23905,.T.);
#19891=FACE_OUTER_BOUND('',#23906,.T.);
#19892=FACE_OUTER_BOUND('',#23907,.T.);
#19893=FACE_OUTER_BOUND('',#23908,.T.);
#19894=FACE_OUTER_BOUND('',#23909,.T.);
#19895=FACE_OUTER_BOUND('',#23910,.T.);
#19896=FACE_OUTER_BOUND('',#23911,.T.);
#19897=FACE_OUTER_BOUND('',#23912,.T.);
#19898=FACE_OUTER_BOUND('',#23913,.T.);
#19899=FACE_OUTER_BOUND('',#23914,.T.);
#19900=FACE_OUTER_BOUND('',#23915,.T.);
#19901=FACE_OUTER_BOUND('',#23916,.T.);
#19902=FACE_OUTER_BOUND('',#23917,.T.);
#19903=FACE_OUTER_BOUND('',#23918,.T.);
#19904=FACE_OUTER_BOUND('',#23919,.T.);
#19905=FACE_OUTER_BOUND('',#23920,.T.);
#19906=FACE_OUTER_BOUND('',#23921,.T.);
#19907=FACE_OUTER_BOUND('',#23922,.T.);
#19908=FACE_OUTER_BOUND('',#23923,.T.);
#19909=FACE_OUTER_BOUND('',#23924,.T.);
#19910=FACE_OUTER_BOUND('',#23925,.T.);
#19911=FACE_OUTER_BOUND('',#23926,.T.);
#19912=FACE_OUTER_BOUND('',#23927,.T.);
#19913=FACE_OUTER_BOUND('',#23928,.T.);
#19914=FACE_OUTER_BOUND('',#23929,.T.);
#19915=FACE_OUTER_BOUND('',#23930,.T.);
#19916=FACE_OUTER_BOUND('',#23931,.T.);
#19917=FACE_OUTER_BOUND('',#23932,.T.);
#19918=FACE_OUTER_BOUND('',#23933,.T.);
#19919=FACE_OUTER_BOUND('',#23934,.T.);
#19920=FACE_OUTER_BOUND('',#23935,.T.);
#19921=FACE_OUTER_BOUND('',#23936,.T.);
#19922=FACE_OUTER_BOUND('',#23937,.T.);
#19923=FACE_OUTER_BOUND('',#23938,.T.);
#19924=FACE_OUTER_BOUND('',#23939,.T.);
#19925=FACE_OUTER_BOUND('',#23940,.T.);
#19926=FACE_OUTER_BOUND('',#23941,.T.);
#19927=FACE_OUTER_BOUND('',#23942,.T.);
#19928=FACE_OUTER_BOUND('',#23943,.T.);
#19929=FACE_OUTER_BOUND('',#23944,.T.);
#19930=FACE_OUTER_BOUND('',#23945,.T.);
#19931=FACE_OUTER_BOUND('',#23946,.T.);
#19932=FACE_OUTER_BOUND('',#23947,.T.);
#19933=FACE_OUTER_BOUND('',#23948,.T.);
#19934=FACE_OUTER_BOUND('',#23949,.T.);
#19935=FACE_OUTER_BOUND('',#23950,.T.);
#19936=FACE_OUTER_BOUND('',#23951,.T.);
#19937=FACE_OUTER_BOUND('',#23952,.T.);
#19938=FACE_OUTER_BOUND('',#23953,.T.);
#19939=FACE_OUTER_BOUND('',#23954,.T.);
#19940=FACE_OUTER_BOUND('',#23955,.T.);
#19941=FACE_OUTER_BOUND('',#23956,.T.);
#19942=FACE_OUTER_BOUND('',#23957,.T.);
#19943=FACE_OUTER_BOUND('',#23958,.T.);
#19944=FACE_OUTER_BOUND('',#23959,.T.);
#19945=FACE_OUTER_BOUND('',#23960,.T.);
#19946=FACE_OUTER_BOUND('',#23961,.T.);
#19947=FACE_OUTER_BOUND('',#23962,.T.);
#19948=FACE_OUTER_BOUND('',#23963,.T.);
#19949=FACE_OUTER_BOUND('',#23964,.T.);
#19950=FACE_OUTER_BOUND('',#23965,.T.);
#19951=FACE_OUTER_BOUND('',#23966,.T.);
#19952=FACE_OUTER_BOUND('',#23967,.T.);
#19953=FACE_OUTER_BOUND('',#23968,.T.);
#19954=FACE_OUTER_BOUND('',#23969,.T.);
#19955=FACE_OUTER_BOUND('',#23970,.T.);
#19956=FACE_OUTER_BOUND('',#23971,.T.);
#19957=FACE_OUTER_BOUND('',#23972,.T.);
#19958=FACE_OUTER_BOUND('',#23973,.T.);
#19959=FACE_OUTER_BOUND('',#23974,.T.);
#19960=FACE_OUTER_BOUND('',#23975,.T.);
#19961=FACE_OUTER_BOUND('',#23976,.T.);
#19962=FACE_OUTER_BOUND('',#23977,.T.);
#19963=FACE_OUTER_BOUND('',#23978,.T.);
#19964=FACE_OUTER_BOUND('',#23979,.T.);
#19965=FACE_OUTER_BOUND('',#23980,.T.);
#19966=FACE_OUTER_BOUND('',#23981,.T.);
#19967=FACE_OUTER_BOUND('',#23982,.T.);
#19968=FACE_OUTER_BOUND('',#23983,.T.);
#19969=FACE_OUTER_BOUND('',#23984,.T.);
#19970=FACE_OUTER_BOUND('',#23985,.T.);
#19971=FACE_OUTER_BOUND('',#23986,.T.);
#19972=FACE_OUTER_BOUND('',#23987,.T.);
#19973=FACE_OUTER_BOUND('',#23988,.T.);
#19974=FACE_OUTER_BOUND('',#23989,.T.);
#19975=FACE_OUTER_BOUND('',#23990,.T.);
#19976=FACE_OUTER_BOUND('',#23991,.T.);
#19977=FACE_OUTER_BOUND('',#23992,.T.);
#19978=FACE_OUTER_BOUND('',#23993,.T.);
#19979=FACE_OUTER_BOUND('',#23994,.T.);
#19980=FACE_OUTER_BOUND('',#23995,.T.);
#19981=FACE_OUTER_BOUND('',#23996,.T.);
#19982=FACE_OUTER_BOUND('',#23997,.T.);
#19983=FACE_OUTER_BOUND('',#23998,.T.);
#19984=FACE_OUTER_BOUND('',#24000,.T.);
#19985=FACE_OUTER_BOUND('',#24001,.T.);
#19986=FACE_OUTER_BOUND('',#24002,.T.);
#19987=FACE_OUTER_BOUND('',#24003,.T.);
#19988=FACE_OUTER_BOUND('',#24004,.T.);
#19989=FACE_OUTER_BOUND('',#24005,.T.);
#19990=FACE_OUTER_BOUND('',#24006,.T.);
#19991=FACE_OUTER_BOUND('',#24008,.T.);
#19992=FACE_OUTER_BOUND('',#24010,.T.);
#19993=FACE_OUTER_BOUND('',#24011,.T.);
#19994=FACE_OUTER_BOUND('',#24012,.T.);
#19995=FACE_OUTER_BOUND('',#24013,.T.);
#19996=FACE_OUTER_BOUND('',#24014,.T.);
#19997=FACE_OUTER_BOUND('',#24015,.T.);
#19998=FACE_OUTER_BOUND('',#24016,.T.);
#19999=FACE_OUTER_BOUND('',#24017,.T.);
#20000=FACE_OUTER_BOUND('',#24018,.T.);
#20001=FACE_OUTER_BOUND('',#24019,.T.);
#20002=FACE_OUTER_BOUND('',#24020,.T.);
#20003=FACE_OUTER_BOUND('',#24021,.T.);
#20004=FACE_OUTER_BOUND('',#24022,.T.);
#20005=FACE_OUTER_BOUND('',#24023,.T.);
#20006=FACE_OUTER_BOUND('',#24024,.T.);
#20007=FACE_OUTER_BOUND('',#24025,.T.);
#20008=FACE_OUTER_BOUND('',#24026,.T.);
#20009=FACE_OUTER_BOUND('',#24027,.T.);
#20010=FACE_OUTER_BOUND('',#24028,.T.);
#20011=FACE_OUTER_BOUND('',#24029,.T.);
#20012=FACE_OUTER_BOUND('',#24030,.T.);
#20013=FACE_OUTER_BOUND('',#24031,.T.);
#20014=FACE_OUTER_BOUND('',#24032,.T.);
#20015=FACE_OUTER_BOUND('',#24033,.T.);
#20016=FACE_OUTER_BOUND('',#24034,.T.);
#20017=FACE_OUTER_BOUND('',#24035,.T.);
#20018=FACE_OUTER_BOUND('',#24036,.T.);
#20019=FACE_OUTER_BOUND('',#24037,.T.);
#20020=FACE_OUTER_BOUND('',#24038,.T.);
#20021=FACE_OUTER_BOUND('',#24039,.T.);
#20022=FACE_OUTER_BOUND('',#24040,.T.);
#20023=FACE_OUTER_BOUND('',#24041,.T.);
#20024=FACE_OUTER_BOUND('',#24042,.T.);
#20025=FACE_OUTER_BOUND('',#24043,.T.);
#20026=FACE_OUTER_BOUND('',#24044,.T.);
#20027=FACE_OUTER_BOUND('',#24045,.T.);
#20028=FACE_OUTER_BOUND('',#24046,.T.);
#20029=FACE_OUTER_BOUND('',#24047,.T.);
#20030=FACE_OUTER_BOUND('',#24048,.T.);
#20031=FACE_OUTER_BOUND('',#24049,.T.);
#20032=FACE_OUTER_BOUND('',#24050,.T.);
#20033=FACE_OUTER_BOUND('',#24051,.T.);
#20034=FACE_OUTER_BOUND('',#24052,.T.);
#20035=FACE_OUTER_BOUND('',#24053,.T.);
#20036=FACE_OUTER_BOUND('',#24054,.T.);
#20037=FACE_OUTER_BOUND('',#24055,.T.);
#20038=FACE_OUTER_BOUND('',#24056,.T.);
#20039=FACE_OUTER_BOUND('',#24057,.T.);
#20040=FACE_OUTER_BOUND('',#24058,.T.);
#20041=FACE_OUTER_BOUND('',#24059,.T.);
#20042=FACE_OUTER_BOUND('',#24060,.T.);
#20043=FACE_OUTER_BOUND('',#24061,.T.);
#20044=FACE_OUTER_BOUND('',#24062,.T.);
#20045=FACE_OUTER_BOUND('',#24063,.T.);
#20046=FACE_OUTER_BOUND('',#24064,.T.);
#20047=FACE_OUTER_BOUND('',#24065,.T.);
#20048=FACE_OUTER_BOUND('',#24066,.T.);
#20049=FACE_OUTER_BOUND('',#24067,.T.);
#20050=FACE_OUTER_BOUND('',#24068,.T.);
#20051=FACE_OUTER_BOUND('',#24069,.T.);
#20052=FACE_OUTER_BOUND('',#24070,.T.);
#20053=FACE_OUTER_BOUND('',#24071,.T.);
#20054=FACE_OUTER_BOUND('',#24072,.T.);
#20055=FACE_OUTER_BOUND('',#24073,.T.);
#20056=FACE_OUTER_BOUND('',#24074,.T.);
#20057=FACE_OUTER_BOUND('',#24075,.T.);
#20058=FACE_OUTER_BOUND('',#24076,.T.);
#20059=FACE_OUTER_BOUND('',#24077,.T.);
#20060=FACE_OUTER_BOUND('',#24079,.T.);
#20061=FACE_OUTER_BOUND('',#24080,.T.);
#20062=FACE_OUTER_BOUND('',#24081,.T.);
#20063=FACE_OUTER_BOUND('',#24082,.T.);
#20064=FACE_OUTER_BOUND('',#24083,.T.);
#20065=FACE_OUTER_BOUND('',#24084,.T.);
#20066=FACE_OUTER_BOUND('',#24085,.T.);
#20067=FACE_OUTER_BOUND('',#24087,.T.);
#20068=FACE_OUTER_BOUND('',#24089,.T.);
#20069=FACE_OUTER_BOUND('',#24090,.T.);
#20070=FACE_OUTER_BOUND('',#24091,.T.);
#20071=FACE_OUTER_BOUND('',#24092,.T.);
#20072=FACE_OUTER_BOUND('',#24093,.T.);
#20073=FACE_OUTER_BOUND('',#24094,.T.);
#20074=FACE_OUTER_BOUND('',#24095,.T.);
#20075=FACE_OUTER_BOUND('',#24097,.T.);
#20076=FACE_OUTER_BOUND('',#24099,.T.);
#20077=FACE_OUTER_BOUND('',#24100,.T.);
#20078=FACE_OUTER_BOUND('',#24101,.T.);
#20079=FACE_OUTER_BOUND('',#24102,.T.);
#20080=FACE_OUTER_BOUND('',#24103,.T.);
#20081=FACE_OUTER_BOUND('',#24104,.T.);
#20082=FACE_OUTER_BOUND('',#24105,.T.);
#20083=FACE_OUTER_BOUND('',#24106,.T.);
#20084=FACE_OUTER_BOUND('',#24107,.T.);
#20085=FACE_OUTER_BOUND('',#24108,.T.);
#20086=FACE_OUTER_BOUND('',#24109,.T.);
#20087=FACE_OUTER_BOUND('',#24110,.T.);
#20088=FACE_OUTER_BOUND('',#24111,.T.);
#20089=FACE_OUTER_BOUND('',#24112,.T.);
#20090=FACE_OUTER_BOUND('',#24113,.T.);
#20091=FACE_OUTER_BOUND('',#24114,.T.);
#20092=FACE_OUTER_BOUND('',#24115,.T.);
#20093=FACE_OUTER_BOUND('',#24116,.T.);
#20094=FACE_OUTER_BOUND('',#24117,.T.);
#20095=FACE_OUTER_BOUND('',#24118,.T.);
#20096=FACE_OUTER_BOUND('',#24119,.T.);
#20097=FACE_OUTER_BOUND('',#24120,.T.);
#20098=FACE_OUTER_BOUND('',#24121,.T.);
#20099=FACE_OUTER_BOUND('',#24122,.T.);
#20100=FACE_OUTER_BOUND('',#24123,.T.);
#20101=FACE_OUTER_BOUND('',#24124,.T.);
#20102=FACE_OUTER_BOUND('',#24125,.T.);
#20103=FACE_OUTER_BOUND('',#24126,.T.);
#20104=FACE_OUTER_BOUND('',#24127,.T.);
#20105=FACE_OUTER_BOUND('',#24128,.T.);
#20106=FACE_OUTER_BOUND('',#24129,.T.);
#20107=FACE_OUTER_BOUND('',#24130,.T.);
#20108=FACE_OUTER_BOUND('',#24131,.T.);
#20109=FACE_OUTER_BOUND('',#24132,.T.);
#20110=FACE_OUTER_BOUND('',#24133,.T.);
#20111=FACE_OUTER_BOUND('',#24134,.T.);
#20112=FACE_OUTER_BOUND('',#24135,.T.);
#20113=FACE_OUTER_BOUND('',#24136,.T.);
#20114=FACE_OUTER_BOUND('',#24137,.T.);
#20115=FACE_OUTER_BOUND('',#24138,.T.);
#20116=FACE_OUTER_BOUND('',#24139,.T.);
#20117=FACE_OUTER_BOUND('',#24140,.T.);
#20118=FACE_OUTER_BOUND('',#24141,.T.);
#20119=FACE_OUTER_BOUND('',#24142,.T.);
#20120=FACE_OUTER_BOUND('',#24143,.T.);
#20121=FACE_OUTER_BOUND('',#24144,.T.);
#20122=FACE_OUTER_BOUND('',#24145,.T.);
#20123=FACE_OUTER_BOUND('',#24146,.T.);
#20124=FACE_OUTER_BOUND('',#24147,.T.);
#20125=FACE_OUTER_BOUND('',#24148,.T.);
#20126=FACE_OUTER_BOUND('',#24149,.T.);
#20127=FACE_OUTER_BOUND('',#24150,.T.);
#20128=FACE_OUTER_BOUND('',#24151,.T.);
#20129=FACE_OUTER_BOUND('',#24152,.T.);
#20130=FACE_OUTER_BOUND('',#24153,.T.);
#20131=FACE_OUTER_BOUND('',#24154,.T.);
#20132=FACE_OUTER_BOUND('',#24155,.T.);
#20133=FACE_OUTER_BOUND('',#24156,.T.);
#20134=FACE_OUTER_BOUND('',#24157,.T.);
#20135=FACE_OUTER_BOUND('',#24158,.T.);
#20136=FACE_OUTER_BOUND('',#24159,.T.);
#20137=FACE_OUTER_BOUND('',#24160,.T.);
#20138=FACE_OUTER_BOUND('',#24161,.T.);
#20139=FACE_OUTER_BOUND('',#24162,.T.);
#20140=FACE_OUTER_BOUND('',#24163,.T.);
#20141=FACE_OUTER_BOUND('',#24164,.T.);
#20142=FACE_OUTER_BOUND('',#24165,.T.);
#20143=FACE_OUTER_BOUND('',#24166,.T.);
#20144=FACE_OUTER_BOUND('',#24168,.T.);
#20145=FACE_OUTER_BOUND('',#24169,.T.);
#20146=FACE_OUTER_BOUND('',#24170,.T.);
#20147=FACE_OUTER_BOUND('',#24171,.T.);
#20148=FACE_OUTER_BOUND('',#24172,.T.);
#20149=FACE_OUTER_BOUND('',#24173,.T.);
#20150=FACE_OUTER_BOUND('',#24174,.T.);
#20151=FACE_OUTER_BOUND('',#24176,.T.);
#20152=FACE_OUTER_BOUND('',#24177,.T.);
#20153=FACE_OUTER_BOUND('',#24178,.T.);
#20154=FACE_OUTER_BOUND('',#24179,.T.);
#20155=FACE_OUTER_BOUND('',#24181,.T.);
#20156=FACE_OUTER_BOUND('',#24182,.T.);
#20157=FACE_OUTER_BOUND('',#24183,.T.);
#20158=FACE_OUTER_BOUND('',#24184,.T.);
#20159=FACE_OUTER_BOUND('',#24185,.T.);
#20160=FACE_OUTER_BOUND('',#24186,.T.);
#20161=FACE_OUTER_BOUND('',#24187,.T.);
#20162=FACE_OUTER_BOUND('',#24188,.T.);
#20163=FACE_OUTER_BOUND('',#24189,.T.);
#20164=FACE_OUTER_BOUND('',#24190,.T.);
#20165=FACE_OUTER_BOUND('',#24191,.T.);
#20166=FACE_OUTER_BOUND('',#24192,.T.);
#20167=FACE_OUTER_BOUND('',#24193,.T.);
#20168=FACE_OUTER_BOUND('',#24194,.T.);
#20169=FACE_OUTER_BOUND('',#24195,.T.);
#20170=FACE_OUTER_BOUND('',#24196,.T.);
#20171=FACE_OUTER_BOUND('',#24197,.T.);
#20172=FACE_OUTER_BOUND('',#24198,.T.);
#20173=FACE_OUTER_BOUND('',#24199,.T.);
#20174=FACE_OUTER_BOUND('',#24200,.T.);
#20175=FACE_OUTER_BOUND('',#24201,.T.);
#20176=FACE_OUTER_BOUND('',#24202,.T.);
#20177=FACE_OUTER_BOUND('',#24203,.T.);
#20178=FACE_OUTER_BOUND('',#24204,.T.);
#20179=FACE_OUTER_BOUND('',#24205,.T.);
#20180=FACE_OUTER_BOUND('',#24206,.T.);
#20181=FACE_OUTER_BOUND('',#24207,.T.);
#20182=FACE_OUTER_BOUND('',#24208,.T.);
#20183=FACE_OUTER_BOUND('',#24209,.T.);
#20184=FACE_OUTER_BOUND('',#24210,.T.);
#20185=FACE_OUTER_BOUND('',#24211,.T.);
#20186=FACE_OUTER_BOUND('',#24212,.T.);
#20187=FACE_OUTER_BOUND('',#24213,.T.);
#20188=FACE_OUTER_BOUND('',#24214,.T.);
#20189=FACE_OUTER_BOUND('',#24215,.T.);
#20190=FACE_OUTER_BOUND('',#24216,.T.);
#20191=FACE_OUTER_BOUND('',#24217,.T.);
#20192=FACE_OUTER_BOUND('',#24218,.T.);
#20193=FACE_OUTER_BOUND('',#24219,.T.);
#20194=FACE_OUTER_BOUND('',#24220,.T.);
#20195=FACE_OUTER_BOUND('',#24221,.T.);
#20196=FACE_OUTER_BOUND('',#24222,.T.);
#20197=FACE_OUTER_BOUND('',#24223,.T.);
#20198=FACE_OUTER_BOUND('',#24224,.T.);
#20199=FACE_OUTER_BOUND('',#24225,.T.);
#20200=FACE_OUTER_BOUND('',#24226,.T.);
#20201=FACE_OUTER_BOUND('',#24227,.T.);
#20202=FACE_OUTER_BOUND('',#24228,.T.);
#20203=FACE_OUTER_BOUND('',#24229,.T.);
#20204=FACE_OUTER_BOUND('',#24230,.T.);
#20205=FACE_OUTER_BOUND('',#24231,.T.);
#20206=FACE_OUTER_BOUND('',#24232,.T.);
#20207=FACE_OUTER_BOUND('',#24233,.T.);
#20208=FACE_OUTER_BOUND('',#24234,.T.);
#20209=FACE_OUTER_BOUND('',#24235,.T.);
#20210=FACE_OUTER_BOUND('',#24236,.T.);
#20211=FACE_OUTER_BOUND('',#24237,.T.);
#20212=FACE_OUTER_BOUND('',#24238,.T.);
#20213=FACE_OUTER_BOUND('',#24239,.T.);
#20214=FACE_OUTER_BOUND('',#24240,.T.);
#20215=FACE_OUTER_BOUND('',#24241,.T.);
#20216=FACE_OUTER_BOUND('',#24243,.T.);
#20217=FACE_OUTER_BOUND('',#24245,.T.);
#20218=FACE_OUTER_BOUND('',#24246,.T.);
#20219=FACE_OUTER_BOUND('',#24247,.T.);
#20220=FACE_OUTER_BOUND('',#24248,.T.);
#20221=FACE_OUTER_BOUND('',#24249,.T.);
#20222=FACE_OUTER_BOUND('',#24250,.T.);
#20223=FACE_OUTER_BOUND('',#24251,.T.);
#20224=FACE_OUTER_BOUND('',#24252,.T.);
#20225=FACE_OUTER_BOUND('',#24253,.T.);
#20226=FACE_OUTER_BOUND('',#24254,.T.);
#20227=FACE_OUTER_BOUND('',#24255,.T.);
#20228=FACE_OUTER_BOUND('',#24256,.T.);
#20229=FACE_OUTER_BOUND('',#24257,.T.);
#20230=FACE_OUTER_BOUND('',#24258,.T.);
#20231=FACE_OUTER_BOUND('',#24259,.T.);
#20232=FACE_OUTER_BOUND('',#24260,.T.);
#20233=FACE_OUTER_BOUND('',#24261,.T.);
#20234=FACE_OUTER_BOUND('',#24262,.T.);
#20235=FACE_OUTER_BOUND('',#24263,.T.);
#20236=FACE_OUTER_BOUND('',#24264,.T.);
#20237=FACE_OUTER_BOUND('',#24265,.T.);
#20238=FACE_OUTER_BOUND('',#24266,.T.);
#20239=FACE_OUTER_BOUND('',#24268,.T.);
#20240=FACE_OUTER_BOUND('',#24270,.T.);
#20241=FACE_OUTER_BOUND('',#24272,.T.);
#20242=FACE_OUTER_BOUND('',#24273,.T.);
#20243=FACE_OUTER_BOUND('',#24274,.T.);
#20244=FACE_OUTER_BOUND('',#24275,.T.);
#20245=FACE_OUTER_BOUND('',#24276,.T.);
#20246=FACE_OUTER_BOUND('',#24277,.T.);
#20247=FACE_OUTER_BOUND('',#24278,.T.);
#20248=FACE_OUTER_BOUND('',#24279,.T.);
#20249=FACE_OUTER_BOUND('',#24280,.T.);
#20250=FACE_OUTER_BOUND('',#24281,.T.);
#20251=FACE_OUTER_BOUND('',#24282,.T.);
#20252=FACE_OUTER_BOUND('',#24283,.T.);
#20253=FACE_OUTER_BOUND('',#24284,.T.);
#20254=FACE_OUTER_BOUND('',#24285,.T.);
#20255=FACE_OUTER_BOUND('',#24286,.T.);
#20256=FACE_OUTER_BOUND('',#24287,.T.);
#20257=FACE_OUTER_BOUND('',#24288,.T.);
#20258=FACE_OUTER_BOUND('',#24289,.T.);
#20259=FACE_OUTER_BOUND('',#24290,.T.);
#20260=FACE_OUTER_BOUND('',#24291,.T.);
#20261=FACE_OUTER_BOUND('',#24292,.T.);
#20262=FACE_OUTER_BOUND('',#24293,.T.);
#20263=FACE_OUTER_BOUND('',#24294,.T.);
#20264=FACE_OUTER_BOUND('',#24295,.T.);
#20265=FACE_OUTER_BOUND('',#24296,.T.);
#20266=FACE_OUTER_BOUND('',#24297,.T.);
#20267=FACE_OUTER_BOUND('',#24298,.T.);
#20268=FACE_OUTER_BOUND('',#24299,.T.);
#20269=FACE_OUTER_BOUND('',#24300,.T.);
#20270=FACE_OUTER_BOUND('',#24301,.T.);
#20271=FACE_OUTER_BOUND('',#24302,.T.);
#20272=FACE_OUTER_BOUND('',#24303,.T.);
#20273=FACE_OUTER_BOUND('',#24304,.T.);
#20274=FACE_OUTER_BOUND('',#24305,.T.);
#20275=FACE_OUTER_BOUND('',#24306,.T.);
#20276=FACE_OUTER_BOUND('',#24307,.T.);
#20277=FACE_OUTER_BOUND('',#24308,.T.);
#20278=FACE_OUTER_BOUND('',#24309,.T.);
#20279=FACE_OUTER_BOUND('',#24310,.T.);
#20280=FACE_OUTER_BOUND('',#24311,.T.);
#20281=FACE_OUTER_BOUND('',#24312,.T.);
#20282=FACE_OUTER_BOUND('',#24313,.T.);
#20283=FACE_OUTER_BOUND('',#24314,.T.);
#20284=FACE_OUTER_BOUND('',#24315,.T.);
#20285=FACE_OUTER_BOUND('',#24316,.T.);
#20286=FACE_OUTER_BOUND('',#24317,.T.);
#20287=FACE_OUTER_BOUND('',#24318,.T.);
#20288=FACE_OUTER_BOUND('',#24319,.T.);
#20289=FACE_OUTER_BOUND('',#24320,.T.);
#20290=FACE_OUTER_BOUND('',#24321,.T.);
#20291=FACE_OUTER_BOUND('',#24322,.T.);
#20292=FACE_OUTER_BOUND('',#24323,.T.);
#20293=FACE_OUTER_BOUND('',#24324,.T.);
#20294=FACE_OUTER_BOUND('',#24325,.T.);
#20295=FACE_OUTER_BOUND('',#24326,.T.);
#20296=FACE_OUTER_BOUND('',#24327,.T.);
#20297=FACE_OUTER_BOUND('',#24328,.T.);
#20298=FACE_OUTER_BOUND('',#24329,.T.);
#20299=FACE_OUTER_BOUND('',#24330,.T.);
#20300=FACE_OUTER_BOUND('',#24331,.T.);
#20301=FACE_OUTER_BOUND('',#24332,.T.);
#20302=FACE_OUTER_BOUND('',#24333,.T.);
#20303=FACE_OUTER_BOUND('',#24334,.T.);
#20304=FACE_OUTER_BOUND('',#24335,.T.);
#20305=FACE_OUTER_BOUND('',#24336,.T.);
#20306=FACE_OUTER_BOUND('',#24337,.T.);
#20307=FACE_OUTER_BOUND('',#24338,.T.);
#20308=FACE_OUTER_BOUND('',#24340,.T.);
#20309=FACE_OUTER_BOUND('',#24342,.T.);
#20310=FACE_OUTER_BOUND('',#24343,.T.);
#20311=FACE_OUTER_BOUND('',#24344,.T.);
#20312=FACE_OUTER_BOUND('',#24345,.T.);
#20313=FACE_OUTER_BOUND('',#24346,.T.);
#20314=FACE_OUTER_BOUND('',#24347,.T.);
#20315=FACE_OUTER_BOUND('',#24348,.T.);
#20316=FACE_OUTER_BOUND('',#24349,.T.);
#20317=FACE_OUTER_BOUND('',#24350,.T.);
#20318=FACE_OUTER_BOUND('',#24351,.T.);
#20319=FACE_OUTER_BOUND('',#24352,.T.);
#20320=FACE_OUTER_BOUND('',#24353,.T.);
#20321=FACE_OUTER_BOUND('',#24354,.T.);
#20322=FACE_OUTER_BOUND('',#24355,.T.);
#20323=FACE_OUTER_BOUND('',#24356,.T.);
#20324=FACE_OUTER_BOUND('',#24357,.T.);
#20325=FACE_OUTER_BOUND('',#24358,.T.);
#20326=FACE_OUTER_BOUND('',#24359,.T.);
#20327=FACE_OUTER_BOUND('',#24360,.T.);
#20328=FACE_OUTER_BOUND('',#24361,.T.);
#20329=FACE_OUTER_BOUND('',#24362,.T.);
#20330=FACE_OUTER_BOUND('',#24363,.T.);
#20331=FACE_OUTER_BOUND('',#24364,.T.);
#20332=FACE_OUTER_BOUND('',#24365,.T.);
#20333=FACE_OUTER_BOUND('',#24366,.T.);
#20334=FACE_OUTER_BOUND('',#24367,.T.);
#20335=FACE_OUTER_BOUND('',#24368,.T.);
#20336=FACE_OUTER_BOUND('',#24369,.T.);
#20337=FACE_OUTER_BOUND('',#24370,.T.);
#20338=FACE_OUTER_BOUND('',#24371,.T.);
#20339=FACE_OUTER_BOUND('',#24372,.T.);
#20340=FACE_OUTER_BOUND('',#24373,.T.);
#20341=FACE_OUTER_BOUND('',#24374,.T.);
#20342=FACE_OUTER_BOUND('',#24375,.T.);
#20343=FACE_OUTER_BOUND('',#24376,.T.);
#20344=FACE_OUTER_BOUND('',#24377,.T.);
#20345=FACE_OUTER_BOUND('',#24378,.T.);
#20346=FACE_OUTER_BOUND('',#24379,.T.);
#20347=FACE_OUTER_BOUND('',#24380,.T.);
#20348=FACE_OUTER_BOUND('',#24381,.T.);
#20349=FACE_OUTER_BOUND('',#24382,.T.);
#20350=FACE_OUTER_BOUND('',#24383,.T.);
#20351=FACE_OUTER_BOUND('',#24384,.T.);
#20352=FACE_OUTER_BOUND('',#24385,.T.);
#20353=FACE_OUTER_BOUND('',#24386,.T.);
#20354=FACE_OUTER_BOUND('',#24387,.T.);
#20355=FACE_OUTER_BOUND('',#24388,.T.);
#20356=FACE_OUTER_BOUND('',#24389,.T.);
#20357=FACE_OUTER_BOUND('',#24390,.T.);
#20358=FACE_OUTER_BOUND('',#24391,.T.);
#20359=FACE_OUTER_BOUND('',#24392,.T.);
#20360=FACE_OUTER_BOUND('',#24393,.T.);
#20361=FACE_OUTER_BOUND('',#24395,.T.);
#20362=FACE_OUTER_BOUND('',#24396,.T.);
#20363=FACE_OUTER_BOUND('',#24397,.T.);
#20364=FACE_OUTER_BOUND('',#24398,.T.);
#20365=FACE_OUTER_BOUND('',#24399,.T.);
#20366=FACE_OUTER_BOUND('',#24400,.T.);
#20367=FACE_OUTER_BOUND('',#24401,.T.);
#20368=FACE_OUTER_BOUND('',#24402,.T.);
#20369=FACE_OUTER_BOUND('',#24403,.T.);
#20370=FACE_OUTER_BOUND('',#24404,.T.);
#20371=FACE_OUTER_BOUND('',#24405,.T.);
#20372=FACE_OUTER_BOUND('',#24406,.T.);
#20373=FACE_OUTER_BOUND('',#24407,.T.);
#20374=FACE_OUTER_BOUND('',#24408,.T.);
#20375=FACE_OUTER_BOUND('',#24409,.T.);
#20376=FACE_OUTER_BOUND('',#24410,.T.);
#20377=FACE_OUTER_BOUND('',#24411,.T.);
#20378=FACE_OUTER_BOUND('',#24412,.T.);
#20379=FACE_OUTER_BOUND('',#24413,.T.);
#20380=FACE_OUTER_BOUND('',#24414,.T.);
#20381=FACE_OUTER_BOUND('',#24415,.T.);
#20382=FACE_OUTER_BOUND('',#24416,.T.);
#20383=FACE_OUTER_BOUND('',#24417,.T.);
#20384=FACE_OUTER_BOUND('',#24418,.T.);
#20385=FACE_OUTER_BOUND('',#24419,.T.);
#20386=FACE_OUTER_BOUND('',#24420,.T.);
#20387=FACE_OUTER_BOUND('',#24421,.T.);
#20388=FACE_OUTER_BOUND('',#24422,.T.);
#20389=FACE_OUTER_BOUND('',#24423,.T.);
#20390=FACE_OUTER_BOUND('',#24424,.T.);
#20391=FACE_OUTER_BOUND('',#24426,.T.);
#20392=FACE_OUTER_BOUND('',#24427,.T.);
#20393=FACE_OUTER_BOUND('',#24428,.T.);
#20394=FACE_OUTER_BOUND('',#24429,.T.);
#20395=FACE_OUTER_BOUND('',#24430,.T.);
#20396=FACE_OUTER_BOUND('',#24431,.T.);
#20397=FACE_OUTER_BOUND('',#24432,.T.);
#20398=FACE_OUTER_BOUND('',#24433,.T.);
#20399=FACE_OUTER_BOUND('',#24434,.T.);
#20400=FACE_OUTER_BOUND('',#24435,.T.);
#20401=FACE_OUTER_BOUND('',#24436,.T.);
#20402=FACE_OUTER_BOUND('',#24437,.T.);
#20403=FACE_OUTER_BOUND('',#24438,.T.);
#20404=FACE_OUTER_BOUND('',#24439,.T.);
#20405=FACE_OUTER_BOUND('',#24440,.T.);
#20406=FACE_OUTER_BOUND('',#24441,.T.);
#20407=FACE_OUTER_BOUND('',#24442,.T.);
#20408=FACE_OUTER_BOUND('',#24443,.T.);
#20409=FACE_OUTER_BOUND('',#24444,.T.);
#20410=FACE_OUTER_BOUND('',#24445,.T.);
#20411=FACE_OUTER_BOUND('',#24446,.T.);
#20412=FACE_OUTER_BOUND('',#24447,.T.);
#20413=FACE_OUTER_BOUND('',#24448,.T.);
#20414=FACE_OUTER_BOUND('',#24449,.T.);
#20415=FACE_OUTER_BOUND('',#24450,.T.);
#20416=FACE_OUTER_BOUND('',#24451,.T.);
#20417=FACE_OUTER_BOUND('',#24452,.T.);
#20418=FACE_OUTER_BOUND('',#24453,.T.);
#20419=FACE_OUTER_BOUND('',#24454,.T.);
#20420=FACE_OUTER_BOUND('',#24456,.T.);
#20421=FACE_OUTER_BOUND('',#24457,.T.);
#20422=FACE_OUTER_BOUND('',#24458,.T.);
#20423=FACE_OUTER_BOUND('',#24459,.T.);
#20424=FACE_OUTER_BOUND('',#24460,.T.);
#20425=FACE_OUTER_BOUND('',#24461,.T.);
#20426=FACE_OUTER_BOUND('',#24462,.T.);
#20427=FACE_OUTER_BOUND('',#24463,.T.);
#20428=FACE_OUTER_BOUND('',#24464,.T.);
#20429=FACE_OUTER_BOUND('',#24465,.T.);
#20430=FACE_OUTER_BOUND('',#24466,.T.);
#20431=FACE_OUTER_BOUND('',#24467,.T.);
#20432=FACE_OUTER_BOUND('',#24468,.T.);
#20433=FACE_OUTER_BOUND('',#24469,.T.);
#20434=FACE_OUTER_BOUND('',#24470,.T.);
#20435=FACE_OUTER_BOUND('',#24471,.T.);
#20436=FACE_OUTER_BOUND('',#24472,.T.);
#20437=FACE_OUTER_BOUND('',#24473,.T.);
#20438=FACE_OUTER_BOUND('',#24475,.T.);
#20439=FACE_OUTER_BOUND('',#24476,.T.);
#20440=FACE_OUTER_BOUND('',#24477,.T.);
#20441=FACE_OUTER_BOUND('',#24479,.T.);
#20442=FACE_OUTER_BOUND('',#24481,.T.);
#20443=FACE_OUTER_BOUND('',#24482,.T.);
#20444=FACE_OUTER_BOUND('',#24483,.T.);
#20445=FACE_OUTER_BOUND('',#24484,.T.);
#20446=FACE_OUTER_BOUND('',#24485,.T.);
#20447=FACE_OUTER_BOUND('',#24486,.T.);
#20448=FACE_OUTER_BOUND('',#24487,.T.);
#20449=FACE_OUTER_BOUND('',#24488,.T.);
#20450=FACE_OUTER_BOUND('',#24489,.T.);
#20451=FACE_OUTER_BOUND('',#24490,.T.);
#20452=FACE_OUTER_BOUND('',#24491,.T.);
#20453=FACE_OUTER_BOUND('',#24492,.T.);
#20454=FACE_OUTER_BOUND('',#24493,.T.);
#20455=FACE_OUTER_BOUND('',#24494,.T.);
#20456=FACE_OUTER_BOUND('',#24495,.T.);
#20457=FACE_OUTER_BOUND('',#24496,.T.);
#20458=FACE_OUTER_BOUND('',#24497,.T.);
#20459=FACE_OUTER_BOUND('',#24498,.T.);
#20460=FACE_OUTER_BOUND('',#24499,.T.);
#20461=FACE_OUTER_BOUND('',#24500,.T.);
#20462=FACE_OUTER_BOUND('',#24501,.T.);
#20463=FACE_OUTER_BOUND('',#24502,.T.);
#20464=FACE_OUTER_BOUND('',#24503,.T.);
#20465=FACE_OUTER_BOUND('',#24504,.T.);
#20466=FACE_OUTER_BOUND('',#24505,.T.);
#20467=FACE_OUTER_BOUND('',#24506,.T.);
#20468=FACE_OUTER_BOUND('',#24507,.T.);
#20469=FACE_OUTER_BOUND('',#24508,.T.);
#20470=FACE_OUTER_BOUND('',#24509,.T.);
#20471=FACE_OUTER_BOUND('',#24510,.T.);
#20472=FACE_OUTER_BOUND('',#24511,.T.);
#20473=FACE_OUTER_BOUND('',#24512,.T.);
#20474=FACE_OUTER_BOUND('',#24513,.T.);
#20475=FACE_OUTER_BOUND('',#24514,.T.);
#20476=FACE_OUTER_BOUND('',#24515,.T.);
#20477=FACE_OUTER_BOUND('',#24516,.T.);
#20478=FACE_OUTER_BOUND('',#24517,.T.);
#20479=FACE_OUTER_BOUND('',#24518,.T.);
#20480=FACE_OUTER_BOUND('',#24519,.T.);
#20481=FACE_OUTER_BOUND('',#24520,.T.);
#20482=FACE_OUTER_BOUND('',#24521,.T.);
#20483=FACE_OUTER_BOUND('',#24522,.T.);
#20484=FACE_OUTER_BOUND('',#24523,.T.);
#20485=FACE_OUTER_BOUND('',#24524,.T.);
#20486=FACE_OUTER_BOUND('',#24525,.T.);
#20487=FACE_OUTER_BOUND('',#24526,.T.);
#20488=FACE_OUTER_BOUND('',#24527,.T.);
#20489=FACE_OUTER_BOUND('',#24528,.T.);
#20490=FACE_OUTER_BOUND('',#24529,.T.);
#20491=FACE_OUTER_BOUND('',#24530,.T.);
#20492=FACE_OUTER_BOUND('',#24531,.T.);
#20493=FACE_OUTER_BOUND('',#24532,.T.);
#20494=FACE_OUTER_BOUND('',#24533,.T.);
#20495=FACE_OUTER_BOUND('',#24534,.T.);
#20496=FACE_OUTER_BOUND('',#24535,.T.);
#20497=FACE_OUTER_BOUND('',#24536,.T.);
#20498=FACE_OUTER_BOUND('',#24537,.T.);
#20499=FACE_OUTER_BOUND('',#24538,.T.);
#20500=FACE_OUTER_BOUND('',#24539,.T.);
#20501=FACE_OUTER_BOUND('',#24540,.T.);
#20502=FACE_OUTER_BOUND('',#24541,.T.);
#20503=FACE_OUTER_BOUND('',#24542,.T.);
#20504=FACE_OUTER_BOUND('',#24543,.T.);
#20505=FACE_OUTER_BOUND('',#24544,.T.);
#20506=FACE_OUTER_BOUND('',#24545,.T.);
#20507=FACE_OUTER_BOUND('',#24546,.T.);
#20508=FACE_OUTER_BOUND('',#24547,.T.);
#20509=FACE_OUTER_BOUND('',#24548,.T.);
#20510=FACE_OUTER_BOUND('',#24549,.T.);
#20511=FACE_OUTER_BOUND('',#24550,.T.);
#20512=FACE_OUTER_BOUND('',#24551,.T.);
#20513=FACE_OUTER_BOUND('',#24552,.T.);
#20514=FACE_OUTER_BOUND('',#24553,.T.);
#20515=FACE_OUTER_BOUND('',#24554,.T.);
#20516=FACE_OUTER_BOUND('',#24555,.T.);
#20517=FACE_OUTER_BOUND('',#24556,.T.);
#20518=FACE_OUTER_BOUND('',#24557,.T.);
#20519=FACE_OUTER_BOUND('',#24558,.T.);
#20520=FACE_OUTER_BOUND('',#24559,.T.);
#20521=FACE_OUTER_BOUND('',#24560,.T.);
#20522=FACE_OUTER_BOUND('',#24561,.T.);
#20523=FACE_OUTER_BOUND('',#24562,.T.);
#20524=FACE_OUTER_BOUND('',#24563,.T.);
#20525=FACE_OUTER_BOUND('',#24564,.T.);
#20526=FACE_OUTER_BOUND('',#24565,.T.);
#20527=FACE_OUTER_BOUND('',#24566,.T.);
#20528=FACE_OUTER_BOUND('',#24567,.T.);
#20529=FACE_OUTER_BOUND('',#24568,.T.);
#20530=FACE_OUTER_BOUND('',#24569,.T.);
#20531=FACE_OUTER_BOUND('',#24570,.T.);
#20532=FACE_OUTER_BOUND('',#24571,.T.);
#20533=FACE_OUTER_BOUND('',#24572,.T.);
#20534=FACE_OUTER_BOUND('',#24573,.T.);
#20535=FACE_OUTER_BOUND('',#24574,.T.);
#20536=FACE_OUTER_BOUND('',#24575,.T.);
#20537=FACE_OUTER_BOUND('',#24576,.T.);
#20538=FACE_OUTER_BOUND('',#24577,.T.);
#20539=FACE_OUTER_BOUND('',#24578,.T.);
#20540=FACE_OUTER_BOUND('',#24579,.T.);
#20541=FACE_OUTER_BOUND('',#24580,.T.);
#20542=FACE_OUTER_BOUND('',#24581,.T.);
#20543=FACE_OUTER_BOUND('',#24582,.T.);
#20544=FACE_OUTER_BOUND('',#24583,.T.);
#20545=FACE_OUTER_BOUND('',#24584,.T.);
#20546=FACE_OUTER_BOUND('',#24585,.T.);
#20547=FACE_OUTER_BOUND('',#24586,.T.);
#20548=FACE_OUTER_BOUND('',#24587,.T.);
#20549=FACE_OUTER_BOUND('',#24588,.T.);
#20550=FACE_OUTER_BOUND('',#24589,.T.);
#20551=FACE_OUTER_BOUND('',#24590,.T.);
#20552=FACE_OUTER_BOUND('',#24591,.T.);
#20553=FACE_OUTER_BOUND('',#24592,.T.);
#20554=FACE_OUTER_BOUND('',#24593,.T.);
#20555=FACE_OUTER_BOUND('',#24595,.T.);
#20556=FACE_OUTER_BOUND('',#24596,.T.);
#20557=FACE_OUTER_BOUND('',#24597,.T.);
#20558=FACE_OUTER_BOUND('',#24598,.T.);
#20559=FACE_OUTER_BOUND('',#24599,.T.);
#20560=FACE_OUTER_BOUND('',#24600,.T.);
#20561=FACE_OUTER_BOUND('',#24601,.T.);
#20562=FACE_OUTER_BOUND('',#24602,.T.);
#20563=FACE_OUTER_BOUND('',#24603,.T.);
#20564=FACE_OUTER_BOUND('',#24604,.T.);
#20565=FACE_OUTER_BOUND('',#24606,.T.);
#20566=FACE_OUTER_BOUND('',#24607,.T.);
#20567=FACE_OUTER_BOUND('',#24608,.T.);
#20568=FACE_OUTER_BOUND('',#24609,.T.);
#20569=FACE_OUTER_BOUND('',#24610,.T.);
#20570=FACE_OUTER_BOUND('',#24612,.T.);
#20571=FACE_OUTER_BOUND('',#24613,.T.);
#20572=FACE_OUTER_BOUND('',#24614,.T.);
#20573=FACE_OUTER_BOUND('',#24615,.T.);
#20574=FACE_OUTER_BOUND('',#24617,.T.);
#20575=FACE_OUTER_BOUND('',#24618,.T.);
#20576=FACE_OUTER_BOUND('',#24619,.T.);
#20577=FACE_OUTER_BOUND('',#24620,.T.);
#20578=FACE_OUTER_BOUND('',#24621,.T.);
#20579=FACE_OUTER_BOUND('',#24622,.T.);
#20580=FACE_OUTER_BOUND('',#24623,.T.);
#20581=FACE_OUTER_BOUND('',#24624,.T.);
#20582=FACE_OUTER_BOUND('',#24625,.T.);
#20583=FACE_OUTER_BOUND('',#24626,.T.);
#20584=FACE_OUTER_BOUND('',#24627,.T.);
#20585=FACE_OUTER_BOUND('',#24628,.T.);
#20586=FACE_OUTER_BOUND('',#24629,.T.);
#20587=FACE_OUTER_BOUND('',#24630,.T.);
#20588=FACE_OUTER_BOUND('',#24631,.T.);
#20589=FACE_OUTER_BOUND('',#24632,.T.);
#20590=FACE_OUTER_BOUND('',#24633,.T.);
#20591=FACE_OUTER_BOUND('',#24634,.T.);
#20592=FACE_OUTER_BOUND('',#24635,.T.);
#20593=FACE_OUTER_BOUND('',#24636,.T.);
#20594=FACE_OUTER_BOUND('',#24637,.T.);
#20595=FACE_OUTER_BOUND('',#24638,.T.);
#20596=FACE_OUTER_BOUND('',#24639,.T.);
#20597=FACE_OUTER_BOUND('',#24640,.T.);
#20598=FACE_OUTER_BOUND('',#24641,.T.);
#20599=FACE_OUTER_BOUND('',#24642,.T.);
#20600=FACE_OUTER_BOUND('',#24643,.T.);
#20601=FACE_OUTER_BOUND('',#24646,.T.);
#20602=FACE_OUTER_BOUND('',#24647,.T.);
#20603=FACE_OUTER_BOUND('',#24648,.T.);
#20604=FACE_OUTER_BOUND('',#24649,.T.);
#20605=FACE_OUTER_BOUND('',#24650,.T.);
#20606=FACE_OUTER_BOUND('',#24651,.T.);
#20607=FACE_OUTER_BOUND('',#24652,.T.);
#20608=FACE_OUTER_BOUND('',#24653,.T.);
#20609=FACE_OUTER_BOUND('',#24654,.T.);
#20610=FACE_OUTER_BOUND('',#24655,.T.);
#20611=FACE_OUTER_BOUND('',#24656,.T.);
#20612=FACE_OUTER_BOUND('',#24657,.T.);
#20613=FACE_OUTER_BOUND('',#24658,.T.);
#20614=FACE_OUTER_BOUND('',#24659,.T.);
#20615=FACE_OUTER_BOUND('',#24660,.T.);
#20616=FACE_OUTER_BOUND('',#24661,.T.);
#20617=FACE_OUTER_BOUND('',#24662,.T.);
#20618=FACE_OUTER_BOUND('',#24663,.T.);
#20619=FACE_OUTER_BOUND('',#24664,.T.);
#20620=FACE_OUTER_BOUND('',#24665,.T.);
#20621=FACE_OUTER_BOUND('',#24666,.T.);
#20622=FACE_OUTER_BOUND('',#24667,.T.);
#20623=FACE_OUTER_BOUND('',#24668,.T.);
#20624=FACE_OUTER_BOUND('',#24669,.T.);
#20625=FACE_OUTER_BOUND('',#24670,.T.);
#20626=FACE_OUTER_BOUND('',#24671,.T.);
#20627=FACE_OUTER_BOUND('',#24672,.T.);
#20628=FACE_OUTER_BOUND('',#24673,.T.);
#20629=FACE_OUTER_BOUND('',#24674,.T.);
#20630=FACE_OUTER_BOUND('',#24675,.T.);
#20631=FACE_OUTER_BOUND('',#24676,.T.);
#20632=FACE_OUTER_BOUND('',#24677,.T.);
#20633=FACE_OUTER_BOUND('',#24678,.T.);
#20634=FACE_OUTER_BOUND('',#24679,.T.);
#20635=FACE_OUTER_BOUND('',#24680,.T.);
#20636=FACE_OUTER_BOUND('',#24681,.T.);
#20637=FACE_OUTER_BOUND('',#24682,.T.);
#20638=FACE_OUTER_BOUND('',#24683,.T.);
#20639=FACE_OUTER_BOUND('',#24684,.T.);
#20640=FACE_OUTER_BOUND('',#24685,.T.);
#20641=FACE_OUTER_BOUND('',#24686,.T.);
#20642=FACE_OUTER_BOUND('',#24687,.T.);
#20643=FACE_OUTER_BOUND('',#24688,.T.);
#20644=FACE_OUTER_BOUND('',#24689,.T.);
#20645=FACE_OUTER_BOUND('',#24690,.T.);
#20646=FACE_OUTER_BOUND('',#24691,.T.);
#20647=FACE_OUTER_BOUND('',#24692,.T.);
#20648=FACE_OUTER_BOUND('',#24693,.T.);
#20649=FACE_OUTER_BOUND('',#24694,.T.);
#20650=FACE_OUTER_BOUND('',#24695,.T.);
#20651=FACE_OUTER_BOUND('',#24696,.T.);
#20652=FACE_OUTER_BOUND('',#24697,.T.);
#20653=FACE_OUTER_BOUND('',#24698,.T.);
#20654=FACE_OUTER_BOUND('',#24699,.T.);
#20655=FACE_OUTER_BOUND('',#24700,.T.);
#20656=FACE_OUTER_BOUND('',#24702,.T.);
#20657=FACE_OUTER_BOUND('',#24704,.T.);
#20658=FACE_OUTER_BOUND('',#24706,.T.);
#20659=FACE_OUTER_BOUND('',#24707,.T.);
#20660=FACE_OUTER_BOUND('',#24708,.T.);
#20661=FACE_OUTER_BOUND('',#24709,.T.);
#20662=FACE_OUTER_BOUND('',#24710,.T.);
#20663=FACE_OUTER_BOUND('',#24711,.T.);
#20664=FACE_OUTER_BOUND('',#24712,.T.);
#20665=FACE_OUTER_BOUND('',#24714,.T.);
#20666=FACE_OUTER_BOUND('',#24716,.T.);
#20667=FACE_OUTER_BOUND('',#24718,.T.);
#20668=FACE_OUTER_BOUND('',#24720,.T.);
#20669=FACE_OUTER_BOUND('',#24721,.T.);
#20670=FACE_OUTER_BOUND('',#24722,.T.);
#20671=FACE_OUTER_BOUND('',#24723,.T.);
#20672=FACE_OUTER_BOUND('',#24724,.T.);
#20673=FACE_OUTER_BOUND('',#24725,.T.);
#20674=FACE_OUTER_BOUND('',#24726,.T.);
#20675=FACE_OUTER_BOUND('',#24727,.T.);
#20676=FACE_OUTER_BOUND('',#24728,.T.);
#20677=FACE_OUTER_BOUND('',#24729,.T.);
#20678=FACE_OUTER_BOUND('',#24730,.T.);
#20679=FACE_OUTER_BOUND('',#24731,.T.);
#20680=FACE_OUTER_BOUND('',#24732,.T.);
#20681=FACE_OUTER_BOUND('',#24734,.T.);
#20682=FACE_OUTER_BOUND('',#24736,.T.);
#20683=FACE_OUTER_BOUND('',#24738,.T.);
#20684=FACE_OUTER_BOUND('',#24740,.T.);
#20685=FACE_OUTER_BOUND('',#24742,.T.);
#20686=FACE_OUTER_BOUND('',#24744,.T.);
#20687=FACE_OUTER_BOUND('',#24745,.T.);
#20688=FACE_OUTER_BOUND('',#24746,.T.);
#20689=FACE_OUTER_BOUND('',#24747,.T.);
#20690=FACE_OUTER_BOUND('',#24748,.T.);
#20691=FACE_OUTER_BOUND('',#24749,.T.);
#20692=FACE_OUTER_BOUND('',#24750,.T.);
#20693=FACE_OUTER_BOUND('',#24751,.T.);
#20694=FACE_OUTER_BOUND('',#24752,.T.);
#20695=FACE_OUTER_BOUND('',#24753,.T.);
#20696=FACE_OUTER_BOUND('',#24754,.T.);
#20697=FACE_OUTER_BOUND('',#24755,.T.);
#20698=FACE_OUTER_BOUND('',#24756,.T.);
#20699=FACE_OUTER_BOUND('',#24757,.T.);
#20700=FACE_OUTER_BOUND('',#24758,.T.);
#20701=FACE_OUTER_BOUND('',#24759,.T.);
#20702=FACE_OUTER_BOUND('',#24760,.T.);
#20703=FACE_OUTER_BOUND('',#24761,.T.);
#20704=FACE_OUTER_BOUND('',#24762,.T.);
#20705=FACE_OUTER_BOUND('',#24763,.T.);
#20706=FACE_OUTER_BOUND('',#24764,.T.);
#20707=FACE_OUTER_BOUND('',#24765,.T.);
#20708=FACE_OUTER_BOUND('',#24766,.T.);
#20709=FACE_OUTER_BOUND('',#24767,.T.);
#20710=FACE_OUTER_BOUND('',#24768,.T.);
#20711=FACE_OUTER_BOUND('',#24769,.T.);
#20712=FACE_OUTER_BOUND('',#24770,.T.);
#20713=FACE_OUTER_BOUND('',#24772,.T.);
#20714=FACE_OUTER_BOUND('',#24773,.T.);
#20715=FACE_OUTER_BOUND('',#24774,.T.);
#20716=FACE_OUTER_BOUND('',#24775,.T.);
#20717=FACE_OUTER_BOUND('',#24776,.T.);
#20718=FACE_OUTER_BOUND('',#24777,.T.);
#20719=FACE_OUTER_BOUND('',#24778,.T.);
#20720=FACE_OUTER_BOUND('',#24779,.T.);
#20721=FACE_OUTER_BOUND('',#24780,.T.);
#20722=FACE_OUTER_BOUND('',#24782,.T.);
#20723=FACE_OUTER_BOUND('',#24784,.T.);
#20724=FACE_OUTER_BOUND('',#24785,.T.);
#20725=FACE_OUTER_BOUND('',#24786,.T.);
#20726=FACE_OUTER_BOUND('',#24787,.T.);
#20727=FACE_OUTER_BOUND('',#24788,.T.);
#20728=FACE_OUTER_BOUND('',#24789,.T.);
#20729=FACE_OUTER_BOUND('',#24790,.T.);
#20730=FACE_OUTER_BOUND('',#24791,.T.);
#20731=FACE_OUTER_BOUND('',#24792,.T.);
#20732=FACE_OUTER_BOUND('',#24793,.T.);
#20733=FACE_OUTER_BOUND('',#24794,.T.);
#20734=FACE_OUTER_BOUND('',#24795,.T.);
#20735=FACE_OUTER_BOUND('',#24796,.T.);
#20736=FACE_OUTER_BOUND('',#24798,.T.);
#20737=FACE_OUTER_BOUND('',#24800,.T.);
#20738=FACE_OUTER_BOUND('',#24802,.T.);
#20739=FACE_OUTER_BOUND('',#24804,.T.);
#20740=FACE_OUTER_BOUND('',#24806,.T.);
#20741=FACE_OUTER_BOUND('',#24808,.T.);
#20742=FACE_OUTER_BOUND('',#24809,.T.);
#20743=FACE_OUTER_BOUND('',#24810,.T.);
#20744=FACE_OUTER_BOUND('',#24811,.T.);
#20745=FACE_OUTER_BOUND('',#24812,.T.);
#20746=FACE_OUTER_BOUND('',#24813,.T.);
#20747=FACE_OUTER_BOUND('',#24814,.T.);
#20748=FACE_OUTER_BOUND('',#24815,.T.);
#20749=FACE_OUTER_BOUND('',#24817,.T.);
#20750=FACE_OUTER_BOUND('',#24819,.T.);
#20751=FACE_OUTER_BOUND('',#24821,.T.);
#20752=FACE_OUTER_BOUND('',#24822,.T.);
#20753=FACE_OUTER_BOUND('',#24824,.T.);
#20754=FACE_OUTER_BOUND('',#24826,.T.);
#20755=FACE_OUTER_BOUND('',#24827,.T.);
#20756=FACE_OUTER_BOUND('',#24828,.T.);
#20757=FACE_OUTER_BOUND('',#24829,.T.);
#20758=FACE_OUTER_BOUND('',#24830,.T.);
#20759=FACE_OUTER_BOUND('',#24831,.T.);
#20760=FACE_OUTER_BOUND('',#24832,.T.);
#20761=FACE_OUTER_BOUND('',#24833,.T.);
#20762=FACE_OUTER_BOUND('',#24834,.T.);
#20763=FACE_OUTER_BOUND('',#24835,.T.);
#20764=FACE_OUTER_BOUND('',#24836,.T.);
#20765=FACE_OUTER_BOUND('',#24837,.T.);
#20766=FACE_OUTER_BOUND('',#24838,.T.);
#20767=FACE_OUTER_BOUND('',#24839,.T.);
#20768=FACE_OUTER_BOUND('',#24840,.T.);
#20769=FACE_OUTER_BOUND('',#24841,.T.);
#20770=FACE_OUTER_BOUND('',#24842,.T.);
#20771=FACE_OUTER_BOUND('',#24843,.T.);
#20772=FACE_OUTER_BOUND('',#24844,.T.);
#20773=FACE_OUTER_BOUND('',#24845,.T.);
#20774=FACE_OUTER_BOUND('',#24846,.T.);
#20775=FACE_OUTER_BOUND('',#24847,.T.);
#20776=FACE_OUTER_BOUND('',#24848,.T.);
#20777=FACE_OUTER_BOUND('',#24849,.T.);
#20778=FACE_OUTER_BOUND('',#24850,.T.);
#20779=FACE_OUTER_BOUND('',#24851,.T.);
#20780=FACE_OUTER_BOUND('',#24852,.T.);
#20781=FACE_OUTER_BOUND('',#24854,.T.);
#20782=FACE_OUTER_BOUND('',#24855,.T.);
#20783=FACE_OUTER_BOUND('',#24856,.T.);
#20784=FACE_OUTER_BOUND('',#24857,.T.);
#20785=FACE_OUTER_BOUND('',#24858,.T.);
#20786=FACE_OUTER_BOUND('',#24859,.T.);
#20787=FACE_OUTER_BOUND('',#24860,.T.);
#20788=FACE_OUTER_BOUND('',#24861,.T.);
#20789=FACE_OUTER_BOUND('',#24862,.T.);
#20790=FACE_OUTER_BOUND('',#24864,.T.);
#20791=FACE_OUTER_BOUND('',#24866,.T.);
#20792=FACE_OUTER_BOUND('',#24867,.T.);
#20793=FACE_OUTER_BOUND('',#24868,.T.);
#20794=FACE_OUTER_BOUND('',#24869,.T.);
#20795=FACE_OUTER_BOUND('',#24870,.T.);
#20796=FACE_OUTER_BOUND('',#24871,.T.);
#20797=FACE_OUTER_BOUND('',#24872,.T.);
#20798=FACE_OUTER_BOUND('',#24873,.T.);
#20799=FACE_OUTER_BOUND('',#24874,.T.);
#20800=FACE_OUTER_BOUND('',#24875,.T.);
#20801=FACE_OUTER_BOUND('',#24876,.T.);
#20802=FACE_OUTER_BOUND('',#24877,.T.);
#20803=FACE_OUTER_BOUND('',#24878,.T.);
#20804=FACE_OUTER_BOUND('',#24879,.T.);
#20805=FACE_OUTER_BOUND('',#24880,.T.);
#20806=FACE_OUTER_BOUND('',#24881,.T.);
#20807=FACE_OUTER_BOUND('',#24882,.T.);
#20808=FACE_OUTER_BOUND('',#24883,.T.);
#20809=FACE_OUTER_BOUND('',#24884,.T.);
#20810=FACE_OUTER_BOUND('',#24885,.T.);
#20811=FACE_OUTER_BOUND('',#24886,.T.);
#20812=FACE_OUTER_BOUND('',#24887,.T.);
#20813=FACE_OUTER_BOUND('',#24888,.T.);
#20814=FACE_OUTER_BOUND('',#24889,.T.);
#20815=FACE_OUTER_BOUND('',#24890,.T.);
#20816=FACE_OUTER_BOUND('',#24891,.T.);
#20817=FACE_OUTER_BOUND('',#24892,.T.);
#20818=FACE_OUTER_BOUND('',#24893,.T.);
#20819=FACE_OUTER_BOUND('',#24894,.T.);
#20820=FACE_OUTER_BOUND('',#24895,.T.);
#20821=FACE_OUTER_BOUND('',#24896,.T.);
#20822=FACE_OUTER_BOUND('',#24897,.T.);
#20823=FACE_OUTER_BOUND('',#24898,.T.);
#20824=FACE_OUTER_BOUND('',#24900,.T.);
#20825=FACE_OUTER_BOUND('',#24902,.T.);
#20826=FACE_OUTER_BOUND('',#24904,.T.);
#20827=FACE_OUTER_BOUND('',#24905,.T.);
#20828=FACE_OUTER_BOUND('',#24907,.T.);
#20829=FACE_OUTER_BOUND('',#24908,.T.);
#20830=FACE_OUTER_BOUND('',#24910,.T.);
#20831=FACE_OUTER_BOUND('',#24911,.T.);
#20832=FACE_OUTER_BOUND('',#24912,.T.);
#20833=FACE_OUTER_BOUND('',#24913,.T.);
#20834=FACE_OUTER_BOUND('',#24914,.T.);
#20835=FACE_OUTER_BOUND('',#24915,.T.);
#20836=FACE_OUTER_BOUND('',#24916,.T.);
#20837=FACE_OUTER_BOUND('',#24918,.T.);
#20838=FACE_OUTER_BOUND('',#24920,.T.);
#20839=FACE_OUTER_BOUND('',#24922,.T.);
#20840=FACE_OUTER_BOUND('',#24923,.T.);
#20841=FACE_OUTER_BOUND('',#24925,.T.);
#20842=FACE_OUTER_BOUND('',#24926,.T.);
#20843=FACE_OUTER_BOUND('',#24927,.T.);
#20844=FACE_OUTER_BOUND('',#24928,.T.);
#20845=FACE_OUTER_BOUND('',#24929,.T.);
#20846=FACE_OUTER_BOUND('',#24930,.T.);
#20847=FACE_OUTER_BOUND('',#24931,.T.);
#20848=FACE_OUTER_BOUND('',#24932,.T.);
#20849=FACE_OUTER_BOUND('',#24934,.T.);
#20850=FACE_OUTER_BOUND('',#24936,.T.);
#20851=FACE_OUTER_BOUND('',#24938,.T.);
#20852=FACE_OUTER_BOUND('',#24939,.T.);
#20853=FACE_OUTER_BOUND('',#24941,.T.);
#20854=FACE_OUTER_BOUND('',#24943,.T.);
#20855=FACE_OUTER_BOUND('',#24944,.T.);
#20856=FACE_OUTER_BOUND('',#24945,.T.);
#20857=FACE_OUTER_BOUND('',#24946,.T.);
#20858=FACE_OUTER_BOUND('',#24947,.T.);
#20859=FACE_OUTER_BOUND('',#24948,.T.);
#20860=FACE_OUTER_BOUND('',#24949,.T.);
#20861=FACE_OUTER_BOUND('',#24950,.T.);
#20862=FACE_OUTER_BOUND('',#24951,.T.);
#20863=FACE_OUTER_BOUND('',#24952,.T.);
#20864=FACE_OUTER_BOUND('',#24956,.T.);
#20865=FACE_OUTER_BOUND('',#24957,.T.);
#20866=FACE_OUTER_BOUND('',#24958,.T.);
#20867=FACE_OUTER_BOUND('',#24962,.T.);
#20868=FACE_OUTER_BOUND('',#24963,.T.);
#20869=FACE_OUTER_BOUND('',#24964,.T.);
#20870=FACE_OUTER_BOUND('',#24965,.T.);
#20871=FACE_OUTER_BOUND('',#24966,.T.);
#20872=FACE_OUTER_BOUND('',#24967,.T.);
#20873=FACE_OUTER_BOUND('',#24968,.T.);
#20874=FACE_OUTER_BOUND('',#24969,.T.);
#20875=FACE_OUTER_BOUND('',#24970,.T.);
#20876=FACE_OUTER_BOUND('',#24971,.T.);
#20877=FACE_OUTER_BOUND('',#24972,.T.);
#20878=FACE_OUTER_BOUND('',#24973,.T.);
#20879=FACE_OUTER_BOUND('',#24974,.T.);
#20880=FACE_OUTER_BOUND('',#24975,.T.);
#20881=FACE_OUTER_BOUND('',#24976,.T.);
#20882=FACE_OUTER_BOUND('',#24977,.T.);
#20883=FACE_OUTER_BOUND('',#24978,.T.);
#20884=FACE_OUTER_BOUND('',#24979,.T.);
#20885=FACE_OUTER_BOUND('',#24980,.T.);
#20886=FACE_OUTER_BOUND('',#24981,.T.);
#20887=FACE_OUTER_BOUND('',#24982,.T.);
#20888=FACE_OUTER_BOUND('',#24983,.T.);
#20889=FACE_OUTER_BOUND('',#24985,.T.);
#20890=FACE_OUTER_BOUND('',#24987,.T.);
#20891=FACE_OUTER_BOUND('',#24988,.T.);
#20892=FACE_OUTER_BOUND('',#24989,.T.);
#20893=FACE_OUTER_BOUND('',#24990,.T.);
#20894=FACE_OUTER_BOUND('',#24991,.T.);
#20895=FACE_OUTER_BOUND('',#24993,.T.);
#20896=FACE_OUTER_BOUND('',#24995,.T.);
#20897=FACE_OUTER_BOUND('',#24997,.T.);
#20898=FACE_OUTER_BOUND('',#24998,.T.);
#20899=FACE_OUTER_BOUND('',#24999,.T.);
#20900=FACE_OUTER_BOUND('',#25000,.T.);
#20901=FACE_OUTER_BOUND('',#25001,.T.);
#20902=FACE_OUTER_BOUND('',#25002,.T.);
#20903=FACE_OUTER_BOUND('',#25003,.T.);
#20904=FACE_OUTER_BOUND('',#25004,.T.);
#20905=FACE_OUTER_BOUND('',#25005,.T.);
#20906=FACE_OUTER_BOUND('',#25006,.T.);
#20907=FACE_OUTER_BOUND('',#25007,.T.);
#20908=FACE_OUTER_BOUND('',#25008,.T.);
#20909=FACE_OUTER_BOUND('',#25009,.T.);
#20910=FACE_OUTER_BOUND('',#25010,.T.);
#20911=FACE_OUTER_BOUND('',#25011,.T.);
#20912=FACE_OUTER_BOUND('',#25012,.T.);
#20913=FACE_OUTER_BOUND('',#25013,.T.);
#20914=FACE_OUTER_BOUND('',#25014,.T.);
#20915=FACE_OUTER_BOUND('',#25015,.T.);
#20916=FACE_OUTER_BOUND('',#25016,.T.);
#20917=FACE_OUTER_BOUND('',#25017,.T.);
#20918=FACE_OUTER_BOUND('',#25018,.T.);
#20919=FACE_OUTER_BOUND('',#25019,.T.);
#20920=FACE_OUTER_BOUND('',#25020,.T.);
#20921=FACE_OUTER_BOUND('',#25021,.T.);
#20922=FACE_OUTER_BOUND('',#25022,.T.);
#20923=FACE_OUTER_BOUND('',#25023,.T.);
#20924=FACE_OUTER_BOUND('',#25024,.T.);
#20925=FACE_OUTER_BOUND('',#25025,.T.);
#20926=FACE_OUTER_BOUND('',#25026,.T.);
#20927=FACE_OUTER_BOUND('',#25027,.T.);
#20928=FACE_OUTER_BOUND('',#25028,.T.);
#20929=FACE_OUTER_BOUND('',#25029,.T.);
#20930=FACE_OUTER_BOUND('',#25030,.T.);
#20931=FACE_OUTER_BOUND('',#25031,.T.);
#20932=FACE_OUTER_BOUND('',#25032,.T.);
#20933=FACE_OUTER_BOUND('',#25033,.T.);
#20934=FACE_OUTER_BOUND('',#25034,.T.);
#20935=FACE_OUTER_BOUND('',#25035,.T.);
#20936=FACE_OUTER_BOUND('',#25036,.T.);
#20937=FACE_OUTER_BOUND('',#25037,.T.);
#20938=FACE_OUTER_BOUND('',#25038,.T.);
#20939=FACE_OUTER_BOUND('',#25039,.T.);
#20940=FACE_OUTER_BOUND('',#25040,.T.);
#20941=FACE_OUTER_BOUND('',#25041,.T.);
#20942=FACE_OUTER_BOUND('',#25042,.T.);
#20943=FACE_OUTER_BOUND('',#25043,.T.);
#20944=FACE_OUTER_BOUND('',#25044,.T.);
#20945=FACE_OUTER_BOUND('',#25045,.T.);
#20946=FACE_OUTER_BOUND('',#25046,.T.);
#20947=FACE_OUTER_BOUND('',#25047,.T.);
#20948=FACE_OUTER_BOUND('',#25048,.T.);
#20949=FACE_OUTER_BOUND('',#25049,.T.);
#20950=FACE_OUTER_BOUND('',#25050,.T.);
#20951=FACE_OUTER_BOUND('',#25051,.T.);
#20952=FACE_OUTER_BOUND('',#25052,.T.);
#20953=FACE_OUTER_BOUND('',#25053,.T.);
#20954=FACE_OUTER_BOUND('',#25054,.T.);
#20955=FACE_OUTER_BOUND('',#25055,.T.);
#20956=FACE_OUTER_BOUND('',#25056,.T.);
#20957=FACE_OUTER_BOUND('',#25057,.T.);
#20958=FACE_OUTER_BOUND('',#25058,.T.);
#20959=FACE_OUTER_BOUND('',#25059,.T.);
#20960=FACE_OUTER_BOUND('',#25060,.T.);
#20961=FACE_OUTER_BOUND('',#25061,.T.);
#20962=FACE_OUTER_BOUND('',#25062,.T.);
#20963=FACE_OUTER_BOUND('',#25063,.T.);
#20964=FACE_OUTER_BOUND('',#25064,.T.);
#20965=FACE_OUTER_BOUND('',#25065,.T.);
#20966=FACE_OUTER_BOUND('',#25066,.T.);
#20967=FACE_OUTER_BOUND('',#25067,.T.);
#20968=FACE_OUTER_BOUND('',#25068,.T.);
#20969=FACE_OUTER_BOUND('',#25069,.T.);
#20970=FACE_OUTER_BOUND('',#25070,.T.);
#20971=FACE_OUTER_BOUND('',#25071,.T.);
#20972=FACE_OUTER_BOUND('',#25072,.T.);
#20973=FACE_OUTER_BOUND('',#25073,.T.);
#20974=FACE_OUTER_BOUND('',#25074,.T.);
#20975=FACE_OUTER_BOUND('',#25075,.T.);
#20976=FACE_OUTER_BOUND('',#25076,.T.);
#20977=FACE_OUTER_BOUND('',#25077,.T.);
#20978=FACE_OUTER_BOUND('',#25078,.T.);
#20979=FACE_OUTER_BOUND('',#25079,.T.);
#20980=FACE_OUTER_BOUND('',#25080,.T.);
#20981=FACE_OUTER_BOUND('',#25081,.T.);
#20982=FACE_OUTER_BOUND('',#25082,.T.);
#20983=FACE_OUTER_BOUND('',#25083,.T.);
#20984=FACE_OUTER_BOUND('',#25084,.T.);
#20985=FACE_OUTER_BOUND('',#25085,.T.);
#20986=FACE_OUTER_BOUND('',#25086,.T.);
#20987=FACE_OUTER_BOUND('',#25087,.T.);
#20988=FACE_OUTER_BOUND('',#25088,.T.);
#20989=FACE_OUTER_BOUND('',#25089,.T.);
#20990=FACE_OUTER_BOUND('',#25090,.T.);
#20991=FACE_OUTER_BOUND('',#25091,.T.);
#20992=FACE_OUTER_BOUND('',#25092,.T.);
#20993=FACE_OUTER_BOUND('',#25093,.T.);
#20994=FACE_OUTER_BOUND('',#25094,.T.);
#20995=FACE_OUTER_BOUND('',#25095,.T.);
#20996=FACE_OUTER_BOUND('',#25096,.T.);
#20997=FACE_OUTER_BOUND('',#25097,.T.);
#20998=FACE_OUTER_BOUND('',#25098,.T.);
#20999=FACE_OUTER_BOUND('',#25099,.T.);
#21000=FACE_OUTER_BOUND('',#25100,.T.);
#21001=FACE_OUTER_BOUND('',#25101,.T.);
#21002=FACE_OUTER_BOUND('',#25102,.T.);
#21003=FACE_OUTER_BOUND('',#25103,.T.);
#21004=FACE_OUTER_BOUND('',#25104,.T.);
#21005=FACE_OUTER_BOUND('',#25105,.T.);
#21006=FACE_OUTER_BOUND('',#25106,.T.);
#21007=FACE_OUTER_BOUND('',#25107,.T.);
#21008=FACE_OUTER_BOUND('',#25108,.T.);
#21009=FACE_OUTER_BOUND('',#25109,.T.);
#21010=FACE_OUTER_BOUND('',#25110,.T.);
#21011=FACE_OUTER_BOUND('',#25111,.T.);
#21012=FACE_OUTER_BOUND('',#25112,.T.);
#21013=FACE_OUTER_BOUND('',#25113,.T.);
#21014=FACE_OUTER_BOUND('',#25114,.T.);
#21015=FACE_OUTER_BOUND('',#25115,.T.);
#21016=FACE_OUTER_BOUND('',#25116,.T.);
#21017=FACE_OUTER_BOUND('',#25117,.T.);
#21018=FACE_OUTER_BOUND('',#25118,.T.);
#21019=FACE_OUTER_BOUND('',#25119,.T.);
#21020=FACE_OUTER_BOUND('',#25120,.T.);
#21021=FACE_OUTER_BOUND('',#25121,.T.);
#21022=FACE_OUTER_BOUND('',#25122,.T.);
#21023=FACE_OUTER_BOUND('',#25123,.T.);
#21024=FACE_OUTER_BOUND('',#25124,.T.);
#21025=FACE_OUTER_BOUND('',#25125,.T.);
#21026=FACE_OUTER_BOUND('',#25126,.T.);
#21027=FACE_OUTER_BOUND('',#25127,.T.);
#21028=FACE_OUTER_BOUND('',#25128,.T.);
#21029=FACE_OUTER_BOUND('',#25129,.T.);
#21030=FACE_OUTER_BOUND('',#25130,.T.);
#21031=FACE_OUTER_BOUND('',#25131,.T.);
#21032=FACE_OUTER_BOUND('',#25132,.T.);
#21033=FACE_OUTER_BOUND('',#25133,.T.);
#21034=FACE_OUTER_BOUND('',#25134,.T.);
#21035=FACE_OUTER_BOUND('',#25135,.T.);
#21036=FACE_OUTER_BOUND('',#25136,.T.);
#21037=FACE_OUTER_BOUND('',#25137,.T.);
#21038=FACE_OUTER_BOUND('',#25138,.T.);
#21039=FACE_OUTER_BOUND('',#25139,.T.);
#21040=FACE_OUTER_BOUND('',#25140,.T.);
#21041=FACE_OUTER_BOUND('',#25141,.T.);
#21042=FACE_OUTER_BOUND('',#25142,.T.);
#21043=FACE_OUTER_BOUND('',#25143,.T.);
#21044=FACE_OUTER_BOUND('',#25144,.T.);
#21045=FACE_OUTER_BOUND('',#25145,.T.);
#21046=FACE_OUTER_BOUND('',#25146,.T.);
#21047=FACE_OUTER_BOUND('',#25147,.T.);
#21048=FACE_OUTER_BOUND('',#25148,.T.);
#21049=FACE_OUTER_BOUND('',#25149,.T.);
#21050=FACE_OUTER_BOUND('',#25150,.T.);
#21051=FACE_OUTER_BOUND('',#25151,.T.);
#21052=FACE_OUTER_BOUND('',#25152,.T.);
#21053=FACE_OUTER_BOUND('',#25153,.T.);
#21054=FACE_OUTER_BOUND('',#25154,.T.);
#21055=FACE_OUTER_BOUND('',#25155,.T.);
#21056=FACE_OUTER_BOUND('',#25156,.T.);
#21057=FACE_OUTER_BOUND('',#25157,.T.);
#21058=FACE_OUTER_BOUND('',#25158,.T.);
#21059=FACE_OUTER_BOUND('',#25159,.T.);
#21060=FACE_OUTER_BOUND('',#25160,.T.);
#21061=FACE_OUTER_BOUND('',#25161,.T.);
#21062=FACE_OUTER_BOUND('',#25162,.T.);
#21063=FACE_OUTER_BOUND('',#25163,.T.);
#21064=FACE_OUTER_BOUND('',#25164,.T.);
#21065=FACE_OUTER_BOUND('',#25165,.T.);
#21066=FACE_OUTER_BOUND('',#25166,.T.);
#21067=FACE_OUTER_BOUND('',#25167,.T.);
#21068=FACE_OUTER_BOUND('',#25168,.T.);
#21069=FACE_OUTER_BOUND('',#25169,.T.);
#21070=FACE_OUTER_BOUND('',#25170,.T.);
#21071=FACE_OUTER_BOUND('',#25171,.T.);
#21072=FACE_OUTER_BOUND('',#25172,.T.);
#21073=FACE_OUTER_BOUND('',#25173,.T.);
#21074=FACE_OUTER_BOUND('',#25174,.T.);
#21075=FACE_OUTER_BOUND('',#25175,.T.);
#21076=FACE_OUTER_BOUND('',#25176,.T.);
#21077=FACE_OUTER_BOUND('',#25177,.T.);
#21078=FACE_OUTER_BOUND('',#25178,.T.);
#21079=FACE_OUTER_BOUND('',#25179,.T.);
#21080=FACE_OUTER_BOUND('',#25180,.T.);
#21081=FACE_OUTER_BOUND('',#25181,.T.);
#21082=FACE_OUTER_BOUND('',#25182,.T.);
#21083=FACE_OUTER_BOUND('',#25183,.T.);
#21084=FACE_OUTER_BOUND('',#25184,.T.);
#21085=FACE_OUTER_BOUND('',#25185,.T.);
#21086=FACE_OUTER_BOUND('',#25186,.T.);
#21087=FACE_OUTER_BOUND('',#25187,.T.);
#21088=FACE_OUTER_BOUND('',#25188,.T.);
#21089=FACE_OUTER_BOUND('',#25189,.T.);
#21090=FACE_OUTER_BOUND('',#25190,.T.);
#21091=FACE_OUTER_BOUND('',#25191,.T.);
#21092=FACE_OUTER_BOUND('',#25192,.T.);
#21093=FACE_OUTER_BOUND('',#25193,.T.);
#21094=FACE_OUTER_BOUND('',#25194,.T.);
#21095=FACE_OUTER_BOUND('',#25195,.T.);
#21096=FACE_OUTER_BOUND('',#25196,.T.);
#21097=FACE_OUTER_BOUND('',#25197,.T.);
#21098=FACE_OUTER_BOUND('',#25198,.T.);
#21099=FACE_OUTER_BOUND('',#25199,.T.);
#21100=FACE_OUTER_BOUND('',#25200,.T.);
#21101=FACE_OUTER_BOUND('',#25201,.T.);
#21102=FACE_OUTER_BOUND('',#25202,.T.);
#21103=FACE_OUTER_BOUND('',#25203,.T.);
#21104=FACE_OUTER_BOUND('',#25204,.T.);
#21105=FACE_OUTER_BOUND('',#25205,.T.);
#21106=FACE_OUTER_BOUND('',#25206,.T.);
#21107=FACE_OUTER_BOUND('',#25207,.T.);
#21108=FACE_OUTER_BOUND('',#25208,.T.);
#21109=FACE_OUTER_BOUND('',#25209,.T.);
#21110=FACE_OUTER_BOUND('',#25210,.T.);
#21111=FACE_OUTER_BOUND('',#25211,.T.);
#21112=FACE_OUTER_BOUND('',#25212,.T.);
#21113=FACE_OUTER_BOUND('',#25213,.T.);
#21114=FACE_OUTER_BOUND('',#25214,.T.);
#21115=FACE_OUTER_BOUND('',#25215,.T.);
#21116=FACE_OUTER_BOUND('',#25216,.T.);
#21117=FACE_OUTER_BOUND('',#25217,.T.);
#21118=FACE_OUTER_BOUND('',#25218,.T.);
#21119=FACE_OUTER_BOUND('',#25219,.T.);
#21120=FACE_OUTER_BOUND('',#25220,.T.);
#21121=FACE_OUTER_BOUND('',#25221,.T.);
#21122=FACE_OUTER_BOUND('',#25222,.T.);
#21123=FACE_OUTER_BOUND('',#25223,.T.);
#21124=FACE_OUTER_BOUND('',#25224,.T.);
#21125=FACE_OUTER_BOUND('',#25225,.T.);
#21126=FACE_OUTER_BOUND('',#25226,.T.);
#21127=FACE_OUTER_BOUND('',#25227,.T.);
#21128=FACE_OUTER_BOUND('',#25228,.T.);
#21129=FACE_OUTER_BOUND('',#25229,.T.);
#21130=FACE_OUTER_BOUND('',#25230,.T.);
#21131=FACE_OUTER_BOUND('',#25231,.T.);
#21132=FACE_OUTER_BOUND('',#25232,.T.);
#21133=FACE_OUTER_BOUND('',#25233,.T.);
#21134=FACE_OUTER_BOUND('',#25234,.T.);
#21135=FACE_OUTER_BOUND('',#25235,.T.);
#21136=FACE_OUTER_BOUND('',#25236,.T.);
#21137=FACE_OUTER_BOUND('',#25237,.T.);
#21138=FACE_OUTER_BOUND('',#25238,.T.);
#21139=FACE_OUTER_BOUND('',#25239,.T.);
#21140=FACE_OUTER_BOUND('',#25240,.T.);
#21141=FACE_OUTER_BOUND('',#25241,.T.);
#21142=FACE_OUTER_BOUND('',#25242,.T.);
#21143=FACE_OUTER_BOUND('',#25243,.T.);
#21144=FACE_OUTER_BOUND('',#25244,.T.);
#21145=FACE_OUTER_BOUND('',#25245,.T.);
#21146=FACE_OUTER_BOUND('',#25246,.T.);
#21147=FACE_OUTER_BOUND('',#25247,.T.);
#21148=FACE_OUTER_BOUND('',#25248,.T.);
#21149=FACE_OUTER_BOUND('',#25249,.T.);
#21150=FACE_OUTER_BOUND('',#25250,.T.);
#21151=FACE_OUTER_BOUND('',#25251,.T.);
#21152=FACE_OUTER_BOUND('',#25252,.T.);
#21153=FACE_OUTER_BOUND('',#25253,.T.);
#21154=FACE_OUTER_BOUND('',#25254,.T.);
#21155=FACE_OUTER_BOUND('',#25255,.T.);
#21156=FACE_OUTER_BOUND('',#25256,.T.);
#21157=FACE_OUTER_BOUND('',#25257,.T.);
#21158=FACE_OUTER_BOUND('',#25258,.T.);
#21159=FACE_OUTER_BOUND('',#25259,.T.);
#21160=FACE_OUTER_BOUND('',#25260,.T.);
#21161=FACE_OUTER_BOUND('',#25261,.T.);
#21162=FACE_OUTER_BOUND('',#25262,.T.);
#21163=FACE_OUTER_BOUND('',#25263,.T.);
#21164=FACE_OUTER_BOUND('',#25264,.T.);
#21165=FACE_OUTER_BOUND('',#25265,.T.);
#21166=FACE_OUTER_BOUND('',#25266,.T.);
#21167=FACE_OUTER_BOUND('',#25267,.T.);
#21168=FACE_OUTER_BOUND('',#25268,.T.);
#21169=FACE_OUTER_BOUND('',#25269,.T.);
#21170=FACE_OUTER_BOUND('',#25270,.T.);
#21171=FACE_OUTER_BOUND('',#25271,.T.);
#21172=FACE_OUTER_BOUND('',#25272,.T.);
#21173=FACE_OUTER_BOUND('',#25273,.T.);
#21174=FACE_OUTER_BOUND('',#25274,.T.);
#21175=FACE_OUTER_BOUND('',#25275,.T.);
#21176=FACE_OUTER_BOUND('',#25276,.T.);
#21177=FACE_OUTER_BOUND('',#25277,.T.);
#21178=FACE_OUTER_BOUND('',#25278,.T.);
#21179=FACE_OUTER_BOUND('',#25279,.T.);
#21180=FACE_OUTER_BOUND('',#25280,.T.);
#21181=FACE_OUTER_BOUND('',#25281,.T.);
#21182=FACE_OUTER_BOUND('',#25282,.T.);
#21183=FACE_OUTER_BOUND('',#25283,.T.);
#21184=FACE_OUTER_BOUND('',#25284,.T.);
#21185=FACE_OUTER_BOUND('',#25285,.T.);
#21186=FACE_OUTER_BOUND('',#25286,.T.);
#21187=FACE_OUTER_BOUND('',#25287,.T.);
#21188=FACE_OUTER_BOUND('',#25288,.T.);
#21189=FACE_OUTER_BOUND('',#25289,.T.);
#21190=FACE_OUTER_BOUND('',#25290,.T.);
#21191=FACE_OUTER_BOUND('',#25291,.T.);
#21192=FACE_OUTER_BOUND('',#25292,.T.);
#21193=FACE_OUTER_BOUND('',#25293,.T.);
#21194=FACE_OUTER_BOUND('',#25294,.T.);
#21195=FACE_OUTER_BOUND('',#25295,.T.);
#21196=FACE_OUTER_BOUND('',#25296,.T.);
#21197=FACE_OUTER_BOUND('',#25297,.T.);
#21198=FACE_OUTER_BOUND('',#25298,.T.);
#21199=FACE_OUTER_BOUND('',#25299,.T.);
#21200=FACE_OUTER_BOUND('',#25300,.T.);
#21201=FACE_OUTER_BOUND('',#25301,.T.);
#21202=FACE_OUTER_BOUND('',#25302,.T.);
#21203=FACE_OUTER_BOUND('',#25303,.T.);
#21204=FACE_OUTER_BOUND('',#25304,.T.);
#21205=FACE_OUTER_BOUND('',#25305,.T.);
#21206=FACE_OUTER_BOUND('',#25306,.T.);
#21207=FACE_OUTER_BOUND('',#25307,.T.);
#21208=FACE_OUTER_BOUND('',#25308,.T.);
#21209=FACE_OUTER_BOUND('',#25309,.T.);
#21210=FACE_OUTER_BOUND('',#25310,.T.);
#21211=FACE_OUTER_BOUND('',#25311,.T.);
#21212=FACE_OUTER_BOUND('',#25312,.T.);
#21213=FACE_OUTER_BOUND('',#25313,.T.);
#21214=FACE_OUTER_BOUND('',#25314,.T.);
#21215=FACE_OUTER_BOUND('',#25315,.T.);
#21216=FACE_OUTER_BOUND('',#25316,.T.);
#21217=FACE_OUTER_BOUND('',#25317,.T.);
#21218=FACE_OUTER_BOUND('',#25318,.T.);
#21219=FACE_OUTER_BOUND('',#25319,.T.);
#21220=FACE_OUTER_BOUND('',#25320,.T.);
#21221=FACE_OUTER_BOUND('',#25321,.T.);
#21222=FACE_OUTER_BOUND('',#25322,.T.);
#21223=FACE_OUTER_BOUND('',#25323,.T.);
#21224=FACE_OUTER_BOUND('',#25324,.T.);
#21225=FACE_OUTER_BOUND('',#25325,.T.);
#21226=FACE_OUTER_BOUND('',#25326,.T.);
#21227=FACE_OUTER_BOUND('',#25327,.T.);
#21228=FACE_OUTER_BOUND('',#25328,.T.);
#21229=FACE_OUTER_BOUND('',#25329,.T.);
#21230=FACE_OUTER_BOUND('',#25330,.T.);
#21231=FACE_OUTER_BOUND('',#25331,.T.);
#21232=FACE_OUTER_BOUND('',#25332,.T.);
#21233=FACE_OUTER_BOUND('',#25333,.T.);
#21234=FACE_OUTER_BOUND('',#25334,.T.);
#21235=FACE_OUTER_BOUND('',#25335,.T.);
#21236=FACE_OUTER_BOUND('',#25336,.T.);
#21237=FACE_OUTER_BOUND('',#25337,.T.);
#21238=FACE_OUTER_BOUND('',#25338,.T.);
#21239=FACE_OUTER_BOUND('',#25339,.T.);
#21240=FACE_OUTER_BOUND('',#25340,.T.);
#21241=FACE_OUTER_BOUND('',#25341,.T.);
#21242=FACE_OUTER_BOUND('',#25342,.T.);
#21243=FACE_OUTER_BOUND('',#25343,.T.);
#21244=FACE_OUTER_BOUND('',#25344,.T.);
#21245=FACE_OUTER_BOUND('',#25345,.T.);
#21246=FACE_OUTER_BOUND('',#25346,.T.);
#21247=FACE_OUTER_BOUND('',#25347,.T.);
#21248=FACE_OUTER_BOUND('',#25348,.T.);
#21249=FACE_OUTER_BOUND('',#25349,.T.);
#21250=FACE_OUTER_BOUND('',#25350,.T.);
#21251=FACE_OUTER_BOUND('',#25351,.T.);
#21252=FACE_OUTER_BOUND('',#25352,.T.);
#21253=FACE_OUTER_BOUND('',#25353,.T.);
#21254=FACE_OUTER_BOUND('',#25354,.T.);
#21255=FACE_OUTER_BOUND('',#25355,.T.);
#21256=FACE_OUTER_BOUND('',#25356,.T.);
#21257=FACE_OUTER_BOUND('',#25357,.T.);
#21258=FACE_OUTER_BOUND('',#25358,.T.);
#21259=FACE_OUTER_BOUND('',#25359,.T.);
#21260=FACE_OUTER_BOUND('',#25360,.T.);
#21261=FACE_OUTER_BOUND('',#25361,.T.);
#21262=FACE_OUTER_BOUND('',#25362,.T.);
#21263=FACE_OUTER_BOUND('',#25363,.T.);
#21264=FACE_OUTER_BOUND('',#25364,.T.);
#21265=FACE_OUTER_BOUND('',#25365,.T.);
#21266=FACE_OUTER_BOUND('',#25366,.T.);
#21267=FACE_OUTER_BOUND('',#25367,.T.);
#21268=FACE_OUTER_BOUND('',#25368,.T.);
#21269=FACE_OUTER_BOUND('',#25369,.T.);
#21270=FACE_OUTER_BOUND('',#25370,.T.);
#21271=FACE_OUTER_BOUND('',#25371,.T.);
#21272=FACE_OUTER_BOUND('',#25372,.T.);
#21273=FACE_OUTER_BOUND('',#25373,.T.);
#21274=FACE_OUTER_BOUND('',#25374,.T.);
#21275=FACE_OUTER_BOUND('',#25375,.T.);
#21276=FACE_OUTER_BOUND('',#25376,.T.);
#21277=FACE_OUTER_BOUND('',#25377,.T.);
#21278=FACE_OUTER_BOUND('',#25378,.T.);
#21279=FACE_OUTER_BOUND('',#25379,.T.);
#21280=FACE_OUTER_BOUND('',#25380,.T.);
#21281=FACE_OUTER_BOUND('',#25381,.T.);
#21282=FACE_OUTER_BOUND('',#25382,.T.);
#21283=FACE_OUTER_BOUND('',#25383,.T.);
#21284=FACE_OUTER_BOUND('',#25384,.T.);
#21285=FACE_OUTER_BOUND('',#25385,.T.);
#21286=FACE_OUTER_BOUND('',#25386,.T.);
#21287=FACE_OUTER_BOUND('',#25387,.T.);
#21288=FACE_OUTER_BOUND('',#25388,.T.);
#21289=FACE_OUTER_BOUND('',#25389,.T.);
#21290=FACE_OUTER_BOUND('',#25390,.T.);
#21291=FACE_OUTER_BOUND('',#25391,.T.);
#21292=FACE_OUTER_BOUND('',#25392,.T.);
#21293=FACE_OUTER_BOUND('',#25393,.T.);
#21294=FACE_OUTER_BOUND('',#25394,.T.);
#21295=FACE_OUTER_BOUND('',#25395,.T.);
#21296=FACE_OUTER_BOUND('',#25396,.T.);
#21297=FACE_OUTER_BOUND('',#25397,.T.);
#21298=FACE_OUTER_BOUND('',#25398,.T.);
#21299=FACE_OUTER_BOUND('',#25399,.T.);
#21300=FACE_OUTER_BOUND('',#25400,.T.);
#21301=FACE_OUTER_BOUND('',#25401,.T.);
#21302=FACE_OUTER_BOUND('',#25402,.T.);
#21303=FACE_OUTER_BOUND('',#25403,.T.);
#21304=FACE_OUTER_BOUND('',#25404,.T.);
#21305=FACE_OUTER_BOUND('',#25405,.T.);
#21306=FACE_OUTER_BOUND('',#25406,.T.);
#21307=FACE_OUTER_BOUND('',#25407,.T.);
#21308=FACE_OUTER_BOUND('',#25408,.T.);
#21309=FACE_OUTER_BOUND('',#25409,.T.);
#21310=FACE_OUTER_BOUND('',#25410,.T.);
#21311=FACE_OUTER_BOUND('',#25411,.T.);
#21312=FACE_OUTER_BOUND('',#25412,.T.);
#21313=FACE_OUTER_BOUND('',#25413,.T.);
#21314=FACE_OUTER_BOUND('',#25414,.T.);
#21315=FACE_OUTER_BOUND('',#25415,.T.);
#21316=FACE_OUTER_BOUND('',#25416,.T.);
#21317=FACE_OUTER_BOUND('',#25417,.T.);
#21318=FACE_OUTER_BOUND('',#25418,.T.);
#21319=FACE_OUTER_BOUND('',#25419,.T.);
#21320=FACE_OUTER_BOUND('',#25420,.T.);
#21321=FACE_OUTER_BOUND('',#25421,.T.);
#21322=FACE_OUTER_BOUND('',#25422,.T.);
#21323=FACE_OUTER_BOUND('',#25423,.T.);
#21324=FACE_OUTER_BOUND('',#25424,.T.);
#21325=FACE_OUTER_BOUND('',#25425,.T.);
#21326=FACE_OUTER_BOUND('',#25426,.T.);
#21327=FACE_OUTER_BOUND('',#25427,.T.);
#21328=FACE_OUTER_BOUND('',#25428,.T.);
#21329=FACE_OUTER_BOUND('',#25429,.T.);
#21330=FACE_OUTER_BOUND('',#25430,.T.);
#21331=FACE_OUTER_BOUND('',#25431,.T.);
#21332=FACE_OUTER_BOUND('',#25432,.T.);
#21333=FACE_OUTER_BOUND('',#25433,.T.);
#21334=FACE_OUTER_BOUND('',#25434,.T.);
#21335=FACE_OUTER_BOUND('',#25435,.T.);
#21336=FACE_OUTER_BOUND('',#25436,.T.);
#21337=FACE_OUTER_BOUND('',#25437,.T.);
#21338=FACE_OUTER_BOUND('',#25438,.T.);
#21339=FACE_OUTER_BOUND('',#25439,.T.);
#21340=FACE_OUTER_BOUND('',#25440,.T.);
#21341=FACE_OUTER_BOUND('',#25441,.T.);
#21342=FACE_OUTER_BOUND('',#25442,.T.);
#21343=FACE_OUTER_BOUND('',#25443,.T.);
#21344=FACE_OUTER_BOUND('',#25444,.T.);
#21345=FACE_OUTER_BOUND('',#25445,.T.);
#21346=FACE_OUTER_BOUND('',#25446,.T.);
#21347=FACE_OUTER_BOUND('',#25447,.T.);
#21348=FACE_OUTER_BOUND('',#25448,.T.);
#21349=FACE_OUTER_BOUND('',#25449,.T.);
#21350=FACE_OUTER_BOUND('',#25450,.T.);
#21351=FACE_OUTER_BOUND('',#25451,.T.);
#21352=FACE_OUTER_BOUND('',#25452,.T.);
#21353=FACE_OUTER_BOUND('',#25453,.T.);
#21354=FACE_OUTER_BOUND('',#25454,.T.);
#21355=FACE_OUTER_BOUND('',#25455,.T.);
#21356=FACE_OUTER_BOUND('',#25456,.T.);
#21357=FACE_OUTER_BOUND('',#25457,.T.);
#21358=FACE_OUTER_BOUND('',#25458,.T.);
#21359=FACE_OUTER_BOUND('',#25459,.T.);
#21360=FACE_OUTER_BOUND('',#25460,.T.);
#21361=FACE_OUTER_BOUND('',#25461,.T.);
#21362=FACE_OUTER_BOUND('',#25462,.T.);
#21363=FACE_OUTER_BOUND('',#25463,.T.);
#21364=FACE_OUTER_BOUND('',#25464,.T.);
#21365=FACE_OUTER_BOUND('',#25465,.T.);
#21366=FACE_OUTER_BOUND('',#25466,.T.);
#21367=FACE_OUTER_BOUND('',#25467,.T.);
#21368=FACE_OUTER_BOUND('',#25468,.T.);
#21369=FACE_OUTER_BOUND('',#25469,.T.);
#21370=FACE_OUTER_BOUND('',#25470,.T.);
#21371=FACE_OUTER_BOUND('',#25471,.T.);
#21372=FACE_OUTER_BOUND('',#25472,.T.);
#21373=FACE_OUTER_BOUND('',#25473,.T.);
#21374=FACE_OUTER_BOUND('',#25474,.T.);
#21375=FACE_OUTER_BOUND('',#25475,.T.);
#21376=FACE_OUTER_BOUND('',#25476,.T.);
#21377=FACE_OUTER_BOUND('',#25477,.T.);
#21378=FACE_OUTER_BOUND('',#25478,.T.);
#21379=FACE_OUTER_BOUND('',#25479,.T.);
#21380=FACE_OUTER_BOUND('',#25480,.T.);
#21381=FACE_OUTER_BOUND('',#25481,.T.);
#21382=FACE_OUTER_BOUND('',#25482,.T.);
#21383=FACE_OUTER_BOUND('',#25483,.T.);
#21384=FACE_OUTER_BOUND('',#25484,.T.);
#21385=FACE_OUTER_BOUND('',#25485,.T.);
#21386=FACE_OUTER_BOUND('',#25486,.T.);
#21387=FACE_OUTER_BOUND('',#25487,.T.);
#21388=FACE_OUTER_BOUND('',#25488,.T.);
#21389=FACE_OUTER_BOUND('',#25489,.T.);
#21390=FACE_OUTER_BOUND('',#25490,.T.);
#21391=FACE_OUTER_BOUND('',#25491,.T.);
#21392=FACE_OUTER_BOUND('',#25492,.T.);
#21393=FACE_OUTER_BOUND('',#25493,.T.);
#21394=FACE_OUTER_BOUND('',#25494,.T.);
#21395=FACE_OUTER_BOUND('',#25495,.T.);
#21396=FACE_OUTER_BOUND('',#25496,.T.);
#21397=FACE_OUTER_BOUND('',#25497,.T.);
#21398=FACE_OUTER_BOUND('',#25498,.T.);
#21399=FACE_OUTER_BOUND('',#25499,.T.);
#21400=FACE_OUTER_BOUND('',#25500,.T.);
#21401=FACE_OUTER_BOUND('',#25501,.T.);
#21402=FACE_OUTER_BOUND('',#25502,.T.);
#21403=FACE_OUTER_BOUND('',#25503,.T.);
#21404=FACE_OUTER_BOUND('',#25504,.T.);
#21405=FACE_OUTER_BOUND('',#25505,.T.);
#21406=FACE_OUTER_BOUND('',#25506,.T.);
#21407=FACE_OUTER_BOUND('',#25507,.T.);
#21408=FACE_OUTER_BOUND('',#25508,.T.);
#21409=FACE_OUTER_BOUND('',#25509,.T.);
#21410=FACE_OUTER_BOUND('',#25510,.T.);
#21411=FACE_OUTER_BOUND('',#25511,.T.);
#21412=FACE_OUTER_BOUND('',#25512,.T.);
#21413=FACE_OUTER_BOUND('',#25513,.T.);
#21414=FACE_OUTER_BOUND('',#25514,.T.);
#21415=FACE_OUTER_BOUND('',#25515,.T.);
#21416=FACE_OUTER_BOUND('',#25516,.T.);
#21417=FACE_OUTER_BOUND('',#25517,.T.);
#21418=FACE_OUTER_BOUND('',#25518,.T.);
#21419=FACE_OUTER_BOUND('',#25519,.T.);
#21420=FACE_OUTER_BOUND('',#25520,.T.);
#21421=FACE_OUTER_BOUND('',#25521,.T.);
#21422=FACE_OUTER_BOUND('',#25522,.T.);
#21423=FACE_OUTER_BOUND('',#25523,.T.);
#21424=FACE_OUTER_BOUND('',#25524,.T.);
#21425=FACE_OUTER_BOUND('',#25525,.T.);
#21426=FACE_OUTER_BOUND('',#25526,.T.);
#21427=FACE_OUTER_BOUND('',#25527,.T.);
#21428=FACE_OUTER_BOUND('',#25528,.T.);
#21429=FACE_OUTER_BOUND('',#25529,.T.);
#21430=FACE_OUTER_BOUND('',#25530,.T.);
#21431=FACE_OUTER_BOUND('',#25531,.T.);
#21432=FACE_OUTER_BOUND('',#25532,.T.);
#21433=FACE_OUTER_BOUND('',#25533,.T.);
#21434=FACE_OUTER_BOUND('',#25534,.T.);
#21435=FACE_OUTER_BOUND('',#25535,.T.);
#21436=FACE_OUTER_BOUND('',#25536,.T.);
#21437=FACE_OUTER_BOUND('',#25537,.T.);
#21438=FACE_OUTER_BOUND('',#25538,.T.);
#21439=FACE_OUTER_BOUND('',#25539,.T.);
#21440=FACE_OUTER_BOUND('',#25540,.T.);
#21441=FACE_OUTER_BOUND('',#25541,.T.);
#21442=FACE_OUTER_BOUND('',#25542,.T.);
#21443=FACE_OUTER_BOUND('',#25543,.T.);
#21444=FACE_OUTER_BOUND('',#25544,.T.);
#21445=FACE_OUTER_BOUND('',#25545,.T.);
#21446=FACE_OUTER_BOUND('',#25546,.T.);
#21447=FACE_OUTER_BOUND('',#25547,.T.);
#21448=FACE_OUTER_BOUND('',#25548,.T.);
#21449=FACE_OUTER_BOUND('',#25549,.T.);
#21450=FACE_OUTER_BOUND('',#25550,.T.);
#21451=FACE_OUTER_BOUND('',#25551,.T.);
#21452=FACE_OUTER_BOUND('',#25552,.T.);
#21453=FACE_OUTER_BOUND('',#25553,.T.);
#21454=FACE_OUTER_BOUND('',#25554,.T.);
#21455=FACE_OUTER_BOUND('',#25555,.T.);
#21456=FACE_OUTER_BOUND('',#25556,.T.);
#21457=FACE_OUTER_BOUND('',#25557,.T.);
#21458=FACE_OUTER_BOUND('',#25558,.T.);
#21459=FACE_OUTER_BOUND('',#25559,.T.);
#21460=FACE_OUTER_BOUND('',#25560,.T.);
#21461=FACE_OUTER_BOUND('',#25561,.T.);
#21462=FACE_OUTER_BOUND('',#25562,.T.);
#21463=FACE_OUTER_BOUND('',#25563,.T.);
#21464=FACE_OUTER_BOUND('',#25564,.T.);
#21465=FACE_OUTER_BOUND('',#25565,.T.);
#21466=FACE_OUTER_BOUND('',#25566,.T.);
#21467=FACE_OUTER_BOUND('',#25567,.T.);
#21468=FACE_OUTER_BOUND('',#25568,.T.);
#21469=FACE_OUTER_BOUND('',#25569,.T.);
#21470=FACE_OUTER_BOUND('',#25570,.T.);
#21471=FACE_OUTER_BOUND('',#25571,.T.);
#21472=FACE_OUTER_BOUND('',#25572,.T.);
#21473=FACE_OUTER_BOUND('',#25573,.T.);
#21474=FACE_OUTER_BOUND('',#25574,.T.);
#21475=FACE_OUTER_BOUND('',#25575,.T.);
#21476=FACE_OUTER_BOUND('',#25576,.T.);
#21477=FACE_OUTER_BOUND('',#25577,.T.);
#21478=FACE_OUTER_BOUND('',#25578,.T.);
#21479=FACE_OUTER_BOUND('',#25579,.T.);
#21480=FACE_OUTER_BOUND('',#25580,.T.);
#21481=FACE_OUTER_BOUND('',#25581,.T.);
#21482=FACE_OUTER_BOUND('',#25582,.T.);
#21483=FACE_OUTER_BOUND('',#25583,.T.);
#21484=FACE_OUTER_BOUND('',#25584,.T.);
#21485=FACE_OUTER_BOUND('',#25585,.T.);
#21486=FACE_OUTER_BOUND('',#25586,.T.);
#21487=FACE_OUTER_BOUND('',#25587,.T.);
#21488=FACE_OUTER_BOUND('',#25588,.T.);
#21489=FACE_OUTER_BOUND('',#25589,.T.);
#21490=FACE_OUTER_BOUND('',#25590,.T.);
#21491=FACE_OUTER_BOUND('',#25591,.T.);
#21492=FACE_OUTER_BOUND('',#25592,.T.);
#21493=FACE_OUTER_BOUND('',#25593,.T.);
#21494=FACE_OUTER_BOUND('',#25594,.T.);
#21495=FACE_OUTER_BOUND('',#25595,.T.);
#21496=FACE_OUTER_BOUND('',#25596,.T.);
#21497=FACE_OUTER_BOUND('',#25597,.T.);
#21498=FACE_OUTER_BOUND('',#25598,.T.);
#21499=FACE_OUTER_BOUND('',#25599,.T.);
#21500=FACE_OUTER_BOUND('',#25600,.T.);
#21501=FACE_OUTER_BOUND('',#25601,.T.);
#21502=FACE_OUTER_BOUND('',#25602,.T.);
#21503=FACE_OUTER_BOUND('',#25603,.T.);
#21504=FACE_OUTER_BOUND('',#25604,.T.);
#21505=FACE_OUTER_BOUND('',#25605,.T.);
#21506=FACE_OUTER_BOUND('',#25606,.T.);
#21507=FACE_OUTER_BOUND('',#25607,.T.);
#21508=FACE_OUTER_BOUND('',#25608,.T.);
#21509=FACE_OUTER_BOUND('',#25609,.T.);
#21510=FACE_OUTER_BOUND('',#25610,.T.);
#21511=FACE_OUTER_BOUND('',#25611,.T.);
#21512=FACE_OUTER_BOUND('',#25612,.T.);
#21513=FACE_OUTER_BOUND('',#25613,.T.);
#21514=FACE_OUTER_BOUND('',#25614,.T.);
#21515=FACE_OUTER_BOUND('',#25615,.T.);
#21516=FACE_OUTER_BOUND('',#25616,.T.);
#21517=FACE_OUTER_BOUND('',#25617,.T.);
#21518=FACE_OUTER_BOUND('',#25618,.T.);
#21519=FACE_OUTER_BOUND('',#25619,.T.);
#21520=FACE_OUTER_BOUND('',#25620,.T.);
#21521=FACE_OUTER_BOUND('',#25621,.T.);
#21522=FACE_OUTER_BOUND('',#25622,.T.);
#21523=FACE_OUTER_BOUND('',#25623,.T.);
#21524=FACE_OUTER_BOUND('',#25624,.T.);
#21525=FACE_OUTER_BOUND('',#25625,.T.);
#21526=FACE_OUTER_BOUND('',#25626,.T.);
#21527=FACE_OUTER_BOUND('',#25627,.T.);
#21528=FACE_OUTER_BOUND('',#25628,.T.);
#21529=FACE_OUTER_BOUND('',#25629,.T.);
#21530=FACE_OUTER_BOUND('',#25630,.T.);
#21531=FACE_OUTER_BOUND('',#25631,.T.);
#21532=FACE_OUTER_BOUND('',#25632,.T.);
#21533=FACE_OUTER_BOUND('',#25633,.T.);
#21534=FACE_OUTER_BOUND('',#25634,.T.);
#21535=FACE_OUTER_BOUND('',#25635,.T.);
#21536=FACE_OUTER_BOUND('',#25636,.T.);
#21537=FACE_OUTER_BOUND('',#25637,.T.);
#21538=FACE_OUTER_BOUND('',#25638,.T.);
#21539=FACE_OUTER_BOUND('',#25639,.T.);
#21540=FACE_OUTER_BOUND('',#25640,.T.);
#21541=FACE_OUTER_BOUND('',#25641,.T.);
#21542=FACE_OUTER_BOUND('',#25642,.T.);
#21543=FACE_OUTER_BOUND('',#25643,.T.);
#21544=FACE_OUTER_BOUND('',#25644,.T.);
#21545=FACE_OUTER_BOUND('',#25645,.T.);
#21546=FACE_OUTER_BOUND('',#25646,.T.);
#21547=FACE_OUTER_BOUND('',#25647,.T.);
#21548=FACE_OUTER_BOUND('',#25648,.T.);
#21549=FACE_OUTER_BOUND('',#25649,.T.);
#21550=FACE_OUTER_BOUND('',#25650,.T.);
#21551=FACE_OUTER_BOUND('',#25651,.T.);
#21552=FACE_OUTER_BOUND('',#25652,.T.);
#21553=FACE_OUTER_BOUND('',#25653,.T.);
#21554=FACE_OUTER_BOUND('',#25654,.T.);
#21555=FACE_OUTER_BOUND('',#25655,.T.);
#21556=FACE_OUTER_BOUND('',#25656,.T.);
#21557=FACE_OUTER_BOUND('',#25657,.T.);
#21558=FACE_OUTER_BOUND('',#25658,.T.);
#21559=FACE_OUTER_BOUND('',#25659,.T.);
#21560=FACE_OUTER_BOUND('',#25660,.T.);
#21561=FACE_OUTER_BOUND('',#25661,.T.);
#21562=FACE_OUTER_BOUND('',#25662,.T.);
#21563=FACE_OUTER_BOUND('',#25663,.T.);
#21564=FACE_OUTER_BOUND('',#25664,.T.);
#21565=FACE_OUTER_BOUND('',#25665,.T.);
#21566=FACE_OUTER_BOUND('',#25666,.T.);
#21567=FACE_OUTER_BOUND('',#25667,.T.);
#21568=FACE_OUTER_BOUND('',#25668,.T.);
#21569=FACE_OUTER_BOUND('',#25669,.T.);
#21570=FACE_OUTER_BOUND('',#25670,.T.);
#21571=FACE_OUTER_BOUND('',#25671,.T.);
#21572=FACE_OUTER_BOUND('',#25672,.T.);
#21573=FACE_OUTER_BOUND('',#25673,.T.);
#21574=FACE_OUTER_BOUND('',#25674,.T.);
#21575=FACE_OUTER_BOUND('',#25675,.T.);
#21576=FACE_OUTER_BOUND('',#25676,.T.);
#21577=FACE_OUTER_BOUND('',#25677,.T.);
#21578=FACE_OUTER_BOUND('',#25678,.T.);
#21579=FACE_OUTER_BOUND('',#25679,.T.);
#21580=FACE_OUTER_BOUND('',#25680,.T.);
#21581=FACE_OUTER_BOUND('',#25681,.T.);
#21582=FACE_OUTER_BOUND('',#25682,.T.);
#21583=FACE_OUTER_BOUND('',#25683,.T.);
#21584=FACE_OUTER_BOUND('',#25684,.T.);
#21585=FACE_OUTER_BOUND('',#25685,.T.);
#21586=FACE_OUTER_BOUND('',#25686,.T.);
#21587=FACE_OUTER_BOUND('',#25687,.T.);
#21588=FACE_OUTER_BOUND('',#25688,.T.);
#21589=FACE_OUTER_BOUND('',#25689,.T.);
#21590=FACE_OUTER_BOUND('',#25690,.T.);
#21591=FACE_OUTER_BOUND('',#25691,.T.);
#21592=FACE_OUTER_BOUND('',#25692,.T.);
#21593=FACE_OUTER_BOUND('',#25693,.T.);
#21594=FACE_OUTER_BOUND('',#25694,.T.);
#21595=FACE_OUTER_BOUND('',#25695,.T.);
#21596=FACE_OUTER_BOUND('',#25696,.T.);
#21597=FACE_OUTER_BOUND('',#25697,.T.);
#21598=FACE_OUTER_BOUND('',#25698,.T.);
#21599=FACE_OUTER_BOUND('',#25699,.T.);
#21600=FACE_OUTER_BOUND('',#25700,.T.);
#21601=FACE_OUTER_BOUND('',#25701,.T.);
#21602=FACE_OUTER_BOUND('',#25702,.T.);
#21603=FACE_OUTER_BOUND('',#25703,.T.);
#21604=FACE_OUTER_BOUND('',#25704,.T.);
#21605=FACE_OUTER_BOUND('',#25705,.T.);
#21606=FACE_OUTER_BOUND('',#25706,.T.);
#21607=FACE_OUTER_BOUND('',#25707,.T.);
#21608=FACE_OUTER_BOUND('',#25708,.T.);
#21609=FACE_OUTER_BOUND('',#25709,.T.);
#21610=FACE_OUTER_BOUND('',#25710,.T.);
#21611=FACE_OUTER_BOUND('',#25711,.T.);
#21612=FACE_OUTER_BOUND('',#25712,.T.);
#21613=FACE_OUTER_BOUND('',#25713,.T.);
#21614=FACE_OUTER_BOUND('',#25714,.T.);
#21615=FACE_OUTER_BOUND('',#25715,.T.);
#21616=FACE_OUTER_BOUND('',#25716,.T.);
#21617=FACE_OUTER_BOUND('',#25717,.T.);
#21618=FACE_OUTER_BOUND('',#25718,.T.);
#21619=FACE_OUTER_BOUND('',#25719,.T.);
#21620=FACE_OUTER_BOUND('',#25720,.T.);
#21621=FACE_OUTER_BOUND('',#25721,.T.);
#21622=FACE_OUTER_BOUND('',#25722,.T.);
#21623=FACE_OUTER_BOUND('',#25723,.T.);
#21624=FACE_OUTER_BOUND('',#25724,.T.);
#21625=FACE_OUTER_BOUND('',#25725,.T.);
#21626=FACE_OUTER_BOUND('',#25726,.T.);
#21627=FACE_OUTER_BOUND('',#25727,.T.);
#21628=FACE_OUTER_BOUND('',#25728,.T.);
#21629=FACE_OUTER_BOUND('',#25729,.T.);
#21630=FACE_OUTER_BOUND('',#25730,.T.);
#21631=FACE_OUTER_BOUND('',#25731,.T.);
#21632=FACE_OUTER_BOUND('',#25732,.T.);
#21633=FACE_OUTER_BOUND('',#25733,.T.);
#21634=FACE_OUTER_BOUND('',#25734,.T.);
#21635=FACE_OUTER_BOUND('',#25735,.T.);
#21636=FACE_OUTER_BOUND('',#25736,.T.);
#21637=FACE_OUTER_BOUND('',#25737,.T.);
#21638=FACE_OUTER_BOUND('',#25738,.T.);
#21639=FACE_OUTER_BOUND('',#25739,.T.);
#21640=FACE_OUTER_BOUND('',#25740,.T.);
#21641=FACE_OUTER_BOUND('',#25741,.T.);
#21642=FACE_OUTER_BOUND('',#25742,.T.);
#21643=FACE_OUTER_BOUND('',#25743,.T.);
#21644=FACE_OUTER_BOUND('',#25744,.T.);
#21645=FACE_OUTER_BOUND('',#25745,.T.);
#21646=FACE_OUTER_BOUND('',#25746,.T.);
#21647=FACE_OUTER_BOUND('',#25747,.T.);
#21648=FACE_OUTER_BOUND('',#25748,.T.);
#21649=FACE_OUTER_BOUND('',#25749,.T.);
#21650=FACE_OUTER_BOUND('',#25750,.T.);
#21651=FACE_OUTER_BOUND('',#25751,.T.);
#21652=FACE_OUTER_BOUND('',#25752,.T.);
#21653=FACE_OUTER_BOUND('',#25753,.T.);
#21654=FACE_OUTER_BOUND('',#25754,.T.);
#21655=FACE_OUTER_BOUND('',#25755,.T.);
#21656=FACE_OUTER_BOUND('',#25756,.T.);
#21657=FACE_OUTER_BOUND('',#25757,.T.);
#21658=FACE_OUTER_BOUND('',#25758,.T.);
#21659=FACE_OUTER_BOUND('',#25759,.T.);
#21660=FACE_OUTER_BOUND('',#25760,.T.);
#21661=FACE_OUTER_BOUND('',#25761,.T.);
#21662=FACE_OUTER_BOUND('',#25762,.T.);
#21663=FACE_OUTER_BOUND('',#25763,.T.);
#21664=FACE_OUTER_BOUND('',#25764,.T.);
#21665=FACE_OUTER_BOUND('',#25765,.T.);
#21666=FACE_OUTER_BOUND('',#25766,.T.);
#21667=FACE_OUTER_BOUND('',#25767,.T.);
#21668=FACE_OUTER_BOUND('',#25768,.T.);
#21669=FACE_OUTER_BOUND('',#25769,.T.);
#21670=FACE_OUTER_BOUND('',#25770,.T.);
#21671=FACE_OUTER_BOUND('',#25771,.T.);
#21672=FACE_OUTER_BOUND('',#25772,.T.);
#21673=FACE_OUTER_BOUND('',#25773,.T.);
#21674=FACE_OUTER_BOUND('',#25774,.T.);
#21675=FACE_OUTER_BOUND('',#25775,.T.);
#21676=FACE_OUTER_BOUND('',#25776,.T.);
#21677=FACE_OUTER_BOUND('',#25777,.T.);
#21678=FACE_OUTER_BOUND('',#25778,.T.);
#21679=FACE_OUTER_BOUND('',#25779,.T.);
#21680=FACE_OUTER_BOUND('',#25780,.T.);
#21681=FACE_OUTER_BOUND('',#25781,.T.);
#21682=FACE_OUTER_BOUND('',#25782,.T.);
#21683=FACE_OUTER_BOUND('',#25783,.T.);
#21684=FACE_OUTER_BOUND('',#25784,.T.);
#21685=FACE_OUTER_BOUND('',#25785,.T.);
#21686=FACE_OUTER_BOUND('',#25786,.T.);
#21687=FACE_OUTER_BOUND('',#25787,.T.);
#21688=FACE_OUTER_BOUND('',#25788,.T.);
#21689=FACE_OUTER_BOUND('',#25789,.T.);
#21690=FACE_OUTER_BOUND('',#25790,.T.);
#21691=FACE_OUTER_BOUND('',#25791,.T.);
#21692=FACE_OUTER_BOUND('',#25792,.T.);
#21693=FACE_OUTER_BOUND('',#25793,.T.);
#21694=FACE_OUTER_BOUND('',#25794,.T.);
#21695=FACE_OUTER_BOUND('',#25795,.T.);
#21696=FACE_OUTER_BOUND('',#25796,.T.);
#21697=FACE_OUTER_BOUND('',#25797,.T.);
#21698=FACE_OUTER_BOUND('',#25798,.T.);
#21699=FACE_OUTER_BOUND('',#25799,.T.);
#21700=FACE_OUTER_BOUND('',#25800,.T.);
#21701=FACE_OUTER_BOUND('',#25801,.T.);
#21702=FACE_OUTER_BOUND('',#25802,.T.);
#21703=FACE_OUTER_BOUND('',#25803,.T.);
#21704=FACE_OUTER_BOUND('',#25804,.T.);
#21705=FACE_OUTER_BOUND('',#25805,.T.);
#21706=FACE_OUTER_BOUND('',#25806,.T.);
#21707=FACE_OUTER_BOUND('',#25807,.T.);
#21708=FACE_OUTER_BOUND('',#25808,.T.);
#21709=FACE_OUTER_BOUND('',#25809,.T.);
#21710=FACE_OUTER_BOUND('',#25810,.T.);
#21711=FACE_OUTER_BOUND('',#25811,.T.);
#21712=FACE_OUTER_BOUND('',#25812,.T.);
#21713=FACE_OUTER_BOUND('',#25813,.T.);
#21714=FACE_OUTER_BOUND('',#25814,.T.);
#21715=FACE_OUTER_BOUND('',#25815,.T.);
#21716=FACE_OUTER_BOUND('',#25816,.T.);
#21717=FACE_OUTER_BOUND('',#25817,.T.);
#21718=FACE_OUTER_BOUND('',#25818,.T.);
#21719=FACE_OUTER_BOUND('',#25819,.T.);
#21720=FACE_OUTER_BOUND('',#25820,.T.);
#21721=FACE_OUTER_BOUND('',#25821,.T.);
#21722=FACE_OUTER_BOUND('',#25822,.T.);
#21723=FACE_OUTER_BOUND('',#25823,.T.);
#21724=FACE_OUTER_BOUND('',#25824,.T.);
#21725=FACE_OUTER_BOUND('',#25825,.T.);
#21726=FACE_OUTER_BOUND('',#25826,.T.);
#21727=FACE_OUTER_BOUND('',#25827,.T.);
#21728=FACE_OUTER_BOUND('',#25828,.T.);
#21729=FACE_OUTER_BOUND('',#25829,.T.);
#21730=FACE_OUTER_BOUND('',#25830,.T.);
#21731=FACE_OUTER_BOUND('',#25831,.T.);
#21732=FACE_OUTER_BOUND('',#25832,.T.);
#21733=FACE_OUTER_BOUND('',#25833,.T.);
#21734=FACE_OUTER_BOUND('',#25834,.T.);
#21735=FACE_OUTER_BOUND('',#25835,.T.);
#21736=FACE_OUTER_BOUND('',#25836,.T.);
#21737=FACE_OUTER_BOUND('',#25837,.T.);
#21738=FACE_OUTER_BOUND('',#25838,.T.);
#21739=FACE_OUTER_BOUND('',#25839,.T.);
#21740=FACE_OUTER_BOUND('',#25840,.T.);
#21741=FACE_OUTER_BOUND('',#25841,.T.);
#21742=FACE_OUTER_BOUND('',#25842,.T.);
#21743=FACE_OUTER_BOUND('',#25843,.T.);
#21744=FACE_OUTER_BOUND('',#25844,.T.);
#21745=FACE_OUTER_BOUND('',#25845,.T.);
#21746=FACE_OUTER_BOUND('',#25846,.T.);
#21747=FACE_OUTER_BOUND('',#25847,.T.);
#21748=FACE_OUTER_BOUND('',#25848,.T.);
#21749=FACE_OUTER_BOUND('',#25849,.T.);
#21750=FACE_OUTER_BOUND('',#25850,.T.);
#21751=FACE_OUTER_BOUND('',#25851,.T.);
#21752=FACE_OUTER_BOUND('',#25852,.T.);
#21753=FACE_OUTER_BOUND('',#25853,.T.);
#21754=FACE_OUTER_BOUND('',#25854,.T.);
#21755=FACE_OUTER_BOUND('',#25855,.T.);
#21756=FACE_OUTER_BOUND('',#25856,.T.);
#21757=FACE_OUTER_BOUND('',#25857,.T.);
#21758=FACE_OUTER_BOUND('',#25858,.T.);
#21759=FACE_OUTER_BOUND('',#25859,.T.);
#21760=FACE_OUTER_BOUND('',#25860,.T.);
#21761=FACE_OUTER_BOUND('',#25861,.T.);
#21762=FACE_OUTER_BOUND('',#25862,.T.);
#21763=FACE_OUTER_BOUND('',#25863,.T.);
#21764=FACE_OUTER_BOUND('',#25864,.T.);
#21765=FACE_OUTER_BOUND('',#25865,.T.);
#21766=FACE_OUTER_BOUND('',#25866,.T.);
#21767=FACE_OUTER_BOUND('',#25867,.T.);
#21768=FACE_OUTER_BOUND('',#25868,.T.);
#21769=FACE_OUTER_BOUND('',#25869,.T.);
#21770=FACE_OUTER_BOUND('',#25870,.T.);
#21771=FACE_OUTER_BOUND('',#25871,.T.);
#21772=FACE_OUTER_BOUND('',#25872,.T.);
#21773=FACE_OUTER_BOUND('',#25873,.T.);
#21774=FACE_OUTER_BOUND('',#25874,.T.);
#21775=FACE_OUTER_BOUND('',#25875,.T.);
#21776=FACE_OUTER_BOUND('',#25876,.T.);
#21777=FACE_OUTER_BOUND('',#25877,.T.);
#21778=FACE_OUTER_BOUND('',#25878,.T.);
#21779=FACE_OUTER_BOUND('',#25879,.T.);
#21780=FACE_OUTER_BOUND('',#25880,.T.);
#21781=FACE_OUTER_BOUND('',#25881,.T.);
#21782=FACE_OUTER_BOUND('',#25882,.T.);
#21783=FACE_OUTER_BOUND('',#25883,.T.);
#21784=FACE_OUTER_BOUND('',#25884,.T.);
#21785=FACE_OUTER_BOUND('',#25885,.T.);
#21786=FACE_OUTER_BOUND('',#25886,.T.);
#21787=FACE_OUTER_BOUND('',#25887,.T.);
#21788=FACE_OUTER_BOUND('',#25888,.T.);
#21789=FACE_OUTER_BOUND('',#25889,.T.);
#21790=FACE_OUTER_BOUND('',#25890,.T.);
#21791=FACE_OUTER_BOUND('',#25891,.T.);
#21792=FACE_OUTER_BOUND('',#25892,.T.);
#21793=FACE_OUTER_BOUND('',#25893,.T.);
#21794=FACE_OUTER_BOUND('',#25894,.T.);
#21795=FACE_OUTER_BOUND('',#25895,.T.);
#21796=FACE_OUTER_BOUND('',#25896,.T.);
#21797=FACE_OUTER_BOUND('',#25897,.T.);
#21798=FACE_OUTER_BOUND('',#25898,.T.);
#21799=FACE_OUTER_BOUND('',#25899,.T.);
#21800=FACE_OUTER_BOUND('',#25900,.T.);
#21801=FACE_OUTER_BOUND('',#25901,.T.);
#21802=FACE_OUTER_BOUND('',#25902,.T.);
#21803=FACE_OUTER_BOUND('',#25903,.T.);
#21804=FACE_OUTER_BOUND('',#25904,.T.);
#21805=FACE_OUTER_BOUND('',#25905,.T.);
#21806=FACE_OUTER_BOUND('',#25906,.T.);
#21807=FACE_OUTER_BOUND('',#25907,.T.);
#21808=FACE_OUTER_BOUND('',#25908,.T.);
#21809=FACE_OUTER_BOUND('',#25909,.T.);
#21810=FACE_OUTER_BOUND('',#25910,.T.);
#21811=FACE_OUTER_BOUND('',#25911,.T.);
#21812=FACE_OUTER_BOUND('',#25912,.T.);
#21813=FACE_OUTER_BOUND('',#25913,.T.);
#21814=FACE_OUTER_BOUND('',#25914,.T.);
#21815=FACE_OUTER_BOUND('',#25915,.T.);
#21816=FACE_OUTER_BOUND('',#25916,.T.);
#21817=FACE_OUTER_BOUND('',#25917,.T.);
#21818=FACE_OUTER_BOUND('',#25918,.T.);
#21819=FACE_OUTER_BOUND('',#25919,.T.);
#21820=FACE_OUTER_BOUND('',#25920,.T.);
#21821=FACE_OUTER_BOUND('',#25921,.T.);
#21822=FACE_OUTER_BOUND('',#25922,.T.);
#21823=FACE_OUTER_BOUND('',#25923,.T.);
#21824=FACE_OUTER_BOUND('',#25924,.T.);
#21825=FACE_OUTER_BOUND('',#25925,.T.);
#21826=FACE_OUTER_BOUND('',#25926,.T.);
#21827=FACE_OUTER_BOUND('',#25927,.T.);
#21828=FACE_OUTER_BOUND('',#25928,.T.);
#21829=FACE_OUTER_BOUND('',#25929,.T.);
#21830=FACE_OUTER_BOUND('',#25930,.T.);
#21831=FACE_OUTER_BOUND('',#25931,.T.);
#21832=FACE_OUTER_BOUND('',#25932,.T.);
#21833=FACE_OUTER_BOUND('',#25933,.T.);
#21834=FACE_OUTER_BOUND('',#25934,.T.);
#21835=FACE_OUTER_BOUND('',#25935,.T.);
#21836=FACE_OUTER_BOUND('',#25936,.T.);
#21837=FACE_OUTER_BOUND('',#25937,.T.);
#21838=FACE_OUTER_BOUND('',#25938,.T.);
#21839=FACE_OUTER_BOUND('',#25939,.T.);
#21840=FACE_OUTER_BOUND('',#25940,.T.);
#21841=FACE_OUTER_BOUND('',#25941,.T.);
#21842=FACE_OUTER_BOUND('',#25942,.T.);
#21843=FACE_OUTER_BOUND('',#25943,.T.);
#21844=FACE_OUTER_BOUND('',#25944,.T.);
#21845=FACE_OUTER_BOUND('',#25945,.T.);
#21846=FACE_OUTER_BOUND('',#25946,.T.);
#21847=FACE_OUTER_BOUND('',#25947,.T.);
#21848=FACE_OUTER_BOUND('',#25948,.T.);
#21849=FACE_OUTER_BOUND('',#25949,.T.);
#21850=FACE_OUTER_BOUND('',#25950,.T.);
#21851=FACE_OUTER_BOUND('',#25951,.T.);
#21852=FACE_OUTER_BOUND('',#25952,.T.);
#21853=FACE_OUTER_BOUND('',#25953,.T.);
#21854=FACE_OUTER_BOUND('',#25954,.T.);
#21855=FACE_OUTER_BOUND('',#25955,.T.);
#21856=FACE_OUTER_BOUND('',#25956,.T.);
#21857=FACE_OUTER_BOUND('',#25957,.T.);
#21858=FACE_OUTER_BOUND('',#25958,.T.);
#21859=FACE_OUTER_BOUND('',#25959,.T.);
#21860=FACE_OUTER_BOUND('',#25960,.T.);
#21861=FACE_OUTER_BOUND('',#25961,.T.);
#21862=FACE_OUTER_BOUND('',#25962,.T.);
#21863=FACE_OUTER_BOUND('',#25963,.T.);
#21864=FACE_OUTER_BOUND('',#25964,.T.);
#21865=FACE_OUTER_BOUND('',#25965,.T.);
#21866=FACE_OUTER_BOUND('',#25966,.T.);
#21867=FACE_OUTER_BOUND('',#25967,.T.);
#21868=FACE_OUTER_BOUND('',#25968,.T.);
#21869=FACE_OUTER_BOUND('',#25969,.T.);
#21870=FACE_OUTER_BOUND('',#25970,.T.);
#21871=FACE_OUTER_BOUND('',#25971,.T.);
#21872=FACE_OUTER_BOUND('',#25972,.T.);
#21873=FACE_OUTER_BOUND('',#25973,.T.);
#21874=FACE_OUTER_BOUND('',#25974,.T.);
#21875=FACE_OUTER_BOUND('',#25975,.T.);
#21876=FACE_OUTER_BOUND('',#25976,.T.);
#21877=FACE_OUTER_BOUND('',#25977,.T.);
#21878=FACE_OUTER_BOUND('',#25978,.T.);
#21879=FACE_OUTER_BOUND('',#25979,.T.);
#21880=FACE_OUTER_BOUND('',#25980,.T.);
#21881=FACE_OUTER_BOUND('',#25981,.T.);
#21882=FACE_OUTER_BOUND('',#25982,.T.);
#21883=FACE_OUTER_BOUND('',#25983,.T.);
#21884=FACE_OUTER_BOUND('',#25984,.T.);
#21885=FACE_OUTER_BOUND('',#25985,.T.);
#21886=FACE_OUTER_BOUND('',#25986,.T.);
#21887=FACE_OUTER_BOUND('',#25987,.T.);
#21888=FACE_OUTER_BOUND('',#25988,.T.);
#21889=FACE_OUTER_BOUND('',#25989,.T.);
#21890=FACE_OUTER_BOUND('',#25990,.T.);
#21891=FACE_OUTER_BOUND('',#25991,.T.);
#21892=FACE_OUTER_BOUND('',#25992,.T.);
#21893=FACE_OUTER_BOUND('',#25993,.T.);
#21894=FACE_OUTER_BOUND('',#25994,.T.);
#21895=FACE_OUTER_BOUND('',#25995,.T.);
#21896=FACE_OUTER_BOUND('',#25996,.T.);
#21897=FACE_OUTER_BOUND('',#25997,.T.);
#21898=FACE_OUTER_BOUND('',#25998,.T.);
#21899=FACE_OUTER_BOUND('',#25999,.T.);
#21900=FACE_OUTER_BOUND('',#26000,.T.);
#21901=FACE_OUTER_BOUND('',#26001,.T.);
#21902=FACE_OUTER_BOUND('',#26002,.T.);
#21903=FACE_OUTER_BOUND('',#26003,.T.);
#21904=FACE_OUTER_BOUND('',#26004,.T.);
#21905=FACE_OUTER_BOUND('',#26005,.T.);
#21906=FACE_OUTER_BOUND('',#26006,.T.);
#21907=FACE_OUTER_BOUND('',#26007,.T.);
#21908=FACE_OUTER_BOUND('',#26008,.T.);
#21909=FACE_OUTER_BOUND('',#26009,.T.);
#21910=FACE_OUTER_BOUND('',#26010,.T.);
#21911=FACE_OUTER_BOUND('',#26011,.T.);
#21912=FACE_OUTER_BOUND('',#26012,.T.);
#21913=FACE_OUTER_BOUND('',#26013,.T.);
#21914=FACE_OUTER_BOUND('',#26014,.T.);
#21915=FACE_OUTER_BOUND('',#26015,.T.);
#21916=FACE_OUTER_BOUND('',#26016,.T.);
#21917=FACE_OUTER_BOUND('',#26017,.T.);
#21918=FACE_OUTER_BOUND('',#26018,.T.);
#21919=FACE_OUTER_BOUND('',#26019,.T.);
#21920=FACE_OUTER_BOUND('',#26020,.T.);
#21921=FACE_OUTER_BOUND('',#26021,.T.);
#21922=FACE_OUTER_BOUND('',#26022,.T.);
#21923=FACE_OUTER_BOUND('',#26023,.T.);
#21924=FACE_OUTER_BOUND('',#26024,.T.);
#21925=FACE_OUTER_BOUND('',#26025,.T.);
#21926=FACE_OUTER_BOUND('',#26026,.T.);
#21927=FACE_OUTER_BOUND('',#26027,.T.);
#21928=FACE_OUTER_BOUND('',#26028,.T.);
#21929=FACE_OUTER_BOUND('',#26029,.T.);
#21930=FACE_OUTER_BOUND('',#26030,.T.);
#21931=FACE_OUTER_BOUND('',#26031,.T.);
#21932=FACE_OUTER_BOUND('',#26032,.T.);
#21933=FACE_OUTER_BOUND('',#26033,.T.);
#21934=FACE_OUTER_BOUND('',#26034,.T.);
#21935=FACE_OUTER_BOUND('',#26035,.T.);
#21936=FACE_OUTER_BOUND('',#26036,.T.);
#21937=FACE_OUTER_BOUND('',#26037,.T.);
#21938=FACE_OUTER_BOUND('',#26038,.T.);
#21939=FACE_OUTER_BOUND('',#26039,.T.);
#21940=FACE_OUTER_BOUND('',#26040,.T.);
#21941=FACE_OUTER_BOUND('',#26041,.T.);
#21942=FACE_OUTER_BOUND('',#26042,.T.);
#21943=FACE_OUTER_BOUND('',#26043,.T.);
#21944=FACE_OUTER_BOUND('',#26044,.T.);
#21945=FACE_OUTER_BOUND('',#26045,.T.);
#21946=FACE_OUTER_BOUND('',#26046,.T.);
#21947=FACE_OUTER_BOUND('',#26047,.T.);
#21948=FACE_OUTER_BOUND('',#26048,.T.);
#21949=FACE_OUTER_BOUND('',#26049,.T.);
#21950=FACE_OUTER_BOUND('',#26050,.T.);
#21951=FACE_OUTER_BOUND('',#26051,.T.);
#21952=FACE_OUTER_BOUND('',#26052,.T.);
#21953=FACE_OUTER_BOUND('',#26053,.T.);
#21954=FACE_OUTER_BOUND('',#26054,.T.);
#21955=FACE_OUTER_BOUND('',#26055,.T.);
#21956=FACE_OUTER_BOUND('',#26057,.T.);
#21957=FACE_OUTER_BOUND('',#26058,.T.);
#21958=FACE_OUTER_BOUND('',#26059,.T.);
#21959=FACE_OUTER_BOUND('',#26060,.T.);
#21960=FACE_OUTER_BOUND('',#26061,.T.);
#21961=FACE_OUTER_BOUND('',#26062,.T.);
#21962=FACE_OUTER_BOUND('',#26063,.T.);
#21963=FACE_OUTER_BOUND('',#26064,.T.);
#21964=FACE_OUTER_BOUND('',#26065,.T.);
#21965=FACE_OUTER_BOUND('',#26066,.T.);
#21966=FACE_OUTER_BOUND('',#26067,.T.);
#21967=FACE_OUTER_BOUND('',#26068,.T.);
#21968=FACE_OUTER_BOUND('',#26069,.T.);
#21969=FACE_OUTER_BOUND('',#26070,.T.);
#21970=FACE_OUTER_BOUND('',#26071,.T.);
#21971=FACE_OUTER_BOUND('',#26072,.T.);
#21972=FACE_OUTER_BOUND('',#26073,.T.);
#21973=FACE_OUTER_BOUND('',#26074,.T.);
#21974=FACE_OUTER_BOUND('',#26075,.T.);
#21975=FACE_OUTER_BOUND('',#26076,.T.);
#21976=FACE_OUTER_BOUND('',#26077,.T.);
#21977=FACE_OUTER_BOUND('',#26078,.T.);
#21978=FACE_OUTER_BOUND('',#26079,.T.);
#21979=FACE_OUTER_BOUND('',#26080,.T.);
#21980=FACE_OUTER_BOUND('',#26081,.T.);
#21981=FACE_OUTER_BOUND('',#26082,.T.);
#21982=FACE_OUTER_BOUND('',#26083,.T.);
#21983=FACE_OUTER_BOUND('',#26084,.T.);
#21984=FACE_OUTER_BOUND('',#26085,.T.);
#21985=FACE_OUTER_BOUND('',#26086,.T.);
#21986=FACE_OUTER_BOUND('',#26087,.T.);
#21987=FACE_OUTER_BOUND('',#26088,.T.);
#21988=FACE_OUTER_BOUND('',#26089,.T.);
#21989=FACE_OUTER_BOUND('',#26090,.T.);
#21990=FACE_OUTER_BOUND('',#26091,.T.);
#21991=FACE_OUTER_BOUND('',#26092,.T.);
#21992=FACE_OUTER_BOUND('',#26093,.T.);
#21993=FACE_OUTER_BOUND('',#26094,.T.);
#21994=FACE_OUTER_BOUND('',#26095,.T.);
#21995=FACE_OUTER_BOUND('',#26096,.T.);
#21996=FACE_OUTER_BOUND('',#26097,.T.);
#21997=FACE_OUTER_BOUND('',#26098,.T.);
#21998=FACE_OUTER_BOUND('',#26099,.T.);
#21999=FACE_OUTER_BOUND('',#26100,.T.);
#22000=FACE_OUTER_BOUND('',#26101,.T.);
#22001=FACE_OUTER_BOUND('',#26102,.T.);
#22002=FACE_OUTER_BOUND('',#26103,.T.);
#22003=FACE_OUTER_BOUND('',#26104,.T.);
#22004=FACE_OUTER_BOUND('',#26105,.T.);
#22005=FACE_OUTER_BOUND('',#26106,.T.);
#22006=FACE_OUTER_BOUND('',#26107,.T.);
#22007=FACE_OUTER_BOUND('',#26108,.T.);
#22008=FACE_OUTER_BOUND('',#26109,.T.);
#22009=FACE_OUTER_BOUND('',#26110,.T.);
#22010=FACE_OUTER_BOUND('',#26111,.T.);
#22011=FACE_OUTER_BOUND('',#26112,.T.);
#22012=FACE_OUTER_BOUND('',#26113,.T.);
#22013=FACE_OUTER_BOUND('',#26114,.T.);
#22014=FACE_OUTER_BOUND('',#26115,.T.);
#22015=FACE_OUTER_BOUND('',#26116,.T.);
#22016=FACE_OUTER_BOUND('',#26117,.T.);
#22017=FACE_OUTER_BOUND('',#26118,.T.);
#22018=FACE_OUTER_BOUND('',#26119,.T.);
#22019=FACE_OUTER_BOUND('',#26120,.T.);
#22020=FACE_OUTER_BOUND('',#26121,.T.);
#22021=FACE_OUTER_BOUND('',#26122,.T.);
#22022=FACE_OUTER_BOUND('',#26123,.T.);
#22023=FACE_OUTER_BOUND('',#26124,.T.);
#22024=FACE_OUTER_BOUND('',#26125,.T.);
#22025=FACE_OUTER_BOUND('',#26126,.T.);
#22026=FACE_OUTER_BOUND('',#26127,.T.);
#22027=FACE_OUTER_BOUND('',#26128,.T.);
#22028=FACE_OUTER_BOUND('',#26129,.T.);
#22029=FACE_OUTER_BOUND('',#26130,.T.);
#22030=FACE_OUTER_BOUND('',#26131,.T.);
#22031=FACE_OUTER_BOUND('',#26132,.T.);
#22032=FACE_OUTER_BOUND('',#26133,.T.);
#22033=FACE_OUTER_BOUND('',#26134,.T.);
#22034=FACE_OUTER_BOUND('',#26135,.T.);
#22035=FACE_OUTER_BOUND('',#26136,.T.);
#22036=FACE_OUTER_BOUND('',#26137,.T.);
#22037=FACE_OUTER_BOUND('',#26138,.T.);
#22038=FACE_OUTER_BOUND('',#26139,.T.);
#22039=FACE_OUTER_BOUND('',#26140,.T.);
#22040=FACE_OUTER_BOUND('',#26141,.T.);
#22041=FACE_OUTER_BOUND('',#26142,.T.);
#22042=FACE_OUTER_BOUND('',#26143,.T.);
#22043=FACE_OUTER_BOUND('',#26144,.T.);
#22044=FACE_OUTER_BOUND('',#26145,.T.);
#22045=FACE_OUTER_BOUND('',#26146,.T.);
#22046=FACE_OUTER_BOUND('',#26147,.T.);
#22047=FACE_OUTER_BOUND('',#26148,.T.);
#22048=FACE_OUTER_BOUND('',#26149,.T.);
#22049=FACE_OUTER_BOUND('',#26150,.T.);
#22050=FACE_OUTER_BOUND('',#26151,.T.);
#22051=FACE_OUTER_BOUND('',#26152,.T.);
#22052=FACE_OUTER_BOUND('',#26153,.T.);
#22053=FACE_OUTER_BOUND('',#26154,.T.);
#22054=FACE_OUTER_BOUND('',#26155,.T.);
#22055=FACE_OUTER_BOUND('',#26156,.T.);
#22056=FACE_OUTER_BOUND('',#26157,.T.);
#22057=FACE_OUTER_BOUND('',#26158,.T.);
#22058=FACE_OUTER_BOUND('',#26159,.T.);
#22059=FACE_OUTER_BOUND('',#26160,.T.);
#22060=FACE_OUTER_BOUND('',#26161,.T.);
#22061=FACE_OUTER_BOUND('',#26162,.T.);
#22062=FACE_OUTER_BOUND('',#26163,.T.);
#22063=FACE_OUTER_BOUND('',#26164,.T.);
#22064=FACE_OUTER_BOUND('',#26165,.T.);
#22065=FACE_OUTER_BOUND('',#26166,.T.);
#22066=FACE_OUTER_BOUND('',#26167,.T.);
#22067=FACE_OUTER_BOUND('',#26168,.T.);
#22068=FACE_OUTER_BOUND('',#26169,.T.);
#22069=FACE_OUTER_BOUND('',#26170,.T.);
#22070=FACE_OUTER_BOUND('',#26171,.T.);
#22071=FACE_OUTER_BOUND('',#26172,.T.);
#22072=FACE_OUTER_BOUND('',#26173,.T.);
#22073=FACE_OUTER_BOUND('',#26174,.T.);
#22074=FACE_OUTER_BOUND('',#26175,.T.);
#22075=FACE_OUTER_BOUND('',#26176,.T.);
#22076=FACE_OUTER_BOUND('',#26177,.T.);
#22077=FACE_OUTER_BOUND('',#26178,.T.);
#22078=FACE_OUTER_BOUND('',#26179,.T.);
#22079=FACE_OUTER_BOUND('',#26180,.T.);
#22080=FACE_OUTER_BOUND('',#26181,.T.);
#22081=FACE_OUTER_BOUND('',#26182,.T.);
#22082=FACE_OUTER_BOUND('',#26183,.T.);
#22083=FACE_OUTER_BOUND('',#26184,.T.);
#22084=FACE_OUTER_BOUND('',#26185,.T.);
#22085=FACE_OUTER_BOUND('',#26186,.T.);
#22086=FACE_OUTER_BOUND('',#26187,.T.);
#22087=FACE_OUTER_BOUND('',#26188,.T.);
#22088=FACE_OUTER_BOUND('',#26189,.T.);
#22089=FACE_OUTER_BOUND('',#26190,.T.);
#22090=FACE_OUTER_BOUND('',#26191,.T.);
#22091=FACE_OUTER_BOUND('',#26192,.T.);
#22092=FACE_OUTER_BOUND('',#26193,.T.);
#22093=FACE_OUTER_BOUND('',#26194,.T.);
#22094=FACE_OUTER_BOUND('',#26195,.T.);
#22095=FACE_OUTER_BOUND('',#26196,.T.);
#22096=FACE_OUTER_BOUND('',#26197,.T.);
#22097=FACE_OUTER_BOUND('',#26198,.T.);
#22098=FACE_OUTER_BOUND('',#26199,.T.);
#22099=FACE_OUTER_BOUND('',#26200,.T.);
#22100=FACE_OUTER_BOUND('',#26201,.T.);
#22101=FACE_OUTER_BOUND('',#26202,.T.);
#22102=FACE_OUTER_BOUND('',#26203,.T.);
#22103=FACE_OUTER_BOUND('',#26204,.T.);
#22104=FACE_OUTER_BOUND('',#26205,.T.);
#22105=FACE_OUTER_BOUND('',#26206,.T.);
#22106=FACE_OUTER_BOUND('',#26207,.T.);
#22107=FACE_OUTER_BOUND('',#26208,.T.);
#22108=FACE_OUTER_BOUND('',#26209,.T.);
#22109=FACE_OUTER_BOUND('',#26210,.T.);
#22110=FACE_OUTER_BOUND('',#26211,.T.);
#22111=FACE_OUTER_BOUND('',#26212,.T.);
#22112=FACE_OUTER_BOUND('',#26213,.T.);
#22113=FACE_OUTER_BOUND('',#26214,.T.);
#22114=FACE_OUTER_BOUND('',#26215,.T.);
#22115=FACE_OUTER_BOUND('',#26216,.T.);
#22116=FACE_OUTER_BOUND('',#26217,.T.);
#22117=FACE_OUTER_BOUND('',#26218,.T.);
#22118=FACE_OUTER_BOUND('',#26219,.T.);
#22119=FACE_OUTER_BOUND('',#26220,.T.);
#22120=FACE_OUTER_BOUND('',#26221,.T.);
#22121=FACE_OUTER_BOUND('',#26222,.T.);
#22122=FACE_OUTER_BOUND('',#26223,.T.);
#22123=FACE_OUTER_BOUND('',#26224,.T.);
#22124=FACE_OUTER_BOUND('',#26225,.T.);
#22125=FACE_OUTER_BOUND('',#26226,.T.);
#22126=FACE_OUTER_BOUND('',#26227,.T.);
#22127=FACE_OUTER_BOUND('',#26228,.T.);
#22128=FACE_OUTER_BOUND('',#26229,.T.);
#22129=FACE_OUTER_BOUND('',#26230,.T.);
#22130=FACE_OUTER_BOUND('',#26231,.T.);
#22131=FACE_OUTER_BOUND('',#26232,.T.);
#22132=FACE_OUTER_BOUND('',#26233,.T.);
#22133=FACE_OUTER_BOUND('',#26234,.T.);
#22134=FACE_OUTER_BOUND('',#26235,.T.);
#22135=FACE_OUTER_BOUND('',#26236,.T.);
#22136=FACE_OUTER_BOUND('',#26237,.T.);
#22137=FACE_OUTER_BOUND('',#26238,.T.);
#22138=FACE_OUTER_BOUND('',#26239,.T.);
#22139=FACE_OUTER_BOUND('',#26240,.T.);
#22140=FACE_OUTER_BOUND('',#26241,.T.);
#22141=FACE_OUTER_BOUND('',#26242,.T.);
#22142=FACE_OUTER_BOUND('',#26243,.T.);
#22143=FACE_OUTER_BOUND('',#26244,.T.);
#22144=FACE_OUTER_BOUND('',#26245,.T.);
#22145=FACE_OUTER_BOUND('',#26246,.T.);
#22146=FACE_OUTER_BOUND('',#26247,.T.);
#22147=FACE_OUTER_BOUND('',#26248,.T.);
#22148=FACE_OUTER_BOUND('',#26249,.T.);
#22149=FACE_OUTER_BOUND('',#26250,.T.);
#22150=FACE_OUTER_BOUND('',#26251,.T.);
#22151=FACE_OUTER_BOUND('',#26252,.T.);
#22152=FACE_OUTER_BOUND('',#26253,.T.);
#22153=FACE_OUTER_BOUND('',#26254,.T.);
#22154=FACE_OUTER_BOUND('',#26255,.T.);
#22155=FACE_OUTER_BOUND('',#26256,.T.);
#22156=FACE_OUTER_BOUND('',#26257,.T.);
#22157=FACE_OUTER_BOUND('',#26258,.T.);
#22158=FACE_OUTER_BOUND('',#26259,.T.);
#22159=FACE_OUTER_BOUND('',#26260,.T.);
#22160=FACE_OUTER_BOUND('',#26261,.T.);
#22161=FACE_OUTER_BOUND('',#26262,.T.);
#22162=FACE_OUTER_BOUND('',#26263,.T.);
#22163=FACE_OUTER_BOUND('',#26264,.T.);
#22164=FACE_OUTER_BOUND('',#26265,.T.);
#22165=FACE_OUTER_BOUND('',#26266,.T.);
#22166=FACE_OUTER_BOUND('',#26267,.T.);
#22167=FACE_OUTER_BOUND('',#26268,.T.);
#22168=FACE_OUTER_BOUND('',#26269,.T.);
#22169=FACE_OUTER_BOUND('',#26270,.T.);
#22170=FACE_OUTER_BOUND('',#26271,.T.);
#22171=FACE_OUTER_BOUND('',#26272,.T.);
#22172=FACE_OUTER_BOUND('',#26273,.T.);
#22173=FACE_OUTER_BOUND('',#26274,.T.);
#22174=FACE_OUTER_BOUND('',#26275,.T.);
#22175=FACE_OUTER_BOUND('',#26276,.T.);
#22176=FACE_OUTER_BOUND('',#26277,.T.);
#22177=FACE_OUTER_BOUND('',#26278,.T.);
#22178=FACE_OUTER_BOUND('',#26279,.T.);
#22179=FACE_OUTER_BOUND('',#26280,.T.);
#22180=FACE_OUTER_BOUND('',#26281,.T.);
#22181=FACE_OUTER_BOUND('',#26282,.T.);
#22182=FACE_OUTER_BOUND('',#26283,.T.);
#22183=FACE_OUTER_BOUND('',#26284,.T.);
#22184=FACE_OUTER_BOUND('',#26285,.T.);
#22185=FACE_OUTER_BOUND('',#26286,.T.);
#22186=FACE_OUTER_BOUND('',#26287,.T.);
#22187=FACE_OUTER_BOUND('',#26288,.T.);
#22188=FACE_OUTER_BOUND('',#26289,.T.);
#22189=FACE_OUTER_BOUND('',#26290,.T.);
#22190=FACE_OUTER_BOUND('',#26291,.T.);
#22191=FACE_OUTER_BOUND('',#26292,.T.);
#22192=FACE_OUTER_BOUND('',#26293,.T.);
#22193=FACE_OUTER_BOUND('',#26294,.T.);
#22194=FACE_OUTER_BOUND('',#26295,.T.);
#22195=FACE_OUTER_BOUND('',#26296,.T.);
#22196=FACE_OUTER_BOUND('',#26297,.T.);
#22197=FACE_OUTER_BOUND('',#26298,.T.);
#22198=FACE_OUTER_BOUND('',#26299,.T.);
#22199=FACE_OUTER_BOUND('',#26300,.T.);
#22200=FACE_OUTER_BOUND('',#26301,.T.);
#22201=FACE_OUTER_BOUND('',#26302,.T.);
#22202=FACE_OUTER_BOUND('',#26303,.T.);
#22203=FACE_OUTER_BOUND('',#26304,.T.);
#22204=FACE_OUTER_BOUND('',#26305,.T.);
#22205=FACE_OUTER_BOUND('',#26306,.T.);
#22206=FACE_OUTER_BOUND('',#26307,.T.);
#22207=FACE_OUTER_BOUND('',#26308,.T.);
#22208=FACE_OUTER_BOUND('',#26309,.T.);
#22209=FACE_OUTER_BOUND('',#26310,.T.);
#22210=FACE_OUTER_BOUND('',#26311,.T.);
#22211=FACE_OUTER_BOUND('',#26312,.T.);
#22212=FACE_OUTER_BOUND('',#26313,.T.);
#22213=FACE_OUTER_BOUND('',#26314,.T.);
#22214=FACE_OUTER_BOUND('',#26315,.T.);
#22215=FACE_OUTER_BOUND('',#26316,.T.);
#22216=FACE_OUTER_BOUND('',#26317,.T.);
#22217=FACE_OUTER_BOUND('',#26318,.T.);
#22218=FACE_OUTER_BOUND('',#26319,.T.);
#22219=FACE_OUTER_BOUND('',#26320,.T.);
#22220=FACE_OUTER_BOUND('',#26321,.T.);
#22221=FACE_OUTER_BOUND('',#26322,.T.);
#22222=FACE_OUTER_BOUND('',#26323,.T.);
#22223=FACE_OUTER_BOUND('',#26324,.T.);
#22224=FACE_OUTER_BOUND('',#26325,.T.);
#22225=FACE_OUTER_BOUND('',#26326,.T.);
#22226=FACE_OUTER_BOUND('',#26327,.T.);
#22227=FACE_OUTER_BOUND('',#26328,.T.);
#22228=FACE_OUTER_BOUND('',#26329,.T.);
#22229=FACE_OUTER_BOUND('',#26330,.T.);
#22230=FACE_OUTER_BOUND('',#26331,.T.);
#22231=FACE_OUTER_BOUND('',#26332,.T.);
#22232=FACE_OUTER_BOUND('',#26333,.T.);
#22233=FACE_OUTER_BOUND('',#26334,.T.);
#22234=FACE_OUTER_BOUND('',#26335,.T.);
#22235=FACE_OUTER_BOUND('',#26336,.T.);
#22236=FACE_OUTER_BOUND('',#26337,.T.);
#22237=FACE_OUTER_BOUND('',#26338,.T.);
#22238=FACE_OUTER_BOUND('',#26339,.T.);
#22239=FACE_OUTER_BOUND('',#26340,.T.);
#22240=FACE_OUTER_BOUND('',#26341,.T.);
#22241=FACE_OUTER_BOUND('',#26342,.T.);
#22242=FACE_OUTER_BOUND('',#26343,.T.);
#22243=FACE_OUTER_BOUND('',#26344,.T.);
#22244=FACE_OUTER_BOUND('',#26345,.T.);
#22245=FACE_OUTER_BOUND('',#26346,.T.);
#22246=FACE_OUTER_BOUND('',#26347,.T.);
#22247=FACE_OUTER_BOUND('',#26348,.T.);
#22248=FACE_OUTER_BOUND('',#26349,.T.);
#22249=FACE_OUTER_BOUND('',#26350,.T.);
#22250=FACE_OUTER_BOUND('',#26351,.T.);
#22251=FACE_OUTER_BOUND('',#26352,.T.);
#22252=FACE_OUTER_BOUND('',#26353,.T.);
#22253=FACE_OUTER_BOUND('',#26354,.T.);
#22254=FACE_OUTER_BOUND('',#26355,.T.);
#22255=FACE_OUTER_BOUND('',#26356,.T.);
#22256=FACE_OUTER_BOUND('',#26357,.T.);
#22257=FACE_OUTER_BOUND('',#26358,.T.);
#22258=FACE_OUTER_BOUND('',#26359,.T.);
#22259=FACE_OUTER_BOUND('',#26360,.T.);
#22260=FACE_OUTER_BOUND('',#26361,.T.);
#22261=FACE_OUTER_BOUND('',#26362,.T.);
#22262=FACE_OUTER_BOUND('',#26363,.T.);
#22263=FACE_OUTER_BOUND('',#26364,.T.);
#22264=FACE_OUTER_BOUND('',#26365,.T.);
#22265=FACE_OUTER_BOUND('',#26366,.T.);
#22266=FACE_OUTER_BOUND('',#26367,.T.);
#22267=FACE_OUTER_BOUND('',#26368,.T.);
#22268=FACE_OUTER_BOUND('',#26369,.T.);
#22269=FACE_OUTER_BOUND('',#26370,.T.);
#22270=FACE_OUTER_BOUND('',#26371,.T.);
#22271=FACE_OUTER_BOUND('',#26372,.T.);
#22272=FACE_OUTER_BOUND('',#26373,.T.);
#22273=FACE_OUTER_BOUND('',#26374,.T.);
#22274=FACE_OUTER_BOUND('',#26375,.T.);
#22275=FACE_OUTER_BOUND('',#26376,.T.);
#22276=FACE_OUTER_BOUND('',#26377,.T.);
#22277=FACE_OUTER_BOUND('',#26378,.T.);
#22278=FACE_OUTER_BOUND('',#26379,.T.);
#22279=FACE_OUTER_BOUND('',#26380,.T.);
#22280=FACE_OUTER_BOUND('',#26381,.T.);
#22281=FACE_OUTER_BOUND('',#26382,.T.);
#22282=FACE_OUTER_BOUND('',#26383,.T.);
#22283=FACE_OUTER_BOUND('',#26384,.T.);
#22284=FACE_OUTER_BOUND('',#26385,.T.);
#22285=FACE_OUTER_BOUND('',#26386,.T.);
#22286=FACE_OUTER_BOUND('',#26387,.T.);
#22287=FACE_OUTER_BOUND('',#26388,.T.);
#22288=FACE_OUTER_BOUND('',#26389,.T.);
#22289=FACE_OUTER_BOUND('',#26390,.T.);
#22290=FACE_OUTER_BOUND('',#26391,.T.);
#22291=FACE_OUTER_BOUND('',#26392,.T.);
#22292=FACE_OUTER_BOUND('',#26393,.T.);
#22293=FACE_OUTER_BOUND('',#26394,.T.);
#22294=FACE_OUTER_BOUND('',#26395,.T.);
#22295=FACE_OUTER_BOUND('',#26396,.T.);
#22296=FACE_OUTER_BOUND('',#26397,.T.);
#22297=FACE_OUTER_BOUND('',#26398,.T.);
#22298=FACE_OUTER_BOUND('',#26399,.T.);
#22299=FACE_OUTER_BOUND('',#26400,.T.);
#22300=FACE_OUTER_BOUND('',#26401,.T.);
#22301=FACE_OUTER_BOUND('',#26402,.T.);
#22302=FACE_OUTER_BOUND('',#26403,.T.);
#22303=FACE_OUTER_BOUND('',#26404,.T.);
#22304=FACE_OUTER_BOUND('',#26405,.T.);
#22305=FACE_OUTER_BOUND('',#26406,.T.);
#22306=FACE_OUTER_BOUND('',#26407,.T.);
#22307=FACE_OUTER_BOUND('',#26408,.T.);
#22308=FACE_OUTER_BOUND('',#26409,.T.);
#22309=FACE_OUTER_BOUND('',#26410,.T.);
#22310=FACE_OUTER_BOUND('',#26411,.T.);
#22311=FACE_OUTER_BOUND('',#26412,.T.);
#22312=FACE_OUTER_BOUND('',#26413,.T.);
#22313=FACE_OUTER_BOUND('',#26414,.T.);
#22314=FACE_OUTER_BOUND('',#26415,.T.);
#22315=FACE_OUTER_BOUND('',#26416,.T.);
#22316=FACE_OUTER_BOUND('',#26417,.T.);
#22317=FACE_OUTER_BOUND('',#26418,.T.);
#22318=FACE_OUTER_BOUND('',#26419,.T.);
#22319=FACE_OUTER_BOUND('',#26420,.T.);
#22320=FACE_OUTER_BOUND('',#26421,.T.);
#22321=FACE_OUTER_BOUND('',#26422,.T.);
#22322=FACE_OUTER_BOUND('',#26423,.T.);
#22323=FACE_OUTER_BOUND('',#26424,.T.);
#22324=FACE_OUTER_BOUND('',#26425,.T.);
#22325=FACE_OUTER_BOUND('',#26426,.T.);
#22326=FACE_OUTER_BOUND('',#26427,.T.);
#22327=FACE_OUTER_BOUND('',#26428,.T.);
#22328=FACE_OUTER_BOUND('',#26429,.T.);
#22329=FACE_OUTER_BOUND('',#26430,.T.);
#22330=FACE_OUTER_BOUND('',#26431,.T.);
#22331=FACE_OUTER_BOUND('',#26432,.T.);
#22332=FACE_OUTER_BOUND('',#26433,.T.);
#22333=FACE_OUTER_BOUND('',#26434,.T.);
#22334=FACE_OUTER_BOUND('',#26435,.T.);
#22335=FACE_OUTER_BOUND('',#26436,.T.);
#22336=FACE_OUTER_BOUND('',#26437,.T.);
#22337=FACE_OUTER_BOUND('',#26438,.T.);
#22338=FACE_OUTER_BOUND('',#26439,.T.);
#22339=FACE_OUTER_BOUND('',#26440,.T.);
#22340=FACE_OUTER_BOUND('',#26441,.T.);
#22341=FACE_OUTER_BOUND('',#26442,.T.);
#22342=FACE_OUTER_BOUND('',#26443,.T.);
#22343=FACE_OUTER_BOUND('',#26444,.T.);
#22344=FACE_OUTER_BOUND('',#26445,.T.);
#22345=FACE_OUTER_BOUND('',#26446,.T.);
#22346=FACE_OUTER_BOUND('',#26447,.T.);
#22347=FACE_OUTER_BOUND('',#26448,.T.);
#22348=FACE_OUTER_BOUND('',#26449,.T.);
#22349=FACE_OUTER_BOUND('',#26450,.T.);
#22350=FACE_OUTER_BOUND('',#26451,.T.);
#22351=FACE_OUTER_BOUND('',#26452,.T.);
#22352=FACE_OUTER_BOUND('',#26453,.T.);
#22353=FACE_OUTER_BOUND('',#26454,.T.);
#22354=FACE_OUTER_BOUND('',#26455,.T.);
#22355=FACE_OUTER_BOUND('',#26456,.T.);
#22356=FACE_OUTER_BOUND('',#26457,.T.);
#22357=FACE_OUTER_BOUND('',#26458,.T.);
#22358=FACE_OUTER_BOUND('',#26459,.T.);
#22359=FACE_OUTER_BOUND('',#26460,.T.);
#22360=FACE_OUTER_BOUND('',#26461,.T.);
#22361=FACE_OUTER_BOUND('',#26462,.T.);
#22362=FACE_OUTER_BOUND('',#26463,.T.);
#22363=FACE_OUTER_BOUND('',#26464,.T.);
#22364=FACE_OUTER_BOUND('',#26465,.T.);
#22365=FACE_OUTER_BOUND('',#26466,.T.);
#22366=FACE_OUTER_BOUND('',#26467,.T.);
#22367=FACE_OUTER_BOUND('',#26468,.T.);
#22368=FACE_OUTER_BOUND('',#26469,.T.);
#22369=FACE_OUTER_BOUND('',#26470,.T.);
#22370=FACE_OUTER_BOUND('',#26471,.T.);
#22371=FACE_OUTER_BOUND('',#26472,.T.);
#22372=FACE_OUTER_BOUND('',#26473,.T.);
#22373=FACE_OUTER_BOUND('',#26474,.T.);
#22374=FACE_OUTER_BOUND('',#26475,.T.);
#22375=FACE_OUTER_BOUND('',#26476,.T.);
#22376=FACE_OUTER_BOUND('',#26477,.T.);
#22377=FACE_OUTER_BOUND('',#26478,.T.);
#22378=FACE_OUTER_BOUND('',#26479,.T.);
#22379=FACE_OUTER_BOUND('',#26480,.T.);
#22380=FACE_OUTER_BOUND('',#26481,.T.);
#22381=FACE_OUTER_BOUND('',#26482,.T.);
#22382=FACE_OUTER_BOUND('',#26483,.T.);
#22383=FACE_OUTER_BOUND('',#26484,.T.);
#22384=FACE_OUTER_BOUND('',#26485,.T.);
#22385=FACE_OUTER_BOUND('',#26486,.T.);
#22386=FACE_OUTER_BOUND('',#26487,.T.);
#22387=FACE_OUTER_BOUND('',#26488,.T.);
#22388=FACE_OUTER_BOUND('',#26489,.T.);
#22389=FACE_OUTER_BOUND('',#26490,.T.);
#22390=FACE_OUTER_BOUND('',#26491,.T.);
#22391=FACE_OUTER_BOUND('',#26492,.T.);
#22392=FACE_OUTER_BOUND('',#26493,.T.);
#22393=FACE_OUTER_BOUND('',#26494,.T.);
#22394=FACE_OUTER_BOUND('',#26495,.T.);
#22395=FACE_OUTER_BOUND('',#26496,.T.);
#22396=FACE_OUTER_BOUND('',#26497,.T.);
#22397=FACE_OUTER_BOUND('',#26498,.T.);
#22398=FACE_OUTER_BOUND('',#26499,.T.);
#22399=FACE_OUTER_BOUND('',#26500,.T.);
#22400=FACE_OUTER_BOUND('',#26501,.T.);
#22401=FACE_OUTER_BOUND('',#26502,.T.);
#22402=FACE_OUTER_BOUND('',#26503,.T.);
#22403=FACE_OUTER_BOUND('',#26504,.T.);
#22404=FACE_OUTER_BOUND('',#26505,.T.);
#22405=FACE_OUTER_BOUND('',#26506,.T.);
#22406=FACE_OUTER_BOUND('',#26507,.T.);
#22407=FACE_OUTER_BOUND('',#26508,.T.);
#22408=FACE_OUTER_BOUND('',#26509,.T.);
#22409=FACE_OUTER_BOUND('',#26510,.T.);
#22410=FACE_OUTER_BOUND('',#26511,.T.);
#22411=FACE_OUTER_BOUND('',#26512,.T.);
#22412=FACE_OUTER_BOUND('',#26513,.T.);
#22413=FACE_OUTER_BOUND('',#26514,.T.);
#22414=FACE_OUTER_BOUND('',#26515,.T.);
#22415=FACE_OUTER_BOUND('',#26516,.T.);
#22416=FACE_OUTER_BOUND('',#26517,.T.);
#22417=FACE_OUTER_BOUND('',#26518,.T.);
#22418=FACE_OUTER_BOUND('',#26519,.T.);
#22419=FACE_OUTER_BOUND('',#26520,.T.);
#22420=FACE_OUTER_BOUND('',#26521,.T.);
#22421=FACE_OUTER_BOUND('',#26522,.T.);
#22422=FACE_OUTER_BOUND('',#26523,.T.);
#22423=FACE_OUTER_BOUND('',#26524,.T.);
#22424=FACE_OUTER_BOUND('',#26525,.T.);
#22425=FACE_OUTER_BOUND('',#26526,.T.);
#22426=FACE_OUTER_BOUND('',#26527,.T.);
#22427=FACE_OUTER_BOUND('',#26528,.T.);
#22428=FACE_OUTER_BOUND('',#26529,.T.);
#22429=FACE_OUTER_BOUND('',#26530,.T.);
#22430=FACE_OUTER_BOUND('',#26531,.T.);
#22431=FACE_OUTER_BOUND('',#26532,.T.);
#22432=FACE_OUTER_BOUND('',#26533,.T.);
#22433=FACE_OUTER_BOUND('',#26534,.T.);
#22434=FACE_OUTER_BOUND('',#26535,.T.);
#22435=FACE_OUTER_BOUND('',#26536,.T.);
#22436=FACE_OUTER_BOUND('',#26537,.T.);
#22437=FACE_OUTER_BOUND('',#26538,.T.);
#22438=FACE_OUTER_BOUND('',#26539,.T.);
#22439=FACE_OUTER_BOUND('',#26540,.T.);
#22440=FACE_OUTER_BOUND('',#26541,.T.);
#22441=FACE_OUTER_BOUND('',#26542,.T.);
#22442=FACE_OUTER_BOUND('',#26543,.T.);
#22443=FACE_OUTER_BOUND('',#26544,.T.);
#22444=FACE_OUTER_BOUND('',#26545,.T.);
#22445=FACE_OUTER_BOUND('',#26546,.T.);
#22446=FACE_OUTER_BOUND('',#26547,.T.);
#22447=FACE_OUTER_BOUND('',#26548,.T.);
#22448=FACE_OUTER_BOUND('',#26549,.T.);
#22449=FACE_OUTER_BOUND('',#26550,.T.);
#22450=FACE_OUTER_BOUND('',#26551,.T.);
#22451=FACE_OUTER_BOUND('',#26552,.T.);
#22452=FACE_OUTER_BOUND('',#26553,.T.);
#22453=FACE_OUTER_BOUND('',#26554,.T.);
#22454=FACE_OUTER_BOUND('',#26555,.T.);
#22455=FACE_OUTER_BOUND('',#26556,.T.);
#22456=FACE_OUTER_BOUND('',#26557,.T.);
#22457=FACE_OUTER_BOUND('',#26558,.T.);
#22458=FACE_OUTER_BOUND('',#26559,.T.);
#22459=FACE_OUTER_BOUND('',#26560,.T.);
#22460=FACE_OUTER_BOUND('',#26561,.T.);
#22461=FACE_OUTER_BOUND('',#26562,.T.);
#22462=FACE_OUTER_BOUND('',#26563,.T.);
#22463=FACE_OUTER_BOUND('',#26564,.T.);
#22464=FACE_OUTER_BOUND('',#26565,.T.);
#22465=FACE_OUTER_BOUND('',#26566,.T.);
#22466=FACE_OUTER_BOUND('',#26567,.T.);
#22467=FACE_OUTER_BOUND('',#26568,.T.);
#22468=FACE_OUTER_BOUND('',#26569,.T.);
#22469=FACE_OUTER_BOUND('',#26570,.T.);
#22470=FACE_OUTER_BOUND('',#26571,.T.);
#22471=FACE_OUTER_BOUND('',#26572,.T.);
#22472=FACE_OUTER_BOUND('',#26573,.T.);
#22473=FACE_OUTER_BOUND('',#26574,.T.);
#22474=FACE_OUTER_BOUND('',#26575,.T.);
#22475=FACE_OUTER_BOUND('',#26576,.T.);
#22476=FACE_OUTER_BOUND('',#26577,.T.);
#22477=FACE_OUTER_BOUND('',#26578,.T.);
#22478=FACE_OUTER_BOUND('',#26579,.T.);
#22479=FACE_OUTER_BOUND('',#26580,.T.);
#22480=FACE_OUTER_BOUND('',#26581,.T.);
#22481=FACE_OUTER_BOUND('',#26582,.T.);
#22482=FACE_OUTER_BOUND('',#26583,.T.);
#22483=FACE_OUTER_BOUND('',#26584,.T.);
#22484=FACE_OUTER_BOUND('',#26585,.T.);
#22485=FACE_OUTER_BOUND('',#26586,.T.);
#22486=FACE_OUTER_BOUND('',#26587,.T.);
#22487=FACE_OUTER_BOUND('',#26588,.T.);
#22488=FACE_OUTER_BOUND('',#26589,.T.);
#22489=FACE_OUTER_BOUND('',#26590,.T.);
#22490=FACE_OUTER_BOUND('',#26591,.T.);
#22491=FACE_OUTER_BOUND('',#26592,.T.);
#22492=FACE_OUTER_BOUND('',#26593,.T.);
#22493=FACE_OUTER_BOUND('',#26594,.T.);
#22494=FACE_OUTER_BOUND('',#26595,.T.);
#22495=FACE_OUTER_BOUND('',#26596,.T.);
#22496=FACE_OUTER_BOUND('',#26597,.T.);
#22497=FACE_OUTER_BOUND('',#26598,.T.);
#22498=FACE_OUTER_BOUND('',#26599,.T.);
#22499=FACE_OUTER_BOUND('',#26600,.T.);
#22500=FACE_OUTER_BOUND('',#26601,.T.);
#22501=FACE_OUTER_BOUND('',#26602,.T.);
#22502=FACE_OUTER_BOUND('',#26603,.T.);
#22503=FACE_OUTER_BOUND('',#26604,.T.);
#22504=FACE_OUTER_BOUND('',#26605,.T.);
#22505=FACE_OUTER_BOUND('',#26606,.T.);
#22506=FACE_OUTER_BOUND('',#26607,.T.);
#22507=FACE_OUTER_BOUND('',#26608,.T.);
#22508=FACE_OUTER_BOUND('',#26609,.T.);
#22509=FACE_OUTER_BOUND('',#26610,.T.);
#22510=FACE_OUTER_BOUND('',#26611,.T.);
#22511=FACE_OUTER_BOUND('',#26612,.T.);
#22512=FACE_OUTER_BOUND('',#26613,.T.);
#22513=FACE_OUTER_BOUND('',#26614,.T.);
#22514=FACE_OUTER_BOUND('',#26615,.T.);
#22515=FACE_OUTER_BOUND('',#26616,.T.);
#22516=FACE_OUTER_BOUND('',#26617,.T.);
#22517=FACE_OUTER_BOUND('',#26618,.T.);
#22518=FACE_OUTER_BOUND('',#26619,.T.);
#22519=FACE_OUTER_BOUND('',#26620,.T.);
#22520=FACE_OUTER_BOUND('',#26621,.T.);
#22521=FACE_OUTER_BOUND('',#26622,.T.);
#22522=FACE_OUTER_BOUND('',#26623,.T.);
#22523=FACE_OUTER_BOUND('',#26624,.T.);
#22524=FACE_OUTER_BOUND('',#26625,.T.);
#22525=FACE_OUTER_BOUND('',#26626,.T.);
#22526=FACE_OUTER_BOUND('',#26627,.T.);
#22527=FACE_OUTER_BOUND('',#26628,.T.);
#22528=FACE_OUTER_BOUND('',#26629,.T.);
#22529=FACE_OUTER_BOUND('',#26630,.T.);
#22530=FACE_OUTER_BOUND('',#26631,.T.);
#22531=FACE_OUTER_BOUND('',#26632,.T.);
#22532=FACE_OUTER_BOUND('',#26633,.T.);
#22533=FACE_OUTER_BOUND('',#26634,.T.);
#22534=FACE_OUTER_BOUND('',#26635,.T.);
#22535=FACE_OUTER_BOUND('',#26636,.T.);
#22536=FACE_OUTER_BOUND('',#26637,.T.);
#22537=FACE_OUTER_BOUND('',#26638,.T.);
#22538=FACE_OUTER_BOUND('',#26639,.T.);
#22539=FACE_OUTER_BOUND('',#26640,.T.);
#22540=FACE_OUTER_BOUND('',#26641,.T.);
#22541=FACE_OUTER_BOUND('',#26642,.T.);
#22542=FACE_OUTER_BOUND('',#26643,.T.);
#22543=FACE_OUTER_BOUND('',#26644,.T.);
#22544=FACE_OUTER_BOUND('',#26645,.T.);
#22545=FACE_OUTER_BOUND('',#26646,.T.);
#22546=FACE_OUTER_BOUND('',#26647,.T.);
#22547=FACE_OUTER_BOUND('',#26648,.T.);
#22548=FACE_OUTER_BOUND('',#26649,.T.);
#22549=FACE_OUTER_BOUND('',#26650,.T.);
#22550=FACE_OUTER_BOUND('',#26651,.T.);
#22551=FACE_OUTER_BOUND('',#26652,.T.);
#22552=FACE_OUTER_BOUND('',#26653,.T.);
#22553=FACE_OUTER_BOUND('',#26654,.T.);
#22554=FACE_OUTER_BOUND('',#26655,.T.);
#22555=FACE_OUTER_BOUND('',#26656,.T.);
#22556=FACE_OUTER_BOUND('',#26657,.T.);
#22557=FACE_OUTER_BOUND('',#26658,.T.);
#22558=FACE_OUTER_BOUND('',#26659,.T.);
#22559=FACE_OUTER_BOUND('',#26660,.T.);
#22560=FACE_OUTER_BOUND('',#26661,.T.);
#22561=FACE_OUTER_BOUND('',#26662,.T.);
#22562=FACE_OUTER_BOUND('',#26663,.T.);
#22563=FACE_OUTER_BOUND('',#26664,.T.);
#22564=FACE_OUTER_BOUND('',#26665,.T.);
#22565=FACE_OUTER_BOUND('',#26666,.T.);
#22566=FACE_OUTER_BOUND('',#26667,.T.);
#22567=FACE_OUTER_BOUND('',#26668,.T.);
#22568=FACE_OUTER_BOUND('',#26669,.T.);
#22569=FACE_OUTER_BOUND('',#26670,.T.);
#22570=FACE_OUTER_BOUND('',#26671,.T.);
#22571=FACE_OUTER_BOUND('',#26672,.T.);
#22572=FACE_OUTER_BOUND('',#26673,.T.);
#22573=FACE_OUTER_BOUND('',#26674,.T.);
#22574=FACE_OUTER_BOUND('',#26675,.T.);
#22575=FACE_OUTER_BOUND('',#26676,.T.);
#22576=FACE_OUTER_BOUND('',#26677,.T.);
#22577=FACE_OUTER_BOUND('',#26678,.T.);
#22578=FACE_OUTER_BOUND('',#26679,.T.);
#22579=FACE_OUTER_BOUND('',#26680,.T.);
#22580=FACE_OUTER_BOUND('',#26681,.T.);
#22581=FACE_OUTER_BOUND('',#26682,.T.);
#22582=FACE_OUTER_BOUND('',#26683,.T.);
#22583=FACE_OUTER_BOUND('',#26684,.T.);
#22584=FACE_OUTER_BOUND('',#26685,.T.);
#22585=FACE_OUTER_BOUND('',#26686,.T.);
#22586=FACE_OUTER_BOUND('',#26687,.T.);
#22587=FACE_OUTER_BOUND('',#26688,.T.);
#22588=FACE_OUTER_BOUND('',#26689,.T.);
#22589=FACE_OUTER_BOUND('',#26690,.T.);
#22590=FACE_OUTER_BOUND('',#26691,.T.);
#22591=FACE_OUTER_BOUND('',#26692,.T.);
#22592=FACE_OUTER_BOUND('',#26693,.T.);
#22593=FACE_OUTER_BOUND('',#26694,.T.);
#22594=FACE_OUTER_BOUND('',#26695,.T.);
#22595=FACE_OUTER_BOUND('',#26696,.T.);
#22596=FACE_OUTER_BOUND('',#26697,.T.);
#22597=FACE_OUTER_BOUND('',#26698,.T.);
#22598=FACE_OUTER_BOUND('',#26699,.T.);
#22599=FACE_OUTER_BOUND('',#26700,.T.);
#22600=FACE_OUTER_BOUND('',#26701,.T.);
#22601=FACE_OUTER_BOUND('',#26702,.T.);
#22602=FACE_OUTER_BOUND('',#26703,.T.);
#22603=FACE_OUTER_BOUND('',#26704,.T.);
#22604=FACE_OUTER_BOUND('',#26705,.T.);
#22605=FACE_OUTER_BOUND('',#26706,.T.);
#22606=FACE_OUTER_BOUND('',#26707,.T.);
#22607=FACE_OUTER_BOUND('',#26708,.T.);
#22608=FACE_OUTER_BOUND('',#26709,.T.);
#22609=FACE_OUTER_BOUND('',#26710,.T.);
#22610=FACE_OUTER_BOUND('',#26711,.T.);
#22611=FACE_OUTER_BOUND('',#26712,.T.);
#22612=FACE_OUTER_BOUND('',#26713,.T.);
#22613=FACE_OUTER_BOUND('',#26714,.T.);
#22614=FACE_OUTER_BOUND('',#26715,.T.);
#22615=FACE_OUTER_BOUND('',#26716,.T.);
#22616=FACE_OUTER_BOUND('',#26717,.T.);
#22617=FACE_OUTER_BOUND('',#26718,.T.);
#22618=FACE_OUTER_BOUND('',#26719,.T.);
#22619=FACE_OUTER_BOUND('',#26720,.T.);
#22620=FACE_OUTER_BOUND('',#26721,.T.);
#22621=FACE_OUTER_BOUND('',#26722,.T.);
#22622=FACE_OUTER_BOUND('',#26723,.T.);
#22623=FACE_OUTER_BOUND('',#26724,.T.);
#22624=FACE_OUTER_BOUND('',#26725,.T.);
#22625=FACE_OUTER_BOUND('',#26726,.T.);
#22626=FACE_OUTER_BOUND('',#26727,.T.);
#22627=FACE_OUTER_BOUND('',#26728,.T.);
#22628=FACE_OUTER_BOUND('',#26729,.T.);
#22629=FACE_OUTER_BOUND('',#26730,.T.);
#22630=FACE_OUTER_BOUND('',#26731,.T.);
#22631=FACE_OUTER_BOUND('',#26732,.T.);
#22632=FACE_OUTER_BOUND('',#26733,.T.);
#22633=FACE_OUTER_BOUND('',#26734,.T.);
#22634=FACE_OUTER_BOUND('',#26735,.T.);
#22635=FACE_OUTER_BOUND('',#26736,.T.);
#22636=FACE_OUTER_BOUND('',#26737,.T.);
#22637=FACE_OUTER_BOUND('',#26738,.T.);
#22638=FACE_OUTER_BOUND('',#26739,.T.);
#22639=FACE_OUTER_BOUND('',#26740,.T.);
#22640=FACE_OUTER_BOUND('',#26741,.T.);
#22641=FACE_OUTER_BOUND('',#26742,.T.);
#22642=FACE_OUTER_BOUND('',#26743,.T.);
#22643=FACE_OUTER_BOUND('',#26744,.T.);
#22644=FACE_OUTER_BOUND('',#26745,.T.);
#22645=FACE_OUTER_BOUND('',#26746,.T.);
#22646=FACE_OUTER_BOUND('',#26747,.T.);
#22647=FACE_OUTER_BOUND('',#26748,.T.);
#22648=FACE_OUTER_BOUND('',#26749,.T.);
#22649=FACE_OUTER_BOUND('',#26750,.T.);
#22650=FACE_OUTER_BOUND('',#26751,.T.);
#22651=FACE_OUTER_BOUND('',#26752,.T.);
#22652=FACE_OUTER_BOUND('',#26753,.T.);
#22653=FACE_OUTER_BOUND('',#26754,.T.);
#22654=FACE_OUTER_BOUND('',#26755,.T.);
#22655=FACE_OUTER_BOUND('',#26756,.T.);
#22656=FACE_OUTER_BOUND('',#26757,.T.);
#22657=FACE_OUTER_BOUND('',#26758,.T.);
#22658=FACE_OUTER_BOUND('',#26759,.T.);
#22659=FACE_OUTER_BOUND('',#26760,.T.);
#22660=FACE_OUTER_BOUND('',#26761,.T.);
#22661=FACE_OUTER_BOUND('',#26762,.T.);
#22662=FACE_OUTER_BOUND('',#26763,.T.);
#22663=FACE_OUTER_BOUND('',#26764,.T.);
#22664=FACE_OUTER_BOUND('',#26765,.T.);
#22665=FACE_OUTER_BOUND('',#26766,.T.);
#22666=FACE_OUTER_BOUND('',#26767,.T.);
#22667=FACE_OUTER_BOUND('',#26768,.T.);
#22668=FACE_OUTER_BOUND('',#26769,.T.);
#22669=FACE_OUTER_BOUND('',#26770,.T.);
#22670=FACE_OUTER_BOUND('',#26771,.T.);
#22671=FACE_OUTER_BOUND('',#26772,.T.);
#22672=FACE_OUTER_BOUND('',#26773,.T.);
#22673=FACE_OUTER_BOUND('',#26774,.T.);
#22674=FACE_OUTER_BOUND('',#26775,.T.);
#22675=FACE_OUTER_BOUND('',#26776,.T.);
#22676=FACE_OUTER_BOUND('',#26777,.T.);
#22677=FACE_OUTER_BOUND('',#26778,.T.);
#22678=FACE_OUTER_BOUND('',#26779,.T.);
#22679=FACE_OUTER_BOUND('',#26780,.T.);
#22680=FACE_OUTER_BOUND('',#26781,.T.);
#22681=FACE_OUTER_BOUND('',#26782,.T.);
#22682=FACE_OUTER_BOUND('',#26783,.T.);
#22683=FACE_OUTER_BOUND('',#26784,.T.);
#22684=FACE_OUTER_BOUND('',#26785,.T.);
#22685=FACE_OUTER_BOUND('',#26786,.T.);
#22686=FACE_OUTER_BOUND('',#26787,.T.);
#22687=FACE_OUTER_BOUND('',#26788,.T.);
#22688=FACE_OUTER_BOUND('',#26789,.T.);
#22689=FACE_OUTER_BOUND('',#26790,.T.);
#22690=FACE_OUTER_BOUND('',#26791,.T.);
#22691=FACE_OUTER_BOUND('',#26792,.T.);
#22692=FACE_OUTER_BOUND('',#26793,.T.);
#22693=FACE_OUTER_BOUND('',#26794,.T.);
#22694=FACE_OUTER_BOUND('',#26795,.T.);
#22695=FACE_OUTER_BOUND('',#26796,.T.);
#22696=FACE_OUTER_BOUND('',#26797,.T.);
#22697=FACE_OUTER_BOUND('',#26798,.T.);
#22698=FACE_OUTER_BOUND('',#26799,.T.);
#22699=FACE_OUTER_BOUND('',#26800,.T.);
#22700=FACE_OUTER_BOUND('',#26801,.T.);
#22701=FACE_OUTER_BOUND('',#26802,.T.);
#22702=FACE_OUTER_BOUND('',#26803,.T.);
#22703=FACE_OUTER_BOUND('',#26804,.T.);
#22704=FACE_OUTER_BOUND('',#26805,.T.);
#22705=FACE_OUTER_BOUND('',#26806,.T.);
#22706=FACE_OUTER_BOUND('',#26807,.T.);
#22707=FACE_OUTER_BOUND('',#26808,.T.);
#22708=FACE_OUTER_BOUND('',#26809,.T.);
#22709=FACE_OUTER_BOUND('',#26810,.T.);
#22710=FACE_OUTER_BOUND('',#26811,.T.);
#22711=FACE_OUTER_BOUND('',#26812,.T.);
#22712=FACE_OUTER_BOUND('',#26813,.T.);
#22713=FACE_OUTER_BOUND('',#26814,.T.);
#22714=FACE_OUTER_BOUND('',#26815,.T.);
#22715=FACE_OUTER_BOUND('',#26816,.T.);
#22716=FACE_OUTER_BOUND('',#26817,.T.);
#22717=FACE_OUTER_BOUND('',#26818,.T.);
#22718=FACE_OUTER_BOUND('',#26819,.T.);
#22719=FACE_OUTER_BOUND('',#26820,.T.);
#22720=FACE_OUTER_BOUND('',#26821,.T.);
#22721=FACE_OUTER_BOUND('',#26822,.T.);
#22722=FACE_OUTER_BOUND('',#26823,.T.);
#22723=FACE_OUTER_BOUND('',#26824,.T.);
#22724=FACE_OUTER_BOUND('',#26825,.T.);
#22725=FACE_OUTER_BOUND('',#26826,.T.);
#22726=FACE_OUTER_BOUND('',#26827,.T.);
#22727=FACE_OUTER_BOUND('',#26828,.T.);
#22728=FACE_OUTER_BOUND('',#26829,.T.);
#22729=FACE_OUTER_BOUND('',#26830,.T.);
#22730=FACE_OUTER_BOUND('',#26831,.T.);
#22731=FACE_OUTER_BOUND('',#26832,.T.);
#22732=FACE_OUTER_BOUND('',#26833,.T.);
#22733=FACE_OUTER_BOUND('',#26834,.T.);
#22734=FACE_OUTER_BOUND('',#26835,.T.);
#22735=FACE_OUTER_BOUND('',#26836,.T.);
#22736=FACE_OUTER_BOUND('',#26837,.T.);
#22737=FACE_OUTER_BOUND('',#26838,.T.);
#22738=FACE_OUTER_BOUND('',#26839,.T.);
#22739=FACE_OUTER_BOUND('',#26840,.T.);
#22740=FACE_OUTER_BOUND('',#26841,.T.);
#22741=FACE_OUTER_BOUND('',#26842,.T.);
#22742=FACE_OUTER_BOUND('',#26843,.T.);
#22743=FACE_OUTER_BOUND('',#26844,.T.);
#22744=FACE_OUTER_BOUND('',#26845,.T.);
#22745=FACE_OUTER_BOUND('',#26846,.T.);
#22746=FACE_OUTER_BOUND('',#26847,.T.);
#22747=FACE_OUTER_BOUND('',#26848,.T.);
#22748=FACE_OUTER_BOUND('',#26849,.T.);
#22749=FACE_OUTER_BOUND('',#26850,.T.);
#22750=FACE_OUTER_BOUND('',#26851,.T.);
#22751=FACE_OUTER_BOUND('',#26852,.T.);
#22752=FACE_OUTER_BOUND('',#26853,.T.);
#22753=FACE_OUTER_BOUND('',#26854,.T.);
#22754=FACE_OUTER_BOUND('',#26855,.T.);
#22755=FACE_OUTER_BOUND('',#26856,.T.);
#22756=FACE_OUTER_BOUND('',#26857,.T.);
#22757=FACE_OUTER_BOUND('',#26858,.T.);
#22758=FACE_OUTER_BOUND('',#26859,.T.);
#22759=FACE_OUTER_BOUND('',#26860,.T.);
#22760=FACE_OUTER_BOUND('',#26861,.T.);
#22761=FACE_OUTER_BOUND('',#26862,.T.);
#22762=FACE_OUTER_BOUND('',#26863,.T.);
#22763=FACE_OUTER_BOUND('',#26864,.T.);
#22764=FACE_OUTER_BOUND('',#26865,.T.);
#22765=FACE_OUTER_BOUND('',#26866,.T.);
#22766=FACE_OUTER_BOUND('',#26867,.T.);
#22767=FACE_OUTER_BOUND('',#26868,.T.);
#22768=FACE_OUTER_BOUND('',#26869,.T.);
#22769=FACE_OUTER_BOUND('',#26870,.T.);
#22770=FACE_OUTER_BOUND('',#26871,.T.);
#22771=FACE_OUTER_BOUND('',#26872,.T.);
#22772=FACE_OUTER_BOUND('',#26873,.T.);
#22773=FACE_OUTER_BOUND('',#26874,.T.);
#22774=FACE_OUTER_BOUND('',#26875,.T.);
#22775=FACE_OUTER_BOUND('',#26876,.T.);
#22776=FACE_OUTER_BOUND('',#26877,.T.);
#22777=FACE_OUTER_BOUND('',#26878,.T.);
#22778=FACE_OUTER_BOUND('',#26879,.T.);
#22779=FACE_OUTER_BOUND('',#26880,.T.);
#22780=FACE_OUTER_BOUND('',#26881,.T.);
#22781=FACE_OUTER_BOUND('',#26882,.T.);
#22782=FACE_OUTER_BOUND('',#26883,.T.);
#22783=FACE_OUTER_BOUND('',#26884,.T.);
#22784=FACE_OUTER_BOUND('',#26885,.T.);
#22785=FACE_OUTER_BOUND('',#26886,.T.);
#22786=FACE_OUTER_BOUND('',#26887,.T.);
#22787=FACE_OUTER_BOUND('',#26888,.T.);
#22788=FACE_OUTER_BOUND('',#26889,.T.);
#22789=FACE_OUTER_BOUND('',#26890,.T.);
#22790=FACE_OUTER_BOUND('',#26891,.T.);
#22791=FACE_OUTER_BOUND('',#26892,.T.);
#22792=FACE_OUTER_BOUND('',#26893,.T.);
#22793=FACE_OUTER_BOUND('',#26894,.T.);
#22794=FACE_OUTER_BOUND('',#26895,.T.);
#22795=FACE_OUTER_BOUND('',#26896,.T.);
#22796=FACE_OUTER_BOUND('',#26897,.T.);
#22797=FACE_OUTER_BOUND('',#26898,.T.);
#22798=FACE_OUTER_BOUND('',#26899,.T.);
#22799=FACE_OUTER_BOUND('',#26900,.T.);
#22800=FACE_OUTER_BOUND('',#26901,.T.);
#22801=FACE_OUTER_BOUND('',#26902,.T.);
#22802=FACE_OUTER_BOUND('',#26903,.T.);
#22803=FACE_OUTER_BOUND('',#26904,.T.);
#22804=FACE_OUTER_BOUND('',#26905,.T.);
#22805=FACE_OUTER_BOUND('',#26906,.T.);
#22806=FACE_OUTER_BOUND('',#26907,.T.);
#22807=FACE_OUTER_BOUND('',#26908,.T.);
#22808=FACE_OUTER_BOUND('',#26909,.T.);
#22809=FACE_OUTER_BOUND('',#26910,.T.);
#22810=FACE_OUTER_BOUND('',#26911,.T.);
#22811=FACE_OUTER_BOUND('',#26912,.T.);
#22812=FACE_OUTER_BOUND('',#26913,.T.);
#22813=FACE_OUTER_BOUND('',#26914,.T.);
#22814=FACE_OUTER_BOUND('',#26915,.T.);
#22815=FACE_OUTER_BOUND('',#26916,.T.);
#22816=FACE_OUTER_BOUND('',#26917,.T.);
#22817=FACE_OUTER_BOUND('',#26918,.T.);
#22818=FACE_OUTER_BOUND('',#26919,.T.);
#22819=FACE_OUTER_BOUND('',#26920,.T.);
#22820=FACE_OUTER_BOUND('',#26921,.T.);
#22821=FACE_OUTER_BOUND('',#26922,.T.);
#22822=FACE_OUTER_BOUND('',#26923,.T.);
#22823=FACE_OUTER_BOUND('',#26924,.T.);
#22824=FACE_OUTER_BOUND('',#26925,.T.);
#22825=FACE_OUTER_BOUND('',#26926,.T.);
#22826=FACE_OUTER_BOUND('',#26927,.T.);
#22827=FACE_OUTER_BOUND('',#26928,.T.);
#22828=FACE_OUTER_BOUND('',#26929,.T.);
#22829=FACE_OUTER_BOUND('',#26930,.T.);
#22830=FACE_OUTER_BOUND('',#26931,.T.);
#22831=FACE_OUTER_BOUND('',#26932,.T.);
#22832=FACE_OUTER_BOUND('',#26933,.T.);
#22833=FACE_OUTER_BOUND('',#26934,.T.);
#22834=FACE_OUTER_BOUND('',#26935,.T.);
#22835=FACE_OUTER_BOUND('',#26936,.T.);
#22836=FACE_OUTER_BOUND('',#26937,.T.);
#22837=FACE_OUTER_BOUND('',#26938,.T.);
#22838=FACE_OUTER_BOUND('',#26939,.T.);
#22839=FACE_OUTER_BOUND('',#26940,.T.);
#22840=FACE_OUTER_BOUND('',#26941,.T.);
#22841=FACE_OUTER_BOUND('',#26942,.T.);
#22842=FACE_OUTER_BOUND('',#26943,.T.);
#22843=FACE_OUTER_BOUND('',#26944,.T.);
#22844=FACE_OUTER_BOUND('',#26945,.T.);
#22845=FACE_OUTER_BOUND('',#26946,.T.);
#22846=FACE_OUTER_BOUND('',#26947,.T.);
#22847=FACE_OUTER_BOUND('',#26948,.T.);
#22848=FACE_OUTER_BOUND('',#26949,.T.);
#22849=FACE_OUTER_BOUND('',#26950,.T.);
#22850=FACE_OUTER_BOUND('',#26951,.T.);
#22851=FACE_OUTER_BOUND('',#26952,.T.);
#22852=FACE_OUTER_BOUND('',#26953,.T.);
#22853=FACE_OUTER_BOUND('',#26954,.T.);
#22854=FACE_OUTER_BOUND('',#26955,.T.);
#22855=FACE_OUTER_BOUND('',#26956,.T.);
#22856=FACE_OUTER_BOUND('',#26957,.T.);
#22857=FACE_OUTER_BOUND('',#26958,.T.);
#22858=FACE_OUTER_BOUND('',#26959,.T.);
#22859=FACE_OUTER_BOUND('',#26960,.T.);
#22860=FACE_OUTER_BOUND('',#26961,.T.);
#22861=FACE_OUTER_BOUND('',#26962,.T.);
#22862=FACE_OUTER_BOUND('',#26963,.T.);
#22863=FACE_OUTER_BOUND('',#26964,.T.);
#22864=FACE_OUTER_BOUND('',#26965,.T.);
#22865=FACE_OUTER_BOUND('',#26966,.T.);
#22866=FACE_OUTER_BOUND('',#26967,.T.);
#22867=FACE_OUTER_BOUND('',#26968,.T.);
#22868=FACE_OUTER_BOUND('',#26969,.T.);
#22869=FACE_OUTER_BOUND('',#26970,.T.);
#22870=FACE_OUTER_BOUND('',#26971,.T.);
#22871=FACE_OUTER_BOUND('',#26972,.T.);
#22872=FACE_OUTER_BOUND('',#26973,.T.);
#22873=FACE_OUTER_BOUND('',#26974,.T.);
#22874=FACE_OUTER_BOUND('',#26975,.T.);
#22875=FACE_OUTER_BOUND('',#26976,.T.);
#22876=FACE_OUTER_BOUND('',#26977,.T.);
#22877=FACE_OUTER_BOUND('',#26978,.T.);
#22878=FACE_OUTER_BOUND('',#26979,.T.);
#22879=FACE_OUTER_BOUND('',#26980,.T.);
#22880=FACE_OUTER_BOUND('',#26981,.T.);
#22881=FACE_OUTER_BOUND('',#26982,.T.);
#22882=FACE_OUTER_BOUND('',#26983,.T.);
#22883=FACE_OUTER_BOUND('',#26984,.T.);
#22884=FACE_OUTER_BOUND('',#26985,.T.);
#22885=FACE_OUTER_BOUND('',#26986,.T.);
#22886=FACE_OUTER_BOUND('',#26987,.T.);
#22887=FACE_OUTER_BOUND('',#26988,.T.);
#22888=FACE_OUTER_BOUND('',#26989,.T.);
#22889=FACE_OUTER_BOUND('',#26990,.T.);
#22890=FACE_OUTER_BOUND('',#26991,.T.);
#22891=FACE_OUTER_BOUND('',#26992,.T.);
#22892=FACE_OUTER_BOUND('',#26993,.T.);
#22893=FACE_OUTER_BOUND('',#26994,.T.);
#22894=FACE_OUTER_BOUND('',#26995,.T.);
#22895=FACE_OUTER_BOUND('',#26996,.T.);
#22896=FACE_OUTER_BOUND('',#26997,.T.);
#22897=FACE_OUTER_BOUND('',#26998,.T.);
#22898=FACE_OUTER_BOUND('',#26999,.T.);
#22899=FACE_OUTER_BOUND('',#27000,.T.);
#22900=FACE_OUTER_BOUND('',#27001,.T.);
#22901=FACE_OUTER_BOUND('',#27002,.T.);
#22902=FACE_OUTER_BOUND('',#27003,.T.);
#22903=FACE_OUTER_BOUND('',#27004,.T.);
#22904=FACE_OUTER_BOUND('',#27005,.T.);
#22905=FACE_OUTER_BOUND('',#27006,.T.);
#22906=FACE_OUTER_BOUND('',#27007,.T.);
#22907=FACE_OUTER_BOUND('',#27008,.T.);
#22908=FACE_OUTER_BOUND('',#27009,.T.);
#22909=FACE_OUTER_BOUND('',#27010,.T.);
#22910=FACE_OUTER_BOUND('',#27011,.T.);
#22911=FACE_OUTER_BOUND('',#27012,.T.);
#22912=FACE_OUTER_BOUND('',#27013,.T.);
#22913=FACE_OUTER_BOUND('',#27014,.T.);
#22914=FACE_OUTER_BOUND('',#27015,.T.);
#22915=FACE_OUTER_BOUND('',#27016,.T.);
#22916=FACE_OUTER_BOUND('',#27017,.T.);
#22917=FACE_OUTER_BOUND('',#27018,.T.);
#22918=FACE_OUTER_BOUND('',#27019,.T.);
#22919=FACE_OUTER_BOUND('',#27020,.T.);
#22920=FACE_OUTER_BOUND('',#27021,.T.);
#22921=FACE_OUTER_BOUND('',#27022,.T.);
#22922=FACE_OUTER_BOUND('',#27023,.T.);
#22923=FACE_OUTER_BOUND('',#27024,.T.);
#22924=FACE_OUTER_BOUND('',#27025,.T.);
#22925=FACE_OUTER_BOUND('',#27026,.T.);
#22926=FACE_OUTER_BOUND('',#27027,.T.);
#22927=FACE_OUTER_BOUND('',#27028,.T.);
#22928=FACE_OUTER_BOUND('',#27029,.T.);
#22929=FACE_OUTER_BOUND('',#27030,.T.);
#22930=FACE_OUTER_BOUND('',#27031,.T.);
#22931=FACE_OUTER_BOUND('',#27032,.T.);
#22932=FACE_OUTER_BOUND('',#27033,.T.);
#22933=FACE_OUTER_BOUND('',#27034,.T.);
#22934=FACE_OUTER_BOUND('',#27035,.T.);
#22935=FACE_OUTER_BOUND('',#27036,.T.);
#22936=FACE_OUTER_BOUND('',#27037,.T.);
#22937=FACE_OUTER_BOUND('',#27038,.T.);
#22938=FACE_OUTER_BOUND('',#27039,.T.);
#22939=FACE_OUTER_BOUND('',#27040,.T.);
#22940=FACE_OUTER_BOUND('',#27041,.T.);
#22941=FACE_OUTER_BOUND('',#27042,.T.);
#22942=FACE_OUTER_BOUND('',#27043,.T.);
#22943=FACE_OUTER_BOUND('',#27044,.T.);
#22944=FACE_OUTER_BOUND('',#27045,.T.);
#22945=FACE_OUTER_BOUND('',#27046,.T.);
#22946=FACE_OUTER_BOUND('',#27047,.T.);
#22947=FACE_OUTER_BOUND('',#27048,.T.);
#22948=FACE_OUTER_BOUND('',#27049,.T.);
#22949=FACE_OUTER_BOUND('',#27050,.T.);
#22950=FACE_OUTER_BOUND('',#27051,.T.);
#22951=FACE_OUTER_BOUND('',#27052,.T.);
#22952=FACE_OUTER_BOUND('',#27053,.T.);
#22953=FACE_OUTER_BOUND('',#27054,.T.);
#22954=FACE_OUTER_BOUND('',#27055,.T.);
#22955=FACE_OUTER_BOUND('',#27056,.T.);
#22956=FACE_OUTER_BOUND('',#27057,.T.);
#22957=FACE_OUTER_BOUND('',#27058,.T.);
#22958=FACE_OUTER_BOUND('',#27059,.T.);
#22959=FACE_OUTER_BOUND('',#27060,.T.);
#22960=FACE_OUTER_BOUND('',#27061,.T.);
#22961=FACE_OUTER_BOUND('',#27062,.T.);
#22962=FACE_OUTER_BOUND('',#27063,.T.);
#22963=FACE_OUTER_BOUND('',#27064,.T.);
#22964=FACE_OUTER_BOUND('',#27065,.T.);
#22965=FACE_OUTER_BOUND('',#27066,.T.);
#22966=FACE_OUTER_BOUND('',#27067,.T.);
#22967=FACE_OUTER_BOUND('',#27068,.T.);
#22968=FACE_OUTER_BOUND('',#27069,.T.);
#22969=FACE_OUTER_BOUND('',#27070,.T.);
#22970=FACE_OUTER_BOUND('',#27071,.T.);
#22971=FACE_OUTER_BOUND('',#27072,.T.);
#22972=FACE_OUTER_BOUND('',#27073,.T.);
#22973=FACE_OUTER_BOUND('',#27074,.T.);
#22974=FACE_OUTER_BOUND('',#27075,.T.);
#22975=FACE_OUTER_BOUND('',#27076,.T.);
#22976=FACE_OUTER_BOUND('',#27077,.T.);
#22977=FACE_OUTER_BOUND('',#27078,.T.);
#22978=FACE_OUTER_BOUND('',#27079,.T.);
#22979=FACE_OUTER_BOUND('',#27080,.T.);
#22980=FACE_OUTER_BOUND('',#27081,.T.);
#22981=FACE_OUTER_BOUND('',#27082,.T.);
#22982=FACE_OUTER_BOUND('',#27083,.T.);
#22983=FACE_OUTER_BOUND('',#27084,.T.);
#22984=FACE_OUTER_BOUND('',#27085,.T.);
#22985=FACE_OUTER_BOUND('',#27086,.T.);
#22986=FACE_OUTER_BOUND('',#27087,.T.);
#22987=FACE_OUTER_BOUND('',#27088,.T.);
#22988=FACE_OUTER_BOUND('',#27089,.T.);
#22989=FACE_OUTER_BOUND('',#27090,.T.);
#22990=FACE_OUTER_BOUND('',#27091,.T.);
#22991=FACE_OUTER_BOUND('',#27092,.T.);
#22992=FACE_OUTER_BOUND('',#27093,.T.);
#22993=FACE_OUTER_BOUND('',#27094,.T.);
#22994=FACE_OUTER_BOUND('',#27095,.T.);
#22995=FACE_OUTER_BOUND('',#27096,.T.);
#22996=FACE_OUTER_BOUND('',#27097,.T.);
#22997=FACE_OUTER_BOUND('',#27098,.T.);
#22998=FACE_OUTER_BOUND('',#27099,.T.);
#22999=FACE_OUTER_BOUND('',#27100,.T.);
#23000=FACE_OUTER_BOUND('',#27101,.T.);
#23001=FACE_OUTER_BOUND('',#27102,.T.);
#23002=FACE_OUTER_BOUND('',#27103,.T.);
#23003=FACE_OUTER_BOUND('',#27104,.T.);
#23004=FACE_OUTER_BOUND('',#27105,.T.);
#23005=FACE_OUTER_BOUND('',#27106,.T.);
#23006=FACE_OUTER_BOUND('',#27107,.T.);
#23007=FACE_OUTER_BOUND('',#27108,.T.);
#23008=FACE_OUTER_BOUND('',#27109,.T.);
#23009=FACE_OUTER_BOUND('',#27110,.T.);
#23010=FACE_OUTER_BOUND('',#27111,.T.);
#23011=FACE_OUTER_BOUND('',#27112,.T.);
#23012=FACE_OUTER_BOUND('',#27113,.T.);
#23013=FACE_OUTER_BOUND('',#27114,.T.);
#23014=FACE_OUTER_BOUND('',#27115,.T.);
#23015=FACE_OUTER_BOUND('',#27116,.T.);
#23016=FACE_OUTER_BOUND('',#27117,.T.);
#23017=FACE_OUTER_BOUND('',#27118,.T.);
#23018=FACE_OUTER_BOUND('',#27119,.T.);
#23019=FACE_OUTER_BOUND('',#27120,.T.);
#23020=FACE_OUTER_BOUND('',#27121,.T.);
#23021=FACE_OUTER_BOUND('',#27122,.T.);
#23022=FACE_OUTER_BOUND('',#27123,.T.);
#23023=FACE_OUTER_BOUND('',#27124,.T.);
#23024=FACE_OUTER_BOUND('',#27125,.T.);
#23025=FACE_OUTER_BOUND('',#27126,.T.);
#23026=FACE_OUTER_BOUND('',#27127,.T.);
#23027=FACE_OUTER_BOUND('',#27128,.T.);
#23028=FACE_OUTER_BOUND('',#27129,.T.);
#23029=FACE_OUTER_BOUND('',#27130,.T.);
#23030=FACE_OUTER_BOUND('',#27131,.T.);
#23031=FACE_OUTER_BOUND('',#27132,.T.);
#23032=FACE_OUTER_BOUND('',#27133,.T.);
#23033=FACE_OUTER_BOUND('',#27134,.T.);
#23034=FACE_OUTER_BOUND('',#27135,.T.);
#23035=FACE_OUTER_BOUND('',#27136,.T.);
#23036=FACE_OUTER_BOUND('',#27137,.T.);
#23037=FACE_OUTER_BOUND('',#27138,.T.);
#23038=FACE_OUTER_BOUND('',#27139,.T.);
#23039=FACE_OUTER_BOUND('',#27140,.T.);
#23040=FACE_OUTER_BOUND('',#27141,.T.);
#23041=FACE_OUTER_BOUND('',#27142,.T.);
#23042=FACE_OUTER_BOUND('',#27143,.T.);
#23043=FACE_OUTER_BOUND('',#27144,.T.);
#23044=FACE_OUTER_BOUND('',#27145,.T.);
#23045=FACE_OUTER_BOUND('',#27146,.T.);
#23046=FACE_OUTER_BOUND('',#27147,.T.);
#23047=FACE_OUTER_BOUND('',#27148,.T.);
#23048=FACE_OUTER_BOUND('',#27149,.T.);
#23049=FACE_OUTER_BOUND('',#27150,.T.);
#23050=FACE_OUTER_BOUND('',#27151,.T.);
#23051=FACE_OUTER_BOUND('',#27152,.T.);
#23052=FACE_OUTER_BOUND('',#27153,.T.);
#23053=FACE_OUTER_BOUND('',#27154,.T.);
#23054=FACE_OUTER_BOUND('',#27155,.T.);
#23055=FACE_OUTER_BOUND('',#27156,.T.);
#23056=FACE_OUTER_BOUND('',#27157,.T.);
#23057=FACE_OUTER_BOUND('',#27158,.T.);
#23058=FACE_OUTER_BOUND('',#27159,.T.);
#23059=FACE_OUTER_BOUND('',#27160,.T.);
#23060=FACE_OUTER_BOUND('',#27161,.T.);
#23061=FACE_OUTER_BOUND('',#27162,.T.);
#23062=FACE_OUTER_BOUND('',#27163,.T.);
#23063=FACE_OUTER_BOUND('',#27164,.T.);
#23064=FACE_OUTER_BOUND('',#27165,.T.);
#23065=FACE_OUTER_BOUND('',#27166,.T.);
#23066=FACE_OUTER_BOUND('',#27167,.T.);
#23067=FACE_OUTER_BOUND('',#27168,.T.);
#23068=FACE_OUTER_BOUND('',#27169,.T.);
#23069=FACE_OUTER_BOUND('',#27170,.T.);
#23070=FACE_OUTER_BOUND('',#27171,.T.);
#23071=FACE_OUTER_BOUND('',#27172,.T.);
#23072=FACE_OUTER_BOUND('',#27173,.T.);
#23073=FACE_OUTER_BOUND('',#27174,.T.);
#23074=FACE_OUTER_BOUND('',#27175,.T.);
#23075=FACE_OUTER_BOUND('',#27176,.T.);
#23076=FACE_OUTER_BOUND('',#27177,.T.);
#23077=FACE_OUTER_BOUND('',#27178,.T.);
#23078=FACE_OUTER_BOUND('',#27179,.T.);
#23079=FACE_OUTER_BOUND('',#27180,.T.);
#23080=FACE_OUTER_BOUND('',#27181,.T.);
#23081=FACE_OUTER_BOUND('',#27182,.T.);
#23082=FACE_OUTER_BOUND('',#27183,.T.);
#23083=FACE_OUTER_BOUND('',#27184,.T.);
#23084=FACE_OUTER_BOUND('',#27185,.T.);
#23085=FACE_OUTER_BOUND('',#27186,.T.);
#23086=FACE_OUTER_BOUND('',#27187,.T.);
#23087=FACE_OUTER_BOUND('',#27188,.T.);
#23088=FACE_OUTER_BOUND('',#27189,.T.);
#23089=FACE_OUTER_BOUND('',#27190,.T.);
#23090=FACE_OUTER_BOUND('',#27191,.T.);
#23091=FACE_OUTER_BOUND('',#27192,.T.);
#23092=FACE_OUTER_BOUND('',#27193,.T.);
#23093=FACE_OUTER_BOUND('',#27194,.T.);
#23094=FACE_OUTER_BOUND('',#27195,.T.);
#23095=FACE_OUTER_BOUND('',#27196,.T.);
#23096=FACE_OUTER_BOUND('',#27197,.T.);
#23097=FACE_OUTER_BOUND('',#27198,.T.);
#23098=FACE_OUTER_BOUND('',#27199,.T.);
#23099=FACE_OUTER_BOUND('',#27200,.T.);
#23100=FACE_OUTER_BOUND('',#27201,.T.);
#23101=FACE_OUTER_BOUND('',#27202,.T.);
#23102=FACE_OUTER_BOUND('',#27203,.T.);
#23103=FACE_OUTER_BOUND('',#27204,.T.);
#23104=FACE_OUTER_BOUND('',#27205,.T.);
#23105=FACE_OUTER_BOUND('',#27206,.T.);
#23106=FACE_OUTER_BOUND('',#27207,.T.);
#23107=FACE_OUTER_BOUND('',#27208,.T.);
#23108=FACE_OUTER_BOUND('',#27209,.T.);
#23109=FACE_OUTER_BOUND('',#27210,.T.);
#23110=FACE_OUTER_BOUND('',#27211,.T.);
#23111=FACE_OUTER_BOUND('',#27212,.T.);
#23112=FACE_OUTER_BOUND('',#27213,.T.);
#23113=FACE_OUTER_BOUND('',#27214,.T.);
#23114=FACE_OUTER_BOUND('',#27215,.T.);
#23115=FACE_OUTER_BOUND('',#27216,.T.);
#23116=FACE_OUTER_BOUND('',#27217,.T.);
#23117=FACE_OUTER_BOUND('',#27218,.T.);
#23118=FACE_OUTER_BOUND('',#27219,.T.);
#23119=FACE_OUTER_BOUND('',#27220,.T.);
#23120=FACE_OUTER_BOUND('',#27221,.T.);
#23121=FACE_OUTER_BOUND('',#27222,.T.);
#23122=FACE_OUTER_BOUND('',#27223,.T.);
#23123=FACE_OUTER_BOUND('',#27224,.T.);
#23124=FACE_OUTER_BOUND('',#27225,.T.);
#23125=FACE_OUTER_BOUND('',#27226,.T.);
#23126=FACE_OUTER_BOUND('',#27227,.T.);
#23127=FACE_OUTER_BOUND('',#27228,.T.);
#23128=FACE_OUTER_BOUND('',#27229,.T.);
#23129=FACE_OUTER_BOUND('',#27230,.T.);
#23130=FACE_OUTER_BOUND('',#27231,.T.);
#23131=FACE_OUTER_BOUND('',#27232,.T.);
#23132=FACE_OUTER_BOUND('',#27233,.T.);
#23133=FACE_OUTER_BOUND('',#27234,.T.);
#23134=FACE_OUTER_BOUND('',#27235,.T.);
#23135=FACE_OUTER_BOUND('',#27236,.T.);
#23136=FACE_OUTER_BOUND('',#27237,.T.);
#23137=FACE_OUTER_BOUND('',#27238,.T.);
#23138=FACE_OUTER_BOUND('',#27239,.T.);
#23139=FACE_OUTER_BOUND('',#27240,.T.);
#23140=FACE_OUTER_BOUND('',#27241,.T.);
#23141=FACE_OUTER_BOUND('',#27242,.T.);
#23142=FACE_OUTER_BOUND('',#27243,.T.);
#23143=FACE_OUTER_BOUND('',#27244,.T.);
#23144=FACE_OUTER_BOUND('',#27245,.T.);
#23145=FACE_OUTER_BOUND('',#27246,.T.);
#23146=FACE_OUTER_BOUND('',#27247,.T.);
#23147=FACE_OUTER_BOUND('',#27248,.T.);
#23148=FACE_OUTER_BOUND('',#27249,.T.);
#23149=FACE_OUTER_BOUND('',#27250,.T.);
#23150=FACE_OUTER_BOUND('',#27251,.T.);
#23151=FACE_OUTER_BOUND('',#27252,.T.);
#23152=FACE_OUTER_BOUND('',#27253,.T.);
#23153=FACE_OUTER_BOUND('',#27254,.T.);
#23154=FACE_OUTER_BOUND('',#27255,.T.);
#23155=FACE_OUTER_BOUND('',#27256,.T.);
#23156=FACE_OUTER_BOUND('',#27257,.T.);
#23157=FACE_OUTER_BOUND('',#27258,.T.);
#23158=FACE_OUTER_BOUND('',#27259,.T.);
#23159=FACE_OUTER_BOUND('',#27260,.T.);
#23160=FACE_OUTER_BOUND('',#27261,.T.);
#23161=FACE_OUTER_BOUND('',#27262,.T.);
#23162=FACE_OUTER_BOUND('',#27263,.T.);
#23163=FACE_OUTER_BOUND('',#27264,.T.);
#23164=FACE_OUTER_BOUND('',#27265,.T.);
#23165=FACE_OUTER_BOUND('',#27266,.T.);
#23166=FACE_OUTER_BOUND('',#27267,.T.);
#23167=FACE_OUTER_BOUND('',#27268,.T.);
#23168=FACE_OUTER_BOUND('',#27269,.T.);
#23169=FACE_OUTER_BOUND('',#27270,.T.);
#23170=FACE_OUTER_BOUND('',#27271,.T.);
#23171=FACE_OUTER_BOUND('',#27272,.T.);
#23172=FACE_OUTER_BOUND('',#27273,.T.);
#23173=FACE_OUTER_BOUND('',#27274,.T.);
#23174=FACE_OUTER_BOUND('',#27275,.T.);
#23175=FACE_OUTER_BOUND('',#27276,.T.);
#23176=FACE_OUTER_BOUND('',#27277,.T.);
#23177=FACE_OUTER_BOUND('',#27278,.T.);
#23178=FACE_OUTER_BOUND('',#27279,.T.);
#23179=FACE_OUTER_BOUND('',#27280,.T.);
#23180=FACE_OUTER_BOUND('',#27281,.T.);
#23181=FACE_OUTER_BOUND('',#27282,.T.);
#23182=FACE_OUTER_BOUND('',#27283,.T.);
#23183=FACE_OUTER_BOUND('',#27284,.T.);
#23184=FACE_OUTER_BOUND('',#27285,.T.);
#23185=FACE_OUTER_BOUND('',#27286,.T.);
#23186=FACE_OUTER_BOUND('',#27287,.T.);
#23187=FACE_OUTER_BOUND('',#27288,.T.);
#23188=FACE_OUTER_BOUND('',#27289,.T.);
#23189=FACE_OUTER_BOUND('',#27290,.T.);
#23190=FACE_OUTER_BOUND('',#27291,.T.);
#23191=FACE_OUTER_BOUND('',#27292,.T.);
#23192=FACE_OUTER_BOUND('',#27293,.T.);
#23193=FACE_OUTER_BOUND('',#27294,.T.);
#23194=FACE_OUTER_BOUND('',#27295,.T.);
#23195=FACE_OUTER_BOUND('',#27296,.T.);
#23196=FACE_OUTER_BOUND('',#27297,.T.);
#23197=FACE_OUTER_BOUND('',#27298,.T.);
#23198=FACE_OUTER_BOUND('',#27299,.T.);
#23199=FACE_OUTER_BOUND('',#27300,.T.);
#23200=FACE_OUTER_BOUND('',#27301,.T.);
#23201=FACE_OUTER_BOUND('',#27302,.T.);
#23202=FACE_OUTER_BOUND('',#27303,.T.);
#23203=FACE_OUTER_BOUND('',#27304,.T.);
#23204=FACE_OUTER_BOUND('',#27305,.T.);
#23205=FACE_OUTER_BOUND('',#27306,.T.);
#23206=FACE_OUTER_BOUND('',#27307,.T.);
#23207=FACE_OUTER_BOUND('',#27308,.T.);
#23208=FACE_OUTER_BOUND('',#27309,.T.);
#23209=FACE_OUTER_BOUND('',#27310,.T.);
#23210=FACE_OUTER_BOUND('',#27311,.T.);
#23211=FACE_OUTER_BOUND('',#27312,.T.);
#23212=FACE_OUTER_BOUND('',#27313,.T.);
#23213=FACE_OUTER_BOUND('',#27314,.T.);
#23214=FACE_OUTER_BOUND('',#27315,.T.);
#23215=FACE_OUTER_BOUND('',#27316,.T.);
#23216=FACE_OUTER_BOUND('',#27317,.T.);
#23217=FACE_OUTER_BOUND('',#27318,.T.);
#23218=FACE_OUTER_BOUND('',#27319,.T.);
#23219=FACE_OUTER_BOUND('',#27320,.T.);
#23220=FACE_OUTER_BOUND('',#27321,.T.);
#23221=FACE_OUTER_BOUND('',#27322,.T.);
#23222=FACE_OUTER_BOUND('',#27323,.T.);
#23223=FACE_OUTER_BOUND('',#27324,.T.);
#23224=FACE_OUTER_BOUND('',#27325,.T.);
#23225=FACE_OUTER_BOUND('',#27326,.T.);
#23226=FACE_OUTER_BOUND('',#27327,.T.);
#23227=FACE_OUTER_BOUND('',#27328,.T.);
#23228=FACE_OUTER_BOUND('',#27329,.T.);
#23229=FACE_OUTER_BOUND('',#27330,.T.);
#23230=FACE_OUTER_BOUND('',#27331,.T.);
#23231=FACE_OUTER_BOUND('',#27332,.T.);
#23232=FACE_OUTER_BOUND('',#27333,.T.);
#23233=FACE_OUTER_BOUND('',#27334,.T.);
#23234=FACE_OUTER_BOUND('',#27335,.T.);
#23235=FACE_OUTER_BOUND('',#27336,.T.);
#23236=FACE_OUTER_BOUND('',#27337,.T.);
#23237=FACE_OUTER_BOUND('',#27338,.T.);
#23238=FACE_OUTER_BOUND('',#27339,.T.);
#23239=FACE_OUTER_BOUND('',#27340,.T.);
#23240=FACE_OUTER_BOUND('',#27341,.T.);
#23241=FACE_OUTER_BOUND('',#27342,.T.);
#23242=FACE_OUTER_BOUND('',#27343,.T.);
#23243=FACE_OUTER_BOUND('',#27344,.T.);
#23244=FACE_OUTER_BOUND('',#27345,.T.);
#23245=FACE_OUTER_BOUND('',#27346,.T.);
#23246=FACE_OUTER_BOUND('',#27347,.T.);
#23247=FACE_OUTER_BOUND('',#27348,.T.);
#23248=FACE_OUTER_BOUND('',#27349,.T.);
#23249=FACE_OUTER_BOUND('',#27350,.T.);
#23250=FACE_OUTER_BOUND('',#27351,.T.);
#23251=FACE_OUTER_BOUND('',#27352,.T.);
#23252=FACE_OUTER_BOUND('',#27353,.T.);
#23253=FACE_OUTER_BOUND('',#27354,.T.);
#23254=FACE_OUTER_BOUND('',#27355,.T.);
#23255=FACE_OUTER_BOUND('',#27356,.T.);
#23256=FACE_OUTER_BOUND('',#27357,.T.);
#23257=FACE_OUTER_BOUND('',#27358,.T.);
#23258=FACE_OUTER_BOUND('',#27359,.T.);
#23259=FACE_OUTER_BOUND('',#27360,.T.);
#23260=FACE_OUTER_BOUND('',#27361,.T.);
#23261=FACE_OUTER_BOUND('',#27362,.T.);
#23262=FACE_OUTER_BOUND('',#27363,.T.);
#23263=FACE_OUTER_BOUND('',#27364,.T.);
#23264=FACE_OUTER_BOUND('',#27365,.T.);
#23265=FACE_OUTER_BOUND('',#27366,.T.);
#23266=FACE_OUTER_BOUND('',#27367,.T.);
#23267=FACE_OUTER_BOUND('',#27368,.T.);
#23268=FACE_OUTER_BOUND('',#27369,.T.);
#23269=FACE_OUTER_BOUND('',#27370,.T.);
#23270=FACE_OUTER_BOUND('',#27371,.T.);
#23271=FACE_OUTER_BOUND('',#27372,.T.);
#23272=FACE_OUTER_BOUND('',#27373,.T.);
#23273=FACE_OUTER_BOUND('',#27374,.T.);
#23274=FACE_OUTER_BOUND('',#27375,.T.);
#23275=FACE_OUTER_BOUND('',#27376,.T.);
#23276=FACE_OUTER_BOUND('',#27377,.T.);
#23277=FACE_OUTER_BOUND('',#27378,.T.);
#23278=FACE_OUTER_BOUND('',#27379,.T.);
#23279=FACE_OUTER_BOUND('',#27380,.T.);
#23280=FACE_OUTER_BOUND('',#27381,.T.);
#23281=FACE_OUTER_BOUND('',#27382,.T.);
#23282=FACE_OUTER_BOUND('',#27383,.T.);
#23283=FACE_OUTER_BOUND('',#27384,.T.);
#23284=FACE_OUTER_BOUND('',#27385,.T.);
#23285=FACE_OUTER_BOUND('',#27386,.T.);
#23286=FACE_OUTER_BOUND('',#27387,.T.);
#23287=FACE_OUTER_BOUND('',#27388,.T.);
#23288=FACE_OUTER_BOUND('',#27389,.T.);
#23289=FACE_OUTER_BOUND('',#27390,.T.);
#23290=FACE_OUTER_BOUND('',#27391,.T.);
#23291=FACE_OUTER_BOUND('',#27392,.T.);
#23292=FACE_OUTER_BOUND('',#27393,.T.);
#23293=FACE_OUTER_BOUND('',#27394,.T.);
#23294=FACE_OUTER_BOUND('',#27395,.T.);
#23295=FACE_OUTER_BOUND('',#27396,.T.);
#23296=FACE_OUTER_BOUND('',#27397,.T.);
#23297=FACE_OUTER_BOUND('',#27398,.T.);
#23298=FACE_OUTER_BOUND('',#27399,.T.);
#23299=FACE_OUTER_BOUND('',#27400,.T.);
#23300=FACE_OUTER_BOUND('',#27401,.T.);
#23301=FACE_OUTER_BOUND('',#27402,.T.);
#23302=FACE_OUTER_BOUND('',#27403,.T.);
#23303=FACE_OUTER_BOUND('',#27404,.T.);
#23304=FACE_OUTER_BOUND('',#27405,.T.);
#23305=FACE_OUTER_BOUND('',#27406,.T.);
#23306=FACE_OUTER_BOUND('',#27407,.T.);
#23307=FACE_OUTER_BOUND('',#27408,.T.);
#23308=FACE_OUTER_BOUND('',#27409,.T.);
#23309=FACE_OUTER_BOUND('',#27410,.T.);
#23310=FACE_OUTER_BOUND('',#27411,.T.);
#23311=FACE_OUTER_BOUND('',#27412,.T.);
#23312=FACE_OUTER_BOUND('',#27413,.T.);
#23313=FACE_OUTER_BOUND('',#27414,.T.);
#23314=FACE_OUTER_BOUND('',#27415,.T.);
#23315=FACE_OUTER_BOUND('',#27416,.T.);
#23316=FACE_OUTER_BOUND('',#27417,.T.);
#23317=FACE_OUTER_BOUND('',#27418,.T.);
#23318=FACE_OUTER_BOUND('',#27419,.T.);
#23319=FACE_OUTER_BOUND('',#27420,.T.);
#23320=FACE_OUTER_BOUND('',#27421,.T.);
#23321=FACE_OUTER_BOUND('',#27422,.T.);
#23322=FACE_OUTER_BOUND('',#27423,.T.);
#23323=FACE_OUTER_BOUND('',#27424,.T.);
#23324=FACE_OUTER_BOUND('',#27425,.T.);
#23325=FACE_OUTER_BOUND('',#27426,.T.);
#23326=FACE_OUTER_BOUND('',#27427,.T.);
#23327=FACE_OUTER_BOUND('',#27428,.T.);
#23328=FACE_OUTER_BOUND('',#27429,.T.);
#23329=FACE_OUTER_BOUND('',#27430,.T.);
#23330=FACE_OUTER_BOUND('',#27431,.T.);
#23331=FACE_OUTER_BOUND('',#27432,.T.);
#23332=FACE_OUTER_BOUND('',#27433,.T.);
#23333=FACE_OUTER_BOUND('',#27434,.T.);
#23334=FACE_OUTER_BOUND('',#27435,.T.);
#23335=FACE_OUTER_BOUND('',#27436,.T.);
#23336=FACE_OUTER_BOUND('',#27437,.T.);
#23337=FACE_OUTER_BOUND('',#27438,.T.);
#23338=FACE_OUTER_BOUND('',#27439,.T.);
#23339=FACE_OUTER_BOUND('',#27440,.T.);
#23340=FACE_OUTER_BOUND('',#27441,.T.);
#23341=FACE_OUTER_BOUND('',#27442,.T.);
#23342=FACE_OUTER_BOUND('',#27443,.T.);
#23343=FACE_OUTER_BOUND('',#27444,.T.);
#23344=FACE_OUTER_BOUND('',#27445,.T.);
#23345=FACE_OUTER_BOUND('',#27446,.T.);
#23346=FACE_OUTER_BOUND('',#27447,.T.);
#23347=FACE_OUTER_BOUND('',#27448,.T.);
#23348=FACE_OUTER_BOUND('',#27449,.T.);
#23349=FACE_OUTER_BOUND('',#27450,.T.);
#23350=FACE_OUTER_BOUND('',#27451,.T.);
#23351=FACE_OUTER_BOUND('',#27452,.T.);
#23352=FACE_OUTER_BOUND('',#27453,.T.);
#23353=FACE_OUTER_BOUND('',#27454,.T.);
#23354=FACE_OUTER_BOUND('',#27455,.T.);
#23355=FACE_OUTER_BOUND('',#27456,.T.);
#23356=FACE_OUTER_BOUND('',#27457,.T.);
#23357=FACE_OUTER_BOUND('',#27458,.T.);
#23358=FACE_OUTER_BOUND('',#27459,.T.);
#23359=FACE_OUTER_BOUND('',#27460,.T.);
#23360=FACE_OUTER_BOUND('',#27461,.T.);
#23361=FACE_OUTER_BOUND('',#27462,.T.);
#23362=FACE_OUTER_BOUND('',#27463,.T.);
#23363=FACE_OUTER_BOUND('',#27464,.T.);
#23364=FACE_OUTER_BOUND('',#27465,.T.);
#23365=FACE_OUTER_BOUND('',#27466,.T.);
#23366=FACE_OUTER_BOUND('',#27467,.T.);
#23367=FACE_OUTER_BOUND('',#27468,.T.);
#23368=FACE_OUTER_BOUND('',#27469,.T.);
#23369=FACE_OUTER_BOUND('',#27470,.T.);
#23370=FACE_OUTER_BOUND('',#27471,.T.);
#23371=FACE_OUTER_BOUND('',#27472,.T.);
#23372=FACE_OUTER_BOUND('',#27473,.T.);
#23373=FACE_OUTER_BOUND('',#27474,.T.);
#23374=FACE_OUTER_BOUND('',#27475,.T.);
#23375=FACE_OUTER_BOUND('',#27476,.T.);
#23376=FACE_OUTER_BOUND('',#27477,.T.);
#23377=FACE_OUTER_BOUND('',#27478,.T.);
#23378=FACE_OUTER_BOUND('',#27479,.T.);
#23379=FACE_OUTER_BOUND('',#27480,.T.);
#23380=FACE_OUTER_BOUND('',#27481,.T.);
#23381=FACE_OUTER_BOUND('',#27482,.T.);
#23382=FACE_OUTER_BOUND('',#27483,.T.);
#23383=FACE_OUTER_BOUND('',#27484,.T.);
#23384=FACE_OUTER_BOUND('',#27485,.T.);
#23385=FACE_OUTER_BOUND('',#27486,.T.);
#23386=FACE_OUTER_BOUND('',#27487,.T.);
#23387=FACE_OUTER_BOUND('',#27488,.T.);
#23388=FACE_OUTER_BOUND('',#27489,.T.);
#23389=FACE_OUTER_BOUND('',#27490,.T.);
#23390=FACE_OUTER_BOUND('',#27491,.T.);
#23391=FACE_OUTER_BOUND('',#27492,.T.);
#23392=FACE_OUTER_BOUND('',#27493,.T.);
#23393=FACE_OUTER_BOUND('',#27494,.T.);
#23394=FACE_OUTER_BOUND('',#27495,.T.);
#23395=FACE_OUTER_BOUND('',#27496,.T.);
#23396=FACE_OUTER_BOUND('',#27497,.T.);
#23397=FACE_OUTER_BOUND('',#27498,.T.);
#23398=FACE_OUTER_BOUND('',#27499,.T.);
#23399=FACE_OUTER_BOUND('',#27500,.T.);
#23400=FACE_OUTER_BOUND('',#27501,.T.);
#23401=FACE_OUTER_BOUND('',#27502,.T.);
#23402=FACE_OUTER_BOUND('',#27503,.T.);
#23403=FACE_OUTER_BOUND('',#27504,.T.);
#23404=FACE_OUTER_BOUND('',#27505,.T.);
#23405=FACE_OUTER_BOUND('',#27506,.T.);
#23406=FACE_OUTER_BOUND('',#27507,.T.);
#23407=FACE_OUTER_BOUND('',#27508,.T.);
#23408=FACE_OUTER_BOUND('',#27509,.T.);
#23409=FACE_OUTER_BOUND('',#27510,.T.);
#23410=FACE_OUTER_BOUND('',#27511,.T.);
#23411=FACE_OUTER_BOUND('',#27512,.T.);
#23412=FACE_OUTER_BOUND('',#27513,.T.);
#23413=FACE_OUTER_BOUND('',#27514,.T.);
#23414=FACE_OUTER_BOUND('',#27515,.T.);
#23415=FACE_OUTER_BOUND('',#27516,.T.);
#23416=FACE_OUTER_BOUND('',#27517,.T.);
#23417=FACE_OUTER_BOUND('',#27518,.T.);
#23418=FACE_OUTER_BOUND('',#27519,.T.);
#23419=FACE_OUTER_BOUND('',#27520,.T.);
#23420=FACE_OUTER_BOUND('',#27521,.T.);
#23421=FACE_OUTER_BOUND('',#27522,.T.);
#23422=FACE_OUTER_BOUND('',#27523,.T.);
#23423=FACE_OUTER_BOUND('',#27524,.T.);
#23424=FACE_OUTER_BOUND('',#27525,.T.);
#23425=FACE_OUTER_BOUND('',#27526,.T.);
#23426=FACE_OUTER_BOUND('',#27527,.T.);
#23427=FACE_OUTER_BOUND('',#27528,.T.);
#23428=FACE_OUTER_BOUND('',#27529,.T.);
#23429=FACE_OUTER_BOUND('',#27530,.T.);
#23430=FACE_OUTER_BOUND('',#27531,.T.);
#23431=FACE_OUTER_BOUND('',#27532,.T.);
#23432=FACE_OUTER_BOUND('',#27533,.T.);
#23433=FACE_OUTER_BOUND('',#27534,.T.);
#23434=FACE_OUTER_BOUND('',#27535,.T.);
#23435=FACE_OUTER_BOUND('',#27536,.T.);
#23436=FACE_OUTER_BOUND('',#27537,.T.);
#23437=FACE_OUTER_BOUND('',#27538,.T.);
#23438=FACE_OUTER_BOUND('',#27539,.T.);
#23439=FACE_OUTER_BOUND('',#27540,.T.);
#23440=FACE_OUTER_BOUND('',#27541,.T.);
#23441=FACE_OUTER_BOUND('',#27542,.T.);
#23442=FACE_OUTER_BOUND('',#27543,.T.);
#23443=FACE_OUTER_BOUND('',#27544,.T.);
#23444=FACE_OUTER_BOUND('',#27545,.T.);
#23445=FACE_OUTER_BOUND('',#27546,.T.);
#23446=FACE_OUTER_BOUND('',#27547,.T.);
#23447=FACE_OUTER_BOUND('',#27548,.T.);
#23448=FACE_OUTER_BOUND('',#27549,.T.);
#23449=FACE_OUTER_BOUND('',#27550,.T.);
#23450=FACE_OUTER_BOUND('',#27551,.T.);
#23451=FACE_OUTER_BOUND('',#27552,.T.);
#23452=FACE_OUTER_BOUND('',#27553,.T.);
#23453=FACE_OUTER_BOUND('',#27554,.T.);
#23454=FACE_OUTER_BOUND('',#27555,.T.);
#23455=FACE_OUTER_BOUND('',#27556,.T.);
#23456=FACE_OUTER_BOUND('',#27557,.T.);
#23457=FACE_OUTER_BOUND('',#27558,.T.);
#23458=FACE_OUTER_BOUND('',#27559,.T.);
#23459=FACE_OUTER_BOUND('',#27560,.T.);
#23460=FACE_OUTER_BOUND('',#27561,.T.);
#23461=FACE_OUTER_BOUND('',#27562,.T.);
#23462=FACE_OUTER_BOUND('',#27563,.T.);
#23463=FACE_OUTER_BOUND('',#27564,.T.);
#23464=FACE_OUTER_BOUND('',#27565,.T.);
#23465=FACE_OUTER_BOUND('',#27566,.T.);
#23466=FACE_OUTER_BOUND('',#27567,.T.);
#23467=FACE_OUTER_BOUND('',#27568,.T.);
#23468=FACE_OUTER_BOUND('',#27569,.T.);
#23469=FACE_OUTER_BOUND('',#27570,.T.);
#23470=FACE_OUTER_BOUND('',#27571,.T.);
#23471=FACE_OUTER_BOUND('',#27572,.T.);
#23472=FACE_OUTER_BOUND('',#27573,.T.);
#23473=FACE_OUTER_BOUND('',#27574,.T.);
#23474=FACE_OUTER_BOUND('',#27575,.T.);
#23475=FACE_OUTER_BOUND('',#27576,.T.);
#23476=FACE_OUTER_BOUND('',#27577,.T.);
#23477=FACE_OUTER_BOUND('',#27578,.T.);
#23478=FACE_OUTER_BOUND('',#27579,.T.);
#23479=FACE_OUTER_BOUND('',#27580,.T.);
#23480=FACE_OUTER_BOUND('',#27581,.T.);
#23481=FACE_OUTER_BOUND('',#27582,.T.);
#23482=FACE_OUTER_BOUND('',#27583,.T.);
#23483=FACE_OUTER_BOUND('',#27584,.T.);
#23484=FACE_OUTER_BOUND('',#27585,.T.);
#23485=FACE_OUTER_BOUND('',#27586,.T.);
#23486=FACE_OUTER_BOUND('',#27587,.T.);
#23487=FACE_OUTER_BOUND('',#27588,.T.);
#23488=FACE_OUTER_BOUND('',#27589,.T.);
#23489=FACE_OUTER_BOUND('',#27590,.T.);
#23490=FACE_OUTER_BOUND('',#27591,.T.);
#23491=FACE_OUTER_BOUND('',#27592,.T.);
#23492=FACE_OUTER_BOUND('',#27593,.T.);
#23493=FACE_OUTER_BOUND('',#27594,.T.);
#23494=FACE_OUTER_BOUND('',#27595,.T.);
#23495=FACE_OUTER_BOUND('',#27596,.T.);
#23496=FACE_OUTER_BOUND('',#27597,.T.);
#23497=FACE_OUTER_BOUND('',#27598,.T.);
#23498=FACE_OUTER_BOUND('',#27599,.T.);
#23499=FACE_OUTER_BOUND('',#27600,.T.);
#23500=FACE_OUTER_BOUND('',#27601,.T.);
#23501=FACE_OUTER_BOUND('',#27602,.T.);
#23502=FACE_OUTER_BOUND('',#27603,.T.);
#23503=FACE_OUTER_BOUND('',#27604,.T.);
#23504=FACE_OUTER_BOUND('',#27605,.T.);
#23505=FACE_OUTER_BOUND('',#27606,.T.);
#23506=FACE_OUTER_BOUND('',#27607,.T.);
#23507=FACE_OUTER_BOUND('',#27608,.T.);
#23508=FACE_OUTER_BOUND('',#27609,.T.);
#23509=FACE_OUTER_BOUND('',#27610,.T.);
#23510=FACE_OUTER_BOUND('',#27611,.T.);
#23511=FACE_OUTER_BOUND('',#27612,.T.);
#23512=FACE_OUTER_BOUND('',#27613,.T.);
#23513=FACE_OUTER_BOUND('',#27614,.T.);
#23514=FACE_OUTER_BOUND('',#27615,.T.);
#23515=FACE_OUTER_BOUND('',#27616,.T.);
#23516=FACE_OUTER_BOUND('',#27617,.T.);
#23517=FACE_OUTER_BOUND('',#27618,.T.);
#23518=FACE_OUTER_BOUND('',#27619,.T.);
#23519=FACE_OUTER_BOUND('',#27620,.T.);
#23520=FACE_OUTER_BOUND('',#27621,.T.);
#23521=FACE_OUTER_BOUND('',#27622,.T.);
#23522=FACE_OUTER_BOUND('',#27623,.T.);
#23523=FACE_OUTER_BOUND('',#27624,.T.);
#23524=FACE_OUTER_BOUND('',#27625,.T.);
#23525=FACE_OUTER_BOUND('',#27626,.T.);
#23526=FACE_OUTER_BOUND('',#27627,.T.);
#23527=FACE_OUTER_BOUND('',#27628,.T.);
#23528=FACE_OUTER_BOUND('',#27629,.T.);
#23529=FACE_OUTER_BOUND('',#27630,.T.);
#23530=FACE_OUTER_BOUND('',#27631,.T.);
#23531=FACE_OUTER_BOUND('',#27632,.T.);
#23532=FACE_OUTER_BOUND('',#27633,.T.);
#23533=FACE_OUTER_BOUND('',#27634,.T.);
#23534=FACE_OUTER_BOUND('',#27635,.T.);
#23535=FACE_OUTER_BOUND('',#27636,.T.);
#23536=FACE_OUTER_BOUND('',#27637,.T.);
#23537=FACE_OUTER_BOUND('',#27638,.T.);
#23538=FACE_OUTER_BOUND('',#27639,.T.);
#23539=FACE_OUTER_BOUND('',#27640,.T.);
#23540=FACE_OUTER_BOUND('',#27641,.T.);
#23541=FACE_OUTER_BOUND('',#27642,.T.);
#23542=FACE_OUTER_BOUND('',#27643,.T.);
#23543=FACE_OUTER_BOUND('',#27644,.T.);
#23544=FACE_OUTER_BOUND('',#27645,.T.);
#23545=FACE_OUTER_BOUND('',#27646,.T.);
#23546=FACE_OUTER_BOUND('',#27647,.T.);
#23547=FACE_OUTER_BOUND('',#27648,.T.);
#23548=FACE_OUTER_BOUND('',#27649,.T.);
#23549=FACE_OUTER_BOUND('',#27650,.T.);
#23550=FACE_OUTER_BOUND('',#27651,.T.);
#23551=FACE_OUTER_BOUND('',#27652,.T.);
#23552=FACE_OUTER_BOUND('',#27653,.T.);
#23553=FACE_OUTER_BOUND('',#27654,.T.);
#23554=FACE_OUTER_BOUND('',#27655,.T.);
#23555=FACE_OUTER_BOUND('',#27656,.T.);
#23556=FACE_OUTER_BOUND('',#27657,.T.);
#23557=FACE_OUTER_BOUND('',#27658,.T.);
#23558=FACE_OUTER_BOUND('',#27659,.T.);
#23559=FACE_OUTER_BOUND('',#27660,.T.);
#23560=FACE_OUTER_BOUND('',#27661,.T.);
#23561=FACE_OUTER_BOUND('',#27662,.T.);
#23562=FACE_OUTER_BOUND('',#27663,.T.);
#23563=FACE_OUTER_BOUND('',#27664,.T.);
#23564=FACE_OUTER_BOUND('',#27665,.T.);
#23565=FACE_OUTER_BOUND('',#27666,.T.);
#23566=FACE_OUTER_BOUND('',#27667,.T.);
#23567=FACE_OUTER_BOUND('',#27668,.T.);
#23568=FACE_OUTER_BOUND('',#27669,.T.);
#23569=FACE_OUTER_BOUND('',#27670,.T.);
#23570=FACE_OUTER_BOUND('',#27671,.T.);
#23571=FACE_OUTER_BOUND('',#27672,.T.);
#23572=FACE_OUTER_BOUND('',#27673,.T.);
#23573=FACE_OUTER_BOUND('',#27674,.T.);
#23574=FACE_OUTER_BOUND('',#27675,.T.);
#23575=FACE_OUTER_BOUND('',#27676,.T.);
#23576=FACE_OUTER_BOUND('',#27677,.T.);
#23577=FACE_OUTER_BOUND('',#27678,.T.);
#23578=FACE_OUTER_BOUND('',#27679,.T.);
#23579=FACE_OUTER_BOUND('',#27680,.T.);
#23580=FACE_OUTER_BOUND('',#27681,.T.);
#23581=FACE_OUTER_BOUND('',#27682,.T.);
#23582=FACE_OUTER_BOUND('',#27683,.T.);
#23583=FACE_OUTER_BOUND('',#27684,.T.);
#23584=FACE_OUTER_BOUND('',#27685,.T.);
#23585=FACE_OUTER_BOUND('',#27686,.T.);
#23586=FACE_OUTER_BOUND('',#27687,.T.);
#23587=FACE_OUTER_BOUND('',#27688,.T.);
#23588=FACE_OUTER_BOUND('',#27689,.T.);
#23589=FACE_OUTER_BOUND('',#27690,.T.);
#23590=FACE_OUTER_BOUND('',#27691,.T.);
#23591=FACE_OUTER_BOUND('',#27692,.T.);
#23592=FACE_OUTER_BOUND('',#27693,.T.);
#23593=FACE_OUTER_BOUND('',#27694,.T.);
#23594=FACE_OUTER_BOUND('',#27695,.T.);
#23595=FACE_OUTER_BOUND('',#27696,.T.);
#23596=FACE_OUTER_BOUND('',#27697,.T.);
#23597=FACE_OUTER_BOUND('',#27698,.T.);
#23598=FACE_OUTER_BOUND('',#27699,.T.);
#23599=FACE_OUTER_BOUND('',#27700,.T.);
#23600=FACE_OUTER_BOUND('',#27701,.T.);
#23601=FACE_OUTER_BOUND('',#27702,.T.);
#23602=FACE_OUTER_BOUND('',#27703,.T.);
#23603=FACE_OUTER_BOUND('',#27704,.T.);
#23604=FACE_OUTER_BOUND('',#27705,.T.);
#23605=FACE_OUTER_BOUND('',#27706,.T.);
#23606=FACE_OUTER_BOUND('',#27707,.T.);
#23607=FACE_OUTER_BOUND('',#27708,.T.);
#23608=FACE_OUTER_BOUND('',#27709,.T.);
#23609=FACE_OUTER_BOUND('',#27710,.T.);
#23610=FACE_OUTER_BOUND('',#27711,.T.);
#23611=FACE_OUTER_BOUND('',#27712,.T.);
#23612=FACE_OUTER_BOUND('',#27713,.T.);
#23613=FACE_OUTER_BOUND('',#27714,.T.);
#23614=FACE_OUTER_BOUND('',#27715,.T.);
#23615=FACE_OUTER_BOUND('',#27716,.T.);
#23616=FACE_OUTER_BOUND('',#27717,.T.);
#23617=FACE_OUTER_BOUND('',#27718,.T.);
#23618=FACE_OUTER_BOUND('',#27719,.T.);
#23619=FACE_OUTER_BOUND('',#27720,.T.);
#23620=FACE_OUTER_BOUND('',#27721,.T.);
#23621=FACE_OUTER_BOUND('',#27722,.T.);
#23622=FACE_OUTER_BOUND('',#27723,.T.);
#23623=FACE_OUTER_BOUND('',#27724,.T.);
#23624=FACE_OUTER_BOUND('',#27725,.T.);
#23625=FACE_OUTER_BOUND('',#27726,.T.);
#23626=FACE_OUTER_BOUND('',#27727,.T.);
#23627=FACE_OUTER_BOUND('',#27728,.T.);
#23628=FACE_OUTER_BOUND('',#27729,.T.);
#23629=FACE_OUTER_BOUND('',#27730,.T.);
#23630=FACE_OUTER_BOUND('',#27731,.T.);
#23631=FACE_OUTER_BOUND('',#27732,.T.);
#23632=FACE_OUTER_BOUND('',#27733,.T.);
#23633=FACE_OUTER_BOUND('',#27734,.T.);
#23634=FACE_OUTER_BOUND('',#27735,.T.);
#23635=FACE_OUTER_BOUND('',#27736,.T.);
#23636=FACE_OUTER_BOUND('',#27737,.T.);
#23637=FACE_OUTER_BOUND('',#27738,.T.);
#23638=FACE_OUTER_BOUND('',#27739,.T.);
#23639=FACE_OUTER_BOUND('',#27740,.T.);
#23640=FACE_OUTER_BOUND('',#27741,.T.);
#23641=FACE_OUTER_BOUND('',#27742,.T.);
#23642=FACE_OUTER_BOUND('',#27743,.T.);
#23643=FACE_OUTER_BOUND('',#27744,.T.);
#23644=FACE_OUTER_BOUND('',#27745,.T.);
#23645=FACE_OUTER_BOUND('',#27746,.T.);
#23646=FACE_OUTER_BOUND('',#27747,.T.);
#23647=FACE_OUTER_BOUND('',#27748,.T.);
#23648=FACE_OUTER_BOUND('',#27749,.T.);
#23649=FACE_OUTER_BOUND('',#27750,.T.);
#23650=FACE_OUTER_BOUND('',#27751,.T.);
#23651=FACE_OUTER_BOUND('',#27752,.T.);
#23652=FACE_OUTER_BOUND('',#27753,.T.);
#23653=FACE_OUTER_BOUND('',#27754,.T.);
#23654=FACE_OUTER_BOUND('',#27755,.T.);
#23655=FACE_OUTER_BOUND('',#27756,.T.);
#23656=FACE_OUTER_BOUND('',#27757,.T.);
#23657=FACE_OUTER_BOUND('',#27758,.T.);
#23658=FACE_OUTER_BOUND('',#27759,.T.);
#23659=FACE_OUTER_BOUND('',#27760,.T.);
#23660=FACE_OUTER_BOUND('',#27761,.T.);
#23661=FACE_OUTER_BOUND('',#27762,.T.);
#23662=FACE_OUTER_BOUND('',#27763,.T.);
#23663=FACE_OUTER_BOUND('',#27764,.T.);
#23664=FACE_OUTER_BOUND('',#27765,.T.);
#23665=FACE_OUTER_BOUND('',#27766,.T.);
#23666=FACE_OUTER_BOUND('',#27767,.T.);
#23667=FACE_OUTER_BOUND('',#27768,.T.);
#23668=FACE_OUTER_BOUND('',#27769,.T.);
#23669=FACE_OUTER_BOUND('',#27770,.T.);
#23670=FACE_OUTER_BOUND('',#27771,.T.);
#23671=FACE_OUTER_BOUND('',#27772,.T.);
#23672=FACE_OUTER_BOUND('',#27773,.T.);
#23673=FACE_OUTER_BOUND('',#27774,.T.);
#23674=FACE_OUTER_BOUND('',#27775,.T.);
#23675=FACE_OUTER_BOUND('',#27776,.T.);
#23676=FACE_OUTER_BOUND('',#27777,.T.);
#23677=FACE_OUTER_BOUND('',#27778,.T.);
#23678=FACE_OUTER_BOUND('',#27779,.T.);
#23679=FACE_OUTER_BOUND('',#27780,.T.);
#23680=FACE_OUTER_BOUND('',#27781,.T.);
#23681=FACE_OUTER_BOUND('',#27782,.T.);
#23682=FACE_OUTER_BOUND('',#27783,.T.);
#23683=FACE_OUTER_BOUND('',#27784,.T.);
#23684=FACE_OUTER_BOUND('',#27785,.T.);
#23685=FACE_OUTER_BOUND('',#27786,.T.);
#23686=FACE_OUTER_BOUND('',#27787,.T.);
#23687=FACE_OUTER_BOUND('',#27788,.T.);
#23688=FACE_OUTER_BOUND('',#27789,.T.);
#23689=FACE_OUTER_BOUND('',#27790,.T.);
#23690=FACE_OUTER_BOUND('',#27791,.T.);
#23691=FACE_OUTER_BOUND('',#27792,.T.);
#23692=FACE_OUTER_BOUND('',#27793,.T.);
#23693=FACE_OUTER_BOUND('',#27794,.T.);
#23694=FACE_OUTER_BOUND('',#27795,.T.);
#23695=FACE_OUTER_BOUND('',#27796,.T.);
#23696=FACE_OUTER_BOUND('',#27797,.T.);
#23697=FACE_OUTER_BOUND('',#27798,.T.);
#23698=FACE_OUTER_BOUND('',#27799,.T.);
#23699=FACE_OUTER_BOUND('',#27800,.T.);
#23700=FACE_OUTER_BOUND('',#27801,.T.);
#23701=FACE_OUTER_BOUND('',#27803,.T.);
#23702=FACE_OUTER_BOUND('',#28241,.T.);
#23703=FACE_OUTER_BOUND('',#28242,.T.);
#23704=FACE_OUTER_BOUND('',#28243,.T.);
#23705=FACE_OUTER_BOUND('',#28244,.T.);
#23706=FACE_OUTER_BOUND('',#28245,.T.);
#23707=FACE_OUTER_BOUND('',#28683,.T.);
#23708=FACE_OUTER_BOUND('',#28685,.T.);
#23709=FACE_OUTER_BOUND('',#28686,.T.);
#23710=FACE_OUTER_BOUND('',#28687,.T.);
#23711=FACE_OUTER_BOUND('',#28688,.T.);
#23712=FACE_OUTER_BOUND('',#28689,.T.);
#23713=FACE_OUTER_BOUND('',#28690,.T.);
#23714=FACE_OUTER_BOUND('',#28691,.T.);
#23715=FACE_OUTER_BOUND('',#28692,.T.);
#23716=FACE_OUTER_BOUND('',#28693,.T.);
#23717=FACE_OUTER_BOUND('',#28694,.T.);
#23718=FACE_OUTER_BOUND('',#28695,.T.);
#23719=FACE_OUTER_BOUND('',#28696,.T.);
#23720=FACE_OUTER_BOUND('',#28697,.T.);
#23721=FACE_OUTER_BOUND('',#28699,.T.);
#23722=FACE_OUTER_BOUND('',#28956,.T.);
#23723=FACE_OUTER_BOUND('',#28957,.T.);
#23724=FACE_OUTER_BOUND('',#28958,.T.);
#23725=FACE_OUTER_BOUND('',#28959,.T.);
#23726=FACE_OUTER_BOUND('',#28960,.T.);
#23727=FACE_OUTER_BOUND('',#29217,.T.);
#23728=FACE_OUTER_BOUND('',#29219,.T.);
#23729=FACE_OUTER_BOUND('',#29220,.T.);
#23730=FACE_OUTER_BOUND('',#29221,.T.);
#23731=FACE_OUTER_BOUND('',#29222,.T.);
#23732=FACE_OUTER_BOUND('',#29223,.T.);
#23733=FACE_OUTER_BOUND('',#29224,.T.);
#23734=FACE_OUTER_BOUND('',#29225,.T.);
#23735=FACE_OUTER_BOUND('',#29226,.T.);
#23736=FACE_OUTER_BOUND('',#29227,.T.);
#23737=FACE_OUTER_BOUND('',#29228,.T.);
#23738=FACE_OUTER_BOUND('',#29229,.T.);
#23739=FACE_OUTER_BOUND('',#29230,.T.);
#23740=FACE_OUTER_BOUND('',#29231,.T.);
#23741=FACE_OUTER_BOUND('',#29232,.T.);
#23742=FACE_OUTER_BOUND('',#29233,.T.);
#23743=FACE_OUTER_BOUND('',#29234,.T.);
#23744=FACE_OUTER_BOUND('',#29235,.T.);
#23745=FACE_OUTER_BOUND('',#29236,.T.);
#23746=FACE_OUTER_BOUND('',#29237,.T.);
#23747=FACE_OUTER_BOUND('',#29238,.T.);
#23748=FACE_OUTER_BOUND('',#29239,.T.);
#23749=FACE_OUTER_BOUND('',#29240,.T.);
#23750=FACE_OUTER_BOUND('',#29241,.T.);
#23751=FACE_OUTER_BOUND('',#29242,.T.);
#23752=FACE_OUTER_BOUND('',#29243,.T.);
#23753=FACE_OUTER_BOUND('',#29244,.T.);
#23754=FACE_OUTER_BOUND('',#29245,.T.);
#23755=FACE_OUTER_BOUND('',#29246,.T.);
#23756=FACE_OUTER_BOUND('',#29247,.T.);
#23757=FACE_OUTER_BOUND('',#29248,.T.);
#23758=FACE_OUTER_BOUND('',#29249,.T.);
#23759=FACE_OUTER_BOUND('',#29250,.T.);
#23760=FACE_OUTER_BOUND('',#29251,.T.);
#23761=FACE_OUTER_BOUND('',#29252,.T.);
#23762=FACE_OUTER_BOUND('',#29253,.T.);
#23763=FACE_OUTER_BOUND('',#29254,.T.);
#23764=FACE_OUTER_BOUND('',#29255,.T.);
#23765=FACE_OUTER_BOUND('',#29256,.T.);
#23766=FACE_OUTER_BOUND('',#29257,.T.);
#23767=FACE_OUTER_BOUND('',#29258,.T.);
#23768=FACE_OUTER_BOUND('',#29259,.T.);
#23769=FACE_OUTER_BOUND('',#29260,.T.);
#23770=FACE_OUTER_BOUND('',#29261,.T.);
#23771=FACE_OUTER_BOUND('',#29262,.T.);
#23772=FACE_OUTER_BOUND('',#29263,.T.);
#23773=FACE_OUTER_BOUND('',#29264,.T.);
#23774=FACE_OUTER_BOUND('',#29265,.T.);
#23775=FACE_OUTER_BOUND('',#29266,.T.);
#23776=FACE_OUTER_BOUND('',#29267,.T.);
#23777=FACE_OUTER_BOUND('',#29268,.T.);
#23778=FACE_OUTER_BOUND('',#29269,.T.);
#23779=FACE_OUTER_BOUND('',#29270,.T.);
#23780=FACE_OUTER_BOUND('',#29271,.T.);
#23781=FACE_OUTER_BOUND('',#29272,.T.);
#23782=FACE_OUTER_BOUND('',#29273,.T.);
#23783=FACE_OUTER_BOUND('',#29274,.T.);
#23784=FACE_OUTER_BOUND('',#29275,.T.);
#23785=FACE_OUTER_BOUND('',#29276,.T.);
#23786=FACE_OUTER_BOUND('',#29277,.T.);
#23787=FACE_OUTER_BOUND('',#29278,.T.);
#23788=FACE_OUTER_BOUND('',#29279,.T.);
#23789=FACE_OUTER_BOUND('',#29280,.T.);
#23790=FACE_OUTER_BOUND('',#29281,.T.);
#23791=FACE_OUTER_BOUND('',#29282,.T.);
#23792=FACE_OUTER_BOUND('',#29283,.T.);
#23793=FACE_OUTER_BOUND('',#29284,.T.);
#23794=FACE_OUTER_BOUND('',#29285,.T.);
#23795=FACE_OUTER_BOUND('',#29286,.T.);
#23796=FACE_OUTER_BOUND('',#29287,.T.);
#23797=FACE_OUTER_BOUND('',#29288,.T.);
#23798=FACE_OUTER_BOUND('',#29290,.T.);
#23799=FACE_OUTER_BOUND('',#29292,.T.);
#23800=FACE_OUTER_BOUND('',#29294,.T.);
#23801=FACE_OUTER_BOUND('',#29295,.T.);
#23802=FACE_OUTER_BOUND('',#29296,.T.);
#23803=FACE_OUTER_BOUND('',#29298,.T.);
#23804=FACE_OUTER_BOUND('',#29299,.T.);
#23805=FACE_OUTER_BOUND('',#29300,.T.);
#23806=FACE_OUTER_BOUND('',#29301,.T.);
#23807=FACE_OUTER_BOUND('',#29302,.T.);
#23808=FACE_OUTER_BOUND('',#29303,.T.);
#23809=FACE_OUTER_BOUND('',#29304,.T.);
#23810=FACE_OUTER_BOUND('',#29305,.T.);
#23811=FACE_OUTER_BOUND('',#29306,.T.);
#23812=FACE_OUTER_BOUND('',#29307,.T.);
#23813=FACE_OUTER_BOUND('',#29308,.T.);
#23814=FACE_OUTER_BOUND('',#29309,.T.);
#23815=FACE_OUTER_BOUND('',#29310,.T.);
#23816=FACE_OUTER_BOUND('',#29311,.T.);
#23817=FACE_OUTER_BOUND('',#29312,.T.);
#23818=FACE_OUTER_BOUND('',#29313,.T.);
#23819=FACE_OUTER_BOUND('',#29314,.T.);
#23820=FACE_OUTER_BOUND('',#29315,.T.);
#23821=FACE_OUTER_BOUND('',#29316,.T.);
#23822=FACE_OUTER_BOUND('',#29317,.T.);
#23823=FACE_OUTER_BOUND('',#29318,.T.);
#23824=FACE_OUTER_BOUND('',#29319,.T.);
#23825=FACE_OUTER_BOUND('',#29320,.T.);
#23826=FACE_OUTER_BOUND('',#29321,.T.);
#23827=FACE_OUTER_BOUND('',#29322,.T.);
#23828=FACE_OUTER_BOUND('',#29323,.T.);
#23829=FACE_OUTER_BOUND('',#29324,.T.);
#23830=FACE_OUTER_BOUND('',#29325,.T.);
#23831=FACE_OUTER_BOUND('',#29326,.T.);
#23832=FACE_OUTER_BOUND('',#29327,.T.);
#23833=FACE_OUTER_BOUND('',#29328,.T.);
#23834=FACE_OUTER_BOUND('',#29329,.T.);
#23835=FACE_OUTER_BOUND('',#29330,.T.);
#23836=FACE_OUTER_BOUND('',#29331,.T.);
#23837=FACE_OUTER_BOUND('',#29332,.T.);
#23838=FACE_OUTER_BOUND('',#29333,.T.);
#23839=FACE_OUTER_BOUND('',#29334,.T.);
#23840=FACE_OUTER_BOUND('',#29335,.T.);
#23841=FACE_OUTER_BOUND('',#29336,.T.);
#23842=FACE_OUTER_BOUND('',#29337,.T.);
#23843=FACE_OUTER_BOUND('',#29338,.T.);
#23844=FACE_OUTER_BOUND('',#29339,.T.);
#23845=FACE_OUTER_BOUND('',#29340,.T.);
#23846=FACE_OUTER_BOUND('',#29341,.T.);
#23847=FACE_OUTER_BOUND('',#29342,.T.);
#23848=FACE_OUTER_BOUND('',#29343,.T.);
#23849=FACE_OUTER_BOUND('',#29344,.T.);
#23850=FACE_OUTER_BOUND('',#29345,.T.);
#23851=FACE_OUTER_BOUND('',#29346,.T.);
#23852=FACE_OUTER_BOUND('',#29347,.T.);
#23853=FACE_OUTER_BOUND('',#29348,.T.);
#23854=FACE_OUTER_BOUND('',#29349,.T.);
#23855=FACE_OUTER_BOUND('',#29350,.T.);
#23856=FACE_OUTER_BOUND('',#29351,.T.);
#23857=FACE_OUTER_BOUND('',#29352,.T.);
#23858=FACE_OUTER_BOUND('',#29353,.T.);
#23859=FACE_OUTER_BOUND('',#29354,.T.);
#23860=FACE_OUTER_BOUND('',#29355,.T.);
#23861=FACE_OUTER_BOUND('',#29356,.T.);
#23862=FACE_OUTER_BOUND('',#29357,.T.);
#23863=FACE_OUTER_BOUND('',#29358,.T.);
#23864=FACE_OUTER_BOUND('',#29359,.T.);
#23865=FACE_OUTER_BOUND('',#29360,.T.);
#23866=FACE_OUTER_BOUND('',#29361,.T.);
#23867=FACE_OUTER_BOUND('',#29362,.T.);
#23868=FACE_OUTER_BOUND('',#29363,.T.);
#23869=FACE_OUTER_BOUND('',#29364,.T.);
#23870=FACE_OUTER_BOUND('',#29365,.T.);
#23871=FACE_OUTER_BOUND('',#29366,.T.);
#23872=FACE_OUTER_BOUND('',#29367,.T.);
#23873=FACE_OUTER_BOUND('',#29368,.T.);
#23874=FACE_OUTER_BOUND('',#29369,.T.);
#23875=FACE_OUTER_BOUND('',#29370,.T.);
#23876=FACE_OUTER_BOUND('',#29371,.T.);
#23877=FACE_OUTER_BOUND('',#29372,.T.);
#23878=FACE_OUTER_BOUND('',#29374,.T.);
#23879=FACE_OUTER_BOUND('',#29376,.T.);
#23880=FACE_OUTER_BOUND('',#29378,.T.);
#23881=FACE_OUTER_BOUND('',#29379,.T.);
#23882=FACE_OUTER_BOUND('',#29380,.T.);
#23883=FACE_OUTER_BOUND('',#29382,.T.);
#23884=FACE_OUTER_BOUND('',#29383,.T.);
#23885=FACE_OUTER_BOUND('',#29384,.T.);
#23886=FACE_OUTER_BOUND('',#29385,.T.);
#23887=FACE_OUTER_BOUND('',#29386,.T.);
#23888=EDGE_LOOP('',(#52473,#52474,#52475,#52476));
#23889=EDGE_LOOP('',(#52477,#52478,#52479));
#23890=EDGE_LOOP('',(#52480,#52481,#52482));
#23891=EDGE_LOOP('',(#52483,#52484,#52485));
#23892=EDGE_LOOP('',(#52486,#52487,#52488,#52489));
#23893=EDGE_LOOP('',(#52490,#52491,#52492));
#23894=EDGE_LOOP('',(#52493,#52494,#52495,#52496,#52497,#52498));
#23895=EDGE_LOOP('',(#52499,#52500,#52501,#52502));
#23896=EDGE_LOOP('',(#52503,#52504,#52505));
#23897=EDGE_LOOP('',(#52506,#52507,#52508));
#23898=EDGE_LOOP('',(#52509,#52510,#52511,#52512));
#23899=EDGE_LOOP('',(#52513,#52514,#52515));
#23900=EDGE_LOOP('',(#52516,#52517,#52518));
#23901=EDGE_LOOP('',(#52519,#52520,#52521,#52522,#52523,#52524));
#23902=EDGE_LOOP('',(#52525,#52526,#52527,#52528,#52529,#52530,#52531));
#23903=EDGE_LOOP('',(#52532,#52533,#52534,#52535));
#23904=EDGE_LOOP('',(#52536,#52537,#52538));
#23905=EDGE_LOOP('',(#52539,#52540,#52541,#52542));
#23906=EDGE_LOOP('',(#52543,#52544,#52545,#52546));
#23907=EDGE_LOOP('',(#52547,#52548,#52549,#52550));
#23908=EDGE_LOOP('',(#52551,#52552,#52553));
#23909=EDGE_LOOP('',(#52554,#52555,#52556,#52557));
#23910=EDGE_LOOP('',(#52558,#52559,#52560,#52561));
#23911=EDGE_LOOP('',(#52562,#52563,#52564));
#23912=EDGE_LOOP('',(#52565,#52566,#52567,#52568,#52569,#52570,#52571));
#23913=EDGE_LOOP('',(#52572,#52573,#52574));
#23914=EDGE_LOOP('',(#52575,#52576,#52577,#52578));
#23915=EDGE_LOOP('',(#52579,#52580,#52581,#52582));
#23916=EDGE_LOOP('',(#52583,#52584,#52585,#52586));
#23917=EDGE_LOOP('',(#52587,#52588,#52589,#52590));
#23918=EDGE_LOOP('',(#52591,#52592,#52593));
#23919=EDGE_LOOP('',(#52594,#52595,#52596,#52597));
#23920=EDGE_LOOP('',(#52598,#52599,#52600,#52601));
#23921=EDGE_LOOP('',(#52602,#52603,#52604));
#23922=EDGE_LOOP('',(#52605,#52606,#52607,#52608));
#23923=EDGE_LOOP('',(#52609,#52610,#52611,#52612,#52613,#52614));
#23924=EDGE_LOOP('',(#52615,#52616,#52617,#52618,#52619));
#23925=EDGE_LOOP('',(#52620,#52621,#52622,#52623,#52624));
#23926=EDGE_LOOP('',(#52625,#52626,#52627,#52628,#52629));
#23927=EDGE_LOOP('',(#52630,#52631,#52632,#52633));
#23928=EDGE_LOOP('',(#52634,#52635,#52636,#52637));
#23929=EDGE_LOOP('',(#52638,#52639,#52640,#52641));
#23930=EDGE_LOOP('',(#52642,#52643,#52644,#52645));
#23931=EDGE_LOOP('',(#52646,#52647,#52648,#52649));
#23932=EDGE_LOOP('',(#52650,#52651,#52652));
#23933=EDGE_LOOP('',(#52653,#52654,#52655,#52656,#52657,#52658,#52659,#52660,
#52661));
#23934=EDGE_LOOP('',(#52662,#52663,#52664,#52665));
#23935=EDGE_LOOP('',(#52666,#52667,#52668,#52669));
#23936=EDGE_LOOP('',(#52670,#52671,#52672,#52673));
#23937=EDGE_LOOP('',(#52674,#52675,#52676,#52677,#52678,#52679,#52680,#52681,
#52682,#52683,#52684,#52685,#52686,#52687,#52688,#52689,#52690,#52691,#52692,
#52693));
#23938=EDGE_LOOP('',(#52694,#52695,#52696,#52697,#52698,#52699));
#23939=EDGE_LOOP('',(#52700,#52701,#52702,#52703,#52704));
#23940=EDGE_LOOP('',(#52705,#52706,#52707,#52708,#52709));
#23941=EDGE_LOOP('',(#52710,#52711,#52712,#52713));
#23942=EDGE_LOOP('',(#52714,#52715,#52716,#52717,#52718));
#23943=EDGE_LOOP('',(#52719,#52720,#52721,#52722,#52723));
#23944=EDGE_LOOP('',(#52724,#52725,#52726,#52727,#52728));
#23945=EDGE_LOOP('',(#52729,#52730,#52731,#52732,#52733));
#23946=EDGE_LOOP('',(#52734,#52735,#52736,#52737));
#23947=EDGE_LOOP('',(#52738,#52739,#52740,#52741,#52742));
#23948=EDGE_LOOP('',(#52743,#52744,#52745,#52746,#52747,#52748,#52749,#52750,
#52751,#52752,#52753,#52754,#52755,#52756,#52757,#52758,#52759,#52760,#52761,
#52762,#52763));
#23949=EDGE_LOOP('',(#52764,#52765,#52766,#52767));
#23950=EDGE_LOOP('',(#52768,#52769,#52770,#52771,#52772,#52773,#52774,#52775,
#52776,#52777));
#23951=EDGE_LOOP('',(#52778,#52779,#52780,#52781,#52782,#52783));
#23952=EDGE_LOOP('',(#52784,#52785,#52786,#52787,#52788,#52789,#52790));
#23953=EDGE_LOOP('',(#52791,#52792,#52793,#52794,#52795));
#23954=EDGE_LOOP('',(#52796,#52797,#52798,#52799,#52800));
#23955=EDGE_LOOP('',(#52801,#52802,#52803,#52804,#52805,#52806));
#23956=EDGE_LOOP('',(#52807,#52808,#52809,#52810,#52811,#52812,#52813,#52814));
#23957=EDGE_LOOP('',(#52815,#52816,#52817,#52818,#52819));
#23958=EDGE_LOOP('',(#52820,#52821,#52822,#52823,#52824));
#23959=EDGE_LOOP('',(#52825,#52826,#52827,#52828));
#23960=EDGE_LOOP('',(#52829,#52830,#52831,#52832,#52833,#52834,#52835,#52836,
#52837));
#23961=EDGE_LOOP('',(#52838,#52839,#52840,#52841,#52842));
#23962=EDGE_LOOP('',(#52843,#52844,#52845,#52846,#52847));
#23963=EDGE_LOOP('',(#52848,#52849,#52850,#52851,#52852));
#23964=EDGE_LOOP('',(#52853,#52854,#52855,#52856,#52857,#52858));
#23965=EDGE_LOOP('',(#52859,#52860,#52861,#52862));
#23966=EDGE_LOOP('',(#52863,#52864,#52865,#52866));
#23967=EDGE_LOOP('',(#52867,#52868,#52869,#52870));
#23968=EDGE_LOOP('',(#52871,#52872,#52873,#52874,#52875));
#23969=EDGE_LOOP('',(#52876,#52877,#52878,#52879,#52880,#52881));
#23970=EDGE_LOOP('',(#52882,#52883,#52884,#52885,#52886,#52887,#52888,#52889,
#52890));
#23971=EDGE_LOOP('',(#52891,#52892,#52893,#52894,#52895));
#23972=EDGE_LOOP('',(#52896,#52897,#52898,#52899,#52900));
#23973=EDGE_LOOP('',(#52901,#52902,#52903,#52904,#52905));
#23974=EDGE_LOOP('',(#52906,#52907,#52908,#52909,#52910,#52911));
#23975=EDGE_LOOP('',(#52912,#52913,#52914,#52915,#52916,#52917));
#23976=EDGE_LOOP('',(#52918,#52919,#52920,#52921,#52922,#52923,#52924,#52925,
#52926,#52927,#52928,#52929));
#23977=EDGE_LOOP('',(#52930,#52931,#52932,#52933,#52934,#52935,#52936));
#23978=EDGE_LOOP('',(#52937,#52938,#52939,#52940,#52941));
#23979=EDGE_LOOP('',(#52942,#52943,#52944,#52945));
#23980=EDGE_LOOP('',(#52946,#52947,#52948,#52949,#52950));
#23981=EDGE_LOOP('',(#52951,#52952,#52953,#52954,#52955));
#23982=EDGE_LOOP('',(#52956,#52957,#52958,#52959,#52960,#52961));
#23983=EDGE_LOOP('',(#52962,#52963,#52964,#52965,#52966,#52967,#52968,#52969,
#52970,#52971,#52972));
#23984=EDGE_LOOP('',(#52973,#52974,#52975,#52976,#52977));
#23985=EDGE_LOOP('',(#52978,#52979,#52980,#52981,#52982));
#23986=EDGE_LOOP('',(#52983,#52984,#52985,#52986,#52987));
#23987=EDGE_LOOP('',(#52988,#52989,#52990,#52991,#52992,#52993));
#23988=EDGE_LOOP('',(#52994,#52995,#52996,#52997,#52998));
#23989=EDGE_LOOP('',(#52999,#53000,#53001,#53002,#53003,#53004,#53005,#53006,
#53007,#53008,#53009,#53010));
#23990=EDGE_LOOP('',(#53011,#53012,#53013,#53014,#53015,#53016,#53017));
#23991=EDGE_LOOP('',(#53018,#53019,#53020,#53021,#53022));
#23992=EDGE_LOOP('',(#53023,#53024,#53025,#53026));
#23993=EDGE_LOOP('',(#53027,#53028,#53029,#53030,#53031));
#23994=EDGE_LOOP('',(#53032,#53033,#53034,#53035,#53036));
#23995=EDGE_LOOP('',(#53037,#53038,#53039,#53040,#53041,#53042));
#23996=EDGE_LOOP('',(#53043,#53044,#53045,#53046,#53047,#53048,#53049,#53050,
#53051,#53052,#53053));
#23997=EDGE_LOOP('',(#53054,#53055,#53056,#53057,#53058));
#23998=EDGE_LOOP('',(#53059));
#23999=EDGE_LOOP('',(#53060,#53061,#53062,#53063,#53064,#53065));
#24000=EDGE_LOOP('',(#53066,#53067,#53068,#53069));
#24001=EDGE_LOOP('',(#53070,#53071,#53072,#53073));
#24002=EDGE_LOOP('',(#53074,#53075,#53076,#53077));
#24003=EDGE_LOOP('',(#53078,#53079,#53080,#53081));
#24004=EDGE_LOOP('',(#53082,#53083,#53084,#53085,#53086));
#24005=EDGE_LOOP('',(#53087,#53088,#53089,#53090));
#24006=EDGE_LOOP('',(#53091));
#24007=EDGE_LOOP('',(#53092));
#24008=EDGE_LOOP('',(#53093));
#24009=EDGE_LOOP('',(#53094));
#24010=EDGE_LOOP('',(#53095,#53096,#53097,#53098));
#24011=EDGE_LOOP('',(#53099,#53100,#53101));
#24012=EDGE_LOOP('',(#53102,#53103,#53104,#53105,#53106));
#24013=EDGE_LOOP('',(#53107,#53108,#53109,#53110));
#24014=EDGE_LOOP('',(#53111,#53112,#53113));
#24015=EDGE_LOOP('',(#53114,#53115,#53116,#53117,#53118));
#24016=EDGE_LOOP('',(#53119,#53120,#53121));
#24017=EDGE_LOOP('',(#53122,#53123,#53124,#53125));
#24018=EDGE_LOOP('',(#53126,#53127,#53128,#53129));
#24019=EDGE_LOOP('',(#53130,#53131,#53132,#53133,#53134,#53135,#53136));
#24020=EDGE_LOOP('',(#53137,#53138,#53139,#53140));
#24021=EDGE_LOOP('',(#53141,#53142,#53143,#53144));
#24022=EDGE_LOOP('',(#53145,#53146,#53147,#53148,#53149,#53150,#53151,#53152));
#24023=EDGE_LOOP('',(#53153,#53154,#53155,#53156));
#24024=EDGE_LOOP('',(#53157,#53158,#53159,#53160));
#24025=EDGE_LOOP('',(#53161,#53162,#53163,#53164,#53165));
#24026=EDGE_LOOP('',(#53166,#53167,#53168,#53169));
#24027=EDGE_LOOP('',(#53170,#53171,#53172,#53173,#53174,#53175));
#24028=EDGE_LOOP('',(#53176,#53177,#53178,#53179));
#24029=EDGE_LOOP('',(#53180,#53181,#53182,#53183));
#24030=EDGE_LOOP('',(#53184,#53185,#53186,#53187));
#24031=EDGE_LOOP('',(#53188,#53189,#53190,#53191,#53192,#53193));
#24032=EDGE_LOOP('',(#53194,#53195,#53196,#53197));
#24033=EDGE_LOOP('',(#53198,#53199,#53200,#53201,#53202));
#24034=EDGE_LOOP('',(#53203,#53204,#53205,#53206));
#24035=EDGE_LOOP('',(#53207,#53208,#53209,#53210,#53211));
#24036=EDGE_LOOP('',(#53212,#53213,#53214,#53215,#53216,#53217,#53218));
#24037=EDGE_LOOP('',(#53219,#53220,#53221));
#24038=EDGE_LOOP('',(#53222,#53223,#53224,#53225,#53226,#53227,#53228));
#24039=EDGE_LOOP('',(#53229,#53230,#53231,#53232));
#24040=EDGE_LOOP('',(#53233,#53234,#53235,#53236,#53237));
#24041=EDGE_LOOP('',(#53238,#53239,#53240));
#24042=EDGE_LOOP('',(#53241,#53242,#53243,#53244));
#24043=EDGE_LOOP('',(#53245,#53246,#53247));
#24044=EDGE_LOOP('',(#53248,#53249,#53250,#53251));
#24045=EDGE_LOOP('',(#53252,#53253,#53254,#53255));
#24046=EDGE_LOOP('',(#53256,#53257,#53258,#53259,#53260,#53261));
#24047=EDGE_LOOP('',(#53262,#53263,#53264,#53265));
#24048=EDGE_LOOP('',(#53266,#53267,#53268,#53269,#53270));
#24049=EDGE_LOOP('',(#53271,#53272,#53273));
#24050=EDGE_LOOP('',(#53274,#53275,#53276,#53277));
#24051=EDGE_LOOP('',(#53278,#53279,#53280,#53281));
#24052=EDGE_LOOP('',(#53282,#53283,#53284,#53285));
#24053=EDGE_LOOP('',(#53286,#53287,#53288,#53289));
#24054=EDGE_LOOP('',(#53290,#53291,#53292,#53293,#53294));
#24055=EDGE_LOOP('',(#53295,#53296,#53297,#53298,#53299,#53300,#53301));
#24056=EDGE_LOOP('',(#53302,#53303,#53304));
#24057=EDGE_LOOP('',(#53305,#53306,#53307,#53308,#53309,#53310));
#24058=EDGE_LOOP('',(#53311,#53312,#53313));
#24059=EDGE_LOOP('',(#53314,#53315,#53316,#53317,#53318,#53319,#53320,#53321,
#53322));
#24060=EDGE_LOOP('',(#53323,#53324,#53325,#53326,#53327));
#24061=EDGE_LOOP('',(#53328,#53329,#53330,#53331));
#24062=EDGE_LOOP('',(#53332,#53333,#53334,#53335));
#24063=EDGE_LOOP('',(#53336,#53337,#53338,#53339));
#24064=EDGE_LOOP('',(#53340,#53341,#53342,#53343));
#24065=EDGE_LOOP('',(#53344,#53345,#53346,#53347));
#24066=EDGE_LOOP('',(#53348,#53349,#53350,#53351));
#24067=EDGE_LOOP('',(#53352,#53353,#53354,#53355));
#24068=EDGE_LOOP('',(#53356,#53357,#53358,#53359));
#24069=EDGE_LOOP('',(#53360,#53361,#53362,#53363));
#24070=EDGE_LOOP('',(#53364,#53365,#53366,#53367));
#24071=EDGE_LOOP('',(#53368,#53369,#53370,#53371));
#24072=EDGE_LOOP('',(#53372,#53373,#53374,#53375));
#24073=EDGE_LOOP('',(#53376,#53377,#53378,#53379));
#24074=EDGE_LOOP('',(#53380,#53381,#53382,#53383));
#24075=EDGE_LOOP('',(#53384,#53385,#53386,#53387));
#24076=EDGE_LOOP('',(#53388,#53389,#53390,#53391));
#24077=EDGE_LOOP('',(#53392));
#24078=EDGE_LOOP('',(#53393,#53394,#53395,#53396));
#24079=EDGE_LOOP('',(#53397,#53398,#53399,#53400,#53401,#53402));
#24080=EDGE_LOOP('',(#53403,#53404,#53405,#53406));
#24081=EDGE_LOOP('',(#53407,#53408,#53409,#53410,#53411,#53412));
#24082=EDGE_LOOP('',(#53413,#53414,#53415,#53416,#53417,#53418,#53419,#53420));
#24083=EDGE_LOOP('',(#53421,#53422,#53423,#53424));
#24084=EDGE_LOOP('',(#53425,#53426,#53427,#53428,#53429,#53430,#53431,#53432));
#24085=EDGE_LOOP('',(#53433));
#24086=EDGE_LOOP('',(#53434,#53435,#53436,#53437));
#24087=EDGE_LOOP('',(#53438));
#24088=EDGE_LOOP('',(#53439,#53440,#53441,#53442,#53443,#53444));
#24089=EDGE_LOOP('',(#53445,#53446,#53447,#53448));
#24090=EDGE_LOOP('',(#53449,#53450,#53451,#53452));
#24091=EDGE_LOOP('',(#53453,#53454,#53455,#53456));
#24092=EDGE_LOOP('',(#53457,#53458,#53459,#53460));
#24093=EDGE_LOOP('',(#53461,#53462,#53463,#53464,#53465));
#24094=EDGE_LOOP('',(#53466,#53467,#53468,#53469));
#24095=EDGE_LOOP('',(#53470));
#24096=EDGE_LOOP('',(#53471));
#24097=EDGE_LOOP('',(#53472));
#24098=EDGE_LOOP('',(#53473));
#24099=EDGE_LOOP('',(#53474,#53475,#53476));
#24100=EDGE_LOOP('',(#53477,#53478,#53479,#53480));
#24101=EDGE_LOOP('',(#53481,#53482,#53483,#53484,#53485));
#24102=EDGE_LOOP('',(#53486,#53487,#53488,#53489));
#24103=EDGE_LOOP('',(#53490,#53491,#53492,#53493));
#24104=EDGE_LOOP('',(#53494,#53495,#53496,#53497));
#24105=EDGE_LOOP('',(#53498,#53499,#53500,#53501));
#24106=EDGE_LOOP('',(#53502,#53503,#53504,#53505));
#24107=EDGE_LOOP('',(#53506,#53507,#53508,#53509));
#24108=EDGE_LOOP('',(#53510,#53511,#53512,#53513,#53514));
#24109=EDGE_LOOP('',(#53515,#53516,#53517));
#24110=EDGE_LOOP('',(#53518,#53519,#53520));
#24111=EDGE_LOOP('',(#53521,#53522,#53523,#53524));
#24112=EDGE_LOOP('',(#53525,#53526,#53527,#53528,#53529,#53530,#53531));
#24113=EDGE_LOOP('',(#53532,#53533,#53534,#53535,#53536,#53537,#53538,#53539));
#24114=EDGE_LOOP('',(#53540,#53541,#53542,#53543,#53544));
#24115=EDGE_LOOP('',(#53545,#53546,#53547,#53548,#53549,#53550));
#24116=EDGE_LOOP('',(#53551,#53552,#53553,#53554));
#24117=EDGE_LOOP('',(#53555,#53556,#53557,#53558));
#24118=EDGE_LOOP('',(#53559,#53560,#53561,#53562,#53563));
#24119=EDGE_LOOP('',(#53564,#53565,#53566));
#24120=EDGE_LOOP('',(#53567,#53568,#53569,#53570,#53571,#53572,#53573));
#24121=EDGE_LOOP('',(#53574,#53575,#53576));
#24122=EDGE_LOOP('',(#53577,#53578,#53579,#53580,#53581,#53582,#53583));
#24123=EDGE_LOOP('',(#53584,#53585,#53586,#53587,#53588));
#24124=EDGE_LOOP('',(#53589,#53590,#53591,#53592));
#24125=EDGE_LOOP('',(#53593,#53594,#53595,#53596,#53597));
#24126=EDGE_LOOP('',(#53598,#53599,#53600,#53601));
#24127=EDGE_LOOP('',(#53602,#53603,#53604,#53605,#53606,#53607));
#24128=EDGE_LOOP('',(#53608,#53609,#53610,#53611));
#24129=EDGE_LOOP('',(#53612,#53613,#53614,#53615));
#24130=EDGE_LOOP('',(#53616,#53617,#53618,#53619));
#24131=EDGE_LOOP('',(#53620,#53621,#53622,#53623));
#24132=EDGE_LOOP('',(#53624,#53625,#53626));
#24133=EDGE_LOOP('',(#53627,#53628,#53629,#53630));
#24134=EDGE_LOOP('',(#53631,#53632,#53633,#53634,#53635));
#24135=EDGE_LOOP('',(#53636,#53637,#53638,#53639));
#24136=EDGE_LOOP('',(#53640,#53641,#53642,#53643));
#24137=EDGE_LOOP('',(#53644,#53645,#53646,#53647));
#24138=EDGE_LOOP('',(#53648,#53649,#53650,#53651));
#24139=EDGE_LOOP('',(#53652,#53653,#53654));
#24140=EDGE_LOOP('',(#53655,#53656,#53657,#53658,#53659));
#24141=EDGE_LOOP('',(#53660,#53661,#53662,#53663));
#24142=EDGE_LOOP('',(#53664,#53665,#53666,#53667,#53668,#53669));
#24143=EDGE_LOOP('',(#53670,#53671,#53672,#53673));
#24144=EDGE_LOOP('',(#53674,#53675,#53676,#53677,#53678,#53679,#53680));
#24145=EDGE_LOOP('',(#53681,#53682,#53683,#53684,#53685,#53686,#53687,#53688,
#53689));
#24146=EDGE_LOOP('',(#53690,#53691,#53692));
#24147=EDGE_LOOP('',(#53693,#53694,#53695,#53696,#53697,#53698,#53699));
#24148=EDGE_LOOP('',(#53700,#53701,#53702));
#24149=EDGE_LOOP('',(#53703,#53704,#53705,#53706,#53707));
#24150=EDGE_LOOP('',(#53708,#53709,#53710,#53711,#53712));
#24151=EDGE_LOOP('',(#53713,#53714,#53715,#53716));
#24152=EDGE_LOOP('',(#53717,#53718,#53719,#53720));
#24153=EDGE_LOOP('',(#53721,#53722,#53723,#53724));
#24154=EDGE_LOOP('',(#53725,#53726,#53727,#53728));
#24155=EDGE_LOOP('',(#53729,#53730,#53731,#53732));
#24156=EDGE_LOOP('',(#53733,#53734,#53735,#53736));
#24157=EDGE_LOOP('',(#53737,#53738,#53739,#53740));
#24158=EDGE_LOOP('',(#53741,#53742,#53743,#53744));
#24159=EDGE_LOOP('',(#53745,#53746,#53747,#53748));
#24160=EDGE_LOOP('',(#53749,#53750,#53751,#53752));
#24161=EDGE_LOOP('',(#53753,#53754,#53755,#53756));
#24162=EDGE_LOOP('',(#53757,#53758,#53759,#53760));
#24163=EDGE_LOOP('',(#53761,#53762,#53763,#53764));
#24164=EDGE_LOOP('',(#53765,#53766,#53767,#53768));
#24165=EDGE_LOOP('',(#53769,#53770,#53771,#53772));
#24166=EDGE_LOOP('',(#53773));
#24167=EDGE_LOOP('',(#53774,#53775,#53776,#53777));
#24168=EDGE_LOOP('',(#53778,#53779,#53780,#53781,#53782,#53783));
#24169=EDGE_LOOP('',(#53784,#53785,#53786,#53787,#53788,#53789));
#24170=EDGE_LOOP('',(#53790,#53791,#53792,#53793));
#24171=EDGE_LOOP('',(#53794,#53795,#53796,#53797,#53798,#53799,#53800,#53801));
#24172=EDGE_LOOP('',(#53802,#53803,#53804,#53805,#53806,#53807,#53808,#53809));
#24173=EDGE_LOOP('',(#53810,#53811,#53812,#53813));
#24174=EDGE_LOOP('',(#53814));
#24175=EDGE_LOOP('',(#53815,#53816,#53817,#53818));
#24176=EDGE_LOOP('',(#53819,#53820,#53821,#53822,#53823,#53824,#53825,#53826,
#53827,#53828,#53829,#53830));
#24177=EDGE_LOOP('',(#53831,#53832,#53833,#53834,#53835,#53836,#53837,#53838,
#53839,#53840,#53841,#53842,#53843));
#24178=EDGE_LOOP('',(#53844,#53845,#53846,#53847));
#24179=EDGE_LOOP('',(#53848));
#24180=EDGE_LOOP('',(#53849));
#24181=EDGE_LOOP('',(#53850));
#24182=EDGE_LOOP('',(#53851,#53852,#53853,#53854,#53855,#53856,#53857,#53858,
#53859));
#24183=EDGE_LOOP('',(#53860,#53861,#53862,#53863,#53864,#53865,#53866,#53867,
#53868));
#24184=EDGE_LOOP('',(#53869,#53870,#53871,#53872));
#24185=EDGE_LOOP('',(#53873,#53874,#53875,#53876));
#24186=EDGE_LOOP('',(#53877,#53878,#53879,#53880,#53881,#53882));
#24187=EDGE_LOOP('',(#53883,#53884,#53885));
#24188=EDGE_LOOP('',(#53886,#53887,#53888,#53889,#53890));
#24189=EDGE_LOOP('',(#53891,#53892,#53893));
#24190=EDGE_LOOP('',(#53894,#53895,#53896,#53897,#53898,#53899,#53900,#53901,
#53902,#53903));
#24191=EDGE_LOOP('',(#53904,#53905,#53906,#53907,#53908,#53909,#53910,#53911,
#53912,#53913,#53914,#53915));
#24192=EDGE_LOOP('',(#53916,#53917,#53918,#53919,#53920,#53921,#53922,#53923,
#53924));
#24193=EDGE_LOOP('',(#53925,#53926,#53927,#53928,#53929,#53930,#53931,#53932,
#53933));
#24194=EDGE_LOOP('',(#53934,#53935,#53936,#53937,#53938,#53939,#53940));
#24195=EDGE_LOOP('',(#53941,#53942,#53943));
#24196=EDGE_LOOP('',(#53944,#53945,#53946,#53947));
#24197=EDGE_LOOP('',(#53948,#53949,#53950));
#24198=EDGE_LOOP('',(#53951,#53952,#53953,#53954));
#24199=EDGE_LOOP('',(#53955,#53956,#53957,#53958));
#24200=EDGE_LOOP('',(#53959,#53960,#53961));
#24201=EDGE_LOOP('',(#53962,#53963,#53964,#53965));
#24202=EDGE_LOOP('',(#53966,#53967,#53968,#53969,#53970,#53971,#53972));
#24203=EDGE_LOOP('',(#53973,#53974,#53975));
#24204=EDGE_LOOP('',(#53976,#53977,#53978,#53979,#53980));
#24205=EDGE_LOOP('',(#53981,#53982,#53983,#53984,#53985,#53986));
#24206=EDGE_LOOP('',(#53987,#53988,#53989,#53990));
#24207=EDGE_LOOP('',(#53991,#53992,#53993));
#24208=EDGE_LOOP('',(#53994,#53995,#53996,#53997,#53998));
#24209=EDGE_LOOP('',(#53999,#54000,#54001));
#24210=EDGE_LOOP('',(#54002,#54003,#54004));
#24211=EDGE_LOOP('',(#54005,#54006,#54007));
#24212=EDGE_LOOP('',(#54008,#54009,#54010,#54011,#54012));
#24213=EDGE_LOOP('',(#54013,#54014,#54015));
#24214=EDGE_LOOP('',(#54016,#54017,#54018));
#24215=EDGE_LOOP('',(#54019,#54020,#54021,#54022,#54023));
#24216=EDGE_LOOP('',(#54024,#54025,#54026));
#24217=EDGE_LOOP('',(#54027,#54028,#54029,#54030,#54031,#54032));
#24218=EDGE_LOOP('',(#54033,#54034,#54035,#54036));
#24219=EDGE_LOOP('',(#54037,#54038,#54039,#54040));
#24220=EDGE_LOOP('',(#54041,#54042,#54043,#54044));
#24221=EDGE_LOOP('',(#54045,#54046,#54047,#54048));
#24222=EDGE_LOOP('',(#54049,#54050,#54051,#54052));
#24223=EDGE_LOOP('',(#54053,#54054,#54055,#54056));
#24224=EDGE_LOOP('',(#54057,#54058,#54059,#54060,#54061));
#24225=EDGE_LOOP('',(#54062,#54063,#54064,#54065));
#24226=EDGE_LOOP('',(#54066,#54067,#54068));
#24227=EDGE_LOOP('',(#54069,#54070,#54071,#54072));
#24228=EDGE_LOOP('',(#54073,#54074,#54075,#54076,#54077));
#24229=EDGE_LOOP('',(#54078,#54079,#54080,#54081));
#24230=EDGE_LOOP('',(#54082,#54083,#54084,#54085));
#24231=EDGE_LOOP('',(#54086,#54087,#54088,#54089,#54090,#54091,#54092,#54093,
#54094,#54095,#54096));
#24232=EDGE_LOOP('',(#54097,#54098,#54099,#54100));
#24233=EDGE_LOOP('',(#54101,#54102,#54103,#54104));
#24234=EDGE_LOOP('',(#54105,#54106,#54107,#54108,#54109));
#24235=EDGE_LOOP('',(#54110,#54111,#54112,#54113,#54114));
#24236=EDGE_LOOP('',(#54115,#54116,#54117,#54118));
#24237=EDGE_LOOP('',(#54119,#54120,#54121,#54122,#54123));
#24238=EDGE_LOOP('',(#54124,#54125,#54126,#54127,#54128));
#24239=EDGE_LOOP('',(#54129,#54130,#54131,#54132));
#24240=EDGE_LOOP('',(#54133,#54134,#54135,#54136,#54137,#54138,#54139,#54140,
#54141));
#24241=EDGE_LOOP('',(#54142));
#24242=EDGE_LOOP('',(#54143));
#24243=EDGE_LOOP('',(#54144));
#24244=EDGE_LOOP('',(#54145));
#24245=EDGE_LOOP('',(#54146,#54147,#54148,#54149));
#24246=EDGE_LOOP('',(#54150,#54151,#54152,#54153,#54154,#54155));
#24247=EDGE_LOOP('',(#54156,#54157,#54158,#54159,#54160));
#24248=EDGE_LOOP('',(#54161,#54162,#54163,#54164,#54165,#54166));
#24249=EDGE_LOOP('',(#54167,#54168,#54169,#54170));
#24250=EDGE_LOOP('',(#54171,#54172,#54173,#54174));
#24251=EDGE_LOOP('',(#54175,#54176,#54177,#54178));
#24252=EDGE_LOOP('',(#54179,#54180,#54181,#54182));
#24253=EDGE_LOOP('',(#54183,#54184,#54185,#54186));
#24254=EDGE_LOOP('',(#54187,#54188,#54189,#54190,#54191,#54192));
#24255=EDGE_LOOP('',(#54193,#54194,#54195,#54196,#54197));
#24256=EDGE_LOOP('',(#54198,#54199,#54200,#54201,#54202));
#24257=EDGE_LOOP('',(#54203,#54204,#54205,#54206,#54207,#54208));
#24258=EDGE_LOOP('',(#54209,#54210,#54211,#54212,#54213,#54214));
#24259=EDGE_LOOP('',(#54215,#54216,#54217,#54218));
#24260=EDGE_LOOP('',(#54219,#54220,#54221,#54222));
#24261=EDGE_LOOP('',(#54223,#54224,#54225,#54226,#54227));
#24262=EDGE_LOOP('',(#54228,#54229,#54230,#54231));
#24263=EDGE_LOOP('',(#54232,#54233,#54234,#54235));
#24264=EDGE_LOOP('',(#54236,#54237,#54238,#54239,#54240,#54241));
#24265=EDGE_LOOP('',(#54242,#54243,#54244,#54245,#54246,#54247));
#24266=EDGE_LOOP('',(#54248,#54249,#54250,#54251));
#24267=EDGE_LOOP('',(#54252));
#24268=EDGE_LOOP('',(#54253));
#24269=EDGE_LOOP('',(#54254));
#24270=EDGE_LOOP('',(#54255));
#24271=EDGE_LOOP('',(#54256));
#24272=EDGE_LOOP('',(#54257,#54258,#54259,#54260,#54261,#54262,#54263));
#24273=EDGE_LOOP('',(#54264,#54265,#54266));
#24274=EDGE_LOOP('',(#54267,#54268,#54269,#54270,#54271,#54272));
#24275=EDGE_LOOP('',(#54273,#54274,#54275,#54276));
#24276=EDGE_LOOP('',(#54277,#54278,#54279,#54280));
#24277=EDGE_LOOP('',(#54281,#54282,#54283,#54284));
#24278=EDGE_LOOP('',(#54285,#54286,#54287,#54288,#54289));
#24279=EDGE_LOOP('',(#54290,#54291,#54292,#54293));
#24280=EDGE_LOOP('',(#54294,#54295,#54296,#54297,#54298,#54299,#54300,#54301,
#54302));
#24281=EDGE_LOOP('',(#54303,#54304,#54305,#54306,#54307,#54308));
#24282=EDGE_LOOP('',(#54309,#54310,#54311,#54312));
#24283=EDGE_LOOP('',(#54313,#54314,#54315,#54316,#54317,#54318,#54319));
#24284=EDGE_LOOP('',(#54320,#54321,#54322,#54323));
#24285=EDGE_LOOP('',(#54324,#54325,#54326,#54327,#54328,#54329));
#24286=EDGE_LOOP('',(#54330,#54331,#54332));
#24287=EDGE_LOOP('',(#54333,#54334,#54335));
#24288=EDGE_LOOP('',(#54336,#54337,#54338,#54339,#54340,#54341,#54342));
#24289=EDGE_LOOP('',(#54343,#54344,#54345,#54346,#54347,#54348,#54349,#54350,
#54351,#54352,#54353));
#24290=EDGE_LOOP('',(#54354,#54355,#54356,#54357));
#24291=EDGE_LOOP('',(#54358,#54359,#54360,#54361));
#24292=EDGE_LOOP('',(#54362,#54363,#54364,#54365,#54366));
#24293=EDGE_LOOP('',(#54367,#54368,#54369,#54370));
#24294=EDGE_LOOP('',(#54371,#54372,#54373,#54374));
#24295=EDGE_LOOP('',(#54375,#54376,#54377,#54378));
#24296=EDGE_LOOP('',(#54379,#54380,#54381,#54382));
#24297=EDGE_LOOP('',(#54383,#54384,#54385,#54386));
#24298=EDGE_LOOP('',(#54387,#54388,#54389,#54390));
#24299=EDGE_LOOP('',(#54391,#54392,#54393,#54394));
#24300=EDGE_LOOP('',(#54395,#54396,#54397,#54398));
#24301=EDGE_LOOP('',(#54399,#54400,#54401));
#24302=EDGE_LOOP('',(#54402,#54403,#54404,#54405,#54406));
#24303=EDGE_LOOP('',(#54407,#54408,#54409,#54410));
#24304=EDGE_LOOP('',(#54411,#54412,#54413,#54414));
#24305=EDGE_LOOP('',(#54415,#54416,#54417,#54418));
#24306=EDGE_LOOP('',(#54419,#54420,#54421,#54422));
#24307=EDGE_LOOP('',(#54423,#54424,#54425,#54426));
#24308=EDGE_LOOP('',(#54427,#54428,#54429,#54430));
#24309=EDGE_LOOP('',(#54431,#54432,#54433,#54434));
#24310=EDGE_LOOP('',(#54435,#54436,#54437,#54438,#54439));
#24311=EDGE_LOOP('',(#54440,#54441,#54442,#54443,#54444,#54445));
#24312=EDGE_LOOP('',(#54446,#54447,#54448));
#24313=EDGE_LOOP('',(#54449,#54450,#54451,#54452));
#24314=EDGE_LOOP('',(#54453,#54454,#54455,#54456));
#24315=EDGE_LOOP('',(#54457,#54458,#54459));
#24316=EDGE_LOOP('',(#54460,#54461,#54462,#54463,#54464,#54465));
#24317=EDGE_LOOP('',(#54466,#54467,#54468,#54469,#54470));
#24318=EDGE_LOOP('',(#54471,#54472,#54473,#54474));
#24319=EDGE_LOOP('',(#54475,#54476,#54477,#54478));
#24320=EDGE_LOOP('',(#54479,#54480,#54481,#54482,#54483));
#24321=EDGE_LOOP('',(#54484,#54485,#54486,#54487));
#24322=EDGE_LOOP('',(#54488,#54489,#54490,#54491));
#24323=EDGE_LOOP('',(#54492,#54493,#54494,#54495));
#24324=EDGE_LOOP('',(#54496,#54497,#54498,#54499,#54500));
#24325=EDGE_LOOP('',(#54501,#54502,#54503,#54504));
#24326=EDGE_LOOP('',(#54505,#54506,#54507,#54508));
#24327=EDGE_LOOP('',(#54509,#54510,#54511,#54512,#54513));
#24328=EDGE_LOOP('',(#54514,#54515,#54516,#54517,#54518));
#24329=EDGE_LOOP('',(#54519,#54520,#54521,#54522));
#24330=EDGE_LOOP('',(#54523,#54524,#54525,#54526));
#24331=EDGE_LOOP('',(#54527,#54528,#54529,#54530));
#24332=EDGE_LOOP('',(#54531,#54532,#54533,#54534));
#24333=EDGE_LOOP('',(#54535,#54536,#54537,#54538,#54539,#54540,#54541,#54542,
#54543,#54544,#54545));
#24334=EDGE_LOOP('',(#54546,#54547,#54548,#54549));
#24335=EDGE_LOOP('',(#54550,#54551,#54552,#54553,#54554,#54555,#54556));
#24336=EDGE_LOOP('',(#54557,#54558,#54559,#54560,#54561,#54562));
#24337=EDGE_LOOP('',(#54563,#54564,#54565,#54566));
#24338=EDGE_LOOP('',(#54567));
#24339=EDGE_LOOP('',(#54568));
#24340=EDGE_LOOP('',(#54569,#54570));
#24341=EDGE_LOOP('',(#54571));
#24342=EDGE_LOOP('',(#54572,#54573,#54574,#54575,#54576,#54577,#54578,#54579));
#24343=EDGE_LOOP('',(#54580,#54581,#54582,#54583,#54584));
#24344=EDGE_LOOP('',(#54585,#54586,#54587,#54588,#54589,#54590,#54591));
#24345=EDGE_LOOP('',(#54592,#54593,#54594,#54595,#54596,#54597,#54598));
#24346=EDGE_LOOP('',(#54599,#54600,#54601,#54602));
#24347=EDGE_LOOP('',(#54603,#54604,#54605,#54606));
#24348=EDGE_LOOP('',(#54607,#54608,#54609,#54610));
#24349=EDGE_LOOP('',(#54611,#54612,#54613,#54614));
#24350=EDGE_LOOP('',(#54615,#54616,#54617,#54618,#54619));
#24351=EDGE_LOOP('',(#54620,#54621,#54622,#54623,#54624,#54625,#54626,#54627,
#54628,#54629,#54630,#54631,#54632,#54633));
#24352=EDGE_LOOP('',(#54634,#54635,#54636,#54637,#54638));
#24353=EDGE_LOOP('',(#54639,#54640,#54641,#54642));
#24354=EDGE_LOOP('',(#54643,#54644,#54645,#54646));
#24355=EDGE_LOOP('',(#54647,#54648,#54649,#54650));
#24356=EDGE_LOOP('',(#54651,#54652,#54653,#54654));
#24357=EDGE_LOOP('',(#54655,#54656,#54657,#54658));
#24358=EDGE_LOOP('',(#54659,#54660,#54661,#54662));
#24359=EDGE_LOOP('',(#54663,#54664,#54665));
#24360=EDGE_LOOP('',(#54666,#54667,#54668));
#24361=EDGE_LOOP('',(#54669,#54670,#54671,#54672,#54673,#54674,#54675,#54676,
#54677,#54678,#54679,#54680));
#24362=EDGE_LOOP('',(#54681,#54682,#54683,#54684,#54685,#54686,#54687));
#24363=EDGE_LOOP('',(#54688,#54689,#54690,#54691));
#24364=EDGE_LOOP('',(#54692,#54693,#54694,#54695,#54696));
#24365=EDGE_LOOP('',(#54697,#54698,#54699,#54700));
#24366=EDGE_LOOP('',(#54701,#54702,#54703,#54704));
#24367=EDGE_LOOP('',(#54705,#54706,#54707,#54708));
#24368=EDGE_LOOP('',(#54709,#54710,#54711,#54712,#54713,#54714,#54715,#54716,
#54717));
#24369=EDGE_LOOP('',(#54718,#54719,#54720));
#24370=EDGE_LOOP('',(#54721,#54722,#54723,#54724,#54725));
#24371=EDGE_LOOP('',(#54726,#54727,#54728,#54729));
#24372=EDGE_LOOP('',(#54730,#54731,#54732,#54733));
#24373=EDGE_LOOP('',(#54734,#54735,#54736,#54737));
#24374=EDGE_LOOP('',(#54738,#54739,#54740));
#24375=EDGE_LOOP('',(#54741,#54742,#54743,#54744));
#24376=EDGE_LOOP('',(#54745,#54746,#54747,#54748));
#24377=EDGE_LOOP('',(#54749,#54750,#54751,#54752,#54753));
#24378=EDGE_LOOP('',(#54754,#54755,#54756,#54757));
#24379=EDGE_LOOP('',(#54758,#54759,#54760,#54761));
#24380=EDGE_LOOP('',(#54762,#54763,#54764,#54765));
#24381=EDGE_LOOP('',(#54766,#54767,#54768,#54769,#54770,#54771,#54772));
#24382=EDGE_LOOP('',(#54773,#54774,#54775,#54776,#54777,#54778,#54779));
#24383=EDGE_LOOP('',(#54780,#54781,#54782,#54783));
#24384=EDGE_LOOP('',(#54784,#54785,#54786));
#24385=EDGE_LOOP('',(#54787,#54788,#54789));
#24386=EDGE_LOOP('',(#54790,#54791,#54792,#54793));
#24387=EDGE_LOOP('',(#54794,#54795,#54796,#54797));
#24388=EDGE_LOOP('',(#54798,#54799,#54800,#54801));
#24389=EDGE_LOOP('',(#54802,#54803,#54804));
#24390=EDGE_LOOP('',(#54805,#54806,#54807,#54808));
#24391=EDGE_LOOP('',(#54809,#54810,#54811,#54812));
#24392=EDGE_LOOP('',(#54813,#54814,#54815,#54816));
#24393=EDGE_LOOP('',(#54817,#54818,#54819,#54820,#54821,#54822));
#24394=EDGE_LOOP('',(#54823));
#24395=EDGE_LOOP('',(#54824,#54825,#54826,#54827));
#24396=EDGE_LOOP('',(#54828,#54829,#54830,#54831));
#24397=EDGE_LOOP('',(#54832,#54833,#54834,#54835));
#24398=EDGE_LOOP('',(#54836,#54837,#54838,#54839));
#24399=EDGE_LOOP('',(#54840,#54841,#54842,#54843));
#24400=EDGE_LOOP('',(#54844,#54845,#54846,#54847,#54848));
#24401=EDGE_LOOP('',(#54849,#54850,#54851,#54852));
#24402=EDGE_LOOP('',(#54853,#54854,#54855,#54856));
#24403=EDGE_LOOP('',(#54857,#54858,#54859,#54860));
#24404=EDGE_LOOP('',(#54861,#54862,#54863,#54864));
#24405=EDGE_LOOP('',(#54865,#54866,#54867,#54868));
#24406=EDGE_LOOP('',(#54869,#54870,#54871,#54872,#54873));
#24407=EDGE_LOOP('',(#54874,#54875,#54876,#54877,#54878,#54879,#54880));
#24408=EDGE_LOOP('',(#54881,#54882,#54883,#54884));
#24409=EDGE_LOOP('',(#54885,#54886,#54887,#54888,#54889,#54890,#54891,#54892,
#54893,#54894));
#24410=EDGE_LOOP('',(#54895,#54896,#54897,#54898));
#24411=EDGE_LOOP('',(#54899,#54900,#54901,#54902,#54903,#54904,#54905));
#24412=EDGE_LOOP('',(#54906,#54907,#54908,#54909));
#24413=EDGE_LOOP('',(#54910,#54911,#54912,#54913,#54914,#54915,#54916,#54917,
#54918,#54919,#54920,#54921));
#24414=EDGE_LOOP('',(#54922,#54923,#54924,#54925));
#24415=EDGE_LOOP('',(#54926,#54927,#54928,#54929));
#24416=EDGE_LOOP('',(#54930,#54931,#54932,#54933));
#24417=EDGE_LOOP('',(#54934,#54935,#54936,#54937));
#24418=EDGE_LOOP('',(#54938,#54939,#54940,#54941,#54942));
#24419=EDGE_LOOP('',(#54943,#54944,#54945,#54946));
#24420=EDGE_LOOP('',(#54947,#54948,#54949,#54950));
#24421=EDGE_LOOP('',(#54951,#54952,#54953,#54954));
#24422=EDGE_LOOP('',(#54955,#54956,#54957,#54958));
#24423=EDGE_LOOP('',(#54959,#54960,#54961,#54962,#54963));
#24424=EDGE_LOOP('',(#54964,#54965,#54966,#54967,#54968,#54969));
#24425=EDGE_LOOP('',(#54970));
#24426=EDGE_LOOP('',(#54971,#54972,#54973,#54974));
#24427=EDGE_LOOP('',(#54975,#54976,#54977,#54978));
#24428=EDGE_LOOP('',(#54979,#54980,#54981,#54982));
#24429=EDGE_LOOP('',(#54983,#54984,#54985,#54986));
#24430=EDGE_LOOP('',(#54987,#54988,#54989,#54990));
#24431=EDGE_LOOP('',(#54991,#54992,#54993,#54994));
#24432=EDGE_LOOP('',(#54995,#54996,#54997,#54998,#54999,#55000));
#24433=EDGE_LOOP('',(#55001,#55002,#55003,#55004));
#24434=EDGE_LOOP('',(#55005,#55006,#55007,#55008));
#24435=EDGE_LOOP('',(#55009,#55010,#55011,#55012));
#24436=EDGE_LOOP('',(#55013,#55014,#55015,#55016,#55017));
#24437=EDGE_LOOP('',(#55018,#55019,#55020,#55021));
#24438=EDGE_LOOP('',(#55022,#55023,#55024,#55025));
#24439=EDGE_LOOP('',(#55026,#55027,#55028));
#24440=EDGE_LOOP('',(#55029,#55030,#55031,#55032,#55033,#55034,#55035,#55036,
#55037));
#24441=EDGE_LOOP('',(#55038,#55039,#55040,#55041,#55042));
#24442=EDGE_LOOP('',(#55043,#55044,#55045,#55046));
#24443=EDGE_LOOP('',(#55047,#55048,#55049,#55050));
#24444=EDGE_LOOP('',(#55051,#55052,#55053,#55054,#55055));
#24445=EDGE_LOOP('',(#55056,#55057,#55058,#55059));
#24446=EDGE_LOOP('',(#55060,#55061,#55062,#55063));
#24447=EDGE_LOOP('',(#55064,#55065,#55066,#55067,#55068));
#24448=EDGE_LOOP('',(#55069,#55070,#55071));
#24449=EDGE_LOOP('',(#55072,#55073,#55074,#55075));
#24450=EDGE_LOOP('',(#55076,#55077,#55078,#55079));
#24451=EDGE_LOOP('',(#55080,#55081,#55082,#55083));
#24452=EDGE_LOOP('',(#55084,#55085,#55086,#55087,#55088,#55089));
#24453=EDGE_LOOP('',(#55090,#55091,#55092,#55093));
#24454=EDGE_LOOP('',(#55094));
#24455=EDGE_LOOP('',(#55095));
#24456=EDGE_LOOP('',(#55096,#55097,#55098,#55099));
#24457=EDGE_LOOP('',(#55100,#55101,#55102,#55103));
#24458=EDGE_LOOP('',(#55104,#55105,#55106,#55107));
#24459=EDGE_LOOP('',(#55108,#55109,#55110,#55111,#55112,#55113,#55114,#55115));
#24460=EDGE_LOOP('',(#55116,#55117,#55118,#55119));
#24461=EDGE_LOOP('',(#55120,#55121,#55122,#55123));
#24462=EDGE_LOOP('',(#55124,#55125,#55126,#55127));
#24463=EDGE_LOOP('',(#55128,#55129,#55130,#55131));
#24464=EDGE_LOOP('',(#55132,#55133,#55134,#55135));
#24465=EDGE_LOOP('',(#55136,#55137,#55138,#55139));
#24466=EDGE_LOOP('',(#55140,#55141,#55142,#55143));
#24467=EDGE_LOOP('',(#55144,#55145,#55146,#55147));
#24468=EDGE_LOOP('',(#55148,#55149,#55150,#55151));
#24469=EDGE_LOOP('',(#55152,#55153,#55154,#55155));
#24470=EDGE_LOOP('',(#55156,#55157,#55158,#55159));
#24471=EDGE_LOOP('',(#55160,#55161,#55162,#55163));
#24472=EDGE_LOOP('',(#55164,#55165,#55166,#55167));
#24473=EDGE_LOOP('',(#55168,#55169,#55170,#55171,#55172,#55173,#55174));
#24474=EDGE_LOOP('',(#55175));
#24475=EDGE_LOOP('',(#55176,#55177,#55178,#55179));
#24476=EDGE_LOOP('',(#55180,#55181,#55182,#55183));
#24477=EDGE_LOOP('',(#55184));
#24478=EDGE_LOOP('',(#55185));
#24479=EDGE_LOOP('',(#55186));
#24480=EDGE_LOOP('',(#55187,#55188));
#24481=EDGE_LOOP('',(#55189,#55190,#55191,#55192));
#24482=EDGE_LOOP('',(#55193,#55194,#55195,#55196,#55197,#55198,#55199));
#24483=EDGE_LOOP('',(#55200,#55201,#55202,#55203,#55204,#55205,#55206,#55207,
#55208,#55209,#55210,#55211));
#24484=EDGE_LOOP('',(#55212,#55213,#55214,#55215));
#24485=EDGE_LOOP('',(#55216,#55217,#55218));
#24486=EDGE_LOOP('',(#55219,#55220,#55221,#55222));
#24487=EDGE_LOOP('',(#55223,#55224,#55225));
#24488=EDGE_LOOP('',(#55226,#55227,#55228,#55229));
#24489=EDGE_LOOP('',(#55230,#55231,#55232,#55233,#55234,#55235));
#24490=EDGE_LOOP('',(#55236,#55237,#55238,#55239));
#24491=EDGE_LOOP('',(#55240,#55241,#55242,#55243));
#24492=EDGE_LOOP('',(#55244,#55245,#55246,#55247));
#24493=EDGE_LOOP('',(#55248,#55249,#55250,#55251,#55252));
#24494=EDGE_LOOP('',(#55253,#55254,#55255,#55256));
#24495=EDGE_LOOP('',(#55257,#55258,#55259,#55260));
#24496=EDGE_LOOP('',(#55261,#55262,#55263));
#24497=EDGE_LOOP('',(#55264,#55265,#55266,#55267));
#24498=EDGE_LOOP('',(#55268,#55269,#55270,#55271));
#24499=EDGE_LOOP('',(#55272,#55273,#55274,#55275));
#24500=EDGE_LOOP('',(#55276,#55277,#55278,#55279,#55280));
#24501=EDGE_LOOP('',(#55281,#55282,#55283,#55284,#55285,#55286,#55287,#55288,
#55289));
#24502=EDGE_LOOP('',(#55290,#55291,#55292,#55293,#55294,#55295));
#24503=EDGE_LOOP('',(#55296,#55297,#55298,#55299));
#24504=EDGE_LOOP('',(#55300,#55301,#55302,#55303));
#24505=EDGE_LOOP('',(#55304,#55305,#55306,#55307));
#24506=EDGE_LOOP('',(#55308,#55309,#55310));
#24507=EDGE_LOOP('',(#55311,#55312,#55313,#55314));
#24508=EDGE_LOOP('',(#55315,#55316,#55317));
#24509=EDGE_LOOP('',(#55318,#55319,#55320,#55321));
#24510=EDGE_LOOP('',(#55322,#55323,#55324,#55325));
#24511=EDGE_LOOP('',(#55326,#55327));
#24512=EDGE_LOOP('',(#55328,#55329,#55330));
#24513=EDGE_LOOP('',(#55331,#55332,#55333,#55334,#55335));
#24514=EDGE_LOOP('',(#55336,#55337,#55338,#55339,#55340,#55341,#55342));
#24515=EDGE_LOOP('',(#55343,#55344,#55345,#55346));
#24516=EDGE_LOOP('',(#55347,#55348,#55349,#55350));
#24517=EDGE_LOOP('',(#55351,#55352,#55353));
#24518=EDGE_LOOP('',(#55354,#55355,#55356,#55357,#55358,#55359,#55360,#55361,
#55362));
#24519=EDGE_LOOP('',(#55363,#55364,#55365,#55366));
#24520=EDGE_LOOP('',(#55367,#55368,#55369,#55370));
#24521=EDGE_LOOP('',(#55371,#55372,#55373,#55374));
#24522=EDGE_LOOP('',(#55375,#55376,#55377,#55378));
#24523=EDGE_LOOP('',(#55379,#55380,#55381));
#24524=EDGE_LOOP('',(#55382,#55383,#55384,#55385));
#24525=EDGE_LOOP('',(#55386,#55387,#55388,#55389));
#24526=EDGE_LOOP('',(#55390,#55391,#55392,#55393));
#24527=EDGE_LOOP('',(#55394,#55395,#55396,#55397));
#24528=EDGE_LOOP('',(#55398,#55399,#55400,#55401));
#24529=EDGE_LOOP('',(#55402,#55403,#55404,#55405));
#24530=EDGE_LOOP('',(#55406,#55407,#55408,#55409));
#24531=EDGE_LOOP('',(#55410,#55411,#55412,#55413));
#24532=EDGE_LOOP('',(#55414,#55415,#55416,#55417));
#24533=EDGE_LOOP('',(#55418,#55419,#55420,#55421));
#24534=EDGE_LOOP('',(#55422,#55423,#55424,#55425,#55426,#55427,#55428));
#24535=EDGE_LOOP('',(#55429,#55430,#55431,#55432,#55433,#55434,#55435,#55436));
#24536=EDGE_LOOP('',(#55437,#55438,#55439,#55440,#55441,#55442));
#24537=EDGE_LOOP('',(#55443,#55444,#55445,#55446,#55447));
#24538=EDGE_LOOP('',(#55448,#55449,#55450,#55451));
#24539=EDGE_LOOP('',(#55452,#55453,#55454,#55455));
#24540=EDGE_LOOP('',(#55456,#55457,#55458));
#24541=EDGE_LOOP('',(#55459,#55460,#55461));
#24542=EDGE_LOOP('',(#55462,#55463,#55464,#55465));
#24543=EDGE_LOOP('',(#55466,#55467,#55468,#55469));
#24544=EDGE_LOOP('',(#55470,#55471,#55472,#55473));
#24545=EDGE_LOOP('',(#55474,#55475,#55476,#55477));
#24546=EDGE_LOOP('',(#55478,#55479,#55480,#55481));
#24547=EDGE_LOOP('',(#55482,#55483,#55484,#55485));
#24548=EDGE_LOOP('',(#55486,#55487,#55488,#55489));
#24549=EDGE_LOOP('',(#55490,#55491,#55492));
#24550=EDGE_LOOP('',(#55493,#55494,#55495,#55496));
#24551=EDGE_LOOP('',(#55497,#55498,#55499,#55500));
#24552=EDGE_LOOP('',(#55501,#55502,#55503,#55504,#55505,#55506,#55507,#55508,
#55509,#55510,#55511,#55512,#55513,#55514,#55515,#55516));
#24553=EDGE_LOOP('',(#55517,#55518,#55519,#55520,#55521,#55522));
#24554=EDGE_LOOP('',(#55523,#55524,#55525,#55526,#55527));
#24555=EDGE_LOOP('',(#55528,#55529,#55530,#55531,#55532,#55533,#55534,#55535,
#55536,#55537,#55538,#55539,#55540,#55541,#55542,#55543,#55544));
#24556=EDGE_LOOP('',(#55545,#55546,#55547,#55548,#55549,#55550));
#24557=EDGE_LOOP('',(#55551,#55552,#55553,#55554,#55555,#55556,#55557,#55558,
#55559,#55560,#55561));
#24558=EDGE_LOOP('',(#55562,#55563,#55564,#55565,#55566,#55567));
#24559=EDGE_LOOP('',(#55568,#55569,#55570,#55571));
#24560=EDGE_LOOP('',(#55572,#55573,#55574,#55575,#55576));
#24561=EDGE_LOOP('',(#55577,#55578,#55579,#55580,#55581));
#24562=EDGE_LOOP('',(#55582,#55583,#55584,#55585,#55586));
#24563=EDGE_LOOP('',(#55587,#55588,#55589,#55590,#55591));
#24564=EDGE_LOOP('',(#55592,#55593,#55594,#55595));
#24565=EDGE_LOOP('',(#55596,#55597,#55598,#55599));
#24566=EDGE_LOOP('',(#55600,#55601,#55602,#55603));
#24567=EDGE_LOOP('',(#55604,#55605,#55606,#55607));
#24568=EDGE_LOOP('',(#55608,#55609,#55610,#55611));
#24569=EDGE_LOOP('',(#55612,#55613,#55614,#55615));
#24570=EDGE_LOOP('',(#55616,#55617,#55618,#55619));
#24571=EDGE_LOOP('',(#55620,#55621,#55622,#55623));
#24572=EDGE_LOOP('',(#55624,#55625,#55626,#55627));
#24573=EDGE_LOOP('',(#55628,#55629,#55630,#55631));
#24574=EDGE_LOOP('',(#55632,#55633,#55634,#55635));
#24575=EDGE_LOOP('',(#55636,#55637,#55638,#55639));
#24576=EDGE_LOOP('',(#55640,#55641,#55642,#55643));
#24577=EDGE_LOOP('',(#55644,#55645,#55646,#55647));
#24578=EDGE_LOOP('',(#55648,#55649,#55650,#55651));
#24579=EDGE_LOOP('',(#55652,#55653,#55654,#55655));
#24580=EDGE_LOOP('',(#55656,#55657,#55658,#55659));
#24581=EDGE_LOOP('',(#55660,#55661,#55662,#55663));
#24582=EDGE_LOOP('',(#55664,#55665,#55666,#55667));
#24583=EDGE_LOOP('',(#55668,#55669,#55670,#55671));
#24584=EDGE_LOOP('',(#55672,#55673,#55674,#55675));
#24585=EDGE_LOOP('',(#55676,#55677,#55678,#55679));
#24586=EDGE_LOOP('',(#55680,#55681,#55682,#55683));
#24587=EDGE_LOOP('',(#55684,#55685,#55686,#55687));
#24588=EDGE_LOOP('',(#55688,#55689,#55690));
#24589=EDGE_LOOP('',(#55691,#55692,#55693,#55694));
#24590=EDGE_LOOP('',(#55695,#55696,#55697,#55698));
#24591=EDGE_LOOP('',(#55699,#55700,#55701,#55702));
#24592=EDGE_LOOP('',(#55703,#55704,#55705,#55706));
#24593=EDGE_LOOP('',(#55707,#55708,#55709,#55710));
#24594=EDGE_LOOP('',(#55711,#55712));
#24595=EDGE_LOOP('',(#55713,#55714,#55715,#55716));
#24596=EDGE_LOOP('',(#55717,#55718,#55719,#55720));
#24597=EDGE_LOOP('',(#55721,#55722,#55723));
#24598=EDGE_LOOP('',(#55724,#55725,#55726,#55727));
#24599=EDGE_LOOP('',(#55728,#55729,#55730,#55731));
#24600=EDGE_LOOP('',(#55732,#55733,#55734,#55735));
#24601=EDGE_LOOP('',(#55736,#55737,#55738,#55739));
#24602=EDGE_LOOP('',(#55740,#55741,#55742,#55743));
#24603=EDGE_LOOP('',(#55744,#55745,#55746,#55747,#55748,#55749));
#24604=EDGE_LOOP('',(#55750,#55751,#55752,#55753,#55754,#55755,#55756,#55757,
#55758,#55759));
#24605=EDGE_LOOP('',(#55760,#55761,#55762,#55763,#55764,#55765,#55766,#55767));
#24606=EDGE_LOOP('',(#55768,#55769,#55770,#55771));
#24607=EDGE_LOOP('',(#55772,#55773,#55774,#55775));
#24608=EDGE_LOOP('',(#55776,#55777,#55778,#55779));
#24609=EDGE_LOOP('',(#55780,#55781,#55782,#55783));
#24610=EDGE_LOOP('',(#55784,#55785,#55786,#55787));
#24611=EDGE_LOOP('',(#55788));
#24612=EDGE_LOOP('',(#55789,#55790,#55791,#55792));
#24613=EDGE_LOOP('',(#55793,#55794,#55795,#55796));
#24614=EDGE_LOOP('',(#55797,#55798,#55799,#55800));
#24615=EDGE_LOOP('',(#55801));
#24616=EDGE_LOOP('',(#55802,#55803,#55804,#55805,#55806,#55807,#55808,#55809,
#55810,#55811,#55812,#55813,#55814,#55815));
#24617=EDGE_LOOP('',(#55816,#55817,#55818,#55819,#55820,#55821,#55822,#55823));
#24618=EDGE_LOOP('',(#55824,#55825,#55826,#55827,#55828,#55829,#55830,#55831));
#24619=EDGE_LOOP('',(#55832,#55833,#55834,#55835));
#24620=EDGE_LOOP('',(#55836,#55837,#55838,#55839,#55840));
#24621=EDGE_LOOP('',(#55841,#55842,#55843,#55844,#55845,#55846));
#24622=EDGE_LOOP('',(#55847,#55848,#55849,#55850));
#24623=EDGE_LOOP('',(#55851,#55852,#55853,#55854));
#24624=EDGE_LOOP('',(#55855,#55856,#55857,#55858));
#24625=EDGE_LOOP('',(#55859,#55860,#55861,#55862));
#24626=EDGE_LOOP('',(#55863,#55864,#55865,#55866));
#24627=EDGE_LOOP('',(#55867,#55868,#55869,#55870));
#24628=EDGE_LOOP('',(#55871,#55872,#55873,#55874));
#24629=EDGE_LOOP('',(#55875,#55876,#55877,#55878));
#24630=EDGE_LOOP('',(#55879,#55880,#55881,#55882));
#24631=EDGE_LOOP('',(#55883,#55884,#55885,#55886,#55887,#55888));
#24632=EDGE_LOOP('',(#55889,#55890,#55891,#55892));
#24633=EDGE_LOOP('',(#55893,#55894,#55895,#55896));
#24634=EDGE_LOOP('',(#55897,#55898,#55899,#55900));
#24635=EDGE_LOOP('',(#55901,#55902,#55903,#55904));
#24636=EDGE_LOOP('',(#55905,#55906,#55907,#55908,#55909,#55910));
#24637=EDGE_LOOP('',(#55911,#55912,#55913,#55914));
#24638=EDGE_LOOP('',(#55915,#55916,#55917,#55918));
#24639=EDGE_LOOP('',(#55919,#55920,#55921,#55922));
#24640=EDGE_LOOP('',(#55923,#55924,#55925,#55926));
#24641=EDGE_LOOP('',(#55927,#55928,#55929,#55930));
#24642=EDGE_LOOP('',(#55931,#55932,#55933,#55934));
#24643=EDGE_LOOP('',(#55935,#55936,#55937,#55938));
#24644=EDGE_LOOP('',(#55939,#55940,#55941,#55942));
#24645=EDGE_LOOP('',(#55943,#55944,#55945,#55946));
#24646=EDGE_LOOP('',(#55947,#55948,#55949,#55950));
#24647=EDGE_LOOP('',(#55951,#55952,#55953,#55954));
#24648=EDGE_LOOP('',(#55955,#55956,#55957,#55958));
#24649=EDGE_LOOP('',(#55959,#55960,#55961,#55962));
#24650=EDGE_LOOP('',(#55963,#55964,#55965,#55966,#55967));
#24651=EDGE_LOOP('',(#55968,#55969,#55970,#55971));
#24652=EDGE_LOOP('',(#55972,#55973,#55974,#55975,#55976));
#24653=EDGE_LOOP('',(#55977,#55978,#55979,#55980));
#24654=EDGE_LOOP('',(#55981,#55982,#55983,#55984));
#24655=EDGE_LOOP('',(#55985,#55986,#55987,#55988));
#24656=EDGE_LOOP('',(#55989,#55990,#55991,#55992,#55993,#55994));
#24657=EDGE_LOOP('',(#55995,#55996,#55997,#55998));
#24658=EDGE_LOOP('',(#55999,#56000,#56001,#56002));
#24659=EDGE_LOOP('',(#56003,#56004,#56005,#56006));
#24660=EDGE_LOOP('',(#56007,#56008,#56009));
#24661=EDGE_LOOP('',(#56010,#56011,#56012,#56013));
#24662=EDGE_LOOP('',(#56014,#56015,#56016,#56017));
#24663=EDGE_LOOP('',(#56018,#56019,#56020,#56021));
#24664=EDGE_LOOP('',(#56022,#56023,#56024,#56025));
#24665=EDGE_LOOP('',(#56026,#56027,#56028,#56029));
#24666=EDGE_LOOP('',(#56030,#56031,#56032,#56033));
#24667=EDGE_LOOP('',(#56034,#56035,#56036,#56037));
#24668=EDGE_LOOP('',(#56038,#56039,#56040,#56041));
#24669=EDGE_LOOP('',(#56042,#56043,#56044,#56045));
#24670=EDGE_LOOP('',(#56046,#56047,#56048,#56049));
#24671=EDGE_LOOP('',(#56050,#56051,#56052,#56053));
#24672=EDGE_LOOP('',(#56054,#56055,#56056,#56057,#56058,#56059,#56060,#56061,
#56062));
#24673=EDGE_LOOP('',(#56063,#56064,#56065,#56066));
#24674=EDGE_LOOP('',(#56067,#56068,#56069,#56070,#56071));
#24675=EDGE_LOOP('',(#56072,#56073,#56074,#56075));
#24676=EDGE_LOOP('',(#56076,#56077,#56078,#56079));
#24677=EDGE_LOOP('',(#56080,#56081,#56082,#56083));
#24678=EDGE_LOOP('',(#56084,#56085,#56086,#56087,#56088,#56089,#56090,#56091,
#56092,#56093));
#24679=EDGE_LOOP('',(#56094,#56095,#56096,#56097,#56098,#56099,#56100,#56101));
#24680=EDGE_LOOP('',(#56102,#56103,#56104,#56105,#56106));
#24681=EDGE_LOOP('',(#56107,#56108,#56109,#56110));
#24682=EDGE_LOOP('',(#56111,#56112,#56113,#56114));
#24683=EDGE_LOOP('',(#56115,#56116,#56117,#56118,#56119));
#24684=EDGE_LOOP('',(#56120,#56121,#56122,#56123));
#24685=EDGE_LOOP('',(#56124,#56125,#56126,#56127,#56128));
#24686=EDGE_LOOP('',(#56129,#56130,#56131,#56132,#56133,#56134,#56135,#56136));
#24687=EDGE_LOOP('',(#56137,#56138,#56139,#56140));
#24688=EDGE_LOOP('',(#56141,#56142,#56143));
#24689=EDGE_LOOP('',(#56144,#56145,#56146,#56147,#56148,#56149,#56150,#56151,
#56152,#56153,#56154,#56155,#56156,#56157,#56158,#56159,#56160));
#24690=EDGE_LOOP('',(#56161,#56162,#56163,#56164,#56165,#56166,#56167,#56168,
#56169,#56170,#56171,#56172,#56173,#56174,#56175,#56176,#56177,#56178,#56179));
#24691=EDGE_LOOP('',(#56180,#56181,#56182,#56183,#56184,#56185,#56186,#56187,
#56188,#56189,#56190,#56191,#56192,#56193,#56194,#56195,#56196,#56197));
#24692=EDGE_LOOP('',(#56198,#56199,#56200,#56201,#56202,#56203,#56204,#56205,
#56206,#56207,#56208,#56209,#56210,#56211,#56212,#56213,#56214,#56215));
#24693=EDGE_LOOP('',(#56216,#56217,#56218,#56219));
#24694=EDGE_LOOP('',(#56220,#56221,#56222,#56223));
#24695=EDGE_LOOP('',(#56224,#56225,#56226,#56227));
#24696=EDGE_LOOP('',(#56228,#56229,#56230,#56231));
#24697=EDGE_LOOP('',(#56232,#56233,#56234,#56235));
#24698=EDGE_LOOP('',(#56236,#56237,#56238,#56239));
#24699=EDGE_LOOP('',(#56240,#56241,#56242,#56243));
#24700=EDGE_LOOP('',(#56244));
#24701=EDGE_LOOP('',(#56245,#56246,#56247,#56248,#56249,#56250,#56251,#56252));
#24702=EDGE_LOOP('',(#56253));
#24703=EDGE_LOOP('',(#56254));
#24704=EDGE_LOOP('',(#56255,#56256,#56257,#56258,#56259,#56260));
#24705=EDGE_LOOP('',(#56261,#56262,#56263,#56264,#56265,#56266,#56267,#56268));
#24706=EDGE_LOOP('',(#56269,#56270,#56271,#56272));
#24707=EDGE_LOOP('',(#56273,#56274,#56275,#56276));
#24708=EDGE_LOOP('',(#56277,#56278,#56279,#56280));
#24709=EDGE_LOOP('',(#56281,#56282,#56283,#56284));
#24710=EDGE_LOOP('',(#56285,#56286,#56287,#56288));
#24711=EDGE_LOOP('',(#56289,#56290,#56291,#56292));
#24712=EDGE_LOOP('',(#56293,#56294,#56295));
#24713=EDGE_LOOP('',(#56296));
#24714=EDGE_LOOP('',(#56297));
#24715=EDGE_LOOP('',(#56298));
#24716=EDGE_LOOP('',(#56299));
#24717=EDGE_LOOP('',(#56300));
#24718=EDGE_LOOP('',(#56301));
#24719=EDGE_LOOP('',(#56302));
#24720=EDGE_LOOP('',(#56303,#56304,#56305,#56306));
#24721=EDGE_LOOP('',(#56307,#56308,#56309,#56310));
#24722=EDGE_LOOP('',(#56311,#56312,#56313,#56314,#56315,#56316,#56317,#56318,
#56319,#56320,#56321,#56322,#56323,#56324,#56325,#56326));
#24723=EDGE_LOOP('',(#56327,#56328,#56329,#56330));
#24724=EDGE_LOOP('',(#56331,#56332,#56333,#56334));
#24725=EDGE_LOOP('',(#56335,#56336,#56337,#56338));
#24726=EDGE_LOOP('',(#56339,#56340,#56341,#56342));
#24727=EDGE_LOOP('',(#56343,#56344,#56345,#56346));
#24728=EDGE_LOOP('',(#56347,#56348));
#24729=EDGE_LOOP('',(#56349,#56350));
#24730=EDGE_LOOP('',(#56351,#56352,#56353,#56354));
#24731=EDGE_LOOP('',(#56355,#56356));
#24732=EDGE_LOOP('',(#56357));
#24733=EDGE_LOOP('',(#56358));
#24734=EDGE_LOOP('',(#56359));
#24735=EDGE_LOOP('',(#56360));
#24736=EDGE_LOOP('',(#56361));
#24737=EDGE_LOOP('',(#56362));
#24738=EDGE_LOOP('',(#56363,#56364,#56365,#56366,#56367,#56368,#56369));
#24739=EDGE_LOOP('',(#56370));
#24740=EDGE_LOOP('',(#56371));
#24741=EDGE_LOOP('',(#56372));
#24742=EDGE_LOOP('',(#56373));
#24743=EDGE_LOOP('',(#56374));
#24744=EDGE_LOOP('',(#56375,#56376,#56377,#56378,#56379));
#24745=EDGE_LOOP('',(#56380,#56381,#56382,#56383));
#24746=EDGE_LOOP('',(#56384,#56385,#56386,#56387));
#24747=EDGE_LOOP('',(#56388,#56389,#56390,#56391,#56392,#56393,#56394,#56395,
#56396,#56397,#56398,#56399));
#24748=EDGE_LOOP('',(#56400,#56401,#56402,#56403));
#24749=EDGE_LOOP('',(#56404,#56405,#56406,#56407,#56408));
#24750=EDGE_LOOP('',(#56409,#56410,#56411,#56412,#56413));
#24751=EDGE_LOOP('',(#56414,#56415,#56416));
#24752=EDGE_LOOP('',(#56417,#56418,#56419,#56420));
#24753=EDGE_LOOP('',(#56421,#56422,#56423,#56424,#56425,#56426));
#24754=EDGE_LOOP('',(#56427,#56428,#56429,#56430));
#24755=EDGE_LOOP('',(#56431,#56432,#56433,#56434,#56435,#56436,#56437,#56438,
#56439,#56440));
#24756=EDGE_LOOP('',(#56441,#56442,#56443,#56444,#56445,#56446,#56447,#56448,
#56449,#56450,#56451,#56452,#56453,#56454,#56455,#56456));
#24757=EDGE_LOOP('',(#56457,#56458,#56459,#56460,#56461,#56462,#56463,#56464,
#56465,#56466,#56467,#56468,#56469,#56470,#56471,#56472));
#24758=EDGE_LOOP('',(#56473,#56474,#56475,#56476,#56477));
#24759=EDGE_LOOP('',(#56478,#56479,#56480,#56481));
#24760=EDGE_LOOP('',(#56482,#56483,#56484,#56485));
#24761=EDGE_LOOP('',(#56486,#56487,#56488,#56489));
#24762=EDGE_LOOP('',(#56490,#56491,#56492,#56493));
#24763=EDGE_LOOP('',(#56494,#56495,#56496,#56497));
#24764=EDGE_LOOP('',(#56498,#56499,#56500,#56501));
#24765=EDGE_LOOP('',(#56502,#56503,#56504,#56505));
#24766=EDGE_LOOP('',(#56506,#56507,#56508,#56509));
#24767=EDGE_LOOP('',(#56510,#56511,#56512,#56513));
#24768=EDGE_LOOP('',(#56514,#56515,#56516,#56517,#56518));
#24769=EDGE_LOOP('',(#56519,#56520,#56521,#56522));
#24770=EDGE_LOOP('',(#56523));
#24771=EDGE_LOOP('',(#56524));
#24772=EDGE_LOOP('',(#56525,#56526,#56527,#56528,#56529,#56530,#56531));
#24773=EDGE_LOOP('',(#56532,#56533,#56534,#56535,#56536));
#24774=EDGE_LOOP('',(#56537,#56538,#56539,#56540,#56541,#56542,#56543,#56544,
#56545,#56546,#56547));
#24775=EDGE_LOOP('',(#56548,#56549,#56550));
#24776=EDGE_LOOP('',(#56551,#56552,#56553,#56554));
#24777=EDGE_LOOP('',(#56555,#56556,#56557));
#24778=EDGE_LOOP('',(#56558,#56559,#56560,#56561,#56562,#56563,#56564,#56565,
#56566,#56567,#56568,#56569));
#24779=EDGE_LOOP('',(#56570,#56571,#56572,#56573,#56574,#56575,#56576));
#24780=EDGE_LOOP('',(#56577));
#24781=EDGE_LOOP('',(#56578));
#24782=EDGE_LOOP('',(#56579));
#24783=EDGE_LOOP('',(#56580));
#24784=EDGE_LOOP('',(#56581,#56582,#56583,#56584));
#24785=EDGE_LOOP('',(#56585,#56586,#56587,#56588));
#24786=EDGE_LOOP('',(#56589,#56590,#56591,#56592,#56593,#56594,#56595,#56596,
#56597,#56598,#56599,#56600,#56601,#56602,#56603,#56604));
#24787=EDGE_LOOP('',(#56605,#56606,#56607,#56608));
#24788=EDGE_LOOP('',(#56609,#56610,#56611,#56612));
#24789=EDGE_LOOP('',(#56613,#56614,#56615,#56616));
#24790=EDGE_LOOP('',(#56617,#56618,#56619,#56620));
#24791=EDGE_LOOP('',(#56621,#56622,#56623,#56624));
#24792=EDGE_LOOP('',(#56625,#56626));
#24793=EDGE_LOOP('',(#56627,#56628));
#24794=EDGE_LOOP('',(#56629,#56630,#56631,#56632));
#24795=EDGE_LOOP('',(#56633,#56634));
#24796=EDGE_LOOP('',(#56635));
#24797=EDGE_LOOP('',(#56636));
#24798=EDGE_LOOP('',(#56637));
#24799=EDGE_LOOP('',(#56638));
#24800=EDGE_LOOP('',(#56639));
#24801=EDGE_LOOP('',(#56640));
#24802=EDGE_LOOP('',(#56641,#56642,#56643,#56644,#56645,#56646,#56647));
#24803=EDGE_LOOP('',(#56648));
#24804=EDGE_LOOP('',(#56649));
#24805=EDGE_LOOP('',(#56650));
#24806=EDGE_LOOP('',(#56651));
#24807=EDGE_LOOP('',(#56652));
#24808=EDGE_LOOP('',(#56653,#56654,#56655,#56656));
#24809=EDGE_LOOP('',(#56657,#56658,#56659,#56660));
#24810=EDGE_LOOP('',(#56661,#56662,#56663,#56664));
#24811=EDGE_LOOP('',(#56665,#56666,#56667,#56668));
#24812=EDGE_LOOP('',(#56669,#56670,#56671,#56672));
#24813=EDGE_LOOP('',(#56673,#56674,#56675,#56676));
#24814=EDGE_LOOP('',(#56677,#56678,#56679,#56680));
#24815=EDGE_LOOP('',(#56681));
#24816=EDGE_LOOP('',(#56682));
#24817=EDGE_LOOP('',(#56683));
#24818=EDGE_LOOP('',(#56684,#56685));
#24819=EDGE_LOOP('',(#56686));
#24820=EDGE_LOOP('',(#56687,#56688));
#24821=EDGE_LOOP('',(#56689,#56690,#56691,#56692));
#24822=EDGE_LOOP('',(#56693));
#24823=EDGE_LOOP('',(#56694));
#24824=EDGE_LOOP('',(#56695));
#24825=EDGE_LOOP('',(#56696));
#24826=EDGE_LOOP('',(#56697,#56698,#56699,#56700,#56701));
#24827=EDGE_LOOP('',(#56702,#56703,#56704,#56705));
#24828=EDGE_LOOP('',(#56706,#56707,#56708,#56709));
#24829=EDGE_LOOP('',(#56710,#56711,#56712,#56713,#56714,#56715,#56716,#56717,
#56718,#56719,#56720,#56721));
#24830=EDGE_LOOP('',(#56722,#56723,#56724,#56725));
#24831=EDGE_LOOP('',(#56726,#56727,#56728,#56729,#56730));
#24832=EDGE_LOOP('',(#56731,#56732,#56733,#56734,#56735));
#24833=EDGE_LOOP('',(#56736,#56737,#56738));
#24834=EDGE_LOOP('',(#56739,#56740,#56741,#56742));
#24835=EDGE_LOOP('',(#56743,#56744,#56745,#56746,#56747,#56748));
#24836=EDGE_LOOP('',(#56749,#56750,#56751,#56752));
#24837=EDGE_LOOP('',(#56753,#56754,#56755,#56756,#56757,#56758,#56759,#56760,
#56761,#56762));
#24838=EDGE_LOOP('',(#56763,#56764,#56765,#56766,#56767,#56768,#56769,#56770,
#56771,#56772,#56773,#56774,#56775,#56776,#56777,#56778));
#24839=EDGE_LOOP('',(#56779,#56780,#56781,#56782,#56783,#56784,#56785,#56786,
#56787,#56788,#56789,#56790,#56791,#56792,#56793,#56794));
#24840=EDGE_LOOP('',(#56795,#56796,#56797,#56798,#56799));
#24841=EDGE_LOOP('',(#56800,#56801,#56802,#56803));
#24842=EDGE_LOOP('',(#56804,#56805,#56806,#56807));
#24843=EDGE_LOOP('',(#56808,#56809,#56810,#56811));
#24844=EDGE_LOOP('',(#56812,#56813,#56814,#56815));
#24845=EDGE_LOOP('',(#56816,#56817,#56818,#56819));
#24846=EDGE_LOOP('',(#56820,#56821,#56822,#56823));
#24847=EDGE_LOOP('',(#56824,#56825,#56826,#56827));
#24848=EDGE_LOOP('',(#56828,#56829,#56830,#56831));
#24849=EDGE_LOOP('',(#56832,#56833,#56834,#56835));
#24850=EDGE_LOOP('',(#56836,#56837,#56838,#56839,#56840));
#24851=EDGE_LOOP('',(#56841,#56842,#56843,#56844));
#24852=EDGE_LOOP('',(#56845));
#24853=EDGE_LOOP('',(#56846));
#24854=EDGE_LOOP('',(#56847,#56848,#56849,#56850,#56851,#56852,#56853));
#24855=EDGE_LOOP('',(#56854,#56855,#56856,#56857,#56858));
#24856=EDGE_LOOP('',(#56859,#56860,#56861,#56862,#56863,#56864,#56865,#56866,
#56867,#56868,#56869));
#24857=EDGE_LOOP('',(#56870,#56871,#56872));
#24858=EDGE_LOOP('',(#56873,#56874,#56875,#56876));
#24859=EDGE_LOOP('',(#56877,#56878,#56879));
#24860=EDGE_LOOP('',(#56880,#56881,#56882,#56883,#56884,#56885,#56886,#56887,
#56888,#56889,#56890,#56891));
#24861=EDGE_LOOP('',(#56892,#56893,#56894,#56895,#56896,#56897,#56898));
#24862=EDGE_LOOP('',(#56899));
#24863=EDGE_LOOP('',(#56900));
#24864=EDGE_LOOP('',(#56901));
#24865=EDGE_LOOP('',(#56902));
#24866=EDGE_LOOP('',(#56903,#56904,#56905,#56906,#56907));
#24867=EDGE_LOOP('',(#56908,#56909,#56910,#56911));
#24868=EDGE_LOOP('',(#56912));
#24869=EDGE_LOOP('',(#56913,#56914,#56915,#56916));
#24870=EDGE_LOOP('',(#56917,#56918,#56919,#56920));
#24871=EDGE_LOOP('',(#56921,#56922,#56923,#56924));
#24872=EDGE_LOOP('',(#56925,#56926,#56927));
#24873=EDGE_LOOP('',(#56928,#56929,#56930,#56931));
#24874=EDGE_LOOP('',(#56932,#56933,#56934,#56935));
#24875=EDGE_LOOP('',(#56936,#56937,#56938,#56939,#56940,#56941,#56942,#56943,
#56944,#56945,#56946,#56947));
#24876=EDGE_LOOP('',(#56948,#56949,#56950,#56951));
#24877=EDGE_LOOP('',(#56952,#56953,#56954,#56955));
#24878=EDGE_LOOP('',(#56956,#56957,#56958,#56959));
#24879=EDGE_LOOP('',(#56960,#56961,#56962,#56963,#56964,#56965,#56966,#56967));
#24880=EDGE_LOOP('',(#56968,#56969,#56970,#56971,#56972));
#24881=EDGE_LOOP('',(#56973,#56974,#56975,#56976,#56977,#56978));
#24882=EDGE_LOOP('',(#56979,#56980,#56981,#56982,#56983,#56984));
#24883=EDGE_LOOP('',(#56985,#56986,#56987,#56988,#56989,#56990));
#24884=EDGE_LOOP('',(#56991,#56992,#56993,#56994,#56995,#56996));
#24885=EDGE_LOOP('',(#56997,#56998,#56999,#57000,#57001));
#24886=EDGE_LOOP('',(#57002,#57003,#57004,#57005));
#24887=EDGE_LOOP('',(#57006,#57007,#57008,#57009));
#24888=EDGE_LOOP('',(#57010,#57011,#57012,#57013));
#24889=EDGE_LOOP('',(#57014,#57015,#57016,#57017));
#24890=EDGE_LOOP('',(#57018,#57019,#57020,#57021,#57022));
#24891=EDGE_LOOP('',(#57023,#57024,#57025,#57026,#57027));
#24892=EDGE_LOOP('',(#57028,#57029,#57030,#57031));
#24893=EDGE_LOOP('',(#57032,#57033,#57034,#57035,#57036));
#24894=EDGE_LOOP('',(#57037,#57038,#57039,#57040,#57041));
#24895=EDGE_LOOP('',(#57042,#57043,#57044,#57045));
#24896=EDGE_LOOP('',(#57046,#57047,#57048,#57049));
#24897=EDGE_LOOP('',(#57050,#57051,#57052,#57053));
#24898=EDGE_LOOP('',(#57054,#57055,#57056,#57057));
#24899=EDGE_LOOP('',(#57058,#57059,#57060,#57061));
#24900=EDGE_LOOP('',(#57062));
#24901=EDGE_LOOP('',(#57063));
#24902=EDGE_LOOP('',(#57064));
#24903=EDGE_LOOP('',(#57065));
#24904=EDGE_LOOP('',(#57066));
#24905=EDGE_LOOP('',(#57067));
#24906=EDGE_LOOP('',(#57068));
#24907=EDGE_LOOP('',(#57069));
#24908=EDGE_LOOP('',(#57070));
#24909=EDGE_LOOP('',(#57071));
#24910=EDGE_LOOP('',(#57072,#57073,#57074,#57075,#57076,#57077,#57078,#57079,
#57080,#57081,#57082));
#24911=EDGE_LOOP('',(#57083,#57084,#57085,#57086,#57087,#57088,#57089,#57090,
#57091,#57092));
#24912=EDGE_LOOP('',(#57093,#57094));
#24913=EDGE_LOOP('',(#57095,#57096,#57097,#57098,#57099,#57100));
#24914=EDGE_LOOP('',(#57101,#57102));
#24915=EDGE_LOOP('',(#57103,#57104,#57105,#57106,#57107,#57108));
#24916=EDGE_LOOP('',(#57109));
#24917=EDGE_LOOP('',(#57110));
#24918=EDGE_LOOP('',(#57111,#57112,#57113));
#24919=EDGE_LOOP('',(#57114));
#24920=EDGE_LOOP('',(#57115));
#24921=EDGE_LOOP('',(#57116));
#24922=EDGE_LOOP('',(#57117,#57118,#57119,#57120,#57121));
#24923=EDGE_LOOP('',(#57122,#57123,#57124,#57125));
#24924=EDGE_LOOP('',(#57126));
#24925=EDGE_LOOP('',(#57127,#57128,#57129,#57130));
#24926=EDGE_LOOP('',(#57131,#57132,#57133,#57134));
#24927=EDGE_LOOP('',(#57135,#57136,#57137,#57138));
#24928=EDGE_LOOP('',(#57139,#57140,#57141,#57142));
#24929=EDGE_LOOP('',(#57143,#57144,#57145,#57146));
#24930=EDGE_LOOP('',(#57147,#57148,#57149,#57150));
#24931=EDGE_LOOP('',(#57151,#57152,#57153,#57154));
#24932=EDGE_LOOP('',(#57155));
#24933=EDGE_LOOP('',(#57156));
#24934=EDGE_LOOP('',(#57157));
#24935=EDGE_LOOP('',(#57158,#57159));
#24936=EDGE_LOOP('',(#57160));
#24937=EDGE_LOOP('',(#57161,#57162));
#24938=EDGE_LOOP('',(#57163,#57164,#57165,#57166));
#24939=EDGE_LOOP('',(#57167));
#24940=EDGE_LOOP('',(#57168));
#24941=EDGE_LOOP('',(#57169));
#24942=EDGE_LOOP('',(#57170));
#24943=EDGE_LOOP('',(#57171,#57172,#57173));
#24944=EDGE_LOOP('',(#57174,#57175,#57176,#57177,#57178));
#24945=EDGE_LOOP('',(#57179,#57180,#57181,#57182));
#24946=EDGE_LOOP('',(#57183,#57184,#57185,#57186,#57187));
#24947=EDGE_LOOP('',(#57188,#57189,#57190,#57191,#57192));
#24948=EDGE_LOOP('',(#57193,#57194,#57195,#57196,#57197));
#24949=EDGE_LOOP('',(#57198,#57199,#57200,#57201));
#24950=EDGE_LOOP('',(#57202,#57203,#57204,#57205));
#24951=EDGE_LOOP('',(#57206,#57207,#57208,#57209));
#24952=EDGE_LOOP('',(#57210,#57211,#57212,#57213,#57214,#57215,#57216,#57217,
#57218,#57219,#57220,#57221));
#24953=EDGE_LOOP('',(#57222,#57223,#57224,#57225));
#24954=EDGE_LOOP('',(#57226,#57227,#57228,#57229));
#24955=EDGE_LOOP('',(#57230,#57231,#57232,#57233));
#24956=EDGE_LOOP('',(#57234,#57235,#57236,#57237));
#24957=EDGE_LOOP('',(#57238,#57239,#57240,#57241));
#24958=EDGE_LOOP('',(#57242,#57243,#57244,#57245,#57246,#57247,#57248,#57249,
#57250,#57251,#57252,#57253));
#24959=EDGE_LOOP('',(#57254,#57255,#57256,#57257));
#24960=EDGE_LOOP('',(#57258,#57259,#57260,#57261));
#24961=EDGE_LOOP('',(#57262,#57263,#57264,#57265));
#24962=EDGE_LOOP('',(#57266,#57267,#57268,#57269));
#24963=EDGE_LOOP('',(#57270,#57271,#57272,#57273));
#24964=EDGE_LOOP('',(#57274,#57275,#57276,#57277));
#24965=EDGE_LOOP('',(#57278,#57279,#57280,#57281));
#24966=EDGE_LOOP('',(#57282,#57283,#57284,#57285,#57286));
#24967=EDGE_LOOP('',(#57287,#57288,#57289,#57290,#57291));
#24968=EDGE_LOOP('',(#57292,#57293,#57294,#57295));
#24969=EDGE_LOOP('',(#57296,#57297,#57298,#57299));
#24970=EDGE_LOOP('',(#57300,#57301,#57302,#57303));
#24971=EDGE_LOOP('',(#57304,#57305,#57306,#57307,#57308,#57309,#57310,#57311,
#57312,#57313,#57314,#57315));
#24972=EDGE_LOOP('',(#57316,#57317,#57318,#57319,#57320,#57321));
#24973=EDGE_LOOP('',(#57322,#57323,#57324,#57325));
#24974=EDGE_LOOP('',(#57326,#57327,#57328,#57329,#57330,#57331,#57332));
#24975=EDGE_LOOP('',(#57333,#57334,#57335,#57336,#57337));
#24976=EDGE_LOOP('',(#57338,#57339,#57340,#57341,#57342));
#24977=EDGE_LOOP('',(#57343,#57344,#57345,#57346,#57347,#57348));
#24978=EDGE_LOOP('',(#57349,#57350,#57351,#57352));
#24979=EDGE_LOOP('',(#57353,#57354,#57355,#57356));
#24980=EDGE_LOOP('',(#57357,#57358,#57359,#57360,#57361,#57362));
#24981=EDGE_LOOP('',(#57363,#57364));
#24982=EDGE_LOOP('',(#57365,#57366,#57367));
#24983=EDGE_LOOP('',(#57368));
#24984=EDGE_LOOP('',(#57369));
#24985=EDGE_LOOP('',(#57370,#57371,#57372,#57373,#57374,#57375,#57376,#57377));
#24986=EDGE_LOOP('',(#57378));
#24987=EDGE_LOOP('',(#57379,#57380,#57381,#57382,#57383,#57384,#57385));
#24988=EDGE_LOOP('',(#57386,#57387,#57388));
#24989=EDGE_LOOP('',(#57389,#57390,#57391,#57392,#57393,#57394));
#24990=EDGE_LOOP('',(#57395,#57396,#57397,#57398,#57399,#57400));
#24991=EDGE_LOOP('',(#57401,#57402,#57403,#57404,#57405,#57406));
#24992=EDGE_LOOP('',(#57407));
#24993=EDGE_LOOP('',(#57408));
#24994=EDGE_LOOP('',(#57409));
#24995=EDGE_LOOP('',(#57410,#57411,#57412,#57413));
#24996=EDGE_LOOP('',(#57414));
#24997=EDGE_LOOP('',(#57415,#57416,#57417,#57418));
#24998=EDGE_LOOP('',(#57419,#57420,#57421,#57422,#57423));
#24999=EDGE_LOOP('',(#57424,#57425,#57426,#57427));
#25000=EDGE_LOOP('',(#57428,#57429,#57430,#57431,#57432));
#25001=EDGE_LOOP('',(#57433,#57434,#57435,#57436));
#25002=EDGE_LOOP('',(#57437,#57438,#57439,#57440));
#25003=EDGE_LOOP('',(#57441,#57442,#57443,#57444,#57445));
#25004=EDGE_LOOP('',(#57446,#57447,#57448,#57449));
#25005=EDGE_LOOP('',(#57450,#57451,#57452,#57453,#57454));
#25006=EDGE_LOOP('',(#57455,#57456,#57457,#57458));
#25007=EDGE_LOOP('',(#57459,#57460,#57461,#57462));
#25008=EDGE_LOOP('',(#57463,#57464,#57465,#57466));
#25009=EDGE_LOOP('',(#57467,#57468,#57469,#57470));
#25010=EDGE_LOOP('',(#57471,#57472,#57473,#57474,#57475));
#25011=EDGE_LOOP('',(#57476,#57477,#57478,#57479));
#25012=EDGE_LOOP('',(#57480,#57481,#57482,#57483));
#25013=EDGE_LOOP('',(#57484,#57485,#57486,#57487));
#25014=EDGE_LOOP('',(#57488,#57489,#57490,#57491));
#25015=EDGE_LOOP('',(#57492,#57493,#57494,#57495));
#25016=EDGE_LOOP('',(#57496,#57497,#57498,#57499));
#25017=EDGE_LOOP('',(#57500,#57501,#57502,#57503));
#25018=EDGE_LOOP('',(#57504,#57505,#57506,#57507));
#25019=EDGE_LOOP('',(#57508,#57509,#57510,#57511));
#25020=EDGE_LOOP('',(#57512,#57513,#57514,#57515));
#25021=EDGE_LOOP('',(#57516,#57517,#57518,#57519));
#25022=EDGE_LOOP('',(#57520,#57521,#57522,#57523));
#25023=EDGE_LOOP('',(#57524,#57525,#57526,#57527));
#25024=EDGE_LOOP('',(#57528,#57529,#57530,#57531));
#25025=EDGE_LOOP('',(#57532,#57533,#57534,#57535));
#25026=EDGE_LOOP('',(#57536,#57537,#57538,#57539));
#25027=EDGE_LOOP('',(#57540,#57541,#57542,#57543));
#25028=EDGE_LOOP('',(#57544,#57545,#57546,#57547));
#25029=EDGE_LOOP('',(#57548,#57549,#57550,#57551,#57552));
#25030=EDGE_LOOP('',(#57553,#57554,#57555,#57556));
#25031=EDGE_LOOP('',(#57557,#57558,#57559,#57560,#57561));
#25032=EDGE_LOOP('',(#57562,#57563,#57564,#57565));
#25033=EDGE_LOOP('',(#57566,#57567,#57568,#57569));
#25034=EDGE_LOOP('',(#57570,#57571,#57572,#57573,#57574));
#25035=EDGE_LOOP('',(#57575,#57576,#57577,#57578));
#25036=EDGE_LOOP('',(#57579,#57580,#57581,#57582,#57583));
#25037=EDGE_LOOP('',(#57584,#57585,#57586,#57587));
#25038=EDGE_LOOP('',(#57588,#57589,#57590,#57591));
#25039=EDGE_LOOP('',(#57592,#57593,#57594,#57595,#57596));
#25040=EDGE_LOOP('',(#57597,#57598,#57599,#57600));
#25041=EDGE_LOOP('',(#57601,#57602,#57603,#57604,#57605));
#25042=EDGE_LOOP('',(#57606,#57607,#57608,#57609));
#25043=EDGE_LOOP('',(#57610,#57611,#57612,#57613));
#25044=EDGE_LOOP('',(#57614,#57615,#57616,#57617));
#25045=EDGE_LOOP('',(#57618,#57619,#57620,#57621,#57622));
#25046=EDGE_LOOP('',(#57623,#57624,#57625,#57626,#57627));
#25047=EDGE_LOOP('',(#57628,#57629,#57630));
#25048=EDGE_LOOP('',(#57631,#57632,#57633,#57634));
#25049=EDGE_LOOP('',(#57635,#57636,#57637,#57638));
#25050=EDGE_LOOP('',(#57639,#57640,#57641,#57642));
#25051=EDGE_LOOP('',(#57643,#57644,#57645,#57646));
#25052=EDGE_LOOP('',(#57647,#57648,#57649,#57650));
#25053=EDGE_LOOP('',(#57651,#57652,#57653,#57654,#57655));
#25054=EDGE_LOOP('',(#57656,#57657,#57658,#57659));
#25055=EDGE_LOOP('',(#57660,#57661,#57662,#57663,#57664));
#25056=EDGE_LOOP('',(#57665,#57666,#57667,#57668));
#25057=EDGE_LOOP('',(#57669,#57670,#57671,#57672));
#25058=EDGE_LOOP('',(#57673,#57674,#57675,#57676,#57677));
#25059=EDGE_LOOP('',(#57678,#57679,#57680,#57681));
#25060=EDGE_LOOP('',(#57682,#57683,#57684,#57685,#57686));
#25061=EDGE_LOOP('',(#57687,#57688,#57689,#57690));
#25062=EDGE_LOOP('',(#57691,#57692,#57693,#57694));
#25063=EDGE_LOOP('',(#57695,#57696,#57697,#57698,#57699));
#25064=EDGE_LOOP('',(#57700,#57701,#57702,#57703));
#25065=EDGE_LOOP('',(#57704,#57705,#57706,#57707,#57708));
#25066=EDGE_LOOP('',(#57709,#57710,#57711,#57712));
#25067=EDGE_LOOP('',(#57713,#57714,#57715,#57716));
#25068=EDGE_LOOP('',(#57717,#57718,#57719,#57720,#57721));
#25069=EDGE_LOOP('',(#57722,#57723,#57724,#57725));
#25070=EDGE_LOOP('',(#57726,#57727,#57728,#57729,#57730));
#25071=EDGE_LOOP('',(#57731,#57732,#57733,#57734));
#25072=EDGE_LOOP('',(#57735,#57736,#57737,#57738));
#25073=EDGE_LOOP('',(#57739,#57740,#57741,#57742));
#25074=EDGE_LOOP('',(#57743,#57744,#57745,#57746));
#25075=EDGE_LOOP('',(#57747,#57748,#57749,#57750));
#25076=EDGE_LOOP('',(#57751,#57752,#57753,#57754));
#25077=EDGE_LOOP('',(#57755,#57756,#57757,#57758));
#25078=EDGE_LOOP('',(#57759,#57760,#57761,#57762));
#25079=EDGE_LOOP('',(#57763,#57764,#57765,#57766));
#25080=EDGE_LOOP('',(#57767,#57768,#57769,#57770));
#25081=EDGE_LOOP('',(#57771,#57772,#57773,#57774));
#25082=EDGE_LOOP('',(#57775,#57776,#57777,#57778));
#25083=EDGE_LOOP('',(#57779,#57780,#57781,#57782));
#25084=EDGE_LOOP('',(#57783,#57784,#57785,#57786));
#25085=EDGE_LOOP('',(#57787,#57788,#57789,#57790));
#25086=EDGE_LOOP('',(#57791,#57792,#57793,#57794));
#25087=EDGE_LOOP('',(#57795,#57796,#57797,#57798));
#25088=EDGE_LOOP('',(#57799,#57800,#57801,#57802));
#25089=EDGE_LOOP('',(#57803,#57804,#57805,#57806));
#25090=EDGE_LOOP('',(#57807,#57808,#57809,#57810));
#25091=EDGE_LOOP('',(#57811,#57812,#57813,#57814));
#25092=EDGE_LOOP('',(#57815,#57816,#57817,#57818));
#25093=EDGE_LOOP('',(#57819,#57820,#57821,#57822));
#25094=EDGE_LOOP('',(#57823,#57824,#57825,#57826));
#25095=EDGE_LOOP('',(#57827,#57828,#57829,#57830));
#25096=EDGE_LOOP('',(#57831,#57832,#57833,#57834));
#25097=EDGE_LOOP('',(#57835,#57836,#57837,#57838));
#25098=EDGE_LOOP('',(#57839,#57840,#57841,#57842,#57843));
#25099=EDGE_LOOP('',(#57844,#57845,#57846,#57847,#57848));
#25100=EDGE_LOOP('',(#57849,#57850,#57851));
#25101=EDGE_LOOP('',(#57852,#57853,#57854,#57855));
#25102=EDGE_LOOP('',(#57856,#57857,#57858,#57859,#57860));
#25103=EDGE_LOOP('',(#57861,#57862,#57863,#57864));
#25104=EDGE_LOOP('',(#57865,#57866,#57867,#57868,#57869));
#25105=EDGE_LOOP('',(#57870,#57871,#57872,#57873));
#25106=EDGE_LOOP('',(#57874,#57875,#57876,#57877));
#25107=EDGE_LOOP('',(#57878,#57879,#57880,#57881));
#25108=EDGE_LOOP('',(#57882,#57883,#57884,#57885));
#25109=EDGE_LOOP('',(#57886,#57887,#57888,#57889));
#25110=EDGE_LOOP('',(#57890,#57891,#57892,#57893));
#25111=EDGE_LOOP('',(#57894,#57895,#57896,#57897));
#25112=EDGE_LOOP('',(#57898,#57899,#57900,#57901));
#25113=EDGE_LOOP('',(#57902,#57903,#57904,#57905));
#25114=EDGE_LOOP('',(#57906,#57907,#57908,#57909));
#25115=EDGE_LOOP('',(#57910,#57911,#57912,#57913));
#25116=EDGE_LOOP('',(#57914,#57915,#57916,#57917));
#25117=EDGE_LOOP('',(#57918,#57919,#57920,#57921));
#25118=EDGE_LOOP('',(#57922,#57923,#57924,#57925));
#25119=EDGE_LOOP('',(#57926,#57927,#57928,#57929));
#25120=EDGE_LOOP('',(#57930,#57931,#57932,#57933));
#25121=EDGE_LOOP('',(#57934,#57935,#57936,#57937));
#25122=EDGE_LOOP('',(#57938,#57939,#57940,#57941));
#25123=EDGE_LOOP('',(#57942,#57943,#57944,#57945));
#25124=EDGE_LOOP('',(#57946,#57947,#57948,#57949));
#25125=EDGE_LOOP('',(#57950,#57951,#57952,#57953));
#25126=EDGE_LOOP('',(#57954,#57955,#57956,#57957));
#25127=EDGE_LOOP('',(#57958,#57959,#57960,#57961));
#25128=EDGE_LOOP('',(#57962,#57963,#57964,#57965));
#25129=EDGE_LOOP('',(#57966,#57967,#57968,#57969));
#25130=EDGE_LOOP('',(#57970,#57971,#57972,#57973));
#25131=EDGE_LOOP('',(#57974,#57975,#57976,#57977));
#25132=EDGE_LOOP('',(#57978,#57979,#57980,#57981));
#25133=EDGE_LOOP('',(#57982,#57983,#57984,#57985));
#25134=EDGE_LOOP('',(#57986,#57987,#57988,#57989));
#25135=EDGE_LOOP('',(#57990,#57991,#57992,#57993));
#25136=EDGE_LOOP('',(#57994,#57995,#57996,#57997));
#25137=EDGE_LOOP('',(#57998,#57999,#58000,#58001));
#25138=EDGE_LOOP('',(#58002,#58003,#58004,#58005));
#25139=EDGE_LOOP('',(#58006,#58007,#58008,#58009,#58010));
#25140=EDGE_LOOP('',(#58011,#58012,#58013,#58014));
#25141=EDGE_LOOP('',(#58015,#58016,#58017,#58018,#58019));
#25142=EDGE_LOOP('',(#58020,#58021,#58022,#58023));
#25143=EDGE_LOOP('',(#58024,#58025,#58026,#58027));
#25144=EDGE_LOOP('',(#58028,#58029,#58030,#58031,#58032));
#25145=EDGE_LOOP('',(#58033,#58034,#58035,#58036));
#25146=EDGE_LOOP('',(#58037,#58038,#58039,#58040,#58041));
#25147=EDGE_LOOP('',(#58042,#58043,#58044,#58045));
#25148=EDGE_LOOP('',(#58046,#58047,#58048,#58049));
#25149=EDGE_LOOP('',(#58050,#58051,#58052,#58053));
#25150=EDGE_LOOP('',(#58054,#58055,#58056,#58057));
#25151=EDGE_LOOP('',(#58058,#58059,#58060,#58061));
#25152=EDGE_LOOP('',(#58062,#58063,#58064,#58065));
#25153=EDGE_LOOP('',(#58066,#58067,#58068,#58069));
#25154=EDGE_LOOP('',(#58070,#58071,#58072,#58073));
#25155=EDGE_LOOP('',(#58074,#58075,#58076,#58077));
#25156=EDGE_LOOP('',(#58078,#58079,#58080,#58081));
#25157=EDGE_LOOP('',(#58082,#58083,#58084,#58085));
#25158=EDGE_LOOP('',(#58086,#58087,#58088,#58089));
#25159=EDGE_LOOP('',(#58090,#58091,#58092,#58093));
#25160=EDGE_LOOP('',(#58094,#58095,#58096,#58097));
#25161=EDGE_LOOP('',(#58098,#58099,#58100,#58101));
#25162=EDGE_LOOP('',(#58102,#58103,#58104,#58105));
#25163=EDGE_LOOP('',(#58106,#58107,#58108,#58109));
#25164=EDGE_LOOP('',(#58110,#58111,#58112,#58113));
#25165=EDGE_LOOP('',(#58114,#58115,#58116,#58117));
#25166=EDGE_LOOP('',(#58118,#58119,#58120,#58121));
#25167=EDGE_LOOP('',(#58122,#58123,#58124,#58125));
#25168=EDGE_LOOP('',(#58126,#58127,#58128,#58129));
#25169=EDGE_LOOP('',(#58130,#58131,#58132,#58133));
#25170=EDGE_LOOP('',(#58134,#58135,#58136,#58137));
#25171=EDGE_LOOP('',(#58138,#58139,#58140,#58141));
#25172=EDGE_LOOP('',(#58142,#58143,#58144,#58145));
#25173=EDGE_LOOP('',(#58146,#58147,#58148,#58149));
#25174=EDGE_LOOP('',(#58150,#58151,#58152,#58153));
#25175=EDGE_LOOP('',(#58154,#58155,#58156,#58157));
#25176=EDGE_LOOP('',(#58158,#58159,#58160,#58161));
#25177=EDGE_LOOP('',(#58162,#58163,#58164,#58165));
#25178=EDGE_LOOP('',(#58166,#58167,#58168,#58169));
#25179=EDGE_LOOP('',(#58170,#58171,#58172,#58173));
#25180=EDGE_LOOP('',(#58174,#58175,#58176,#58177));
#25181=EDGE_LOOP('',(#58178,#58179,#58180,#58181));
#25182=EDGE_LOOP('',(#58182,#58183,#58184,#58185));
#25183=EDGE_LOOP('',(#58186,#58187,#58188,#58189));
#25184=EDGE_LOOP('',(#58190,#58191,#58192,#58193));
#25185=EDGE_LOOP('',(#58194,#58195,#58196,#58197));
#25186=EDGE_LOOP('',(#58198,#58199,#58200,#58201));
#25187=EDGE_LOOP('',(#58202,#58203,#58204,#58205));
#25188=EDGE_LOOP('',(#58206,#58207,#58208));
#25189=EDGE_LOOP('',(#58209,#58210,#58211,#58212));
#25190=EDGE_LOOP('',(#58213,#58214,#58215,#58216));
#25191=EDGE_LOOP('',(#58217,#58218,#58219,#58220,#58221));
#25192=EDGE_LOOP('',(#58222,#58223,#58224,#58225,#58226));
#25193=EDGE_LOOP('',(#58227,#58228,#58229,#58230));
#25194=EDGE_LOOP('',(#58231,#58232,#58233,#58234));
#25195=EDGE_LOOP('',(#58235,#58236,#58237,#58238));
#25196=EDGE_LOOP('',(#58239,#58240,#58241,#58242));
#25197=EDGE_LOOP('',(#58243,#58244,#58245,#58246));
#25198=EDGE_LOOP('',(#58247,#58248,#58249,#58250));
#25199=EDGE_LOOP('',(#58251,#58252,#58253,#58254));
#25200=EDGE_LOOP('',(#58255,#58256,#58257,#58258));
#25201=EDGE_LOOP('',(#58259,#58260,#58261,#58262));
#25202=EDGE_LOOP('',(#58263,#58264,#58265,#58266));
#25203=EDGE_LOOP('',(#58267,#58268,#58269,#58270));
#25204=EDGE_LOOP('',(#58271,#58272,#58273,#58274));
#25205=EDGE_LOOP('',(#58275,#58276,#58277,#58278));
#25206=EDGE_LOOP('',(#58279,#58280,#58281,#58282));
#25207=EDGE_LOOP('',(#58283,#58284,#58285,#58286));
#25208=EDGE_LOOP('',(#58287,#58288,#58289,#58290));
#25209=EDGE_LOOP('',(#58291,#58292,#58293,#58294));
#25210=EDGE_LOOP('',(#58295,#58296,#58297,#58298));
#25211=EDGE_LOOP('',(#58299,#58300,#58301,#58302));
#25212=EDGE_LOOP('',(#58303,#58304,#58305,#58306));
#25213=EDGE_LOOP('',(#58307,#58308,#58309,#58310));
#25214=EDGE_LOOP('',(#58311,#58312,#58313,#58314));
#25215=EDGE_LOOP('',(#58315,#58316,#58317,#58318));
#25216=EDGE_LOOP('',(#58319,#58320,#58321,#58322));
#25217=EDGE_LOOP('',(#58323,#58324,#58325,#58326));
#25218=EDGE_LOOP('',(#58327,#58328,#58329,#58330));
#25219=EDGE_LOOP('',(#58331,#58332,#58333,#58334));
#25220=EDGE_LOOP('',(#58335,#58336,#58337,#58338));
#25221=EDGE_LOOP('',(#58339,#58340,#58341,#58342));
#25222=EDGE_LOOP('',(#58343,#58344,#58345,#58346));
#25223=EDGE_LOOP('',(#58347,#58348,#58349,#58350));
#25224=EDGE_LOOP('',(#58351,#58352,#58353,#58354));
#25225=EDGE_LOOP('',(#58355,#58356,#58357,#58358));
#25226=EDGE_LOOP('',(#58359,#58360,#58361,#58362));
#25227=EDGE_LOOP('',(#58363,#58364,#58365,#58366));
#25228=EDGE_LOOP('',(#58367,#58368,#58369,#58370));
#25229=EDGE_LOOP('',(#58371,#58372,#58373,#58374));
#25230=EDGE_LOOP('',(#58375,#58376,#58377,#58378));
#25231=EDGE_LOOP('',(#58379,#58380,#58381,#58382));
#25232=EDGE_LOOP('',(#58383,#58384,#58385,#58386));
#25233=EDGE_LOOP('',(#58387,#58388,#58389,#58390));
#25234=EDGE_LOOP('',(#58391,#58392,#58393,#58394));
#25235=EDGE_LOOP('',(#58395,#58396,#58397,#58398,#58399));
#25236=EDGE_LOOP('',(#58400,#58401,#58402,#58403,#58404));
#25237=EDGE_LOOP('',(#58405,#58406,#58407));
#25238=EDGE_LOOP('',(#58408,#58409,#58410,#58411));
#25239=EDGE_LOOP('',(#58412,#58413,#58414,#58415));
#25240=EDGE_LOOP('',(#58416,#58417,#58418,#58419,#58420));
#25241=EDGE_LOOP('',(#58421,#58422,#58423,#58424,#58425));
#25242=EDGE_LOOP('',(#58426,#58427,#58428));
#25243=EDGE_LOOP('',(#58429,#58430,#58431,#58432));
#25244=EDGE_LOOP('',(#58433,#58434,#58435,#58436));
#25245=EDGE_LOOP('',(#58437,#58438,#58439,#58440));
#25246=EDGE_LOOP('',(#58441,#58442,#58443,#58444));
#25247=EDGE_LOOP('',(#58445,#58446,#58447,#58448));
#25248=EDGE_LOOP('',(#58449,#58450,#58451,#58452));
#25249=EDGE_LOOP('',(#58453,#58454,#58455,#58456));
#25250=EDGE_LOOP('',(#58457,#58458,#58459,#58460));
#25251=EDGE_LOOP('',(#58461,#58462,#58463,#58464));
#25252=EDGE_LOOP('',(#58465,#58466,#58467,#58468));
#25253=EDGE_LOOP('',(#58469,#58470,#58471,#58472));
#25254=EDGE_LOOP('',(#58473,#58474,#58475,#58476));
#25255=EDGE_LOOP('',(#58477,#58478,#58479,#58480));
#25256=EDGE_LOOP('',(#58481,#58482,#58483,#58484));
#25257=EDGE_LOOP('',(#58485,#58486,#58487,#58488));
#25258=EDGE_LOOP('',(#58489,#58490,#58491,#58492));
#25259=EDGE_LOOP('',(#58493,#58494,#58495,#58496));
#25260=EDGE_LOOP('',(#58497,#58498,#58499,#58500));
#25261=EDGE_LOOP('',(#58501,#58502,#58503,#58504));
#25262=EDGE_LOOP('',(#58505,#58506,#58507,#58508));
#25263=EDGE_LOOP('',(#58509,#58510,#58511,#58512));
#25264=EDGE_LOOP('',(#58513,#58514,#58515,#58516));
#25265=EDGE_LOOP('',(#58517,#58518,#58519,#58520));
#25266=EDGE_LOOP('',(#58521,#58522,#58523,#58524));
#25267=EDGE_LOOP('',(#58525,#58526,#58527,#58528));
#25268=EDGE_LOOP('',(#58529,#58530,#58531,#58532));
#25269=EDGE_LOOP('',(#58533,#58534,#58535,#58536));
#25270=EDGE_LOOP('',(#58537,#58538,#58539,#58540));
#25271=EDGE_LOOP('',(#58541,#58542,#58543,#58544));
#25272=EDGE_LOOP('',(#58545,#58546,#58547,#58548));
#25273=EDGE_LOOP('',(#58549,#58550,#58551,#58552));
#25274=EDGE_LOOP('',(#58553,#58554,#58555,#58556));
#25275=EDGE_LOOP('',(#58557,#58558,#58559,#58560));
#25276=EDGE_LOOP('',(#58561,#58562,#58563,#58564));
#25277=EDGE_LOOP('',(#58565,#58566,#58567,#58568));
#25278=EDGE_LOOP('',(#58569,#58570,#58571,#58572));
#25279=EDGE_LOOP('',(#58573,#58574,#58575,#58576));
#25280=EDGE_LOOP('',(#58577,#58578,#58579,#58580));
#25281=EDGE_LOOP('',(#58581,#58582,#58583,#58584));
#25282=EDGE_LOOP('',(#58585,#58586,#58587,#58588));
#25283=EDGE_LOOP('',(#58589,#58590,#58591,#58592));
#25284=EDGE_LOOP('',(#58593,#58594,#58595,#58596));
#25285=EDGE_LOOP('',(#58597,#58598,#58599,#58600));
#25286=EDGE_LOOP('',(#58601,#58602,#58603,#58604));
#25287=EDGE_LOOP('',(#58605,#58606,#58607,#58608));
#25288=EDGE_LOOP('',(#58609,#58610,#58611,#58612));
#25289=EDGE_LOOP('',(#58613,#58614,#58615,#58616));
#25290=EDGE_LOOP('',(#58617,#58618,#58619,#58620));
#25291=EDGE_LOOP('',(#58621,#58622,#58623,#58624));
#25292=EDGE_LOOP('',(#58625,#58626,#58627,#58628));
#25293=EDGE_LOOP('',(#58629,#58630,#58631,#58632));
#25294=EDGE_LOOP('',(#58633,#58634,#58635,#58636));
#25295=EDGE_LOOP('',(#58637,#58638,#58639,#58640));
#25296=EDGE_LOOP('',(#58641,#58642,#58643,#58644));
#25297=EDGE_LOOP('',(#58645,#58646,#58647,#58648));
#25298=EDGE_LOOP('',(#58649,#58650,#58651,#58652));
#25299=EDGE_LOOP('',(#58653,#58654,#58655,#58656));
#25300=EDGE_LOOP('',(#58657,#58658,#58659,#58660));
#25301=EDGE_LOOP('',(#58661,#58662,#58663,#58664));
#25302=EDGE_LOOP('',(#58665,#58666,#58667,#58668));
#25303=EDGE_LOOP('',(#58669,#58670,#58671,#58672));
#25304=EDGE_LOOP('',(#58673,#58674,#58675,#58676));
#25305=EDGE_LOOP('',(#58677,#58678,#58679,#58680));
#25306=EDGE_LOOP('',(#58681,#58682,#58683,#58684));
#25307=EDGE_LOOP('',(#58685,#58686,#58687,#58688));
#25308=EDGE_LOOP('',(#58689,#58690,#58691,#58692));
#25309=EDGE_LOOP('',(#58693,#58694,#58695,#58696));
#25310=EDGE_LOOP('',(#58697,#58698,#58699,#58700));
#25311=EDGE_LOOP('',(#58701,#58702,#58703,#58704));
#25312=EDGE_LOOP('',(#58705,#58706,#58707,#58708));
#25313=EDGE_LOOP('',(#58709,#58710,#58711,#58712));
#25314=EDGE_LOOP('',(#58713,#58714,#58715,#58716));
#25315=EDGE_LOOP('',(#58717,#58718,#58719,#58720));
#25316=EDGE_LOOP('',(#58721,#58722,#58723,#58724));
#25317=EDGE_LOOP('',(#58725,#58726,#58727,#58728));
#25318=EDGE_LOOP('',(#58729,#58730,#58731,#58732));
#25319=EDGE_LOOP('',(#58733,#58734,#58735,#58736));
#25320=EDGE_LOOP('',(#58737,#58738,#58739,#58740));
#25321=EDGE_LOOP('',(#58741,#58742,#58743,#58744));
#25322=EDGE_LOOP('',(#58745,#58746,#58747,#58748));
#25323=EDGE_LOOP('',(#58749,#58750,#58751,#58752));
#25324=EDGE_LOOP('',(#58753,#58754,#58755,#58756));
#25325=EDGE_LOOP('',(#58757,#58758,#58759,#58760));
#25326=EDGE_LOOP('',(#58761,#58762,#58763,#58764));
#25327=EDGE_LOOP('',(#58765,#58766,#58767,#58768));
#25328=EDGE_LOOP('',(#58769,#58770,#58771,#58772));
#25329=EDGE_LOOP('',(#58773,#58774,#58775,#58776));
#25330=EDGE_LOOP('',(#58777,#58778,#58779,#58780));
#25331=EDGE_LOOP('',(#58781,#58782,#58783,#58784));
#25332=EDGE_LOOP('',(#58785,#58786,#58787,#58788));
#25333=EDGE_LOOP('',(#58789,#58790,#58791,#58792));
#25334=EDGE_LOOP('',(#58793,#58794,#58795,#58796));
#25335=EDGE_LOOP('',(#58797,#58798,#58799,#58800));
#25336=EDGE_LOOP('',(#58801,#58802,#58803,#58804));
#25337=EDGE_LOOP('',(#58805,#58806,#58807,#58808));
#25338=EDGE_LOOP('',(#58809,#58810,#58811,#58812));
#25339=EDGE_LOOP('',(#58813,#58814,#58815,#58816));
#25340=EDGE_LOOP('',(#58817,#58818,#58819,#58820));
#25341=EDGE_LOOP('',(#58821,#58822,#58823,#58824));
#25342=EDGE_LOOP('',(#58825,#58826,#58827,#58828));
#25343=EDGE_LOOP('',(#58829,#58830,#58831,#58832));
#25344=EDGE_LOOP('',(#58833,#58834,#58835,#58836));
#25345=EDGE_LOOP('',(#58837,#58838,#58839,#58840));
#25346=EDGE_LOOP('',(#58841,#58842,#58843,#58844));
#25347=EDGE_LOOP('',(#58845,#58846,#58847,#58848));
#25348=EDGE_LOOP('',(#58849,#58850,#58851,#58852));
#25349=EDGE_LOOP('',(#58853,#58854,#58855,#58856));
#25350=EDGE_LOOP('',(#58857,#58858,#58859,#58860));
#25351=EDGE_LOOP('',(#58861,#58862,#58863,#58864));
#25352=EDGE_LOOP('',(#58865,#58866,#58867,#58868));
#25353=EDGE_LOOP('',(#58869,#58870,#58871,#58872));
#25354=EDGE_LOOP('',(#58873,#58874,#58875,#58876));
#25355=EDGE_LOOP('',(#58877,#58878,#58879,#58880));
#25356=EDGE_LOOP('',(#58881,#58882,#58883,#58884));
#25357=EDGE_LOOP('',(#58885,#58886,#58887,#58888));
#25358=EDGE_LOOP('',(#58889,#58890,#58891,#58892));
#25359=EDGE_LOOP('',(#58893,#58894,#58895,#58896));
#25360=EDGE_LOOP('',(#58897,#58898,#58899,#58900));
#25361=EDGE_LOOP('',(#58901,#58902,#58903,#58904));
#25362=EDGE_LOOP('',(#58905,#58906,#58907,#58908));
#25363=EDGE_LOOP('',(#58909,#58910,#58911,#58912));
#25364=EDGE_LOOP('',(#58913,#58914,#58915,#58916));
#25365=EDGE_LOOP('',(#58917,#58918,#58919,#58920));
#25366=EDGE_LOOP('',(#58921,#58922,#58923,#58924));
#25367=EDGE_LOOP('',(#58925,#58926,#58927,#58928));
#25368=EDGE_LOOP('',(#58929,#58930,#58931,#58932));
#25369=EDGE_LOOP('',(#58933,#58934,#58935,#58936));
#25370=EDGE_LOOP('',(#58937,#58938,#58939,#58940));
#25371=EDGE_LOOP('',(#58941,#58942,#58943,#58944));
#25372=EDGE_LOOP('',(#58945,#58946,#58947,#58948));
#25373=EDGE_LOOP('',(#58949,#58950,#58951,#58952));
#25374=EDGE_LOOP('',(#58953,#58954,#58955,#58956));
#25375=EDGE_LOOP('',(#58957,#58958,#58959,#58960));
#25376=EDGE_LOOP('',(#58961,#58962,#58963,#58964));
#25377=EDGE_LOOP('',(#58965,#58966,#58967,#58968));
#25378=EDGE_LOOP('',(#58969,#58970,#58971,#58972));
#25379=EDGE_LOOP('',(#58973,#58974,#58975,#58976));
#25380=EDGE_LOOP('',(#58977,#58978,#58979,#58980));
#25381=EDGE_LOOP('',(#58981,#58982,#58983,#58984));
#25382=EDGE_LOOP('',(#58985,#58986,#58987,#58988));
#25383=EDGE_LOOP('',(#58989,#58990,#58991,#58992));
#25384=EDGE_LOOP('',(#58993,#58994,#58995,#58996));
#25385=EDGE_LOOP('',(#58997,#58998,#58999,#59000));
#25386=EDGE_LOOP('',(#59001,#59002,#59003,#59004));
#25387=EDGE_LOOP('',(#59005,#59006,#59007,#59008));
#25388=EDGE_LOOP('',(#59009,#59010,#59011,#59012));
#25389=EDGE_LOOP('',(#59013,#59014,#59015,#59016));
#25390=EDGE_LOOP('',(#59017,#59018,#59019,#59020));
#25391=EDGE_LOOP('',(#59021,#59022,#59023,#59024));
#25392=EDGE_LOOP('',(#59025,#59026,#59027,#59028));
#25393=EDGE_LOOP('',(#59029,#59030,#59031,#59032));
#25394=EDGE_LOOP('',(#59033,#59034,#59035,#59036));
#25395=EDGE_LOOP('',(#59037,#59038,#59039,#59040));
#25396=EDGE_LOOP('',(#59041,#59042,#59043,#59044));
#25397=EDGE_LOOP('',(#59045,#59046,#59047,#59048));
#25398=EDGE_LOOP('',(#59049,#59050,#59051,#59052));
#25399=EDGE_LOOP('',(#59053,#59054,#59055,#59056));
#25400=EDGE_LOOP('',(#59057,#59058,#59059,#59060));
#25401=EDGE_LOOP('',(#59061,#59062,#59063,#59064));
#25402=EDGE_LOOP('',(#59065,#59066,#59067,#59068));
#25403=EDGE_LOOP('',(#59069,#59070,#59071,#59072));
#25404=EDGE_LOOP('',(#59073,#59074,#59075,#59076));
#25405=EDGE_LOOP('',(#59077,#59078,#59079,#59080));
#25406=EDGE_LOOP('',(#59081,#59082,#59083,#59084));
#25407=EDGE_LOOP('',(#59085,#59086,#59087,#59088));
#25408=EDGE_LOOP('',(#59089,#59090,#59091,#59092));
#25409=EDGE_LOOP('',(#59093,#59094,#59095,#59096));
#25410=EDGE_LOOP('',(#59097,#59098,#59099,#59100));
#25411=EDGE_LOOP('',(#59101,#59102,#59103,#59104));
#25412=EDGE_LOOP('',(#59105,#59106,#59107,#59108));
#25413=EDGE_LOOP('',(#59109,#59110,#59111,#59112));
#25414=EDGE_LOOP('',(#59113,#59114,#59115,#59116));
#25415=EDGE_LOOP('',(#59117,#59118,#59119,#59120));
#25416=EDGE_LOOP('',(#59121,#59122,#59123,#59124));
#25417=EDGE_LOOP('',(#59125,#59126,#59127,#59128));
#25418=EDGE_LOOP('',(#59129,#59130,#59131,#59132));
#25419=EDGE_LOOP('',(#59133,#59134,#59135,#59136));
#25420=EDGE_LOOP('',(#59137,#59138,#59139,#59140));
#25421=EDGE_LOOP('',(#59141,#59142,#59143,#59144));
#25422=EDGE_LOOP('',(#59145,#59146,#59147,#59148));
#25423=EDGE_LOOP('',(#59149,#59150,#59151,#59152));
#25424=EDGE_LOOP('',(#59153,#59154,#59155,#59156));
#25425=EDGE_LOOP('',(#59157,#59158,#59159,#59160));
#25426=EDGE_LOOP('',(#59161,#59162,#59163,#59164));
#25427=EDGE_LOOP('',(#59165,#59166,#59167,#59168));
#25428=EDGE_LOOP('',(#59169,#59170,#59171,#59172));
#25429=EDGE_LOOP('',(#59173,#59174,#59175,#59176));
#25430=EDGE_LOOP('',(#59177,#59178,#59179,#59180));
#25431=EDGE_LOOP('',(#59181,#59182,#59183,#59184));
#25432=EDGE_LOOP('',(#59185,#59186,#59187,#59188));
#25433=EDGE_LOOP('',(#59189,#59190,#59191,#59192));
#25434=EDGE_LOOP('',(#59193,#59194,#59195,#59196));
#25435=EDGE_LOOP('',(#59197,#59198,#59199,#59200));
#25436=EDGE_LOOP('',(#59201,#59202,#59203,#59204));
#25437=EDGE_LOOP('',(#59205,#59206,#59207,#59208));
#25438=EDGE_LOOP('',(#59209,#59210,#59211,#59212));
#25439=EDGE_LOOP('',(#59213,#59214,#59215,#59216));
#25440=EDGE_LOOP('',(#59217,#59218,#59219,#59220));
#25441=EDGE_LOOP('',(#59221,#59222,#59223,#59224));
#25442=EDGE_LOOP('',(#59225,#59226,#59227,#59228));
#25443=EDGE_LOOP('',(#59229,#59230,#59231,#59232));
#25444=EDGE_LOOP('',(#59233,#59234,#59235,#59236));
#25445=EDGE_LOOP('',(#59237,#59238,#59239,#59240));
#25446=EDGE_LOOP('',(#59241,#59242,#59243,#59244));
#25447=EDGE_LOOP('',(#59245,#59246,#59247,#59248));
#25448=EDGE_LOOP('',(#59249,#59250,#59251,#59252));
#25449=EDGE_LOOP('',(#59253,#59254,#59255,#59256));
#25450=EDGE_LOOP('',(#59257,#59258,#59259,#59260));
#25451=EDGE_LOOP('',(#59261,#59262,#59263,#59264));
#25452=EDGE_LOOP('',(#59265,#59266,#59267,#59268));
#25453=EDGE_LOOP('',(#59269,#59270,#59271,#59272));
#25454=EDGE_LOOP('',(#59273,#59274,#59275,#59276));
#25455=EDGE_LOOP('',(#59277,#59278,#59279,#59280));
#25456=EDGE_LOOP('',(#59281,#59282,#59283,#59284));
#25457=EDGE_LOOP('',(#59285,#59286,#59287,#59288));
#25458=EDGE_LOOP('',(#59289,#59290,#59291,#59292));
#25459=EDGE_LOOP('',(#59293,#59294,#59295,#59296));
#25460=EDGE_LOOP('',(#59297,#59298,#59299,#59300));
#25461=EDGE_LOOP('',(#59301,#59302,#59303,#59304));
#25462=EDGE_LOOP('',(#59305,#59306,#59307,#59308));
#25463=EDGE_LOOP('',(#59309,#59310,#59311,#59312));
#25464=EDGE_LOOP('',(#59313,#59314,#59315,#59316));
#25465=EDGE_LOOP('',(#59317,#59318,#59319,#59320));
#25466=EDGE_LOOP('',(#59321,#59322,#59323,#59324));
#25467=EDGE_LOOP('',(#59325,#59326,#59327,#59328));
#25468=EDGE_LOOP('',(#59329,#59330,#59331,#59332));
#25469=EDGE_LOOP('',(#59333,#59334,#59335,#59336));
#25470=EDGE_LOOP('',(#59337,#59338,#59339,#59340));
#25471=EDGE_LOOP('',(#59341,#59342,#59343,#59344));
#25472=EDGE_LOOP('',(#59345,#59346,#59347,#59348));
#25473=EDGE_LOOP('',(#59349,#59350,#59351,#59352));
#25474=EDGE_LOOP('',(#59353,#59354,#59355,#59356));
#25475=EDGE_LOOP('',(#59357,#59358,#59359,#59360));
#25476=EDGE_LOOP('',(#59361,#59362,#59363,#59364));
#25477=EDGE_LOOP('',(#59365,#59366,#59367,#59368));
#25478=EDGE_LOOP('',(#59369,#59370,#59371,#59372));
#25479=EDGE_LOOP('',(#59373,#59374,#59375,#59376));
#25480=EDGE_LOOP('',(#59377,#59378,#59379,#59380));
#25481=EDGE_LOOP('',(#59381,#59382,#59383,#59384));
#25482=EDGE_LOOP('',(#59385,#59386,#59387,#59388));
#25483=EDGE_LOOP('',(#59389,#59390,#59391,#59392));
#25484=EDGE_LOOP('',(#59393,#59394,#59395,#59396));
#25485=EDGE_LOOP('',(#59397,#59398,#59399,#59400));
#25486=EDGE_LOOP('',(#59401,#59402,#59403,#59404));
#25487=EDGE_LOOP('',(#59405,#59406,#59407,#59408));
#25488=EDGE_LOOP('',(#59409,#59410,#59411,#59412));
#25489=EDGE_LOOP('',(#59413,#59414,#59415,#59416));
#25490=EDGE_LOOP('',(#59417,#59418,#59419,#59420));
#25491=EDGE_LOOP('',(#59421,#59422,#59423,#59424));
#25492=EDGE_LOOP('',(#59425,#59426,#59427,#59428));
#25493=EDGE_LOOP('',(#59429,#59430,#59431,#59432));
#25494=EDGE_LOOP('',(#59433,#59434,#59435,#59436));
#25495=EDGE_LOOP('',(#59437,#59438,#59439,#59440));
#25496=EDGE_LOOP('',(#59441,#59442,#59443,#59444));
#25497=EDGE_LOOP('',(#59445,#59446,#59447,#59448));
#25498=EDGE_LOOP('',(#59449,#59450,#59451,#59452));
#25499=EDGE_LOOP('',(#59453,#59454,#59455,#59456));
#25500=EDGE_LOOP('',(#59457,#59458,#59459,#59460));
#25501=EDGE_LOOP('',(#59461,#59462,#59463,#59464));
#25502=EDGE_LOOP('',(#59465,#59466,#59467,#59468));
#25503=EDGE_LOOP('',(#59469,#59470,#59471,#59472));
#25504=EDGE_LOOP('',(#59473,#59474,#59475,#59476));
#25505=EDGE_LOOP('',(#59477,#59478,#59479,#59480));
#25506=EDGE_LOOP('',(#59481,#59482,#59483,#59484));
#25507=EDGE_LOOP('',(#59485,#59486,#59487,#59488));
#25508=EDGE_LOOP('',(#59489,#59490,#59491,#59492));
#25509=EDGE_LOOP('',(#59493,#59494,#59495,#59496));
#25510=EDGE_LOOP('',(#59497,#59498,#59499,#59500));
#25511=EDGE_LOOP('',(#59501,#59502,#59503,#59504));
#25512=EDGE_LOOP('',(#59505,#59506,#59507,#59508));
#25513=EDGE_LOOP('',(#59509,#59510,#59511,#59512));
#25514=EDGE_LOOP('',(#59513,#59514,#59515,#59516));
#25515=EDGE_LOOP('',(#59517,#59518,#59519,#59520));
#25516=EDGE_LOOP('',(#59521,#59522,#59523,#59524));
#25517=EDGE_LOOP('',(#59525,#59526,#59527,#59528));
#25518=EDGE_LOOP('',(#59529,#59530,#59531,#59532));
#25519=EDGE_LOOP('',(#59533,#59534,#59535,#59536));
#25520=EDGE_LOOP('',(#59537,#59538,#59539,#59540));
#25521=EDGE_LOOP('',(#59541,#59542,#59543,#59544));
#25522=EDGE_LOOP('',(#59545,#59546,#59547,#59548));
#25523=EDGE_LOOP('',(#59549,#59550,#59551,#59552));
#25524=EDGE_LOOP('',(#59553,#59554,#59555,#59556,#59557));
#25525=EDGE_LOOP('',(#59558,#59559,#59560,#59561));
#25526=EDGE_LOOP('',(#59562,#59563,#59564,#59565));
#25527=EDGE_LOOP('',(#59566,#59567,#59568,#59569));
#25528=EDGE_LOOP('',(#59570,#59571,#59572,#59573));
#25529=EDGE_LOOP('',(#59574,#59575,#59576,#59577,#59578));
#25530=EDGE_LOOP('',(#59579,#59580,#59581,#59582));
#25531=EDGE_LOOP('',(#59583,#59584,#59585,#59586,#59587));
#25532=EDGE_LOOP('',(#59588,#59589,#59590,#59591));
#25533=EDGE_LOOP('',(#59592,#59593,#59594,#59595));
#25534=EDGE_LOOP('',(#59596,#59597,#59598,#59599,#59600));
#25535=EDGE_LOOP('',(#59601,#59602,#59603,#59604));
#25536=EDGE_LOOP('',(#59605,#59606,#59607,#59608,#59609));
#25537=EDGE_LOOP('',(#59610,#59611,#59612,#59613));
#25538=EDGE_LOOP('',(#59614,#59615,#59616,#59617));
#25539=EDGE_LOOP('',(#59618,#59619,#59620,#59621,#59622));
#25540=EDGE_LOOP('',(#59623,#59624,#59625,#59626));
#25541=EDGE_LOOP('',(#59627,#59628,#59629,#59630,#59631));
#25542=EDGE_LOOP('',(#59632,#59633,#59634,#59635));
#25543=EDGE_LOOP('',(#59636,#59637,#59638,#59639));
#25544=EDGE_LOOP('',(#59640,#59641,#59642,#59643,#59644));
#25545=EDGE_LOOP('',(#59645,#59646,#59647,#59648));
#25546=EDGE_LOOP('',(#59649,#59650,#59651,#59652,#59653));
#25547=EDGE_LOOP('',(#59654,#59655,#59656,#59657));
#25548=EDGE_LOOP('',(#59658,#59659,#59660,#59661,#59662));
#25549=EDGE_LOOP('',(#59663,#59664,#59665,#59666));
#25550=EDGE_LOOP('',(#59667,#59668,#59669,#59670));
#25551=EDGE_LOOP('',(#59671,#59672,#59673,#59674,#59675));
#25552=EDGE_LOOP('',(#59676,#59677,#59678,#59679,#59680));
#25553=EDGE_LOOP('',(#59681,#59682,#59683,#59684,#59685));
#25554=EDGE_LOOP('',(#59686,#59687,#59688,#59689));
#25555=EDGE_LOOP('',(#59690,#59691,#59692,#59693));
#25556=EDGE_LOOP('',(#59694,#59695,#59696,#59697,#59698));
#25557=EDGE_LOOP('',(#59699,#59700,#59701,#59702,#59703));
#25558=EDGE_LOOP('',(#59704,#59705,#59706,#59707));
#25559=EDGE_LOOP('',(#59708,#59709,#59710,#59711,#59712));
#25560=EDGE_LOOP('',(#59713,#59714,#59715,#59716));
#25561=EDGE_LOOP('',(#59717,#59718,#59719,#59720,#59721));
#25562=EDGE_LOOP('',(#59722,#59723,#59724,#59725));
#25563=EDGE_LOOP('',(#59726,#59727,#59728,#59729));
#25564=EDGE_LOOP('',(#59730,#59731,#59732,#59733,#59734));
#25565=EDGE_LOOP('',(#59735,#59736,#59737,#59738));
#25566=EDGE_LOOP('',(#59739,#59740,#59741,#59742,#59743));
#25567=EDGE_LOOP('',(#59744,#59745,#59746,#59747));
#25568=EDGE_LOOP('',(#59748,#59749,#59750,#59751));
#25569=EDGE_LOOP('',(#59752,#59753,#59754,#59755,#59756));
#25570=EDGE_LOOP('',(#59757,#59758,#59759,#59760));
#25571=EDGE_LOOP('',(#59761,#59762,#59763,#59764,#59765));
#25572=EDGE_LOOP('',(#59766,#59767,#59768,#59769));
#25573=EDGE_LOOP('',(#59770,#59771,#59772,#59773));
#25574=EDGE_LOOP('',(#59774,#59775,#59776,#59777));
#25575=EDGE_LOOP('',(#59778,#59779,#59780,#59781));
#25576=EDGE_LOOP('',(#59782,#59783,#59784,#59785));
#25577=EDGE_LOOP('',(#59786,#59787,#59788,#59789));
#25578=EDGE_LOOP('',(#59790,#59791,#59792,#59793));
#25579=EDGE_LOOP('',(#59794,#59795,#59796,#59797));
#25580=EDGE_LOOP('',(#59798,#59799,#59800,#59801));
#25581=EDGE_LOOP('',(#59802,#59803,#59804,#59805));
#25582=EDGE_LOOP('',(#59806,#59807,#59808,#59809));
#25583=EDGE_LOOP('',(#59810,#59811,#59812,#59813));
#25584=EDGE_LOOP('',(#59814,#59815,#59816,#59817));
#25585=EDGE_LOOP('',(#59818,#59819,#59820,#59821));
#25586=EDGE_LOOP('',(#59822,#59823,#59824,#59825));
#25587=EDGE_LOOP('',(#59826,#59827,#59828,#59829));
#25588=EDGE_LOOP('',(#59830,#59831,#59832,#59833));
#25589=EDGE_LOOP('',(#59834,#59835,#59836,#59837));
#25590=EDGE_LOOP('',(#59838,#59839,#59840,#59841));
#25591=EDGE_LOOP('',(#59842,#59843,#59844,#59845));
#25592=EDGE_LOOP('',(#59846,#59847,#59848,#59849));
#25593=EDGE_LOOP('',(#59850,#59851,#59852,#59853));
#25594=EDGE_LOOP('',(#59854,#59855,#59856,#59857));
#25595=EDGE_LOOP('',(#59858,#59859,#59860,#59861));
#25596=EDGE_LOOP('',(#59862,#59863,#59864,#59865));
#25597=EDGE_LOOP('',(#59866,#59867,#59868,#59869));
#25598=EDGE_LOOP('',(#59870,#59871,#59872,#59873));
#25599=EDGE_LOOP('',(#59874,#59875,#59876,#59877));
#25600=EDGE_LOOP('',(#59878,#59879,#59880,#59881));
#25601=EDGE_LOOP('',(#59882,#59883,#59884,#59885));
#25602=EDGE_LOOP('',(#59886,#59887,#59888,#59889));
#25603=EDGE_LOOP('',(#59890,#59891,#59892,#59893));
#25604=EDGE_LOOP('',(#59894,#59895,#59896,#59897));
#25605=EDGE_LOOP('',(#59898,#59899,#59900,#59901,#59902));
#25606=EDGE_LOOP('',(#59903,#59904,#59905,#59906));
#25607=EDGE_LOOP('',(#59907,#59908,#59909,#59910));
#25608=EDGE_LOOP('',(#59911,#59912,#59913,#59914,#59915));
#25609=EDGE_LOOP('',(#59916,#59917,#59918,#59919,#59920));
#25610=EDGE_LOOP('',(#59921,#59922,#59923,#59924,#59925));
#25611=EDGE_LOOP('',(#59926,#59927,#59928,#59929));
#25612=EDGE_LOOP('',(#59930,#59931,#59932,#59933));
#25613=EDGE_LOOP('',(#59934,#59935,#59936,#59937,#59938));
#25614=EDGE_LOOP('',(#59939,#59940,#59941,#59942,#59943));
#25615=EDGE_LOOP('',(#59944,#59945,#59946,#59947));
#25616=EDGE_LOOP('',(#59948,#59949,#59950,#59951));
#25617=EDGE_LOOP('',(#59952,#59953,#59954,#59955));
#25618=EDGE_LOOP('',(#59956,#59957,#59958,#59959));
#25619=EDGE_LOOP('',(#59960,#59961,#59962,#59963));
#25620=EDGE_LOOP('',(#59964,#59965,#59966,#59967));
#25621=EDGE_LOOP('',(#59968,#59969,#59970,#59971));
#25622=EDGE_LOOP('',(#59972,#59973,#59974,#59975));
#25623=EDGE_LOOP('',(#59976,#59977,#59978,#59979));
#25624=EDGE_LOOP('',(#59980,#59981,#59982,#59983));
#25625=EDGE_LOOP('',(#59984,#59985,#59986,#59987));
#25626=EDGE_LOOP('',(#59988,#59989,#59990,#59991));
#25627=EDGE_LOOP('',(#59992,#59993,#59994,#59995));
#25628=EDGE_LOOP('',(#59996,#59997,#59998,#59999));
#25629=EDGE_LOOP('',(#60000,#60001,#60002,#60003));
#25630=EDGE_LOOP('',(#60004,#60005,#60006,#60007));
#25631=EDGE_LOOP('',(#60008,#60009,#60010,#60011));
#25632=EDGE_LOOP('',(#60012,#60013,#60014,#60015));
#25633=EDGE_LOOP('',(#60016,#60017,#60018,#60019,#60020));
#25634=EDGE_LOOP('',(#60021,#60022,#60023,#60024,#60025));
#25635=EDGE_LOOP('',(#60026,#60027,#60028));
#25636=EDGE_LOOP('',(#60029,#60030,#60031,#60032));
#25637=EDGE_LOOP('',(#60033,#60034,#60035,#60036,#60037));
#25638=EDGE_LOOP('',(#60038,#60039,#60040,#60041));
#25639=EDGE_LOOP('',(#60042,#60043,#60044,#60045,#60046));
#25640=EDGE_LOOP('',(#60047,#60048,#60049,#60050));
#25641=EDGE_LOOP('',(#60051,#60052,#60053,#60054));
#25642=EDGE_LOOP('',(#60055,#60056,#60057,#60058,#60059));
#25643=EDGE_LOOP('',(#60060,#60061,#60062,#60063));
#25644=EDGE_LOOP('',(#60064,#60065,#60066,#60067,#60068));
#25645=EDGE_LOOP('',(#60069,#60070,#60071,#60072));
#25646=EDGE_LOOP('',(#60073,#60074,#60075,#60076));
#25647=EDGE_LOOP('',(#60077,#60078,#60079,#60080));
#25648=EDGE_LOOP('',(#60081,#60082,#60083,#60084,#60085));
#25649=EDGE_LOOP('',(#60086,#60087,#60088,#60089,#60090));
#25650=EDGE_LOOP('',(#60091,#60092,#60093));
#25651=EDGE_LOOP('',(#60094,#60095,#60096,#60097));
#25652=EDGE_LOOP('',(#60098,#60099,#60100,#60101));
#25653=EDGE_LOOP('',(#60102,#60103,#60104,#60105));
#25654=EDGE_LOOP('',(#60106,#60107,#60108,#60109));
#25655=EDGE_LOOP('',(#60110,#60111,#60112,#60113));
#25656=EDGE_LOOP('',(#60114,#60115,#60116,#60117));
#25657=EDGE_LOOP('',(#60118,#60119,#60120,#60121));
#25658=EDGE_LOOP('',(#60122,#60123,#60124,#60125));
#25659=EDGE_LOOP('',(#60126,#60127,#60128,#60129));
#25660=EDGE_LOOP('',(#60130,#60131,#60132,#60133));
#25661=EDGE_LOOP('',(#60134,#60135,#60136,#60137));
#25662=EDGE_LOOP('',(#60138,#60139,#60140,#60141));
#25663=EDGE_LOOP('',(#60142,#60143,#60144,#60145));
#25664=EDGE_LOOP('',(#60146,#60147,#60148,#60149));
#25665=EDGE_LOOP('',(#60150,#60151,#60152,#60153));
#25666=EDGE_LOOP('',(#60154,#60155,#60156,#60157));
#25667=EDGE_LOOP('',(#60158,#60159,#60160,#60161));
#25668=EDGE_LOOP('',(#60162,#60163,#60164,#60165));
#25669=EDGE_LOOP('',(#60166,#60167,#60168,#60169));
#25670=EDGE_LOOP('',(#60170,#60171,#60172,#60173));
#25671=EDGE_LOOP('',(#60174,#60175,#60176,#60177));
#25672=EDGE_LOOP('',(#60178,#60179,#60180,#60181));
#25673=EDGE_LOOP('',(#60182,#60183,#60184,#60185));
#25674=EDGE_LOOP('',(#60186,#60187,#60188,#60189));
#25675=EDGE_LOOP('',(#60190,#60191,#60192,#60193));
#25676=EDGE_LOOP('',(#60194,#60195,#60196,#60197));
#25677=EDGE_LOOP('',(#60198,#60199,#60200,#60201));
#25678=EDGE_LOOP('',(#60202,#60203,#60204,#60205));
#25679=EDGE_LOOP('',(#60206,#60207,#60208,#60209));
#25680=EDGE_LOOP('',(#60210,#60211,#60212,#60213));
#25681=EDGE_LOOP('',(#60214,#60215,#60216,#60217));
#25682=EDGE_LOOP('',(#60218,#60219,#60220,#60221));
#25683=EDGE_LOOP('',(#60222,#60223,#60224,#60225));
#25684=EDGE_LOOP('',(#60226,#60227,#60228,#60229));
#25685=EDGE_LOOP('',(#60230,#60231,#60232,#60233));
#25686=EDGE_LOOP('',(#60234,#60235,#60236,#60237));
#25687=EDGE_LOOP('',(#60238,#60239,#60240,#60241));
#25688=EDGE_LOOP('',(#60242,#60243,#60244,#60245));
#25689=EDGE_LOOP('',(#60246,#60247,#60248,#60249));
#25690=EDGE_LOOP('',(#60250,#60251,#60252,#60253));
#25691=EDGE_LOOP('',(#60254,#60255,#60256,#60257));
#25692=EDGE_LOOP('',(#60258,#60259,#60260,#60261));
#25693=EDGE_LOOP('',(#60262,#60263,#60264,#60265,#60266));
#25694=EDGE_LOOP('',(#60267,#60268,#60269,#60270,#60271));
#25695=EDGE_LOOP('',(#60272,#60273,#60274));
#25696=EDGE_LOOP('',(#60275,#60276,#60277,#60278));
#25697=EDGE_LOOP('',(#60279,#60280,#60281,#60282));
#25698=EDGE_LOOP('',(#60283,#60284,#60285,#60286,#60287));
#25699=EDGE_LOOP('',(#60288,#60289,#60290,#60291,#60292));
#25700=EDGE_LOOP('',(#60293,#60294,#60295));
#25701=EDGE_LOOP('',(#60296,#60297,#60298,#60299));
#25702=EDGE_LOOP('',(#60300,#60301,#60302,#60303));
#25703=EDGE_LOOP('',(#60304,#60305,#60306,#60307));
#25704=EDGE_LOOP('',(#60308,#60309,#60310,#60311));
#25705=EDGE_LOOP('',(#60312,#60313,#60314,#60315));
#25706=EDGE_LOOP('',(#60316,#60317,#60318,#60319));
#25707=EDGE_LOOP('',(#60320,#60321,#60322,#60323));
#25708=EDGE_LOOP('',(#60324,#60325,#60326,#60327));
#25709=EDGE_LOOP('',(#60328,#60329,#60330,#60331));
#25710=EDGE_LOOP('',(#60332,#60333,#60334,#60335));
#25711=EDGE_LOOP('',(#60336,#60337,#60338,#60339));
#25712=EDGE_LOOP('',(#60340,#60341,#60342,#60343));
#25713=EDGE_LOOP('',(#60344,#60345,#60346,#60347));
#25714=EDGE_LOOP('',(#60348,#60349,#60350,#60351));
#25715=EDGE_LOOP('',(#60352,#60353,#60354,#60355));
#25716=EDGE_LOOP('',(#60356,#60357,#60358,#60359));
#25717=EDGE_LOOP('',(#60360,#60361,#60362,#60363));
#25718=EDGE_LOOP('',(#60364,#60365,#60366,#60367));
#25719=EDGE_LOOP('',(#60368,#60369,#60370,#60371));
#25720=EDGE_LOOP('',(#60372,#60373,#60374,#60375));
#25721=EDGE_LOOP('',(#60376,#60377,#60378,#60379));
#25722=EDGE_LOOP('',(#60380,#60381,#60382,#60383));
#25723=EDGE_LOOP('',(#60384,#60385,#60386,#60387));
#25724=EDGE_LOOP('',(#60388,#60389,#60390,#60391));
#25725=EDGE_LOOP('',(#60392,#60393,#60394,#60395));
#25726=EDGE_LOOP('',(#60396,#60397,#60398,#60399));
#25727=EDGE_LOOP('',(#60400,#60401,#60402,#60403));
#25728=EDGE_LOOP('',(#60404,#60405,#60406,#60407));
#25729=EDGE_LOOP('',(#60408,#60409,#60410,#60411));
#25730=EDGE_LOOP('',(#60412,#60413,#60414,#60415));
#25731=EDGE_LOOP('',(#60416,#60417,#60418,#60419));
#25732=EDGE_LOOP('',(#60420,#60421,#60422,#60423));
#25733=EDGE_LOOP('',(#60424,#60425,#60426,#60427));
#25734=EDGE_LOOP('',(#60428,#60429,#60430,#60431));
#25735=EDGE_LOOP('',(#60432,#60433,#60434,#60435));
#25736=EDGE_LOOP('',(#60436,#60437,#60438,#60439));
#25737=EDGE_LOOP('',(#60440,#60441,#60442,#60443));
#25738=EDGE_LOOP('',(#60444,#60445,#60446,#60447,#60448));
#25739=EDGE_LOOP('',(#60449,#60450,#60451,#60452));
#25740=EDGE_LOOP('',(#60453,#60454,#60455,#60456,#60457));
#25741=EDGE_LOOP('',(#60458,#60459,#60460,#60461));
#25742=EDGE_LOOP('',(#60462,#60463,#60464,#60465));
#25743=EDGE_LOOP('',(#60466,#60467,#60468,#60469));
#25744=EDGE_LOOP('',(#60470,#60471,#60472,#60473,#60474));
#25745=EDGE_LOOP('',(#60475,#60476,#60477,#60478,#60479));
#25746=EDGE_LOOP('',(#60480,#60481,#60482));
#25747=EDGE_LOOP('',(#60483,#60484,#60485,#60486));
#25748=EDGE_LOOP('',(#60487,#60488,#60489,#60490));
#25749=EDGE_LOOP('',(#60491,#60492,#60493,#60494));
#25750=EDGE_LOOP('',(#60495,#60496,#60497,#60498));
#25751=EDGE_LOOP('',(#60499,#60500,#60501,#60502));
#25752=EDGE_LOOP('',(#60503,#60504,#60505,#60506));
#25753=EDGE_LOOP('',(#60507,#60508,#60509,#60510));
#25754=EDGE_LOOP('',(#60511,#60512,#60513,#60514));
#25755=EDGE_LOOP('',(#60515,#60516,#60517,#60518));
#25756=EDGE_LOOP('',(#60519,#60520,#60521,#60522));
#25757=EDGE_LOOP('',(#60523,#60524,#60525,#60526));
#25758=EDGE_LOOP('',(#60527,#60528,#60529,#60530));
#25759=EDGE_LOOP('',(#60531,#60532,#60533,#60534));
#25760=EDGE_LOOP('',(#60535,#60536,#60537,#60538));
#25761=EDGE_LOOP('',(#60539,#60540,#60541,#60542));
#25762=EDGE_LOOP('',(#60543,#60544,#60545,#60546));
#25763=EDGE_LOOP('',(#60547,#60548,#60549,#60550));
#25764=EDGE_LOOP('',(#60551,#60552,#60553,#60554));
#25765=EDGE_LOOP('',(#60555,#60556,#60557,#60558));
#25766=EDGE_LOOP('',(#60559,#60560,#60561,#60562));
#25767=EDGE_LOOP('',(#60563,#60564,#60565,#60566));
#25768=EDGE_LOOP('',(#60567,#60568,#60569,#60570));
#25769=EDGE_LOOP('',(#60571,#60572,#60573,#60574));
#25770=EDGE_LOOP('',(#60575,#60576,#60577,#60578));
#25771=EDGE_LOOP('',(#60579,#60580,#60581,#60582));
#25772=EDGE_LOOP('',(#60583,#60584,#60585,#60586));
#25773=EDGE_LOOP('',(#60587,#60588,#60589,#60590));
#25774=EDGE_LOOP('',(#60591,#60592,#60593,#60594));
#25775=EDGE_LOOP('',(#60595,#60596,#60597,#60598));
#25776=EDGE_LOOP('',(#60599,#60600,#60601,#60602));
#25777=EDGE_LOOP('',(#60603,#60604,#60605,#60606));
#25778=EDGE_LOOP('',(#60607,#60608,#60609,#60610));
#25779=EDGE_LOOP('',(#60611,#60612,#60613,#60614));
#25780=EDGE_LOOP('',(#60615,#60616,#60617,#60618));
#25781=EDGE_LOOP('',(#60619,#60620,#60621,#60622));
#25782=EDGE_LOOP('',(#60623,#60624,#60625,#60626));
#25783=EDGE_LOOP('',(#60627,#60628,#60629,#60630));
#25784=EDGE_LOOP('',(#60631,#60632,#60633,#60634));
#25785=EDGE_LOOP('',(#60635,#60636,#60637,#60638));
#25786=EDGE_LOOP('',(#60639,#60640,#60641,#60642));
#25787=EDGE_LOOP('',(#60643,#60644,#60645,#60646));
#25788=EDGE_LOOP('',(#60647,#60648,#60649,#60650));
#25789=EDGE_LOOP('',(#60651,#60652,#60653,#60654));
#25790=EDGE_LOOP('',(#60655,#60656,#60657,#60658));
#25791=EDGE_LOOP('',(#60659,#60660,#60661,#60662));
#25792=EDGE_LOOP('',(#60663,#60664,#60665,#60666));
#25793=EDGE_LOOP('',(#60667,#60668,#60669,#60670));
#25794=EDGE_LOOP('',(#60671,#60672,#60673,#60674));
#25795=EDGE_LOOP('',(#60675,#60676,#60677,#60678));
#25796=EDGE_LOOP('',(#60679,#60680,#60681,#60682));
#25797=EDGE_LOOP('',(#60683,#60684,#60685,#60686));
#25798=EDGE_LOOP('',(#60687,#60688,#60689,#60690));
#25799=EDGE_LOOP('',(#60691,#60692,#60693,#60694));
#25800=EDGE_LOOP('',(#60695,#60696,#60697,#60698));
#25801=EDGE_LOOP('',(#60699,#60700,#60701,#60702));
#25802=EDGE_LOOP('',(#60703,#60704,#60705,#60706));
#25803=EDGE_LOOP('',(#60707,#60708,#60709,#60710));
#25804=EDGE_LOOP('',(#60711,#60712,#60713,#60714));
#25805=EDGE_LOOP('',(#60715,#60716,#60717,#60718));
#25806=EDGE_LOOP('',(#60719,#60720,#60721,#60722));
#25807=EDGE_LOOP('',(#60723,#60724,#60725,#60726));
#25808=EDGE_LOOP('',(#60727,#60728,#60729,#60730));
#25809=EDGE_LOOP('',(#60731,#60732,#60733,#60734));
#25810=EDGE_LOOP('',(#60735,#60736,#60737,#60738));
#25811=EDGE_LOOP('',(#60739,#60740,#60741,#60742));
#25812=EDGE_LOOP('',(#60743,#60744,#60745,#60746));
#25813=EDGE_LOOP('',(#60747,#60748,#60749,#60750));
#25814=EDGE_LOOP('',(#60751,#60752,#60753,#60754));
#25815=EDGE_LOOP('',(#60755,#60756,#60757,#60758));
#25816=EDGE_LOOP('',(#60759,#60760,#60761,#60762));
#25817=EDGE_LOOP('',(#60763,#60764,#60765,#60766));
#25818=EDGE_LOOP('',(#60767,#60768,#60769,#60770));
#25819=EDGE_LOOP('',(#60771,#60772,#60773,#60774));
#25820=EDGE_LOOP('',(#60775,#60776,#60777,#60778));
#25821=EDGE_LOOP('',(#60779,#60780,#60781,#60782));
#25822=EDGE_LOOP('',(#60783,#60784,#60785,#60786));
#25823=EDGE_LOOP('',(#60787,#60788,#60789,#60790));
#25824=EDGE_LOOP('',(#60791,#60792,#60793,#60794));
#25825=EDGE_LOOP('',(#60795,#60796,#60797,#60798));
#25826=EDGE_LOOP('',(#60799,#60800,#60801,#60802));
#25827=EDGE_LOOP('',(#60803,#60804,#60805,#60806));
#25828=EDGE_LOOP('',(#60807,#60808,#60809,#60810));
#25829=EDGE_LOOP('',(#60811,#60812,#60813,#60814));
#25830=EDGE_LOOP('',(#60815,#60816,#60817,#60818));
#25831=EDGE_LOOP('',(#60819,#60820,#60821,#60822));
#25832=EDGE_LOOP('',(#60823,#60824,#60825,#60826));
#25833=EDGE_LOOP('',(#60827,#60828,#60829,#60830));
#25834=EDGE_LOOP('',(#60831,#60832,#60833,#60834));
#25835=EDGE_LOOP('',(#60835,#60836,#60837,#60838));
#25836=EDGE_LOOP('',(#60839,#60840,#60841,#60842));
#25837=EDGE_LOOP('',(#60843,#60844,#60845,#60846));
#25838=EDGE_LOOP('',(#60847,#60848,#60849,#60850));
#25839=EDGE_LOOP('',(#60851,#60852,#60853,#60854));
#25840=EDGE_LOOP('',(#60855,#60856,#60857,#60858));
#25841=EDGE_LOOP('',(#60859,#60860,#60861,#60862));
#25842=EDGE_LOOP('',(#60863,#60864,#60865,#60866));
#25843=EDGE_LOOP('',(#60867,#60868,#60869,#60870));
#25844=EDGE_LOOP('',(#60871,#60872,#60873,#60874));
#25845=EDGE_LOOP('',(#60875,#60876,#60877,#60878));
#25846=EDGE_LOOP('',(#60879,#60880,#60881,#60882));
#25847=EDGE_LOOP('',(#60883,#60884,#60885,#60886));
#25848=EDGE_LOOP('',(#60887,#60888,#60889,#60890));
#25849=EDGE_LOOP('',(#60891,#60892,#60893,#60894));
#25850=EDGE_LOOP('',(#60895,#60896,#60897,#60898));
#25851=EDGE_LOOP('',(#60899,#60900,#60901,#60902));
#25852=EDGE_LOOP('',(#60903,#60904,#60905,#60906));
#25853=EDGE_LOOP('',(#60907,#60908,#60909,#60910));
#25854=EDGE_LOOP('',(#60911,#60912,#60913,#60914));
#25855=EDGE_LOOP('',(#60915,#60916,#60917,#60918));
#25856=EDGE_LOOP('',(#60919,#60920,#60921,#60922));
#25857=EDGE_LOOP('',(#60923,#60924,#60925,#60926));
#25858=EDGE_LOOP('',(#60927,#60928,#60929,#60930));
#25859=EDGE_LOOP('',(#60931,#60932,#60933,#60934));
#25860=EDGE_LOOP('',(#60935,#60936,#60937,#60938));
#25861=EDGE_LOOP('',(#60939,#60940,#60941,#60942));
#25862=EDGE_LOOP('',(#60943,#60944,#60945,#60946));
#25863=EDGE_LOOP('',(#60947,#60948,#60949,#60950));
#25864=EDGE_LOOP('',(#60951,#60952,#60953,#60954));
#25865=EDGE_LOOP('',(#60955,#60956,#60957,#60958));
#25866=EDGE_LOOP('',(#60959,#60960,#60961,#60962));
#25867=EDGE_LOOP('',(#60963,#60964,#60965,#60966));
#25868=EDGE_LOOP('',(#60967,#60968,#60969,#60970));
#25869=EDGE_LOOP('',(#60971,#60972,#60973,#60974));
#25870=EDGE_LOOP('',(#60975,#60976,#60977,#60978));
#25871=EDGE_LOOP('',(#60979,#60980,#60981,#60982));
#25872=EDGE_LOOP('',(#60983,#60984,#60985,#60986));
#25873=EDGE_LOOP('',(#60987,#60988,#60989,#60990));
#25874=EDGE_LOOP('',(#60991,#60992,#60993,#60994));
#25875=EDGE_LOOP('',(#60995,#60996,#60997,#60998));
#25876=EDGE_LOOP('',(#60999,#61000,#61001,#61002));
#25877=EDGE_LOOP('',(#61003,#61004,#61005,#61006));
#25878=EDGE_LOOP('',(#61007,#61008,#61009,#61010));
#25879=EDGE_LOOP('',(#61011,#61012,#61013,#61014));
#25880=EDGE_LOOP('',(#61015,#61016,#61017,#61018));
#25881=EDGE_LOOP('',(#61019,#61020,#61021,#61022));
#25882=EDGE_LOOP('',(#61023,#61024,#61025,#61026));
#25883=EDGE_LOOP('',(#61027,#61028,#61029,#61030));
#25884=EDGE_LOOP('',(#61031,#61032,#61033,#61034));
#25885=EDGE_LOOP('',(#61035,#61036,#61037,#61038));
#25886=EDGE_LOOP('',(#61039,#61040,#61041,#61042));
#25887=EDGE_LOOP('',(#61043,#61044,#61045,#61046));
#25888=EDGE_LOOP('',(#61047,#61048,#61049,#61050));
#25889=EDGE_LOOP('',(#61051,#61052,#61053,#61054));
#25890=EDGE_LOOP('',(#61055,#61056,#61057,#61058));
#25891=EDGE_LOOP('',(#61059,#61060,#61061,#61062));
#25892=EDGE_LOOP('',(#61063,#61064,#61065,#61066));
#25893=EDGE_LOOP('',(#61067,#61068,#61069,#61070));
#25894=EDGE_LOOP('',(#61071,#61072,#61073,#61074));
#25895=EDGE_LOOP('',(#61075,#61076,#61077,#61078));
#25896=EDGE_LOOP('',(#61079,#61080,#61081,#61082));
#25897=EDGE_LOOP('',(#61083,#61084,#61085,#61086));
#25898=EDGE_LOOP('',(#61087,#61088,#61089,#61090));
#25899=EDGE_LOOP('',(#61091,#61092,#61093,#61094));
#25900=EDGE_LOOP('',(#61095,#61096,#61097,#61098));
#25901=EDGE_LOOP('',(#61099,#61100,#61101,#61102));
#25902=EDGE_LOOP('',(#61103,#61104,#61105,#61106));
#25903=EDGE_LOOP('',(#61107,#61108,#61109,#61110));
#25904=EDGE_LOOP('',(#61111,#61112,#61113,#61114));
#25905=EDGE_LOOP('',(#61115,#61116,#61117,#61118));
#25906=EDGE_LOOP('',(#61119,#61120,#61121,#61122));
#25907=EDGE_LOOP('',(#61123,#61124,#61125,#61126));
#25908=EDGE_LOOP('',(#61127,#61128,#61129,#61130));
#25909=EDGE_LOOP('',(#61131,#61132,#61133,#61134));
#25910=EDGE_LOOP('',(#61135,#61136,#61137,#61138));
#25911=EDGE_LOOP('',(#61139,#61140,#61141,#61142));
#25912=EDGE_LOOP('',(#61143,#61144,#61145,#61146));
#25913=EDGE_LOOP('',(#61147,#61148,#61149,#61150));
#25914=EDGE_LOOP('',(#61151,#61152,#61153,#61154));
#25915=EDGE_LOOP('',(#61155,#61156,#61157,#61158));
#25916=EDGE_LOOP('',(#61159,#61160,#61161,#61162));
#25917=EDGE_LOOP('',(#61163,#61164,#61165,#61166));
#25918=EDGE_LOOP('',(#61167,#61168,#61169,#61170));
#25919=EDGE_LOOP('',(#61171,#61172,#61173,#61174));
#25920=EDGE_LOOP('',(#61175,#61176,#61177,#61178));
#25921=EDGE_LOOP('',(#61179,#61180,#61181,#61182));
#25922=EDGE_LOOP('',(#61183,#61184,#61185,#61186));
#25923=EDGE_LOOP('',(#61187,#61188,#61189,#61190));
#25924=EDGE_LOOP('',(#61191,#61192,#61193,#61194));
#25925=EDGE_LOOP('',(#61195,#61196,#61197,#61198));
#25926=EDGE_LOOP('',(#61199,#61200,#61201,#61202));
#25927=EDGE_LOOP('',(#61203,#61204,#61205,#61206));
#25928=EDGE_LOOP('',(#61207,#61208,#61209,#61210));
#25929=EDGE_LOOP('',(#61211,#61212,#61213,#61214));
#25930=EDGE_LOOP('',(#61215,#61216,#61217,#61218));
#25931=EDGE_LOOP('',(#61219,#61220,#61221,#61222));
#25932=EDGE_LOOP('',(#61223,#61224,#61225,#61226));
#25933=EDGE_LOOP('',(#61227,#61228,#61229,#61230));
#25934=EDGE_LOOP('',(#61231,#61232,#61233,#61234));
#25935=EDGE_LOOP('',(#61235,#61236,#61237,#61238));
#25936=EDGE_LOOP('',(#61239,#61240,#61241,#61242));
#25937=EDGE_LOOP('',(#61243,#61244,#61245,#61246));
#25938=EDGE_LOOP('',(#61247,#61248,#61249,#61250));
#25939=EDGE_LOOP('',(#61251,#61252,#61253,#61254));
#25940=EDGE_LOOP('',(#61255,#61256,#61257,#61258));
#25941=EDGE_LOOP('',(#61259,#61260,#61261,#61262));
#25942=EDGE_LOOP('',(#61263,#61264,#61265,#61266));
#25943=EDGE_LOOP('',(#61267,#61268,#61269,#61270));
#25944=EDGE_LOOP('',(#61271,#61272,#61273,#61274));
#25945=EDGE_LOOP('',(#61275,#61276,#61277,#61278));
#25946=EDGE_LOOP('',(#61279,#61280,#61281,#61282));
#25947=EDGE_LOOP('',(#61283,#61284,#61285,#61286));
#25948=EDGE_LOOP('',(#61287,#61288,#61289,#61290));
#25949=EDGE_LOOP('',(#61291,#61292,#61293,#61294));
#25950=EDGE_LOOP('',(#61295,#61296,#61297,#61298));
#25951=EDGE_LOOP('',(#61299,#61300,#61301,#61302));
#25952=EDGE_LOOP('',(#61303,#61304,#61305,#61306));
#25953=EDGE_LOOP('',(#61307,#61308,#61309,#61310));
#25954=EDGE_LOOP('',(#61311,#61312,#61313,#61314));
#25955=EDGE_LOOP('',(#61315,#61316,#61317,#61318));
#25956=EDGE_LOOP('',(#61319,#61320,#61321,#61322));
#25957=EDGE_LOOP('',(#61323,#61324,#61325,#61326));
#25958=EDGE_LOOP('',(#61327,#61328,#61329,#61330));
#25959=EDGE_LOOP('',(#61331,#61332,#61333,#61334));
#25960=EDGE_LOOP('',(#61335,#61336,#61337,#61338));
#25961=EDGE_LOOP('',(#61339,#61340,#61341,#61342));
#25962=EDGE_LOOP('',(#61343,#61344,#61345,#61346));
#25963=EDGE_LOOP('',(#61347,#61348,#61349,#61350));
#25964=EDGE_LOOP('',(#61351,#61352,#61353,#61354));
#25965=EDGE_LOOP('',(#61355,#61356,#61357,#61358));
#25966=EDGE_LOOP('',(#61359,#61360,#61361,#61362));
#25967=EDGE_LOOP('',(#61363,#61364,#61365,#61366));
#25968=EDGE_LOOP('',(#61367,#61368,#61369,#61370));
#25969=EDGE_LOOP('',(#61371,#61372,#61373,#61374));
#25970=EDGE_LOOP('',(#61375,#61376,#61377,#61378));
#25971=EDGE_LOOP('',(#61379,#61380,#61381,#61382));
#25972=EDGE_LOOP('',(#61383,#61384,#61385,#61386));
#25973=EDGE_LOOP('',(#61387,#61388,#61389,#61390));
#25974=EDGE_LOOP('',(#61391,#61392,#61393,#61394));
#25975=EDGE_LOOP('',(#61395,#61396,#61397,#61398));
#25976=EDGE_LOOP('',(#61399,#61400,#61401,#61402));
#25977=EDGE_LOOP('',(#61403,#61404,#61405,#61406));
#25978=EDGE_LOOP('',(#61407,#61408,#61409,#61410));
#25979=EDGE_LOOP('',(#61411,#61412,#61413,#61414));
#25980=EDGE_LOOP('',(#61415,#61416,#61417,#61418));
#25981=EDGE_LOOP('',(#61419,#61420,#61421,#61422));
#25982=EDGE_LOOP('',(#61423,#61424,#61425,#61426));
#25983=EDGE_LOOP('',(#61427,#61428,#61429,#61430));
#25984=EDGE_LOOP('',(#61431,#61432,#61433,#61434));
#25985=EDGE_LOOP('',(#61435,#61436,#61437,#61438));
#25986=EDGE_LOOP('',(#61439,#61440,#61441,#61442));
#25987=EDGE_LOOP('',(#61443,#61444,#61445,#61446));
#25988=EDGE_LOOP('',(#61447,#61448,#61449,#61450));
#25989=EDGE_LOOP('',(#61451,#61452,#61453,#61454));
#25990=EDGE_LOOP('',(#61455,#61456,#61457,#61458));
#25991=EDGE_LOOP('',(#61459,#61460,#61461,#61462));
#25992=EDGE_LOOP('',(#61463,#61464,#61465,#61466));
#25993=EDGE_LOOP('',(#61467,#61468,#61469,#61470));
#25994=EDGE_LOOP('',(#61471,#61472,#61473,#61474));
#25995=EDGE_LOOP('',(#61475,#61476,#61477,#61478));
#25996=EDGE_LOOP('',(#61479,#61480,#61481,#61482));
#25997=EDGE_LOOP('',(#61483,#61484,#61485,#61486));
#25998=EDGE_LOOP('',(#61487,#61488,#61489,#61490));
#25999=EDGE_LOOP('',(#61491,#61492,#61493,#61494));
#26000=EDGE_LOOP('',(#61495,#61496,#61497,#61498));
#26001=EDGE_LOOP('',(#61499,#61500,#61501,#61502));
#26002=EDGE_LOOP('',(#61503,#61504,#61505,#61506));
#26003=EDGE_LOOP('',(#61507,#61508,#61509,#61510));
#26004=EDGE_LOOP('',(#61511,#61512,#61513,#61514));
#26005=EDGE_LOOP('',(#61515,#61516,#61517,#61518));
#26006=EDGE_LOOP('',(#61519,#61520,#61521,#61522));
#26007=EDGE_LOOP('',(#61523,#61524,#61525,#61526));
#26008=EDGE_LOOP('',(#61527,#61528,#61529,#61530));
#26009=EDGE_LOOP('',(#61531,#61532,#61533,#61534));
#26010=EDGE_LOOP('',(#61535,#61536,#61537,#61538));
#26011=EDGE_LOOP('',(#61539,#61540,#61541,#61542));
#26012=EDGE_LOOP('',(#61543,#61544,#61545,#61546));
#26013=EDGE_LOOP('',(#61547,#61548,#61549,#61550));
#26014=EDGE_LOOP('',(#61551,#61552,#61553,#61554));
#26015=EDGE_LOOP('',(#61555,#61556,#61557,#61558));
#26016=EDGE_LOOP('',(#61559,#61560,#61561,#61562));
#26017=EDGE_LOOP('',(#61563,#61564,#61565,#61566));
#26018=EDGE_LOOP('',(#61567,#61568,#61569,#61570));
#26019=EDGE_LOOP('',(#61571,#61572,#61573,#61574));
#26020=EDGE_LOOP('',(#61575,#61576,#61577,#61578));
#26021=EDGE_LOOP('',(#61579,#61580,#61581,#61582));
#26022=EDGE_LOOP('',(#61583,#61584,#61585,#61586));
#26023=EDGE_LOOP('',(#61587,#61588,#61589,#61590));
#26024=EDGE_LOOP('',(#61591,#61592,#61593,#61594));
#26025=EDGE_LOOP('',(#61595,#61596,#61597,#61598));
#26026=EDGE_LOOP('',(#61599,#61600,#61601,#61602));
#26027=EDGE_LOOP('',(#61603,#61604,#61605,#61606));
#26028=EDGE_LOOP('',(#61607,#61608,#61609,#61610));
#26029=EDGE_LOOP('',(#61611,#61612,#61613,#61614));
#26030=EDGE_LOOP('',(#61615,#61616,#61617,#61618));
#26031=EDGE_LOOP('',(#61619,#61620,#61621,#61622));
#26032=EDGE_LOOP('',(#61623,#61624,#61625,#61626));
#26033=EDGE_LOOP('',(#61627,#61628,#61629,#61630));
#26034=EDGE_LOOP('',(#61631,#61632,#61633,#61634));
#26035=EDGE_LOOP('',(#61635,#61636,#61637,#61638));
#26036=EDGE_LOOP('',(#61639,#61640,#61641,#61642));
#26037=EDGE_LOOP('',(#61643,#61644,#61645,#61646));
#26038=EDGE_LOOP('',(#61647,#61648,#61649,#61650));
#26039=EDGE_LOOP('',(#61651,#61652,#61653,#61654));
#26040=EDGE_LOOP('',(#61655,#61656,#61657,#61658));
#26041=EDGE_LOOP('',(#61659,#61660,#61661,#61662));
#26042=EDGE_LOOP('',(#61663,#61664,#61665,#61666));
#26043=EDGE_LOOP('',(#61667,#61668,#61669,#61670));
#26044=EDGE_LOOP('',(#61671,#61672,#61673,#61674));
#26045=EDGE_LOOP('',(#61675,#61676,#61677,#61678));
#26046=EDGE_LOOP('',(#61679,#61680,#61681,#61682));
#26047=EDGE_LOOP('',(#61683,#61684,#61685,#61686));
#26048=EDGE_LOOP('',(#61687,#61688,#61689,#61690));
#26049=EDGE_LOOP('',(#61691,#61692,#61693,#61694));
#26050=EDGE_LOOP('',(#61695,#61696,#61697,#61698));
#26051=EDGE_LOOP('',(#61699,#61700,#61701,#61702));
#26052=EDGE_LOOP('',(#61703,#61704,#61705,#61706));
#26053=EDGE_LOOP('',(#61707,#61708,#61709,#61710));
#26054=EDGE_LOOP('',(#61711,#61712,#61713,#61714));
#26055=EDGE_LOOP('',(#61715));
#26056=EDGE_LOOP('',(#61716));
#26057=EDGE_LOOP('',(#61717,#61718,#61719,#61720));
#26058=EDGE_LOOP('',(#61721,#61722,#61723,#61724));
#26059=EDGE_LOOP('',(#61725,#61726,#61727,#61728));
#26060=EDGE_LOOP('',(#61729,#61730,#61731,#61732));
#26061=EDGE_LOOP('',(#61733,#61734,#61735,#61736));
#26062=EDGE_LOOP('',(#61737,#61738,#61739,#61740));
#26063=EDGE_LOOP('',(#61741,#61742,#61743,#61744));
#26064=EDGE_LOOP('',(#61745,#61746,#61747,#61748));
#26065=EDGE_LOOP('',(#61749,#61750,#61751,#61752));
#26066=EDGE_LOOP('',(#61753,#61754,#61755,#61756));
#26067=EDGE_LOOP('',(#61757,#61758,#61759,#61760));
#26068=EDGE_LOOP('',(#61761,#61762,#61763,#61764));
#26069=EDGE_LOOP('',(#61765,#61766,#61767,#61768));
#26070=EDGE_LOOP('',(#61769,#61770,#61771,#61772));
#26071=EDGE_LOOP('',(#61773,#61774,#61775,#61776));
#26072=EDGE_LOOP('',(#61777,#61778,#61779,#61780));
#26073=EDGE_LOOP('',(#61781,#61782,#61783,#61784));
#26074=EDGE_LOOP('',(#61785,#61786,#61787,#61788));
#26075=EDGE_LOOP('',(#61789,#61790,#61791,#61792));
#26076=EDGE_LOOP('',(#61793,#61794,#61795,#61796));
#26077=EDGE_LOOP('',(#61797,#61798,#61799,#61800));
#26078=EDGE_LOOP('',(#61801,#61802,#61803,#61804));
#26079=EDGE_LOOP('',(#61805,#61806,#61807,#61808));
#26080=EDGE_LOOP('',(#61809,#61810,#61811,#61812));
#26081=EDGE_LOOP('',(#61813,#61814,#61815,#61816));
#26082=EDGE_LOOP('',(#61817,#61818,#61819,#61820));
#26083=EDGE_LOOP('',(#61821,#61822,#61823,#61824));
#26084=EDGE_LOOP('',(#61825,#61826,#61827,#61828));
#26085=EDGE_LOOP('',(#61829,#61830,#61831,#61832));
#26086=EDGE_LOOP('',(#61833,#61834,#61835,#61836));
#26087=EDGE_LOOP('',(#61837,#61838,#61839,#61840));
#26088=EDGE_LOOP('',(#61841,#61842,#61843,#61844));
#26089=EDGE_LOOP('',(#61845,#61846,#61847,#61848));
#26090=EDGE_LOOP('',(#61849,#61850,#61851,#61852));
#26091=EDGE_LOOP('',(#61853,#61854,#61855,#61856));
#26092=EDGE_LOOP('',(#61857,#61858,#61859,#61860));
#26093=EDGE_LOOP('',(#61861,#61862,#61863,#61864));
#26094=EDGE_LOOP('',(#61865,#61866,#61867,#61868));
#26095=EDGE_LOOP('',(#61869,#61870,#61871,#61872));
#26096=EDGE_LOOP('',(#61873,#61874,#61875,#61876));
#26097=EDGE_LOOP('',(#61877,#61878,#61879,#61880));
#26098=EDGE_LOOP('',(#61881,#61882,#61883,#61884));
#26099=EDGE_LOOP('',(#61885,#61886,#61887,#61888));
#26100=EDGE_LOOP('',(#61889,#61890,#61891,#61892));
#26101=EDGE_LOOP('',(#61893,#61894,#61895,#61896));
#26102=EDGE_LOOP('',(#61897,#61898,#61899,#61900));
#26103=EDGE_LOOP('',(#61901,#61902,#61903,#61904));
#26104=EDGE_LOOP('',(#61905,#61906,#61907,#61908));
#26105=EDGE_LOOP('',(#61909,#61910,#61911,#61912));
#26106=EDGE_LOOP('',(#61913,#61914,#61915,#61916));
#26107=EDGE_LOOP('',(#61917,#61918,#61919,#61920));
#26108=EDGE_LOOP('',(#61921,#61922,#61923,#61924));
#26109=EDGE_LOOP('',(#61925,#61926,#61927,#61928));
#26110=EDGE_LOOP('',(#61929,#61930,#61931,#61932));
#26111=EDGE_LOOP('',(#61933,#61934,#61935,#61936));
#26112=EDGE_LOOP('',(#61937,#61938,#61939,#61940));
#26113=EDGE_LOOP('',(#61941,#61942,#61943,#61944));
#26114=EDGE_LOOP('',(#61945,#61946,#61947,#61948));
#26115=EDGE_LOOP('',(#61949,#61950,#61951,#61952));
#26116=EDGE_LOOP('',(#61953,#61954,#61955,#61956));
#26117=EDGE_LOOP('',(#61957,#61958,#61959,#61960));
#26118=EDGE_LOOP('',(#61961,#61962,#61963,#61964));
#26119=EDGE_LOOP('',(#61965,#61966,#61967,#61968));
#26120=EDGE_LOOP('',(#61969,#61970,#61971,#61972));
#26121=EDGE_LOOP('',(#61973,#61974,#61975,#61976));
#26122=EDGE_LOOP('',(#61977,#61978,#61979,#61980));
#26123=EDGE_LOOP('',(#61981,#61982,#61983,#61984));
#26124=EDGE_LOOP('',(#61985,#61986,#61987,#61988));
#26125=EDGE_LOOP('',(#61989,#61990,#61991,#61992));
#26126=EDGE_LOOP('',(#61993,#61994,#61995,#61996));
#26127=EDGE_LOOP('',(#61997,#61998,#61999,#62000));
#26128=EDGE_LOOP('',(#62001,#62002,#62003,#62004));
#26129=EDGE_LOOP('',(#62005,#62006,#62007,#62008));
#26130=EDGE_LOOP('',(#62009,#62010,#62011,#62012));
#26131=EDGE_LOOP('',(#62013,#62014,#62015,#62016));
#26132=EDGE_LOOP('',(#62017,#62018,#62019,#62020));
#26133=EDGE_LOOP('',(#62021,#62022,#62023,#62024));
#26134=EDGE_LOOP('',(#62025,#62026,#62027,#62028));
#26135=EDGE_LOOP('',(#62029,#62030,#62031,#62032));
#26136=EDGE_LOOP('',(#62033,#62034,#62035,#62036));
#26137=EDGE_LOOP('',(#62037,#62038,#62039,#62040));
#26138=EDGE_LOOP('',(#62041,#62042,#62043,#62044));
#26139=EDGE_LOOP('',(#62045,#62046,#62047,#62048));
#26140=EDGE_LOOP('',(#62049,#62050,#62051,#62052));
#26141=EDGE_LOOP('',(#62053,#62054,#62055,#62056));
#26142=EDGE_LOOP('',(#62057,#62058,#62059,#62060));
#26143=EDGE_LOOP('',(#62061,#62062,#62063,#62064));
#26144=EDGE_LOOP('',(#62065,#62066,#62067,#62068));
#26145=EDGE_LOOP('',(#62069,#62070,#62071,#62072));
#26146=EDGE_LOOP('',(#62073,#62074,#62075,#62076));
#26147=EDGE_LOOP('',(#62077,#62078,#62079,#62080));
#26148=EDGE_LOOP('',(#62081,#62082,#62083,#62084));
#26149=EDGE_LOOP('',(#62085,#62086,#62087,#62088));
#26150=EDGE_LOOP('',(#62089,#62090,#62091,#62092));
#26151=EDGE_LOOP('',(#62093,#62094,#62095,#62096));
#26152=EDGE_LOOP('',(#62097,#62098,#62099,#62100));
#26153=EDGE_LOOP('',(#62101,#62102,#62103,#62104));
#26154=EDGE_LOOP('',(#62105,#62106,#62107,#62108));
#26155=EDGE_LOOP('',(#62109,#62110,#62111,#62112));
#26156=EDGE_LOOP('',(#62113,#62114,#62115,#62116));
#26157=EDGE_LOOP('',(#62117,#62118,#62119,#62120));
#26158=EDGE_LOOP('',(#62121,#62122,#62123,#62124));
#26159=EDGE_LOOP('',(#62125,#62126,#62127,#62128));
#26160=EDGE_LOOP('',(#62129,#62130,#62131,#62132));
#26161=EDGE_LOOP('',(#62133,#62134,#62135,#62136));
#26162=EDGE_LOOP('',(#62137,#62138,#62139,#62140));
#26163=EDGE_LOOP('',(#62141,#62142,#62143,#62144));
#26164=EDGE_LOOP('',(#62145,#62146,#62147,#62148));
#26165=EDGE_LOOP('',(#62149,#62150,#62151,#62152));
#26166=EDGE_LOOP('',(#62153,#62154,#62155,#62156));
#26167=EDGE_LOOP('',(#62157,#62158,#62159,#62160));
#26168=EDGE_LOOP('',(#62161,#62162,#62163,#62164));
#26169=EDGE_LOOP('',(#62165,#62166,#62167,#62168));
#26170=EDGE_LOOP('',(#62169,#62170,#62171,#62172));
#26171=EDGE_LOOP('',(#62173,#62174,#62175,#62176));
#26172=EDGE_LOOP('',(#62177,#62178,#62179,#62180));
#26173=EDGE_LOOP('',(#62181,#62182,#62183,#62184));
#26174=EDGE_LOOP('',(#62185,#62186,#62187,#62188));
#26175=EDGE_LOOP('',(#62189,#62190,#62191,#62192));
#26176=EDGE_LOOP('',(#62193,#62194,#62195,#62196));
#26177=EDGE_LOOP('',(#62197,#62198,#62199,#62200));
#26178=EDGE_LOOP('',(#62201,#62202,#62203,#62204));
#26179=EDGE_LOOP('',(#62205,#62206,#62207,#62208));
#26180=EDGE_LOOP('',(#62209,#62210,#62211,#62212));
#26181=EDGE_LOOP('',(#62213,#62214,#62215,#62216));
#26182=EDGE_LOOP('',(#62217,#62218,#62219,#62220));
#26183=EDGE_LOOP('',(#62221,#62222,#62223,#62224));
#26184=EDGE_LOOP('',(#62225,#62226,#62227,#62228));
#26185=EDGE_LOOP('',(#62229,#62230,#62231,#62232));
#26186=EDGE_LOOP('',(#62233,#62234,#62235,#62236));
#26187=EDGE_LOOP('',(#62237,#62238,#62239,#62240));
#26188=EDGE_LOOP('',(#62241,#62242,#62243,#62244));
#26189=EDGE_LOOP('',(#62245,#62246,#62247,#62248));
#26190=EDGE_LOOP('',(#62249,#62250,#62251,#62252));
#26191=EDGE_LOOP('',(#62253,#62254,#62255,#62256));
#26192=EDGE_LOOP('',(#62257,#62258,#62259,#62260));
#26193=EDGE_LOOP('',(#62261,#62262,#62263,#62264));
#26194=EDGE_LOOP('',(#62265,#62266,#62267,#62268));
#26195=EDGE_LOOP('',(#62269,#62270,#62271,#62272));
#26196=EDGE_LOOP('',(#62273,#62274,#62275,#62276));
#26197=EDGE_LOOP('',(#62277,#62278,#62279,#62280));
#26198=EDGE_LOOP('',(#62281,#62282,#62283,#62284));
#26199=EDGE_LOOP('',(#62285,#62286,#62287,#62288));
#26200=EDGE_LOOP('',(#62289,#62290,#62291,#62292));
#26201=EDGE_LOOP('',(#62293,#62294,#62295,#62296));
#26202=EDGE_LOOP('',(#62297,#62298,#62299,#62300));
#26203=EDGE_LOOP('',(#62301,#62302,#62303,#62304));
#26204=EDGE_LOOP('',(#62305,#62306,#62307,#62308));
#26205=EDGE_LOOP('',(#62309,#62310,#62311,#62312));
#26206=EDGE_LOOP('',(#62313,#62314,#62315,#62316));
#26207=EDGE_LOOP('',(#62317,#62318,#62319,#62320));
#26208=EDGE_LOOP('',(#62321,#62322,#62323,#62324));
#26209=EDGE_LOOP('',(#62325,#62326,#62327,#62328));
#26210=EDGE_LOOP('',(#62329,#62330,#62331,#62332));
#26211=EDGE_LOOP('',(#62333,#62334,#62335,#62336));
#26212=EDGE_LOOP('',(#62337,#62338,#62339,#62340));
#26213=EDGE_LOOP('',(#62341,#62342,#62343,#62344));
#26214=EDGE_LOOP('',(#62345,#62346,#62347,#62348));
#26215=EDGE_LOOP('',(#62349,#62350,#62351,#62352));
#26216=EDGE_LOOP('',(#62353,#62354,#62355,#62356));
#26217=EDGE_LOOP('',(#62357,#62358,#62359,#62360));
#26218=EDGE_LOOP('',(#62361,#62362,#62363,#62364));
#26219=EDGE_LOOP('',(#62365,#62366,#62367,#62368));
#26220=EDGE_LOOP('',(#62369,#62370,#62371,#62372));
#26221=EDGE_LOOP('',(#62373,#62374,#62375,#62376));
#26222=EDGE_LOOP('',(#62377,#62378,#62379,#62380));
#26223=EDGE_LOOP('',(#62381,#62382,#62383,#62384));
#26224=EDGE_LOOP('',(#62385,#62386,#62387,#62388));
#26225=EDGE_LOOP('',(#62389,#62390,#62391,#62392));
#26226=EDGE_LOOP('',(#62393,#62394,#62395,#62396));
#26227=EDGE_LOOP('',(#62397,#62398,#62399,#62400));
#26228=EDGE_LOOP('',(#62401,#62402,#62403,#62404));
#26229=EDGE_LOOP('',(#62405,#62406,#62407,#62408));
#26230=EDGE_LOOP('',(#62409,#62410,#62411,#62412));
#26231=EDGE_LOOP('',(#62413,#62414,#62415,#62416));
#26232=EDGE_LOOP('',(#62417,#62418,#62419,#62420));
#26233=EDGE_LOOP('',(#62421,#62422,#62423,#62424));
#26234=EDGE_LOOP('',(#62425,#62426,#62427,#62428));
#26235=EDGE_LOOP('',(#62429,#62430,#62431,#62432));
#26236=EDGE_LOOP('',(#62433,#62434,#62435,#62436));
#26237=EDGE_LOOP('',(#62437,#62438,#62439,#62440));
#26238=EDGE_LOOP('',(#62441,#62442,#62443,#62444));
#26239=EDGE_LOOP('',(#62445,#62446,#62447,#62448));
#26240=EDGE_LOOP('',(#62449,#62450,#62451,#62452));
#26241=EDGE_LOOP('',(#62453,#62454,#62455,#62456));
#26242=EDGE_LOOP('',(#62457,#62458,#62459,#62460));
#26243=EDGE_LOOP('',(#62461,#62462,#62463,#62464));
#26244=EDGE_LOOP('',(#62465,#62466,#62467,#62468));
#26245=EDGE_LOOP('',(#62469,#62470,#62471,#62472));
#26246=EDGE_LOOP('',(#62473,#62474,#62475,#62476));
#26247=EDGE_LOOP('',(#62477,#62478,#62479,#62480));
#26248=EDGE_LOOP('',(#62481,#62482,#62483,#62484));
#26249=EDGE_LOOP('',(#62485,#62486,#62487,#62488));
#26250=EDGE_LOOP('',(#62489,#62490,#62491,#62492));
#26251=EDGE_LOOP('',(#62493,#62494,#62495,#62496));
#26252=EDGE_LOOP('',(#62497,#62498,#62499,#62500));
#26253=EDGE_LOOP('',(#62501,#62502,#62503,#62504));
#26254=EDGE_LOOP('',(#62505,#62506,#62507,#62508));
#26255=EDGE_LOOP('',(#62509,#62510,#62511,#62512));
#26256=EDGE_LOOP('',(#62513,#62514,#62515,#62516));
#26257=EDGE_LOOP('',(#62517,#62518,#62519,#62520));
#26258=EDGE_LOOP('',(#62521,#62522,#62523,#62524));
#26259=EDGE_LOOP('',(#62525,#62526,#62527,#62528));
#26260=EDGE_LOOP('',(#62529,#62530,#62531,#62532));
#26261=EDGE_LOOP('',(#62533,#62534,#62535,#62536));
#26262=EDGE_LOOP('',(#62537,#62538,#62539,#62540));
#26263=EDGE_LOOP('',(#62541,#62542,#62543,#62544));
#26264=EDGE_LOOP('',(#62545,#62546,#62547,#62548));
#26265=EDGE_LOOP('',(#62549,#62550,#62551,#62552));
#26266=EDGE_LOOP('',(#62553,#62554,#62555,#62556));
#26267=EDGE_LOOP('',(#62557,#62558,#62559,#62560));
#26268=EDGE_LOOP('',(#62561,#62562,#62563,#62564));
#26269=EDGE_LOOP('',(#62565,#62566,#62567,#62568));
#26270=EDGE_LOOP('',(#62569,#62570,#62571,#62572));
#26271=EDGE_LOOP('',(#62573,#62574,#62575,#62576));
#26272=EDGE_LOOP('',(#62577,#62578,#62579,#62580));
#26273=EDGE_LOOP('',(#62581,#62582,#62583,#62584));
#26274=EDGE_LOOP('',(#62585,#62586,#62587,#62588));
#26275=EDGE_LOOP('',(#62589,#62590,#62591,#62592));
#26276=EDGE_LOOP('',(#62593,#62594,#62595,#62596));
#26277=EDGE_LOOP('',(#62597,#62598,#62599,#62600));
#26278=EDGE_LOOP('',(#62601,#62602,#62603,#62604));
#26279=EDGE_LOOP('',(#62605,#62606,#62607,#62608));
#26280=EDGE_LOOP('',(#62609,#62610,#62611,#62612));
#26281=EDGE_LOOP('',(#62613,#62614,#62615,#62616));
#26282=EDGE_LOOP('',(#62617,#62618,#62619,#62620));
#26283=EDGE_LOOP('',(#62621,#62622,#62623,#62624));
#26284=EDGE_LOOP('',(#62625,#62626,#62627,#62628));
#26285=EDGE_LOOP('',(#62629,#62630,#62631,#62632));
#26286=EDGE_LOOP('',(#62633,#62634,#62635,#62636));
#26287=EDGE_LOOP('',(#62637,#62638,#62639,#62640));
#26288=EDGE_LOOP('',(#62641,#62642,#62643,#62644));
#26289=EDGE_LOOP('',(#62645,#62646,#62647,#62648));
#26290=EDGE_LOOP('',(#62649,#62650,#62651,#62652));
#26291=EDGE_LOOP('',(#62653,#62654,#62655,#62656));
#26292=EDGE_LOOP('',(#62657,#62658,#62659,#62660));
#26293=EDGE_LOOP('',(#62661,#62662,#62663,#62664));
#26294=EDGE_LOOP('',(#62665,#62666,#62667,#62668));
#26295=EDGE_LOOP('',(#62669,#62670,#62671,#62672));
#26296=EDGE_LOOP('',(#62673,#62674,#62675,#62676));
#26297=EDGE_LOOP('',(#62677,#62678,#62679,#62680));
#26298=EDGE_LOOP('',(#62681,#62682,#62683,#62684));
#26299=EDGE_LOOP('',(#62685,#62686,#62687,#62688));
#26300=EDGE_LOOP('',(#62689,#62690,#62691,#62692));
#26301=EDGE_LOOP('',(#62693,#62694,#62695,#62696));
#26302=EDGE_LOOP('',(#62697,#62698,#62699,#62700));
#26303=EDGE_LOOP('',(#62701,#62702,#62703,#62704));
#26304=EDGE_LOOP('',(#62705,#62706,#62707,#62708));
#26305=EDGE_LOOP('',(#62709,#62710,#62711,#62712));
#26306=EDGE_LOOP('',(#62713,#62714,#62715,#62716));
#26307=EDGE_LOOP('',(#62717,#62718,#62719,#62720));
#26308=EDGE_LOOP('',(#62721,#62722,#62723,#62724));
#26309=EDGE_LOOP('',(#62725,#62726,#62727,#62728));
#26310=EDGE_LOOP('',(#62729,#62730,#62731,#62732));
#26311=EDGE_LOOP('',(#62733,#62734,#62735,#62736));
#26312=EDGE_LOOP('',(#62737,#62738,#62739,#62740));
#26313=EDGE_LOOP('',(#62741,#62742,#62743,#62744));
#26314=EDGE_LOOP('',(#62745,#62746,#62747,#62748));
#26315=EDGE_LOOP('',(#62749,#62750,#62751,#62752));
#26316=EDGE_LOOP('',(#62753,#62754,#62755,#62756));
#26317=EDGE_LOOP('',(#62757,#62758,#62759,#62760));
#26318=EDGE_LOOP('',(#62761,#62762,#62763,#62764));
#26319=EDGE_LOOP('',(#62765,#62766,#62767,#62768));
#26320=EDGE_LOOP('',(#62769,#62770,#62771,#62772));
#26321=EDGE_LOOP('',(#62773,#62774,#62775,#62776));
#26322=EDGE_LOOP('',(#62777,#62778,#62779,#62780));
#26323=EDGE_LOOP('',(#62781,#62782,#62783,#62784));
#26324=EDGE_LOOP('',(#62785,#62786,#62787,#62788));
#26325=EDGE_LOOP('',(#62789,#62790,#62791,#62792));
#26326=EDGE_LOOP('',(#62793,#62794,#62795,#62796));
#26327=EDGE_LOOP('',(#62797,#62798,#62799,#62800));
#26328=EDGE_LOOP('',(#62801,#62802,#62803,#62804));
#26329=EDGE_LOOP('',(#62805,#62806,#62807,#62808));
#26330=EDGE_LOOP('',(#62809,#62810,#62811,#62812));
#26331=EDGE_LOOP('',(#62813,#62814,#62815,#62816));
#26332=EDGE_LOOP('',(#62817,#62818,#62819,#62820));
#26333=EDGE_LOOP('',(#62821,#62822,#62823,#62824));
#26334=EDGE_LOOP('',(#62825,#62826,#62827,#62828));
#26335=EDGE_LOOP('',(#62829,#62830,#62831,#62832));
#26336=EDGE_LOOP('',(#62833,#62834,#62835,#62836));
#26337=EDGE_LOOP('',(#62837,#62838,#62839,#62840));
#26338=EDGE_LOOP('',(#62841,#62842,#62843,#62844));
#26339=EDGE_LOOP('',(#62845,#62846,#62847,#62848));
#26340=EDGE_LOOP('',(#62849,#62850,#62851,#62852));
#26341=EDGE_LOOP('',(#62853,#62854,#62855,#62856));
#26342=EDGE_LOOP('',(#62857,#62858,#62859,#62860));
#26343=EDGE_LOOP('',(#62861,#62862,#62863,#62864));
#26344=EDGE_LOOP('',(#62865,#62866,#62867,#62868));
#26345=EDGE_LOOP('',(#62869,#62870,#62871,#62872));
#26346=EDGE_LOOP('',(#62873,#62874,#62875,#62876));
#26347=EDGE_LOOP('',(#62877,#62878,#62879,#62880));
#26348=EDGE_LOOP('',(#62881,#62882,#62883,#62884));
#26349=EDGE_LOOP('',(#62885,#62886,#62887,#62888));
#26350=EDGE_LOOP('',(#62889,#62890,#62891,#62892));
#26351=EDGE_LOOP('',(#62893,#62894,#62895,#62896));
#26352=EDGE_LOOP('',(#62897,#62898,#62899,#62900));
#26353=EDGE_LOOP('',(#62901,#62902,#62903,#62904));
#26354=EDGE_LOOP('',(#62905,#62906,#62907,#62908));
#26355=EDGE_LOOP('',(#62909,#62910,#62911,#62912));
#26356=EDGE_LOOP('',(#62913,#62914,#62915,#62916));
#26357=EDGE_LOOP('',(#62917,#62918,#62919,#62920));
#26358=EDGE_LOOP('',(#62921,#62922,#62923,#62924));
#26359=EDGE_LOOP('',(#62925,#62926,#62927,#62928));
#26360=EDGE_LOOP('',(#62929,#62930,#62931,#62932));
#26361=EDGE_LOOP('',(#62933,#62934,#62935,#62936));
#26362=EDGE_LOOP('',(#62937,#62938,#62939,#62940));
#26363=EDGE_LOOP('',(#62941,#62942,#62943,#62944));
#26364=EDGE_LOOP('',(#62945,#62946,#62947,#62948));
#26365=EDGE_LOOP('',(#62949,#62950,#62951,#62952));
#26366=EDGE_LOOP('',(#62953,#62954,#62955,#62956));
#26367=EDGE_LOOP('',(#62957,#62958,#62959,#62960));
#26368=EDGE_LOOP('',(#62961,#62962,#62963,#62964));
#26369=EDGE_LOOP('',(#62965,#62966,#62967,#62968));
#26370=EDGE_LOOP('',(#62969,#62970,#62971,#62972));
#26371=EDGE_LOOP('',(#62973,#62974,#62975,#62976));
#26372=EDGE_LOOP('',(#62977,#62978,#62979,#62980));
#26373=EDGE_LOOP('',(#62981,#62982,#62983,#62984));
#26374=EDGE_LOOP('',(#62985,#62986,#62987,#62988));
#26375=EDGE_LOOP('',(#62989,#62990,#62991,#62992));
#26376=EDGE_LOOP('',(#62993,#62994,#62995,#62996));
#26377=EDGE_LOOP('',(#62997,#62998,#62999,#63000));
#26378=EDGE_LOOP('',(#63001,#63002,#63003,#63004));
#26379=EDGE_LOOP('',(#63005,#63006,#63007,#63008));
#26380=EDGE_LOOP('',(#63009,#63010,#63011,#63012));
#26381=EDGE_LOOP('',(#63013,#63014,#63015,#63016));
#26382=EDGE_LOOP('',(#63017,#63018,#63019,#63020));
#26383=EDGE_LOOP('',(#63021,#63022,#63023,#63024));
#26384=EDGE_LOOP('',(#63025,#63026,#63027,#63028));
#26385=EDGE_LOOP('',(#63029,#63030,#63031,#63032));
#26386=EDGE_LOOP('',(#63033,#63034,#63035,#63036));
#26387=EDGE_LOOP('',(#63037,#63038,#63039,#63040));
#26388=EDGE_LOOP('',(#63041,#63042,#63043,#63044));
#26389=EDGE_LOOP('',(#63045,#63046,#63047,#63048));
#26390=EDGE_LOOP('',(#63049,#63050,#63051,#63052));
#26391=EDGE_LOOP('',(#63053,#63054,#63055,#63056));
#26392=EDGE_LOOP('',(#63057,#63058,#63059,#63060));
#26393=EDGE_LOOP('',(#63061,#63062,#63063,#63064));
#26394=EDGE_LOOP('',(#63065,#63066,#63067,#63068));
#26395=EDGE_LOOP('',(#63069,#63070,#63071,#63072));
#26396=EDGE_LOOP('',(#63073,#63074,#63075,#63076));
#26397=EDGE_LOOP('',(#63077,#63078,#63079,#63080));
#26398=EDGE_LOOP('',(#63081,#63082,#63083,#63084));
#26399=EDGE_LOOP('',(#63085,#63086,#63087,#63088));
#26400=EDGE_LOOP('',(#63089,#63090,#63091,#63092));
#26401=EDGE_LOOP('',(#63093,#63094,#63095,#63096));
#26402=EDGE_LOOP('',(#63097,#63098,#63099,#63100));
#26403=EDGE_LOOP('',(#63101,#63102,#63103,#63104));
#26404=EDGE_LOOP('',(#63105,#63106,#63107,#63108));
#26405=EDGE_LOOP('',(#63109,#63110,#63111,#63112));
#26406=EDGE_LOOP('',(#63113,#63114,#63115,#63116));
#26407=EDGE_LOOP('',(#63117,#63118,#63119,#63120));
#26408=EDGE_LOOP('',(#63121,#63122,#63123,#63124));
#26409=EDGE_LOOP('',(#63125,#63126,#63127,#63128));
#26410=EDGE_LOOP('',(#63129,#63130,#63131,#63132));
#26411=EDGE_LOOP('',(#63133,#63134,#63135,#63136));
#26412=EDGE_LOOP('',(#63137,#63138,#63139,#63140));
#26413=EDGE_LOOP('',(#63141,#63142,#63143,#63144));
#26414=EDGE_LOOP('',(#63145,#63146,#63147,#63148));
#26415=EDGE_LOOP('',(#63149,#63150,#63151,#63152));
#26416=EDGE_LOOP('',(#63153,#63154,#63155,#63156));
#26417=EDGE_LOOP('',(#63157,#63158,#63159,#63160));
#26418=EDGE_LOOP('',(#63161,#63162,#63163,#63164));
#26419=EDGE_LOOP('',(#63165,#63166,#63167,#63168));
#26420=EDGE_LOOP('',(#63169,#63170,#63171,#63172));
#26421=EDGE_LOOP('',(#63173,#63174,#63175,#63176));
#26422=EDGE_LOOP('',(#63177,#63178,#63179,#63180));
#26423=EDGE_LOOP('',(#63181,#63182,#63183,#63184));
#26424=EDGE_LOOP('',(#63185,#63186,#63187,#63188));
#26425=EDGE_LOOP('',(#63189,#63190,#63191,#63192));
#26426=EDGE_LOOP('',(#63193,#63194,#63195,#63196));
#26427=EDGE_LOOP('',(#63197,#63198,#63199,#63200));
#26428=EDGE_LOOP('',(#63201,#63202,#63203,#63204));
#26429=EDGE_LOOP('',(#63205,#63206,#63207,#63208));
#26430=EDGE_LOOP('',(#63209,#63210,#63211,#63212));
#26431=EDGE_LOOP('',(#63213,#63214,#63215,#63216));
#26432=EDGE_LOOP('',(#63217,#63218,#63219,#63220));
#26433=EDGE_LOOP('',(#63221,#63222,#63223,#63224));
#26434=EDGE_LOOP('',(#63225,#63226,#63227,#63228));
#26435=EDGE_LOOP('',(#63229,#63230,#63231,#63232));
#26436=EDGE_LOOP('',(#63233,#63234,#63235,#63236));
#26437=EDGE_LOOP('',(#63237,#63238,#63239,#63240));
#26438=EDGE_LOOP('',(#63241,#63242,#63243,#63244));
#26439=EDGE_LOOP('',(#63245,#63246,#63247,#63248));
#26440=EDGE_LOOP('',(#63249,#63250,#63251,#63252));
#26441=EDGE_LOOP('',(#63253,#63254,#63255,#63256));
#26442=EDGE_LOOP('',(#63257,#63258,#63259,#63260));
#26443=EDGE_LOOP('',(#63261,#63262,#63263,#63264));
#26444=EDGE_LOOP('',(#63265,#63266,#63267,#63268));
#26445=EDGE_LOOP('',(#63269,#63270,#63271,#63272));
#26446=EDGE_LOOP('',(#63273,#63274,#63275,#63276));
#26447=EDGE_LOOP('',(#63277,#63278,#63279,#63280));
#26448=EDGE_LOOP('',(#63281,#63282,#63283,#63284));
#26449=EDGE_LOOP('',(#63285,#63286,#63287,#63288));
#26450=EDGE_LOOP('',(#63289,#63290,#63291,#63292));
#26451=EDGE_LOOP('',(#63293,#63294,#63295,#63296));
#26452=EDGE_LOOP('',(#63297,#63298,#63299,#63300));
#26453=EDGE_LOOP('',(#63301,#63302,#63303,#63304));
#26454=EDGE_LOOP('',(#63305,#63306,#63307,#63308));
#26455=EDGE_LOOP('',(#63309,#63310,#63311,#63312));
#26456=EDGE_LOOP('',(#63313,#63314,#63315,#63316));
#26457=EDGE_LOOP('',(#63317,#63318,#63319,#63320));
#26458=EDGE_LOOP('',(#63321,#63322,#63323,#63324));
#26459=EDGE_LOOP('',(#63325,#63326,#63327,#63328));
#26460=EDGE_LOOP('',(#63329,#63330,#63331,#63332));
#26461=EDGE_LOOP('',(#63333,#63334,#63335,#63336));
#26462=EDGE_LOOP('',(#63337,#63338,#63339,#63340));
#26463=EDGE_LOOP('',(#63341,#63342,#63343,#63344));
#26464=EDGE_LOOP('',(#63345,#63346,#63347,#63348));
#26465=EDGE_LOOP('',(#63349,#63350,#63351,#63352));
#26466=EDGE_LOOP('',(#63353,#63354,#63355,#63356));
#26467=EDGE_LOOP('',(#63357,#63358,#63359,#63360));
#26468=EDGE_LOOP('',(#63361,#63362,#63363,#63364));
#26469=EDGE_LOOP('',(#63365,#63366,#63367,#63368));
#26470=EDGE_LOOP('',(#63369,#63370,#63371,#63372));
#26471=EDGE_LOOP('',(#63373,#63374,#63375,#63376));
#26472=EDGE_LOOP('',(#63377,#63378,#63379,#63380));
#26473=EDGE_LOOP('',(#63381,#63382,#63383,#63384));
#26474=EDGE_LOOP('',(#63385,#63386,#63387,#63388));
#26475=EDGE_LOOP('',(#63389,#63390,#63391,#63392));
#26476=EDGE_LOOP('',(#63393,#63394,#63395,#63396));
#26477=EDGE_LOOP('',(#63397,#63398,#63399,#63400));
#26478=EDGE_LOOP('',(#63401,#63402,#63403,#63404));
#26479=EDGE_LOOP('',(#63405,#63406,#63407,#63408));
#26480=EDGE_LOOP('',(#63409,#63410,#63411,#63412));
#26481=EDGE_LOOP('',(#63413,#63414,#63415,#63416));
#26482=EDGE_LOOP('',(#63417,#63418,#63419,#63420));
#26483=EDGE_LOOP('',(#63421,#63422,#63423,#63424));
#26484=EDGE_LOOP('',(#63425,#63426,#63427,#63428));
#26485=EDGE_LOOP('',(#63429,#63430,#63431,#63432));
#26486=EDGE_LOOP('',(#63433,#63434,#63435,#63436));
#26487=EDGE_LOOP('',(#63437,#63438,#63439,#63440));
#26488=EDGE_LOOP('',(#63441,#63442,#63443,#63444));
#26489=EDGE_LOOP('',(#63445,#63446,#63447,#63448));
#26490=EDGE_LOOP('',(#63449,#63450,#63451,#63452));
#26491=EDGE_LOOP('',(#63453,#63454,#63455,#63456));
#26492=EDGE_LOOP('',(#63457,#63458,#63459,#63460));
#26493=EDGE_LOOP('',(#63461,#63462,#63463,#63464));
#26494=EDGE_LOOP('',(#63465,#63466,#63467,#63468));
#26495=EDGE_LOOP('',(#63469,#63470,#63471,#63472));
#26496=EDGE_LOOP('',(#63473,#63474,#63475,#63476));
#26497=EDGE_LOOP('',(#63477,#63478,#63479,#63480));
#26498=EDGE_LOOP('',(#63481,#63482,#63483,#63484));
#26499=EDGE_LOOP('',(#63485,#63486,#63487,#63488));
#26500=EDGE_LOOP('',(#63489,#63490,#63491,#63492));
#26501=EDGE_LOOP('',(#63493,#63494,#63495,#63496));
#26502=EDGE_LOOP('',(#63497,#63498,#63499,#63500));
#26503=EDGE_LOOP('',(#63501,#63502,#63503,#63504));
#26504=EDGE_LOOP('',(#63505,#63506,#63507,#63508));
#26505=EDGE_LOOP('',(#63509,#63510,#63511,#63512));
#26506=EDGE_LOOP('',(#63513,#63514,#63515,#63516));
#26507=EDGE_LOOP('',(#63517,#63518,#63519,#63520));
#26508=EDGE_LOOP('',(#63521,#63522,#63523,#63524));
#26509=EDGE_LOOP('',(#63525,#63526,#63527,#63528));
#26510=EDGE_LOOP('',(#63529,#63530,#63531,#63532));
#26511=EDGE_LOOP('',(#63533,#63534,#63535,#63536));
#26512=EDGE_LOOP('',(#63537,#63538,#63539,#63540));
#26513=EDGE_LOOP('',(#63541,#63542,#63543,#63544));
#26514=EDGE_LOOP('',(#63545,#63546,#63547,#63548));
#26515=EDGE_LOOP('',(#63549,#63550,#63551,#63552));
#26516=EDGE_LOOP('',(#63553,#63554,#63555,#63556));
#26517=EDGE_LOOP('',(#63557,#63558,#63559,#63560));
#26518=EDGE_LOOP('',(#63561,#63562,#63563,#63564));
#26519=EDGE_LOOP('',(#63565,#63566,#63567,#63568));
#26520=EDGE_LOOP('',(#63569,#63570,#63571,#63572));
#26521=EDGE_LOOP('',(#63573,#63574,#63575,#63576));
#26522=EDGE_LOOP('',(#63577,#63578,#63579,#63580));
#26523=EDGE_LOOP('',(#63581,#63582,#63583,#63584));
#26524=EDGE_LOOP('',(#63585,#63586,#63587,#63588));
#26525=EDGE_LOOP('',(#63589,#63590,#63591,#63592));
#26526=EDGE_LOOP('',(#63593,#63594,#63595,#63596));
#26527=EDGE_LOOP('',(#63597,#63598,#63599,#63600));
#26528=EDGE_LOOP('',(#63601,#63602,#63603,#63604));
#26529=EDGE_LOOP('',(#63605,#63606,#63607,#63608));
#26530=EDGE_LOOP('',(#63609,#63610,#63611,#63612));
#26531=EDGE_LOOP('',(#63613,#63614,#63615,#63616));
#26532=EDGE_LOOP('',(#63617,#63618,#63619,#63620));
#26533=EDGE_LOOP('',(#63621,#63622,#63623,#63624));
#26534=EDGE_LOOP('',(#63625,#63626,#63627,#63628));
#26535=EDGE_LOOP('',(#63629,#63630,#63631,#63632));
#26536=EDGE_LOOP('',(#63633,#63634,#63635,#63636));
#26537=EDGE_LOOP('',(#63637,#63638,#63639,#63640));
#26538=EDGE_LOOP('',(#63641,#63642,#63643,#63644));
#26539=EDGE_LOOP('',(#63645,#63646,#63647,#63648));
#26540=EDGE_LOOP('',(#63649,#63650,#63651,#63652));
#26541=EDGE_LOOP('',(#63653,#63654,#63655,#63656));
#26542=EDGE_LOOP('',(#63657,#63658,#63659,#63660));
#26543=EDGE_LOOP('',(#63661,#63662,#63663,#63664));
#26544=EDGE_LOOP('',(#63665,#63666,#63667,#63668));
#26545=EDGE_LOOP('',(#63669,#63670,#63671,#63672));
#26546=EDGE_LOOP('',(#63673,#63674,#63675,#63676));
#26547=EDGE_LOOP('',(#63677,#63678,#63679,#63680));
#26548=EDGE_LOOP('',(#63681,#63682,#63683,#63684));
#26549=EDGE_LOOP('',(#63685,#63686,#63687,#63688));
#26550=EDGE_LOOP('',(#63689,#63690,#63691,#63692));
#26551=EDGE_LOOP('',(#63693,#63694,#63695,#63696));
#26552=EDGE_LOOP('',(#63697,#63698,#63699,#63700));
#26553=EDGE_LOOP('',(#63701,#63702,#63703,#63704));
#26554=EDGE_LOOP('',(#63705,#63706,#63707,#63708));
#26555=EDGE_LOOP('',(#63709,#63710,#63711,#63712));
#26556=EDGE_LOOP('',(#63713,#63714,#63715,#63716));
#26557=EDGE_LOOP('',(#63717,#63718,#63719,#63720));
#26558=EDGE_LOOP('',(#63721,#63722,#63723,#63724));
#26559=EDGE_LOOP('',(#63725,#63726,#63727,#63728));
#26560=EDGE_LOOP('',(#63729,#63730,#63731,#63732));
#26561=EDGE_LOOP('',(#63733,#63734,#63735,#63736));
#26562=EDGE_LOOP('',(#63737,#63738,#63739,#63740));
#26563=EDGE_LOOP('',(#63741,#63742,#63743,#63744));
#26564=EDGE_LOOP('',(#63745,#63746,#63747,#63748));
#26565=EDGE_LOOP('',(#63749,#63750,#63751,#63752));
#26566=EDGE_LOOP('',(#63753,#63754,#63755,#63756));
#26567=EDGE_LOOP('',(#63757,#63758,#63759,#63760));
#26568=EDGE_LOOP('',(#63761,#63762,#63763,#63764));
#26569=EDGE_LOOP('',(#63765,#63766,#63767,#63768));
#26570=EDGE_LOOP('',(#63769,#63770,#63771,#63772));
#26571=EDGE_LOOP('',(#63773,#63774,#63775,#63776));
#26572=EDGE_LOOP('',(#63777,#63778,#63779,#63780));
#26573=EDGE_LOOP('',(#63781,#63782,#63783,#63784));
#26574=EDGE_LOOP('',(#63785,#63786,#63787,#63788));
#26575=EDGE_LOOP('',(#63789,#63790,#63791,#63792));
#26576=EDGE_LOOP('',(#63793,#63794,#63795,#63796));
#26577=EDGE_LOOP('',(#63797,#63798,#63799,#63800));
#26578=EDGE_LOOP('',(#63801,#63802,#63803,#63804));
#26579=EDGE_LOOP('',(#63805,#63806,#63807,#63808));
#26580=EDGE_LOOP('',(#63809,#63810,#63811,#63812));
#26581=EDGE_LOOP('',(#63813,#63814,#63815,#63816));
#26582=EDGE_LOOP('',(#63817,#63818,#63819,#63820));
#26583=EDGE_LOOP('',(#63821,#63822,#63823,#63824));
#26584=EDGE_LOOP('',(#63825,#63826,#63827,#63828));
#26585=EDGE_LOOP('',(#63829,#63830,#63831,#63832));
#26586=EDGE_LOOP('',(#63833,#63834,#63835,#63836));
#26587=EDGE_LOOP('',(#63837,#63838,#63839,#63840));
#26588=EDGE_LOOP('',(#63841,#63842,#63843,#63844));
#26589=EDGE_LOOP('',(#63845,#63846,#63847,#63848));
#26590=EDGE_LOOP('',(#63849,#63850,#63851,#63852));
#26591=EDGE_LOOP('',(#63853,#63854,#63855,#63856));
#26592=EDGE_LOOP('',(#63857,#63858,#63859,#63860));
#26593=EDGE_LOOP('',(#63861,#63862,#63863,#63864));
#26594=EDGE_LOOP('',(#63865,#63866,#63867,#63868));
#26595=EDGE_LOOP('',(#63869,#63870,#63871,#63872));
#26596=EDGE_LOOP('',(#63873,#63874,#63875,#63876));
#26597=EDGE_LOOP('',(#63877,#63878,#63879,#63880));
#26598=EDGE_LOOP('',(#63881,#63882,#63883,#63884));
#26599=EDGE_LOOP('',(#63885,#63886,#63887,#63888));
#26600=EDGE_LOOP('',(#63889,#63890,#63891,#63892));
#26601=EDGE_LOOP('',(#63893,#63894,#63895,#63896));
#26602=EDGE_LOOP('',(#63897,#63898,#63899,#63900));
#26603=EDGE_LOOP('',(#63901,#63902,#63903,#63904));
#26604=EDGE_LOOP('',(#63905,#63906,#63907,#63908));
#26605=EDGE_LOOP('',(#63909,#63910,#63911,#63912));
#26606=EDGE_LOOP('',(#63913,#63914,#63915,#63916));
#26607=EDGE_LOOP('',(#63917,#63918,#63919,#63920));
#26608=EDGE_LOOP('',(#63921,#63922,#63923,#63924));
#26609=EDGE_LOOP('',(#63925,#63926,#63927,#63928));
#26610=EDGE_LOOP('',(#63929,#63930,#63931,#63932));
#26611=EDGE_LOOP('',(#63933,#63934,#63935,#63936));
#26612=EDGE_LOOP('',(#63937,#63938,#63939,#63940));
#26613=EDGE_LOOP('',(#63941,#63942,#63943,#63944));
#26614=EDGE_LOOP('',(#63945,#63946,#63947,#63948));
#26615=EDGE_LOOP('',(#63949,#63950,#63951,#63952));
#26616=EDGE_LOOP('',(#63953,#63954,#63955,#63956));
#26617=EDGE_LOOP('',(#63957,#63958,#63959,#63960));
#26618=EDGE_LOOP('',(#63961,#63962,#63963,#63964));
#26619=EDGE_LOOP('',(#63965,#63966,#63967,#63968));
#26620=EDGE_LOOP('',(#63969,#63970,#63971,#63972));
#26621=EDGE_LOOP('',(#63973,#63974,#63975,#63976));
#26622=EDGE_LOOP('',(#63977,#63978,#63979,#63980));
#26623=EDGE_LOOP('',(#63981,#63982,#63983,#63984));
#26624=EDGE_LOOP('',(#63985,#63986,#63987,#63988));
#26625=EDGE_LOOP('',(#63989,#63990,#63991,#63992));
#26626=EDGE_LOOP('',(#63993,#63994,#63995,#63996));
#26627=EDGE_LOOP('',(#63997,#63998,#63999,#64000));
#26628=EDGE_LOOP('',(#64001,#64002,#64003,#64004));
#26629=EDGE_LOOP('',(#64005,#64006,#64007,#64008));
#26630=EDGE_LOOP('',(#64009,#64010,#64011,#64012));
#26631=EDGE_LOOP('',(#64013,#64014,#64015,#64016));
#26632=EDGE_LOOP('',(#64017,#64018,#64019,#64020));
#26633=EDGE_LOOP('',(#64021,#64022,#64023,#64024));
#26634=EDGE_LOOP('',(#64025,#64026,#64027,#64028));
#26635=EDGE_LOOP('',(#64029,#64030,#64031,#64032));
#26636=EDGE_LOOP('',(#64033,#64034,#64035,#64036));
#26637=EDGE_LOOP('',(#64037,#64038,#64039,#64040));
#26638=EDGE_LOOP('',(#64041,#64042,#64043,#64044));
#26639=EDGE_LOOP('',(#64045,#64046,#64047,#64048));
#26640=EDGE_LOOP('',(#64049,#64050,#64051,#64052));
#26641=EDGE_LOOP('',(#64053,#64054,#64055,#64056));
#26642=EDGE_LOOP('',(#64057,#64058,#64059,#64060));
#26643=EDGE_LOOP('',(#64061,#64062,#64063,#64064));
#26644=EDGE_LOOP('',(#64065,#64066,#64067,#64068));
#26645=EDGE_LOOP('',(#64069,#64070,#64071,#64072));
#26646=EDGE_LOOP('',(#64073,#64074,#64075,#64076));
#26647=EDGE_LOOP('',(#64077,#64078,#64079,#64080));
#26648=EDGE_LOOP('',(#64081,#64082,#64083,#64084));
#26649=EDGE_LOOP('',(#64085,#64086,#64087,#64088));
#26650=EDGE_LOOP('',(#64089,#64090,#64091,#64092));
#26651=EDGE_LOOP('',(#64093,#64094,#64095,#64096));
#26652=EDGE_LOOP('',(#64097,#64098,#64099,#64100));
#26653=EDGE_LOOP('',(#64101,#64102,#64103,#64104));
#26654=EDGE_LOOP('',(#64105,#64106,#64107,#64108));
#26655=EDGE_LOOP('',(#64109,#64110,#64111,#64112));
#26656=EDGE_LOOP('',(#64113,#64114,#64115,#64116));
#26657=EDGE_LOOP('',(#64117,#64118,#64119,#64120));
#26658=EDGE_LOOP('',(#64121,#64122,#64123,#64124));
#26659=EDGE_LOOP('',(#64125,#64126,#64127,#64128));
#26660=EDGE_LOOP('',(#64129,#64130,#64131,#64132));
#26661=EDGE_LOOP('',(#64133,#64134,#64135,#64136));
#26662=EDGE_LOOP('',(#64137,#64138,#64139,#64140));
#26663=EDGE_LOOP('',(#64141,#64142,#64143,#64144));
#26664=EDGE_LOOP('',(#64145,#64146,#64147,#64148));
#26665=EDGE_LOOP('',(#64149,#64150,#64151,#64152));
#26666=EDGE_LOOP('',(#64153,#64154,#64155,#64156));
#26667=EDGE_LOOP('',(#64157,#64158,#64159,#64160));
#26668=EDGE_LOOP('',(#64161,#64162,#64163,#64164));
#26669=EDGE_LOOP('',(#64165,#64166,#64167,#64168));
#26670=EDGE_LOOP('',(#64169,#64170,#64171,#64172));
#26671=EDGE_LOOP('',(#64173,#64174,#64175,#64176));
#26672=EDGE_LOOP('',(#64177,#64178,#64179,#64180));
#26673=EDGE_LOOP('',(#64181,#64182,#64183,#64184));
#26674=EDGE_LOOP('',(#64185,#64186,#64187,#64188));
#26675=EDGE_LOOP('',(#64189,#64190,#64191,#64192));
#26676=EDGE_LOOP('',(#64193,#64194,#64195,#64196));
#26677=EDGE_LOOP('',(#64197,#64198,#64199,#64200));
#26678=EDGE_LOOP('',(#64201,#64202,#64203,#64204));
#26679=EDGE_LOOP('',(#64205,#64206,#64207,#64208));
#26680=EDGE_LOOP('',(#64209,#64210,#64211,#64212));
#26681=EDGE_LOOP('',(#64213,#64214,#64215,#64216));
#26682=EDGE_LOOP('',(#64217,#64218,#64219,#64220));
#26683=EDGE_LOOP('',(#64221,#64222,#64223,#64224));
#26684=EDGE_LOOP('',(#64225,#64226,#64227,#64228));
#26685=EDGE_LOOP('',(#64229,#64230,#64231,#64232));
#26686=EDGE_LOOP('',(#64233,#64234,#64235,#64236));
#26687=EDGE_LOOP('',(#64237,#64238,#64239,#64240));
#26688=EDGE_LOOP('',(#64241,#64242,#64243,#64244));
#26689=EDGE_LOOP('',(#64245,#64246,#64247,#64248));
#26690=EDGE_LOOP('',(#64249,#64250,#64251,#64252));
#26691=EDGE_LOOP('',(#64253,#64254,#64255,#64256));
#26692=EDGE_LOOP('',(#64257,#64258,#64259,#64260));
#26693=EDGE_LOOP('',(#64261,#64262,#64263,#64264));
#26694=EDGE_LOOP('',(#64265,#64266,#64267,#64268));
#26695=EDGE_LOOP('',(#64269,#64270,#64271,#64272));
#26696=EDGE_LOOP('',(#64273,#64274,#64275,#64276));
#26697=EDGE_LOOP('',(#64277,#64278,#64279,#64280));
#26698=EDGE_LOOP('',(#64281,#64282,#64283,#64284));
#26699=EDGE_LOOP('',(#64285,#64286,#64287,#64288));
#26700=EDGE_LOOP('',(#64289,#64290,#64291,#64292));
#26701=EDGE_LOOP('',(#64293,#64294,#64295,#64296));
#26702=EDGE_LOOP('',(#64297,#64298,#64299,#64300));
#26703=EDGE_LOOP('',(#64301,#64302,#64303,#64304));
#26704=EDGE_LOOP('',(#64305,#64306,#64307,#64308));
#26705=EDGE_LOOP('',(#64309,#64310,#64311,#64312));
#26706=EDGE_LOOP('',(#64313,#64314,#64315,#64316));
#26707=EDGE_LOOP('',(#64317,#64318,#64319,#64320));
#26708=EDGE_LOOP('',(#64321,#64322,#64323,#64324));
#26709=EDGE_LOOP('',(#64325,#64326,#64327,#64328));
#26710=EDGE_LOOP('',(#64329,#64330,#64331,#64332));
#26711=EDGE_LOOP('',(#64333,#64334,#64335,#64336));
#26712=EDGE_LOOP('',(#64337,#64338,#64339,#64340));
#26713=EDGE_LOOP('',(#64341,#64342,#64343,#64344));
#26714=EDGE_LOOP('',(#64345,#64346,#64347,#64348));
#26715=EDGE_LOOP('',(#64349,#64350,#64351,#64352));
#26716=EDGE_LOOP('',(#64353,#64354,#64355,#64356));
#26717=EDGE_LOOP('',(#64357,#64358,#64359,#64360));
#26718=EDGE_LOOP('',(#64361,#64362,#64363,#64364));
#26719=EDGE_LOOP('',(#64365,#64366,#64367,#64368));
#26720=EDGE_LOOP('',(#64369,#64370,#64371,#64372));
#26721=EDGE_LOOP('',(#64373,#64374,#64375,#64376));
#26722=EDGE_LOOP('',(#64377,#64378,#64379,#64380));
#26723=EDGE_LOOP('',(#64381,#64382,#64383,#64384));
#26724=EDGE_LOOP('',(#64385,#64386,#64387,#64388));
#26725=EDGE_LOOP('',(#64389,#64390,#64391,#64392));
#26726=EDGE_LOOP('',(#64393,#64394,#64395,#64396));
#26727=EDGE_LOOP('',(#64397,#64398,#64399,#64400));
#26728=EDGE_LOOP('',(#64401,#64402,#64403,#64404));
#26729=EDGE_LOOP('',(#64405,#64406,#64407,#64408));
#26730=EDGE_LOOP('',(#64409,#64410,#64411,#64412));
#26731=EDGE_LOOP('',(#64413,#64414,#64415,#64416));
#26732=EDGE_LOOP('',(#64417,#64418,#64419,#64420));
#26733=EDGE_LOOP('',(#64421,#64422,#64423,#64424));
#26734=EDGE_LOOP('',(#64425,#64426,#64427,#64428));
#26735=EDGE_LOOP('',(#64429,#64430,#64431,#64432));
#26736=EDGE_LOOP('',(#64433,#64434,#64435,#64436));
#26737=EDGE_LOOP('',(#64437,#64438,#64439,#64440));
#26738=EDGE_LOOP('',(#64441,#64442,#64443,#64444));
#26739=EDGE_LOOP('',(#64445,#64446,#64447,#64448));
#26740=EDGE_LOOP('',(#64449,#64450,#64451,#64452));
#26741=EDGE_LOOP('',(#64453,#64454,#64455,#64456));
#26742=EDGE_LOOP('',(#64457,#64458,#64459,#64460));
#26743=EDGE_LOOP('',(#64461,#64462,#64463,#64464));
#26744=EDGE_LOOP('',(#64465,#64466,#64467,#64468));
#26745=EDGE_LOOP('',(#64469,#64470,#64471,#64472));
#26746=EDGE_LOOP('',(#64473,#64474,#64475,#64476));
#26747=EDGE_LOOP('',(#64477,#64478,#64479,#64480));
#26748=EDGE_LOOP('',(#64481,#64482,#64483,#64484));
#26749=EDGE_LOOP('',(#64485,#64486,#64487,#64488));
#26750=EDGE_LOOP('',(#64489,#64490,#64491,#64492));
#26751=EDGE_LOOP('',(#64493,#64494,#64495,#64496));
#26752=EDGE_LOOP('',(#64497,#64498,#64499,#64500));
#26753=EDGE_LOOP('',(#64501,#64502,#64503,#64504));
#26754=EDGE_LOOP('',(#64505,#64506,#64507,#64508));
#26755=EDGE_LOOP('',(#64509,#64510,#64511,#64512));
#26756=EDGE_LOOP('',(#64513,#64514,#64515,#64516));
#26757=EDGE_LOOP('',(#64517,#64518,#64519,#64520));
#26758=EDGE_LOOP('',(#64521,#64522,#64523,#64524));
#26759=EDGE_LOOP('',(#64525,#64526,#64527,#64528));
#26760=EDGE_LOOP('',(#64529,#64530,#64531,#64532));
#26761=EDGE_LOOP('',(#64533,#64534,#64535,#64536));
#26762=EDGE_LOOP('',(#64537,#64538,#64539,#64540));
#26763=EDGE_LOOP('',(#64541,#64542,#64543,#64544));
#26764=EDGE_LOOP('',(#64545,#64546,#64547,#64548));
#26765=EDGE_LOOP('',(#64549,#64550,#64551,#64552));
#26766=EDGE_LOOP('',(#64553,#64554,#64555,#64556));
#26767=EDGE_LOOP('',(#64557,#64558,#64559,#64560));
#26768=EDGE_LOOP('',(#64561,#64562,#64563,#64564));
#26769=EDGE_LOOP('',(#64565,#64566,#64567,#64568));
#26770=EDGE_LOOP('',(#64569,#64570,#64571,#64572));
#26771=EDGE_LOOP('',(#64573,#64574,#64575,#64576));
#26772=EDGE_LOOP('',(#64577,#64578,#64579,#64580));
#26773=EDGE_LOOP('',(#64581,#64582,#64583,#64584));
#26774=EDGE_LOOP('',(#64585,#64586,#64587,#64588));
#26775=EDGE_LOOP('',(#64589,#64590,#64591,#64592));
#26776=EDGE_LOOP('',(#64593,#64594,#64595,#64596));
#26777=EDGE_LOOP('',(#64597,#64598,#64599,#64600));
#26778=EDGE_LOOP('',(#64601,#64602,#64603,#64604));
#26779=EDGE_LOOP('',(#64605,#64606,#64607,#64608));
#26780=EDGE_LOOP('',(#64609,#64610,#64611,#64612));
#26781=EDGE_LOOP('',(#64613,#64614,#64615,#64616));
#26782=EDGE_LOOP('',(#64617,#64618,#64619,#64620));
#26783=EDGE_LOOP('',(#64621,#64622,#64623,#64624));
#26784=EDGE_LOOP('',(#64625,#64626,#64627,#64628));
#26785=EDGE_LOOP('',(#64629,#64630,#64631,#64632));
#26786=EDGE_LOOP('',(#64633,#64634,#64635,#64636));
#26787=EDGE_LOOP('',(#64637,#64638,#64639,#64640));
#26788=EDGE_LOOP('',(#64641,#64642,#64643,#64644));
#26789=EDGE_LOOP('',(#64645,#64646,#64647,#64648));
#26790=EDGE_LOOP('',(#64649,#64650,#64651,#64652));
#26791=EDGE_LOOP('',(#64653,#64654,#64655,#64656));
#26792=EDGE_LOOP('',(#64657,#64658,#64659,#64660));
#26793=EDGE_LOOP('',(#64661,#64662,#64663,#64664));
#26794=EDGE_LOOP('',(#64665,#64666,#64667,#64668));
#26795=EDGE_LOOP('',(#64669,#64670,#64671,#64672));
#26796=EDGE_LOOP('',(#64673,#64674,#64675,#64676));
#26797=EDGE_LOOP('',(#64677,#64678,#64679,#64680));
#26798=EDGE_LOOP('',(#64681,#64682,#64683,#64684));
#26799=EDGE_LOOP('',(#64685,#64686,#64687,#64688));
#26800=EDGE_LOOP('',(#64689,#64690,#64691,#64692));
#26801=EDGE_LOOP('',(#64693,#64694,#64695,#64696));
#26802=EDGE_LOOP('',(#64697,#64698,#64699,#64700));
#26803=EDGE_LOOP('',(#64701,#64702,#64703,#64704));
#26804=EDGE_LOOP('',(#64705,#64706,#64707,#64708));
#26805=EDGE_LOOP('',(#64709,#64710,#64711,#64712));
#26806=EDGE_LOOP('',(#64713,#64714,#64715,#64716));
#26807=EDGE_LOOP('',(#64717,#64718,#64719,#64720));
#26808=EDGE_LOOP('',(#64721,#64722,#64723,#64724));
#26809=EDGE_LOOP('',(#64725,#64726,#64727,#64728));
#26810=EDGE_LOOP('',(#64729,#64730,#64731,#64732));
#26811=EDGE_LOOP('',(#64733,#64734,#64735,#64736));
#26812=EDGE_LOOP('',(#64737,#64738,#64739,#64740));
#26813=EDGE_LOOP('',(#64741,#64742,#64743,#64744));
#26814=EDGE_LOOP('',(#64745,#64746,#64747,#64748));
#26815=EDGE_LOOP('',(#64749,#64750,#64751,#64752));
#26816=EDGE_LOOP('',(#64753,#64754,#64755,#64756));
#26817=EDGE_LOOP('',(#64757,#64758,#64759,#64760));
#26818=EDGE_LOOP('',(#64761,#64762,#64763,#64764));
#26819=EDGE_LOOP('',(#64765,#64766,#64767,#64768));
#26820=EDGE_LOOP('',(#64769,#64770,#64771,#64772));
#26821=EDGE_LOOP('',(#64773,#64774,#64775,#64776));
#26822=EDGE_LOOP('',(#64777,#64778,#64779,#64780));
#26823=EDGE_LOOP('',(#64781,#64782,#64783,#64784));
#26824=EDGE_LOOP('',(#64785,#64786,#64787,#64788));
#26825=EDGE_LOOP('',(#64789,#64790,#64791,#64792));
#26826=EDGE_LOOP('',(#64793,#64794,#64795,#64796));
#26827=EDGE_LOOP('',(#64797,#64798,#64799,#64800));
#26828=EDGE_LOOP('',(#64801,#64802,#64803,#64804));
#26829=EDGE_LOOP('',(#64805,#64806,#64807,#64808));
#26830=EDGE_LOOP('',(#64809,#64810,#64811,#64812));
#26831=EDGE_LOOP('',(#64813,#64814,#64815,#64816));
#26832=EDGE_LOOP('',(#64817,#64818,#64819,#64820));
#26833=EDGE_LOOP('',(#64821,#64822,#64823,#64824));
#26834=EDGE_LOOP('',(#64825,#64826,#64827,#64828));
#26835=EDGE_LOOP('',(#64829,#64830,#64831,#64832));
#26836=EDGE_LOOP('',(#64833,#64834,#64835,#64836));
#26837=EDGE_LOOP('',(#64837,#64838,#64839,#64840));
#26838=EDGE_LOOP('',(#64841,#64842,#64843,#64844));
#26839=EDGE_LOOP('',(#64845,#64846,#64847,#64848));
#26840=EDGE_LOOP('',(#64849,#64850,#64851,#64852));
#26841=EDGE_LOOP('',(#64853,#64854,#64855,#64856));
#26842=EDGE_LOOP('',(#64857,#64858,#64859,#64860));
#26843=EDGE_LOOP('',(#64861,#64862,#64863,#64864));
#26844=EDGE_LOOP('',(#64865,#64866,#64867,#64868));
#26845=EDGE_LOOP('',(#64869,#64870,#64871,#64872));
#26846=EDGE_LOOP('',(#64873,#64874,#64875,#64876));
#26847=EDGE_LOOP('',(#64877,#64878,#64879,#64880));
#26848=EDGE_LOOP('',(#64881,#64882,#64883,#64884));
#26849=EDGE_LOOP('',(#64885,#64886,#64887,#64888));
#26850=EDGE_LOOP('',(#64889,#64890,#64891,#64892));
#26851=EDGE_LOOP('',(#64893,#64894,#64895,#64896));
#26852=EDGE_LOOP('',(#64897,#64898,#64899,#64900));
#26853=EDGE_LOOP('',(#64901,#64902,#64903,#64904));
#26854=EDGE_LOOP('',(#64905,#64906,#64907,#64908));
#26855=EDGE_LOOP('',(#64909,#64910,#64911,#64912));
#26856=EDGE_LOOP('',(#64913,#64914,#64915,#64916));
#26857=EDGE_LOOP('',(#64917,#64918,#64919,#64920));
#26858=EDGE_LOOP('',(#64921,#64922,#64923,#64924));
#26859=EDGE_LOOP('',(#64925,#64926,#64927,#64928));
#26860=EDGE_LOOP('',(#64929,#64930,#64931,#64932));
#26861=EDGE_LOOP('',(#64933,#64934,#64935,#64936));
#26862=EDGE_LOOP('',(#64937,#64938,#64939,#64940));
#26863=EDGE_LOOP('',(#64941,#64942,#64943,#64944));
#26864=EDGE_LOOP('',(#64945,#64946,#64947,#64948));
#26865=EDGE_LOOP('',(#64949,#64950,#64951,#64952));
#26866=EDGE_LOOP('',(#64953,#64954,#64955,#64956));
#26867=EDGE_LOOP('',(#64957,#64958,#64959,#64960));
#26868=EDGE_LOOP('',(#64961,#64962,#64963,#64964));
#26869=EDGE_LOOP('',(#64965,#64966,#64967,#64968));
#26870=EDGE_LOOP('',(#64969,#64970,#64971,#64972));
#26871=EDGE_LOOP('',(#64973,#64974,#64975,#64976));
#26872=EDGE_LOOP('',(#64977,#64978,#64979,#64980));
#26873=EDGE_LOOP('',(#64981,#64982,#64983,#64984));
#26874=EDGE_LOOP('',(#64985,#64986,#64987,#64988));
#26875=EDGE_LOOP('',(#64989,#64990,#64991,#64992));
#26876=EDGE_LOOP('',(#64993,#64994,#64995,#64996));
#26877=EDGE_LOOP('',(#64997,#64998,#64999,#65000));
#26878=EDGE_LOOP('',(#65001,#65002,#65003,#65004));
#26879=EDGE_LOOP('',(#65005,#65006,#65007,#65008));
#26880=EDGE_LOOP('',(#65009,#65010,#65011,#65012));
#26881=EDGE_LOOP('',(#65013,#65014,#65015,#65016));
#26882=EDGE_LOOP('',(#65017,#65018,#65019,#65020));
#26883=EDGE_LOOP('',(#65021,#65022,#65023,#65024));
#26884=EDGE_LOOP('',(#65025,#65026,#65027,#65028));
#26885=EDGE_LOOP('',(#65029,#65030,#65031,#65032));
#26886=EDGE_LOOP('',(#65033,#65034,#65035,#65036));
#26887=EDGE_LOOP('',(#65037,#65038,#65039,#65040));
#26888=EDGE_LOOP('',(#65041,#65042,#65043,#65044));
#26889=EDGE_LOOP('',(#65045,#65046,#65047,#65048));
#26890=EDGE_LOOP('',(#65049,#65050,#65051,#65052));
#26891=EDGE_LOOP('',(#65053,#65054,#65055,#65056));
#26892=EDGE_LOOP('',(#65057,#65058,#65059,#65060));
#26893=EDGE_LOOP('',(#65061,#65062,#65063,#65064));
#26894=EDGE_LOOP('',(#65065,#65066,#65067,#65068));
#26895=EDGE_LOOP('',(#65069,#65070,#65071,#65072));
#26896=EDGE_LOOP('',(#65073,#65074,#65075,#65076));
#26897=EDGE_LOOP('',(#65077,#65078,#65079,#65080));
#26898=EDGE_LOOP('',(#65081,#65082,#65083,#65084));
#26899=EDGE_LOOP('',(#65085,#65086,#65087,#65088));
#26900=EDGE_LOOP('',(#65089,#65090,#65091,#65092));
#26901=EDGE_LOOP('',(#65093,#65094,#65095,#65096));
#26902=EDGE_LOOP('',(#65097,#65098,#65099,#65100));
#26903=EDGE_LOOP('',(#65101,#65102,#65103,#65104));
#26904=EDGE_LOOP('',(#65105,#65106,#65107,#65108));
#26905=EDGE_LOOP('',(#65109,#65110,#65111,#65112));
#26906=EDGE_LOOP('',(#65113,#65114,#65115,#65116));
#26907=EDGE_LOOP('',(#65117,#65118,#65119,#65120));
#26908=EDGE_LOOP('',(#65121,#65122,#65123,#65124));
#26909=EDGE_LOOP('',(#65125,#65126,#65127,#65128));
#26910=EDGE_LOOP('',(#65129,#65130,#65131,#65132));
#26911=EDGE_LOOP('',(#65133,#65134,#65135,#65136));
#26912=EDGE_LOOP('',(#65137,#65138,#65139,#65140));
#26913=EDGE_LOOP('',(#65141,#65142,#65143,#65144));
#26914=EDGE_LOOP('',(#65145,#65146,#65147,#65148));
#26915=EDGE_LOOP('',(#65149,#65150,#65151,#65152));
#26916=EDGE_LOOP('',(#65153,#65154,#65155,#65156));
#26917=EDGE_LOOP('',(#65157,#65158,#65159,#65160));
#26918=EDGE_LOOP('',(#65161,#65162,#65163,#65164));
#26919=EDGE_LOOP('',(#65165,#65166,#65167,#65168));
#26920=EDGE_LOOP('',(#65169,#65170,#65171,#65172));
#26921=EDGE_LOOP('',(#65173,#65174,#65175,#65176));
#26922=EDGE_LOOP('',(#65177,#65178,#65179,#65180));
#26923=EDGE_LOOP('',(#65181,#65182,#65183,#65184));
#26924=EDGE_LOOP('',(#65185,#65186,#65187,#65188));
#26925=EDGE_LOOP('',(#65189,#65190,#65191,#65192));
#26926=EDGE_LOOP('',(#65193,#65194,#65195,#65196));
#26927=EDGE_LOOP('',(#65197,#65198,#65199,#65200));
#26928=EDGE_LOOP('',(#65201,#65202,#65203,#65204));
#26929=EDGE_LOOP('',(#65205,#65206,#65207,#65208));
#26930=EDGE_LOOP('',(#65209,#65210,#65211,#65212));
#26931=EDGE_LOOP('',(#65213,#65214,#65215,#65216));
#26932=EDGE_LOOP('',(#65217,#65218,#65219,#65220));
#26933=EDGE_LOOP('',(#65221,#65222,#65223,#65224));
#26934=EDGE_LOOP('',(#65225,#65226,#65227,#65228));
#26935=EDGE_LOOP('',(#65229,#65230,#65231,#65232));
#26936=EDGE_LOOP('',(#65233,#65234,#65235,#65236));
#26937=EDGE_LOOP('',(#65237,#65238,#65239,#65240));
#26938=EDGE_LOOP('',(#65241,#65242,#65243,#65244));
#26939=EDGE_LOOP('',(#65245,#65246,#65247,#65248));
#26940=EDGE_LOOP('',(#65249,#65250,#65251,#65252));
#26941=EDGE_LOOP('',(#65253,#65254,#65255,#65256));
#26942=EDGE_LOOP('',(#65257,#65258,#65259,#65260));
#26943=EDGE_LOOP('',(#65261,#65262,#65263,#65264));
#26944=EDGE_LOOP('',(#65265,#65266,#65267,#65268));
#26945=EDGE_LOOP('',(#65269,#65270,#65271,#65272));
#26946=EDGE_LOOP('',(#65273,#65274,#65275,#65276));
#26947=EDGE_LOOP('',(#65277,#65278,#65279,#65280));
#26948=EDGE_LOOP('',(#65281,#65282,#65283,#65284));
#26949=EDGE_LOOP('',(#65285,#65286,#65287,#65288));
#26950=EDGE_LOOP('',(#65289,#65290,#65291,#65292));
#26951=EDGE_LOOP('',(#65293,#65294,#65295,#65296));
#26952=EDGE_LOOP('',(#65297,#65298,#65299,#65300));
#26953=EDGE_LOOP('',(#65301,#65302,#65303,#65304));
#26954=EDGE_LOOP('',(#65305,#65306,#65307,#65308));
#26955=EDGE_LOOP('',(#65309,#65310,#65311,#65312));
#26956=EDGE_LOOP('',(#65313,#65314,#65315,#65316));
#26957=EDGE_LOOP('',(#65317,#65318,#65319,#65320));
#26958=EDGE_LOOP('',(#65321,#65322,#65323,#65324));
#26959=EDGE_LOOP('',(#65325,#65326,#65327,#65328));
#26960=EDGE_LOOP('',(#65329,#65330,#65331,#65332));
#26961=EDGE_LOOP('',(#65333,#65334,#65335,#65336));
#26962=EDGE_LOOP('',(#65337,#65338,#65339,#65340));
#26963=EDGE_LOOP('',(#65341,#65342,#65343,#65344));
#26964=EDGE_LOOP('',(#65345,#65346,#65347,#65348));
#26965=EDGE_LOOP('',(#65349,#65350,#65351,#65352));
#26966=EDGE_LOOP('',(#65353,#65354,#65355,#65356));
#26967=EDGE_LOOP('',(#65357,#65358,#65359,#65360));
#26968=EDGE_LOOP('',(#65361,#65362,#65363,#65364));
#26969=EDGE_LOOP('',(#65365,#65366,#65367,#65368));
#26970=EDGE_LOOP('',(#65369,#65370,#65371,#65372));
#26971=EDGE_LOOP('',(#65373,#65374,#65375,#65376));
#26972=EDGE_LOOP('',(#65377,#65378,#65379,#65380));
#26973=EDGE_LOOP('',(#65381,#65382,#65383,#65384));
#26974=EDGE_LOOP('',(#65385,#65386,#65387,#65388));
#26975=EDGE_LOOP('',(#65389,#65390,#65391,#65392));
#26976=EDGE_LOOP('',(#65393,#65394,#65395,#65396));
#26977=EDGE_LOOP('',(#65397,#65398,#65399,#65400));
#26978=EDGE_LOOP('',(#65401,#65402,#65403,#65404));
#26979=EDGE_LOOP('',(#65405,#65406,#65407,#65408));
#26980=EDGE_LOOP('',(#65409,#65410,#65411,#65412));
#26981=EDGE_LOOP('',(#65413,#65414,#65415,#65416));
#26982=EDGE_LOOP('',(#65417,#65418,#65419,#65420));
#26983=EDGE_LOOP('',(#65421,#65422,#65423,#65424));
#26984=EDGE_LOOP('',(#65425,#65426,#65427,#65428));
#26985=EDGE_LOOP('',(#65429,#65430,#65431,#65432));
#26986=EDGE_LOOP('',(#65433,#65434,#65435,#65436));
#26987=EDGE_LOOP('',(#65437,#65438,#65439,#65440));
#26988=EDGE_LOOP('',(#65441,#65442,#65443,#65444));
#26989=EDGE_LOOP('',(#65445,#65446,#65447,#65448));
#26990=EDGE_LOOP('',(#65449,#65450,#65451,#65452));
#26991=EDGE_LOOP('',(#65453,#65454,#65455,#65456));
#26992=EDGE_LOOP('',(#65457,#65458,#65459,#65460));
#26993=EDGE_LOOP('',(#65461,#65462,#65463,#65464));
#26994=EDGE_LOOP('',(#65465,#65466,#65467,#65468));
#26995=EDGE_LOOP('',(#65469,#65470,#65471,#65472));
#26996=EDGE_LOOP('',(#65473,#65474,#65475,#65476));
#26997=EDGE_LOOP('',(#65477,#65478,#65479,#65480));
#26998=EDGE_LOOP('',(#65481,#65482,#65483,#65484));
#26999=EDGE_LOOP('',(#65485,#65486,#65487,#65488));
#27000=EDGE_LOOP('',(#65489,#65490,#65491,#65492));
#27001=EDGE_LOOP('',(#65493,#65494,#65495,#65496));
#27002=EDGE_LOOP('',(#65497,#65498,#65499,#65500));
#27003=EDGE_LOOP('',(#65501,#65502,#65503,#65504));
#27004=EDGE_LOOP('',(#65505,#65506,#65507,#65508));
#27005=EDGE_LOOP('',(#65509,#65510,#65511,#65512));
#27006=EDGE_LOOP('',(#65513,#65514,#65515,#65516));
#27007=EDGE_LOOP('',(#65517,#65518,#65519,#65520));
#27008=EDGE_LOOP('',(#65521,#65522,#65523,#65524));
#27009=EDGE_LOOP('',(#65525,#65526,#65527,#65528));
#27010=EDGE_LOOP('',(#65529,#65530,#65531,#65532));
#27011=EDGE_LOOP('',(#65533,#65534,#65535,#65536));
#27012=EDGE_LOOP('',(#65537,#65538,#65539,#65540));
#27013=EDGE_LOOP('',(#65541,#65542,#65543,#65544));
#27014=EDGE_LOOP('',(#65545,#65546,#65547,#65548));
#27015=EDGE_LOOP('',(#65549,#65550,#65551,#65552));
#27016=EDGE_LOOP('',(#65553,#65554,#65555,#65556));
#27017=EDGE_LOOP('',(#65557,#65558,#65559,#65560));
#27018=EDGE_LOOP('',(#65561,#65562,#65563,#65564));
#27019=EDGE_LOOP('',(#65565,#65566,#65567,#65568));
#27020=EDGE_LOOP('',(#65569,#65570,#65571,#65572));
#27021=EDGE_LOOP('',(#65573,#65574,#65575,#65576));
#27022=EDGE_LOOP('',(#65577,#65578,#65579,#65580));
#27023=EDGE_LOOP('',(#65581,#65582,#65583,#65584));
#27024=EDGE_LOOP('',(#65585,#65586,#65587,#65588));
#27025=EDGE_LOOP('',(#65589,#65590,#65591,#65592));
#27026=EDGE_LOOP('',(#65593,#65594,#65595,#65596));
#27027=EDGE_LOOP('',(#65597,#65598,#65599,#65600));
#27028=EDGE_LOOP('',(#65601,#65602,#65603,#65604));
#27029=EDGE_LOOP('',(#65605,#65606,#65607,#65608));
#27030=EDGE_LOOP('',(#65609,#65610,#65611,#65612));
#27031=EDGE_LOOP('',(#65613,#65614,#65615,#65616));
#27032=EDGE_LOOP('',(#65617,#65618,#65619,#65620));
#27033=EDGE_LOOP('',(#65621,#65622,#65623,#65624));
#27034=EDGE_LOOP('',(#65625,#65626,#65627,#65628));
#27035=EDGE_LOOP('',(#65629,#65630,#65631,#65632));
#27036=EDGE_LOOP('',(#65633,#65634,#65635,#65636));
#27037=EDGE_LOOP('',(#65637,#65638,#65639,#65640));
#27038=EDGE_LOOP('',(#65641,#65642,#65643,#65644));
#27039=EDGE_LOOP('',(#65645,#65646,#65647,#65648));
#27040=EDGE_LOOP('',(#65649,#65650,#65651,#65652));
#27041=EDGE_LOOP('',(#65653,#65654,#65655,#65656));
#27042=EDGE_LOOP('',(#65657,#65658,#65659,#65660));
#27043=EDGE_LOOP('',(#65661,#65662,#65663,#65664));
#27044=EDGE_LOOP('',(#65665,#65666,#65667,#65668));
#27045=EDGE_LOOP('',(#65669,#65670,#65671,#65672));
#27046=EDGE_LOOP('',(#65673,#65674,#65675,#65676));
#27047=EDGE_LOOP('',(#65677,#65678,#65679,#65680));
#27048=EDGE_LOOP('',(#65681,#65682,#65683,#65684));
#27049=EDGE_LOOP('',(#65685,#65686,#65687,#65688));
#27050=EDGE_LOOP('',(#65689,#65690,#65691,#65692));
#27051=EDGE_LOOP('',(#65693,#65694,#65695,#65696));
#27052=EDGE_LOOP('',(#65697,#65698,#65699,#65700));
#27053=EDGE_LOOP('',(#65701,#65702,#65703,#65704));
#27054=EDGE_LOOP('',(#65705,#65706,#65707,#65708));
#27055=EDGE_LOOP('',(#65709,#65710,#65711,#65712));
#27056=EDGE_LOOP('',(#65713,#65714,#65715,#65716));
#27057=EDGE_LOOP('',(#65717,#65718,#65719,#65720));
#27058=EDGE_LOOP('',(#65721,#65722,#65723,#65724));
#27059=EDGE_LOOP('',(#65725,#65726,#65727,#65728));
#27060=EDGE_LOOP('',(#65729,#65730,#65731,#65732));
#27061=EDGE_LOOP('',(#65733,#65734,#65735,#65736));
#27062=EDGE_LOOP('',(#65737,#65738,#65739,#65740));
#27063=EDGE_LOOP('',(#65741,#65742,#65743,#65744));
#27064=EDGE_LOOP('',(#65745,#65746,#65747,#65748));
#27065=EDGE_LOOP('',(#65749,#65750,#65751,#65752));
#27066=EDGE_LOOP('',(#65753,#65754,#65755,#65756));
#27067=EDGE_LOOP('',(#65757,#65758,#65759,#65760));
#27068=EDGE_LOOP('',(#65761,#65762,#65763,#65764));
#27069=EDGE_LOOP('',(#65765,#65766,#65767,#65768));
#27070=EDGE_LOOP('',(#65769,#65770,#65771,#65772));
#27071=EDGE_LOOP('',(#65773,#65774,#65775,#65776));
#27072=EDGE_LOOP('',(#65777,#65778,#65779,#65780));
#27073=EDGE_LOOP('',(#65781,#65782,#65783,#65784));
#27074=EDGE_LOOP('',(#65785,#65786,#65787,#65788));
#27075=EDGE_LOOP('',(#65789,#65790,#65791,#65792));
#27076=EDGE_LOOP('',(#65793,#65794,#65795,#65796));
#27077=EDGE_LOOP('',(#65797,#65798,#65799,#65800));
#27078=EDGE_LOOP('',(#65801,#65802,#65803,#65804));
#27079=EDGE_LOOP('',(#65805,#65806,#65807,#65808));
#27080=EDGE_LOOP('',(#65809,#65810,#65811,#65812));
#27081=EDGE_LOOP('',(#65813,#65814,#65815,#65816));
#27082=EDGE_LOOP('',(#65817,#65818,#65819,#65820));
#27083=EDGE_LOOP('',(#65821,#65822,#65823,#65824));
#27084=EDGE_LOOP('',(#65825,#65826,#65827,#65828));
#27085=EDGE_LOOP('',(#65829,#65830,#65831,#65832));
#27086=EDGE_LOOP('',(#65833,#65834,#65835,#65836));
#27087=EDGE_LOOP('',(#65837,#65838,#65839,#65840));
#27088=EDGE_LOOP('',(#65841,#65842,#65843,#65844));
#27089=EDGE_LOOP('',(#65845,#65846,#65847,#65848));
#27090=EDGE_LOOP('',(#65849,#65850,#65851,#65852));
#27091=EDGE_LOOP('',(#65853,#65854,#65855,#65856));
#27092=EDGE_LOOP('',(#65857,#65858,#65859,#65860));
#27093=EDGE_LOOP('',(#65861,#65862,#65863,#65864));
#27094=EDGE_LOOP('',(#65865,#65866,#65867,#65868));
#27095=EDGE_LOOP('',(#65869,#65870,#65871,#65872));
#27096=EDGE_LOOP('',(#65873,#65874,#65875,#65876));
#27097=EDGE_LOOP('',(#65877,#65878,#65879,#65880));
#27098=EDGE_LOOP('',(#65881,#65882,#65883,#65884));
#27099=EDGE_LOOP('',(#65885,#65886,#65887,#65888));
#27100=EDGE_LOOP('',(#65889,#65890,#65891,#65892));
#27101=EDGE_LOOP('',(#65893,#65894,#65895,#65896));
#27102=EDGE_LOOP('',(#65897,#65898,#65899,#65900));
#27103=EDGE_LOOP('',(#65901,#65902,#65903,#65904));
#27104=EDGE_LOOP('',(#65905,#65906,#65907,#65908));
#27105=EDGE_LOOP('',(#65909,#65910,#65911,#65912));
#27106=EDGE_LOOP('',(#65913,#65914,#65915,#65916));
#27107=EDGE_LOOP('',(#65917,#65918,#65919,#65920));
#27108=EDGE_LOOP('',(#65921,#65922,#65923,#65924));
#27109=EDGE_LOOP('',(#65925,#65926,#65927,#65928));
#27110=EDGE_LOOP('',(#65929,#65930,#65931,#65932));
#27111=EDGE_LOOP('',(#65933,#65934,#65935,#65936));
#27112=EDGE_LOOP('',(#65937,#65938,#65939,#65940));
#27113=EDGE_LOOP('',(#65941,#65942,#65943,#65944));
#27114=EDGE_LOOP('',(#65945,#65946,#65947,#65948));
#27115=EDGE_LOOP('',(#65949,#65950,#65951,#65952));
#27116=EDGE_LOOP('',(#65953,#65954,#65955,#65956));
#27117=EDGE_LOOP('',(#65957,#65958,#65959,#65960));
#27118=EDGE_LOOP('',(#65961,#65962,#65963,#65964));
#27119=EDGE_LOOP('',(#65965,#65966,#65967,#65968));
#27120=EDGE_LOOP('',(#65969,#65970,#65971,#65972));
#27121=EDGE_LOOP('',(#65973,#65974,#65975,#65976));
#27122=EDGE_LOOP('',(#65977,#65978,#65979,#65980));
#27123=EDGE_LOOP('',(#65981,#65982,#65983,#65984));
#27124=EDGE_LOOP('',(#65985,#65986,#65987,#65988));
#27125=EDGE_LOOP('',(#65989,#65990,#65991,#65992));
#27126=EDGE_LOOP('',(#65993,#65994,#65995,#65996));
#27127=EDGE_LOOP('',(#65997,#65998,#65999,#66000));
#27128=EDGE_LOOP('',(#66001,#66002,#66003,#66004));
#27129=EDGE_LOOP('',(#66005,#66006,#66007,#66008));
#27130=EDGE_LOOP('',(#66009,#66010,#66011,#66012));
#27131=EDGE_LOOP('',(#66013,#66014,#66015,#66016));
#27132=EDGE_LOOP('',(#66017,#66018,#66019,#66020));
#27133=EDGE_LOOP('',(#66021,#66022,#66023,#66024));
#27134=EDGE_LOOP('',(#66025,#66026,#66027,#66028));
#27135=EDGE_LOOP('',(#66029,#66030,#66031,#66032));
#27136=EDGE_LOOP('',(#66033,#66034,#66035,#66036));
#27137=EDGE_LOOP('',(#66037,#66038,#66039,#66040));
#27138=EDGE_LOOP('',(#66041,#66042,#66043,#66044));
#27139=EDGE_LOOP('',(#66045,#66046,#66047,#66048));
#27140=EDGE_LOOP('',(#66049,#66050,#66051,#66052));
#27141=EDGE_LOOP('',(#66053,#66054,#66055,#66056));
#27142=EDGE_LOOP('',(#66057,#66058,#66059,#66060));
#27143=EDGE_LOOP('',(#66061,#66062,#66063,#66064));
#27144=EDGE_LOOP('',(#66065,#66066,#66067,#66068));
#27145=EDGE_LOOP('',(#66069,#66070,#66071,#66072));
#27146=EDGE_LOOP('',(#66073,#66074,#66075,#66076));
#27147=EDGE_LOOP('',(#66077,#66078,#66079,#66080));
#27148=EDGE_LOOP('',(#66081,#66082,#66083,#66084));
#27149=EDGE_LOOP('',(#66085,#66086,#66087,#66088));
#27150=EDGE_LOOP('',(#66089,#66090,#66091,#66092));
#27151=EDGE_LOOP('',(#66093,#66094,#66095,#66096));
#27152=EDGE_LOOP('',(#66097,#66098,#66099,#66100));
#27153=EDGE_LOOP('',(#66101,#66102,#66103,#66104));
#27154=EDGE_LOOP('',(#66105,#66106,#66107,#66108));
#27155=EDGE_LOOP('',(#66109,#66110,#66111,#66112));
#27156=EDGE_LOOP('',(#66113,#66114,#66115,#66116));
#27157=EDGE_LOOP('',(#66117,#66118,#66119,#66120));
#27158=EDGE_LOOP('',(#66121,#66122,#66123,#66124));
#27159=EDGE_LOOP('',(#66125,#66126,#66127,#66128));
#27160=EDGE_LOOP('',(#66129,#66130,#66131,#66132));
#27161=EDGE_LOOP('',(#66133,#66134,#66135,#66136));
#27162=EDGE_LOOP('',(#66137,#66138,#66139,#66140));
#27163=EDGE_LOOP('',(#66141,#66142,#66143,#66144));
#27164=EDGE_LOOP('',(#66145,#66146,#66147,#66148));
#27165=EDGE_LOOP('',(#66149,#66150,#66151,#66152));
#27166=EDGE_LOOP('',(#66153,#66154,#66155,#66156));
#27167=EDGE_LOOP('',(#66157,#66158,#66159,#66160));
#27168=EDGE_LOOP('',(#66161,#66162,#66163,#66164));
#27169=EDGE_LOOP('',(#66165,#66166,#66167,#66168));
#27170=EDGE_LOOP('',(#66169,#66170,#66171,#66172));
#27171=EDGE_LOOP('',(#66173,#66174,#66175,#66176));
#27172=EDGE_LOOP('',(#66177,#66178,#66179,#66180));
#27173=EDGE_LOOP('',(#66181,#66182,#66183,#66184));
#27174=EDGE_LOOP('',(#66185,#66186,#66187,#66188));
#27175=EDGE_LOOP('',(#66189,#66190,#66191,#66192));
#27176=EDGE_LOOP('',(#66193,#66194,#66195,#66196));
#27177=EDGE_LOOP('',(#66197,#66198,#66199,#66200));
#27178=EDGE_LOOP('',(#66201,#66202,#66203,#66204));
#27179=EDGE_LOOP('',(#66205,#66206,#66207,#66208));
#27180=EDGE_LOOP('',(#66209,#66210,#66211,#66212));
#27181=EDGE_LOOP('',(#66213,#66214,#66215,#66216));
#27182=EDGE_LOOP('',(#66217,#66218,#66219,#66220));
#27183=EDGE_LOOP('',(#66221,#66222,#66223,#66224));
#27184=EDGE_LOOP('',(#66225,#66226,#66227,#66228));
#27185=EDGE_LOOP('',(#66229,#66230,#66231,#66232));
#27186=EDGE_LOOP('',(#66233,#66234,#66235,#66236));
#27187=EDGE_LOOP('',(#66237,#66238,#66239,#66240));
#27188=EDGE_LOOP('',(#66241,#66242,#66243,#66244));
#27189=EDGE_LOOP('',(#66245,#66246,#66247,#66248));
#27190=EDGE_LOOP('',(#66249,#66250,#66251,#66252));
#27191=EDGE_LOOP('',(#66253,#66254,#66255,#66256));
#27192=EDGE_LOOP('',(#66257,#66258,#66259,#66260));
#27193=EDGE_LOOP('',(#66261,#66262,#66263,#66264));
#27194=EDGE_LOOP('',(#66265,#66266,#66267,#66268));
#27195=EDGE_LOOP('',(#66269,#66270,#66271,#66272));
#27196=EDGE_LOOP('',(#66273,#66274,#66275,#66276));
#27197=EDGE_LOOP('',(#66277,#66278,#66279,#66280));
#27198=EDGE_LOOP('',(#66281,#66282,#66283,#66284));
#27199=EDGE_LOOP('',(#66285,#66286,#66287,#66288));
#27200=EDGE_LOOP('',(#66289,#66290,#66291,#66292));
#27201=EDGE_LOOP('',(#66293,#66294,#66295,#66296));
#27202=EDGE_LOOP('',(#66297,#66298,#66299,#66300));
#27203=EDGE_LOOP('',(#66301,#66302,#66303,#66304));
#27204=EDGE_LOOP('',(#66305,#66306,#66307,#66308));
#27205=EDGE_LOOP('',(#66309,#66310,#66311,#66312));
#27206=EDGE_LOOP('',(#66313,#66314,#66315,#66316));
#27207=EDGE_LOOP('',(#66317,#66318,#66319,#66320));
#27208=EDGE_LOOP('',(#66321,#66322,#66323,#66324));
#27209=EDGE_LOOP('',(#66325,#66326,#66327,#66328));
#27210=EDGE_LOOP('',(#66329,#66330,#66331,#66332));
#27211=EDGE_LOOP('',(#66333,#66334,#66335,#66336));
#27212=EDGE_LOOP('',(#66337,#66338,#66339,#66340));
#27213=EDGE_LOOP('',(#66341,#66342,#66343,#66344));
#27214=EDGE_LOOP('',(#66345,#66346,#66347,#66348));
#27215=EDGE_LOOP('',(#66349,#66350,#66351,#66352));
#27216=EDGE_LOOP('',(#66353,#66354,#66355,#66356));
#27217=EDGE_LOOP('',(#66357,#66358,#66359,#66360));
#27218=EDGE_LOOP('',(#66361,#66362,#66363,#66364));
#27219=EDGE_LOOP('',(#66365,#66366,#66367,#66368));
#27220=EDGE_LOOP('',(#66369,#66370,#66371,#66372));
#27221=EDGE_LOOP('',(#66373,#66374,#66375,#66376));
#27222=EDGE_LOOP('',(#66377,#66378,#66379,#66380));
#27223=EDGE_LOOP('',(#66381,#66382,#66383,#66384));
#27224=EDGE_LOOP('',(#66385,#66386,#66387,#66388));
#27225=EDGE_LOOP('',(#66389,#66390,#66391,#66392));
#27226=EDGE_LOOP('',(#66393,#66394,#66395,#66396));
#27227=EDGE_LOOP('',(#66397,#66398,#66399,#66400));
#27228=EDGE_LOOP('',(#66401,#66402,#66403,#66404));
#27229=EDGE_LOOP('',(#66405,#66406,#66407,#66408));
#27230=EDGE_LOOP('',(#66409,#66410,#66411,#66412));
#27231=EDGE_LOOP('',(#66413,#66414,#66415,#66416));
#27232=EDGE_LOOP('',(#66417,#66418,#66419,#66420));
#27233=EDGE_LOOP('',(#66421,#66422,#66423,#66424));
#27234=EDGE_LOOP('',(#66425,#66426,#66427,#66428));
#27235=EDGE_LOOP('',(#66429,#66430,#66431,#66432));
#27236=EDGE_LOOP('',(#66433,#66434,#66435,#66436));
#27237=EDGE_LOOP('',(#66437,#66438,#66439,#66440));
#27238=EDGE_LOOP('',(#66441,#66442,#66443,#66444));
#27239=EDGE_LOOP('',(#66445,#66446,#66447,#66448));
#27240=EDGE_LOOP('',(#66449,#66450,#66451,#66452));
#27241=EDGE_LOOP('',(#66453,#66454,#66455,#66456));
#27242=EDGE_LOOP('',(#66457,#66458,#66459,#66460));
#27243=EDGE_LOOP('',(#66461,#66462,#66463,#66464));
#27244=EDGE_LOOP('',(#66465,#66466,#66467,#66468));
#27245=EDGE_LOOP('',(#66469,#66470,#66471,#66472));
#27246=EDGE_LOOP('',(#66473,#66474,#66475,#66476));
#27247=EDGE_LOOP('',(#66477,#66478,#66479,#66480));
#27248=EDGE_LOOP('',(#66481,#66482,#66483,#66484));
#27249=EDGE_LOOP('',(#66485,#66486,#66487,#66488));
#27250=EDGE_LOOP('',(#66489,#66490,#66491,#66492));
#27251=EDGE_LOOP('',(#66493,#66494,#66495,#66496));
#27252=EDGE_LOOP('',(#66497,#66498,#66499,#66500));
#27253=EDGE_LOOP('',(#66501,#66502,#66503,#66504));
#27254=EDGE_LOOP('',(#66505,#66506,#66507,#66508));
#27255=EDGE_LOOP('',(#66509,#66510,#66511,#66512));
#27256=EDGE_LOOP('',(#66513,#66514,#66515,#66516));
#27257=EDGE_LOOP('',(#66517,#66518,#66519,#66520));
#27258=EDGE_LOOP('',(#66521,#66522,#66523,#66524));
#27259=EDGE_LOOP('',(#66525,#66526,#66527,#66528));
#27260=EDGE_LOOP('',(#66529,#66530,#66531,#66532));
#27261=EDGE_LOOP('',(#66533,#66534,#66535,#66536));
#27262=EDGE_LOOP('',(#66537,#66538,#66539,#66540));
#27263=EDGE_LOOP('',(#66541,#66542,#66543,#66544));
#27264=EDGE_LOOP('',(#66545,#66546,#66547,#66548));
#27265=EDGE_LOOP('',(#66549,#66550,#66551,#66552));
#27266=EDGE_LOOP('',(#66553,#66554,#66555,#66556));
#27267=EDGE_LOOP('',(#66557,#66558,#66559,#66560));
#27268=EDGE_LOOP('',(#66561,#66562,#66563,#66564));
#27269=EDGE_LOOP('',(#66565,#66566,#66567,#66568));
#27270=EDGE_LOOP('',(#66569,#66570,#66571,#66572));
#27271=EDGE_LOOP('',(#66573,#66574,#66575,#66576));
#27272=EDGE_LOOP('',(#66577,#66578,#66579,#66580));
#27273=EDGE_LOOP('',(#66581,#66582,#66583,#66584));
#27274=EDGE_LOOP('',(#66585,#66586,#66587,#66588));
#27275=EDGE_LOOP('',(#66589,#66590,#66591,#66592));
#27276=EDGE_LOOP('',(#66593,#66594,#66595,#66596));
#27277=EDGE_LOOP('',(#66597,#66598,#66599,#66600));
#27278=EDGE_LOOP('',(#66601,#66602,#66603,#66604));
#27279=EDGE_LOOP('',(#66605,#66606,#66607,#66608));
#27280=EDGE_LOOP('',(#66609,#66610,#66611,#66612));
#27281=EDGE_LOOP('',(#66613,#66614,#66615,#66616));
#27282=EDGE_LOOP('',(#66617,#66618,#66619,#66620));
#27283=EDGE_LOOP('',(#66621,#66622,#66623,#66624));
#27284=EDGE_LOOP('',(#66625,#66626,#66627,#66628));
#27285=EDGE_LOOP('',(#66629,#66630,#66631,#66632));
#27286=EDGE_LOOP('',(#66633,#66634,#66635,#66636));
#27287=EDGE_LOOP('',(#66637,#66638,#66639,#66640));
#27288=EDGE_LOOP('',(#66641,#66642,#66643,#66644));
#27289=EDGE_LOOP('',(#66645,#66646,#66647,#66648));
#27290=EDGE_LOOP('',(#66649,#66650,#66651,#66652));
#27291=EDGE_LOOP('',(#66653,#66654,#66655,#66656));
#27292=EDGE_LOOP('',(#66657,#66658,#66659,#66660));
#27293=EDGE_LOOP('',(#66661,#66662,#66663,#66664));
#27294=EDGE_LOOP('',(#66665,#66666,#66667,#66668));
#27295=EDGE_LOOP('',(#66669,#66670,#66671,#66672));
#27296=EDGE_LOOP('',(#66673,#66674,#66675,#66676));
#27297=EDGE_LOOP('',(#66677,#66678,#66679,#66680));
#27298=EDGE_LOOP('',(#66681,#66682,#66683,#66684));
#27299=EDGE_LOOP('',(#66685,#66686,#66687,#66688));
#27300=EDGE_LOOP('',(#66689,#66690,#66691,#66692));
#27301=EDGE_LOOP('',(#66693,#66694,#66695,#66696));
#27302=EDGE_LOOP('',(#66697,#66698,#66699,#66700));
#27303=EDGE_LOOP('',(#66701,#66702,#66703,#66704));
#27304=EDGE_LOOP('',(#66705,#66706,#66707,#66708));
#27305=EDGE_LOOP('',(#66709,#66710,#66711,#66712));
#27306=EDGE_LOOP('',(#66713,#66714,#66715,#66716));
#27307=EDGE_LOOP('',(#66717,#66718,#66719,#66720));
#27308=EDGE_LOOP('',(#66721,#66722,#66723,#66724));
#27309=EDGE_LOOP('',(#66725,#66726,#66727,#66728));
#27310=EDGE_LOOP('',(#66729,#66730,#66731,#66732));
#27311=EDGE_LOOP('',(#66733,#66734,#66735,#66736));
#27312=EDGE_LOOP('',(#66737,#66738,#66739,#66740));
#27313=EDGE_LOOP('',(#66741,#66742,#66743,#66744));
#27314=EDGE_LOOP('',(#66745,#66746,#66747,#66748));
#27315=EDGE_LOOP('',(#66749,#66750,#66751,#66752));
#27316=EDGE_LOOP('',(#66753,#66754,#66755,#66756));
#27317=EDGE_LOOP('',(#66757,#66758,#66759,#66760));
#27318=EDGE_LOOP('',(#66761,#66762,#66763,#66764));
#27319=EDGE_LOOP('',(#66765,#66766,#66767,#66768));
#27320=EDGE_LOOP('',(#66769,#66770,#66771,#66772));
#27321=EDGE_LOOP('',(#66773,#66774,#66775,#66776));
#27322=EDGE_LOOP('',(#66777,#66778,#66779,#66780));
#27323=EDGE_LOOP('',(#66781,#66782,#66783,#66784));
#27324=EDGE_LOOP('',(#66785,#66786,#66787,#66788));
#27325=EDGE_LOOP('',(#66789,#66790,#66791,#66792));
#27326=EDGE_LOOP('',(#66793,#66794,#66795,#66796));
#27327=EDGE_LOOP('',(#66797,#66798,#66799,#66800));
#27328=EDGE_LOOP('',(#66801,#66802,#66803,#66804));
#27329=EDGE_LOOP('',(#66805,#66806,#66807,#66808));
#27330=EDGE_LOOP('',(#66809,#66810,#66811,#66812));
#27331=EDGE_LOOP('',(#66813,#66814,#66815,#66816));
#27332=EDGE_LOOP('',(#66817,#66818,#66819,#66820));
#27333=EDGE_LOOP('',(#66821,#66822,#66823,#66824));
#27334=EDGE_LOOP('',(#66825,#66826,#66827,#66828));
#27335=EDGE_LOOP('',(#66829,#66830,#66831,#66832));
#27336=EDGE_LOOP('',(#66833,#66834,#66835,#66836));
#27337=EDGE_LOOP('',(#66837,#66838,#66839,#66840));
#27338=EDGE_LOOP('',(#66841,#66842,#66843,#66844));
#27339=EDGE_LOOP('',(#66845,#66846,#66847,#66848));
#27340=EDGE_LOOP('',(#66849,#66850,#66851,#66852));
#27341=EDGE_LOOP('',(#66853,#66854,#66855,#66856));
#27342=EDGE_LOOP('',(#66857,#66858,#66859,#66860));
#27343=EDGE_LOOP('',(#66861,#66862,#66863,#66864));
#27344=EDGE_LOOP('',(#66865,#66866,#66867,#66868));
#27345=EDGE_LOOP('',(#66869,#66870,#66871,#66872));
#27346=EDGE_LOOP('',(#66873,#66874,#66875,#66876));
#27347=EDGE_LOOP('',(#66877,#66878,#66879,#66880));
#27348=EDGE_LOOP('',(#66881,#66882,#66883,#66884));
#27349=EDGE_LOOP('',(#66885,#66886,#66887,#66888));
#27350=EDGE_LOOP('',(#66889,#66890,#66891,#66892));
#27351=EDGE_LOOP('',(#66893,#66894,#66895,#66896));
#27352=EDGE_LOOP('',(#66897,#66898,#66899,#66900));
#27353=EDGE_LOOP('',(#66901,#66902,#66903,#66904));
#27354=EDGE_LOOP('',(#66905,#66906,#66907,#66908));
#27355=EDGE_LOOP('',(#66909,#66910,#66911,#66912));
#27356=EDGE_LOOP('',(#66913,#66914,#66915,#66916));
#27357=EDGE_LOOP('',(#66917,#66918,#66919,#66920));
#27358=EDGE_LOOP('',(#66921,#66922,#66923,#66924));
#27359=EDGE_LOOP('',(#66925,#66926,#66927,#66928));
#27360=EDGE_LOOP('',(#66929,#66930,#66931,#66932));
#27361=EDGE_LOOP('',(#66933,#66934,#66935,#66936));
#27362=EDGE_LOOP('',(#66937,#66938,#66939,#66940));
#27363=EDGE_LOOP('',(#66941,#66942,#66943,#66944));
#27364=EDGE_LOOP('',(#66945,#66946,#66947,#66948));
#27365=EDGE_LOOP('',(#66949,#66950,#66951,#66952));
#27366=EDGE_LOOP('',(#66953,#66954,#66955,#66956));
#27367=EDGE_LOOP('',(#66957,#66958,#66959,#66960));
#27368=EDGE_LOOP('',(#66961,#66962,#66963,#66964));
#27369=EDGE_LOOP('',(#66965,#66966,#66967,#66968));
#27370=EDGE_LOOP('',(#66969,#66970,#66971,#66972));
#27371=EDGE_LOOP('',(#66973,#66974,#66975,#66976));
#27372=EDGE_LOOP('',(#66977,#66978,#66979,#66980));
#27373=EDGE_LOOP('',(#66981,#66982,#66983,#66984));
#27374=EDGE_LOOP('',(#66985,#66986,#66987,#66988));
#27375=EDGE_LOOP('',(#66989,#66990,#66991,#66992));
#27376=EDGE_LOOP('',(#66993,#66994,#66995,#66996));
#27377=EDGE_LOOP('',(#66997,#66998,#66999,#67000));
#27378=EDGE_LOOP('',(#67001,#67002,#67003,#67004));
#27379=EDGE_LOOP('',(#67005,#67006,#67007,#67008));
#27380=EDGE_LOOP('',(#67009,#67010,#67011,#67012));
#27381=EDGE_LOOP('',(#67013,#67014,#67015,#67016));
#27382=EDGE_LOOP('',(#67017,#67018,#67019,#67020));
#27383=EDGE_LOOP('',(#67021,#67022,#67023,#67024));
#27384=EDGE_LOOP('',(#67025,#67026,#67027,#67028));
#27385=EDGE_LOOP('',(#67029,#67030,#67031,#67032));
#27386=EDGE_LOOP('',(#67033,#67034,#67035,#67036));
#27387=EDGE_LOOP('',(#67037,#67038,#67039,#67040));
#27388=EDGE_LOOP('',(#67041,#67042,#67043,#67044));
#27389=EDGE_LOOP('',(#67045,#67046,#67047,#67048));
#27390=EDGE_LOOP('',(#67049,#67050,#67051,#67052));
#27391=EDGE_LOOP('',(#67053,#67054,#67055,#67056));
#27392=EDGE_LOOP('',(#67057,#67058,#67059,#67060));
#27393=EDGE_LOOP('',(#67061,#67062,#67063,#67064));
#27394=EDGE_LOOP('',(#67065,#67066,#67067,#67068));
#27395=EDGE_LOOP('',(#67069,#67070,#67071,#67072));
#27396=EDGE_LOOP('',(#67073,#67074,#67075,#67076));
#27397=EDGE_LOOP('',(#67077,#67078,#67079,#67080));
#27398=EDGE_LOOP('',(#67081,#67082,#67083,#67084));
#27399=EDGE_LOOP('',(#67085,#67086,#67087,#67088));
#27400=EDGE_LOOP('',(#67089,#67090,#67091,#67092));
#27401=EDGE_LOOP('',(#67093,#67094,#67095,#67096));
#27402=EDGE_LOOP('',(#67097,#67098,#67099,#67100));
#27403=EDGE_LOOP('',(#67101,#67102,#67103,#67104));
#27404=EDGE_LOOP('',(#67105,#67106,#67107,#67108));
#27405=EDGE_LOOP('',(#67109,#67110,#67111,#67112));
#27406=EDGE_LOOP('',(#67113,#67114,#67115,#67116));
#27407=EDGE_LOOP('',(#67117,#67118,#67119,#67120));
#27408=EDGE_LOOP('',(#67121,#67122,#67123,#67124));
#27409=EDGE_LOOP('',(#67125,#67126,#67127,#67128));
#27410=EDGE_LOOP('',(#67129,#67130,#67131,#67132));
#27411=EDGE_LOOP('',(#67133,#67134,#67135,#67136));
#27412=EDGE_LOOP('',(#67137,#67138,#67139,#67140));
#27413=EDGE_LOOP('',(#67141,#67142,#67143,#67144));
#27414=EDGE_LOOP('',(#67145,#67146,#67147,#67148));
#27415=EDGE_LOOP('',(#67149,#67150,#67151,#67152));
#27416=EDGE_LOOP('',(#67153,#67154,#67155,#67156));
#27417=EDGE_LOOP('',(#67157,#67158,#67159,#67160));
#27418=EDGE_LOOP('',(#67161,#67162,#67163,#67164));
#27419=EDGE_LOOP('',(#67165,#67166,#67167,#67168));
#27420=EDGE_LOOP('',(#67169,#67170,#67171,#67172));
#27421=EDGE_LOOP('',(#67173,#67174,#67175,#67176));
#27422=EDGE_LOOP('',(#67177,#67178,#67179,#67180));
#27423=EDGE_LOOP('',(#67181,#67182,#67183,#67184));
#27424=EDGE_LOOP('',(#67185,#67186,#67187,#67188));
#27425=EDGE_LOOP('',(#67189,#67190,#67191,#67192));
#27426=EDGE_LOOP('',(#67193,#67194,#67195,#67196));
#27427=EDGE_LOOP('',(#67197,#67198,#67199,#67200));
#27428=EDGE_LOOP('',(#67201,#67202,#67203,#67204));
#27429=EDGE_LOOP('',(#67205,#67206,#67207,#67208));
#27430=EDGE_LOOP('',(#67209,#67210,#67211,#67212));
#27431=EDGE_LOOP('',(#67213,#67214,#67215,#67216));
#27432=EDGE_LOOP('',(#67217,#67218,#67219,#67220));
#27433=EDGE_LOOP('',(#67221,#67222,#67223,#67224));
#27434=EDGE_LOOP('',(#67225,#67226,#67227,#67228));
#27435=EDGE_LOOP('',(#67229,#67230,#67231,#67232));
#27436=EDGE_LOOP('',(#67233,#67234,#67235,#67236));
#27437=EDGE_LOOP('',(#67237,#67238,#67239,#67240));
#27438=EDGE_LOOP('',(#67241,#67242,#67243,#67244));
#27439=EDGE_LOOP('',(#67245,#67246,#67247,#67248));
#27440=EDGE_LOOP('',(#67249,#67250,#67251,#67252));
#27441=EDGE_LOOP('',(#67253,#67254,#67255,#67256));
#27442=EDGE_LOOP('',(#67257,#67258,#67259,#67260));
#27443=EDGE_LOOP('',(#67261,#67262,#67263,#67264));
#27444=EDGE_LOOP('',(#67265,#67266,#67267,#67268));
#27445=EDGE_LOOP('',(#67269,#67270,#67271,#67272));
#27446=EDGE_LOOP('',(#67273,#67274,#67275,#67276));
#27447=EDGE_LOOP('',(#67277,#67278,#67279,#67280));
#27448=EDGE_LOOP('',(#67281,#67282,#67283,#67284));
#27449=EDGE_LOOP('',(#67285,#67286,#67287,#67288));
#27450=EDGE_LOOP('',(#67289,#67290,#67291,#67292));
#27451=EDGE_LOOP('',(#67293,#67294,#67295,#67296));
#27452=EDGE_LOOP('',(#67297,#67298,#67299,#67300));
#27453=EDGE_LOOP('',(#67301,#67302,#67303,#67304));
#27454=EDGE_LOOP('',(#67305,#67306,#67307,#67308));
#27455=EDGE_LOOP('',(#67309,#67310,#67311,#67312));
#27456=EDGE_LOOP('',(#67313,#67314,#67315,#67316));
#27457=EDGE_LOOP('',(#67317,#67318,#67319,#67320));
#27458=EDGE_LOOP('',(#67321,#67322,#67323,#67324));
#27459=EDGE_LOOP('',(#67325,#67326,#67327,#67328));
#27460=EDGE_LOOP('',(#67329,#67330,#67331,#67332));
#27461=EDGE_LOOP('',(#67333,#67334,#67335,#67336));
#27462=EDGE_LOOP('',(#67337,#67338,#67339,#67340));
#27463=EDGE_LOOP('',(#67341,#67342,#67343,#67344));
#27464=EDGE_LOOP('',(#67345,#67346,#67347,#67348));
#27465=EDGE_LOOP('',(#67349,#67350,#67351,#67352));
#27466=EDGE_LOOP('',(#67353,#67354,#67355,#67356));
#27467=EDGE_LOOP('',(#67357,#67358,#67359,#67360));
#27468=EDGE_LOOP('',(#67361,#67362,#67363,#67364));
#27469=EDGE_LOOP('',(#67365,#67366,#67367,#67368));
#27470=EDGE_LOOP('',(#67369,#67370,#67371,#67372));
#27471=EDGE_LOOP('',(#67373,#67374,#67375,#67376));
#27472=EDGE_LOOP('',(#67377,#67378,#67379,#67380));
#27473=EDGE_LOOP('',(#67381,#67382,#67383,#67384));
#27474=EDGE_LOOP('',(#67385,#67386,#67387,#67388));
#27475=EDGE_LOOP('',(#67389,#67390,#67391,#67392));
#27476=EDGE_LOOP('',(#67393,#67394,#67395,#67396));
#27477=EDGE_LOOP('',(#67397,#67398,#67399,#67400));
#27478=EDGE_LOOP('',(#67401,#67402,#67403,#67404));
#27479=EDGE_LOOP('',(#67405,#67406,#67407,#67408));
#27480=EDGE_LOOP('',(#67409,#67410,#67411,#67412));
#27481=EDGE_LOOP('',(#67413,#67414,#67415,#67416));
#27482=EDGE_LOOP('',(#67417,#67418,#67419,#67420));
#27483=EDGE_LOOP('',(#67421,#67422,#67423,#67424));
#27484=EDGE_LOOP('',(#67425,#67426,#67427,#67428));
#27485=EDGE_LOOP('',(#67429,#67430,#67431,#67432));
#27486=EDGE_LOOP('',(#67433,#67434,#67435,#67436));
#27487=EDGE_LOOP('',(#67437,#67438,#67439,#67440));
#27488=EDGE_LOOP('',(#67441,#67442,#67443,#67444));
#27489=EDGE_LOOP('',(#67445,#67446,#67447,#67448));
#27490=EDGE_LOOP('',(#67449,#67450,#67451,#67452));
#27491=EDGE_LOOP('',(#67453,#67454,#67455,#67456));
#27492=EDGE_LOOP('',(#67457,#67458,#67459,#67460));
#27493=EDGE_LOOP('',(#67461,#67462,#67463,#67464));
#27494=EDGE_LOOP('',(#67465,#67466,#67467,#67468));
#27495=EDGE_LOOP('',(#67469,#67470,#67471,#67472));
#27496=EDGE_LOOP('',(#67473,#67474,#67475,#67476));
#27497=EDGE_LOOP('',(#67477,#67478,#67479,#67480));
#27498=EDGE_LOOP('',(#67481,#67482,#67483,#67484));
#27499=EDGE_LOOP('',(#67485,#67486,#67487,#67488));
#27500=EDGE_LOOP('',(#67489,#67490,#67491,#67492));
#27501=EDGE_LOOP('',(#67493,#67494,#67495,#67496));
#27502=EDGE_LOOP('',(#67497,#67498,#67499,#67500));
#27503=EDGE_LOOP('',(#67501,#67502,#67503,#67504));
#27504=EDGE_LOOP('',(#67505,#67506,#67507,#67508));
#27505=EDGE_LOOP('',(#67509,#67510,#67511,#67512));
#27506=EDGE_LOOP('',(#67513,#67514,#67515,#67516));
#27507=EDGE_LOOP('',(#67517,#67518,#67519,#67520));
#27508=EDGE_LOOP('',(#67521,#67522,#67523,#67524));
#27509=EDGE_LOOP('',(#67525,#67526,#67527,#67528));
#27510=EDGE_LOOP('',(#67529,#67530,#67531,#67532));
#27511=EDGE_LOOP('',(#67533,#67534,#67535,#67536));
#27512=EDGE_LOOP('',(#67537,#67538,#67539,#67540));
#27513=EDGE_LOOP('',(#67541,#67542,#67543,#67544));
#27514=EDGE_LOOP('',(#67545,#67546,#67547,#67548));
#27515=EDGE_LOOP('',(#67549,#67550,#67551,#67552));
#27516=EDGE_LOOP('',(#67553,#67554,#67555,#67556));
#27517=EDGE_LOOP('',(#67557,#67558,#67559,#67560));
#27518=EDGE_LOOP('',(#67561,#67562,#67563,#67564));
#27519=EDGE_LOOP('',(#67565,#67566,#67567,#67568));
#27520=EDGE_LOOP('',(#67569,#67570,#67571,#67572));
#27521=EDGE_LOOP('',(#67573,#67574,#67575,#67576));
#27522=EDGE_LOOP('',(#67577,#67578,#67579,#67580));
#27523=EDGE_LOOP('',(#67581,#67582,#67583,#67584));
#27524=EDGE_LOOP('',(#67585,#67586,#67587,#67588));
#27525=EDGE_LOOP('',(#67589,#67590,#67591,#67592));
#27526=EDGE_LOOP('',(#67593,#67594,#67595,#67596));
#27527=EDGE_LOOP('',(#67597,#67598,#67599,#67600));
#27528=EDGE_LOOP('',(#67601,#67602,#67603,#67604));
#27529=EDGE_LOOP('',(#67605,#67606,#67607,#67608));
#27530=EDGE_LOOP('',(#67609,#67610,#67611,#67612));
#27531=EDGE_LOOP('',(#67613,#67614,#67615,#67616));
#27532=EDGE_LOOP('',(#67617,#67618,#67619,#67620));
#27533=EDGE_LOOP('',(#67621,#67622,#67623,#67624));
#27534=EDGE_LOOP('',(#67625,#67626,#67627,#67628));
#27535=EDGE_LOOP('',(#67629,#67630,#67631,#67632));
#27536=EDGE_LOOP('',(#67633,#67634,#67635,#67636));
#27537=EDGE_LOOP('',(#67637,#67638,#67639,#67640));
#27538=EDGE_LOOP('',(#67641,#67642,#67643,#67644));
#27539=EDGE_LOOP('',(#67645,#67646,#67647,#67648));
#27540=EDGE_LOOP('',(#67649,#67650,#67651,#67652));
#27541=EDGE_LOOP('',(#67653,#67654,#67655,#67656));
#27542=EDGE_LOOP('',(#67657,#67658,#67659,#67660));
#27543=EDGE_LOOP('',(#67661,#67662,#67663,#67664));
#27544=EDGE_LOOP('',(#67665,#67666,#67667,#67668));
#27545=EDGE_LOOP('',(#67669,#67670,#67671,#67672));
#27546=EDGE_LOOP('',(#67673,#67674,#67675,#67676));
#27547=EDGE_LOOP('',(#67677,#67678,#67679,#67680));
#27548=EDGE_LOOP('',(#67681,#67682,#67683,#67684));
#27549=EDGE_LOOP('',(#67685,#67686,#67687,#67688));
#27550=EDGE_LOOP('',(#67689,#67690,#67691,#67692));
#27551=EDGE_LOOP('',(#67693,#67694,#67695,#67696));
#27552=EDGE_LOOP('',(#67697,#67698,#67699,#67700));
#27553=EDGE_LOOP('',(#67701,#67702,#67703,#67704));
#27554=EDGE_LOOP('',(#67705,#67706,#67707,#67708));
#27555=EDGE_LOOP('',(#67709,#67710,#67711,#67712));
#27556=EDGE_LOOP('',(#67713,#67714,#67715,#67716));
#27557=EDGE_LOOP('',(#67717,#67718,#67719,#67720));
#27558=EDGE_LOOP('',(#67721,#67722,#67723,#67724));
#27559=EDGE_LOOP('',(#67725,#67726,#67727,#67728));
#27560=EDGE_LOOP('',(#67729,#67730,#67731,#67732));
#27561=EDGE_LOOP('',(#67733,#67734,#67735,#67736));
#27562=EDGE_LOOP('',(#67737,#67738,#67739,#67740));
#27563=EDGE_LOOP('',(#67741,#67742,#67743,#67744));
#27564=EDGE_LOOP('',(#67745,#67746,#67747,#67748));
#27565=EDGE_LOOP('',(#67749,#67750,#67751,#67752));
#27566=EDGE_LOOP('',(#67753,#67754,#67755,#67756));
#27567=EDGE_LOOP('',(#67757,#67758,#67759,#67760));
#27568=EDGE_LOOP('',(#67761,#67762,#67763,#67764));
#27569=EDGE_LOOP('',(#67765,#67766,#67767,#67768));
#27570=EDGE_LOOP('',(#67769,#67770,#67771,#67772));
#27571=EDGE_LOOP('',(#67773,#67774,#67775,#67776));
#27572=EDGE_LOOP('',(#67777,#67778,#67779,#67780));
#27573=EDGE_LOOP('',(#67781,#67782,#67783,#67784));
#27574=EDGE_LOOP('',(#67785,#67786,#67787,#67788));
#27575=EDGE_LOOP('',(#67789,#67790,#67791,#67792));
#27576=EDGE_LOOP('',(#67793,#67794,#67795,#67796));
#27577=EDGE_LOOP('',(#67797,#67798,#67799,#67800));
#27578=EDGE_LOOP('',(#67801,#67802,#67803,#67804));
#27579=EDGE_LOOP('',(#67805,#67806,#67807,#67808));
#27580=EDGE_LOOP('',(#67809,#67810,#67811,#67812));
#27581=EDGE_LOOP('',(#67813,#67814,#67815,#67816));
#27582=EDGE_LOOP('',(#67817,#67818,#67819,#67820));
#27583=EDGE_LOOP('',(#67821,#67822,#67823,#67824));
#27584=EDGE_LOOP('',(#67825,#67826,#67827,#67828));
#27585=EDGE_LOOP('',(#67829,#67830,#67831,#67832));
#27586=EDGE_LOOP('',(#67833,#67834,#67835,#67836));
#27587=EDGE_LOOP('',(#67837,#67838,#67839,#67840));
#27588=EDGE_LOOP('',(#67841,#67842,#67843,#67844));
#27589=EDGE_LOOP('',(#67845,#67846,#67847,#67848));
#27590=EDGE_LOOP('',(#67849,#67850,#67851,#67852));
#27591=EDGE_LOOP('',(#67853,#67854,#67855,#67856));
#27592=EDGE_LOOP('',(#67857,#67858,#67859,#67860));
#27593=EDGE_LOOP('',(#67861,#67862,#67863,#67864));
#27594=EDGE_LOOP('',(#67865,#67866,#67867,#67868));
#27595=EDGE_LOOP('',(#67869,#67870,#67871,#67872));
#27596=EDGE_LOOP('',(#67873,#67874,#67875,#67876));
#27597=EDGE_LOOP('',(#67877,#67878,#67879,#67880));
#27598=EDGE_LOOP('',(#67881,#67882,#67883,#67884));
#27599=EDGE_LOOP('',(#67885,#67886,#67887,#67888));
#27600=EDGE_LOOP('',(#67889,#67890,#67891,#67892));
#27601=EDGE_LOOP('',(#67893,#67894,#67895,#67896));
#27602=EDGE_LOOP('',(#67897,#67898,#67899,#67900));
#27603=EDGE_LOOP('',(#67901,#67902,#67903,#67904));
#27604=EDGE_LOOP('',(#67905,#67906,#67907,#67908));
#27605=EDGE_LOOP('',(#67909,#67910,#67911,#67912));
#27606=EDGE_LOOP('',(#67913,#67914,#67915,#67916));
#27607=EDGE_LOOP('',(#67917,#67918,#67919,#67920));
#27608=EDGE_LOOP('',(#67921,#67922,#67923,#67924));
#27609=EDGE_LOOP('',(#67925,#67926,#67927,#67928));
#27610=EDGE_LOOP('',(#67929,#67930,#67931,#67932));
#27611=EDGE_LOOP('',(#67933,#67934,#67935,#67936));
#27612=EDGE_LOOP('',(#67937,#67938,#67939,#67940));
#27613=EDGE_LOOP('',(#67941,#67942,#67943,#67944));
#27614=EDGE_LOOP('',(#67945,#67946,#67947,#67948));
#27615=EDGE_LOOP('',(#67949,#67950,#67951,#67952));
#27616=EDGE_LOOP('',(#67953,#67954,#67955,#67956));
#27617=EDGE_LOOP('',(#67957,#67958,#67959,#67960));
#27618=EDGE_LOOP('',(#67961,#67962,#67963,#67964));
#27619=EDGE_LOOP('',(#67965,#67966,#67967,#67968));
#27620=EDGE_LOOP('',(#67969,#67970,#67971,#67972));
#27621=EDGE_LOOP('',(#67973,#67974,#67975,#67976));
#27622=EDGE_LOOP('',(#67977,#67978,#67979,#67980));
#27623=EDGE_LOOP('',(#67981,#67982,#67983,#67984));
#27624=EDGE_LOOP('',(#67985,#67986,#67987,#67988));
#27625=EDGE_LOOP('',(#67989,#67990,#67991,#67992));
#27626=EDGE_LOOP('',(#67993,#67994,#67995,#67996));
#27627=EDGE_LOOP('',(#67997,#67998,#67999,#68000));
#27628=EDGE_LOOP('',(#68001,#68002,#68003,#68004));
#27629=EDGE_LOOP('',(#68005,#68006,#68007,#68008));
#27630=EDGE_LOOP('',(#68009,#68010,#68011,#68012));
#27631=EDGE_LOOP('',(#68013,#68014,#68015,#68016));
#27632=EDGE_LOOP('',(#68017,#68018,#68019,#68020));
#27633=EDGE_LOOP('',(#68021,#68022,#68023,#68024));
#27634=EDGE_LOOP('',(#68025,#68026,#68027,#68028));
#27635=EDGE_LOOP('',(#68029,#68030,#68031,#68032));
#27636=EDGE_LOOP('',(#68033,#68034,#68035,#68036));
#27637=EDGE_LOOP('',(#68037,#68038,#68039,#68040));
#27638=EDGE_LOOP('',(#68041,#68042,#68043,#68044));
#27639=EDGE_LOOP('',(#68045,#68046,#68047,#68048));
#27640=EDGE_LOOP('',(#68049,#68050,#68051,#68052));
#27641=EDGE_LOOP('',(#68053,#68054,#68055,#68056));
#27642=EDGE_LOOP('',(#68057,#68058,#68059,#68060));
#27643=EDGE_LOOP('',(#68061,#68062,#68063,#68064));
#27644=EDGE_LOOP('',(#68065,#68066,#68067,#68068));
#27645=EDGE_LOOP('',(#68069,#68070,#68071,#68072));
#27646=EDGE_LOOP('',(#68073,#68074,#68075,#68076));
#27647=EDGE_LOOP('',(#68077,#68078,#68079,#68080));
#27648=EDGE_LOOP('',(#68081,#68082,#68083,#68084));
#27649=EDGE_LOOP('',(#68085,#68086,#68087,#68088));
#27650=EDGE_LOOP('',(#68089,#68090,#68091,#68092));
#27651=EDGE_LOOP('',(#68093,#68094,#68095,#68096));
#27652=EDGE_LOOP('',(#68097,#68098,#68099,#68100));
#27653=EDGE_LOOP('',(#68101,#68102,#68103,#68104));
#27654=EDGE_LOOP('',(#68105,#68106,#68107,#68108));
#27655=EDGE_LOOP('',(#68109,#68110,#68111,#68112));
#27656=EDGE_LOOP('',(#68113,#68114,#68115,#68116));
#27657=EDGE_LOOP('',(#68117,#68118,#68119,#68120));
#27658=EDGE_LOOP('',(#68121,#68122,#68123,#68124));
#27659=EDGE_LOOP('',(#68125,#68126,#68127,#68128));
#27660=EDGE_LOOP('',(#68129,#68130,#68131,#68132));
#27661=EDGE_LOOP('',(#68133,#68134,#68135,#68136));
#27662=EDGE_LOOP('',(#68137,#68138,#68139,#68140));
#27663=EDGE_LOOP('',(#68141,#68142,#68143,#68144));
#27664=EDGE_LOOP('',(#68145,#68146,#68147,#68148));
#27665=EDGE_LOOP('',(#68149,#68150,#68151,#68152));
#27666=EDGE_LOOP('',(#68153,#68154,#68155,#68156));
#27667=EDGE_LOOP('',(#68157,#68158,#68159,#68160));
#27668=EDGE_LOOP('',(#68161,#68162,#68163,#68164));
#27669=EDGE_LOOP('',(#68165,#68166,#68167,#68168));
#27670=EDGE_LOOP('',(#68169,#68170,#68171,#68172));
#27671=EDGE_LOOP('',(#68173,#68174,#68175,#68176));
#27672=EDGE_LOOP('',(#68177,#68178,#68179,#68180));
#27673=EDGE_LOOP('',(#68181,#68182,#68183,#68184));
#27674=EDGE_LOOP('',(#68185,#68186,#68187,#68188));
#27675=EDGE_LOOP('',(#68189,#68190,#68191,#68192));
#27676=EDGE_LOOP('',(#68193,#68194,#68195,#68196));
#27677=EDGE_LOOP('',(#68197,#68198,#68199,#68200));
#27678=EDGE_LOOP('',(#68201,#68202,#68203,#68204));
#27679=EDGE_LOOP('',(#68205,#68206,#68207,#68208));
#27680=EDGE_LOOP('',(#68209,#68210,#68211,#68212));
#27681=EDGE_LOOP('',(#68213,#68214,#68215,#68216));
#27682=EDGE_LOOP('',(#68217,#68218,#68219,#68220));
#27683=EDGE_LOOP('',(#68221,#68222,#68223,#68224));
#27684=EDGE_LOOP('',(#68225,#68226,#68227,#68228));
#27685=EDGE_LOOP('',(#68229,#68230,#68231,#68232));
#27686=EDGE_LOOP('',(#68233,#68234,#68235,#68236));
#27687=EDGE_LOOP('',(#68237,#68238,#68239,#68240));
#27688=EDGE_LOOP('',(#68241,#68242,#68243,#68244));
#27689=EDGE_LOOP('',(#68245,#68246,#68247,#68248));
#27690=EDGE_LOOP('',(#68249,#68250,#68251,#68252));
#27691=EDGE_LOOP('',(#68253,#68254,#68255,#68256));
#27692=EDGE_LOOP('',(#68257,#68258,#68259,#68260));
#27693=EDGE_LOOP('',(#68261,#68262,#68263,#68264));
#27694=EDGE_LOOP('',(#68265,#68266,#68267,#68268));
#27695=EDGE_LOOP('',(#68269,#68270,#68271,#68272));
#27696=EDGE_LOOP('',(#68273,#68274,#68275,#68276));
#27697=EDGE_LOOP('',(#68277,#68278,#68279,#68280));
#27698=EDGE_LOOP('',(#68281,#68282,#68283,#68284));
#27699=EDGE_LOOP('',(#68285,#68286,#68287,#68288));
#27700=EDGE_LOOP('',(#68289,#68290,#68291,#68292));
#27701=EDGE_LOOP('',(#68293,#68294,#68295,#68296));
#27702=EDGE_LOOP('',(#68297,#68298,#68299,#68300));
#27703=EDGE_LOOP('',(#68301,#68302,#68303,#68304));
#27704=EDGE_LOOP('',(#68305,#68306,#68307,#68308));
#27705=EDGE_LOOP('',(#68309,#68310,#68311,#68312));
#27706=EDGE_LOOP('',(#68313,#68314,#68315,#68316));
#27707=EDGE_LOOP('',(#68317,#68318,#68319,#68320));
#27708=EDGE_LOOP('',(#68321,#68322,#68323,#68324));
#27709=EDGE_LOOP('',(#68325,#68326,#68327,#68328));
#27710=EDGE_LOOP('',(#68329,#68330,#68331,#68332));
#27711=EDGE_LOOP('',(#68333,#68334,#68335,#68336));
#27712=EDGE_LOOP('',(#68337,#68338,#68339,#68340));
#27713=EDGE_LOOP('',(#68341,#68342,#68343,#68344));
#27714=EDGE_LOOP('',(#68345,#68346,#68347,#68348));
#27715=EDGE_LOOP('',(#68349,#68350,#68351,#68352));
#27716=EDGE_LOOP('',(#68353,#68354,#68355,#68356));
#27717=EDGE_LOOP('',(#68357,#68358,#68359,#68360));
#27718=EDGE_LOOP('',(#68361,#68362,#68363,#68364));
#27719=EDGE_LOOP('',(#68365,#68366,#68367,#68368));
#27720=EDGE_LOOP('',(#68369,#68370,#68371,#68372));
#27721=EDGE_LOOP('',(#68373,#68374,#68375,#68376));
#27722=EDGE_LOOP('',(#68377,#68378,#68379,#68380));
#27723=EDGE_LOOP('',(#68381,#68382,#68383,#68384));
#27724=EDGE_LOOP('',(#68385,#68386,#68387,#68388));
#27725=EDGE_LOOP('',(#68389,#68390,#68391,#68392));
#27726=EDGE_LOOP('',(#68393,#68394,#68395,#68396));
#27727=EDGE_LOOP('',(#68397,#68398,#68399,#68400));
#27728=EDGE_LOOP('',(#68401,#68402,#68403,#68404));
#27729=EDGE_LOOP('',(#68405,#68406,#68407,#68408));
#27730=EDGE_LOOP('',(#68409,#68410,#68411,#68412));
#27731=EDGE_LOOP('',(#68413,#68414,#68415,#68416));
#27732=EDGE_LOOP('',(#68417,#68418,#68419,#68420));
#27733=EDGE_LOOP('',(#68421,#68422,#68423,#68424));
#27734=EDGE_LOOP('',(#68425,#68426,#68427,#68428));
#27735=EDGE_LOOP('',(#68429,#68430,#68431,#68432));
#27736=EDGE_LOOP('',(#68433,#68434,#68435,#68436));
#27737=EDGE_LOOP('',(#68437,#68438,#68439,#68440));
#27738=EDGE_LOOP('',(#68441,#68442,#68443,#68444));
#27739=EDGE_LOOP('',(#68445,#68446,#68447,#68448));
#27740=EDGE_LOOP('',(#68449,#68450,#68451,#68452));
#27741=EDGE_LOOP('',(#68453,#68454,#68455,#68456));
#27742=EDGE_LOOP('',(#68457,#68458,#68459,#68460));
#27743=EDGE_LOOP('',(#68461,#68462,#68463,#68464));
#27744=EDGE_LOOP('',(#68465,#68466,#68467,#68468));
#27745=EDGE_LOOP('',(#68469,#68470,#68471,#68472));
#27746=EDGE_LOOP('',(#68473,#68474,#68475,#68476));
#27747=EDGE_LOOP('',(#68477,#68478,#68479,#68480));
#27748=EDGE_LOOP('',(#68481,#68482,#68483,#68484));
#27749=EDGE_LOOP('',(#68485,#68486,#68487,#68488));
#27750=EDGE_LOOP('',(#68489,#68490,#68491,#68492));
#27751=EDGE_LOOP('',(#68493,#68494,#68495,#68496));
#27752=EDGE_LOOP('',(#68497,#68498,#68499,#68500));
#27753=EDGE_LOOP('',(#68501,#68502,#68503,#68504));
#27754=EDGE_LOOP('',(#68505,#68506,#68507,#68508));
#27755=EDGE_LOOP('',(#68509,#68510,#68511,#68512));
#27756=EDGE_LOOP('',(#68513,#68514,#68515,#68516));
#27757=EDGE_LOOP('',(#68517,#68518,#68519,#68520));
#27758=EDGE_LOOP('',(#68521,#68522,#68523,#68524));
#27759=EDGE_LOOP('',(#68525,#68526,#68527,#68528));
#27760=EDGE_LOOP('',(#68529,#68530,#68531,#68532));
#27761=EDGE_LOOP('',(#68533,#68534,#68535,#68536));
#27762=EDGE_LOOP('',(#68537,#68538,#68539,#68540));
#27763=EDGE_LOOP('',(#68541,#68542,#68543,#68544));
#27764=EDGE_LOOP('',(#68545,#68546,#68547,#68548));
#27765=EDGE_LOOP('',(#68549,#68550,#68551,#68552));
#27766=EDGE_LOOP('',(#68553,#68554,#68555,#68556));
#27767=EDGE_LOOP('',(#68557,#68558,#68559,#68560));
#27768=EDGE_LOOP('',(#68561,#68562,#68563,#68564));
#27769=EDGE_LOOP('',(#68565,#68566,#68567,#68568));
#27770=EDGE_LOOP('',(#68569,#68570,#68571,#68572));
#27771=EDGE_LOOP('',(#68573,#68574,#68575,#68576));
#27772=EDGE_LOOP('',(#68577,#68578,#68579,#68580));
#27773=EDGE_LOOP('',(#68581,#68582,#68583,#68584));
#27774=EDGE_LOOP('',(#68585,#68586,#68587,#68588));
#27775=EDGE_LOOP('',(#68589,#68590,#68591,#68592));
#27776=EDGE_LOOP('',(#68593,#68594,#68595,#68596));
#27777=EDGE_LOOP('',(#68597,#68598,#68599,#68600));
#27778=EDGE_LOOP('',(#68601,#68602,#68603,#68604));
#27779=EDGE_LOOP('',(#68605,#68606,#68607,#68608));
#27780=EDGE_LOOP('',(#68609,#68610,#68611,#68612));
#27781=EDGE_LOOP('',(#68613,#68614,#68615,#68616));
#27782=EDGE_LOOP('',(#68617,#68618,#68619,#68620));
#27783=EDGE_LOOP('',(#68621,#68622,#68623,#68624));
#27784=EDGE_LOOP('',(#68625,#68626,#68627,#68628));
#27785=EDGE_LOOP('',(#68629,#68630,#68631,#68632));
#27786=EDGE_LOOP('',(#68633,#68634,#68635,#68636));
#27787=EDGE_LOOP('',(#68637,#68638,#68639,#68640));
#27788=EDGE_LOOP('',(#68641,#68642,#68643,#68644));
#27789=EDGE_LOOP('',(#68645,#68646,#68647,#68648));
#27790=EDGE_LOOP('',(#68649,#68650,#68651,#68652));
#27791=EDGE_LOOP('',(#68653,#68654,#68655,#68656));
#27792=EDGE_LOOP('',(#68657,#68658,#68659,#68660));
#27793=EDGE_LOOP('',(#68661,#68662,#68663,#68664));
#27794=EDGE_LOOP('',(#68665,#68666,#68667,#68668));
#27795=EDGE_LOOP('',(#68669,#68670,#68671,#68672));
#27796=EDGE_LOOP('',(#68673,#68674,#68675,#68676));
#27797=EDGE_LOOP('',(#68677,#68678,#68679,#68680));
#27798=EDGE_LOOP('',(#68681,#68682,#68683,#68684));
#27799=EDGE_LOOP('',(#68685,#68686,#68687,#68688));
#27800=EDGE_LOOP('',(#68689,#68690,#68691,#68692));
#27801=EDGE_LOOP('',(#68693));
#27802=EDGE_LOOP('',(#68694));
#27803=EDGE_LOOP('',(#68695));
#27804=EDGE_LOOP('',(#68696,#68697,#68698,#68699));
#27805=EDGE_LOOP('',(#68700,#68701,#68702,#68703));
#27806=EDGE_LOOP('',(#68704,#68705,#68706,#68707));
#27807=EDGE_LOOP('',(#68708,#68709,#68710,#68711));
#27808=EDGE_LOOP('',(#68712,#68713,#68714,#68715));
#27809=EDGE_LOOP('',(#68716,#68717,#68718,#68719));
#27810=EDGE_LOOP('',(#68720,#68721,#68722,#68723));
#27811=EDGE_LOOP('',(#68724,#68725,#68726,#68727));
#27812=EDGE_LOOP('',(#68728,#68729,#68730,#68731));
#27813=EDGE_LOOP('',(#68732,#68733,#68734,#68735));
#27814=EDGE_LOOP('',(#68736,#68737,#68738,#68739));
#27815=EDGE_LOOP('',(#68740,#68741,#68742,#68743));
#27816=EDGE_LOOP('',(#68744,#68745,#68746,#68747));
#27817=EDGE_LOOP('',(#68748,#68749,#68750,#68751));
#27818=EDGE_LOOP('',(#68752,#68753,#68754,#68755));
#27819=EDGE_LOOP('',(#68756,#68757,#68758,#68759));
#27820=EDGE_LOOP('',(#68760,#68761,#68762,#68763));
#27821=EDGE_LOOP('',(#68764,#68765,#68766,#68767));
#27822=EDGE_LOOP('',(#68768,#68769,#68770,#68771));
#27823=EDGE_LOOP('',(#68772,#68773,#68774,#68775));
#27824=EDGE_LOOP('',(#68776,#68777,#68778,#68779));
#27825=EDGE_LOOP('',(#68780,#68781,#68782,#68783));
#27826=EDGE_LOOP('',(#68784,#68785,#68786,#68787));
#27827=EDGE_LOOP('',(#68788,#68789,#68790,#68791));
#27828=EDGE_LOOP('',(#68792,#68793,#68794,#68795));
#27829=EDGE_LOOP('',(#68796,#68797,#68798,#68799));
#27830=EDGE_LOOP('',(#68800,#68801,#68802,#68803));
#27831=EDGE_LOOP('',(#68804,#68805,#68806,#68807));
#27832=EDGE_LOOP('',(#68808,#68809,#68810,#68811));
#27833=EDGE_LOOP('',(#68812,#68813,#68814,#68815));
#27834=EDGE_LOOP('',(#68816,#68817,#68818,#68819));
#27835=EDGE_LOOP('',(#68820,#68821,#68822,#68823));
#27836=EDGE_LOOP('',(#68824,#68825,#68826,#68827));
#27837=EDGE_LOOP('',(#68828,#68829,#68830,#68831));
#27838=EDGE_LOOP('',(#68832,#68833,#68834,#68835));
#27839=EDGE_LOOP('',(#68836,#68837,#68838,#68839));
#27840=EDGE_LOOP('',(#68840,#68841,#68842,#68843));
#27841=EDGE_LOOP('',(#68844,#68845,#68846,#68847));
#27842=EDGE_LOOP('',(#68848,#68849,#68850,#68851));
#27843=EDGE_LOOP('',(#68852,#68853,#68854,#68855));
#27844=EDGE_LOOP('',(#68856,#68857,#68858,#68859));
#27845=EDGE_LOOP('',(#68860,#68861,#68862,#68863));
#27846=EDGE_LOOP('',(#68864,#68865,#68866,#68867));
#27847=EDGE_LOOP('',(#68868,#68869,#68870,#68871));
#27848=EDGE_LOOP('',(#68872,#68873,#68874,#68875));
#27849=EDGE_LOOP('',(#68876,#68877,#68878,#68879));
#27850=EDGE_LOOP('',(#68880,#68881,#68882,#68883));
#27851=EDGE_LOOP('',(#68884,#68885,#68886,#68887));
#27852=EDGE_LOOP('',(#68888,#68889,#68890,#68891));
#27853=EDGE_LOOP('',(#68892,#68893,#68894,#68895));
#27854=EDGE_LOOP('',(#68896,#68897,#68898,#68899));
#27855=EDGE_LOOP('',(#68900,#68901,#68902,#68903));
#27856=EDGE_LOOP('',(#68904,#68905,#68906,#68907));
#27857=EDGE_LOOP('',(#68908,#68909,#68910,#68911));
#27858=EDGE_LOOP('',(#68912,#68913,#68914,#68915));
#27859=EDGE_LOOP('',(#68916,#68917,#68918,#68919));
#27860=EDGE_LOOP('',(#68920,#68921,#68922,#68923));
#27861=EDGE_LOOP('',(#68924,#68925,#68926,#68927));
#27862=EDGE_LOOP('',(#68928,#68929,#68930,#68931));
#27863=EDGE_LOOP('',(#68932,#68933,#68934,#68935));
#27864=EDGE_LOOP('',(#68936,#68937,#68938,#68939));
#27865=EDGE_LOOP('',(#68940,#68941,#68942,#68943));
#27866=EDGE_LOOP('',(#68944,#68945,#68946,#68947));
#27867=EDGE_LOOP('',(#68948,#68949,#68950,#68951));
#27868=EDGE_LOOP('',(#68952,#68953,#68954,#68955));
#27869=EDGE_LOOP('',(#68956,#68957,#68958,#68959));
#27870=EDGE_LOOP('',(#68960,#68961,#68962,#68963));
#27871=EDGE_LOOP('',(#68964,#68965,#68966,#68967));
#27872=EDGE_LOOP('',(#68968,#68969,#68970,#68971));
#27873=EDGE_LOOP('',(#68972,#68973,#68974,#68975));
#27874=EDGE_LOOP('',(#68976,#68977,#68978,#68979));
#27875=EDGE_LOOP('',(#68980,#68981,#68982,#68983));
#27876=EDGE_LOOP('',(#68984,#68985,#68986,#68987));
#27877=EDGE_LOOP('',(#68988,#68989,#68990,#68991));
#27878=EDGE_LOOP('',(#68992,#68993,#68994,#68995));
#27879=EDGE_LOOP('',(#68996,#68997,#68998,#68999));
#27880=EDGE_LOOP('',(#69000,#69001,#69002,#69003));
#27881=EDGE_LOOP('',(#69004,#69005,#69006,#69007));
#27882=EDGE_LOOP('',(#69008,#69009,#69010,#69011));
#27883=EDGE_LOOP('',(#69012,#69013,#69014,#69015));
#27884=EDGE_LOOP('',(#69016,#69017,#69018,#69019));
#27885=EDGE_LOOP('',(#69020,#69021,#69022,#69023));
#27886=EDGE_LOOP('',(#69024,#69025,#69026,#69027));
#27887=EDGE_LOOP('',(#69028,#69029,#69030,#69031));
#27888=EDGE_LOOP('',(#69032,#69033,#69034,#69035));
#27889=EDGE_LOOP('',(#69036,#69037,#69038,#69039));
#27890=EDGE_LOOP('',(#69040,#69041,#69042,#69043));
#27891=EDGE_LOOP('',(#69044,#69045,#69046,#69047));
#27892=EDGE_LOOP('',(#69048,#69049,#69050,#69051));
#27893=EDGE_LOOP('',(#69052,#69053,#69054,#69055));
#27894=EDGE_LOOP('',(#69056,#69057,#69058,#69059));
#27895=EDGE_LOOP('',(#69060,#69061,#69062,#69063));
#27896=EDGE_LOOP('',(#69064,#69065,#69066,#69067));
#27897=EDGE_LOOP('',(#69068,#69069,#69070,#69071));
#27898=EDGE_LOOP('',(#69072,#69073,#69074,#69075));
#27899=EDGE_LOOP('',(#69076,#69077,#69078,#69079));
#27900=EDGE_LOOP('',(#69080,#69081,#69082,#69083));
#27901=EDGE_LOOP('',(#69084,#69085,#69086,#69087));
#27902=EDGE_LOOP('',(#69088,#69089,#69090,#69091));
#27903=EDGE_LOOP('',(#69092,#69093,#69094,#69095));
#27904=EDGE_LOOP('',(#69096,#69097,#69098,#69099));
#27905=EDGE_LOOP('',(#69100,#69101,#69102,#69103));
#27906=EDGE_LOOP('',(#69104,#69105,#69106,#69107));
#27907=EDGE_LOOP('',(#69108,#69109,#69110,#69111));
#27908=EDGE_LOOP('',(#69112,#69113,#69114,#69115));
#27909=EDGE_LOOP('',(#69116,#69117,#69118,#69119));
#27910=EDGE_LOOP('',(#69120,#69121,#69122,#69123));
#27911=EDGE_LOOP('',(#69124,#69125,#69126,#69127));
#27912=EDGE_LOOP('',(#69128,#69129,#69130,#69131));
#27913=EDGE_LOOP('',(#69132,#69133,#69134,#69135));
#27914=EDGE_LOOP('',(#69136,#69137,#69138,#69139));
#27915=EDGE_LOOP('',(#69140,#69141,#69142,#69143));
#27916=EDGE_LOOP('',(#69144,#69145,#69146,#69147));
#27917=EDGE_LOOP('',(#69148,#69149,#69150,#69151));
#27918=EDGE_LOOP('',(#69152,#69153,#69154,#69155));
#27919=EDGE_LOOP('',(#69156,#69157,#69158,#69159));
#27920=EDGE_LOOP('',(#69160,#69161,#69162,#69163));
#27921=EDGE_LOOP('',(#69164,#69165,#69166,#69167));
#27922=EDGE_LOOP('',(#69168,#69169,#69170,#69171));
#27923=EDGE_LOOP('',(#69172,#69173,#69174,#69175));
#27924=EDGE_LOOP('',(#69176,#69177,#69178,#69179));
#27925=EDGE_LOOP('',(#69180,#69181,#69182,#69183));
#27926=EDGE_LOOP('',(#69184,#69185,#69186,#69187));
#27927=EDGE_LOOP('',(#69188,#69189,#69190,#69191));
#27928=EDGE_LOOP('',(#69192,#69193,#69194,#69195));
#27929=EDGE_LOOP('',(#69196,#69197,#69198,#69199));
#27930=EDGE_LOOP('',(#69200,#69201,#69202,#69203));
#27931=EDGE_LOOP('',(#69204,#69205,#69206,#69207));
#27932=EDGE_LOOP('',(#69208,#69209,#69210,#69211));
#27933=EDGE_LOOP('',(#69212,#69213,#69214,#69215));
#27934=EDGE_LOOP('',(#69216,#69217,#69218,#69219));
#27935=EDGE_LOOP('',(#69220,#69221,#69222,#69223));
#27936=EDGE_LOOP('',(#69224,#69225,#69226,#69227));
#27937=EDGE_LOOP('',(#69228,#69229,#69230,#69231));
#27938=EDGE_LOOP('',(#69232,#69233,#69234,#69235));
#27939=EDGE_LOOP('',(#69236,#69237,#69238,#69239));
#27940=EDGE_LOOP('',(#69240,#69241,#69242,#69243));
#27941=EDGE_LOOP('',(#69244,#69245,#69246,#69247));
#27942=EDGE_LOOP('',(#69248,#69249,#69250,#69251));
#27943=EDGE_LOOP('',(#69252,#69253,#69254,#69255));
#27944=EDGE_LOOP('',(#69256,#69257,#69258,#69259));
#27945=EDGE_LOOP('',(#69260,#69261,#69262,#69263));
#27946=EDGE_LOOP('',(#69264,#69265,#69266,#69267));
#27947=EDGE_LOOP('',(#69268,#69269,#69270,#69271));
#27948=EDGE_LOOP('',(#69272,#69273,#69274,#69275));
#27949=EDGE_LOOP('',(#69276,#69277,#69278,#69279));
#27950=EDGE_LOOP('',(#69280,#69281,#69282,#69283));
#27951=EDGE_LOOP('',(#69284,#69285,#69286,#69287));
#27952=EDGE_LOOP('',(#69288,#69289,#69290,#69291));
#27953=EDGE_LOOP('',(#69292,#69293,#69294,#69295));
#27954=EDGE_LOOP('',(#69296,#69297,#69298,#69299));
#27955=EDGE_LOOP('',(#69300,#69301,#69302,#69303));
#27956=EDGE_LOOP('',(#69304,#69305,#69306,#69307));
#27957=EDGE_LOOP('',(#69308,#69309,#69310,#69311));
#27958=EDGE_LOOP('',(#69312,#69313,#69314,#69315));
#27959=EDGE_LOOP('',(#69316,#69317,#69318,#69319));
#27960=EDGE_LOOP('',(#69320,#69321,#69322,#69323));
#27961=EDGE_LOOP('',(#69324,#69325,#69326,#69327));
#27962=EDGE_LOOP('',(#69328,#69329,#69330,#69331));
#27963=EDGE_LOOP('',(#69332,#69333,#69334,#69335));
#27964=EDGE_LOOP('',(#69336,#69337,#69338,#69339));
#27965=EDGE_LOOP('',(#69340,#69341,#69342,#69343));
#27966=EDGE_LOOP('',(#69344,#69345,#69346,#69347));
#27967=EDGE_LOOP('',(#69348,#69349,#69350,#69351));
#27968=EDGE_LOOP('',(#69352,#69353,#69354,#69355));
#27969=EDGE_LOOP('',(#69356,#69357,#69358,#69359));
#27970=EDGE_LOOP('',(#69360,#69361,#69362,#69363));
#27971=EDGE_LOOP('',(#69364,#69365,#69366,#69367));
#27972=EDGE_LOOP('',(#69368,#69369,#69370,#69371));
#27973=EDGE_LOOP('',(#69372,#69373,#69374,#69375));
#27974=EDGE_LOOP('',(#69376,#69377,#69378,#69379));
#27975=EDGE_LOOP('',(#69380,#69381,#69382,#69383));
#27976=EDGE_LOOP('',(#69384,#69385,#69386,#69387));
#27977=EDGE_LOOP('',(#69388,#69389,#69390,#69391));
#27978=EDGE_LOOP('',(#69392,#69393,#69394,#69395));
#27979=EDGE_LOOP('',(#69396,#69397,#69398,#69399));
#27980=EDGE_LOOP('',(#69400,#69401,#69402,#69403));
#27981=EDGE_LOOP('',(#69404,#69405,#69406,#69407));
#27982=EDGE_LOOP('',(#69408,#69409,#69410,#69411));
#27983=EDGE_LOOP('',(#69412,#69413,#69414,#69415));
#27984=EDGE_LOOP('',(#69416,#69417,#69418,#69419));
#27985=EDGE_LOOP('',(#69420,#69421,#69422,#69423));
#27986=EDGE_LOOP('',(#69424,#69425,#69426,#69427));
#27987=EDGE_LOOP('',(#69428,#69429,#69430,#69431));
#27988=EDGE_LOOP('',(#69432,#69433,#69434,#69435));
#27989=EDGE_LOOP('',(#69436,#69437,#69438,#69439));
#27990=EDGE_LOOP('',(#69440,#69441,#69442,#69443));
#27991=EDGE_LOOP('',(#69444,#69445,#69446,#69447));
#27992=EDGE_LOOP('',(#69448,#69449,#69450,#69451));
#27993=EDGE_LOOP('',(#69452,#69453,#69454,#69455));
#27994=EDGE_LOOP('',(#69456,#69457,#69458,#69459));
#27995=EDGE_LOOP('',(#69460,#69461,#69462,#69463));
#27996=EDGE_LOOP('',(#69464,#69465,#69466,#69467));
#27997=EDGE_LOOP('',(#69468,#69469,#69470,#69471));
#27998=EDGE_LOOP('',(#69472,#69473,#69474,#69475));
#27999=EDGE_LOOP('',(#69476,#69477,#69478,#69479));
#28000=EDGE_LOOP('',(#69480,#69481,#69482,#69483));
#28001=EDGE_LOOP('',(#69484,#69485,#69486,#69487));
#28002=EDGE_LOOP('',(#69488,#69489,#69490,#69491));
#28003=EDGE_LOOP('',(#69492,#69493,#69494,#69495));
#28004=EDGE_LOOP('',(#69496,#69497,#69498,#69499));
#28005=EDGE_LOOP('',(#69500,#69501,#69502,#69503));
#28006=EDGE_LOOP('',(#69504,#69505,#69506,#69507));
#28007=EDGE_LOOP('',(#69508,#69509,#69510,#69511));
#28008=EDGE_LOOP('',(#69512,#69513,#69514,#69515));
#28009=EDGE_LOOP('',(#69516,#69517,#69518,#69519));
#28010=EDGE_LOOP('',(#69520,#69521,#69522,#69523));
#28011=EDGE_LOOP('',(#69524,#69525,#69526,#69527));
#28012=EDGE_LOOP('',(#69528,#69529,#69530,#69531));
#28013=EDGE_LOOP('',(#69532,#69533,#69534,#69535));
#28014=EDGE_LOOP('',(#69536,#69537,#69538,#69539));
#28015=EDGE_LOOP('',(#69540,#69541,#69542,#69543));
#28016=EDGE_LOOP('',(#69544,#69545,#69546,#69547));
#28017=EDGE_LOOP('',(#69548,#69549,#69550,#69551));
#28018=EDGE_LOOP('',(#69552,#69553,#69554,#69555));
#28019=EDGE_LOOP('',(#69556,#69557,#69558,#69559));
#28020=EDGE_LOOP('',(#69560,#69561,#69562,#69563));
#28021=EDGE_LOOP('',(#69564,#69565,#69566,#69567));
#28022=EDGE_LOOP('',(#69568,#69569,#69570,#69571));
#28023=EDGE_LOOP('',(#69572,#69573,#69574,#69575));
#28024=EDGE_LOOP('',(#69576,#69577,#69578,#69579));
#28025=EDGE_LOOP('',(#69580,#69581,#69582,#69583));
#28026=EDGE_LOOP('',(#69584,#69585,#69586,#69587));
#28027=EDGE_LOOP('',(#69588,#69589,#69590,#69591));
#28028=EDGE_LOOP('',(#69592,#69593,#69594,#69595));
#28029=EDGE_LOOP('',(#69596,#69597,#69598,#69599));
#28030=EDGE_LOOP('',(#69600,#69601,#69602,#69603));
#28031=EDGE_LOOP('',(#69604,#69605,#69606,#69607));
#28032=EDGE_LOOP('',(#69608,#69609,#69610,#69611));
#28033=EDGE_LOOP('',(#69612,#69613,#69614,#69615));
#28034=EDGE_LOOP('',(#69616,#69617,#69618,#69619));
#28035=EDGE_LOOP('',(#69620,#69621,#69622,#69623));
#28036=EDGE_LOOP('',(#69624,#69625,#69626,#69627));
#28037=EDGE_LOOP('',(#69628,#69629,#69630,#69631));
#28038=EDGE_LOOP('',(#69632,#69633,#69634,#69635));
#28039=EDGE_LOOP('',(#69636,#69637,#69638,#69639));
#28040=EDGE_LOOP('',(#69640,#69641,#69642,#69643));
#28041=EDGE_LOOP('',(#69644,#69645,#69646,#69647));
#28042=EDGE_LOOP('',(#69648,#69649,#69650,#69651));
#28043=EDGE_LOOP('',(#69652,#69653,#69654,#69655));
#28044=EDGE_LOOP('',(#69656,#69657,#69658,#69659));
#28045=EDGE_LOOP('',(#69660,#69661,#69662,#69663));
#28046=EDGE_LOOP('',(#69664,#69665,#69666,#69667));
#28047=EDGE_LOOP('',(#69668,#69669,#69670,#69671));
#28048=EDGE_LOOP('',(#69672,#69673,#69674,#69675));
#28049=EDGE_LOOP('',(#69676,#69677,#69678,#69679));
#28050=EDGE_LOOP('',(#69680,#69681,#69682,#69683));
#28051=EDGE_LOOP('',(#69684,#69685,#69686,#69687));
#28052=EDGE_LOOP('',(#69688,#69689,#69690,#69691));
#28053=EDGE_LOOP('',(#69692,#69693,#69694,#69695));
#28054=EDGE_LOOP('',(#69696,#69697,#69698,#69699));
#28055=EDGE_LOOP('',(#69700,#69701,#69702,#69703));
#28056=EDGE_LOOP('',(#69704,#69705,#69706,#69707));
#28057=EDGE_LOOP('',(#69708,#69709,#69710,#69711));
#28058=EDGE_LOOP('',(#69712,#69713,#69714,#69715));
#28059=EDGE_LOOP('',(#69716,#69717,#69718,#69719));
#28060=EDGE_LOOP('',(#69720,#69721,#69722,#69723));
#28061=EDGE_LOOP('',(#69724,#69725,#69726,#69727));
#28062=EDGE_LOOP('',(#69728,#69729,#69730,#69731));
#28063=EDGE_LOOP('',(#69732,#69733,#69734,#69735));
#28064=EDGE_LOOP('',(#69736,#69737,#69738,#69739));
#28065=EDGE_LOOP('',(#69740,#69741,#69742,#69743));
#28066=EDGE_LOOP('',(#69744,#69745,#69746,#69747));
#28067=EDGE_LOOP('',(#69748,#69749,#69750,#69751));
#28068=EDGE_LOOP('',(#69752,#69753,#69754,#69755));
#28069=EDGE_LOOP('',(#69756,#69757,#69758,#69759));
#28070=EDGE_LOOP('',(#69760,#69761,#69762,#69763));
#28071=EDGE_LOOP('',(#69764,#69765,#69766,#69767));
#28072=EDGE_LOOP('',(#69768,#69769,#69770,#69771));
#28073=EDGE_LOOP('',(#69772,#69773,#69774,#69775));
#28074=EDGE_LOOP('',(#69776,#69777,#69778,#69779));
#28075=EDGE_LOOP('',(#69780,#69781,#69782,#69783));
#28076=EDGE_LOOP('',(#69784,#69785,#69786,#69787));
#28077=EDGE_LOOP('',(#69788,#69789,#69790,#69791));
#28078=EDGE_LOOP('',(#69792,#69793,#69794,#69795));
#28079=EDGE_LOOP('',(#69796,#69797,#69798,#69799));
#28080=EDGE_LOOP('',(#69800,#69801,#69802,#69803));
#28081=EDGE_LOOP('',(#69804,#69805,#69806,#69807));
#28082=EDGE_LOOP('',(#69808,#69809,#69810,#69811));
#28083=EDGE_LOOP('',(#69812,#69813,#69814,#69815));
#28084=EDGE_LOOP('',(#69816,#69817,#69818,#69819));
#28085=EDGE_LOOP('',(#69820,#69821,#69822,#69823));
#28086=EDGE_LOOP('',(#69824,#69825,#69826,#69827));
#28087=EDGE_LOOP('',(#69828,#69829,#69830,#69831));
#28088=EDGE_LOOP('',(#69832,#69833,#69834,#69835));
#28089=EDGE_LOOP('',(#69836,#69837,#69838,#69839));
#28090=EDGE_LOOP('',(#69840,#69841,#69842,#69843));
#28091=EDGE_LOOP('',(#69844,#69845,#69846,#69847));
#28092=EDGE_LOOP('',(#69848,#69849,#69850,#69851));
#28093=EDGE_LOOP('',(#69852,#69853,#69854,#69855));
#28094=EDGE_LOOP('',(#69856,#69857,#69858,#69859));
#28095=EDGE_LOOP('',(#69860,#69861,#69862,#69863));
#28096=EDGE_LOOP('',(#69864,#69865,#69866,#69867));
#28097=EDGE_LOOP('',(#69868,#69869,#69870,#69871));
#28098=EDGE_LOOP('',(#69872,#69873,#69874,#69875));
#28099=EDGE_LOOP('',(#69876,#69877,#69878,#69879));
#28100=EDGE_LOOP('',(#69880,#69881,#69882,#69883));
#28101=EDGE_LOOP('',(#69884,#69885,#69886,#69887));
#28102=EDGE_LOOP('',(#69888,#69889,#69890,#69891));
#28103=EDGE_LOOP('',(#69892,#69893,#69894,#69895));
#28104=EDGE_LOOP('',(#69896,#69897,#69898,#69899));
#28105=EDGE_LOOP('',(#69900,#69901,#69902,#69903));
#28106=EDGE_LOOP('',(#69904,#69905,#69906,#69907));
#28107=EDGE_LOOP('',(#69908,#69909,#69910,#69911));
#28108=EDGE_LOOP('',(#69912,#69913,#69914,#69915));
#28109=EDGE_LOOP('',(#69916,#69917,#69918,#69919));
#28110=EDGE_LOOP('',(#69920,#69921,#69922,#69923));
#28111=EDGE_LOOP('',(#69924,#69925,#69926,#69927));
#28112=EDGE_LOOP('',(#69928,#69929,#69930,#69931));
#28113=EDGE_LOOP('',(#69932,#69933,#69934,#69935));
#28114=EDGE_LOOP('',(#69936,#69937,#69938,#69939));
#28115=EDGE_LOOP('',(#69940,#69941,#69942,#69943));
#28116=EDGE_LOOP('',(#69944,#69945,#69946,#69947));
#28117=EDGE_LOOP('',(#69948,#69949,#69950,#69951));
#28118=EDGE_LOOP('',(#69952,#69953,#69954,#69955));
#28119=EDGE_LOOP('',(#69956,#69957,#69958,#69959));
#28120=EDGE_LOOP('',(#69960,#69961,#69962,#69963));
#28121=EDGE_LOOP('',(#69964,#69965,#69966,#69967));
#28122=EDGE_LOOP('',(#69968,#69969,#69970,#69971));
#28123=EDGE_LOOP('',(#69972,#69973,#69974,#69975));
#28124=EDGE_LOOP('',(#69976,#69977,#69978,#69979));
#28125=EDGE_LOOP('',(#69980,#69981,#69982,#69983));
#28126=EDGE_LOOP('',(#69984,#69985,#69986,#69987));
#28127=EDGE_LOOP('',(#69988,#69989,#69990,#69991));
#28128=EDGE_LOOP('',(#69992,#69993,#69994,#69995));
#28129=EDGE_LOOP('',(#69996,#69997,#69998,#69999));
#28130=EDGE_LOOP('',(#70000,#70001,#70002,#70003));
#28131=EDGE_LOOP('',(#70004,#70005,#70006,#70007));
#28132=EDGE_LOOP('',(#70008,#70009,#70010,#70011));
#28133=EDGE_LOOP('',(#70012,#70013,#70014,#70015));
#28134=EDGE_LOOP('',(#70016,#70017,#70018,#70019));
#28135=EDGE_LOOP('',(#70020,#70021,#70022,#70023));
#28136=EDGE_LOOP('',(#70024,#70025,#70026,#70027));
#28137=EDGE_LOOP('',(#70028,#70029,#70030,#70031));
#28138=EDGE_LOOP('',(#70032,#70033,#70034,#70035));
#28139=EDGE_LOOP('',(#70036,#70037,#70038,#70039));
#28140=EDGE_LOOP('',(#70040,#70041,#70042,#70043));
#28141=EDGE_LOOP('',(#70044,#70045,#70046,#70047));
#28142=EDGE_LOOP('',(#70048,#70049,#70050,#70051));
#28143=EDGE_LOOP('',(#70052,#70053,#70054,#70055));
#28144=EDGE_LOOP('',(#70056,#70057,#70058,#70059));
#28145=EDGE_LOOP('',(#70060,#70061,#70062,#70063));
#28146=EDGE_LOOP('',(#70064,#70065,#70066,#70067));
#28147=EDGE_LOOP('',(#70068,#70069,#70070,#70071));
#28148=EDGE_LOOP('',(#70072,#70073,#70074,#70075));
#28149=EDGE_LOOP('',(#70076,#70077,#70078,#70079));
#28150=EDGE_LOOP('',(#70080,#70081,#70082,#70083));
#28151=EDGE_LOOP('',(#70084,#70085,#70086,#70087));
#28152=EDGE_LOOP('',(#70088,#70089,#70090,#70091));
#28153=EDGE_LOOP('',(#70092,#70093,#70094,#70095));
#28154=EDGE_LOOP('',(#70096,#70097,#70098,#70099));
#28155=EDGE_LOOP('',(#70100,#70101,#70102,#70103));
#28156=EDGE_LOOP('',(#70104,#70105,#70106,#70107));
#28157=EDGE_LOOP('',(#70108,#70109,#70110,#70111));
#28158=EDGE_LOOP('',(#70112,#70113,#70114,#70115));
#28159=EDGE_LOOP('',(#70116,#70117,#70118,#70119));
#28160=EDGE_LOOP('',(#70120,#70121,#70122,#70123));
#28161=EDGE_LOOP('',(#70124,#70125,#70126,#70127));
#28162=EDGE_LOOP('',(#70128,#70129,#70130,#70131));
#28163=EDGE_LOOP('',(#70132,#70133,#70134,#70135));
#28164=EDGE_LOOP('',(#70136,#70137,#70138,#70139));
#28165=EDGE_LOOP('',(#70140,#70141,#70142,#70143));
#28166=EDGE_LOOP('',(#70144,#70145,#70146,#70147));
#28167=EDGE_LOOP('',(#70148,#70149,#70150,#70151));
#28168=EDGE_LOOP('',(#70152,#70153,#70154,#70155));
#28169=EDGE_LOOP('',(#70156,#70157,#70158,#70159));
#28170=EDGE_LOOP('',(#70160,#70161,#70162,#70163));
#28171=EDGE_LOOP('',(#70164,#70165,#70166,#70167));
#28172=EDGE_LOOP('',(#70168,#70169,#70170,#70171));
#28173=EDGE_LOOP('',(#70172,#70173,#70174,#70175));
#28174=EDGE_LOOP('',(#70176,#70177,#70178,#70179));
#28175=EDGE_LOOP('',(#70180,#70181,#70182,#70183));
#28176=EDGE_LOOP('',(#70184,#70185,#70186,#70187));
#28177=EDGE_LOOP('',(#70188,#70189,#70190,#70191));
#28178=EDGE_LOOP('',(#70192,#70193,#70194,#70195));
#28179=EDGE_LOOP('',(#70196,#70197,#70198,#70199));
#28180=EDGE_LOOP('',(#70200,#70201,#70202,#70203));
#28181=EDGE_LOOP('',(#70204,#70205,#70206,#70207));
#28182=EDGE_LOOP('',(#70208,#70209,#70210,#70211));
#28183=EDGE_LOOP('',(#70212,#70213,#70214,#70215));
#28184=EDGE_LOOP('',(#70216,#70217,#70218,#70219));
#28185=EDGE_LOOP('',(#70220,#70221,#70222,#70223));
#28186=EDGE_LOOP('',(#70224,#70225,#70226,#70227));
#28187=EDGE_LOOP('',(#70228,#70229,#70230,#70231));
#28188=EDGE_LOOP('',(#70232,#70233,#70234,#70235));
#28189=EDGE_LOOP('',(#70236,#70237,#70238,#70239));
#28190=EDGE_LOOP('',(#70240,#70241,#70242,#70243));
#28191=EDGE_LOOP('',(#70244,#70245,#70246,#70247));
#28192=EDGE_LOOP('',(#70248,#70249,#70250,#70251));
#28193=EDGE_LOOP('',(#70252,#70253,#70254,#70255));
#28194=EDGE_LOOP('',(#70256,#70257,#70258,#70259));
#28195=EDGE_LOOP('',(#70260,#70261,#70262,#70263));
#28196=EDGE_LOOP('',(#70264,#70265,#70266,#70267));
#28197=EDGE_LOOP('',(#70268,#70269,#70270,#70271));
#28198=EDGE_LOOP('',(#70272,#70273,#70274,#70275));
#28199=EDGE_LOOP('',(#70276,#70277,#70278,#70279));
#28200=EDGE_LOOP('',(#70280,#70281,#70282,#70283));
#28201=EDGE_LOOP('',(#70284,#70285,#70286,#70287));
#28202=EDGE_LOOP('',(#70288,#70289,#70290,#70291));
#28203=EDGE_LOOP('',(#70292,#70293,#70294,#70295));
#28204=EDGE_LOOP('',(#70296,#70297,#70298,#70299));
#28205=EDGE_LOOP('',(#70300,#70301,#70302,#70303));
#28206=EDGE_LOOP('',(#70304,#70305,#70306,#70307));
#28207=EDGE_LOOP('',(#70308,#70309,#70310,#70311));
#28208=EDGE_LOOP('',(#70312,#70313,#70314,#70315));
#28209=EDGE_LOOP('',(#70316,#70317,#70318,#70319));
#28210=EDGE_LOOP('',(#70320,#70321,#70322,#70323));
#28211=EDGE_LOOP('',(#70324,#70325,#70326,#70327));
#28212=EDGE_LOOP('',(#70328,#70329,#70330,#70331));
#28213=EDGE_LOOP('',(#70332,#70333,#70334,#70335));
#28214=EDGE_LOOP('',(#70336,#70337,#70338,#70339));
#28215=EDGE_LOOP('',(#70340,#70341,#70342,#70343));
#28216=EDGE_LOOP('',(#70344,#70345,#70346,#70347));
#28217=EDGE_LOOP('',(#70348,#70349,#70350,#70351));
#28218=EDGE_LOOP('',(#70352,#70353,#70354,#70355));
#28219=EDGE_LOOP('',(#70356,#70357,#70358,#70359));
#28220=EDGE_LOOP('',(#70360,#70361,#70362,#70363));
#28221=EDGE_LOOP('',(#70364,#70365,#70366,#70367));
#28222=EDGE_LOOP('',(#70368,#70369,#70370,#70371));
#28223=EDGE_LOOP('',(#70372,#70373,#70374,#70375));
#28224=EDGE_LOOP('',(#70376,#70377,#70378,#70379));
#28225=EDGE_LOOP('',(#70380,#70381,#70382,#70383));
#28226=EDGE_LOOP('',(#70384,#70385,#70386,#70387));
#28227=EDGE_LOOP('',(#70388,#70389,#70390,#70391));
#28228=EDGE_LOOP('',(#70392,#70393,#70394,#70395));
#28229=EDGE_LOOP('',(#70396,#70397,#70398,#70399));
#28230=EDGE_LOOP('',(#70400,#70401,#70402,#70403));
#28231=EDGE_LOOP('',(#70404,#70405,#70406,#70407));
#28232=EDGE_LOOP('',(#70408,#70409,#70410,#70411));
#28233=EDGE_LOOP('',(#70412,#70413,#70414,#70415));
#28234=EDGE_LOOP('',(#70416,#70417,#70418,#70419));
#28235=EDGE_LOOP('',(#70420,#70421,#70422,#70423));
#28236=EDGE_LOOP('',(#70424,#70425,#70426,#70427));
#28237=EDGE_LOOP('',(#70428,#70429,#70430,#70431));
#28238=EDGE_LOOP('',(#70432,#70433,#70434,#70435));
#28239=EDGE_LOOP('',(#70436,#70437,#70438,#70439));
#28240=EDGE_LOOP('',(#70440,#70441,#70442,#70443));
#28241=EDGE_LOOP('',(#70444,#70445,#70446,#70447));
#28242=EDGE_LOOP('',(#70448,#70449,#70450,#70451));
#28243=EDGE_LOOP('',(#70452,#70453,#70454,#70455));
#28244=EDGE_LOOP('',(#70456,#70457,#70458,#70459));
#28245=EDGE_LOOP('',(#70460));
#28246=EDGE_LOOP('',(#70461,#70462,#70463,#70464));
#28247=EDGE_LOOP('',(#70465,#70466,#70467,#70468));
#28248=EDGE_LOOP('',(#70469,#70470,#70471,#70472));
#28249=EDGE_LOOP('',(#70473,#70474,#70475,#70476));
#28250=EDGE_LOOP('',(#70477,#70478,#70479,#70480));
#28251=EDGE_LOOP('',(#70481,#70482,#70483,#70484));
#28252=EDGE_LOOP('',(#70485,#70486,#70487,#70488));
#28253=EDGE_LOOP('',(#70489,#70490,#70491,#70492));
#28254=EDGE_LOOP('',(#70493,#70494,#70495,#70496));
#28255=EDGE_LOOP('',(#70497,#70498,#70499,#70500));
#28256=EDGE_LOOP('',(#70501,#70502,#70503,#70504));
#28257=EDGE_LOOP('',(#70505,#70506,#70507,#70508));
#28258=EDGE_LOOP('',(#70509,#70510,#70511,#70512));
#28259=EDGE_LOOP('',(#70513,#70514,#70515,#70516));
#28260=EDGE_LOOP('',(#70517,#70518,#70519,#70520));
#28261=EDGE_LOOP('',(#70521,#70522,#70523,#70524));
#28262=EDGE_LOOP('',(#70525,#70526,#70527,#70528));
#28263=EDGE_LOOP('',(#70529,#70530,#70531,#70532));
#28264=EDGE_LOOP('',(#70533,#70534,#70535,#70536));
#28265=EDGE_LOOP('',(#70537,#70538,#70539,#70540));
#28266=EDGE_LOOP('',(#70541,#70542,#70543,#70544));
#28267=EDGE_LOOP('',(#70545,#70546,#70547,#70548));
#28268=EDGE_LOOP('',(#70549,#70550,#70551,#70552));
#28269=EDGE_LOOP('',(#70553,#70554,#70555,#70556));
#28270=EDGE_LOOP('',(#70557,#70558,#70559,#70560));
#28271=EDGE_LOOP('',(#70561,#70562,#70563,#70564));
#28272=EDGE_LOOP('',(#70565,#70566,#70567,#70568));
#28273=EDGE_LOOP('',(#70569,#70570,#70571,#70572));
#28274=EDGE_LOOP('',(#70573,#70574,#70575,#70576));
#28275=EDGE_LOOP('',(#70577,#70578,#70579,#70580));
#28276=EDGE_LOOP('',(#70581,#70582,#70583,#70584));
#28277=EDGE_LOOP('',(#70585,#70586,#70587,#70588));
#28278=EDGE_LOOP('',(#70589,#70590,#70591,#70592));
#28279=EDGE_LOOP('',(#70593,#70594,#70595,#70596));
#28280=EDGE_LOOP('',(#70597,#70598,#70599,#70600));
#28281=EDGE_LOOP('',(#70601,#70602,#70603,#70604));
#28282=EDGE_LOOP('',(#70605,#70606,#70607,#70608));
#28283=EDGE_LOOP('',(#70609,#70610,#70611,#70612));
#28284=EDGE_LOOP('',(#70613,#70614,#70615,#70616));
#28285=EDGE_LOOP('',(#70617,#70618,#70619,#70620));
#28286=EDGE_LOOP('',(#70621,#70622,#70623,#70624));
#28287=EDGE_LOOP('',(#70625,#70626,#70627,#70628));
#28288=EDGE_LOOP('',(#70629,#70630,#70631,#70632));
#28289=EDGE_LOOP('',(#70633,#70634,#70635,#70636));
#28290=EDGE_LOOP('',(#70637,#70638,#70639,#70640));
#28291=EDGE_LOOP('',(#70641,#70642,#70643,#70644));
#28292=EDGE_LOOP('',(#70645,#70646,#70647,#70648));
#28293=EDGE_LOOP('',(#70649,#70650,#70651,#70652));
#28294=EDGE_LOOP('',(#70653,#70654,#70655,#70656));
#28295=EDGE_LOOP('',(#70657,#70658,#70659,#70660));
#28296=EDGE_LOOP('',(#70661,#70662,#70663,#70664));
#28297=EDGE_LOOP('',(#70665,#70666,#70667,#70668));
#28298=EDGE_LOOP('',(#70669,#70670,#70671,#70672));
#28299=EDGE_LOOP('',(#70673,#70674,#70675,#70676));
#28300=EDGE_LOOP('',(#70677,#70678,#70679,#70680));
#28301=EDGE_LOOP('',(#70681,#70682,#70683,#70684));
#28302=EDGE_LOOP('',(#70685,#70686,#70687,#70688));
#28303=EDGE_LOOP('',(#70689,#70690,#70691,#70692));
#28304=EDGE_LOOP('',(#70693,#70694,#70695,#70696));
#28305=EDGE_LOOP('',(#70697,#70698,#70699,#70700));
#28306=EDGE_LOOP('',(#70701,#70702,#70703,#70704));
#28307=EDGE_LOOP('',(#70705,#70706,#70707,#70708));
#28308=EDGE_LOOP('',(#70709,#70710,#70711,#70712));
#28309=EDGE_LOOP('',(#70713,#70714,#70715,#70716));
#28310=EDGE_LOOP('',(#70717,#70718,#70719,#70720));
#28311=EDGE_LOOP('',(#70721,#70722,#70723,#70724));
#28312=EDGE_LOOP('',(#70725,#70726,#70727,#70728));
#28313=EDGE_LOOP('',(#70729,#70730,#70731,#70732));
#28314=EDGE_LOOP('',(#70733,#70734,#70735,#70736));
#28315=EDGE_LOOP('',(#70737,#70738,#70739,#70740));
#28316=EDGE_LOOP('',(#70741,#70742,#70743,#70744));
#28317=EDGE_LOOP('',(#70745,#70746,#70747,#70748));
#28318=EDGE_LOOP('',(#70749,#70750,#70751,#70752));
#28319=EDGE_LOOP('',(#70753,#70754,#70755,#70756));
#28320=EDGE_LOOP('',(#70757,#70758,#70759,#70760));
#28321=EDGE_LOOP('',(#70761,#70762,#70763,#70764));
#28322=EDGE_LOOP('',(#70765,#70766,#70767,#70768));
#28323=EDGE_LOOP('',(#70769,#70770,#70771,#70772));
#28324=EDGE_LOOP('',(#70773,#70774,#70775,#70776));
#28325=EDGE_LOOP('',(#70777,#70778,#70779,#70780));
#28326=EDGE_LOOP('',(#70781,#70782,#70783,#70784));
#28327=EDGE_LOOP('',(#70785,#70786,#70787,#70788));
#28328=EDGE_LOOP('',(#70789,#70790,#70791,#70792));
#28329=EDGE_LOOP('',(#70793,#70794,#70795,#70796));
#28330=EDGE_LOOP('',(#70797,#70798,#70799,#70800));
#28331=EDGE_LOOP('',(#70801,#70802,#70803,#70804));
#28332=EDGE_LOOP('',(#70805,#70806,#70807,#70808));
#28333=EDGE_LOOP('',(#70809,#70810,#70811,#70812));
#28334=EDGE_LOOP('',(#70813,#70814,#70815,#70816));
#28335=EDGE_LOOP('',(#70817,#70818,#70819,#70820));
#28336=EDGE_LOOP('',(#70821,#70822,#70823,#70824));
#28337=EDGE_LOOP('',(#70825,#70826,#70827,#70828));
#28338=EDGE_LOOP('',(#70829,#70830,#70831,#70832));
#28339=EDGE_LOOP('',(#70833,#70834,#70835,#70836));
#28340=EDGE_LOOP('',(#70837,#70838,#70839,#70840));
#28341=EDGE_LOOP('',(#70841,#70842,#70843,#70844));
#28342=EDGE_LOOP('',(#70845,#70846,#70847,#70848));
#28343=EDGE_LOOP('',(#70849,#70850,#70851,#70852));
#28344=EDGE_LOOP('',(#70853,#70854,#70855,#70856));
#28345=EDGE_LOOP('',(#70857,#70858,#70859,#70860));
#28346=EDGE_LOOP('',(#70861,#70862,#70863,#70864));
#28347=EDGE_LOOP('',(#70865,#70866,#70867,#70868));
#28348=EDGE_LOOP('',(#70869,#70870,#70871,#70872));
#28349=EDGE_LOOP('',(#70873,#70874,#70875,#70876));
#28350=EDGE_LOOP('',(#70877,#70878,#70879,#70880));
#28351=EDGE_LOOP('',(#70881,#70882,#70883,#70884));
#28352=EDGE_LOOP('',(#70885,#70886,#70887,#70888));
#28353=EDGE_LOOP('',(#70889,#70890,#70891,#70892));
#28354=EDGE_LOOP('',(#70893,#70894,#70895,#70896));
#28355=EDGE_LOOP('',(#70897,#70898,#70899,#70900));
#28356=EDGE_LOOP('',(#70901,#70902,#70903,#70904));
#28357=EDGE_LOOP('',(#70905,#70906,#70907,#70908));
#28358=EDGE_LOOP('',(#70909,#70910,#70911,#70912));
#28359=EDGE_LOOP('',(#70913,#70914,#70915,#70916));
#28360=EDGE_LOOP('',(#70917,#70918,#70919,#70920));
#28361=EDGE_LOOP('',(#70921,#70922,#70923,#70924));
#28362=EDGE_LOOP('',(#70925,#70926,#70927,#70928));
#28363=EDGE_LOOP('',(#70929,#70930,#70931,#70932));
#28364=EDGE_LOOP('',(#70933,#70934,#70935,#70936));
#28365=EDGE_LOOP('',(#70937,#70938,#70939,#70940));
#28366=EDGE_LOOP('',(#70941,#70942,#70943,#70944));
#28367=EDGE_LOOP('',(#70945,#70946,#70947,#70948));
#28368=EDGE_LOOP('',(#70949,#70950,#70951,#70952));
#28369=EDGE_LOOP('',(#70953,#70954,#70955,#70956));
#28370=EDGE_LOOP('',(#70957,#70958,#70959,#70960));
#28371=EDGE_LOOP('',(#70961,#70962,#70963,#70964));
#28372=EDGE_LOOP('',(#70965,#70966,#70967,#70968));
#28373=EDGE_LOOP('',(#70969,#70970,#70971,#70972));
#28374=EDGE_LOOP('',(#70973,#70974,#70975,#70976));
#28375=EDGE_LOOP('',(#70977,#70978,#70979,#70980));
#28376=EDGE_LOOP('',(#70981,#70982,#70983,#70984));
#28377=EDGE_LOOP('',(#70985,#70986,#70987,#70988));
#28378=EDGE_LOOP('',(#70989,#70990,#70991,#70992));
#28379=EDGE_LOOP('',(#70993,#70994,#70995,#70996));
#28380=EDGE_LOOP('',(#70997,#70998,#70999,#71000));
#28381=EDGE_LOOP('',(#71001,#71002,#71003,#71004));
#28382=EDGE_LOOP('',(#71005,#71006,#71007,#71008));
#28383=EDGE_LOOP('',(#71009,#71010,#71011,#71012));
#28384=EDGE_LOOP('',(#71013,#71014,#71015,#71016));
#28385=EDGE_LOOP('',(#71017,#71018,#71019,#71020));
#28386=EDGE_LOOP('',(#71021,#71022,#71023,#71024));
#28387=EDGE_LOOP('',(#71025,#71026,#71027,#71028));
#28388=EDGE_LOOP('',(#71029,#71030,#71031,#71032));
#28389=EDGE_LOOP('',(#71033,#71034,#71035,#71036));
#28390=EDGE_LOOP('',(#71037,#71038,#71039,#71040));
#28391=EDGE_LOOP('',(#71041,#71042,#71043,#71044));
#28392=EDGE_LOOP('',(#71045,#71046,#71047,#71048));
#28393=EDGE_LOOP('',(#71049,#71050,#71051,#71052));
#28394=EDGE_LOOP('',(#71053,#71054,#71055,#71056));
#28395=EDGE_LOOP('',(#71057,#71058,#71059,#71060));
#28396=EDGE_LOOP('',(#71061,#71062,#71063,#71064));
#28397=EDGE_LOOP('',(#71065,#71066,#71067,#71068));
#28398=EDGE_LOOP('',(#71069,#71070,#71071,#71072));
#28399=EDGE_LOOP('',(#71073,#71074,#71075,#71076));
#28400=EDGE_LOOP('',(#71077,#71078,#71079,#71080));
#28401=EDGE_LOOP('',(#71081,#71082,#71083,#71084));
#28402=EDGE_LOOP('',(#71085,#71086,#71087,#71088));
#28403=EDGE_LOOP('',(#71089,#71090,#71091,#71092));
#28404=EDGE_LOOP('',(#71093,#71094,#71095,#71096));
#28405=EDGE_LOOP('',(#71097,#71098,#71099,#71100));
#28406=EDGE_LOOP('',(#71101,#71102,#71103,#71104));
#28407=EDGE_LOOP('',(#71105,#71106,#71107,#71108));
#28408=EDGE_LOOP('',(#71109,#71110,#71111,#71112));
#28409=EDGE_LOOP('',(#71113,#71114,#71115,#71116));
#28410=EDGE_LOOP('',(#71117,#71118,#71119,#71120));
#28411=EDGE_LOOP('',(#71121,#71122,#71123,#71124));
#28412=EDGE_LOOP('',(#71125,#71126,#71127,#71128));
#28413=EDGE_LOOP('',(#71129,#71130,#71131,#71132));
#28414=EDGE_LOOP('',(#71133,#71134,#71135,#71136));
#28415=EDGE_LOOP('',(#71137,#71138,#71139,#71140));
#28416=EDGE_LOOP('',(#71141,#71142,#71143,#71144));
#28417=EDGE_LOOP('',(#71145,#71146,#71147,#71148));
#28418=EDGE_LOOP('',(#71149,#71150,#71151,#71152));
#28419=EDGE_LOOP('',(#71153,#71154,#71155,#71156));
#28420=EDGE_LOOP('',(#71157,#71158,#71159,#71160));
#28421=EDGE_LOOP('',(#71161,#71162,#71163,#71164));
#28422=EDGE_LOOP('',(#71165,#71166,#71167,#71168));
#28423=EDGE_LOOP('',(#71169,#71170,#71171,#71172));
#28424=EDGE_LOOP('',(#71173,#71174,#71175,#71176));
#28425=EDGE_LOOP('',(#71177,#71178,#71179,#71180));
#28426=EDGE_LOOP('',(#71181,#71182,#71183,#71184));
#28427=EDGE_LOOP('',(#71185,#71186,#71187,#71188));
#28428=EDGE_LOOP('',(#71189,#71190,#71191,#71192));
#28429=EDGE_LOOP('',(#71193,#71194,#71195,#71196));
#28430=EDGE_LOOP('',(#71197,#71198,#71199,#71200));
#28431=EDGE_LOOP('',(#71201,#71202,#71203,#71204));
#28432=EDGE_LOOP('',(#71205,#71206,#71207,#71208));
#28433=EDGE_LOOP('',(#71209,#71210,#71211,#71212));
#28434=EDGE_LOOP('',(#71213,#71214,#71215,#71216));
#28435=EDGE_LOOP('',(#71217,#71218,#71219,#71220));
#28436=EDGE_LOOP('',(#71221,#71222,#71223,#71224));
#28437=EDGE_LOOP('',(#71225,#71226,#71227,#71228));
#28438=EDGE_LOOP('',(#71229,#71230,#71231,#71232));
#28439=EDGE_LOOP('',(#71233,#71234,#71235,#71236));
#28440=EDGE_LOOP('',(#71237,#71238,#71239,#71240));
#28441=EDGE_LOOP('',(#71241,#71242,#71243,#71244));
#28442=EDGE_LOOP('',(#71245,#71246,#71247,#71248));
#28443=EDGE_LOOP('',(#71249,#71250,#71251,#71252));
#28444=EDGE_LOOP('',(#71253,#71254,#71255,#71256));
#28445=EDGE_LOOP('',(#71257,#71258,#71259,#71260));
#28446=EDGE_LOOP('',(#71261,#71262,#71263,#71264));
#28447=EDGE_LOOP('',(#71265,#71266,#71267,#71268));
#28448=EDGE_LOOP('',(#71269,#71270,#71271,#71272));
#28449=EDGE_LOOP('',(#71273,#71274,#71275,#71276));
#28450=EDGE_LOOP('',(#71277,#71278,#71279,#71280));
#28451=EDGE_LOOP('',(#71281,#71282,#71283,#71284));
#28452=EDGE_LOOP('',(#71285,#71286,#71287,#71288));
#28453=EDGE_LOOP('',(#71289,#71290,#71291,#71292));
#28454=EDGE_LOOP('',(#71293,#71294,#71295,#71296));
#28455=EDGE_LOOP('',(#71297,#71298,#71299,#71300));
#28456=EDGE_LOOP('',(#71301,#71302,#71303,#71304));
#28457=EDGE_LOOP('',(#71305,#71306,#71307,#71308));
#28458=EDGE_LOOP('',(#71309,#71310,#71311,#71312));
#28459=EDGE_LOOP('',(#71313,#71314,#71315,#71316));
#28460=EDGE_LOOP('',(#71317,#71318,#71319,#71320));
#28461=EDGE_LOOP('',(#71321,#71322,#71323,#71324));
#28462=EDGE_LOOP('',(#71325,#71326,#71327,#71328));
#28463=EDGE_LOOP('',(#71329,#71330,#71331,#71332));
#28464=EDGE_LOOP('',(#71333,#71334,#71335,#71336));
#28465=EDGE_LOOP('',(#71337,#71338,#71339,#71340));
#28466=EDGE_LOOP('',(#71341,#71342,#71343,#71344));
#28467=EDGE_LOOP('',(#71345,#71346,#71347,#71348));
#28468=EDGE_LOOP('',(#71349,#71350,#71351,#71352));
#28469=EDGE_LOOP('',(#71353,#71354,#71355,#71356));
#28470=EDGE_LOOP('',(#71357,#71358,#71359,#71360));
#28471=EDGE_LOOP('',(#71361,#71362,#71363,#71364));
#28472=EDGE_LOOP('',(#71365,#71366,#71367,#71368));
#28473=EDGE_LOOP('',(#71369,#71370,#71371,#71372));
#28474=EDGE_LOOP('',(#71373,#71374,#71375,#71376));
#28475=EDGE_LOOP('',(#71377,#71378,#71379,#71380));
#28476=EDGE_LOOP('',(#71381,#71382,#71383,#71384));
#28477=EDGE_LOOP('',(#71385,#71386,#71387,#71388));
#28478=EDGE_LOOP('',(#71389,#71390,#71391,#71392));
#28479=EDGE_LOOP('',(#71393,#71394,#71395,#71396));
#28480=EDGE_LOOP('',(#71397,#71398,#71399,#71400));
#28481=EDGE_LOOP('',(#71401,#71402,#71403,#71404));
#28482=EDGE_LOOP('',(#71405,#71406,#71407,#71408));
#28483=EDGE_LOOP('',(#71409,#71410,#71411,#71412));
#28484=EDGE_LOOP('',(#71413,#71414,#71415,#71416));
#28485=EDGE_LOOP('',(#71417,#71418,#71419,#71420));
#28486=EDGE_LOOP('',(#71421,#71422,#71423,#71424));
#28487=EDGE_LOOP('',(#71425,#71426,#71427,#71428));
#28488=EDGE_LOOP('',(#71429,#71430,#71431,#71432));
#28489=EDGE_LOOP('',(#71433,#71434,#71435,#71436));
#28490=EDGE_LOOP('',(#71437,#71438,#71439,#71440));
#28491=EDGE_LOOP('',(#71441,#71442,#71443,#71444));
#28492=EDGE_LOOP('',(#71445,#71446,#71447,#71448));
#28493=EDGE_LOOP('',(#71449,#71450,#71451,#71452));
#28494=EDGE_LOOP('',(#71453,#71454,#71455,#71456));
#28495=EDGE_LOOP('',(#71457,#71458,#71459,#71460));
#28496=EDGE_LOOP('',(#71461,#71462,#71463,#71464));
#28497=EDGE_LOOP('',(#71465,#71466,#71467,#71468));
#28498=EDGE_LOOP('',(#71469,#71470,#71471,#71472));
#28499=EDGE_LOOP('',(#71473,#71474,#71475,#71476));
#28500=EDGE_LOOP('',(#71477,#71478,#71479,#71480));
#28501=EDGE_LOOP('',(#71481,#71482,#71483,#71484));
#28502=EDGE_LOOP('',(#71485,#71486,#71487,#71488));
#28503=EDGE_LOOP('',(#71489,#71490,#71491,#71492));
#28504=EDGE_LOOP('',(#71493,#71494,#71495,#71496));
#28505=EDGE_LOOP('',(#71497,#71498,#71499,#71500));
#28506=EDGE_LOOP('',(#71501,#71502,#71503,#71504));
#28507=EDGE_LOOP('',(#71505,#71506,#71507,#71508));
#28508=EDGE_LOOP('',(#71509,#71510,#71511,#71512));
#28509=EDGE_LOOP('',(#71513,#71514,#71515,#71516));
#28510=EDGE_LOOP('',(#71517,#71518,#71519,#71520));
#28511=EDGE_LOOP('',(#71521,#71522,#71523,#71524));
#28512=EDGE_LOOP('',(#71525,#71526,#71527,#71528));
#28513=EDGE_LOOP('',(#71529,#71530,#71531,#71532));
#28514=EDGE_LOOP('',(#71533,#71534,#71535,#71536));
#28515=EDGE_LOOP('',(#71537,#71538,#71539,#71540));
#28516=EDGE_LOOP('',(#71541,#71542,#71543,#71544));
#28517=EDGE_LOOP('',(#71545,#71546,#71547,#71548));
#28518=EDGE_LOOP('',(#71549,#71550,#71551,#71552));
#28519=EDGE_LOOP('',(#71553,#71554,#71555,#71556));
#28520=EDGE_LOOP('',(#71557,#71558,#71559,#71560));
#28521=EDGE_LOOP('',(#71561,#71562,#71563,#71564));
#28522=EDGE_LOOP('',(#71565,#71566,#71567,#71568));
#28523=EDGE_LOOP('',(#71569,#71570,#71571,#71572));
#28524=EDGE_LOOP('',(#71573,#71574,#71575,#71576));
#28525=EDGE_LOOP('',(#71577,#71578,#71579,#71580));
#28526=EDGE_LOOP('',(#71581,#71582,#71583,#71584));
#28527=EDGE_LOOP('',(#71585,#71586,#71587,#71588));
#28528=EDGE_LOOP('',(#71589,#71590,#71591,#71592));
#28529=EDGE_LOOP('',(#71593,#71594,#71595,#71596));
#28530=EDGE_LOOP('',(#71597,#71598,#71599,#71600));
#28531=EDGE_LOOP('',(#71601,#71602,#71603,#71604));
#28532=EDGE_LOOP('',(#71605,#71606,#71607,#71608));
#28533=EDGE_LOOP('',(#71609,#71610,#71611,#71612));
#28534=EDGE_LOOP('',(#71613,#71614,#71615,#71616));
#28535=EDGE_LOOP('',(#71617,#71618,#71619,#71620));
#28536=EDGE_LOOP('',(#71621,#71622,#71623,#71624));
#28537=EDGE_LOOP('',(#71625,#71626,#71627,#71628));
#28538=EDGE_LOOP('',(#71629,#71630,#71631,#71632));
#28539=EDGE_LOOP('',(#71633,#71634,#71635,#71636));
#28540=EDGE_LOOP('',(#71637,#71638,#71639,#71640));
#28541=EDGE_LOOP('',(#71641,#71642,#71643,#71644));
#28542=EDGE_LOOP('',(#71645,#71646,#71647,#71648));
#28543=EDGE_LOOP('',(#71649,#71650,#71651,#71652));
#28544=EDGE_LOOP('',(#71653,#71654,#71655,#71656));
#28545=EDGE_LOOP('',(#71657,#71658,#71659,#71660));
#28546=EDGE_LOOP('',(#71661,#71662,#71663,#71664));
#28547=EDGE_LOOP('',(#71665,#71666,#71667,#71668));
#28548=EDGE_LOOP('',(#71669,#71670,#71671,#71672));
#28549=EDGE_LOOP('',(#71673,#71674,#71675,#71676));
#28550=EDGE_LOOP('',(#71677,#71678,#71679,#71680));
#28551=EDGE_LOOP('',(#71681,#71682,#71683,#71684));
#28552=EDGE_LOOP('',(#71685,#71686,#71687,#71688));
#28553=EDGE_LOOP('',(#71689,#71690,#71691,#71692));
#28554=EDGE_LOOP('',(#71693,#71694,#71695,#71696));
#28555=EDGE_LOOP('',(#71697,#71698,#71699,#71700));
#28556=EDGE_LOOP('',(#71701,#71702,#71703,#71704));
#28557=EDGE_LOOP('',(#71705,#71706,#71707,#71708));
#28558=EDGE_LOOP('',(#71709,#71710,#71711,#71712));
#28559=EDGE_LOOP('',(#71713,#71714,#71715,#71716));
#28560=EDGE_LOOP('',(#71717,#71718,#71719,#71720));
#28561=EDGE_LOOP('',(#71721,#71722,#71723,#71724));
#28562=EDGE_LOOP('',(#71725,#71726,#71727,#71728));
#28563=EDGE_LOOP('',(#71729,#71730,#71731,#71732));
#28564=EDGE_LOOP('',(#71733,#71734,#71735,#71736));
#28565=EDGE_LOOP('',(#71737,#71738,#71739,#71740));
#28566=EDGE_LOOP('',(#71741,#71742,#71743,#71744));
#28567=EDGE_LOOP('',(#71745,#71746,#71747,#71748));
#28568=EDGE_LOOP('',(#71749,#71750,#71751,#71752));
#28569=EDGE_LOOP('',(#71753,#71754,#71755,#71756));
#28570=EDGE_LOOP('',(#71757,#71758,#71759,#71760));
#28571=EDGE_LOOP('',(#71761,#71762,#71763,#71764));
#28572=EDGE_LOOP('',(#71765,#71766,#71767,#71768));
#28573=EDGE_LOOP('',(#71769,#71770,#71771,#71772));
#28574=EDGE_LOOP('',(#71773,#71774,#71775,#71776));
#28575=EDGE_LOOP('',(#71777,#71778,#71779,#71780));
#28576=EDGE_LOOP('',(#71781,#71782,#71783,#71784));
#28577=EDGE_LOOP('',(#71785,#71786,#71787,#71788));
#28578=EDGE_LOOP('',(#71789,#71790,#71791,#71792));
#28579=EDGE_LOOP('',(#71793,#71794,#71795,#71796));
#28580=EDGE_LOOP('',(#71797,#71798,#71799,#71800));
#28581=EDGE_LOOP('',(#71801,#71802,#71803,#71804));
#28582=EDGE_LOOP('',(#71805,#71806,#71807,#71808));
#28583=EDGE_LOOP('',(#71809,#71810,#71811,#71812));
#28584=EDGE_LOOP('',(#71813,#71814,#71815,#71816));
#28585=EDGE_LOOP('',(#71817,#71818,#71819,#71820));
#28586=EDGE_LOOP('',(#71821,#71822,#71823,#71824));
#28587=EDGE_LOOP('',(#71825,#71826,#71827,#71828));
#28588=EDGE_LOOP('',(#71829,#71830,#71831,#71832));
#28589=EDGE_LOOP('',(#71833,#71834,#71835,#71836));
#28590=EDGE_LOOP('',(#71837,#71838,#71839,#71840));
#28591=EDGE_LOOP('',(#71841,#71842,#71843,#71844));
#28592=EDGE_LOOP('',(#71845,#71846,#71847,#71848));
#28593=EDGE_LOOP('',(#71849,#71850,#71851,#71852));
#28594=EDGE_LOOP('',(#71853,#71854,#71855,#71856));
#28595=EDGE_LOOP('',(#71857,#71858,#71859,#71860));
#28596=EDGE_LOOP('',(#71861,#71862,#71863,#71864));
#28597=EDGE_LOOP('',(#71865,#71866,#71867,#71868));
#28598=EDGE_LOOP('',(#71869,#71870,#71871,#71872));
#28599=EDGE_LOOP('',(#71873,#71874,#71875,#71876));
#28600=EDGE_LOOP('',(#71877,#71878,#71879,#71880));
#28601=EDGE_LOOP('',(#71881,#71882,#71883,#71884));
#28602=EDGE_LOOP('',(#71885,#71886,#71887,#71888));
#28603=EDGE_LOOP('',(#71889,#71890,#71891,#71892));
#28604=EDGE_LOOP('',(#71893,#71894,#71895,#71896));
#28605=EDGE_LOOP('',(#71897,#71898,#71899,#71900));
#28606=EDGE_LOOP('',(#71901,#71902,#71903,#71904));
#28607=EDGE_LOOP('',(#71905,#71906,#71907,#71908));
#28608=EDGE_LOOP('',(#71909,#71910,#71911,#71912));
#28609=EDGE_LOOP('',(#71913,#71914,#71915,#71916));
#28610=EDGE_LOOP('',(#71917,#71918,#71919,#71920));
#28611=EDGE_LOOP('',(#71921,#71922,#71923,#71924));
#28612=EDGE_LOOP('',(#71925,#71926,#71927,#71928));
#28613=EDGE_LOOP('',(#71929,#71930,#71931,#71932));
#28614=EDGE_LOOP('',(#71933,#71934,#71935,#71936));
#28615=EDGE_LOOP('',(#71937,#71938,#71939,#71940));
#28616=EDGE_LOOP('',(#71941,#71942,#71943,#71944));
#28617=EDGE_LOOP('',(#71945,#71946,#71947,#71948));
#28618=EDGE_LOOP('',(#71949,#71950,#71951,#71952));
#28619=EDGE_LOOP('',(#71953,#71954,#71955,#71956));
#28620=EDGE_LOOP('',(#71957,#71958,#71959,#71960));
#28621=EDGE_LOOP('',(#71961,#71962,#71963,#71964));
#28622=EDGE_LOOP('',(#71965,#71966,#71967,#71968));
#28623=EDGE_LOOP('',(#71969,#71970,#71971,#71972));
#28624=EDGE_LOOP('',(#71973,#71974,#71975,#71976));
#28625=EDGE_LOOP('',(#71977,#71978,#71979,#71980));
#28626=EDGE_LOOP('',(#71981,#71982,#71983,#71984));
#28627=EDGE_LOOP('',(#71985,#71986,#71987,#71988));
#28628=EDGE_LOOP('',(#71989,#71990,#71991,#71992));
#28629=EDGE_LOOP('',(#71993,#71994,#71995,#71996));
#28630=EDGE_LOOP('',(#71997,#71998,#71999,#72000));
#28631=EDGE_LOOP('',(#72001,#72002,#72003,#72004));
#28632=EDGE_LOOP('',(#72005,#72006,#72007,#72008));
#28633=EDGE_LOOP('',(#72009,#72010,#72011,#72012));
#28634=EDGE_LOOP('',(#72013,#72014,#72015,#72016));
#28635=EDGE_LOOP('',(#72017,#72018,#72019,#72020));
#28636=EDGE_LOOP('',(#72021,#72022,#72023,#72024));
#28637=EDGE_LOOP('',(#72025,#72026,#72027,#72028));
#28638=EDGE_LOOP('',(#72029,#72030,#72031,#72032));
#28639=EDGE_LOOP('',(#72033,#72034,#72035,#72036));
#28640=EDGE_LOOP('',(#72037,#72038,#72039,#72040));
#28641=EDGE_LOOP('',(#72041,#72042,#72043,#72044));
#28642=EDGE_LOOP('',(#72045,#72046,#72047,#72048));
#28643=EDGE_LOOP('',(#72049,#72050,#72051,#72052));
#28644=EDGE_LOOP('',(#72053,#72054,#72055,#72056));
#28645=EDGE_LOOP('',(#72057,#72058,#72059,#72060));
#28646=EDGE_LOOP('',(#72061,#72062,#72063,#72064));
#28647=EDGE_LOOP('',(#72065,#72066,#72067,#72068));
#28648=EDGE_LOOP('',(#72069,#72070,#72071,#72072));
#28649=EDGE_LOOP('',(#72073,#72074,#72075,#72076));
#28650=EDGE_LOOP('',(#72077,#72078,#72079,#72080));
#28651=EDGE_LOOP('',(#72081,#72082,#72083,#72084));
#28652=EDGE_LOOP('',(#72085,#72086,#72087,#72088));
#28653=EDGE_LOOP('',(#72089,#72090,#72091,#72092));
#28654=EDGE_LOOP('',(#72093,#72094,#72095,#72096));
#28655=EDGE_LOOP('',(#72097,#72098,#72099,#72100));
#28656=EDGE_LOOP('',(#72101,#72102,#72103,#72104));
#28657=EDGE_LOOP('',(#72105,#72106,#72107,#72108));
#28658=EDGE_LOOP('',(#72109,#72110,#72111,#72112));
#28659=EDGE_LOOP('',(#72113,#72114,#72115,#72116));
#28660=EDGE_LOOP('',(#72117,#72118,#72119,#72120));
#28661=EDGE_LOOP('',(#72121,#72122,#72123,#72124));
#28662=EDGE_LOOP('',(#72125,#72126,#72127,#72128));
#28663=EDGE_LOOP('',(#72129,#72130,#72131,#72132));
#28664=EDGE_LOOP('',(#72133,#72134,#72135,#72136));
#28665=EDGE_LOOP('',(#72137,#72138,#72139,#72140));
#28666=EDGE_LOOP('',(#72141,#72142,#72143,#72144));
#28667=EDGE_LOOP('',(#72145,#72146,#72147,#72148));
#28668=EDGE_LOOP('',(#72149,#72150,#72151,#72152));
#28669=EDGE_LOOP('',(#72153,#72154,#72155,#72156));
#28670=EDGE_LOOP('',(#72157,#72158,#72159,#72160));
#28671=EDGE_LOOP('',(#72161,#72162,#72163,#72164));
#28672=EDGE_LOOP('',(#72165,#72166,#72167,#72168));
#28673=EDGE_LOOP('',(#72169,#72170,#72171,#72172));
#28674=EDGE_LOOP('',(#72173,#72174,#72175,#72176));
#28675=EDGE_LOOP('',(#72177,#72178,#72179,#72180));
#28676=EDGE_LOOP('',(#72181,#72182,#72183,#72184));
#28677=EDGE_LOOP('',(#72185,#72186,#72187,#72188));
#28678=EDGE_LOOP('',(#72189,#72190,#72191,#72192));
#28679=EDGE_LOOP('',(#72193,#72194,#72195,#72196));
#28680=EDGE_LOOP('',(#72197,#72198,#72199,#72200));
#28681=EDGE_LOOP('',(#72201,#72202,#72203,#72204));
#28682=EDGE_LOOP('',(#72205,#72206,#72207,#72208));
#28683=EDGE_LOOP('',(#72209));
#28684=EDGE_LOOP('',(#72210));
#28685=EDGE_LOOP('',(#72211,#72212,#72213,#72214));
#28686=EDGE_LOOP('',(#72215,#72216,#72217,#72218));
#28687=EDGE_LOOP('',(#72219,#72220,#72221,#72222));
#28688=EDGE_LOOP('',(#72223,#72224,#72225,#72226));
#28689=EDGE_LOOP('',(#72227,#72228,#72229,#72230));
#28690=EDGE_LOOP('',(#72231,#72232,#72233,#72234));
#28691=EDGE_LOOP('',(#72235,#72236,#72237,#72238));
#28692=EDGE_LOOP('',(#72239,#72240,#72241,#72242,#72243,#72244));
#28693=EDGE_LOOP('',(#72245,#72246,#72247,#72248));
#28694=EDGE_LOOP('',(#72249,#72250,#72251,#72252,#72253,#72254));
#28695=EDGE_LOOP('',(#72255,#72256,#72257,#72258));
#28696=EDGE_LOOP('',(#72259,#72260,#72261,#72262));
#28697=EDGE_LOOP('',(#72263));
#28698=EDGE_LOOP('',(#72264));
#28699=EDGE_LOOP('',(#72265));
#28700=EDGE_LOOP('',(#72266,#72267,#72268,#72269));
#28701=EDGE_LOOP('',(#72270,#72271,#72272,#72273));
#28702=EDGE_LOOP('',(#72274,#72275,#72276,#72277));
#28703=EDGE_LOOP('',(#72278,#72279,#72280,#72281));
#28704=EDGE_LOOP('',(#72282,#72283,#72284,#72285));
#28705=EDGE_LOOP('',(#72286,#72287,#72288,#72289));
#28706=EDGE_LOOP('',(#72290,#72291,#72292,#72293));
#28707=EDGE_LOOP('',(#72294,#72295,#72296,#72297));
#28708=EDGE_LOOP('',(#72298,#72299,#72300,#72301));
#28709=EDGE_LOOP('',(#72302,#72303,#72304,#72305));
#28710=EDGE_LOOP('',(#72306,#72307,#72308,#72309));
#28711=EDGE_LOOP('',(#72310,#72311,#72312,#72313));
#28712=EDGE_LOOP('',(#72314,#72315,#72316,#72317));
#28713=EDGE_LOOP('',(#72318,#72319,#72320,#72321));
#28714=EDGE_LOOP('',(#72322,#72323,#72324,#72325));
#28715=EDGE_LOOP('',(#72326,#72327,#72328,#72329));
#28716=EDGE_LOOP('',(#72330,#72331,#72332,#72333));
#28717=EDGE_LOOP('',(#72334,#72335,#72336,#72337));
#28718=EDGE_LOOP('',(#72338,#72339,#72340,#72341));
#28719=EDGE_LOOP('',(#72342,#72343,#72344,#72345));
#28720=EDGE_LOOP('',(#72346,#72347,#72348,#72349));
#28721=EDGE_LOOP('',(#72350,#72351,#72352,#72353));
#28722=EDGE_LOOP('',(#72354,#72355,#72356,#72357));
#28723=EDGE_LOOP('',(#72358,#72359,#72360,#72361));
#28724=EDGE_LOOP('',(#72362,#72363,#72364,#72365));
#28725=EDGE_LOOP('',(#72366,#72367,#72368,#72369));
#28726=EDGE_LOOP('',(#72370,#72371,#72372,#72373));
#28727=EDGE_LOOP('',(#72374,#72375,#72376,#72377));
#28728=EDGE_LOOP('',(#72378,#72379,#72380,#72381));
#28729=EDGE_LOOP('',(#72382,#72383,#72384,#72385));
#28730=EDGE_LOOP('',(#72386,#72387,#72388,#72389));
#28731=EDGE_LOOP('',(#72390,#72391,#72392,#72393));
#28732=EDGE_LOOP('',(#72394,#72395,#72396,#72397));
#28733=EDGE_LOOP('',(#72398,#72399,#72400,#72401));
#28734=EDGE_LOOP('',(#72402,#72403,#72404,#72405));
#28735=EDGE_LOOP('',(#72406,#72407,#72408,#72409));
#28736=EDGE_LOOP('',(#72410,#72411,#72412,#72413));
#28737=EDGE_LOOP('',(#72414,#72415,#72416,#72417));
#28738=EDGE_LOOP('',(#72418,#72419,#72420,#72421));
#28739=EDGE_LOOP('',(#72422,#72423,#72424,#72425));
#28740=EDGE_LOOP('',(#72426,#72427,#72428,#72429));
#28741=EDGE_LOOP('',(#72430,#72431,#72432,#72433));
#28742=EDGE_LOOP('',(#72434,#72435,#72436,#72437));
#28743=EDGE_LOOP('',(#72438,#72439,#72440,#72441));
#28744=EDGE_LOOP('',(#72442,#72443,#72444,#72445));
#28745=EDGE_LOOP('',(#72446,#72447,#72448,#72449));
#28746=EDGE_LOOP('',(#72450,#72451,#72452,#72453));
#28747=EDGE_LOOP('',(#72454,#72455,#72456,#72457));
#28748=EDGE_LOOP('',(#72458,#72459,#72460,#72461));
#28749=EDGE_LOOP('',(#72462,#72463,#72464,#72465));
#28750=EDGE_LOOP('',(#72466,#72467,#72468,#72469));
#28751=EDGE_LOOP('',(#72470,#72471,#72472,#72473));
#28752=EDGE_LOOP('',(#72474,#72475,#72476,#72477));
#28753=EDGE_LOOP('',(#72478,#72479,#72480,#72481));
#28754=EDGE_LOOP('',(#72482,#72483,#72484,#72485));
#28755=EDGE_LOOP('',(#72486,#72487,#72488,#72489));
#28756=EDGE_LOOP('',(#72490,#72491,#72492,#72493));
#28757=EDGE_LOOP('',(#72494,#72495,#72496,#72497));
#28758=EDGE_LOOP('',(#72498,#72499,#72500,#72501));
#28759=EDGE_LOOP('',(#72502,#72503,#72504,#72505));
#28760=EDGE_LOOP('',(#72506,#72507,#72508,#72509));
#28761=EDGE_LOOP('',(#72510,#72511,#72512,#72513));
#28762=EDGE_LOOP('',(#72514,#72515,#72516,#72517));
#28763=EDGE_LOOP('',(#72518,#72519,#72520,#72521));
#28764=EDGE_LOOP('',(#72522,#72523,#72524,#72525));
#28765=EDGE_LOOP('',(#72526,#72527,#72528,#72529));
#28766=EDGE_LOOP('',(#72530,#72531,#72532,#72533));
#28767=EDGE_LOOP('',(#72534,#72535,#72536,#72537));
#28768=EDGE_LOOP('',(#72538,#72539,#72540,#72541));
#28769=EDGE_LOOP('',(#72542,#72543,#72544,#72545));
#28770=EDGE_LOOP('',(#72546,#72547,#72548,#72549));
#28771=EDGE_LOOP('',(#72550,#72551,#72552,#72553,#72554));
#28772=EDGE_LOOP('',(#72555,#72556,#72557,#72558,#72559));
#28773=EDGE_LOOP('',(#72560,#72561,#72562,#72563));
#28774=EDGE_LOOP('',(#72564,#72565,#72566,#72567));
#28775=EDGE_LOOP('',(#72568,#72569,#72570,#72571));
#28776=EDGE_LOOP('',(#72572,#72573,#72574,#72575));
#28777=EDGE_LOOP('',(#72576,#72577,#72578,#72579));
#28778=EDGE_LOOP('',(#72580,#72581,#72582,#72583));
#28779=EDGE_LOOP('',(#72584,#72585,#72586,#72587));
#28780=EDGE_LOOP('',(#72588,#72589,#72590,#72591));
#28781=EDGE_LOOP('',(#72592,#72593,#72594,#72595));
#28782=EDGE_LOOP('',(#72596,#72597,#72598,#72599));
#28783=EDGE_LOOP('',(#72600,#72601,#72602,#72603,#72604));
#28784=EDGE_LOOP('',(#72605,#72606,#72607,#72608));
#28785=EDGE_LOOP('',(#72609,#72610,#72611,#72612));
#28786=EDGE_LOOP('',(#72613,#72614,#72615,#72616));
#28787=EDGE_LOOP('',(#72617,#72618,#72619,#72620));
#28788=EDGE_LOOP('',(#72621,#72622,#72623,#72624));
#28789=EDGE_LOOP('',(#72625,#72626,#72627,#72628));
#28790=EDGE_LOOP('',(#72629,#72630,#72631,#72632));
#28791=EDGE_LOOP('',(#72633,#72634,#72635,#72636));
#28792=EDGE_LOOP('',(#72637,#72638,#72639,#72640));
#28793=EDGE_LOOP('',(#72641,#72642,#72643,#72644));
#28794=EDGE_LOOP('',(#72645,#72646,#72647,#72648));
#28795=EDGE_LOOP('',(#72649,#72650,#72651,#72652));
#28796=EDGE_LOOP('',(#72653,#72654,#72655,#72656));
#28797=EDGE_LOOP('',(#72657,#72658,#72659,#72660));
#28798=EDGE_LOOP('',(#72661,#72662,#72663,#72664));
#28799=EDGE_LOOP('',(#72665,#72666,#72667,#72668));
#28800=EDGE_LOOP('',(#72669,#72670,#72671,#72672));
#28801=EDGE_LOOP('',(#72673,#72674,#72675,#72676));
#28802=EDGE_LOOP('',(#72677,#72678,#72679,#72680));
#28803=EDGE_LOOP('',(#72681,#72682,#72683,#72684));
#28804=EDGE_LOOP('',(#72685,#72686,#72687,#72688));
#28805=EDGE_LOOP('',(#72689,#72690,#72691,#72692,#72693));
#28806=EDGE_LOOP('',(#72694,#72695,#72696,#72697));
#28807=EDGE_LOOP('',(#72698,#72699,#72700,#72701));
#28808=EDGE_LOOP('',(#72702,#72703,#72704,#72705));
#28809=EDGE_LOOP('',(#72706,#72707,#72708,#72709));
#28810=EDGE_LOOP('',(#72710,#72711,#72712,#72713));
#28811=EDGE_LOOP('',(#72714,#72715,#72716,#72717));
#28812=EDGE_LOOP('',(#72718,#72719,#72720,#72721));
#28813=EDGE_LOOP('',(#72722,#72723,#72724,#72725));
#28814=EDGE_LOOP('',(#72726,#72727,#72728,#72729));
#28815=EDGE_LOOP('',(#72730,#72731,#72732,#72733));
#28816=EDGE_LOOP('',(#72734,#72735,#72736,#72737));
#28817=EDGE_LOOP('',(#72738,#72739,#72740,#72741,#72742));
#28818=EDGE_LOOP('',(#72743,#72744,#72745,#72746));
#28819=EDGE_LOOP('',(#72747,#72748,#72749,#72750));
#28820=EDGE_LOOP('',(#72751,#72752,#72753,#72754));
#28821=EDGE_LOOP('',(#72755,#72756,#72757,#72758));
#28822=EDGE_LOOP('',(#72759,#72760,#72761,#72762));
#28823=EDGE_LOOP('',(#72763,#72764,#72765,#72766));
#28824=EDGE_LOOP('',(#72767,#72768,#72769,#72770));
#28825=EDGE_LOOP('',(#72771,#72772,#72773));
#28826=EDGE_LOOP('',(#72774,#72775,#72776,#72777));
#28827=EDGE_LOOP('',(#72778,#72779,#72780,#72781));
#28828=EDGE_LOOP('',(#72782,#72783,#72784));
#28829=EDGE_LOOP('',(#72785,#72786,#72787,#72788));
#28830=EDGE_LOOP('',(#72789,#72790,#72791,#72792));
#28831=EDGE_LOOP('',(#72793,#72794,#72795,#72796));
#28832=EDGE_LOOP('',(#72797,#72798,#72799,#72800));
#28833=EDGE_LOOP('',(#72801,#72802,#72803));
#28834=EDGE_LOOP('',(#72804,#72805,#72806));
#28835=EDGE_LOOP('',(#72807,#72808,#72809,#72810));
#28836=EDGE_LOOP('',(#72811,#72812,#72813,#72814));
#28837=EDGE_LOOP('',(#72815,#72816,#72817,#72818));
#28838=EDGE_LOOP('',(#72819,#72820,#72821,#72822));
#28839=EDGE_LOOP('',(#72823,#72824,#72825,#72826));
#28840=EDGE_LOOP('',(#72827,#72828,#72829,#72830));
#28841=EDGE_LOOP('',(#72831,#72832,#72833,#72834));
#28842=EDGE_LOOP('',(#72835,#72836,#72837,#72838));
#28843=EDGE_LOOP('',(#72839,#72840,#72841,#72842));
#28844=EDGE_LOOP('',(#72843,#72844,#72845,#72846));
#28845=EDGE_LOOP('',(#72847,#72848,#72849,#72850));
#28846=EDGE_LOOP('',(#72851,#72852,#72853));
#28847=EDGE_LOOP('',(#72854,#72855,#72856));
#28848=EDGE_LOOP('',(#72857,#72858,#72859,#72860));
#28849=EDGE_LOOP('',(#72861,#72862,#72863,#72864));
#28850=EDGE_LOOP('',(#72865,#72866,#72867,#72868));
#28851=EDGE_LOOP('',(#72869,#72870,#72871,#72872));
#28852=EDGE_LOOP('',(#72873,#72874,#72875,#72876,#72877));
#28853=EDGE_LOOP('',(#72878,#72879,#72880,#72881));
#28854=EDGE_LOOP('',(#72882,#72883,#72884,#72885));
#28855=EDGE_LOOP('',(#72886,#72887,#72888,#72889,#72890));
#28856=EDGE_LOOP('',(#72891,#72892,#72893,#72894));
#28857=EDGE_LOOP('',(#72895,#72896,#72897,#72898));
#28858=EDGE_LOOP('',(#72899,#72900,#72901,#72902));
#28859=EDGE_LOOP('',(#72903,#72904,#72905,#72906));
#28860=EDGE_LOOP('',(#72907,#72908,#72909,#72910));
#28861=EDGE_LOOP('',(#72911,#72912,#72913,#72914));
#28862=EDGE_LOOP('',(#72915,#72916,#72917,#72918));
#28863=EDGE_LOOP('',(#72919,#72920,#72921,#72922));
#28864=EDGE_LOOP('',(#72923,#72924,#72925,#72926));
#28865=EDGE_LOOP('',(#72927,#72928,#72929,#72930));
#28866=EDGE_LOOP('',(#72931,#72932,#72933,#72934,#72935));
#28867=EDGE_LOOP('',(#72936,#72937,#72938,#72939,#72940));
#28868=EDGE_LOOP('',(#72941,#72942,#72943,#72944));
#28869=EDGE_LOOP('',(#72945,#72946,#72947,#72948));
#28870=EDGE_LOOP('',(#72949,#72950,#72951,#72952));
#28871=EDGE_LOOP('',(#72953,#72954,#72955,#72956));
#28872=EDGE_LOOP('',(#72957,#72958,#72959,#72960));
#28873=EDGE_LOOP('',(#72961,#72962,#72963,#72964));
#28874=EDGE_LOOP('',(#72965,#72966,#72967,#72968));
#28875=EDGE_LOOP('',(#72969,#72970,#72971,#72972));
#28876=EDGE_LOOP('',(#72973,#72974,#72975,#72976));
#28877=EDGE_LOOP('',(#72977,#72978,#72979,#72980));
#28878=EDGE_LOOP('',(#72981,#72982,#72983,#72984,#72985));
#28879=EDGE_LOOP('',(#72986,#72987,#72988,#72989));
#28880=EDGE_LOOP('',(#72990,#72991,#72992,#72993));
#28881=EDGE_LOOP('',(#72994,#72995,#72996,#72997));
#28882=EDGE_LOOP('',(#72998,#72999,#73000,#73001));
#28883=EDGE_LOOP('',(#73002,#73003,#73004,#73005));
#28884=EDGE_LOOP('',(#73006,#73007,#73008,#73009));
#28885=EDGE_LOOP('',(#73010,#73011,#73012,#73013));
#28886=EDGE_LOOP('',(#73014,#73015,#73016,#73017));
#28887=EDGE_LOOP('',(#73018,#73019,#73020,#73021));
#28888=EDGE_LOOP('',(#73022,#73023,#73024,#73025));
#28889=EDGE_LOOP('',(#73026,#73027,#73028,#73029));
#28890=EDGE_LOOP('',(#73030,#73031,#73032,#73033));
#28891=EDGE_LOOP('',(#73034,#73035,#73036,#73037));
#28892=EDGE_LOOP('',(#73038,#73039,#73040,#73041));
#28893=EDGE_LOOP('',(#73042,#73043,#73044,#73045));
#28894=EDGE_LOOP('',(#73046,#73047,#73048,#73049));
#28895=EDGE_LOOP('',(#73050,#73051,#73052,#73053));
#28896=EDGE_LOOP('',(#73054,#73055,#73056,#73057));
#28897=EDGE_LOOP('',(#73058,#73059,#73060,#73061));
#28898=EDGE_LOOP('',(#73062,#73063,#73064,#73065));
#28899=EDGE_LOOP('',(#73066,#73067,#73068,#73069));
#28900=EDGE_LOOP('',(#73070,#73071,#73072,#73073));
#28901=EDGE_LOOP('',(#73074,#73075,#73076,#73077));
#28902=EDGE_LOOP('',(#73078,#73079,#73080,#73081));
#28903=EDGE_LOOP('',(#73082,#73083,#73084,#73085));
#28904=EDGE_LOOP('',(#73086,#73087,#73088,#73089));
#28905=EDGE_LOOP('',(#73090,#73091,#73092,#73093));
#28906=EDGE_LOOP('',(#73094,#73095,#73096,#73097));
#28907=EDGE_LOOP('',(#73098,#73099,#73100,#73101));
#28908=EDGE_LOOP('',(#73102,#73103,#73104,#73105));
#28909=EDGE_LOOP('',(#73106,#73107,#73108,#73109));
#28910=EDGE_LOOP('',(#73110,#73111,#73112,#73113));
#28911=EDGE_LOOP('',(#73114,#73115,#73116,#73117));
#28912=EDGE_LOOP('',(#73118,#73119,#73120,#73121));
#28913=EDGE_LOOP('',(#73122,#73123,#73124,#73125));
#28914=EDGE_LOOP('',(#73126,#73127,#73128,#73129));
#28915=EDGE_LOOP('',(#73130,#73131,#73132,#73133));
#28916=EDGE_LOOP('',(#73134,#73135,#73136,#73137));
#28917=EDGE_LOOP('',(#73138,#73139,#73140,#73141));
#28918=EDGE_LOOP('',(#73142,#73143,#73144,#73145));
#28919=EDGE_LOOP('',(#73146,#73147,#73148,#73149));
#28920=EDGE_LOOP('',(#73150,#73151,#73152,#73153));
#28921=EDGE_LOOP('',(#73154,#73155,#73156,#73157));
#28922=EDGE_LOOP('',(#73158,#73159,#73160,#73161));
#28923=EDGE_LOOP('',(#73162,#73163,#73164,#73165));
#28924=EDGE_LOOP('',(#73166,#73167,#73168,#73169));
#28925=EDGE_LOOP('',(#73170,#73171,#73172,#73173));
#28926=EDGE_LOOP('',(#73174,#73175,#73176,#73177));
#28927=EDGE_LOOP('',(#73178,#73179,#73180,#73181));
#28928=EDGE_LOOP('',(#73182,#73183,#73184,#73185));
#28929=EDGE_LOOP('',(#73186,#73187,#73188,#73189));
#28930=EDGE_LOOP('',(#73190,#73191,#73192,#73193));
#28931=EDGE_LOOP('',(#73194,#73195,#73196,#73197));
#28932=EDGE_LOOP('',(#73198,#73199,#73200,#73201));
#28933=EDGE_LOOP('',(#73202,#73203,#73204,#73205));
#28934=EDGE_LOOP('',(#73206,#73207,#73208,#73209));
#28935=EDGE_LOOP('',(#73210,#73211,#73212,#73213));
#28936=EDGE_LOOP('',(#73214,#73215,#73216,#73217));
#28937=EDGE_LOOP('',(#73218,#73219,#73220,#73221));
#28938=EDGE_LOOP('',(#73222,#73223,#73224,#73225));
#28939=EDGE_LOOP('',(#73226,#73227,#73228,#73229));
#28940=EDGE_LOOP('',(#73230,#73231,#73232,#73233));
#28941=EDGE_LOOP('',(#73234,#73235,#73236,#73237));
#28942=EDGE_LOOP('',(#73238,#73239,#73240,#73241));
#28943=EDGE_LOOP('',(#73242,#73243,#73244,#73245));
#28944=EDGE_LOOP('',(#73246,#73247,#73248,#73249));
#28945=EDGE_LOOP('',(#73250,#73251,#73252,#73253));
#28946=EDGE_LOOP('',(#73254,#73255,#73256,#73257));
#28947=EDGE_LOOP('',(#73258,#73259,#73260,#73261));
#28948=EDGE_LOOP('',(#73262,#73263,#73264,#73265));
#28949=EDGE_LOOP('',(#73266,#73267,#73268,#73269));
#28950=EDGE_LOOP('',(#73270,#73271,#73272,#73273));
#28951=EDGE_LOOP('',(#73274,#73275,#73276,#73277));
#28952=EDGE_LOOP('',(#73278,#73279,#73280,#73281));
#28953=EDGE_LOOP('',(#73282,#73283,#73284,#73285));
#28954=EDGE_LOOP('',(#73286,#73287,#73288,#73289));
#28955=EDGE_LOOP('',(#73290,#73291,#73292,#73293));
#28956=EDGE_LOOP('',(#73294,#73295,#73296,#73297));
#28957=EDGE_LOOP('',(#73298,#73299,#73300,#73301));
#28958=EDGE_LOOP('',(#73302,#73303,#73304,#73305));
#28959=EDGE_LOOP('',(#73306,#73307,#73308,#73309));
#28960=EDGE_LOOP('',(#73310));
#28961=EDGE_LOOP('',(#73311,#73312,#73313,#73314));
#28962=EDGE_LOOP('',(#73315,#73316,#73317,#73318));
#28963=EDGE_LOOP('',(#73319,#73320,#73321,#73322));
#28964=EDGE_LOOP('',(#73323,#73324,#73325,#73326));
#28965=EDGE_LOOP('',(#73327,#73328,#73329,#73330));
#28966=EDGE_LOOP('',(#73331,#73332,#73333,#73334));
#28967=EDGE_LOOP('',(#73335,#73336,#73337,#73338));
#28968=EDGE_LOOP('',(#73339,#73340,#73341,#73342));
#28969=EDGE_LOOP('',(#73343,#73344,#73345,#73346));
#28970=EDGE_LOOP('',(#73347,#73348,#73349,#73350));
#28971=EDGE_LOOP('',(#73351,#73352,#73353,#73354));
#28972=EDGE_LOOP('',(#73355,#73356,#73357,#73358));
#28973=EDGE_LOOP('',(#73359,#73360,#73361,#73362));
#28974=EDGE_LOOP('',(#73363,#73364,#73365,#73366));
#28975=EDGE_LOOP('',(#73367,#73368,#73369,#73370));
#28976=EDGE_LOOP('',(#73371,#73372,#73373,#73374));
#28977=EDGE_LOOP('',(#73375,#73376,#73377,#73378));
#28978=EDGE_LOOP('',(#73379,#73380,#73381,#73382));
#28979=EDGE_LOOP('',(#73383,#73384,#73385,#73386));
#28980=EDGE_LOOP('',(#73387,#73388,#73389,#73390));
#28981=EDGE_LOOP('',(#73391,#73392,#73393,#73394));
#28982=EDGE_LOOP('',(#73395,#73396,#73397,#73398));
#28983=EDGE_LOOP('',(#73399,#73400,#73401,#73402));
#28984=EDGE_LOOP('',(#73403,#73404,#73405,#73406));
#28985=EDGE_LOOP('',(#73407,#73408,#73409,#73410));
#28986=EDGE_LOOP('',(#73411,#73412,#73413,#73414));
#28987=EDGE_LOOP('',(#73415,#73416,#73417,#73418));
#28988=EDGE_LOOP('',(#73419,#73420,#73421,#73422));
#28989=EDGE_LOOP('',(#73423,#73424,#73425,#73426));
#28990=EDGE_LOOP('',(#73427,#73428,#73429,#73430));
#28991=EDGE_LOOP('',(#73431,#73432,#73433,#73434));
#28992=EDGE_LOOP('',(#73435,#73436,#73437,#73438));
#28993=EDGE_LOOP('',(#73439,#73440,#73441,#73442));
#28994=EDGE_LOOP('',(#73443,#73444,#73445,#73446));
#28995=EDGE_LOOP('',(#73447,#73448,#73449,#73450));
#28996=EDGE_LOOP('',(#73451,#73452,#73453,#73454));
#28997=EDGE_LOOP('',(#73455,#73456,#73457,#73458));
#28998=EDGE_LOOP('',(#73459,#73460,#73461,#73462));
#28999=EDGE_LOOP('',(#73463,#73464,#73465,#73466));
#29000=EDGE_LOOP('',(#73467,#73468,#73469,#73470));
#29001=EDGE_LOOP('',(#73471,#73472,#73473,#73474));
#29002=EDGE_LOOP('',(#73475,#73476,#73477,#73478));
#29003=EDGE_LOOP('',(#73479,#73480,#73481,#73482));
#29004=EDGE_LOOP('',(#73483,#73484,#73485,#73486));
#29005=EDGE_LOOP('',(#73487,#73488,#73489,#73490));
#29006=EDGE_LOOP('',(#73491,#73492,#73493,#73494));
#29007=EDGE_LOOP('',(#73495,#73496,#73497,#73498));
#29008=EDGE_LOOP('',(#73499,#73500,#73501,#73502));
#29009=EDGE_LOOP('',(#73503,#73504,#73505,#73506));
#29010=EDGE_LOOP('',(#73507,#73508,#73509,#73510));
#29011=EDGE_LOOP('',(#73511,#73512,#73513,#73514));
#29012=EDGE_LOOP('',(#73515,#73516,#73517,#73518));
#29013=EDGE_LOOP('',(#73519,#73520,#73521,#73522));
#29014=EDGE_LOOP('',(#73523,#73524,#73525,#73526));
#29015=EDGE_LOOP('',(#73527,#73528,#73529,#73530));
#29016=EDGE_LOOP('',(#73531,#73532,#73533,#73534));
#29017=EDGE_LOOP('',(#73535,#73536,#73537,#73538));
#29018=EDGE_LOOP('',(#73539,#73540,#73541,#73542));
#29019=EDGE_LOOP('',(#73543,#73544,#73545,#73546));
#29020=EDGE_LOOP('',(#73547,#73548,#73549,#73550));
#29021=EDGE_LOOP('',(#73551,#73552,#73553,#73554));
#29022=EDGE_LOOP('',(#73555,#73556,#73557,#73558));
#29023=EDGE_LOOP('',(#73559,#73560,#73561,#73562));
#29024=EDGE_LOOP('',(#73563,#73564,#73565,#73566));
#29025=EDGE_LOOP('',(#73567,#73568,#73569,#73570));
#29026=EDGE_LOOP('',(#73571,#73572,#73573,#73574));
#29027=EDGE_LOOP('',(#73575,#73576,#73577,#73578));
#29028=EDGE_LOOP('',(#73579,#73580,#73581,#73582));
#29029=EDGE_LOOP('',(#73583,#73584,#73585,#73586));
#29030=EDGE_LOOP('',(#73587,#73588,#73589,#73590));
#29031=EDGE_LOOP('',(#73591,#73592,#73593,#73594));
#29032=EDGE_LOOP('',(#73595,#73596,#73597,#73598));
#29033=EDGE_LOOP('',(#73599,#73600,#73601,#73602));
#29034=EDGE_LOOP('',(#73603,#73604,#73605,#73606));
#29035=EDGE_LOOP('',(#73607,#73608,#73609,#73610));
#29036=EDGE_LOOP('',(#73611,#73612,#73613,#73614));
#29037=EDGE_LOOP('',(#73615,#73616,#73617,#73618));
#29038=EDGE_LOOP('',(#73619,#73620,#73621,#73622));
#29039=EDGE_LOOP('',(#73623,#73624,#73625,#73626));
#29040=EDGE_LOOP('',(#73627,#73628,#73629,#73630));
#29041=EDGE_LOOP('',(#73631,#73632,#73633,#73634));
#29042=EDGE_LOOP('',(#73635,#73636,#73637,#73638));
#29043=EDGE_LOOP('',(#73639,#73640,#73641,#73642));
#29044=EDGE_LOOP('',(#73643,#73644,#73645,#73646));
#29045=EDGE_LOOP('',(#73647,#73648,#73649,#73650));
#29046=EDGE_LOOP('',(#73651,#73652,#73653,#73654));
#29047=EDGE_LOOP('',(#73655,#73656,#73657,#73658));
#29048=EDGE_LOOP('',(#73659,#73660,#73661,#73662));
#29049=EDGE_LOOP('',(#73663,#73664,#73665,#73666));
#29050=EDGE_LOOP('',(#73667,#73668,#73669,#73670));
#29051=EDGE_LOOP('',(#73671,#73672,#73673,#73674));
#29052=EDGE_LOOP('',(#73675,#73676,#73677,#73678));
#29053=EDGE_LOOP('',(#73679,#73680,#73681,#73682));
#29054=EDGE_LOOP('',(#73683,#73684,#73685,#73686));
#29055=EDGE_LOOP('',(#73687,#73688,#73689,#73690));
#29056=EDGE_LOOP('',(#73691,#73692,#73693,#73694));
#29057=EDGE_LOOP('',(#73695,#73696,#73697,#73698));
#29058=EDGE_LOOP('',(#73699,#73700,#73701,#73702));
#29059=EDGE_LOOP('',(#73703,#73704,#73705,#73706));
#29060=EDGE_LOOP('',(#73707,#73708,#73709,#73710));
#29061=EDGE_LOOP('',(#73711,#73712,#73713,#73714));
#29062=EDGE_LOOP('',(#73715,#73716,#73717,#73718));
#29063=EDGE_LOOP('',(#73719,#73720,#73721,#73722));
#29064=EDGE_LOOP('',(#73723,#73724,#73725,#73726));
#29065=EDGE_LOOP('',(#73727,#73728,#73729,#73730));
#29066=EDGE_LOOP('',(#73731,#73732,#73733,#73734));
#29067=EDGE_LOOP('',(#73735,#73736,#73737,#73738));
#29068=EDGE_LOOP('',(#73739,#73740,#73741,#73742));
#29069=EDGE_LOOP('',(#73743,#73744,#73745,#73746));
#29070=EDGE_LOOP('',(#73747,#73748,#73749,#73750));
#29071=EDGE_LOOP('',(#73751,#73752,#73753,#73754));
#29072=EDGE_LOOP('',(#73755,#73756,#73757,#73758));
#29073=EDGE_LOOP('',(#73759,#73760,#73761,#73762));
#29074=EDGE_LOOP('',(#73763,#73764,#73765,#73766));
#29075=EDGE_LOOP('',(#73767,#73768,#73769,#73770));
#29076=EDGE_LOOP('',(#73771,#73772,#73773,#73774));
#29077=EDGE_LOOP('',(#73775,#73776,#73777,#73778));
#29078=EDGE_LOOP('',(#73779,#73780,#73781,#73782));
#29079=EDGE_LOOP('',(#73783,#73784,#73785,#73786));
#29080=EDGE_LOOP('',(#73787,#73788,#73789,#73790));
#29081=EDGE_LOOP('',(#73791,#73792,#73793,#73794));
#29082=EDGE_LOOP('',(#73795,#73796,#73797,#73798));
#29083=EDGE_LOOP('',(#73799,#73800,#73801,#73802));
#29084=EDGE_LOOP('',(#73803,#73804,#73805,#73806));
#29085=EDGE_LOOP('',(#73807,#73808,#73809,#73810));
#29086=EDGE_LOOP('',(#73811,#73812,#73813,#73814));
#29087=EDGE_LOOP('',(#73815,#73816,#73817,#73818));
#29088=EDGE_LOOP('',(#73819,#73820,#73821,#73822));
#29089=EDGE_LOOP('',(#73823,#73824,#73825,#73826));
#29090=EDGE_LOOP('',(#73827,#73828,#73829,#73830));
#29091=EDGE_LOOP('',(#73831,#73832,#73833,#73834));
#29092=EDGE_LOOP('',(#73835,#73836,#73837,#73838));
#29093=EDGE_LOOP('',(#73839,#73840,#73841,#73842));
#29094=EDGE_LOOP('',(#73843,#73844,#73845,#73846));
#29095=EDGE_LOOP('',(#73847,#73848,#73849,#73850));
#29096=EDGE_LOOP('',(#73851,#73852,#73853,#73854));
#29097=EDGE_LOOP('',(#73855,#73856,#73857,#73858));
#29098=EDGE_LOOP('',(#73859,#73860,#73861,#73862));
#29099=EDGE_LOOP('',(#73863,#73864,#73865,#73866));
#29100=EDGE_LOOP('',(#73867,#73868,#73869,#73870));
#29101=EDGE_LOOP('',(#73871,#73872,#73873,#73874));
#29102=EDGE_LOOP('',(#73875,#73876,#73877,#73878));
#29103=EDGE_LOOP('',(#73879,#73880,#73881,#73882));
#29104=EDGE_LOOP('',(#73883,#73884,#73885,#73886));
#29105=EDGE_LOOP('',(#73887,#73888,#73889,#73890));
#29106=EDGE_LOOP('',(#73891,#73892,#73893,#73894));
#29107=EDGE_LOOP('',(#73895,#73896,#73897,#73898));
#29108=EDGE_LOOP('',(#73899,#73900,#73901,#73902));
#29109=EDGE_LOOP('',(#73903,#73904,#73905,#73906));
#29110=EDGE_LOOP('',(#73907,#73908,#73909,#73910));
#29111=EDGE_LOOP('',(#73911,#73912,#73913,#73914));
#29112=EDGE_LOOP('',(#73915,#73916,#73917,#73918));
#29113=EDGE_LOOP('',(#73919,#73920,#73921,#73922));
#29114=EDGE_LOOP('',(#73923,#73924,#73925,#73926));
#29115=EDGE_LOOP('',(#73927,#73928,#73929,#73930));
#29116=EDGE_LOOP('',(#73931,#73932,#73933,#73934));
#29117=EDGE_LOOP('',(#73935,#73936,#73937,#73938));
#29118=EDGE_LOOP('',(#73939,#73940,#73941,#73942));
#29119=EDGE_LOOP('',(#73943,#73944,#73945,#73946));
#29120=EDGE_LOOP('',(#73947,#73948,#73949,#73950));
#29121=EDGE_LOOP('',(#73951,#73952,#73953,#73954));
#29122=EDGE_LOOP('',(#73955,#73956,#73957,#73958));
#29123=EDGE_LOOP('',(#73959,#73960,#73961,#73962));
#29124=EDGE_LOOP('',(#73963,#73964,#73965,#73966));
#29125=EDGE_LOOP('',(#73967,#73968,#73969,#73970));
#29126=EDGE_LOOP('',(#73971,#73972,#73973,#73974));
#29127=EDGE_LOOP('',(#73975,#73976,#73977,#73978));
#29128=EDGE_LOOP('',(#73979,#73980,#73981,#73982));
#29129=EDGE_LOOP('',(#73983,#73984,#73985,#73986));
#29130=EDGE_LOOP('',(#73987,#73988,#73989,#73990));
#29131=EDGE_LOOP('',(#73991,#73992,#73993,#73994));
#29132=EDGE_LOOP('',(#73995,#73996,#73997,#73998));
#29133=EDGE_LOOP('',(#73999,#74000,#74001,#74002));
#29134=EDGE_LOOP('',(#74003,#74004,#74005,#74006));
#29135=EDGE_LOOP('',(#74007,#74008,#74009,#74010));
#29136=EDGE_LOOP('',(#74011,#74012,#74013,#74014));
#29137=EDGE_LOOP('',(#74015,#74016,#74017,#74018));
#29138=EDGE_LOOP('',(#74019,#74020,#74021,#74022));
#29139=EDGE_LOOP('',(#74023,#74024,#74025,#74026));
#29140=EDGE_LOOP('',(#74027,#74028,#74029,#74030));
#29141=EDGE_LOOP('',(#74031,#74032,#74033,#74034));
#29142=EDGE_LOOP('',(#74035,#74036,#74037,#74038));
#29143=EDGE_LOOP('',(#74039,#74040,#74041,#74042));
#29144=EDGE_LOOP('',(#74043,#74044,#74045,#74046));
#29145=EDGE_LOOP('',(#74047,#74048,#74049,#74050));
#29146=EDGE_LOOP('',(#74051,#74052,#74053,#74054));
#29147=EDGE_LOOP('',(#74055,#74056,#74057,#74058));
#29148=EDGE_LOOP('',(#74059,#74060,#74061,#74062));
#29149=EDGE_LOOP('',(#74063,#74064,#74065,#74066));
#29150=EDGE_LOOP('',(#74067,#74068,#74069,#74070));
#29151=EDGE_LOOP('',(#74071,#74072,#74073,#74074));
#29152=EDGE_LOOP('',(#74075,#74076,#74077,#74078));
#29153=EDGE_LOOP('',(#74079,#74080,#74081,#74082));
#29154=EDGE_LOOP('',(#74083,#74084,#74085,#74086));
#29155=EDGE_LOOP('',(#74087,#74088,#74089,#74090));
#29156=EDGE_LOOP('',(#74091,#74092,#74093,#74094));
#29157=EDGE_LOOP('',(#74095,#74096,#74097,#74098));
#29158=EDGE_LOOP('',(#74099,#74100,#74101,#74102));
#29159=EDGE_LOOP('',(#74103,#74104,#74105,#74106));
#29160=EDGE_LOOP('',(#74107,#74108,#74109,#74110));
#29161=EDGE_LOOP('',(#74111,#74112,#74113,#74114));
#29162=EDGE_LOOP('',(#74115,#74116,#74117,#74118));
#29163=EDGE_LOOP('',(#74119,#74120,#74121,#74122));
#29164=EDGE_LOOP('',(#74123,#74124,#74125,#74126));
#29165=EDGE_LOOP('',(#74127,#74128,#74129,#74130));
#29166=EDGE_LOOP('',(#74131,#74132,#74133,#74134));
#29167=EDGE_LOOP('',(#74135,#74136,#74137,#74138));
#29168=EDGE_LOOP('',(#74139,#74140,#74141,#74142));
#29169=EDGE_LOOP('',(#74143,#74144,#74145,#74146));
#29170=EDGE_LOOP('',(#74147,#74148,#74149,#74150));
#29171=EDGE_LOOP('',(#74151,#74152,#74153,#74154));
#29172=EDGE_LOOP('',(#74155,#74156,#74157,#74158));
#29173=EDGE_LOOP('',(#74159,#74160,#74161,#74162));
#29174=EDGE_LOOP('',(#74163,#74164,#74165,#74166));
#29175=EDGE_LOOP('',(#74167,#74168,#74169,#74170));
#29176=EDGE_LOOP('',(#74171,#74172,#74173,#74174));
#29177=EDGE_LOOP('',(#74175,#74176,#74177,#74178));
#29178=EDGE_LOOP('',(#74179,#74180,#74181,#74182));
#29179=EDGE_LOOP('',(#74183,#74184,#74185,#74186));
#29180=EDGE_LOOP('',(#74187,#74188,#74189,#74190));
#29181=EDGE_LOOP('',(#74191,#74192,#74193,#74194));
#29182=EDGE_LOOP('',(#74195,#74196,#74197,#74198));
#29183=EDGE_LOOP('',(#74199,#74200,#74201,#74202));
#29184=EDGE_LOOP('',(#74203,#74204,#74205,#74206));
#29185=EDGE_LOOP('',(#74207,#74208,#74209,#74210));
#29186=EDGE_LOOP('',(#74211,#74212,#74213,#74214));
#29187=EDGE_LOOP('',(#74215,#74216,#74217,#74218));
#29188=EDGE_LOOP('',(#74219,#74220,#74221,#74222));
#29189=EDGE_LOOP('',(#74223,#74224,#74225,#74226));
#29190=EDGE_LOOP('',(#74227,#74228,#74229,#74230));
#29191=EDGE_LOOP('',(#74231,#74232,#74233,#74234));
#29192=EDGE_LOOP('',(#74235,#74236,#74237,#74238));
#29193=EDGE_LOOP('',(#74239,#74240,#74241,#74242));
#29194=EDGE_LOOP('',(#74243,#74244,#74245,#74246));
#29195=EDGE_LOOP('',(#74247,#74248,#74249,#74250));
#29196=EDGE_LOOP('',(#74251,#74252,#74253,#74254));
#29197=EDGE_LOOP('',(#74255,#74256,#74257,#74258));
#29198=EDGE_LOOP('',(#74259,#74260,#74261,#74262));
#29199=EDGE_LOOP('',(#74263,#74264,#74265,#74266));
#29200=EDGE_LOOP('',(#74267,#74268,#74269,#74270));
#29201=EDGE_LOOP('',(#74271,#74272,#74273,#74274));
#29202=EDGE_LOOP('',(#74275,#74276,#74277,#74278));
#29203=EDGE_LOOP('',(#74279,#74280,#74281,#74282));
#29204=EDGE_LOOP('',(#74283,#74284,#74285,#74286));
#29205=EDGE_LOOP('',(#74287,#74288,#74289,#74290));
#29206=EDGE_LOOP('',(#74291,#74292,#74293,#74294));
#29207=EDGE_LOOP('',(#74295,#74296,#74297,#74298));
#29208=EDGE_LOOP('',(#74299,#74300,#74301,#74302));
#29209=EDGE_LOOP('',(#74303,#74304,#74305,#74306));
#29210=EDGE_LOOP('',(#74307,#74308,#74309,#74310));
#29211=EDGE_LOOP('',(#74311,#74312,#74313,#74314));
#29212=EDGE_LOOP('',(#74315,#74316,#74317,#74318));
#29213=EDGE_LOOP('',(#74319,#74320,#74321,#74322));
#29214=EDGE_LOOP('',(#74323,#74324,#74325,#74326));
#29215=EDGE_LOOP('',(#74327,#74328,#74329,#74330));
#29216=EDGE_LOOP('',(#74331,#74332,#74333,#74334));
#29217=EDGE_LOOP('',(#74335));
#29218=EDGE_LOOP('',(#74336));
#29219=EDGE_LOOP('',(#74337,#74338,#74339,#74340,#74341,#74342,#74343,#74344,
#74345,#74346,#74347,#74348,#74349));
#29220=EDGE_LOOP('',(#74350,#74351,#74352,#74353));
#29221=EDGE_LOOP('',(#74354,#74355,#74356,#74357));
#29222=EDGE_LOOP('',(#74358,#74359,#74360,#74361,#74362));
#29223=EDGE_LOOP('',(#74363,#74364,#74365,#74366,#74367));
#29224=EDGE_LOOP('',(#74368,#74369,#74370,#74371));
#29225=EDGE_LOOP('',(#74372,#74373,#74374,#74375));
#29226=EDGE_LOOP('',(#74376,#74377,#74378,#74379,#74380));
#29227=EDGE_LOOP('',(#74381,#74382,#74383));
#29228=EDGE_LOOP('',(#74384,#74385,#74386,#74387,#74388,#74389,#74390));
#29229=EDGE_LOOP('',(#74391,#74392,#74393,#74394,#74395));
#29230=EDGE_LOOP('',(#74396,#74397,#74398,#74399,#74400));
#29231=EDGE_LOOP('',(#74401,#74402,#74403,#74404));
#29232=EDGE_LOOP('',(#74405,#74406,#74407,#74408,#74409));
#29233=EDGE_LOOP('',(#74410,#74411,#74412,#74413,#74414));
#29234=EDGE_LOOP('',(#74415,#74416,#74417,#74418));
#29235=EDGE_LOOP('',(#74419,#74420,#74421,#74422,#74423,#74424,#74425,#74426,
#74427,#74428));
#29236=EDGE_LOOP('',(#74429,#74430,#74431,#74432,#74433,#74434));
#29237=EDGE_LOOP('',(#74435,#74436,#74437,#74438,#74439));
#29238=EDGE_LOOP('',(#74440,#74441,#74442,#74443));
#29239=EDGE_LOOP('',(#74444,#74445,#74446,#74447));
#29240=EDGE_LOOP('',(#74448,#74449,#74450,#74451));
#29241=EDGE_LOOP('',(#74452,#74453,#74454,#74455,#74456));
#29242=EDGE_LOOP('',(#74457,#74458,#74459,#74460));
#29243=EDGE_LOOP('',(#74461,#74462,#74463,#74464));
#29244=EDGE_LOOP('',(#74465,#74466,#74467,#74468));
#29245=EDGE_LOOP('',(#74469,#74470,#74471,#74472));
#29246=EDGE_LOOP('',(#74473,#74474,#74475,#74476));
#29247=EDGE_LOOP('',(#74477,#74478,#74479,#74480));
#29248=EDGE_LOOP('',(#74481,#74482,#74483,#74484));
#29249=EDGE_LOOP('',(#74485,#74486,#74487,#74488,#74489));
#29250=EDGE_LOOP('',(#74490,#74491,#74492,#74493));
#29251=EDGE_LOOP('',(#74494,#74495,#74496,#74497));
#29252=EDGE_LOOP('',(#74498,#74499,#74500,#74501));
#29253=EDGE_LOOP('',(#74502,#74503,#74504,#74505,#74506,#74507,#74508));
#29254=EDGE_LOOP('',(#74509,#74510,#74511));
#29255=EDGE_LOOP('',(#74512,#74513,#74514,#74515));
#29256=EDGE_LOOP('',(#74516,#74517,#74518,#74519));
#29257=EDGE_LOOP('',(#74520,#74521,#74522,#74523));
#29258=EDGE_LOOP('',(#74524,#74525,#74526,#74527,#74528));
#29259=EDGE_LOOP('',(#74529,#74530,#74531,#74532,#74533,#74534,#74535));
#29260=EDGE_LOOP('',(#74536,#74537,#74538,#74539,#74540,#74541));
#29261=EDGE_LOOP('',(#74542,#74543,#74544,#74545,#74546,#74547));
#29262=EDGE_LOOP('',(#74548,#74549,#74550,#74551));
#29263=EDGE_LOOP('',(#74552,#74553,#74554,#74555,#74556,#74557,#74558,#74559,
#74560,#74561,#74562,#74563,#74564));
#29264=EDGE_LOOP('',(#74565,#74566,#74567,#74568,#74569,#74570,#74571,#74572,
#74573,#74574,#74575,#74576,#74577));
#29265=EDGE_LOOP('',(#74578,#74579,#74580,#74581,#74582));
#29266=EDGE_LOOP('',(#74583,#74584,#74585,#74586));
#29267=EDGE_LOOP('',(#74587,#74588,#74589,#74590,#74591));
#29268=EDGE_LOOP('',(#74592,#74593,#74594,#74595,#74596,#74597,#74598,#74599,
#74600,#74601,#74602,#74603,#74604,#74605));
#29269=EDGE_LOOP('',(#74606,#74607,#74608,#74609,#74610,#74611,#74612,#74613,
#74614,#74615,#74616,#74617,#74618,#74619));
#29270=EDGE_LOOP('',(#74620,#74621,#74622,#74623,#74624,#74625,#74626,#74627));
#29271=EDGE_LOOP('',(#74628,#74629,#74630,#74631,#74632));
#29272=EDGE_LOOP('',(#74633,#74634,#74635,#74636,#74637,#74638,#74639,#74640,
#74641));
#29273=EDGE_LOOP('',(#74642,#74643,#74644));
#29274=EDGE_LOOP('',(#74645,#74646,#74647,#74648));
#29275=EDGE_LOOP('',(#74649,#74650,#74651,#74652,#74653));
#29276=EDGE_LOOP('',(#74654,#74655,#74656,#74657,#74658,#74659,#74660,#74661,
#74662,#74663,#74664,#74665));
#29277=EDGE_LOOP('',(#74666,#74667,#74668,#74669,#74670));
#29278=EDGE_LOOP('',(#74671,#74672,#74673,#74674));
#29279=EDGE_LOOP('',(#74675,#74676,#74677,#74678,#74679));
#29280=EDGE_LOOP('',(#74680,#74681,#74682,#74683,#74684,#74685,#74686,#74687,
#74688,#74689,#74690));
#29281=EDGE_LOOP('',(#74691,#74692,#74693,#74694,#74695,#74696,#74697,#74698,
#74699,#74700));
#29282=EDGE_LOOP('',(#74701,#74702,#74703,#74704,#74705,#74706,#74707,#74708,
#74709,#74710,#74711));
#29283=EDGE_LOOP('',(#74712,#74713,#74714,#74715,#74716));
#29284=EDGE_LOOP('',(#74717,#74718,#74719,#74720,#74721,#74722,#74723,#74724,
#74725,#74726));
#29285=EDGE_LOOP('',(#74727,#74728,#74729,#74730,#74731,#74732,#74733,#74734,
#74735));
#29286=EDGE_LOOP('',(#74736,#74737,#74738,#74739,#74740));
#29287=EDGE_LOOP('',(#74741,#74742,#74743,#74744,#74745));
#29288=EDGE_LOOP('',(#74746,#74747,#74748,#74749,#74750,#74751,#74752));
#29289=EDGE_LOOP('',(#74753));
#29290=EDGE_LOOP('',(#74754));
#29291=EDGE_LOOP('',(#74755));
#29292=EDGE_LOOP('',(#74756));
#29293=EDGE_LOOP('',(#74757));
#29294=EDGE_LOOP('',(#74758,#74759,#74760,#74761));
#29295=EDGE_LOOP('',(#74762,#74763,#74764,#74765));
#29296=EDGE_LOOP('',(#74766,#74767,#74768,#74769,#74770));
#29297=EDGE_LOOP('',(#74771));
#29298=EDGE_LOOP('',(#74772,#74773,#74774,#74775,#74776,#74777,#74778,#74779));
#29299=EDGE_LOOP('',(#74780,#74781,#74782,#74783,#74784,#74785,#74786,#74787,
#74788,#74789,#74790,#74791));
#29300=EDGE_LOOP('',(#74792,#74793,#74794,#74795,#74796,#74797,#74798,#74799,
#74800));
#29301=EDGE_LOOP('',(#74801,#74802,#74803,#74804));
#29302=EDGE_LOOP('',(#74805,#74806,#74807,#74808));
#29303=EDGE_LOOP('',(#74809,#74810,#74811,#74812,#74813,#74814,#74815,#74816,
#74817,#74818,#74819,#74820,#74821));
#29304=EDGE_LOOP('',(#74822,#74823,#74824,#74825));
#29305=EDGE_LOOP('',(#74826,#74827,#74828,#74829));
#29306=EDGE_LOOP('',(#74830,#74831,#74832,#74833,#74834));
#29307=EDGE_LOOP('',(#74835,#74836,#74837,#74838,#74839));
#29308=EDGE_LOOP('',(#74840,#74841,#74842,#74843));
#29309=EDGE_LOOP('',(#74844,#74845,#74846,#74847));
#29310=EDGE_LOOP('',(#74848,#74849,#74850,#74851,#74852));
#29311=EDGE_LOOP('',(#74853,#74854,#74855));
#29312=EDGE_LOOP('',(#74856,#74857,#74858,#74859,#74860,#74861,#74862));
#29313=EDGE_LOOP('',(#74863,#74864,#74865,#74866,#74867));
#29314=EDGE_LOOP('',(#74868,#74869,#74870,#74871,#74872));
#29315=EDGE_LOOP('',(#74873,#74874,#74875,#74876));
#29316=EDGE_LOOP('',(#74877,#74878,#74879,#74880,#74881));
#29317=EDGE_LOOP('',(#74882,#74883,#74884,#74885,#74886));
#29318=EDGE_LOOP('',(#74887,#74888,#74889,#74890));
#29319=EDGE_LOOP('',(#74891,#74892,#74893,#74894,#74895,#74896,#74897,#74898,
#74899,#74900));
#29320=EDGE_LOOP('',(#74901,#74902,#74903,#74904,#74905,#74906));
#29321=EDGE_LOOP('',(#74907,#74908,#74909,#74910,#74911));
#29322=EDGE_LOOP('',(#74912,#74913,#74914,#74915));
#29323=EDGE_LOOP('',(#74916,#74917,#74918,#74919));
#29324=EDGE_LOOP('',(#74920,#74921,#74922,#74923));
#29325=EDGE_LOOP('',(#74924,#74925,#74926,#74927,#74928));
#29326=EDGE_LOOP('',(#74929,#74930,#74931,#74932));
#29327=EDGE_LOOP('',(#74933,#74934,#74935,#74936));
#29328=EDGE_LOOP('',(#74937,#74938,#74939,#74940));
#29329=EDGE_LOOP('',(#74941,#74942,#74943,#74944));
#29330=EDGE_LOOP('',(#74945,#74946,#74947,#74948));
#29331=EDGE_LOOP('',(#74949,#74950,#74951,#74952));
#29332=EDGE_LOOP('',(#74953,#74954,#74955,#74956));
#29333=EDGE_LOOP('',(#74957,#74958,#74959,#74960,#74961));
#29334=EDGE_LOOP('',(#74962,#74963,#74964,#74965));
#29335=EDGE_LOOP('',(#74966,#74967,#74968,#74969));
#29336=EDGE_LOOP('',(#74970,#74971,#74972,#74973));
#29337=EDGE_LOOP('',(#74974,#74975,#74976,#74977,#74978,#74979,#74980));
#29338=EDGE_LOOP('',(#74981,#74982,#74983));
#29339=EDGE_LOOP('',(#74984,#74985,#74986,#74987));
#29340=EDGE_LOOP('',(#74988,#74989,#74990,#74991));
#29341=EDGE_LOOP('',(#74992,#74993,#74994,#74995));
#29342=EDGE_LOOP('',(#74996,#74997,#74998,#74999,#75000));
#29343=EDGE_LOOP('',(#75001,#75002,#75003,#75004,#75005,#75006,#75007));
#29344=EDGE_LOOP('',(#75008,#75009,#75010,#75011,#75012,#75013));
#29345=EDGE_LOOP('',(#75014,#75015,#75016,#75017,#75018,#75019));
#29346=EDGE_LOOP('',(#75020,#75021,#75022,#75023));
#29347=EDGE_LOOP('',(#75024,#75025,#75026,#75027,#75028,#75029,#75030,#75031,
#75032,#75033,#75034,#75035,#75036));
#29348=EDGE_LOOP('',(#75037,#75038,#75039,#75040,#75041,#75042,#75043,#75044,
#75045,#75046,#75047,#75048,#75049));
#29349=EDGE_LOOP('',(#75050,#75051,#75052,#75053,#75054));
#29350=EDGE_LOOP('',(#75055,#75056,#75057,#75058));
#29351=EDGE_LOOP('',(#75059,#75060,#75061,#75062,#75063));
#29352=EDGE_LOOP('',(#75064,#75065,#75066,#75067,#75068,#75069,#75070,#75071,
#75072,#75073,#75074,#75075,#75076,#75077));
#29353=EDGE_LOOP('',(#75078,#75079,#75080,#75081,#75082,#75083,#75084,#75085,
#75086,#75087,#75088,#75089,#75090,#75091));
#29354=EDGE_LOOP('',(#75092,#75093,#75094,#75095,#75096,#75097,#75098,#75099));
#29355=EDGE_LOOP('',(#75100,#75101,#75102,#75103,#75104));
#29356=EDGE_LOOP('',(#75105,#75106,#75107,#75108,#75109,#75110,#75111,#75112,
#75113));
#29357=EDGE_LOOP('',(#75114,#75115,#75116));
#29358=EDGE_LOOP('',(#75117,#75118,#75119,#75120));
#29359=EDGE_LOOP('',(#75121,#75122,#75123,#75124,#75125));
#29360=EDGE_LOOP('',(#75126,#75127,#75128,#75129,#75130,#75131,#75132,#75133,
#75134,#75135,#75136,#75137));
#29361=EDGE_LOOP('',(#75138,#75139,#75140,#75141,#75142));
#29362=EDGE_LOOP('',(#75143,#75144,#75145,#75146));
#29363=EDGE_LOOP('',(#75147,#75148,#75149,#75150,#75151));
#29364=EDGE_LOOP('',(#75152,#75153,#75154,#75155,#75156,#75157,#75158,#75159,
#75160,#75161,#75162));
#29365=EDGE_LOOP('',(#75163,#75164,#75165,#75166,#75167,#75168,#75169,#75170,
#75171,#75172));
#29366=EDGE_LOOP('',(#75173,#75174,#75175,#75176,#75177,#75178,#75179,#75180,
#75181,#75182,#75183));
#29367=EDGE_LOOP('',(#75184,#75185,#75186,#75187,#75188));
#29368=EDGE_LOOP('',(#75189,#75190,#75191,#75192,#75193,#75194,#75195,#75196,
#75197,#75198));
#29369=EDGE_LOOP('',(#75199,#75200,#75201,#75202,#75203,#75204,#75205,#75206,
#75207));
#29370=EDGE_LOOP('',(#75208,#75209,#75210,#75211,#75212));
#29371=EDGE_LOOP('',(#75213,#75214,#75215,#75216,#75217));
#29372=EDGE_LOOP('',(#75218,#75219,#75220,#75221,#75222,#75223,#75224));
#29373=EDGE_LOOP('',(#75225));
#29374=EDGE_LOOP('',(#75226));
#29375=EDGE_LOOP('',(#75227));
#29376=EDGE_LOOP('',(#75228));
#29377=EDGE_LOOP('',(#75229));
#29378=EDGE_LOOP('',(#75230,#75231,#75232,#75233));
#29379=EDGE_LOOP('',(#75234,#75235,#75236,#75237));
#29380=EDGE_LOOP('',(#75238,#75239,#75240,#75241,#75242));
#29381=EDGE_LOOP('',(#75243));
#29382=EDGE_LOOP('',(#75244,#75245,#75246,#75247,#75248,#75249,#75250,#75251));
#29383=EDGE_LOOP('',(#75252,#75253,#75254,#75255,#75256,#75257,#75258,#75259,
#75260,#75261,#75262,#75263));
#29384=EDGE_LOOP('',(#75264,#75265,#75266,#75267,#75268,#75269,#75270,#75271,
#75272));
#29385=EDGE_LOOP('',(#75273,#75274,#75275,#75276));
#29386=EDGE_LOOP('',(#75277,#75278,#75279,#75280));
#29387=B_SPLINE_CURVE_WITH_KNOTS('',3,(#106605,#106606,#106607,#106608,
#106609,#106610),.UNSPECIFIED.,.F.,.F.,(4,2,4),(-0.241430299538162,-0.206580137455089,
-0.156109273606686),.UNSPECIFIED.);
#29388=B_SPLINE_CURVE_WITH_KNOTS('',3,(#106654,#106655,#106656,#106657,
#106658,#106659,#106660,#106661,#106662,#106663,#106664,#106665,#106666,
#106667),.UNSPECIFIED.,.F.,.F.,(4,2,2,2,2,2,4),(-0.241853105666202,-0.175836100044282,
-0.122112436673168,-0.0803073887927507,-0.0455467331302326,-0.0227627040768013,
-1.73601080630016E-6),.UNSPECIFIED.);
#29389=B_SPLINE_CURVE_WITH_KNOTS('',3,(#106668,#106669,#106670,#106671),
 .UNSPECIFIED.,.F.,.F.,(4,4),(0.,0.999989990831842),.UNSPECIFIED.);
#29390=B_SPLINE_CURVE_WITH_KNOTS('',3,(#106753,#106754,#106755,#106756,
#106757,#106758,#106759,#106760,#106761,#106762),.UNSPECIFIED.,.F.,.F.,
(4,3,3,4),(0.,0.354579189327693,0.679902554719739,1.),.UNSPECIFIED.);
#29391=B_SPLINE_CURVE_WITH_KNOTS('',3,(#106763,#106764,#106765,#106766,
#106767,#106768),.UNSPECIFIED.,.F.,.F.,(4,2,4),(-0.278077459546498,-0.155434077993828,
-1.73601828061288E-6),.UNSPECIFIED.);
#29392=B_SPLINE_CURVE_WITH_KNOTS('',3,(#106849,#106850,#106851,#106852,
#106853,#106854,#106855,#106856,#106857,#106858,#106859,#106860,#106861,
#106862,#106863,#106864),.UNSPECIFIED.,.F.,.F.,(4,2,2,2,2,2,2,4),(-0.280256489498076,
-0.161862440487671,-0.12787619266535,-0.10766826527807,-0.092664611109678,
-0.0777869012640525,-0.056960032780691,-9.99999003770125E-7),
 .UNSPECIFIED.);
#29393=B_SPLINE_CURVE_WITH_KNOTS('',3,(#106866,#106867,#106868,#106869,
#106870,#106871,#106872,#106873,#106874,#106875),.UNSPECIFIED.,.F.,.F.,
(4,2,2,2,4),(-2.67982627711791E-10,0.0296331580141952,0.0592663162963728,
0.118532632860728,0.223499171284228),.UNSPECIFIED.);
#29394=B_SPLINE_CURVE_WITH_KNOTS('',3,(#106885,#106886,#106887,#106888,
#106889,#106890),.UNSPECIFIED.,.F.,.F.,(4,2,4),(-0.257051044346983,-0.206580142016457,
-0.171729983682942),.UNSPECIFIED.);
#29395=B_SPLINE_CURVE_WITH_KNOTS('',3,(#106928,#106929,#106930,#106931,
#106932,#106933,#106934,#106935,#106936,#106937,#106938,#106939,#106940,
#106941),.UNSPECIFIED.,.F.,.F.,(4,2,2,2,2,2,4),(-0.2438079662112,-0.220869823866369,
-0.197908662602918,-0.162873889664189,-0.1207435672921,-0.0666091518365065,
-1.00053347902397E-6),.UNSPECIFIED.);
#29396=B_SPLINE_CURVE_WITH_KNOTS('',3,(#106942,#106943,#106944,#106945),
 .UNSPECIFIED.,.F.,.F.,(4,4),(0.,0.999999972395555),.UNSPECIFIED.);
#29397=B_SPLINE_CURVE_WITH_KNOTS('',3,(#107029,#107030,#107031,#107032,
#107033,#107034,#107035,#107036,#107037,#107038,#107039,#107040,#107041,
#107042,#107043,#107044),.UNSPECIFIED.,.F.,.F.,(4,2,2,2,2,2,2,4),(-0.442279703755202,
-0.352763675612789,-0.319586925582681,-0.29601592754955,-0.27234102291881,
-0.240616391884951,-0.187314080741787,-9.99999260398177E-7),
 .UNSPECIFIED.);
#29398=B_SPLINE_CURVE_WITH_KNOTS('',3,(#107045,#107046,#107047,#107048,
#107049,#107050,#107051,#107052,#107053,#107054),.UNSPECIFIED.,.F.,.F.,
(4,3,3,4),(2.36937065112853E-5,0.199673744617112,0.681815427418137,1.),
 .UNSPECIFIED.);
#29399=B_SPLINE_CURVE_WITH_KNOTS('',3,(#107135,#107136,#107137,#107138,
#107139,#107140),.UNSPECIFIED.,.F.,.F.,(4,2,4),(-0.278517062048807,-0.122825079395318,
-1.00000141813119E-6),.UNSPECIFIED.);
#29400=B_SPLINE_CURVE_WITH_KNOTS('',3,(#107142,#107143,#107144,#107145,
#107146,#107147,#107148,#107149,#107150,#107151),.UNSPECIFIED.,.F.,.F.,
(4,2,2,2,4),(-0.218420289446346,-0.143529737322937,-0.051830543878608,-0.0259152720267801,
-1.7495224713393E-10),.UNSPECIFIED.);
#29401=B_SPLINE_CURVE_WITH_KNOTS('',3,(#107156,#107157,#107158,#107159,
#107160,#107161,#107162,#107163,#107164,#107165,#107166,#107167),
 .UNSPECIFIED.,.F.,.F.,(4,2,2,2,2,4),(-0.761165579403507,-0.582021759725205,
-0.420760911541275,-0.213198071172165,-0.116802189854271,-7.01180062234323E-6),
 .UNSPECIFIED.);
#29402=B_SPLINE_CURVE_WITH_KNOTS('',3,(#107169,#107170,#107171,#107172,
#107173,#107174,#107175,#107176,#107177,#107178,#107179,#107180,#107181,
#107182,#107183,#107184,#107185,#107186,#107187,#107188,#107189,#107190),
 .UNSPECIFIED.,.F.,.F.,(4,2,2,2,2,2,2,2,2,2,4),(-1.34392737370477,-1.014404550101,
-0.888242703317446,-0.838521487626843,-0.812981145439651,-0.795161744961047,
-0.777218608043124,-0.752854386147025,-0.707252167674362,-0.454372104568619,
-9.99999739524789E-7),.UNSPECIFIED.);
#29403=B_SPLINE_CURVE_WITH_KNOTS('',3,(#107194,#107195,#107196,#107197,
#107198,#107199,#107200,#107201,#107202,#107203,#107204,#107205),
 .UNSPECIFIED.,.F.,.F.,(4,2,2,2,2,4),(0.954693196677972,1.07014467842961,
1.18559616018125,1.24486247667459,1.27449563492126,1.30411858773122),
 .UNSPECIFIED.);
#29404=B_SPLINE_CURVE_WITH_KNOTS('',3,(#107209,#107210,#107211,#107212,
#107213,#107214,#107215,#107216,#107217,#107218,#107219,#107220),
 .UNSPECIFIED.,.F.,.F.,(4,2,2,2,2,4),(-0.109324587965852,-0.0960313413287254,
-0.0826995239600266,-0.0543197165532493,-0.0285691916501081,-1.00000465952576E-6),
 .UNSPECIFIED.);
#29405=B_SPLINE_CURVE_WITH_KNOTS('',3,(#107221,#107222,#107223,#107224,
#107225,#107226),.UNSPECIFIED.,.F.,.F.,(4,2,4),(-0.159987069735286,-0.0797279100080487,
-9.99997231576621E-7),.UNSPECIFIED.);
#29406=B_SPLINE_CURVE_WITH_KNOTS('',3,(#107301,#107302,#107303,#107304,
#107305,#107306,#107307,#107308,#107309,#107310,#107311,#107312,#107313,
#107314,#107315,#107316,#107317,#107318,#107319,#107320,#107321,#107322,
#107323,#107324,#107325,#107326,#107327,#107328,#107329,#107330,#107331),
 .UNSPECIFIED.,.F.,.F.,(4,3,3,3,3,3,3,3,3,3,4),(0.,0.108970225117902,0.218406669395091,
0.328218209138362,0.439039967350302,0.5,0.612445244717792,0.727056478754142,
0.843061292777059,0.961495204479547,1.),.UNSPECIFIED.);
#29407=B_SPLINE_CURVE_WITH_KNOTS('',3,(#107333,#107334,#107335,#107336,
#107337,#107338,#107339,#107340,#107341,#107342,#107343,#107344,#107345,
#107346,#107347,#107348,#107349,#107350,#107351,#107352,#107353,#107354,
#107355,#107356,#107357,#107358,#107359,#107360,#107361,#107362,#107363,
#107364,#107365,#107366,#107367,#107368,#107369,#107370,#107371,#107372,
#107373,#107374,#107375,#107376,#107377,#107378,#107379,#107380,#107381,
#107382,#107383,#107384,#107385,#107386,#107387,#107388,#107389,#107390,
#107391,#107392,#107393,#107394,#107395,#107396,#107397,#107398,#107399,
#107400,#107401,#107402,#107403,#107404,#107405,#107406,#107407,#107408,
#107409,#107410,#107411,#107412,#107413,#107414,#107415,#107416,#107417,
#107418,#107419,#107420,#107421,#107422,#107423,#107424,#107425,#107426,
#107427,#107428,#107429,#107430,#107431,#107432,#107433,#107434,#107435,
#107436,#107437,#107438,#107439,#107440,#107441),.UNSPECIFIED.,.F.,.F.,
(4,3,3,3,3,3,3,3,3,3,3,3,3,3,3,3,3,3,3,3,3,3,3,3,3,3,3,3,3,3,3,3,3,3,3,
3,4),(4.63591186593161E-13,0.0352304133180864,0.0496679699621724,0.07142857142857,
0.116839227155713,0.124882006224014,0.1428571428571,0.179126833876683,0.19987991330948,
0.2142857142857,0.254438827359413,0.275004526555019,0.2857142857143,0.327232537354997,
0.350098755170649,0.3571428571429,0.402277134059596,0.42521990674884,0.4285714285714,
0.479462989405757,0.5,0.500342945580645,0.551400032933508,0.5714285714286,
0.57545998934806,0.630187215511676,0.6428571428571,0.650577761732493,0.7142857142857,
0.725693303545247,0.7857142857143,0.800806742377481,0.8571428571429,0.875935814320093,
0.9285714285714,0.950971031508945,1.),.UNSPECIFIED.);
#29408=B_SPLINE_CURVE_WITH_KNOTS('',3,(#107443,#107444,#107445,#107446,
#107447,#107448,#107449,#107450,#107451,#107452,#107453,#107454,#107455,
#107456,#107457,#107458,#107459,#107460,#107461,#107462,#107463,#107464,
#107465,#107466,#107467,#107468,#107469,#107470,#107471,#107472),
 .UNSPECIFIED.,.F.,.F.,(4,2,2,2,1,1,2,2,2,2,2,1,1,2,2,2,4),(2.30700482817146E-8,
0.124999999999894,0.187499999999842,0.218749999999815,0.2343749999998,0.242187499999795,
0.246093749999791,0.249999999999787,0.374999999999697,0.437499999999653,
0.468749999999625,0.484374999999608,0.492187499999599,0.496093749999589,
0.499999999999578,0.749999999999789,1.),.UNSPECIFIED.);
#29409=B_SPLINE_CURVE_WITH_KNOTS('',3,(#107473,#107474,#107475,#107476,
#107477,#107478,#107479,#107480,#107481,#107482,#107483,#107484,#107485,
#107486,#107487,#107488,#107489,#107490,#107491,#107492,#107493,#107494,
#107495,#107496,#107497,#107498,#107499,#107500,#107501,#107502,#107503,
#107504,#107505,#107506,#107507,#107508,#107509,#107510,#107511,#107512,
#107513,#107514,#107515,#107516,#107517,#107518,#107519,#107520,#107521,
#107522,#107523,#107524,#107525,#107526,#107527,#107528,#107529,#107530,
#107531,#107532,#107533,#107534,#107535,#107536,#107537,#107538,#107539,
#107540,#107541,#107542,#107543,#107544,#107545,#107546,#107547,#107548,
#107549,#107550,#107551,#107552,#107553,#107554,#107555,#107556,#107557,
#107558,#107559,#107560,#107561,#107562,#107563,#107564,#107565,#107566,
#107567,#107568,#107569,#107570,#107571,#107572,#107573,#107574,#107575),
 .UNSPECIFIED.,.F.,.F.,(4,3,3,3,3,3,3,3,3,3,3,3,3,3,3,3,3,3,3,3,3,3,3,3,
3,3,3,3,3,3,3,3,3,3,4),(1.68547190877228E-9,0.04838995602028,0.0978468067776024,
0.118523443707981,0.169551292093508,0.221702103432071,0.249999999999981,
0.280746417338719,0.338633928132514,0.374999999999971,0.434952886602702,
0.437499999999966,0.468749999999964,0.484374999999963,0.492187499999962,
0.496093749999961,0.498046874999961,0.499999999999961,0.56407974531281,
0.624999999999964,0.635959106366061,0.687499999999965,0.718749999999966,
0.734374999999967,0.742187499999967,0.746093749999967,0.748046874999967,
0.749999999999967,0.79840618544373,0.845021640793756,0.88913814197588,0.900369257313181,
0.94302038072256,0.983460917668321,1.),.UNSPECIFIED.);
#29410=B_SPLINE_CURVE_WITH_KNOTS('',3,(#107578,#107579,#107580,#107581,
#107582,#107583,#107584,#107585,#107586,#107587,#107588,#107589,#107590,
#107591,#107592,#107593,#107594,#107595,#107596,#107597,#107598,#107599,
#107600,#107601,#107602,#107603,#107604,#107605,#107606,#107607,#107608,
#107609,#107610,#107611,#107612,#107613,#107614,#107615,#107616,#107617,
#107618,#107619,#107620,#107621,#107622,#107623,#107624,#107625,#107626,
#107627,#107628,#107629,#107630,#107631,#107632,#107633,#107634,#107635,
#107636,#107637,#107638,#107639,#107640,#107641,#107642,#107643,#107644,
#107645,#107646,#107647,#107648,#107649,#107650,#107651,#107652,#107653,
#107654,#107655,#107656,#107657,#107658,#107659,#107660,#107661,#107662,
#107663,#107664,#107665,#107666,#107667,#107668,#107669,#107670,#107671,
#107672,#107673,#107674,#107675,#107676,#107677,#107678,#107679,#107680,
#107681,#107682,#107683),.UNSPECIFIED.,.F.,.F.,(4,3,3,3,3,3,3,3,3,3,3,3,
3,3,3,3,3,3,3,3,3,3,3,3,3,3,3,3,3,3,3,3,3,3,3,4),(0.,0.0764808248342431,
0.152821059018209,0.228907286392826,0.25,0.322571962172829,0.39359505610544,
0.4628389830717,0.5,0.546141355518709,0.591012295465604,0.634660406546386,
0.677861768276641,0.720673067745511,0.75,0.774539320541827,0.79898661610755,
0.823367802660232,0.845152365397452,0.861159832875906,0.87718336701521,
0.893272345997422,0.897541889062698,0.90750437030887,0.91782101386449,0.927979055773836,
0.938396106216881,0.948770944531349,0.96157820839839,0.969207846796616,
0.975863277854313,0.981897458390613,0.987341821099734,0.992436269089802,
0.997046562336808,0.999999999999513),.UNSPECIFIED.);
#29411=B_SPLINE_CURVE_WITH_KNOTS('',3,(#107684,#107685,#107686,#107687,
#107688,#107689,#107690,#107691,#107692,#107693,#107694,#107695,#107696,
#107697,#107698,#107699,#107700,#107701,#107702,#107703,#107704,#107705,
#107706,#107707,#107708,#107709,#107710,#107711,#107712,#107713,#107714,
#107715,#107716,#107717,#107718,#107719,#107720,#107721,#107722,#107723,
#107724,#107725,#107726,#107727,#107728,#107729,#107730,#107731,#107732,
#107733,#107734,#107735,#107736,#107737,#107738,#107739,#107740,#107741,
#107742,#107743,#107744,#107745,#107746,#107747,#107748,#107749,#107750,
#107751,#107752,#107753,#107754,#107755,#107756),.UNSPECIFIED.,.F.,.F.,
(4,3,3,3,3,3,3,3,3,3,3,3,3,3,3,3,3,3,3,3,3,3,3,3,4),(0.,0.0434808822299742,
0.0869588497355593,0.130444807126091,0.173924303377971,0.217408477205238,
0.25,0.293489967069525,0.336977356303322,0.380473012066834,0.423962292814937,
0.467456176409864,0.5,0.543489938002949,0.586977312558548,0.630472970571102,
0.673962260376084,0.717456157789405,0.75,0.793396057067662,0.836788578850184,
0.880190246262028,0.923586689734074,0.966991615126708,1.),.UNSPECIFIED.);
#29412=B_SPLINE_CURVE_WITH_KNOTS('',3,(#107761,#107762,#107763,#107764,
#107765,#107766),.UNSPECIFIED.,.F.,.F.,(4,1,1,4),(0.,0.03448275862069,0.06896551724138,
0.0937639678077082),.UNSPECIFIED.);
#29413=B_SPLINE_CURVE_WITH_KNOTS('',3,(#107899,#107900,#107901,#107902,
#107903,#107904,#107905,#107906,#107907,#107908,#107909,#107910,#107911,
#107912,#107913,#107914),.UNSPECIFIED.,.F.,.F.,(4,3,3,3,3,4),(0.,0.262965024567732,
0.294538946299642,0.575526066696717,0.749091361952922,1.),.UNSPECIFIED.);
#29414=B_SPLINE_CURVE_WITH_KNOTS('',3,(#108082,#108083,#108084,#108085,
#108086,#108087,#108088,#108089,#108090,#108091,#108092,#108093,#108094,
#108095,#108096,#108097,#108098,#108099),.UNSPECIFIED.,.F.,.F.,(4,2,2,1,
1,1,1,2,2,2,4),(6.6564892292755E-9,0.250000000000036,0.375000000000054,
0.437500000000063,0.468750000000068,0.48437500000007,0.492187500000071,
0.499023437500072,0.500000000000072,0.750000000000036,1.),.UNSPECIFIED.);
#29415=B_SPLINE_CURVE_WITH_KNOTS('',3,(#108100,#108101,#108102,#108103,
#108104,#108105,#108106,#108107,#108108,#108109,#108110,#108111,#108112,
#108113,#108114,#108115,#108116,#108117,#108118,#108119,#108120,#108121,
#108122,#108123,#108124,#108125,#108126,#108127,#108128,#108129,#108130,
#108131,#108132,#108133,#108134,#108135,#108136),.UNSPECIFIED.,.F.,.F.,
(4,3,3,3,3,3,3,3,3,3,3,3,4),(0.608849847266439,0.6363636363636,0.685017726170025,
0.7272727272727,0.780361478699975,0.786226863948396,0.8181818181818,0.863485254733718,
0.887113979905965,0.9090909090909,0.952071682476561,0.989449454899762,1.),
 .UNSPECIFIED.);
#29416=B_SPLINE_CURVE_WITH_KNOTS('',3,(#108211,#108212,#108213,#108214,
#108215,#108216,#108217,#108218,#108219,#108220,#108221,#108222,#108223,
#108224,#108225,#108226,#108227,#108228,#108229,#108230,#108231,#108232),
 .UNSPECIFIED.,.F.,.F.,(4,2,2,2,2,2,2,2,2,2,4),(-0.940544117189131,-0.619332516558265,
-0.444109071613271,-0.412240309690337,-0.3952445331146,-0.38272974366006,
-0.370302866822156,-0.352494573845886,-0.317827384886972,-0.229879312811828,
-2.62880783342726E-6),.UNSPECIFIED.);
#29417=B_SPLINE_CURVE_WITH_KNOTS('',3,(#108234,#108235,#108236,#108237,
#108238,#108239,#108240,#108241,#108242,#108243,#108244,#108245),
 .UNSPECIFIED.,.F.,.F.,(4,2,2,2,2,4),(-1.93111365758677,-1.63478602703977,
-1.39013179726251,-0.863381002602519,-0.454372300253159,-2.62886509751779E-6),
 .UNSPECIFIED.);
#29418=B_SPLINE_CURVE_WITH_KNOTS('',3,(#108247,#108248,#108249,#108250,
#108251,#108252),.UNSPECIFIED.,.F.,.F.,(4,2,4),(-0.159887729495531,-0.0801211550522599,
-7.07627439308216E-6),.UNSPECIFIED.);
#29419=B_SPLINE_CURVE_WITH_KNOTS('',3,(#108254,#108255,#108256,#108257,
#108258,#108259,#108260,#108261,#108262,#108263,#108264,#108265),
 .UNSPECIFIED.,.F.,.F.,(4,2,2,2,2,4),(-0.109162067299797,-0.0810886277464997,
-0.0548476741806072,-0.0268518386947001,-0.013401596358416,-1.00000063842087E-6),
 .UNSPECIFIED.);
#29420=B_SPLINE_CURVE_WITH_KNOTS('',3,(#108268,#108269,#108270,#108271,
#108272,#108273,#108274,#108275,#108276,#108277,#108278,#108279),
 .UNSPECIFIED.,.F.,.F.,(4,2,2,2,2,4),(2.14051970094785E-5,0.0296331551158527,
0.0592663102294422,0.118532620456621,0.233984090001705,0.34943555954679),
 .UNSPECIFIED.);
#29421=B_SPLINE_CURVE_WITH_KNOTS('',3,(#108285,#108286,#108287,#108288,
#108289,#108290,#108291,#108292,#108293,#108294,#108295,#108296,#108297,
#108298,#108299,#108300,#108301,#108302,#108303,#108304,#108305,#108306,
#108307,#108308,#108309,#108310,#108311,#108312,#108313,#108314,#108315,
#108316,#108317,#108318,#108319,#108320,#108321,#108322,#108323,#108324,
#108325,#108326,#108327,#108328,#108329,#108330,#108331,#108332,#108333,
#108334,#108335,#108336,#108337,#108338,#108339,#108340,#108341,#108342,
#108343,#108344,#108345,#108346,#108347,#108348,#108349,#108350,#108351,
#108352,#108353,#108354,#108355,#108356,#108357,#108358,#108359,#108360,
#108361,#108362,#108363,#108364,#108365,#108366,#108367,#108368,#108369,
#108370,#108371,#108372,#108373,#108374,#108375,#108376,#108377,#108378,
#108379,#108380,#108381,#108382,#108383,#108384,#108385,#108386,#108387,
#108388,#108389,#108390,#108391,#108392,#108393,#108394,#108395,#108396,
#108397,#108398,#108399,#108400,#108401,#108402,#108403,#108404,#108405,
#108406,#108407,#108408,#108409,#108410,#108411,#108412,#108413,#108414,
#108415,#108416,#108417,#108418,#108419,#108420,#108421,#108422,#108423,
#108424,#108425,#108426,#108427,#108428,#108429,#108430,#108431,#108432,
#108433,#108434,#108435,#108436,#108437,#108438,#108439,#108440,#108441,
#108442,#108443,#108444,#108445,#108446,#108447,#108448,#108449,#108450,
#108451,#108452,#108453,#108454,#108455,#108456,#108457,#108458,#108459,
#108460,#108461,#108462,#108463,#108464,#108465,#108466,#108467,#108468,
#108469,#108470,#108471),.UNSPECIFIED.,.F.,.F.,(4,3,3,3,3,3,3,3,3,3,3,3,
3,3,3,3,3,3,3,3,3,3,3,3,3,3,3,3,3,3,3,3,3,3,3,3,3,3,3,3,3,3,3,3,3,3,3,3,
3,3,3,3,3,3,3,3,3,3,3,3,3,3,4),(0.,0.0329872437640412,0.0654476758840371,
0.0969825963291745,0.124999999999463,0.15624999999933,0.185079449321472,
0.187499999999197,0.215101382804894,0.218749999999062,0.234374999998994,
0.242187499998957,0.24609374999894,0.248046874998929,0.249654188187563,
0.249999999998917,0.281763147934628,0.313158438634503,0.344079219316766,
0.374999999999029,0.406249999999055,0.435043122561979,0.437499999999081,
0.465242747494911,0.468749999999105,0.484374999999117,0.492187499999128,
0.496093749999134,0.498046874999133,0.499630666281772,0.499999999999131,
0.534013529034568,0.567884321792066,0.601244268276834,0.624999999999322,
0.656249999999369,0.687499999999416,0.713991711576831,0.718749999999463,
0.734374999999486,0.742187499999503,0.746739145083346,0.749999999999519,
0.773629762604092,0.797741505499532,0.822215741749771,0.847347843083106,
0.854183532832394,0.87006509986984,0.886169192967915,0.902675549776158,
0.905747160718163,0.91628137237736,0.927109967024123,0.938187604547772,
0.94978201511235,0.952873580359081,0.961664311184405,0.972461163011459,
0.98111395701081,0.988582770586387,0.994957883184895,1.),.UNSPECIFIED.);
#29422=B_SPLINE_CURVE_WITH_KNOTS('',3,(#108472,#108473,#108474,#108475,
#108476,#108477,#108478,#108479,#108480,#108481,#108482,#108483,#108484,
#108485,#108486,#108487,#108488,#108489,#108490,#108491,#108492,#108493,
#108494,#108495,#108496,#108497,#108498,#108499,#108500,#108501,#108502,
#108503,#108504,#108505,#108506,#108507,#108508,#108509,#108510,#108511,
#108512,#108513,#108514,#108515,#108516,#108517,#108518,#108519,#108520,
#108521,#108522,#108523,#108524,#108525,#108526,#108527,#108528,#108529,
#108530,#108531,#108532,#108533,#108534,#108535,#108536,#108537,#108538,
#108539,#108540,#108541,#108542,#108543,#108544),.UNSPECIFIED.,.F.,.F.,
(4,3,3,3,3,3,3,3,3,3,3,3,3,3,3,3,3,3,3,3,3,3,3,3,4),(0.,0.0433422658552247,
0.086676909263646,0.13001585118668,0.173347263402444,0.216684760879611,
0.25,0.293486389657058,0.336970195806956,0.380462253926406,0.423947924714859,
0.46743817868338,0.5,0.543486382048098,0.586970181756904,0.63046223937264,
0.673947914476551,0.717438182744027,0.75,0.793486863123022,0.836971158394904,
0.88046371763125,0.923949893701111,0.967440645880335,0.999992112340553),
 .UNSPECIFIED.);
#29423=B_SPLINE_CURVE_WITH_KNOTS('',3,(#108618,#108619,#108620,#108621,
#108622,#108623,#108624,#108625,#108626,#108627,#108628,#108629,#108630,
#108631,#108632,#108633,#108634),.UNSPECIFIED.,.F.,.F.,(4,1,1,1,1,1,1,1,
1,1,1,1,1,1,4),(0.,0.07142857142857,0.1428571428571,0.2142857142857,0.2857142857143,
0.3571428571429,0.4285714285714,0.5,0.5714285714286,0.6428571428571,0.7142857142857,
0.7857142857143,0.8571428571429,0.9285714285714,0.999986468334629),
 .UNSPECIFIED.);
#29424=B_SPLINE_CURVE_WITH_KNOTS('',3,(#108636,#108637,#108638,#108639,
#108640,#108641,#108642,#108643,#108644,#108645,#108646,#108647,#108648,
#108649,#108650,#108651,#108652,#108653,#108654,#108655,#108656,#108657,
#108658,#108659,#108660,#108661,#108662,#108663,#108664,#108665,#108666),
 .UNSPECIFIED.,.F.,.F.,(4,3,3,3,3,3,3,3,3,3,4),(0.,0.115432015922713,0.229642812946616,
0.343276270183446,0.456483616450404,0.5,0.613381340000953,0.727229291454172,
0.841467570588938,0.956691948556023,1.),.UNSPECIFIED.);
#29425=B_SPLINE_CURVE_WITH_KNOTS('',3,(#108667,#108668,#108669,#108670,
#108671,#108672,#108673,#108674,#108675,#108676,#108677,#108678,#108679,
#108680,#108681,#108682,#108683,#108684,#108685,#108686,#108687,#108688,
#108689,#108690,#108691,#108692,#108693,#108694,#108695,#108696,#108697,
#108698,#108699,#108700,#108701,#108702,#108703,#108704,#108705,#108706,
#108707,#108708,#108709,#108710,#108711,#108712,#108713,#108714,#108715,
#108716,#108717,#108718,#108719,#108720,#108721,#108722,#108723,#108724,
#108725,#108726,#108727,#108728,#108729,#108730,#108731,#108732,#108733,
#108734,#108735,#108736,#108737,#108738,#108739,#108740,#108741,#108742,
#108743,#108744,#108745,#108746,#108747,#108748,#108749,#108750,#108751,
#108752,#108753,#108754,#108755,#108756,#108757,#108758,#108759,#108760),
 .UNSPECIFIED.,.F.,.F.,(4,3,3,3,3,3,3,3,3,3,3,3,3,3,3,3,3,3,3,3,3,3,3,3,
3,3,3,3,3,3,3,4),(0.,0.0345582872736374,0.0929845941816202,0.157419102930535,
0.221550743226399,0.22882816245317,0.24999999999998,0.308202198694642,0.38790552997828,
0.396561948834285,0.437499999999966,0.468749999999965,0.484374999999963,
0.492187499999963,0.494958900481429,0.496093749999963,0.498046874999963,
0.499999999999962,0.545721469363609,0.56291392955358,0.608712744210545,
0.631330920648744,0.678550479743205,0.702223009876759,0.749999999999981,
0.775856937482844,0.824689978755202,0.853522500825404,0.902667675715774,
0.936704266922385,0.986072527972056,1.),.UNSPECIFIED.);
#29426=B_SPLINE_CURVE_WITH_KNOTS('',3,(#108789,#108790,#108791,#108792,
#108793,#108794,#108795,#108796,#108797,#108798,#108799,#108800,#108801,
#108802,#108803,#108804),.UNSPECIFIED.,.F.,.F.,(4,3,3,3,3,4),(0.,0.282010262916946,
0.574348464349707,0.70424617169464,0.982799336161222,1.),.UNSPECIFIED.);
#29427=B_SPLINE_CURVE_WITH_KNOTS('',3,(#108805,#108806,#108807,#108808,
#108809,#108810,#108811,#108812,#108813,#108814,#108815,#108816,#108817,
#108818,#108819,#108820,#108821,#108822,#108823),.UNSPECIFIED.,.F.,.F.,
(4,3,3,3,3,3,4),(0.925378193668854,0.92910797034335,0.9487179487179,0.954912373067182,
0.974358974359,0.980737698040363,1.),.UNSPECIFIED.);
#29428=B_SPLINE_CURVE_WITH_KNOTS('',3,(#108965,#108966,#108967,#108968,
#108969,#108970,#108971,#108972,#108973,#108974,#108975,#108976,#108977,
#108978,#108979,#108980,#108981,#108982),.UNSPECIFIED.,.F.,.F.,(4,2,2,2,
1,1,1,1,2,2,4),(0.,0.124999999999973,0.249999999999946,0.37499999999992,
0.437499999999906,0.4687499999999,0.484374999999896,0.492187499999895,0.499023437499893,
0.499999999999893,1.),.UNSPECIFIED.);
#29429=B_SPLINE_CURVE_WITH_KNOTS('',3,(#109081,#109082,#109083,#109084,
#109085,#109086,#109087,#109088,#109089,#109090,#109091,#109092,#109093,
#109094,#109095,#109096,#109097,#109098,#109099,#109100,#109101,#109102,
#109103,#109104,#109105,#109106,#109107,#109108,#109109,#109110,#109111,
#109112,#109113,#109114,#109115,#109116,#109117,#109118,#109119,#109120),
 .UNSPECIFIED.,.F.,.F.,(4,3,3,3,3,3,3,3,3,3,3,3,3,4),(5.38788773699695E-8,
0.0227676697894301,0.0252326097521616,0.0647859254359117,0.09090909090909,
0.125968648152783,0.1688459408452,0.1818181818182,0.220252907477361,0.225296523956686,
0.2727272727273,0.325087831629694,0.3636363636364,0.379334069832486),
 .UNSPECIFIED.);
#29430=B_SPLINE_CURVE_WITH_KNOTS('',3,(#109127,#109128,#109129,#109130,
#109131,#109132,#109133,#109134,#109135,#109136,#109137,#109138,#109139,
#109140,#109141,#109142,#109143,#109144,#109145,#109146,#109147,#109148,
#109149,#109150,#109151,#109152,#109153,#109154,#109155,#109156,#109157,
#109158,#109159,#109160,#109161,#109162,#109163,#109164,#109165,#109166,
#109167,#109168,#109169,#109170),.UNSPECIFIED.,.F.,.F.,(4,2,2,2,2,2,2,2,
2,2,2,2,2,2,2,2,2,2,2,2,2,4),(2.64508255509259,2.67742444567248,2.83696368675036,
2.91868445378747,3.08595278393744,3.2459923366502,3.56763265862368,3.89772471020104,
4.11625324465983,4.27602450013281,4.44011329228324,4.52179781769355,4.68127923539211,
4.85058653401297,5.01076125898609,5.34010312659572,5.4997579249911,5.65126686288735,
5.80859392641738,6.13704517509721,6.31195283117778,6.49346299030963),
 .UNSPECIFIED.);
#29431=B_SPLINE_CURVE_WITH_KNOTS('',3,(#109173,#109174,#109175,#109176,
#109177,#109178,#109179,#109180,#109181,#109182,#109183,#109184,#109185,
#109186,#109187,#109188,#109189,#109190,#109191,#109192,#109193,#109194,
#109195,#109196),.UNSPECIFIED.,.F.,.F.,(4,2,2,2,2,2,2,2,2,2,2,4),(4.15472255972604E-5,
0.17982649437324,0.358364203739333,0.537917209024395,0.774537605184956,
0.933638986493987,1.09395573577978,1.42368019863028,1.5488568065964,1.88031437861517,
2.03196092149598,2.18921446062996),.UNSPECIFIED.);
#29432=B_SPLINE_CURVE_WITH_KNOTS('',3,(#109199,#109200,#109201,#109202,
#109203,#109204,#109205,#109206,#109207,#109208,#109209,#109210,#109211,
#109212,#109213,#109214,#109215,#109216,#109217,#109218,#109219,#109220,
#109221,#109222,#109223,#109224,#109225,#109226,#109227,#109228,#109229,
#109230,#109231,#109232,#109233,#109234,#109235,#109236,#109237,#109238,
#109239,#109240,#109241,#109242,#109243,#109244,#109245,#109246,#109247,
#109248,#109249,#109250,#109251,#109252),.UNSPECIFIED.,.F.,.F.,(4,2,2,2,
2,2,2,2,2,2,2,2,2,2,2,2,2,2,2,2,2,2,2,2,2,2,4),(1.00000000832767E-6,0.0937993211963754,
0.186006529692417,0.371316915687891,0.51521015489977,0.762878301760565,
0.929855471078699,1.26119411668655,1.38653891902511,1.54201439058365,1.77748339152866,
2.01600554589248,2.21643358592222,2.45329646508949,2.64837263290439,2.94654123765676,
3.13520341574287,3.27613465667508,3.60835599039887,3.77341017939711,3.93955099501437,
4.17631270410318,4.33609163100963,4.67139221186229,4.81889318040861,5.08150161034807,
5.28919429578275),.UNSPECIFIED.);
#29433=B_SPLINE_CURVE_WITH_KNOTS('',3,(#109256,#109257,#109258,#109259,
#109260,#109261,#109262,#109263),.UNSPECIFIED.,.F.,.F.,(4,2,2,4),(3.00455393844332E-5,
0.103997999408186,0.20738927106044,0.414937403627889),.UNSPECIFIED.);
#29434=B_SPLINE_CURVE_WITH_KNOTS('',3,(#109265,#109266,#109267,#109268,
#109269,#109270,#109271,#109272,#109273,#109274,#109275,#109276,#109277,
#109278,#109279,#109280,#109281,#109282,#109283,#109284,#109285,#109286,
#109287,#109288,#109289,#109290,#109291,#109292,#109293,#109294),
 .UNSPECIFIED.,.F.,.F.,(4,2,2,2,2,2,2,2,2,2,2,2,2,2,4),(0.000332275491302904,
0.0840966458402627,0.166687246349549,0.242589704370946,0.456211102935291,
0.570011730232724,0.811990911514058,0.947245253154911,1.11349936008019,
1.2791925587542,1.60988734602343,1.76049112393223,1.97945211479166,2.10332751572814,
2.22822768913076),.UNSPECIFIED.);
#29435=B_SPLINE_CURVE_WITH_KNOTS('',3,(#109295,#109296,#109297,#109298,
#109299,#109300,#109301,#109302,#109303,#109304,#109305,#109306,#109307,
#109308,#109309,#109310,#109311,#109312,#109313,#109314,#109315,#109316,
#109317,#109318,#109319,#109320,#109321,#109322),.UNSPECIFIED.,.F.,.F.,
(4,2,2,2,2,2,2,2,2,2,2,2,2,4),(9.99999997225233E-7,0.316380988376829,0.420339193601812,
0.746639351878567,0.902016774938394,1.06080893086254,1.22053675681677,1.54934292636645,
1.70751623430856,1.85716806248915,2.01680576343376,2.34625710726857,2.50713459399319,
2.64508255509259),.UNSPECIFIED.);
#29436=B_SPLINE_CURVE_WITH_KNOTS('',3,(#109327,#109328,#109329,#109330,
#109331,#109332,#109333,#109334,#109335,#109336,#109337,#109338,#109339,
#109340,#109341,#109342,#109343,#109344,#109345,#109346,#109347,#109348,
#109349,#109350,#109351,#109352,#109353,#109354,#109355,#109356,#109357,
#109358,#109359,#109360,#109361,#109362,#109363,#109364,#109365,#109366,
#109367,#109368,#109369,#109370,#109371,#109372,#109373,#109374,#109375,
#109376,#109377,#109378),.UNSPECIFIED.,.F.,.F.,(4,2,2,2,2,2,2,2,2,2,2,2,
2,2,2,2,2,2,2,2,2,2,2,2,2,4),(1.08729832187199,1.17595088380344,1.33778570454322,
1.61392601185733,1.7757756305946,2.05493223416506,2.21679753879183,2.54025561678765,
2.7026900931946,2.86620583049052,3.18933753411709,3.35213283091687,3.67938788358257,
3.84130843842076,4.17584086404189,4.33859835896819,4.50095601740349,4.66406304349631,
4.99307628290177,5.15514214643947,5.48970140028481,5.57141128126531,5.89662036271308,
6.01657896885547,6.19774098437255,6.37927915487514),.UNSPECIFIED.);
#29437=B_SPLINE_CURVE_WITH_KNOTS('',3,(#109380,#109381,#109382,#109383,
#109384,#109385,#109386,#109387,#109388,#109389,#109390,#109391,#109392,
#109393,#109394,#109395,#109396,#109397,#109398,#109399,#109400,#109401,
#109402,#109403,#109404,#109405,#109406,#109407,#109408,#109409,#109410,
#109411,#109412,#109413,#109414,#109415,#109416,#109417,#109418,#109419,
#109420,#109421,#109422,#109423,#109424,#109425,#109426,#109427,#109428,
#109429,#109430,#109431),.UNSPECIFIED.,.F.,.F.,(4,2,2,2,2,2,2,2,2,2,2,2,
2,2,2,2,2,2,2,2,2,2,2,2,2,4),(5.28919429578275,5.3324848721458,5.49310439715847,
5.73141270289315,5.96292206244042,6.11206963141141,6.25697378422631,6.58716063505421,
6.79605341158305,7.04034155290596,7.19896984076246,7.43590957632683,7.59911565187969,
7.85553254220341,7.99989361468925,8.33497198064668,8.49404727731464,8.73066918018472,
8.90981619304874,9.07479140820227,9.40588960985194,9.55500945800335,9.70146218968651,
9.81681549265543,9.98709458790283,10.1622070063764),.UNSPECIFIED.);
#29438=B_SPLINE_CURVE_WITH_KNOTS('',3,(#109432,#109433,#109434,#109435,
#109436,#109437),.UNSPECIFIED.,.F.,.F.,(4,2,4),(9.84111781119226E-6,0.225748591139482,
0.415214370670141),.UNSPECIFIED.);
#29439=B_SPLINE_CURVE_WITH_KNOTS('',3,(#109443,#109444,#109445,#109446,
#109447,#109448,#109449,#109450,#109451,#109452,#109453,#109454),
 .UNSPECIFIED.,.F.,.F.,(4,2,2,2,2,4),(-1.08694468321814,-0.849318901329702,
-0.686604059603595,-0.524313844518721,-0.264814390599367,-9.9999999880751E-7),
 .UNSPECIFIED.);
#29440=B_SPLINE_CURVE_WITH_KNOTS('',3,(#109458,#109459,#109460,#109461,
#109462,#109463),.UNSPECIFIED.,.F.,.F.,(4,2,4),(4.25996487515901E-5,0.058348665794391,
0.103898374931251),.UNSPECIFIED.);
#29441=B_SPLINE_CURVE_WITH_KNOTS('',3,(#109464,#109465,#109466,#109467,
#109468,#109469,#109470,#109471,#109472,#109473,#109474,#109475,#109476,
#109477,#109478,#109479,#109480,#109481,#109482,#109483,#109484,#109485,
#109486,#109487),.UNSPECIFIED.,.F.,.F.,(4,2,2,2,2,2,2,2,2,2,2,4),(-3.06207312432449,
-2.78609444561215,-2.51065494233778,-2.23496348902561,-1.90651189086599,
-1.69364069136703,-1.53125874524034,-1.36663044472209,-1.04803598247908,
-0.761188827947358,-0.444145659374973,-0.415211727770225),.UNSPECIFIED.);
#29442=B_SPLINE_CURVE_WITH_KNOTS('',3,(#109492,#109493,#109494,#109495,
#109496,#109497,#109498,#109499,#109500,#109501,#109502,#109503,#109504,
#109505,#109506,#109507,#109508,#109509,#109510,#109511,#109512,#109513,
#109514,#109515,#109516,#109517,#109518,#109519,#109520,#109521,#109522,
#109523,#109524,#109525,#109526,#109527,#109528,#109529,#109530,#109531,
#109532,#109533,#109534,#109535,#109536,#109537,#109538,#109539,#109540,
#109541,#109542,#109543),.UNSPECIFIED.,.F.,.F.,(4,2,2,2,2,2,2,2,2,2,2,2,
2,2,2,2,2,2,2,2,2,2,2,2,2,4),(-6.3789533061886,-6.19752540699852,-6.01647535816193,
-5.89659061833356,-5.57148058423157,-5.48976790348919,-5.15521209696545,
-4.99315258417474,-4.66417843590823,-4.50108218501608,-4.33870537818856,
-4.17593333632225,-3.84140152444433,-3.67948513698676,-3.35232154086754,
-3.18953825850364,-2.86636304145829,-2.70286273730807,-2.54041822649752,
-2.21681608328943,-2.05495155736083,-1.77714959629158,-1.61530229675366,
-1.34565532190014,-1.18376871477307,-1.08694468321814),.UNSPECIFIED.);
#29443=B_SPLINE_CURVE_WITH_KNOTS('',3,(#109545,#109546,#109547,#109548,
#109549,#109550),.UNSPECIFIED.,.F.,.F.,(4,2,4),(-0.415211727770225,-0.225749000382965,
-7.22216956189878E-6),.UNSPECIFIED.);
#29444=B_SPLINE_CURVE_WITH_KNOTS('',3,(#109551,#109552,#109553,#109554,
#109555,#109556,#109557,#109558,#109559,#109560,#109561,#109562,#109563,
#109564,#109565,#109566,#109567,#109568,#109569,#109570,#109571,#109572,
#109573,#109574,#109575,#109576,#109577,#109578,#109579,#109580,#109581,
#109582,#109583,#109584,#109585,#109586,#109587,#109588,#109589,#109590,
#109591,#109592,#109593,#109594,#109595,#109596,#109597,#109598,#109599,
#109600),.UNSPECIFIED.,.F.,.F.,(4,2,2,2,2,2,2,2,2,2,2,2,2,2,2,2,2,2,2,2,
2,2,2,2,4),(-10.162288201987,-9.95449044952228,-9.74761344805875,-9.61484561556136,
-9.28928775962058,-9.14607554855514,-8.89667320787399,-8.75278270818488,
-8.5120156150304,-8.30763540975586,-8.07065964378126,-7.91068566964841,
-7.57538438350904,-7.42685701181995,-7.16273754121012,-6.95127001708957,
-6.81320480002116,-6.59034568908175,-6.26098331233411,-6.12764696294493,
-5.97014605611139,-5.73247499024949,-5.49383205799769,-5.33310123773781,
-5.28894858945498),.UNSPECIFIED.);
#29445=B_SPLINE_CURVE_WITH_KNOTS('',3,(#109606,#109607,#109608,#109609,
#109610,#109611,#109612,#109613,#109614,#109615,#109616,#109617,#109618,
#109619,#109620,#109621,#109622,#109623,#109624,#109625,#109626,#109627,
#109628,#109629),.UNSPECIFIED.,.F.,.F.,(4,2,2,2,2,2,2,2,2,2,2,4),(-2.18921446063053,
-2.03196092150216,-1.88031437862538,-1.54885680660905,-1.42368019863116,
-1.09395573578003,-0.93363898649323,-0.774537605184621,-0.537917209023631,
-0.358364203732708,-0.179826494370147,-4.1547225594898E-5),
 .UNSPECIFIED.);
#29446=B_SPLINE_CURVE_WITH_KNOTS('',3,(#109632,#109633,#109634,#109635,
#109636,#109637,#109638,#109639,#109640,#109641,#109642,#109643,#109644,
#109645,#109646,#109647,#109648,#109649,#109650,#109651,#109652,#109653,
#109654,#109655,#109656,#109657,#109658,#109659,#109660,#109661,#109662,
#109663,#109664,#109665,#109666,#109667,#109668,#109669,#109670,#109671,
#109672,#109673,#109674,#109675,#109676,#109677),.UNSPECIFIED.,.F.,.F.,
(4,2,2,2,2,2,2,2,2,2,2,2,2,2,2,2,2,2,2,2,2,2,4),(-6.49276334357195,-6.26669129627648,
-6.04438319173055,-5.89990959341052,-5.74011293729422,-5.41181691433256,
-5.25476581773821,-5.10256055685507,-4.94289957223829,-4.6136056717894,
-4.45367107155358,-4.30712152953011,-4.14751266919742,-3.81785037133824,
-3.65541399409842,-3.48831833314667,-3.32879089951008,-3.24707909133012,
-3.08698762043823,-2.91705494880014,-2.83535718105171,-2.67585877419533,
-2.64509018645311),.UNSPECIFIED.);
#29447=B_SPLINE_CURVE_WITH_KNOTS('',3,(#109683,#109684,#109685,#109686,
#109687,#109688,#109689,#109690,#109691,#109692,#109693,#109694,#109695,
#109696,#109697,#109698,#109699,#109700,#109701,#109702,#109703,#109704,
#109705,#109706,#109707,#109708,#109709,#109710,#109711,#109712,#109713,
#109714,#109715,#109716,#109717,#109718,#109719,#109720,#109721,#109722),
 .UNSPECIFIED.,.F.,.F.,(4,2,2,2,2,2,2,2,2,2,2,2,2,2,2,2,2,2,2,4),(45.1636811624521,
45.1859895775379,45.2909818652286,45.5404043845585,45.7173330695028,45.8583336706336,
46.1022835664149,46.3125310429476,46.5254507861948,46.7755846171368,46.9899008738256,
47.1935127202563,47.4417976479436,47.6581123658742,47.8657808033474,48.1142491024031,
48.3347494994277,48.4289037755271,48.5489428743058,48.7694667551308),
 .UNSPECIFIED.);
#29448=B_SPLINE_CURVE_WITH_KNOTS('',3,(#109725,#109726,#109727,#109728,
#109729,#109730,#109731,#109732,#109733,#109734,#109735,#109736,#109737,
#109738,#109739,#109740,#109741,#109742,#109743,#109744,#109745,#109746,
#109747,#109748,#109749,#109750,#109751,#109752,#109753,#109754,#109755,
#109756,#109757,#109758,#109759,#109760,#109761,#109762,#109763,#109764),
 .UNSPECIFIED.,.F.,.F.,(4,2,2,2,2,2,2,2,2,2,2,2,2,2,2,2,2,2,2,4),(0.,0.2201415667957,
0.339971629687818,0.439268623717367,0.656555209190466,0.904321640813465,
1.10966254441214,1.32710919499732,1.57591624251713,1.7795942888701,1.99387887225677,
2.24400153032728,2.45689921852262,2.66715220225339,2.91106168072629,3.052663104263,
3.22941548161296,3.48018527327844,3.58427704060106,3.60575464092561),
 .UNSPECIFIED.);
#29449=B_SPLINE_CURVE_WITH_KNOTS('',3,(#109769,#109770,#109771,#109772,
#109773,#109774,#109775,#109776,#109777,#109778,#109779,#109780,#109781,
#109782,#109783,#109784,#109785,#109786,#109787,#109788,#109789,#109790,
#109791,#109792,#109793,#109794,#109795,#109796,#109797,#109798,#109799,
#109800,#109801,#109802,#109803,#109804,#109805,#109806,#109807,#109808,
#109809,#109810,#109811,#109812,#109813,#109814,#109815,#109816,#109817,
#109818,#109819,#109820,#109821,#109822,#109823,#109824,#109825,#109826,
#109827,#109828,#109829,#109830,#109831,#109832,#109833,#109834,#109835,
#109836,#109837,#109838,#109839,#109840,#109841,#109842,#109843,#109844,
#109845,#109846,#109847,#109848,#109849,#109850,#109851,#109852,#109853,
#109854,#109855,#109856,#109857,#109858,#109859,#109860,#109861,#109862,
#109863,#109864,#109865,#109866,#109867,#109868,#109869,#109870,#109871,
#109872,#109873,#109874,#109875,#109876,#109877,#109878,#109879,#109880),
 .UNSPECIFIED.,.F.,.F.,(4,2,2,2,2,2,2,2,2,2,2,2,2,2,2,2,2,2,2,2,2,2,2,2,
2,2,2,2,2,2,2,2,2,2,2,2,2,2,2,2,2,2,2,2,2,2,2,2,2,2,2,2,2,2,2,4),(34.4761216253511,
34.4979172951594,34.6023693954826,34.8526887743558,35.0295472782581,35.1709371656285,
35.4189309688937,35.6359352997608,35.8328963334246,35.9362065969497,36.1876018834163,
36.3639547026121,36.5070333217856,36.7546764575407,36.971106225807,37.1692923075338,
37.2730069669589,37.524393883275,37.7010920830533,37.8430292585465,38.0906378467652,
38.3070037787261,38.5053127979877,38.6090676395425,38.8603863189785,39.0370895140391,
39.1789876391809,39.4263179204561,39.6421303069469,39.8416408578658,39.9458004001765,
40.1965152151265,40.3732998895649,40.5148766763876,40.7643540376504,40.9849038360371,
41.1837686424467,41.4322349228299,41.6466582370236,41.8500979980946,42.0970191531081,
42.3106845724003,42.5150805514149,42.6209619147639,42.869039564485,43.0461288157834,
43.1866492687327,43.4306106150213,43.6408570981889,43.8538204907908,44.1039835109216,
44.3183594933174,44.5218709671828,44.7693560633028,44.9840659861086,45.1636811624521),
 .UNSPECIFIED.);
#29450=B_SPLINE_CURVE_WITH_KNOTS('',3,(#109881,#109882,#109883,#109884,
#109885,#109886,#109887,#109888,#109889,#109890,#109891,#109892,#109893,
#109894,#109895,#109896,#109897,#109898,#109899,#109900,#109901,#109902,
#109903,#109904,#109905,#109906,#109907,#109908,#109909,#109910,#109911,
#109912,#109913,#109914,#109915,#109916,#109917,#109918,#109919,#109920,
#109921,#109922,#109923,#109924,#109925,#109926,#109927,#109928,#109929,
#109930,#109931,#109932,#109933,#109934,#109935,#109936,#109937,#109938,
#109939,#109940,#109941,#109942,#109943,#109944,#109945,#109946,#109947,
#109948,#109949,#109950,#109951,#109952,#109953,#109954,#109955,#109956,
#109957,#109958,#109959,#109960,#109961,#109962,#109963,#109964,#109965,
#109966,#109967,#109968,#109969,#109970,#109971,#109972,#109973,#109974,
#109975,#109976,#109977,#109978,#109979,#109980,#109981,#109982,#109983,
#109984,#109985,#109986,#109987,#109988,#109989,#109990,#109991,#109992),
 .UNSPECIFIED.,.F.,.F.,(4,2,2,2,2,2,2,2,2,2,2,2,2,2,2,2,2,2,2,2,2,2,2,2,
2,2,2,2,2,2,2,2,2,2,2,2,2,2,2,2,2,2,2,2,2,2,2,2,2,2,2,2,2,2,2,4),(3.60575464092561,
3.78359886408125,3.99946083484741,4.24708388702773,4.39236370283358,4.56793595394828,
4.8186906336666,4.92138850485364,5.11647310940841,5.33431338911229,5.58259250518372,
5.72459723690218,5.9012529332293,6.15275589785826,6.25635973945805,6.45422443026423,
6.67076629369559,6.91871291519129,7.06376525715824,7.23942224292656,7.49025154511468,
7.59301626702443,7.78830418819424,8.00606241048629,8.25472024889112,8.45938882436026,
8.6732843485801,8.92149695428521,9.12149373452797,9.34120210231813,9.59035578276094,
9.73190774048285,9.90870126959051,10.159367954283,10.2635642219125,10.398281453743,
10.5764045119693,10.807132946455,10.923513855605,11.1373467101536,11.3475658062745,
11.5943089788604,11.8094599884568,12.0189302366049,12.263042231856,12.466391556441,
12.68088166963,12.9311089195156,13.1441582158934,13.3544140888988,13.5983720406559,
13.7397004466345,13.9165747479684,14.1667613476217,14.2713015560327,14.2931793607378),
 .UNSPECIFIED.);
#29451=B_SPLINE_CURVE_WITH_KNOTS('',3,(#109997,#109998,#109999,#110000,
#110001,#110002,#110003,#110004,#110005,#110006,#110007,#110008,#110009,
#110010,#110011,#110012,#110013,#110014,#110015,#110016,#110017,#110018,
#110019,#110020,#110021,#110022,#110023,#110024,#110025,#110026,#110027,
#110028,#110029,#110030,#110031,#110032,#110033,#110034,#110035,#110036,
#110037,#110038,#110039,#110040,#110041,#110042,#110043,#110044,#110045,
#110046,#110047,#110048,#110049,#110050,#110051,#110052,#110053,#110054,
#110055,#110056,#110057,#110058,#110059,#110060,#110061,#110062,#110063,
#110064,#110065,#110066,#110067,#110068,#110069,#110070,#110071,#110072,
#110073,#110074,#110075,#110076,#110077,#110078,#110079,#110080,#110081,
#110082,#110083,#110084,#110085,#110086,#110087,#110088,#110089,#110090,
#110091,#110092,#110093,#110094,#110095,#110096,#110097,#110098,#110099,
#110100,#110101,#110102,#110103,#110104,#110105,#110106,#110107,#110108,
#110109,#110110),.UNSPECIFIED.,.F.,.F.,(4,2,2,2,2,2,2,2,2,2,2,2,2,2,2,2,
2,2,2,2,2,2,2,2,2,2,2,2,2,2,2,2,2,2,2,2,2,2,2,2,2,2,2,2,2,2,2,2,2,2,2,2,
2,2,2,2,4),(23.7864907164679,23.8600639976838,24.0542846994271,24.3840968250959,
24.4971715165633,24.6330208701138,24.8469376514058,25.0346122986433,25.1606329989249,
25.2855425024337,25.5042341007853,25.6834576792019,25.8267691843993,25.9520184150769,
26.1697796229055,26.3490328893123,26.481026560496,26.5857283218547,26.835737628172,
27.0126691422952,27.1539259336804,27.4033991467519,27.6237508415675,27.8230105963696,
28.0714965084728,28.2858833510739,28.4895842322703,28.7380762425912,28.9547166091719,
29.1525471320625,29.2561491615275,29.50776076928,29.6844576808734,29.8265266170278,
30.0751049001722,30.2935384751636,30.4932806994328,30.6019456262967,30.845689151055,
31.0231916363084,31.1626154796419,31.4119757064893,31.6321290211168,31.8316181013685,
32.0800461296406,32.2943364330095,32.4982050554351,32.7422107336455,32.9517436244225,
33.1667909413486,33.4109673000422,33.6180184359698,33.8403444537529,33.9603314256126,
34.1855282423232,34.3640236325502,34.4761216253511),.UNSPECIFIED.);
#29452=B_SPLINE_CURVE_WITH_KNOTS('',3,(#110111,#110112,#110113,#110114,
#110115,#110116,#110117,#110118,#110119,#110120,#110121,#110122,#110123,
#110124,#110125,#110126,#110127,#110128,#110129,#110130,#110131,#110132,
#110133,#110134,#110135,#110136,#110137,#110138,#110139,#110140,#110141,
#110142,#110143,#110144,#110145,#110146,#110147,#110148,#110149,#110150,
#110151,#110152,#110153,#110154,#110155,#110156,#110157,#110158,#110159,
#110160,#110161,#110162,#110163,#110164,#110165,#110166,#110167,#110168,
#110169,#110170,#110171,#110172,#110173,#110174,#110175,#110176,#110177,
#110178,#110179,#110180,#110181,#110182,#110183,#110184,#110185,#110186,
#110187,#110188,#110189,#110190,#110191,#110192,#110193,#110194,#110195,
#110196,#110197,#110198,#110199,#110200,#110201,#110202,#110203,#110204,
#110205,#110206,#110207,#110208,#110209,#110210,#110211,#110212,#110213,
#110214,#110215,#110216,#110217,#110218),.UNSPECIFIED.,.F.,.F.,(4,2,2,2,
2,2,2,2,2,2,2,2,2,2,2,2,2,2,2,2,2,2,2,2,2,2,2,2,2,2,2,2,2,2,2,2,2,2,2,2,
2,2,2,2,2,2,2,2,2,2,2,2,2,4),(14.2931793607378,14.4719098425484,14.6872583759001,
14.9351026692841,15.1386971335507,15.3530966410328,15.6033037705098,15.8162964769165,
16.0265891038553,16.2706031058181,16.4112504626503,16.5883428601802,16.8367703417248,
16.9424796939961,17.1463839003186,17.3603166283152,17.6074137217094,17.8109118097724,
18.0253695011367,18.2738820176566,18.4728078227829,18.6933852905092,18.941885950872,
19.1507625149527,19.3629700308906,19.6117464009867,19.8250974060452,20.035279940003,
20.2791833581233,20.4206775644385,20.5975340742559,20.8480724242665,20.9524141261965,
21.0868029155594,21.2651217691753,21.4932588084231,21.6113526553399,21.8291758340079,
22.0379331058812,22.2817432043622,22.5020467265233,22.7097652725934,22.9539842354375,
23.0867579418792,23.3199522342735,23.4885961536804,23.6723009005603,23.916471372828,
24.1224173322998,24.3480071497465,24.4694211502622,24.6925614637182,24.8712489134122,
24.9828701266438),.UNSPECIFIED.);
#29453=B_SPLINE_CURVE_WITH_KNOTS('',3,(#110223,#110224,#110225,#110226,
#110227,#110228,#110229,#110230,#110231,#110232,#110233,#110234,#110235,
#110236,#110237,#110238,#110239,#110240,#110241,#110242,#110243,#110244,
#110245,#110246,#110247,#110248,#110249,#110250,#110251,#110252,#110253,
#110254,#110255,#110256,#110257,#110258,#110259,#110260,#110261,#110262,
#110263,#110264,#110265,#110266,#110267,#110268,#110269,#110270,#110271,
#110272,#110273,#110274,#110275,#110276,#110277,#110278,#110279,#110280,
#110281,#110282,#110283,#110284,#110285,#110286,#110287,#110288,#110289,
#110290,#110291,#110292,#110293,#110294,#110295,#110296,#110297,#110298,
#110299,#110300,#110301,#110302,#110303,#110304,#110305,#110306,#110307,
#110308,#110309,#110310,#110311,#110312,#110313,#110314,#110315,#110316,
#110317,#110318,#110319,#110320,#110321,#110322,#110323,#110324,#110325,
#110326,#110327,#110328,#110329,#110330,#110331,#110332,#110333,#110334,
#110335,#110336,#110337,#110338),.UNSPECIFIED.,.F.,.F.,(4,2,2,2,2,2,2,2,
2,2,2,2,2,2,2,2,2,2,2,2,2,2,2,2,2,2,2,2,2,2,2,2,2,2,2,2,2,2,2,2,2,2,2,2,
2,2,2,2,2,2,2,2,2,2,2,2,2,4),(13.0972599015927,13.2088828109584,13.3875334083998,
13.6107174250379,13.7320572875133,13.9574866046717,14.1634411494772,14.4074934721232,
14.6198640778286,14.830385732743,15.0744021000641,15.2121076743174,15.3901968600944,
15.6232620182162,15.7384871167831,15.9428362432387,16.1617584586995,16.4106155859748,
16.552127272608,16.7289621853694,16.9795405830886,17.0838343658739,17.2183386710432,
17.3965893870818,17.6255881568458,17.7431067818442,17.9442863416335,18.1631905505658,
18.4147148656307,18.6302600478368,18.8396270523619,19.0836785105287,19.2870272477183,
19.5015598569899,19.7501128405144,19.9487018496239,20.1695396125155,20.4190495433896,
20.5567802222878,20.7348844425986,20.9680455918345,21.0832382004914,21.2873872231948,
21.5064642813777,21.7554244536792,21.8966798707429,22.0736115378505,22.3236200606198,
22.4283237575531,22.5602905911023,22.7395532376602,22.9572385707407,23.0825455561075,
23.2257497280802,23.4050230633458,23.5985515058283,23.7392262097004,23.7864907164679),
 .UNSPECIFIED.);
#29454=B_SPLINE_CURVE_WITH_KNOTS('',3,(#110339,#110340,#110341,#110342,
#110343,#110344,#110345,#110346,#110347,#110348,#110349,#110350,#110351,
#110352,#110353,#110354,#110355,#110356,#110357,#110358,#110359,#110360,
#110361,#110362,#110363,#110364,#110365,#110366,#110367,#110368,#110369,
#110370,#110371,#110372,#110373,#110374,#110375,#110376,#110377,#110378,
#110379,#110380,#110381,#110382,#110383,#110384,#110385,#110386,#110387,
#110388,#110389,#110390,#110391,#110392,#110393,#110394,#110395,#110396,
#110397,#110398,#110399,#110400,#110401,#110402,#110403,#110404,#110405,
#110406,#110407,#110408,#110409,#110410,#110411,#110412,#110413,#110414,
#110415,#110416,#110417,#110418,#110419,#110420,#110421,#110422,#110423,
#110424,#110425,#110426,#110427,#110428,#110429,#110430,#110431,#110432,
#110433,#110434,#110435,#110436,#110437,#110438,#110439,#110440,#110441,
#110442,#110443,#110444,#110445,#110446,#110447,#110448,#110449,#110450),
 .UNSPECIFIED.,.F.,.F.,(4,2,2,2,2,2,2,2,2,2,2,2,2,2,2,2,2,2,2,2,2,2,2,2,
2,2,2,2,2,2,2,2,2,2,2,2,2,2,2,2,2,2,2,2,2,2,2,2,2,2,2,2,2,2,2,4),(24.9828701266438,
25.0047437426501,25.1092917244477,25.3595256298742,25.536425165321,25.6777802263797,
25.9269916394664,26.146704044784,26.3467271041175,26.5945217846717,26.8075316126368,
27.0144611916814,27.2623182684099,27.479834605962,27.6757810316877,27.7787657608995,
28.0298495783055,28.2057922252096,28.3501372639755,28.5941240660552,28.804267754094,
29.0176912708963,29.1270790527437,29.3696427046905,29.5472215910744,29.6864116441914,
29.9338935621333,30.1498971464094,30.3490772925246,30.4531295853532,30.7040580372953,
30.8808418343143,31.0225290299326,31.2706128526426,31.4878561599192,31.6843333167744,
31.7874871124857,32.0387306114881,32.2148840736119,32.3585605441454,32.6073592275527,
32.8260861401882,33.0307434417365,33.1460277507439,33.3789808560992,33.5570691230152,
33.6947547740834,33.944640995557,34.1665970254851,34.3635944165894,34.6121184634748,
34.8266361796678,35.0299201573721,35.2739093239344,35.4831982054315,35.6719042779843),
 .UNSPECIFIED.);
#29455=B_SPLINE_CURVE_WITH_KNOTS('',3,(#110457,#110458,#110459,#110460,
#110461,#110462,#110463,#110464,#110465,#110466,#110467,#110468,#110469,
#110470,#110471,#110472,#110473,#110474,#110475,#110476,#110477,#110478,
#110479,#110480,#110481,#110482),.UNSPECIFIED.,.F.,.F.,(4,2,2,2,2,2,2,2,
2,2,2,2,4),(1.0000000086885E-6,0.368005088305128,0.597205559032035,0.80384623486168,
1.04823515581348,1.26147811522057,1.47159759188732,1.71543402139935,1.85674376816772,
2.03357552274096,2.28373478672066,2.38823344563787,2.41008863111305),
 .UNSPECIFIED.);
#29456=B_SPLINE_CURVE_WITH_KNOTS('',3,(#110488,#110489,#110490,#110491,
#110492,#110493,#110494,#110495,#110496,#110497,#110498,#110499,#110500,
#110501,#110502,#110503,#110504,#110505,#110506,#110507,#110508,#110509,
#110510,#110511,#110512,#110513,#110514,#110515,#110516,#110517,#110518,
#110519,#110520,#110521,#110522,#110523,#110524,#110525,#110526,#110527,
#110528,#110529,#110530,#110531,#110532,#110533,#110534,#110535,#110536,
#110537,#110538,#110539,#110540,#110541,#110542,#110543,#110544,#110545,
#110546,#110547,#110548,#110549,#110550,#110551,#110552,#110553,#110554,
#110555,#110556,#110557,#110558,#110559,#110560,#110561,#110562,#110563,
#110564,#110565),.UNSPECIFIED.,.F.,.F.,(4,2,2,2,2,2,2,2,2,2,2,2,2,2,2,2,
2,2,2,2,2,2,2,2,2,2,2,2,2,2,2,2,2,2,2,2,2,2,4),(-6.04591668252116,-6.00476951035527,
-5.87222595335921,-5.67235526281456,-5.48950750851185,-5.36878304006732,
-5.24465029945799,-5.03006846521196,-4.84621171253538,-4.71821442823858,
-4.58567217775998,-4.38580592098932,-4.20296115284965,-4.08223804754818,
-3.95810761088525,-3.74352838666824,-3.55967449478355,-3.43167889162868,
-3.29913885159351,-3.09927498044057,-2.91643280631889,-2.79571164775362,
-2.67158286570741,-2.45700702974226,-2.27315580075226,-2.14516217087974,
-2.0126239935607,-1.8127632957672,-1.6299238664427,-1.50920443010279,-1.38507755238952,
-1.17050480527998,-0.986656315246761,-0.858664546249773,-0.72612836535116,
-0.518106196771695,-0.329531023944945,-0.208588893485145,0.),
 .UNSPECIFIED.);
#29457=B_SPLINE_CURVE_WITH_KNOTS('',3,(#110569,#110570,#110571,#110572,
#110573,#110574,#110575,#110576,#110577,#110578,#110579,#110580,#110581,
#110582,#110583,#110584,#110585,#110586,#110587,#110588,#110589,#110590,
#110591,#110592,#110593,#110594,#110595,#110596,#110597,#110598,#110599,
#110600,#110601,#110602,#110603,#110604,#110605,#110606,#110607,#110608,
#110609,#110610,#110611,#110612,#110613,#110614,#110615,#110616,#110617,
#110618,#110619,#110620,#110621,#110622,#110623,#110624,#110625,#110626,
#110627,#110628,#110629,#110630,#110631,#110632,#110633,#110634,#110635,
#110636,#110637,#110638,#110639,#110640,#110641,#110642,#110643,#110644,
#110645,#110646),.UNSPECIFIED.,.F.,.F.,(4,2,2,2,2,2,2,2,2,2,2,2,2,2,2,2,
2,2,2,2,2,2,2,2,2,2,2,2,2,2,2,2,2,2,2,2,2,2,4),(-44.7046953009418,-44.4961174550277,
-44.3751813824112,-44.1866150987334,-43.9786034224711,-43.8460746896715,
-43.7180893074422,-43.5342494045959,-43.319687980552,-43.1955677260083,
-43.0748545558397,-42.8920235107033,-42.6921725900386,-42.5596418820413,
-42.4316545870372,-42.2478119418575,-42.0332473087007,-41.9091252070089,
-41.7884102301501,-41.6055764593785,-41.4057225730062,-41.2731898792282,
-41.145200680294,-40.9613552867331,-40.7467874680579,-40.6226634994675,
-40.5019467336222,-40.3191102252629,-40.1192533109191,-39.9867186587913,
-39.8587275328118,-39.674879406461,-39.4603083407335,-39.3361825565139,
-39.2154639555481,-39.0326247405373,-38.8327649599833,-38.7002282780622,
-38.6590831067128),.UNSPECIFIED.);
#29458=B_SPLINE_CURVE_WITH_KNOTS('',3,(#110652,#110653,#110654,#110655,
#110656,#110657,#110658,#110659,#110660,#110661,#110662,#110663,#110664,
#110665,#110666,#110667,#110668,#110669,#110670,#110671,#110672,#110673,
#110674,#110675,#110676,#110677,#110678,#110679,#110680,#110681,#110682,
#110683,#110684,#110685,#110686,#110687,#110688,#110689,#110690,#110691,
#110692,#110693,#110694,#110695,#110696,#110697,#110698,#110699,#110700,
#110701,#110702,#110703,#110704,#110705,#110706,#110707,#110708,#110709,
#110710,#110711,#110712,#110713,#110714,#110715,#110716,#110717,#110718,
#110719,#110720,#110721,#110722,#110723,#110724,#110725,#110726,#110727,
#110728,#110729,#110730,#110731,#110732,#110733,#110734,#110735,#110736,
#110737,#110738,#110739,#110740,#110741,#110742,#110743,#110744,#110745,
#110746,#110747,#110748,#110749,#110750,#110751,#110752,#110753,#110754,
#110755,#110756,#110757,#110758,#110759,#110760,#110761,#110762,#110763,
#110764,#110765,#110766,#110767,#110768,#110769,#110770,#110771,#110772,
#110773,#110774,#110775,#110776,#110777,#110778,#110779,#110780,#110781,
#110782,#110783),.UNSPECIFIED.,.F.,.F.,(4,2,2,2,2,2,2,2,2,2,2,2,2,2,2,2,
2,2,2,2,2,2,2,2,2,2,2,2,2,2,2,2,2,2,2,2,2,2,2,2,2,2,2,2,2,2,2,2,2,2,2,2,
2,2,2,2,2,2,2,2,2,2,2,2,2,4),(-38.6590831067128,-38.5722352850204,-38.3883843851979,
-38.1738102322154,-38.0496824989805,-37.9289621827312,-37.7461201804974,
-37.5462571130413,-37.4137185869527,-37.2857235708196,-37.1018700031292,
-36.8872923472881,-36.7631630117032,-36.6424406685207,-36.4595960883871,
-36.2597308275695,-36.1271899746231,-35.9991933409473,-35.8153368306907,
-35.6007567523108,-35.47662491301,-35.3559013530122,-35.1730536506359,-34.9731833533706,
-34.8406414283239,-34.7126421226622,-34.5287833838445,-34.314198074117,
-34.190066074372,-34.0693391912543,-33.886489781691,-33.6866218396677,-33.5540755800713,
-33.426076343729,-33.2422135198448,-33.0276302806854,-32.9034920284243,
-32.7827672974878,-32.5999125019413,-32.4000277011298,-32.2674855869042,
-32.1394792934867,-31.9556172102756,-31.7410170567801,-31.6168883901235,
-31.496151573051,-31.3133009567084,-31.1134492691578,-30.9808892431195,
-30.8528944231952,-30.6690205303196,-30.4544528103358,-30.3302925542304,
-30.2095806433422,-30.0267093469457,-29.8267609886913,-29.6942403203475,
-29.5662088219705,-29.3823557187603,-29.1676920783934,-29.0436072853419,
-28.9228239434374,-28.7399966527432,-28.5402899448457,-28.4076592357397,
-28.3664636591338),.UNSPECIFIED.);
#29459=B_SPLINE_CURVE_WITH_KNOTS('',3,(#110788,#110789,#110790,#110791,
#110792,#110793,#110794,#110795,#110796,#110797,#110798,#110799,#110800,
#110801,#110802,#110803,#110804,#110805,#110806,#110807,#110808,#110809,
#110810,#110811,#110812,#110813,#110814,#110815,#110816,#110817,#110818,
#110819,#110820,#110821,#110822,#110823,#110824,#110825,#110826,#110827,
#110828,#110829,#110830,#110831,#110832,#110833,#110834,#110835,#110836,
#110837,#110838,#110839,#110840,#110841,#110842,#110843,#110844,#110845,
#110846,#110847,#110848,#110849,#110850,#110851,#110852,#110853,#110854,
#110855,#110856,#110857,#110858,#110859,#110860,#110861,#110862,#110863,
#110864,#110865,#110866,#110867,#110868,#110869,#110870,#110871,#110872,
#110873,#110874,#110875,#110876,#110877,#110878,#110879,#110880,#110881,
#110882,#110883,#110884,#110885,#110886,#110887,#110888,#110889,#110890,
#110891,#110892,#110893,#110894,#110895,#110896,#110897,#110898,#110899,
#110900,#110901,#110902,#110903,#110904,#110905,#110906,#110907,#110908,
#110909,#110910,#110911,#110912,#110913,#110914,#110915,#110916,#110917,
#110918,#110919),.UNSPECIFIED.,.F.,.F.,(4,2,2,2,2,2,2,2,2,2,2,2,2,2,2,2,
2,2,2,2,2,2,2,2,2,2,2,2,2,2,2,2,2,2,2,2,2,2,2,2,2,2,2,2,2,2,2,2,2,2,2,2,
2,2,2,2,2,2,2,2,2,2,2,2,2,4),(-16.3390445012698,-16.298426200689,-16.166778655205,
-15.9647852229255,-15.7814976184508,-15.6613692539658,-15.5365156611228,
-15.3227464875177,-15.1386478417236,-15.0109573811329,-14.8780085731732,
-14.6789982417746,-14.4962973493348,-14.3753117150272,-14.251438549892,
-14.0365067439024,-13.8527132572171,-13.7245807727206,-13.5921688649728,
-13.3919547030279,-13.2090279708675,-13.0883859304888,-12.9641379473126,
-12.7496618317777,-12.5657569020848,-12.4377952576735,-12.3051851627858,
-12.1054281309303,-11.9225913885721,-11.8018214480026,-11.6777201024695,
-11.4630737509824,-11.279215755038,-11.151190767859,-11.0186604052744,-10.8187302245468,
-10.6358625226298,-10.5151445065074,-10.390989291289,-10.1764129045308,
-9.99254066580108,-9.86454262459124,-9.73198442629992,-9.53212472352012,
-9.34927265927946,-9.22853718096996,-9.10440522551202,-8.88980633429332,
-8.70594334413277,-8.57793755307151,-8.44539279197424,-8.24551004092596,
-8.0626557027428,-7.94192941787983,-7.81779105664513,-7.60320521590703,
-7.41934243289807,-7.29134224194124,-7.15879502810392,-6.95892522880392,
-6.77607550773787,-6.65534815874714,-6.53121480227879,-6.31662833452605,
-6.13276923541242,-6.04591668252116),.UNSPECIFIED.);
#29460=B_SPLINE_CURVE_WITH_KNOTS('',3,(#110920,#110921,#110922,#110923,
#110924,#110925,#110926,#110927,#110928,#110929,#110930,#110931,#110932,
#110933,#110934,#110935,#110936,#110937,#110938,#110939,#110940,#110941,
#110942,#110943,#110944,#110945,#110946,#110947,#110948,#110949,#110950,
#110951,#110952,#110953,#110954,#110955,#110956,#110957,#110958,#110959,
#110960,#110961,#110962,#110963,#110964,#110965,#110966,#110967,#110968,
#110969,#110970,#110971,#110972,#110973,#110974,#110975,#110976,#110977,
#110978,#110979,#110980,#110981,#110982,#110983,#110984,#110985,#110986,
#110987,#110988,#110989,#110990,#110991,#110992,#110993,#110994,#110995,
#110996,#110997,#110998,#110999,#111000,#111001,#111002,#111003,#111004,
#111005,#111006,#111007,#111008,#111009,#111010,#111011,#111012,#111013,
#111014,#111015,#111016,#111017,#111018,#111019,#111020,#111021,#111022,
#111023,#111024,#111025,#111026,#111027,#111028,#111029,#111030,#111031,
#111032,#111033,#111034,#111035,#111036,#111037,#111038,#111039,#111040,
#111041,#111042,#111043),.UNSPECIFIED.,.F.,.F.,(4,2,2,2,2,2,2,2,2,2,2,2,
2,2,2,2,2,2,2,2,2,2,2,2,2,2,2,2,2,2,2,2,2,2,2,2,2,2,2,2,2,2,2,2,2,2,2,2,
2,2,2,2,2,2,2,2,2,2,2,2,2,4),(-28.3664636591338,-28.2797164067546,-28.0957991446076,
-27.8813728801688,-27.7570852714097,-27.6364798580693,-27.4535287823062,
-27.2531901316938,-27.1208344506832,-26.9926554760349,-26.8088936135346,
-26.5938354358871,-26.4700688114316,-26.3489853264082,-26.166349363524,
-25.9676936590255,-25.8345873150101,-25.7070245448486,-25.5228377739724,
-25.309390712311,-25.1842638792361,-25.0643606619124,-24.880914873015,-24.678168502708,
-24.5468424897756,-24.4177225832527,-24.2345671466329,-24.0167535315306,
-23.8951880884269,-23.7717293855261,-23.5905460589239,-23.3579655954052,
-23.2465264208019,-23.0825156762046,-22.865983031935,-22.6737097020076,
-22.5350681654638,-22.3527744370753,-22.1566459550718,-21.9799356327157,
-21.8558264126631,-21.5279549309628,-21.3734881578538,-21.2542705816141,
-21.1282476137618,-20.9158238967757,-20.7313360509443,-20.604194473977,
-20.4705375834989,-20.2581262018923,-20.0645349087967,-19.9518595706235,
-19.7964644208917,-19.6067510181749,-19.4027874754777,-19.2759433238808,
-18.9596269287533,-18.7693531702309,-18.6425637212898,-18.3115867582224,
-18.1333371708877,-18.0721778794789),.UNSPECIFIED.);
#29461=B_SPLINE_CURVE_WITH_KNOTS('',3,(#111049,#111050,#111051,#111052,
#111053,#111054,#111055,#111056,#111057,#111058,#111059,#111060,#111061,
#111062,#111063,#111064,#111065,#111066,#111067,#111068,#111069,#111070,
#111071,#111072,#111073,#111074,#111075,#111076,#111077,#111078,#111079,
#111080,#111081,#111082,#111083,#111084,#111085,#111086,#111087,#111088,
#111089,#111090,#111091,#111092,#111093,#111094,#111095,#111096,#111097,
#111098,#111099,#111100,#111101,#111102,#111103,#111104,#111105,#111106,
#111107,#111108,#111109,#111110,#111111,#111112,#111113,#111114,#111115,
#111116,#111117,#111118,#111119,#111120,#111121,#111122,#111123,#111124,
#111125,#111126,#111127,#111128,#111129,#111130,#111131,#111132,#111133,
#111134,#111135,#111136,#111137,#111138,#111139,#111140,#111141,#111142,
#111143,#111144,#111145,#111146,#111147,#111148,#111149,#111150),
 .UNSPECIFIED.,.F.,.F.,(4,2,2,2,2,2,2,2,2,2,2,2,2,2,2,2,2,2,2,2,2,2,2,2,
2,2,2,2,2,2,2,2,2,2,2,2,2,2,2,2,2,2,2,2,2,2,2,2,2,2,4),(-7.77890601744087,
-7.73775952422739,-7.60521657566241,-7.40533999301184,-7.22248980594114,
-7.10176541325388,-6.97763025612404,-6.76304803944614,-6.57918923266191,
-6.45119137673529,-6.31864723598035,-6.11878074870569,-5.93593463178674,
-5.81520998891301,-5.69107893079637,-5.47649717261703,-5.29264177366034,
-5.16464479115933,-5.03210382215314,-4.83223754253986,-4.64939360270815,
-4.52867152720027,-4.40454143327114,-4.18996389096452,-4.006110944537,-3.87811624601041,
-3.74557677001655,-3.54571450147723,-3.3628734668396,-3.2421528748727,-3.11802495086557,
-2.90345017912367,-2.71960005260632,-2.59160709546981,-2.45906975813039,
-2.25921003770872,-2.0763716281537,-1.95565293656456,-1.83152671866895,
-1.61695527334596,-1.43310782537051,-1.3051168182877,-1.1725813712171,-0.972724761576554,
-0.789889084794008,-0.66917213320999,-0.545047799792159,-0.338165976073822,
-0.171332043416279,-0.0714908710089851,-1.00000000013978E-6),
 .UNSPECIFIED.);
#29462=B_SPLINE_CURVE_WITH_KNOTS('',3,(#111153,#111154,#111155,#111156,
#111157,#111158,#111159,#111160,#111161,#111162,#111163,#111164,#111165,
#111166,#111167,#111168,#111169,#111170,#111171,#111172,#111173,#111174,
#111175,#111176,#111177,#111178,#111179,#111180,#111181,#111182,#111183,
#111184,#111185,#111186,#111187,#111188,#111189,#111190,#111191,#111192,
#111193,#111194,#111195,#111196,#111197,#111198,#111199,#111200,#111201,
#111202,#111203,#111204,#111205,#111206,#111207,#111208,#111209,#111210,
#111211,#111212,#111213,#111214,#111215,#111216,#111217,#111218,#111219,
#111220,#111221,#111222,#111223,#111224,#111225,#111226,#111227,#111228,
#111229,#111230,#111231,#111232,#111233,#111234,#111235,#111236,#111237,
#111238,#111239,#111240,#111241,#111242,#111243,#111244,#111245,#111246,
#111247,#111248,#111249,#111250,#111251,#111252,#111253,#111254,#111255,
#111256,#111257,#111258,#111259,#111260,#111261,#111262,#111263,#111264,
#111265,#111266,#111267,#111268,#111269,#111270),.UNSPECIFIED.,.F.,.F.,
(4,2,2,2,2,2,2,2,2,2,2,2,2,2,2,2,2,2,2,2,2,2,2,2,2,2,2,2,2,2,2,2,2,2,2,
2,2,2,2,2,2,2,2,2,2,2,2,2,2,2,2,2,2,2,2,2,2,2,4),(-36.0129143984966,-35.6654593228707,
-35.537072950901,-35.3588637813898,-35.1538708028347,-35.029741652255,-34.9090199548459,
-34.7261758635798,-34.5263105162429,-34.3937704731966,-34.265773995761,
-34.0819183254459,-33.8673382214782,-33.7432074632986,-33.6224837436366,
-33.4396370712807,-33.2397695140582,-33.1072271514087,-32.9792290502946,
-32.7953704415222,-32.5807878986877,-32.4566546503621,-32.335929701651,
-32.1530799152275,-31.9532073643807,-31.8206639106931,-31.6926631534603,
-31.508802305335,-31.2942145734511,-31.1700811293413,-31.0493528892366,
-30.8665013742659,-30.6666310672203,-30.5340833281315,-30.4060825988881,
-30.2222176936415,-30.0076319222705,-29.8834923174173,-29.7627661469876,
-29.5799093014275,-29.3800224249991,-29.2474787035248,-29.1194710245465,
-28.9356067872445,-28.7210043875804,-28.5968741296704,-28.4761360877002,
-28.2932832771621,-28.0934287605428,-27.9608674598407,-27.8328709750455,
-27.6489951172486,-27.4344244077396,-27.3102631807291,-27.1895494881339,
-27.0066763718689,-26.8067271367829,-26.6742043326556,-26.6330714141515),
 .UNSPECIFIED.);
#29463=B_SPLINE_CURVE_WITH_KNOTS('',3,(#111308,#111309,#111310,#111311,
#111312,#111313),.UNSPECIFIED.,.F.,.F.,(4,2,4),(-0.363774153394201,-0.193995614301166,
-9.9999999492173E-7),.UNSPECIFIED.);
#29464=B_SPLINE_CURVE_WITH_KNOTS('',3,(#111315,#111316,#111317,#111318,
#111319,#111320),.UNSPECIFIED.,.F.,.F.,(4,2,4),(-0.0532370215568508,-0.0266540826832716,
-6.04251272476367E-5),.UNSPECIFIED.);
#29465=B_SPLINE_CURVE_WITH_KNOTS('',3,(#111322,#111323,#111324,#111325,
#111326,#111327,#111328,#111329),.UNSPECIFIED.,.F.,.F.,(4,2,2,4),(-0.97744616972974,
-0.755136975405854,-0.488475539962772,-4.97420921147455E-6),
 .UNSPECIFIED.);
#29466=B_SPLINE_CURVE_WITH_KNOTS('',3,(#111331,#111332,#111333,#111334,
#111335,#111336),.UNSPECIFIED.,.F.,.F.,(4,2,4),(-1.85769505606768,-1.79339407393835,
-1.78591587085069),.UNSPECIFIED.);
#29467=B_SPLINE_CURVE_WITH_KNOTS('',3,(#111338,#111339,#111340,#111341),
 .UNSPECIFIED.,.F.,.F.,(4,4),(-4.93178416469503,-4.7947631910491),
 .UNSPECIFIED.);
#29468=B_SPLINE_CURVE_WITH_KNOTS('',3,(#111343,#111344,#111345,#111346,
#111347,#111348),.UNSPECIFIED.,.F.,.F.,(4,2,4),(-0.283103945271065,-0.141864378167519,
-2.13228232499812E-5),.UNSPECIFIED.);
#29469=B_SPLINE_CURVE_WITH_KNOTS('',3,(#111350,#111351,#111352,#111353,
#111354,#111355,#111356,#111357,#111358,#111359),.UNSPECIFIED.,.F.,.F.,
(4,2,2,2,4),(-0.201081696163703,-0.163457552386683,-0.100078064474262,-0.0500222454439804,
-9.99999075795843E-7),.UNSPECIFIED.);
#29470=B_SPLINE_CURVE_WITH_KNOTS('',3,(#111361,#111362,#111363,#111364),
 .UNSPECIFIED.,.F.,.F.,(4,4),(-0.298447768546908,-0.255015273222757),
 .UNSPECIFIED.);
#29471=B_SPLINE_CURVE_WITH_KNOTS('',3,(#111368,#111369,#111370,#111371,
#111372,#111373,#111374,#111375,#111376,#111377,#111378,#111379,#111380,
#111381,#111382,#111383,#111384,#111385,#111386),.UNSPECIFIED.,.F.,.F.,
(4,2,2,2,3,2,2,2,4),(-0.610180623927036,-0.587175612996075,-0.39145040866405,
-0.195725204332025,0.,0.195725204332025,0.39145040866405,0.587175612996075,
0.610180623930912),.UNSPECIFIED.);
#29472=B_SPLINE_CURVE_WITH_KNOTS('',3,(#111390,#111391,#111392,#111393),
 .UNSPECIFIED.,.F.,.F.,(4,4),(0.255015307744493,0.298443104215235),
 .UNSPECIFIED.);
#29473=B_SPLINE_CURVE_WITH_KNOTS('',3,(#111395,#111396,#111397,#111398,
#111399,#111400,#111401,#111402,#111403,#111404),.UNSPECIFIED.,.F.,.F.,
(4,2,2,2,4),(-0.199687815022838,-0.149974116571578,-0.100216949852256,-0.0373389572995741,
-7.28195441159246E-6),.UNSPECIFIED.);
#29474=B_SPLINE_CURVE_WITH_KNOTS('',3,(#111406,#111407,#111408,#111409,
#111410,#111411),.UNSPECIFIED.,.F.,.F.,(4,2,4),(-0.282640897342865,-0.141106701828136,
-7.28089112813694E-6),.UNSPECIFIED.);
#29475=B_SPLINE_CURVE_WITH_KNOTS('',3,(#111413,#111414,#111415,#111416),
 .UNSPECIFIED.,.F.,.F.,(4,4),(-0.15813773249332,-0.0210839373106531),
 .UNSPECIFIED.);
#29476=B_SPLINE_CURVE_WITH_KNOTS('',3,(#111418,#111419,#111420,#111421,
#111422,#111423,#111424),.UNSPECIFIED.,.F.,.F.,(4,3,4),(3.57860390370164,
3.58607926747234,3.65058765243316),.UNSPECIFIED.);
#29477=B_SPLINE_CURVE_WITH_KNOTS('',3,(#111426,#111427,#111428,#111429,
#111430,#111431,#111432,#111433),.UNSPECIFIED.,.F.,.F.,(4,2,2,4),(-0.854961148274419,
-0.437424717360482,-0.208632467898837,-1.3315846961078E-6),
 .UNSPECIFIED.);
#29478=B_SPLINE_CURVE_WITH_KNOTS('',3,(#111435,#111436,#111437,#111438,
#111439,#111440),.UNSPECIFIED.,.F.,.F.,(4,2,4),(-0.0532242538119046,-0.0266129661743925,
-9.99979108816385E-7),.UNSPECIFIED.);
#29479=B_SPLINE_CURVE_WITH_KNOTS('',3,(#111441,#111442,#111443,#111444,
#111445,#111446),.UNSPECIFIED.,.F.,.F.,(4,2,4),(-0.366235065052103,-0.18359159279208,
-6.68175113310375E-5),.UNSPECIFIED.);
#29480=B_SPLINE_CURVE_WITH_KNOTS('',3,(#111465,#111466,#111467,#111468,
#111469,#111470,#111471,#111472,#111473,#111474,#111475,#111476,#111477,
#111478,#111479,#111480),.UNSPECIFIED.,.F.,.F.,(4,3,3,3,3,4),(0.502459200378718,
0.620190407064421,0.733279471434336,0.843062918436606,0.948007554888288,
1.),.UNSPECIFIED.);
#29481=B_SPLINE_CURVE_WITH_KNOTS('',3,(#111482,#111483,#111484,#111485,
#111486,#111487,#111488,#111489,#111490,#111491),.UNSPECIFIED.,.F.,.F.,
(4,3,3,4),(0.,0.250000032895274,0.500000001353585,0.502459200168118),
 .UNSPECIFIED.);
#29482=B_SPLINE_CURVE_WITH_KNOTS('',3,(#111498,#111499,#111500,#111501,
#111502,#111503,#111504,#111505,#111506,#111507,#111508,#111509,#111510,
#111511,#111512,#111513,#111514,#111515,#111516,#111517,#111518,#111519,
#111520,#111521,#111522,#111523,#111524,#111525,#111526,#111527,#111528),
 .UNSPECIFIED.,.F.,.F.,(4,3,3,3,3,3,3,3,3,3,4),(2.2999675379427E-5,0.107908156121774,
0.216746941279355,0.325262700986818,0.432143196947118,0.5,0.625,0.740855777232924,
0.853585574556454,0.962004883925567,1.),.UNSPECIFIED.);
#29483=B_SPLINE_CURVE_WITH_KNOTS('',3,(#111530,#111531,#111532,#111533,
#111534,#111535,#111536,#111537,#111538,#111539,#111540,#111541,#111542,
#111543,#111544,#111545,#111546,#111547,#111548,#111549,#111550,#111551,
#111552,#111553,#111554,#111555,#111556,#111557,#111558,#111559,#111560,
#111561,#111562,#111563,#111564,#111565,#111566,#111567,#111568,#111569),
 .UNSPECIFIED.,.F.,.F.,(4,3,3,3,3,3,3,3,3,3,3,3,3,4),(0.,0.0652545873447945,
0.130565334251207,0.195328617575902,0.259486956805454,0.323171822834989,
0.386813145579456,0.450743489197714,0.5,0.596291449745224,0.697218586866101,
0.798920501895149,0.903698189064629,0.999999998228732),.UNSPECIFIED.);
#29484=B_SPLINE_CURVE_WITH_KNOTS('',3,(#111618,#111619,#111620,#111621,
#111622,#111623),.UNSPECIFIED.,.F.,.F.,(4,2,4),(0.498212563703856,0.749106281851928,
1.),.UNSPECIFIED.);
#29485=B_SPLINE_CURVE_WITH_KNOTS('',3,(#111625,#111626,#111627,#111628,
#111629,#111630,#111631,#111632,#111633,#111634,#111635,#111636,#111637,
#111638,#111639,#111640,#111641,#111642,#111643,#111644,#111645,#111646,
#111647,#111648,#111649),.UNSPECIFIED.,.F.,.F.,(4,3,3,3,3,3,3,3,4),(0.,
0.0689055252943441,0.137761127810044,0.206585336728476,0.249106281851928,
0.323525151579527,0.397954655315057,0.472431765057328,0.498212563703856),
 .UNSPECIFIED.);
#29486=B_SPLINE_CURVE_WITH_KNOTS('',3,(#111655,#111656,#111657,#111658,
#111659,#111660,#111661,#111662,#111663,#111664,#111665,#111666,#111667,
#111668,#111669,#111670,#111671,#111672,#111673,#111674,#111675,#111676,
#111677,#111678,#111679,#111680,#111681,#111682,#111683,#111684,#111685,
#111686,#111687,#111688,#111689,#111690,#111691,#111692,#111693,#111694,
#111695,#111696,#111697,#111698,#111699,#111700,#111701,#111702,#111703,
#111704,#111705,#111706,#111707,#111708,#111709,#111710,#111711,#111712,
#111713,#111714,#111715),.UNSPECIFIED.,.F.,.F.,(4,2,1,1,1,2,2,2,2,1,1,1,
2,2,2,2,2,1,1,1,2,2,2,2,2,2,2,2,2,2,2,1,1,2,2,4),(0.,0.0624999999999867,
0.09374999999998,0.109374999999977,0.117187499999975,0.121093749999974,
0.124999999999974,0.18749999999996,0.218749999999953,0.234374999999949,
0.242187499999947,0.246093749999946,0.248046874999946,0.249999999999946,
0.312499999999934,0.343749999999927,0.359374999999924,0.367187499999923,
0.371093749999922,0.373046874999922,0.374023437499922,0.374999999999922,
0.406249999999926,0.437499999999929,0.499999999999936,0.562499999999943,
0.593749999999947,0.609374999999949,0.62499999999995,0.687499999999957,
0.718749999999961,0.734374999999963,0.742187499999963,0.746093749999964,
0.749999999999964,1.),.UNSPECIFIED.);
#29487=B_SPLINE_CURVE_WITH_KNOTS('',3,(#111717,#111718,#111719,#111720,
#111721,#111722,#111723,#111724,#111725,#111726,#111727,#111728,#111729,
#111730,#111731,#111732,#111733,#111734,#111735,#111736,#111737,#111738,
#111739,#111740,#111741,#111742,#111743,#111744,#111745,#111746,#111747,
#111748,#111749,#111750,#111751,#111752,#111753,#111754,#111755,#111756,
#111757,#111758,#111759,#111760,#111761,#111762,#111763,#111764,#111765,
#111766,#111767,#111768,#111769,#111770,#111771,#111772,#111773,#111774,
#111775,#111776,#111777,#111778,#111779,#111780,#111781,#111782,#111783,
#111784,#111785,#111786,#111787,#111788,#111789,#111790,#111791,#111792,
#111793,#111794,#111795,#111796,#111797,#111798,#111799,#111800,#111801,
#111802,#111803,#111804,#111805,#111806,#111807,#111808,#111809,#111810,
#111811,#111812,#111813,#111814,#111815,#111816,#111817,#111818,#111819,
#111820,#111821,#111822,#111823,#111824,#111825,#111826,#111827,#111828,
#111829,#111830,#111831,#111832,#111833,#111834,#111835,#111836,#111837,
#111838,#111839,#111840,#111841,#111842,#111843,#111844,#111845,#111846,
#111847,#111848,#111849,#111850,#111851,#111852,#111853,#111854,#111855,
#111856,#111857,#111858,#111859,#111860,#111861,#111862,#111863,#111864,
#111865,#111866,#111867,#111868,#111869,#111870,#111871,#111872,#111873,
#111874,#111875,#111876,#111877,#111878,#111879,#111880,#111881,#111882,
#111883,#111884,#111885,#111886,#111887,#111888,#111889,#111890,#111891,
#111892,#111893,#111894,#111895,#111896,#111897),.UNSPECIFIED.,.F.,.F.,
(4,3,3,3,3,3,3,3,3,3,3,3,3,3,3,3,3,3,3,3,3,3,3,3,3,3,3,3,3,3,3,3,3,3,3,
3,3,3,3,3,3,3,3,3,3,3,3,3,3,3,3,3,3,3,3,3,3,3,3,3,4),(0.,0.0262353854799647,
0.0513882004402501,0.0760178707878943,0.100508935393731,0.124999999999569,
0.146668664871975,0.167619212130507,0.187499999999353,0.206963439919906,
0.218749999999244,0.23437499999919,0.242187499999164,0.246093749999151,
0.248046874999144,0.249023437499141,0.249755859374139,0.249999999999139,
0.27775990491465,0.304665955204806,0.331126738408159,0.356935472854795,
0.374999999999302,0.399714190734549,0.423855306551184,0.437499999999384,
0.460793596117878,0.468749999999425,0.484374999999445,0.492187499999455,
0.496093749999461,0.498046874999463,0.499023437499464,0.499999999999465,
0.536295573395747,0.572992063007457,0.610419270902384,0.624999999999589,
0.663936021974758,0.687499999999651,0.718749999999682,0.734374999999698,
0.742187499999706,0.746093749999709,0.749999999999712,0.778491977107122,
0.806509853673822,0.812499999999779,0.839780690346737,0.843749999999813,
0.85937499999983,0.867187499999838,0.871093749999843,0.874558700595564,
0.874999999999847,0.900177168816563,0.925224410427566,0.937499999999923,
0.962146915143125,0.986446671485073,1.),.UNSPECIFIED.);
#29488=B_SPLINE_CURVE_WITH_KNOTS('',3,(#111899,#111900,#111901,#111902,
#111903,#111904,#111905,#111906,#111907,#111908,#111909,#111910,#111911,
#111912,#111913,#111914,#111915,#111916,#111917,#111918,#111919,#111920,
#111921,#111922,#111923,#111924,#111925,#111926,#111927,#111928,#111929,
#111930,#111931,#111932,#111933,#111934,#111935,#111936,#111937,#111938,
#111939,#111940,#111941,#111942,#111943,#111944,#111945,#111946,#111947,
#111948,#111949,#111950,#111951,#111952,#111953,#111954,#111955,#111956,
#111957,#111958,#111959,#111960,#111961,#111962,#111963,#111964,#111965,
#111966,#111967,#111968,#111969,#111970,#111971,#111972,#111973,#111974,
#111975,#111976,#111977),.UNSPECIFIED.,.F.,.F.,(4,3,3,3,3,3,3,3,3,3,3,3,
3,3,3,3,3,3,3,3,3,3,3,3,3,3,4),(0.,0.052534295743839,0.106576781307671,
0.161234944024884,0.216296509746233,0.245421908055237,0.250000000000013,
0.305725650220763,0.362692703373066,0.37500000000002,0.431487410462525,
0.437500000000023,0.468750000000026,0.484375000000029,0.49218750000003,
0.49726975938631,0.500000000000032,0.562069345831075,0.622388694423505,
0.685333038873855,0.748277383324204,0.750000000000016,0.812500000000012,
0.872426273840813,0.932272985466431,0.991740773404511,1.),.UNSPECIFIED.);
#29489=B_SPLINE_CURVE_WITH_KNOTS('',3,(#111979,#111980,#111981,#111982,
#111983,#111984,#111985,#111986,#111987,#111988,#111989,#111990,#111991,
#111992,#111993,#111994,#111995,#111996,#111997,#111998,#111999,#112000,
#112001,#112002,#112003),.UNSPECIFIED.,.F.,.F.,(4,3,3,3,3,3,3,3,4),(7.26160252641012E-16,
0.131689505404652,0.260452970173316,0.385904363725134,0.5,0.645695716670177,
0.792716448908783,0.939175390751928,0.999999995177892),.UNSPECIFIED.);
#29490=B_SPLINE_CURVE_WITH_KNOTS('',3,(#112005,#112006,#112007,#112008,
#112009,#112010,#112011,#112012,#112013,#112014,#112015,#112016,#112017,
#112018,#112019,#112020,#112021,#112022,#112023,#112024,#112025,#112026,
#112027,#112028,#112029,#112030,#112031,#112032,#112033,#112034,#112035,
#112036,#112037,#112038,#112039,#112040,#112041,#112042,#112043,#112044,
#112045,#112046),.UNSPECIFIED.,.F.,.F.,(4,2,2,1,1,1,1,2,2,2,2,2,1,1,2,2,
2,2,2,1,1,1,1,2,2,4),(3.3708601358344E-9,0.125000000000098,0.187500000000147,
0.218750000000172,0.234375000000184,0.24218750000019,0.246093750000193,
0.249511718750197,0.250000000000197,0.375000000000224,0.437500000000236,
0.468750000000243,0.484375000000246,0.492187500000248,0.496093750000249,
0.50000000000025,0.625000000000263,0.68750000000027,0.718750000000273,0.734375000000275,
0.742187500000275,0.746093750000276,0.748046875000276,0.749511718750276,
0.750000000000276,1.),.UNSPECIFIED.);
#29491=B_SPLINE_CURVE_WITH_KNOTS('',3,(#112048,#112049,#112050,#112051,
#112052,#112053,#112054),.UNSPECIFIED.,.F.,.F.,(4,3,4),(4.999036296921E-14,
0.550250096230919,1.),.UNSPECIFIED.);
#29492=B_SPLINE_CURVE_WITH_KNOTS('',3,(#112056,#112057,#112058,#112059,
#112060,#112061,#112062,#112063,#112064,#112065,#112066,#112067,#112068,
#112069,#112070,#112071,#112072,#112073,#112074,#112075,#112076,#112077,
#112078,#112079,#112080,#112081,#112082,#112083,#112084,#112085,#112086,
#112087,#112088,#112089,#112090,#112091,#112092,#112093,#112094,#112095,
#112096,#112097,#112098,#112099,#112100,#112101,#112102,#112103,#112104,
#112105,#112106,#112107,#112108,#112109,#112110,#112111,#112112,#112113,
#112114,#112115,#112116,#112117,#112118,#112119,#112120,#112121,#112122,
#112123,#112124,#112125,#112126,#112127,#112128,#112129,#112130,#112131,
#112132,#112133,#112134,#112135,#112136,#112137,#112138,#112139,#112140,
#112141,#112142,#112143,#112144,#112145,#112146,#112147,#112148,#112149,
#112150,#112151,#112152,#112153,#112154,#112155,#112156,#112157,#112158,
#112159,#112160,#112161,#112162,#112163,#112164,#112165,#112166,#112167,
#112168,#112169,#112170,#112171,#112172,#112173,#112174,#112175,#112176,
#112177,#112178,#112179,#112180,#112181,#112182,#112183,#112184,#112185,
#112186,#112187,#112188,#112189,#112190,#112191,#112192,#112193,#112194,
#112195,#112196,#112197,#112198,#112199,#112200,#112201,#112202,#112203,
#112204,#112205,#112206,#112207,#112208,#112209,#112210,#112211,#112212,
#112213,#112214,#112215,#112216,#112217,#112218,#112219,#112220,#112221,
#112222,#112223,#112224,#112225,#112226,#112227,#112228,#112229,#112230,
#112231,#112232,#112233),.UNSPECIFIED.,.F.,.F.,(4,3,3,3,3,3,3,3,3,3,3,3,
3,3,3,3,3,3,3,3,3,3,3,3,3,3,3,3,3,3,3,3,3,3,3,3,3,3,3,3,3,3,3,3,3,3,3,3,
3,3,3,3,3,3,3,3,3,3,3,4),(0.,0.14352010892212,0.157701972276987,0.187500000000143,
0.218750000000166,0.234375000000178,0.242187500000183,0.246093750000185,
0.249659449839678,0.250000000000188,0.281779335707362,0.312823317660577,
0.317344564634756,0.349964665468181,0.381768385729566,0.392730548659543,
0.429582778946505,0.462987101572329,0.468750000000182,0.484375000000181,
0.49218750000018,0.49609375000018,0.498046875000181,0.499511718750183,0.500000000000183,
0.520007430934713,0.564789698817782,0.593750000000083,0.609375000000066,
0.617187500000057,0.624023437500051,0.62500000000005,0.663088784225902,
0.702110465150732,0.718750000000061,0.734375000000064,0.742187500000065,
0.746093750000066,0.749023437500067,0.750000000000069,0.771164208394432,
0.792032424081969,0.797583188711953,0.817998066584681,0.838686533292382,
0.859375000000083,0.867187500000084,0.871093750000085,0.873046875000085,
0.874023437500085,0.874511718750085,0.875000000000085,0.892460570687305,
0.909577023073872,0.926237545524542,0.937500000000042,0.953627291503346,
0.96958168681015,0.98530977827609,1.),.UNSPECIFIED.);
#29493=B_SPLINE_CURVE_WITH_KNOTS('',3,(#112235,#112236,#112237,#112238,
#112239,#112240,#112241,#112242,#112243,#112244,#112245,#112246,#112247,
#112248,#112249,#112250,#112251,#112252),.UNSPECIFIED.,.F.,.F.,(4,1,2,1,
2,2,2,1,1,1,1,4),(0.,0.125,0.25,0.3125,0.375,0.5,0.625,0.6875,0.75,0.8125,
0.874999999999999,1.),.UNSPECIFIED.);
#29494=B_SPLINE_CURVE_WITH_KNOTS('',3,(#112261,#112262,#112263,#112264,
#112265,#112266,#112267,#112268,#112269,#112270,#112271,#112272,#112273,
#112274,#112275,#112276,#112277,#112278,#112279,#112280,#112281,#112282,
#112283,#112284,#112285,#112286,#112287,#112288,#112289,#112290,#112291,
#112292,#112293,#112294,#112295,#112296,#112297,#112298,#112299,#112300,
#112301,#112302,#112303,#112304,#112305,#112306,#112307,#112308,#112309,
#112310,#112311,#112312,#112313,#112314,#112315,#112316,#112317,#112318,
#112319,#112320,#112321,#112322,#112323,#112324,#112325,#112326,#112327,
#112328,#112329,#112330,#112331,#112332,#112333,#112334,#112335,#112336,
#112337,#112338,#112339,#112340,#112341,#112342,#112343,#112344,#112345,
#112346,#112347,#112348,#112349,#112350,#112351,#112352,#112353,#112354,
#112355,#112356,#112357,#112358,#112359,#112360,#112361,#112362,#112363,
#112364,#112365,#112366,#112367,#112368,#112369),.UNSPECIFIED.,.F.,.F.,
(4,3,3,3,3,3,3,3,3,3,3,3,3,3,3,3,3,3,3,3,3,3,3,3,3,3,3,3,3,3,3,3,3,3,3,
3,4),(0.,0.0221285907803649,0.0457146490130174,0.0624999316519651,0.0936982528543991,
0.124999863304009,0.156249829130032,0.183271416696792,0.187499794956055,
0.220371047068795,0.249999726608099,0.281249692434121,0.310392278499468,
0.338981017787981,0.3669802812056,0.374999589912188,0.410712814329141,0.445935995865815,
0.480427395075885,0.499999453216277,0.532474023028728,0.564651000993001,
0.596435510326097,0.624999316520367,0.659415128053142,0.693382150709312,
0.726649798606273,0.749999179824455,0.778823340006754,0.807383283604156,
0.835813998348854,0.864094537414675,0.874999043128545,0.910273598518763,
0.945062381131166,0.979104413886319,1.),.UNSPECIFIED.);
#29495=B_SPLINE_CURVE_WITH_KNOTS('',3,(#112371,#112372,#112373,#112374,
#112375,#112376,#112377,#112378,#112379,#112380,#112381,#112382,#112383,
#112384,#112385,#112386,#112387,#112388,#112389,#112390,#112391,#112392,
#112393,#112394,#112395,#112396,#112397,#112398,#112399,#112400,#112401,
#112402,#112403,#112404,#112405,#112406,#112407,#112408,#112409,#112410,
#112411,#112412,#112413,#112414,#112415,#112416,#112417,#112418,#112419,
#112420,#112421,#112422,#112423,#112424,#112425,#112426,#112427,#112428,
#112429,#112430,#112431,#112432,#112433,#112434,#112435,#112436,#112437,
#112438,#112439,#112440,#112441,#112442,#112443,#112444,#112445,#112446,
#112447,#112448,#112449,#112450),.UNSPECIFIED.,.F.,.F.,(4,2,2,1,2,2,1,2,
2,1,1,2,2,1,2,2,2,1,2,2,1,1,1,2,2,2,2,1,2,2,2,2,2,1,1,2,2,2,2,2,2,1,2,2,
1,2,4),(0.,0.1249999999995,0.249999999999001,0.281249999998876,0.285156249998862,
0.289062499998847,0.296874999998818,0.31249999999876,0.374999999998527,
0.406249999998409,0.421874999998351,0.427734374998332,0.428710937498328,
0.429687499998324,0.437499999998293,0.499999999998021,0.562499999997748,
0.570312499997713,0.571289062497709,0.571777343747708,0.572265624997707,
0.574218749997718,0.578124999997741,0.593749999997826,0.624999999998001,
0.687499999998352,0.718749999998528,0.734374999998614,0.742187499998659,
0.746093749998681,0.749999999998703,0.812499999999069,0.843749999999253,
0.859374999999346,0.867187499999392,0.871093749999416,0.873046874999426,
0.874999999999437,0.906249999999573,0.921874999999641,0.929687499999675,
0.933593749999692,0.935546874999701,0.936523437499705,0.937499999999709,
0.968749999999855,1.),.UNSPECIFIED.);
#29496=B_SPLINE_CURVE_WITH_KNOTS('',3,(#112452,#112453,#112454,#112455,
#112456,#112457,#112458),.UNSPECIFIED.,.F.,.F.,(4,3,4),(0.,0.552168243797124,
0.99999996236639),.UNSPECIFIED.);
#29497=B_SPLINE_CURVE_WITH_KNOTS('',3,(#112460,#112461,#112462,#112463,
#112464,#112465,#112466,#112467,#112468,#112469,#112470,#112471,#112472,
#112473,#112474,#112475,#112476,#112477,#112478,#112479,#112480,#112481,
#112482,#112483,#112484,#112485,#112486,#112487,#112488,#112489,#112490,
#112491,#112492,#112493,#112494,#112495,#112496,#112497,#112498,#112499,
#112500,#112501,#112502,#112503,#112504,#112505,#112506,#112507,#112508,
#112509,#112510,#112511,#112512,#112513,#112514,#112515,#112516,#112517,
#112518,#112519,#112520,#112521,#112522,#112523,#112524,#112525,#112526,
#112527,#112528,#112529,#112530,#112531,#112532,#112533,#112534,#112535,
#112536,#112537,#112538,#112539,#112540,#112541,#112542,#112543,#112544,
#112545,#112546,#112547,#112548,#112549,#112550,#112551,#112552,#112553,
#112554,#112555,#112556,#112557,#112558,#112559,#112560,#112561,#112562,
#112563,#112564,#112565,#112566,#112567,#112568,#112569,#112570,#112571,
#112572,#112573,#112574,#112575,#112576,#112577,#112578,#112579,#112580,
#112581,#112582,#112583,#112584,#112585,#112586,#112587,#112588,#112589,
#112590,#112591,#112592,#112593,#112594,#112595,#112596,#112597,#112598,
#112599,#112600,#112601,#112602,#112603,#112604,#112605,#112606,#112607,
#112608,#112609,#112610,#112611,#112612,#112613,#112614,#112615,#112616,
#112617,#112618,#112619,#112620,#112621,#112622,#112623,#112624,#112625,
#112626,#112627,#112628,#112629,#112630,#112631,#112632,#112633,#112634,
#112635,#112636,#112637,#112638,#112639,#112640,#112641,#112642,#112643,
#112644,#112645,#112646,#112647,#112648,#112649,#112650,#112651,#112652,
#112653,#112654,#112655,#112656,#112657,#112658,#112659,#112660,#112661,
#112662,#112663,#112664,#112665,#112666,#112667,#112668,#112669,#112670,
#112671,#112672,#112673),.UNSPECIFIED.,.F.,.F.,(4,3,3,3,3,3,3,3,3,3,3,3,
3,3,3,3,3,3,3,3,3,3,3,3,3,3,3,3,3,3,3,3,3,3,3,3,3,3,3,3,3,3,3,3,3,3,3,3,
3,3,3,3,3,3,3,3,3,3,3,3,3,3,3,3,3,3,3,3,3,3,3,4),(1.72563345367939E-9,0.0251902887445909,
0.0431288153335098,0.0624999999999211,0.0895200409842773,0.0937499999998817,
0.109374999999862,0.117187499999852,0.121093749999847,0.123046874999844,
0.124999999999842,0.144918719463055,0.165108115533264,0.176831133963176,
0.197350519867584,0.218134806338091,0.234374999999699,0.242187499999689,
0.246093749999683,0.248046874999681,0.249755859374679,0.249877929687179,
0.249999999999679,0.273529672022163,0.297668999478059,0.317227671725171,
0.342520462487478,0.368140297657527,0.394182158920048,0.420410072964651,
0.446860880515511,0.468749999999632,0.484374999999629,0.492187499999627,
0.496093749999626,0.498046874999626,0.499511718749626,0.499755859374627,
0.499999999999627,0.53315145702459,0.566804203446233,0.601247768565495,
0.630326335104507,0.664700120223858,0.699891114094579,0.718749999999988,
0.734375000000014,0.742187500000027,0.746093750000033,0.748046875000036,
0.749511718750039,0.75000000000004,0.763329402270841,0.776642772728383,
0.789909749239645,0.803137903948878,0.816279431179592,0.825842999740232,
0.838787243962379,0.85158256388443,0.859375000000014,0.867187500000012,
0.871093750000011,0.87304687500001,0.87402343750001,0.87451171875001,0.87500000000001,
0.902182619157957,0.929229736943535,0.94702964207556,0.974458771224453,
0.999999996801779),.UNSPECIFIED.);
#29498=B_SPLINE_CURVE_WITH_KNOTS('',3,(#112675,#112676,#112677,#112678,
#112679,#112680,#112681,#112682,#112683,#112684,#112685,#112686,#112687,
#112688,#112689,#112690,#112691,#112692,#112693,#112694,#112695,#112696,
#112697,#112698,#112699,#112700,#112701,#112702),.UNSPECIFIED.,.F.,.F.,
(4,3,3,3,3,3,3,3,3,4),(4.84983446249765E-9,0.132630715103507,0.268748748725146,
0.409090067082655,0.5,0.612453315498843,0.727402227633262,0.843933478268945,
0.963413781542886,1.),.UNSPECIFIED.);
#29499=B_SPLINE_CURVE_WITH_KNOTS('',3,(#112704,#112705,#112706,#112707,
#112708,#112709,#112710,#112711,#112712,#112713,#112714,#112715,#112716,
#112717,#112718,#112719,#112720,#112721,#112722,#112723,#112724,#112725),
 .UNSPECIFIED.,.F.,.F.,(4,2,2,2,2,2,2,2,2,2,4),(0.,0.125000000000008,0.187500000000011,
0.218750000000013,0.250000000000016,0.375000000000019,0.437500000000019,
0.468750000000018,0.500000000000016,0.750000000000008,1.),.UNSPECIFIED.);
#29500=B_SPLINE_CURVE_WITH_KNOTS('',3,(#112727,#112728,#112729,#112730,
#112731,#112732,#112733,#112734,#112735,#112736,#112737,#112738,#112739,
#112740,#112741,#112742,#112743,#112744,#112745,#112746,#112747,#112748,
#112749,#112750,#112751,#112752,#112753,#112754,#112755,#112756,#112757,
#112758,#112759,#112760,#112761,#112762,#112763,#112764,#112765,#112766,
#112767,#112768,#112769,#112770,#112771,#112772,#112773,#112774,#112775,
#112776,#112777,#112778,#112779,#112780,#112781,#112782,#112783,#112784,
#112785,#112786,#112787,#112788,#112789,#112790,#112791,#112792,#112793,
#112794,#112795,#112796,#112797,#112798,#112799,#112800,#112801,#112802,
#112803,#112804,#112805,#112806,#112807,#112808,#112809,#112810,#112811,
#112812,#112813,#112814,#112815,#112816,#112817,#112818,#112819,#112820,
#112821,#112822,#112823,#112824,#112825,#112826,#112827,#112828,#112829,
#112830,#112831,#112832,#112833,#112834,#112835,#112836,#112837,#112838,
#112839,#112840,#112841,#112842,#112843,#112844,#112845,#112846,#112847,
#112848,#112849,#112850,#112851,#112852,#112853),.UNSPECIFIED.,.F.,.F.,
(4,3,3,3,3,3,3,3,3,3,3,3,3,3,3,3,3,3,3,3,3,3,3,3,3,3,3,3,3,3,3,3,3,3,3,
3,3,3,3,3,3,3,4),(0.,0.021047851700448,0.0420641562918161,0.0625000000000671,
0.0834215117481714,0.104231039484499,0.109375000000118,0.117187500000127,
0.121093750000131,0.124211568697334,0.125000000000136,0.143426311945488,
0.170178097660854,0.197400256138289,0.218750000000252,0.234375000000271,
0.24218750000028,0.246093750000284,0.248046875000286,0.250000000000288,
0.275019250919516,0.296988168551031,0.322708916352598,0.34790789542466,
0.372156990324995,0.395828889732673,0.418651543771118,0.430683726473005,
0.456873584251504,0.468750000000375,0.484375000000381,0.492187500000384,
0.496093750000386,0.498046875000388,0.499023437500388,0.500000000000389,
0.536638842599964,0.630613966148358,0.652479703862573,0.75633333254645,
0.768320183847596,0.877828717397992,1.),.UNSPECIFIED.);
#29501=B_SPLINE_CURVE_WITH_KNOTS('',3,(#112854,#112855,#112856,#112857,
#112858,#112859,#112860,#112861,#112862,#112863,#112864,#112865,#112866,
#112867,#112868,#112869,#112870,#112871,#112872,#112873,#112874,#112875,
#112876,#112877,#112878,#112879,#112880,#112881,#112882,#112883,#112884,
#112885,#112886,#112887,#112888,#112889,#112890,#112891,#112892,#112893,
#112894,#112895,#112896,#112897,#112898,#112899,#112900,#112901,#112902,
#112903,#112904,#112905,#112906,#112907,#112908,#112909,#112910,#112911,
#112912,#112913,#112914,#112915,#112916,#112917,#112918,#112919,#112920,
#112921,#112922,#112923,#112924,#112925,#112926,#112927,#112928,#112929,
#112930,#112931,#112932),.UNSPECIFIED.,.F.,.F.,(4,2,2,2,1,1,1,1,2,2,2,2,
1,1,1,1,2,2,2,2,1,1,1,1,2,2,2,2,2,1,1,1,1,2,2,2,2,1,1,1,1,2,2,2,2,1,1,1,
2,2,4),(0.,0.124999999999979,0.187499999999968,0.218749999999963,0.23437499999996,
0.242187499999958,0.246093749999958,0.248046874999957,0.249023437499957,
0.249999999999957,0.312499999999942,0.343749999999934,0.35937499999993,
0.367187499999928,0.371093749999927,0.373046874999927,0.374023437499926,
0.374999999999926,0.437499999999906,0.468749999999896,0.484374999999891,
0.492187499999889,0.496093749999888,0.498046874999887,0.499755859374888,
0.499999999999888,0.562499999999828,0.593749999999799,0.609374999999784,
0.617187499999776,0.621093749999773,0.623046874999771,0.62402343749977,
0.62475585937477,0.62499999999977,0.687499999999799,0.718749999999813,0.73437499999982,
0.742187499999824,0.746093749999826,0.748046874999826,0.749511718749826,
0.749999999999826,0.812499999999865,0.843749999999885,0.859374999999894,
0.867187499999899,0.871093749999902,0.873046874999903,0.874999999999905,
1.),.UNSPECIFIED.);
#29502=B_SPLINE_CURVE_WITH_KNOTS('',3,(#112942,#112943,#112944,#112945,
#112946,#112947,#112948,#112949,#112950,#112951,#112952,#112953,#112954,
#112955,#112956,#112957,#112958,#112959,#112960,#112961,#112962,#112963,
#112964,#112965,#112966,#112967,#112968,#112969,#112970,#112971,#112972,
#112973,#112974,#112975,#112976,#112977,#112978,#112979,#112980,#112981,
#112982,#112983,#112984,#112985,#112986,#112987,#112988,#112989,#112990,
#112991,#112992,#112993,#112994,#112995,#112996,#112997,#112998,#112999),
 .UNSPECIFIED.,.F.,.F.,(4,3,3,3,3,3,3,3,3,3,3,3,3,3,3,3,3,3,3,4),(0.,0.0832713098445368,
0.165797375546863,0.187499999999976,0.218749999999971,0.23437499999997,
0.247637083347011,0.249999999999968,0.367385209176164,0.374999999999965,
0.437499999999964,0.468749999999964,0.484374999999965,0.499182128881398,
0.499999999999967,0.618394583046436,0.734930438524368,0.850408746057064,
0.964416460208876,0.999999999999995),.UNSPECIFIED.);
#29503=B_SPLINE_CURVE_WITH_KNOTS('',3,(#113001,#113002,#113003,#113004,
#113005,#113006,#113007,#113008,#113009,#113010,#113011,#113012,#113013,
#113014,#113015,#113016,#113017,#113018,#113019,#113020,#113021,#113022,
#113023,#113024,#113025,#113026,#113027,#113028,#113029,#113030,#113031,
#113032,#113033,#113034,#113035,#113036,#113037,#113038,#113039,#113040,
#113041,#113042,#113043,#113044,#113045,#113046,#113047,#113048,#113049,
#113050,#113051,#113052,#113053,#113054,#113055,#113056,#113057,#113058,
#113059,#113060,#113061,#113062,#113063,#113064,#113065,#113066,#113067,
#113068,#113069,#113070,#113071,#113072,#113073,#113074,#113075,#113076,
#113077,#113078,#113079,#113080,#113081,#113082,#113083,#113084,#113085,
#113086,#113087,#113088,#113089,#113090,#113091,#113092,#113093,#113094,
#113095,#113096,#113097,#113098,#113099,#113100),.UNSPECIFIED.,.F.,.F.,
(4,3,3,3,3,3,3,3,3,3,3,3,3,3,3,3,3,3,3,3,3,3,3,3,3,3,3,3,3,3,3,3,3,4),(0.,
0.00157583922411374,0.0826938458291058,0.124999999999998,0.12541626163461,
0.169971053142697,0.214255800133528,0.249510415781629,0.249999999999996,
0.306480976121043,0.363470399754044,0.374207181925756,0.374999999999994,
0.437499999999993,0.468749999999993,0.484374999999994,0.492187499999995,
0.498780286635775,0.499999999999996,0.500783062716376,0.57069940241407,
0.624281140924415,0.624999999999999,0.674699886918992,0.6875,0.71875,0.73649200577412,
0.748843590324373,0.750000000000001,0.801976158225286,0.854862646973396,
0.907963524134435,0.960913180138766,1.),.UNSPECIFIED.);
#29504=B_SPLINE_CURVE_WITH_KNOTS('',3,(#113102,#113103,#113104,#113105,
#113106,#113107,#113108,#113109,#113110,#113111,#113112,#113113,#113114,
#113115,#113116,#113117,#113118,#113119,#113120,#113121,#113122,#113123,
#113124,#113125,#113126),.UNSPECIFIED.,.F.,.F.,(4,3,3,3,3,3,3,3,4),(0.,
0.195180208056074,0.250000000000001,0.375,0.4375,0.5,0.682692739872639,
0.866396142559968,1.),.UNSPECIFIED.);
#29505=B_SPLINE_CURVE_WITH_KNOTS('',3,(#113130,#113131,#113132,#113133,
#113134,#113135,#113136,#113137,#113138,#113139,#113140,#113141,#113142,
#113143,#113144,#113145,#113146,#113147,#113148,#113149,#113150,#113151),
 .UNSPECIFIED.,.F.,.F.,(4,3,3,3,3,3,3,4),(0.,0.180290242506945,0.25,0.43116946893496,
0.5,0.702896747154662,0.903673086907349,1.),.UNSPECIFIED.);
#29506=B_SPLINE_CURVE_WITH_KNOTS('',3,(#113153,#113154,#113155,#113156,
#113157,#113158,#113159,#113160,#113161,#113162,#113163,#113164,#113165,
#113166,#113167,#113168,#113169,#113170,#113171,#113172,#113173,#113174,
#113175,#113176,#113177,#113178,#113179,#113180,#113181,#113182,#113183,
#113184,#113185,#113186,#113187,#113188,#113189,#113190,#113191,#113192,
#113193,#113194,#113195,#113196,#113197,#113198,#113199,#113200,#113201,
#113202,#113203,#113204,#113205,#113206,#113207,#113208,#113209,#113210),
 .UNSPECIFIED.,.F.,.F.,(4,3,3,3,3,3,3,3,3,3,3,3,3,3,3,3,3,3,3,4),(0.,0.0832713098165828,
0.165797375467783,0.187500000000001,0.218750000000002,0.234375000000003,
0.247637083317996,0.250000000000004,0.367385208916902,0.375000000000004,
0.437500000000006,0.468750000000006,0.484375000000006,0.499182128806393,
0.500000000000005,0.61839458300907,0.734930438447227,0.850408745939979,
0.964416460051457,0.999999999999995),.UNSPECIFIED.);
#29507=B_SPLINE_CURVE_WITH_KNOTS('',3,(#113212,#113213,#113214,#113215,
#113216,#113217,#113218,#113219,#113220,#113221,#113222,#113223,#113224,
#113225,#113226,#113227,#113228,#113229,#113230,#113231,#113232,#113233,
#113234,#113235,#113236,#113237,#113238,#113239,#113240,#113241,#113242,
#113243,#113244,#113245,#113246,#113247,#113248,#113249,#113250,#113251,
#113252,#113253,#113254,#113255,#113256,#113257,#113258,#113259,#113260,
#113261,#113262,#113263,#113264,#113265,#113266,#113267,#113268,#113269,
#113270,#113271,#113272,#113273,#113274,#113275,#113276,#113277,#113278,
#113279,#113280,#113281,#113282,#113283,#113284,#113285,#113286,#113287,
#113288,#113289,#113290,#113291,#113292,#113293,#113294,#113295,#113296,
#113297,#113298,#113299,#113300,#113301,#113302,#113303,#113304,#113305,
#113306,#113307,#113308,#113309,#113310,#113311),.UNSPECIFIED.,.F.,.F.,
(4,3,3,3,3,3,3,3,3,3,3,3,3,3,3,3,3,3,3,3,3,3,3,3,3,3,3,3,3,3,3,3,3,4),(0.,
0.00157583922263862,0.0826938457606489,0.124999999999983,0.125416261644559,
0.169971053528897,0.214255800893783,0.249510415781452,0.249999999999966,
0.30648097610305,0.363470399718357,0.374207181925786,0.37499999999995,0.437499999999941,
0.468749999999939,0.484374999999937,0.492187499999937,0.498780286636739,
0.499999999999938,0.500783062713993,0.570699402452992,0.624281140920161,
0.624999999999953,0.674699886914206,0.687499999999959,0.718749999999964,
0.736492005804936,0.748843590315732,0.749999999999968,0.80197615821585,
0.854862646954884,0.907963524106764,0.960913180101409,1.),.UNSPECIFIED.);
#29508=B_SPLINE_CURVE_WITH_KNOTS('',3,(#113313,#113314,#113315,#113316,
#113317,#113318,#113319,#113320,#113321,#113322,#113323),.UNSPECIFIED.,
 .F.,.F.,(4,2,1,2,2,4),(0.,0.250000000000001,0.375000000000002,0.437500000000001,
0.500000000000001,1.),.UNSPECIFIED.);
#29509=B_SPLINE_CURVE_WITH_KNOTS('',3,(#113326,#113327,#113328,#113329,
#113330,#113331,#113332,#113333,#113334,#113335,#113336,#113337,#113338,
#113339,#113340,#113341,#113342,#113343,#113344,#113345,#113346,#113347),
 .UNSPECIFIED.,.F.,.F.,(4,3,3,3,3,3,3,4),(0.,0.187500000000001,0.375000000000002,
0.465350260778303,0.500000000000003,0.702064785007046,0.902038946571831,
1.),.UNSPECIFIED.);
#29510=B_SPLINE_CURVE_WITH_KNOTS('',3,(#113364,#113365,#113366,#113367,
#113368,#113369),.UNSPECIFIED.,.F.,.F.,(4,2,4),(0.659245462660571,0.848526904814134,
0.950302518199856),.UNSPECIFIED.);
#29511=B_SPLINE_CURVE_WITH_KNOTS('',3,(#113372,#113373,#113374,#113375,
#113376,#113377),.UNSPECIFIED.,.F.,.F.,(4,2,4),(0.368188407121287,0.469964020507009,
0.659245462660571),.UNSPECIFIED.);
#29512=B_SPLINE_CURVE_WITH_KNOTS('',3,(#113398,#113399,#113400,#113401,
#113402,#113403,#113404,#113405,#113406,#113407),.UNSPECIFIED.,.F.,.F.,
(4,2,2,2,4),(-0.989948967812353,-0.817116807788299,-0.638223028190753,-0.459329248593207,
-0.286497088569423),.UNSPECIFIED.);
#29513=B_SPLINE_CURVE_WITH_KNOTS('',3,(#113414,#113415,#113416,#113417,
#113418,#113419,#113420,#113421,#113422,#113423,#113424,#113425,#113426,
#113427),.UNSPECIFIED.,.F.,.F.,(4,2,2,2,2,2,4),(9.999995437339E-7,0.259748030405366,
0.508379521897915,0.568189856021016,0.593019351884581,0.603881938758307,
0.614169443343448),.UNSPECIFIED.);
#29514=B_SPLINE_CURVE_WITH_KNOTS('',3,(#113435,#113436,#113437,#113438,
#113439,#113440,#113441,#113442,#113443,#113444,#113445,#113446,#113447,
#113448),.UNSPECIFIED.,.F.,.F.,(4,2,2,2,2,2,4),(1.00000361513827E-6,0.00712177767761689,
0.0148839153232921,0.032515583953615,0.0900479458768181,0.184553013873431,
0.25295173128519),.UNSPECIFIED.);
#29515=B_SPLINE_CURVE_WITH_KNOTS('',3,(#113544,#113545,#113546,#113547,
#113548,#113549,#113550,#113551,#113552,#113553,#113554,#113555,#113556,
#113557,#113558,#113559,#113560,#113561,#113562,#113563,#113564,#113565,
#113566,#113567,#113568,#113569,#113570,#113571,#113572,#113573,#113574,
#113575,#113576,#113577,#113578,#113579,#113580,#113581,#113582,#113583,
#113584,#113585,#113586,#113587,#113588,#113589,#113590,#113591,#113592,
#113593,#113594,#113595,#113596,#113597,#113598),.UNSPECIFIED.,.F.,.F.,
(4,3,3,3,3,3,3,3,3,3,3,3,3,3,3,3,3,3,4),(0.,0.0969544955629047,0.192024794958463,
0.229538341359698,0.249999999999967,0.35554605419242,0.374999999999951,
0.437499999999944,0.46874999999994,0.484374999999939,0.494786925416321,
0.499999999999939,0.53995794249682,0.622741542029251,0.703614813184483,
0.781706215824503,0.84330713965756,0.92367183712412,0.999998921631664),
 .UNSPECIFIED.);
#29516=B_SPLINE_CURVE_WITH_KNOTS('',3,(#113601,#113602,#113603,#113604,
#113605,#113606,#113607,#113608,#113609,#113610,#113611,#113612,#113613,
#113614,#113615,#113616,#113617,#113618,#113619,#113620,#113621,#113622,
#113623,#113624,#113625,#113626,#113627,#113628,#113629,#113630,#113631,
#113632,#113633,#113634,#113635,#113636,#113637,#113638,#113639,#113640,
#113641,#113642,#113643,#113644,#113645,#113646,#113647,#113648,#113649,
#113650,#113651,#113652,#113653,#113654,#113655,#113656,#113657,#113658),
 .UNSPECIFIED.,.F.,.F.,(4,3,3,3,3,3,3,3,3,3,3,3,3,3,3,3,3,3,3,4),(1.22754616606188E-6,
0.077127828978588,0.155720459280002,0.164018043179436,0.238669858928981,
0.25000000000002,0.33192992133946,0.375000000000029,0.437500000000033,0.466959333266612,
0.468750000000036,0.484375000000037,0.494691856545788,0.500000000000039,
0.603437310447197,0.709278989321924,0.777007528128708,0.876123815416302,
0.97719726753376,1.),.UNSPECIFIED.);
#29517=B_SPLINE_CURVE_WITH_KNOTS('',3,(#113669,#113670,#113671,#113672,
#113673,#113674,#113675,#113676,#113677,#113678,#113679,#113680,#113681,
#113682,#113683,#113684,#113685,#113686,#113687,#113688,#113689,#113690,
#113691,#113692,#113693,#113694,#113695,#113696,#113697,#113698,#113699,
#113700,#113701,#113702,#113703,#113704,#113705,#113706,#113707,#113708,
#113709,#113710,#113711,#113712,#113713,#113714,#113715,#113716,#113717,
#113718,#113719,#113720,#113721,#113722,#113723,#113724,#113725,#113726,
#113727,#113728,#113729,#113730,#113731,#113732,#113733,#113734,#113735,
#113736,#113737,#113738,#113739,#113740,#113741,#113742,#113743,#113744,
#113745,#113746,#113747,#113748,#113749,#113750,#113751,#113752,#113753,
#113754,#113755,#113756,#113757,#113758,#113759,#113760,#113761,#113762,
#113763,#113764,#113765,#113766,#113767,#113768,#113769,#113770,#113771,
#113772,#113773,#113774,#113775,#113776,#113777,#113778,#113779,#113780,
#113781,#113782,#113783,#113784,#113785,#113786,#113787,#113788,#113789,
#113790,#113791,#113792,#113793,#113794),.UNSPECIFIED.,.F.,.F.,(4,2,2,2,
2,2,2,2,2,2,2,2,2,2,2,2,2,2,2,2,2,2,2,2,2,2,2,2,2,2,2,2,2,2,2,2,2,2,2,2,
2,2,2,2,2,2,2,2,2,2,2,2,2,2,2,2,2,2,2,2,2,2,4),(-26.6330714141515,-26.5461718850615,
-26.3623163068096,-26.1476515893506,-26.0235641990265,-25.9027805180327,
-25.7199504119376,-25.52023768622,-25.3876070905798,-25.2596614153778,-25.075742962878,
-24.8613106090056,-24.7370245950165,-24.6164151116154,-24.4334637395033,
-24.2331320927081,-24.1007708017898,-23.9725938499412,-23.7888275193191,
-23.5737764190362,-23.4500004740476,-23.328922994976,-23.146280056007,-22.9475953530379,
-22.8144994884482,-22.6869256936087,-22.5027434433308,-22.2892700348955,
-22.1641622465145,-22.0442410956717,-21.8608049283298,-21.6581114786105,
-21.5267605884321,-21.3976615518945,-21.2144897688346,-20.9967439736818,
-20.8751222092299,-20.7517296234012,-20.5705052234198,-20.3382869277355,
-20.2266059298047,-20.0233423698298,-19.8491553360417,-19.6541417125856,
-19.5151391277833,-19.3112475069076,-18.9971860038498,-18.8697053091383,
-18.6654013868218,-18.4761495657214,-18.3202149817156,-18.1926036175017,
-18.0055480775392,-17.7772911355014,-17.5965622030943,-17.4820501552149,
-17.254067231833,-17.0723774292265,-16.9497776930168,-16.8274806751369,
-16.6105938804691,-16.42724496372,-16.3390445012698),.UNSPECIFIED.);
#29518=B_SPLINE_CURVE_WITH_KNOTS('',3,(#113795,#113796,#113797,#113798,
#113799,#113800,#113801,#113802,#113803,#113804,#113805,#113806,#113807,
#113808,#113809,#113810,#113811,#113812,#113813,#113814,#113815,#113816,
#113817,#113818,#113819,#113820,#113821,#113822,#113823,#113824,#113825,
#113826,#113827,#113828,#113829,#113830,#113831,#113832,#113833,#113834,
#113835,#113836,#113837,#113838,#113839,#113840,#113841,#113842,#113843,
#113844,#113845,#113846,#113847,#113848,#113849,#113850,#113851,#113852,
#113853,#113854,#113855,#113856,#113857,#113858,#113859,#113860,#113861,
#113862,#113863,#113864,#113865,#113866,#113867,#113868,#113869,#113870,
#113871,#113872,#113873,#113874,#113875,#113876,#113877,#113878,#113879,
#113880,#113881,#113882,#113883,#113884,#113885,#113886,#113887,#113888,
#113889,#113890,#113891,#113892,#113893,#113894,#113895,#113896,#113897,
#113898,#113899,#113900,#113901,#113902,#113903,#113904,#113905,#113906,
#113907,#113908,#113909,#113910,#113911,#113912,#113913,#113914,#113915,
#113916,#113917,#113918,#113919,#113920,#113921,#113922,#113923,#113924),
 .UNSPECIFIED.,.F.,.F.,(4,2,2,2,2,2,2,2,2,2,2,2,2,2,2,2,2,2,2,2,2,2,2,2,
2,2,2,2,2,2,2,2,2,2,2,2,2,2,2,2,2,2,2,2,2,2,2,2,2,2,2,2,2,2,2,2,2,2,2,2,
2,2,2,2,4),(-18.0721778794789,-18.0147391790313,-17.848488462182,-17.6523618007567,
-17.4700564061978,-17.3315069833901,-17.1399140645343,-16.9510607065254,
-16.7547238024059,-16.6382243763846,-16.4131310110674,-16.2310907448218,
-16.1090716764663,-15.9862441360979,-15.7700282293703,-15.5865362500968,
-15.4579456815901,-15.3260537827938,-15.1246399336788,-14.9414739734795,
-14.8211784252922,-14.6965292288557,-14.4825265993111,-14.2984956615897,
-14.1707149237915,-14.0378832037766,-13.8386208210009,-13.6558760636882,
-13.5349646836358,-13.4110162700538,-13.196182681518,-13.012369598465,-12.8842744198052,
-12.7518244552662,-12.5517071320015,-12.3688020842637,-12.2481359237797,
-12.1239203513428,-11.9094128952947,-11.7255208756108,-11.5975483555581,
-11.4649570988441,-11.2651676578925,-11.0823276922443,-10.9615705901044,
-10.8374602821415,-10.6228321046749,-10.4389743666522,-10.3109571588975,
-10.1784233654973,-9.97851117792921,-9.79564987665335,-9.67493035708778,
-9.55078209715648,-9.33620479360897,-9.15233765659768,-9.02434023802163,
-8.89178711592832,-8.69192612399274,-8.50907676515503,-8.38834528084005,
-8.26421415879336,-8.04962168685307,-7.86576193192956,-7.77890601744087),
 .UNSPECIFIED.);
#29519=B_SPLINE_CURVE_WITH_KNOTS('',3,(#113939,#113940,#113941,#113942,
#113943,#113944,#113945,#113946,#113947,#113948,#113949,#113950,#113951,
#113952,#113953,#113954,#113955,#113956,#113957,#113958),.UNSPECIFIED.,
 .F.,.F.,(4,2,2,2,2,2,2,2,2,4),(-8.47209184883771,-8.00048983906625,-7.52055114659877,
-6.8722219354319,-6.22309965668783,-5.57315017673749,-4.92241575243503,
-4.27087199654946,-3.61860418547544,-3.49997929625738),.UNSPECIFIED.);
#29520=B_SPLINE_CURVE_WITH_KNOTS('',3,(#113962,#113963,#113964,#113965,
#113966,#113967,#113968,#113969,#113970,#113971,#113972,#113973,#113974,
#113975,#113976,#113977,#113978,#113979,#113980,#113981),.UNSPECIFIED.,
 .F.,.F.,(4,2,2,2,2,2,2,2,2,4),(-3.49997929625738,-2.96555708180064,-2.63548584285813,
-2.32891559001148,-1.67589454653547,-1.34607632565228,-1.03948591871613,
-0.517021270138503,-0.266082667592821,-9.99999997031153E-7),
 .UNSPECIFIED.);
#29521=B_SPLINE_CURVE_WITH_KNOTS('',3,(#113982,#113983,#113984,#113985,
#113986,#113987,#113988,#113989,#113990,#113991,#113992,#113993,#113994,
#113995,#113996,#113997),.UNSPECIFIED.,.F.,.F.,(4,2,2,2,2,2,2,4),(1.00000001422647E-6,
0.289657184683206,0.584406985012342,1.32553765774545,1.87661181724534,2.26478053342409,
2.87644457082816,3.45555001571885),.UNSPECIFIED.);
#29522=B_SPLINE_CURVE_WITH_KNOTS('',3,(#113999,#114000,#114001,#114002,
#114003,#114004,#114005,#114006,#114007,#114008,#114009,#114010,#114011,
#114012,#114013,#114014,#114015,#114016,#114017,#114018,#114019,#114020,
#114021,#114022,#114023,#114024,#114025,#114026,#114027,#114028,#114029,
#114030,#114031,#114032,#114033,#114034,#114035,#114036,#114037,#114038,
#114039,#114040,#114041,#114042,#114043,#114044,#114045,#114046,#114047,
#114048,#114049,#114050,#114051,#114052,#114053,#114054,#114055,#114056,
#114057,#114058,#114059,#114060,#114061,#114062,#114063,#114064,#114065,
#114066,#114067,#114068,#114069,#114070,#114071,#114072,#114073,#114074,
#114075,#114076,#114077,#114078,#114079,#114080,#114081,#114082,#114083,
#114084,#114085,#114086,#114087,#114088,#114089,#114090,#114091,#114092,
#114093,#114094,#114095,#114096,#114097,#114098,#114099,#114100,#114101,
#114102,#114103,#114104,#114105,#114106,#114107,#114108,#114109,#114110,
#114111,#114112),.UNSPECIFIED.,.F.,.F.,(4,2,2,2,2,2,2,2,2,2,2,2,2,2,2,2,
2,2,2,2,2,2,2,2,2,2,2,2,2,2,2,2,2,2,2,2,2,2,2,2,2,2,2,2,2,2,2,2,2,2,2,2,
2,2,2,2,4),(2.41008863111305,2.52174442163098,2.70033972549205,2.92369762280168,
3.04486262995073,3.2699058204366,3.47593555345123,3.71971767488146,3.93301751394918,
4.14313038398822,4.38696718236632,4.52827216930786,4.70511631179351,4.95526170895235,
5.05978336461602,5.19319665811648,5.37184186831745,5.59474028269326,5.7162341072511,
5.94201868468735,6.14780793011872,6.39208756826504,6.59175960584656,6.81006046539538,
7.05854698653331,7.20057922269586,7.37723602770402,7.62878532831887,7.73236772863619,
7.93016354412659,8.14674889545556,8.39450091527641,8.53613198848105,8.71290018477586,
8.96372521774679,9.06781001094518,9.2027827813947,9.3807836127047,9.61369745721821,
9.72870340636482,9.93943009685857,10.150844445182,10.3980528363782,10.61427984803,
10.8233562392541,11.0673155262955,11.2701613800128,11.4848671499499,11.735161198995,
11.9483525425192,12.1585505827427,12.4024637528689,12.5437967955747,12.7206663052054,
12.9708642740141,13.075392587722,13.0972599015927),.UNSPECIFIED.);
#29523=B_SPLINE_CURVE_WITH_KNOTS('',3,(#114113,#114114,#114115,#114116,
#114117,#114118,#114119,#114120,#114121,#114122,#114123,#114124,#114125,
#114126,#114127,#114128,#114129,#114130,#114131,#114132,#114133,#114134,
#114135,#114136,#114137,#114138,#114139,#114140,#114141,#114142,#114143,
#114144,#114145,#114146,#114147,#114148,#114149,#114150,#114151,#114152,
#114153,#114154,#114155,#114156,#114157,#114158,#114159,#114160,#114161,
#114162,#114163,#114164,#114165,#114166,#114167,#114168,#114169,#114170,
#114171,#114172,#114173,#114174,#114175,#114176,#114177,#114178,#114179,
#114180,#114181,#114182,#114183,#114184,#114185,#114186,#114187,#114188,
#114189,#114190,#114191,#114192,#114193,#114194,#114195,#114196,#114197,
#114198,#114199,#114200,#114201,#114202,#114203,#114204,#114205,#114206,
#114207,#114208,#114209,#114210,#114211,#114212,#114213,#114214,#114215,
#114216,#114217,#114218,#114219,#114220,#114221,#114222,#114223,#114224),
 .UNSPECIFIED.,.F.,.F.,(4,2,2,2,2,2,2,2,2,2,2,2,2,2,2,2,2,2,2,2,2,2,2,2,
2,2,2,2,2,2,2,2,2,2,2,2,2,2,2,2,2,2,2,2,2,2,2,2,2,2,2,2,2,2,2,4),(35.6719042779843,
35.698846252975,35.9456358690002,36.1561600266645,36.3691876752439,36.4852065366329,
36.7165059103028,36.8945968142958,37.0293842265218,37.1335515931008,37.3842580697099,
37.5610455870247,37.7026183581998,37.9465483670245,38.156808619327,38.3697830199319,
38.6199604238591,38.8343464422794,39.0378777959768,39.2854304033603,39.5002526882164,
39.7019618265655,39.8068806810891,40.0564398533407,40.2333648418571,40.374422708839,
40.6183598224011,40.828585309869,41.0416113215738,41.2918064614692,41.5062756580261,
41.7095792835508,41.9536140589348,42.1629930736033,42.3782883405402,42.6224005275956,
42.8295076043742,43.0515020881796,43.1713412678411,43.396670626196,43.5751131440329,
43.7090103891009,43.8134320109559,44.0637072404468,44.240525253567,44.3818890339293,
44.6299725742976,44.8472345963081,45.0435004559988,45.1465753469289,45.4038401488928,
45.5827799938148,45.7182660506219,45.8319348150512,46.018095320874,46.173488535676),
 .UNSPECIFIED.);
#29524=B_SPLINE_CURVE_WITH_KNOTS('',3,(#114240,#114241,#114242,#114243,
#114244,#114245,#114246,#114247,#114248,#114249,#114250,#114251,#114252,
#114253,#114254,#114255,#114256,#114257),.UNSPECIFIED.,.F.,.F.,(4,2,2,2,
2,2,2,2,4),(0.000255302998063218,0.246325831779527,0.49141476805784,0.65921643818013,
0.997718736921762,1.17390964291707,1.34739888243814,1.62418200982642,1.88073156156305),
 .UNSPECIFIED.);
#29525=B_SPLINE_CURVE_WITH_KNOTS('',3,(#114258,#114259,#114260,#114261,
#114262,#114263,#114264,#114265,#114266,#114267,#114268,#114269,#114270,
#114271,#114272,#114273),.UNSPECIFIED.,.F.,.F.,(4,2,2,2,2,2,2,4),(4.9144922740773E-5,
0.142815688788647,0.281124699864451,0.565337366058049,0.730491337491295,
0.901589879048025,1.18024330277771,1.46497496578543),.UNSPECIFIED.);
#29526=B_SPLINE_CURVE_WITH_KNOTS('',3,(#114275,#114276,#114277,#114278,
#114279,#114280),.UNSPECIFIED.,.F.,.F.,(4,2,4),(0.490673357805338,0.745336678902669,
0.999999351274048),.UNSPECIFIED.);
#29527=B_SPLINE_CURVE_WITH_KNOTS('',3,(#114282,#114283,#114284,#114285,
#114286,#114287),.UNSPECIFIED.,.F.,.F.,(4,2,4),(0.000935847610688105,0.245336678902669,
0.490673357805338),.UNSPECIFIED.);
#29528=B_SPLINE_CURVE_WITH_KNOTS('',3,(#114291,#114292,#114293,#114294,
#114295,#114296,#114297,#114298,#114299,#114300,#114301,#114302,#114303,
#114304,#114305,#114306,#114307,#114308,#114309,#114310,#114311,#114312,
#114313,#114314,#114315,#114316,#114317,#114318),.UNSPECIFIED.,.F.,.F.,
(4,2,2,2,2,2,2,2,2,2,2,2,2,4),(-2.64509018645311,-2.50816004857991,-2.34671657830517,
-2.01718588845666,-1.85756130276746,-1.70918083912142,-1.55034169509354,
-1.22132434868371,-1.06162752878633,-0.905703863111212,-0.749839080353907,
-0.422524714244554,-0.31803881392449,-9.99999997919332E-7),
 .UNSPECIFIED.);
#29529=B_SPLINE_CURVE_WITH_KNOTS('',3,(#114320,#114321,#114322,#114323,
#114324,#114325,#114326,#114327,#114328,#114329,#114330,#114331,#114332,
#114333,#114334,#114335,#114336,#114337,#114338,#114339,#114340,#114341,
#114342,#114343,#114344,#114345,#114346,#114347,#114348,#114349),
 .UNSPECIFIED.,.F.,.F.,(4,2,2,2,2,2,2,2,2,2,2,2,2,2,4),(-2.22830115735267,
-2.10423539530511,-1.98117528854211,-1.76090462968372,-1.61039047033868,
-1.27976081955513,-1.11407105510081,-0.947815483327209,-0.811106554685308,
-0.570211254781244,-0.456895349287952,-0.242344900393441,-0.166499094513352,
-0.0837880375494301,-0.00040012110997669),.UNSPECIFIED.);
#29530=B_SPLINE_CURVE_WITH_KNOTS('',3,(#114350,#114351,#114352,#114353,
#114354,#114355,#114356,#114357),.UNSPECIFIED.,.F.,.F.,(4,2,2,4),(-0.414938412676938,
-0.20738927105766,-0.103997999406809,-3.00555698333633E-5),
 .UNSPECIFIED.);
#29531=B_SPLINE_CURVE_WITH_KNOTS('',3,(#114358,#114359,#114360,#114361,
#114362,#114363,#114364,#114365,#114366,#114367,#114368,#114369,#114370,
#114371,#114372,#114373,#114374,#114375,#114376,#114377,#114378,#114379,
#114380,#114381,#114382,#114383,#114384,#114385,#114386,#114387,#114388,
#114389,#114390,#114391,#114392,#114393,#114394,#114395,#114396,#114397,
#114398,#114399,#114400,#114401,#114402,#114403,#114404,#114405,#114406,
#114407,#114408,#114409,#114410,#114411),.UNSPECIFIED.,.F.,.F.,(4,2,2,2,
2,2,2,2,2,2,2,2,2,2,2,2,2,2,2,2,2,2,2,2,2,2,4),(-5.28894858945498,-5.08167259374315,
-4.81846912921226,-4.67057708951716,-4.33526508630831,-4.17540607219834,
-3.93856667323282,-3.73878662711519,-3.50054599788927,-3.27019447785332,
-3.12273109480938,-2.97074609410328,-2.64130975684182,-2.41922687895394,
-2.28199475627433,-2.06266818806845,-1.80663906162605,-1.6623990385579,
-1.32730358543026,-1.16824509313182,-0.931652725510682,-0.768974340438366,
-0.515348342954449,-0.371740570718675,-0.186227377844307,-0.093912563896873,
-1.00000000813338E-6),.UNSPECIFIED.);
#29532=B_SPLINE_CURVE_WITH_KNOTS('',3,(#114415,#114416,#114417,#114418,
#114419,#114420,#114421,#114422,#114423,#114424,#114425,#114426,#114427,
#114428,#114429,#114430,#114431,#114432,#114433,#114434,#114435,#114436,
#114437,#114438,#114439,#114440,#114441,#114442,#114443,#114444,#114445,
#114446,#114447,#114448,#114449,#114450,#114451,#114452,#114453,#114454,
#114455,#114456,#114457,#114458,#114459,#114460),.UNSPECIFIED.,.F.,.F.,
(4,2,2,1,1,1,2,2,2,2,1,1,1,1,2,2,2,2,2,2,2,2,1,1,1,2,2,4),(0.,0.124999999999551,
0.187499999999329,0.21874999999922,0.234374999999166,0.242187499999141,
0.248046874999122,0.249999999999116,0.374999999998904,0.437499999998797,
0.468749999998741,0.484374999998712,0.492187499998699,0.496093749998692,
0.499023437498686,0.499999999998685,0.562499999998843,0.593749999998923,
0.609374999998965,0.624999999999006,0.687499999999173,0.718749999999255,
0.734374999999296,0.742187499999314,0.746093749999326,0.748046874999334,
0.749999999999342,0.999999681575655),.UNSPECIFIED.);
#29533=B_SPLINE_CURVE_WITH_KNOTS('',3,(#114462,#114463,#114464,#114465,
#114466,#114467,#114468,#114469,#114470,#114471,#114472,#114473,#114474,
#114475,#114476,#114477,#114478,#114479,#114480,#114481,#114482,#114483,
#114484,#114485,#114486,#114487,#114488,#114489,#114490,#114491,#114492,
#114493,#114494,#114495,#114496,#114497,#114498,#114499,#114500,#114501,
#114502,#114503,#114504),.UNSPECIFIED.,.F.,.F.,(4,3,3,3,3,3,3,3,3,3,3,3,
3,3,4),(0.,0.0851829461708695,0.125,0.222485710899397,0.25,0.359792863725203,
0.375,0.5,0.625,0.634408323454812,0.75,0.771715737793405,0.875,0.909019034253072,
1.),.UNSPECIFIED.);
#29534=B_SPLINE_CURVE_WITH_KNOTS('',3,(#114506,#114507,#114508,#114509,
#114510,#114511,#114512,#114513,#114514,#114515,#114516,#114517,#114518,
#114519,#114520,#114521,#114522,#114523,#114524,#114525,#114526,#114527,
#114528,#114529,#114530,#114531,#114532,#114533,#114534,#114535,#114536,
#114537,#114538,#114539,#114540,#114541,#114542,#114543,#114544,#114545,
#114546,#114547,#114548,#114549,#114550,#114551,#114552,#114553,#114554,
#114555,#114556,#114557,#114558,#114559,#114560,#114561,#114562,#114563,
#114564,#114565,#114566,#114567,#114568,#114569,#114570,#114571,#114572,
#114573,#114574,#114575,#114576,#114577,#114578,#114579,#114580,#114581,
#114582,#114583,#114584,#114585,#114586,#114587,#114588,#114589,#114590,
#114591,#114592,#114593,#114594,#114595,#114596,#114597,#114598,#114599,
#114600,#114601,#114602,#114603,#114604,#114605,#114606,#114607,#114608,
#114609,#114610,#114611,#114612,#114613,#114614,#114615,#114616,#114617,
#114618,#114619,#114620,#114621,#114622,#114623,#114624,#114625,#114626,
#114627,#114628,#114629,#114630,#114631,#114632,#114633,#114634,#114635,
#114636,#114637,#114638,#114639,#114640,#114641,#114642,#114643,#114644,
#114645,#114646,#114647,#114648,#114649,#114650,#114651,#114652,#114653,
#114654,#114655,#114656,#114657,#114658,#114659,#114660,#114661,#114662,
#114663,#114664,#114665,#114666,#114667,#114668,#114669,#114670,#114671),
 .UNSPECIFIED.,.F.,.F.,(4,3,3,3,3,3,3,3,3,3,3,3,3,3,3,3,3,3,3,3,3,3,3,3,
3,3,3,3,3,3,3,3,3,3,3,3,3,3,3,3,3,3,3,3,3,3,3,3,3,3,3,3,3,3,3,4),(0.,0.0502845361710956,
0.0994669690397177,0.126508894795659,0.177997127033869,0.202535883941732,
0.250000000000155,0.275210682027024,0.336732694395824,0.343185824135615,
0.375000000000234,0.407090352173637,0.437500000000274,0.468541360955746,
0.468750000000296,0.484375000000307,0.492187500000312,0.496093750000314,
0.500000000000316,0.533182600914947,0.562500000000305,0.593750000000299,
0.602610758708892,0.609375000000297,0.617187500000295,0.621093750000294,
0.623046875000291,0.625000000000289,0.646711254898203,0.668295817163414,
0.683216765640327,0.687500000000225,0.708161347198757,0.718750000000194,
0.73437500000018,0.742187500000173,0.743753663871175,0.74609375000017,0.74975032942102,
0.750000000000166,0.773417459328957,0.797812834268651,0.804484657939817,
0.812500000000111,0.839850659045814,0.843750000000082,0.859375000000067,
0.867187500000061,0.87109375000006,0.873046875000058,0.875000000000055,
0.880771660675667,0.92555749543768,0.951439720715529,0.994584358314706,
1.),.UNSPECIFIED.);
#29535=B_SPLINE_CURVE_WITH_KNOTS('',3,(#114673,#114674,#114675,#114676,
#114677,#114678,#114679,#114680,#114681,#114682,#114683,#114684,#114685,
#114686,#114687,#114688,#114689,#114690,#114691,#114692,#114693,#114694,
#114695,#114696,#114697,#114698,#114699,#114700,#114701,#114702,#114703,
#114704,#114705,#114706,#114707,#114708,#114709,#114710,#114711,#114712,
#114713,#114714,#114715,#114716,#114717,#114718,#114719,#114720,#114721,
#114722,#114723,#114724,#114725,#114726,#114727,#114728,#114729,#114730,
#114731,#114732,#114733,#114734,#114735,#114736,#114737,#114738,#114739,
#114740,#114741,#114742,#114743,#114744,#114745,#114746,#114747,#114748,
#114749,#114750,#114751,#114752,#114753,#114754,#114755,#114756,#114757,
#114758,#114759,#114760,#114761,#114762,#114763,#114764,#114765,#114766,
#114767,#114768,#114769,#114770,#114771,#114772,#114773,#114774,#114775,
#114776,#114777,#114778,#114779,#114780,#114781,#114782,#114783,#114784,
#114785,#114786,#114787,#114788,#114789,#114790,#114791,#114792,#114793,
#114794,#114795,#114796,#114797,#114798,#114799,#114800,#114801,#114802,
#114803,#114804,#114805,#114806,#114807,#114808,#114809,#114810,#114811),
 .UNSPECIFIED.,.F.,.F.,(4,3,3,3,3,3,3,3,3,3,3,3,3,3,3,3,3,3,3,3,3,3,3,3,
3,3,3,3,3,3,3,3,3,3,3,3,3,3,3,3,3,3,3,3,3,3,4),(0.,0.0387804699265066,0.0942195402664754,
0.102869907782688,0.124999999999886,0.168539308649517,0.187499999999826,
0.218749999999794,0.234374999999778,0.236283397554344,0.242187499999772,
0.24609374999977,0.249718717532596,0.249999999999769,0.301433219361833,
0.312499999999771,0.343749999999771,0.359374999999769,0.367187499999768,
0.368285161567645,0.373965193564266,0.374999999999768,0.4186575976671,0.43658151927549,
0.437499999999769,0.468749999999769,0.484374999999771,0.492187499999769,
0.496093749999768,0.498046874999767,0.499600428894499,0.499999999999766,
0.552876401003889,0.572979629602993,0.627644747305819,0.644937199235735,
0.698789788204271,0.71444928382849,0.749999999999883,0.781357579985869,
0.833170646642696,0.845560939644304,0.896652264821656,0.906911855988006,
0.955116861547587,0.965240055383411,1.),.UNSPECIFIED.);
#29536=B_SPLINE_CURVE_WITH_KNOTS('',3,(#114813,#114814,#114815,#114816,
#114817,#114818,#114819,#114820,#114821,#114822,#114823,#114824,#114825,
#114826,#114827,#114828,#114829,#114830,#114831,#114832,#114833,#114834,
#114835,#114836,#114837,#114838,#114839,#114840,#114841,#114842,#114843,
#114844,#114845,#114846,#114847,#114848,#114849,#114850,#114851,#114852,
#114853,#114854,#114855),.UNSPECIFIED.,.F.,.F.,(4,3,3,3,3,3,3,3,3,3,3,3,
3,3,4),(0.,0.0891026163983255,0.125,0.226410788650375,0.25,0.363723238331853,
0.375,0.5,0.625,0.638348932643424,0.75,0.775661264039743,0.875,0.912969309651361,
1.),.UNSPECIFIED.);
#29537=B_SPLINE_CURVE_WITH_KNOTS('',3,(#114857,#114858,#114859,#114860,
#114861,#114862,#114863,#114864,#114865,#114866,#114867,#114868,#114869,
#114870,#114871,#114872,#114873,#114874,#114875,#114876,#114877,#114878,
#114879,#114880,#114881,#114882,#114883,#114884,#114885,#114886,#114887,
#114888,#114889,#114890,#114891,#114892,#114893,#114894,#114895,#114896,
#114897,#114898,#114899,#114900,#114901,#114902,#114903,#114904,#114905,
#114906,#114907,#114908,#114909,#114910,#114911,#114912),.UNSPECIFIED.,
 .F.,.F.,(4,2,2,1,1,1,1,2,2,2,2,2,2,2,2,1,1,1,1,2,2,2,1,1,1,1,2,2,2,1,1,
1,1,2,2,4),(0.,0.124999999999216,0.187499999998822,0.218749999998626,0.234374999998527,
0.242187499998475,0.246093749998447,0.248046874998435,0.249999999998424,
0.312499999998387,0.343749999998366,0.359374999998357,0.374999999998348,
0.437499999998312,0.468749999998293,0.484374999998284,0.492187499998276,
0.496093749998271,0.498046874998268,0.499023437498271,0.499999999998274,
0.562499999998525,0.593749999998648,0.609374999998706,0.617187499998738,
0.621093749998754,0.623046874998761,0.624999999998768,0.687499999998984,
0.71874999999909,0.734374999999143,0.742187499999172,0.746093749999189,
0.748046874999198,0.749999999999207,1.),.UNSPECIFIED.);
#29538=B_SPLINE_CURVE_WITH_KNOTS('',3,(#114917,#114918,#114919,#114920,
#114921,#114922,#114923,#114924,#114925,#114926,#114927,#114928,#114929,
#114930,#114931,#114932,#114933,#114934,#114935,#114936,#114937,#114938,
#114939,#114940,#114941,#114942,#114943,#114944,#114945,#114946,#114947,
#114948,#114949,#114950,#114951,#114952,#114953,#114954,#114955,#114956,
#114957,#114958,#114959,#114960,#114961,#114962,#114963,#114964,#114965,
#114966,#114967,#114968,#114969,#114970,#114971,#114972,#114973,#114974,
#114975,#114976,#114977,#114978,#114979,#114980,#114981,#114982,#114983,
#114984,#114985,#114986,#114987,#114988,#114989,#114990,#114991,#114992,
#114993,#114994,#114995,#114996,#114997,#114998,#114999,#115000,#115001,
#115002,#115003,#115004,#115005,#115006,#115007,#115008,#115009,#115010,
#115011,#115012,#115013,#115014,#115015,#115016,#115017,#115018,#115019,
#115020,#115021,#115022,#115023,#115024,#115025,#115026,#115027,#115028,
#115029,#115030,#115031,#115032,#115033,#115034,#115035,#115036,#115037,
#115038,#115039,#115040,#115041,#115042,#115043,#115044,#115045,#115046,
#115047,#115048,#115049,#115050,#115051,#115052,#115053,#115054,#115055,
#115056,#115057,#115058,#115059,#115060,#115061,#115062,#115063,#115064,
#115065,#115066,#115067),.UNSPECIFIED.,.F.,.F.,(4,3,3,3,3,3,3,3,3,3,3,3,
3,3,3,3,3,3,3,3,3,3,3,3,3,3,3,3,3,3,3,3,3,3,3,3,3,3,3,3,3,3,3,3,3,3,3,3,
3,3,4),(0.,0.062500000000062,0.121231089415165,0.125000000000124,0.163221664701878,
0.187500000000186,0.218750000000215,0.234375000000229,0.242187500000236,
0.24804687500024,0.250000000000239,0.304896813849926,0.312500000000136,
0.332752681627818,0.343750000000084,0.35937500000006,0.367187500000049,
0.371093750000046,0.373046875000042,0.375000000000038,0.416499412144631,
0.437500000000003,0.468749999999986,0.48437499999998,0.492187499999977,
0.496093749999974,0.498046874999974,0.499999999999975,0.505620037612421,
0.542493516498535,0.562500000000078,0.59375000000013,0.609375000000156,
0.617187500000171,0.624056075689695,0.625000000000187,0.652859210405975,
0.667499665105052,0.687500000000334,0.716973604152224,0.718750000000407,
0.734375000000444,0.742187500000462,0.746093750000471,0.748046875000471,
0.750000000000471,0.80654618724685,0.848568566521544,0.91466210797078,0.984037448506897,
1.),.UNSPECIFIED.);
#29539=B_SPLINE_CURVE_WITH_KNOTS('',3,(#115069,#115070,#115071,#115072,
#115073,#115074,#115075,#115076,#115077,#115078,#115079,#115080,#115081,
#115082,#115083,#115084,#115085,#115086,#115087,#115088,#115089,#115090,
#115091,#115092,#115093,#115094,#115095,#115096,#115097,#115098,#115099,
#115100,#115101,#115102,#115103,#115104,#115105,#115106,#115107,#115108,
#115109,#115110,#115111,#115112,#115113,#115114,#115115,#115116,#115117,
#115118,#115119,#115120,#115121,#115122,#115123,#115124,#115125,#115126,
#115127,#115128,#115129,#115130,#115131,#115132,#115133,#115134,#115135,
#115136,#115137,#115138,#115139,#115140,#115141,#115142,#115143,#115144,
#115145,#115146,#115147,#115148,#115149,#115150,#115151,#115152,#115153,
#115154,#115155,#115156,#115157,#115158,#115159,#115160,#115161,#115162,
#115163,#115164,#115165,#115166,#115167,#115168,#115169,#115170,#115171,
#115172,#115173,#115174,#115175,#115176,#115177,#115178,#115179,#115180,
#115181,#115182,#115183,#115184,#115185,#115186,#115187,#115188,#115189,
#115190,#115191,#115192,#115193,#115194,#115195,#115196,#115197,#115198,
#115199,#115200,#115201,#115202,#115203,#115204,#115205,#115206,#115207,
#115208,#115209,#115210,#115211,#115212,#115213,#115214,#115215,#115216,
#115217,#115218,#115219),.UNSPECIFIED.,.F.,.F.,(4,3,3,3,3,3,3,3,3,3,3,3,
3,3,3,3,3,3,3,3,3,3,3,3,3,3,3,3,3,3,3,3,3,3,3,3,3,3,3,3,3,3,3,3,3,3,3,3,
3,3,4),(1.72657252367726E-14,0.0313585598533987,0.0630900598213949,0.0954643376068659,
0.124999999999572,0.158293445510127,0.192289017368953,0.218749999999252,
0.234374999999199,0.242187499999174,0.246093749999162,0.248046874999155,
0.249511718749151,0.249999999999149,0.277343749999143,0.303223001372441,
0.328859577421254,0.354258958240136,0.379426422600146,0.404255272733001,
0.42889482456838,0.453251627638804,0.468749999999104,0.484374999999102,
0.492187499999101,0.496093749999101,0.499126022146931,0.499999999999101,
0.523490792672927,0.547898193588698,0.571926688005287,0.596161788289904,
0.620607891014182,0.64539693871608,0.670375825827579,0.695677573208496,
0.718749999999088,0.734374999999086,0.742187499999085,0.746093749999085,
0.748046874999085,0.749511718749087,0.749999999999087,0.784171524212072,
0.81788730066329,0.850916982531674,0.874999999999544,0.907027947890119,
0.938664708227929,0.969685288090575,1.),.UNSPECIFIED.);
#29540=B_SPLINE_CURVE_WITH_KNOTS('',3,(#115220,#115221,#115222,#115223,
#115224,#115225,#115226,#115227,#115228,#115229,#115230,#115231,#115232,
#115233,#115234,#115235,#115236,#115237,#115238,#115239,#115240,#115241,
#115242,#115243,#115244,#115245,#115246,#115247,#115248,#115249,#115250,
#115251,#115252,#115253,#115254,#115255,#115256,#115257,#115258,#115259,
#115260,#115261,#115262,#115263,#115264,#115265,#115266,#115267,#115268,
#115269,#115270,#115271,#115272,#115273,#115274),.UNSPECIFIED.,.F.,.F.,
(4,2,2,1,1,1,1,2,2,2,2,1,2,2,2,2,1,1,1,2,2,2,1,1,1,1,2,2,2,1,1,1,2,2,4),
(0.,0.12500000000011,0.187500000000167,0.218750000000197,0.234375000000212,
0.242187500000223,0.246093750000225,0.248046875000223,0.250000000000222,
0.312500000000213,0.343750000000213,0.35937500000021,0.367187500000211,
0.375000000000212,0.437500000000193,0.468750000000179,0.484375000000175,
0.492187500000171,0.496093750000168,0.498046875000166,0.500000000000165,
0.562500000000093,0.593750000000061,0.609375000000042,0.617187500000036,
0.621093750000036,0.623046875000033,0.62500000000003,0.687500000000018,
0.718750000000013,0.734375000000011,0.74218750000001,0.746093750000013,
0.750000000000015,1.),.UNSPECIFIED.);
#29541=B_SPLINE_CURVE_WITH_KNOTS('',3,(#115286,#115287,#115288,#115289,
#115290,#115291,#115292,#115293,#115294,#115295,#115296,#115297,#115298,
#115299,#115300,#115301,#115302,#115303,#115304,#115305,#115306,#115307,
#115308,#115309,#115310,#115311,#115312,#115313,#115314,#115315,#115316,
#115317,#115318,#115319,#115320,#115321,#115322,#115323,#115324,#115325,
#115326,#115327,#115328,#115329,#115330,#115331,#115332,#115333,#115334,
#115335,#115336,#115337,#115338,#115339,#115340,#115341,#115342,#115343,
#115344,#115345,#115346,#115347,#115348,#115349,#115350,#115351,#115352,
#115353,#115354,#115355,#115356,#115357,#115358,#115359,#115360,#115361,
#115362,#115363,#115364,#115365,#115366,#115367,#115368,#115369,#115370,
#115371,#115372,#115373,#115374,#115375,#115376,#115377,#115378,#115379,
#115380,#115381,#115382,#115383,#115384,#115385,#115386,#115387,#115388,
#115389,#115390,#115391,#115392,#115393,#115394,#115395,#115396,#115397,
#115398,#115399,#115400,#115401,#115402,#115403,#115404,#115405,#115406,
#115407,#115408,#115409,#115410,#115411,#115412,#115413,#115414,#115415),
 .UNSPECIFIED.,.F.,.F.,(4,3,3,3,3,3,3,3,3,3,3,3,3,3,3,3,3,3,3,3,3,3,3,3,
3,3,3,3,3,3,3,3,3,3,3,3,3,3,3,3,3,3,3,4),(0.,0.0155305327960008,0.0311496512367539,
0.0467827647740799,0.0524931088100301,0.0681787493894734,0.0835455441413793,
0.0993906076345913,0.115235671127803,0.120656007198578,0.124426507423533,
0.125369132479772,0.126311757536011,0.128197007648489,0.135738008098405,
0.150820008998236,0.170300375377521,0.1809840107979,0.18297180671857,0.202416974502378,
0.221864494449803,0.241312014397229,0.243677276861593,0.248853014847146,
0.249795639903385,0.250738264959625,0.252623515072105,0.256394015297065,
0.271476016196905,0.297137858146395,0.301640017996586,0.310841253760449,
0.336445877357579,0.361968021595948,0.365738521820908,0.36831758881443,
0.369509022045868,0.371220548011419,0.377050022495787,0.392132023395624,
0.422296025195297,0.434902671324438,0.463575489153042,0.482624028794642),
 .UNSPECIFIED.);
#29542=B_SPLINE_CURVE_WITH_KNOTS('',3,(#115417,#115418,#115419,#115420,
#115421,#115422,#115423,#115424,#115425,#115426,#115427,#115428,#115429,
#115430,#115431,#115432,#115433,#115434,#115435,#115436,#115437,#115438,
#115439,#115440,#115441,#115442,#115443,#115444,#115445,#115446,#115447,
#115448,#115449,#115450,#115451,#115452,#115453,#115454),.UNSPECIFIED.,
 .F.,.F.,(4,2,2,1,2,2,2,2,2,1,1,1,1,2,2,2,2,1,1,1,2,2,4),(0.482624028794642,
0.498792027894815,0.514960026994988,0.547296025195333,0.611968021596022,
0.676640017996712,0.741312014397401,0.749396013947487,0.750406513891247,
0.751417013835008,0.753438013722528,0.757480013497569,0.77364801259773,
0.805984010798051,0.870656007198694,0.874698006973734,0.875708506917494,
0.876719006861254,0.878740006748774,0.886824006298856,0.902992005399019,
0.935328003599346,1.),.UNSPECIFIED.);
#29543=B_SPLINE_CURVE_WITH_KNOTS('',3,(#115463,#115464,#115465,#115466,
#115467,#115468,#115469,#115470,#115471,#115472,#115473,#115474,#115475,
#115476,#115477,#115478,#115479,#115480,#115481,#115482,#115483,#115484,
#115485,#115486,#115487,#115488,#115489,#115490,#115491,#115492,#115493,
#115494,#115495,#115496,#115497,#115498,#115499,#115500,#115501,#115502,
#115503,#115504,#115505,#115506,#115507,#115508,#115509,#115510,#115511,
#115512,#115513,#115514,#115515,#115516,#115517,#115518,#115519,#115520,
#115521,#115522,#115523,#115524,#115525,#115526,#115527,#115528,#115529),
 .UNSPECIFIED.,.F.,.F.,(4,3,3,3,3,3,3,3,3,3,3,3,3,3,3,3,3,3,3,3,3,3,4),
(0.51166377080594,0.527494550556984,0.543364644919874,0.559320212793699,
0.572705799393256,0.588776327230632,0.590143328248497,0.606753705472004,
0.618487320886823,0.622302447677953,0.624210011073519,0.626117574469085,
0.63374782805135,0.665558992312902,0.694789856709447,0.725310871038494,
0.740571378203017,0.748201631785278,0.754270747493039,0.755831885367539,
0.800644721001023,0.970898896272127,1.),.UNSPECIFIED.);
#29544=B_SPLINE_CURVE_WITH_KNOTS('',3,(#115531,#115532,#115533,#115534,
#115535,#115536,#115537,#115538,#115539,#115540,#115541,#115542,#115543,
#115544,#115545,#115546,#115547,#115548,#115549,#115550,#115551,#115552,
#115553,#115554,#115555,#115556,#115557,#115558,#115559,#115560,#115561,
#115562,#115563,#115564,#115565,#115566,#115567,#115568,#115569,#115570,
#115571,#115572,#115573,#115574,#115575,#115576,#115577,#115578,#115579,
#115580,#115581,#115582,#115583,#115584,#115585,#115586,#115587,#115588,
#115589,#115590,#115591,#115592,#115593,#115594,#115595,#115596,#115597,
#115598,#115599,#115600,#115601,#115602,#115603),.UNSPECIFIED.,.F.,.F.,
(4,3,3,3,3,3,3,3,3,3,3,3,3,3,3,3,3,3,3,3,3,3,3,3,4),(3.53787488667062E-13,
0.0213362951863518,0.0426471332641246,0.0639579713418974,0.0845324772100754,
0.104712953249514,0.111926449848326,0.119921196266065,0.123918569474935,
0.127076608691764,0.127915942683804,0.141403650168183,0.20292737719542,
0.223852899696638,0.239842392532111,0.255831885367583,0.352228943328355,
0.38374782805135,0.447705799393233,0.479684785064172,0.495674277899644,
0.499671651108512,0.501670337712947,0.503669024317381,0.511663770735164),
 .UNSPECIFIED.);
#29545=B_SPLINE_CURVE_WITH_KNOTS('',3,(#115681,#115682,#115683,#115684,
#115685,#115686,#115687,#115688,#115689,#115690,#115691,#115692,#115693,
#115694,#115695,#115696),.UNSPECIFIED.,.F.,.F.,(4,2,2,2,2,2,2,4),(-1.46479957099081,
-1.1805105246837,-0.90257725733764,-0.731520481211716,-0.566447433224417,
-0.281660671194902,-0.143091894881949,-4.91448849857019E-5),
 .UNSPECIFIED.);
#29546=B_SPLINE_CURVE_WITH_KNOTS('',3,(#115698,#115699,#115700,#115701,
#115702,#115703,#115704,#115705,#115706,#115707,#115708,#115709,#115710,
#115711,#115712,#115713,#115714,#115715),.UNSPECIFIED.,.F.,.F.,(4,2,2,2,
2,2,2,2,4),(-1.88059535984106,-1.62418108159893,-1.34742306272744,-1.17391543699637,
-0.99773934830901,-0.659269873371318,-0.49144696425701,-0.246353941888789,
-1.00000001190814E-6),.UNSPECIFIED.);
#29547=B_SPLINE_CURVE_WITH_KNOTS('',3,(#115719,#115720,#115721,#115722,
#115723,#115724),.UNSPECIFIED.,.F.,.F.,(4,2,4),(0.509326642194732,0.754663321097366,
0.999997368427725),.UNSPECIFIED.);
#29548=B_SPLINE_CURVE_WITH_KNOTS('',3,(#115725,#115726,#115727,#115728,
#115729,#115730),.UNSPECIFIED.,.F.,.F.,(4,2,4),(6.48725954440461E-7,0.254663321097366,
0.509326642194732),.UNSPECIFIED.);
#29549=B_SPLINE_CURVE_WITH_KNOTS('',3,(#115733,#115734,#115735,#115736,
#115737,#115738,#115739,#115740,#115741,#115742,#115743,#115744,#115745,
#115746,#115747,#115748,#115749,#115750,#115751,#115752,#115753,#115754,
#115755,#115756),.UNSPECIFIED.,.F.,.F.,(4,2,2,2,2,2,2,2,2,2,2,4),(0.415214370670141,
0.44414492098826,0.761187688701984,1.04803781412441,1.36663216176434,1.53126048254232,
1.69364240787812,1.9065115824004,2.23496333776899,2.51066490402767,2.78610480852283,
3.06208402115945),.UNSPECIFIED.);
#29550=B_SPLINE_CURVE_WITH_KNOTS('',3,(#115758,#115759,#115760,#115761,
#115762,#115763),.UNSPECIFIED.,.F.,.F.,(4,2,4),(-0.103830434024033,-0.0610640491738462,
-5.68668496666812E-5),.UNSPECIFIED.);
#29551=B_SPLINE_CURVE_WITH_KNOTS('',3,(#115766,#115767,#115768,#115769,
#115770,#115771,#115772,#115773,#115774,#115775,#115776,#115777),
 .UNSPECIFIED.,.F.,.F.,(4,2,2,2,2,4),(1.00000003078193E-6,0.31287663257672,
0.416307716745341,0.750817151791374,0.912809059863007,1.08729832187199),
 .UNSPECIFIED.);
#29552=B_SPLINE_CURVE_WITH_KNOTS('',3,(#115781,#115782,#115783,#115784,
#115785,#115786,#115787,#115788,#115789,#115790,#115791,#115792,#115793,
#115794,#115795,#115796,#115797,#115798,#115799,#115800,#115801,#115802,
#115803,#115804,#115805,#115806,#115807,#115808,#115809,#115810,#115811,
#115812,#115813,#115814,#115815,#115816,#115817,#115818,#115819,#115820,
#115821,#115822,#115823,#115824,#115825,#115826),.UNSPECIFIED.,.F.,.F.,
(4,2,2,1,1,1,2,2,2,2,1,1,1,1,2,2,2,2,2,2,2,2,1,1,1,2,2,4),(0.,0.124999999999755,
0.187499999999633,0.218749999999572,0.234374999999541,0.242187499999528,
0.248046874999513,0.249999999999507,0.374999999998963,0.437499999998691,
0.468749999998555,0.484374999998485,0.492187499998451,0.496093749998433,
0.499023437498418,0.499999999998412,0.562499999998579,0.593749999998663,
0.609374999998708,0.624999999998753,0.687499999998917,0.718749999999002,
0.734374999999047,0.742187499999073,0.746093749999086,0.748046874999093,
0.7499999999991,1.),.UNSPECIFIED.);
#29553=B_SPLINE_CURVE_WITH_KNOTS('',3,(#115828,#115829,#115830,#115831,
#115832,#115833,#115834,#115835,#115836,#115837,#115838,#115839,#115840,
#115841,#115842,#115843,#115844,#115845,#115846,#115847,#115848,#115849,
#115850,#115851,#115852,#115853,#115854,#115855,#115856,#115857,#115858,
#115859,#115860,#115861,#115862,#115863,#115864,#115865,#115866,#115867,
#115868,#115869,#115870,#115871,#115872,#115873,#115874,#115875,#115876,
#115877,#115878,#115879,#115880,#115881,#115882,#115883,#115884,#115885,
#115886,#115887,#115888,#115889,#115890,#115891,#115892,#115893,#115894,
#115895,#115896,#115897,#115898,#115899,#115900,#115901,#115902,#115903,
#115904,#115905,#115906,#115907,#115908,#115909,#115910,#115911,#115912,
#115913,#115914,#115915,#115916,#115917,#115918,#115919,#115920,#115921,
#115922,#115923,#115924,#115925,#115926,#115927,#115928,#115929,#115930,
#115931,#115932,#115933),.UNSPECIFIED.,.F.,.F.,(4,3,3,3,3,3,3,3,3,3,3,3,
3,3,3,3,3,3,3,3,3,3,3,3,3,3,3,3,3,3,3,3,3,3,3,4),(0.,0.0349290761455846,
0.0707303823045988,0.095011048545903,0.124999999999988,0.166181057698321,
0.187499999999982,0.218749999999978,0.234374999999977,0.240157824751891,
0.242187499999976,0.246093749999979,0.24902343749998,0.249999999999982,
0.31267456409958,0.372848667033719,0.375000000000061,0.432592797080129,
0.4375000000001,0.468750000000121,0.484375000000131,0.492187500000136,0.496093750000137,
0.499023437500137,0.500000000000137,0.500974800543195,0.574225292197682,
0.646387457364885,0.657372771579407,0.728223741866551,0.750000000000069,
0.792392860831951,0.863966896072285,0.909141464253675,0.975114473482201,
0.999999999977459),.UNSPECIFIED.);
#29554=B_SPLINE_CURVE_WITH_KNOTS('',3,(#115935,#115936,#115937,#115938,
#115939,#115940,#115941,#115942,#115943,#115944,#115945,#115946,#115947,
#115948,#115949,#115950,#115951,#115952,#115953,#115954,#115955,#115956,
#115957,#115958,#115959,#115960,#115961,#115962,#115963,#115964,#115965,
#115966,#115967,#115968,#115969,#115970,#115971,#115972,#115973,#115974,
#115975,#115976,#115977,#115978,#115979,#115980,#115981,#115982,#115983,
#115984,#115985,#115986,#115987,#115988,#115989,#115990,#115991,#115992,
#115993,#115994,#115995,#115996,#115997,#115998,#115999,#116000,#116001,
#116002,#116003,#116004,#116005,#116006,#116007,#116008,#116009,#116010,
#116011,#116012,#116013,#116014,#116015,#116016,#116017,#116018,#116019,
#116020,#116021,#116022,#116023,#116024,#116025,#116026,#116027,#116028,
#116029,#116030,#116031,#116032,#116033,#116034),.UNSPECIFIED.,.F.,.F.,
(4,3,3,3,3,3,3,3,3,3,3,3,3,3,3,3,3,3,3,3,3,3,3,3,3,3,3,3,3,3,3,3,3,4),(1.29149088468994E-15,
0.0582680136424074,0.11778957915424,0.132355339703123,0.195189423730358,
0.2499999999999,0.301027172061525,0.364795158597509,0.374999999999851,0.437499999999827,
0.468749999999815,0.484374999999807,0.492187499999803,0.496093749999802,
0.4980468749998,0.49993495296673,0.499999999999798,0.562499999999693,0.624999999999588,
0.675813194782976,0.687499999999484,0.718749999999429,0.734374999999402,
0.74218749999939,0.746093749999385,0.749023437499379,0.749999999999377,
0.794477594674165,0.837925486107252,0.859170308090223,0.898790378500282,
0.937526932086563,0.975001831172104,1.),.UNSPECIFIED.);
#29555=B_SPLINE_CURVE_WITH_KNOTS('',3,(#116036,#116037,#116038,#116039,
#116040,#116041,#116042,#116043,#116044,#116045,#116046,#116047,#116048,
#116049,#116050,#116051,#116052,#116053,#116054,#116055,#116056,#116057,
#116058,#116059,#116060,#116061,#116062,#116063,#116064,#116065,#116066,
#116067,#116068,#116069,#116070,#116071,#116072,#116073,#116074,#116075,
#116076,#116077,#116078,#116079,#116080,#116081,#116082,#116083,#116084,
#116085,#116086,#116087,#116088,#116089,#116090,#116091),.UNSPECIFIED.,
 .F.,.F.,(4,2,2,1,1,1,1,2,2,2,2,2,2,2,2,1,1,1,1,2,2,2,1,1,1,1,2,2,2,1,1,
1,1,2,2,4),(0.,0.125000000000341,0.187500000000507,0.218750000000587,0.234375000000627,
0.242187500000643,0.246093750000651,0.248046875000653,0.250000000000654,
0.312500000000671,0.343750000000679,0.359375000000681,0.375000000000683,
0.43750000000069,0.468750000000697,0.484375000000704,0.492187500000707,
0.496093750000704,0.498046875000703,0.499023437500703,0.500000000000703,
0.562500000000648,0.593750000000621,0.609375000000607,0.617187500000603,
0.621093750000601,0.6230468750006,0.625000000000599,0.687500000000444,0.718750000000368,
0.734375000000333,0.742187500000316,0.746093750000307,0.748046875000303,
0.750000000000299,1.),.UNSPECIFIED.);
#29556=B_SPLINE_CURVE_WITH_KNOTS('',3,(#116096,#116097,#116098,#116099,
#116100,#116101,#116102,#116103,#116104,#116105,#116106,#116107,#116108,
#116109,#116110,#116111,#116112,#116113,#116114,#116115,#116116,#116117,
#116118,#116119,#116120,#116121,#116122,#116123,#116124,#116125,#116126,
#116127,#116128,#116129,#116130,#116131,#116132,#116133,#116134,#116135,
#116136,#116137,#116138,#116139,#116140,#116141,#116142,#116143,#116144,
#116145,#116146,#116147,#116148,#116149,#116150,#116151,#116152,#116153,
#116154,#116155,#116156,#116157,#116158,#116159,#116160,#116161,#116162,
#116163,#116164,#116165,#116166,#116167,#116168,#116169,#116170,#116171,
#116172,#116173,#116174,#116175,#116176,#116177,#116178,#116179,#116180,
#116181,#116182,#116183,#116184,#116185,#116186,#116187,#116188,#116189,
#116190,#116191,#116192,#116193,#116194,#116195,#116196,#116197,#116198,
#116199,#116200,#116201,#116202,#116203,#116204,#116205,#116206,#116207,
#116208,#116209,#116210,#116211,#116212,#116213,#116214,#116215,#116216,
#116217,#116218,#116219,#116220,#116221,#116222,#116223,#116224,#116225,
#116226,#116227,#116228,#116229,#116230,#116231,#116232,#116233,#116234,
#116235,#116236,#116237,#116238,#116239,#116240,#116241,#116242,#116243,
#116244,#116245,#116246),.UNSPECIFIED.,.F.,.F.,(4,3,3,3,3,3,3,3,3,3,3,3,
3,3,3,3,3,3,3,3,3,3,3,3,3,3,3,3,3,3,3,3,3,3,3,3,3,3,3,3,3,3,3,3,3,3,3,3,
3,3,4),(0.,0.0624999999998672,0.121231102053757,0.124999999999734,0.163221688707204,
0.187499999999604,0.218749999999539,0.234374999999508,0.242187499999495,
0.248046874999491,0.249999999999491,0.304896852417071,0.312499999999486,
0.332752736514499,0.343749999999486,0.359374999999489,0.36718749999949,
0.371093749999491,0.373046874999494,0.374999999999496,0.416499783200529,
0.437499999999609,0.468749999999662,0.484374999999692,0.492187499999707,
0.496093749999711,0.498046874999714,0.499999999999717,0.505620558654761,
0.542490554879664,0.562499999999747,0.593749999999762,0.609374999999769,
0.617187499999773,0.624061796612807,0.624999999999776,0.652866429296472,
0.66750585984053,0.687499999999818,0.716981488664328,0.718749999999839,
0.734374999999854,0.742187499999857,0.746093749999853,0.748046874999851,
0.74999999999985,0.806521545396385,0.848556247067743,0.914625004658987,
0.983976194844835,1.),.UNSPECIFIED.);
#29557=B_SPLINE_CURVE_WITH_KNOTS('',3,(#116248,#116249,#116250,#116251,
#116252,#116253,#116254,#116255,#116256,#116257,#116258,#116259,#116260,
#116261,#116262,#116263,#116264,#116265,#116266,#116267,#116268,#116269,
#116270,#116271,#116272),.UNSPECIFIED.,.F.,.F.,(4,3,3,3,3,3,3,3,4),(0.,
0.125,0.25,0.375,0.5,0.625,0.75,0.875,1.),.UNSPECIFIED.);
#29558=B_SPLINE_CURVE_WITH_KNOTS('',3,(#116274,#116275,#116276,#116277,
#116278,#116279,#116280,#116281,#116282,#116283,#116284,#116285,#116286,
#116287,#116288,#116289,#116290,#116291,#116292,#116293,#116294,#116295,
#116296,#116297,#116298,#116299,#116300,#116301,#116302,#116303,#116304,
#116305,#116306,#116307,#116308,#116309,#116310,#116311,#116312,#116313,
#116314,#116315,#116316,#116317,#116318,#116319,#116320,#116321,#116322,
#116323,#116324,#116325,#116326,#116327,#116328,#116329,#116330,#116331,
#116332,#116333,#116334,#116335,#116336,#116337,#116338,#116339,#116340,
#116341,#116342,#116343,#116344,#116345,#116346,#116347,#116348,#116349,
#116350,#116351,#116352,#116353,#116354,#116355,#116356,#116357,#116358,
#116359,#116360,#116361,#116362,#116363,#116364,#116365,#116366,#116367,
#116368,#116369,#116370,#116371,#116372,#116373,#116374,#116375,#116376,
#116377,#116378,#116379,#116380,#116381,#116382,#116383,#116384,#116385,
#116386,#116387,#116388,#116389,#116390,#116391,#116392,#116393,#116394,
#116395,#116396,#116397,#116398,#116399,#116400,#116401,#116402,#116403,
#116404,#116405,#116406,#116407,#116408,#116409,#116410,#116411,#116412,
#116413,#116414,#116415,#116416,#116417,#116418,#116419,#116420,#116421,
#116422,#116423,#116424,#116425,#116426,#116427,#116428,#116429,#116430,
#116431,#116432,#116433,#116434,#116435,#116436,#116437,#116438,#116439,
#116440,#116441,#116442,#116443,#116444,#116445,#116446,#116447,#116448,
#116449,#116450,#116451,#116452,#116453,#116454,#116455,#116456,#116457,
#116458,#116459,#116460,#116461,#116462,#116463,#116464,#116465,#116466,
#116467,#116468,#116469,#116470,#116471,#116472,#116473,#116474,#116475,
#116476,#116477,#116478,#116479,#116480,#116481,#116482,#116483,#116484,
#116485,#116486,#116487,#116488,#116489,#116490,#116491,#116492,#116493,
#116494,#116495,#116496,#116497,#116498,#116499,#116500,#116501,#116502,
#116503,#116504,#116505,#116506,#116507,#116508,#116509,#116510,#116511,
#116512,#116513,#116514,#116515,#116516,#116517,#116518,#116519,#116520,
#116521,#116522,#116523,#116524,#116525,#116526,#116527,#116528,#116529,
#116530,#116531,#116532,#116533,#116534,#116535,#116536,#116537,#116538,
#116539,#116540,#116541,#116542,#116543,#116544,#116545,#116546,#116547,
#116548,#116549,#116550,#116551,#116552,#116553,#116554,#116555,#116556),
 .UNSPECIFIED.,.F.,.F.,(4,3,3,3,3,3,3,3,3,3,3,3,3,3,3,3,3,3,3,3,3,3,3,3,
3,3,3,3,3,3,3,3,3,3,3,3,3,3,3,3,3,3,3,3,3,3,3,3,3,3,3,3,3,3,3,3,3,3,3,3,
3,3,3,3,3,3,3,3,3,3,3,3,3,3,3,3,3,3,3,3,3,3,3,3,3,3,3,3,3,3,3,3,3,3,4),
(0.,0.0218553192416152,0.0239909676408461,0.047404899596648,0.0576150789306258,
0.0817019507604128,0.0923175822312087,0.11725378633643,0.125000000000385,
0.12782188704429,0.153315965606252,0.163932697097646,0.187500000000578,
0.200455026760637,0.218750000000674,0.234375000000722,0.236703243244336,
0.242187500000746,0.246093750000759,0.248046875000764,0.249750884846123,
0.25000000000077,0.266748876337169,0.274607654122715,0.281250000000843,
0.296875000000879,0.304687500000897,0.307933981749264,0.308593750000907,
0.310546875000913,0.311523437500915,0.312500000000917,0.342097572559386,
0.34375000000095,0.359375000000966,0.367558307807294,0.375000000000983,
0.377517642532591,0.403712695856758,0.413666303605555,0.437500000001046,
0.448741255419369,0.468750000001077,0.483155469156573,0.484375000001092,
0.492187500001098,0.496093750001103,0.498046875001104,0.499818401517535,
0.500000000001105,0.520741585243092,0.542287513872453,0.557662955585771,
0.562500000001145,0.581759226316266,0.591897962726741,0.593750000001166,
0.609375000001177,0.617187500001182,0.621093750001185,0.623046875001185,
0.623651136778459,0.624023437501185,0.625000000001186,0.637497695748092,
0.648624211071175,0.661971401128478,0.675806858384994,0.678364062535773,
0.687500000001248,0.702496729367031,0.717149250528625,0.718750000001278,
0.734375000001294,0.742187500001303,0.746093750001308,0.74804687500131,
0.74902343750131,0.749511718751307,0.750000000001304,0.764878648076392,
0.791680428121145,0.802651410975554,0.829731221647044,0.840058129334189,
0.867079580400336,0.875000000000652,0.876521389536748,0.902828525497309,
0.911862695096826,0.937111114145424,0.945833175269185,0.970733896748208,
0.978118639161034,1.),.UNSPECIFIED.);
#29559=B_SPLINE_CURVE_WITH_KNOTS('',3,(#116558,#116559,#116560,#116561,
#116562,#116563,#116564,#116565,#116566,#116567,#116568,#116569,#116570,
#116571,#116572,#116573,#116574,#116575,#116576,#116577,#116578,#116579,
#116580,#116581,#116582),.UNSPECIFIED.,.F.,.F.,(4,3,3,3,3,3,3,3,4),(0.,
0.125,0.25,0.375,0.5,0.625,0.75,0.875,0.999999873942638),.UNSPECIFIED.);
#29560=B_SPLINE_CURVE_WITH_KNOTS('',3,(#116583,#116584,#116585,#116586,
#116587,#116588,#116589,#116590,#116591,#116592,#116593,#116594,#116595,
#116596,#116597,#116598,#116599,#116600,#116601,#116602,#116603,#116604,
#116605,#116606,#116607,#116608,#116609,#116610,#116611,#116612,#116613,
#116614,#116615,#116616,#116617,#116618,#116619,#116620,#116621,#116622,
#116623,#116624,#116625,#116626,#116627,#116628,#116629,#116630,#116631,
#116632,#116633,#116634,#116635,#116636,#116637),.UNSPECIFIED.,.F.,.F.,
(4,2,2,1,1,1,1,2,2,2,2,1,2,2,2,2,1,1,1,2,2,2,1,1,1,1,2,2,2,1,1,1,2,2,4),
(0.,0.124999999999915,0.187499999999874,0.218749999999858,0.23437499999985,
0.242187499999846,0.24609374999984,0.248046874999841,0.249999999999842,
0.312499999999878,0.343749999999894,0.359374999999902,0.367187499999908,
0.374999999999913,0.437499999999939,0.468749999999949,0.484374999999953,
0.492187499999951,0.49609374999995,0.498046874999954,0.499999999999959,
0.562500000000051,0.593750000000098,0.609375000000121,0.617187500000129,
0.621093750000132,0.623046875000133,0.625000000000134,0.687500000000118,
0.718750000000112,0.73437500000011,0.742187500000109,0.746093750000106,
0.750000000000103,1.),.UNSPECIFIED.);
#29561=B_SPLINE_CURVE_WITH_KNOTS('',3,(#116641,#116642,#116643,#116644,
#116645,#116646,#116647,#116648,#116649,#116650,#116651,#116652,#116653,
#116654,#116655,#116656,#116657,#116658,#116659,#116660,#116661,#116662,
#116663,#116664,#116665,#116666,#116667,#116668),.UNSPECIFIED.,.F.,.F.,
(4,2,2,1,2,2,2,2,2,2,2,1,2,2,4),(0.,0.125000000000002,0.187500000000005,
0.218750000000006,0.234375000000007,0.250000000000008,0.375000000000012,
0.437500000000012,0.500000000000012,0.625000000000009,0.687500000000007,
0.718750000000006,0.734375000000006,0.750000000000007,1.),.UNSPECIFIED.);
#29562=B_SPLINE_CURVE_WITH_KNOTS('',3,(#116670,#116671,#116672,#116673,
#116674,#116675,#116676,#116677,#116678,#116679,#116680,#116681,#116682,
#116683,#116684,#116685,#116686,#116687,#116688,#116689,#116690,#116691,
#116692,#116693,#116694,#116695,#116696,#116697,#116698,#116699,#116700,
#116701,#116702,#116703,#116704,#116705),.UNSPECIFIED.,.F.,.F.,(4,2,1,1,
1,1,2,2,2,2,1,2,2,2,1,2,2,2,2,2,4),(0.,0.124999999999964,0.187499999999947,
0.218749999999938,0.234374999999932,0.242187499999929,0.246093749999927,
0.249999999999926,0.37499999999994,0.437499999999946,0.46874999999995,0.484374999999953,
0.499999999999956,0.562499999999969,0.593749999999976,0.609374999999978,
0.624999999999981,0.687499999999985,0.718749999999986,0.749999999999987,
1.),.UNSPECIFIED.);
#29563=B_SPLINE_CURVE_WITH_KNOTS('',3,(#116728,#116729,#116730,#116731,
#116732,#116733,#116734,#116735,#116736,#116737,#116738,#116739,#116740,
#116741,#116742,#116743,#116744,#116745,#116746),.UNSPECIFIED.,.F.,.F.,
(4,3,3,3,3,3,4),(0.,0.0815195060317968,0.185640530775494,0.274473694370806,
0.363855401859883,0.461632447753659,0.498245638802628),.UNSPECIFIED.);
#29564=B_SPLINE_CURVE_WITH_KNOTS('',3,(#116884,#116885,#116886,#116887,
#116888,#116889,#116890,#116891,#116892,#116893,#116894,#116895,#116896,
#116897,#116898,#116899,#116900,#116901,#116902,#116903,#116904,#116905,
#116906,#116907,#116908,#116909,#116910,#116911,#116912,#116913,#116914,
#116915,#116916,#116917,#116918,#116919,#116920,#116921,#116922,#116923,
#116924,#116925,#116926,#116927,#116928,#116929,#116930,#116931,#116932,
#116933,#116934,#116935,#116936,#116937,#116938,#116939,#116940,#116941,
#116942,#116943,#116944),.UNSPECIFIED.,.F.,.F.,(4,3,3,3,3,3,3,3,3,3,3,3,
3,3,3,3,3,3,3,3,4),(0.,0.0927792530957532,0.181143034095441,0.250000000000402,
0.302029203004749,0.375000000000606,0.437500000000711,0.468750000000757,
0.484375000000779,0.492187500000791,0.496093750000796,0.500000000000801,
0.569042640114168,0.636907417646122,0.691184957664156,0.750000000000401,
0.8125000000003,0.870058800372124,0.925905746294812,0.980241350328491,1.),
 .UNSPECIFIED.);
#29565=B_SPLINE_CURVE_WITH_KNOTS('',3,(#116946,#116947,#116948,#116949,
#116950,#116951,#116952,#116953,#116954,#116955,#116956,#116957,#116958,
#116959,#116960,#116961,#116962,#116963,#116964,#116965,#116966,#116967,
#116968,#116969,#116970,#116971,#116972,#116973,#116974,#116975,#116976),
 .UNSPECIFIED.,.F.,.F.,(4,3,3,3,3,3,3,3,3,3,4),(2.46560854681056E-10,0.113253207042464,
0.225068571246234,0.336211172061686,0.446873791004117,0.5,0.610600731635704,
0.721861535753223,0.833640664344923,0.946719460130871,0.99999999991526),
 .UNSPECIFIED.);
#29566=B_SPLINE_CURVE_WITH_KNOTS('',3,(#116977,#116978,#116979,#116980,
#116981,#116982,#116983,#116984,#116985,#116986,#116987,#116988,#116989,
#116990,#116991,#116992),.UNSPECIFIED.,.F.,.F.,(4,2,2,1,1,2,2,2,4),(0.,
0.249999999999911,0.374999999999873,0.437499999999854,0.468749999999844,
0.484374999999845,0.499999999999846,0.749999999999923,1.),.UNSPECIFIED.);
#29567=B_SPLINE_CURVE_WITH_KNOTS('',3,(#117052,#117053,#117054,#117055,
#117056,#117057),.UNSPECIFIED.,.F.,.F.,(4,2,4),(-0.918590950811215,-0.473516281042627,
-9.99999057782475E-7),.UNSPECIFIED.);
#29568=B_SPLINE_CURVE_WITH_KNOTS('',3,(#117063,#117064,#117065,#117066,
#117067,#117068,#117069,#117070,#117071,#117072,#117073,#117074,#117075,
#117076,#117077,#117078,#117079,#117080,#117081,#117082,#117083,#117084,
#117085,#117086,#117087),.UNSPECIFIED.,.F.,.F.,(4,3,3,3,3,3,3,3,4),(0.,
0.131958835404557,0.26974144616476,0.407524056924964,0.545524898370289,
0.683735650569008,0.821345328537211,0.953680929508149,1.),.UNSPECIFIED.);
#29569=B_SPLINE_CURVE_WITH_KNOTS('',3,(#117088,#117089,#117090,#117091,
#117092,#117093,#117094,#117095,#117096,#117097,#117098,#117099,#117100,
#117101,#117102,#117103,#117104,#117105,#117106),.UNSPECIFIED.,.F.,.F.,
(4,3,3,3,3,3,4),(4.45019463169606E-7,0.162711821023231,0.327779237456247,
0.496643240664868,0.667586333454032,0.841952576666844,1.),.UNSPECIFIED.);
#29570=B_SPLINE_CURVE_WITH_KNOTS('',3,(#117172,#117173,#117174,#117175,
#117176,#117177,#117178,#117179,#117180,#117181,#117182,#117183,#117184,
#117185,#117186,#117187,#117188,#117189,#117190,#117191,#117192,#117193,
#117194,#117195,#117196,#117197,#117198,#117199,#117200,#117201,#117202,
#117203,#117204,#117205,#117206,#117207,#117208,#117209,#117210,#117211,
#117212,#117213,#117214,#117215,#117216,#117217,#117218,#117219,#117220,
#117221,#117222,#117223,#117224,#117225,#117226,#117227,#117228,#117229),
 .UNSPECIFIED.,.F.,.F.,(4,3,3,3,3,3,3,3,3,3,3,3,3,3,3,3,3,3,3,4),(0.,0.0619432161112905,
0.124508308999197,0.142068526750139,0.205837696787764,0.249999999999997,
0.279531917274151,0.346849139134802,0.413029519231283,0.483936394515832,
0.499999999999994,0.543184869644407,0.614814399058056,0.671122191652417,
0.743062292031408,0.79701922190678,0.867896471689319,0.922141629836563,
0.991397233405132,0.999997239496597),.UNSPECIFIED.);
#29571=B_SPLINE_CURVE_WITH_KNOTS('',3,(#117231,#117232,#117233,#117234,
#117235,#117236,#117237,#117238,#117239,#117240,#117241,#117242,#117243,
#117244,#117245,#117246,#117247,#117248,#117249,#117250,#117251,#117252,
#117253,#117254,#117255,#117256,#117257,#117258,#117259,#117260,#117261,
#117262,#117263,#117264,#117265,#117266,#117267,#117268,#117269,#117270,
#117271,#117272,#117273),.UNSPECIFIED.,.F.,.F.,(4,3,3,3,3,3,3,3,3,3,3,3,
3,3,4),(0.,0.0937334144157132,0.185189062989018,0.273500600704511,0.360125764759083,
0.444327725505443,0.5,0.581147963193658,0.66094496171836,0.738987112431448,
0.75,0.825900760301095,0.900636141668165,0.973772467019908,1.),
 .UNSPECIFIED.);
#29572=B_SPLINE_CURVE_WITH_KNOTS('',3,(#117300,#117301,#117302,#117303,
#117304,#117305),.UNSPECIFIED.,.F.,.F.,(4,2,4),(0.,0.5,1.),
 .UNSPECIFIED.);
#29573=B_SPLINE_CURVE_WITH_KNOTS('',3,(#117306,#117307,#117308,#117309,
#117310,#117311,#117312,#117313,#117314,#117315,#117316,#117317,#117318,
#117319,#117320,#117321,#117322,#117323,#117324,#117325,#117326,#117327,
#117328,#117329,#117330,#117331,#117332,#117333,#117334,#117335,#117336,
#117337,#117338,#117339,#117340,#117341,#117342,#117343,#117344,#117345,
#117346,#117347,#117348,#117349,#117350,#117351,#117352,#117353,#117354),
 .UNSPECIFIED.,.F.,.F.,(4,3,3,3,3,3,3,3,3,3,3,3,3,3,3,3,4),(0.,0.0659495801766569,
0.1308373231871,0.19438095135116,0.25,0.3125,0.374042589957,0.435265209100815,
0.496321655486699,0.559741241615024,0.621102771689104,0.685551385844552,
0.75,0.813619167758251,0.87800524330354,0.944005251946419,1.),
 .UNSPECIFIED.);
#29574=B_SPLINE_CURVE_WITH_KNOTS('',3,(#117363,#117364,#117365,#117366,
#117367,#117368),.UNSPECIFIED.,.F.,.F.,(4,2,4),(1.00000000968122E-6,0.267925099545075,
0.535347184622059),.UNSPECIFIED.);
#29575=B_SPLINE_CURVE_WITH_KNOTS('',3,(#117418,#117419,#117420,#117421,
#117422,#117423,#117424,#117425,#117426,#117427,#117428,#117429,#117430,
#117431,#117432,#117433,#117434,#117435,#117436,#117437,#117438,#117439,
#117440,#117441,#117442,#117443,#117444,#117445,#117446,#117447,#117448,
#117449,#117450,#117451,#117452,#117453,#117454,#117455,#117456,#117457,
#117458,#117459,#117460,#117461,#117462,#117463,#117464,#117465,#117466,
#117467,#117468,#117469,#117470,#117471,#117472,#117473,#117474,#117475,
#117476,#117477,#117478,#117479,#117480,#117481,#117482,#117483,#117484,
#117485,#117486,#117487),.UNSPECIFIED.,.F.,.F.,(4,3,3,3,3,3,3,3,3,3,3,3,
3,3,3,3,3,3,3,3,3,3,3,4),(0.,0.11048788577789,0.124999999999995,0.201428248706923,
0.218749999999992,0.235851895407793,0.249999999999992,0.312861916977878,
0.386450511607397,0.437499999999996,0.464170261187618,0.490703896049709,
0.499999999999997,0.514209169182011,0.578362302765488,0.624999999999998,
0.673321561493809,0.714910737311328,0.749999999999999,0.807840811261223,
0.869314910339536,0.914553166950376,0.969583186255868,0.999999999703888),
 .UNSPECIFIED.);
#29576=B_SPLINE_CURVE_WITH_KNOTS('',3,(#117491,#117492,#117493,#117494,
#117495,#117496,#117497,#117498,#117499,#117500,#117501,#117502),
 .UNSPECIFIED.,.F.,.F.,(4,2,2,2,2,4),(-0.486148537655684,-0.486124291092022,
-0.428314815488407,-0.370505339884792,-0.308168734459638,-0.245832129034485),
 .UNSPECIFIED.);
#29577=B_SPLINE_CURVE_WITH_KNOTS('',3,(#117513,#117514,#117515,#117516,
#117517,#117518,#117519,#117520,#117521,#117522),.UNSPECIFIED.,.F.,.F.,
(4,2,2,2,4),(-0.231634949000231,-0.17437767996901,-0.115937607104994,-0.0533819428831184,
-9.99999772544058E-7),.UNSPECIFIED.);
#29578=B_SPLINE_CURVE_WITH_KNOTS('',3,(#117523,#117524,#117525,#117526,
#117527,#117528,#117529,#117530,#117531,#117532),.UNSPECIFIED.,.F.,.F.,
(4,3,3,4),(3.09320682459972E-12,0.485988696847241,0.738935319808724,1.),
 .UNSPECIFIED.);
#29579=B_SPLINE_CURVE_WITH_KNOTS('',3,(#117533,#117534,#117535,#117536,
#117537,#117538,#117539),.UNSPECIFIED.,.F.,.F.,(4,3,4),(0.,0.734307685730172,
1.),.UNSPECIFIED.);
#29580=B_SPLINE_CURVE_WITH_KNOTS('',3,(#117600,#117601,#117602,#117603,
#117604,#117605,#117606),.UNSPECIFIED.,.F.,.F.,(4,3,4),(0.,0.1,0.126954494999424),
 .UNSPECIFIED.);
#29581=B_SPLINE_CURVE_WITH_KNOTS('',3,(#117681,#117682,#117683,#117684,
#117685,#117686,#117687,#117688,#117689,#117690,#117691,#117692,#117693,
#117694,#117695,#117696,#117697,#117698,#117699,#117700,#117701,#117702,
#117703,#117704,#117705,#117706,#117707,#117708,#117709,#117710,#117711,
#117712,#117713,#117714,#117715,#117716,#117717,#117718,#117719,#117720,
#117721,#117722,#117723,#117724,#117725,#117726,#117727,#117728,#117729,
#117730,#117731,#117732,#117733,#117734,#117735,#117736,#117737,#117738,
#117739,#117740,#117741,#117742,#117743,#117744,#117745,#117746,#117747,
#117748,#117749,#117750,#117751,#117752,#117753,#117754,#117755,#117756,
#117757,#117758,#117759,#117760,#117761,#117762,#117763,#117764,#117765,
#117766,#117767,#117768,#117769,#117770,#117771,#117772,#117773,#117774),
 .UNSPECIFIED.,.F.,.F.,(4,3,3,3,3,3,3,3,3,3,3,3,3,3,3,3,3,3,3,3,3,3,3,3,
3,3,3,3,3,3,3,4),(0.,0.0434329855669776,0.08907548745578,0.0992782405803121,
0.1111111111111,0.150652206158072,0.189763811698692,0.216719719165669,0.2222222222222,
0.27777777777775,0.328951791908699,0.3333333333333,0.33411341030855,0.367911781436324,
0.401192650050171,0.43352701848881,0.4444444444444,0.451268763306688,0.494769905150912,
0.536743026897841,0.5555555555556,0.568707898163555,0.617687282415127,0.6666666666667,
0.686226797860462,0.73658037633076,0.7777777777778,0.803542347385094,0.85501524701251,
0.8888888888889,0.920843304974927,0.999999999998517),.UNSPECIFIED.);
#29582=B_SPLINE_CURVE_WITH_KNOTS('',3,(#117777,#117778,#117779,#117780,
#117781,#117782,#117783,#117784,#117785,#117786,#117787,#117788,#117789,
#117790,#117791,#117792,#117793,#117794,#117795,#117796,#117797,#117798,
#117799,#117800,#117801,#117802,#117803,#117804,#117805,#117806,#117807,
#117808,#117809,#117810,#117811,#117812,#117813,#117814,#117815,#117816,
#117817,#117818,#117819,#117820,#117821,#117822,#117823,#117824,#117825,
#117826,#117827,#117828,#117829,#117830,#117831,#117832,#117833,#117834,
#117835,#117836,#117837,#117838,#117839,#117840,#117841,#117842,#117843,
#117844,#117845,#117846,#117847,#117848,#117849,#117850,#117851,#117852,
#117853,#117854,#117855,#117856,#117857,#117858,#117859,#117860,#117861,
#117862,#117863,#117864,#117865,#117866,#117867,#117868,#117869,#117870,
#117871,#117872,#117873,#117874,#117875,#117876),.UNSPECIFIED.,.F.,.F.,
(4,3,3,3,3,3,3,3,3,3,3,3,3,3,3,3,3,3,3,3,3,3,3,3,3,3,3,3,3,3,3,3,3,4),(0.,
0.0482896592338093,0.102692540909445,0.136650408423194,0.190645379027607,
0.225179914594825,0.25000000000002,0.304085285007251,0.313864436259833,
0.365917320127364,0.375000000000032,0.402681143263378,0.437500000000037,
0.468750000000041,0.484375000000044,0.492187500000046,0.492692625002022,
0.496093750000046,0.498046875000046,0.500000000000047,0.536325374785433,
0.569651731954972,0.606130649818242,0.644147897050678,0.647285809980453,
0.686930286977043,0.724488661589305,0.750000000000023,0.802797594861853,
0.809964462253265,0.867077701254393,0.908266360714621,0.975423950021811,
0.99999999995535),.UNSPECIFIED.);
#29583=B_SPLINE_CURVE_WITH_KNOTS('',3,(#117914,#117915,#117916,#117917,
#117918,#117919,#117920,#117921),.UNSPECIFIED.,.F.,.F.,(4,1,1,1,1,4),(2.28402671907889E-6,
0.2,0.4,0.6,0.8,1.),.UNSPECIFIED.);
#29584=B_SPLINE_CURVE_WITH_KNOTS('',3,(#117924,#117925,#117926,#117927,
#117928,#117929,#117930,#117931,#117932,#117933,#117934,#117935,#117936,
#117937,#117938,#117939,#117940,#117941,#117942,#117943,#117944,#117945,
#117946,#117947,#117948),.UNSPECIFIED.,.F.,.F.,(4,3,3,3,3,3,3,3,4),(2.23348816774046E-5,
0.0628477441748189,0.220194717015139,0.373526365176584,0.524161382659806,
0.670551898649584,0.744053228789804,0.90146949799915,1.),.UNSPECIFIED.);
#29585=B_SPLINE_CURVE_WITH_KNOTS('',3,(#118019,#118020,#118021,#118022,
#118023,#118024,#118025,#118026,#118027,#118028,#118029,#118030,#118031,
#118032,#118033,#118034,#118035,#118036,#118037,#118038,#118039,#118040,
#118041,#118042,#118043,#118044,#118045,#118046,#118047,#118048,#118049,
#118050,#118051,#118052,#118053,#118054,#118055,#118056,#118057,#118058,
#118059,#118060,#118061,#118062,#118063,#118064,#118065,#118066,#118067,
#118068,#118069,#118070,#118071,#118072,#118073,#118074,#118075,#118076,
#118077,#118078,#118079,#118080,#118081,#118082,#118083,#118084,#118085,
#118086,#118087,#118088,#118089,#118090,#118091,#118092,#118093,#118094,
#118095,#118096,#118097,#118098,#118099,#118100,#118101,#118102,#118103,
#118104,#118105,#118106,#118107,#118108,#118109,#118110,#118111,#118112,
#118113,#118114,#118115,#118116,#118117,#118118,#118119,#118120,#118121,
#118122,#118123,#118124,#118125,#118126,#118127,#118128,#118129,#118130,
#118131,#118132,#118133,#118134,#118135,#118136,#118137,#118138,#118139,
#118140,#118141,#118142,#118143,#118144,#118145,#118146,#118147,#118148,
#118149,#118150,#118151,#118152,#118153,#118154,#118155,#118156,#118157,
#118158,#118159,#118160,#118161,#118162,#118163,#118164,#118165,#118166,
#118167,#118168,#118169,#118170,#118171,#118172,#118173,#118174,#118175,
#118176,#118177,#118178,#118179,#118180,#118181,#118182,#118183,#118184,
#118185,#118186,#118187,#118188,#118189,#118190,#118191,#118192,#118193,
#118194,#118195,#118196),.UNSPECIFIED.,.F.,.F.,(4,3,3,3,3,3,3,3,3,3,3,3,
3,3,3,3,3,3,3,3,3,3,3,3,3,3,3,3,3,3,3,3,3,3,3,3,3,3,3,3,3,3,3,3,3,3,3,3,
3,3,3,3,3,3,3,3,3,3,3,4),(0.,0.0488641282796294,0.104159161587302,0.123022321598326,
0.124999999999995,0.179678682731705,0.187499999999992,0.197853928883569,
0.21874999999999,0.234374999999989,0.242187499999989,0.248089771096223,
0.249999999999988,0.274414806619095,0.332705726838955,0.351483832875215,
0.410368538967155,0.425145513293437,0.437499999999992,0.468749999999993,
0.484374999999992,0.492187499999991,0.496093749999991,0.496290295252264,
0.499999999999991,0.543327592310242,0.570763138693585,0.613636521352308,
0.644189079608782,0.685332797437125,0.68749999999999,0.718749999999989,
0.718953363471053,0.73437499999999,0.742187499999989,0.746093749999989,
0.748046874999988,0.749023437499988,0.749999999999988,0.769489339732673,
0.789169556834021,0.801427018275548,0.821475974402478,0.841466221066801,
0.859375000000003,0.867187500000004,0.869582291779894,0.871093750000004,
0.873046875000005,0.874023437500005,0.875000000000005,0.890106498209821,
0.905512726506942,0.921370222932082,0.930397372833373,0.937500000000002,
0.954034229226621,0.970837951409062,0.988025978151,1.),.UNSPECIFIED.);
#29586=B_SPLINE_CURVE_WITH_KNOTS('',3,(#118240,#118241,#118242,#118243,
#118244,#118245,#118246,#118247,#118248,#118249,#118250,#118251,#118252,
#118253,#118254,#118255,#118256,#118257,#118258,#118259,#118260,#118261,
#118262,#118263,#118264,#118265,#118266,#118267,#118268,#118269,#118270,
#118271,#118272,#118273,#118274,#118275,#118276,#118277,#118278,#118279,
#118280,#118281,#118282,#118283,#118284,#118285,#118286,#118287,#118288,
#118289,#118290,#118291,#118292,#118293,#118294,#118295,#118296,#118297,
#118298,#118299,#118300,#118301,#118302,#118303,#118304,#118305,#118306,
#118307,#118308,#118309),.UNSPECIFIED.,.F.,.F.,(4,3,3,3,3,3,3,3,3,3,3,3,
3,3,3,3,3,3,3,3,3,3,3,4),(2.33665370772347E-6,0.0496371691506646,0.0994512751400878,
0.12500000000005,0.17474957176903,0.187500000000073,0.218750000000083,0.234375000000087,
0.24218750000009,0.249493988611268,0.250000000000093,0.304451733242835,
0.359731547709945,0.416068672295921,0.43224145509044,0.437500000000231,
0.468750000000251,0.484375000000263,0.492187500000273,0.496093750000274,
0.498046875000272,0.50000000000027,0.956286239664588,0.999999847835327),
 .UNSPECIFIED.);
#29587=B_SPLINE_CURVE_WITH_KNOTS('',3,(#118364,#118365,#118366,#118367,
#118368,#118369,#118370,#118371,#118372,#118373,#118374,#118375,#118376,
#118377,#118378,#118379,#118380,#118381,#118382,#118383,#118384,#118385,
#118386,#118387,#118388,#118389,#118390,#118391,#118392,#118393,#118394,
#118395,#118396,#118397,#118398,#118399,#118400,#118401,#118402,#118403,
#118404,#118405,#118406,#118407,#118408,#118409,#118410,#118411,#118412,
#118413,#118414,#118415,#118416,#118417,#118418,#118419,#118420,#118421,
#118422,#118423,#118424,#118425,#118426,#118427,#118428,#118429,#118430,
#118431,#118432,#118433,#118434,#118435,#118436,#118437,#118438,#118439,
#118440,#118441,#118442,#118443,#118444,#118445,#118446,#118447,#118448,
#118449,#118450,#118451,#118452,#118453,#118454,#118455,#118456,#118457,
#118458,#118459,#118460,#118461,#118462,#118463,#118464,#118465,#118466,
#118467,#118468,#118469,#118470,#118471,#118472,#118473,#118474,#118475,
#118476,#118477,#118478,#118479,#118480,#118481,#118482,#118483,#118484,
#118485,#118486,#118487,#118488,#118489,#118490,#118491,#118492,#118493,
#118494,#118495,#118496,#118497,#118498,#118499,#118500,#118501,#118502,
#118503,#118504,#118505,#118506,#118507,#118508,#118509,#118510,#118511,
#118512,#118513,#118514,#118515,#118516,#118517,#118518,#118519,#118520,
#118521,#118522,#118523,#118524,#118525,#118526,#118527,#118528,#118529,
#118530,#118531,#118532,#118533,#118534,#118535,#118536,#118537,#118538),
 .UNSPECIFIED.,.F.,.F.,(4,3,3,3,3,3,3,3,3,3,3,3,3,3,3,3,3,3,3,3,3,3,3,3,
3,3,3,3,3,3,3,3,3,3,3,3,3,3,3,3,3,3,3,3,3,3,3,3,3,3,3,3,3,3,3,3,3,3,4),
(0.,0.0555382977619952,0.0624999999999407,0.0692575826362369,0.0937499999999123,
0.109374999999899,0.117187499999892,0.121093749999889,0.124023437499886,
0.124999999999885,0.144081499360291,0.163253233995527,0.171874999999873,
0.179028327204326,0.179687499999871,0.185657163721033,0.187499999999869,
0.211416108967977,0.218749999999859,0.234374999999853,0.24218749999985,
0.246093749999849,0.248046874999848,0.249999999999847,0.283186761764929,
0.322905151422521,0.343749999999848,0.359374999999848,0.367187499999848,
0.373100637420652,0.374999999999848,0.394064544065694,0.437499999999848,
0.468749999999848,0.484374999999849,0.492187499999849,0.49609374999985,
0.499384498321497,0.49999999999985,0.501066362102164,0.554831394622692,
0.608443932593253,0.659742424080655,0.709573207920356,0.716593188313347,
0.718749999999909,0.734374999999914,0.742187499999916,0.746093749999917,
0.748046874999918,0.749999999999918,0.793255601342627,0.81956640435806,
0.858098769840019,0.897160626316328,0.929164183156927,0.961210686803325,
0.993512835337006,1.),.UNSPECIFIED.);
#29588=B_SPLINE_CURVE_WITH_KNOTS('',3,(#118544,#118545,#118546,#118547,
#118548,#118549,#118550,#118551,#118552,#118553,#118554,#118555,#118556,
#118557,#118558,#118559,#118560,#118561,#118562,#118563,#118564,#118565,
#118566,#118567,#118568,#118569,#118570,#118571,#118572,#118573,#118574,
#118575,#118576,#118577,#118578,#118579,#118580,#118581,#118582,#118583,
#118584,#118585,#118586,#118587,#118588,#118589,#118590,#118591,#118592,
#118593,#118594,#118595,#118596,#118597,#118598,#118599,#118600,#118601,
#118602,#118603,#118604,#118605,#118606,#118607,#118608,#118609,#118610,
#118611,#118612,#118613,#118614,#118615,#118616,#118617,#118618,#118619,
#118620,#118621,#118622,#118623,#118624,#118625,#118626,#118627,#118628,
#118629,#118630,#118631),.UNSPECIFIED.,.F.,.F.,(4,3,3,3,3,3,3,3,3,3,3,3,
3,3,3,3,3,3,3,3,3,3,3,3,3,3,3,3,3,4),(3.36783202418071E-7,0.0704310134426517,
0.154324908618331,0.178703893197204,0.250000000000081,0.291512562001931,
0.375000000000122,0.399673169085418,0.437500000000142,0.468750000000152,
0.484375000000157,0.492187500000159,0.499023437500161,0.500000000000161,
0.501549258011091,0.5461457214218,0.59050184840333,0.63104355844614,0.67441742482806,
0.717108969540505,0.739637705241223,0.75000000000008,0.791454313031361,
0.832044716531103,0.843349397267229,0.87500000000004,0.916301019532102,
0.942758457577564,0.976122915483621,1.),.UNSPECIFIED.);
#29589=B_SPLINE_CURVE_WITH_KNOTS('',3,(#118721,#118722,#118723,#118724,
#118725,#118726,#118727,#118728,#118729,#118730,#118731,#118732,#118733,
#118734,#118735,#118736,#118737,#118738,#118739,#118740,#118741,#118742,
#118743,#118744,#118745,#118746,#118747,#118748,#118749,#118750,#118751,
#118752,#118753,#118754,#118755,#118756,#118757,#118758,#118759,#118760,
#118761,#118762,#118763,#118764,#118765,#118766,#118767,#118768,#118769,
#118770,#118771,#118772,#118773,#118774,#118775),.UNSPECIFIED.,.F.,.F.,
(4,3,3,3,3,3,3,3,3,3,3,3,3,3,3,3,3,3,4),(0.,0.0682759325374089,0.154250463005588,
0.238795938723332,0.250000000000005,0.332839120626675,0.346908656220202,
0.430143950681296,0.437500000000009,0.46875000000001,0.48437500000001,0.49218750000001,
0.498046875000011,0.500000000000011,0.634899028144559,0.670690163863966,
0.802255340146405,0.929676150621539,1.),.UNSPECIFIED.);
#29590=B_SPLINE_CURVE_WITH_KNOTS('',3,(#118776,#118777,#118778,#118779,
#118780,#118781,#118782,#118783,#118784,#118785,#118786,#118787,#118788,
#118789,#118790,#118791,#118792,#118793,#118794,#118795,#118796,#118797,
#118798,#118799,#118800,#118801,#118802,#118803,#118804,#118805,#118806,
#118807,#118808,#118809,#118810,#118811,#118812,#118813,#118814,#118815,
#118816,#118817,#118818,#118819,#118820,#118821,#118822,#118823,#118824,
#118825,#118826,#118827,#118828,#118829,#118830,#118831,#118832,#118833,
#118834,#118835,#118836,#118837,#118838,#118839,#118840,#118841,#118842,
#118843,#118844,#118845,#118846,#118847,#118848,#118849,#118850,#118851,
#118852,#118853,#118854,#118855,#118856,#118857,#118858,#118859,#118860,
#118861,#118862,#118863,#118864,#118865,#118866,#118867,#118868,#118869,
#118870,#118871,#118872,#118873,#118874,#118875,#118876,#118877,#118878,
#118879,#118880,#118881,#118882,#118883,#118884,#118885,#118886,#118887,
#118888,#118889,#118890,#118891,#118892,#118893,#118894,#118895,#118896,
#118897,#118898,#118899,#118900,#118901,#118902,#118903,#118904,#118905,
#118906,#118907,#118908,#118909,#118910,#118911,#118912,#118913,#118914,
#118915,#118916,#118917,#118918,#118919,#118920,#118921,#118922,#118923,
#118924,#118925,#118926,#118927,#118928,#118929,#118930,#118931,#118932,
#118933,#118934,#118935,#118936,#118937,#118938,#118939,#118940,#118941,
#118942,#118943,#118944,#118945,#118946,#118947,#118948,#118949,#118950,
#118951,#118952,#118953),.UNSPECIFIED.,.F.,.F.,(4,3,3,3,3,3,3,3,3,3,3,3,
3,3,3,3,3,3,3,3,3,3,3,3,3,3,3,3,3,3,3,3,3,3,3,3,3,3,3,3,3,3,3,3,3,3,3,3,
3,3,3,3,3,3,3,3,3,3,3,4),(0.,0.0457546736928399,0.0595877683597098,0.0625000000000001,
0.0937500000000003,0.109375,0.1171875,0.123526663010336,0.125,0.154802074788136,
0.192739789732303,0.230157223808861,0.249999999999998,0.251214518677982,
0.294717106205779,0.33793097163504,0.347765493387925,0.374999999999996,
0.390624999999996,0.398926310167048,0.406249999999995,0.437499999999994,
0.443749474057719,0.468749999999993,0.484374999999993,0.492187499999993,
0.497995340860155,0.499999999999993,0.535787989099162,0.56249999999999,
0.593749999999989,0.609374999999989,0.617187499999989,0.624023437499989,
0.624999999999989,0.632640348092497,0.667465916356947,0.687499999999993,
0.718749999999994,0.727500196920872,0.734374999999995,0.742187499999996,
0.749023437499996,0.749999999999996,0.779007516334961,0.808104573985199,
0.812499999999994,0.822012805932175,0.843749999999993,0.859374999999993,
0.867187499999992,0.871093749999992,0.874023437499992,0.874999999999992,
0.899004394474957,0.917844380165313,0.941858795920938,0.965884596741871,
0.989772975332555,1.),.UNSPECIFIED.);
#29591=B_SPLINE_CURVE_WITH_KNOTS('',3,(#118972,#118973,#118974,#118975),
 .UNSPECIFIED.,.F.,.F.,(4,4),(0.,1.),.UNSPECIFIED.);
#29592=B_SPLINE_CURVE_WITH_KNOTS('',3,(#119063,#119064,#119065,#119066,
#119067,#119068,#119069,#119070,#119071,#119072,#119073,#119074,#119075,
#119076,#119077,#119078,#119079,#119080,#119081,#119082,#119083,#119084,
#119085,#119086,#119087,#119088,#119089,#119090,#119091,#119092,#119093,
#119094,#119095,#119096,#119097,#119098,#119099,#119100,#119101,#119102,
#119103,#119104,#119105,#119106,#119107,#119108,#119109,#119110,#119111,
#119112,#119113,#119114,#119115,#119116,#119117,#119118,#119119,#119120,
#119121,#119122,#119123,#119124,#119125,#119126,#119127,#119128,#119129,
#119130,#119131,#119132,#119133,#119134,#119135,#119136,#119137,#119138,
#119139,#119140,#119141,#119142,#119143,#119144,#119145,#119146,#119147,
#119148,#119149,#119150,#119151,#119152,#119153,#119154,#119155,#119156,
#119157,#119158,#119159,#119160,#119161,#119162,#119163,#119164,#119165),
 .UNSPECIFIED.,.F.,.F.,(4,3,3,3,3,3,3,3,3,3,3,3,3,3,3,3,3,3,3,3,3,3,3,3,
3,3,3,3,3,3,3,3,3,3,4),(0.,0.067563816995275,0.130591467722512,0.181054213924464,
0.236634402691202,0.288380007132738,0.306370007127845,0.354266716525829,
0.399092160822195,0.402163425923814,0.44373159496594,0.468750000000269,
0.478404816342543,0.484375000000277,0.492187500000285,0.496093750000291,
0.498046875000291,0.500000000000291,0.544044020950823,0.564564733044594,
0.605001389397497,0.642763780545731,0.680551013373682,0.687500000000175,
0.706851062819798,0.71038379496846,0.730191897484299,0.750000000000139,
0.783679309806148,0.837365834608666,0.863499857353213,0.912275470648177,
0.95177477806762,0.995440622620178,1.),.UNSPECIFIED.);
#29593=B_SPLINE_CURVE_WITH_KNOTS('',3,(#119166,#119167,#119168,#119169,
#119170,#119171,#119172,#119173,#119174,#119175,#119176,#119177,#119178,
#119179,#119180,#119181,#119182,#119183,#119184,#119185,#119186,#119187,
#119188,#119189,#119190,#119191,#119192,#119193,#119194,#119195,#119196,
#119197,#119198,#119199,#119200,#119201,#119202,#119203,#119204,#119205,
#119206,#119207,#119208,#119209,#119210,#119211,#119212,#119213,#119214,
#119215,#119216,#119217,#119218,#119219,#119220,#119221,#119222,#119223,
#119224,#119225,#119226,#119227,#119228,#119229,#119230,#119231,#119232,
#119233,#119234,#119235,#119236,#119237,#119238,#119239,#119240,#119241,
#119242,#119243,#119244,#119245,#119246,#119247,#119248,#119249,#119250,
#119251,#119252,#119253,#119254,#119255,#119256,#119257,#119258,#119259,
#119260,#119261,#119262,#119263,#119264,#119265,#119266,#119267,#119268),
 .UNSPECIFIED.,.F.,.F.,(4,3,3,3,3,3,3,3,3,3,3,3,3,3,3,3,3,3,3,3,3,3,3,3,
3,3,3,3,3,3,3,3,3,3,4),(0.,0.0501535530149427,0.0843408069737685,0.125000000000027,
0.16757754732749,0.179135824507627,0.187500000000039,0.218750000000045,
0.234375000000044,0.242187500000042,0.248359381055688,0.250000000000041,
0.285533837129323,0.346076131737884,0.374999999999979,0.380522902976463,
0.437499999999947,0.468749999999931,0.474795911141055,0.484374999999925,
0.492187499999923,0.496093749999925,0.499999999999927,0.553255897370739,
0.603065113704012,0.627088768202908,0.675665818704117,0.707465524125276,
0.749999999999963,0.80466568180373,0.85475077335072,0.910734288428706,0.926422203511138,
0.978719943194182,1.),.UNSPECIFIED.);
#29594=B_SPLINE_CURVE_WITH_KNOTS('',3,(#119340,#119341,#119342,#119343,
#119344,#119345,#119346,#119347,#119348,#119349,#119350,#119351,#119352,
#119353,#119354,#119355),.UNSPECIFIED.,.F.,.F.,(4,3,3,3,3,4),(1.44815538111642E-5,
0.210256084640174,0.423632741635552,0.639251052850045,0.859563807440021,
0.999999999994534),.UNSPECIFIED.);
#29595=B_SPLINE_CURVE_WITH_KNOTS('',3,(#119422,#119423,#119424,#119425,
#119426,#119427,#119428,#119429,#119430,#119431,#119432,#119433,#119434,
#119435,#119436,#119437,#119438,#119439,#119440,#119441,#119442,#119443,
#119444,#119445,#119446,#119447,#119448,#119449,#119450,#119451,#119452,
#119453,#119454,#119455,#119456,#119457,#119458,#119459,#119460,#119461,
#119462,#119463,#119464,#119465,#119466,#119467,#119468,#119469,#119470,
#119471,#119472,#119473,#119474,#119475,#119476,#119477,#119478,#119479,
#119480,#119481,#119482,#119483,#119484,#119485,#119486,#119487,#119488),
 .UNSPECIFIED.,.F.,.F.,(4,3,3,3,3,3,3,3,3,3,3,3,3,3,3,3,3,3,3,3,3,3,4),
(2.0903552712953E-10,0.0302476823861621,0.0946324368287587,0.162216233220878,
0.18810280752984,0.250000000000002,0.328856575995871,0.390941197142464,
0.453025818289058,0.468750000000002,0.484375000000002,0.492187500000003,
0.496093750000003,0.498046875000003,0.500000000000004,0.585458270036095,
0.655183530447372,0.72490879085865,0.750000000000002,0.861552612219485,
0.906217681176828,0.953108840588414,1.),.UNSPECIFIED.);
#29596=B_SPLINE_CURVE_WITH_KNOTS('',3,(#119499,#119500,#119501,#119502,
#119503,#119504,#119505,#119506,#119507,#119508,#119509,#119510,#119511,
#119512,#119513,#119514,#119515,#119516,#119517,#119518,#119519,#119520,
#119521,#119522,#119523,#119524,#119525,#119526,#119527,#119528,#119529,
#119530,#119531,#119532,#119533,#119534,#119535,#119536,#119537,#119538,
#119539,#119540,#119541,#119542,#119543,#119544,#119545,#119546,#119547,
#119548,#119549,#119550,#119551,#119552,#119553,#119554,#119555,#119556,
#119557,#119558,#119559,#119560,#119561,#119562,#119563,#119564,#119565,
#119566,#119567,#119568,#119569,#119570,#119571,#119572,#119573,#119574,
#119575,#119576,#119577,#119578,#119579,#119580,#119581,#119582,#119583,
#119584,#119585,#119586,#119587,#119588,#119589,#119590,#119591,#119592,
#119593,#119594,#119595,#119596,#119597,#119598,#119599,#119600,#119601,
#119602,#119603,#119604,#119605,#119606,#119607,#119608,#119609,#119610,
#119611,#119612,#119613,#119614,#119615,#119616,#119617,#119618,#119619,
#119620,#119621,#119622),.UNSPECIFIED.,.F.,.F.,(4,3,3,3,3,3,3,3,3,3,3,3,
3,3,3,3,3,3,3,3,3,3,3,3,3,3,3,3,3,3,3,3,3,3,3,3,3,3,3,3,3,4),(1.06186481877749E-15,
0.0340851358066496,0.0691999299672166,0.105785020111385,0.117362581696846,
0.125000000000004,0.160169392187649,0.187500000000007,0.218750000000008,
0.234375000000009,0.242187500000011,0.246093750000011,0.250000000000011,
0.285437709422724,0.309021567011856,0.343532732159649,0.37857221360227,
0.413947095861862,0.449222909696327,0.483968840156166,0.500000000000016,
0.500003316435609,0.534824037905456,0.570002504688142,0.605300892498013,
0.625000000000019,0.659693858326166,0.68750000000002,0.691017683145083,
0.718750000000021,0.734375000000022,0.742187500000022,0.746093750000022,
0.750000000000022,0.787161509091454,0.823722624830958,0.859049261837564,
0.882626506205646,0.918399913913295,0.953209132777543,0.986561655878065,
1.),.UNSPECIFIED.);
#29597=B_SPLINE_CURVE_WITH_KNOTS('',3,(#119626,#119627,#119628,#119629,
#119630,#119631,#119632,#119633,#119634,#119635,#119636,#119637,#119638,
#119639,#119640,#119641,#119642,#119643,#119644,#119645,#119646,#119647),
 .UNSPECIFIED.,.F.,.F.,(4,3,3,3,3,3,3,4),(4.08364197003503E-10,0.250000000000007,
0.375000000000007,0.437500000000006,0.496331466076166,0.500000000000005,
0.753785934071933,0.999999999974308),.UNSPECIFIED.);
#29598=B_SPLINE_CURVE_WITH_KNOTS('',3,(#119651,#119652,#119653,#119654,
#119655,#119656,#119657,#119658,#119659,#119660,#119661,#119662,#119663,
#119664,#119665,#119666,#119667,#119668,#119669,#119670,#119671,#119672,
#119673,#119674,#119675,#119676,#119677,#119678,#119679,#119680,#119681,
#119682,#119683,#119684,#119685,#119686,#119687,#119688,#119689,#119690,
#119691,#119692,#119693,#119694,#119695,#119696,#119697,#119698,#119699,
#119700,#119701,#119702,#119703,#119704,#119705,#119706,#119707,#119708,
#119709,#119710,#119711,#119712,#119713,#119714,#119715,#119716,#119717,
#119718,#119719,#119720,#119721,#119722,#119723,#119724,#119725,#119726,
#119727,#119728,#119729,#119730,#119731,#119732,#119733,#119734,#119735,
#119736,#119737,#119738,#119739,#119740,#119741,#119742,#119743,#119744,
#119745,#119746,#119747,#119748,#119749,#119750,#119751,#119752,#119753,
#119754,#119755,#119756,#119757,#119758,#119759,#119760,#119761,#119762,
#119763,#119764,#119765,#119766,#119767,#119768),.UNSPECIFIED.,.F.,.F.,
(4,3,3,3,3,3,3,3,3,3,3,3,3,3,3,3,3,3,3,3,3,3,3,3,3,3,3,3,3,3,3,3,3,3,3,
3,3,3,3,4),(0.,0.0271623998492999,0.0553322026502384,0.0841874376300376,
0.113763564313068,0.144091135811689,0.175190924106879,0.207067488782461,
0.240096712177752,0.273752683323411,0.30795455313194,0.342604883632704,
0.377744298735794,0.413067078246304,0.448574733468898,0.468749999999997,
0.484374999999999,0.492187499999999,0.49883613893283,0.5,0.537434732927738,
0.574951049695804,0.611904861516709,0.649702430758356,0.687500000000003,
0.697178248398173,0.703125000000003,0.718750000000002,0.750000000000002,
0.784381124832368,0.81809272813315,0.850771307730581,0.875000000000004,
0.890625000000004,0.898437500000004,0.904724710564298,0.906250000000003,
0.937500000000002,0.980487098276565,1.),.UNSPECIFIED.);
#29599=B_SPLINE_CURVE_WITH_KNOTS('',3,(#119772,#119773,#119774,#119775,
#119776,#119777,#119778,#119779,#119780,#119781,#119782,#119783,#119784,
#119785,#119786,#119787,#119788,#119789,#119790,#119791,#119792,#119793,
#119794,#119795,#119796,#119797,#119798,#119799,#119800,#119801,#119802),
 .UNSPECIFIED.,.F.,.F.,(4,3,3,3,3,3,3,3,3,3,4),(1.10824284158061E-6,0.249999999999966,
0.374999999999952,0.43749999999995,0.468749999999949,0.484374999999949,
0.496093749999949,0.499999999999948,0.719932202069709,0.941144134881108,
1.),.UNSPECIFIED.);
#29600=B_SPLINE_CURVE_WITH_KNOTS('',3,(#119806,#119807,#119808,#119809,
#119810,#119811,#119812,#119813,#119814,#119815,#119816,#119817,#119818,
#119819),.UNSPECIFIED.,.F.,.F.,(4,2,2,1,1,2,2,4),(0.,0.250000000000008,
0.375000000000012,0.437500000000012,0.468750000000011,0.484375000000011,
0.500000000000012,0.999999993863129),.UNSPECIFIED.);
#29601=B_SPLINE_CURVE_WITH_KNOTS('',3,(#119820,#119821,#119822,#119823,
#119824,#119825,#119826,#119827,#119828,#119829,#119830,#119831,#119832,
#119833),.UNSPECIFIED.,.F.,.F.,(4,2,2,1,1,2,2,4),(0.,0.249999999999992,
0.374999999999991,0.43749999999999,0.468749999999991,0.484374999999992,
0.499999999999993,1.),.UNSPECIFIED.);
#29602=B_SPLINE_CURVE_WITH_KNOTS('',3,(#119873,#119874,#119875,#119876,
#119877,#119878,#119879,#119880,#119881,#119882,#119883,#119884,#119885,
#119886,#119887,#119888,#119889,#119890,#119891,#119892,#119893,#119894,
#119895,#119896,#119897,#119898,#119899,#119900,#119901,#119902,#119903,
#119904,#119905,#119906,#119907,#119908,#119909,#119910,#119911,#119912),
 .UNSPECIFIED.,.F.,.F.,(4,3,3,3,3,3,3,3,3,3,3,3,3,4),(0.,0.0829435186321783,
0.16544324384915,0.247585715556801,0.329456585306884,0.413274512143524,
0.494872951961396,0.576482179278369,0.65817673585635,0.743632551892263,
0.825892623948683,0.908430785310346,0.991464788229984,1.),.UNSPECIFIED.);
#29603=B_SPLINE_CURVE_WITH_KNOTS('',3,(#119914,#119915,#119916,#119917,
#119918,#119919,#119920,#119921,#119922,#119923),.UNSPECIFIED.,.F.,.F.,
(4,2,2,2,4),(0.,0.25,0.5,0.75,1.),.UNSPECIFIED.);
#29604=B_SPLINE_CURVE_WITH_KNOTS('',3,(#119924,#119925,#119926,#119927,
#119928,#119929,#119930,#119931,#119932,#119933,#119934,#119935,#119936,
#119937,#119938,#119939,#119940,#119941,#119942,#119943,#119944,#119945,
#119946,#119947,#119948),.UNSPECIFIED.,.F.,.F.,(4,2,2,2,2,2,2,1,1,1,2,2,
2,4),(1.36445938018877E-7,0.124999999999883,0.187499999999825,0.249999999999766,
0.374999999999658,0.437499999999601,0.468749999999574,0.484374999999559,
0.492187499999552,0.496093749999551,0.498046874999548,0.499999999999545,
0.749999999999773,1.),.UNSPECIFIED.);
#29605=B_SPLINE_CURVE_WITH_KNOTS('',3,(#119975,#119976,#119977,#119978,
#119979,#119980,#119981,#119982,#119983,#119984,#119985),.UNSPECIFIED.,
 .F.,.F.,(4,1,1,1,1,1,1,1,4),(0.,0.125,0.25,0.375,0.5,0.625,0.75,0.875,
1.),.UNSPECIFIED.);
#29606=B_SPLINE_CURVE_WITH_KNOTS('',3,(#120092,#120093,#120094,#120095,
#120096,#120097,#120098,#120099,#120100,#120101,#120102,#120103,#120104,
#120105,#120106,#120107,#120108,#120109,#120110,#120111,#120112,#120113,
#120114,#120115,#120116,#120117,#120118,#120119,#120120,#120121,#120122,
#120123,#120124,#120125,#120126,#120127,#120128,#120129,#120130,#120131,
#120132,#120133,#120134,#120135,#120136,#120137,#120138,#120139,#120140,
#120141,#120142,#120143,#120144,#120145,#120146,#120147,#120148,#120149,
#120150,#120151,#120152,#120153,#120154,#120155,#120156,#120157,#120158,
#120159,#120160,#120161,#120162,#120163,#120164,#120165,#120166,#120167,
#120168,#120169,#120170,#120171,#120172,#120173,#120174,#120175,#120176,
#120177,#120178,#120179,#120180,#120181,#120182,#120183,#120184,#120185,
#120186,#120187,#120188,#120189,#120190,#120191,#120192,#120193,#120194,
#120195,#120196,#120197,#120198,#120199,#120200,#120201,#120202,#120203,
#120204,#120205,#120206,#120207,#120208,#120209,#120210,#120211,#120212,
#120213,#120214,#120215,#120216,#120217,#120218,#120219,#120220,#120221,
#120222,#120223,#120224,#120225,#120226,#120227,#120228,#120229,#120230,
#120231,#120232,#120233,#120234,#120235,#120236,#120237,#120238,#120239,
#120240,#120241,#120242,#120243,#120244,#120245,#120246,#120247,#120248,
#120249,#120250,#120251,#120252,#120253,#120254,#120255,#120256,#120257,
#120258,#120259,#120260,#120261,#120262,#120263,#120264,#120265,#120266,
#120267,#120268,#120269,#120270,#120271,#120272,#120273,#120274,#120275,
#120276,#120277,#120278,#120279,#120280,#120281,#120282,#120283,#120284,
#120285,#120286,#120287,#120288,#120289,#120290,#120291,#120292,#120293,
#120294,#120295,#120296,#120297,#120298,#120299,#120300,#120301,#120302,
#120303,#120304,#120305,#120306,#120307,#120308,#120309,#120310,#120311,
#120312,#120313,#120314,#120315,#120316,#120317,#120318,#120319,#120320,
#120321,#120322,#120323,#120324,#120325,#120326,#120327,#120328,#120329,
#120330,#120331,#120332,#120333,#120334,#120335,#120336,#120337,#120338,
#120339,#120340,#120341,#120342,#120343,#120344,#120345,#120346,#120347,
#120348,#120349,#120350,#120351,#120352,#120353),.UNSPECIFIED.,.F.,.F.,
(4,3,3,3,3,3,3,3,3,3,3,3,3,3,3,3,3,3,3,3,3,3,3,3,3,3,3,3,3,3,3,3,3,3,3,
3,3,3,3,3,3,3,3,3,3,3,3,3,3,3,3,3,3,3,3,3,3,3,3,3,3,3,3,3,3,3,3,3,3,3,3,
3,3,3,3,3,3,3,3,3,3,3,3,3,3,3,3,4),(0.,0.0238209341068048,0.0467771592652955,
0.0716124027086975,0.0960789029123286,0.121297615955388,0.124999999999497,
0.1448631456153,0.177264818887828,0.187499999999245,0.192104350528002,0.218749999999119,
0.234374999999057,0.236532403911906,0.242187499999027,0.246093749999012,
0.248046874999006,0.249999999999,0.277130585388565,0.306461178729683,0.312499999998764,
0.31866267267183,0.343749999998647,0.357129683416764,0.359374999998589,
0.367187499998561,0.371093749998547,0.374023437498536,0.374999999998531,
0.396143077643392,0.397799905177464,0.417649952587889,0.437499999998313,
0.438016277914377,0.455310479258491,0.468749999998204,0.474778249992469,
0.484374999998149,0.492187499998122,0.496093749998109,0.498046874998102,
0.499511718748098,0.499999999998097,0.512502904327935,0.531852979385863,
0.550582392521049,0.555525187566182,0.562499999997784,0.581209522793947,
0.593412137124177,0.593749999997628,0.609374999997549,0.61718749999751,
0.621093749997491,0.623046874997481,0.624023437497476,0.624755859372473,
0.624999999997473,0.626485940845937,0.637328140931271,0.64811722289407,
0.656249999997412,0.667544912414052,0.6778997253239,0.687499999997352,0.698454072030051,
0.709299235852108,0.718749999997292,0.729412231271347,0.734374999997263,
0.742187499997248,0.742996539894464,0.746093749997245,0.748046874997241,
0.749023437497239,0.749755859372251,0.749999999997255,0.787581559332529,
0.80494092963963,0.845391786652635,0.868911827543509,0.874999999998627,
0.901163899253755,0.926976316555449,0.941952390352306,0.966830975600087,
0.990868090258758,1.),.UNSPECIFIED.);
#29607=B_SPLINE_CURVE_WITH_KNOTS('',3,(#120391,#120392,#120393,#120394,
#120395,#120396,#120397,#120398,#120399,#120400,#120401,#120402,#120403,
#120404,#120405,#120406,#120407,#120408,#120409,#120410,#120411,#120412,
#120413,#120414,#120415,#120416,#120417,#120418,#120419,#120420,#120421,
#120422,#120423,#120424,#120425,#120426,#120427),.UNSPECIFIED.,.F.,.F.,
(4,3,3,3,3,3,3,3,3,3,3,3,4),(0.,0.125,0.159379704574452,0.25,0.375,0.442772260766343,
0.5,0.625,0.695069700307422,0.75,0.875,0.9182517730451,1.),
 .UNSPECIFIED.);
#29608=B_SPLINE_CURVE_WITH_KNOTS('',3,(#120454,#120455,#120456,#120457,
#120458,#120459,#120460,#120461,#120462,#120463,#120464,#120465,#120466,
#120467,#120468,#120469,#120470,#120471,#120472,#120473,#120474,#120475,
#120476,#120477,#120478,#120479,#120480,#120481,#120482,#120483,#120484,
#120485,#120486,#120487,#120488,#120489,#120490,#120491,#120492,#120493,
#120494,#120495,#120496,#120497,#120498,#120499,#120500,#120501,#120502,
#120503,#120504,#120505,#120506,#120507,#120508,#120509,#120510,#120511),
 .UNSPECIFIED.,.F.,.F.,(4,3,3,3,3,3,3,3,3,3,3,3,3,3,3,3,3,3,3,4),(2.46869136895203E-9,
0.0537338962153679,0.107904863661443,0.162436722894872,0.217699031243316,
0.25,0.304279076375914,0.325891175570963,0.382268789223474,0.441134394611737,
0.5,0.565029224088735,0.631574437929143,0.701211809658827,0.727527916786862,
0.75,0.829316881692732,0.908964210246409,0.988920295930411,1.),
 .UNSPECIFIED.);
#29609=B_SPLINE_CURVE_WITH_KNOTS('',3,(#120538,#120539,#120540,#120541,
#120542,#120543,#120544,#120545,#120546,#120547,#120548,#120549,#120550,
#120551,#120552,#120553,#120554,#120555,#120556,#120557,#120558,#120559,
#120560,#120561,#120562,#120563,#120564,#120565,#120566,#120567,#120568,
#120569,#120570,#120571,#120572,#120573,#120574,#120575,#120576,#120577,
#120578,#120579,#120580,#120581,#120582,#120583,#120584,#120585,#120586,
#120587,#120588,#120589,#120590,#120591,#120592,#120593,#120594,#120595,
#120596,#120597,#120598),.UNSPECIFIED.,.F.,.F.,(4,3,3,3,3,3,3,3,3,3,3,3,
3,3,3,3,3,3,3,3,4),(3.09719472403435E-11,0.0796519720589834,0.159046227126963,
0.237897866026407,0.25,0.280661606842029,0.349436459717617,0.416021534400952,
0.480361119054478,0.5,0.557540612918763,0.614138830092457,0.669699825343428,
0.689729105407977,0.743459053446208,0.75,0.805600763210536,0.860275880253665,
0.91452354817423,0.96831217149722,1.),.UNSPECIFIED.);
#29610=B_SPLINE_CURVE_WITH_KNOTS('',3,(#120637,#120638,#120639,#120640,
#120641,#120642,#120643,#120644,#120645,#120646,#120647,#120648,#120649,
#120650,#120651,#120652,#120653,#120654,#120655,#120656,#120657,#120658,
#120659,#120660,#120661,#120662,#120663,#120664,#120665,#120666,#120667,
#120668,#120669,#120670,#120671,#120672,#120673,#120674,#120675,#120676,
#120677,#120678,#120679,#120680,#120681,#120682,#120683,#120684,#120685,
#120686,#120687,#120688,#120689,#120690,#120691,#120692,#120693,#120694,
#120695,#120696,#120697,#120698,#120699,#120700,#120701,#120702,#120703,
#120704,#120705,#120706,#120707,#120708,#120709,#120710,#120711,#120712,
#120713,#120714,#120715,#120716,#120717,#120718,#120719,#120720,#120721,
#120722,#120723,#120724,#120725,#120726,#120727,#120728,#120729,#120730,
#120731,#120732,#120733,#120734,#120735,#120736,#120737,#120738,#120739,
#120740,#120741,#120742,#120743,#120744,#120745,#120746,#120747,#120748),
 .UNSPECIFIED.,.F.,.F.,(4,3,3,3,3,3,3,3,3,3,3,3,3,3,3,3,3,3,3,3,3,3,3,3,
3,3,3,3,3,3,3,3,3,3,3,3,3,4),(1.35859990185527E-10,0.0470443616163219,0.0914258222496483,
0.134880138091579,0.177094202045214,0.188177446057708,0.232586222210198,
0.249999999999647,0.292935299290597,0.334529543417577,0.370069482793404,
0.374999999999471,0.419953636131847,0.437499999999383,0.468749999999339,
0.484374999999316,0.492187499999305,0.497503839155331,0.499999999999294,
0.527504839471645,0.586107358467935,0.624999999999114,0.680623224833669,
0.687499999999023,0.718749999998977,0.734374999998954,0.742187499998943,
0.746093749998938,0.749023437498937,0.749999999998938,0.790947953022685,
0.831969774017496,0.866381434603491,0.87499999999947,0.917111533151109,
0.958555766575555,0.997597822520349,1.),.UNSPECIFIED.);
#29611=B_SPLINE_CURVE_WITH_KNOTS('',3,(#120785,#120786,#120787,#120788,
#120789,#120790,#120791,#120792,#120793,#120794,#120795,#120796,#120797,
#120798,#120799,#120800,#120801,#120802,#120803,#120804,#120805,#120806,
#120807,#120808,#120809,#120810,#120811,#120812,#120813,#120814,#120815,
#120816,#120817,#120818,#120819,#120820,#120821,#120822,#120823,#120824,
#120825,#120826,#120827,#120828,#120829,#120830,#120831,#120832,#120833,
#120834,#120835,#120836,#120837,#120838,#120839,#120840,#120841,#120842,
#120843,#120844,#120845,#120846,#120847,#120848,#120849,#120850,#120851,
#120852,#120853,#120854,#120855,#120856,#120857,#120858,#120859,#120860,
#120861,#120862,#120863,#120864,#120865,#120866,#120867,#120868,#120869,
#120870,#120871,#120872,#120873,#120874,#120875,#120876,#120877,#120878),
 .UNSPECIFIED.,.F.,.F.,(4,3,3,3,3,3,3,3,3,3,3,3,3,3,3,3,3,3,3,3,3,3,3,3,
3,3,3,3,3,3,3,4),(1.82471863577943E-15,0.0480765556136813,0.0950049750541619,
0.109486100629603,0.125000000000092,0.17303730245179,0.187500000000138,
0.218750000000161,0.234375000000174,0.242187500000179,0.242327475881498,
0.246093750000182,0.249352229155617,0.250000000000186,0.333497092429205,
0.371351184332586,0.375000000000239,0.437500000000266,0.46875000000028,
0.484375000000287,0.492187500000291,0.499023437500293,0.500000000000293,
0.500924792082816,0.597383972836421,0.652289628044168,0.743514330544788,
0.750000000000146,0.786603976412445,0.885125481150069,0.905550136399524,
1.),.UNSPECIFIED.);
#29612=B_SPLINE_CURVE_WITH_KNOTS('',3,(#120950,#120951,#120952,#120953,
#120954,#120955,#120956,#120957,#120958,#120959,#120960,#120961,#120962,
#120963,#120964,#120965,#120966,#120967,#120968,#120969,#120970,#120971,
#120972,#120973,#120974,#120975,#120976,#120977,#120978,#120979,#120980,
#120981,#120982,#120983,#120984,#120985,#120986,#120987,#120988,#120989,
#120990,#120991,#120992,#120993,#120994,#120995,#120996,#120997,#120998,
#120999,#121000,#121001,#121002,#121003,#121004,#121005,#121006,#121007,
#121008,#121009,#121010,#121011,#121012,#121013,#121014,#121015,#121016,
#121017,#121018,#121019,#121020,#121021,#121022,#121023,#121024,#121025,
#121026,#121027,#121028,#121029,#121030,#121031,#121032,#121033,#121034),
 .UNSPECIFIED.,.F.,.F.,(4,3,3,3,3,3,3,3,3,3,3,3,3,3,3,3,3,3,3,3,3,3,3,3,
3,3,3,3,4),(0.,0.0377356474345836,0.0750359183060471,0.112014973382577,
0.148784553462237,0.185454708791299,0.222134505688996,0.259084364534882,
0.296281779749553,0.333825646040157,0.37181660829074,0.410693571798126,
0.450151209829126,0.490604164911084,0.49999988363958,0.540309510289047,
0.579736856800743,0.618411911999495,0.656459211910049,0.69399873229563,
0.732248890758676,0.769066832853226,0.805766270351344,0.842443980675107,
0.87919658146079,0.916274247721778,0.953595787796437,0.99142322355931,1.),
 .UNSPECIFIED.);
#29613=B_SPLINE_CURVE_WITH_KNOTS('',3,(#121585,#121586,#121587,#121588,
#121589,#121590,#121591,#121592,#121593,#121594,#121595,#121596,#121597,
#121598,#121599,#121600,#121601,#121602),.UNSPECIFIED.,.F.,.F.,(4,2,2,2,
2,2,2,2,4),(0.,0.125,0.25,0.375,0.5,0.625,0.75,0.875,1.),.UNSPECIFIED.);
#29614=B_SPLINE_CURVE_WITH_KNOTS('',3,(#121744,#121745,#121746,#121747,
#121748,#121749,#121750,#121751,#121752,#121753,#121754,#121755,#121756,
#121757,#121758,#121759,#121760,#121761,#121762,#121763,#121764,#121765,
#121766,#121767,#121768,#121769,#121770,#121771,#121772,#121773,#121774,
#121775,#121776,#121777,#121778,#121779,#121780,#121781,#121782,#121783,
#121784,#121785,#121786,#121787,#121788,#121789,#121790,#121791,#121792,
#121793,#121794,#121795,#121796,#121797,#121798,#121799,#121800,#121801,
#121802,#121803,#121804,#121805,#121806,#121807,#121808,#121809,#121810,
#121811,#121812,#121813,#121814,#121815,#121816,#121817,#121818,#121819),
 .UNSPECIFIED.,.F.,.F.,(4,3,3,3,3,3,3,3,3,3,3,3,3,3,3,3,3,3,3,3,3,3,3,3,
3,4),(0.,0.0425596242447764,0.0850361814342877,0.127671390328244,0.170444375881725,
0.213698376037449,0.25,0.294181213942584,0.339346412338439,0.375,0.421689901291409,
0.433453762242374,0.480051410417501,0.5,0.545161817254489,0.589577224406666,
0.633151386249373,0.676316383684887,0.719082658493756,0.75,0.792498951096667,
0.835001497275773,0.877796290208396,0.920803849450017,0.964410339796297,
1.),.UNSPECIFIED.);
#29615=B_SPLINE_CURVE_WITH_KNOTS('',3,(#121907,#121908,#121909,#121910,
#121911,#121912,#121913,#121914,#121915,#121916),.UNSPECIFIED.,.F.,.F.,
(4,2,2,2,4),(0.000307180223244836,0.23813963987228,0.403654270152061,0.532445083611112,
0.661208903651667),.UNSPECIFIED.);
#29616=B_SPLINE_CURVE_WITH_KNOTS('',3,(#121917,#121918,#121919,#121920,
#121921,#121922,#121923,#121924,#121925,#121926,#121927,#121928,#121929,
#121930),.UNSPECIFIED.,.F.,.F.,(4,2,2,2,2,2,4),(0.000330903451301007,0.188084532547518,
0.374775943028081,0.612257137717574,0.795567417884798,0.901363102744604,
1.00443306905523),.UNSPECIFIED.);
#29617=B_SPLINE_CURVE_WITH_KNOTS('',3,(#121931,#121932,#121933,#121934,
#121935,#121936,#121937,#121938,#121939,#121940,#121941,#121942,#121943,
#121944,#121945,#121946,#121947,#121948,#121949,#121950,#121951,#121952,
#121953,#121954,#121955,#121956,#121957,#121958,#121959,#121960,#121961,
#121962,#121963,#121964,#121965,#121966,#121967,#121968,#121969,#121970,
#121971,#121972,#121973,#121974,#121975,#121976,#121977,#121978,#121979,
#121980,#121981,#121982,#121983,#121984,#121985,#121986,#121987,#121988,
#121989,#121990,#121991,#121992,#121993,#121994,#121995,#121996,#121997,
#121998,#121999,#122000,#122001,#122002,#122003,#122004,#122005,#122006,
#122007,#122008,#122009,#122010,#122011,#122012,#122013,#122014,#122015,
#122016,#122017,#122018,#122019,#122020,#122021,#122022,#122023,#122024,
#122025,#122026,#122027,#122028,#122029,#122030,#122031,#122032,#122033,
#122034,#122035,#122036,#122037,#122038,#122039),.UNSPECIFIED.,.F.,.F.,
(4,3,3,3,3,3,3,3,3,3,3,3,3,3,3,3,3,3,3,3,3,3,3,3,3,3,3,3,3,3,3,3,3,3,3,
3,4),(5.49757971508832E-5,0.0323764919258928,0.0647628196246539,0.0969949948714976,
0.124999999999994,0.157798122778746,0.189882334389919,0.201607571319194,
0.234374999999991,0.243938228638234,0.249999999999991,0.281697673924662,
0.313958065309001,0.346679963238968,0.379829992946779,0.413050745110431,
0.446112843622199,0.468749999999984,0.484374999999984,0.499999999999983,
0.533983406046698,0.56790148030433,0.601435499225249,0.629514094834484,
0.663266314189443,0.687499999999991,0.715194727768877,0.743005238070075,
0.749999999999992,0.782919512243476,0.816298218352298,0.850005157037389,
0.883880530988718,0.917676982175652,0.951261736544021,0.984338012747187,
0.999964300005559),.UNSPECIFIED.);
#29618=B_SPLINE_CURVE_WITH_KNOTS('',3,(#122085,#122086,#122087,#122088,
#122089,#122090,#122091,#122092,#122093,#122094,#122095,#122096,#122097,
#122098,#122099,#122100,#122101,#122102,#122103,#122104,#122105,#122106,
#122107,#122108,#122109,#122110,#122111,#122112,#122113,#122114,#122115,
#122116,#122117,#122118,#122119,#122120,#122121,#122122,#122123,#122124,
#122125,#122126,#122127,#122128,#122129,#122130,#122131,#122132,#122133,
#122134,#122135,#122136,#122137,#122138,#122139,#122140,#122141,#122142,
#122143,#122144,#122145,#122146,#122147,#122148,#122149,#122150,#122151,
#122152,#122153,#122154,#122155,#122156,#122157,#122158,#122159,#122160,
#122161,#122162,#122163,#122164,#122165,#122166,#122167,#122168,#122169,
#122170,#122171,#122172,#122173,#122174,#122175,#122176,#122177,#122178,
#122179,#122180,#122181,#122182,#122183,#122184,#122185,#122186,#122187,
#122188,#122189,#122190,#122191,#122192,#122193,#122194,#122195,#122196,
#122197,#122198,#122199,#122200,#122201,#122202,#122203,#122204,#122205,
#122206,#122207,#122208,#122209,#122210,#122211,#122212,#122213,#122214,
#122215,#122216,#122217,#122218,#122219,#122220,#122221,#122222,#122223,
#122224,#122225,#122226,#122227,#122228,#122229,#122230,#122231,#122232,
#122233,#122234,#122235,#122236,#122237,#122238,#122239,#122240,#122241,
#122242,#122243,#122244),.UNSPECIFIED.,.F.,.F.,(4,3,3,3,3,3,3,3,3,3,3,3,
3,3,3,3,3,3,3,3,3,3,3,3,3,3,3,3,3,3,3,3,3,3,3,3,3,3,3,3,3,3,3,3,3,3,3,3,
3,3,3,3,3,4),(0.,0.033129419996528,0.0625,0.082406368093979,0.101976381960474,
0.120919538933606,0.125,0.131399088166994,0.155178211525652,0.180376994852815,
0.206264449066017,0.23253290097541,0.25,0.269300260094727,0.286686870246049,
0.305558168739884,0.324831549147336,0.344082508667133,0.362955762961432,
0.375,0.39250067506772,0.41010515685722,0.42757262063518,0.441864639561154,
0.459372727734466,0.476982526010831,0.494482045172937,0.5,0.520230351612384,
0.541125772179517,0.562132098769343,0.582818980361532,0.597074992568842,
0.61807026910004,0.625,0.648247295937558,0.671966741455924,0.695535554643394,
0.718590663848995,0.740681955330333,0.75,0.752375849440358,0.775477859920143,
0.800358394940107,0.825273162437448,0.850161922207706,0.874999999999999,
0.893484411102079,0.907662745170859,0.925963795076234,0.9375,0.958867940339968,
0.981119642099533,0.999990983828168),.UNSPECIFIED.);
#29619=B_SPLINE_CURVE_WITH_KNOTS('',3,(#122358,#122359,#122360,#122361,
#122362,#122363,#122364,#122365,#122366,#122367,#122368,#122369,#122370,
#122371,#122372,#122373,#122374,#122375,#122376,#122377,#122378,#122379,
#122380,#122381,#122382,#122383,#122384,#122385,#122386,#122387,#122388,
#122389,#122390,#122391,#122392,#122393,#122394,#122395,#122396,#122397,
#122398,#122399,#122400,#122401,#122402,#122403,#122404,#122405,#122406,
#122407,#122408,#122409,#122410,#122411,#122412,#122413,#122414,#122415,
#122416,#122417,#122418,#122419,#122420,#122421,#122422,#122423,#122424,
#122425,#122426,#122427,#122428,#122429,#122430,#122431),.UNSPECIFIED.,
 .F.,.F.,(4,2,2,2,2,2,2,2,2,2,2,2,2,2,2,2,2,2,2,2,2,2,2,2,2,2,2,2,2,2,2,
2,2,2,2,2,4),(0.000380014155147578,0.245400900644386,0.378255056806249,
0.463178941729333,0.615939968604413,0.712651720402226,0.856256025420663,
0.962182568221084,1.24868208289919,1.37004830733658,1.46833903165977,1.67247354457994,
1.76813658054073,1.98089867447481,2.11019670522888,2.24182819113389,2.50529938263797,
2.70189252294529,2.80669898539374,2.94035387038927,3.05860534802554,3.30159424022801,
3.45351780809231,3.71018557888163,3.82068057363443,4.00827847738079,4.09333004173814,
4.25652959393851,4.3142784495563,4.44522754595014,4.62073300232603,4.82402568991634,
4.90519387006344,5.0009249225532,5.14395581948815,5.28962261426793,5.35030271608699),
 .UNSPECIFIED.);
#29620=B_SPLINE_CURVE_WITH_KNOTS('',3,(#122650,#122651,#122652,#122653,
#122654,#122655),.UNSPECIFIED.,.F.,.F.,(4,2,4),(-0.164978192357391,-0.0826598660794179,
-6.1266948559559E-5),.UNSPECIFIED.);
#29621=B_SPLINE_CURVE_WITH_KNOTS('',3,(#122656,#122657,#122658,#122659,
#122660,#122661,#122662,#122663,#122664,#122665,#122666,#122667,#122668,
#122669,#122670,#122671,#122672,#122673,#122674,#122675,#122676,#122677,
#122678,#122679,#122680,#122681,#122682,#122683,#122684,#122685,#122686,
#122687,#122688,#122689,#122690,#122691,#122692,#122693,#122694,#122695,
#122696,#122697,#122698,#122699,#122700,#122701,#122702,#122703,#122704,
#122705,#122706,#122707,#122708,#122709,#122710,#122711,#122712,#122713,
#122714,#122715,#122716,#122717,#122718,#122719,#122720,#122721,#122722,
#122723,#122724,#122725,#122726,#122727,#122728,#122729,#122730,#122731,
#122732,#122733,#122734,#122735,#122736,#122737,#122738,#122739,#122740,
#122741,#122742,#122743,#122744,#122745,#122746,#122747,#122748,#122749,
#122750,#122751,#122752,#122753,#122754,#122755,#122756,#122757,#122758,
#122759,#122760,#122761,#122762,#122763,#122764,#122765,#122766,#122767,
#122768,#122769,#122770,#122771,#122772,#122773,#122774,#122775,#122776,
#122777,#122778,#122779,#122780,#122781,#122782,#122783,#122784,#122785,
#122786,#122787,#122788,#122789,#122790,#122791,#122792,#122793,#122794,
#122795,#122796,#122797,#122798,#122799,#122800,#122801,#122802,#122803,
#122804,#122805,#122806,#122807,#122808,#122809,#122810,#122811,#122812,
#122813,#122814,#122815,#122816,#122817,#122818,#122819,#122820,#122821,
#122822,#122823,#122824,#122825,#122826,#122827,#122828,#122829,#122830,
#122831,#122832,#122833,#122834,#122835,#122836,#122837,#122838,#122839,
#122840,#122841,#122842,#122843,#122844,#122845,#122846,#122847,#122848,
#122849,#122850,#122851,#122852,#122853,#122854,#122855,#122856,#122857,
#122858,#122859,#122860,#122861,#122862,#122863,#122864,#122865,#122866,
#122867,#122868,#122869,#122870,#122871,#122872,#122873,#122874,#122875,
#122876,#122877,#122878,#122879,#122880,#122881,#122882,#122883,#122884,
#122885,#122886,#122887,#122888,#122889,#122890,#122891,#122892,#122893,
#122894,#122895,#122896,#122897,#122898,#122899,#122900,#122901,#122902,
#122903,#122904,#122905,#122906,#122907,#122908,#122909,#122910,#122911,
#122912,#122913,#122914,#122915,#122916,#122917,#122918,#122919,#122920,
#122921,#122922,#122923,#122924,#122925,#122926,#122927,#122928,#122929),
 .UNSPECIFIED.,.F.,.F.,(4,2,2,2,2,2,2,2,2,2,2,2,2,2,2,2,2,2,2,2,2,2,2,2,
2,2,2,2,2,2,2,2,2,2,2,2,2,2,2,2,2,2,2,2,2,2,2,2,2,2,2,2,2,2,2,2,2,2,2,2,
2,2,2,2,2,2,2,2,2,2,2,2,2,2,2,2,2,2,2,2,2,2,2,2,2,2,2,2,2,2,2,2,2,2,2,2,
2,2,2,2,2,2,2,2,2,2,2,2,2,2,2,2,2,2,2,2,2,2,2,2,2,2,2,2,2,2,2,2,2,2,2,2,
2,2,2,2,4),(0.000107512992587567,0.0307029019400883,0.100674212329956,0.180228075751325,
0.223629579703032,0.323919845537183,0.427401544199471,0.471224803865406,
0.583011397883141,0.626400339262408,0.66873184127474,0.737215545709424,
0.845622646823796,0.911171121611078,0.953287896144272,1.02549345955771,
1.09680105460438,1.14185700300284,1.25541675409781,1.35851753679182,1.40299698368004,
1.47702838572308,1.5551977984083,1.60115722077726,1.71873749126671,1.81817866078206,
1.86436795535943,1.93730809028004,2.01368613423001,2.06088763331795,2.20020985446626,
2.26468915413711,2.31672947233915,2.4246770501876,2.46671363402353,2.51411350596787,
2.65381332413122,2.72275435940137,2.777342380313,2.88426525387493,2.92678175415279,
2.97615763886728,3.10740549087446,3.180980377387,3.23815711434674,3.34215362263346,
3.38601797756853,3.43741188267961,3.54467777649841,3.63171848251686,3.69481537016392,
3.75212879385147,3.82275558517828,3.87612962526921,3.95177424416194,4.07393090099034,
4.13172841019533,4.18351479411174,4.2705764461913,4.31912584057365,4.38250782077004,
4.5251978320351,4.60817147112523,4.66273098314723,4.75271255076504,4.80889116540233,
4.90294295753267,5.00850630294855,5.08083401316878,5.15285202196741,5.20910477165492,
5.26759899494988,5.36663118994816,5.47251101319393,5.54617039862718,5.63257611663657,
5.6862460524546,5.75288766489232,5.90524576359981,5.99823452074483,6.0990762014458,
6.17136776695553,6.35777567918109,6.46014851823537,6.55091370704972,6.61114640499581,
6.69291504150126,6.84207985177244,6.91279980483302,6.98265522377385,7.0445092411034,
7.11723125794406,7.20271918433045,7.38789940501584,7.4583079712193,7.55592669346919,
7.69308787750945,7.84085311941344,7.92076956771712,8.01940122147781,8.10637205006814,
8.32606194523382,8.39803835772438,8.4817437542093,8.57639856983484,8.7850038869388,
8.86453348834936,8.95410792023663,9.06348271921736,9.25315373748551,9.33890568952937,
9.44906848541356,9.60176037303482,9.72921770001139,9.81940238786216,9.97563038872898,
10.2009413300206,10.2906338093867,10.479299785875,10.6556209495947,10.7576154833082,
10.8890151810613,11.0616734096201,11.2444507251959,11.4132342709487,11.5897230164771,
11.7152242220242,11.9303380425397,12.2870964789061,12.4637943364461,12.7344749369786,
12.9129627166077,13.0899098943205,13.4398693363585,13.613254539275,13.8661682772203,
14.1207718959965),.UNSPECIFIED.);
#29622=B_SPLINE_CURVE_WITH_KNOTS('',3,(#123071,#123072,#123073,#123074,
#123075,#123076,#123077,#123078,#123079,#123080,#123081,#123082,#123083,
#123084,#123085,#123086,#123087,#123088,#123089,#123090,#123091,#123092,
#123093,#123094,#123095,#123096,#123097,#123098,#123099,#123100,#123101,
#123102,#123103,#123104,#123105,#123106,#123107,#123108,#123109,#123110,
#123111,#123112,#123113,#123114,#123115,#123116,#123117,#123118,#123119,
#123120,#123121,#123122,#123123,#123124,#123125,#123126,#123127,#123128,
#123129,#123130,#123131,#123132,#123133,#123134,#123135,#123136,#123137,
#123138,#123139,#123140),.UNSPECIFIED.,.F.,.F.,(4,3,3,3,3,3,3,3,3,3,3,3,
3,3,3,3,3,3,3,3,3,3,3,4),(0.000487461485702938,0.0513587634045652,0.102739521495275,
0.154402996931755,0.206009843163793,0.25733899970698,0.30794881997648,0.334407148518828,
0.385559996521794,0.436202598467051,0.483282059114614,0.493580691131268,
0.498350316792659,0.502179951010243,0.551475747420326,0.601611641439809,
0.654418301991745,0.705919568722183,0.759378926184868,0.812838283647554,
0.864463775759805,0.916113864982514,0.967433679917503,1.),.UNSPECIFIED.);
#29623=B_SPLINE_CURVE_WITH_KNOTS('',3,(#123141,#123142,#123143,#123144,
#123145,#123146,#123147,#123148,#123149,#123150,#123151,#123152,#123153,
#123154,#123155,#123156,#123157,#123158,#123159,#123160,#123161,#123162,
#123163,#123164,#123165,#123166,#123167,#123168,#123169,#123170,#123171,
#123172,#123173,#123174,#123175,#123176,#123177,#123178,#123179,#123180,
#123181,#123182,#123183,#123184,#123185,#123186,#123187,#123188,#123189,
#123190,#123191,#123192,#123193,#123194,#123195,#123196,#123197,#123198,
#123199,#123200,#123201,#123202,#123203,#123204,#123205,#123206,#123207,
#123208,#123209,#123210,#123211,#123212,#123213,#123214,#123215,#123216,
#123217,#123218,#123219,#123220,#123221,#123222,#123223,#123224,#123225,
#123226,#123227,#123228,#123229,#123230,#123231,#123232,#123233,#123234,
#123235,#123236,#123237,#123238,#123239,#123240,#123241,#123242,#123243,
#123244,#123245,#123246,#123247,#123248,#123249,#123250,#123251,#123252,
#123253,#123254,#123255,#123256,#123257,#123258,#123259,#123260,#123261,
#123262,#123263,#123264,#123265,#123266,#123267,#123268,#123269,#123270,
#123271,#123272,#123273,#123274,#123275,#123276,#123277,#123278,#123279,
#123280,#123281,#123282,#123283,#123284,#123285,#123286,#123287,#123288,
#123289,#123290,#123291,#123292,#123293,#123294,#123295,#123296,#123297,
#123298,#123299,#123300,#123301,#123302,#123303,#123304,#123305,#123306,
#123307,#123308,#123309,#123310,#123311,#123312,#123313,#123314,#123315,
#123316,#123317,#123318,#123319,#123320,#123321,#123322,#123323,#123324,
#123325,#123326,#123327,#123328,#123329,#123330,#123331,#123332,#123333,
#123334,#123335,#123336,#123337,#123338,#123339,#123340,#123341,#123342,
#123343,#123344,#123345,#123346,#123347,#123348,#123349,#123350,#123351,
#123352,#123353,#123354,#123355,#123356,#123357,#123358,#123359,#123360,
#123361,#123362,#123363,#123364,#123365,#123366,#123367,#123368,#123369,
#123370,#123371,#123372,#123373,#123374,#123375,#123376,#123377,#123378,
#123379,#123380,#123381,#123382,#123383,#123384,#123385,#123386,#123387,
#123388,#123389,#123390,#123391,#123392,#123393,#123394,#123395,#123396,
#123397,#123398,#123399,#123400,#123401,#123402,#123403,#123404,#123405,
#123406,#123407,#123408,#123409,#123410,#123411,#123412,#123413,#123414,
#123415,#123416,#123417,#123418,#123419,#123420,#123421,#123422,#123423,
#123424,#123425,#123426,#123427,#123428,#123429,#123430,#123431,#123432,
#123433,#123434,#123435,#123436,#123437,#123438,#123439,#123440,#123441,
#123442,#123443,#123444,#123445,#123446,#123447,#123448,#123449,#123450,
#123451,#123452),.UNSPECIFIED.,.F.,.F.,(4,2,2,2,2,2,2,2,2,2,2,2,2,2,2,2,
2,2,2,2,2,2,2,2,2,2,2,2,2,2,2,2,2,2,2,2,2,2,2,2,2,2,2,2,2,2,2,2,2,2,2,2,
2,2,2,2,2,2,2,2,2,2,2,2,2,2,2,2,2,2,2,2,2,2,2,2,2,2,2,2,2,2,2,2,2,2,2,2,
2,2,2,2,2,2,2,2,2,2,2,2,2,2,2,2,2,2,2,2,2,2,2,2,2,2,2,2,2,2,2,2,2,2,2,2,
2,2,2,2,2,2,2,2,2,2,2,2,2,2,2,2,2,2,2,2,2,2,2,2,2,2,2,2,2,2,2,4),(-18.5336227826717,
-18.4514448464926,-18.3192192351927,-18.2650075335487,-18.2296714748852,
-18.1936764844934,-18.1398332323042,-17.9787567624792,-17.6074573856008,
-17.4091261341456,-17.2859748498613,-17.1486066700017,-16.8265679635732,
-16.6714026169584,-16.5369101371266,-16.3635946951212,-16.1449777165132,
-15.976591588593,-15.850232744328,-15.719410379549,-15.4335967644799,-15.3021203406268,
-15.0737477187498,-14.9686633592023,-14.6821199003543,-14.5166018440642,
-14.4190871127192,-14.2365688695425,-14.1549985867376,-14.0094123223151,
-13.8390819603086,-13.7262967303264,-13.6376584314877,-13.4760226296493,
-13.3832983618377,-13.2972446525463,-13.0899731981048,-12.9983742927356,
-12.920788894281,-12.7456562217242,-12.6050338049676,-12.5359590214847,
-12.3689141170616,-12.2113297245226,-12.1394297703413,-12.0218491054587,
-11.8753788793851,-11.7807108351215,-11.7066713015056,-11.523302821056,
-11.4412051755254,-11.3676144563314,-11.1253926001387,-11.0293198021,-10.9504792860078,
-10.7430838491658,-10.6623854411574,-10.5829348304118,-10.4242381587643,
-10.2707780527122,-10.1645906166968,-10.0761279647731,-9.89450227377428,
-9.80277984150293,-9.64601940897569,-9.47027339843058,-9.34923892594618,
-9.18181695131492,-9.0807999609014,-8.94229176178927,-8.68557879400708,
-8.56254906259355,-8.44364973517209,-8.30539798661457,-7.89871833726101,
-7.73145721019517,-7.45916760741117,-6.83025432997125,-6.52534187991016,
-6.07249570523818,-5.89165241152614,-5.79714214963211,-5.63598606556114,
-5.52969354225683,-5.3423835033615,-5.25759186065315,-5.18724048257733,
-5.1175100810236,-4.96593366239356,-4.89035567654671,-4.83259928305064,
-4.75029160524615,-4.6849317220865,-4.59312652184032,-4.49460001409083,
-4.44161946958288,-4.33894081785888,-4.28905965363311,-4.22808891227909,
-4.13686583498971,-4.05095250786917,-4.00560939785189,-3.95669382763748,
-3.85483321893934,-3.81312267865046,-3.71393955714425,-3.62374250053462,
-3.58177584901668,-3.50096552738975,-3.40620773382679,-3.36751847198954,
-3.32526910970592,-3.2327219323547,-3.17161730698468,-3.12911420654313,
-3.07675136756009,-2.95087046426691,-2.91184371074789,-2.82377441762149,
-2.74097048134806,-2.69835381872593,-2.64854468976623,-2.53188028518126,
-2.48203230616119,-2.4328648000492,-2.35512837158407,-2.29536984943275,
-2.24180082960586,-2.17243444539022,-2.04973933686738,-2.00344232911898,
-1.95639296462131,-1.85954692193472,-1.79502549613509,-1.70634293710404,
-1.59827660739526,-1.54298367544123,-1.48200932828646,-1.41686546373561,
-1.33260166363418,-1.19565746731822,-1.12254945361788,-1.04777428960563,
-0.945985362306715,-0.782164001502387,-0.679764347521197,-0.600110757961878,
-0.517945998215963,-0.330531509823378,-0.233428033688739,-0.204144318222011,
-0.185289377988479,-0.166925413601217,-0.13677198850432,-0.0618204439494522,
-0.000371176546537626),.UNSPECIFIED.);
#29624=B_SPLINE_CURVE_WITH_KNOTS('',3,(#123585,#123586,#123587,#123588,
#123589,#123590),.UNSPECIFIED.,.F.,.F.,(4,2,4),(-0.164574081374655,-0.0827307715189429,
0.),.UNSPECIFIED.);
#29625=B_SPLINE_CURVE_WITH_KNOTS('',3,(#123653,#123654,#123655,#123656,
#123657,#123658,#123659,#123660,#123661,#123662,#123663,#123664,#123665,
#123666,#123667,#123668,#123669,#123670,#123671,#123672,#123673,#123674,
#123675,#123676,#123677,#123678,#123679,#123680,#123681,#123682,#123683,
#123684,#123685,#123686,#123687,#123688,#123689,#123690,#123691,#123692,
#123693,#123694,#123695,#123696,#123697,#123698,#123699,#123700,#123701),
 .UNSPECIFIED.,.F.,.F.,(4,3,3,3,3,3,3,3,3,3,3,3,3,3,3,3,4),(0.,0.0904233751484227,
0.178899056629695,0.24999999999995,0.336290310678144,0.374999999999928,
0.398831360155259,0.437499999999918,0.468749999999913,0.487949724956403,
0.499999999999908,0.586414266141055,0.67420168428988,0.764518735858738,
0.856393583171992,0.950989960497635,1.),.UNSPECIFIED.);
#29626=B_SPLINE_CURVE_WITH_KNOTS('',3,(#123703,#123704,#123705,#123706,
#123707,#123708,#123709,#123710,#123711,#123712,#123713,#123714,#123715,
#123716,#123717,#123718,#123719,#123720,#123721,#123722,#123723,#123724,
#123725,#123726,#123727,#123728,#123729,#123730,#123731,#123732,#123733),
 .UNSPECIFIED.,.F.,.F.,(4,3,3,3,3,3,3,3,3,3,4),(3.51711785548937E-10,0.113284432153487,
0.225129807988068,0.336301994397872,0.446993881464188,0.5,0.610566778230462,
0.721794516243209,0.833540970047342,0.946588755238846,1.),.UNSPECIFIED.);
#29627=B_SPLINE_CURVE_WITH_KNOTS('',3,(#123734,#123735,#123736,#123737,
#123738,#123739),.UNSPECIFIED.,.F.,.F.,(4,2,4),(0.,0.5,1.),
 .UNSPECIFIED.);
#29628=B_SPLINE_CURVE_WITH_KNOTS('',3,(#123810,#123811,#123812,#123813,
#123814,#123815,#123816,#123817,#123818,#123819,#123820,#123821,#123822,
#123823,#123824,#123825,#123826,#123827,#123828,#123829,#123830,#123831,
#123832,#123833,#123834,#123835,#123836,#123837,#123838,#123839,#123840,
#123841,#123842,#123843,#123844,#123845,#123846,#123847,#123848,#123849,
#123850,#123851,#123852,#123853,#123854,#123855,#123856,#123857,#123858,
#123859,#123860,#123861,#123862,#123863,#123864,#123865,#123866,#123867,
#123868,#123869,#123870,#123871,#123872,#123873,#123874,#123875,#123876,
#123877,#123878,#123879,#123880,#123881,#123882,#123883,#123884,#123885,
#123886,#123887,#123888,#123889,#123890,#123891,#123892,#123893,#123894,
#123895,#123896,#123897,#123898,#123899,#123900,#123901,#123902,#123903,
#123904,#123905,#123906,#123907,#123908,#123909),.UNSPECIFIED.,.F.,.F.,
(4,3,3,3,3,3,3,3,3,3,3,3,3,3,3,3,3,3,3,3,3,3,3,3,3,3,3,3,3,3,3,3,3,4),(0.,
0.0675516705121917,0.085904273434277,0.143599051494154,0.180074662513404,
0.232991527865125,0.25000000000006,0.263677503500483,0.304234548981259,
0.340135041073349,0.37500000000009,0.411897079421141,0.417227647478623,
0.437500000000106,0.468750000000114,0.484375000000117,0.492187500000118,
0.49283408507591,0.496093750000118,0.498046875000118,0.500000000000118,
0.549453116060544,0.580671458879676,0.630985226919279,0.669322200424887,
0.721053052147648,0.750000000000059,0.75885720396782,0.812757172953105,
0.849107112554098,0.90344480954754,0.939801610670112,0.995535258890343,
1.),.UNSPECIFIED.);
#29629=B_SPLINE_CURVE_WITH_KNOTS('',3,(#123913,#123914,#123915,#123916,
#123917,#123918,#123919,#123920,#123921,#123922,#123923,#123924,#123925,
#123926,#123927,#123928,#123929,#123930,#123931,#123932,#123933,#123934,
#123935,#123936,#123937,#123938,#123939,#123940,#123941,#123942,#123943,
#123944,#123945,#123946,#123947,#123948,#123949,#123950,#123951,#123952,
#123953,#123954,#123955,#123956,#123957,#123958,#123959,#123960,#123961,
#123962,#123963,#123964,#123965,#123966,#123967,#123968,#123969,#123970,
#123971,#123972,#123973,#123974,#123975,#123976,#123977,#123978,#123979,
#123980,#123981,#123982,#123983,#123984,#123985,#123986,#123987,#123988,
#123989,#123990,#123991,#123992,#123993,#123994,#123995,#123996,#123997,
#123998,#123999,#124000,#124001,#124002,#124003,#124004,#124005,#124006,
#124007,#124008,#124009),.UNSPECIFIED.,.F.,.F.,(4,3,3,3,3,3,3,3,3,3,3,3,
3,3,3,3,3,3,3,3,3,3,3,3,3,3,3,3,3,3,3,3,4),(1.13242242768556E-6,0.0650063186321231,
0.0987043254187582,0.1,0.146470218313343,0.192972087340009,0.2,0.213812109012698,
0.259692574051291,0.3,0.328657232220735,0.382282662717156,0.4,0.444122225894707,
0.488445076783722,0.5,0.549055659943903,0.559727753542975,0.6,0.634781863006224,
0.670535134136114,0.67404569477506,0.7,0.773428608298956,0.789454090675106,
0.8,0.8448500120543,0.888980980115078,0.9,0.904688768249668,0.949235840745,
0.992552407694861,1.),.UNSPECIFIED.);
#29630=B_SPLINE_CURVE_WITH_KNOTS('',3,(#124010,#124011,#124012,#124013,
#124014,#124015,#124016,#124017,#124018,#124019,#124020,#124021,#124022,
#124023,#124024,#124025,#124026,#124027,#124028,#124029,#124030,#124031,
#124032,#124033,#124034,#124035,#124036,#124037,#124038,#124039,#124040,
#124041,#124042,#124043,#124044,#124045,#124046,#124047,#124048,#124049,
#124050,#124051,#124052,#124053,#124054,#124055,#124056,#124057,#124058,
#124059,#124060,#124061,#124062,#124063,#124064,#124065,#124066,#124067,
#124068,#124069,#124070,#124071,#124072,#124073,#124074,#124075,#124076,
#124077,#124078,#124079,#124080,#124081,#124082,#124083,#124084,#124085,
#124086,#124087,#124088,#124089,#124090,#124091,#124092,#124093,#124094),
 .UNSPECIFIED.,.F.,.F.,(4,3,3,3,3,3,3,3,3,3,3,3,3,3,3,3,3,3,3,3,3,3,3,3,
3,3,3,3,4),(0.,0.0464234475031527,0.0972394848002348,0.124999999999925,
0.18293996388668,0.187499999999885,0.218749999999865,0.234374999999855,
0.242187499999853,0.246093749999855,0.249999999999857,0.312499999999872,
0.374999999999887,0.394398921641171,0.437499999999902,0.468749999999906,
0.484374999999908,0.495923412975398,0.49999999999991,0.569072679957118,
0.596914948823617,0.659857187217588,0.72408610632743,0.749999999999955,
0.79535387639268,0.860907736963063,0.93010399676668,0.998673877112228,0.999999999665933),
 .UNSPECIFIED.);
#29631=B_SPLINE_CURVE_WITH_KNOTS('',3,(#124143,#124144,#124145,#124146,
#124147,#124148,#124149,#124150,#124151,#124152,#124153,#124154,#124155,
#124156,#124157,#124158,#124159,#124160,#124161,#124162,#124163,#124164,
#124165,#124166,#124167,#124168,#124169,#124170,#124171,#124172,#124173,
#124174,#124175,#124176,#124177,#124178,#124179,#124180,#124181,#124182,
#124183,#124184,#124185,#124186,#124187,#124188,#124189,#124190,#124191,
#124192,#124193,#124194,#124195,#124196,#124197,#124198,#124199,#124200),
 .UNSPECIFIED.,.F.,.F.,(4,2,2,2,2,2,2,2,2,1,1,2,2,2,2,2,1,2,2,2,2,1,1,1,
2,2,2,2,2,2,2,4),(4.03773831338313E-9,0.125000000000036,0.187500000000054,
0.218750000000064,0.234375000000069,0.250000000000074,0.375000000000128,
0.437500000000155,0.468750000000169,0.484375000000176,0.492187500000179,
0.49609375000018,0.500000000000181,0.562500000000179,0.59375000000018,0.60156250000018,
0.609375000000181,0.62500000000018,0.656250000000178,0.671875000000176,
0.687500000000174,0.718750000000168,0.734375000000164,0.74218750000016,
0.746093750000158,0.750000000000155,0.812500000000121,0.820312500000117,
0.828125000000113,0.843750000000102,0.875000000000082,1.),.UNSPECIFIED.);
#29632=B_SPLINE_CURVE_WITH_KNOTS('',3,(#124263,#124264,#124265,#124266,
#124267,#124268,#124269,#124270,#124271,#124272),.UNSPECIFIED.,.F.,.F.,
(4,2,2,2,4),(-0.23344982273972,-0.179647450786024,-0.11659637991489,-0.0577031790998955,
-9.99999849621291E-7),.UNSPECIFIED.);
#29633=B_SPLINE_CURVE_WITH_KNOTS('',3,(#124273,#124274,#124275,#124276,
#124277,#124278,#124279,#124280,#124281,#124282,#124283,#124284,#124285,
#124286,#124287,#124288,#124289,#124290,#124291,#124292,#124293,#124294,
#124295,#124296,#124297,#124298,#124299,#124300,#124301,#124302,#124303,
#124304,#124305,#124306,#124307,#124308,#124309,#124310,#124311,#124312,
#124313,#124314,#124315,#124316,#124317,#124318,#124319,#124320,#124321,
#124322,#124323,#124324,#124325,#124326,#124327,#124328,#124329,#124330,
#124331,#124332,#124333,#124334,#124335,#124336,#124337,#124338,#124339,
#124340,#124341,#124342,#124343,#124344,#124345),.UNSPECIFIED.,.F.,.F.,
(4,3,3,3,3,3,3,3,3,3,3,3,3,3,3,3,3,3,3,3,3,3,3,3,4),(0.,0.12757222074774,
0.25000000000007,0.29760660917728,0.375000000000104,0.437500000000121,0.468750000000129,
0.484375000000132,0.492187500000134,0.496093750000137,0.500000000000139,
0.555888236349678,0.62500000000008,0.687500000000052,0.718750000000038,
0.734375000000033,0.742187500000031,0.74609375000003,0.750000000000029,
0.777889116176992,0.822699163900004,0.868116122275604,0.913783777296168,
0.959719246544919,1.),.UNSPECIFIED.);
#29634=B_SPLINE_CURVE_WITH_KNOTS('',3,(#124346,#124347,#124348,#124349,
#124350,#124351,#124352,#124353,#124354,#124355,#124356,#124357,#124358),
 .UNSPECIFIED.,.F.,.F.,(4,3,3,3,4),(0.,0.0494576143635624,0.0970068022307913,
0.1,0.12449382449223),.UNSPECIFIED.);
#29635=B_SPLINE_CURVE_WITH_KNOTS('',3,(#124366,#124367,#124368,#124369),
 .UNSPECIFIED.,.F.,.F.,(4,4),(0.,1.),.UNSPECIFIED.);
#29636=B_SPLINE_CURVE_WITH_KNOTS('',3,(#124370,#124371,#124372,#124373,
#124374,#124375,#124376,#124377,#124378,#124379,#124380,#124381,#124382,
#124383,#124384,#124385,#124386,#124387,#124388,#124389,#124390,#124391,
#124392,#124393,#124394,#124395,#124396,#124397,#124398,#124399,#124400,
#124401,#124402,#124403,#124404,#124405,#124406,#124407,#124408,#124409,
#124410,#124411,#124412,#124413,#124414,#124415,#124416,#124417,#124418),
 .UNSPECIFIED.,.F.,.F.,(4,3,3,3,3,3,3,3,3,3,3,3,3,3,3,3,4),(1.46675811174605E-9,
0.0686791264152932,0.136755536608584,0.20412240032792,0.25,0.3125,0.374509470854035,
0.437254735427017,0.5,0.5625,0.624427008921756,0.687213504460878,0.75,0.817395177031026,
0.885212462891086,0.953912866973348,1.),.UNSPECIFIED.);
#29637=B_SPLINE_CURVE_WITH_KNOTS('',3,(#124422,#124423,#124424,#124425,
#124426,#124427,#124428,#124429,#124430,#124431),.UNSPECIFIED.,.F.,.F.,
(4,2,2,2,4),(-0.726405805381144,-0.662305272963298,-0.598204740545452,-0.542164515818623,
-0.486124291091795),.UNSPECIFIED.);
#29638=B_SPLINE_CURVE_WITH_KNOTS('',3,(#124462,#124463,#124464,#124465,
#124466,#124467),.UNSPECIFIED.,.F.,.F.,(4,2,4),(0.,0.5,1.),
 .UNSPECIFIED.);
#29639=B_SPLINE_CURVE_WITH_KNOTS('',3,(#124535,#124536,#124537,#124538,
#124539,#124540,#124541,#124542,#124543,#124544,#124545,#124546,#124547,
#124548,#124549,#124550,#124551,#124552,#124553,#124554,#124555,#124556,
#124557,#124558,#124559,#124560,#124561,#124562,#124563,#124564,#124565,
#124566,#124567,#124568,#124569,#124570,#124571,#124572,#124573,#124574,
#124575,#124576,#124577,#124578,#124579,#124580),.UNSPECIFIED.,.F.,.F.,
(4,3,3,3,3,3,3,3,3,3,3,3,3,3,3,4),(0.,0.0589597084867831,0.119779732984347,
0.184889866492172,0.249999999999997,0.315933256860396,0.384199006139739,
0.437499999999991,0.466976182919735,0.496747691491063,0.499999999999988,
0.60353311268981,0.709573998306953,0.817048051970079,0.926891247804535,
0.999999998760338),.UNSPECIFIED.);
#29640=B_SPLINE_CURVE_WITH_KNOTS('',3,(#124581,#124582,#124583,#124584,
#124585,#124586,#124587,#124588,#124589,#124590,#124591,#124592,#124593,
#124594,#124595,#124596,#124597,#124598,#124599,#124600,#124601,#124602,
#124603,#124604,#124605,#124606,#124607,#124608,#124609,#124610,#124611,
#124612,#124613,#124614,#124615,#124616,#124617,#124618,#124619,#124620,
#124621,#124622,#124623,#124624,#124625,#124626,#124627,#124628,#124629,
#124630,#124631,#124632,#124633,#124634,#124635,#124636,#124637,#124638,
#124639,#124640,#124641,#124642,#124643,#124644,#124645,#124646,#124647,
#124648,#124649,#124650,#124651,#124652,#124653),.UNSPECIFIED.,.F.,.F.,
(4,3,3,3,3,3,3,3,3,3,3,3,3,3,3,3,3,3,3,3,3,3,3,3,4),(0.,0.0711144888714902,
0.0945275596457417,0.167636396974067,0.208716067427079,0.249999999999987,
0.320184542884328,0.374999999999986,0.431373619662498,0.437499999999988,
0.466325239000227,0.495576657133584,0.499999999999989,0.547812431517224,
0.611883700119326,0.663674500140904,0.722930038864494,0.749999999999994,
0.776562960482692,0.832323559435951,0.88400805595098,0.888084158389211,
0.939713999835979,0.99090756022988,1.),.UNSPECIFIED.);
#29641=B_SPLINE_CURVE_WITH_KNOTS('',3,(#124661,#124662,#124663,#124664,
#124665,#124666,#124667,#124668,#124669,#124670,#124671,#124672,#124673,
#124674,#124675,#124676,#124677,#124678,#124679,#124680,#124681,#124682,
#124683,#124684,#124685),.UNSPECIFIED.,.F.,.F.,(4,3,3,3,3,3,3,3,4),(0.,
0.0465847089982569,0.184218794802992,0.322341777280543,0.460351258074531,
0.592494069563406,0.725479240786321,0.862739620393161,1.),.UNSPECIFIED.);
#29642=B_SPLINE_CURVE_WITH_KNOTS('',3,(#124687,#124688,#124689,#124690,
#124691,#124692,#124693,#124694,#124695,#124696,#124697,#124698,#124699,
#124700,#124701,#124702,#124703,#124704,#124705),.UNSPECIFIED.,.F.,.F.,
(4,3,3,3,3,3,4),(3.48947356593272E-12,0.174977590683796,0.347502183077061,
0.516223131647767,0.682841488005358,0.846077647659188,1.),.UNSPECIFIED.);
#29643=B_SPLINE_CURVE_WITH_KNOTS('',3,(#124708,#124709,#124710,#124711,
#124712,#124713),.UNSPECIFIED.,.F.,.F.,(4,2,4),(2.51526495094515E-6,0.266858815172523,
0.535468336387855),.UNSPECIFIED.);
#29644=B_SPLINE_CURVE_WITH_KNOTS('',3,(#124719,#124720,#124721,#124722,
#124723,#124724),.UNSPECIFIED.,.F.,.F.,(4,2,4),(-0.194540442929235,-0.0972716515835901,
-9.99999999418133E-7),.UNSPECIFIED.);
#29645=B_SPLINE_CURVE_WITH_KNOTS('',3,(#124726,#124727,#124728,#124729,
#124730,#124731),.UNSPECIFIED.,.F.,.F.,(4,2,4),(-1.07453211284631,-0.509989083706148,
-4.22263312715382E-6),.UNSPECIFIED.);
#29646=B_SPLINE_CURVE_WITH_KNOTS('',3,(#124732,#124733,#124734,#124735,
#124736,#124737),.UNSPECIFIED.,.F.,.F.,(4,2,4),(-0.252023834669692,-0.127427092192949,
-2.00386101438639E-6),.UNSPECIFIED.);
#29647=B_SPLINE_CURVE_WITH_KNOTS('',3,(#124843,#124844,#124845,#124846,
#124847,#124848,#124849,#124850,#124851,#124852,#124853,#124854,#124855,
#124856,#124857,#124858,#124859,#124860,#124861,#124862,#124863,#124864,
#124865,#124866,#124867,#124868,#124869,#124870,#124871,#124872,#124873,
#124874,#124875,#124876,#124877,#124878,#124879,#124880,#124881,#124882,
#124883,#124884,#124885,#124886,#124887,#124888,#124889,#124890,#124891,
#124892,#124893,#124894,#124895,#124896,#124897,#124898,#124899,#124900,
#124901,#124902,#124903,#124904,#124905,#124906,#124907,#124908,#124909,
#124910,#124911,#124912,#124913,#124914,#124915,#124916,#124917,#124918,
#124919,#124920,#124921,#124922,#124923,#124924,#124925,#124926,#124927,
#124928,#124929,#124930,#124931,#124932,#124933,#124934,#124935,#124936,
#124937,#124938,#124939,#124940,#124941,#124942,#124943,#124944,#124945,
#124946,#124947,#124948,#124949,#124950,#124951,#124952,#124953,#124954,
#124955,#124956,#124957,#124958,#124959,#124960,#124961,#124962,#124963,
#124964,#124965,#124966,#124967,#124968,#124969,#124970,#124971,#124972,
#124973,#124974,#124975,#124976,#124977,#124978,#124979,#124980,#124981,
#124982,#124983,#124984,#124985,#124986,#124987,#124988,#124989,#124990,
#124991,#124992,#124993,#124994,#124995,#124996,#124997,#124998,#124999,
#125000,#125001,#125002,#125003,#125004,#125005),.UNSPECIFIED.,.F.,.F.,
(4,3,3,3,3,3,3,3,3,3,3,3,3,3,3,3,3,3,3,3,3,3,3,3,3,3,3,3,3,3,3,3,3,3,3,
3,3,3,3,3,3,3,3,3,3,3,3,3,3,3,3,3,3,3,4),(5.06083412936115E-12,0.0171539559720731,
0.0340650402423521,0.0505541415213171,0.0624999999999573,0.0696180872669653,
0.0855236320894016,0.100975672650675,0.109374999999926,0.117187499999921,
0.121093749999919,0.123046874999918,0.124023437499918,0.124999999999917,
0.13042801320028,0.15034045199903,0.17036742202076,0.190437495147897,0.198613274729677,
0.218301764397597,0.234374999999947,0.242187499999948,0.24609374999995,
0.248046874999951,0.249023437499951,0.24999999999995,0.28107801214436,0.322352060126167,
0.355872213215164,0.398801088383518,0.429267293437837,0.468749999999988,
0.48437499999999,0.49218749999999,0.49609374999999,0.499733967514589,0.499999999999991,
0.50367996751005,0.562817552938163,0.57466735513887,0.633872953101113,0.648359273799131,
0.687499999999987,0.718749999999986,0.725680974454021,0.734374999999985,
0.742187499999985,0.746093749999985,0.749999999999985,0.802396398205991,
0.856875204425067,0.877172016234362,0.932464864793394,0.951194936350549,
1.),.UNSPECIFIED.);
#29648=B_SPLINE_CURVE_WITH_KNOTS('',3,(#125050,#125051,#125052,#125053,
#125054,#125055,#125056,#125057),.UNSPECIFIED.,.F.,.F.,(4,1,1,1,1,4),(0.,
0.2,0.4,0.6,0.8,1.),.UNSPECIFIED.);
#29649=B_SPLINE_CURVE_WITH_KNOTS('',3,(#125058,#125059,#125060,#125061,
#125062,#125063,#125064,#125065,#125066,#125067,#125068,#125069,#125070,
#125071,#125072,#125073,#125074,#125075,#125076,#125077,#125078,#125079,
#125080,#125081,#125082,#125083,#125084,#125085,#125086,#125087,#125088),
 .UNSPECIFIED.,.F.,.F.,(4,3,3,3,3,3,3,3,3,3,4),(0.,0.136431436038453,0.269177825084775,
0.340888348203681,0.486556920879233,0.552216379427244,0.703562789808188,
0.762705775705736,0.91923339399344,0.967149486305342,0.999969191797008),
 .UNSPECIFIED.);
#29650=B_SPLINE_CURVE_WITH_KNOTS('',3,(#125198,#125199,#125200,#125201,
#125202,#125203,#125204,#125205,#125206,#125207,#125208,#125209,#125210,
#125211,#125212,#125213,#125214,#125215,#125216,#125217,#125218,#125219,
#125220,#125221,#125222,#125223,#125224,#125225,#125226,#125227,#125228,
#125229,#125230,#125231,#125232,#125233,#125234,#125235,#125236,#125237,
#125238,#125239,#125240,#125241,#125242,#125243,#125244,#125245,#125246,
#125247,#125248,#125249,#125250,#125251,#125252,#125253,#125254,#125255,
#125256,#125257,#125258,#125259,#125260,#125261,#125262,#125263,#125264,
#125265,#125266,#125267,#125268,#125269,#125270,#125271,#125272,#125273,
#125274,#125275,#125276,#125277,#125278,#125279,#125280,#125281,#125282,
#125283,#125284,#125285,#125286,#125287,#125288,#125289,#125290,#125291,
#125292,#125293,#125294,#125295,#125296,#125297,#125298,#125299,#125300),
 .UNSPECIFIED.,.F.,.F.,(4,3,3,3,3,3,3,3,3,3,3,3,3,3,3,3,3,3,3,3,3,3,3,3,
3,3,3,3,3,3,3,3,3,3,4),(0.,0.0548361818126014,0.06666666666667,0.069441502424314,
0.114564908225941,0.1333333333333,0.138885271670704,0.189448418695147,0.2,
0.208327253730071,0.259706436177619,0.2666666666667,0.277771362672896,0.330517828067452,
0.3333333333333,0.347212826950769,0.4,0.416644409960725,0.4666666666667,
0.486092163022652,0.5333333333333,0.555533216886878,0.6,0.624946427182303,
0.6666666666667,0.694406514328659,0.7333333333333,0.763870816800353,0.8,
0.833291783351506,0.8666666666667,0.902746432778773,0.9333333333333,0.9720818174012,
0.99999998908041),.UNSPECIFIED.);
#29651=B_SPLINE_CURVE_WITH_KNOTS('',3,(#125301,#125302,#125303,#125304,
#125305,#125306,#125307,#125308,#125309,#125310,#125311,#125312,#125313,
#125314,#125315,#125316,#125317,#125318,#125319,#125320,#125321,#125322,
#125323,#125324,#125325,#125326,#125327,#125328,#125329,#125330,#125331,
#125332,#125333,#125334,#125335,#125336,#125337,#125338,#125339,#125340,
#125341,#125342,#125343,#125344,#125345,#125346,#125347,#125348,#125349,
#125350,#125351,#125352,#125353,#125354,#125355,#125356,#125357,#125358,
#125359,#125360,#125361,#125362,#125363,#125364,#125365,#125366,#125367,
#125368,#125369,#125370,#125371,#125372,#125373,#125374,#125375,#125376,
#125377,#125378,#125379,#125380,#125381,#125382,#125383,#125384,#125385,
#125386,#125387,#125388,#125389,#125390,#125391,#125392,#125393,#125394,
#125395,#125396,#125397,#125398,#125399,#125400,#125401,#125402,#125403),
 .UNSPECIFIED.,.F.,.F.,(4,3,3,3,3,3,3,3,3,3,3,3,3,3,3,3,3,3,3,3,3,3,3,3,
3,3,3,3,3,3,3,3,3,3,4),(0.,0.0355393849942929,0.06666666666667,0.0694416969043181,
0.107940146958524,0.1333333333333,0.138885647269038,0.181937310148047,0.2,
0.208327299984056,0.254737431641626,0.2666666666667,0.277771268979535,0.326713057347023,
0.3333333333333,0.347212653366961,0.4,0.416644220166199,0.4666666666667,
0.486091967689304,0.5333333333333,0.555533081355431,0.6,0.624946070796763,
0.6666666666667,0.694405739054948,0.7333333333333,0.763869845720447,0.8,
0.833290765384722,0.8666666666667,0.902745177151871,0.9333333333333,0.972081604890996,
1.),.UNSPECIFIED.);
#29652=B_SPLINE_CURVE_WITH_KNOTS('',3,(#125510,#125511,#125512,#125513,
#125514,#125515,#125516,#125517,#125518,#125519,#125520,#125521,#125522,
#125523,#125524,#125525,#125526,#125527,#125528,#125529,#125530,#125531,
#125532,#125533,#125534,#125535,#125536,#125537,#125538,#125539,#125540,
#125541,#125542,#125543,#125544,#125545,#125546,#125547,#125548,#125549,
#125550,#125551,#125552,#125553,#125554,#125555,#125556,#125557,#125558,
#125559,#125560,#125561,#125562,#125563,#125564,#125565,#125566,#125567,
#125568,#125569,#125570,#125571,#125572,#125573,#125574,#125575,#125576,
#125577,#125578,#125579,#125580,#125581,#125582,#125583,#125584,#125585,
#125586,#125587,#125588,#125589,#125590,#125591,#125592,#125593,#125594,
#125595,#125596,#125597,#125598,#125599,#125600,#125601,#125602,#125603,
#125604,#125605,#125606,#125607,#125608,#125609,#125610,#125611,#125612,
#125613,#125614,#125615,#125616,#125617,#125618,#125619,#125620,#125621,
#125622,#125623,#125624,#125625,#125626,#125627,#125628,#125629,#125630,
#125631,#125632,#125633,#125634,#125635,#125636,#125637,#125638,#125639,
#125640,#125641,#125642,#125643,#125644,#125645,#125646,#125647,#125648,
#125649,#125650,#125651,#125652,#125653,#125654,#125655,#125656,#125657,
#125658,#125659,#125660,#125661,#125662,#125663,#125664,#125665,#125666,
#125667,#125668,#125669,#125670,#125671,#125672,#125673,#125674,#125675,
#125676,#125677,#125678,#125679,#125680,#125681,#125682,#125683,#125684),
 .UNSPECIFIED.,.F.,.F.,(4,3,3,3,3,3,3,3,3,3,3,3,3,3,3,3,3,3,3,3,3,3,3,3,
3,3,3,3,3,3,3,3,3,3,3,3,3,3,3,3,3,3,3,3,3,3,3,3,3,3,3,3,3,3,3,3,3,3,4),
(0.,0.0235492679861395,0.0472137911635587,0.0625000000000093,0.0822518681564539,
0.093750000000014,0.109375000000016,0.117187500000018,0.121093750000018,
0.124023437500019,0.125000000000019,0.154178375199939,0.178178863460657,
0.187500000000026,0.216538644948386,0.218750000000029,0.234375000000031,
0.242187500000032,0.246093750000032,0.249023437500033,0.250000000000033,
0.272786625660294,0.307326218844534,0.312500000000031,0.34375000000003,
0.359375000000029,0.367187500000029,0.367684567420504,0.374023437500029,
0.375000000000029,0.406250000000027,0.421875000000026,0.4310209687631,0.437500000000026,
0.464080358294731,0.500000000000023,0.531250000000021,0.54687500000002,
0.556871877293205,0.557630128037314,0.56250000000002,0.593750000000018,
0.610383926884643,0.625000000000017,0.653411097831424,0.687500000000013,
0.718750000000012,0.734375000000011,0.74218750000001,0.748042269832564,
0.749392484289949,0.75000000000001,0.795146546828096,0.840684774852451,
0.847431192599437,0.894737435067752,0.942043677536068,0.987527628774997,
0.999999716407811),.UNSPECIFIED.);
#29653=B_SPLINE_CURVE_WITH_KNOTS('',3,(#125686,#125687,#125688,#125689,
#125690,#125691,#125692,#125693,#125694,#125695,#125696,#125697,#125698,
#125699,#125700,#125701,#125702,#125703,#125704,#125705,#125706,#125707,
#125708,#125709,#125710,#125711,#125712,#125713,#125714,#125715,#125716,
#125717,#125718,#125719,#125720,#125721,#125722,#125723,#125724,#125725,
#125726,#125727,#125728,#125729,#125730,#125731,#125732,#125733,#125734,
#125735,#125736,#125737),.UNSPECIFIED.,.F.,.F.,(4,3,3,3,3,3,3,3,3,3,3,3,
3,3,3,3,3,4),(2.99130189936697E-13,0.126968394289133,0.249999999999985,
0.329706325480795,0.374999999999978,0.437499999999975,0.468749999999973,
0.484374999999973,0.492187499999972,0.498046874999972,0.499999999999971,
0.582586360741502,0.654012877805904,0.737251808022353,0.821597889449064,
0.907434469096319,0.933231048795402,1.),.UNSPECIFIED.);
#29654=B_SPLINE_CURVE_WITH_KNOTS('',3,(#125738,#125739,#125740,#125741,
#125742,#125743,#125744,#125745,#125746,#125747,#125748,#125749,#125750,
#125751,#125752,#125753,#125754,#125755,#125756,#125757,#125758,#125759,
#125760,#125761,#125762,#125763,#125764,#125765,#125766,#125767,#125768,
#125769,#125770,#125771,#125772,#125773,#125774,#125775,#125776,#125777,
#125778,#125779,#125780,#125781,#125782,#125783,#125784,#125785,#125786,
#125787,#125788,#125789,#125790,#125791,#125792,#125793,#125794,#125795,
#125796,#125797,#125798,#125799,#125800,#125801,#125802,#125803,#125804,
#125805,#125806,#125807,#125808,#125809,#125810,#125811,#125812,#125813,
#125814,#125815,#125816,#125817,#125818,#125819,#125820,#125821,#125822,
#125823,#125824,#125825,#125826,#125827,#125828,#125829,#125830,#125831,
#125832,#125833,#125834,#125835,#125836,#125837,#125838,#125839,#125840),
 .UNSPECIFIED.,.F.,.F.,(4,3,3,3,3,3,3,3,3,3,3,3,3,3,3,3,3,3,3,3,3,3,3,3,
3,3,3,3,3,3,3,3,3,3,4),(0.,0.0624999999999969,0.0937499999999951,0.109374999999994,
0.117187499999994,0.121093749999994,0.123046874999994,0.123242106419626,
0.124999999999993,0.163746701278836,0.20166480609802,0.218750000000004,
0.234375000000005,0.242187500000006,0.246093750000006,0.248046875000006,
0.250000000000006,0.290663556421084,0.352736974639709,0.415434775032593,
0.4375,0.468749999999998,0.478234768091092,0.484374999999998,0.492187499999998,
0.496093749999998,0.499999999999998,0.579044129469348,0.657254873091502,
0.674737829808071,0.749999999999999,0.828546295365536,0.889501455477367,
0.968672694605542,1.),.UNSPECIFIED.);
#29655=B_SPLINE_CURVE_WITH_KNOTS('',3,(#125899,#125900,#125901,#125902,
#125903,#125904,#125905,#125906,#125907,#125908,#125909,#125910,#125911,
#125912,#125913,#125914,#125915,#125916,#125917,#125918,#125919,#125920,
#125921,#125922,#125923,#125924,#125925,#125926,#125927,#125928,#125929,
#125930),.UNSPECIFIED.,.F.,.F.,(4,1,1,1,1,1,1,1,1,1,1,1,1,1,1,1,1,1,1,1,
1,1,1,1,1,1,1,1,1,4),(0.,0.0268581202847227,0.053576525889946,0.0801578745940373,
0.106606641707507,0.132924195530782,0.159110310690199,0.185166065577177,
0.211093744297133,0.236896651377879,0.262577255427033,0.288136464224189,
0.313575794895345,0.338897466804712,0.364104280017708,0.389198781870568,
0.414183265290867,0.439060365533827,0.463833043802139,0.495403201210392,
0.587316390229939,0.642835451771974,0.704686515759081,0.772883347569249,
0.814032578447846,0.853827591278796,0.892297474609331,0.929469891075696,
0.965365253976918,1.),.UNSPECIFIED.);
#29656=B_SPLINE_CURVE_WITH_KNOTS('',3,(#126050,#126051,#126052,#126053,
#126054,#126055,#126056,#126057,#126058,#126059,#126060,#126061,#126062,
#126063,#126064,#126065),.UNSPECIFIED.,.F.,.F.,(4,3,3,3,3,4),(0.,0.221610690796373,
0.437664957226359,0.651285519899787,0.862133513064776,0.999985703601229),
 .UNSPECIFIED.);
#29657=B_SPLINE_CURVE_WITH_KNOTS('',3,(#126125,#126126,#126127,#126128,
#126129,#126130,#126131,#126132,#126133,#126134,#126135,#126136,#126137,
#126138,#126139,#126140,#126141,#126142,#126143,#126144,#126145,#126146,
#126147,#126148,#126149,#126150,#126151,#126152,#126153,#126154,#126155,
#126156,#126157,#126158,#126159,#126160,#126161,#126162,#126163,#126164,
#126165,#126166,#126167,#126168,#126169,#126170,#126171,#126172,#126173,
#126174,#126175,#126176,#126177,#126178,#126179,#126180,#126181,#126182,
#126183,#126184,#126185,#126186,#126187,#126188,#126189,#126190,#126191,
#126192,#126193,#126194,#126195,#126196,#126197,#126198,#126199,#126200,
#126201,#126202,#126203,#126204,#126205,#126206,#126207,#126208,#126209,
#126210,#126211,#126212),.UNSPECIFIED.,.F.,.F.,(4,3,3,3,3,3,3,3,3,3,3,3,
3,3,3,3,3,3,3,3,3,3,3,3,3,3,3,3,3,4),(0.,1.36955922228348E-5,0.0462209864660522,
0.0923085477371591,0.138396109008266,0.249999999999993,0.275014435602624,
0.344752712976046,0.414490990349467,0.437499999999987,0.468749999999986,
0.484374999999986,0.492187499999986,0.496093749999986,0.499999999999987,
0.552744721211975,0.620122360605994,0.687500000000013,0.691683644659851,
0.718750000000017,0.73437500000002,0.742187500000021,0.748046875000022,
0.750000000000022,0.813958948873022,0.829406161009669,0.895045917261246,
0.957116251376177,0.972386509597121,0.999999999927525),.UNSPECIFIED.);
#29658=B_SPLINE_CURVE_WITH_KNOTS('',3,(#126232,#126233,#126234,#126235,
#126236,#126237,#126238,#126239,#126240,#126241,#126242,#126243,#126244,
#126245,#126246,#126247,#126248,#126249,#126250,#126251,#126252,#126253,
#126254,#126255,#126256,#126257,#126258,#126259,#126260,#126261,#126262,
#126263,#126264,#126265,#126266,#126267,#126268,#126269,#126270,#126271,
#126272,#126273,#126274,#126275,#126276,#126277,#126278,#126279,#126280,
#126281,#126282,#126283,#126284,#126285,#126286,#126287,#126288,#126289,
#126290,#126291,#126292,#126293,#126294,#126295,#126296,#126297,#126298,
#126299,#126300,#126301,#126302,#126303,#126304,#126305,#126306,#126307,
#126308,#126309,#126310,#126311,#126312,#126313,#126314,#126315,#126316,
#126317,#126318,#126319,#126320,#126321,#126322,#126323,#126324,#126325,
#126326,#126327,#126328,#126329,#126330,#126331,#126332,#126333,#126334,
#126335,#126336,#126337,#126338,#126339,#126340,#126341,#126342,#126343,
#126344,#126345,#126346,#126347,#126348,#126349,#126350,#126351,#126352,
#126353,#126354,#126355),.UNSPECIFIED.,.F.,.F.,(4,3,3,3,3,3,3,3,3,3,3,3,
3,3,3,3,3,3,3,3,3,3,3,3,3,3,3,3,3,3,3,3,3,3,3,3,3,3,3,3,3,4),(0.,0.0340829424126167,
0.0691949614776787,0.105776364582913,0.117363353323133,0.125000000000056,
0.160169501196136,0.187500000000084,0.218750000000098,0.234375000000105,
0.242187500000108,0.246093750000108,0.250000000000108,0.285436053496591,
0.309021515795873,0.343531233663922,0.378569260057507,0.413942671359278,
0.44921700327509,0.483961412343902,0.500000000000092,0.500003316427969,
0.534823892860835,0.570002258034842,0.605300618146352,0.625000000000085,
0.659693928278741,0.68750000000008,0.691017580435165,0.718750000000077,
0.734375000000075,0.742187500000074,0.746093750000073,0.750000000000071,
0.787162851469644,0.823724950689069,0.8590520932407,0.882627289955567,0.918401461247141,
0.953211128280996,0.986563735801074,1.),.UNSPECIFIED.);
#29659=B_SPLINE_CURVE_WITH_KNOTS('',3,(#126358,#126359,#126360,#126361,
#126362,#126363,#126364,#126365,#126366,#126367,#126368,#126369,#126370,
#126371),.UNSPECIFIED.,.F.,.F.,(4,2,2,1,1,2,2,4),(0.,0.249999999999985,
0.37499999999998,0.437499999999977,0.468749999999975,0.484374999999977,
0.499999999999978,0.999999993863134),.UNSPECIFIED.);
#29660=B_SPLINE_CURVE_WITH_KNOTS('',3,(#126373,#126374,#126375,#126376,
#126377,#126378,#126379,#126380,#126381,#126382,#126383,#126384,#126385,
#126386),.UNSPECIFIED.,.F.,.F.,(4,2,2,1,1,2,2,4),(0.,0.249999999999981,
0.37499999999997,0.437499999999966,0.468749999999966,0.484374999999966,
0.499999999999966,1.),.UNSPECIFIED.);
#29661=B_SPLINE_CURVE_WITH_KNOTS('',3,(#126390,#126391,#126392,#126393,
#126394,#126395,#126396,#126397,#126398,#126399,#126400,#126401,#126402,
#126403,#126404,#126405,#126406,#126407,#126408),.UNSPECIFIED.,.F.,.F.,
(4,3,3,3,3,3,4),(0.,0.250000000000009,0.375000000000016,0.437500000000016,
0.500000000000016,0.753487667768314,1.),.UNSPECIFIED.);
#29662=B_SPLINE_CURVE_WITH_KNOTS('',3,(#126412,#126413,#126414,#126415,
#126416,#126417,#126418,#126419,#126420,#126421,#126422,#126423,#126424,
#126425,#126426,#126427,#126428,#126429,#126430,#126431,#126432,#126433,
#126434,#126435,#126436,#126437,#126438,#126439,#126440,#126441,#126442,
#126443,#126444,#126445,#126446,#126447,#126448,#126449,#126450,#126451,
#126452,#126453,#126454,#126455,#126456,#126457,#126458,#126459,#126460,
#126461,#126462,#126463,#126464,#126465,#126466,#126467,#126468,#126469,
#126470,#126471,#126472,#126473,#126474,#126475,#126476,#126477,#126478,
#126479,#126480,#126481,#126482,#126483,#126484,#126485,#126486,#126487,
#126488,#126489,#126490,#126491,#126492,#126493,#126494,#126495,#126496,
#126497,#126498,#126499,#126500,#126501,#126502,#126503,#126504,#126505,
#126506,#126507,#126508,#126509,#126510,#126511,#126512,#126513,#126514,
#126515,#126516,#126517,#126518,#126519,#126520,#126521,#126522,#126523,
#126524,#126525,#126526,#126527,#126528,#126529,#126530,#126531,#126532),
 .UNSPECIFIED.,.F.,.F.,(4,3,3,3,3,3,3,3,3,3,3,3,3,3,3,3,3,3,3,3,3,3,3,3,
3,3,3,3,3,3,3,3,3,3,3,3,3,3,3,3,4),(1.35350574291754E-11,0.0307091849465562,
0.0778545924732743,0.124999999999992,0.155534322638056,0.18749999999999,
0.218749999999991,0.234374999999991,0.2452894568283,0.249999999999992,0.280109082038762,
0.327554541019382,0.375000000000003,0.40543633558073,0.437500000000006,
0.468750000000008,0.48437500000001,0.492187500000014,0.496093750000014,
0.498046875000011,0.500000000000009,0.525870094542647,0.579929503357328,
0.624999999999902,0.644130534816122,0.687499999999847,0.718749999999819,
0.734374999999805,0.742187499999796,0.74609374999979,0.749023437499785,
0.749999999999784,0.77607790488667,0.805973888385761,0.836642472345653,
0.868991593120488,0.895661838883031,0.927139320876192,0.960297481709551,
0.995806785180928,0.999999984939203),.UNSPECIFIED.);
#29663=B_SPLINE_CURVE_WITH_KNOTS('',3,(#126534,#126535,#126536,#126537,
#126538,#126539,#126540,#126541,#126542,#126543,#126544,#126545,#126546,
#126547,#126548,#126549,#126550,#126551,#126552,#126553),.UNSPECIFIED.,
 .F.,.F.,(4,2,2,2,1,1,1,1,2,2,2,4),(0.,0.249999999999962,0.374999999999941,
0.437499999999932,0.468749999999929,0.484374999999928,0.492187499999926,
0.496093749999923,0.49804687499992,0.499999999999918,0.749999999999959,
1.),.UNSPECIFIED.);
#29664=B_SPLINE_CURVE_WITH_KNOTS('',3,(#126556,#126557,#126558,#126559,
#126560,#126561,#126562,#126563,#126564,#126565,#126566,#126567,#126568,
#126569,#126570,#126571,#126572,#126573,#126574),.UNSPECIFIED.,.F.,.F.,
(4,3,3,3,3,3,4),(0.,0.249999999999981,0.374999999999971,0.43749999999997,
0.499999999999968,0.749999999760635,0.999999999521302),.UNSPECIFIED.);
#29665=B_SPLINE_CURVE_WITH_KNOTS('',3,(#126619,#126620,#126621,#126622,
#126623,#126624,#126625,#126626,#126627,#126628),.UNSPECIFIED.,.F.,.F.,
(4,2,2,2,4),(0.,0.25,0.5,0.75,1.),.UNSPECIFIED.);
#29666=B_SPLINE_CURVE_WITH_KNOTS('',3,(#126629,#126630,#126631,#126632,
#126633,#126634,#126635,#126636,#126637,#126638,#126639,#126640,#126641,
#126642,#126643,#126644,#126645,#126646,#126647,#126648,#126649,#126650,
#126651,#126652,#126653),.UNSPECIFIED.,.F.,.F.,(4,2,2,2,2,2,2,1,1,1,2,2,
2,4),(0.,0.125000000000013,0.187500000000021,0.250000000000029,0.375000000000041,
0.437500000000047,0.468750000000048,0.48437500000005,0.492187500000048,
0.49609375000005,0.498046875000053,0.500000000000057,0.750000000000028,
1.),.UNSPECIFIED.);
#29667=B_SPLINE_CURVE_WITH_KNOTS('',3,(#126735,#126736,#126737,#126738,
#126739,#126740,#126741,#126742,#126743,#126744,#126745,#126746,#126747,
#126748,#126749,#126750,#126751,#126752,#126753,#126754,#126755,#126756,
#126757,#126758,#126759,#126760,#126761,#126762,#126763,#126764,#126765,
#126766,#126767,#126768,#126769,#126770,#126771,#126772,#126773,#126774,
#126775,#126776,#126777,#126778,#126779,#126780,#126781,#126782,#126783,
#126784,#126785,#126786,#126787,#126788,#126789,#126790,#126791,#126792,
#126793,#126794,#126795,#126796,#126797,#126798,#126799,#126800,#126801,
#126802,#126803,#126804,#126805,#126806,#126807,#126808,#126809,#126810,
#126811,#126812,#126813,#126814,#126815,#126816,#126817,#126818,#126819,
#126820,#126821,#126822,#126823,#126824,#126825,#126826,#126827,#126828,
#126829,#126830,#126831,#126832,#126833,#126834,#126835,#126836,#126837,
#126838,#126839,#126840,#126841,#126842,#126843,#126844,#126845,#126846,
#126847,#126848,#126849,#126850,#126851,#126852,#126853,#126854,#126855,
#126856,#126857,#126858,#126859,#126860,#126861,#126862,#126863,#126864,
#126865,#126866,#126867,#126868,#126869,#126870,#126871,#126872,#126873,
#126874,#126875,#126876,#126877,#126878,#126879,#126880,#126881,#126882,
#126883,#126884,#126885,#126886,#126887,#126888,#126889,#126890,#126891,
#126892,#126893,#126894,#126895,#126896,#126897,#126898,#126899,#126900,
#126901,#126902,#126903,#126904,#126905,#126906,#126907,#126908,#126909,
#126910,#126911,#126912,#126913,#126914,#126915,#126916,#126917,#126918,
#126919,#126920,#126921,#126922,#126923,#126924,#126925,#126926,#126927,
#126928,#126929,#126930,#126931,#126932,#126933,#126934,#126935,#126936,
#126937,#126938,#126939,#126940,#126941,#126942,#126943,#126944,#126945,
#126946,#126947,#126948),.UNSPECIFIED.,.F.,.F.,(4,3,3,3,3,3,3,3,3,3,3,3,
3,3,3,3,3,3,3,3,3,3,3,3,3,3,3,3,3,3,3,3,3,3,3,3,3,3,3,3,3,3,3,3,3,3,3,3,
3,3,3,3,3,3,3,3,3,3,3,3,3,3,3,3,3,3,3,3,3,3,3,4),(0.,0.0282178331377545,
0.0561330259963789,0.0834964584640116,0.105856518636603,0.124999999999945,
0.157071974609684,0.187499999999919,0.203569253523847,0.218749999999905,
0.234374999999898,0.242187499999895,0.246093749999893,0.248046874999891,
0.249755859374893,0.249999999999893,0.267047585275722,0.284291037965404,
0.30185817244769,0.308180029008359,0.31249999999989,0.328204075134219,0.344328892806464,
0.348280256700363,0.364286610611002,0.374999999999886,0.388280152658778,
0.404495028033477,0.421258823707265,0.435513775269351,0.437499999999883,
0.454742790478908,0.468749999999881,0.484374999999881,0.490871007459825,
0.492187499999882,0.496093749999883,0.49909253482406,0.499999999999883,
0.518016063137528,0.535457441797552,0.545566661066867,0.562499999999891,
0.579018449955007,0.5921657794438,0.608582889721849,0.624999999999898,0.635193611489272,
0.651282564283057,0.666884015919654,0.679131883867457,0.687499999999906,
0.704012137647359,0.71874999999991,0.724717457344516,0.734374999999912,
0.742187499999913,0.746093749999914,0.748046874999915,0.749023437499915,
0.749755859374914,0.749999999999914,0.776532649485828,0.78835186737661,
0.818021368597962,0.848252842493185,0.874999999999957,0.891177430866168,
0.918383073149626,0.945148095559187,0.972574047779593,0.999999999999999),
 .UNSPECIFIED.);
#29668=B_SPLINE_CURVE_WITH_KNOTS('',3,(#126975,#126976,#126977,#126978,
#126979,#126980,#126981,#126982,#126983,#126984,#126985,#126986,#126987,
#126988,#126989,#126990,#126991,#126992,#126993,#126994,#126995,#126996,
#126997,#126998,#126999,#127000,#127001,#127002,#127003,#127004,#127005,
#127006,#127007,#127008,#127009,#127010,#127011,#127012,#127013,#127014,
#127015,#127016,#127017,#127018,#127019,#127020,#127021,#127022,#127023,
#127024,#127025,#127026,#127027,#127028,#127029,#127030,#127031,#127032),
 .UNSPECIFIED.,.F.,.F.,(4,3,3,3,3,3,3,3,3,3,3,3,3,3,3,3,3,3,3,4),(2.46876960649128E-9,
0.0537367748554289,0.107910543359844,0.162445165998166,0.217710133013511,
0.25,0.304280929502245,0.325898769308603,0.382277994389015,0.441138997194507,
0.5,0.565029573834012,0.631575019684094,0.701212572652556,0.727536024996926,
0.75,0.829317054604299,0.908964390223096,0.988919926273896,1.),
 .UNSPECIFIED.);
#29669=B_SPLINE_CURVE_WITH_KNOTS('',3,(#127059,#127060,#127061,#127062,
#127063,#127064,#127065,#127066,#127067,#127068,#127069,#127070,#127071,
#127072,#127073,#127074,#127075,#127076,#127077,#127078,#127079,#127080,
#127081,#127082,#127083,#127084,#127085,#127086,#127087,#127088,#127089,
#127090,#127091,#127092,#127093,#127094,#127095,#127096,#127097,#127098,
#127099,#127100,#127101,#127102,#127103,#127104,#127105,#127106,#127107,
#127108,#127109,#127110,#127111,#127112,#127113,#127114,#127115,#127116,
#127117,#127118,#127119),.UNSPECIFIED.,.F.,.F.,(4,3,3,3,3,3,3,3,3,3,3,3,
3,3,3,3,3,3,3,3,4),(0.,0.0796513800767319,0.159044881296861,0.237895722259121,
0.25,0.280665700157712,0.349440429576461,0.416025348655478,0.480364738776273,
0.5,0.557540039378102,0.614137632699517,0.669697924521297,0.689732568620921,
0.743461700114881,0.75,0.805599575422341,0.860273458499742,0.914519873462587,
0.968307205903025,1.),.UNSPECIFIED.);
#29670=B_SPLINE_CURVE_WITH_KNOTS('',3,(#127146,#127147,#127148,#127149,
#127150,#127151,#127152,#127153,#127154,#127155,#127156),.UNSPECIFIED.,
 .F.,.F.,(4,1,1,1,1,1,1,1,4),(0.,0.125,0.25,0.375,0.5,0.625,0.75,0.875,
1.),.UNSPECIFIED.);
#29671=B_SPLINE_CURVE_WITH_KNOTS('',3,(#127207,#127208,#127209,#127210,
#127211,#127212,#127213,#127214,#127215,#127216,#127217,#127218,#127219,
#127220,#127221,#127222,#127223,#127224,#127225,#127226,#127227,#127228,
#127229,#127230,#127231,#127232,#127233,#127234,#127235,#127236,#127237,
#127238,#127239,#127240,#127241,#127242,#127243,#127244,#127245,#127246,
#127247,#127248,#127249,#127250,#127251,#127252,#127253,#127254,#127255,
#127256,#127257,#127258,#127259,#127260,#127261,#127262,#127263,#127264,
#127265,#127266,#127267,#127268,#127269,#127270,#127271,#127272,#127273,
#127274,#127275,#127276,#127277,#127278,#127279,#127280,#127281,#127282,
#127283,#127284,#127285,#127286,#127287,#127288,#127289,#127290,#127291,
#127292,#127293,#127294,#127295,#127296,#127297,#127298,#127299,#127300,
#127301,#127302,#127303,#127304,#127305,#127306,#127307,#127308,#127309,
#127310,#127311,#127312,#127313,#127314,#127315,#127316,#127317,#127318,
#127319,#127320,#127321,#127322,#127323,#127324,#127325,#127326,#127327,
#127328,#127329,#127330,#127331,#127332,#127333,#127334,#127335,#127336,
#127337,#127338,#127339,#127340,#127341,#127342,#127343,#127344,#127345,
#127346,#127347,#127348,#127349,#127350,#127351,#127352,#127353,#127354,
#127355,#127356,#127357),.UNSPECIFIED.,.F.,.F.,(4,3,3,3,3,3,3,3,3,3,3,3,
3,3,3,3,3,3,3,3,3,3,3,3,3,3,3,3,3,3,3,3,3,3,3,3,3,3,3,3,3,3,3,3,3,3,3,3,
3,3,4),(3.37531681360733E-8,0.017205386283455,0.0344007668864576,0.0514925949099461,
0.0625000000003226,0.0788325765450556,0.093750000000486,0.109375000000568,
0.117187500000608,0.121093750000628,0.123046875000637,0.124023437500642,
0.124511718750645,0.125000000000647,0.132155380101528,0.154901536392429,
0.177338716362301,0.187500000000683,0.209154443768504,0.218750000000699,
0.234375000000707,0.242187500000711,0.246093750000714,0.248046875000715,
0.250000000000715,0.275941425824807,0.321226396871429,0.367758215452313,
0.375000000000597,0.401097960541236,0.437500000000536,0.468750000000505,
0.484375000000489,0.494714665161877,0.500000000000472,0.532447775598141,
0.586688269433701,0.638600054374137,0.652704130622242,0.701352065311238,
0.750000000000234,0.769959744739266,0.808596168225151,0.845577084750668,
0.875000000000117,0.879285832015869,0.909685991152717,0.939197353512371,
0.96748243414976,0.977540640360751,1.),.UNSPECIFIED.);
#29672=B_SPLINE_CURVE_WITH_KNOTS('',3,(#127392,#127393,#127394,#127395,
#127396,#127397,#127398,#127399,#127400,#127401,#127402,#127403,#127404,
#127405,#127406,#127407,#127408,#127409,#127410,#127411,#127412,#127413,
#127414,#127415,#127416,#127417,#127418,#127419,#127420,#127421,#127422,
#127423,#127424),.UNSPECIFIED.,.F.,.F.,(4,2,2,2,1,1,1,1,2,2,2,2,2,1,1,1,
2,2,2,4),(0.,0.250000000000239,0.375000000000361,0.437500000000424,0.468750000000454,
0.484375000000468,0.492187500000475,0.49609375000048,0.499023437500488,
0.500000000000492,0.625000000000438,0.687500000000413,0.7187500000004,0.734375000000394,
0.742187500000391,0.746093750000391,0.748046875000389,0.750000000000388,
0.875000000000194,1.),.UNSPECIFIED.);
#29673=B_SPLINE_CURVE_WITH_KNOTS('',3,(#127449,#127450,#127451,#127452,
#127453,#127454,#127455,#127456,#127457,#127458,#127459,#127460,#127461,
#127462,#127463,#127464,#127465,#127466,#127467,#127468,#127469,#127470,
#127471,#127472,#127473,#127474,#127475,#127476,#127477,#127478,#127479,
#127480,#127481,#127482,#127483,#127484,#127485,#127486,#127487,#127488),
 .UNSPECIFIED.,.F.,.F.,(4,3,3,3,3,3,3,3,3,3,3,3,3,4),(6.02213740706731E-7,
0.18780417571379,0.250000000000018,0.279295317709131,0.375000000000028,
0.437500000000024,0.468750000000018,0.493606973159941,0.500000000000012,
0.628564160145021,0.732916122017548,0.858621496952094,0.982199270722659,
1.),.UNSPECIFIED.);
#29674=B_SPLINE_CURVE_WITH_KNOTS('',3,(#127560,#127561,#127562,#127563,
#127564,#127565,#127566,#127567,#127568,#127569,#127570,#127571,#127572,
#127573,#127574,#127575,#127576,#127577,#127578,#127579,#127580,#127581,
#127582,#127583,#127584,#127585,#127586,#127587,#127588,#127589,#127590,
#127591,#127592,#127593,#127594,#127595,#127596,#127597,#127598,#127599,
#127600,#127601,#127602,#127603,#127604,#127605,#127606,#127607,#127608,
#127609,#127610,#127611,#127612,#127613,#127614,#127615,#127616,#127617,
#127618,#127619,#127620,#127621,#127622,#127623,#127624,#127625,#127626,
#127627,#127628,#127629,#127630,#127631,#127632,#127633,#127634,#127635,
#127636,#127637,#127638,#127639,#127640,#127641,#127642,#127643,#127644),
 .UNSPECIFIED.,.F.,.F.,(4,3,3,3,3,3,3,3,3,3,3,3,3,3,3,3,3,3,3,3,3,3,3,3,
3,3,3,3,4),(4.27405454084845E-15,0.0377356474346085,0.0750359183061167,
0.112014973382717,0.148784553462517,0.185454708791789,0.222134505689713,
0.259084364535886,0.296281779750846,0.333825646041853,0.371816608292509,
0.410693571800077,0.450151209830871,0.490604164912764,0.499999883639221,
0.540309510288622,0.579736856800223,0.618411911999041,0.656459211909535,
0.693998732295002,0.732248890758127,0.769066832852564,0.805766270350655,
0.842443980674244,0.879196581460098,0.916274247721184,0.953595787795862,
0.991423223558937,1.),.UNSPECIFIED.);
#29675=B_SPLINE_CURVE_WITH_KNOTS('',3,(#127969,#127970,#127971,#127972,
#127973,#127974,#127975,#127976,#127977,#127978,#127979,#127980,#127981,
#127982,#127983,#127984,#127985,#127986),.UNSPECIFIED.,.F.,.F.,(4,2,2,2,
2,2,2,2,4),(0.,0.125,0.25,0.375,0.5,0.625,0.75,0.875,1.),.UNSPECIFIED.);
#29676=B_SPLINE_CURVE_WITH_KNOTS('',3,(#128290,#128291,#128292,#128293,
#128294,#128295,#128296,#128297,#128298,#128299,#128300,#128301,#128302,
#128303,#128304,#128305,#128306,#128307),.UNSPECIFIED.,.F.,.F.,(4,2,2,2,
2,2,2,2,4),(0.,0.125,0.25,0.375,0.5,0.625,0.75,0.875,1.),.UNSPECIFIED.);
#29677=B_SPLINE_CURVE_WITH_KNOTS('',3,(#128441,#128442,#128443,#128444,
#128445,#128446,#128447,#128448,#128449,#128450,#128451,#128452,#128453,
#128454,#128455,#128456,#128457,#128458,#128459,#128460,#128461,#128462,
#128463,#128464,#128465,#128466,#128467,#128468,#128469,#128470,#128471,
#128472,#128473,#128474,#128475,#128476,#128477,#128478,#128479,#128480,
#128481,#128482,#128483,#128484,#128485,#128486,#128487,#128488,#128489,
#128490,#128491,#128492,#128493,#128494,#128495,#128496,#128497,#128498,
#128499,#128500,#128501,#128502,#128503,#128504,#128505,#128506,#128507,
#128508,#128509,#128510,#128511,#128512,#128513,#128514,#128515,#128516,
#128517,#128518,#128519,#128520,#128521,#128522),.UNSPECIFIED.,.F.,.F.,
(4,3,3,3,3,3,3,3,3,3,3,3,3,3,3,3,3,3,3,3,3,3,3,3,3,3,3,4),(0.,0.0394358656769841,
0.0785691055717362,0.11744545980691,0.125,0.163728602867978,0.203692449020046,
0.242758028571359,0.282103574403945,0.321833855203582,0.362445642816848,
0.403594461611848,0.445876068134623,0.483439372084522,0.52606025705519,
0.569677724923291,0.610226588911753,0.650200831769538,0.689710220697424,
0.728861943519438,0.767724842093286,0.806475376386791,0.84527239412539,
0.875,0.914134277322075,0.953517865253058,0.993412874544988,1.),
 .UNSPECIFIED.);
#29678=B_SPLINE_CURVE_WITH_KNOTS('',3,(#128609,#128610,#128611,#128612,
#128613,#128614,#128615,#128616,#128617,#128618,#128619,#128620,#128621,
#128622),.UNSPECIFIED.,.F.,.F.,(4,2,2,2,2,2,4),(-1.00304124093577,-0.900314725496988,
-0.794873156144138,-0.612050855402291,-0.374992741653492,-0.188195460796421,
-0.000330903306112853),.UNSPECIFIED.);
#29679=B_SPLINE_CURVE_WITH_KNOTS('',3,(#128624,#128625,#128626,#128627,
#128628,#128629,#128630,#128631,#128632,#128633),.UNSPECIFIED.,.F.,.F.,
(4,2,2,2,4),(-0.66037468527763,-0.531312380184094,-0.402225004171424,-0.237342302443342,
-0.00010611583071703),.UNSPECIFIED.);
#29680=B_SPLINE_CURVE_WITH_KNOTS('',3,(#128634,#128635,#128636,#128637,
#128638,#128639,#128640,#128641,#128642,#128643,#128644,#128645,#128646,
#128647),.UNSPECIFIED.,.F.,.F.,(4,2,2,2,2,2,4),(-1.42617023783195,-1.24379379176015,
-1.06262174742879,-0.713770494942383,-0.373736089754977,-0.185591640376111,
-0.00031726611114529),.UNSPECIFIED.);
#29681=B_SPLINE_CURVE_WITH_KNOTS('',3,(#128693,#128694,#128695,#128696,
#128697,#128698,#128699,#128700,#128701,#128702,#128703,#128704,#128705,
#128706,#128707,#128708,#128709,#128710,#128711,#128712,#128713,#128714,
#128715,#128716,#128717,#128718,#128719,#128720),.UNSPECIFIED.,.F.,.F.,
(4,2,2,2,2,2,2,2,2,2,2,2,2,4),(2.58033318348083E-7,0.125000000000001,0.250000000000002,
0.281250000000002,0.312500000000001,0.437499999999999,0.499999999999998,
0.593749999999996,0.624999999999996,0.749999999999997,0.874999999999998,
0.906249999999999,0.937499999999999,0.999953591056302),.UNSPECIFIED.);
#29682=B_SPLINE_CURVE_WITH_KNOTS('',3,(#128800,#128801,#128802,#128803,
#128804,#128805,#128806,#128807,#128808,#128809,#128810,#128811,#128812,
#128813,#128814,#128815,#128816,#128817,#128818,#128819,#128820,#128821,
#128822,#128823,#128824,#128825,#128826,#128827,#128828,#128829,#128830,
#128831,#128832,#128833,#128834,#128835,#128836,#128837,#128838,#128839,
#128840,#128841,#128842,#128843,#128844,#128845,#128846,#128847,#128848,
#128849,#128850,#128851,#128852,#128853,#128854,#128855,#128856,#128857,
#128858,#128859,#128860,#128861,#128862,#128863,#128864,#128865,#128866,
#128867,#128868,#128869,#128870,#128871,#128872,#128873),.UNSPECIFIED.,
 .F.,.F.,(4,2,2,2,2,2,2,2,2,2,2,2,2,2,2,2,2,2,2,2,2,2,2,2,2,2,2,2,2,2,2,
2,2,2,2,2,4),(-5.75143272123174,-5.51425389802513,-5.38581494958568,-5.30282096642187,
-5.15632832998793,-5.0625607905497,-4.92381637402678,-4.8214199017456,-4.54353032383151,
-4.42739783573035,-4.3324600201362,-4.13063478019986,-4.0342164491489,-3.82372116145262,
-3.70528204848231,-3.57327965413493,-3.32474231832744,-3.13615410152035,
-3.02764808010997,-2.90892832901364,-2.79616302940586,-2.55643264429745,
-2.40818598215869,-2.11545935413461,-1.9712552015513,-1.7324587016481,-1.62232234512572,
-1.41548413105099,-1.33888975016641,-1.17684236228568,-0.952280572602755,
-0.698170153676864,-0.594739755733359,-0.489501749629593,-0.294699430069487,
-0.149216263156714,-0.000229344986775188),.UNSPECIFIED.);
#29683=B_SPLINE_CURVE_WITH_KNOTS('',3,(#129093,#129094,#129095,#129096,
#129097,#129098,#129099,#129100,#129101,#129102,#129103,#129104,#129105,
#129106,#129107,#129108,#129109,#129110,#129111,#129112,#129113,#129114,
#129115,#129116,#129117,#129118,#129119,#129120,#129121,#129122,#129123,
#129124,#129125,#129126,#129127,#129128,#129129,#129130,#129131,#129132,
#129133,#129134,#129135,#129136,#129137,#129138,#129139,#129140,#129141,
#129142,#129143,#129144,#129145,#129146,#129147,#129148,#129149,#129150,
#129151,#129152,#129153,#129154,#129155,#129156,#129157,#129158,#129159,
#129160,#129161,#129162,#129163,#129164,#129165,#129166,#129167,#129168,
#129169,#129170,#129171,#129172,#129173,#129174,#129175,#129176,#129177,
#129178,#129179,#129180,#129181,#129182,#129183,#129184,#129185,#129186,
#129187,#129188,#129189,#129190,#129191,#129192,#129193,#129194,#129195,
#129196,#129197,#129198,#129199,#129200,#129201,#129202,#129203,#129204,
#129205,#129206,#129207,#129208,#129209,#129210,#129211,#129212,#129213,
#129214,#129215,#129216,#129217,#129218,#129219,#129220,#129221,#129222,
#129223,#129224,#129225,#129226,#129227,#129228,#129229,#129230,#129231,
#129232,#129233,#129234,#129235,#129236,#129237,#129238,#129239,#129240,
#129241,#129242,#129243,#129244,#129245,#129246,#129247,#129248,#129249,
#129250,#129251,#129252,#129253,#129254,#129255,#129256,#129257,#129258,
#129259,#129260,#129261,#129262,#129263,#129264,#129265,#129266,#129267,
#129268,#129269,#129270,#129271,#129272,#129273,#129274,#129275,#129276,
#129277,#129278,#129279,#129280,#129281,#129282,#129283,#129284,#129285,
#129286,#129287,#129288,#129289,#129290,#129291,#129292,#129293,#129294,
#129295,#129296,#129297,#129298,#129299,#129300,#129301,#129302,#129303,
#129304,#129305,#129306,#129307,#129308,#129309,#129310,#129311,#129312,
#129313,#129314,#129315,#129316,#129317,#129318,#129319,#129320,#129321,
#129322,#129323,#129324,#129325,#129326,#129327,#129328,#129329,#129330,
#129331,#129332,#129333,#129334,#129335,#129336,#129337,#129338,#129339,
#129340,#129341,#129342,#129343,#129344,#129345,#129346,#129347,#129348,
#129349,#129350,#129351,#129352,#129353,#129354,#129355,#129356,#129357,
#129358,#129359,#129360,#129361,#129362,#129363,#129364),.UNSPECIFIED.,
 .F.,.F.,(4,2,2,2,2,2,2,2,2,2,2,2,2,2,2,2,2,2,2,2,2,2,2,2,2,2,2,2,2,2,2,
2,2,2,2,2,2,2,2,2,2,2,2,2,2,2,2,2,2,2,2,2,2,2,2,2,2,2,2,2,2,2,2,2,2,2,2,
2,2,2,2,2,2,2,2,2,2,2,2,2,2,2,2,2,2,2,2,2,2,2,2,2,2,2,2,2,2,2,2,2,2,2,2,
2,2,2,2,2,2,2,2,2,2,2,2,2,2,2,2,2,2,2,2,2,2,2,2,2,2,2,2,2,2,2,2,4),(-13.9545132561037,
-13.9243030347878,-13.8575170995572,-13.7785668713752,-13.7363373288312,
-13.6253227823618,-13.5243077460179,-13.4833877659198,-13.4030198483249,
-13.3284452205562,-13.2858020755448,-13.189303459552,-13.1074519173399,
-13.0504571298454,-13.0076680275537,-12.9176522169789,-12.87866620077,-12.8355501446248,
-12.6930731819753,-12.6321432772867,-12.5829931309723,-12.5301482343459,
-12.4529024056035,-12.403313338851,-12.3494336337027,-12.2225984085807,
-12.1670628471684,-12.1199144497519,-12.0484147414705,-11.9693330995282,
-11.9229510002117,-11.7841889511872,-11.72065110925,-11.6693287546292,-11.5631721644431,
-11.5215261585167,-11.4747646633081,-11.336582485301,-11.2685496843921,
-11.2146703139058,-11.1091993946513,-11.0672227875629,-11.0184919885405,
-10.8868200257123,-10.8151746930919,-10.7591366586285,-10.6594788673485,
-10.6160890886625,-10.5659061606284,-10.4336417282592,-10.3600070767517,
-10.3024464292213,-10.2309151663927,-10.1747020296126,-10.123457696155,
-10.0440113070302,-9.93064217307638,-9.85860877432813,-9.8050648596685,
-9.71297606393378,-9.65914341719085,-9.5404548514819,-9.42480737878252,
-9.37094702494681,-9.28398853774682,-9.224575986282,-9.14504171662432,-9.02074473675671,
-8.9434072201311,-8.83429935998517,-8.77068589316592,-8.68763185293676,
-8.56247735742417,-8.48355843939953,-8.39498619186753,-8.34209848688848,
-8.27644926478958,-8.12312435399313,-8.03114001084608,-7.93136637309668,
-7.85989734033156,-7.67560598889003,-7.57433200921146,-7.48453368081615,
-7.42496102203331,-7.34406973953897,-7.19659109542607,-7.12665726422423,
-7.05756427926115,-6.99640672785181,-6.92448537424654,-6.83993498028912,
-6.65681728040653,-6.5872013227692,-6.49064247711442,-6.35498028494421,
-6.20884708319934,-6.12963523553158,-6.03237383964925,-5.94640062904513,
-5.7289825886956,-5.65781097228224,-5.57515679238814,-5.48160063377645,
-5.27541159940625,-5.19666533043402,-5.10815835870751,-5.00016934485196,
-4.81195237411132,-4.72722527119558,-4.61820771918028,-4.46691676878017,
-4.34057070962386,-4.25166078773298,-4.09537792947731,-3.87430507429907,
-3.78572847737797,-3.5977727605266,-3.42324722260386,-3.32305025872687,
-3.19251305750451,-3.02160159678814,-2.84379246729926,-2.67766870850884,
-2.50316178137508,-2.37785241780002,-2.1660464726187,-1.8128682400176,-1.63820944838796,
-1.36589316898249,-1.18932485818936,-1.01455646022611,-0.6682097331427,
-0.582399699183827,-0.292247528397441,-0.000240302142428214),
 .UNSPECIFIED.);
#29684=B_SPLINE_CURVE_WITH_KNOTS('',3,(#129365,#129366,#129367,#129368,
#129369,#129370),.UNSPECIFIED.,.F.,.F.,(4,2,4),(-0.164149603932805,-0.0824424404676746,
-0.000154614832286251),.UNSPECIFIED.);
#29685=B_SPLINE_CURVE_WITH_KNOTS('',3,(#129504,#129505,#129506,#129507,
#129508,#129509,#129510,#129511,#129512,#129513,#129514,#129515,#129516,
#129517,#129518,#129519,#129520,#129521,#129522,#129523,#129524,#129525,
#129526,#129527,#129528,#129529,#129530,#129531,#129532,#129533,#129534,
#129535,#129536,#129537,#129538,#129539,#129540,#129541,#129542,#129543,
#129544,#129545,#129546,#129547,#129548,#129549,#129550,#129551,#129552,
#129553,#129554,#129555,#129556,#129557,#129558,#129559,#129560,#129561,
#129562,#129563,#129564,#129565,#129566,#129567,#129568,#129569,#129570,
#129571,#129572,#129573,#129574,#129575,#129576,#129577,#129578,#129579,
#129580,#129581,#129582,#129583,#129584,#129585,#129586,#129587,#129588,
#129589,#129590,#129591,#129592,#129593,#129594,#129595,#129596,#129597,
#129598,#129599,#129600,#129601,#129602,#129603,#129604,#129605,#129606,
#129607,#129608,#129609,#129610,#129611,#129612,#129613,#129614,#129615,
#129616,#129617,#129618,#129619,#129620,#129621,#129622,#129623,#129624,
#129625,#129626,#129627,#129628,#129629,#129630,#129631,#129632,#129633,
#129634,#129635,#129636,#129637,#129638,#129639,#129640,#129641,#129642,
#129643,#129644,#129645,#129646,#129647,#129648,#129649,#129650,#129651,
#129652,#129653,#129654,#129655,#129656,#129657,#129658,#129659,#129660,
#129661,#129662,#129663,#129664,#129665,#129666,#129667,#129668,#129669,
#129670,#129671,#129672,#129673,#129674,#129675,#129676,#129677,#129678,
#129679,#129680,#129681,#129682,#129683,#129684,#129685,#129686,#129687,
#129688,#129689,#129690,#129691,#129692,#129693,#129694,#129695,#129696,
#129697,#129698,#129699,#129700,#129701,#129702,#129703,#129704,#129705,
#129706,#129707,#129708,#129709,#129710,#129711,#129712,#129713,#129714,
#129715,#129716,#129717,#129718,#129719,#129720,#129721,#129722,#129723,
#129724,#129725,#129726,#129727,#129728,#129729,#129730,#129731,#129732,
#129733,#129734,#129735,#129736,#129737,#129738,#129739,#129740,#129741,
#129742,#129743,#129744,#129745,#129746,#129747,#129748,#129749,#129750,
#129751,#129752,#129753,#129754,#129755,#129756,#129757,#129758,#129759,
#129760,#129761,#129762,#129763,#129764,#129765,#129766,#129767,#129768,
#129769,#129770,#129771,#129772,#129773,#129774,#129775,#129776,#129777,
#129778,#129779,#129780,#129781,#129782,#129783,#129784,#129785,#129786,
#129787,#129788,#129789,#129790,#129791,#129792,#129793,#129794,#129795,
#129796,#129797,#129798,#129799,#129800,#129801,#129802,#129803,#129804,
#129805,#129806,#129807,#129808,#129809,#129810,#129811,#129812,#129813,
#129814,#129815,#129816,#129817),.UNSPECIFIED.,.F.,.F.,(4,2,2,2,2,2,2,2,
2,2,2,2,2,2,2,2,2,2,2,2,2,2,2,2,2,2,2,2,2,2,2,2,2,2,2,2,2,2,2,2,2,2,2,2,
2,2,2,2,2,2,2,2,2,2,2,2,2,2,2,2,2,2,2,2,2,2,2,2,2,2,2,2,2,2,2,2,2,2,2,2,
2,2,2,2,2,2,2,2,2,2,2,2,2,2,2,2,2,2,2,2,2,2,2,2,2,2,2,2,2,2,2,2,2,2,2,2,
2,2,2,2,2,2,2,2,2,2,2,2,2,2,2,2,2,2,2,2,2,2,2,2,2,2,2,2,2,2,2,2,2,2,2,2,
2,2,2,2,4),(0.,0.032292413384482,0.11338718692391,0.148040637360976,0.168457618704367,
0.188241267176605,0.216038652259134,0.284641193115187,0.516477879067667,
0.628828996864852,0.698718093436911,0.774482230614078,1.01964708834714,
1.08748899446127,1.28277707866717,1.3781384951923,1.46460487362281,1.50518672809182,
1.57800422200734,1.73771378462538,1.81311152286536,1.88176895350014,1.95404514404598,
2.00976777043747,2.09658527865148,2.19998313419955,2.27067456521156,2.37364567285775,
2.41997691965579,2.46564898784514,2.58691325670246,2.65712644782479,2.71143601938331,
2.82794621827374,2.87254740263902,2.91367632676383,2.98020888418034,3.0753799403036,
3.13535568618203,3.17968681150426,3.28186089602486,3.32557799525498,3.36461674882526,
3.49176004613578,3.5441977239118,3.58686713316643,3.64812307506937,3.73946558923753,
3.78172916415125,3.82042537563761,3.88402172937341,3.96156672397072,4.01204824266024,
4.06119724607902,4.17634788817974,4.24269266121792,4.28380509965422,4.38055741765955,
4.42537444493737,4.46996733633555,4.59727073297398,4.66224549973719,4.71375714915893,
4.78346138227071,4.84676247744024,4.89890054546601,4.98583850473261,5.09036543444882,
5.16016149181101,5.23257607886221,5.31344437235388,5.3920060656924,5.53474468458556,
5.60359021446961,5.67281256216165,5.75141742025346,5.96539223474982,6.0626546923424,
6.24539619154649,6.41562405879438,6.58288154350623,6.93438230015164,7.10968814663871,
7.41650283228968,7.48753766525244,7.60660749658937,7.79833043443923,7.90069890178098,
7.9918943868596,8.12012415913234,8.25291457596143,8.32075540014824,8.40878778808261,
8.46337012536212,8.52754771413151,8.69630599603858,8.75047744326148,8.82021519340532,
8.87981752418822,8.93185513408938,8.99843303084257,9.12503452987674,9.17054070891333,
9.2160938364855,9.33101367297571,9.37508646137077,9.4289483232484,9.56648674393166,
9.60816961500189,9.65398813669105,9.75702981795865,9.79873482965581,9.85217651583745,
9.93589798757444,10.0047129824676,10.0455924923016,10.0926323646473,10.2020178262266,
10.2475433702179,10.2955529207173,10.3673739495341,10.4414644234633,10.4843910944375,
10.5350239462422,10.6516584989123,10.7006690121429,10.7511670411831,10.8342347958694,
10.890001742534,10.9464695831528,11.0231499654804,11.1290376384701,11.1756073459244,
11.2201404018214,11.3276326418953,11.397372897746,11.5017623038629,11.5870601969509,
11.6427638139526,11.7103971351646,11.7750294377741,11.8800807922603,12.0379343848749,
12.0936733175175,12.1497862113955,12.3415494616393,12.4613597357732,12.5535607266093,
12.6245905782894,12.7178066948602,12.9154555835334,12.9619081589602,12.9841322280929,
13.001682382259,13.0233152594812,13.0726241508325,13.1773028203083),
 .UNSPECIFIED.);
#29686=B_SPLINE_CURVE_WITH_KNOTS('',3,(#129818,#129819,#129820,#129821,
#129822,#129823),.UNSPECIFIED.,.F.,.F.,(4,2,4),(-0.166256920440251,-0.0836095578472467,
-0.00165050313143913),.UNSPECIFIED.);
#29687=B_SPLINE_CURVE_WITH_KNOTS('',3,(#129964,#129965,#129966,#129967,
#129968,#129969,#129970,#129971,#129972,#129973),.UNSPECIFIED.,.F.,.F.,
(4,2,2,2,4),(-0.95725541846645,-0.716501478982729,-0.477123522853866,-0.237827282638415,
-0.000965045394558864),.UNSPECIFIED.);
#29688=B_SPLINE_CURVE_WITH_KNOTS('',3,(#130398,#130399,#130400,#130401),
 .UNSPECIFIED.,.F.,.F.,(4,4),(0.,1.),.UNSPECIFIED.);
#29689=B_SPLINE_CURVE_WITH_KNOTS('',3,(#130407,#130408,#130409,#130410,
#130411,#130412,#130413,#130414,#130415,#130416,#130417,#130418,#130419,
#130420,#130421,#130422,#130423,#130424,#130425,#130426,#130427,#130428,
#130429,#130430,#130431,#130432,#130433,#130434,#130435,#130436,#130437,
#130438,#130439,#130440,#130441,#130442,#130443,#130444,#130445,#130446,
#130447,#130448,#130449,#130450,#130451,#130452,#130453,#130454,#130455,
#130456,#130457,#130458),.UNSPECIFIED.,.F.,.F.,(4,3,3,3,3,3,3,3,3,3,3,3,
3,3,3,3,3,4),(0.850540505530354,0.8518518518519,0.869052332122078,0.878364846193632,
0.8888888888889,0.902430518835671,0.914652441047175,0.915972148782441,0.9259259259259,
0.935258076282245,0.944312112201459,0.953366148120672,0.962155996387792,
0.962962962963,0.976212027251997,0.989052760382921,0.991448955688734,0.999999999999999),
 .UNSPECIFIED.);
#29690=B_SPLINE_CURVE_WITH_KNOTS('',3,(#130544,#130545,#130546,#130547,
#130548,#130549,#130550,#130551,#130552,#130553,#130554,#130555,#130556,
#130557,#130558,#130559),.UNSPECIFIED.,.F.,.F.,(4,3,3,3,3,4),(1.4363549744475E-5,
0.234649898876813,0.25,0.410893410472241,0.5,0.590850967488242),
 .UNSPECIFIED.);
#29691=B_SPLINE_CURVE_WITH_KNOTS('',3,(#130560,#130561,#130562,#130563,
#130564,#130565,#130566,#130567,#130568,#130569,#130570,#130571,#130572,
#130573,#130574,#130575),.UNSPECIFIED.,.F.,.F.,(4,3,3,3,3,4),(6.08869750723345E-5,
0.237050635026911,0.475427842837836,0.5,0.768673980783898,0.999995089856074),
 .UNSPECIFIED.);
#29692=B_SPLINE_CURVE_WITH_KNOTS('',3,(#130578,#130579,#130580,#130581),
 .UNSPECIFIED.,.F.,.F.,(4,4),(0.,1.),.UNSPECIFIED.);
#29693=B_SPLINE_CURVE_WITH_KNOTS('',3,(#130583,#130584,#130585,#130586,
#130587,#130588,#130589,#130590,#130591,#130592,#130593,#130594,#130595),
 .UNSPECIFIED.,.F.,.F.,(4,3,3,3,4),(0.,0.249999996691539,0.495025461485148,
0.747512724125653,0.999999986766158),.UNSPECIFIED.);
#29694=B_SPLINE_CURVE_WITH_KNOTS('',3,(#130601,#130602,#130603,#130604,
#130605,#130606,#130607,#130608,#130609,#130610,#130611,#130612),
 .UNSPECIFIED.,.F.,.F.,(4,2,2,2,2,4),(5.38437140579657E-7,0.25,0.5,0.75,
0.875,1.),.UNSPECIFIED.);
#29695=B_SPLINE_CURVE_WITH_KNOTS('',3,(#130616,#130617,#130618,#130619,
#130620,#130621,#130622,#130623,#130624,#130625,#130626,#130627,#130628,
#130629,#130630,#130631,#130632,#130633,#130634,#130635,#130636,#130637,
#130638,#130639,#130640,#130641,#130642,#130643,#130644,#130645,#130646,
#130647,#130648,#130649,#130650,#130651,#130652,#130653,#130654,#130655,
#130656,#130657,#130658,#130659,#130660,#130661,#130662,#130663,#130664,
#130665,#130666,#130667,#130668,#130669,#130670,#130671,#130672,#130673,
#130674,#130675,#130676,#130677,#130678,#130679,#130680,#130681,#130682,
#130683,#130684,#130685,#130686,#130687,#130688,#130689,#130690,#130691,
#130692,#130693,#130694,#130695,#130696,#130697,#130698,#130699,#130700,
#130701,#130702,#130703,#130704,#130705,#130706,#130707,#130708,#130709,
#130710,#130711,#130712,#130713,#130714,#130715,#130716,#130717,#130718,
#130719,#130720,#130721,#130722,#130723,#130724,#130725,#130726,#130727,
#130728,#130729,#130730,#130731,#130732,#130733,#130734,#130735,#130736,
#130737,#130738,#130739,#130740,#130741,#130742,#130743,#130744,#130745,
#130746,#130747,#130748,#130749,#130750,#130751,#130752,#130753,#130754,
#130755,#130756,#130757,#130758,#130759,#130760,#130761,#130762,#130763,
#130764,#130765,#130766,#130767,#130768,#130769,#130770,#130771,#130772,
#130773,#130774,#130775,#130776,#130777,#130778,#130779,#130780,#130781,
#130782,#130783,#130784,#130785,#130786,#130787,#130788,#130789,#130790,
#130791,#130792,#130793,#130794,#130795,#130796,#130797,#130798,#130799,
#130800,#130801,#130802,#130803,#130804,#130805,#130806,#130807,#130808),
 .UNSPECIFIED.,.F.,.F.,(4,3,3,3,3,3,3,3,3,3,3,3,3,3,3,3,3,3,3,3,3,3,3,3,
3,3,3,3,3,3,3,3,3,3,3,3,3,3,3,3,3,3,3,3,3,3,3,3,3,3,3,3,3,3,3,3,3,3,3,3,
3,3,3,3,4),(2.74350323131394E-5,0.0624999999997235,0.0937499999995802,0.109374999999565,
0.117187499999557,0.121093749999553,0.124999999999549,0.187499999999655,
0.218749999999689,0.234374999999707,0.249111998385219,0.249999999999725,
0.312499999999783,0.3546748106784,0.374999999999841,0.406249999999865,0.422838753251247,
0.437499999999889,0.454769316094528,0.460746878832215,0.468749999999913,
0.484374999999921,0.49218749999992,0.496898696477359,0.499999999999918,
0.517209260150661,0.529730256140993,0.562499999999972,0.570312499999985,
0.575426028661125,0.578124999999998,0.593750000000013,0.594551426193997,
0.623324356174083,0.625000000000046,0.642774596457414,0.644014348734208,
0.662522111460604,0.681015861169127,0.687500000000103,0.688469968606538,
0.718750000000133,0.732476180168218,0.73437500000015,0.742187500000159,
0.74804687500016,0.750000000000159,0.76909300821462,0.80116220296322,0.812500000000106,
0.833321748262734,0.843750000000081,0.859375000000067,0.865392429488015,
0.86718750000006,0.871093750000055,0.873046875000055,0.874658875118369,
0.875000000000055,0.890541952448512,0.913010890352078,0.935653276704301,
0.958350383364628,0.980987301333187,1.),.UNSPECIFIED.);
#29696=B_SPLINE_CURVE_WITH_KNOTS('',3,(#130811,#130812,#130813,#130814,
#130815,#130816,#130817,#130818,#130819,#130820,#130821,#130822,#130823,
#130824,#130825,#130826),.UNSPECIFIED.,.F.,.F.,(4,3,3,3,3,4),(0.,0.272018137403932,
0.5,0.733225822333112,0.965046929604712,0.999871379634594),
 .UNSPECIFIED.);
#29697=B_SPLINE_CURVE_WITH_KNOTS('',3,(#130828,#130829,#130830,#130831,
#130832,#130833,#130834,#130835,#130836,#130837,#130838,#130839,#130840,
#130841,#130842,#130843,#130844,#130845,#130846,#130847,#130848,#130849,
#130850,#130851,#130852,#130853,#130854,#130855,#130856,#130857,#130858,
#130859,#130860,#130861,#130862,#130863,#130864,#130865,#130866,#130867,
#130868,#130869,#130870,#130871,#130872,#130873,#130874,#130875,#130876,
#130877,#130878,#130879,#130880,#130881,#130882,#130883,#130884,#130885,
#130886,#130887,#130888,#130889,#130890,#130891,#130892,#130893,#130894,
#130895,#130896,#130897,#130898,#130899,#130900,#130901,#130902,#130903,
#130904,#130905,#130906,#130907,#130908,#130909,#130910,#130911,#130912,
#130913,#130914,#130915,#130916,#130917,#130918,#130919,#130920,#130921,
#130922,#130923,#130924,#130925,#130926,#130927,#130928,#130929,#130930,
#130931,#130932,#130933,#130934,#130935,#130936,#130937,#130938,#130939,
#130940,#130941,#130942,#130943,#130944,#130945,#130946,#130947,#130948,
#130949,#130950,#130951,#130952,#130953,#130954,#130955,#130956,#130957,
#130958,#130959,#130960,#130961,#130962,#130963,#130964,#130965,#130966,
#130967,#130968,#130969,#130970,#130971,#130972,#130973,#130974,#130975,
#130976,#130977,#130978,#130979,#130980,#130981,#130982,#130983,#130984,
#130985,#130986,#130987,#130988,#130989,#130990,#130991,#130992,#130993,
#130994,#130995,#130996,#130997,#130998,#130999),.UNSPECIFIED.,.F.,.F.,
(4,3,3,3,3,3,3,3,3,3,3,3,3,3,3,3,3,3,3,3,3,3,3,3,3,3,3,3,3,3,3,3,3,3,3,
3,3,3,3,3,3,3,3,3,3,3,3,3,3,3,3,3,3,3,3,3,3,4),(0.,0.027175431995618,0.0625000000000007,
0.0880630432418482,0.0937500000000011,0.109375000000001,0.1171875,0.121093749999997,
0.124350215203792,0.124999999999995,0.146206578525037,0.18750000000001,
0.204900747761968,0.218750000000018,0.234375000000023,0.242187500000027,
0.246093750000027,0.249409409547392,0.250000000000028,0.259834344000549,
0.29426179667726,0.312500000000027,0.314402755346343,0.320312500000027,
0.325489425754323,0.328125000000026,0.343750000000025,0.373866631016789,
0.375000000000014,0.406250000000002,0.437499999999991,0.439137004609811,
0.468749999999979,0.484374999999977,0.494881653599767,0.499999999999974,
0.502112536539499,0.551112506283609,0.562382890212236,0.562499999999971,
0.593749999999965,0.609374999999967,0.612898884207516,0.617187499999969,
0.623058384348781,0.624999999999971,0.66474708209181,0.687499999999985,
0.718749999999986,0.720444473291107,0.73437499999999,0.744928262125903,
0.749999999999993,0.783323050751545,0.848613134581319,0.90975816302401,
0.966654952023228,1.),.UNSPECIFIED.);
#29698=B_SPLINE_CURVE_WITH_KNOTS('',3,(#131001,#131002,#131003,#131004,
#131005,#131006,#131007,#131008,#131009),.UNSPECIFIED.,.F.,.F.,(4,1,2,2,
4),(0.,0.250000000000002,0.37500000000002,0.500000000000039,0.999998122610419),
 .UNSPECIFIED.);
#29699=B_SPLINE_CURVE_WITH_KNOTS('',3,(#131011,#131012,#131013,#131014),
 .UNSPECIFIED.,.F.,.F.,(4,4),(0.,0.987417625481105),.UNSPECIFIED.);
#29700=B_SPLINE_CURVE_WITH_KNOTS('',3,(#131018,#131019,#131020,#131021,
#131022,#131023,#131024,#131025,#131026,#131027,#131028,#131029),
 .UNSPECIFIED.,.F.,.F.,(4,2,2,2,2,4),(0.,0.125,0.25,0.5,0.75,0.999999414381818),
 .UNSPECIFIED.);
#29701=B_SPLINE_CURVE_WITH_KNOTS('',3,(#131035,#131036,#131037,#131038,
#131039,#131040,#131041,#131042,#131043,#131044,#131045,#131046,#131047),
 .UNSPECIFIED.,.F.,.F.,(4,3,3,3,4),(1.05547686689035E-8,0.250000007878098,
0.495573600746854,0.74778680029747,0.999999999848086),.UNSPECIFIED.);
#29702=B_SPLINE_CURVE_WITH_KNOTS('',3,(#131048,#131049,#131050,#131051),
 .UNSPECIFIED.,.F.,.F.,(4,4),(0.,1.),.UNSPECIFIED.);
#29703=B_SPLINE_CURVE_WITH_KNOTS('',3,(#131054,#131055,#131056,#131057,
#131058,#131059,#131060,#131061,#131062,#131063,#131064,#131065,#131066,
#131067,#131068,#131069,#131070,#131071,#131072,#131073,#131074,#131075,
#131076,#131077,#131078,#131079,#131080,#131081,#131082,#131083,#131084,
#131085,#131086,#131087,#131088,#131089,#131090,#131091,#131092,#131093,
#131094,#131095,#131096,#131097,#131098,#131099,#131100,#131101,#131102,
#131103,#131104,#131105,#131106,#131107,#131108,#131109,#131110,#131111,
#131112,#131113,#131114,#131115,#131116,#131117,#131118,#131119,#131120,
#131121,#131122,#131123,#131124,#131125,#131126,#131127,#131128,#131129,
#131130,#131131,#131132,#131133,#131134,#131135,#131136,#131137,#131138,
#131139,#131140,#131141,#131142,#131143,#131144,#131145,#131146,#131147,
#131148,#131149,#131150,#131151,#131152,#131153,#131154,#131155,#131156),
 .UNSPECIFIED.,.F.,.F.,(4,3,3,3,3,3,3,3,3,3,3,3,3,3,3,3,3,3,3,3,3,3,3,3,
3,3,3,3,3,3,3,3,3,3,4),(0.,0.0723506085258293,0.125000000000116,0.18750000000018,
0.218750000000209,0.234375000000217,0.242187500000227,0.250000000000237,
0.299895474419656,0.345551114878514,0.375000000000126,0.41500361137732,
0.437500000000074,0.468750000000044,0.48437500000003,0.492187500000022,
0.499388887162804,0.500000000000015,0.562499999999964,0.593749999999936,
0.609374999999922,0.617187499999912,0.624999999999901,0.665272339956595,
0.687499999999829,0.718749999999794,0.734374999999776,0.742187499999767,
0.746093749999763,0.749999999999758,0.80362415793811,0.855431431549843,
0.874999999999879,0.93749999999994,1.),.UNSPECIFIED.);
#29704=B_SPLINE_CURVE_WITH_KNOTS('',3,(#131162,#131163,#131164,#131165,
#131166,#131167,#131168,#131169,#131170,#131171,#131172,#131173,#131174,
#131175,#131176,#131177,#131178,#131179,#131180,#131181,#131182,#131183,
#131184,#131185,#131186,#131187,#131188),.UNSPECIFIED.,.F.,.F.,(4,2,2,2,
2,2,2,2,2,1,1,1,2,2,4),(0.,0.124999999999985,0.249999999999971,0.374999999999956,
0.437499999999948,0.468749999999943,0.499999999999939,0.62499999999992,
0.687499999999912,0.718749999999909,0.734374999999908,0.742187499999908,
0.746093749999909,0.74999999999991,1.),.UNSPECIFIED.);
#29705=B_SPLINE_CURVE_WITH_KNOTS('',3,(#131192,#131193,#131194,#131195,
#131196,#131197,#131198,#131199,#131200,#131201),.UNSPECIFIED.,.F.,.F.,
(4,3,3,4),(0.,0.343291977175944,0.694006915258001,1.),.UNSPECIFIED.);
#29706=B_SPLINE_CURVE_WITH_KNOTS('',3,(#131202,#131203,#131204,#131205,
#131206,#131207,#131208,#131209,#131210,#131211,#131212,#131213,#131214,
#131215,#131216,#131217,#131218,#131219,#131220,#131221,#131222,#131223,
#131224,#131225,#131226,#131227,#131228,#131229,#131230,#131231,#131232,
#131233,#131234,#131235,#131236,#131237,#131238,#131239,#131240,#131241,
#131242,#131243,#131244,#131245,#131246,#131247,#131248,#131249,#131250,
#131251,#131252,#131253,#131254,#131255,#131256),.UNSPECIFIED.,.F.,.F.,
(4,3,3,3,3,3,3,3,3,3,3,3,3,3,3,3,3,3,4),(5.35764201986684E-7,0.0626028178933704,
0.125,0.183946083050093,0.244293768613518,0.25,0.309271075467163,0.369561477217816,
0.374999999999999,0.439386734520521,0.499999999999999,0.570406759789097,
0.640766647615167,0.710632672526661,0.75,0.820183692041351,0.889379411738386,
0.956887378896293,1.),.UNSPECIFIED.);
#29707=B_SPLINE_CURVE_WITH_KNOTS('',3,(#131259,#131260,#131261,#131262,
#131263,#131264,#131265,#131266,#131267,#131268,#131269,#131270,#131271,
#131272,#131273,#131274,#131275,#131276,#131277,#131278,#131279,#131280,
#131281,#131282,#131283,#131284,#131285,#131286,#131287,#131288,#131289,
#131290,#131291,#131292,#131293,#131294,#131295,#131296,#131297,#131298,
#131299,#131300,#131301,#131302,#131303,#131304,#131305,#131306,#131307,
#131308,#131309,#131310,#131311,#131312,#131313),.UNSPECIFIED.,.F.,.F.,
(4,3,3,3,3,3,3,3,3,3,3,3,3,3,3,3,3,3,4),(0.,0.0675500997162986,0.136181197824484,
0.20632392252024,0.25,0.319906911503152,0.390159163770846,0.460517396300711,
0.5,0.564174428820622,0.625,0.6875,0.746428238623813,0.75,0.8125,0.870495037255567,
0.875,0.937499678080067,0.999999356160134),.UNSPECIFIED.);
#29708=B_SPLINE_CURVE_WITH_KNOTS('',3,(#131315,#131316,#131317,#131318,
#131319,#131320,#131321),.UNSPECIFIED.,.F.,.F.,(4,3,4),(3.32652296912383E-8,
0.56832246895326,0.999999998771275),.UNSPECIFIED.);
#29709=B_SPLINE_CURVE_WITH_KNOTS('',3,(#131325,#131326,#131327,#131328,
#131329,#131330,#131331,#131332,#131333,#131334,#131335,#131336,#131337,
#131338,#131339,#131340,#131341,#131342,#131343,#131344,#131345,#131346,
#131347),.UNSPECIFIED.,.F.,.F.,(4,2,2,1,1,1,2,2,2,2,2,2,4),(0.,0.125000000000061,
0.187500000000091,0.218750000000105,0.234375000000112,0.242187500000114,
0.246093750000114,0.250000000000115,0.375000000000096,0.437500000000086,
0.500000000000076,0.750000000000038,1.),.UNSPECIFIED.);
#29710=B_SPLINE_CURVE_WITH_KNOTS('',3,(#131352,#131353,#131354,#131355,
#131356,#131357,#131358,#131359,#131360,#131361,#131362,#131363,#131364,
#131365,#131366,#131367,#131368,#131369,#131370,#131371,#131372,#131373,
#131374,#131375,#131376,#131377,#131378,#131379,#131380,#131381,#131382,
#131383,#131384,#131385,#131386,#131387,#131388,#131389,#131390,#131391,
#131392,#131393,#131394,#131395,#131396,#131397,#131398,#131399,#131400,
#131401,#131402,#131403,#131404,#131405,#131406,#131407,#131408,#131409,
#131410,#131411,#131412,#131413,#131414,#131415,#131416,#131417,#131418,
#131419,#131420,#131421,#131422,#131423,#131424,#131425,#131426,#131427,
#131428,#131429,#131430,#131431,#131432,#131433,#131434,#131435,#131436,
#131437,#131438,#131439,#131440,#131441,#131442,#131443,#131444,#131445,
#131446,#131447,#131448,#131449,#131450,#131451),.UNSPECIFIED.,.F.,.F.,
(4,3,3,3,3,3,3,3,3,3,3,3,3,3,3,3,3,3,3,3,3,3,3,3,3,3,3,3,3,3,3,3,3,4),(0.,
0.0508232102907746,0.0999610534001555,0.124999999999707,0.156249999999633,
0.164062499999615,0.167968749999606,0.171874999999596,0.187499999999589,
0.249999999999539,0.298872692796552,0.343285506562304,0.374999999999437,
0.413686183409598,0.437499999999392,0.468749999999367,0.484374999999355,
0.492187499999351,0.496093749999351,0.499999999999351,0.535775879334486,
0.572857181333828,0.612180962308859,0.624999999999508,0.668969590894529,
0.687499999999586,0.71874999999963,0.734374999999642,0.742187499999655,
0.749999999999668,0.833516144219682,0.912374151136646,0.986436512705714,
1.),.UNSPECIFIED.);
#29711=B_SPLINE_CURVE_WITH_KNOTS('',3,(#131525,#131526,#131527,#131528,
#131529,#131530),.UNSPECIFIED.,.F.,.F.,(4,2,4),(1.00000001544255E-6,0.194540681199865,
0.386597804410077),.UNSPECIFIED.);
#29712=B_SPLINE_CURVE_WITH_KNOTS('',3,(#131536,#131537,#131538,#131539,
#131540,#131541,#131542,#131543,#131544,#131545,#131546,#131547,#131548,
#131549,#131550,#131551,#131552,#131553,#131554,#131555,#131556,#131557,
#131558,#131559,#131560,#131561,#131562,#131563,#131564,#131565,#131566,
#131567,#131568,#131569,#131570,#131571,#131572,#131573,#131574,#131575,
#131576,#131577,#131578,#131579,#131580,#131581),.UNSPECIFIED.,.F.,.F.,
(4,3,3,3,3,3,3,3,3,3,3,3,3,3,3,4),(0.,0.0415381079537162,0.126736790018611,
0.207848081378628,0.25,0.286439332862369,0.363980210205771,0.441585087808742,
0.519085230204526,0.595965602261323,0.671739736746559,0.745880813468968,
0.817826906179531,0.886990404412328,0.952762686580257,1.),.UNSPECIFIED.);
#29713=B_SPLINE_CURVE_WITH_KNOTS('',3,(#131585,#131586,#131587,#131588,
#131589,#131590,#131591,#131592,#131593,#131594,#131595,#131596,#131597,
#131598,#131599,#131600,#131601,#131602,#131603,#131604,#131605,#131606,
#131607,#131608,#131609,#131610,#131611,#131612,#131613,#131614,#131615,
#131616,#131617,#131618,#131619,#131620,#131621,#131622,#131623,#131624,
#131625,#131626,#131627,#131628,#131629,#131630,#131631,#131632,#131633,
#131634,#131635,#131636,#131637,#131638,#131639,#131640,#131641,#131642,
#131643,#131644,#131645,#131646,#131647,#131648,#131649,#131650,#131651,
#131652,#131653,#131654,#131655,#131656,#131657,#131658,#131659,#131660,
#131661,#131662,#131663,#131664,#131665,#131666),.UNSPECIFIED.,.F.,.F.,
(4,3,3,3,3,3,3,3,3,3,3,3,3,3,3,3,3,3,3,3,3,3,3,3,3,3,3,4),(0.,0.0334067132104181,
0.0951069985116222,0.103593870574672,0.160292573944682,0.172810003123751,
0.225452114130447,0.242418205893516,0.25,0.298890317737418,0.313853438307388,
0.362302570675681,0.388221306904702,0.436699311471132,0.465433186831388,
0.5,0.544971053720226,0.590222923525372,0.626161235508926,0.671327272640816,
0.707999949658858,0.75,0.789293973450788,0.837497575175666,0.868788214041699,
0.922151731283876,0.94510500688402,0.99999771126323),.UNSPECIFIED.);
#29714=B_SPLINE_CURVE_WITH_KNOTS('',3,(#131731,#131732,#131733,#131734,
#131735,#131736,#131737,#131738,#131739,#131740,#131741,#131742,#131743,
#131744,#131745,#131746,#131747,#131748,#131749,#131750,#131751,#131752,
#131753,#131754,#131755,#131756,#131757,#131758,#131759,#131760,#131761,
#131762,#131763,#131764,#131765,#131766,#131767),.UNSPECIFIED.,.F.,.F.,
(4,3,3,3,3,3,3,3,3,3,3,3,4),(4.74817631795029E-11,0.0827291018525572,0.166364550926279,
0.25,0.333157078619199,0.416730922791078,0.499999999999999,0.584300894672092,
0.669074900194399,0.754752782585889,0.840964366055479,0.928186520372598,
1.),.UNSPECIFIED.);
#29715=B_SPLINE_CURVE_WITH_KNOTS('',3,(#131866,#131867,#131868,#131869,
#131870,#131871,#131872,#131873,#131874,#131875),.UNSPECIFIED.,.F.,.F.,
(4,2,2,2,4),(-0.612259894639514,-0.574621721277036,-0.536983547914558,-0.497876710714951,
-0.458769873515343),.UNSPECIFIED.);
#29716=B_SPLINE_CURVE_WITH_KNOTS('',3,(#131881,#131882,#131883,#131884,
#131885,#131886,#131887,#131888,#131889,#131890),.UNSPECIFIED.,.F.,.F.,
(4,2,2,2,4),(-0.153491378099786,-0.114756863309896,-0.0760223485200071,
-0.038011174259927,1.52988732793347E-13),.UNSPECIFIED.);
#29717=B_SPLINE_CURVE_WITH_KNOTS('',3,(#131967,#131968,#131969,#131970,
#131971,#131972,#131973,#131974,#131975,#131976),.UNSPECIFIED.,.F.,.F.,
(4,2,2,2,4),(1.40619031198242E-8,0.250000000000001,0.500000000000001,0.75,
0.999999870300648),.UNSPECIFIED.);
#29718=B_SPLINE_CURVE_WITH_KNOTS('',3,(#132050,#132051,#132052,#132053,
#132054,#132055),.UNSPECIFIED.,.F.,.F.,(4,2,4),(4.58324947990726E-5,0.192154614647802,
0.386590702245323),.UNSPECIFIED.);
#29719=B_SPLINE_CURVE_WITH_KNOTS('',3,(#132057,#132058,#132059,#132060,
#132061,#132062),.UNSPECIFIED.,.F.,.F.,(4,2,4),(0.,0.500000000000002,1.),
 .UNSPECIFIED.);
#29720=B_SPLINE_CURVE_WITH_KNOTS('',3,(#132063,#132064,#132065,#132066,
#132067,#132068,#132069,#132070,#132071,#132072,#132073,#132074,#132075,
#132076,#132077,#132078,#132079,#132080,#132081,#132082,#132083,#132084,
#132085,#132086,#132087,#132088,#132089,#132090,#132091,#132092,#132093,
#132094,#132095,#132096,#132097,#132098,#132099,#132100,#132101,#132102,
#132103,#132104,#132105,#132106,#132107,#132108,#132109,#132110,#132111,
#132112,#132113,#132114,#132115,#132116,#132117,#132118,#132119,#132120,
#132121,#132122,#132123,#132124,#132125,#132126,#132127,#132128,#132129,
#132130,#132131,#132132,#132133,#132134,#132135),.UNSPECIFIED.,.F.,.F.,
(4,3,3,3,3,3,3,3,3,3,3,3,3,3,3,3,3,3,3,3,3,3,3,3,4),(0.,0.0694189172578119,
0.141890572965811,0.210576021946684,0.21436222867381,0.249999999999992,
0.315883055493651,0.380615641482329,0.443499936334932,0.468749999999985,
0.4748539020741,0.484374999999985,0.492187499999985,0.496093749999985,0.498046874999985,
0.499999999999985,0.568648136554788,0.63598650772398,0.701417617452483,
0.749999999999993,0.793695925425306,0.856370695328245,0.918075299204161,
0.978538384319356,1.),.UNSPECIFIED.);
#29721=B_SPLINE_CURVE_WITH_KNOTS('',3,(#132136,#132137,#132138,#132139,
#132140,#132141,#132142,#132143,#132144,#132145,#132146,#132147,#132148,
#132149,#132150,#132151,#132152,#132153,#132154,#132155,#132156,#132157,
#132158,#132159,#132160,#132161,#132162,#132163,#132164,#132165,#132166,
#132167,#132168,#132169,#132170,#132171,#132172,#132173,#132174,#132175,
#132176,#132177,#132178,#132179,#132180,#132181,#132182,#132183,#132184,
#132185,#132186,#132187,#132188,#132189,#132190,#132191,#132192,#132193,
#132194,#132195,#132196,#132197,#132198,#132199,#132200,#132201,#132202,
#132203,#132204,#132205,#132206,#132207,#132208,#132209,#132210,#132211,
#132212,#132213,#132214,#132215,#132216,#132217,#132218,#132219,#132220,
#132221,#132222,#132223,#132224,#132225,#132226,#132227,#132228,#132229,
#132230,#132231,#132232,#132233,#132234,#132235,#132236,#132237,#132238,
#132239,#132240,#132241,#132242,#132243,#132244,#132245,#132246,#132247,
#132248,#132249,#132250,#132251,#132252,#132253,#132254,#132255,#132256,
#132257,#132258,#132259,#132260,#132261,#132262,#132263,#132264,#132265,
#132266,#132267,#132268,#132269,#132270,#132271,#132272,#132273,#132274,
#132275,#132276,#132277,#132278,#132279,#132280,#132281,#132282,#132283,
#132284,#132285,#132286,#132287,#132288,#132289,#132290,#132291,#132292,
#132293,#132294,#132295,#132296,#132297,#132298),.UNSPECIFIED.,.F.,.F.,
(4,3,3,3,3,3,3,3,3,3,3,3,3,3,3,3,3,3,3,3,3,3,3,3,3,3,3,3,3,3,3,3,3,3,3,
3,3,3,3,3,3,3,3,3,3,3,3,3,3,3,3,3,3,3,4),(3.40946049943408E-6,0.054842748741813,
0.106432016312161,0.125000000000608,0.129350108745852,0.178571945306471,
0.205765448657295,0.218750000001064,0.23437500000114,0.242187500001178,
0.246093750001197,0.248046875001207,0.250000000001216,0.288792477778297,
0.332542876341043,0.370249106745186,0.411741696022687,0.441542507192826,
0.468750000002289,0.484375000002366,0.492187500002404,0.496093750002423,
0.498046875002432,0.49975585937744,0.500000000002441,0.514416732036424,
0.522335100169526,0.536786245068709,0.551261014077162,0.565758932084681,
0.580251982159897,0.594687007165219,0.599198235475945,0.609375000001889,
0.61718750000185,0.62109375000183,0.62304687500182,0.624023437501815,0.624511718751812,
0.62500000000181,0.652077693741378,0.685413846871352,0.718750000001327,
0.72732126050095,0.734375000001246,0.742187500001204,0.746093750001184,
0.748046875001174,0.750000000001164,0.802585370019843,0.854434672410697,
0.875607568098376,0.929894244795768,0.951979590739165,1.),.UNSPECIFIED.);
#29722=B_SPLINE_CURVE_WITH_KNOTS('',3,(#132333,#132334,#132335,#132336,
#132337,#132338,#132339,#132340,#132341,#132342,#132343,#132344,#132345,
#132346,#132347,#132348,#132349,#132350,#132351,#132352,#132353,#132354,
#132355,#132356,#132357,#132358,#132359,#132360,#132361,#132362,#132363,
#132364,#132365,#132366,#132367,#132368,#132369,#132370,#132371,#132372,
#132373,#132374,#132375,#132376,#132377,#132378,#132379,#132380,#132381),
 .UNSPECIFIED.,.F.,.F.,(4,3,3,3,3,3,3,3,3,3,3,3,3,3,3,3,4),(0.,0.0744307467764002,
0.148427940845822,0.221954288050944,0.25,0.319609640865989,0.389063697351913,
0.458416657409939,0.5,0.569367807722475,0.638779849028523,0.708396453691038,
0.75,0.823587544912622,0.897476995603493,0.971968625959274,0.999999999975216),
 .UNSPECIFIED.);
#29723=B_SPLINE_CURVE_WITH_KNOTS('',3,(#132387,#132388,#132389,#132390,
#132391,#132392,#132393,#132394,#132395,#132396,#132397,#132398,#132399,
#132400,#132401,#132402,#132403,#132404,#132405,#132406,#132407,#132408,
#132409,#132410,#132411,#132412,#132413,#132414,#132415,#132416,#132417,
#132418,#132419,#132420,#132421,#132422,#132423,#132424,#132425,#132426,
#132427,#132428,#132429,#132430,#132431,#132432),.UNSPECIFIED.,.F.,.F.,
(4,3,3,3,3,3,3,3,3,3,3,3,3,3,3,4),(2.64815152994146E-6,0.0765183545169465,
0.153024457583502,0.229532776872433,0.25,0.326519104574361,0.403032996572845,
0.479542540666675,0.55606478721308,0.632576548147086,0.70909348482205,0.75,
0.826508908783698,0.903008250114437,0.97950997539458,1.),.UNSPECIFIED.);
#29724=B_SPLINE_CURVE_WITH_KNOTS('',3,(#132490,#132491,#132492,#132493,
#132494,#132495,#132496,#132497,#132498,#132499,#132500,#132501,#132502,
#132503,#132504,#132505,#132506,#132507,#132508,#132509,#132510,#132511,
#132512,#132513,#132514,#132515,#132516,#132517,#132518,#132519,#132520,
#132521,#132522,#132523,#132524,#132525,#132526,#132527,#132528,#132529,
#132530,#132531,#132532,#132533,#132534,#132535,#132536,#132537,#132538,
#132539,#132540,#132541,#132542,#132543,#132544),.UNSPECIFIED.,.F.,.F.,
(4,3,3,3,3,3,3,3,3,3,3,3,3,3,3,3,3,3,4),(0.0078125,0.0332755574502296,0.065666662832044,
0.10663681473059,0.131835937499996,0.193847656249995,0.229850852495821,
0.255859374999993,0.28686523437499,0.305008654602828,0.317871093749986,
0.348876953124983,0.366851135809689,0.37988281249998,0.433610794258693,
0.476339196060823,0.503906250000037,0.564135200036142,0.625021704863166),
 .UNSPECIFIED.);
#29725=B_SPLINE_CURVE_WITH_KNOTS('',3,(#132545,#132546,#132547,#132548),
 .UNSPECIFIED.,.F.,.F.,(4,4),(-0.0351695698157893,0.),.UNSPECIFIED.);
#29726=B_SPLINE_CURVE_WITH_KNOTS('',3,(#132590,#132591,#132592,#132593),
 .UNSPECIFIED.,.F.,.F.,(4,4),(1.45270373485029E-10,1.),.UNSPECIFIED.);
#29727=B_SPLINE_CURVE_WITH_KNOTS('',3,(#132630,#132631,#132632,#132633,
#132634,#132635,#132636,#132637,#132638,#132639,#132640,#132641),
 .UNSPECIFIED.,.F.,.F.,(4,2,2,2,2,4),(0.,0.249999999999838,0.374999999999759,
0.437499999999719,0.499999999999679,1.),.UNSPECIFIED.);
#29728=B_SPLINE_CURVE_WITH_KNOTS('',3,(#132728,#132729,#132730,#132731,
#132732,#132733,#132734,#132735,#132736,#132737,#132738,#132739,#132740,
#132741,#132742,#132743,#132744,#132745,#132746,#132747,#132748,#132749,
#132750,#132751,#132752,#132753,#132754,#132755,#132756,#132757,#132758,
#132759,#132760,#132761,#132762,#132763,#132764,#132765,#132766,#132767),
 .UNSPECIFIED.,.F.,.F.,(4,3,3,3,3,3,3,3,3,3,3,3,3,4),(0.00704145220077311,
0.0546624749950295,0.160757685575355,0.256729617165409,0.343735196321369,
0.422731592898268,0.494638559250071,0.560248549174547,0.620252323655667,
0.6753431121518,0.726138185608107,0.772911121896331,0.815853204906754,0.818639731362567),
 .UNSPECIFIED.);
#29729=B_SPLINE_CURVE_WITH_KNOTS('',3,(#132768,#132769,#132770,#132771,
#132772,#132773,#132774,#132775,#132776,#132777,#132778,#132779,#132780,
#132781,#132782,#132783,#132784,#132785,#132786,#132787,#132788,#132789,
#132790,#132791,#132792,#132793,#132794,#132795,#132796,#132797,#132798,
#132799,#132800,#132801,#132802,#132803,#132804,#132805,#132806,#132807,
#132808,#132809,#132810,#132811,#132812,#132813,#132814,#132815,#132816,
#132817,#132818,#132819,#132820,#132821,#132822),.UNSPECIFIED.,.F.,.F.,
(4,3,3,3,3,3,3,3,3,3,3,3,3,3,3,3,3,3,4),(3.4986814498593E-6,0.0718168524834047,
0.144450116073449,0.218617782422917,0.250000000000133,0.324851340463086,
0.3750000000002,0.437500000000237,0.46875000000026,0.484375000000269,0.492187500000267,
0.498371542815579,0.500000000000264,0.550121069632035,0.64802203477807,
0.748418884904067,0.850267541208494,0.954333458676404,1.),.UNSPECIFIED.);
#29730=B_SPLINE_CURVE_WITH_KNOTS('',3,(#132851,#132852,#132853,#132854,
#132855,#132856,#132857,#132858,#132859,#132860,#132861,#132862,#132863),
 .UNSPECIFIED.,.F.,.F.,(4,3,3,3,4),(2.27623555205564E-8,0.250485617068881,
0.495662151858339,0.697586558037137,1.),.UNSPECIFIED.);
#29731=B_SPLINE_CURVE_WITH_KNOTS('',3,(#132864,#132865,#132866,#132867,
#132868,#132869,#132870,#132871,#132872,#132873,#132874,#132875,#132876,
#132877,#132878,#132879,#132880,#132881,#132882),.UNSPECIFIED.,.F.,.F.,
(4,3,3,3,3,3,4),(3.83662521257097E-8,0.190570751481294,0.368121042182241,
0.56520196650433,0.694927749154686,0.76228289082642,1.),.UNSPECIFIED.);
#29732=B_SPLINE_CURVE_WITH_KNOTS('',3,(#132919,#132920,#132921,#132922,
#132923,#132924,#132925,#132926,#132927,#132928,#132929,#132930,#132931),
 .UNSPECIFIED.,.F.,.F.,(4,2,1,2,2,2,4),(0.,0.500000000000364,0.625000000000329,
0.687500000000449,0.750000000000568,0.875000000000284,0.996873152388077),
 .UNSPECIFIED.);
#29733=B_SPLINE_CURVE_WITH_KNOTS('',3,(#132966,#132967,#132968,#132969,
#132970,#132971,#132972,#132973,#132974,#132975,#132976,#132977,#132978,
#132979,#132980,#132981,#132982,#132983,#132984,#132985,#132986,#132987,
#132988,#132989,#132990),.UNSPECIFIED.,.F.,.F.,(4,3,3,3,3,3,3,3,4),(4.68314545443848E-6,
0.126309882651852,0.341277948136751,0.371917171174264,0.592944537541651,
0.616839507849623,0.837854929064512,0.858095091419386,0.999999798284643),
 .UNSPECIFIED.);
#29734=B_SPLINE_CURVE_WITH_KNOTS('',3,(#132991,#132992,#132993,#132994),
 .UNSPECIFIED.,.F.,.F.,(4,4),(0.,0.999997220816645),.UNSPECIFIED.);
#29735=B_SPLINE_CURVE_WITH_KNOTS('',3,(#133062,#133063,#133064,#133065,
#133066,#133067,#133068,#133069,#133070,#133071,#133072,#133073,#133074,
#133075,#133076,#133077,#133078,#133079,#133080,#133081,#133082,#133083,
#133084,#133085,#133086,#133087,#133088,#133089),.UNSPECIFIED.,.F.,.F.,
(4,3,3,3,3,3,3,3,3,4),(0.214741457420206,0.244976288689619,0.314185121458223,
0.389489559305443,0.47162927932211,0.561313355930194,0.659220518921088,
0.766025144246682,0.882569333512905,0.992703055040362),.UNSPECIFIED.);
#29736=B_SPLINE_CURVE_WITH_KNOTS('',3,(#133091,#133092,#133093,#133094,
#133095,#133096,#133097,#133098,#133099,#133100,#133101,#133102,#133103,
#133104,#133105,#133106,#133107,#133108,#133109,#133110,#133111,#133112,
#133113,#133114,#133115,#133116,#133117,#133118),.UNSPECIFIED.,.F.,.F.,
(4,2,2,1,2,2,2,2,1,2,2,2,2,2,4),(0.00114265111152173,0.031250000000139,
0.0625000000002779,0.0937500000004169,0.109375000000459,0.125000000000502,
0.187500000000573,0.218750000000609,0.23437500000061,0.24218750000061,0.250000000000609,
0.375000000000563,0.437500000000518,0.500000000000472,1.),.UNSPECIFIED.);
#29737=B_SPLINE_CURVE_WITH_KNOTS('',3,(#133119,#133120,#133121,#133122,
#133123,#133124,#133125,#133126,#133127,#133128),.UNSPECIFIED.,.F.,.F.,
(4,3,3,4),(0.,0.419606594749395,0.828176819914611,1.),.UNSPECIFIED.);
#29738=B_SPLINE_CURVE_WITH_KNOTS('',3,(#133157,#133158,#133159,#133160),
 .UNSPECIFIED.,.F.,.F.,(4,4),(0.,1.),.UNSPECIFIED.);
#29739=B_SPLINE_CURVE_WITH_KNOTS('',3,(#133161,#133162,#133163,#133164,
#133165,#133166,#133167,#133168,#133169,#133170,#133171,#133172,#133173),
 .UNSPECIFIED.,.F.,.F.,(4,3,3,3,4),(1.30992509567256E-8,0.000738091185335242,
0.604572500785313,0.636544025568632,1.),.UNSPECIFIED.);
#29740=B_SPLINE_CURVE_WITH_KNOTS('',3,(#133207,#133208,#133209,#133210),
 .UNSPECIFIED.,.F.,.F.,(4,4),(0.,0.999998862998874),.UNSPECIFIED.);
#29741=B_SPLINE_CURVE_WITH_KNOTS('',3,(#133249,#133250,#133251,#133252),
 .UNSPECIFIED.,.F.,.F.,(4,4),(0.,0.9999560856806),.UNSPECIFIED.);
#29742=B_SPLINE_CURVE_WITH_KNOTS('',3,(#133323,#133324,#133325,#133326,
#133327,#133328,#133329,#133330,#133331,#133332),.UNSPECIFIED.,.F.,.F.,
(4,2,2,2,4),(0.,0.249999999999965,0.374999999999948,0.499999999999931,1.),
 .UNSPECIFIED.);
#29743=B_SPLINE_CURVE_WITH_KNOTS('',3,(#133334,#133335,#133336,#133337,
#133338,#133339,#133340,#133341,#133342,#133343,#133344,#133345,#133346,
#133347,#133348,#133349,#133350,#133351,#133352,#133353,#133354,#133355,
#133356,#133357,#133358,#133359,#133360,#133361,#133362,#133363,#133364,
#133365,#133366,#133367,#133368,#133369,#133370,#133371,#133372,#133373,
#133374,#133375,#133376),.UNSPECIFIED.,.F.,.F.,(4,3,3,3,3,3,3,3,3,3,3,3,
3,3,4),(0.,0.0170350126721402,0.0659003937260698,0.119026578604631,0.177082319856503,
0.240669318325304,0.309931937354791,0.384677289941797,0.464737806725433,
0.550706641745405,0.643772022188173,0.745112545500137,0.855846190868192,
0.977028739045804,1.),.UNSPECIFIED.);
#29744=B_SPLINE_CURVE_WITH_KNOTS('',3,(#133379,#133380,#133381,#133382,
#133383,#133384,#133385,#133386,#133387,#133388,#133389,#133390,#133391,
#133392,#133393,#133394,#133395,#133396,#133397,#133398,#133399,#133400,
#133401,#133402,#133403,#133404,#133405,#133406,#133407,#133408,#133409),
 .UNSPECIFIED.,.F.,.F.,(4,3,3,3,3,3,3,3,3,3,4),(0.212527788159309,0.238929210760529,
0.307690566088615,0.381894800562219,0.461375561007429,0.546721723948187,
0.639112945312709,0.739719346812922,0.849650913359874,0.96995594614347,
0.992688397423917),.UNSPECIFIED.);
#29745=B_SPLINE_CURVE_WITH_KNOTS('',3,(#133415,#133416,#133417,#133418,
#133419,#133420,#133421,#133422,#133423,#133424,#133425,#133426,#133427,
#133428,#133429,#133430,#133431,#133432,#133433,#133434,#133435,#133436,
#133437,#133438,#133439,#133440,#133441,#133442,#133443,#133444,#133445,
#133446,#133447,#133448,#133449,#133450,#133451),.UNSPECIFIED.,.F.,.F.,
(4,3,3,3,3,3,3,3,3,3,3,3,4),(1.05070778171511E-6,0.0846709690617889,0.169333918564356,
0.254017969883459,0.338685915870495,0.423368260937166,0.5,0.584710646576704,
0.669415319125059,0.754141291593392,0.838850899372478,0.923573259875887,
0.999999999818943),.UNSPECIFIED.);
#29746=B_SPLINE_CURVE_WITH_KNOTS('',3,(#133476,#133477,#133478,#133479,
#133480,#133481,#133482,#133483,#133484,#133485,#133486,#133487,#133488,
#133489,#133490,#133491,#133492,#133493,#133494,#133495,#133496,#133497,
#133498,#133499,#133500,#133501,#133502,#133503,#133504,#133505,#133506,
#133507,#133508,#133509,#133510,#133511,#133512,#133513,#133514,#133515,
#133516,#133517,#133518,#133519,#133520,#133521,#133522,#133523,#133524),
 .UNSPECIFIED.,.F.,.F.,(4,3,3,3,3,3,3,3,3,3,3,3,3,3,3,3,4),(4.14194216132566E-7,
0.0104023161409394,0.032404745883467,0.03703703703704,0.0478687762215131,
0.064929592738566,0.07407407407407,0.0852992481295061,0.103435575750171,
0.1111111111111,0.122727871410933,0.140785542467441,0.1481481481481,0.160147068559508,
0.178135173528707,0.1851851851852,0.188788270697576),.UNSPECIFIED.);
#29747=B_SPLINE_CURVE_WITH_KNOTS('',3,(#133610,#133611,#133612,#133613,
#133614,#133615,#133616,#133617,#133618,#133619,#133620,#133621,#133622,
#133623,#133624,#133625,#133626,#133627,#133628,#133629,#133630,#133631,
#133632,#133633,#133634,#133635,#133636,#133637,#133638,#133639,#133640,
#133641,#133642,#133643,#133644,#133645,#133646,#133647,#133648,#133649,
#133650,#133651,#133652,#133653,#133654,#133655,#133656,#133657,#133658,
#133659,#133660,#133661,#133662,#133663,#133664,#133665,#133666,#133667,
#133668,#133669,#133670,#133671,#133672,#133673,#133674,#133675,#133676,
#133677,#133678,#133679,#133680,#133681,#133682,#133683,#133684,#133685,
#133686,#133687,#133688,#133689,#133690,#133691,#133692,#133693,#133694,
#133695,#133696,#133697,#133698,#133699,#133700,#133701,#133702,#133703,
#133704,#133705,#133706,#133707,#133708,#133709,#133710,#133711,#133712,
#133713,#133714,#133715,#133716,#133717,#133718,#133719,#133720,#133721,
#133722,#133723,#133724,#133725,#133726,#133727,#133728,#133729,#133730),
 .UNSPECIFIED.,.F.,.F.,(4,3,3,3,3,3,3,3,3,3,3,3,3,3,3,3,3,3,3,3,3,3,3,3,
3,3,3,3,3,3,3,3,3,3,3,3,3,3,3,3,4),(1.53023996016127E-7,0.0538427975473875,
0.106014120122847,0.138416004234508,0.188613008991339,0.237253646912087,
0.249999999999905,0.29089575167527,0.332947875837564,0.374999999999858,
0.412763016597034,0.430211822807126,0.437499999999834,0.468749999999821,
0.484374999999816,0.492187499999813,0.496093749999812,0.498046874999813,
0.499999999999813,0.530073715669157,0.545349746812652,0.577232219491959,
0.612722550574342,0.624999999999838,0.667651696788102,0.6854298162725,0.687499999999852,
0.718749999999858,0.734374999999862,0.742187499999864,0.746093749999865,
0.748046874999865,0.749023437499864,0.749999999999864,0.788119952138273,
0.826960318898607,0.861440854495596,0.874999999999932,0.916050892639579,
0.958617696487004,1.),.UNSPECIFIED.);
#29748=B_SPLINE_CURVE_WITH_KNOTS('',3,(#133772,#133773,#133774,#133775,
#133776,#133777,#133778,#133779,#133780,#133781,#133782,#133783,#133784,
#133785,#133786,#133787,#133788,#133789,#133790,#133791,#133792,#133793,
#133794,#133795,#133796,#133797,#133798,#133799,#133800,#133801,#133802,
#133803,#133804,#133805,#133806,#133807,#133808,#133809,#133810,#133811,
#133812,#133813,#133814,#133815,#133816,#133817,#133818,#133819,#133820,
#133821,#133822,#133823,#133824,#133825,#133826,#133827,#133828,#133829,
#133830,#133831,#133832,#133833,#133834,#133835,#133836,#133837,#133838,
#133839,#133840,#133841,#133842,#133843,#133844,#133845,#133846,#133847),
 .UNSPECIFIED.,.F.,.F.,(4,3,3,3,3,3,3,3,3,3,3,3,3,3,3,3,3,3,3,3,3,3,3,3,
3,4),(0.,0.0456119370812063,0.0901169024201462,0.133174944288965,0.175489150215472,
0.21680962027251,0.249999999999996,0.290181447017008,0.329860550964997,
0.369132815094579,0.408091464900065,0.446827929532484,0.485444282452249,
0.524050417570924,0.562725051494045,0.601547160582328,0.640796170375351,
0.680321689677691,0.720459842891237,0.749999999999995,0.79120051762038,
0.833087720599072,0.876268031681826,0.920221939306363,0.965605219388956,
1.),.UNSPECIFIED.);
#29749=B_SPLINE_CURVE_WITH_KNOTS('',3,(#133849,#133850,#133851,#133852,
#133853,#133854,#133855,#133856,#133857,#133858,#133859,#133860,#133861,
#133862,#133863,#133864,#133865,#133866,#133867,#133868,#133869,#133870,
#133871,#133872,#133873,#133874,#133875,#133876,#133877,#133878,#133879,
#133880,#133881,#133882,#133883,#133884,#133885,#133886,#133887,#133888,
#133889,#133890,#133891,#133892,#133893,#133894,#133895,#133896,#133897,
#133898,#133899,#133900,#133901,#133902,#133903,#133904,#133905,#133906,
#133907,#133908,#133909,#133910,#133911,#133912,#133913,#133914,#133915,
#133916,#133917,#133918,#133919,#133920,#133921,#133922,#133923,#133924,
#133925,#133926,#133927),.UNSPECIFIED.,.F.,.F.,(4,3,3,3,3,3,3,3,3,3,3,3,
3,3,3,3,3,3,3,3,3,3,3,3,3,3,4),(0.,0.0579592582826019,0.117537310561431,
0.137605588686488,0.1666666666667,0.221698698493835,0.278959935509025,0.312671189889294,
0.3333333333333,0.384068668956614,0.436358111426463,0.48775592023987,0.5,
0.548139419643831,0.597217471856499,0.647741698863853,0.662828277240584,
0.6666666666667,0.710131267633883,0.753817884952815,0.797986207280148,0.8333333333333,
0.837876903054292,0.884001153291541,0.930724356583334,0.977764846540732,
1.),.UNSPECIFIED.);
#29750=B_SPLINE_CURVE_WITH_KNOTS('',3,(#133928,#133929,#133930,#133931,
#133932,#133933,#133934,#133935,#133936,#133937,#133938,#133939,#133940,
#133941,#133942,#133943,#133944,#133945,#133946,#133947,#133948,#133949,
#133950,#133951,#133952,#133953,#133954,#133955,#133956,#133957,#133958,
#133959,#133960,#133961,#133962,#133963,#133964,#133965,#133966,#133967,
#133968,#133969,#133970,#133971,#133972,#133973,#133974,#133975,#133976),
 .UNSPECIFIED.,.F.,.F.,(4,3,3,3,3,3,3,3,3,3,3,3,3,3,3,3,4),(0.,0.0730059574833017,
0.148337817232831,0.227137820373852,0.25,0.327004186947971,0.403735606439391,
0.478795951017224,0.5,0.578287285905121,0.652570479575901,0.722752191628911,
0.75,0.821415096305571,0.889388191525017,0.953935905694943,1.),
 .UNSPECIFIED.);
#29751=B_SPLINE_CURVE_WITH_KNOTS('',3,(#133980,#133981,#133982,#133983,
#133984,#133985,#133986,#133987,#133988,#133989,#133990,#133991,#133992,
#133993,#133994,#133995,#133996,#133997,#133998,#133999,#134000,#134001,
#134002,#134003,#134004,#134005,#134006,#134007,#134008,#134009,#134010,
#134011,#134012,#134013,#134014,#134015,#134016,#134017,#134018,#134019,
#134020,#134021,#134022,#134023,#134024,#134025),.UNSPECIFIED.,.F.,.F.,
(4,3,3,3,3,3,3,3,3,3,3,3,3,3,3,4),(0.,0.0690009757230223,0.139000969046554,
0.210540625571563,0.250000000000003,0.323645213950312,0.375000000000004,
0.420107205654051,0.465619287340062,0.500000000000005,0.580484011806695,
0.660881352942184,0.74112761125252,0.750000000000003,0.830053892628388,
0.87579096992742),.UNSPECIFIED.);
#29752=B_SPLINE_CURVE_WITH_KNOTS('',3,(#134026,#134027,#134028,#134029,
#134030,#134031,#134032,#134033,#134034,#134035,#134036,#134037,#134038,
#134039,#134040,#134041,#134042,#134043,#134044,#134045,#134046,#134047,
#134048,#134049,#134050,#134051,#134052,#134053,#134054,#134055,#134056,
#134057,#134058,#134059,#134060,#134061,#134062,#134063,#134064,#134065,
#134066,#134067,#134068,#134069,#134070,#134071,#134072,#134073,#134074,
#134075,#134076,#134077,#134078,#134079,#134080,#134081,#134082,#134083,
#134084,#134085,#134086,#134087,#134088,#134089),.UNSPECIFIED.,.F.,.F.,
(4,3,3,3,3,3,3,3,3,3,3,3,3,3,3,3,3,3,3,3,3,4),(9.24012471371765E-5,0.00781249999997771,
0.0123214344920132,0.0156249999999554,0.0252180688217443,0.0312499999999034,
0.0468749999998515,0.0546874999998286,0.0567075535144753,0.0616623599061952,
0.0624999999998058,0.0781249999997706,0.0859374999997557,0.0916222253068236,
0.0937499999997409,0.104842993274865,0.109374999999727,0.11718749999972,
0.121093749999716,0.123667271168975,0.124999999999712,0.125769234561334),
 .UNSPECIFIED.);
#29753=B_SPLINE_CURVE_WITH_KNOTS('',3,(#134130,#134131,#134132,#134133,
#134134,#134135,#134136,#134137,#134138,#134139,#134140,#134141,#134142,
#134143,#134144,#134145,#134146,#134147,#134148,#134149,#134150,#134151,
#134152,#134153,#134154,#134155,#134156,#134157,#134158,#134159,#134160,
#134161,#134162,#134163,#134164,#134165,#134166,#134167,#134168,#134169,
#134170,#134171,#134172,#134173,#134174,#134175,#134176,#134177,#134178,
#134179,#134180,#134181,#134182,#134183,#134184,#134185,#134186,#134187,
#134188,#134189,#134190,#134191,#134192,#134193,#134194,#134195,#134196,
#134197,#134198,#134199,#134200,#134201,#134202,#134203,#134204,#134205,
#134206,#134207,#134208,#134209,#134210,#134211,#134212,#134213,#134214,
#134215,#134216,#134217,#134218,#134219,#134220,#134221,#134222,#134223,
#134224,#134225,#134226,#134227,#134228,#134229,#134230,#134231,#134232,
#134233,#134234,#134235,#134236,#134237,#134238,#134239,#134240,#134241,
#134242,#134243,#134244,#134245,#134246,#134247,#134248,#134249,#134250,
#134251,#134252,#134253),.UNSPECIFIED.,.F.,.F.,(4,3,3,3,3,3,3,3,3,3,3,3,
3,3,3,3,3,3,3,3,3,3,3,3,3,3,3,3,3,3,3,3,3,3,3,3,3,3,3,3,3,4),(0.125769234561334,
0.156249999999699,0.171874999999696,0.179687499999699,0.18510387473411,
0.187499999999701,0.20993433329871,0.218749999999721,0.234374999999732,
0.236573630102243,0.242187499999737,0.247339650344557,0.249999999999742,
0.292365467774003,0.312499999999742,0.343749999999746,0.359374999999748,
0.368677766486324,0.37499999999975,0.407840430019361,0.441178081221039,
0.449378570186183,0.482419525033026,0.499999999999794,0.541113598173256,
0.583056799086548,0.621560046995617,0.624999999999839,0.662035042781543,
0.687499999999861,0.707481972235775,0.718749999999871,0.734701024419774,
0.749999999999882,0.785989295627372,0.821188223681543,0.855344319121138,
0.874999999999941,0.907317639185196,0.939018051031254,0.969895301305895,
1.),.UNSPECIFIED.);
#29754=B_SPLINE_CURVE_WITH_KNOTS('',3,(#134349,#134350,#134351,#134352,
#134353,#134354,#134355,#134356,#134357,#134358,#134359,#134360,#134361,
#134362,#134363,#134364,#134365,#134366,#134367,#134368,#134369,#134370,
#134371,#134372,#134373,#134374,#134375,#134376,#134377,#134378,#134379,
#134380,#134381,#134382,#134383,#134384,#134385,#134386,#134387,#134388,
#134389,#134390,#134391,#134392,#134393,#134394,#134395,#134396,#134397,
#134398,#134399,#134400,#134401,#134402,#134403,#134404,#134405,#134406,
#134407,#134408,#134409),.UNSPECIFIED.,.F.,.F.,(4,3,3,3,3,3,3,3,3,3,3,3,
3,3,3,3,3,3,3,3,4),(4.41879037505324E-7,0.00293416295367035,0.0671893044344527,
0.133594652217226,0.2,0.23548216482957,0.317741082414785,0.395209823031483,
0.4,0.468144568890046,0.571815881128029,0.6,0.682012670063369,0.700986784537182,
0.782354872297676,0.8,0.86055647464313,0.919767494757683,0.935528803203491,
0.994611937942401,1.),.UNSPECIFIED.);
#29755=B_SPLINE_CURVE_WITH_KNOTS('',3,(#134413,#134414,#134415,#134416,
#134417,#134418,#134419,#134420,#134421,#134422,#134423,#134424,#134425,
#134426,#134427,#134428,#134429,#134430,#134431,#134432,#134433,#134434),
 .UNSPECIFIED.,.F.,.F.,(4,3,3,3,3,3,3,4),(1.50238356842823E-7,0.174712592830832,
0.2,0.4,0.6,0.757840534374447,0.8,0.999999999914443),.UNSPECIFIED.);
#29756=B_SPLINE_CURVE_WITH_KNOTS('',3,(#134438,#134439,#134440,#134441,
#134442,#134443,#134444,#134445,#134446,#134447,#134448,#134449,#134450,
#134451,#134452,#134453,#134454,#134455,#134456,#134457,#134458,#134459,
#134460,#134461,#134462,#134463,#134464,#134465,#134466,#134467,#134468,
#134469,#134470,#134471,#134472,#134473,#134474,#134475,#134476,#134477,
#134478,#134479,#134480,#134481,#134482,#134483,#134484,#134485,#134486,
#134487,#134488,#134489,#134490,#134491,#134492,#134493,#134494,#134495,
#134496,#134497,#134498,#134499,#134500,#134501,#134502,#134503,#134504,
#134505,#134506,#134507,#134508,#134509,#134510,#134511,#134512,#134513,
#134514,#134515,#134516,#134517,#134518,#134519,#134520,#134521,#134522,
#134523,#134524,#134525,#134526,#134527,#134528,#134529,#134530,#134531,
#134532,#134533,#134534,#134535,#134536,#134537,#134538,#134539,#134540,
#134541,#134542,#134543,#134544,#134545,#134546,#134547,#134548,#134549,
#134550,#134551,#134552,#134553,#134554,#134555,#134556,#134557,#134558,
#134559,#134560,#134561),.UNSPECIFIED.,.F.,.F.,(4,3,3,3,3,3,3,3,3,3,3,3,
3,3,3,3,3,3,3,3,3,3,3,3,3,3,3,3,3,3,3,3,3,3,3,3,3,3,3,3,3,4),(0.,0.0279278080041807,
0.0557827086768811,0.0625000000001052,0.0899713451083436,0.11793110647808,
0.12500000000021,0.14062500000023,0.142578125000225,0.144531250000221,0.148437500000221,
0.15625000000021,0.18750000000016,0.250000000000059,0.312499999999954,0.37499999999985,
0.437499999999747,0.468749999999689,0.484374999999664,0.492187499999655,
0.498046874999639,0.499999999999631,0.535126545335568,0.562499999999678,
0.593749999999709,0.609374999999727,0.617187499999733,0.621093749999737,
0.62304687499974,0.624999999999744,0.676210940457145,0.687499999999654,
0.71874999999961,0.734374999999588,0.742187499999573,0.746093749999566,
0.748046874999562,0.749999999999559,0.82786552888256,0.874999999999779,
0.938760612897857,0.999999999913687),.UNSPECIFIED.);
#29757=B_SPLINE_CURVE_WITH_KNOTS('',3,(#134565,#134566,#134567,#134568),
 .UNSPECIFIED.,.F.,.F.,(4,4),(0.,1.),.UNSPECIFIED.);
#29758=B_SPLINE_CURVE_WITH_KNOTS('',3,(#134570,#134571,#134572,#134573,
#134574,#134575,#134576,#134577,#134578,#134579,#134580,#134581),
 .UNSPECIFIED.,.F.,.F.,(4,1,1,1,1,1,1,1,1,4),(7.9860235734547E-5,0.0276758837216907,
0.0924977068314539,0.157319299200597,0.22214089156974,0.351784076308025,
0.481427261046311,0.740713630522883,0.870356815261168,0.999999999137475),
 .UNSPECIFIED.);
#29759=B_SPLINE_CURVE_WITH_KNOTS('',3,(#134585,#134586,#134587,#134588,
#134589,#134590,#134591,#134592,#134593,#134594,#134595,#134596,#134597,
#134598,#134599,#134600,#134601,#134602,#134603,#134604,#134605,#134606,
#134607,#134608,#134609,#134610,#134611,#134612,#134613,#134614,#134615,
#134616,#134617,#134618,#134619,#134620,#134621,#134622,#134623,#134624,
#134625,#134626,#134627,#134628,#134629,#134630,#134631,#134632,#134633,
#134634,#134635,#134636,#134637,#134638,#134639,#134640,#134641,#134642,
#134643,#134644,#134645,#134646,#134647,#134648,#134649,#134650,#134651,
#134652,#134653,#134654,#134655,#134656,#134657,#134658,#134659,#134660,
#134661,#134662,#134663,#134664,#134665,#134666,#134667,#134668,#134669,
#134670,#134671,#134672,#134673,#134674,#134675,#134676,#134677,#134678,
#134679,#134680,#134681,#134682,#134683,#134684,#134685,#134686,#134687,
#134688,#134689,#134690,#134691,#134692,#134693),.UNSPECIFIED.,.F.,.F.,
(4,3,3,3,3,3,3,3,3,3,3,3,3,3,3,3,3,3,3,3,3,3,3,3,3,3,3,3,3,3,3,3,3,3,3,
3,4),(9.49981110155694E-5,0.0439079474192139,0.0874336360946032,0.122157576242435,
0.16721492818219,0.212076568275687,0.250000000000103,0.295096146098991,
0.344309653086449,0.375000000000154,0.422725953413255,0.437500000000179,
0.468750000000191,0.482012101196372,0.484375000000197,0.4921875000002,0.496093750000201,
0.499589070935268,0.500000000000202,0.551495839462826,0.601713414256964,
0.625000000000169,0.657972729458139,0.687500000000153,0.718750000000144,
0.73437500000014,0.742187500000137,0.748177025422295,0.750000000000133,
0.791495676503256,0.814047913622898,0.85483988042624,0.896403261494273,
0.939242980538536,0.956354100682218,0.99563199192476,0.999999999985943),
 .UNSPECIFIED.);
#29760=B_SPLINE_CURVE_WITH_KNOTS('',3,(#134742,#134743,#134744,#134745,
#134746,#134747,#134748,#134749,#134750,#134751,#134752,#134753,#134754,
#134755,#134756,#134757,#134758,#134759,#134760,#134761,#134762,#134763,
#134764,#134765,#134766,#134767,#134768,#134769,#134770,#134771,#134772,
#134773,#134774,#134775,#134776,#134777,#134778,#134779,#134780,#134781,
#134782,#134783,#134784,#134785,#134786,#134787,#134788,#134789,#134790,
#134791,#134792,#134793,#134794,#134795,#134796,#134797,#134798,#134799,
#134800,#134801,#134802),.UNSPECIFIED.,.F.,.F.,(4,3,3,3,3,3,3,3,3,3,3,3,
3,3,3,3,3,3,3,3,4),(0.,0.0573467126579996,0.113335897514098,0.168615343495432,
0.223030306420361,0.25,0.303580319758419,0.359382779788616,0.412115475219052,
0.464689063753643,0.517201688167575,0.569751228579584,0.622581475411049,
0.675624819261524,0.729158060796906,0.75,0.804273166293312,0.859584359029149,
0.915547401796053,0.972684308211155,0.999999999999995),.UNSPECIFIED.);
#29761=B_SPLINE_CURVE_WITH_KNOTS('',3,(#134803,#134804,#134805,#134806,
#134807,#134808,#134809,#134810,#134811,#134812,#134813,#134814,#134815,
#134816,#134817,#134818,#134819,#134820,#134821,#134822,#134823,#134824,
#134825,#134826,#134827,#134828,#134829,#134830,#134831,#134832,#134833,
#134834,#134835,#134836,#134837,#134838,#134839,#134840,#134841,#134842,
#134843,#134844,#134845,#134846,#134847,#134848,#134849,#134850,#134851,
#134852,#134853,#134854,#134855,#134856,#134857,#134858,#134859,#134860,
#134861,#134862,#134863),.UNSPECIFIED.,.F.,.F.,(4,3,3,3,3,3,3,3,3,3,3,3,
3,3,3,3,3,3,3,3,4),(7.44116098701117E-15,0.0512371487041215,0.101989469318509,
0.152519576430421,0.202910903303978,0.25,0.300261981465075,0.350846320516069,
0.40164929578049,0.453037776867762,0.5,0.552205879476937,0.605524420566545,
0.659525200433921,0.714793533787152,0.75,0.806897139877591,0.865686533687191,
0.925670351357924,0.98752344482043,1.),.UNSPECIFIED.);
#29762=B_SPLINE_CURVE_WITH_KNOTS('',3,(#134905,#134906,#134907,#134908,
#134909,#134910,#134911,#134912,#134913,#134914,#134915,#134916,#134917,
#134918,#134919,#134920,#134921,#134922,#134923,#134924,#134925,#134926,
#134927,#134928,#134929,#134930,#134931,#134932,#134933,#134934,#134935,
#134936,#134937,#134938,#134939,#134940,#134941,#134942,#134943,#134944,
#134945,#134946,#134947,#134948,#134949,#134950,#134951,#134952,#134953,
#134954,#134955,#134956,#134957,#134958,#134959,#134960,#134961,#134962,
#134963,#134964,#134965,#134966,#134967,#134968,#134969,#134970,#134971,
#134972,#134973,#134974,#134975,#134976,#134977,#134978,#134979,#134980),
 .UNSPECIFIED.,.F.,.F.,(4,3,3,3,3,3,3,3,3,3,3,3,3,3,3,3,3,3,3,3,3,3,3,3,
3,4),(0.,0.0240095347924936,0.0480575330575472,0.0624999999999994,0.0939199229640899,
0.124999999999999,0.156695647248868,0.189726142714701,0.223167127401312,
0.249999999999999,0.288838755939898,0.32816014520085,0.368106946620112,
0.374999999999999,0.422671007495536,0.471592059303987,0.499999999999999,
0.517768565868439,0.578191826686414,0.640220818655331,0.704885773476388,
0.749999999999999,0.823691392983596,0.852261955107439,0.928556327574316,
1.),.UNSPECIFIED.);
#29763=B_SPLINE_CURVE_WITH_KNOTS('',3,(#134981,#134982,#134983,#134984,
#134985,#134986,#134987,#134988,#134989,#134990,#134991,#134992,#134993),
 .UNSPECIFIED.,.F.,.F.,(4,3,3,3,4),(0.,0.392244811655611,0.5,0.76234491070066,
1.),.UNSPECIFIED.);
#29764=B_SPLINE_CURVE_WITH_KNOTS('',3,(#135035,#135036,#135037,#135038,
#135039,#135040,#135041,#135042,#135043,#135044,#135045,#135046,#135047,
#135048,#135049,#135050,#135051,#135052,#135053,#135054,#135055,#135056,
#135057,#135058,#135059,#135060,#135061),.UNSPECIFIED.,.F.,.F.,(4,2,2,1,
1,2,2,2,2,1,1,1,2,2,2,4),(0.,0.125000000000001,0.187500000000001,0.218750000000002,
0.234375000000002,0.242187500000002,0.250000000000002,0.37499999999999,
0.437499999999985,0.468749999999982,0.48437499999998,0.492187499999979,
0.496093749999979,0.49999999999998,0.74999999999999,0.999906678651906),
 .UNSPECIFIED.);
#29765=B_SPLINE_CURVE_WITH_KNOTS('',3,(#135063,#135064,#135065,#135066,
#135067,#135068,#135069,#135070,#135071,#135072,#135073,#135074,#135075),
 .UNSPECIFIED.,.F.,.F.,(4,3,3,3,4),(7.78289278789026E-10,0.237624182551005,
0.5,0.607655001033738,0.999999999858253),.UNSPECIFIED.);
#29766=B_SPLINE_CURVE_WITH_KNOTS('',3,(#135076,#135077,#135078,#135079,
#135080,#135081,#135082,#135083,#135084,#135085,#135086,#135087,#135088,
#135089,#135090,#135091,#135092,#135093,#135094,#135095,#135096,#135097,
#135098,#135099,#135100,#135101,#135102,#135103,#135104,#135105,#135106,
#135107,#135108,#135109,#135110,#135111,#135112,#135113,#135114,#135115,
#135116,#135117,#135118,#135119,#135120,#135121,#135122,#135123,#135124,
#135125,#135126,#135127,#135128,#135129,#135130,#135131,#135132,#135133,
#135134,#135135,#135136,#135137,#135138,#135139,#135140,#135141,#135142,
#135143,#135144,#135145,#135146,#135147,#135148,#135149,#135150,#135151,
#135152,#135153,#135154),.UNSPECIFIED.,.F.,.F.,(4,3,3,3,3,3,3,3,3,3,3,3,
3,3,3,3,3,3,3,3,3,3,3,3,3,3,4),(0.,0.0781417538335214,0.156283507667043,
0.229903094289744,0.25,0.314389271872266,0.377077783281621,0.43711271294967,
0.490712794158447,0.499999999999999,0.549101400831195,0.596959248933236,
0.624999999999999,0.664843799387995,0.704220170720158,0.742896099962853,
0.75,0.783424128120187,0.816659225360256,0.849374153129844,0.853956214206258,
0.875,0.906271016403279,0.9375,0.961323616750085,0.985107754960295,1.),
 .UNSPECIFIED.);
#29767=B_SPLINE_CURVE_WITH_KNOTS('',3,(#135221,#135222,#135223,#135224,
#135225,#135226,#135227,#135228,#135229,#135230,#135231,#135232,#135233,
#135234,#135235,#135236,#135237,#135238,#135239),.UNSPECIFIED.,.F.,.F.,
(4,3,3,3,3,3,4),(0.,0.181519090760199,0.362120636613677,0.542234912997426,
0.72225841896039,0.902871075785579,1.),.UNSPECIFIED.);
#29768=B_SPLINE_CURVE_WITH_KNOTS('',3,(#135240,#135241,#135242,#135243,
#135244,#135245,#135246,#135247,#135248,#135249,#135250,#135251,#135252,
#135253,#135254,#135255,#135256,#135257,#135258,#135259,#135260,#135261,
#135262,#135263,#135264,#135265,#135266,#135267,#135268,#135269,#135270,
#135271,#135272,#135273,#135274,#135275,#135276,#135277,#135278,#135279,
#135280,#135281,#135282,#135283,#135284,#135285,#135286,#135287,#135288,
#135289,#135290,#135291,#135292,#135293,#135294,#135295,#135296,#135297,
#135298,#135299,#135300,#135301,#135302,#135303,#135304,#135305,#135306,
#135307,#135308,#135309,#135310,#135311,#135312,#135313,#135314,#135315,
#135316,#135317,#135318,#135319,#135320,#135321,#135322,#135323,#135324,
#135325,#135326,#135327,#135328,#135329,#135330,#135331,#135332,#135333,
#135334,#135335,#135336,#135337,#135338,#135339,#135340,#135341,#135342,
#135343,#135344,#135345,#135346,#135347,#135348,#135349,#135350,#135351,
#135352,#135353,#135354,#135355,#135356,#135357,#135358,#135359,#135360,
#135361,#135362,#135363,#135364,#135365,#135366,#135367,#135368,#135369,
#135370,#135371,#135372,#135373,#135374,#135375,#135376,#135377,#135378,
#135379,#135380,#135381,#135382,#135383,#135384,#135385,#135386,#135387,
#135388,#135389,#135390,#135391,#135392,#135393),.UNSPECIFIED.,.F.,.F.,
(4,3,3,3,3,3,3,3,3,3,3,3,3,3,3,3,3,3,3,3,3,3,3,3,3,3,3,3,3,3,3,3,3,3,3,
3,3,3,3,3,3,3,3,3,3,3,3,3,3,3,3,4),(2.73322965884126E-10,0.0264549111194651,
0.0485516362526499,0.062499999999984,0.0850151135779835,0.0867625902511057,
0.116275778153569,0.124023437499972,0.124999999999974,0.160063595048907,
0.189301312632248,0.223901320758205,0.248046875000073,0.250000000000073,
0.28653488326189,0.292550069720856,0.326377468207769,0.364655941592613,
0.367187500000048,0.374510310049938,0.375000000000045,0.397544446166902,
0.434809267245017,0.474466284754075,0.492187500000022,0.498183594972155,
0.500000000000021,0.527222702158733,0.55616511346704,0.588322976640463,
0.596116434011651,0.609375000000011,0.618910390786312,0.62500000000001,
0.658201936263826,0.694362627592558,0.700819345682431,0.718750000000008,
0.732543917215725,0.745471055817449,0.750000000000008,0.779429696038487,
0.80209682307013,0.824435228005092,0.848926685652495,0.874561887630016,
0.900806883711232,0.905330311691599,0.927606641474703,0.951122356025715,
0.975561177979689,0.999999999933663),.UNSPECIFIED.);
#29769=B_SPLINE_CURVE_WITH_KNOTS('',3,(#135400,#135401,#135402,#135403,
#135404,#135405,#135406,#135407,#135408,#135409,#135410,#135411,#135412,
#135413,#135414,#135415,#135416,#135417,#135418,#135419,#135420,#135421,
#135422,#135423,#135424,#135425,#135426,#135427,#135428,#135429,#135430,
#135431,#135432,#135433,#135434,#135435,#135436,#135437,#135438,#135439,
#135440,#135441,#135442,#135443,#135444,#135445,#135446,#135447,#135448,
#135449,#135450,#135451,#135452,#135453,#135454,#135455,#135456,#135457,
#135458,#135459,#135460,#135461,#135462,#135463,#135464,#135465,#135466,
#135467,#135468,#135469,#135470,#135471,#135472,#135473,#135474,#135475,
#135476,#135477,#135478,#135479,#135480,#135481,#135482,#135483,#135484,
#135485,#135486,#135487,#135488,#135489,#135490,#135491,#135492,#135493,
#135494,#135495,#135496,#135497,#135498,#135499,#135500,#135501,#135502,
#135503,#135504,#135505,#135506,#135507,#135508,#135509,#135510,#135511,
#135512,#135513,#135514,#135515,#135516,#135517,#135518,#135519,#135520,
#135521,#135522,#135523,#135524,#135525,#135526,#135527,#135528,#135529,
#135530,#135531,#135532,#135533,#135534,#135535,#135536,#135537,#135538,
#135539,#135540,#135541,#135542,#135543,#135544,#135545,#135546,#135547,
#135548,#135549,#135550,#135551,#135552,#135553,#135554,#135555,#135556,
#135557,#135558,#135559,#135560,#135561,#135562,#135563,#135564,#135565,
#135566,#135567,#135568,#135569,#135570,#135571,#135572,#135573,#135574),
 .UNSPECIFIED.,.F.,.F.,(4,3,3,3,3,3,3,3,3,3,3,3,3,3,3,3,3,3,3,3,3,3,3,3,
3,3,3,3,3,3,3,3,3,3,3,3,3,3,3,3,3,3,3,3,3,3,3,3,3,3,3,3,3,3,3,3,3,3,4),
(8.96765241561959E-11,0.0241198469644619,0.0474038529016274,0.0625000000000184,
0.0836216493288717,0.0973629920783003,0.109375000000032,0.116503694188718,
0.123844299441502,0.125000000000036,0.147610163784958,0.170591682874619,
0.193590311413262,0.196215774040552,0.218750000000064,0.231600729773752,
0.245051809224319,0.250000000000072,0.277441233902207,0.301886806087822,
0.338443403043965,0.368343375402564,0.375000000000108,0.394858108367889,
0.401874435804676,0.424366897198985,0.437500000000125,0.475573217952329,
0.492187500000139,0.497520504312495,0.50000000000014,0.534667154153412,
0.546875000000145,0.557645435349896,0.562500000000147,0.59375000000015,
0.596577244630875,0.61546646504238,0.625000000000153,0.66314840319689,0.698751804371271,
0.737883241891824,0.746093750000162,0.750000000000161,0.785934144325005,
0.800108539909645,0.837065988704875,0.871303163694748,0.874023437500105,
0.875000000000105,0.898592058160894,0.9047087781261,0.92187500000007,0.936535331259133,
0.937500000000057,0.955831751877182,0.976381324473505,0.992332357317893,
0.999999999999997),.UNSPECIFIED.);
#29770=B_SPLINE_CURVE_WITH_KNOTS('',3,(#135633,#135634,#135635,#135636,
#135637,#135638,#135639,#135640,#135641,#135642),.UNSPECIFIED.,.F.,.F.,
(4,2,2,2,4),(0.,0.25,0.5,0.75,1.),.UNSPECIFIED.);
#29771=B_SPLINE_CURVE_WITH_KNOTS('',3,(#135645,#135646,#135647,#135648,
#135649,#135650,#135651,#135652,#135653,#135654,#135655,#135656,#135657,
#135658,#135659,#135660,#135661,#135662,#135663,#135664,#135665,#135666,
#135667,#135668,#135669,#135670,#135671,#135672,#135673,#135674,#135675),
 .UNSPECIFIED.,.F.,.F.,(4,3,3,3,3,3,3,3,3,3,4),(0.,0.125000017210984,0.250000014806018,
0.375000012401051,0.500000009996085,0.62500000759112,0.750000005186153,
0.812500003983669,0.875000002781187,0.937500001578704,1.),.UNSPECIFIED.);
#29772=B_SPLINE_CURVE_WITH_KNOTS('',3,(#135676,#135677,#135678,#135679,
#135680,#135681,#135682,#135683,#135684,#135685,#135686,#135687,#135688,
#135689,#135690,#135691,#135692,#135693,#135694,#135695,#135696,#135697,
#135698,#135699,#135700,#135701,#135702,#135703,#135704,#135705,#135706,
#135707,#135708,#135709,#135710,#135711,#135712,#135713,#135714,#135715,
#135716,#135717,#135718,#135719,#135720,#135721,#135722,#135723,#135724,
#135725,#135726,#135727,#135728,#135729,#135730,#135731,#135732,#135733,
#135734,#135735,#135736,#135737,#135738,#135739,#135740,#135741,#135742,
#135743,#135744,#135745,#135746,#135747,#135748,#135749,#135750,#135751,
#135752,#135753,#135754,#135755,#135756,#135757,#135758,#135759,#135760,
#135761,#135762,#135763,#135764,#135765,#135766,#135767,#135768,#135769,
#135770,#135771,#135772,#135773,#135774,#135775,#135776,#135777,#135778,
#135779,#135780,#135781,#135782,#135783,#135784,#135785,#135786,#135787,
#135788,#135789,#135790,#135791,#135792,#135793,#135794,#135795,#135796,
#135797,#135798,#135799,#135800,#135801,#135802,#135803,#135804,#135805,
#135806,#135807,#135808,#135809,#135810,#135811,#135812,#135813,#135814,
#135815,#135816,#135817,#135818,#135819,#135820,#135821,#135822,#135823,
#135824,#135825,#135826,#135827,#135828,#135829,#135830,#135831,#135832,
#135833,#135834,#135835,#135836,#135837,#135838),.UNSPECIFIED.,.F.,.F.,
(4,3,3,3,3,3,3,3,3,3,3,3,3,3,3,3,3,3,3,3,3,3,3,3,3,3,3,3,3,3,3,3,3,3,3,
3,3,3,3,3,3,3,3,3,3,3,3,3,3,3,3,3,3,3,4),(4.48981150760254E-9,0.0393536153485956,
0.0624999999999912,0.0937499999999866,0.109374999999985,0.117187499999983,
0.121093749999983,0.124999999999982,0.154799793759501,0.184939633053664,
0.215527805974844,0.218749999999966,0.234374999999964,0.242187499999962,
0.248759787824685,0.249999999999961,0.276843317058182,0.303796959875753,
0.330874054305417,0.343749999999956,0.359374999999956,0.367187499999956,
0.374999999999956,0.400813537045637,0.426642884048751,0.452475164185863,
0.478308677755654,0.499999999999977,0.525829006322467,0.551657601353355,
0.577482865841678,0.593749999999991,0.609374999999993,0.617187499999993,
0.624999999999994,0.651988603271001,0.67892648510348,0.705754490984526,
0.718749999999989,0.734374999999988,0.742187499999988,0.749108314032712,
0.749999999999988,0.780820961713403,0.812285480856701,0.84375,0.859375000000001,
0.867187500000002,0.871093750000002,0.874779879052441,0.875000000000003,
0.91517837097112,0.954934021116031,0.994126825971164,0.999999999998253),
 .UNSPECIFIED.);
#29773=B_SPLINE_CURVE_WITH_KNOTS('',3,(#136157,#136158,#136159,#136160,
#136161,#136162,#136163,#136164,#136165,#136166,#136167,#136168,#136169,
#136170,#136171,#136172,#136173,#136174,#136175,#136176,#136177,#136178,
#136179,#136180,#136181,#136182,#136183,#136184,#136185,#136186,#136187,
#136188,#136189,#136190,#136191,#136192,#136193,#136194,#136195,#136196,
#136197,#136198,#136199,#136200,#136201,#136202,#136203,#136204,#136205,
#136206,#136207,#136208,#136209,#136210,#136211,#136212,#136213,#136214,
#136215,#136216,#136217,#136218,#136219,#136220,#136221,#136222,#136223,
#136224,#136225,#136226,#136227,#136228,#136229,#136230,#136231,#136232,
#136233,#136234,#136235,#136236,#136237,#136238,#136239,#136240,#136241,
#136242,#136243,#136244,#136245,#136246,#136247,#136248,#136249,#136250,
#136251,#136252,#136253,#136254,#136255,#136256,#136257,#136258,#136259,
#136260,#136261,#136262,#136263,#136264,#136265,#136266,#136267,#136268,
#136269,#136270,#136271,#136272,#136273,#136274,#136275,#136276,#136277,
#136278,#136279,#136280,#136281,#136282,#136283,#136284,#136285,#136286,
#136287,#136288,#136289,#136290,#136291,#136292,#136293,#136294,#136295,
#136296,#136297,#136298,#136299,#136300,#136301,#136302,#136303,#136304,
#136305,#136306,#136307,#136308,#136309,#136310,#136311,#136312,#136313,
#136314,#136315,#136316,#136317,#136318,#136319,#136320,#136321,#136322,
#136323,#136324,#136325,#136326,#136327,#136328,#136329,#136330,#136331,
#136332,#136333,#136334,#136335,#136336,#136337,#136338,#136339,#136340,
#136341,#136342,#136343,#136344,#136345,#136346,#136347,#136348,#136349,
#136350,#136351,#136352,#136353,#136354,#136355,#136356,#136357,#136358,
#136359,#136360,#136361,#136362,#136363,#136364,#136365,#136366,#136367,
#136368,#136369,#136370,#136371,#136372,#136373,#136374,#136375,#136376,
#136377,#136378,#136379,#136380,#136381,#136382,#136383,#136384,#136385,
#136386,#136387,#136388,#136389,#136390,#136391,#136392,#136393,#136394,
#136395,#136396,#136397,#136398,#136399,#136400,#136401,#136402,#136403),
 .UNSPECIFIED.,.F.,.F.,(4,3,3,3,3,3,3,3,3,3,3,3,3,3,3,3,3,3,3,3,3,3,3,3,
3,3,3,3,3,3,3,3,3,3,3,3,3,3,3,3,3,3,3,3,3,3,3,3,3,3,3,3,3,3,3,3,3,3,3,3,
3,3,3,3,3,3,3,3,3,3,3,3,3,3,3,3,3,3,3,3,3,3,4),(0.,0.0182036326055988,0.0365586805154091,
0.0549664507454061,0.0618630850421433,0.0625000000000037,0.082871203764013,
0.0937500000000058,0.109375000000006,0.117187500000006,0.121093750000007,
0.123955543489655,0.125000000000008,0.141772636856682,0.160701514674118,
0.179933095227437,0.187500000000012,0.206742027831368,0.218750000000015,
0.221802188213591,0.234375000000016,0.242187500000016,0.246587970153079,
0.250000000000015,0.269649006232186,0.289649551960229,0.302311004851823,
0.312500000000011,0.331828586949002,0.34375000000001,0.359375000000009,
0.367187500000009,0.371839982042231,0.375000000000009,0.381564892865856,
0.401351920256644,0.420725587216239,0.440719294822623,0.460713002429007,
0.480356501214506,0.500000000000005,0.519655374734875,0.539310749469746,
0.55873928442422,0.562500000000005,0.582101419253175,0.593750000000003,
0.609375000000003,0.617187500000004,0.618517773284973,0.623131725816646,
0.625000000000005,0.643925066155593,0.663072701417495,0.682366749879823,
0.687500000000011,0.697796532795641,0.717621058411164,0.718750000000013,
0.734375000000014,0.742187500000014,0.746829629420927,0.750000000000014,
0.769077781416545,0.778274111050064,0.79759938395752,0.812500000000014,
0.831723467455908,0.843750000000013,0.858266019020329,0.859375000000013,
0.867187500000012,0.871093750000012,0.873908642882608,0.875000000000011,
0.894275615001603,0.913642445688952,0.932986570725005,0.93820730918229,
0.957307698559546,0.97634626547438,0.995134148476193,0.999999998885172),
 .UNSPECIFIED.);
#29774=B_SPLINE_CURVE_WITH_KNOTS('',3,(#136406,#136407,#136408,#136409,
#136410,#136411,#136412,#136413,#136414,#136415,#136416,#136417,#136418,
#136419,#136420,#136421,#136422,#136423,#136424,#136425,#136426,#136427,
#136428,#136429,#136430,#136431,#136432,#136433,#136434,#136435,#136436,
#136437,#136438,#136439,#136440,#136441,#136442,#136443,#136444,#136445,
#136446,#136447,#136448,#136449,#136450,#136451,#136452,#136453,#136454,
#136455,#136456,#136457,#136458,#136459,#136460,#136461,#136462,#136463,
#136464,#136465,#136466,#136467,#136468,#136469,#136470,#136471,#136472,
#136473,#136474,#136475,#136476,#136477,#136478,#136479,#136480,#136481,
#136482,#136483,#136484,#136485,#136486,#136487,#136488,#136489,#136490,
#136491,#136492,#136493,#136494,#136495,#136496,#136497,#136498,#136499,
#136500,#136501,#136502,#136503,#136504,#136505,#136506,#136507,#136508,
#136509,#136510,#136511,#136512,#136513,#136514,#136515,#136516,#136517,
#136518,#136519,#136520),.UNSPECIFIED.,.F.,.F.,(4,3,3,3,3,3,3,3,3,3,3,3,
3,3,3,3,3,3,3,3,3,3,3,3,3,3,3,3,3,3,3,3,3,3,3,3,3,3,4),(0.,0.0312499994700485,
0.0620396289050024,0.0935803778640139,0.124999997880194,0.159516816915742,
0.187499996904519,0.215676877869275,0.244239375088295,0.249999995928844,
0.276585162517748,0.303351488571435,0.312499994953169,0.36324402498958,
0.374999993977494,0.418857054128309,0.437499993001819,0.466980128711126,
0.496376788249355,0.499999992026143,0.533828245823419,0.562499991050468,
0.601187995873233,0.624999990074793,0.662802044869547,0.687499989099118,
0.715357883472307,0.742917981241798,0.749999988123444,0.776876675242584,
0.803610334516972,0.830278666812802,0.856879045765974,0.874999986172094,
0.903656784953601,0.932051835173095,0.960238948507373,0.988060471740437,
1.),.UNSPECIFIED.);
#29775=B_SPLINE_CURVE_WITH_KNOTS('',3,(#136523,#136524,#136525,#136526,
#136527,#136528,#136529,#136530,#136531,#136532),.UNSPECIFIED.,.F.,.F.,
(4,2,2,2,4),(0.,0.25,0.5,0.75,1.),.UNSPECIFIED.);
#29776=B_SPLINE_CURVE_WITH_KNOTS('',3,(#136820,#136821,#136822,#136823,
#136824,#136825,#136826,#136827,#136828,#136829,#136830,#136831,#136832,
#136833),.UNSPECIFIED.,.F.,.F.,(4,1,1,1,1,1,1,1,1,1,1,4),(2.16135430569987E-6,
0.0624986405827758,0.124998731210682,0.187498821838588,0.249998912466494,
0.3124990030944,0.374999093722306,0.499999274978118,0.624999456233931,0.749999637489742,
0.874999818745554,1.),.UNSPECIFIED.);
#29777=B_SPLINE_CURVE_WITH_KNOTS('',3,(#136835,#136836,#136837,#136838,
#136839,#136840,#136841,#136842,#136843,#136844,#136845,#136846),
 .UNSPECIFIED.,.F.,.F.,(4,2,2,2,2,4),(1.00000004342141E-6,0.403419775728668,
0.804091688335629,1.59898592457929,2.38592377386386,3.42850354275929),
 .UNSPECIFIED.);
#29778=B_SPLINE_CURVE_WITH_KNOTS('',3,(#136847,#136848,#136849,#136850,
#136851,#136852,#136853,#136854,#136855,#136856,#136857,#136858,#136859,
#136860,#136861,#136862,#136863,#136864,#136865,#136866,#136867,#136868,
#136869,#136870,#136871,#136872,#136873,#136874,#136875,#136876,#136877,
#136878,#136879,#136880,#136881,#136882,#136883,#136884,#136885,#136886,
#136887,#136888,#136889,#136890,#136891,#136892,#136893,#136894,#136895,
#136896,#136897,#136898,#136899,#136900,#136901),.UNSPECIFIED.,.F.,.F.,
(4,3,3,3,3,3,3,3,3,3,3,3,3,3,3,3,3,3,4),(0.,0.1249992580603,0.2499985161206,
0.3124981451508,0.3437479596658,0.3515604132946,0.355466640109,0.3593728669234,
0.3671853205522,0.3749977741809,0.4374974032111,0.4999970322412,0.6249962903015,
0.6874959193317,0.7499955483619,0.812495177392,0.8749948064222,0.9374944354523,
0.999997046746475),.UNSPECIFIED.);
#29779=B_SPLINE_CURVE_WITH_KNOTS('',3,(#137189,#137190,#137191,#137192,
#137193,#137194,#137195,#137196,#137197,#137198,#137199,#137200),
 .UNSPECIFIED.,.F.,.F.,(4,2,2,2,2,4),(-3.42848865728252,-2.38586959064534,
-1.59889051136132,-0.80404245339222,-0.403394192455397,-1.00000004321643E-6),
 .UNSPECIFIED.);
#29780=B_SPLINE_CURVE_WITH_KNOTS('',3,(#137201,#137202,#137203,#137204,
#137205,#137206,#137207,#137208,#137209,#137210,#137211,#137212,#137213,
#137214,#137215,#137216,#137217,#137218,#137219,#137220,#137221,#137222,
#137223,#137224,#137225,#137226,#137227,#137228,#137229,#137230,#137231,
#137232,#137233,#137234,#137235,#137236,#137237,#137238,#137239,#137240,
#137241,#137242,#137243,#137244,#137245,#137246,#137247,#137248,#137249,
#137250,#137251,#137252,#137253,#137254,#137255,#137256,#137257,#137258,
#137259,#137260,#137261,#137262,#137263,#137264,#137265,#137266,#137267,
#137268,#137269,#137270,#137271,#137272,#137273,#137274,#137275,#137276,
#137277,#137278,#137279,#137280,#137281,#137282,#137283,#137284,#137285,
#137286,#137287,#137288,#137289,#137290,#137291,#137292,#137293,#137294,
#137295,#137296,#137297,#137298,#137299,#137300,#137301,#137302,#137303,
#137304,#137305,#137306,#137307,#137308,#137309,#137310,#137311,#137312,
#137313,#137314,#137315,#137316,#137317,#137318,#137319,#137320,#137321,
#137322,#137323,#137324,#137325,#137326,#137327,#137328,#137329,#137330,
#137331,#137332,#137333,#137334,#137335,#137336,#137337,#137338,#137339,
#137340,#137341,#137342,#137343,#137344,#137345,#137346,#137347,#137348,
#137349,#137350,#137351,#137352,#137353,#137354,#137355,#137356,#137357,
#137358,#137359,#137360,#137361,#137362,#137363,#137364,#137365,#137366,
#137367,#137368,#137369,#137370,#137371,#137372,#137373,#137374,#137375,
#137376,#137377,#137378,#137379,#137380,#137381,#137382,#137383,#137384,
#137385,#137386,#137387,#137388,#137389,#137390,#137391,#137392,#137393,
#137394,#137395,#137396,#137397,#137398,#137399,#137400,#137401,#137402,
#137403,#137404,#137405,#137406,#137407,#137408,#137409,#137410,#137411,
#137412,#137413,#137414,#137415,#137416,#137417,#137418,#137419,#137420,
#137421,#137422,#137423,#137424,#137425,#137426,#137427,#137428,#137429,
#137430,#137431,#137432,#137433,#137434,#137435,#137436,#137437,#137438,
#137439,#137440,#137441,#137442,#137443,#137444,#137445,#137446,#137447,
#137448,#137449,#137450,#137451,#137452,#137453,#137454,#137455,#137456,
#137457,#137458,#137459,#137460,#137461,#137462,#137463,#137464,#137465,
#137466,#137467,#137468,#137469,#137470,#137471,#137472,#137473,#137474,
#137475,#137476,#137477,#137478,#137479,#137480,#137481,#137482,#137483,
#137484,#137485,#137486,#137487,#137488,#137489,#137490,#137491,#137492,
#137493,#137494,#137495,#137496,#137497,#137498,#137499,#137500,#137501,
#137502,#137503,#137504,#137505,#137506,#137507,#137508,#137509,#137510,
#137511,#137512,#137513,#137514,#137515,#137516,#137517,#137518,#137519,
#137520,#137521,#137522,#137523,#137524,#137525,#137526,#137527,#137528,
#137529,#137530,#137531,#137532,#137533,#137534,#137535,#137536,#137537,
#137538,#137539,#137540,#137541,#137542,#137543,#137544,#137545,#137546,
#137547,#137548,#137549,#137550,#137551,#137552,#137553,#137554,#137555,
#137556,#137557,#137558,#137559,#137560,#137561,#137562,#137563,#137564,
#137565,#137566,#137567,#137568,#137569,#137570,#137571,#137572,#137573,
#137574,#137575,#137576,#137577,#137578,#137579,#137580,#137581,#137582,
#137583,#137584,#137585,#137586,#137587,#137588,#137589,#137590,#137591,
#137592,#137593,#137594,#137595,#137596,#137597,#137598,#137599,#137600,
#137601,#137602,#137603,#137604,#137605,#137606,#137607,#137608,#137609),
 .UNSPECIFIED.,.F.,.F.,(4,3,3,3,3,3,3,3,3,3,3,3,3,3,3,3,3,3,3,3,3,3,3,3,
3,3,3,3,3,3,3,3,3,3,3,3,3,3,3,3,3,3,3,3,3,3,3,3,3,3,3,3,3,3,3,3,3,3,3,3,
3,3,3,3,3,3,3,3,3,3,3,3,3,3,3,3,3,3,3,3,3,3,3,3,3,3,3,3,3,3,3,3,3,3,3,3,
3,3,3,3,3,3,3,3,3,3,3,3,3,3,3,3,3,3,3,3,3,3,3,3,3,3,3,3,3,3,3,3,3,3,3,3,
3,3,3,3,4),(6.47368976766051E-6,0.00725838257496969,0.0141323813951552,
0.0156249999999179,0.0221230041052499,0.0234374999998775,0.0278231632375317,
0.0312499999998371,0.0412979481287643,0.0515362268175401,0.0546874999997163,
0.0585937499996962,0.0614614635536616,0.0624225099282763,0.0624999999996762,
0.0692488858490118,0.0759171946668936,0.0824400660205615,0.0859374999995616,
0.0898437499995427,0.0917968749995329,0.093362181664774,0.0937499999995232,
0.101619833110208,0.109489660904306,0.1171874999994,0.121093749999379,0.12304687499937,
0.124023437499365,0.124511718749363,0.124999999999361,0.125000421843579,
0.156249999999298,0.171874999999267,0.179687499999252,0.183593749999245,
0.187255859374237,0.187499999999235,0.187812734412932,0.193285114515677,
0.198943721724235,0.204940610861751,0.210937499999267,0.214843749999272,
0.216796874999274,0.217773437499276,0.21864351577971,0.218749999999278,
0.224777092603502,0.230968753176944,0.237434536816778,0.242187499999301,
0.246093749999304,0.248046874999305,0.249023437499305,0.249999999999305,
0.250000896937272,0.258949631909927,0.26861453161126,0.279019268751896,
0.291936888674985,0.296874999999176,0.304687499999154,0.308593749999144,
0.310546874999139,0.311523437499137,0.312011718749137,0.312438123073067,
0.312499999999136,0.327192126832278,0.342180569775975,0.357615807070226,
0.35937499999909,0.367187499999082,0.371093749999079,0.373046874999077,
0.374023437499076,0.374511718749076,0.37486588780349,0.374999999999077,
0.389541902170744,0.405702934607373,0.421874999999136,0.429687499999146,
0.433593749999152,0.435546874999154,0.437499999999156,0.450421377890763,
0.4637608580172,0.477821333311977,0.484374999999216,0.492187499999226,0.496093749999231,
0.498046874999233,0.499023437499234,0.499511718749235,0.499999999999237,
0.50000061815793,0.518844646217501,0.539458313992307,0.563321627450737,
0.580035098181879,0.599659339325083,0.609374999999321,0.617187499999327,
0.621093749999329,0.623046874999331,0.624023437499331,0.62475585937433,
0.624912515890386,0.62499999999933,0.632203687527198,0.639579179896025,
0.643289262967552,0.647014480029964,0.654511066905249,0.685142110349945,
0.718749999999486,0.734374999999512,0.742187499999524,0.74609374999953,
0.749023437499535,0.749862397068581,0.749999999999536,0.796874999999623,
0.833576459585674,0.843749999999709,0.859374999999738,0.867187499999752,
0.871093749999759,0.873046874999763,0.874991355581291,0.874999999999767,
0.902852656589029,0.932807157055022,0.964284959295619,1.),.UNSPECIFIED.);
#29781=B_SPLINE_CURVE_WITH_KNOTS('',3,(#137835,#137836,#137837,#137838,
#137839,#137840,#137841,#137842,#137843,#137844,#137845,#137846),
 .UNSPECIFIED.,.F.,.F.,(4,2,2,2,2,4),(5.39127788108557E-6,0.702745616718545,
1.35698856532349,2.35941555843787,3.02455033620795,3.69163212190561),
 .UNSPECIFIED.);
#29782=B_SPLINE_CURVE_WITH_KNOTS('',3,(#137850,#137851,#137852,#137853,
#137854,#137855,#137856,#137857,#137858,#137859,#137860,#137861,#137862,
#137863,#137864,#137865,#137866,#137867,#137868,#137869,#137870,#137871,
#137872,#137873,#137874,#137875,#137876,#137877,#137878,#137879,#137880),
 .UNSPECIFIED.,.F.,.F.,(4,3,3,3,3,3,3,3,3,3,4),(0.,0.149815463957079,0.25,
0.402389145397824,0.4375,0.481435618988557,0.5,0.638702449716338,0.775917053246462,
0.911161507515076,1.),.UNSPECIFIED.);
#29783=B_SPLINE_CURVE_WITH_KNOTS('',3,(#137883,#137884,#137885,#137886,
#137887,#137888,#137889,#137890,#137891,#137892),.UNSPECIFIED.,.F.,.F.,
(4,2,2,2,4),(0.,0.25,0.5,0.75,1.),.UNSPECIFIED.);
#29784=B_SPLINE_CURVE_WITH_KNOTS('',3,(#137897,#137898,#137899,#137900,
#137901,#137902,#137903,#137904,#137905,#137906,#137907,#137908,#137909,
#137910,#137911,#137912,#137913,#137914,#137915,#137916,#137917,#137918,
#137919,#137920,#137921,#137922,#137923,#137924,#137925,#137926,#137927,
#137928,#137929,#137930,#137931,#137932),.UNSPECIFIED.,.F.,.F.,(4,2,2,2,
1,1,1,2,2,2,2,2,2,2,1,1,1,2,2,2,4),(0.,0.124999999999928,0.187499999999891,
0.218749999999872,0.234374999999863,0.242187499999859,0.246093749999857,
0.248046874999856,0.249999999999856,0.374999999999863,0.499999999999871,
0.624999999999879,0.687499999999884,0.718749999999886,0.734374999999888,
0.742187499999889,0.746093749999889,0.74804687499989,0.74999999999989,0.874999999999945,
1.),.UNSPECIFIED.);
#29785=B_SPLINE_CURVE_WITH_KNOTS('',3,(#137935,#137936,#137937,#137938,
#137939,#137940,#137941,#137942,#137943,#137944,#137945,#137946,#137947,
#137948,#137949,#137950,#137951,#137952,#137953,#137954,#137955,#137956,
#137957,#137958,#137959,#137960,#137961,#137962,#137963,#137964,#137965,
#137966,#137967,#137968,#137969,#137970,#137971,#137972,#137973,#137974,
#137975,#137976,#137977,#137978,#137979,#137980,#137981,#137982,#137983,
#137984,#137985,#137986,#137987,#137988,#137989,#137990,#137991,#137992,
#137993,#137994,#137995,#137996,#137997,#137998,#137999,#138000,#138001,
#138002,#138003,#138004,#138005,#138006,#138007,#138008,#138009,#138010,
#138011,#138012,#138013,#138014,#138015,#138016,#138017,#138018,#138019,
#138020,#138021,#138022,#138023,#138024,#138025,#138026,#138027,#138028,
#138029,#138030,#138031,#138032,#138033,#138034,#138035,#138036,#138037,
#138038,#138039,#138040,#138041,#138042,#138043,#138044,#138045,#138046,
#138047,#138048,#138049,#138050,#138051,#138052,#138053,#138054,#138055,
#138056,#138057,#138058,#138059,#138060,#138061,#138062,#138063,#138064,
#138065,#138066,#138067,#138068,#138069,#138070,#138071,#138072,#138073,
#138074,#138075,#138076,#138077,#138078,#138079,#138080,#138081,#138082,
#138083,#138084,#138085,#138086,#138087,#138088,#138089,#138090,#138091,
#138092,#138093,#138094,#138095,#138096,#138097,#138098,#138099,#138100,
#138101,#138102,#138103,#138104,#138105,#138106,#138107,#138108,#138109,
#138110,#138111,#138112,#138113,#138114,#138115,#138116,#138117,#138118,
#138119,#138120,#138121,#138122,#138123,#138124),.UNSPECIFIED.,.F.,.F.,
(4,3,3,3,3,3,3,3,3,3,3,3,3,3,3,3,3,3,3,3,3,3,3,3,3,3,3,3,3,3,3,3,3,3,3,
3,3,3,3,3,3,3,3,3,3,3,3,3,3,3,3,3,3,3,3,3,3,3,3,3,3,3,3,4),(7.48046056638122E-14,
0.0567206634532088,0.062499999999308,0.0937499999989595,0.109374999998785,
0.117187499998698,0.121093749998655,0.123046874998633,0.124023437498624,
0.124999999998615,0.136819606049853,0.148727050045804,0.156249999998778,
0.168434086306113,0.17187499999886,0.179687499998901,0.183593749998921,
0.185546874998933,0.186523437498939,0.187499999998944,0.212520418034415,
0.218749999999069,0.234374999999131,0.242187499999162,0.246093749999176,
0.249793570825364,0.249999999999189,0.292343721475176,0.312499999999426,
0.343749999999545,0.359374999999606,0.367187499999637,0.371093749999655,
0.374511718749671,0.374999999999672,0.391450481329379,0.408065573550668,
0.424947768379996,0.437499999999929,0.455064117344876,0.468750000000057,
0.484375000000121,0.492187500000154,0.49609375000017,0.498046875000178,
0.499023437500183,0.499511718750185,0.500000000000188,0.543812045995623,
0.587944303750082,0.625000000000253,0.687500000000286,0.718750000000301,
0.734375000000308,0.742187500000312,0.749023437500313,0.750000000000313,
0.792697234305152,0.835164563984767,0.875000000000156,0.910161204145841,
0.944986000859805,0.979192521511994,1.),.UNSPECIFIED.);
#29786=B_SPLINE_CURVE_WITH_KNOTS('',3,(#138233,#138234,#138235,#138236,
#138237,#138238,#138239,#138240,#138241),.UNSPECIFIED.,.F.,.F.,(4,1,1,1,
1,1,4),(0.,0.249667236143351,0.375008055254049,0.500348874364846,0.625689693475543,
0.75103051258624,1.),.UNSPECIFIED.);
#29787=B_SPLINE_CURVE_WITH_KNOTS('',3,(#138242,#138243,#138244,#138245,
#138246,#138247,#138248,#138249,#138250),.UNSPECIFIED.,.F.,.F.,(4,1,1,1,
1,1,4),(0.,0.2489687868754,0.3743093060332,0.499649825191,0.6249903443489,
0.7503308635067,1.),.UNSPECIFIED.);
#29788=B_SPLINE_CURVE_WITH_KNOTS('',3,(#138368,#138369,#138370,#138371,
#138372,#138373,#138374,#138375,#138376),.UNSPECIFIED.,.F.,.F.,(4,1,1,1,
1,1,4),(0.,0.249612957690097,0.37469441872057,0.499775879751044,0.624857340781618,
0.749938801812092,1.),.UNSPECIFIED.);
#29789=B_SPLINE_CURVE_WITH_KNOTS('',3,(#138393,#138394,#138395,#138396,
#138397,#138398,#138399,#138400,#138401,#138402,#138403,#138404,#138405,
#138406,#138407,#138408,#138409,#138410,#138411),.UNSPECIFIED.,.F.,.F.,
(4,3,3,3,3,3,4),(0.,0.249979519116017,0.3749906021302,0.500001685144484,
0.625012768158668,0.750023851172851,1.),.UNSPECIFIED.);
#29790=B_SPLINE_CURVE_WITH_KNOTS('',3,(#138556,#138557,#138558,#138559,
#138560,#138561,#138562,#138563,#138564),.UNSPECIFIED.,.F.,.F.,(4,1,1,1,
1,1,4),(0.,0.249978015946122,0.374989466361611,0.500000916777201,0.62501236719269,
0.750023817608178,1.),.UNSPECIFIED.);
#29791=B_SPLINE_CURVE_WITH_KNOTS('',3,(#138651,#138652,#138653,#138654,
#138655,#138656,#138657,#138658,#138659,#138660,#138661,#138662,#138663),
 .UNSPECIFIED.,.F.,.F.,(4,2,2,2,2,1,4),(0.,0.250000000000001,0.500000000000002,
0.625000000000002,0.750000000000001,0.875000000000001,1.),.UNSPECIFIED.);
#29792=B_SPLINE_CURVE_WITH_KNOTS('',3,(#138668,#138669,#138670,#138671,
#138672,#138673,#138674,#138675,#138676,#138677,#138678,#138679,#138680,
#138681,#138682,#138683,#138684,#138685,#138686,#138687,#138688,#138689,
#138690,#138691,#138692,#138693,#138694,#138695,#138696,#138697,#138698,
#138699,#138700,#138701,#138702,#138703),.UNSPECIFIED.,.F.,.F.,(4,2,2,2,
1,1,1,2,2,2,2,2,2,2,1,1,1,2,2,2,4),(0.,0.124999999999949,0.187499999999923,
0.218749999999911,0.234374999999906,0.242187499999904,0.246093749999903,
0.248046874999902,0.249999999999901,0.374999999999893,0.499999999999885,
0.624999999999877,0.687499999999873,0.718749999999871,0.73437499999987,
0.74218749999987,0.746093749999869,0.748046874999869,0.749999999999869,
0.874999999999935,1.),.UNSPECIFIED.);
#29793=B_SPLINE_CURVE_WITH_KNOTS('',3,(#138706,#138707,#138708,#138709,
#138710,#138711,#138712,#138713,#138714,#138715),.UNSPECIFIED.,.F.,.F.,
(4,2,2,2,4),(0.,0.25,0.5,0.75,1.),.UNSPECIFIED.);
#29794=B_SPLINE_CURVE_WITH_KNOTS('',3,(#138942,#138943,#138944,#138945,
#138946,#138947,#138948,#138949,#138950,#138951,#138952,#138953,#138954,
#138955,#138956,#138957,#138958,#138959,#138960,#138961,#138962,#138963,
#138964,#138965,#138966,#138967,#138968,#138969),.UNSPECIFIED.,.F.,.F.,
(4,3,3,3,3,3,3,3,3,4),(0.,0.117080806693866,0.233583246000496,0.348303590725999,
0.46135301553334,0.5,0.625,0.744908083513982,0.872454041756991,1.),
 .UNSPECIFIED.);
#29795=B_SPLINE_CURVE_WITH_KNOTS('',3,(#138970,#138971,#138972,#138973,
#138974,#138975,#138976,#138977,#138978,#138979,#138980,#138981),
 .UNSPECIFIED.,.F.,.F.,(4,2,2,2,2,4),(-3.42420775850897,-2.83987518299694,
-2.25725819870026,-1.34987067298873,-0.707053266798169,-5.39057101361098E-6),
 .UNSPECIFIED.);
#29796=B_SPLINE_CURVE_WITH_KNOTS('',3,(#138987,#138988,#138989,#138990,
#138991,#138992,#138993,#138994,#138995,#138996,#138997,#138998,#138999,
#139000,#139001,#139002,#139003,#139004,#139005,#139006,#139007,#139008,
#139009,#139010,#139011,#139012,#139013,#139014,#139015,#139016,#139017,
#139018,#139019,#139020,#139021,#139022,#139023),.UNSPECIFIED.,.F.,.F.,
(4,1,1,1,1,1,1,1,1,1,1,1,1,1,1,1,1,1,1,1,1,1,1,1,1,1,1,1,1,1,1,1,1,1,4),
(0.,0.02941176470588,0.05882352941176,0.08823529411765,0.1176470588235,
0.1470588235294,0.1764705882353,0.2058823529412,0.2352941176471,0.2647058823529,
0.2941176470588,0.3235294117647,0.3529411764706,0.3823529411765,0.4117647058824,
0.4411764705882,0.4705882352941,0.5,0.5294117647059,0.5588235294118,0.5882352941176,
0.6176470588235,0.6470588235294,0.6764705882353,0.7058823529412,0.7352941176471,
0.7647058823529,0.7941176470588,0.8235294117647,0.8529411764706,0.8823529411765,
0.9117647058824,0.9411764705882,0.9705882352941,0.999994374858691),
 .UNSPECIFIED.);
#29797=B_SPLINE_CURVE_WITH_KNOTS('',3,(#139025,#139026,#139027,#139028,
#139029,#139030,#139031,#139032,#139033,#139034,#139035,#139036,#139037,
#139038,#139039,#139040,#139041,#139042,#139043,#139044,#139045,#139046,
#139047,#139048,#139049,#139050,#139051,#139052,#139053,#139054,#139055,
#139056,#139057,#139058,#139059,#139060,#139061,#139062,#139063,#139064),
 .UNSPECIFIED.,.F.,.F.,(4,3,3,3,3,3,3,3,3,3,3,3,3,4),(0.,0.07692307692308,
0.1538461538462,0.2307692307692,0.3076923076923,0.3846153846154,0.4615384615385,
0.5384615384615,0.6153846153846,0.6923076923077,0.7692307692308,0.8461538461538,
0.9230769230769,1.),.UNSPECIFIED.);
#29798=B_SPLINE_CURVE_WITH_KNOTS('',3,(#139068,#139069,#139070,#139071,
#139072,#139073,#139074,#139075,#139076,#139077,#139078,#139079,#139080,
#139081,#139082,#139083,#139084,#139085,#139086,#139087,#139088,#139089,
#139090,#139091,#139092,#139093,#139094,#139095,#139096,#139097,#139098,
#139099,#139100,#139101,#139102,#139103,#139104,#139105,#139106,#139107),
 .UNSPECIFIED.,.F.,.F.,(4,3,3,3,3,3,3,3,3,3,3,3,3,4),(0.,0.07692307692308,
0.1538461538462,0.2307692307692,0.3076923076923,0.3846153846154,0.4615384615385,
0.5384615384615,0.6153846153846,0.6923076923077,0.7692307692308,0.8461538461538,
0.9230769230769,0.999990181765799),.UNSPECIFIED.);
#29799=B_SPLINE_CURVE_WITH_KNOTS('',3,(#139108,#139109,#139110,#139111,
#139112,#139113,#139114,#139115,#139116,#139117,#139118,#139119,#139120,
#139121,#139122,#139123,#139124,#139125,#139126,#139127,#139128,#139129,
#139130,#139131,#139132,#139133,#139134,#139135,#139136,#139137,#139138,
#139139,#139140),.UNSPECIFIED.,.F.,.F.,(4,1,1,1,1,1,1,1,1,1,1,1,1,1,1,1,
1,1,1,1,1,1,1,1,1,1,1,1,1,1,4),(0.,0.03333333333333,0.06666666666667,0.1,
0.1333333333333,0.1666666666667,0.2,0.2333333333333,0.2666666666667,0.3,
0.3333333333333,0.3666666666667,0.4,0.4333333333333,0.4666666666667,0.5,
0.5333333333333,0.5666666666667,0.6,0.6333333333333,0.6666666666667,0.7,
0.7333333333333,0.7666666666667,0.8,0.8333333333333,0.8666666666667,0.9,
0.9333333333333,0.9666666666667,1.),.UNSPECIFIED.);
#29800=B_SPLINE_CURVE_WITH_KNOTS('',3,(#139143,#139144,#139145,#139146,
#139147,#139148,#139149,#139150,#139151,#139152,#139153,#139154,#139155,
#139156,#139157,#139158,#139159,#139160,#139161,#139162,#139163,#139164,
#139165,#139166,#139167,#139168,#139169,#139170,#139171,#139172,#139173,
#139174,#139175,#139176,#139177,#139178,#139179,#139180,#139181,#139182,
#139183,#139184,#139185,#139186,#139187,#139188,#139189,#139190,#139191,
#139192,#139193,#139194),.UNSPECIFIED.,.F.,.F.,(4,3,3,3,3,3,3,3,3,3,3,3,
3,3,3,3,3,4),(0.,0.0104300641450095,0.0403038134976636,0.0731177483969922,
0.109196822930784,0.148840753280782,0.192353399031002,0.240049789161611,
0.292260775959177,0.349343693489284,0.412033590379295,0.481362584134171,
0.557244485460841,0.640756781399926,0.733854635093322,0.838472312208226,
0.95702604171734,1.),.UNSPECIFIED.);
#29801=B_SPLINE_CURVE_WITH_KNOTS('',3,(#139195,#139196,#139197,#139198,
#139199,#139200,#139201,#139202,#139203,#139204,#139205,#139206,#139207,
#139208,#139209,#139210,#139211,#139212,#139213,#139214,#139215,#139216,
#139217,#139218,#139219,#139220,#139221,#139222,#139223,#139224,#139225,
#139226,#139227,#139228,#139229,#139230,#139231,#139232,#139233,#139234,
#139235,#139236,#139237),.UNSPECIFIED.,.F.,.F.,(4,3,3,3,3,3,3,3,3,3,3,3,
3,3,4),(0.,0.0569254788267774,0.181698225622002,0.29475495478262,0.397219013347534,
0.490602660719935,0.576270367287962,0.653393539486814,0.721886944980528,
0.78340723675226,0.83937561533012,0.890301000193252,0.936516969810281,0.978362059982727,
1.),.UNSPECIFIED.);
#29802=B_SPLINE_CURVE_WITH_KNOTS('',3,(#139469,#139470,#139471,#139472,
#139473,#139474,#139475,#139476,#139477,#139478,#139479,#139480,#139481,
#139482,#139483,#139484,#139485,#139486,#139487,#139488,#139489,#139490,
#139491,#139492,#139493,#139494,#139495,#139496,#139497,#139498,#139499,
#139500,#139501,#139502,#139503,#139504,#139505,#139506,#139507,#139508,
#139509,#139510,#139511,#139512,#139513,#139514,#139515,#139516,#139517,
#139518,#139519,#139520,#139521,#139522,#139523,#139524,#139525,#139526,
#139527,#139528,#139529,#139530,#139531,#139532,#139533,#139534,#139535,
#139536,#139537,#139538,#139539,#139540,#139541,#139542,#139543,#139544,
#139545,#139546,#139547,#139548,#139549,#139550,#139551,#139552,#139553,
#139554,#139555,#139556,#139557,#139558,#139559,#139560,#139561,#139562,
#139563,#139564,#139565,#139566,#139567,#139568,#139569,#139570,#139571,
#139572,#139573,#139574,#139575,#139576,#139577,#139578,#139579,#139580,
#139581,#139582,#139583,#139584,#139585,#139586,#139587,#139588,#139589,
#139590,#139591,#139592,#139593,#139594,#139595,#139596,#139597,#139598,
#139599,#139600,#139601,#139602,#139603,#139604,#139605,#139606,#139607,
#139608,#139609,#139610,#139611,#139612,#139613,#139614,#139615,#139616,
#139617,#139618,#139619,#139620,#139621,#139622,#139623,#139624,#139625,
#139626,#139627,#139628,#139629,#139630,#139631,#139632,#139633,#139634,
#139635,#139636,#139637,#139638,#139639,#139640,#139641,#139642,#139643,
#139644,#139645,#139646,#139647,#139648,#139649,#139650,#139651,#139652,
#139653,#139654,#139655,#139656,#139657,#139658,#139659,#139660,#139661,
#139662,#139663,#139664,#139665,#139666,#139667,#139668,#139669,#139670,
#139671,#139672,#139673,#139674,#139675,#139676,#139677,#139678,#139679,
#139680,#139681,#139682,#139683,#139684,#139685,#139686,#139687,#139688,
#139689,#139690,#139691,#139692,#139693,#139694,#139695,#139696,#139697,
#139698,#139699,#139700,#139701,#139702,#139703,#139704,#139705,#139706,
#139707,#139708,#139709,#139710,#139711,#139712,#139713,#139714,#139715,
#139716,#139717,#139718,#139719,#139720,#139721,#139722,#139723,#139724,
#139725,#139726,#139727,#139728,#139729,#139730,#139731,#139732,#139733,
#139734,#139735,#139736,#139737,#139738,#139739,#139740,#139741,#139742,
#139743,#139744,#139745,#139746,#139747,#139748,#139749,#139750,#139751,
#139752,#139753,#139754,#139755,#139756,#139757,#139758,#139759,#139760,
#139761,#139762,#139763,#139764,#139765,#139766,#139767,#139768,#139769,
#139770,#139771,#139772,#139773,#139774,#139775,#139776,#139777,#139778,
#139779,#139780,#139781,#139782,#139783,#139784,#139785,#139786,#139787,
#139788,#139789,#139790,#139791,#139792,#139793,#139794,#139795,#139796,
#139797,#139798,#139799,#139800,#139801,#139802,#139803,#139804,#139805,
#139806,#139807,#139808,#139809,#139810,#139811,#139812,#139813,#139814,
#139815,#139816,#139817,#139818,#139819,#139820,#139821,#139822,#139823,
#139824,#139825,#139826,#139827,#139828,#139829,#139830,#139831,#139832,
#139833,#139834,#139835,#139836,#139837,#139838,#139839,#139840,#139841,
#139842,#139843,#139844,#139845,#139846,#139847,#139848,#139849,#139850,
#139851,#139852,#139853,#139854,#139855,#139856,#139857,#139858,#139859,
#139860,#139861,#139862,#139863,#139864,#139865,#139866,#139867,#139868,
#139869,#139870,#139871,#139872,#139873,#139874,#139875,#139876,#139877,
#139878,#139879,#139880,#139881,#139882,#139883,#139884,#139885,#139886,
#139887,#139888,#139889,#139890,#139891,#139892,#139893,#139894,#139895,
#139896,#139897,#139898,#139899,#139900,#139901,#139902,#139903,#139904,
#139905,#139906,#139907,#139908,#139909,#139910,#139911,#139912,#139913,
#139914,#139915,#139916,#139917,#139918,#139919,#139920,#139921,#139922,
#139923,#139924,#139925,#139926,#139927,#139928,#139929,#139930,#139931,
#139932,#139933,#139934,#139935,#139936,#139937,#139938,#139939,#139940,
#139941,#139942,#139943,#139944,#139945,#139946,#139947,#139948,#139949,
#139950,#139951,#139952,#139953,#139954,#139955,#139956,#139957,#139958,
#139959,#139960,#139961,#139962,#139963,#139964,#139965,#139966,#139967,
#139968,#139969,#139970,#139971,#139972,#139973,#139974,#139975,#139976),
 .UNSPECIFIED.,.F.,.F.,(4,3,3,3,3,3,3,3,3,3,3,3,3,3,3,3,3,3,3,3,3,3,3,3,
3,3,3,3,3,3,3,3,3,3,3,3,3,3,3,3,3,3,3,3,3,3,3,3,3,3,3,3,3,3,3,3,3,3,3,3,
3,3,3,3,3,3,3,3,3,3,3,3,3,3,3,3,3,3,3,3,3,3,3,3,3,3,3,3,3,3,3,3,3,3,3,3,
3,3,3,3,3,3,3,3,3,3,3,3,3,3,3,3,3,3,3,3,3,3,3,3,3,3,3,3,3,3,3,3,3,3,3,3,
3,3,3,3,3,3,3,3,3,3,3,3,3,3,3,3,3,3,3,3,3,3,3,3,3,3,3,3,3,3,3,3,3,3,3,3,
3,4),(5.26314413123426E-7,0.0113155790796151,0.0251388647517376,0.0310479652170974,
0.0312499999999604,0.0453461316134197,0.0504424803060528,0.0546874999999304,
0.0585937499999254,0.060546874999923,0.0615234374999218,0.0624999999999207,
0.068812174829043,0.0868926240447748,0.106944947332055,0.109374999999864,
0.117316441901434,0.124999999999845,0.129323876863945,0.138802102939861,
0.147918081323925,0.150435171341309,0.160121428953758,0.169646632060944,
0.17968749999978,0.183593749999775,0.185546874999773,0.186523437499772,
0.187356316568156,0.18749999999977,0.187612433563859,0.19852836668657,0.207386871759649,
0.210937499999736,0.214843749999731,0.216796874999728,0.217773437499727,
0.218261718749726,0.218627929687226,0.218749999999725,0.222280520679915,
0.223685847591065,0.22735827302368,0.231153270031486,0.235015757477918,
0.238982945278941,0.242461789679081,0.246093749999737,0.248046874999738,
0.249023437499738,0.249511718749739,0.249755859374739,0.249877929687239,
0.249999999999739,0.26375570429153,0.272081592566711,0.286146390012587,
0.297869928440458,0.312213441963219,0.319939108622709,0.334363175203937,
0.338507769117277,0.353008489557291,0.354400873634069,0.359374999999608,
0.367187499999598,0.368187520310837,0.371093749999594,0.373046874999591,
0.37402343749959,0.374877929687089,0.374999999999589,0.386016201521818,
0.408995234585906,0.430287360079277,0.450033444879799,0.468370688663691,
0.468749999999059,0.484374999998971,0.485418078837636,0.492187499998926,
0.496093749998902,0.498046874998891,0.499511718748883,0.499999999998881,
0.502215778241268,0.527808479215655,0.551648453387262,0.573847489919669,
0.594524368852247,0.613814210682214,0.63184891774307,0.648649582659718,
0.664177872392781,0.678439363988811,0.687499999998774,0.691709046355161,
0.69531249999877,0.699218749998768,0.703124999998766,0.7070337496537,0.718749999998772,
0.726954573406456,0.746903046788504,0.749999999998779,0.765624999998783,
0.767111069151479,0.779817712431221,0.781249999998786,0.788479240017865,
0.79687499999879,0.804687499998791,0.808593749998796,0.810546874998799,
0.812499999998802,0.816347726587709,0.825122186626889,0.828124999998883,
0.832031249998907,0.834060327467434,0.83593749999893,0.841284161873138,
0.843749999998977,0.847656249999001,0.849609374999007,0.851562499999012,
0.855274741365915,0.859374999999035,0.865479004774198,0.867187499999057,
0.86836688933082,0.869140624999062,0.871093749999068,0.87314150143147,0.874999999999078,
0.876834002406975,0.878906249999089,0.882812499999099,0.886466989130165,
0.886718749999109,0.889851811247551,0.89062499999912,0.893182462397039,
0.898437499999135,0.902343749999146,0.904296874999155,0.905864048581422,
0.906249999999164,0.912210533917316,0.915434747904591,0.920209721935489,
0.921874999999294,0.924080465062891,0.925781249999328,0.929687499999361,
0.936091306260822,0.943409695495072,0.949693108201396,0.953124999999578,
0.953429994527388,0.958676452650152,0.964971871567472,0.968749999999721,
0.972942846958018,0.976562499999789,0.980800250809871,0.984374999999857,
0.991373939213844,0.993657578315312,1.),.UNSPECIFIED.);
#29803=B_SPLINE_CURVE_WITH_KNOTS('',3,(#140050,#140051,#140052,#140053,
#140054,#140055,#140056,#140057,#140058,#140059,#140060,#140061,#140062,
#140063,#140064,#140065,#140066,#140067,#140068,#140069,#140070,#140071,
#140072,#140073,#140074,#140075,#140076,#140077,#140078,#140079,#140080,
#140081,#140082,#140083,#140084,#140085,#140086,#140087,#140088,#140089,
#140090,#140091,#140092,#140093,#140094,#140095,#140096,#140097,#140098,
#140099,#140100,#140101,#140102,#140103,#140104,#140105,#140106,#140107,
#140108,#140109,#140110,#140111,#140112,#140113,#140114,#140115,#140116,
#140117,#140118,#140119,#140120,#140121,#140122,#140123,#140124,#140125,
#140126,#140127,#140128,#140129,#140130,#140131,#140132,#140133,#140134),
 .UNSPECIFIED.,.F.,.F.,(4,3,3,3,3,3,3,3,3,3,3,3,3,3,3,3,3,3,3,3,3,3,3,3,
3,3,3,3,4),(1.46586088669429E-9,0.0147856209054546,0.0788187793390021,0.148252710563286,
0.223677641753622,0.249999999999859,0.305663645075048,0.374999999999792,
0.394777161192625,0.437499999999753,0.468749999999731,0.484374999999723,
0.491632695048001,0.492187499999724,0.499999999999724,0.565831577623568,
0.589741931466674,0.65688948573569,0.669154414594773,0.687499999999827,
0.718749999999843,0.734374999999853,0.739649768105247,0.74218749999986,
0.749999999999866,0.806188103222823,0.879930291384157,0.963019849159479,
1.),.UNSPECIFIED.);
#29804=B_SPLINE_CURVE_WITH_KNOTS('',3,(#140177,#140178,#140179,#140180,
#140181,#140182,#140183,#140184,#140185,#140186,#140187,#140188,#140189,
#140190,#140191,#140192,#140193,#140194,#140195,#140196,#140197,#140198,
#140199,#140200,#140201,#140202,#140203,#140204,#140205,#140206,#140207,
#140208,#140209,#140210,#140211,#140212,#140213,#140214,#140215,#140216,
#140217,#140218,#140219,#140220,#140221,#140222,#140223,#140224,#140225,
#140226,#140227,#140228,#140229,#140230,#140231,#140232,#140233,#140234,
#140235,#140236,#140237,#140238,#140239,#140240,#140241,#140242,#140243),
 .UNSPECIFIED.,.F.,.F.,(4,3,3,3,3,3,3,3,3,3,3,3,3,3,3,3,3,3,3,3,3,3,4),
(0.,0.0624999999999875,0.124999999999975,0.182979972803975,0.187499999999971,
0.215193239530195,0.242577553898054,0.249999999999967,0.329473835291726,
0.40895094369529,0.437499999999961,0.468749999999968,0.483425128960071,
0.497765120795587,0.499999999999974,0.572711351548969,0.645848264911811,
0.719643398937141,0.749999999999987,0.824765188414245,0.899992548619747,
0.975917224544569,1.),.UNSPECIFIED.);
#29805=B_SPLINE_CURVE_WITH_KNOTS('',3,(#140245,#140246,#140247,#140248,
#140249,#140250,#140251,#140252,#140253,#140254,#140255,#140256,#140257,
#140258,#140259,#140260,#140261,#140262,#140263,#140264,#140265,#140266,
#140267,#140268,#140269,#140270,#140271,#140272,#140273,#140274,#140275,
#140276,#140277,#140278,#140279,#140280,#140281,#140282,#140283,#140284,
#140285,#140286,#140287,#140288,#140289,#140290,#140291,#140292,#140293,
#140294,#140295,#140296,#140297,#140298,#140299,#140300,#140301,#140302,
#140303,#140304,#140305,#140306,#140307,#140308,#140309,#140310,#140311,
#140312,#140313,#140314,#140315,#140316,#140317,#140318,#140319,#140320,
#140321,#140322,#140323,#140324,#140325,#140326,#140327,#140328,#140329,
#140330,#140331,#140332,#140333,#140334,#140335,#140336,#140337,#140338,
#140339,#140340,#140341,#140342,#140343,#140344,#140345,#140346,#140347,
#140348,#140349,#140350,#140351,#140352,#140353,#140354,#140355,#140356,
#140357,#140358,#140359,#140360,#140361,#140362,#140363,#140364,#140365),
 .UNSPECIFIED.,.F.,.F.,(4,3,3,3,3,3,3,3,3,3,3,3,3,3,3,3,3,3,3,3,3,3,3,3,
3,3,3,3,3,3,3,3,3,3,3,3,3,3,3,3,4),(4.84503357369714E-12,0.0625000000038769,
0.119886196849213,0.125000000002909,0.179080353524112,0.187500000004363,
0.218750000005092,0.234375000005453,0.242187500005639,0.250000000005825,
0.312500000007308,0.343750000008051,0.359375000008415,0.367187500008598,
0.374023437508775,0.375000000008799,0.392863091523399,0.40625000000836,
0.421875000008141,0.429687500008027,0.433593750007968,0.435546875007939,
0.437500000007909,0.440114549658553,0.472413623124356,0.500000000007027,
0.547747027865969,0.592672173262821,0.625000000005261,0.665016457000979,
0.687500000004373,0.718750000003932,0.734375000003712,0.746910733725364,
0.750000000003492,0.791768980893818,0.83477727983257,0.875000000001746,
0.92207412377465,0.972243230788792,1.),.UNSPECIFIED.);
#29806=B_SPLINE_CURVE_WITH_KNOTS('',3,(#140366,#140367,#140368,#140369,
#140370,#140371,#140372,#140373,#140374,#140375,#140376,#140377,#140378,
#140379,#140380,#140381,#140382,#140383,#140384,#140385,#140386,#140387,
#140388,#140389,#140390,#140391,#140392,#140393,#140394,#140395,#140396,
#140397,#140398,#140399,#140400,#140401,#140402,#140403,#140404,#140405,
#140406,#140407,#140408,#140409,#140410,#140411,#140412,#140413,#140414,
#140415,#140416,#140417,#140418,#140419,#140420,#140421,#140422,#140423),
 .UNSPECIFIED.,.F.,.F.,(4,3,3,3,3,3,3,3,3,3,3,3,3,3,3,3,3,3,3,4),(1.2576115163105E-9,
0.0582372114102846,0.115345099826069,0.171871515531986,0.227755575554621,
0.25,0.30535089973337,0.360932037266699,0.415956126690006,0.471025812356985,
0.526253513839453,0.58219013537959,0.638316250545109,0.695300688824847,
0.75,0.808269975267283,0.867972281236829,0.928599616214729,0.990708785988877,
1.),.UNSPECIFIED.);
#29807=B_SPLINE_CURVE_WITH_KNOTS('',3,(#140442,#140443,#140444,#140445,
#140446,#140447,#140448,#140449,#140450,#140451,#140452,#140453,#140454,
#140455,#140456,#140457,#140458,#140459,#140460,#140461,#140462,#140463,
#140464,#140465,#140466,#140467,#140468,#140469,#140470,#140471,#140472,
#140473,#140474,#140475,#140476,#140477,#140478,#140479,#140480,#140481,
#140482,#140483,#140484,#140485,#140486,#140487,#140488,#140489,#140490,
#140491,#140492,#140493,#140494,#140495,#140496,#140497,#140498,#140499),
 .UNSPECIFIED.,.F.,.F.,(4,3,3,3,3,3,3,3,3,3,3,3,3,3,3,3,3,3,3,4),(5.75195662416378E-12,
0.062500000004314,0.120799294736565,0.178331807923707,0.234974821688961,
0.25,0.305845453226057,0.3613647715728,0.416311125147688,0.471089488762509,
0.525811881558363,0.581858911168772,0.636959838781275,0.693479919390638,
0.75,0.806575787009208,0.864269428679939,0.922683317676143,0.982337040140753,
1.),.UNSPECIFIED.);
#29808=B_SPLINE_CURVE_WITH_KNOTS('',3,(#140532,#140533,#140534,#140535),
 .UNSPECIFIED.,.F.,.F.,(4,4),(0.,1.),.UNSPECIFIED.);
#29809=B_SPLINE_CURVE_WITH_KNOTS('',3,(#140537,#140538,#140539,#140540,
#140541,#140542,#140543,#140544,#140545,#140546),.UNSPECIFIED.,.F.,.F.,
(4,2,2,2,4),(1.0680348650496E-8,0.25,0.5,0.75,1.),.UNSPECIFIED.);
#29810=B_SPLINE_CURVE_WITH_KNOTS('',3,(#140548,#140549,#140550,#140551,
#140552,#140553,#140554),.UNSPECIFIED.,.F.,.F.,(4,3,4),(0.,0.362128916600015,
1.),.UNSPECIFIED.);
#29811=B_SPLINE_CURVE_WITH_KNOTS('',3,(#140555,#140556,#140557,#140558,
#140559,#140560,#140561,#140562,#140563,#140564),.UNSPECIFIED.,.F.,.F.,
(4,2,2,2,4),(0.,0.25,0.5,0.75,1.),.UNSPECIFIED.);
#29812=B_SPLINE_CURVE_WITH_KNOTS('',3,(#140595,#140596,#140597,#140598,
#140599,#140600,#140601,#140602,#140603,#140604,#140605,#140606,#140607,
#140608,#140609,#140610,#140611,#140612,#140613,#140614,#140615,#140616,
#140617,#140618,#140619,#140620,#140621,#140622,#140623,#140624,#140625,
#140626,#140627,#140628,#140629,#140630,#140631,#140632,#140633,#140634,
#140635,#140636,#140637,#140638,#140639,#140640,#140641,#140642,#140643,
#140644,#140645,#140646),.UNSPECIFIED.,.F.,.F.,(4,3,3,3,3,3,3,3,3,3,3,3,
3,3,3,3,3,4),(0.,0.0606123631499776,0.121810480050351,0.183182706218067,
0.200869175620174,0.25,0.328361933407609,0.406263651642803,0.479625687786031,
0.5,0.59129802050641,0.682804917911111,0.75,0.757779334258463,0.821554838527955,
0.885141851778926,0.947606732206778,1.),.UNSPECIFIED.);
#29813=B_SPLINE_CURVE_WITH_KNOTS('',3,(#140649,#140650,#140651,#140652,
#140653,#140654,#140655,#140656,#140657,#140658,#140659,#140660,#140661,
#140662,#140663,#140664,#140665,#140666,#140667,#140668,#140669,#140670,
#140671,#140672,#140673,#140674,#140675,#140676,#140677,#140678,#140679,
#140680,#140681,#140682,#140683,#140684,#140685,#140686,#140687,#140688,
#140689,#140690,#140691,#140692,#140693,#140694,#140695,#140696,#140697),
 .UNSPECIFIED.,.F.,.F.,(4,3,3,3,3,3,3,3,3,3,3,3,3,3,3,3,4),(0.,0.101045004834656,
0.1428571428571,0.247561218121864,0.255765081058048,0.2857142857143,0.409190479713353,
0.4285714285714,0.519960169066042,0.56339195277172,0.5714285714286,0.657014403441729,
0.7142857142857,0.717414049033271,0.8571428571429,0.871468788702833,1.),
 .UNSPECIFIED.);
#29814=B_SPLINE_CURVE_WITH_KNOTS('',3,(#140699,#140700,#140701,#140702,
#140703,#140704),.UNSPECIFIED.,.F.,.F.,(4,1,1,4),(0.,0.3333333333333,0.6666666666667,
1.),.UNSPECIFIED.);
#29815=B_SPLINE_CURVE_WITH_KNOTS('',3,(#140706,#140707,#140708,#140709,
#140710,#140711,#140712,#140713,#140714,#140715,#140716,#140717,#140718,
#140719,#140720,#140721,#140722,#140723,#140724,#140725,#140726,#140727,
#140728,#140729,#140730,#140731,#140732,#140733,#140734,#140735,#140736,
#140737,#140738,#140739,#140740,#140741,#140742,#140743,#140744,#140745,
#140746,#140747,#140748,#140749,#140750,#140751,#140752,#140753,#140754,
#140755,#140756,#140757,#140758,#140759,#140760,#140761,#140762,#140763,
#140764,#140765,#140766,#140767,#140768,#140769,#140770,#140771,#140772,
#140773,#140774,#140775,#140776,#140777,#140778,#140779,#140780,#140781,
#140782,#140783,#140784,#140785,#140786,#140787,#140788,#140789,#140790,
#140791,#140792,#140793,#140794,#140795,#140796,#140797,#140798,#140799,
#140800,#140801,#140802,#140803,#140804,#140805),.UNSPECIFIED.,.F.,.F.,
(4,3,3,3,3,3,3,3,3,3,3,3,3,3,3,3,3,3,3,3,3,3,3,3,3,3,3,3,3,3,3,3,3,4),(1.42536501268589E-7,
0.0477654802612144,0.07692307692308,0.12794560731773,0.1538461538462,0.208199907711091,
0.2307692307692,0.288440067990146,0.3076923076923,0.368684577671203,0.3846153846154,
0.440455527634295,0.448926709032301,0.4615384615385,0.515233835999228,0.529168651732405,
0.5384615384615,0.587702308433438,0.609417787020049,0.6153846153846,0.689658855316415,
0.6923076923077,0.733559153082206,0.7692307692308,0.76990413797734,0.809524173197566,
0.8461538461538,0.850154012702905,0.886615467889903,0.921164890063805,0.9230769230769,
0.930386224751045,0.970178482045245,0.999999996823438),.UNSPECIFIED.);
#29816=B_SPLINE_CURVE_WITH_KNOTS('',3,(#140807,#140808,#140809,#140810,
#140811,#140812,#140813,#140814,#140815,#140816,#140817,#140818,#140819,
#140820,#140821,#140822,#140823,#140824,#140825,#140826,#140827,#140828,
#140829,#140830,#140831,#140832,#140833,#140834,#140835,#140836,#140837,
#140838,#140839,#140840,#140841,#140842,#140843,#140844,#140845,#140846,
#140847,#140848,#140849,#140850,#140851,#140852,#140853,#140854,#140855,
#140856,#140857,#140858,#140859,#140860,#140861,#140862,#140863,#140864,
#140865,#140866,#140867,#140868,#140869,#140870,#140871,#140872,#140873,
#140874,#140875,#140876,#140877,#140878,#140879,#140880,#140881,#140882,
#140883,#140884,#140885,#140886,#140887,#140888,#140889,#140890,#140891,
#140892,#140893,#140894,#140895,#140896,#140897,#140898,#140899,#140900,
#140901,#140902,#140903),.UNSPECIFIED.,.F.,.F.,(4,3,3,3,3,3,3,3,3,3,3,3,
3,3,3,3,3,3,3,3,3,3,3,3,3,3,3,3,3,3,3,3,4),(0.,0.0528043674744117,0.101411794382289,
0.1111111111111,0.15644763557432,0.203145303458736,0.216184392620985,0.2222222222222,
0.268327215607274,0.315677403819418,0.331009546931535,0.3333333333333,0.383603126000518,
0.435467618888511,0.4444444444444,0.445827374170425,0.479865806193693,0.514265446278494,
0.548751475142092,0.5555555555556,0.560638706485747,0.604765726042025,0.64872763385938,
0.6666666666667,0.675334559394413,0.731216324970566,0.7777777777778,0.79015606296775,
0.842285728432088,0.8888888888889,0.905015646757144,0.971815255624162,1.),
 .UNSPECIFIED.);
#29817=B_SPLINE_CURVE_WITH_KNOTS('',3,(#140905,#140906,#140907,#140908,
#140909,#140910),.UNSPECIFIED.,.F.,.F.,(4,1,1,4),(2.01511427487787E-6,0.3333333333333,
0.6666666666667,1.),.UNSPECIFIED.);
#29818=B_SPLINE_CURVE_WITH_KNOTS('',3,(#140912,#140913,#140914,#140915,
#140916,#140917,#140918,#140919,#140920,#140921,#140922,#140923,#140924,
#140925,#140926,#140927,#140928,#140929,#140930,#140931,#140932,#140933,
#140934,#140935,#140936,#140937,#140938,#140939,#140940,#140941,#140942,
#140943,#140944,#140945,#140946,#140947,#140948,#140949,#140950,#140951,
#140952,#140953,#140954,#140955,#140956,#140957,#140958,#140959,#140960,
#140961,#140962,#140963),.UNSPECIFIED.,.F.,.F.,(4,3,3,3,3,3,3,3,3,3,3,3,
3,3,3,3,3,4),(2.54841849385267E-8,0.142339474713401,0.1428571428571,0.2857142857143,
0.2872008613377,0.4285714285714,0.432100905493033,0.534601452193607,0.5714285714286,
0.576982678559165,0.664494236306334,0.7142857142857,0.721781321793795,0.836816076392738,
0.8571428571429,0.866672992875378,0.98528256580256,1.),.UNSPECIFIED.);
#29819=B_SPLINE_CURVE_WITH_KNOTS('',3,(#140965,#140966,#140967,#140968,
#140969,#140970,#140971,#140972,#140973,#140974,#140975,#140976,#140977,
#140978,#140979,#140980,#140981,#140982,#140983,#140984,#140985,#140986,
#140987,#140988,#140989,#140990,#140991,#140992,#140993,#140994,#140995,
#140996,#140997,#140998,#140999,#141000,#141001,#141002,#141003,#141004,
#141005,#141006,#141007,#141008,#141009,#141010,#141011,#141012,#141013,
#141014,#141015,#141016,#141017,#141018,#141019,#141020,#141021,#141022,
#141023,#141024,#141025),.UNSPECIFIED.,.F.,.F.,(4,3,3,3,3,3,3,3,3,3,3,3,
3,3,3,3,3,3,3,3,4),(0.,0.0630782732840507,0.127042279284709,0.191683536836724,
0.245591759692709,0.25,0.318849375572925,0.387799611033952,0.456438644994925,
0.5,0.524717413166611,0.577360244871049,0.630453687094251,0.683820373655777,
0.73762295854436,0.75,0.805440391682254,0.860809675952561,0.916874810401688,
0.973450529840081,1.),.UNSPECIFIED.);
#29820=B_SPLINE_CURVE_WITH_KNOTS('',3,(#141030,#141031,#141032,#141033,
#141034,#141035,#141036,#141037,#141038,#141039,#141040,#141041,#141042,
#141043,#141044,#141045,#141046,#141047,#141048,#141049,#141050,#141051,
#141052,#141053),.UNSPECIFIED.,.F.,.F.,(4,2,2,2,1,2,2,2,2,1,2,2,4),(0.,
0.249999999999934,0.374999999999892,0.437499999999875,0.46874999999986,
0.484374999999857,0.499999999999854,0.624999999999859,0.68749999999986,
0.718749999999861,0.734374999999859,0.749999999999857,1.),.UNSPECIFIED.);
#29821=B_SPLINE_CURVE_WITH_KNOTS('',3,(#141097,#141098,#141099,#141100,
#141101,#141102,#141103,#141104,#141105,#141106,#141107,#141108,#141109,
#141110,#141111,#141112,#141113,#141114,#141115,#141116,#141117,#141118,
#141119,#141120,#141121,#141122,#141123,#141124,#141125,#141126,#141127,
#141128,#141129,#141130,#141131,#141132,#141133,#141134,#141135,#141136,
#141137,#141138,#141139,#141140,#141141,#141142,#141143,#141144,#141145,
#141146,#141147,#141148,#141149,#141150,#141151,#141152,#141153,#141154,
#141155,#141156,#141157),.UNSPECIFIED.,.F.,.F.,(4,3,3,3,3,3,3,3,3,3,3,3,
3,3,3,3,3,3,3,3,4),(9.41833711872304E-10,0.0625000007063753,0.121242456281344,
0.179227817213172,0.236342485654817,0.25,0.306333949112938,0.362097082496164,
0.4175941270922,0.472908213704477,0.5,0.555299901063676,0.610886228909014,
0.666693722114869,0.723046964424233,0.75,0.807180637358659,0.865491041455086,
0.924532986353485,0.984817318215386,1.),.UNSPECIFIED.);
#29822=B_SPLINE_CURVE_WITH_KNOTS('',3,(#141158,#141159,#141160,#141161,
#141162,#141163,#141164,#141165,#141166,#141167,#141168,#141169,#141170,
#141171,#141172,#141173,#141174,#141175,#141176,#141177,#141178,#141179,
#141180,#141181,#141182,#141183,#141184,#141185,#141186,#141187,#141188,
#141189,#141190,#141191,#141192,#141193,#141194,#141195,#141196,#141197,
#141198,#141199,#141200,#141201,#141202,#141203,#141204,#141205,#141206,
#141207,#141208,#141209,#141210,#141211,#141212,#141213,#141214,#141215,
#141216,#141217,#141218,#141219,#141220,#141221,#141222,#141223,#141224,
#141225,#141226,#141227,#141228,#141229,#141230,#141231,#141232,#141233,
#141234,#141235,#141236,#141237,#141238,#141239,#141240,#141241,#141242,
#141243,#141244,#141245,#141246,#141247,#141248,#141249,#141250,#141251,
#141252,#141253,#141254,#141255,#141256,#141257,#141258,#141259,#141260,
#141261,#141262,#141263,#141264,#141265,#141266,#141267,#141268,#141269,
#141270,#141271,#141272,#141273,#141274,#141275,#141276,#141277,#141278,
#141279,#141280,#141281,#141282,#141283,#141284,#141285,#141286,#141287,
#141288,#141289,#141290,#141291,#141292,#141293,#141294,#141295,#141296,
#141297,#141298,#141299,#141300,#141301,#141302,#141303,#141304,#141305),
 .UNSPECIFIED.,.F.,.F.,(4,3,3,3,3,3,3,3,3,3,3,3,3,3,3,3,3,3,3,3,3,3,3,3,
3,3,3,3,3,3,3,3,3,3,3,3,3,3,3,3,3,3,3,3,3,3,3,3,3,4),(0.,0.0264084774457084,
0.0540004211451316,0.0624999999999468,0.0915694128606951,0.0937499999999201,
0.109374999999903,0.119184263010084,0.124999999999885,0.145880152879992,
0.177607617245252,0.187499999999834,0.218749999999808,0.234374999999798,
0.24218749999979,0.246093749999782,0.249087826771642,0.249999999999775,
0.293126079918406,0.334757157073219,0.342577256663599,0.386121644454048,
0.427849055909688,0.468749999999184,0.484374999999145,0.492187499999127,
0.496093749999121,0.498046874999117,0.499836436232448,0.499999999999114,
0.531787217869695,0.541498700431291,0.574411422832711,0.606759999982205,
0.63772744515156,0.667782336245535,0.696377557994492,0.718749999999466,
0.726270401674991,0.734374999999495,0.742187499999505,0.746093749999508,
0.748046874999507,0.749999999999506,0.794307853808405,0.839179251836691,
0.884989399471881,0.897490307255218,0.948745153627609,1.),.UNSPECIFIED.);
#29823=B_SPLINE_CURVE_WITH_KNOTS('',3,(#141403,#141404,#141405,#141406,
#141407,#141408,#141409,#141410,#141411,#141412,#141413,#141414,#141415,
#141416,#141417,#141418,#141419,#141420,#141421,#141422,#141423,#141424,
#141425,#141426,#141427,#141428,#141429,#141430,#141431,#141432,#141433,
#141434,#141435,#141436,#141437,#141438,#141439,#141440,#141441,#141442,
#141443,#141444,#141445,#141446,#141447,#141448),.UNSPECIFIED.,.F.,.F.,
(4,3,3,3,3,3,3,3,3,3,3,3,3,3,3,4),(0.,0.0871565653129833,0.124999999999222,
0.187499999998834,0.218749999998644,0.230568207164711,0.234374999998548,
0.242187499998501,0.249023437498464,0.249999999998459,0.374999999998704,
0.437499999998831,0.468749999998894,0.484374999998931,0.499999999998967,
0.999999999995782),.UNSPECIFIED.);
#29824=B_SPLINE_CURVE_WITH_KNOTS('',3,(#141449,#141450,#141451,#141452,
#141453,#141454,#141455,#141456,#141457,#141458,#141459,#141460),
 .UNSPECIFIED.,.F.,.F.,(4,1,1,1,1,1,1,1,1,4),(8.62526419816179E-10,0.129643184459891,
0.259286368919425,0.518572737838491,0.648215922298025,0.777859106757558,
0.842680698987325,0.907502291217091,0.972323883446858,0.999920136454838),
 .UNSPECIFIED.);
#29825=B_SPLINE_CURVE_WITH_KNOTS('',3,(#141462,#141463,#141464,#141465,
#141466,#141467,#141468,#141469,#141470,#141471,#141472,#141473,#141474,
#141475,#141476,#141477),.UNSPECIFIED.,.F.,.F.,(4,3,3,3,3,4),(0.,0.36363630059361,
0.727272601186151,0.818181676334287,0.909090751482421,1.),.UNSPECIFIED.);
#29826=B_SPLINE_CURVE_WITH_KNOTS('',3,(#141479,#141480,#141481,#141482,
#141483,#141484,#141485,#141486,#141487,#141488,#141489),.UNSPECIFIED.,
 .F.,.F.,(4,1,1,1,1,1,1,1,4),(0.,0.0812515846062436,0.265002401744267,0.448753218882289,
0.632504036020311,0.724379444589322,0.816254853158334,0.90813274562238,
1.),.UNSPECIFIED.);
#29827=B_SPLINE_CURVE_WITH_KNOTS('',3,(#141490,#141491,#141492,#141493,
#141494,#141495,#141496,#141497,#141498,#141499,#141500,#141501,#141502,
#141503,#141504,#141505,#141506,#141507,#141508,#141509,#141510,#141511,
#141512,#141513,#141514,#141515,#141516,#141517,#141518,#141519,#141520,
#141521,#141522,#141523,#141524,#141525,#141526,#141527,#141528,#141529,
#141530,#141531,#141532,#141533,#141534,#141535),.UNSPECIFIED.,.F.,.F.,
(4,3,3,3,3,3,3,3,3,3,3,3,3,3,3,4),(0.,0.0570300637188032,0.185099460109903,
0.299971203046531,0.403465598063635,0.497076472649179,0.5,0.581844924036565,
0.658648191461615,0.728294917113762,0.791519404429945,0.848980821447152,
0.901257474787093,0.948894557413619,0.992419572443448,1.),.UNSPECIFIED.);
#29828=B_SPLINE_CURVE_WITH_KNOTS('',3,(#141604,#141605,#141606,#141607,
#141608,#141609,#141610,#141611,#141612,#141613,#141614,#141615,#141616,
#141617,#141618,#141619,#141620,#141621,#141622,#141623,#141624,#141625,
#141626,#141627,#141628,#141629,#141630,#141631,#141632,#141633,#141634,
#141635,#141636,#141637,#141638,#141639,#141640,#141641,#141642,#141643,
#141644,#141645,#141646,#141647,#141648,#141649,#141650,#141651,#141652,
#141653,#141654,#141655,#141656,#141657,#141658,#141659,#141660,#141661,
#141662,#141663,#141664,#141665,#141666,#141667,#141668,#141669,#141670,
#141671,#141672,#141673,#141674,#141675,#141676),.UNSPECIFIED.,.F.,.F.,
(4,3,3,3,3,3,3,3,3,3,3,3,3,3,3,3,3,3,3,3,3,3,3,3,4),(0.,0.0480603990646371,
0.0950212146263362,0.140589379788711,0.185423925913468,0.229341106002203,
0.25,0.292898936761959,0.335299629910999,0.377303576459375,0.419010031839926,
0.460499854771804,0.501925680604814,0.543371999439227,0.584923371415726,
0.626860203634118,0.669047367421796,0.711846231343259,0.75,0.793852299612026,
0.838391808404164,0.884188277214604,0.930765244414424,0.978681703509444,
0.999999999999208),.UNSPECIFIED.);
#29829=B_SPLINE_CURVE_WITH_KNOTS('',3,(#141905,#141906,#141907,#141908,
#141909,#141910,#141911,#141912,#141913,#141914,#141915,#141916,#141917,
#141918,#141919,#141920,#141921,#141922,#141923,#141924,#141925,#141926,
#141927,#141928,#141929,#141930,#141931,#141932,#141933,#141934,#141935,
#141936,#141937,#141938,#141939,#141940,#141941,#141942,#141943,#141944,
#141945,#141946,#141947,#141948,#141949,#141950,#141951,#141952,#141953,
#141954,#141955,#141956,#141957,#141958,#141959,#141960,#141961,#141962,
#141963,#141964,#141965,#141966,#141967,#141968,#141969,#141970,#141971,
#141972,#141973,#141974,#141975,#141976,#141977,#141978,#141979,#141980,
#141981,#141982,#141983,#141984,#141985,#141986,#141987,#141988,#141989,
#141990,#141991,#141992,#141993,#141994,#141995,#141996,#141997,#141998,
#141999,#142000,#142001,#142002,#142003,#142004,#142005,#142006,#142007,
#142008,#142009,#142010,#142011,#142012,#142013,#142014,#142015,#142016,
#142017,#142018,#142019,#142020,#142021,#142022,#142023,#142024,#142025,
#142026,#142027,#142028,#142029,#142030,#142031,#142032,#142033,#142034,
#142035,#142036,#142037,#142038,#142039,#142040,#142041,#142042,#142043,
#142044,#142045,#142046,#142047,#142048,#142049,#142050,#142051,#142052,
#142053,#142054,#142055,#142056,#142057,#142058,#142059,#142060,#142061,
#142062,#142063,#142064,#142065,#142066,#142067,#142068,#142069,#142070,
#142071,#142072,#142073,#142074,#142075,#142076,#142077,#142078,#142079,
#142080,#142081,#142082,#142083,#142084,#142085,#142086,#142087,#142088,
#142089,#142090,#142091,#142092,#142093,#142094,#142095,#142096,#142097,
#142098,#142099,#142100,#142101,#142102,#142103,#142104,#142105,#142106,
#142107,#142108,#142109,#142110,#142111,#142112,#142113,#142114,#142115,
#142116,#142117,#142118,#142119,#142120,#142121,#142122,#142123,#142124,
#142125,#142126,#142127,#142128,#142129,#142130,#142131,#142132,#142133,
#142134,#142135,#142136,#142137,#142138,#142139,#142140,#142141,#142142,
#142143,#142144,#142145,#142146,#142147,#142148,#142149,#142150,#142151,
#142152,#142153,#142154,#142155,#142156,#142157,#142158,#142159,#142160,
#142161,#142162,#142163,#142164,#142165,#142166,#142167,#142168,#142169,
#142170,#142171,#142172,#142173,#142174,#142175,#142176,#142177,#142178,
#142179,#142180,#142181,#142182,#142183,#142184,#142185,#142186,#142187,
#142188,#142189,#142190,#142191,#142192,#142193,#142194,#142195,#142196,
#142197,#142198,#142199,#142200,#142201,#142202,#142203,#142204,#142205,
#142206,#142207,#142208,#142209,#142210,#142211,#142212,#142213,#142214,
#142215,#142216,#142217,#142218,#142219,#142220,#142221,#142222,#142223,
#142224,#142225,#142226,#142227,#142228,#142229,#142230,#142231,#142232,
#142233,#142234,#142235,#142236,#142237,#142238,#142239,#142240,#142241,
#142242,#142243,#142244,#142245,#142246,#142247,#142248,#142249,#142250,
#142251,#142252,#142253,#142254,#142255,#142256,#142257,#142258,#142259,
#142260,#142261,#142262,#142263,#142264,#142265,#142266,#142267,#142268,
#142269,#142270,#142271,#142272,#142273,#142274,#142275,#142276,#142277,
#142278,#142279,#142280,#142281,#142282,#142283,#142284,#142285,#142286,
#142287,#142288,#142289),.UNSPECIFIED.,.F.,.F.,(4,3,3,3,3,3,3,3,3,3,3,3,
3,3,3,3,3,3,3,3,3,3,3,3,3,3,3,3,3,3,3,3,3,3,3,3,3,3,3,3,3,3,3,3,3,3,3,3,
3,3,3,3,3,3,3,3,3,3,3,3,3,3,3,3,3,3,3,3,3,3,3,3,3,3,3,3,3,3,3,3,3,3,3,3,
3,3,3,3,3,3,3,3,3,3,3,3,3,3,3,3,3,3,3,3,3,3,3,3,3,3,3,3,3,3,3,3,3,3,3,3,
3,3,3,3,3,3,3,3,4),(0.,0.00521449698044272,0.0113488205456387,0.0178358694463679,
0.0234650279830911,0.0243229183470971,0.0292986400166019,0.0312499999989362,
0.0382626231936421,0.0497978180709293,0.0564051787566613,0.0618583024771885,
0.0624999999978725,0.0689925129920575,0.0703124999976079,0.0712890624975725,
0.0722656249975372,0.0742187499974694,0.0766934911129652,0.0781249999973303,
0.0820312499971913,0.0839843749971273,0.0857099042925744,0.0859374999970634,
0.0894444052754588,0.0926142549496846,0.0937499999968183,0.0959369608234018,
0.0978509239991937,0.0987752323809756,0.101358853034054,0.101562499996573,
0.103648949249782,0.105468749996451,0.106220025523178,0.106783782019121,
0.107421874996389,0.108664772469553,0.109374999996328,0.110500918498203,
0.110828843478205,0.112253795390214,0.113861390132636,0.115696843465077,
0.11718749999609,0.119800214430568,0.121093749995968,0.123046874995902,
0.124498774121639,0.124999999995837,0.135004728902792,0.140624999995255,
0.145085768584857,0.148437499994964,0.156249999994673,0.164069778087939,
0.187499999993506,0.203124999992923,0.210937499992628,0.212890624992553,
0.214843749992478,0.218749999992334,0.22735411870143,0.234374999991791,
0.242187499991519,0.246093749991382,0.248046874991314,0.249023437491279,
0.249511718741263,0.249755859366256,0.249999999991249,0.269690675432299,
0.281249999991643,0.285156249991687,0.285644531241691,0.286132812491694,
0.287109374991704,0.289062499991721,0.296874999991792,0.306919225954505,
0.312499999991936,0.321016191980661,0.353149448606746,0.374999999992511,
0.432000932161343,0.437499999993086,0.455335442631984,0.468749999993373,
0.484374999993516,0.492187499993586,0.496093749993623,0.498046874993641,
0.499755859368656,0.499999999993659,0.525196633496263,0.542217052572066,
0.563483502376743,0.584129658100889,0.591456271900779,0.611541339049758,
0.624999999995042,0.64356144097782,0.661716660603838,0.679380722824786,
0.687499999995734,0.705132772898844,0.71874999999608,0.730587760228015,
0.734374999996252,0.742187499996338,0.746093749996381,0.748046874996403,
0.749755859371422,0.749999999996425,0.770904489841411,0.782034308694622,
0.802645260226518,0.812499999997319,0.833204988474798,0.847304939070212,
0.865266431846127,0.874999999998213,0.89362961551321,0.913178662494567,
0.919532052425721,0.937499999999106,0.95788376607959,0.979974477596612,
1.),.UNSPECIFIED.);
#29830=B_SPLINE_CURVE_WITH_KNOTS('',3,(#142477,#142478,#142479,#142480,
#142481,#142482,#142483,#142484,#142485,#142486,#142487,#142488,#142489,
#142490,#142491,#142492,#142493),.UNSPECIFIED.,.F.,.F.,(4,1,1,1,1,1,1,1,
1,1,1,1,1,1,4),(0.,0.0171470494701,0.0342940989402,0.04286762367525,0.0514411484103,
0.06001467314535,0.0685881978804,0.0857352473505,0.1028822968206,0.1371763957608,
0.2057645936412,0.2743527915216,0.4115291872824,0.685881978804,1.),
 .UNSPECIFIED.);
#29831=B_SPLINE_CURVE_WITH_KNOTS('',3,(#142681,#142682,#142683,#142684,
#142685,#142686,#142687,#142688,#142689,#142690,#142691),.UNSPECIFIED.,
 .F.,.F.,(4,1,1,1,1,1,1,1,4),(0.,0.0918420543167816,0.183748190378033,0.275623105346068,
0.367498020314102,0.55124785025017,0.734997680186239,0.918747510122307,
1.),.UNSPECIFIED.);
#29832=B_SPLINE_CURVE_WITH_KNOTS('',3,(#142790,#142791,#142792,#142793),
 .UNSPECIFIED.,.F.,.F.,(4,4),(0.,1.),.UNSPECIFIED.);
#29833=B_SPLINE_CURVE_WITH_KNOTS('',3,(#142797,#142798,#142799,#142800,
#142801,#142802,#142803,#142804,#142805,#142806,#142807,#142808,#142809,
#142810,#142811,#142812,#142813,#142814,#142815,#142816,#142817,#142818,
#142819,#142820,#142821,#142822,#142823,#142824,#142825,#142826,#142827,
#142828,#142829,#142830,#142831,#142832,#142833,#142834,#142835,#142836,
#142837,#142838,#142839,#142840,#142841,#142842,#142843,#142844,#142845,
#142846,#142847,#142848,#142849,#142850,#142851,#142852,#142853,#142854,
#142855,#142856,#142857,#142858,#142859,#142860,#142861,#142862,#142863,
#142864,#142865,#142866,#142867,#142868,#142869,#142870,#142871,#142872,
#142873,#142874,#142875,#142876,#142877,#142878,#142879,#142880,#142881,
#142882,#142883,#142884,#142885,#142886,#142887,#142888,#142889,#142890,
#142891,#142892,#142893,#142894,#142895,#142896,#142897,#142898,#142899,
#142900,#142901,#142902,#142903,#142904,#142905,#142906,#142907,#142908,
#142909,#142910,#142911,#142912,#142913,#142914,#142915,#142916,#142917,
#142918,#142919,#142920,#142921,#142922,#142923,#142924,#142925,#142926,
#142927,#142928,#142929,#142930,#142931,#142932,#142933,#142934,#142935,
#142936,#142937,#142938),.UNSPECIFIED.,.F.,.F.,(4,3,3,3,3,3,3,3,3,3,3,3,
3,3,3,3,3,3,3,3,3,3,3,3,3,3,3,3,3,3,3,3,3,3,3,3,3,3,3,3,3,3,3,3,3,3,3,4),
(1.73463430039571E-9,0.0335107622719545,0.0886020995752468,0.143100924356775,
0.196889311633565,0.2500000000009,0.254017552135438,0.302432649453191,0.350353609669106,
0.397676447026696,0.437500000001574,0.437860949912641,0.46875000000169,
0.484375000001741,0.49218750000177,0.496093750001781,0.498914845875728,
0.500000000001793,0.525979626844155,0.552783114604028,0.580825272327736,
0.593673938705637,0.620738510610158,0.649058596437683,0.677973658530814,
0.707468186587495,0.718750000002402,0.734375000002449,0.74218750000248,
0.746093750002493,0.74804687500251,0.749023437502518,0.750000000002527,
0.825232812730111,0.843750000003066,0.859375000003151,0.867187500003194,
0.874023437503235,0.875000000003245,0.891046614145269,0.907083150610724,
0.923049256526572,0.937500000001623,0.953124999998386,0.968447616826583,
0.984223808407629,0.998753350832935,0.999999999988675),.UNSPECIFIED.);
#29834=B_SPLINE_CURVE_WITH_KNOTS('',3,(#142942,#142943,#142944,#142945,
#142946,#142947,#142948,#142949,#142950,#142951,#142952,#142953,#142954,
#142955,#142956,#142957,#142958,#142959,#142960,#142961,#142962,#142963),
 .UNSPECIFIED.,.F.,.F.,(4,3,3,3,3,3,3,4),(8.55806068908103E-11,0.2,0.357842525431517,
0.4,0.6,0.8,0.974718041105161,1.),.UNSPECIFIED.);
#29835=B_SPLINE_CURVE_WITH_KNOTS('',3,(#142967,#142968,#142969,#142970,
#142971,#142972,#142973,#142974,#142975,#142976,#142977,#142978,#142979,
#142980,#142981,#142982,#142983,#142984,#142985,#142986,#142987,#142988,
#142989,#142990,#142991,#142992,#142993,#142994,#142995,#142996,#142997,
#142998,#142999,#143000,#143001,#143002,#143003,#143004,#143005,#143006,
#143007,#143008,#143009,#143010,#143011,#143012,#143013,#143014,#143015,
#143016,#143017,#143018,#143019,#143020,#143021,#143022,#143023,#143024,
#143025,#143026,#143027),.UNSPECIFIED.,.F.,.F.,(4,3,3,3,3,3,3,3,3,3,3,3,
3,3,3,3,3,3,3,3,4),(2.95674022625425E-11,0.0590835197265977,0.0644729979353127,
0.123579051781818,0.184080539447088,0.2,0.281365249285575,0.299014851252803,
0.381024531865931,0.4,0.503697847279184,0.5318585389134,0.6,0.677481482895928,
0.757900617461102,0.764520989067543,0.8,0.866123989598734,0.931596831446147,
0.99706967329356,1.),.UNSPECIFIED.);
#29836=B_SPLINE_CURVE_WITH_KNOTS('',3,(#143056,#143057,#143058,#143059,
#143060,#143061,#143062,#143063,#143064,#143065,#143066,#143067,#143068),
 .UNSPECIFIED.,.F.,.F.,(4,3,3,3,4),(0.,0.258977222641322,0.520864720696312,
0.787686771689713,1.),.UNSPECIFIED.);
#29837=B_SPLINE_CURVE_WITH_KNOTS('',3,(#143111,#143112,#143113,#143114,
#143115,#143116,#143117,#143118,#143119,#143120,#143121,#143122,#143123,
#143124,#143125,#143126,#143127,#143128,#143129,#143130,#143131,#143132,
#143133,#143134,#143135,#143136,#143137,#143138,#143139,#143140,#143141,
#143142,#143143,#143144,#143145,#143146,#143147,#143148,#143149,#143150,
#143151,#143152,#143153,#143154,#143155,#143156,#143157,#143158,#143159,
#143160,#143161,#143162,#143163,#143164,#143165,#143166,#143167,#143168,
#143169,#143170,#143171,#143172,#143173,#143174,#143175,#143176,#143177),
 .UNSPECIFIED.,.F.,.F.,(4,3,3,3,3,3,3,3,3,3,3,3,3,3,3,3,3,3,3,3,3,3,4),
(0.,0.08027036975129,0.15868466085864,0.23464894294463,0.250000000000064,
0.323297303695469,0.394307113162551,0.437500000000121,0.468750000000125,
0.484375000000122,0.49218750000012,0.497768800090433,0.500000000000119,
0.551027785102183,0.604025486376891,0.65818398549835,0.714271007151812,
0.750000000000059,0.808455080078342,0.869171922711029,0.931152591310257,
0.994693264380135,1.),.UNSPECIFIED.);
#29838=B_SPLINE_CURVE_WITH_KNOTS('',3,(#143178,#143179,#143180,#143181,
#143182,#143183,#143184,#143185,#143186,#143187,#143188,#143189,#143190,
#143191,#143192,#143193,#143194,#143195,#143196,#143197,#143198,#143199,
#143200,#143201,#143202,#143203,#143204,#143205,#143206,#143207,#143208,
#143209,#143210,#143211,#143212,#143213,#143214,#143215,#143216,#143217,
#143218,#143219,#143220,#143221,#143222,#143223,#143224,#143225,#143226,
#143227,#143228,#143229,#143230,#143231,#143232,#143233,#143234,#143235,
#143236,#143237,#143238),.UNSPECIFIED.,.F.,.F.,(4,3,3,3,3,3,3,3,3,3,3,3,
3,3,3,3,3,3,3,3,4),(0.,0.0500140916140122,0.102810472433336,0.157768197269118,
0.218317721152486,0.25,0.305665021786033,0.364108822971698,0.424270070064475,
0.486191448667807,0.5,0.5625,0.622367801824673,0.680496857852398,0.736297030446486,
0.75,0.8125,0.867577176507066,0.920267714681305,0.970593913147975,1.),
 .UNSPECIFIED.);
#29839=B_SPLINE_CURVE_WITH_KNOTS('',3,(#143241,#143242,#143243,#143244,
#143245,#143246,#143247,#143248,#143249,#143250),.UNSPECIFIED.,.F.,.F.,
(4,2,2,2,4),(0.,0.25,0.5,0.75,0.999999989319756),.UNSPECIFIED.);
#29840=B_SPLINE_CURVE_WITH_KNOTS('',3,(#143252,#143253,#143254,#143255),
 .UNSPECIFIED.,.F.,.F.,(4,4),(0.,0.999980732155484),.UNSPECIFIED.);
#29841=B_SPLINE_CURVE_WITH_KNOTS('',3,(#143257,#143258,#143259,#143260),
 .UNSPECIFIED.,.F.,.F.,(4,4),(0.,1.),.UNSPECIFIED.);
#29842=B_SPLINE_CURVE_WITH_KNOTS('',3,(#143264,#143265,#143266,#143267,
#143268,#143269,#143270,#143271,#143272,#143273,#143274,#143275,#143276,
#143277,#143278,#143279,#143280,#143281,#143282,#143283,#143284,#143285,
#143286,#143287,#143288,#143289,#143290,#143291,#143292,#143293,#143294,
#143295,#143296,#143297,#143298,#143299,#143300),.UNSPECIFIED.,.F.,.F.,
(4,3,3,3,3,3,3,3,3,3,3,3,4),(2.99246483692683E-10,0.0840858906723014,0.168136003243227,
0.252183926484771,0.336208591087671,0.420255785707517,0.5,0.584777283150557,
0.669548215185025,0.75434071751584,0.839117300724285,0.923908041707433,
1.),.UNSPECIFIED.);
#29843=B_SPLINE_CURVE_WITH_KNOTS('',3,(#143303,#143304,#143305,#143306,
#143307,#143308),.UNSPECIFIED.,.F.,.F.,(4,2,4),(0.,0.5,0.999484898490112),
 .UNSPECIFIED.);
#29844=B_SPLINE_CURVE_WITH_KNOTS('',3,(#143354,#143355,#143356,#143357,
#143358,#143359,#143360,#143361,#143362,#143363,#143364,#143365,#143366,
#143367,#143368,#143369,#143370,#143371,#143372,#143373,#143374,#143375,
#143376,#143377,#143378,#143379,#143380,#143381,#143382,#143383,#143384,
#143385,#143386,#143387,#143388,#143389,#143390,#143391,#143392,#143393,
#143394,#143395,#143396,#143397,#143398,#143399,#143400,#143401,#143402,
#143403,#143404,#143405,#143406,#143407,#143408,#143409,#143410,#143411,
#143412,#143413,#143414,#143415,#143416,#143417,#143418,#143419,#143420,
#143421,#143422,#143423,#143424,#143425,#143426,#143427,#143428,#143429),
 .UNSPECIFIED.,.F.,.F.,(4,3,3,3,3,3,3,3,3,3,3,3,3,3,3,3,3,3,3,3,3,3,3,3,
3,4),(1.88018170531242E-9,0.0645057624885224,0.127700538116555,0.188893270247744,
0.250000000000156,0.30857082095324,0.366124740049286,0.422323360922472,
0.437500000000273,0.468750000000288,0.484375000000291,0.492187500000292,
0.496930650753609,0.500000000000293,0.538964511246705,0.578808443724839,
0.621606332793664,0.663892028395619,0.707754775287589,0.750000000000138,
0.796133698674557,0.843505573269289,0.892672648356596,0.942812405953015,
0.994119325581967,0.99999999896473),.UNSPECIFIED.);
#29845=B_SPLINE_CURVE_WITH_KNOTS('',3,(#143430,#143431,#143432,#143433,
#143434,#143435,#143436,#143437,#143438,#143439,#143440,#143441,#143442,
#143443,#143444,#143445,#143446,#143447,#143448,#143449,#143450,#143451,
#143452,#143453,#143454,#143455,#143456,#143457,#143458,#143459,#143460,
#143461,#143462,#143463,#143464,#143465,#143466,#143467,#143468,#143469,
#143470,#143471,#143472,#143473,#143474,#143475,#143476,#143477,#143478),
 .UNSPECIFIED.,.F.,.F.,(4,3,3,3,3,3,3,3,3,3,3,3,3,3,3,3,4),(1.15239154642677E-10,
0.0649165563113629,0.132403698407869,0.206726934240605,0.25,0.320782786022654,
0.393717759036282,0.469211508163737,0.5,0.575238128201483,0.648757748742531,
0.719054838158213,0.75,0.82388280728322,0.892741770995936,0.95719031445221,
1.),.UNSPECIFIED.);
#29846=B_SPLINE_CURVE_WITH_KNOTS('',3,(#143524,#143525,#143526,#143527,
#143528,#143529,#143530,#143531,#143532,#143533,#143534,#143535,#143536,
#143537,#143538,#143539,#143540,#143541,#143542,#143543,#143544,#143545,
#143546,#143547,#143548,#143549,#143550,#143551,#143552,#143553,#143554,
#143555,#143556,#143557,#143558,#143559,#143560,#143561,#143562,#143563,
#143564,#143565,#143566,#143567,#143568,#143569,#143570,#143571,#143572,
#143573,#143574,#143575,#143576,#143577,#143578,#143579,#143580,#143581),
 .UNSPECIFIED.,.F.,.F.,(4,3,3,3,3,3,3,3,3,3,3,3,3,3,3,3,3,3,3,4),(0.,0.0591362138677374,
0.120878268797879,0.18543913439894,0.25,0.267238582825178,0.329519130380692,
0.392905904843487,0.458231542232862,0.490447831179993,0.5,0.5658716799357,
0.633420574512136,0.703676255632175,0.732777413191121,0.75,0.821897558034854,
0.895738132611241,0.972481734941369,0.999925149981118),.UNSPECIFIED.);
#29847=B_SPLINE_CURVE_WITH_KNOTS('',3,(#143623,#143624,#143625,#143626,
#143627,#143628,#143629,#143630,#143631,#143632,#143633,#143634,#143635,
#143636,#143637,#143638,#143639,#143640,#143641),.UNSPECIFIED.,.F.,.F.,
(4,2,2,2,1,1,1,2,2,2,4),(0.,0.249999999999776,0.374999999999666,0.437499999999608,
0.468749999999578,0.484374999999568,0.49218749999957,0.496093749999578,
0.499999999999585,0.749999999999793,0.999999787290037),.UNSPECIFIED.);
#29848=B_SPLINE_CURVE_WITH_KNOTS('',3,(#143642,#143643,#143644,#143645,
#143646,#143647),.UNSPECIFIED.,.F.,.F.,(4,2,4),(0.,0.5,0.99999995988345),
 .UNSPECIFIED.);
#29849=B_SPLINE_CURVE_WITH_KNOTS('',3,(#143649,#143650,#143651,#143652,
#143653,#143654),.UNSPECIFIED.,.F.,.F.,(4,2,4),(0.,0.5,1.),
 .UNSPECIFIED.);
#29850=B_SPLINE_CURVE_WITH_KNOTS('',3,(#143690,#143691,#143692,#143693,
#143694,#143695,#143696,#143697,#143698,#143699,#143700,#143701,#143702,
#143703,#143704,#143705,#143706,#143707,#143708),.UNSPECIFIED.,.F.,.F.,
(4,2,2,2,1,1,1,2,2,2,4),(3.26475431587078E-8,0.249999999999144,0.374999999998711,
0.437499999998487,0.468749999998368,0.484374999998299,0.492187499998282,
0.496093749998283,0.499999999998285,0.749999999999143,0.999999893028112),
 .UNSPECIFIED.);
#29851=B_SPLINE_CURVE_WITH_KNOTS('',3,(#143792,#143793,#143794,#143795,
#143796,#143797,#143798,#143799,#143800,#143801,#143802,#143803,#143804,
#143805,#143806,#143807,#143808,#143809,#143810,#143811,#143812,#143813,
#143814,#143815,#143816,#143817,#143818,#143819,#143820,#143821,#143822,
#143823,#143824,#143825,#143826,#143827,#143828,#143829,#143830,#143831,
#143832,#143833,#143834,#143835,#143836,#143837,#143838,#143839,#143840,
#143841,#143842,#143843,#143844,#143845,#143846,#143847,#143848,#143849),
 .UNSPECIFIED.,.F.,.F.,(4,3,3,3,3,3,3,3,3,3,3,3,3,3,3,3,3,3,3,4),(7.4513935169651E-5,
0.0764390166688387,0.15077462552214,0.222227128795632,0.25,0.267224468266891,
0.337159446103622,0.405216324088469,0.47073909310234,0.5,0.509557862772661,
0.574682549819007,0.63847798460608,0.700563150132604,0.732763275912864,
0.75,0.812223755461616,0.876545948829822,0.940868142198028,1.),
 .UNSPECIFIED.);
#29852=B_SPLINE_CURVE_WITH_KNOTS('',3,(#143896,#143897,#143898,#143899,
#143900,#143901,#143902,#143903,#143904,#143905,#143906,#143907,#143908,
#143909,#143910,#143911,#143912,#143913,#143914,#143915,#143916,#143917,
#143918,#143919,#143920,#143921,#143922,#143923,#143924,#143925,#143926,
#143927,#143928,#143929,#143930,#143931,#143932,#143933,#143934,#143935,
#143936,#143937,#143938,#143939,#143940,#143941,#143942,#143943,#143944,
#143945,#143946,#143947,#143948,#143949,#143950,#143951,#143952,#143953,
#143954,#143955,#143956,#143957,#143958,#143959,#143960,#143961,#143962,
#143963,#143964,#143965,#143966,#143967,#143968),.UNSPECIFIED.,.F.,.F.,
(4,3,3,3,3,3,3,3,3,3,3,3,3,3,3,3,3,3,3,3,3,3,3,3,4),(0.,0.0533424467156048,
0.104743634528447,0.154982248749812,0.203334709437968,0.250000000000053,
0.296875000000063,0.341353352128222,0.384893437136361,0.427201223511014,
0.437500000000092,0.468750000000099,0.484375000000094,0.49218750000009,
0.496935227016766,0.500000000000086,0.556761117887998,0.615044467063844,
0.674247131807778,0.7348358278879,0.750000000000043,0.812906270780981,0.876937510189453,
0.942948224179702,1.),.UNSPECIFIED.);
#29853=B_SPLINE_CURVE_WITH_KNOTS('',3,(#143976,#143977,#143978,#143979,
#143980,#143981,#143982,#143983),.UNSPECIFIED.,.F.,.F.,(4,1,1,1,1,4),(1.14974297182232E-6,
0.199999999999993,0.399999999999986,0.599999999999979,0.799999999999972,
0.999999999999965),.UNSPECIFIED.);
#29854=B_SPLINE_CURVE_WITH_KNOTS('',3,(#143985,#143986,#143987,#143988,
#143989,#143990),.UNSPECIFIED.,.F.,.F.,(4,2,4),(0.,0.5,0.999787114378974),
 .UNSPECIFIED.);
#29855=B_SPLINE_CURVE_WITH_KNOTS('',3,(#143994,#143995,#143996,#143997),
 .UNSPECIFIED.,.F.,.F.,(4,4),(1.81327895980828E-5,1.),.UNSPECIFIED.);
#29856=B_SPLINE_CURVE_WITH_KNOTS('',3,(#143998,#143999,#144000,#144001),
 .UNSPECIFIED.,.F.,.F.,(4,4),(0.,1.),.UNSPECIFIED.);
#29857=B_SPLINE_CURVE_WITH_KNOTS('',3,(#144005,#144006,#144007,#144008,
#144009,#144010),.UNSPECIFIED.,.F.,.F.,(4,2,4),(5.64578029880314E-9,0.5,
0.999999996578219),.UNSPECIFIED.);
#29858=B_SPLINE_CURVE_WITH_KNOTS('',3,(#144012,#144013,#144014,#144015),
 .UNSPECIFIED.,.F.,.F.,(4,4),(0.,0.999999846333988),.UNSPECIFIED.);
#29859=B_SPLINE_CURVE_WITH_KNOTS('',3,(#144016,#144017,#144018,#144019),
 .UNSPECIFIED.,.F.,.F.,(4,4),(0.,1.),.UNSPECIFIED.);
#29860=B_SPLINE_CURVE_WITH_KNOTS('',3,(#144022,#144023,#144024,#144025,
#144026,#144027),.UNSPECIFIED.,.F.,.F.,(4,2,4),(0.,0.5,0.999999995317697),
 .UNSPECIFIED.);
#29861=B_SPLINE_CURVE_WITH_KNOTS('',3,(#144057,#144058,#144059,#144060,
#144061,#144062,#144063,#144064,#144065,#144066,#144067,#144068,#144069,
#144070,#144071,#144072,#144073,#144074,#144075,#144076,#144077,#144078),
 .UNSPECIFIED.,.F.,.F.,(4,3,3,3,3,3,3,4),(0.,0.234589466263676,0.25,0.467093428636511,
0.500000000000001,0.677237910839018,0.868423764703068,1.),.UNSPECIFIED.);
#29862=B_SPLINE_CURVE_WITH_KNOTS('',3,(#144097,#144098,#144099,#144100,
#144101,#144102,#144103,#144104,#144105,#144106,#144107,#144108,#144109,
#144110,#144111,#144112,#144113,#144114,#144115,#144116,#144117,#144118,
#144119,#144120,#144121),.UNSPECIFIED.,.F.,.F.,(4,3,3,3,3,3,3,3,4),(0.,
0.151395870213908,0.303640552398499,0.356919349785617,0.5,0.653533854511357,
0.807219568466739,0.960969667135148,1.),.UNSPECIFIED.);
#29863=B_SPLINE_CURVE_WITH_KNOTS('',3,(#144123,#144124,#144125,#144126,
#144127,#144128,#144129,#144130,#144131,#144132,#144133,#144134,#144135,
#144136,#144137,#144138,#144139,#144140,#144141),.UNSPECIFIED.,.F.,.F.,
(4,3,3,3,3,3,4),(7.3073587088353E-11,0.191104891355974,0.310139280686363,
0.5,0.678403737752968,0.853738983746465,0.999999999299965),
 .UNSPECIFIED.);
#29864=B_SPLINE_CURVE_WITH_KNOTS('',3,(#144160,#144161,#144162,#144163,
#144164,#144165,#144166,#144167,#144168,#144169,#144170,#144171,#144172),
 .UNSPECIFIED.,.F.,.F.,(4,2,2,1,2,2,4),(0.,0.249999999999996,0.374999999999994,
0.437499999999994,0.468749999999993,0.499999999999993,1.),.UNSPECIFIED.);
#29865=B_SPLINE_CURVE_WITH_KNOTS('',3,(#144174,#144175,#144176,#144177,
#144178,#144179,#144180,#144181,#144182,#144183,#144184,#144185,#144186,
#144187,#144188,#144189,#144190,#144191,#144192),.UNSPECIFIED.,.F.,.F.,
(4,3,3,3,3,3,4),(0.,0.175269520094249,0.326885779417009,0.5,0.695471343358672,
0.886047081605195,1.),.UNSPECIFIED.);
#29866=B_SPLINE_CURVE_WITH_KNOTS('',3,(#144211,#144212,#144213,#144214,
#144215,#144216,#144217,#144218,#144219,#144220,#144221,#144222,#144223,
#144224,#144225,#144226,#144227,#144228,#144229,#144230,#144231,#144232,
#144233,#144234,#144235,#144236,#144237,#144238,#144239,#144240,#144241,
#144242,#144243,#144244,#144245,#144246,#144247,#144248,#144249,#144250,
#144251,#144252,#144253,#144254,#144255,#144256,#144257,#144258,#144259,
#144260,#144261,#144262,#144263,#144264,#144265,#144266,#144267,#144268,
#144269,#144270,#144271,#144272,#144273,#144274,#144275,#144276,#144277,
#144278,#144279,#144280,#144281,#144282,#144283,#144284,#144285,#144286),
 .UNSPECIFIED.,.F.,.F.,(4,3,3,3,3,3,3,3,3,3,3,3,3,3,3,3,3,3,3,3,3,3,3,3,
3,4),(0.,0.0540181594619873,0.107259627625218,0.160152504466205,0.2125889741831,
0.250000000000005,0.297638439728598,0.344247373429098,0.375000000000007,
0.418390387038428,0.437500000000008,0.468750000000008,0.484375000000008,
0.492187500000008,0.498508254699402,0.500000000000007,0.549786412774844,
0.600525719911558,0.651666776290185,0.703442746339702,0.750000000000004,
0.802143792479376,0.856713325005992,0.912968224892903,0.972431465331863,
1.),.UNSPECIFIED.);
#29867=B_SPLINE_CURVE_WITH_KNOTS('',3,(#144287,#144288,#144289,#144290,
#144291,#144292,#144293,#144294,#144295,#144296,#144297,#144298,#144299,
#144300,#144301,#144302,#144303,#144304,#144305,#144306,#144307,#144308,
#144309,#144310,#144311,#144312,#144313,#144314,#144315,#144316,#144317,
#144318,#144319,#144320,#144321,#144322,#144323),.UNSPECIFIED.,.F.,.F.,
(4,3,3,3,3,3,3,3,3,3,3,3,4),(2.58573610941644E-9,0.0877143487115733,0.177079072050148,
0.268548046153447,0.360941000981022,0.45425873055312,0.5,0.5960451564699,
0.691319690101686,0.784873547168815,0.877122526712708,0.967109401539248,
0.999999999999998),.UNSPECIFIED.);
#29868=B_SPLINE_CURVE_WITH_KNOTS('',3,(#144327,#144328,#144329,#144330),
 .UNSPECIFIED.,.F.,.F.,(4,4),(4.0356730508919E-7,1.),.UNSPECIFIED.);
#29869=B_SPLINE_CURVE_WITH_KNOTS('',3,(#144332,#144333,#144334,#144335),
 .UNSPECIFIED.,.F.,.F.,(4,4),(0.,1.),.UNSPECIFIED.);
#29870=B_SPLINE_CURVE_WITH_KNOTS('',3,(#144336,#144337,#144338,#144339,
#144340,#144341),.UNSPECIFIED.,.F.,.F.,(4,2,4),(2.43156888848096E-9,0.5,
0.999999884413479),.UNSPECIFIED.);
#29871=B_SPLINE_CURVE_WITH_KNOTS('',3,(#144375,#144376,#144377,#144378),
 .UNSPECIFIED.,.F.,.F.,(4,4),(0.,1.),.UNSPECIFIED.);
#29872=B_SPLINE_CURVE_WITH_KNOTS('',3,(#144379,#144380,#144381,#144382,
#144383,#144384,#144385,#144386,#144387,#144388,#144389,#144390,#144391,
#144392,#144393,#144394,#144395,#144396,#144397,#144398,#144399,#144400,
#144401,#144402,#144403,#144404,#144405,#144406,#144407,#144408,#144409,
#144410,#144411,#144412,#144413,#144414,#144415,#144416,#144417,#144418,
#144419,#144420,#144421,#144422,#144423,#144424,#144425,#144426,#144427,
#144428,#144429,#144430),.UNSPECIFIED.,.F.,.F.,(4,3,3,3,3,3,3,3,3,3,3,3,
3,3,3,3,3,4),(0.,0.0957981934517183,0.15219996804128,0.252309664578997,
0.298257045469927,0.395284374327465,0.423903020998006,0.514444308082931,
0.534757075323245,0.617053500050071,0.634002062399949,0.726315695614125,
0.734247069000456,0.75,0.833172583328939,0.917077637468813,0.92726894121381,
0.999999840603065),.UNSPECIFIED.);
#29873=B_SPLINE_CURVE_WITH_KNOTS('',3,(#144547,#144548,#144549,#144550,
#144551,#144552,#144553,#144554,#144555,#144556,#144557,#144558,#144559,
#144560,#144561,#144562,#144563,#144564,#144565,#144566,#144567,#144568,
#144569,#144570,#144571,#144572,#144573,#144574,#144575,#144576,#144577,
#144578,#144579,#144580,#144581,#144582,#144583,#144584,#144585,#144586,
#144587,#144588,#144589,#144590,#144591,#144592,#144593,#144594,#144595,
#144596,#144597,#144598,#144599,#144600,#144601,#144602,#144603,#144604,
#144605,#144606,#144607),.UNSPECIFIED.,.F.,.F.,(4,3,3,3,3,3,3,3,3,3,3,3,
3,3,3,3,3,3,3,3,4),(0.,0.0425624458950865,0.116206183539185,0.192860166407389,
0.250000000000012,0.27276457930784,0.356076441493708,0.437500000000022,
0.442882711310174,0.468750000000024,0.484375000000025,0.492187500000025,
0.499023437500025,0.500000000000025,0.522730186331662,0.588945716513302,
0.660745283754589,0.73803325288249,0.821793505481187,0.913325820897002,
1.),.UNSPECIFIED.);
#29874=B_SPLINE_CURVE_WITH_KNOTS('',3,(#144662,#144663,#144664,#144665),
 .UNSPECIFIED.,.F.,.F.,(4,4),(2.76646221668592E-8,0.999999999601257),
 .UNSPECIFIED.);
#29875=B_SPLINE_CURVE_WITH_KNOTS('',3,(#144683,#144684,#144685,#144686),
 .UNSPECIFIED.,.F.,.F.,(4,4),(0.,1.),.UNSPECIFIED.);
#29876=B_SPLINE_CURVE_WITH_KNOTS('',3,(#144687,#144688,#144689,#144690,
#144691,#144692,#144693,#144694,#144695,#144696),.UNSPECIFIED.,.F.,.F.,
(4,3,3,4),(0.,0.320682330949903,0.721806394077566,0.999999187310508),
 .UNSPECIFIED.);
#29877=B_SPLINE_CURVE_WITH_KNOTS('',3,(#144774,#144775,#144776,#144777,
#144778,#144779,#144780,#144781,#144782,#144783,#144784,#144785,#144786,
#144787,#144788,#144789,#144790,#144791,#144792,#144793,#144794,#144795,
#144796,#144797,#144798,#144799,#144800,#144801,#144802,#144803,#144804,
#144805,#144806,#144807,#144808,#144809,#144810,#144811,#144812,#144813),
 .UNSPECIFIED.,.F.,.F.,(4,3,3,3,3,3,3,3,3,3,3,3,3,4),(0.,0.0869925140249388,
0.176057719812484,0.227923063318706,0.25,0.347107344576692,0.373508987913521,
0.457206582786402,0.525564563146908,0.621947310577417,0.687900209279146,
0.75,0.856805504898761,1.),.UNSPECIFIED.);
#29878=B_SPLINE_CURVE_WITH_KNOTS('',3,(#144874,#144875,#144876,#144877,
#144878,#144879,#144880,#144881,#144882,#144883,#144884,#144885,#144886,
#144887,#144888,#144889,#144890,#144891,#144892),.UNSPECIFIED.,.F.,.F.,
(4,3,3,3,3,3,4),(0.,0.249999996790803,0.443916949821269,0.622856224213297,
0.793090569014283,0.95621014018365,0.99999998716321),.UNSPECIFIED.);
#29879=B_SPLINE_CURVE_WITH_KNOTS('',3,(#144951,#144952,#144953,#144954,
#144955,#144956,#144957,#144958,#144959,#144960,#144961,#144962,#144963,
#144964,#144965,#144966,#144967,#144968,#144969,#144970,#144971,#144972,
#144973,#144974,#144975,#144976,#144977,#144978,#144979,#144980,#144981,
#144982,#144983,#144984,#144985,#144986,#144987,#144988,#144989,#144990,
#144991,#144992,#144993,#144994,#144995,#144996,#144997,#144998,#144999,
#145000,#145001,#145002,#145003,#145004,#145005,#145006,#145007,#145008,
#145009,#145010,#145011,#145012,#145013,#145014),.UNSPECIFIED.,.F.,.F.,
(4,3,3,3,3,3,3,3,3,3,3,3,3,3,3,3,3,3,3,3,3,4),(0.,0.0515115307653243,0.101465397062888,
0.150637075398089,0.200318537699045,0.25,0.29693317301872,0.343393495909613,
0.389491202373321,0.435297728742739,0.481002063614683,0.526697487832872,
0.572477227545014,0.618626393499786,0.665023537321272,0.712032314967765,
0.75,0.798017220119162,0.848512915089372,0.898501582141251,0.94994422338954,
1.),.UNSPECIFIED.);
#29880=B_SPLINE_CURVE_WITH_KNOTS('',3,(#145015,#145016,#145017,#145018,
#145019,#145020,#145021,#145022,#145023,#145024,#145025,#145026,#145027,
#145028,#145029,#145030,#145031,#145032,#145033,#145034,#145035,#145036,
#145037,#145038,#145039,#145040,#145041,#145042,#145043,#145044,#145045,
#145046,#145047,#145048,#145049,#145050,#145051,#145052,#145053,#145054,
#145055,#145056,#145057,#145058,#145059,#145060,#145061,#145062,#145063,
#145064,#145065,#145066),.UNSPECIFIED.,.F.,.F.,(4,3,3,3,3,3,3,3,3,3,3,3,
3,3,3,3,3,4),(0.,0.125000000000006,0.250000000000012,0.280520976309935,
0.375000000000025,0.437500000000022,0.468750000000023,0.491716905195655,
0.500000000000025,0.558110951675689,0.585560299651521,0.65132272256481,
0.7199614534636,0.750000000000013,0.810121111210684,0.882590846461046,0.941450522833902,
0.999999999705399),.UNSPECIFIED.);
#29881=B_SPLINE_CURVE_WITH_KNOTS('',3,(#145095,#145096,#145097,#145098),
 .UNSPECIFIED.,.F.,.F.,(4,4),(1.29351143961801E-10,1.),.UNSPECIFIED.);
#29882=B_SPLINE_CURVE_WITH_KNOTS('',3,(#145099,#145100,#145101,#145102,
#145103,#145104,#145105),.UNSPECIFIED.,.F.,.F.,(4,3,4),(0.,0.677804750977032,
1.),.UNSPECIFIED.);
#29883=B_SPLINE_CURVE_WITH_KNOTS('',3,(#145132,#145133,#145134,#145135,
#145136,#145137,#145138,#145139,#145140,#145141,#145142,#145143,#145144,
#145145,#145146,#145147,#145148,#145149,#145150,#145151,#145152,#145153,
#145154,#145155,#145156,#145157,#145158,#145159,#145160,#145161,#145162,
#145163,#145164,#145165,#145166,#145167,#145168,#145169,#145170,#145171,
#145172,#145173,#145174,#145175,#145176,#145177,#145178,#145179,#145180,
#145181,#145182,#145183,#145184,#145185,#145186,#145187,#145188,#145189),
 .UNSPECIFIED.,.F.,.F.,(4,3,3,3,3,3,3,3,3,3,3,3,3,3,3,3,3,3,3,4),(0.,0.0737543241068619,
0.145149085023866,0.213031250709547,0.25,0.31502001785785,0.376605523383129,
0.421989433543571,0.491109534182326,0.5,0.565784535589313,0.630017581033254,
0.692094840029708,0.74989259282035,0.75,0.807003071333124,0.861841800614466,
0.915723256400594,0.968482946301467,1.),.UNSPECIFIED.);
#29884=B_SPLINE_CURVE_WITH_KNOTS('',3,(#145257,#145258,#145259,#145260,
#145261,#145262,#145263,#145264,#145265,#145266,#145267,#145268,#145269,
#145270,#145271,#145272,#145273,#145274,#145275,#145276,#145277,#145278,
#145279,#145280,#145281,#145282,#145283,#145284,#145285,#145286,#145287,
#145288,#145289,#145290,#145291,#145292,#145293),.UNSPECIFIED.,.F.,.F.,
(4,3,3,3,3,3,3,3,3,3,3,3,4),(3.50891768936283E-5,0.0843180394326553,0.168576167404038,
0.252840967918579,0.337085284669226,0.421349077367453,0.5,0.584702371040028,
0.669398412098734,0.754116061274742,0.838817762323477,0.923533655731094,
1.),.UNSPECIFIED.);
#29885=B_SPLINE_CURVE_WITH_KNOTS('',3,(#145297,#145298,#145299,#145300,
#145301,#145302,#145303),.UNSPECIFIED.,.F.,.F.,(4,1,1,1,4),(0.,0.25,0.5,
0.75,1.),.UNSPECIFIED.);
#29886=B_SPLINE_CURVE_WITH_KNOTS('',3,(#145305,#145306,#145307,#145308,
#145309,#145310,#145311,#145312,#145313,#145314,#145315,#145316,#145317,
#145318,#145319,#145320,#145321,#145322,#145323,#145324,#145325,#145326,
#145327,#145328,#145329,#145330,#145331,#145332),.UNSPECIFIED.,.F.,.F.,
(4,3,3,3,3,3,3,3,3,4),(0.,0.160240490642099,0.320480981284198,0.3333333333333,
0.46964884726713,0.60577008378555,0.6666666666667,0.691528796069726,0.919246361875947,
1.),.UNSPECIFIED.);
#29887=B_SPLINE_CURVE_WITH_KNOTS('',3,(#145334,#145335,#145336,#145337,
#145338,#145339,#145340,#145341,#145342,#145343,#145344,#145345,#145346,
#145347,#145348,#145349,#145350,#145351,#145352,#145353,#145354,#145355,
#145356,#145357,#145358,#145359,#145360,#145361),.UNSPECIFIED.,.F.,.F.,
(4,3,3,3,3,3,3,3,3,4),(0.,0.223462991617817,0.313827993255978,0.3333333333333,
0.467162238544904,0.601309120325676,0.6666666666667,0.684616796514498,0.8431885857511,
1.),.UNSPECIFIED.);
#29888=B_SPLINE_CURVE_WITH_KNOTS('',3,(#145363,#145364,#145365,#145366,
#145367,#145368,#145369,#145370,#145371,#145372,#145373,#145374,#145375,
#145376,#145377,#145378,#145379,#145380,#145381,#145382,#145383,#145384,
#145385,#145386,#145387,#145388,#145389,#145390,#145391,#145392,#145393,
#145394,#145395),.UNSPECIFIED.,.F.,.F.,(4,1,2,2,2,2,2,2,2,2,2,2,2,2,2,2,
4),(0.,0.0312500000000643,0.0546875000001129,0.0625000000001292,0.109375000000229,
0.125000000000262,0.246093750000515,0.250000000000523,0.373046875000797,
0.375000000000802,0.499023437501035,0.500000000001037,0.624023437500881,
0.62500000000088,0.746093750000591,0.750000000000581,1.),.UNSPECIFIED.);
#29889=B_SPLINE_CURVE_WITH_KNOTS('',3,(#145417,#145418,#145419,#145420,
#145421,#145422,#145423,#145424,#145425,#145426,#145427,#145428,#145429,
#145430,#145431,#145432,#145433,#145434,#145435,#145436,#145437,#145438,
#145439,#145440,#145441,#145442,#145443,#145444,#145445,#145446,#145447,
#145448,#145449,#145450,#145451,#145452,#145453,#145454,#145455,#145456,
#145457,#145458,#145459,#145460,#145461,#145462,#145463,#145464,#145465,
#145466,#145467,#145468,#145469,#145470,#145471,#145472,#145473,#145474,
#145475,#145476,#145477,#145478,#145479,#145480,#145481,#145482,#145483,
#145484,#145485,#145486,#145487,#145488,#145489,#145490,#145491,#145492,
#145493,#145494,#145495,#145496,#145497,#145498),.UNSPECIFIED.,.F.,.F.,
(4,3,3,3,3,3,3,3,3,3,3,3,3,3,3,3,3,3,3,3,3,3,3,3,3,3,3,4),(0.,0.0588671038353967,
0.115769444603005,0.171765650658291,0.226748779862293,0.250000000000507,
0.312500000000632,0.320312500000644,0.326103898030806,0.328125000000656,
0.343750000000655,0.375000000000631,0.424118674845255,0.47154061341085,
0.500000000000517,0.545140118142051,0.562500000000471,0.578125000000458,
0.592606776586451,0.593750000000444,0.625000000000417,0.676269578279683,
0.729670216140662,0.750000000000281,0.812499188271712,0.874919170302411,
0.940466393599129,0.999996753086006),.UNSPECIFIED.);
#29890=B_SPLINE_CURVE_WITH_KNOTS('',3,(#145502,#145503,#145504,#145505,
#145506,#145507,#145508,#145509,#145510,#145511,#145512,#145513,#145514,
#145515,#145516,#145517,#145518,#145519,#145520,#145521,#145522,#145523,
#145524,#145525,#145526,#145527,#145528,#145529,#145530,#145531,#145532,
#145533,#145534,#145535,#145536,#145537,#145538,#145539,#145540,#145541,
#145542,#145543,#145544,#145545,#145546,#145547,#145548,#145549,#145550,
#145551,#145552,#145553,#145554,#145555,#145556,#145557,#145558,#145559,
#145560,#145561,#145562,#145563,#145564,#145565,#145566,#145567,#145568,
#145569,#145570,#145571,#145572,#145573,#145574),.UNSPECIFIED.,.F.,.F.,
(4,3,3,3,3,3,3,3,3,3,3,3,3,3,3,3,3,3,3,3,3,3,3,3,4),(1.9928678793837E-13,
0.0860107073934107,0.170441003692805,0.249999999999952,0.332517288333061,
0.413780234995208,0.437499999999927,0.468749999999926,0.484374999999937,
0.492187499999939,0.497856535392512,0.499999999999941,0.548330130830557,
0.595519789803843,0.641493515213737,0.686233649869448,0.729763227325348,
0.771593001760249,0.812496612229918,0.852092647954145,0.874999999999985,
0.912928094030672,0.950130538294064,0.986349268772354,1.),.UNSPECIFIED.);
#29891=B_SPLINE_CURVE_WITH_KNOTS('',3,(#145577,#145578,#145579,#145580,
#145581,#145582),.UNSPECIFIED.,.F.,.F.,(4,2,4),(-0.541273296520499,-0.270636648260383,
-0.132804212465021),.UNSPECIFIED.);
#29892=B_SPLINE_CURVE_WITH_KNOTS('',3,(#145583,#145584,#145585,#145586,
#145587,#145588),.UNSPECIFIED.,.F.,.F.,(4,2,4),(-1.54420814271699,-1.40637570692167,
-1.13573905866164),.UNSPECIFIED.);
#29893=B_SPLINE_CURVE_WITH_KNOTS('',3,(#145601,#145602,#145603,#145604,
#145605,#145606,#145607,#145608,#145609,#145610,#145611,#145612,#145613,
#145614,#145615,#145616),.UNSPECIFIED.,.F.,.F.,(4,3,3,3,3,4),(2.40891265344009E-9,
0.20000000192713,0.400000001445348,0.600000000963565,0.800000000481783,
1.),.UNSPECIFIED.);
#29894=B_SPLINE_CURVE_WITH_KNOTS('',3,(#145622,#145623,#145624,#145625,
#145626),.UNSPECIFIED.,.F.,.F.,(4,1,4),(0.,0.5,1.),.UNSPECIFIED.);
#29895=B_SPLINE_CURVE_WITH_KNOTS('',3,(#145704,#145705,#145706,#145707,
#145708,#145709,#145710,#145711,#145712,#145713,#145714,#145715,#145716,
#145717,#145718,#145719,#145720,#145721,#145722,#145723,#145724,#145725,
#145726,#145727,#145728,#145729,#145730,#145731,#145732,#145733,#145734,
#145735,#145736,#145737,#145738,#145739,#145740,#145741,#145742,#145743,
#145744,#145745,#145746,#145747,#145748,#145749,#145750,#145751,#145752,
#145753,#145754,#145755,#145756,#145757,#145758,#145759,#145760,#145761,
#145762,#145763,#145764,#145765,#145766,#145767,#145768,#145769,#145770,
#145771,#145772,#145773,#145774,#145775,#145776,#145777,#145778,#145779,
#145780,#145781,#145782,#145783,#145784,#145785,#145786,#145787,#145788,
#145789,#145790,#145791,#145792,#145793,#145794,#145795,#145796,#145797),
 .UNSPECIFIED.,.F.,.F.,(4,3,3,3,3,3,3,3,3,3,3,3,3,3,3,3,3,3,3,3,3,3,3,3,
3,3,3,3,3,3,3,4),(0.,0.0503273433392803,0.0705363966084534,0.09090909090909,
0.145845069792584,0.165424748295987,0.1818181818182,0.254342976911016,0.260135405827298,
0.2727272727273,0.354924390092219,0.3636363636364,0.43720034945726,0.449680449551842,
0.4545454545455,0.524937984162795,0.54443382589536,0.5454545454545,0.599437773241359,
0.6363636363636,0.639231171883239,0.701503428544661,0.7272727272727,0.733981119727695,
0.796476371383321,0.8181818181818,0.82875679278927,0.887282233501452,0.9090909090909,
0.92353921349181,0.975376204950871,0.999999996385405),.UNSPECIFIED.);
#29896=B_SPLINE_CURVE_WITH_KNOTS('',3,(#145800,#145801,#145802,#145803,
#145804,#145805,#145806,#145807,#145808,#145809,#145810,#145811,#145812,
#145813,#145814,#145815,#145816,#145817,#145818,#145819,#145820,#145821,
#145822,#145823,#145824,#145825,#145826,#145827,#145828,#145829,#145830),
 .UNSPECIFIED.,.F.,.F.,(4,3,3,3,3,3,3,3,3,3,4),(1.55097127508771E-10,0.185276535990514,
0.249999999999993,0.263984396772149,0.374999999999989,0.437499999999986,
0.499999999999984,0.691147771436497,0.825408769424091,0.970656694537131,
1.),.UNSPECIFIED.);
#29897=B_SPLINE_CURVE_WITH_KNOTS('',3,(#145836,#145837,#145838,#145839,
#145840,#145841,#145842,#145843,#145844,#145845,#145846,#145847,#145848,
#145849,#145850,#145851,#145852,#145853,#145854),.UNSPECIFIED.,.F.,.F.,
(4,3,3,3,3,3,4),(0.,0.249999999999992,0.374999999999993,0.463820810658223,
0.499999999999994,0.804024102868561,1.),.UNSPECIFIED.);
#29898=B_SPLINE_CURVE_WITH_KNOTS('',3,(#145871,#145872,#145873,#145874,
#145875,#145876,#145877,#145878,#145879,#145880),.UNSPECIFIED.,.F.,.F.,
(4,3,3,4),(0.,0.416125778815456,0.832277185977338,1.),.UNSPECIFIED.);
#29899=B_SPLINE_CURVE_WITH_KNOTS('',3,(#145887,#145888,#145889,#145890,
#145891,#145892,#145893,#145894,#145895,#145896,#145897,#145898,#145899,
#145900,#145901,#145902,#145903,#145904,#145905,#145906,#145907,#145908,
#145909,#145910,#145911,#145912,#145913,#145914,#145915,#145916,#145917,
#145918,#145919,#145920,#145921,#145922,#145923,#145924,#145925,#145926,
#145927,#145928,#145929,#145930,#145931,#145932,#145933,#145934,#145935,
#145936,#145937,#145938,#145939,#145940,#145941,#145942,#145943,#145944,
#145945,#145946,#145947),.UNSPECIFIED.,.F.,.F.,(4,3,3,3,3,3,3,3,3,3,3,3,
3,3,3,3,3,3,3,3,4),(0.,0.0302549049560431,0.107699539561875,0.187447489182287,
0.268742965198622,0.350914596186216,0.43361546396603,0.5,0.516809378194048,
0.583584210388533,0.597628782117945,0.660260938893525,0.676918155576055,
0.739525996857477,0.756610374301218,0.817971707078341,0.838101869863211,
0.902215138768424,0.922705812894093,0.990587366249333,1.),.UNSPECIFIED.);
#29900=B_SPLINE_CURVE_WITH_KNOTS('',3,(#146035,#146036,#146037,#146038,
#146039,#146040),.UNSPECIFIED.,.F.,.F.,(4,2,4),(3.71650158233969E-7,0.5,
0.999999989920246),.UNSPECIFIED.);
#29901=B_SPLINE_CURVE_WITH_KNOTS('',3,(#146041,#146042,#146043,#146044,
#146045,#146046,#146047,#146048,#146049,#146050,#146051,#146052,#146053,
#146054,#146055,#146056,#146057,#146058,#146059,#146060,#146061,#146062,
#146063,#146064,#146065,#146066,#146067,#146068,#146069,#146070,#146071,
#146072,#146073,#146074,#146075,#146076,#146077),.UNSPECIFIED.,.F.,.F.,
(4,3,3,3,3,3,3,3,3,3,3,3,4),(0.,0.0851665874734178,0.173246627155873,0.267902347683297,
0.368005119889117,0.478252701139369,0.5,0.601785236450079,0.701338926617578,
0.797284493127895,0.890006807195087,0.978859996903235,0.999999997120075),
 .UNSPECIFIED.);
#29902=B_SPLINE_CURVE_WITH_KNOTS('',3,(#146082,#146083,#146084,#146085,
#146086,#146087,#146088,#146089,#146090,#146091,#146092,#146093,#146094,
#146095,#146096,#146097,#146098,#146099,#146100,#146101,#146102,#146103,
#146104,#146105,#146106,#146107,#146108,#146109,#146110,#146111,#146112,
#146113,#146114,#146115,#146116,#146117,#146118,#146119,#146120,#146121,
#146122,#146123,#146124,#146125,#146126,#146127,#146128,#146129,#146130),
 .UNSPECIFIED.,.F.,.F.,(4,3,3,3,3,3,3,3,3,3,3,3,3,3,3,3,4),(9.31491747942225E-7,
0.0775965643526843,0.154644840464124,0.231115057634255,0.25,0.321927191564919,
0.393664323259736,0.465280451197901,0.5,0.571646826427887,0.643349061639341,
0.715296736344095,0.75,0.826607919696912,0.903602320363381,0.981339531684117,
1.),.UNSPECIFIED.);
#29903=B_SPLINE_CURVE_WITH_KNOTS('',3,(#146168,#146169,#146170,#146171,
#146172,#146173,#146174,#146175,#146176,#146177,#146178,#146179,#146180,
#146181,#146182,#146183,#146184,#146185,#146186,#146187,#146188,#146189),
 .UNSPECIFIED.,.F.,.F.,(4,3,3,3,3,3,3,4),(3.08423462885857E-7,0.152032233615953,
0.306191896926236,0.463527373595914,0.5,0.661792255427938,0.830896126248164,
0.99999999706839),.UNSPECIFIED.);
#29904=B_SPLINE_CURVE_WITH_KNOTS('',3,(#146227,#146228,#146229,#146230,
#146231,#146232,#146233,#146234,#146235,#146236,#146237,#146238,#146239,
#146240,#146241,#146242,#146243,#146244,#146245,#146246,#146247,#146248,
#146249,#146250,#146251,#146252,#146253,#146254,#146255,#146256,#146257,
#146258,#146259,#146260,#146261,#146262,#146263,#146264,#146265,#146266,
#146267,#146268,#146269,#146270,#146271,#146272,#146273,#146274,#146275,
#146276,#146277,#146278,#146279,#146280,#146281),.UNSPECIFIED.,.F.,.F.,
(4,3,3,3,3,3,3,3,3,3,3,3,3,3,3,3,3,3,4),(0.,0.113195272986155,0.216845394807799,
0.249999999999949,0.329316019412936,0.374999999999922,0.43749999999991,
0.468749999999903,0.484374999999899,0.4921874999999,0.4999999999999,0.591157716507977,
0.673823762126518,0.682315433016053,0.761940801371688,0.838990173165727,
0.914264268728704,0.988334189438011,1.),.UNSPECIFIED.);
#29905=B_SPLINE_CURVE_WITH_KNOTS('',3,(#146282,#146283,#146284,#146285,
#146286,#146287,#146288,#146289,#146290,#146291,#146292,#146293,#146294),
 .UNSPECIFIED.,.F.,.F.,(4,3,3,3,4),(0.,0.286212728725273,0.5,0.62499418580237,
1.),.UNSPECIFIED.);
#29906=B_SPLINE_CURVE_WITH_KNOTS('',3,(#146301,#146302,#146303,#146304,
#146305,#146306,#146307,#146308,#146309,#146310),.UNSPECIFIED.,.F.,.F.,
(4,3,3,4),(6.80373258488048E-7,0.3333333333333,0.6666666666667,1.),
 .UNSPECIFIED.);
#29907=B_SPLINE_CURVE_WITH_KNOTS('',3,(#146312,#146313,#146314,#146315,
#146316,#146317,#146318,#146319,#146320),.UNSPECIFIED.,.F.,.F.,(4,1,2,2,
4),(0.,0.249999999999992,0.43749999999999,0.499999999999991,1.),
 .UNSPECIFIED.);
#29908=B_SPLINE_CURVE_WITH_KNOTS('',3,(#146322,#146323,#146324,#146325,
#146326,#146327,#146328,#146329,#146330,#146331),.UNSPECIFIED.,.F.,.F.,
(4,3,3,4),(1.28220999446224E-10,0.395671114820227,0.5,0.999991077247271),
 .UNSPECIFIED.);
#29909=B_SPLINE_CURVE_WITH_KNOTS('',3,(#146335,#146336,#146337,#146338,
#146339,#146340,#146341),.UNSPECIFIED.,.F.,.F.,(4,3,4),(6.08353928510026E-5,
0.5,1.),.UNSPECIFIED.);
#29910=B_SPLINE_CURVE_WITH_KNOTS('',3,(#146343,#146344,#146345,#146346,
#146347,#146348,#146349,#146350,#146351),.UNSPECIFIED.,.F.,.F.,(4,1,2,2,
4),(0.,0.250000000000012,0.437500000000015,0.500000000000015,1.),
 .UNSPECIFIED.);
#29911=B_SPLINE_CURVE_WITH_KNOTS('',3,(#146353,#146354,#146355,#146356,
#146357,#146358,#146359,#146360,#146361,#146362),.UNSPECIFIED.,.F.,.F.,
(4,3,3,4),(0.,0.3333333333333,0.6666666666667,1.),.UNSPECIFIED.);
#29912=B_SPLINE_CURVE_WITH_KNOTS('',3,(#146370,#146371,#146372,#146373,
#146374,#146375,#146376,#146377,#146378,#146379,#146380,#146381,#146382,
#146383,#146384,#146385,#146386,#146387,#146388,#146389,#146390,#146391,
#146392,#146393,#146394,#146395,#146396,#146397),.UNSPECIFIED.,.F.,.F.,
(4,3,3,3,3,3,3,3,3,4),(7.74771400272031E-10,0.101808906684311,0.209007899927755,
0.319213880211576,0.433855115514003,0.5,0.633394711854997,0.769804406161013,
0.909129008998587,1.),.UNSPECIFIED.);
#29913=B_SPLINE_CURVE_WITH_KNOTS('',3,(#146398,#146399,#146400,#146401,
#146402,#146403,#146404,#146405,#146406,#146407,#146408,#146409,#146410,
#146411,#146412,#146413,#146414,#146415,#146416,#146417,#146418,#146419,
#146420,#146421,#146422,#146423,#146424,#146425,#146426,#146427,#146428),
 .UNSPECIFIED.,.F.,.F.,(4,3,3,3,3,3,3,3,3,3,4),(1.19933140293008E-6,0.131666198962597,
0.263331198593791,0.381665599296896,0.5,0.604251376078316,0.707930455352679,
0.809312850427695,0.85384492428718,0.947128621831252,0.999999999652553),
 .UNSPECIFIED.);
#29914=B_SPLINE_CURVE_WITH_KNOTS('',3,(#146462,#146463,#146464,#146465,
#146466,#146467,#146468,#146469,#146470,#146471,#146472,#146473,#146474,
#146475,#146476,#146477,#146478,#146479,#146480,#146481,#146482,#146483,
#146484,#146485,#146486,#146487,#146488,#146489,#146490,#146491,#146492,
#146493,#146494,#146495,#146496,#146497,#146498,#146499,#146500,#146501,
#146502,#146503,#146504,#146505,#146506,#146507),.UNSPECIFIED.,.F.,.F.,
(4,3,3,3,3,3,3,3,3,3,3,3,3,3,3,4),(0.,0.075211943614556,0.149374857838509,
0.222342548672234,0.24999999999999,0.321768616869141,0.393073017284843,
0.46409303977792,0.535569779833439,0.606705160188612,0.678432144318015,
0.749999999999997,0.823144987521618,0.897062157875133,0.972435540661161,
0.999997996759352),.UNSPECIFIED.);
#29915=B_SPLINE_CURVE_WITH_KNOTS('',3,(#146509,#146510,#146511,#146512,
#146513,#146514,#146515,#146516,#146517,#146518,#146519,#146520,#146521,
#146522,#146523,#146524,#146525,#146526,#146527,#146528,#146529,#146530,
#146531,#146532,#146533,#146534,#146535,#146536,#146537,#146538,#146539,
#146540,#146541,#146542,#146543,#146544,#146545,#146546,#146547,#146548,
#146549,#146550,#146551,#146552,#146553,#146554),.UNSPECIFIED.,.F.,.F.,
(4,3,3,3,3,3,3,3,3,3,3,3,3,3,3,4),(2.60632369190722E-5,0.0888951179664604,
0.174399962481206,0.250000000000064,0.331533505523139,0.375000000000089,
0.437500000000094,0.468750000000098,0.48601987249119,0.500000000000103,
0.59250523058956,0.685269749800581,0.77894690994834,0.873279069584689,0.968967243094595,
1.),.UNSPECIFIED.);
#29916=B_SPLINE_CURVE_WITH_KNOTS('',3,(#146555,#146556,#146557,#146558,
#146559,#146560,#146561,#146562,#146563,#146564,#146565,#146566,#146567,
#146568,#146569,#146570,#146571,#146572,#146573,#146574,#146575,#146576,
#146577,#146578,#146579,#146580,#146581,#146582,#146583,#146584,#146585,
#146586,#146587,#146588,#146589,#146590,#146591,#146592,#146593,#146594,
#146595,#146596,#146597,#146598,#146599,#146600,#146601,#146602,#146603,
#146604,#146605,#146606),.UNSPECIFIED.,.F.,.F.,(4,3,3,3,3,3,3,3,3,3,3,3,
3,3,3,3,3,4),(0.,0.0950940026076129,0.176000808070446,0.250000000000337,
0.341236634860541,0.375000000000488,0.437500000000555,0.468750000000575,
0.484375000000586,0.49218750000059,0.497660107483689,0.500000000000595,
0.593847149190447,0.684418942999604,0.770105050752368,0.853413617968863,
0.933763885470399,1.),.UNSPECIFIED.);
#29917=B_SPLINE_CURVE_WITH_KNOTS('',3,(#146618,#146619,#146620,#146621,
#146622,#146623,#146624,#146625,#146626,#146627,#146628,#146629,#146630,
#146631,#146632,#146633,#146634,#146635,#146636,#146637,#146638,#146639,
#146640,#146641,#146642,#146643,#146644,#146645,#146646,#146647,#146648,
#146649,#146650,#146651,#146652,#146653,#146654),.UNSPECIFIED.,.F.,.F.,
(4,3,3,3,3,3,3,3,3,3,3,3,4),(0.,0.0971273534595727,0.19784551509468,0.294981060322154,
0.392102579023238,0.489225386209634,0.5,0.597127342691812,0.697845507018859,
0.794981048125729,0.892102564806965,0.989225372332922,1.),.UNSPECIFIED.);
#29918=B_SPLINE_CURVE_WITH_KNOTS('',3,(#146659,#146660,#146661,#146662,
#146663,#146664,#146665,#146666,#146667,#146668,#146669,#146670,#146671,
#146672,#146673,#146674,#146675,#146676,#146677,#146678,#146679,#146680,
#146681,#146682,#146683,#146684,#146685,#146686,#146687,#146688,#146689,
#146690,#146691,#146692,#146693,#146694,#146695),.UNSPECIFIED.,.F.,.F.,
(4,3,3,3,3,3,3,3,3,3,3,3,4),(1.27559074915848E-5,0.0877775439371207,0.175537174689751,
0.263312957184923,0.351076072595288,0.438847608910549,0.5,0.587764801064224,
0.675524453920255,0.763300261792778,0.851063397830683,0.938834946164502,
1.),.UNSPECIFIED.);
#29919=B_SPLINE_CURVE_WITH_KNOTS('',3,(#146748,#146749,#146750,#146751,
#146752,#146753),.UNSPECIFIED.,.F.,.F.,(4,2,4),(0.,0.5,1.),
 .UNSPECIFIED.);
#29920=B_SPLINE_CURVE_WITH_KNOTS('',3,(#146754,#146755,#146756,#146757,
#146758,#146759,#146760,#146761,#146762,#146763,#146764,#146765,#146766,
#146767,#146768,#146769,#146770,#146771,#146772,#146773,#146774,#146775,
#146776,#146777,#146778,#146779,#146780,#146781,#146782,#146783,#146784,
#146785,#146786,#146787,#146788,#146789,#146790),.UNSPECIFIED.,.F.,.F.,
(4,3,3,3,3,3,3,3,3,3,3,3,4),(0.,0.0171128929119407,0.190218335415339,0.250000000000002,
0.342243520336091,0.478336826191752,0.600628348881761,0.711130774206828,
0.811077032826439,0.875000000000001,0.901524999490352,0.982438882590532,
0.999999999878368),.UNSPECIFIED.);
#29921=B_SPLINE_CURVE_WITH_KNOTS('',3,(#146791,#146792,#146793,#146794,
#146795,#146796,#146797,#146798,#146799,#146800,#146801,#146802,#146803,
#146804,#146805,#146806,#146807,#146808,#146809,#146810,#146811,#146812,
#146813,#146814,#146815,#146816,#146817,#146818,#146819,#146820,#146821,
#146822,#146823,#146824,#146825,#146826,#146827,#146828,#146829,#146830,
#146831,#146832,#146833,#146834,#146835,#146836),.UNSPECIFIED.,.F.,.F.,
(4,3,3,3,3,3,3,3,3,3,3,3,3,3,3,4),(0.,0.0645900761448876,0.191864486905108,
0.206466423904439,0.332843758757244,0.418999255127509,0.449056161984938,
0.5,0.55881796002962,0.665119182877143,0.770052640000822,0.860961845222702,
0.874974935448854,0.951626181348456,0.98078069154919,1.),.UNSPECIFIED.);
#29922=B_SPLINE_CURVE_WITH_KNOTS('',3,(#146925,#146926,#146927,#146928,
#146929,#146930,#146931,#146932,#146933,#146934),.UNSPECIFIED.,.F.,.F.,
(4,2,2,2,4),(2.04724411541053E-5,0.25,0.5,0.75,1.),.UNSPECIFIED.);
#29923=B_SPLINE_CURVE_WITH_KNOTS('',3,(#146960,#146961,#146962,#146963,
#146964,#146965,#146966,#146967,#146968,#146969,#146970,#146971,#146972,
#146973,#146974,#146975,#146976,#146977,#146978,#146979,#146980,#146981,
#146982,#146983,#146984,#146985,#146986,#146987,#146988,#146989,#146990,
#146991,#146992,#146993,#146994,#146995,#146996,#146997,#146998,#146999,
#147000,#147001,#147002,#147003,#147004,#147005,#147006,#147007,#147008),
 .UNSPECIFIED.,.F.,.F.,(4,3,3,3,3,3,3,3,3,3,3,3,3,3,3,3,4),(6.71413000258348E-9,
0.0675549200623969,0.134250059598761,0.199881392616613,0.25,0.314474527898111,
0.378587916313949,0.442420828705989,0.5,0.563842660090154,0.627812047922959,
0.692296526943969,0.75,0.815739886669369,0.882105973707192,0.949759631829514,
0.999999999917591),.UNSPECIFIED.);
#29924=B_SPLINE_CURVE_WITH_KNOTS('',3,(#147009,#147010,#147011,#147012,
#147013,#147014,#147015,#147016,#147017,#147018,#147019,#147020,#147021),
 .UNSPECIFIED.,.F.,.F.,(4,3,3,3,4),(8.57328517562898E-9,0.311955394560608,
0.68142062992333,0.716097880297857,0.999997541441199),.UNSPECIFIED.);
#29925=B_SPLINE_CURVE_WITH_KNOTS('',3,(#147098,#147099,#147100,#147101,
#147102,#147103,#147104,#147105,#147106,#147107,#147108,#147109,#147110,
#147111,#147112,#147113),.UNSPECIFIED.,.F.,.F.,(4,3,3,3,3,4),(0.,0.25,0.486439579144033,
0.5,0.723876910618796,0.999999995616857),.UNSPECIFIED.);
#29926=B_SPLINE_CURVE_WITH_KNOTS('',3,(#147116,#147117,#147118,#147119,
#147120,#147121,#147122,#147123,#147124,#147125,#147126,#147127,#147128,
#147129,#147130,#147131,#147132,#147133,#147134,#147135,#147136,#147137,
#147138,#147139,#147140,#147141,#147142,#147143,#147144,#147145,#147146,
#147147,#147148,#147149,#147150,#147151,#147152,#147153,#147154,#147155,
#147156,#147157,#147158,#147159,#147160,#147161,#147162,#147163,#147164,
#147165,#147166,#147167,#147168,#147169,#147170,#147171,#147172,#147173,
#147174,#147175,#147176,#147177,#147178,#147179,#147180,#147181,#147182,
#147183,#147184,#147185,#147186,#147187,#147188,#147189,#147190,#147191,
#147192,#147193,#147194,#147195,#147196,#147197,#147198,#147199,#147200,
#147201,#147202,#147203,#147204,#147205,#147206,#147207,#147208,#147209,
#147210,#147211,#147212,#147213,#147214,#147215,#147216,#147217,#147218),
 .UNSPECIFIED.,.F.,.F.,(4,3,3,3,3,3,3,3,3,3,3,3,3,3,3,3,3,3,3,3,3,3,3,3,
3,3,3,3,3,3,3,3,3,3,4),(0.,0.0271165187228091,0.0552398060865508,0.0805407362303379,
0.11740359361469,0.125000000000032,0.16370517204992,0.191078705246372,0.238272675229252,
0.287092952974552,0.326326031747244,0.381913015873678,0.437500000000112,
0.46875000000012,0.484375000000123,0.492187500000123,0.496093750000122,
0.498046875000122,0.498822511000944,0.500000000000122,0.550409406874595,
0.600158691511717,0.649053077344895,0.666386441247509,0.716491390494292,
0.764059731313792,0.805072474509961,0.843451464096043,0.87500000000003,
0.911087483580574,0.917362256906651,0.944900321435466,0.972450160717733,
0.998184909872044,1.),.UNSPECIFIED.);
#29927=B_SPLINE_CURVE_WITH_KNOTS('',3,(#147266,#147267,#147268,#147269,
#147270,#147271,#147272,#147273,#147274,#147275,#147276,#147277,#147278,
#147279,#147280,#147281,#147282,#147283,#147284,#147285,#147286,#147287,
#147288,#147289,#147290,#147291,#147292,#147293,#147294,#147295,#147296,
#147297,#147298,#147299,#147300,#147301,#147302,#147303,#147304,#147305,
#147306,#147307,#147308,#147309,#147310,#147311,#147312,#147313,#147314,
#147315,#147316,#147317,#147318,#147319,#147320,#147321,#147322,#147323,
#147324,#147325,#147326,#147327,#147328,#147329,#147330,#147331,#147332,
#147333,#147334,#147335,#147336,#147337,#147338,#147339,#147340,#147341,
#147342,#147343,#147344,#147345,#147346,#147347,#147348,#147349,#147350,
#147351,#147352,#147353,#147354,#147355,#147356,#147357,#147358,#147359,
#147360,#147361,#147362,#147363,#147364,#147365,#147366,#147367,#147368,
#147369,#147370,#147371,#147372,#147373,#147374),.UNSPECIFIED.,.F.,.F.,
(4,3,3,3,3,3,3,3,3,3,3,3,3,3,3,3,3,3,3,3,3,3,3,3,3,3,3,3,3,3,3,3,3,3,3,
3,4),(0.,0.0394411860672323,0.0768210319013784,0.111222926509573,0.125,
0.177992535930477,0.22748163487749,0.240547850416774,0.25,0.304443876426796,
0.357336889466944,0.369855255981034,0.375,0.408918181293526,0.442204793974763,
0.474505684652355,0.499217918791245,0.5,0.523587954797688,0.547077257231226,
0.570611985363674,0.594260904686012,0.618209786487464,0.625,0.628457442866467,
0.669404051401495,0.711444340562682,0.75,0.757882574283839,0.804582763960082,
0.852316761814482,0.875,0.887184989110887,0.920800954231189,0.955229031809878,
0.990899627273368,1.),.UNSPECIFIED.);
#29928=B_SPLINE_CURVE_WITH_KNOTS('',3,(#147401,#147402,#147403,#147404,
#147405,#147406),.UNSPECIFIED.,.F.,.F.,(4,1,1,4),(0.,0.3333333333333,0.6666666666667,
1.),.UNSPECIFIED.);
#29929=B_SPLINE_CURVE_WITH_KNOTS('',3,(#147408,#147409,#147410,#147411,
#147412,#147413),.UNSPECIFIED.,.F.,.F.,(4,2,4),(3.86991307802236E-7,0.5,
1.),.UNSPECIFIED.);
#29930=B_SPLINE_CURVE_WITH_KNOTS('',3,(#147414,#147415,#147416,#147417,
#147418,#147419,#147420,#147421,#147422,#147423,#147424,#147425,#147426),
 .UNSPECIFIED.,.F.,.F.,(4,3,3,3,4),(3.21889366672523E-15,0.236467493280666,
0.483668534912693,0.741834250234171,0.99999996555565),.UNSPECIFIED.);
#29931=B_SPLINE_CURVE_WITH_KNOTS('',3,(#147445,#147446,#147447,#147448),
 .UNSPECIFIED.,.F.,.F.,(4,4),(0.,1.),.UNSPECIFIED.);
#29932=B_SPLINE_CURVE_WITH_KNOTS('',3,(#147451,#147452,#147453,#147454,
#147455,#147456,#147457,#147458,#147459,#147460,#147461,#147462,#147463,
#147464,#147465,#147466,#147467,#147468,#147469,#147470,#147471,#147472,
#147473,#147474,#147475,#147476,#147477,#147478,#147479,#147480),
 .UNSPECIFIED.,.F.,.F.,(4,2,2,1,1,1,2,2,2,2,2,2,1,1,1,2,2,4),(0.,0.125000000000004,
0.187500000000005,0.218750000000006,0.234375000000007,0.242187500000007,
0.246093750000007,0.250000000000007,0.375000000000004,0.500000000000002,
0.624999999999999,0.687499999999998,0.718749999999998,0.734374999999997,
0.742187499999997,0.746093749999997,0.749999999999997,1.),.UNSPECIFIED.);
#29933=B_SPLINE_CURVE_WITH_KNOTS('',3,(#147481,#147482,#147483,#147484),
 .UNSPECIFIED.,.F.,.F.,(4,4),(0.,1.),.UNSPECIFIED.);
#29934=B_SPLINE_CURVE_WITH_KNOTS('',3,(#147578,#147579,#147580,#147581,
#147582,#147583,#147584,#147585,#147586,#147587,#147588,#147589,#147590,
#147591,#147592,#147593,#147594,#147595,#147596,#147597,#147598,#147599,
#147600,#147601,#147602,#147603,#147604,#147605,#147606,#147607,#147608,
#147609),.UNSPECIFIED.,.F.,.F.,(4,2,2,2,2,1,2,2,2,2,2,1,2,2,2,2,4),(0.,
0.0624999999999979,0.124999999999996,0.156249999999995,0.187499999999995,
0.218749999999994,0.234374999999994,0.249999999999994,0.374999999999995,
0.437499999999995,0.499999999999996,0.562499999999996,0.593749999999996,
0.624999999999997,0.687499999999997,0.749999999999998,1.),.UNSPECIFIED.);
#29935=B_SPLINE_CURVE_WITH_KNOTS('',3,(#147612,#147613,#147614,#147615,
#147616,#147617,#147618,#147619,#147620,#147621,#147622,#147623,#147624,
#147625,#147626,#147627,#147628,#147629,#147630,#147631,#147632,#147633,
#147634,#147635,#147636,#147637,#147638,#147639,#147640,#147641,#147642,
#147643,#147644,#147645,#147646,#147647,#147648,#147649,#147650,#147651,
#147652,#147653,#147654,#147655,#147656,#147657,#147658,#147659,#147660,
#147661,#147662,#147663,#147664,#147665,#147666,#147667,#147668,#147669,
#147670,#147671,#147672,#147673,#147674,#147675,#147676,#147677,#147678,
#147679,#147680,#147681,#147682,#147683,#147684,#147685,#147686,#147687,
#147688,#147689,#147690,#147691,#147692,#147693,#147694,#147695,#147696,
#147697,#147698,#147699,#147700,#147701,#147702),.UNSPECIFIED.,.F.,.F.,
(4,3,3,3,3,3,3,3,3,3,3,3,3,3,3,3,3,3,3,3,3,3,3,3,3,3,3,3,3,3,4),(1.67456784270334E-10,
0.0427557053620654,0.0840496960542369,0.125,0.16402161588874,0.202518234123198,
0.240354961866521,0.25,0.284884473303822,0.319542661327307,0.353941760428521,
0.375,0.407307079188093,0.439535083171299,0.471710072620308,0.5,0.532177878059925,
0.564377035663142,0.596685525002144,0.625,0.659425247468669,0.694006863967103,
0.728915833082306,0.75,0.787960510615582,0.826376766939918,0.865520707439689,
0.875,0.916019294839705,0.958474750871701,1.),.UNSPECIFIED.);
#29936=B_SPLINE_CURVE_WITH_KNOTS('',3,(#147703,#147704,#147705,#147706),
 .UNSPECIFIED.,.F.,.F.,(4,4),(2.04876468490802E-12,0.999998797216457),
 .UNSPECIFIED.);
#29937=B_SPLINE_CURVE_WITH_KNOTS('',3,(#147708,#147709,#147710,#147711),
 .UNSPECIFIED.,.F.,.F.,(4,4),(1.1801908511746E-6,1.),.UNSPECIFIED.);
#29938=B_SPLINE_CURVE_WITH_KNOTS('',3,(#147716,#147717,#147718,#147719,
#147720),.UNSPECIFIED.,.F.,.F.,(4,1,4),(0.000586994153978791,0.5,0.999443784375688),
 .UNSPECIFIED.);
#29939=B_SPLINE_CURVE_WITH_KNOTS('',3,(#147784,#147785,#147786,#147787,
#147788,#147789),.UNSPECIFIED.,.F.,.F.,(4,2,4),(1.44830354259436E-6,0.148225594517564,
0.296892255518428),.UNSPECIFIED.);
#29940=B_SPLINE_CURVE_WITH_KNOTS('',3,(#147790,#147791,#147792,#147793,
#147794,#147795,#147796,#147797,#147798,#147799,#147800,#147801,#147802,
#147803,#147804,#147805,#147806,#147807,#147808,#147809,#147810,#147811,
#147812,#147813,#147814,#147815,#147816,#147817),.UNSPECIFIED.,.F.,.F.,
(4,3,3,3,3,3,3,3,3,4),(0.,0.125349741004805,0.249758349526999,0.3748791747635,
0.5,0.625,0.74576818111402,0.866052850311141,0.985817153946618,1.),
 .UNSPECIFIED.);
#29941=B_SPLINE_CURVE_WITH_KNOTS('',3,(#147818,#147819,#147820,#147821,
#147822,#147823,#147824,#147825,#147826,#147827,#147828,#147829,#147830,
#147831,#147832,#147833,#147834),.UNSPECIFIED.,.F.,.F.,(4,2,2,1,1,1,2,2,
2,4),(0.,0.124999999999656,0.187499999999483,0.218749999999393,0.234374999999343,
0.242187499999318,0.24804687499931,0.24999999999931,0.49999999999954,1.),
 .UNSPECIFIED.);
#29942=B_SPLINE_CURVE_WITH_KNOTS('',3,(#147963,#147964,#147965,#147966,
#147967,#147968,#147969,#147970,#147971,#147972,#147973,#147974,#147975,
#147976),.UNSPECIFIED.,.F.,.F.,(4,2,2,2,2,2,4),(1.00000010829612E-6,0.0551684498922181,
0.111833996135768,0.16861384802555,0.226550710039574,0.281514160236136,
0.337551625530067),.UNSPECIFIED.);
#29943=B_SPLINE_CURVE_WITH_KNOTS('',3,(#147993,#147994,#147995,#147996,
#147997,#147998),.UNSPECIFIED.,.F.,.F.,(4,2,4),(4.92574313644089E-5,0.0292970799088927,
0.0585464725933476),.UNSPECIFIED.);
#29944=B_SPLINE_CURVE_WITH_KNOTS('',3,(#148081,#148082,#148083,#148084,
#148085,#148086,#148087,#148088,#148089,#148090,#148091,#148092,#148093,
#148094,#148095,#148096,#148097,#148098,#148099,#148100,#148101,#148102,
#148103,#148104,#148105,#148106,#148107,#148108,#148109,#148110,#148111,
#148112,#148113,#148114,#148115,#148116,#148117,#148118,#148119,#148120,
#148121,#148122,#148123,#148124,#148125,#148126,#148127,#148128,#148129,
#148130,#148131,#148132,#148133,#148134,#148135,#148136,#148137,#148138,
#148139,#148140,#148141,#148142,#148143,#148144,#148145,#148146,#148147,
#148148,#148149,#148150,#148151,#148152,#148153,#148154,#148155,#148156,
#148157,#148158,#148159,#148160,#148161,#148162,#148163,#148164,#148165,
#148166,#148167,#148168,#148169,#148170,#148171,#148172,#148173,#148174,
#148175,#148176,#148177,#148178,#148179,#148180,#148181,#148182,#148183,
#148184,#148185,#148186,#148187,#148188,#148189,#148190,#148191,#148192,
#148193,#148194,#148195,#148196,#148197,#148198,#148199,#148200,#148201,
#148202,#148203,#148204,#148205,#148206,#148207),.UNSPECIFIED.,.F.,.F.,
(4,3,3,3,3,3,3,3,3,3,3,3,3,3,3,3,3,3,3,3,3,3,3,3,3,3,3,3,3,3,3,3,3,3,3,
3,3,3,3,3,3,3,4),(0.,0.0395378850437958,0.0780200915431913,0.114432547161542,
0.125000000000007,0.159102920826881,0.191386870635889,0.201074434816447,
0.238265273042362,0.272243296330936,0.304871992254801,0.335705256204608,
0.365685268499672,0.400362784779306,0.434556392389667,0.466745053874986,
0.468750000000028,0.484375000000029,0.49218750000003,0.49609375000003,0.49804687500003,
0.499023437500029,0.500000000000029,0.507883393611758,0.532289603728898,
0.557189218947549,0.582919841466742,0.609182080991284,0.636315979770474,
0.6470686088343,0.678028335052706,0.710032700462084,0.718749999999933,0.734374999999928,
0.742187499999925,0.746093749999923,0.748046874999921,0.74999999999992,
0.803643684670449,0.849622242689776,0.910065827990631,0.968705713846152,
0.999999772449722),.UNSPECIFIED.);
#29945=B_SPLINE_CURVE_WITH_KNOTS('',3,(#148254,#148255,#148256,#148257,
#148258,#148259,#148260,#148261,#148262,#148263,#148264,#148265,#148266,
#148267,#148268,#148269,#148270,#148271,#148272,#148273,#148274,#148275,
#148276,#148277,#148278,#148279,#148280,#148281,#148282,#148283,#148284,
#148285,#148286,#148287,#148288,#148289,#148290,#148291,#148292,#148293,
#148294,#148295,#148296,#148297,#148298,#148299,#148300,#148301,#148302,
#148303,#148304,#148305,#148306,#148307,#148308,#148309,#148310,#148311,
#148312,#148313,#148314,#148315,#148316,#148317,#148318,#148319,#148320,
#148321,#148322,#148323,#148324,#148325,#148326,#148327,#148328,#148329,
#148330,#148331,#148332),.UNSPECIFIED.,.F.,.F.,(4,3,3,3,3,3,3,3,3,3,3,3,
3,3,3,3,3,3,3,3,3,3,3,3,3,3,4),(0.,0.0474320767126572,0.0946326886006528,
0.140923092999167,0.162439384980431,0.1666666666667,0.210993419848256,0.254956231845612,
0.298464378985549,0.3333333333333,0.337383184424287,0.387642864546409,0.436820715093529,
0.484559346746784,0.5,0.512349724231562,0.564394734908946,0.615530700787823,
0.6666666666667,0.687332440500564,0.74511395135353,0.800305157394242,0.8333333333333,
0.862289173200801,0.921296729034223,0.978711644555806,1.),.UNSPECIFIED.);
#29946=B_SPLINE_CURVE_WITH_KNOTS('',3,(#148333,#148334,#148335,#148336,
#148337,#148338,#148339,#148340,#148341,#148342,#148343,#148344,#148345,
#148346,#148347,#148348,#148349,#148350,#148351,#148352,#148353,#148354,
#148355,#148356,#148357,#148358,#148359,#148360,#148361,#148362,#148363,
#148364,#148365,#148366,#148367,#148368,#148369,#148370,#148371,#148372,
#148373,#148374,#148375,#148376,#148377,#148378,#148379,#148380,#148381,
#148382,#148383,#148384,#148385,#148386,#148387,#148388,#148389,#148390,
#148391,#148392,#148393,#148394,#148395,#148396,#148397,#148398,#148399,
#148400,#148401,#148402,#148403,#148404,#148405,#148406,#148407,#148408,
#148409,#148410,#148411,#148412,#148413,#148414,#148415,#148416,#148417),
 .UNSPECIFIED.,.F.,.F.,(4,3,3,3,3,3,3,3,3,3,3,3,3,3,3,3,3,3,3,3,3,3,3,3,
3,3,3,3,4),(0.,0.0455858941264268,0.0900676722499013,0.133106253218741,
0.175403108755941,0.216708992426193,0.250000000000003,0.290162447841863,
0.329903895741327,0.369192000698554,0.375000000000003,0.413876900465313,
0.452580956666026,0.491171017134247,0.500000000000004,0.538625685578037,
0.577322592156103,0.616249147781696,0.625000000000004,0.66442046172197,
0.704160089651944,0.744467769580063,0.750000000000004,0.791224950398625,
0.833139877316173,0.876352631852926,0.920342081968076,0.965764533040775,
1.),.UNSPECIFIED.);
#29947=B_SPLINE_CURVE_WITH_KNOTS('',3,(#148451,#148452,#148453,#148454,
#148455),.UNSPECIFIED.,.F.,.F.,(4,1,4),(0.,0.5,1.),.UNSPECIFIED.);
#29948=B_SPLINE_CURVE_WITH_KNOTS('',3,(#148489,#148490,#148491,#148492,
#148493,#148494,#148495,#148496,#148497,#148498),.UNSPECIFIED.,.F.,.F.,
(4,2,2,2,4),(-2.05526489217093,-1.54831938115258,-1.00799606378119,-0.491432960923045,
-0.000105186411817316),.UNSPECIFIED.);
#29949=B_SPLINE_CURVE_WITH_KNOTS('',3,(#148502,#148503,#148504,#148505),
 .UNSPECIFIED.,.F.,.F.,(4,4),(0.,0.999999598452425),.UNSPECIFIED.);
#29950=B_SPLINE_CURVE_WITH_KNOTS('',3,(#148507,#148508,#148509,#148510,
#148511,#148512,#148513,#148514,#148515,#148516,#148517,#148518,#148519,
#148520,#148521,#148522,#148523,#148524,#148525,#148526,#148527,#148528,
#148529,#148530,#148531,#148532,#148533,#148534,#148535,#148536,#148537),
 .UNSPECIFIED.,.F.,.F.,(4,3,3,3,3,3,3,3,3,3,4),(0.,0.124999894110832,0.24999992934917,
0.374999964587508,0.437499982206676,0.499999999825845,0.562500017445014,
0.625000035064183,0.750000070302521,0.875000105540858,1.),.UNSPECIFIED.);
#29951=B_SPLINE_CURVE_WITH_KNOTS('',3,(#148538,#148539,#148540,#148541),
 .UNSPECIFIED.,.F.,.F.,(4,4),(4.05016088455375E-7,1.),.UNSPECIFIED.);
#29952=B_SPLINE_CURVE_WITH_KNOTS('',3,(#148561,#148562,#148563,#148564),
 .UNSPECIFIED.,.F.,.F.,(4,4),(0.,1.),.UNSPECIFIED.);
#29953=B_SPLINE_CURVE_WITH_KNOTS('',3,(#148583,#148584,#148585,#148586,
#148587,#148588,#148589,#148590,#148591,#148592,#148593,#148594,#148595,
#148596,#148597,#148598,#148599,#148600,#148601,#148602,#148603,#148604,
#148605,#148606,#148607,#148608,#148609,#148610,#148611,#148612,#148613,
#148614,#148615,#148616,#148617,#148618,#148619,#148620,#148621,#148622,
#148623,#148624,#148625,#148626,#148627,#148628,#148629,#148630,#148631,
#148632,#148633,#148634,#148635,#148636,#148637,#148638,#148639,#148640,
#148641,#148642,#148643),.UNSPECIFIED.,.F.,.F.,(4,3,3,3,3,3,3,3,3,3,3,3,
3,3,3,3,3,3,3,3,4),(0.,0.190770165214888,0.250000000000013,0.375000000000016,
0.437500000000018,0.468750000000019,0.484375000000019,0.492187500000019,
0.500000000000019,0.569018803380385,0.636641230509603,0.702130813965924,
0.750000000000097,0.781250000000105,0.785156250000104,0.789062500000103,
0.7968750000001,0.812500000000088,0.875000000000057,0.976209630883769,1.),
 .UNSPECIFIED.);
#29954=B_SPLINE_CURVE_WITH_KNOTS('',3,(#148645,#148646,#148647,#148648,
#148649,#148650,#148651,#148652,#148653,#148654,#148655,#148656,#148657,
#148658,#148659,#148660,#148661,#148662,#148663,#148664,#148665,#148666),
 .UNSPECIFIED.,.F.,.F.,(4,3,3,3,3,3,3,4),(0.,0.187499999999997,0.374999999999994,
0.465346374523407,0.499999999999993,0.702063552429337,0.902036509644966,
1.),.UNSPECIFIED.);
#29955=B_SPLINE_CURVE_WITH_KNOTS('',3,(#148731,#148732,#148733,#148734,
#148735,#148736,#148737,#148738,#148739,#148740,#148741,#148742,#148743,
#148744,#148745,#148746,#148747,#148748,#148749,#148750,#148751,#148752,
#148753,#148754,#148755,#148756,#148757,#148758,#148759,#148760,#148761,
#148762,#148763,#148764),.UNSPECIFIED.,.F.,.F.,(4,2,2,1,1,1,2,2,2,2,2,2,
2,2,1,1,1,2,2,4),(0.,0.125000000000082,0.187500000000122,0.218750000000142,
0.234375000000152,0.242187500000155,0.246093750000156,0.250000000000157,
0.375000000000151,0.437500000000148,0.468750000000146,0.500000000000143,
0.625000000000127,0.687500000000118,0.718750000000113,0.734375000000109,
0.742187500000108,0.746093750000107,0.750000000000105,1.),.UNSPECIFIED.);
#29956=B_SPLINE_CURVE_WITH_KNOTS('',3,(#148767,#148768,#148769,#148770,
#148771,#148772,#148773,#148774,#148775,#148776,#148777,#148778,#148779,
#148780,#148781,#148782,#148783,#148784,#148785,#148786,#148787,#148788,
#148789,#148790,#148791,#148792,#148793,#148794,#148795,#148796,#148797,
#148798,#148799,#148800,#148801,#148802,#148803,#148804,#148805,#148806,
#148807,#148808,#148809,#148810,#148811,#148812,#148813,#148814,#148815,
#148816,#148817,#148818,#148819,#148820,#148821,#148822,#148823,#148824,
#148825,#148826,#148827,#148828,#148829,#148830,#148831,#148832,#148833,
#148834,#148835,#148836,#148837,#148838,#148839,#148840,#148841,#148842,
#148843,#148844,#148845,#148846,#148847,#148848,#148849,#148850,#148851,
#148852,#148853,#148854,#148855,#148856,#148857,#148858,#148859,#148860,
#148861,#148862,#148863,#148864,#148865,#148866,#148867,#148868,#148869,
#148870,#148871,#148872,#148873,#148874,#148875,#148876,#148877,#148878,
#148879,#148880,#148881,#148882,#148883,#148884,#148885,#148886,#148887,
#148888,#148889,#148890,#148891,#148892,#148893,#148894,#148895,#148896,
#148897,#148898,#148899,#148900,#148901,#148902,#148903,#148904,#148905,
#148906,#148907,#148908,#148909,#148910,#148911,#148912,#148913,#148914,
#148915,#148916,#148917,#148918,#148919,#148920,#148921,#148922,#148923,
#148924,#148925,#148926,#148927,#148928,#148929,#148930,#148931,#148932,
#148933,#148934,#148935,#148936,#148937,#148938,#148939,#148940,#148941,
#148942,#148943,#148944,#148945,#148946,#148947,#148948,#148949,#148950,
#148951,#148952,#148953,#148954,#148955,#148956),.UNSPECIFIED.,.F.,.F.,
(4,3,3,3,3,3,3,3,3,3,3,3,3,3,3,3,3,3,3,3,3,3,3,3,3,3,3,3,3,3,3,3,3,3,3,
3,3,3,3,3,3,3,3,3,3,3,3,3,3,3,3,3,3,3,3,3,3,3,3,3,3,3,3,4),(0.,0.0325663096439314,
0.0652395420398298,0.0979584965072984,0.125000000002429,0.140625000002734,
0.142578125002771,0.144377797393464,0.144531250002809,0.148437500002884,
0.156250000003032,0.187500000003627,0.229178571732012,0.250000000004818,
0.281250000005412,0.285156250005487,0.285644531255495,0.286132812505503,
0.287109375005499,0.289062500005488,0.296875000005429,0.312500000005324,
0.336074545739341,0.359628477884607,0.375000000004924,0.398483031248456,
0.421881190788266,0.437500000004523,0.460689275415805,0.468750000004323,
0.484375000004223,0.492187500004174,0.496093750004149,0.498046875004136,
0.500000000004123,0.553525721980606,0.60702301589617,0.625000000003431,
0.677521774987248,0.687500000003084,0.71875000000291,0.734375000002825,
0.742187500002782,0.749511718752743,0.75000000000274,0.765625000002564,
0.780744058039143,0.796622029020588,0.812500000002033,0.828125000001857,
0.843750000001681,0.858514060594805,0.859375000001504,0.867187500001415,
0.87109375000137,0.873046875001348,0.874023437501338,0.875000000001327,
0.897607080137333,0.920471072316808,0.937500000000664,0.960507524861031,
0.983627731936416,1.),.UNSPECIFIED.);
#29957=B_SPLINE_CURVE_WITH_KNOTS('',3,(#148958,#148959,#148960,#148961,
#148962,#148963,#148964,#148965,#148966,#148967,#148968,#148969,#148970,
#148971,#148972,#148973,#148974,#148975,#148976,#148977,#148978,#148979,
#148980,#148981,#148982,#148983,#148984,#148985,#148986,#148987,#148988,
#148989,#148990,#148991,#148992,#148993,#148994),.UNSPECIFIED.,.F.,.F.,
(4,3,3,3,3,3,3,3,3,3,3,3,4),(0.,0.0930590071063409,0.185651390275755,0.277313404654321,
0.368302886143633,0.45813055065145,0.5,0.588081733577098,0.674994332807131,
0.760020789035996,0.843967295660058,0.926160665559156,1.),.UNSPECIFIED.);
#29958=B_SPLINE_CURVE_WITH_KNOTS('',3,(#149136,#149137,#149138,#149139,
#149140,#149141,#149142,#149143,#149144,#149145,#149146,#149147,#149148,
#149149,#149150,#149151,#149152,#149153,#149154,#149155,#149156,#149157,
#149158,#149159,#149160,#149161,#149162,#149163,#149164,#149165,#149166,
#149167,#149168,#149169,#149170,#149171,#149172,#149173,#149174,#149175,
#149176,#149177,#149178,#149179,#149180,#149181,#149182,#149183,#149184,
#149185,#149186,#149187,#149188,#149189,#149190,#149191,#149192,#149193,
#149194,#149195,#149196,#149197,#149198,#149199,#149200,#149201,#149202,
#149203,#149204,#149205),.UNSPECIFIED.,.F.,.F.,(4,3,3,3,3,3,3,3,3,3,3,3,
3,3,3,3,3,3,3,3,3,3,3,4),(0.,0.0530696375713618,0.10597175525186,0.125000000000207,
0.184073079506744,0.242252390671621,0.250000000000417,0.300353856516711,
0.351927538736091,0.375000000000626,0.427736269402923,0.437500000000733,
0.468750000000782,0.484375000000809,0.492187500000819,0.496093750000821,
0.498046875000821,0.50000000000082,0.585242731062141,0.672617291309937,
0.763561346558681,0.856698761090278,0.953299858538298,1.),.UNSPECIFIED.);
#29959=B_SPLINE_CURVE_WITH_KNOTS('',3,(#149208,#149209,#149210,#149211,
#149212,#149213,#149214,#149215,#149216,#149217,#149218,#149219,#149220,
#149221,#149222,#149223,#149224,#149225,#149226,#149227,#149228,#149229,
#149230,#149231,#149232,#149233,#149234,#149235,#149236,#149237,#149238,
#149239,#149240,#149241,#149242,#149243,#149244,#149245,#149246,#149247,
#149248,#149249,#149250,#149251,#149252,#149253,#149254,#149255,#149256,
#149257,#149258,#149259,#149260,#149261,#149262,#149263,#149264,#149265,
#149266,#149267,#149268,#149269,#149270,#149271),.UNSPECIFIED.,.F.,.F.,
(4,3,3,3,3,3,3,3,3,3,3,3,3,3,3,3,3,3,3,3,3,4),(0.,0.101946695149731,0.202232035950964,
0.2500000000002,0.348102987925477,0.375000000000297,0.437500000000346,0.468750000000372,
0.484375000000385,0.49218750000039,0.498046875000392,0.500000000000393,
0.553018142384203,0.605910416481641,0.625000000000295,0.690733261304678,
0.750000000000197,0.802837365431866,0.856075997664884,0.909470261574667,
0.963029692389013,0.999997713195439),.UNSPECIFIED.);
#29960=B_SPLINE_CURVE_WITH_KNOTS('',3,(#149272,#149273,#149274,#149275,
#149276,#149277,#149278,#149279,#149280,#149281,#149282,#149283,#149284,
#149285,#149286,#149287,#149288,#149289,#149290,#149291,#149292,#149293,
#149294,#149295,#149296,#149297,#149298,#149299,#149300,#149301,#149302,
#149303,#149304,#149305,#149306,#149307,#149308,#149309,#149310,#149311,
#149312,#149313,#149314,#149315,#149316,#149317,#149318,#149319,#149320,
#149321,#149322,#149323,#149324,#149325,#149326,#149327,#149328,#149329,
#149330,#149331,#149332,#149333,#149334,#149335,#149336,#149337,#149338,
#149339,#149340,#149341,#149342,#149343,#149344,#149345,#149346,#149347,
#149348,#149349,#149350,#149351,#149352,#149353,#149354,#149355,#149356,
#149357,#149358,#149359,#149360,#149361,#149362,#149363,#149364,#149365,
#149366,#149367,#149368,#149369,#149370,#149371,#149372,#149373,#149374,
#149375,#149376,#149377,#149378,#149379,#149380,#149381,#149382,#149383,
#149384,#149385,#149386,#149387,#149388,#149389,#149390,#149391,#149392,
#149393,#149394,#149395,#149396,#149397,#149398,#149399,#149400,#149401,
#149402,#149403,#149404,#149405,#149406,#149407,#149408,#149409,#149410,
#149411,#149412,#149413,#149414,#149415,#149416,#149417,#149418,#149419,
#149420,#149421,#149422,#149423,#149424,#149425,#149426,#149427,#149428,
#149429,#149430,#149431,#149432,#149433,#149434,#149435,#149436,#149437,
#149438,#149439,#149440,#149441,#149442,#149443,#149444,#149445,#149446,
#149447,#149448,#149449,#149450,#149451,#149452,#149453,#149454,#149455,
#149456,#149457,#149458,#149459,#149460,#149461,#149462,#149463,#149464),
 .UNSPECIFIED.,.F.,.F.,(4,3,3,3,3,3,3,3,3,3,3,3,3,3,3,3,3,3,3,3,3,3,3,3,
3,3,3,3,3,3,3,3,3,3,3,3,3,3,3,3,3,3,3,3,3,3,3,3,3,3,3,3,3,3,3,3,3,3,3,3,
3,3,3,3,4),(0.,0.0824357364239239,0.119148634600739,0.125000000000686,0.18750000000103,
0.218750000001204,0.23437500000129,0.238310205703374,0.242187500001333,
0.246093750001353,0.248046875001364,0.249511718751369,0.250000000001371,
0.275393681203308,0.301516346052999,0.325694808248701,0.349380831708483,
0.372569384114915,0.395265609773867,0.417542957330609,0.439097282978513,
0.460279537636208,0.480970724120933,0.484375000000832,0.492187500000815,
0.496093750000807,0.498046875000803,0.498929468592768,0.499023437500802,
0.4995117187508,0.4997558593758,0.5000000000008,0.594238858917815,0.625000000000623,
0.687500000000534,0.695312500000524,0.699218750000517,0.701653256210494,
0.703125000000509,0.726683948334691,0.797244553002977,0.842069531868659,
0.843750000000286,0.848842741425888,0.851562500000274,0.865178344060018,
0.879352508045055,0.892721009198138,0.905807159823004,0.918394647074556,
0.921875000000165,0.923828125000163,0.92480468750016,0.925710282043078,
0.925781250000158,0.92968750000015,0.937500000000134,0.946187537931024,
0.95508063298552,0.964250861347624,0.968750000000067,0.97819414757121,0.987711388661645,
0.997278309415761,1.),.UNSPECIFIED.);
#29961=B_SPLINE_CURVE_WITH_KNOTS('',3,(#149529,#149530,#149531,#149532,
#149533,#149534,#149535,#149536,#149537,#149538,#149539,#149540,#149541,
#149542,#149543,#149544,#149545,#149546,#149547,#149548,#149549,#149550,
#149551,#149552,#149553,#149554,#149555,#149556,#149557,#149558,#149559,
#149560,#149561,#149562),.UNSPECIFIED.,.F.,.F.,(4,2,2,1,1,1,2,2,2,2,2,2,
2,2,1,1,1,2,2,4),(0.,0.125000000000023,0.187500000000035,0.218750000000042,
0.234375000000045,0.242187500000047,0.246093750000046,0.250000000000046,
0.375000000000051,0.437500000000054,0.468750000000056,0.500000000000057,
0.625000000000062,0.687500000000065,0.718750000000066,0.734375000000066,
0.742187500000066,0.746093750000067,0.750000000000067,1.),.UNSPECIFIED.);
#29962=B_SPLINE_CURVE_WITH_KNOTS('',3,(#149581,#149582,#149583,#149584,
#149585,#149586,#149587,#149588,#149589,#149590,#149591,#149592,#149593,
#149594,#149595,#149596,#149597,#149598,#149599,#149600,#149601,#149602,
#149603,#149604,#149605),.UNSPECIFIED.,.F.,.F.,(4,3,3,3,3,3,3,3,4),(0.,
0.195180283024368,0.250000000000003,0.375000000000002,0.4375,0.499999999999999,
0.682692802577324,0.866396269045124,1.),.UNSPECIFIED.);
#29963=B_SPLINE_CURVE_WITH_KNOTS('',3,(#149624,#149625,#149626,#149627,
#149628,#149629,#149630,#149631,#149632,#149633),.UNSPECIFIED.,.F.,.F.,
(4,3,3,4),(0.,0.464229907836084,0.91726039913087,1.),.UNSPECIFIED.);
#29964=B_SPLINE_CURVE_WITH_KNOTS('',3,(#149727,#149728,#149729,#149730,
#149731,#149732,#149733,#149734,#149735,#149736,#149737,#149738,#149739,
#149740,#149741,#149742,#149743,#149744,#149745,#149746,#149747,#149748,
#149749,#149750,#149751,#149752,#149753,#149754,#149755,#149756,#149757,
#149758,#149759,#149760,#149761,#149762,#149763,#149764,#149765,#149766,
#149767,#149768,#149769),.UNSPECIFIED.,.F.,.F.,(4,3,3,3,3,3,3,3,3,3,3,3,
3,3,4),(0.,0.105418333178882,0.210324340120241,0.313988331761175,0.375000000000047,
0.437500000000058,0.468750000000063,0.484375000000066,0.492187500000065,
0.500000000000064,0.625000000000048,0.742475783864713,0.856307677060081,
0.965238555229571,1.),.UNSPECIFIED.);
#29965=B_SPLINE_CURVE_WITH_KNOTS('',3,(#149770,#149771,#149772,#149773,
#149774,#149775,#149776,#149777,#149778,#149779,#149780,#149781,#149782,
#149783,#149784,#149785,#149786,#149787,#149788,#149789,#149790,#149791,
#149792,#149793,#149794,#149795,#149796,#149797,#149798,#149799,#149800,
#149801,#149802,#149803,#149804,#149805,#149806,#149807,#149808,#149809,
#149810,#149811,#149812,#149813,#149814,#149815),.UNSPECIFIED.,.F.,.F.,
(4,3,3,3,3,3,3,3,3,3,3,3,3,3,3,4),(0.,0.108316449197884,0.221360934376212,
0.250000000000046,0.368521273790907,0.375000000000071,0.437500000000084,
0.46875000000009,0.484375000000091,0.492187500000092,0.500000000000092,
0.601086242546387,0.704740924634103,0.809297948134376,0.914777359348703,
1.),.UNSPECIFIED.);
#29966=B_SPLINE_CURVE_WITH_KNOTS('',3,(#149830,#149831,#149832,#149833,
#149834,#149835,#149836,#149837,#149838,#149839,#149840,#149841,#149842,
#149843,#149844,#149845,#149846,#149847,#149848,#149849,#149850,#149851,
#149852,#149853,#149854,#149855,#149856,#149857,#149858,#149859,#149860,
#149861,#149862,#149863),.UNSPECIFIED.,.F.,.F.,(4,2,2,1,1,1,2,2,2,2,2,2,
2,2,1,1,1,2,2,4),(0.,0.124999999999981,0.187499999999971,0.218749999999967,
0.234374999999966,0.242187499999966,0.246093749999967,0.249999999999967,
0.374999999999974,0.437499999999977,0.468749999999979,0.499999999999981,
0.624999999999986,0.687499999999989,0.71874999999999,0.734374999999991,
0.742187499999992,0.746093749999993,0.749999999999994,1.),.UNSPECIFIED.);
#29967=B_SPLINE_CURVE_WITH_KNOTS('',3,(#149869,#149870,#149871,#149872,
#149873,#149874,#149875,#149876,#149877,#149878,#149879,#149880,#149881,
#149882,#149883,#149884,#149885,#149886,#149887,#149888,#149889,#149890,
#149891,#149892,#149893,#149894,#149895,#149896,#149897,#149898,#149899,
#149900,#149901,#149902,#149903,#149904,#149905,#149906,#149907,#149908,
#149909,#149910,#149911,#149912,#149913,#149914,#149915,#149916,#149917,
#149918,#149919,#149920,#149921,#149922,#149923,#149924,#149925,#149926,
#149927,#149928,#149929,#149930,#149931,#149932,#149933,#149934,#149935,
#149936,#149937,#149938,#149939,#149940,#149941,#149942,#149943,#149944,
#149945,#149946,#149947,#149948,#149949,#149950,#149951,#149952),
 .UNSPECIFIED.,.F.,.F.,(4,2,2,2,1,1,1,2,2,2,2,1,1,2,2,2,2,2,1,1,1,2,2,2,
2,2,2,2,1,1,1,1,2,2,2,2,2,1,2,2,2,2,2,1,1,1,2,2,2,4),(0.,0.0624999999999929,
0.0937499999999894,0.109374999999988,0.117187499999987,0.121093749999986,
0.123046874999986,0.124023437499986,0.124999999999986,0.187499999999978,
0.218749999999974,0.234374999999972,0.242187499999971,0.24609374999997,
0.24999999999997,0.312499999999963,0.34374999999996,0.359374999999958,0.367187499999957,
0.371093749999957,0.373046874999956,0.374511718749956,0.374999999999956,
0.43749999999996,0.499999999999964,0.562499999999968,0.59374999999997,0.609374999999971,
0.617187499999972,0.621093749999972,0.623046874999972,0.624023437499972,
0.624511718749972,0.624999999999972,0.687499999999977,0.718749999999979,
0.734374999999981,0.742187499999981,0.746093749999982,0.749999999999982,
0.812499999999987,0.84374999999999,0.859374999999991,0.867187499999992,
0.871093749999992,0.873046874999992,0.874023437499992,0.874999999999992,
0.937499999999996,1.),.UNSPECIFIED.);
#29968=B_SPLINE_CURVE_WITH_KNOTS('',3,(#149961,#149962,#149963,#149964,
#149965,#149966,#149967,#149968,#149969,#149970),.UNSPECIFIED.,.F.,.F.,
(4,3,3,4),(0.,0.373730880508955,0.752279314625459,1.),.UNSPECIFIED.);
#29969=B_SPLINE_CURVE_WITH_KNOTS('',3,(#149971,#149972,#149973,#149974,
#149975,#149976,#149977,#149978,#149979,#149980,#149981),.UNSPECIFIED.,
 .F.,.F.,(4,2,1,2,2,4),(0.,0.249999999999999,0.375000000000002,0.437500000000004,
0.500000000000006,1.),.UNSPECIFIED.);
#29970=B_SPLINE_CURVE_WITH_KNOTS('',3,(#149986,#149987,#149988,#149989,
#149990,#149991,#149992,#149993,#149994,#149995,#149996,#149997,#149998,
#149999,#150000,#150001,#150002,#150003,#150004,#150005,#150006,#150007,
#150008,#150009,#150010,#150011,#150012,#150013,#150014,#150015,#150016,
#150017,#150018,#150019,#150020,#150021,#150022,#150023,#150024,#150025,
#150026,#150027,#150028,#150029,#150030,#150031),.UNSPECIFIED.,.F.,.F.,
(4,3,3,3,3,3,3,3,3,3,3,3,3,3,3,4),(0.,0.108316449757411,0.221360935466982,
0.25000000000009,0.368521274253321,0.375000000000133,0.437500000000155,
0.468750000000163,0.484375000000169,0.49218750000017,0.500000000000171,
0.601086242782471,0.704740925103917,0.809297948826885,0.914777360240454,
1.),.UNSPECIFIED.);
#29971=B_SPLINE_CURVE_WITH_KNOTS('',3,(#150032,#150033,#150034,#150035,
#150036,#150037,#150038,#150039,#150040,#150041,#150042,#150043,#150044,
#150045,#150046,#150047,#150048,#150049,#150050,#150051,#150052,#150053,
#150054,#150055,#150056,#150057,#150058,#150059,#150060,#150061,#150062,
#150063,#150064,#150065,#150066,#150067,#150068,#150069,#150070,#150071,
#150072,#150073,#150074),.UNSPECIFIED.,.F.,.F.,(4,3,3,3,3,3,3,3,3,3,3,3,
3,3,4),(0.,0.105418332522525,0.210324338766372,0.313988329643646,0.374999999999986,
0.437499999999983,0.468749999999982,0.484374999999981,0.492187499999981,
0.499999999999981,0.624999999999986,0.742475782470587,0.856307674220441,
0.965238550848876,1.),.UNSPECIFIED.);
#29972=B_SPLINE_CURVE_WITH_KNOTS('',3,(#150085,#150086,#150087,#150088,
#150089,#150090,#150091,#150092,#150093,#150094,#150095,#150096,#150097,
#150098,#150099,#150100,#150101,#150102,#150103,#150104,#150105,#150106),
 .UNSPECIFIED.,.F.,.F.,(4,3,3,3,3,3,3,4),(0.,0.180289307661493,0.249999999999999,
0.431141781739715,0.499999999999998,0.702895542735386,0.903670705606259,
1.),.UNSPECIFIED.);
#29973=B_SPLINE_CURVE_WITH_KNOTS('',3,(#150107,#150108,#150109,#150110),
 .UNSPECIFIED.,.F.,.F.,(4,4),(0.,1.),.UNSPECIFIED.);
#29974=B_SPLINE_CURVE_WITH_KNOTS('',3,(#150113,#150114,#150115,#150116,
#150117,#150118,#150119,#150120,#150121,#150122,#150123,#150124,#150125,
#150126,#150127,#150128,#150129,#150130,#150131,#150132,#150133,#150134,
#150135,#150136,#150137,#150138,#150139,#150140,#150141,#150142,#150143,
#150144,#150145,#150146),.UNSPECIFIED.,.F.,.F.,(4,2,2,1,1,1,2,2,2,2,2,2,
2,2,1,1,1,2,2,4),(0.,0.125000000000041,0.18750000000006,0.218750000000069,
0.234375000000073,0.242187500000074,0.246093750000074,0.250000000000075,
0.375000000000062,0.437500000000056,0.468750000000052,0.500000000000048,
0.625000000000036,0.687500000000029,0.718750000000026,0.734375000000026,
0.742187500000025,0.746093750000024,0.750000000000024,1.),.UNSPECIFIED.);
#29975=B_SPLINE_CURVE_WITH_KNOTS('',3,(#150152,#150153,#150154,#150155,
#150156,#150157,#150158,#150159,#150160,#150161,#150162,#150163,#150164,
#150165,#150166,#150167,#150168,#150169,#150170,#150171,#150172,#150173,
#150174,#150175,#150176,#150177,#150178,#150179,#150180,#150181,#150182,
#150183,#150184,#150185,#150186,#150187,#150188,#150189,#150190,#150191,
#150192,#150193,#150194,#150195,#150196,#150197,#150198,#150199,#150200),
 .UNSPECIFIED.,.F.,.F.,(4,3,3,3,3,3,3,3,3,3,3,3,3,3,3,3,4),(0.,0.109992936268947,
0.221949217369093,0.334801520989419,0.449102907007153,0.5,0.603481968790449,
0.704814151412179,0.804699849390782,0.90242602165943,0.970121880641722,
0.97576964577923,0.981411740183398,0.987055876046289,0.992706300207867,
0.998373224606916,0.999999673423569),.UNSPECIFIED.);
#29976=B_SPLINE_CURVE_WITH_KNOTS('',3,(#150204,#150205,#150206,#150207,
#150208,#150209,#150210,#150211,#150212,#150213,#150214,#150215,#150216,
#150217,#150218,#150219,#150220,#150221,#150222,#150223,#150224,#150225,
#150226,#150227,#150228,#150229,#150230,#150231,#150232,#150233,#150234,
#150235,#150236,#150237,#150238,#150239,#150240,#150241,#150242,#150243,
#150244,#150245,#150246,#150247,#150248,#150249,#150250,#150251,#150252,
#150253,#150254,#150255),.UNSPECIFIED.,.F.,.F.,(4,3,3,3,3,3,3,3,3,3,3,3,
3,3,3,3,3,4),(3.07266740300672E-8,0.00572935959947857,0.0114446916406082,
0.0171497697196053,0.0228539059676719,0.0285640551379987,0.0303446246564232,
0.119140475170575,0.20920674037596,0.301032873773031,0.393773848547507,
0.487512351689386,0.5,0.613468602015531,0.725847537169989,0.837599874204618,
0.947948107414092,1.),.UNSPECIFIED.);
#29977=B_SPLINE_CURVE_WITH_KNOTS('',3,(#150279,#150280,#150281,#150282,
#150283,#150284,#150285,#150286,#150287,#150288,#150289,#150290,#150291,
#150292,#150293,#150294,#150295,#150296,#150297,#150298,#150299,#150300,
#150301,#150302,#150303,#150304,#150305,#150306,#150307,#150308,#150309,
#150310,#150311,#150312,#150313,#150314,#150315,#150316,#150317,#150318,
#150319,#150320,#150321,#150322,#150323,#150324,#150325,#150326,#150327,
#150328,#150329,#150330,#150331,#150332,#150333,#150334,#150335,#150336,
#150337,#150338,#150339,#150340,#150341,#150342),.UNSPECIFIED.,.F.,.F.,
(4,3,3,3,3,3,3,3,3,3,3,3,3,3,3,3,3,3,3,3,3,4),(0.,0.100687893601304,0.198167089124769,
0.250000000000073,0.3445731459175,0.375000000000112,0.43750000000013,0.46875000000014,
0.484375000000144,0.49218750000015,0.498046875000151,0.50000000000015,0.552999469608863,
0.605798665097521,0.625000000000113,0.687726037350389,0.750000000000075,
0.801899439950902,0.854740992711349,0.907950839930716,0.961508538596217,
1.),.UNSPECIFIED.);
#29978=B_SPLINE_CURVE_WITH_KNOTS('',3,(#150408,#150409,#150410,#150411,
#150412,#150413,#150414,#150415,#150416,#150417,#150418,#150419,#150420,
#150421,#150422,#150423,#150424,#150425,#150426,#150427,#150428,#150429,
#150430,#150431,#150432,#150433,#150434,#150435,#150436,#150437,#150438,
#150439,#150440,#150441,#150442,#150443,#150444,#150445,#150446,#150447,
#150448,#150449,#150450,#150451,#150452,#150453,#150454,#150455,#150456,
#150457,#150458,#150459,#150460,#150461,#150462,#150463,#150464,#150465,
#150466,#150467,#150468,#150469,#150470,#150471,#150472,#150473,#150474,
#150475,#150476,#150477,#150478,#150479,#150480,#150481,#150482,#150483,
#150484,#150485,#150486,#150487,#150488,#150489,#150490,#150491,#150492,
#150493,#150494,#150495,#150496,#150497,#150498,#150499,#150500,#150501,
#150502,#150503,#150504,#150505,#150506,#150507,#150508,#150509,#150510,
#150511,#150512,#150513,#150514,#150515,#150516,#150517,#150518,#150519,
#150520,#150521,#150522,#150523,#150524,#150525,#150526,#150527,#150528,
#150529,#150530,#150531,#150532,#150533,#150534,#150535,#150536,#150537,
#150538,#150539,#150540,#150541,#150542,#150543,#150544,#150545,#150546,
#150547,#150548,#150549,#150550,#150551,#150552,#150553,#150554,#150555,
#150556,#150557,#150558,#150559,#150560,#150561,#150562,#150563,#150564,
#150565,#150566,#150567,#150568,#150569,#150570,#150571,#150572,#150573,
#150574,#150575,#150576,#150577,#150578,#150579,#150580,#150581,#150582,
#150583,#150584,#150585,#150586,#150587,#150588,#150589,#150590,#150591,
#150592,#150593,#150594,#150595,#150596,#150597,#150598,#150599,#150600),
 .UNSPECIFIED.,.F.,.F.,(4,3,3,3,3,3,3,3,3,3,3,3,3,3,3,3,3,3,3,3,3,3,3,3,
3,3,3,3,3,3,3,3,3,3,3,3,3,3,3,3,3,3,3,3,3,3,3,3,3,3,3,3,3,3,3,3,3,3,3,3,
3,3,3,3,4),(0.,0.0824357367819663,0.119148634599032,0.124999999999361,0.187499999999041,
0.218749999998882,0.234374999998803,0.238310205699827,0.242187499998764,
0.246093749998744,0.248046874998735,0.249511718748729,0.249999999998727,
0.275393681554515,0.301516346360106,0.325694808867796,0.349380832626729,
0.372569385322311,0.39526561126473,0.417542958448358,0.439097284383825,
0.460279539328191,0.480970726129676,0.484374999999241,0.492187499999257,
0.496093749999266,0.49804687499927,0.498929468578901,0.499023437499272,
0.499511718749273,0.499755859374274,0.499999999999275,0.59423884968362,
0.624999999999407,0.687499999999472,0.695312499999481,0.699218749999488,
0.701653256213793,0.703124999999495,0.726683948276255,0.797244553124197,
0.842069531816328,0.843749999999701,0.848842741410648,0.851562499999713,
0.865178344045717,0.879352508034244,0.892721009175091,0.905807159789695,
0.918394647030647,0.921874999999826,0.923828124999829,0.924804687499831,
0.925710282042496,0.925781249999833,0.929687499999842,0.93749999999986,
0.946187537924857,0.955080632973159,0.964250861328642,0.96874999999993,
0.978194147563431,0.987711388645982,0.997278309392134,1.),.UNSPECIFIED.);
#29979=B_SPLINE_CURVE_WITH_KNOTS('',3,(#150619,#150620,#150621,#150622,
#150623,#150624,#150625,#150626,#150627,#150628,#150629,#150630,#150631,
#150632,#150633,#150634,#150635,#150636,#150637,#150638,#150639,#150640,
#150641,#150642,#150643,#150644,#150645,#150646,#150647,#150648,#150649,
#150650,#150651,#150652,#150653,#150654,#150655,#150656,#150657,#150658,
#150659,#150660,#150661,#150662,#150663,#150664,#150665,#150666,#150667,
#150668,#150669,#150670,#150671,#150672,#150673,#150674,#150675,#150676,
#150677,#150678,#150679,#150680,#150681,#150682,#150683,#150684,#150685,
#150686,#150687,#150688),.UNSPECIFIED.,.F.,.F.,(4,3,3,3,3,3,3,3,3,3,3,3,
3,3,3,3,3,3,3,3,3,3,3,4),(0.,0.0530717197273206,0.105975615459485,0.125000000000379,
0.184023522900716,0.242174112607182,0.250000000000761,0.300351902020698,
0.351923554506319,0.375000000001143,0.427734152108808,0.43750000000133,
0.468750000001425,0.484375000001472,0.492187500001492,0.496093750001495,
0.498046875001492,0.500000000001488,0.585242141687435,0.672616116979766,
0.763559607395129,0.856696459690941,0.95329701090269,1.),.UNSPECIFIED.);
#29980=B_SPLINE_CURVE_WITH_KNOTS('',3,(#150707,#150708,#150709,#150710),
 .UNSPECIFIED.,.F.,.F.,(4,4),(0.,1.),.UNSPECIFIED.);
#29981=B_SPLINE_CURVE_WITH_KNOTS('',3,(#150804,#150805,#150806,#150807,
#150808,#150809,#150810,#150811,#150812,#150813),.UNSPECIFIED.,.F.,.F.,
(4,2,2,2,4),(6.05089101874855E-5,0.409283590266413,0.822960520941385,1.23673775115811,
1.64591231877855),.UNSPECIFIED.);
#29982=B_SPLINE_CURVE_WITH_KNOTS('',3,(#150832,#150833,#150834,#150835),
 .UNSPECIFIED.,.F.,.F.,(4,4),(2.1150751113916E-14,1.),.UNSPECIFIED.);
#29983=B_SPLINE_CURVE_WITH_KNOTS('',3,(#150854,#150855,#150856,#150857,
#150858,#150859,#150860,#150861,#150862,#150863,#150864,#150865,#150866,
#150867,#150868,#150869,#150870,#150871,#150872,#150873,#150874,#150875,
#150876,#150877,#150878,#150879,#150880,#150881,#150882,#150883,#150884,
#150885,#150886,#150887,#150888,#150889,#150890),.UNSPECIFIED.,.F.,.F.,
(4,3,3,3,3,3,3,3,3,3,3,3,4),(3.61916304046134E-14,0.0930574396876964,0.185648309493891,
0.277308890382779,0.3682969898436,0.458123321944239,0.5,0.588079575907268,
0.674990027831864,0.760014342027675,0.843958727689798,0.92614995473359,
1.),.UNSPECIFIED.);
#29984=B_SPLINE_CURVE_WITH_KNOTS('',3,(#150956,#150957,#150958,#150959,
#150960,#150961,#150962,#150963,#150964,#150965,#150966,#150967,#150968,
#150969,#150970,#150971,#150972,#150973,#150974,#150975,#150976,#150977,
#150978,#150979,#150980,#150981,#150982,#150983,#150984,#150985,#150986,
#150987,#150988,#150989,#150990,#150991,#150992,#150993,#150994,#150995,
#150996,#150997,#150998,#150999,#151000,#151001,#151002,#151003,#151004,
#151005,#151006,#151007,#151008,#151009,#151010,#151011,#151012,#151013,
#151014,#151015,#151016,#151017,#151018,#151019,#151020,#151021,#151022,
#151023,#151024,#151025,#151026,#151027,#151028,#151029,#151030,#151031,
#151032,#151033,#151034,#151035,#151036,#151037,#151038,#151039,#151040,
#151041,#151042,#151043,#151044,#151045,#151046,#151047,#151048,#151049,
#151050,#151051,#151052,#151053,#151054,#151055,#151056,#151057,#151058,
#151059,#151060,#151061,#151062,#151063,#151064,#151065,#151066,#151067,
#151068,#151069,#151070,#151071,#151072,#151073,#151074,#151075,#151076,
#151077,#151078,#151079,#151080,#151081,#151082,#151083,#151084,#151085,
#151086,#151087,#151088,#151089,#151090,#151091,#151092,#151093,#151094,
#151095,#151096,#151097,#151098,#151099,#151100,#151101,#151102,#151103,
#151104,#151105,#151106,#151107,#151108,#151109,#151110,#151111,#151112,
#151113,#151114,#151115,#151116,#151117,#151118,#151119,#151120,#151121,
#151122,#151123,#151124,#151125,#151126,#151127,#151128,#151129,#151130,
#151131,#151132,#151133,#151134,#151135,#151136,#151137,#151138,#151139,
#151140,#151141,#151142,#151143,#151144,#151145),.UNSPECIFIED.,.F.,.F.,
(4,3,3,3,3,3,3,3,3,3,3,3,3,3,3,3,3,3,3,3,3,3,3,3,3,3,3,3,3,3,3,3,3,3,3,
3,3,3,3,3,3,3,3,3,3,3,3,3,3,3,3,3,3,3,3,3,3,3,3,3,3,3,3,4),(0.,0.0325663099035258,
0.0652395425604615,0.0979584972904591,0.12500000000312,0.14062500000351,
0.14257812500356,0.144377797408,0.144531250003609,0.148437500003707,0.156250000003902,
0.18750000000468,0.22917857178013,0.250000000006234,0.281250000007011,0.285156250007108,
0.285644531257119,0.28613281250713,0.287109375007128,0.289062500007128,
0.296875000007075,0.312500000006967,0.336074545596588,0.359628477597324,
0.375000000006548,0.398483031103689,0.421881190495673,0.437500000006129,
0.460689275266742,0.468750000005918,0.484375000005812,0.492187500005759,
0.496093750005733,0.49804687500572,0.500000000005706,0.553525722250135,
0.607023016338207,0.625000000004783,0.67752177447689,0.687500000004321,
0.718750000004092,0.734375000003977,0.74218750000392,0.749511718753869,
0.750000000003866,0.765625000003613,0.78074405805616,0.796622029029507,
0.812500000002854,0.828125000002601,0.843750000002347,0.858514060610061,
0.859375000002094,0.867187500001968,0.871093750001905,0.873046875001874,
0.874023437501859,0.875000000001845,0.897607080129362,0.920471072300298,
0.937500000000922,0.96050752485429,0.983627731922649,1.),.UNSPECIFIED.);
#29985=B_SPLINE_CURVE_WITH_KNOTS('',3,(#151164,#151165,#151166,#151167,
#151168,#151169,#151170,#151171,#151172,#151173,#151174,#151175,#151176,
#151177,#151178,#151179,#151180,#151181,#151182,#151183,#151184,#151185,
#151186,#151187,#151188,#151189,#151190,#151191,#151192,#151193,#151194,
#151195,#151196,#151197,#151198,#151199,#151200,#151201,#151202,#151203,
#151204,#151205,#151206,#151207,#151208,#151209,#151210,#151211,#151212,
#151213,#151214,#151215,#151216,#151217,#151218,#151219,#151220,#151221,
#151222,#151223,#151224),.UNSPECIFIED.,.F.,.F.,(4,3,3,3,3,3,3,3,3,3,3,3,
3,3,3,3,3,3,3,3,4),(0.,0.190753989572696,0.249999999999875,0.374999999999816,
0.437499999999784,0.468749999999765,0.484374999999756,0.492187499999754,
0.499999999999751,0.569019421689051,0.636642444566116,0.702132614905151,
0.749999999999842,0.78124999999985,0.785156249999851,0.789062499999853,
0.796874999999853,0.81249999999986,0.874999999999903,0.976210201063579,
1.),.UNSPECIFIED.);
#29986=B_SPLINE_CURVE_WITH_KNOTS('',3,(#151331,#151332,#151333,#151334,
#151335,#151336,#151337,#151338,#151339,#151340,#151341,#151342,#151343,
#151344,#151345),.UNSPECIFIED.,.F.,.F.,(4,1,1,1,1,1,1,1,1,1,1,1,4),(0.,
0.125000000000091,0.187500000000107,0.250000000000123,0.312500000000139,
0.375000000000156,0.437500000000172,0.500000000000188,0.562500000000204,
0.62500000000022,0.750000000000253,0.875000000000285,1.),.UNSPECIFIED.);
#29987=B_SPLINE_CURVE_WITH_KNOTS('',3,(#151368,#151369,#151370,#151371,
#151372,#151373,#151374,#151375,#151376,#151377,#151378,#151379,#151380,
#151381,#151382,#151383,#151384,#151385,#151386,#151387,#151388,#151389,
#151390,#151391,#151392,#151393,#151394,#151395,#151396,#151397,#151398,
#151399,#151400,#151401,#151402,#151403,#151404,#151405,#151406,#151407,
#151408,#151409,#151410,#151411,#151412,#151413,#151414,#151415,#151416,
#151417,#151418,#151419,#151420,#151421,#151422,#151423,#151424,#151425,
#151426,#151427,#151428,#151429,#151430,#151431,#151432,#151433,#151434,
#151435,#151436,#151437,#151438,#151439,#151440,#151441,#151442,#151443,
#151444,#151445,#151446,#151447,#151448,#151449,#151450,#151451,#151452,
#151453,#151454,#151455,#151456,#151457,#151458,#151459,#151460,#151461,
#151462,#151463,#151464,#151465,#151466,#151467),.UNSPECIFIED.,.F.,.F.,
(4,3,3,3,3,3,3,3,3,3,3,3,3,3,3,3,3,3,3,3,3,3,3,3,3,3,3,3,3,3,3,3,3,4),(0.,
0.0386486109998501,0.0777867154540601,0.117663230486258,0.157951378049023,
0.198841740487247,0.218749999999743,0.234374999999724,0.242187499999713,
0.246093749999708,0.249023437499706,0.249999999999706,0.298141994905816,
0.346774720025382,0.396229275286474,0.437499999999819,0.468749999999837,
0.484374999999846,0.492187499999852,0.496093749999854,0.498046874999855,
0.499999999999857,0.552515324753874,0.605587467781269,0.66122185083594,
0.715745966306094,0.771935483153023,0.828124999999952,0.835937499999954,
0.843749999999957,0.874999999999965,0.93110858870555,0.988008673189029,
1.),.UNSPECIFIED.);
#29988=B_SPLINE_CURVE_WITH_KNOTS('',3,(#151567,#151568,#151569,#151570,
#151571,#151572,#151573,#151574,#151575,#151576,#151577),.UNSPECIFIED.,
 .F.,.F.,(4,1,1,1,1,1,1,1,4),(0.,0.1245291089182,0.2495963790728,0.3746636492273,
0.4997309193818,0.6247981895364,0.7498654596909,0.8749327298455,1.),
 .UNSPECIFIED.);
#29989=B_SPLINE_CURVE_WITH_KNOTS('',3,(#151578,#151579,#151580,#151581,
#151582,#151583,#151584,#151585,#151586,#151587,#151588,#151589,#151590,
#151591,#151592,#151593,#151594,#151595,#151596,#151597,#151598,#151599,
#151600,#151601,#151602,#151603,#151604,#151605,#151606,#151607,#151608,
#151609,#151610,#151611,#151612,#151613,#151614,#151615,#151616,#151617,
#151618,#151619,#151620,#151621,#151622,#151623,#151624,#151625,#151626,
#151627,#151628,#151629,#151630,#151631,#151632,#151633,#151634,#151635),
 .UNSPECIFIED.,.F.,.F.,(4,3,3,3,3,3,3,3,3,3,3,3,3,3,3,3,3,3,3,4),(0.,0.115952588797155,
0.124516431282423,0.235365088827962,0.249596230510871,0.249941321206761,
0.338919844563841,0.37465645055649,0.462274221309376,0.49973067485326,0.500093646297469,
0.587781056470055,0.624805668103668,0.713861152125916,0.749865296158966,
0.750245971388176,0.861850585209343,0.874945606912365,0.991723863510178,
1.),.UNSPECIFIED.);
#29990=B_SPLINE_CURVE_WITH_KNOTS('',3,(#151703,#151704,#151705,#151706,
#151707,#151708,#151709,#151710,#151711,#151712,#151713,#151714,#151715,
#151716,#151717,#151718,#151719,#151720,#151721,#151722,#151723,#151724,
#151725,#151726,#151727,#151728,#151729,#151730,#151731,#151732,#151733,
#151734,#151735,#151736,#151737,#151738,#151739,#151740,#151741,#151742,
#151743,#151744,#151745,#151746,#151747,#151748,#151749,#151750,#151751,
#151752,#151753,#151754,#151755,#151756,#151757,#151758,#151759,#151760,
#151761,#151762,#151763,#151764,#151765,#151766,#151767,#151768,#151769,
#151770,#151771,#151772,#151773,#151774,#151775,#151776,#151777,#151778),
 .UNSPECIFIED.,.F.,.F.,(4,3,3,3,3,3,3,3,3,3,3,3,3,3,3,3,3,3,3,3,3,3,3,3,
3,4),(0.,0.0564989974727729,0.112185881107388,0.167214689987301,0.221006398970003,
0.249999999999978,0.302086836977158,0.35259446820029,0.374999999999967,
0.423333605828074,0.437499999999961,0.468749999999959,0.484374999999957,
0.492187499999956,0.49936885374005,0.499999999999955,0.551387355728607,
0.604385896613103,0.658323980269711,0.713760631639018,0.749999999999977,
0.805263132233714,0.862599288093799,0.921043602076914,0.980820544657335,
1.),.UNSPECIFIED.);
#29991=B_SPLINE_CURVE_WITH_KNOTS('',3,(#151779,#151780,#151781,#151782,
#151783,#151784,#151785,#151786,#151787,#151788,#151789,#151790,#151791,
#151792,#151793,#151794,#151795,#151796,#151797,#151798,#151799,#151800,
#151801,#151802,#151803),.UNSPECIFIED.,.F.,.F.,(4,3,3,3,3,3,3,3,4),(1.08860685774249E-9,
0.125010000617742,0.249999999999999,0.374999999999999,0.499999999999999,
0.624999999999999,0.749999999999999,0.875005695145605,1.),.UNSPECIFIED.);
#29992=B_SPLINE_CURVE_WITH_KNOTS('',3,(#151882,#151883,#151884,#151885,
#151886,#151887,#151888,#151889),.UNSPECIFIED.,.F.,.F.,(4,2,2,4),(0.,0.5,
0.75,1.),.UNSPECIFIED.);
#29993=B_SPLINE_CURVE_WITH_KNOTS('',3,(#151890,#151891,#151892,#151893,
#151894,#151895,#151896,#151897,#151898,#151899,#151900,#151901,#151902,
#151903,#151904,#151905,#151906,#151907),.UNSPECIFIED.,.F.,.F.,(4,2,1,1,
2,2,2,2,2,4),(0.,0.124999999999996,0.187499999999995,0.218749999999994,
0.234374999999993,0.249999999999993,0.374999999999995,0.437499999999996,
0.499999999999997,1.),.UNSPECIFIED.);
#29994=B_SPLINE_CURVE_WITH_KNOTS('',3,(#151908,#151909,#151910,#151911,
#151912,#151913,#151914,#151915,#151916,#151917,#151918,#151919,#151920,
#151921,#151922,#151923,#151924,#151925,#151926,#151927,#151928,#151929,
#151930,#151931,#151932),.UNSPECIFIED.,.F.,.F.,(4,3,3,3,3,3,3,3,4),(1.33819881907442E-9,
0.125001094910741,0.25,0.374998724065209,0.5,0.624998829992135,0.75,0.87499945771442,
1.),.UNSPECIFIED.);
#29995=B_SPLINE_CURVE_WITH_KNOTS('',3,(#151949,#151950,#151951,#151952),
 .UNSPECIFIED.,.F.,.F.,(4,4),(2.56540938759315E-6,0.999999991294677),
 .UNSPECIFIED.);
#29996=B_SPLINE_CURVE_WITH_KNOTS('',3,(#152184,#152185,#152186,#152187,
#152188,#152189,#152190,#152191,#152192,#152193,#152194,#152195,#152196,
#152197,#152198,#152199,#152200,#152201,#152202,#152203,#152204,#152205,
#152206,#152207,#152208,#152209,#152210,#152211,#152212,#152213,#152214,
#152215,#152216,#152217,#152218),.UNSPECIFIED.,.F.,.F.,(4,2,2,2,1,1,2,2,
2,2,2,2,2,1,1,1,2,2,2,4),(0.,0.124999999999998,0.187499999999997,0.218749999999997,
0.234374999999997,0.242187499999997,0.246093749999997,0.249999999999997,
0.374999999999998,0.437499999999998,0.499999999999999,0.625,0.6875,0.71875,
0.734375000000001,0.742187500000001,0.746093750000001,0.750000000000001,
0.875,1.),.UNSPECIFIED.);
#29997=B_SPLINE_CURVE_WITH_KNOTS('',3,(#152220,#152221,#152222,#152223,
#152224,#152225,#152226,#152227,#152228,#152229,#152230,#152231,#152232,
#152233,#152234,#152235,#152236,#152237,#152238,#152239,#152240,#152241,
#152242,#152243,#152244,#152245,#152246,#152247,#152248,#152249,#152250,
#152251,#152252,#152253,#152254,#152255,#152256,#152257,#152258,#152259,
#152260,#152261,#152262,#152263,#152264,#152265,#152266,#152267,#152268,
#152269,#152270,#152271,#152272,#152273,#152274,#152275,#152276,#152277,
#152278,#152279,#152280,#152281,#152282,#152283,#152284,#152285,#152286,
#152287,#152288,#152289,#152290,#152291,#152292,#152293,#152294,#152295,
#152296,#152297,#152298,#152299,#152300,#152301,#152302,#152303,#152304,
#152305,#152306,#152307,#152308,#152309,#152310,#152311,#152312,#152313,
#152314,#152315,#152316,#152317,#152318,#152319,#152320,#152321,#152322,
#152323,#152324),.UNSPECIFIED.,.F.,.F.,(4,2,2,2,2,2,2,1,2,2,2,2,2,2,2,2,
2,1,1,1,1,2,2,2,2,2,2,2,1,1,1,2,2,2,2,2,1,2,2,1,1,1,2,2,2,1,2,2,1,1,2,2,
2,2,2,1,2,2,1,1,1,4),(7.72626726236311E-7,0.031249999999956,0.062499999999912,
0.0937499999998679,0.109374999999846,0.117187499999835,0.121093749999829,
0.123046874999827,0.124023437499825,0.124999999999824,0.140624999999802,
0.15624999999978,0.171874999999758,0.187499999999736,0.218749999999693,
0.234374999999671,0.24218749999966,0.246093749999654,0.248046874999652,
0.24902343749965,0.24951171874965,0.249938964843399,0.249999999999649,0.281249999999659,
0.312499999999668,0.32031249999967,0.321289062499671,0.321533203124671,
0.321777343749671,0.322265624999671,0.324218749999673,0.328124999999677,
0.343749999999693,0.351562499999701,0.355468749999705,0.357421874999707,
0.359374999999709,0.367187499999717,0.371093749999721,0.373046874999723,
0.374023437499724,0.374511718749724,0.374938964843474,0.374999999999724,
0.390624999999737,0.392578124999738,0.392822265624738,0.393066406249738,
0.393554687499739,0.394531249999739,0.398437499999742,0.406249999999746,
0.421874999999755,0.437499999999764,0.453124999999773,0.453613281249774,
0.453979492187274,0.454101562499774,0.455078124999775,0.457031249999776,
0.460937499999778,0.465501376528164),.UNSPECIFIED.);
#29998=B_SPLINE_CURVE_WITH_KNOTS('',3,(#152325,#152326,#152327,#152328,
#152329,#152330,#152331,#152332,#152333,#152334,#152335,#152336,#152337,
#152338,#152339,#152340,#152341,#152342,#152343,#152344,#152345,#152346,
#152347,#152348,#152349,#152350,#152351,#152352,#152353,#152354,#152355,
#152356,#152357,#152358,#152359,#152360,#152361,#152362,#152363,#152364,
#152365,#152366,#152367,#152368,#152369,#152370,#152371,#152372,#152373,
#152374,#152375,#152376,#152377,#152378,#152379,#152380,#152381,#152382,
#152383,#152384,#152385,#152386,#152387,#152388,#152389,#152390,#152391,
#152392,#152393,#152394,#152395,#152396,#152397,#152398,#152399,#152400,
#152401,#152402,#152403,#152404,#152405,#152406,#152407,#152408,#152409,
#152410,#152411,#152412,#152413,#152414,#152415,#152416,#152417,#152418,
#152419,#152420,#152421,#152422,#152423,#152424,#152425,#152426,#152427,
#152428,#152429),.UNSPECIFIED.,.F.,.F.,(4,2,2,2,1,1,1,1,2,2,2,2,2,2,2,1,
1,1,2,2,2,2,2,1,2,2,1,2,2,2,2,2,2,2,2,2,2,2,1,1,2,2,2,2,1,1,1,1,2,2,2,2,
2,2,2,1,1,2,2,2,4),(0.465501376528164,0.468749999999783,0.484374999999792,
0.492187499999797,0.496093749999799,0.4980468749998,0.499023437499801,0.499511718749801,
0.499938964843552,0.499999999999802,0.515624999999806,0.531249999999811,
0.535156249999812,0.535644531249812,0.536132812499813,0.537109374999813,
0.539062499999813,0.546874999999816,0.562499999999821,0.570312499999824,
0.574218749999825,0.578124999999826,0.585937499999829,0.58789062499983,
0.58886718749983,0.58935546874983,0.58984374999983,0.593749999999831,0.601562499999834,
0.605468749999835,0.606445312499835,0.607421874999835,0.609374999999836,
0.62499999999984,0.640624999999843,0.642578124999844,0.642822265624844,
0.643066406249844,0.643554687499844,0.644531249999845,0.648437499999847,
0.65624999999985,0.687499999999867,0.718749999999883,0.734374999999891,
0.742187499999895,0.746093749999897,0.748046874999898,0.749511718749899,
0.749999999999899,0.781249999999915,0.812499999999931,0.843749999999946,
0.859374999999954,0.867187499999958,0.87109374999996,0.873046874999961,
0.874938964843712,0.874999999999962,0.937499999999981,0.999999692106287),
 .UNSPECIFIED.);
#29999=B_SPLINE_CURVE_WITH_KNOTS('',3,(#152431,#152432,#152433,#152434),
 .UNSPECIFIED.,.F.,.F.,(4,4),(6.46566861907642E-9,0.999998547516504),
 .UNSPECIFIED.);
#30000=B_SPLINE_CURVE_WITH_KNOTS('',3,(#152435,#152436,#152437,#152438,
#152439,#152440,#152441,#152442),.UNSPECIFIED.,.F.,.F.,(4,2,2,4),(0.,0.25,
0.5,1.),.UNSPECIFIED.);
#30001=B_SPLINE_CURVE_WITH_KNOTS('',3,(#152663,#152664,#152665,#152666,
#152667,#152668,#152669,#152670,#152671,#152672,#152673),.UNSPECIFIED.,
 .F.,.F.,(4,1,1,1,1,1,1,1,4),(0.,0.125,0.25,0.375,0.5,0.625,0.75,0.875,
1.),.UNSPECIFIED.);
#30002=B_SPLINE_CURVE_WITH_KNOTS('',3,(#152784,#152785,#152786,#152787,
#152788,#152789,#152790,#152791,#152792,#152793,#152794,#152795,#152796,
#152797,#152798,#152799,#152800,#152801,#152802,#152803,#152804,#152805,
#152806,#152807,#152808,#152809,#152810,#152811,#152812,#152813,#152814,
#152815,#152816,#152817,#152818,#152819,#152820,#152821,#152822,#152823,
#152824,#152825,#152826,#152827,#152828,#152829,#152830,#152831,#152832,
#152833,#152834,#152835,#152836,#152837,#152838,#152839,#152840,#152841),
 .UNSPECIFIED.,.F.,.F.,(4,3,3,3,3,3,3,3,3,3,3,3,3,3,3,3,3,3,3,4),(0.,0.067608122116081,
0.124556588133259,0.193621577458384,0.249619932699945,0.249837494557552,
0.324680401583297,0.37468327726673,0.471469027662659,0.499746621833416,
0.499948939665128,0.596293297167373,0.624809966400102,0.699690355925683,
0.749873310966788,0.750060380763928,0.818979536087593,0.874936655533574,
0.942644019861922,1.),.UNSPECIFIED.);
#30003=B_SPLINE_CURVE_WITH_KNOTS('',3,(#152842,#152843,#152844,#152845,
#152846,#152847,#152848,#152849,#152850,#152851,#152852,#152853,#152854,
#152855,#152856,#152857,#152858,#152859,#152860,#152861,#152862,#152863,
#152864,#152865,#152866,#152867,#152868,#152869,#152870,#152871,#152872,
#152873,#152874,#152875,#152876,#152877,#152878,#152879,#152880,#152881,
#152882),.UNSPECIFIED.,.F.,.F.,(4,2,2,1,1,1,2,2,2,2,1,1,1,1,2,2,2,2,1,1,
1,1,2,2,2,4),(0.,0.125000000000034,0.187500000000051,0.218750000000059,
0.234375000000063,0.242187500000065,0.246093750000066,0.250000000000068,
0.375000000000105,0.437500000000124,0.468750000000133,0.484375000000137,
0.492187500000139,0.49609375000014,0.498046875000141,0.500000000000143,
0.625000000000156,0.687500000000162,0.718750000000165,0.734375000000166,
0.742187500000166,0.746093750000167,0.749023437500166,0.750000000000166,
0.875000000000083,1.),.UNSPECIFIED.);
#30004=B_SPLINE_CURVE_WITH_KNOTS('',3,(#152888,#152889,#152890,#152891,
#152892,#152893,#152894,#152895,#152896,#152897,#152898,#152899,#152900,
#152901,#152902,#152903,#152904,#152905,#152906,#152907,#152908,#152909,
#152910,#152911,#152912,#152913,#152914,#152915,#152916,#152917,#152918,
#152919,#152920,#152921,#152922,#152923,#152924,#152925,#152926,#152927,
#152928,#152929,#152930,#152931,#152932,#152933,#152934,#152935,#152936,
#152937,#152938,#152939,#152940,#152941,#152942,#152943,#152944,#152945,
#152946,#152947,#152948,#152949,#152950,#152951,#152952,#152953,#152954,
#152955,#152956,#152957,#152958,#152959,#152960,#152961,#152962,#152963,
#152964,#152965,#152966),.UNSPECIFIED.,.F.,.F.,(4,3,3,3,3,3,3,3,3,3,3,3,
3,3,3,3,3,3,3,3,3,3,3,3,3,3,4),(1.59010835072902E-15,0.0624999999999996,
0.121020838093803,0.178392295984127,0.233986563636919,0.249999999999994,
0.305023024426928,0.358470295259852,0.37499999999999,0.427815351538303,
0.437499999999989,0.468749999999989,0.48437499999999,0.492187499999991,
0.499429264202313,0.499999999999991,0.546752076236196,0.594486765223972,
0.643796040196902,0.694112041083609,0.745881187044065,0.749999999999996,
0.803525367030386,0.858545471985278,0.914246979722377,0.970685664969118,
1.),.UNSPECIFIED.);
#30005=B_SPLINE_CURVE_WITH_KNOTS('',3,(#152967,#152968,#152969,#152970,
#152971,#152972,#152973,#152974,#152975,#152976,#152977,#152978,#152979,
#152980,#152981,#152982,#152983,#152984,#152985,#152986,#152987,#152988,
#152989,#152990,#152991,#152992,#152993,#152994,#152995,#152996,#152997,
#152998,#152999,#153000,#153001,#153002,#153003,#153004,#153005,#153006,
#153007,#153008,#153009,#153010,#153011,#153012,#153013,#153014,#153015,
#153016,#153017,#153018,#153019,#153020,#153021,#153022,#153023,#153024,
#153025,#153026,#153027,#153028,#153029,#153030,#153031,#153032,#153033,
#153034,#153035,#153036,#153037,#153038,#153039,#153040,#153041,#153042,
#153043,#153044,#153045,#153046,#153047,#153048,#153049,#153050,#153051,
#153052,#153053,#153054,#153055,#153056,#153057,#153058,#153059,#153060,
#153061,#153062,#153063),.UNSPECIFIED.,.F.,.F.,(4,3,3,3,3,3,3,3,3,3,3,3,
3,3,3,3,3,3,3,3,3,3,3,3,3,3,3,3,3,3,3,3,4),(0.,0.031249999999975,0.0607010736965204,
0.0897270673465461,0.118195311223028,0.1249999999999,0.15207935224579,0.178485600985883,
0.18749999999985,0.21311147226121,0.218749999999824,0.234374999999812,0.242187499999805,
0.246093749999802,0.248046874999801,0.2490234374998,0.249511718749799,0.249999999999799,
0.335458392498475,0.374999999999826,0.43749999999984,0.468749999999847,
0.48437499999985,0.492187499999852,0.499471027976032,0.499999999999853,
0.582099180943044,0.666049590471485,0.749999999999927,0.825751814325505,
0.90133264277272,0.976826393250221,1.),.UNSPECIFIED.);
#30006=B_SPLINE_CURVE_WITH_KNOTS('',3,(#153127,#153128,#153129,#153130,
#153131,#153132,#153133,#153134,#153135,#153136,#153137,#153138,#153139,
#153140,#153141,#153142,#153143,#153144,#153145,#153146,#153147,#153148,
#153149,#153150,#153151,#153152,#153153,#153154),.UNSPECIFIED.,.F.,.F.,
(4,3,3,3,3,3,3,3,3,4),(9.89807669334734E-10,0.232893555433494,0.25,0.250189537138593,
0.375284087663041,0.5,0.50037833656381,0.625472138461813,0.750565940359238,
1.),.UNSPECIFIED.);
#30007=B_SPLINE_CURVE_WITH_KNOTS('',3,(#153155,#153156,#153157,#153158,
#153159,#153160,#153161,#153162,#153163,#153164,#153165,#153166,#153167,
#153168),.UNSPECIFIED.,.F.,.F.,(4,2,2,2,2,2,4),(0.,0.250000000000001,0.375000000000001,
0.500000000000001,0.625000000000001,0.75,1.),.UNSPECIFIED.);
#30008=B_SPLINE_CURVE_WITH_KNOTS('',3,(#153282,#153283,#153284,#153285),
 .UNSPECIFIED.,.F.,.F.,(4,4),(0.,1.),.UNSPECIFIED.);
#30009=B_SPLINE_CURVE_WITH_KNOTS('',3,(#153286,#153287,#153288,#153289,
#153290,#153291,#153292,#153293,#153294,#153295,#153296,#153297,#153298,
#153299,#153300,#153301,#153302,#153303,#153304,#153305,#153306,#153307,
#153308,#153309,#153310,#153311,#153312,#153313,#153314,#153315,#153316,
#153317,#153318,#153319,#153320,#153321,#153322,#153323,#153324,#153325,
#153326,#153327,#153328,#153329,#153330,#153331,#153332,#153333,#153334,
#153335,#153336,#153337,#153338,#153339,#153340,#153341,#153342,#153343,
#153344,#153345,#153346,#153347,#153348,#153349,#153350,#153351,#153352,
#153353,#153354,#153355,#153356,#153357,#153358),.UNSPECIFIED.,.F.,.F.,
(4,3,3,3,3,3,3,3,3,3,3,3,3,3,3,3,3,3,3,3,3,3,3,3,4),(0.,0.0444154464726,
0.088382210368451,0.131763087129373,0.174838624328436,0.217515042786487,
0.249939927815387,0.291563369073533,0.332989920633538,0.37473289612189,
0.415853341206836,0.45790758189689,0.499961822586944,0.540995736379099,
0.582060349521465,0.624041191480699,0.665355026237124,0.707669371797763,
0.749983717358402,0.792598675882721,0.835493364945415,0.878917478176752,
0.92265717931407,0.966982523655085,1.),.UNSPECIFIED.);
#30010=B_SPLINE_CURVE_WITH_KNOTS('',3,(#153444,#153445,#153446,#153447,
#153448,#153449,#153450,#153451,#153452,#153453,#153454,#153455,#153456,
#153457,#153458,#153459,#153460,#153461,#153462,#153463,#153464,#153465,
#153466,#153467,#153468,#153469,#153470,#153471,#153472,#153473,#153474,
#153475,#153476,#153477,#153478,#153479,#153480,#153481,#153482,#153483,
#153484,#153485,#153486,#153487,#153488,#153489,#153490,#153491,#153492,
#153493,#153494,#153495,#153496,#153497,#153498,#153499,#153500,#153501,
#153502,#153503,#153504,#153505,#153506,#153507,#153508,#153509,#153510,
#153511,#153512,#153513,#153514,#153515,#153516,#153517,#153518,#153519,
#153520,#153521,#153522,#153523,#153524,#153525,#153526,#153527,#153528,
#153529,#153530,#153531,#153532,#153533,#153534,#153535,#153536,#153537,
#153538,#153539,#153540,#153541,#153542,#153543,#153544,#153545,#153546,
#153547,#153548,#153549,#153550,#153551,#153552,#153553,#153554,#153555,
#153556,#153557,#153558,#153559,#153560,#153561,#153562,#153563,#153564,
#153565,#153566,#153567,#153568,#153569,#153570,#153571,#153572,#153573,
#153574,#153575,#153576,#153577,#153578,#153579,#153580,#153581,#153582,
#153583,#153584,#153585,#153586,#153587,#153588,#153589,#153590,#153591,
#153592,#153593,#153594,#153595,#153596,#153597,#153598,#153599,#153600,
#153601,#153602,#153603,#153604,#153605,#153606,#153607,#153608,#153609,
#153610,#153611,#153612,#153613,#153614,#153615,#153616,#153617,#153618,
#153619,#153620,#153621,#153622,#153623,#153624,#153625,#153626,#153627,
#153628,#153629,#153630,#153631,#153632,#153633,#153634,#153635,#153636,
#153637,#153638,#153639,#153640,#153641,#153642,#153643,#153644,#153645,
#153646,#153647,#153648,#153649,#153650,#153651),.UNSPECIFIED.,.F.,.F.,
(4,3,3,3,3,3,3,3,3,3,3,3,3,3,3,3,3,3,3,3,3,3,3,3,3,3,3,3,3,3,3,3,3,3,3,
3,3,3,3,3,3,3,3,3,3,3,3,3,3,3,3,3,3,3,3,3,3,3,3,3,3,3,3,3,3,3,3,3,3,4),
(0.,0.0400589307361862,0.0797406453201286,0.118620801173798,0.125000000000011,
0.158233673552439,0.187500000000015,0.218750000000018,0.234375000000019,
0.24218750000002,0.24609375000002,0.249197866572958,0.25000000000002,0.274801018258469,
0.299154388956895,0.312500000000027,0.332141319272399,0.34375000000003,
0.359375000000031,0.367187500000032,0.371093750000032,0.373046875000033,
0.374023437500033,0.375000000000033,0.391246335883929,0.406278833684744,
0.413951005682541,0.430418756934123,0.437500000000032,0.453125000000031,
0.467852567759811,0.468750000000031,0.482935516148494,0.484375000000031,
0.493680329367665,0.499685418008973,0.50000000000003,0.512751122340329,
0.525998905586144,0.538496063904995,0.553131951474991,0.562500000000029,
0.578631755981225,0.585352841872323,0.593750000000029,0.609375000000029,
0.617187500000028,0.621093750000028,0.623046875000028,0.624023437500028,
0.625000000000028,0.643647435582588,0.662533544580982,0.68183911773363,
0.687500000000025,0.70072917260516,0.718750000000024,0.734375000000023,
0.742187500000022,0.746093750000022,0.749183103148108,0.750000000000021,
0.783169859588238,0.817376344468976,0.84161230871826,0.876448322903235,
0.911687871399364,0.94688403398269,0.981633629845859,1.),.UNSPECIFIED.);
#30011=B_SPLINE_CURVE_WITH_KNOTS('',3,(#153669,#153670,#153671,#153672),
 .UNSPECIFIED.,.F.,.F.,(4,4),(0.,1.),.UNSPECIFIED.);
#30012=B_SPLINE_CURVE_WITH_KNOTS('',3,(#153675,#153676,#153677,#153678,
#153679,#153680,#153681,#153682,#153683,#153684),.UNSPECIFIED.,.F.,.F.,
(4,3,3,4),(0.,0.355575480078952,0.708688526690115,1.),.UNSPECIFIED.);
#30013=B_SPLINE_CURVE_WITH_KNOTS('',3,(#153686,#153687,#153688,#153689,
#153690,#153691,#153692,#153693,#153694,#153695,#153696,#153697,#153698,
#153699,#153700,#153701,#153702,#153703,#153704,#153705,#153706,#153707,
#153708,#153709,#153710,#153711,#153712,#153713,#153714,#153715,#153716,
#153717,#153718,#153719,#153720,#153721,#153722,#153723,#153724,#153725,
#153726,#153727,#153728,#153729,#153730,#153731,#153732,#153733,#153734,
#153735,#153736,#153737,#153738,#153739,#153740,#153741,#153742,#153743,
#153744,#153745,#153746,#153747,#153748,#153749,#153750,#153751,#153752,
#153753,#153754,#153755,#153756,#153757,#153758,#153759,#153760,#153761,
#153762,#153763,#153764,#153765,#153766,#153767,#153768,#153769,#153770,
#153771,#153772,#153773,#153774,#153775,#153776,#153777,#153778,#153779,
#153780,#153781,#153782,#153783,#153784,#153785,#153786,#153787,#153788,
#153789,#153790,#153791,#153792,#153793,#153794,#153795,#153796,#153797,
#153798,#153799,#153800,#153801,#153802,#153803,#153804,#153805,#153806,
#153807,#153808,#153809,#153810,#153811,#153812,#153813,#153814,#153815,
#153816,#153817,#153818,#153819,#153820,#153821,#153822,#153823,#153824,
#153825,#153826,#153827,#153828,#153829,#153830,#153831,#153832,#153833,
#153834,#153835,#153836),.UNSPECIFIED.,.F.,.F.,(4,3,3,3,3,3,3,3,3,3,3,3,
3,3,3,3,3,3,3,3,3,3,3,3,3,3,3,3,3,3,3,3,3,3,3,3,3,3,3,3,3,3,3,3,3,3,3,3,
3,3,4),(0.,0.0266572530362359,0.0529474029428651,0.0625000000000029,0.0880857890087234,
0.0937500000000047,0.109375000000006,0.117187500000006,0.122072505131236,
0.124806686990945,0.125000000000006,0.150224861065753,0.175595927078806,
0.187142286124972,0.187500000000007,0.218750000000007,0.234375000000007,
0.242660532900981,0.250000000000007,0.282477540622239,0.313776512685994,
0.345310797249849,0.375000000000007,0.377013825968837,0.407760369476629,
0.438211040162093,0.469105520081049,0.500000000000006,0.532769453185549,
0.565934692720068,0.59970342888731,0.622796551583423,0.625000000000005,
0.656333797697557,0.687500000000005,0.718750000000005,0.734375000000005,
0.742187500000005,0.746093750000005,0.748046875000004,0.750000000000004,
0.776677040852684,0.804022779420661,0.83169633877836,0.859747497852255,
0.873068492291997,0.901180604984381,0.929428841358404,0.957620752845238,
0.98555271402396,1.),.UNSPECIFIED.);
#30014=B_SPLINE_CURVE_WITH_KNOTS('',3,(#153837,#153838,#153839,#153840,
#153841,#153842,#153843,#153844,#153845,#153846),.UNSPECIFIED.,.F.,.F.,
(4,3,3,4),(0.,0.371972328017731,0.745231674146774,1.),.UNSPECIFIED.);
#30015=B_SPLINE_CURVE_WITH_KNOTS('',3,(#153864,#153865,#153866,#153867,
#153868,#153869,#153870,#153871,#153872,#153873),.UNSPECIFIED.,.F.,.F.,
(4,2,2,2,4),(0.,0.25,0.5,0.75,1.),.UNSPECIFIED.);
#30016=B_SPLINE_CURVE_WITH_KNOTS('',3,(#153875,#153876,#153877,#153878,
#153879,#153880,#153881,#153882,#153883,#153884),.UNSPECIFIED.,.F.,.F.,
(4,3,3,4),(0.,0.341585033093189,0.68318654002556,1.),.UNSPECIFIED.);
#30017=B_SPLINE_CURVE_WITH_KNOTS('',3,(#153985,#153986,#153987,#153988,
#153989,#153990,#153991,#153992,#153993,#153994,#153995,#153996,#153997,
#153998,#153999,#154000,#154001,#154002,#154003,#154004,#154005,#154006,
#154007,#154008,#154009,#154010,#154011,#154012,#154013,#154014,#154015,
#154016,#154017,#154018,#154019,#154020,#154021,#154022,#154023,#154024,
#154025,#154026,#154027,#154028,#154029,#154030,#154031,#154032,#154033,
#154034,#154035,#154036,#154037,#154038,#154039,#154040,#154041,#154042,
#154043,#154044,#154045,#154046,#154047,#154048,#154049,#154050,#154051,
#154052,#154053,#154054,#154055,#154056,#154057,#154058,#154059,#154060,
#154061,#154062,#154063,#154064,#154065,#154066,#154067,#154068,#154069,
#154070,#154071,#154072,#154073,#154074,#154075,#154076,#154077,#154078,
#154079,#154080),.UNSPECIFIED.,.F.,.F.,(4,2,1,1,1,1,2,2,2,2,1,1,1,2,2,2,
1,1,1,1,2,2,2,2,1,1,1,2,2,2,2,2,1,1,1,2,2,2,2,1,1,1,1,2,2,2,2,1,1,1,1,2,
2,2,2,2,1,1,1,2,2,4),(0.,0.0624999999995465,0.0937499999993206,0.109374999999209,
0.117187499999153,0.121093749999124,0.123046874999109,0.124999999999095,
0.156249999998887,0.171874999998781,0.179687499998729,0.183593749998702,
0.185546874998689,0.186523437498682,0.187499999998676,0.218749999998446,
0.234374999998332,0.242187499998274,0.246093749998246,0.248046874998231,
0.249023437498222,0.249999999998212,0.312499999997693,0.343749999997435,
0.359374999997306,0.367187499997241,0.371093749997209,0.373046874997192,
0.374999999997174,0.499999999996056,0.562499999995497,0.593749999995218,
0.609374999995079,0.61718749999501,0.621093749994975,0.623046874994959,
0.624999999994943,0.687499999994446,0.718749999994198,0.734374999994075,
0.742187499994012,0.74609374999398,0.748046874993965,0.749023437493958,
0.749999999993951,0.812499999993504,0.843749999993281,0.859374999993169,
0.867187499993113,0.871093749993084,0.87304687499307,0.874755859368059,
0.874999999993057,0.906249999994804,0.921874999995676,0.929687499996112,
0.933593749996331,0.93554687499644,0.936523437496495,0.937011718746522,
0.93749999999655,1.),.UNSPECIFIED.);
#30018=B_SPLINE_CURVE_WITH_KNOTS('',3,(#154099,#154100,#154101,#154102,
#154103,#154104,#154105,#154106,#154107,#154108,#154109,#154110,#154111,
#154112,#154113,#154114,#154115),.UNSPECIFIED.,.F.,.F.,(4,2,2,2,1,1,1,2,
2,4),(0.,0.24999999999989,0.374999999999839,0.437499999999813,0.4687499999998,
0.484374999999796,0.492187499999792,0.496093749999792,0.499999999999793,
1.),.UNSPECIFIED.);
#30019=B_SPLINE_CURVE_WITH_KNOTS('',3,(#154118,#154119,#154120,#154121,
#154122,#154123,#154124,#154125,#154126,#154127),.UNSPECIFIED.,.F.,.F.,
(4,3,3,4),(6.77035784782114E-15,0.355575475820603,0.70868851966236,1.),
 .UNSPECIFIED.);
#30020=B_SPLINE_CURVE_WITH_KNOTS('',3,(#154129,#154130,#154131,#154132,
#154133,#154134,#154135,#154136,#154137,#154138,#154139,#154140,#154141,
#154142,#154143,#154144,#154145,#154146,#154147,#154148,#154149,#154150,
#154151,#154152,#154153,#154154,#154155,#154156,#154157,#154158,#154159,
#154160,#154161,#154162,#154163,#154164,#154165,#154166,#154167,#154168,
#154169,#154170,#154171,#154172,#154173,#154174,#154175,#154176,#154177),
 .UNSPECIFIED.,.F.,.F.,(4,3,3,3,3,3,3,3,3,3,3,3,3,3,3,3,4),(0.,0.0910455835011647,
0.182439138574727,0.250000000000011,0.339921904045264,0.375000000000017,
0.43750000000002,0.46875000000002,0.484375000000021,0.495831044563394,0.500000000000021,
0.5909385551545,0.681877417910837,0.772012506325215,0.861316606459104,0.948942207273129,
1.),.UNSPECIFIED.);
#30021=B_SPLINE_CURVE_WITH_KNOTS('',3,(#154195,#154196,#154197,#154198,
#154199,#154200),.UNSPECIFIED.,.F.,.F.,(4,2,4),(-0.606451718743048,-0.299493685602885,
-9.99999995198692E-7),.UNSPECIFIED.);
#30022=B_SPLINE_CURVE_WITH_KNOTS('',3,(#154223,#154224,#154225,#154226,
#154227,#154228),.UNSPECIFIED.,.F.,.F.,(4,2,4),(-0.372442319355049,-0.186223020487114,
-3.03100744253534E-6),.UNSPECIFIED.);
#30023=B_SPLINE_CURVE_WITH_KNOTS('',3,(#154229,#154230,#154231,#154232,
#154233),.UNSPECIFIED.,.F.,.F.,(4,1,4),(4.77483324436819E-6,0.503003588545041,
1.),.UNSPECIFIED.);
#30024=B_SPLINE_CURVE_WITH_KNOTS('',3,(#154251,#154252,#154253,#154254,
#154255,#154256),.UNSPECIFIED.,.F.,.F.,(4,2,4),(-0.3724515983366,-0.186230562103344,
-4.29627198925348E-6),.UNSPECIFIED.);
#30025=B_SPLINE_CURVE_WITH_KNOTS('',3,(#154257,#154258,#154259,#154260,
#154261,#154262,#154263,#154264,#154265,#154266,#154267,#154268,#154269,
#154270,#154271,#154272,#154273,#154274,#154275,#154276,#154277,#154278,
#154279,#154280,#154281,#154282,#154283,#154284,#154285,#154286,#154287,
#154288,#154289,#154290,#154291,#154292,#154293,#154294,#154295,#154296,
#154297,#154298,#154299,#154300,#154301,#154302,#154303,#154304,#154305,
#154306,#154307,#154308,#154309,#154310,#154311,#154312,#154313,#154314),
 .UNSPECIFIED.,.F.,.F.,(4,3,3,3,3,3,3,3,3,3,3,3,3,3,3,3,3,3,3,4),(2.72798627453737E-6,
0.0553540505734548,0.110169237189544,0.164514703027846,0.218455604332041,
0.272056050301599,0.325379106943922,0.378456718575932,0.431385880590234,
0.484247453423519,0.53709545654247,0.590321592406853,0.643381688533521,
0.696726047499516,0.75,0.803819714741727,0.858209994582057,0.912952977410288,
0.968345446498143,1.),.UNSPECIFIED.);
#30026=B_SPLINE_CURVE_WITH_KNOTS('',3,(#154332,#154333,#154334,#154335,
#154336,#154337),.UNSPECIFIED.,.F.,.F.,(4,2,4),(-0.608015977036257,-0.307733847198884,
-2.53573569086033E-6),.UNSPECIFIED.);
#30027=B_SPLINE_CURVE_WITH_KNOTS('',3,(#154340,#154341,#154342,#154343,
#154344,#154345,#154346,#154347,#154348,#154349,#154350,#154351,#154352,
#154353,#154354,#154355,#154356,#154357,#154358,#154359,#154360,#154361,
#154362,#154363,#154364,#154365,#154366,#154367,#154368,#154369,#154370,
#154371,#154372,#154373,#154374,#154375,#154376),.UNSPECIFIED.,.F.,.F.,
(4,3,3,3,3,3,3,3,3,3,3,3,4),(1.88907660345648E-10,0.0909364924096919,0.183637933662997,
0.278561470178532,0.37450130725563,0.471472916587379,0.5,0.597277769481169,
0.697958327110877,0.792495880377744,0.885613970721787,0.976356605035924,
1.),.UNSPECIFIED.);
#30028=B_SPLINE_CURVE_WITH_KNOTS('',3,(#154378,#154379,#154380,#154381,
#154382,#154383,#154384,#154385,#154386,#154387),.UNSPECIFIED.,.F.,.F.,
(4,3,3,4),(0.,0.371972324766811,0.745231666277941,0.999999999999995),
 .UNSPECIFIED.);
#30029=B_SPLINE_CURVE_WITH_KNOTS('',3,(#154405,#154406,#154407,#154408,
#154409,#154410,#154411,#154412,#154413,#154414),.UNSPECIFIED.,.F.,.F.,
(4,3,3,4),(0.,0.341585064612949,0.68318660305952,1.),.UNSPECIFIED.);
#30030=B_SPLINE_CURVE_WITH_KNOTS('',3,(#154515,#154516,#154517,#154518,
#154519,#154520,#154521,#154522,#154523,#154524,#154525,#154526,#154527,
#154528,#154529,#154530,#154531,#154532,#154533,#154534,#154535,#154536,
#154537,#154538,#154539,#154540,#154541,#154542,#154543,#154544,#154545,
#154546,#154547,#154548,#154549,#154550,#154551,#154552,#154553,#154554,
#154555,#154556,#154557,#154558,#154559,#154560,#154561,#154562,#154563,
#154564,#154565,#154566,#154567,#154568,#154569,#154570,#154571,#154572,
#154573,#154574,#154575,#154576,#154577,#154578,#154579,#154580,#154581,
#154582,#154583,#154584,#154585,#154586,#154587,#154588,#154589,#154590,
#154591,#154592,#154593,#154594,#154595,#154596,#154597,#154598,#154599,
#154600,#154601,#154602,#154603,#154604,#154605,#154606,#154607,#154608,
#154609,#154610),.UNSPECIFIED.,.F.,.F.,(4,2,1,1,1,1,2,2,2,2,1,1,1,2,2,2,
1,1,1,1,2,2,2,2,1,1,1,2,2,2,2,2,1,1,1,2,2,2,2,1,1,1,1,2,2,2,2,1,1,1,1,2,
2,2,2,2,1,1,1,2,2,4),(0.,0.0625000000001708,0.0937500000002552,0.109375000000297,
0.117187500000319,0.121093750000329,0.123046875000333,0.125000000000337,
0.156250000000383,0.171875000000407,0.179687500000418,0.183593750000423,
0.185546875000425,0.186523437500426,0.187500000000426,0.21875000000041,
0.234375000000404,0.2421875000004,0.2460937500004,0.248046875000401,0.249023437500402,
0.250000000000403,0.312500000000517,0.343750000000574,0.359375000000602,
0.367187500000616,0.371093750000624,0.373046875000628,0.375000000000633,
0.500000000001077,0.562500000001299,0.593750000001411,0.609375000001468,
0.617187500001496,0.621093750001509,0.623046875001517,0.625000000001525,
0.687500000001828,0.718750000001978,0.734375000002053,0.742187500002091,
0.746093750002109,0.748046875002119,0.749023437502122,0.750000000002126,
0.812500000002261,0.843750000002328,0.859375000002362,0.867187500002379,
0.871093750002388,0.873046875002393,0.874755859377398,0.875000000002398,
0.906250000001822,0.921875000001533,0.929687500001389,0.933593750001317,
0.935546875001281,0.936523437501262,0.937011718751253,0.937500000001243,
1.),.UNSPECIFIED.);
#30031=B_SPLINE_CURVE_WITH_KNOTS('',3,(#154629,#154630,#154631,#154632,
#154633,#154634,#154635,#154636,#154637,#154638,#154639,#154640,#154641,
#154642,#154643,#154644,#154645),.UNSPECIFIED.,.F.,.F.,(4,2,2,2,1,1,1,2,
2,4),(0.,0.249999999999954,0.374999999999937,0.437499999999928,0.468749999999923,
0.484374999999921,0.49218749999992,0.496093749999922,0.499999999999924,
1.),.UNSPECIFIED.);
#30032=B_SPLINE_CURVE_WITH_KNOTS('',3,(#154646,#154647,#154648,#154649,
#154650,#154651,#154652,#154653,#154654,#154655,#154656,#154657,#154658,
#154659,#154660,#154661,#154662,#154663,#154664,#154665,#154666,#154667,
#154668,#154669,#154670,#154671,#154672,#154673,#154674,#154675,#154676,
#154677,#154678,#154679,#154680,#154681,#154682,#154683,#154684,#154685,
#154686,#154687,#154688,#154689,#154690,#154691,#154692,#154693,#154694,
#154695,#154696,#154697,#154698,#154699,#154700,#154701,#154702,#154703,
#154704,#154705,#154706,#154707,#154708,#154709,#154710,#154711,#154712,
#154713,#154714,#154715),.UNSPECIFIED.,.F.,.F.,(4,3,3,3,3,3,3,3,3,3,3,3,
3,3,3,3,3,3,3,3,3,3,3,4),(0.,0.0497162850538284,0.0997854118434574,0.148349769878621,
0.19657310085876,0.244406250169066,0.249992792212344,0.296849141910662,
0.343480318803109,0.389891233648019,0.43620088824267,0.482450015571192,
0.499995230081589,0.5462432932865,0.592530815463781,0.638989031954228,0.685571564742959,
0.732423225621977,0.749997667950833,0.797873988738031,0.848405491553523,
0.897207740062206,0.948603870031103,1.),.UNSPECIFIED.);
#30033=B_SPLINE_CURVE_WITH_KNOTS('',3,(#154807,#154808,#154809,#154810,
#154811,#154812,#154813,#154814,#154815,#154816),.UNSPECIFIED.,.F.,.F.,
(4,2,2,2,4),(7.91321415605965E-5,0.461550908372518,0.883826720447071,1.3071784210996,
1.78873513688511),.UNSPECIFIED.);
#30034=B_SPLINE_CURVE_WITH_KNOTS('',3,(#154835,#154836,#154837,#154838,
#154839),.UNSPECIFIED.,.F.,.F.,(4,1,4),(1.32451275613523E-5,0.5,1.),
 .UNSPECIFIED.);
#30035=B_SPLINE_CURVE_WITH_KNOTS('',3,(#154841,#154842,#154843,#154844,
#154845,#154846,#154847,#154848,#154849,#154850,#154851,#154852,#154853,
#154854,#154855,#154856,#154857,#154858,#154859,#154860,#154861,#154862,
#154863,#154864,#154865,#154866,#154867,#154868,#154869,#154870,#154871,
#154872,#154873,#154874,#154875,#154876,#154877,#154878,#154879,#154880,
#154881,#154882,#154883,#154884,#154885,#154886,#154887,#154888,#154889,
#154890,#154891,#154892,#154893,#154894,#154895,#154896,#154897,#154898,
#154899,#154900,#154901,#154902,#154903,#154904,#154905,#154906,#154907,
#154908,#154909,#154910,#154911,#154912,#154913,#154914,#154915,#154916,
#154917,#154918,#154919,#154920,#154921,#154922,#154923,#154924,#154925,
#154926,#154927,#154928,#154929,#154930,#154931,#154932,#154933,#154934,
#154935,#154936,#154937,#154938,#154939,#154940,#154941,#154942,#154943,
#154944,#154945,#154946,#154947,#154948,#154949),.UNSPECIFIED.,.F.,.F.,
(4,3,3,3,3,3,3,3,3,3,3,3,3,3,3,3,3,3,3,3,3,3,3,3,3,3,3,3,3,3,3,3,3,3,3,
3,4),(2.73301476691168E-15,0.039441191303371,0.0768210354237637,0.11122288018331,
0.125,0.177992474343909,0.227481533149721,0.240547827143166,0.25,0.304443784156054,
0.357336706676159,0.369855256013052,0.375,0.40891821135081,0.442204853614617,
0.474505774150831,0.499217941560634,0.5,0.523587949419504,0.547077247101464,
0.57061197134477,0.594260887285262,0.618209766593177,0.625,0.628457488463763,
0.669404035577509,0.711444268396472,0.75,0.757882644294487,0.804582852109327,
0.852316895707969,0.875,0.887185081605594,0.920801047847144,0.955229129512886,
0.99089973413878,1.),.UNSPECIFIED.);
#30036=B_SPLINE_CURVE_WITH_KNOTS('',3,(#154951,#154952,#154953,#154954,
#154955,#154956),.UNSPECIFIED.,.F.,.F.,(4,1,1,4),(0.,0.3333333333333,0.6666666666667,
1.),.UNSPECIFIED.);
#30037=B_SPLINE_CURVE_WITH_KNOTS('',3,(#154958,#154959,#154960,#154961,
#154962,#154963,#154964),.UNSPECIFIED.,.F.,.F.,(4,3,4),(0.,0.5,1.),
 .UNSPECIFIED.);
#30038=B_SPLINE_CURVE_WITH_KNOTS('',3,(#154967,#154968,#154969,#154970,
#154971,#154972,#154973),.UNSPECIFIED.,.F.,.F.,(4,3,4),(0.,0.5,1.),
 .UNSPECIFIED.);
#30039=B_SPLINE_CURVE_WITH_KNOTS('',3,(#154974,#154975,#154976,#154977,
#154978),.UNSPECIFIED.,.F.,.F.,(4,1,4),(0.,0.5,0.999976693117295),
 .UNSPECIFIED.);
#30040=B_SPLINE_CURVE_WITH_KNOTS('',3,(#155022,#155023,#155024,#155025,
#155026,#155027,#155028),.UNSPECIFIED.,.F.,.F.,(4,3,4),(0.,0.737738535805643,
0.999999999999949),.UNSPECIFIED.);
#30041=B_SPLINE_CURVE_WITH_KNOTS('',3,(#155080,#155081,#155082,#155083),
 .UNSPECIFIED.,.F.,.F.,(4,4),(0.,0.999999733456458),.UNSPECIFIED.);
#30042=B_SPLINE_CURVE_WITH_KNOTS('',3,(#155149,#155150,#155151,#155152),
 .UNSPECIFIED.,.F.,.F.,(4,4),(0.,1.),.UNSPECIFIED.);
#30043=B_SPLINE_CURVE_WITH_KNOTS('',3,(#155154,#155155,#155156,#155157,
#155158,#155159,#155160,#155161,#155162,#155163,#155164,#155165,#155166,
#155167,#155168,#155169,#155170,#155171,#155172,#155173,#155174,#155175,
#155176,#155177,#155178,#155179,#155180,#155181,#155182,#155183,#155184,
#155185,#155186,#155187,#155188,#155189,#155190,#155191,#155192,#155193,
#155194,#155195,#155196,#155197,#155198,#155199,#155200,#155201,#155202,
#155203,#155204,#155205,#155206,#155207,#155208,#155209,#155210,#155211,
#155212,#155213,#155214,#155215,#155216,#155217,#155218,#155219,#155220,
#155221,#155222,#155223,#155224,#155225,#155226,#155227,#155228,#155229,
#155230,#155231,#155232,#155233,#155234,#155235,#155236,#155237,#155238,
#155239,#155240,#155241,#155242,#155243,#155244,#155245,#155246,#155247,
#155248,#155249,#155250,#155251,#155252,#155253,#155254,#155255,#155256,
#155257,#155258,#155259,#155260,#155261,#155262,#155263,#155264,#155265,
#155266,#155267,#155268,#155269,#155270,#155271,#155272,#155273,#155274,
#155275,#155276,#155277,#155278,#155279,#155280,#155281,#155282,#155283,
#155284,#155285,#155286,#155287,#155288,#155289,#155290,#155291,#155292,
#155293,#155294,#155295,#155296,#155297,#155298,#155299,#155300,#155301,
#155302,#155303,#155304,#155305,#155306,#155307,#155308,#155309,#155310,
#155311,#155312,#155313,#155314,#155315,#155316,#155317,#155318,#155319,
#155320,#155321,#155322,#155323,#155324,#155325,#155326,#155327,#155328,
#155329,#155330,#155331,#155332,#155333,#155334,#155335,#155336,#155337,
#155338,#155339,#155340,#155341,#155342,#155343,#155344,#155345,#155346,
#155347,#155348,#155349,#155350,#155351,#155352,#155353,#155354,#155355,
#155356,#155357,#155358,#155359,#155360,#155361,#155362,#155363,#155364,
#155365,#155366,#155367,#155368,#155369,#155370,#155371,#155372,#155373,
#155374,#155375,#155376,#155377,#155378,#155379,#155380,#155381,#155382,
#155383,#155384,#155385,#155386,#155387,#155388,#155389,#155390,#155391,
#155392,#155393,#155394,#155395,#155396,#155397,#155398,#155399,#155400,
#155401,#155402,#155403,#155404,#155405,#155406,#155407,#155408,#155409,
#155410,#155411,#155412,#155413,#155414,#155415,#155416,#155417,#155418,
#155419,#155420,#155421,#155422,#155423,#155424),.UNSPECIFIED.,.F.,.F.,
(4,3,3,3,3,3,3,3,3,3,3,3,3,3,3,3,3,3,3,3,3,3,3,3,3,3,3,3,3,3,3,3,3,3,3,
3,3,3,3,3,3,3,3,3,3,3,3,3,3,3,3,3,3,3,3,3,3,3,3,3,3,3,3,3,3,3,3,3,3,3,3,
3,3,3,3,3,3,3,3,3,3,3,3,3,3,3,3,3,3,3,4),(0.,0.0156249999999938,0.0312499999999876,
0.0468749999999821,0.05468749999998,0.0585937499999794,0.0605468749999791,
0.0615234374999789,0.0620117187499788,0.0624999999999787,0.0737022644319959,
0.084645872498037,0.0937499999999818,0.104685910244887,0.109374999999983,
0.118663537724106,0.124999999999984,0.139243619738437,0.146301019042459,
0.161162267135373,0.176716398763141,0.187499999999988,0.207644104682402,
0.21874999999999,0.234374999999992,0.242187499999992,0.246093749999993,
0.248046874999993,0.249023437499993,0.249511718749992,0.249999999999992,
0.272731652445828,0.302235313168796,0.312499999999973,0.326809661104179,
0.353843405339416,0.374999999999953,0.383302879496592,0.412729393604404,
0.437499999999933,0.442461712707441,0.468749999999924,0.484374999999919,
0.492215068290938,0.499999999999914,0.504389899607464,0.536742275540799,
0.569776777538791,0.602077537598559,0.622092744943588,0.624999999999875,
0.652975419385661,0.677138851153577,0.687499999999855,0.712581838697012,
0.718749999999845,0.730023511366994,0.73437499999984,0.742187499999838,
0.746093749999836,0.748046874999835,0.749023437499835,0.749511718749835,
0.749999999999835,0.772497759731973,0.794313424727545,0.812499999999868,
0.829511372540639,0.843749999999884,0.854252480274351,0.859374999999892,
0.867187499999896,0.872391286447649,0.8749999999999,0.885692729179628,0.896423825799802,
0.906249999999915,0.91699473121533,0.921874999999922,0.929687499999924,
0.933593749999927,0.935546874999927,0.936523437499928,0.937011718749928,
0.937255859374929,0.937499999999929,0.955209733027919,0.968749999999964,
0.98350921182179,0.998604231401742,1.),.UNSPECIFIED.);
#30044=B_SPLINE_CURVE_WITH_KNOTS('',3,(#155425,#155426,#155427,#155428),
 .UNSPECIFIED.,.F.,.F.,(4,4),(4.21851813676615E-6,1.),.UNSPECIFIED.);
#30045=B_SPLINE_CURVE_WITH_KNOTS('',3,(#155453,#155454,#155455,#155456,
#155457,#155458),.UNSPECIFIED.,.F.,.F.,(4,2,4),(6.01557958534666E-6,0.5,
1.),.UNSPECIFIED.);
#30046=B_SPLINE_CURVE_WITH_KNOTS('',3,(#155485,#155486,#155487,#155488,
#155489,#155490,#155491,#155492,#155493,#155494,#155495,#155496,#155497,
#155498,#155499,#155500),.UNSPECIFIED.,.F.,.F.,(4,3,3,3,3,4),(0.,0.25,0.499016891676494,
0.749508445838247,0.986332989034377,1.),.UNSPECIFIED.);
#30047=B_SPLINE_CURVE_WITH_KNOTS('',3,(#155517,#155518,#155519,#155520,
#155521,#155522,#155523,#155524,#155525,#155526,#155527,#155528,#155529,
#155530,#155531,#155532,#155533,#155534,#155535,#155536,#155537,#155538,
#155539,#155540,#155541),.UNSPECIFIED.,.F.,.F.,(4,3,3,3,3,3,3,3,4),(0.,
0.143229396317443,0.288391134800666,0.428837100197094,0.56846061529328,
0.707144473842968,0.723876350250335,0.861938175125168,1.),.UNSPECIFIED.);
#30048=B_SPLINE_CURVE_WITH_KNOTS('',3,(#155618,#155619,#155620,#155621,
#155622,#155623,#155624,#155625,#155626,#155627,#155628,#155629,#155630,
#155631,#155632,#155633,#155634,#155635,#155636,#155637,#155638,#155639,
#155640,#155641,#155642,#155643,#155644,#155645,#155646,#155647,#155648,
#155649,#155650,#155651,#155652,#155653,#155654,#155655,#155656,#155657,
#155658,#155659,#155660,#155661,#155662,#155663,#155664,#155665,#155666,
#155667,#155668,#155669,#155670,#155671,#155672,#155673,#155674,#155675,
#155676,#155677,#155678,#155679,#155680,#155681,#155682,#155683,#155684,
#155685,#155686,#155687,#155688,#155689,#155690,#155691,#155692,#155693,
#155694,#155695,#155696,#155697,#155698,#155699,#155700,#155701,#155702,
#155703,#155704,#155705,#155706,#155707,#155708,#155709,#155710,#155711,
#155712,#155713,#155714,#155715,#155716,#155717,#155718,#155719,#155720),
 .UNSPECIFIED.,.F.,.F.,(4,3,3,3,3,3,3,3,3,3,3,3,3,3,3,3,3,3,3,3,3,3,3,3,
3,3,3,3,3,3,3,3,3,3,4),(0.,0.0271165157246254,0.0552397979707361,0.0805406843846776,
0.117403543853953,0.124999999999937,0.163705158930506,0.191078655875936,
0.238272614623893,0.287092880371944,0.326326003103155,0.381913001551468,
0.437499999999781,0.468749999999766,0.484374999999758,0.492187499999756,
0.496093749999755,0.498046874999754,0.498822546661111,0.499999999999754,
0.550409420598624,0.600158718135214,0.649053115359039,0.666386519103641,
0.716491463985741,0.764059802343202,0.805072556691199,0.843451541598094,
0.874999999999939,0.911087468126675,0.917362338160448,0.944900395318624,
0.972450197659312,0.998184941463724,1.),.UNSPECIFIED.);
#30049=B_SPLINE_CURVE_WITH_KNOTS('',3,(#155723,#155724,#155725,#155726,
#155727,#155728,#155729,#155730,#155731,#155732,#155733,#155734,#155735,
#155736,#155737,#155738,#155739,#155740,#155741),.UNSPECIFIED.,.F.,.F.,
(4,3,3,3,3,3,4),(1.40360687088514E-7,0.188647371465953,0.385548650834157,
0.587125074313563,0.794262989574996,0.92226232086797,0.999999996838511),
 .UNSPECIFIED.);
#30050=B_SPLINE_CURVE_WITH_KNOTS('',3,(#155766,#155767,#155768,#155769,
#155770,#155771,#155772,#155773,#155774,#155775,#155776,#155777,#155778,
#155779,#155780,#155781,#155782,#155783,#155784,#155785,#155786,#155787,
#155788,#155789,#155790,#155791,#155792,#155793,#155794,#155795,#155796,
#155797,#155798,#155799,#155800,#155801,#155802,#155803,#155804,#155805,
#155806,#155807,#155808,#155809,#155810,#155811,#155812,#155813,#155814),
 .UNSPECIFIED.,.F.,.F.,(4,3,3,3,3,3,3,3,3,3,3,3,3,3,3,3,4),(2.72844949517765E-9,
0.0688980942246612,0.136773037531096,0.203343850945352,0.25,0.315004214893658,
0.379445255356854,0.443457188921027,0.507172269215425,0.570759851800854,
0.634335833368114,0.698186251307407,0.75,0.814712454999434,0.879894274521964,
0.946132007109019,1.),.UNSPECIFIED.);
#30051=B_SPLINE_CURVE_WITH_KNOTS('',3,(#155815,#155816,#155817,#155818,
#155819,#155820,#155821,#155822,#155823,#155824,#155825,#155826,#155827,
#155828,#155829,#155830,#155831,#155832,#155833,#155834,#155835,#155836,
#155837,#155838,#155839,#155840,#155841,#155842,#155843,#155844,#155845,
#155846,#155847,#155848,#155849,#155850,#155851,#155852,#155853,#155854,
#155855,#155856,#155857,#155858,#155859,#155860,#155861,#155862,#155863),
 .UNSPECIFIED.,.F.,.F.,(4,3,3,3,3,3,3,3,3,3,3,3,3,3,3,3,4),(0.,0.0692784102920228,
0.14120044859868,0.219196668058418,0.25,0.324115642155737,0.40008119894174,
0.478002093519741,0.5,0.577710157022752,0.654118301000089,0.727900984558949,
0.75,0.827504812018075,0.90052310253359,0.969341196485938,1.),
 .UNSPECIFIED.);
#30052=B_SPLINE_CURVE_WITH_KNOTS('',3,(#155870,#155871,#155872,#155873,
#155874,#155875,#155876,#155877,#155878,#155879,#155880,#155881,#155882,
#155883,#155884,#155885,#155886,#155887,#155888,#155889,#155890,#155891,
#155892,#155893,#155894,#155895,#155896,#155897,#155898,#155899,#155900,
#155901,#155902,#155903,#155904,#155905,#155906,#155907,#155908,#155909,
#155910,#155911,#155912,#155913,#155914,#155915,#155916,#155917,#155918,
#155919,#155920,#155921,#155922,#155923,#155924,#155925,#155926,#155927,
#155928,#155929,#155930,#155931,#155932,#155933,#155934,#155935,#155936,
#155937,#155938,#155939),.UNSPECIFIED.,.F.,.F.,(4,3,3,3,3,3,3,3,3,3,3,3,
3,3,3,3,3,3,3,3,3,3,3,4),(1.30324300997627E-11,0.0505870658958078,0.100440299421859,
0.149328502274208,0.19966425113711,0.247432688679266,0.250000000000012,
0.293728580204281,0.337185021169438,0.37500000000001,0.416703010961095,
0.458351505480552,0.500000000000008,0.541602652045577,0.583301326022791,
0.625000000000006,0.668398095794137,0.712079215319331,0.750000000000004,
0.79783378980656,0.84837534235492,0.89760075028844,0.94880037514422,1.),
 .UNSPECIFIED.);
#30053=B_SPLINE_CURVE_WITH_KNOTS('',3,(#155981,#155982,#155983,#155984,
#155985,#155986,#155987,#155988,#155989,#155990,#155991,#155992,#155993,
#155994,#155995,#155996,#155997,#155998,#155999,#156000,#156001,#156002,
#156003,#156004,#156005,#156006,#156007,#156008,#156009,#156010,#156011,
#156012,#156013,#156014),.UNSPECIFIED.,.F.,.F.,(4,2,2,1,1,1,2,2,2,2,2,1,
2,2,2,2,2,2,4),(0.,0.125000000000211,0.187500000000305,0.218750000000348,
0.234375000000365,0.242187500000373,0.246093750000373,0.250000000000373,
0.375000000000463,0.437500000000502,0.468750000000521,0.484375000000531,
0.492187500000526,0.50000000000052,0.62500000000035,0.687500000000268,0.718750000000221,
0.750000000000175,1.),.UNSPECIFIED.);
#30054=B_SPLINE_CURVE_WITH_KNOTS('',3,(#156015,#156016,#156017,#156018,
#156019,#156020,#156021,#156022,#156023,#156024),.UNSPECIFIED.,.F.,.F.,
(4,2,2,2,4),(2.13390469791841E-7,0.25,0.5,0.75,1.),.UNSPECIFIED.);
#30055=B_SPLINE_CURVE_WITH_KNOTS('',3,(#156049,#156050,#156051,#156052,
#156053,#156054,#156055,#156056,#156057,#156058,#156059,#156060,#156061),
 .UNSPECIFIED.,.F.,.F.,(4,3,3,3,4),(0.,0.266292368485203,0.529417506706766,
0.787742675205748,1.),.UNSPECIFIED.);
#30056=B_SPLINE_CURVE_WITH_KNOTS('',3,(#156063,#156064,#156065,#156066,
#156067,#156068,#156069,#156070,#156071,#156072,#156073,#156074,#156075,
#156076,#156077,#156078,#156079,#156080,#156081,#156082,#156083,#156084,
#156085,#156086,#156087,#156088,#156089,#156090,#156091,#156092,#156093,
#156094,#156095,#156096,#156097,#156098,#156099),.UNSPECIFIED.,.F.,.F.,
(4,3,3,3,3,3,3,3,3,3,3,3,4),(3.31179824555737E-10,0.017425231587708,0.0982830680925832,
0.125,0.188631792544538,0.288498005434872,0.398901768809661,0.521077852077812,
0.657045747770235,0.749999999999999,0.808620188251583,0.981759508105347,
1.),.UNSPECIFIED.);
#30057=B_SPLINE_CURVE_WITH_KNOTS('',3,(#156156,#156157,#156158,#156159),
 .UNSPECIFIED.,.F.,.F.,(4,4),(0.,1.),.UNSPECIFIED.);
#30058=B_SPLINE_CURVE_WITH_KNOTS('',3,(#156252,#156253,#156254,#156255,
#156256,#156257,#156258),.UNSPECIFIED.,.F.,.F.,(4,3,4),(2.76766290252202E-14,
0.394366854122773,1.),.UNSPECIFIED.);
#30059=B_SPLINE_CURVE_WITH_KNOTS('',3,(#156455,#156456,#156457,#156458,
#156459,#156460,#156461,#156462,#156463,#156464,#156465,#156466,#156467,
#156468,#156469,#156470,#156471,#156472,#156473,#156474,#156475,#156476,
#156477,#156478,#156479,#156480,#156481,#156482,#156483,#156484,#156485,
#156486,#156487,#156488,#156489,#156490,#156491,#156492,#156493,#156494,
#156495,#156496,#156497,#156498,#156499,#156500,#156501,#156502,#156503,
#156504,#156505,#156506,#156507,#156508,#156509,#156510,#156511,#156512,
#156513,#156514,#156515,#156516,#156517,#156518,#156519,#156520,#156521,
#156522,#156523,#156524,#156525,#156526,#156527,#156528,#156529,#156530,
#156531,#156532,#156533,#156534,#156535,#156536,#156537,#156538,#156539,
#156540,#156541,#156542,#156543,#156544,#156545,#156546,#156547,#156548,
#156549,#156550,#156551,#156552,#156553,#156554,#156555,#156556,#156557,
#156558,#156559,#156560,#156561,#156562,#156563,#156564,#156565,#156566,
#156567,#156568,#156569,#156570,#156571,#156572,#156573,#156574,#156575,
#156576,#156577,#156578,#156579,#156580,#156581,#156582,#156583,#156584,
#156585,#156586,#156587,#156588,#156589,#156590,#156591,#156592,#156593,
#156594,#156595,#156596,#156597,#156598,#156599,#156600,#156601,#156602,
#156603,#156604,#156605,#156606,#156607,#156608,#156609,#156610,#156611,
#156612,#156613,#156614,#156615,#156616,#156617,#156618,#156619,#156620,
#156621,#156622,#156623,#156624,#156625,#156626,#156627,#156628,#156629,
#156630,#156631,#156632,#156633,#156634,#156635,#156636,#156637,#156638,
#156639,#156640,#156641,#156642,#156643,#156644,#156645,#156646,#156647,
#156648,#156649,#156650,#156651,#156652,#156653,#156654,#156655,#156656,
#156657,#156658,#156659,#156660,#156661,#156662,#156663,#156664,#156665,
#156666,#156667,#156668,#156669,#156670,#156671,#156672,#156673,#156674,
#156675,#156676,#156677,#156678,#156679,#156680),.UNSPECIFIED.,.F.,.F.,
(4,3,3,3,3,3,3,3,3,3,3,3,3,3,3,3,3,3,3,3,3,3,3,3,3,3,3,3,3,3,3,3,3,3,3,
3,3,3,3,3,3,3,3,3,3,3,3,3,3,3,3,3,3,3,3,3,3,3,3,3,3,3,3,3,3,3,3,3,3,3,3,
3,3,3,3,4),(7.6013246015319E-11,0.0041559545228748,0.0210327898696483,0.0364291191706356,
0.0506222225081979,0.0518254484716229,0.062500000000003,0.0768035721053361,
0.0901372856082214,0.0937500000000051,0.0957761658748245,0.109375000000006,
0.117187500000006,0.121621389086509,0.125000000000006,0.138007198100994,
0.157743784493814,0.17744665752372,0.183453626090955,0.187500000000005,
0.211871023920911,0.218750000000005,0.229271298665007,0.234375000000004,
0.244589973646335,0.250000000000004,0.275239681532887,0.308690342494038,
0.322549049282618,0.357856894736005,0.368021252616143,0.375000000000001,
0.412158293166225,0.4375,0.456105693290628,0.468749999999999,0.484374999999998,
0.494801092711084,0.499999999999998,0.500025444460262,0.535118723365545,
0.543900825062066,0.585389277369181,0.588656357587658,0.624999999999995,
0.633432881746038,0.67375366506979,0.678858288706035,0.687499999999994,
0.718749999999993,0.725429350075826,0.734374999999993,0.742187499999993,
0.748453902845257,0.749999999999992,0.770125508965917,0.793523145696441,
0.812499999999992,0.814944956455603,0.834716949094254,0.843749999999992,
0.859374999999993,0.860947350563149,0.867187499999993,0.872125445495224,
0.874999999999993,0.891067994006378,0.90431467626986,0.918228777029266,
0.933515770458162,0.94866558411337,0.962510547721232,0.977069250318923,
0.992781062457308,0.996004191295995,0.999999999923944),.UNSPECIFIED.);
#30060=B_SPLINE_CURVE_WITH_KNOTS('',3,(#156772,#156773,#156774,#156775,
#156776,#156777,#156778,#156779,#156780,#156781,#156782,#156783,#156784,
#156785,#156786,#156787,#156788,#156789,#156790,#156791,#156792,#156793,
#156794,#156795,#156796,#156797,#156798,#156799,#156800,#156801),
 .UNSPECIFIED.,.F.,.F.,(4,1,2,2,2,2,2,2,2,2,2,2,1,2,2,4),(0.,0.0624999999999996,
0.0937499999999994,0.124999999999999,0.187499999999999,0.249999999999998,
0.374999999999997,0.499999999999997,0.562499999999996,0.624999999999996,
0.656249999999996,0.687499999999996,0.718749999999995,0.734374999999995,
0.749999999999995,1.),.UNSPECIFIED.);
#30061=B_SPLINE_CURVE_WITH_KNOTS('',3,(#156802,#156803,#156804,#156805),
 .UNSPECIFIED.,.F.,.F.,(4,4),(0.,1.),.UNSPECIFIED.);
#30062=B_SPLINE_CURVE_WITH_KNOTS('',3,(#156867,#156868,#156869,#156870,
#156871,#156872,#156873,#156874,#156875,#156876,#156877,#156878,#156879,
#156880,#156881,#156882,#156883,#156884,#156885,#156886,#156887,#156888,
#156889,#156890,#156891,#156892,#156893,#156894,#156895,#156896,#156897,
#156898,#156899,#156900,#156901,#156902,#156903,#156904,#156905,#156906,
#156907,#156908,#156909,#156910,#156911,#156912,#156913,#156914,#156915,
#156916,#156917,#156918,#156919,#156920,#156921,#156922,#156923,#156924,
#156925,#156926,#156927,#156928,#156929,#156930,#156931,#156932,#156933,
#156934,#156935,#156936,#156937,#156938,#156939,#156940,#156941,#156942,
#156943,#156944,#156945,#156946,#156947,#156948,#156949,#156950,#156951,
#156952,#156953,#156954,#156955,#156956,#156957,#156958,#156959,#156960,
#156961,#156962,#156963,#156964,#156965,#156966,#156967,#156968,#156969,
#156970,#156971,#156972,#156973,#156974,#156975,#156976,#156977,#156978,
#156979,#156980,#156981,#156982,#156983,#156984,#156985,#156986,#156987,
#156988,#156989,#156990,#156991,#156992,#156993,#156994,#156995,#156996),
 .UNSPECIFIED.,.F.,.F.,(4,3,3,3,3,3,3,3,3,3,3,3,3,3,3,3,3,3,3,3,3,3,3,3,
3,3,3,3,3,3,3,3,3,3,3,3,3,3,3,3,3,3,3,4),(0.,0.0222450806380213,0.0461572035151902,
0.073857491338037,0.107011041434932,0.125000000000011,0.136894536412116,
0.165629046527801,0.187500000000016,0.21875000000002,0.234375000000022,
0.248046875000024,0.249023437500024,0.250000000000024,0.276355845277275,
0.306209016223028,0.312500000000028,0.315840428150021,0.343618932232895,
0.371772527297605,0.375000000000032,0.406250000000034,0.429246372797829,
0.437500000000037,0.468750000000039,0.48437500000004,0.490901035393806,
0.492187500000041,0.500000000000042,0.532608092654646,0.567801163203751,
0.607335064867353,0.625000000000031,0.651439700206761,0.690432671400696,
0.727656080590827,0.750000000000021,0.799191181786869,0.817962618702426,
0.863110957751424,0.907571031864983,0.950396133988827,0.983659176247363,
0.999999999636422),.UNSPECIFIED.);
#30063=B_SPLINE_CURVE_WITH_KNOTS('',3,(#157001,#157002,#157003,#157004,
#157005,#157006,#157007,#157008,#157009,#157010,#157011,#157012,#157013,
#157014,#157015,#157016,#157017,#157018,#157019,#157020,#157021,#157022,
#157023,#157024,#157025,#157026,#157027),.UNSPECIFIED.,.F.,.F.,(4,1,1,2,
2,2,1,1,1,2,2,1,1,1,1,2,2,4),(3.14323848108535E-9,0.125000000000001,0.187500000000002,
0.218750000000002,0.250000000000002,0.375000000000001,0.4375,0.46875,0.484374999999999,
0.496093749999996,0.499999999999995,0.624999999999936,0.687499999999908,
0.718749999999894,0.734374999999886,0.748046874999877,0.749999999999876,
1.),.UNSPECIFIED.);
#30064=B_SPLINE_CURVE_WITH_KNOTS('',3,(#157051,#157052,#157053,#157054,
#157055,#157056,#157057,#157058,#157059,#157060,#157061,#157062,#157063,
#157064),.UNSPECIFIED.,.F.,.F.,(4,2,2,2,2,2,4),(0.,0.25,0.499999999999999,
0.624999999999999,0.75,0.875,1.),.UNSPECIFIED.);
#30065=B_SPLINE_CURVE_WITH_KNOTS('',3,(#157255,#157256,#157257,#157258,
#157259,#157260,#157261,#157262,#157263,#157264,#157265,#157266,#157267,
#157268,#157269,#157270,#157271,#157272,#157273,#157274,#157275,#157276,
#157277,#157278,#157279,#157280,#157281,#157282,#157283,#157284,#157285,
#157286,#157287,#157288,#157289,#157290,#157291),.UNSPECIFIED.,.F.,.F.,
(4,3,3,3,3,3,3,3,3,3,3,3,4),(0.,0.0396954288592127,0.184386182462915,0.194668024552279,
0.347219950006161,0.368101049680069,0.499999999999998,0.558416630619174,
0.724544290911746,0.76399353681739,0.924890186709707,0.981597205952527,
0.999999988137177),.UNSPECIFIED.);
#30066=B_SPLINE_CURVE_WITH_KNOTS('',3,(#157292,#157293,#157294,#157295,
#157296,#157297,#157298,#157299,#157300,#157301,#157302,#157303,#157304,
#157305),.UNSPECIFIED.,.F.,.F.,(4,2,2,2,2,2,4),(3.42050715226368E-6,0.0559041406044768,
0.110821873002056,0.16870681326424,0.225445105585076,0.2820690083687,0.337327565891503),
 .UNSPECIFIED.);
#30067=B_SPLINE_CURVE_WITH_KNOTS('',3,(#157363,#157364,#157365,#157366,
#157367,#157368),.UNSPECIFIED.,.F.,.F.,(4,2,4),(3.41822380810718E-6,0.143396991606946,
0.286369799377383),.UNSPECIFIED.);
#30068=B_SPLINE_CURVE_WITH_KNOTS('',3,(#157386,#157387,#157388,#157389,
#157390,#157391),.UNSPECIFIED.,.F.,.F.,(4,2,4),(4.9161935946595E-6,0.0292090733184409,
0.0584199189037688),.UNSPECIFIED.);
#30069=B_SPLINE_CURVE_WITH_KNOTS('',3,(#157449,#157450,#157451,#157452,
#157453),.UNSPECIFIED.,.F.,.F.,(4,1,4),(0.,0.5,0.999995825079256),
 .UNSPECIFIED.);
#30070=B_SPLINE_CURVE_WITH_KNOTS('',3,(#157496,#157497,#157498,#157499,
#157500,#157501,#157502,#157503,#157504,#157505,#157506,#157507,#157508,
#157509,#157510,#157511,#157512,#157513,#157514,#157515,#157516,#157517,
#157518,#157519,#157520,#157521,#157522,#157523,#157524,#157525,#157526,
#157527,#157528,#157529,#157530,#157531,#157532,#157533,#157534,#157535,
#157536,#157537,#157538,#157539,#157540,#157541,#157542,#157543,#157544,
#157545,#157546,#157547,#157548,#157549,#157550,#157551,#157552,#157553,
#157554,#157555,#157556,#157557,#157558,#157559),.UNSPECIFIED.,.F.,.F.,
(4,3,3,3,3,3,3,3,3,3,3,3,3,3,3,3,3,3,3,3,3,4),(0.0475883983781192,0.0504715149112503,
0.101359766783617,0.153027051352179,0.205253844737498,0.229513928442054,
0.249999999999997,0.3270059293996,0.374999999999996,0.412568101857693,0.456284050928844,
0.499999999999995,0.568529833373717,0.596947337798161,0.668057214031891,
0.735905642822662,0.749999999999998,0.78220040594856,0.848341524055653,
0.914724761179046,0.969216113718377,1.),.UNSPECIFIED.);
#30071=B_SPLINE_CURVE_WITH_KNOTS('',3,(#157560,#157561,#157562,#157563,
#157564,#157565,#157566,#157567,#157568,#157569,#157570,#157571,#157572,
#157573,#157574,#157575,#157576,#157577,#157578,#157579,#157580,#157581,
#157582,#157583,#157584,#157585,#157586,#157587,#157588,#157589,#157590,
#157591,#157592,#157593,#157594,#157595,#157596,#157597,#157598,#157599,
#157600,#157601,#157602,#157603,#157604,#157605,#157606,#157607,#157608,
#157609,#157610,#157611,#157612,#157613,#157614,#157615,#157616,#157617,
#157618,#157619,#157620),.UNSPECIFIED.,.F.,.F.,(4,3,3,3,3,3,3,3,3,3,3,3,
3,3,3,3,3,3,3,3,4),(3.7300084670044E-6,0.0744120387739684,0.125000000000108,
0.18750000000019,0.218750000000223,0.233569723016874,0.234375000000221,
0.246852766807326,0.250000000000218,0.500000000000137,0.625000000000087,
0.687500000000034,0.718750000000016,0.742152599453903,0.749999999999997,
0.804729863476949,0.859609535575322,0.874999999999999,0.928349847165128,
0.981841124851018,0.999998027188981),.UNSPECIFIED.);
#30072=B_SPLINE_CURVE_WITH_KNOTS('',3,(#157748,#157749,#157750,#157751,
#157752,#157753,#157754,#157755,#157756,#157757,#157758,#157759,#157760,
#157761,#157762,#157763,#157764),.UNSPECIFIED.,.F.,.F.,(4,2,2,1,1,1,2,2,
2,4),(1.43410335955E-5,0.249999999999933,0.374999999999896,0.437499999999873,
0.468749999999867,0.484374999999859,0.492187499999856,0.499999999999853,
0.749999999999926,1.),.UNSPECIFIED.);
#30073=B_SPLINE_CURVE_WITH_KNOTS('',3,(#157799,#157800,#157801,#157802,
#157803,#157804,#157805,#157806,#157807,#157808),.UNSPECIFIED.,.F.,.F.,
(4,2,2,2,4),(9.6294942429E-6,0.25,0.5,0.75,1.),.UNSPECIFIED.);
#30074=B_SPLINE_CURVE_WITH_KNOTS('',3,(#157841,#157842,#157843,#157844,
#157845,#157846,#157847,#157848,#157849,#157850,#157851,#157852,#157853,
#157854,#157855,#157856,#157857,#157858,#157859,#157860,#157861,#157862,
#157863,#157864,#157865,#157866,#157867,#157868,#157869,#157870,#157871,
#157872,#157873,#157874,#157875,#157876,#157877,#157878,#157879,#157880,
#157881,#157882,#157883,#157884,#157885,#157886,#157887,#157888,#157889,
#157890,#157891,#157892,#157893,#157894,#157895,#157896,#157897,#157898,
#157899,#157900,#157901,#157902,#157903,#157904,#157905,#157906,#157907),
 .UNSPECIFIED.,.F.,.F.,(4,3,3,3,3,3,3,3,3,3,3,3,3,3,3,3,3,3,3,3,3,3,4),
(1.24011628705212E-10,0.0531053496019451,0.10437770154546,0.154727528060671,
0.203864455437261,0.25,0.297836570659254,0.345161045291314,0.392002186152137,
0.438626827965545,0.485141010125923,0.5,0.546606499906862,0.593402564378951,
0.64074134746124,0.688461599503242,0.736927113385546,0.75,0.799583122725084,
0.85071410427355,0.90277575624421,0.95662774238403,1.),.UNSPECIFIED.);
#30075=B_SPLINE_CURVE_WITH_KNOTS('',3,(#157957,#157958,#157959,#157960,
#157961,#157962,#157963,#157964,#157965,#157966,#157967,#157968,#157969,
#157970,#157971,#157972,#157973,#157974,#157975,#157976,#157977,#157978,
#157979,#157980,#157981,#157982,#157983,#157984,#157985,#157986,#157987,
#157988,#157989,#157990,#157991,#157992,#157993,#157994,#157995,#157996,
#157997,#157998,#157999,#158000,#158001,#158002,#158003,#158004,#158005,
#158006,#158007,#158008,#158009,#158010,#158011,#158012,#158013,#158014,
#158015,#158016,#158017,#158018,#158019,#158020,#158021,#158022,#158023),
 .UNSPECIFIED.,.F.,.F.,(4,3,3,3,3,3,3,3,3,3,3,3,3,3,3,3,3,3,3,3,3,3,4),
(1.19754065422301E-14,0.0537123221293526,0.105496107116609,0.156304258830716,
0.20582389888184,0.25,0.298149632596059,0.34572619551662,0.392732615136169,
0.439472860332929,0.486031305273164,0.5,0.546563122917741,0.593256574146164,
0.640406002773063,0.687884574046229,0.736036975820931,0.75,0.799190988175816,
0.849837660146647,0.901356920133292,0.954590545665251,1.),.UNSPECIFIED.);
#30076=B_SPLINE_CURVE_WITH_KNOTS('',3,(#158053,#158054,#158055,#158056,
#158057,#158058),.UNSPECIFIED.,.F.,.F.,(4,2,4),(0.,0.5,1.),
 .UNSPECIFIED.);
#30077=B_SPLINE_CURVE_WITH_KNOTS('',3,(#158152,#158153,#158154,#158155,
#158156,#158157,#158158,#158159,#158160,#158161,#158162,#158163,#158164,
#158165,#158166,#158167,#158168,#158169,#158170,#158171,#158172,#158173,
#158174,#158175,#158176,#158177,#158178,#158179,#158180,#158181,#158182,
#158183,#158184,#158185,#158186,#158187,#158188,#158189,#158190,#158191,
#158192,#158193,#158194,#158195,#158196,#158197,#158198,#158199,#158200),
 .UNSPECIFIED.,.F.,.F.,(4,3,3,3,3,3,3,3,3,3,3,3,3,3,3,3,4),(0.,0.0693090958433355,
0.141292481527221,0.219438370094957,0.25,0.324257641112822,0.400369388793943,
0.47840899005484,0.5,0.577797592734866,0.654240606146742,0.728007698508539,
0.75,0.827331791071793,0.900155287073229,0.968761945896699,1.),
 .UNSPECIFIED.);
#30078=B_SPLINE_CURVE_WITH_KNOTS('',3,(#158211,#158212,#158213,#158214,
#158215,#158216,#158217,#158218,#158219,#158220,#158221,#158222,#158223,
#158224,#158225,#158226,#158227,#158228,#158229,#158230,#158231,#158232,
#158233,#158234,#158235,#158236,#158237,#158238,#158239,#158240,#158241,
#158242,#158243,#158244,#158245,#158246,#158247,#158248,#158249,#158250),
 .UNSPECIFIED.,.F.,.F.,(4,3,3,3,3,3,3,3,3,3,3,3,3,4),(2.84045680779053E-7,
0.0708895786428518,0.143736697789595,0.219098426622223,0.25,0.341086442232413,
0.42712793766834,0.5,0.591704542904046,0.681910213301737,0.75,0.837802729425135,
0.925712313270966,1.),.UNSPECIFIED.);
#30079=B_SPLINE_CURVE_WITH_KNOTS('',3,(#158254,#158255,#158256,#158257,
#158258,#158259,#158260,#158261,#158262,#158263,#158264,#158265,#158266,
#158267,#158268,#158269,#158270,#158271,#158272,#158273,#158274,#158275,
#158276,#158277,#158278,#158279,#158280,#158281,#158282,#158283,#158284,
#158285,#158286,#158287,#158288,#158289,#158290,#158291,#158292,#158293),
 .UNSPECIFIED.,.F.,.F.,(4,3,3,3,3,3,3,3,3,3,3,3,3,4),(1.58810254343732E-6,
0.0878641086721794,0.175637059567264,0.25,0.340009209441351,0.431407081049676,
0.5,0.585248315379607,0.675577235252377,0.75,0.82515554011605,0.898549327885159,
0.968977560346211,0.999999710276602),.UNSPECIFIED.);
#30080=B_SPLINE_CURVE_WITH_KNOTS('',3,(#158298,#158299,#158300,#158301,
#158302,#158303,#158304,#158305,#158306,#158307,#158308,#158309,#158310,
#158311,#158312,#158313,#158314,#158315,#158316),.UNSPECIFIED.,.F.,.F.,
(4,3,3,3,3,3,4),(0.,0.181023284717183,0.362342525582545,0.544428388735039,
0.727084718844238,0.910885371459506,1.),.UNSPECIFIED.);
#30081=B_SPLINE_CURVE_WITH_KNOTS('',3,(#158318,#158319,#158320,#158321,
#158322,#158323,#158324,#158325,#158326,#158327,#158328,#158329,#158330,
#158331,#158332,#158333,#158334,#158335,#158336,#158337,#158338,#158339,
#158340,#158341,#158342,#158343,#158344,#158345,#158346,#158347,#158348,
#158349,#158350,#158351,#158352,#158353,#158354,#158355,#158356,#158357,
#158358,#158359,#158360,#158361,#158362,#158363,#158364,#158365,#158366,
#158367,#158368,#158369,#158370,#158371,#158372,#158373,#158374,#158375,
#158376,#158377,#158378,#158379,#158380,#158381,#158382,#158383,#158384,
#158385,#158386,#158387,#158388,#158389,#158390,#158391,#158392,#158393,
#158394,#158395,#158396,#158397,#158398,#158399,#158400,#158401,#158402,
#158403,#158404,#158405,#158406,#158407,#158408,#158409,#158410,#158411,
#158412,#158413,#158414,#158415,#158416,#158417,#158418,#158419,#158420,
#158421,#158422,#158423,#158424,#158425,#158426,#158427),.UNSPECIFIED.,
 .F.,.F.,(4,2,2,2,2,2,1,2,2,2,2,2,2,1,2,2,2,2,1,2,2,2,2,1,1,2,2,2,2,2,1,
2,2,2,2,1,2,2,2,1,1,1,2,2,2,2,1,1,1,1,2,2,2,2,2,2,2,2,1,1,2,2,4),(0.,0.0625000000001419,
0.0937500000002126,0.125000000000283,0.187500000000425,0.21875000000049,
0.234375000000523,0.24218750000054,0.250000000000556,0.281250000000613,
0.296875000000641,0.312500000000669,0.343750000000725,0.359375000000754,
0.367187500000772,0.375000000000791,0.406250000000858,0.421875000000896,
0.429687500000909,0.43359375000091,0.437500000000912,0.46875000000088,0.484375000000864,
0.492187500000856,0.496093750000852,0.498046875000846,0.500000000000841,
0.531250000000882,0.546875000000903,0.550781250000911,0.554687500000918,
0.56250000000094,0.578125000000991,0.585937500001011,0.587890625001022,
0.589843750001033,0.593750000001075,0.60937500000126,0.617187500001356,
0.621093750001404,0.623046875001428,0.62402343750144,0.624511718751444,
0.625000000001447,0.687500000000793,0.718750000000462,0.734375000000297,
0.742187500000214,0.746093750000173,0.748046875000155,0.749023437500146,
0.750000000000137,0.781250000000108,0.796875000000098,0.804687500000092,
0.812500000000087,0.843750000000052,0.859375000000034,0.867187500000022,
0.87109375000002,0.873046875000015,0.87500000000001,1.),.UNSPECIFIED.);
#30082=B_SPLINE_CURVE_WITH_KNOTS('',3,(#158428,#158429,#158430,#158431,
#158432,#158433,#158434,#158435,#158436,#158437,#158438,#158439,#158440),
 .UNSPECIFIED.,.F.,.F.,(4,3,3,3,4),(2.68456744279971E-6,0.320124870241623,
0.652764750436627,0.752696531034302,0.999999999255413),.UNSPECIFIED.);
#30083=B_SPLINE_CURVE_WITH_KNOTS('',3,(#158444,#158445,#158446,#158447,
#158448,#158449,#158450,#158451,#158452,#158453,#158454,#158455,#158456,
#158457,#158458,#158459,#158460,#158461),.UNSPECIFIED.,.F.,.F.,(4,2,2,2,
2,2,2,2,4),(0.51322060328706,0.641524368772129,0.769828134257199,0.898134670047327,
1.02644120583745,1.15474774162758,1.28305427741771,1.41135804290278,1.53966180838785),
 .UNSPECIFIED.);
#30084=B_SPLINE_CURVE_WITH_KNOTS('',3,(#158469,#158470,#158471,#158472,
#158473,#158474,#158475,#158476,#158477,#158478,#158479,#158480,#158481,
#158482,#158483,#158484,#158485,#158486,#158487),.UNSPECIFIED.,.F.,.F.,
(4,2,2,2,3,2,2,2,4),(1.53966180838785,1.66796557393431,1.79626933948077,
1.92457587533228,2.0528824111838,2.18118894703532,2.30949548288683,2.43779924843329,
2.56610301397975),.UNSPECIFIED.);
#30085=B_SPLINE_CURVE_WITH_KNOTS('',3,(#158489,#158490,#158491,#158492,
#158493,#158494,#158495,#158496,#158497,#158498),.UNSPECIFIED.,.F.,.F.,
(4,3,3,4),(0.,0.403447226841839,0.793186801599581,1.),.UNSPECIFIED.);
#30086=B_SPLINE_CURVE_WITH_KNOTS('',3,(#158500,#158501,#158502,#158503,
#158504,#158505,#158506,#158507,#158508,#158509,#158510,#158511,#158512,
#158513,#158514,#158515,#158516,#158517,#158518,#158519,#158520,#158521,
#158522,#158523,#158524,#158525,#158526,#158527,#158528,#158529,#158530,
#158531,#158532,#158533,#158534,#158535,#158536,#158537,#158538,#158539,
#158540,#158541,#158542,#158543,#158544,#158545,#158546,#158547,#158548,
#158549,#158550,#158551,#158552,#158553,#158554,#158555,#158556,#158557,
#158558,#158559,#158560,#158561,#158562,#158563,#158564,#158565,#158566,
#158567,#158568,#158569,#158570,#158571,#158572,#158573,#158574,#158575,
#158576,#158577,#158578,#158579,#158580,#158581,#158582,#158583,#158584,
#158585,#158586,#158587,#158588,#158589,#158590,#158591,#158592,#158593,
#158594,#158595,#158596,#158597,#158598,#158599,#158600,#158601,#158602,
#158603,#158604,#158605,#158606,#158607,#158608),.UNSPECIFIED.,.F.,.F.,
(4,3,3,3,3,3,3,3,3,3,3,3,3,3,3,3,3,3,3,3,3,3,3,3,3,3,3,3,3,3,3,3,3,3,3,
3,4),(0.,0.0624999999999996,0.0937499999999992,0.109374999999997,0.123111553381916,
0.124999999999994,0.187499999999983,0.218749999999978,0.234374999999976,
0.242187499999971,0.246093749999972,0.248046874999973,0.249999999999973,
0.297621066886665,0.346682799104137,0.374999999999908,0.424324169177522,
0.437499999999879,0.468749999999865,0.484374999999863,0.492187499999863,
0.496093749999862,0.499999999999862,0.556713517041172,0.562499999999931,
0.612693929493909,0.624999999999999,0.674000499948216,0.687500000000068,
0.718750000000097,0.734375000000107,0.742187500000111,0.750000000000116,
0.815478788185251,0.878658773482917,0.939329386741458,1.),.UNSPECIFIED.);
#30087=B_SPLINE_CURVE_WITH_KNOTS('',3,(#158609,#158610,#158611,#158612,
#158613,#158614,#158615,#158616,#158617,#158618,#158619,#158620,#158621,
#158622,#158623,#158624,#158625,#158626,#158627),.UNSPECIFIED.,.F.,.F.,
(4,3,3,3,3,3,4),(9.58549878410965E-9,0.18399938603316,0.367063643664044,
0.549112471565754,0.730714957127349,0.911898041126138,1.),.UNSPECIFIED.);
#30088=B_SPLINE_CURVE_WITH_KNOTS('',3,(#158631,#158632,#158633,#158634,
#158635,#158636,#158637,#158638,#158639,#158640,#158641,#158642,#158643,
#158644,#158645,#158646),.UNSPECIFIED.,.F.,.F.,(4,3,3,3,3,4),(0.,0.232374498505923,
0.466846360420569,0.702548243138269,0.940039941077079,1.),.UNSPECIFIED.);
#30089=B_SPLINE_CURVE_WITH_KNOTS('',3,(#158648,#158649,#158650,#158651,
#158652,#158653,#158654,#158655,#158656,#158657,#158658,#158659,#158660,
#158661,#158662,#158663),.UNSPECIFIED.,.F.,.F.,(4,3,3,3,3,4),(0.,0.25,0.485488277204038,
0.719726015794557,0.952254864143456,1.),.UNSPECIFIED.);
#30090=B_SPLINE_CURVE_WITH_KNOTS('',3,(#158667,#158668,#158669,#158670,
#158671,#158672,#158673,#158674,#158675,#158676,#158677,#158678,#158679,
#158680),.UNSPECIFIED.,.F.,.F.,(4,2,2,1,1,1,1,2,4),(0.,0.232087643384168,
0.348131465076251,0.406153375922293,0.435164331345314,0.449669809056824,
0.456922547912579,0.460548917340457,0.464175286768335),.UNSPECIFIED.);
#30091=B_SPLINE_CURVE_WITH_KNOTS('',3,(#158682,#158683,#158684,#158685,
#158686,#158687,#158688,#158689,#158690,#158691,#158692,#158693,#158694,
#158695,#158696,#158697,#158698,#158699,#158700,#158701,#158702,#158703,
#158704,#158705,#158706,#158707,#158708,#158709),.UNSPECIFIED.,.F.,.F.,
(4,3,3,3,3,3,3,3,3,4),(0.464175286768335,0.507402740532681,0.575182101073047,
0.642961461613413,0.711443014313486,0.779924567013559,0.846485208441788,
0.909070904439081,0.97458738612463,1.),.UNSPECIFIED.);
#30092=B_SPLINE_CURVE_WITH_KNOTS('',3,(#158720,#158721,#158722,#158723,
#158724,#158725,#158726,#158727,#158728,#158729,#158730,#158731,#158732,
#158733,#158734,#158735,#158736,#158737),.UNSPECIFIED.,.F.,.F.,(4,2,2,2,
2,2,2,2,4),(0.51336686968484,0.64170672987966,0.77004659007448,0.89839016472208,
1.02673373936968,1.15507731401728,1.28342088866488,1.4117607488597,1.54010060905452),
 .UNSPECIFIED.);
#30093=B_SPLINE_CURVE_WITH_KNOTS('',3,(#158743,#158744,#158745,#158746,
#158747,#158748,#158749,#158750,#158751,#158752,#158753,#158754,#158755,
#158756,#158757,#158758,#158759,#158760,#158761),.UNSPECIFIED.,.F.,.F.,
(4,2,2,2,3,2,2,2,4),(-0.513366869684842,-0.385027009490022,-0.256687149295202,
-0.128343574647601,0.,0.1283435746476,0.256687149295201,0.38502700949002,
0.51336686968484),.UNSPECIFIED.);
#30094=B_SPLINE_CURVE_WITH_KNOTS('',3,(#158778,#158779,#158780,#158781,
#158782,#158783,#158784,#158785,#158786,#158787,#158788,#158789,#158790,
#158791,#158792,#158793,#158794,#158795,#158796,#158797,#158798,#158799,
#158800,#158801,#158802,#158803,#158804,#158805),.UNSPECIFIED.,.F.,.F.,
(4,3,3,3,3,3,3,3,3,4),(0.,0.0692777929336496,0.139135815966921,0.209342132953863,
0.25,0.334195898995659,0.41802748141099,0.5,0.583268776058614,0.611956694219027),
 .UNSPECIFIED.);
#30095=B_SPLINE_CURVE_WITH_KNOTS('',3,(#158807,#158808,#158809,#158810,
#158811),.UNSPECIFIED.,.F.,.F.,(4,1,4),(0.61195669421903,0.75,1.),
 .UNSPECIFIED.);
#30096=B_SPLINE_CURVE_WITH_KNOTS('',3,(#158813,#158814,#158815,#158816,
#158817,#158818,#158819,#158820,#158821,#158822,#158823,#158824,#158825,
#158826,#158827,#158828,#158829,#158830,#158831,#158832,#158833,#158834,
#158835,#158836,#158837,#158838,#158839,#158840,#158841,#158842,#158843,
#158844,#158845,#158846,#158847,#158848,#158849,#158850,#158851,#158852,
#158853,#158854,#158855,#158856,#158857,#158858,#158859,#158860,#158861),
 .UNSPECIFIED.,.F.,.F.,(4,3,3,3,3,3,3,3,3,3,3,3,3,3,3,3,4),(3.20680933356649E-11,
0.0721626588620015,0.144249523483548,0.216264815990394,0.25,0.3125,0.37457156013175,
0.437285780065875,0.5,0.566086889009772,0.632312810085566,0.698659995783495,
0.75,0.816474333249973,0.883044627621702,0.949906691452303,0.999998850808007),
 .UNSPECIFIED.);
#30097=B_SPLINE_CURVE_WITH_KNOTS('',3,(#158868,#158869,#158870,#158871,
#158872),.UNSPECIFIED.,.F.,.F.,(4,1,4),(0.,0.25,0.389921870034298),
 .UNSPECIFIED.);
#30098=B_SPLINE_CURVE_WITH_KNOTS('',3,(#158874,#158875,#158876,#158877,
#158878,#158879,#158880,#158881,#158882,#158883,#158884,#158885,#158886,
#158887,#158888,#158889,#158890,#158891,#158892,#158893,#158894,#158895,
#158896,#158897,#158898,#158899,#158900,#158901),.UNSPECIFIED.,.F.,.F.,
(4,3,3,3,3,3,3,3,3,4),(0.389921870034299,0.47318252991096,0.5,0.583741991428506,
0.667878721710084,0.75,0.820206723618715,0.890218982451227,0.959387708460516,
1.),.UNSPECIFIED.);
#30099=B_SPLINE_CURVE_WITH_KNOTS('',3,(#158906,#158907,#158908,#158909,
#158910,#158911,#158912,#158913,#158914,#158915,#158916,#158917,#158918,
#158919,#158920,#158921,#158922,#158923,#158924,#158925,#158926,#158927,
#158928,#158929,#158930,#158931,#158932,#158933,#158934,#158935,#158936,
#158937,#158938,#158939,#158940,#158941,#158942,#158943,#158944,#158945,
#158946,#158947,#158948,#158949,#158950,#158951,#158952,#158953,#158954,
#158955,#158956,#158957,#158958,#158959,#158960,#158961,#158962,#158963,
#158964,#158965,#158966,#158967,#158968,#158969,#158970,#158971,#158972,
#158973,#158974,#158975,#158976,#158977,#158978,#158979,#158980,#158981,
#158982,#158983,#158984,#158985,#158986,#158987,#158988,#158989,#158990,
#158991,#158992,#158993),.UNSPECIFIED.,.F.,.F.,(4,3,3,3,3,3,3,3,3,3,3,3,
3,3,3,3,3,3,3,3,3,3,3,3,3,3,3,3,3,4),(1.32079360702953E-6,0.0634845576880265,
0.125515787929973,0.187757893964395,0.249999999998816,0.307401094352583,
0.363909034203173,0.419246044651787,0.437499999997953,0.468749999997809,
0.484374999997749,0.492187499997707,0.496093749997697,0.499293107485499,
0.499999999997688,0.53960553479907,0.578426698983766,0.615841437993178,
0.652408482162967,0.687620805096765,0.718749999998711,0.734374999998786,
0.742609120743371,0.749999999998861,0.791313621232325,0.833775310097632,
0.87810969517575,0.923492227091124,0.970483197925126,0.999999999951529),
 .UNSPECIFIED.);
#30100=B_SPLINE_CURVE_WITH_KNOTS('',3,(#158997,#158998,#158999,#159000,
#159001,#159002,#159003,#159004,#159005,#159006,#159007,#159008,#159009,
#159010,#159011,#159012,#159013,#159014,#159015,#159016,#159017,#159018,
#159019,#159020,#159021,#159022,#159023,#159024),.UNSPECIFIED.,.F.,.F.,
(4,2,2,2,2,2,2,2,2,2,2,2,2,4),(2.81817193270301E-5,0.0404457711470591,0.0821080166266323,
0.110432701109432,0.148650946238688,0.169579357071198,0.211681646196492,
0.296346265170852,0.338302678525459,0.422553326948518,0.464657288078779,
0.549286472942467,0.61432552910643,0.676705893035455),.UNSPECIFIED.);
#30101=B_SPLINE_CURVE_WITH_KNOTS('',3,(#159028,#159029,#159030,#159031,
#159032,#159033,#159034,#159035,#159036,#159037,#159038,#159039,#159040,
#159041,#159042,#159043,#159044,#159045,#159046,#159047,#159048,#159049,
#159050,#159051,#159052,#159053,#159054,#159055),.UNSPECIFIED.,.F.,.F.,
(4,2,2,2,2,2,2,2,2,2,2,2,2,4),(2.89082885123981E-5,0.0404449424899443,0.0821047169019943,
0.110431583524439,0.148652542514045,0.169585165239432,0.211678148580102,
0.296322903616727,0.338268652222239,0.422497424572656,0.464590884909859,
0.549204383970884,0.614271515124411,0.676678486418186),.UNSPECIFIED.);
#30102=B_SPLINE_CURVE_WITH_KNOTS('',3,(#159178,#159179,#159180,#159181),
 .UNSPECIFIED.,.F.,.F.,(4,4),(6.8213951312265E-9,1.),.UNSPECIFIED.);
#30103=B_SPLINE_CURVE_WITH_KNOTS('',3,(#159182,#159183,#159184,#159185,
#159186,#159187,#159188,#159189,#159190,#159191,#159192,#159193,#159194,
#159195,#159196,#159197,#159198,#159199,#159200,#159201,#159202,#159203,
#159204,#159205,#159206,#159207,#159208,#159209,#159210,#159211,#159212,
#159213,#159214,#159215,#159216,#159217,#159218,#159219,#159220,#159221,
#159222,#159223,#159224,#159225,#159226,#159227,#159228,#159229,#159230,
#159231,#159232,#159233,#159234,#159235,#159236,#159237,#159238,#159239,
#159240,#159241,#159242,#159243,#159244,#159245,#159246,#159247,#159248,
#159249,#159250,#159251,#159252,#159253,#159254,#159255,#159256,#159257,
#159258,#159259,#159260,#159261,#159262,#159263,#159264,#159265,#159266,
#159267,#159268,#159269,#159270,#159271,#159272,#159273,#159274,#159275,
#159276,#159277,#159278),.UNSPECIFIED.,.F.,.F.,(4,3,3,3,3,3,3,3,3,3,3,3,
3,3,3,3,3,3,3,3,3,3,3,3,3,3,3,3,3,3,3,3,4),(1.50075895639123E-11,0.000238979584925606,
0.0558987779250573,0.0977547066978565,0.142061784128592,0.187141708528323,
0.20732602029247,0.249999999999667,0.299653723551624,0.335843648311373,
0.37499999999951,0.427633424273377,0.437499999999434,0.468749999999395,
0.484374999999356,0.492187499999339,0.496093749999349,0.499650467854497,
0.49999999999936,0.500176177799037,0.554344798352206,0.606121874922227,
0.61934335806653,0.670016874088742,0.719933839051705,0.742243911611287,
0.74999999999968,0.800995588371744,0.854431348938874,0.868854865545914,
0.922079159827303,0.977549834363125,1.),.UNSPECIFIED.);
#30104=B_SPLINE_CURVE_WITH_KNOTS('',3,(#159404,#159405,#159406,#159407,
#159408,#159409,#159410,#159411,#159412,#159413,#159414,#159415,#159416,
#159417,#159418,#159419,#159420,#159421,#159422,#159423),.UNSPECIFIED.,
 .F.,.F.,(4,2,2,2,2,2,2,2,2,4),(3.59015293165016E-5,0.104891984779917,0.190225981061743,
0.26444222512504,0.33832214678602,0.41214617480156,0.486142936498696,0.573670416532694,
0.630728791195145,0.686453015103136),.UNSPECIFIED.);
#30105=B_SPLINE_CURVE_WITH_KNOTS('',3,(#159488,#159489,#159490,#159491,
#159492,#159493,#159494,#159495,#159496,#159497,#159498,#159499,#159500,
#159501,#159502,#159503,#159504,#159505,#159506,#159507),.UNSPECIFIED.,
 .F.,.F.,(4,2,2,2,2,2,2,2,2,4),(3.6508494893667E-5,0.104892585500239,0.190226574989672,
0.264442813369599,0.338322729362654,0.412146751705904,0.486143507715768,
0.5736709810378,0.630729019146168,0.686453571241528),.UNSPECIFIED.);
#30106=B_SPLINE_CURVE_WITH_KNOTS('',3,(#159576,#159577,#159578,#159579,
#159580,#159581,#159582,#159583,#159584,#159585,#159586,#159587,#159588,
#159589,#159590,#159591,#159592,#159593,#159594,#159595,#159596,#159597,
#159598,#159599,#159600,#159601,#159602,#159603,#159604,#159605,#159606,
#159607,#159608,#159609,#159610,#159611,#159612,#159613,#159614,#159615,
#159616,#159617,#159618,#159619,#159620,#159621,#159622,#159623,#159624,
#159625,#159626,#159627,#159628,#159629,#159630,#159631,#159632,#159633,
#159634,#159635,#159636,#159637,#159638,#159639,#159640,#159641,#159642,
#159643,#159644,#159645,#159646,#159647,#159648,#159649,#159650,#159651,
#159652,#159653,#159654,#159655,#159656,#159657,#159658,#159659,#159660,
#159661,#159662,#159663,#159664,#159665,#159666,#159667,#159668,#159669,
#159670,#159671,#159672,#159673,#159674,#159675),.UNSPECIFIED.,.F.,.F.,
(4,3,3,3,3,3,3,3,3,3,3,3,3,3,3,3,3,3,3,3,3,3,3,3,3,3,3,3,3,3,3,3,3,4),(0.,
0.0557515009067887,0.109134396540876,0.131151604238023,0.184820483632369,
0.235915446823191,0.250000000000389,0.257780850626982,0.307754474945911,
0.358372863084605,0.375000000000583,0.380667131633151,0.432389024101429,
0.437500000000679,0.468750000000728,0.484375000000739,0.492187500000756,
0.496093750000777,0.499385919082227,0.49972917749395,0.500000000000798,
0.555330908565005,0.609768022337765,0.660505155979448,0.664205136110525,
0.713728196959825,0.750000000000399,0.792718751150899,0.837891574655351,
0.882239272625951,0.902271834341869,0.955075233491463,0.999761056440961,
0.999999999988578),.UNSPECIFIED.);
#30107=B_SPLINE_CURVE_WITH_KNOTS('',3,(#159679,#159680,#159681,#159682),
 .UNSPECIFIED.,.F.,.F.,(4,4),(0.,0.999999998785804),.UNSPECIFIED.);
#30108=B_SPLINE_CURVE_WITH_KNOTS('',3,(#159824,#159825,#159826,#159827,
#159828,#159829,#159830,#159831,#159832,#159833,#159834,#159835,#159836,
#159837,#159838,#159839,#159840,#159841,#159842,#159843,#159844,#159845),
 .UNSPECIFIED.,.F.,.F.,(4,3,3,3,3,3,3,4),(0.,0.0750543931589244,0.206343465886641,
0.353310648156244,0.51730486526382,0.695194909544737,0.877697846671489,
0.999999999887282),.UNSPECIFIED.);
#30109=B_SPLINE_CURVE_WITH_KNOTS('',3,(#159847,#159848,#159849,#159850,
#159851,#159852,#159853,#159854,#159855,#159856,#159857,#159858,#159859,
#159860,#159861,#159862,#159863,#159864,#159865,#159866,#159867,#159868),
 .UNSPECIFIED.,.F.,.F.,(4,3,3,3,3,3,3,4),(0.,0.127557126282854,0.310458518240933,
0.488256908441061,0.651827440567707,0.798268038187216,0.929115949337431,
1.),.UNSPECIFIED.);
#30110=B_SPLINE_CURVE_WITH_KNOTS('',3,(#159937,#159938,#159939,#159940,
#159941,#159942,#159943,#159944,#159945,#159946,#159947,#159948,#159949,
#159950,#159951,#159952,#159953,#159954,#159955,#159956,#159957,#159958,
#159959,#159960,#159961,#159962,#159963,#159964,#159965,#159966,#159967,
#159968,#159969,#159970,#159971,#159972,#159973,#159974,#159975,#159976,
#159977,#159978,#159979,#159980,#159981,#159982,#159983,#159984,#159985,
#159986,#159987,#159988,#159989,#159990,#159991,#159992,#159993,#159994,
#159995,#159996,#159997,#159998,#159999,#160000,#160001,#160002,#160003,
#160004,#160005,#160006,#160007,#160008,#160009,#160010,#160011,#160012,
#160013,#160014,#160015,#160016,#160017,#160018,#160019,#160020,#160021,
#160022,#160023,#160024,#160025,#160026,#160027,#160028,#160029,#160030,
#160031,#160032,#160033,#160034,#160035,#160036),.UNSPECIFIED.,.F.,.F.,
(4,3,3,3,3,3,3,3,3,3,3,3,3,3,3,3,3,3,3,3,3,3,3,3,3,3,3,3,3,3,3,3,3,4),(0.,
0.0637983485556601,0.126550304599327,0.188275152299192,0.249999999999057,
0.308956613413127,0.367063086841327,0.424032424344218,0.43749999999836,
0.468749999998245,0.484374999998192,0.492187499998172,0.496093749998165,
0.498046874998163,0.499999999998161,0.53394514537071,0.567537891023036,
0.60037914982785,0.632691384971143,0.664083874098615,0.687499999998855,
0.718749999998964,0.734374999999016,0.74218749999905,0.747353760782758,
0.749999999999083,0.785423610256769,0.821544299578016,0.858755278828813,
0.874999999999542,0.913784018887876,0.953334061394135,0.993917181375185,
0.999999999998668),.UNSPECIFIED.);
#30111=B_SPLINE_CURVE_WITH_KNOTS('',3,(#160083,#160084,#160085,#160086,
#160087,#160088,#160089,#160090,#160091,#160092,#160093,#160094,#160095,
#160096,#160097,#160098,#160099,#160100,#160101,#160102,#160103,#160104,
#160105,#160106,#160107,#160108,#160109,#160110,#160111,#160112,#160113,
#160114,#160115,#160116,#160117,#160118,#160119,#160120,#160121,#160122,
#160123,#160124,#160125,#160126,#160127,#160128,#160129,#160130,#160131,
#160132,#160133,#160134,#160135,#160136,#160137,#160138,#160139,#160140,
#160141,#160142,#160143,#160144,#160145,#160146,#160147,#160148,#160149,
#160150,#160151,#160152,#160153,#160154,#160155,#160156,#160157,#160158,
#160159,#160160,#160161,#160162,#160163,#160164,#160165,#160166,#160167,
#160168,#160169,#160170,#160171,#160172,#160173,#160174,#160175,#160176),
 .UNSPECIFIED.,.F.,.F.,(4,3,3,3,3,3,3,3,3,3,3,3,3,3,3,3,3,3,3,3,3,3,3,3,
3,3,3,3,3,3,3,4),(0.,0.0712138616603836,0.0959974304540653,0.163570456441593,
0.230073164868291,0.238936586100471,0.249999999999584,0.32929390933836,
0.374999999999386,0.376333406220443,0.437499999999286,0.468749999999227,
0.484374999999198,0.492187499999174,0.496093749999172,0.499075981956204,
0.499999999999169,0.522267304887566,0.573723493912687,0.62315099740726,
0.669708470515297,0.700946575201161,0.745077730004171,0.749999999999585,
0.791696967031908,0.832303089116417,0.838388393259743,0.878729024470567,
0.918083425162144,0.953549722072797,0.991458140984172,0.999999999987821),
 .UNSPECIFIED.);
#30112=B_SPLINE_CURVE_WITH_KNOTS('',3,(#160226,#160227,#160228,#160229,
#160230,#160231,#160232,#160233,#160234,#160235,#160236,#160237,#160238,
#160239,#160240,#160241,#160242,#160243,#160244,#160245,#160246,#160247,
#160248,#160249,#160250,#160251,#160252,#160253,#160254,#160255,#160256,
#160257,#160258,#160259,#160260,#160261,#160262,#160263,#160264,#160265,
#160266,#160267,#160268,#160269,#160270,#160271,#160272,#160273,#160274,
#160275,#160276,#160277,#160278,#160279,#160280,#160281,#160282,#160283,
#160284,#160285,#160286,#160287,#160288,#160289,#160290,#160291,#160292,
#160293,#160294,#160295,#160296,#160297,#160298,#160299,#160300,#160301,
#160302,#160303,#160304,#160305,#160306,#160307,#160308,#160309,#160310,
#160311,#160312,#160313,#160314,#160315,#160316,#160317,#160318,#160319,
#160320,#160321,#160322,#160323,#160324,#160325,#160326,#160327,#160328),
 .UNSPECIFIED.,.F.,.F.,(4,3,3,3,3,3,3,3,3,3,3,3,3,3,3,3,3,3,3,3,3,3,3,3,
3,3,3,3,3,3,3,3,3,3,4),(0.,0.029481217809345,0.0602385454853888,0.0686801150520231,
0.100978168772228,0.125000000000109,0.159373975577551,0.187500000000164,
0.194690117654056,0.200802070347523,0.203125000000173,0.218750000000182,
0.222426540538282,0.25000000000021,0.293843807324644,0.338816651531641,
0.353275723840616,0.375000000000334,0.423151004836134,0.437500000000387,
0.468750000000404,0.484375000000411,0.492187500000405,0.497285529739406,
0.500000000000398,0.507014931348073,0.584324663738214,0.644386345777789,
0.714267082163826,0.750000000000199,0.781872567237418,0.849296687796906,
0.917966672394119,0.925357651915143,0.999999999997567),.UNSPECIFIED.);
#30113=B_SPLINE_CURVE_WITH_KNOTS('',3,(#160333,#160334,#160335,#160336,
#160337,#160338,#160339,#160340,#160341,#160342,#160343,#160344,#160345,
#160346,#160347,#160348,#160349,#160350,#160351,#160352,#160353,#160354,
#160355,#160356,#160357,#160358,#160359,#160360,#160361,#160362,#160363,
#160364,#160365,#160366,#160367,#160368,#160369,#160370,#160371,#160372,
#160373,#160374,#160375,#160376,#160377,#160378,#160379,#160380,#160381,
#160382,#160383,#160384,#160385,#160386,#160387,#160388,#160389,#160390,
#160391,#160392,#160393,#160394,#160395,#160396,#160397,#160398,#160399,
#160400,#160401,#160402,#160403,#160404,#160405,#160406,#160407,#160408,
#160409,#160410,#160411,#160412,#160413,#160414,#160415,#160416,#160417,
#160418,#160419,#160420,#160421,#160422,#160423,#160424,#160425,#160426,
#160427,#160428,#160429),.UNSPECIFIED.,.F.,.F.,(4,3,3,3,3,3,3,3,3,3,3,3,
3,3,3,3,3,3,3,3,3,3,3,3,3,3,3,3,3,3,3,3,4),(5.99380613808649E-13,0.0403188271445495,
0.0798755860320985,0.118348163388507,0.125000000000114,0.162224576751813,
0.19831761361769,0.218750000000206,0.234375000000222,0.242187500000228,
0.247459770958609,0.250000000000234,0.279672982211991,0.310049892003495,
0.341912419002755,0.374007078695027,0.406978512859473,0.437500000000535,
0.468750000000584,0.484375000000598,0.492187500000601,0.496093750000596,
0.498046875000589,0.500000000000582,0.555864552409697,0.613054399144187,
0.671034612436339,0.73022202415885,0.750000000000291,0.812500000000179,
0.874695238678225,0.938574052066678,0.999999999999844),.UNSPECIFIED.);
#30114=B_SPLINE_CURVE_WITH_KNOTS('',3,(#160501,#160502,#160503,#160504,
#160505,#160506,#160507,#160508,#160509,#160510,#160511,#160512,#160513,
#160514,#160515),.UNSPECIFIED.,.F.,.F.,(4,2,2,1,1,1,2,2,4),(0.,0.249999999999863,
0.37499999999979,0.437499999999753,0.468749999999736,0.484374999999732,
0.492187499999731,0.499999999999731,1.),.UNSPECIFIED.);
#30115=B_SPLINE_CURVE_WITH_KNOTS('',3,(#160558,#160559,#160560,#160561,
#160562,#160563,#160564,#160565,#160566,#160567,#160568,#160569,#160570,
#160571,#160572,#160573,#160574,#160575,#160576,#160577,#160578,#160579,
#160580,#160581,#160582,#160583,#160584,#160585,#160586,#160587,#160588,
#160589,#160590,#160591,#160592,#160593,#160594,#160595,#160596,#160597,
#160598,#160599,#160600,#160601,#160602,#160603,#160604,#160605,#160606,
#160607,#160608,#160609,#160610,#160611,#160612,#160613,#160614,#160615,
#160616,#160617,#160618),.UNSPECIFIED.,.F.,.F.,(4,3,3,3,3,3,3,3,3,3,3,3,
3,3,3,3,3,3,3,3,4),(1.12835699204868E-7,0.0630290528050693,0.120826709348546,
0.186129648127262,0.25,0.273112941507023,0.341600487464973,0.411837351393341,
0.425308806931081,0.495917670505428,0.5,0.570579142873041,0.57752795855047,
0.647780195209018,0.716295689304132,0.72972590512184,0.75,0.816009649590574,
0.882019299181147,0.945231797138478,1.),.UNSPECIFIED.);
#30116=B_SPLINE_CURVE_WITH_KNOTS('',3,(#160647,#160648,#160649,#160650,
#160651,#160652,#160653,#160654,#160655,#160656,#160657,#160658,#160659,
#160660,#160661),.UNSPECIFIED.,.F.,.F.,(4,2,2,1,1,1,2,2,4),(0.,0.249999999999984,
0.374999999999977,0.437499999999977,0.468749999999978,0.484374999999972,
0.492187499999968,0.499999999999964,1.),.UNSPECIFIED.);
#30117=B_SPLINE_CURVE_WITH_KNOTS('',3,(#160664,#160665,#160666,#160667,
#160668,#160669,#160670,#160671,#160672,#160673),.UNSPECIFIED.,.F.,.F.,
(4,3,3,4),(0.,0.3333333333333,0.6666666666667,0.999999999699132),
 .UNSPECIFIED.);
#30118=B_SPLINE_CURVE_WITH_KNOTS('',3,(#160678,#160679,#160680,#160681,
#160682,#160683,#160684,#160685,#160686,#160687,#160688,#160689,#160690,
#160691,#160692,#160693,#160694,#160695,#160696,#160697,#160698,#160699,
#160700,#160701,#160702,#160703,#160704,#160705,#160706,#160707,#160708,
#160709,#160710,#160711,#160712,#160713,#160714,#160715,#160716,#160717,
#160718,#160719,#160720,#160721,#160722,#160723,#160724,#160725,#160726,
#160727,#160728,#160729,#160730,#160731,#160732,#160733,#160734,#160735,
#160736,#160737,#160738,#160739,#160740,#160741,#160742,#160743,#160744,
#160745,#160746,#160747,#160748,#160749,#160750,#160751,#160752,#160753,
#160754,#160755,#160756,#160757,#160758,#160759,#160760,#160761,#160762,
#160763,#160764,#160765),.UNSPECIFIED.,.F.,.F.,(4,3,3,3,3,3,3,3,3,3,3,3,
3,3,3,3,3,3,3,3,3,3,3,3,3,3,3,3,3,4),(3.0518593689493E-11,0.0861618174244873,
0.124999999999937,0.1874999999999,0.218749999999882,0.234374999999876,0.242187499999873,
0.249999999999871,0.312499999999858,0.343749999999858,0.359374999999852,
0.374999999999845,0.437499999999816,0.468749999999801,0.484374999999793,
0.492187499999794,0.499999999999796,0.56249999999989,0.593749999999938,
0.609374999999962,0.617187499999974,0.624999999999986,0.687500000000037,
0.718750000000062,0.734375000000069,0.742187500000067,0.749396528653654,
0.750000000000064,0.874999986397288,0.999999972794511),.UNSPECIFIED.);
#30119=B_SPLINE_CURVE_WITH_KNOTS('',3,(#160866,#160867,#160868,#160869,
#160870,#160871,#160872,#160873,#160874,#160875,#160876,#160877,#160878,
#160879,#160880,#160881),.UNSPECIFIED.,.F.,.F.,(4,3,3,3,3,4),(0.,0.279637227187237,
0.3333333333333,0.6666666666667,0.692929821402801,0.999995691343251),
 .UNSPECIFIED.);
#30120=B_SPLINE_CURVE_WITH_KNOTS('',3,(#160884,#160885,#160886,#160887,
#160888,#160889,#160890,#160891,#160892,#160893,#160894,#160895,#160896,
#160897,#160898,#160899,#160900,#160901,#160902,#160903,#160904,#160905,
#160906,#160907,#160908,#160909,#160910,#160911,#160912,#160913,#160914,
#160915,#160916,#160917,#160918,#160919,#160920,#160921,#160922,#160923,
#160924,#160925,#160926,#160927,#160928,#160929,#160930,#160931,#160932,
#160933,#160934,#160935,#160936,#160937,#160938,#160939,#160940,#160941,
#160942,#160943,#160944,#160945,#160946,#160947,#160948,#160949,#160950,
#160951,#160952,#160953,#160954,#160955,#160956,#160957,#160958,#160959,
#160960,#160961,#160962,#160963,#160964,#160965,#160966,#160967,#160968,
#160969,#160970,#160971,#160972,#160973,#160974,#160975,#160976,#160977),
 .UNSPECIFIED.,.F.,.F.,(4,3,3,3,3,3,3,3,3,3,3,3,3,3,3,3,3,3,3,3,3,3,3,3,
3,3,3,3,3,3,3,4),(0.,0.0625000000000142,0.0937500000000213,0.109375000000025,
0.120030834327565,0.125000000000029,0.187500000000019,0.218750000000021,
0.234375000000022,0.242187500000023,0.249602352649526,0.250000000000024,
0.312500000000072,0.343750000000095,0.359375000000101,0.367187500000099,
0.374597896383853,0.375000000000096,0.437500000000043,0.468750000000023,
0.484375000000018,0.498281689012045,0.500000000000012,0.583999870627186,
0.668503420094752,0.687500000000055,0.71875000000006,0.734375000000059,
0.750000000000058,0.836055337224158,0.922187361649025,0.999999999918209),
 .UNSPECIFIED.);
#30121=B_SPLINE_CURVE_WITH_KNOTS('',3,(#160982,#160983,#160984,#160985,
#160986,#160987,#160988,#160989,#160990,#160991,#160992,#160993,#160994,
#160995,#160996,#160997,#160998,#160999,#161000,#161001,#161002,#161003,
#161004,#161005,#161006,#161007,#161008,#161009,#161010,#161011,#161012,
#161013,#161014,#161015,#161016,#161017,#161018,#161019,#161020,#161021,
#161022,#161023,#161024,#161025,#161026,#161027,#161028,#161029,#161030,
#161031,#161032,#161033,#161034,#161035,#161036,#161037,#161038,#161039,
#161040,#161041,#161042,#161043,#161044,#161045,#161046,#161047,#161048,
#161049,#161050,#161051,#161052,#161053,#161054,#161055,#161056,#161057,
#161058,#161059,#161060,#161061,#161062,#161063,#161064,#161065,#161066,
#161067,#161068,#161069,#161070,#161071,#161072,#161073,#161074,#161075,
#161076,#161077,#161078,#161079,#161080,#161081,#161082,#161083,#161084,
#161085,#161086,#161087,#161088,#161089,#161090,#161091,#161092,#161093,
#161094,#161095,#161096,#161097,#161098,#161099,#161100,#161101,#161102,
#161103,#161104,#161105,#161106,#161107,#161108,#161109,#161110,#161111,
#161112,#161113,#161114,#161115,#161116,#161117,#161118,#161119,#161120,
#161121,#161122,#161123,#161124,#161125,#161126,#161127,#161128,#161129,
#161130,#161131,#161132,#161133,#161134,#161135,#161136,#161137,#161138,
#161139,#161140,#161141,#161142,#161143,#161144,#161145,#161146,#161147,
#161148,#161149,#161150,#161151,#161152,#161153,#161154,#161155,#161156,
#161157,#161158,#161159,#161160,#161161,#161162,#161163,#161164,#161165,
#161166,#161167,#161168,#161169,#161170,#161171,#161172,#161173,#161174,
#161175,#161176,#161177,#161178,#161179,#161180,#161181,#161182,#161183,
#161184,#161185,#161186,#161187,#161188,#161189,#161190,#161191,#161192,
#161193,#161194,#161195,#161196,#161197,#161198,#161199,#161200,#161201,
#161202,#161203,#161204,#161205,#161206,#161207,#161208,#161209,#161210,
#161211,#161212,#161213,#161214,#161215,#161216,#161217,#161218,#161219,
#161220,#161221,#161222,#161223,#161224,#161225,#161226,#161227,#161228,
#161229,#161230,#161231,#161232,#161233,#161234,#161235,#161236,#161237,
#161238,#161239,#161240,#161241,#161242,#161243,#161244,#161245,#161246,
#161247,#161248,#161249,#161250,#161251,#161252,#161253,#161254,#161255,
#161256,#161257,#161258,#161259,#161260,#161261,#161262,#161263,#161264,
#161265,#161266,#161267),.UNSPECIFIED.,.F.,.F.,(4,3,3,3,3,3,3,3,3,3,3,3,
3,3,3,3,3,3,3,3,3,3,3,3,3,3,3,3,3,3,3,3,3,3,3,3,3,3,3,3,3,3,3,3,3,3,3,3,
3,3,3,3,3,3,3,3,3,3,3,3,3,3,3,3,3,3,3,3,3,3,3,3,3,3,3,3,3,3,3,3,3,3,3,3,
3,3,3,3,3,3,3,3,3,3,3,4),(1.01228942666207E-13,0.0258517188462294,0.0291944722982846,
0.0539167902517146,0.0583388729783417,0.0819837452472311,0.0867941512072641,
0.109368785932464,0.114710180560498,0.124999999999964,0.14228679457853,
0.162838950593894,0.169724963574536,0.187499999999946,0.197102796308362,
0.215442428354756,0.218749999999937,0.224501124246269,0.234374999999933,
0.242187499999931,0.24609374999993,0.248046874999929,0.249999999999929,
0.251854256678714,0.267164879481683,0.277122765238224,0.291428278200627,
0.302730930762253,0.31600929783533,0.328978329984541,0.340881913919205,
0.35344885723419,0.35614179665251,0.367162819454531,0.374999999999932,0.384425830148499,
0.395213261190277,0.407256750918518,0.414246739447086,0.424887397515132,
0.436707838233527,0.437499999999933,0.445291520326618,0.457020760163276,
0.467982121877994,0.468749999999933,0.475797933560337,0.487960486538108,
0.499999999999934,0.505117363585142,0.518189178195458,0.531700070758596,
0.534549590305634,0.548524795152785,0.559882688873538,0.562499999999935,
0.563805319330323,0.57511664286713,0.585492659469396,0.591852345706755,
0.593749999999936,0.605206908028143,0.609374999999936,0.617187499999937,
0.619227423581006,0.621093749999937,0.623657692195749,0.624999999999937,
0.638897705866528,0.648439480043727,0.663784977517374,0.677550678837764,
0.687499999999947,0.702962444654866,0.705331409608235,0.722208861060543,
0.731604666063896,0.749999999999958,0.756846444820027,0.775981773237512,
0.78257796017835,0.802738978947917,0.80863570172481,0.829821062713248,0.834983243688876,
0.857208050362122,0.861970014046411,0.885261265678161,0.88982978307567,
0.914216652890968,0.91863289448201,0.944143940103395,0.948414026215984,
0.975074204659781,0.979491551762633,0.999999934582838),.UNSPECIFIED.);
#30122=B_SPLINE_CURVE_WITH_KNOTS('',3,(#161432,#161433,#161434,#161435,
#161436,#161437,#161438,#161439,#161440,#161441,#161442,#161443,#161444,
#161445,#161446,#161447,#161448,#161449,#161450,#161451,#161452,#161453,
#161454,#161455,#161456,#161457,#161458,#161459,#161460,#161461,#161462,
#161463,#161464,#161465,#161466,#161467,#161468,#161469,#161470,#161471,
#161472,#161473,#161474,#161475,#161476,#161477,#161478,#161479,#161480,
#161481,#161482,#161483,#161484,#161485,#161486,#161487,#161488,#161489,
#161490,#161491,#161492,#161493,#161494,#161495,#161496,#161497,#161498,
#161499,#161500,#161501,#161502,#161503,#161504,#161505,#161506,#161507,
#161508,#161509,#161510,#161511,#161512,#161513,#161514,#161515,#161516,
#161517,#161518,#161519,#161520,#161521,#161522,#161523,#161524,#161525,
#161526,#161527,#161528,#161529,#161530,#161531,#161532,#161533,#161534,
#161535,#161536,#161537,#161538,#161539,#161540,#161541,#161542,#161543,
#161544,#161545,#161546,#161547,#161548,#161549,#161550,#161551,#161552,
#161553,#161554,#161555,#161556,#161557,#161558,#161559,#161560,#161561,
#161562,#161563,#161564,#161565,#161566,#161567,#161568,#161569,#161570,
#161571,#161572,#161573,#161574,#161575,#161576,#161577,#161578,#161579,
#161580,#161581,#161582,#161583,#161584,#161585,#161586,#161587,#161588,
#161589,#161590,#161591,#161592,#161593,#161594,#161595,#161596,#161597,
#161598,#161599,#161600,#161601,#161602,#161603,#161604,#161605,#161606,
#161607,#161608,#161609,#161610,#161611,#161612,#161613,#161614,#161615,
#161616,#161617,#161618,#161619,#161620,#161621,#161622,#161623,#161624,
#161625,#161626,#161627,#161628,#161629,#161630,#161631,#161632,#161633,
#161634,#161635,#161636,#161637,#161638,#161639,#161640,#161641,#161642,
#161643,#161644,#161645,#161646,#161647,#161648,#161649,#161650,#161651,
#161652,#161653,#161654,#161655,#161656,#161657,#161658,#161659,#161660,
#161661,#161662,#161663,#161664,#161665,#161666,#161667,#161668,#161669,
#161670,#161671,#161672,#161673,#161674,#161675,#161676,#161677,#161678,
#161679,#161680,#161681,#161682,#161683,#161684,#161685,#161686,#161687,
#161688,#161689,#161690,#161691,#161692,#161693,#161694,#161695,#161696,
#161697,#161698,#161699,#161700,#161701,#161702,#161703,#161704,#161705,
#161706,#161707,#161708,#161709,#161710,#161711,#161712,#161713,#161714,
#161715,#161716,#161717,#161718,#161719,#161720,#161721,#161722,#161723,
#161724,#161725,#161726,#161727,#161728,#161729,#161730,#161731,#161732,
#161733,#161734,#161735,#161736,#161737,#161738,#161739,#161740,#161741,
#161742,#161743,#161744,#161745,#161746,#161747,#161748,#161749,#161750,
#161751,#161752,#161753,#161754,#161755,#161756,#161757,#161758,#161759,
#161760,#161761,#161762,#161763,#161764,#161765,#161766,#161767,#161768,
#161769,#161770,#161771),.UNSPECIFIED.,.F.,.F.,(4,3,3,3,3,3,3,3,3,3,3,3,
3,3,3,3,3,3,3,3,3,3,3,3,3,3,3,3,3,3,3,3,3,3,3,3,3,3,3,3,3,3,3,3,3,3,3,3,
3,3,3,3,3,3,3,3,3,3,3,3,3,3,3,3,3,3,3,3,3,3,3,3,3,3,3,3,3,3,3,3,3,3,3,3,
3,3,3,3,3,3,3,3,3,3,3,3,3,3,3,3,3,3,3,3,3,3,3,3,3,3,3,3,3,4),(0.,0.0200355867142946,
0.0273934559852642,0.02777777777778,0.0523571512332771,0.0554778740025501,
0.05555555555556,0.0780129429070063,0.08333333333333,0.0835626833505441,
0.105775578670446,0.1111111111111,0.111647540558516,0.132756838179549,0.1388888888889,
0.139731706177186,0.158229694933432,0.1666666666667,0.16781571188038,0.185503873437475,
0.1944444444444,0.195900322246756,0.212581714497131,0.2222222222222,0.223984844942246,
0.239668353537612,0.25,0.25206969643164,0.266829520339375,0.2777777777778,
0.280154959579243,0.294004855399001,0.3055555555556,0.308238363387252,0.320785848360276,
0.3333333333333,0.33631798841208,0.346836434794149,0.357823186972442,0.3611111111111,
0.364404840781021,0.374276807137445,0.384994346725833,0.3888888888889,0.392483554061635,
0.401252108118,0.410562749498785,0.4166666666667,0.420542409231562,0.427797937356122,
0.435140251960111,0.442644355403895,0.4444444444444,0.448642742632016,0.455753384099796,
0.463226096058239,0.471202663316992,0.4722222222222,0.476778765924896,0.483477707510161,
0.490325972528195,0.497204379959601,0.5,0.504840583711416,0.512744519139026,
0.520447152811956,0.5277777777778,0.532869464526171,0.540810626085051,0.548620408076424,
0.5555555555556,0.561003783620005,0.572168558476653,0.581785957831427,0.5833333333333,
0.589072583566232,0.599528783954322,0.609285938807755,0.6111111111111,0.617146865199343,
0.628017877044121,0.6388888888889,0.645234800695991,0.656989588181199,0.6666666666667,
0.673328052991939,0.687201179480869,0.6944444444444,0.701409633095276,0.716402048341608,
0.7222222222222,0.729573556853193,0.744017066992862,0.75,0.757556694920181,
0.776654469077291,0.7777777777778,0.785669915631699,0.803449019432371,0.8055555555556,
0.813769928908346,0.8333333333333,0.841844335008108,0.8611111111111,0.869925239036782,
0.8888888888889,0.898008744487289,0.9166666666667,0.926101900071302,0.9444444444444,
0.954197326598602,0.9722222222222,0.982241351582234,0.999999988745194),
 .UNSPECIFIED.);
#30123=B_SPLINE_CURVE_WITH_KNOTS('',3,(#161943,#161944,#161945,#161946,
#161947,#161948,#161949,#161950,#161951,#161952,#161953,#161954,#161955,
#161956,#161957,#161958,#161959,#161960,#161961,#161962,#161963,#161964,
#161965,#161966,#161967,#161968,#161969,#161970,#161971,#161972,#161973,
#161974,#161975,#161976,#161977,#161978,#161979,#161980,#161981,#161982,
#161983,#161984,#161985,#161986,#161987,#161988,#161989,#161990,#161991,
#161992,#161993,#161994,#161995,#161996,#161997,#161998,#161999,#162000,
#162001,#162002,#162003,#162004,#162005,#162006,#162007,#162008,#162009,
#162010,#162011,#162012,#162013,#162014,#162015,#162016,#162017,#162018,
#162019,#162020,#162021,#162022,#162023,#162024,#162025,#162026,#162027,
#162028,#162029,#162030,#162031,#162032,#162033,#162034,#162035,#162036,
#162037,#162038,#162039,#162040,#162041,#162042,#162043,#162044,#162045,
#162046,#162047,#162048,#162049,#162050,#162051,#162052,#162053,#162054,
#162055,#162056,#162057,#162058,#162059,#162060,#162061,#162062,#162063,
#162064,#162065,#162066,#162067,#162068,#162069,#162070,#162071,#162072,
#162073,#162074,#162075,#162076,#162077,#162078,#162079,#162080,#162081,
#162082,#162083,#162084,#162085,#162086,#162087,#162088,#162089,#162090,
#162091,#162092,#162093,#162094,#162095,#162096,#162097,#162098,#162099,
#162100,#162101,#162102,#162103,#162104,#162105,#162106,#162107,#162108,
#162109,#162110,#162111,#162112,#162113,#162114,#162115,#162116,#162117,
#162118,#162119,#162120,#162121,#162122,#162123,#162124,#162125,#162126,
#162127,#162128,#162129,#162130,#162131,#162132,#162133,#162134,#162135,
#162136,#162137,#162138,#162139,#162140,#162141,#162142,#162143,#162144),
 .UNSPECIFIED.,.F.,.F.,(4,2,2,2,2,2,2,2,2,2,2,2,2,2,2,2,2,2,2,2,2,2,2,2,
2,2,2,2,2,2,2,2,2,2,2,2,2,2,2,2,2,2,2,2,2,2,2,2,2,2,2,2,2,2,2,2,2,2,2,2,
2,2,2,2,2,2,2,2,2,2,2,2,2,2,2,2,2,2,2,2,2,2,2,2,2,2,2,2,2,2,2,2,2,2,2,2,
2,2,2,2,4),(-5.80673691874591,-5.80311558456603,-5.78521951548741,-5.74936542742757,
-5.69789658982925,-5.55469108508799,-5.47835921867039,-5.44224050505522,
-5.41337094993437,-5.37911111324198,-5.30769462254877,-5.19011243008685,
-5.1078364512622,-5.08324731886244,-5.06654399501397,-5.04601596685676,
-4.99854432371449,-4.91830532015885,-4.78499374848092,-4.74318259301805,
-4.71370033935409,-4.6823336174823,-4.6296968329514,-4.56208732768372,-4.47613359739696,
-4.38165464089175,-4.35365106186554,-4.33726741584425,-4.32077052078011,
-4.29220578521379,-4.19215569564271,-4.02482294360284,-3.9823839054569,
-3.9530819167607,-3.92201642443015,-3.8707363199192,-3.83543283172867,-3.71055225609258,
-3.63739932108507,-3.61332061828525,-3.59666780468482,-3.57581690019977,
-3.52601539924736,-3.4385685991293,-3.31662702727645,-3.27439545448113,
-3.24514210062318,-3.21398488565512,-3.16251724931886,-3.06903864772341,
-2.91054203146376,-2.88348211392876,-2.86728626244473,-2.85057629001149,
-2.82094837620054,-2.7817347539378,-2.67149231740343,-2.54909724995236,
-2.50941118672945,-2.48021170712932,-2.4480865615984,-2.39060713882964,
-2.31115601623141,-2.17122053541862,-2.14565849354444,-2.12883882530887,
-2.10884676183292,-2.06498560927209,-1.99486879103477,-1.8440265326523,
-1.80321525945184,-1.77387759557024,-1.74217324047111,-1.68763358136074,
-1.6163625826057,-1.51764607929113,-1.4347617200489,-1.4110028515639,-1.39555525777792,
-1.37784773159648,-1.34302416000173,-1.29369949695151,-1.19799736808929,
-1.07974823682673,-1.04009726750669,-1.01090298265717,-0.978763975383292,
-0.921197537526748,-0.841549942479151,-0.701890581981484,-0.676365628406667,
-0.659551239060342,-0.639541471368818,-0.595562919387754,-0.525133199857429,
-0.374882540968986,-0.334029316432046,-0.304686498507445,-0.272998728748237,
-0.218549124060644,-1.00000001435063E-6),.UNSPECIFIED.);
#30124=B_SPLINE_CURVE_WITH_KNOTS('',3,(#162147,#162148,#162149,#162150,
#162151,#162152,#162153,#162154,#162155,#162156,#162157,#162158,#162159,
#162160,#162161,#162162,#162163,#162164,#162165,#162166,#162167,#162168,
#162169,#162170,#162171,#162172,#162173,#162174,#162175,#162176,#162177,
#162178,#162179,#162180,#162181,#162182,#162183,#162184,#162185,#162186,
#162187,#162188,#162189,#162190,#162191,#162192,#162193,#162194,#162195,
#162196,#162197,#162198,#162199,#162200,#162201,#162202,#162203,#162204,
#162205,#162206,#162207,#162208,#162209,#162210,#162211,#162212,#162213,
#162214,#162215,#162216,#162217,#162218,#162219,#162220,#162221,#162222,
#162223,#162224,#162225,#162226,#162227,#162228,#162229,#162230,#162231,
#162232,#162233,#162234,#162235,#162236,#162237,#162238,#162239,#162240,
#162241,#162242,#162243,#162244,#162245,#162246,#162247,#162248,#162249,
#162250,#162251,#162252,#162253,#162254,#162255,#162256,#162257,#162258,
#162259,#162260,#162261,#162262,#162263,#162264,#162265,#162266,#162267,
#162268,#162269,#162270,#162271,#162272,#162273,#162274,#162275,#162276,
#162277,#162278,#162279,#162280,#162281,#162282,#162283,#162284,#162285,
#162286,#162287,#162288,#162289,#162290,#162291,#162292,#162293,#162294,
#162295,#162296,#162297,#162298,#162299,#162300,#162301,#162302,#162303,
#162304,#162305,#162306,#162307,#162308,#162309,#162310,#162311,#162312,
#162313,#162314,#162315,#162316,#162317,#162318,#162319,#162320,#162321,
#162322,#162323,#162324,#162325,#162326),.UNSPECIFIED.,.F.,.F.,(4,2,2,2,
2,2,2,2,2,2,2,2,2,2,2,2,2,2,2,2,2,2,2,2,2,2,2,2,2,2,2,2,2,2,2,2,2,2,2,2,
2,2,2,2,2,2,2,2,2,2,2,2,2,2,2,2,2,2,2,2,2,2,2,2,2,2,2,2,2,2,2,2,2,2,2,2,
2,2,2,2,2,2,2,2,2,2,2,2,2,4),(-28.462078608473,-28.3866548311619,-28.3415640456688,
-28.3139836013474,-28.2851402865027,-28.2498725241615,-28.1727391509134,
-28.0276202040923,-27.9762895199563,-27.9405029136976,-27.9226205962435,
-27.9070576963559,-27.8835404957315,-27.799784969196,-27.7010835025185,
-27.6300241283045,-27.5755935925949,-27.5439101464897,-27.5145673445461,
-27.4737074668686,-27.3235559695455,-27.2530676138123,-27.2090677021112,
-27.1890551445635,-27.1722423347026,-27.1467255074532,-27.0071246534371,
-26.9274530031814,-26.8698765206144,-26.8377367496269,-26.8085440961376,
-26.7688990369699,-26.6510052576259,-26.5570035453015,-26.5064981574161,
-26.4711052813981,-26.4532940091875,-26.4378833110121,-26.4143654381337,
-26.3306061123437,-26.2319014706414,-26.1608403040848,-26.1064082708122,
-26.0747238510428,-26.045380088863,-26.0045187746979,-25.85436419259,-25.7838726296274,
-25.7398709498093,-25.7198576946395,-25.7030443585834,-25.6775268190117,
-25.5379220805613,-25.4582473970294,-25.4006688534241,-25.3685280144069,
-25.3393344329808,-25.2996881799948,-25.1817954462825,-25.0878143825943,
-25.0372910199182,-25.0018891637963,-24.9840758916647,-24.9686651747599,
-24.9451497507252,-24.8613357356013,-24.7626277773463,-24.6915881953645,
-24.6371666422563,-24.6054833705243,-24.5761378290026,-24.535269208448,
-24.3851947435507,-24.3146549163278,-24.2706345365833,-24.2506179801848,
-24.2338047935297,-24.2082916912617,-24.0687112068533,-23.9890112592286,
-23.931420751605,-23.8992771939593,-23.8700831671917,-23.8304394951872,
-23.7127704669023,-23.6199974742871,-23.5686447890576,-23.5328466286805,
-23.5149611243724,-23.511361333244),.UNSPECIFIED.);
#30125=B_SPLINE_CURVE_WITH_KNOTS('',3,(#162331,#162332,#162333,#162334,
#162335,#162336,#162337,#162338,#162339,#162340,#162341,#162342,#162343,
#162344,#162345,#162346,#162347,#162348,#162349,#162350,#162351,#162352,
#162353,#162354,#162355,#162356,#162357,#162358,#162359,#162360,#162361,
#162362,#162363,#162364,#162365,#162366,#162367,#162368,#162369,#162370,
#162371,#162372,#162373,#162374,#162375,#162376,#162377,#162378,#162379,
#162380,#162381,#162382,#162383,#162384,#162385,#162386,#162387,#162388,
#162389,#162390,#162391,#162392,#162393,#162394,#162395,#162396,#162397,
#162398,#162399,#162400,#162401,#162402,#162403,#162404,#162405,#162406,
#162407,#162408,#162409,#162410,#162411,#162412,#162413,#162414,#162415,
#162416,#162417,#162418,#162419,#162420,#162421,#162422,#162423,#162424,
#162425,#162426,#162427,#162428,#162429,#162430,#162431,#162432,#162433,
#162434,#162435,#162436,#162437,#162438,#162439,#162440,#162441,#162442,
#162443,#162444,#162445,#162446,#162447,#162448,#162449,#162450,#162451,
#162452,#162453,#162454,#162455,#162456,#162457,#162458,#162459,#162460,
#162461,#162462,#162463,#162464,#162465,#162466,#162467,#162468,#162469,
#162470,#162471,#162472,#162473,#162474,#162475,#162476,#162477,#162478,
#162479,#162480,#162481,#162482,#162483,#162484,#162485,#162486,#162487,
#162488,#162489,#162490,#162491,#162492,#162493,#162494,#162495,#162496,
#162497,#162498,#162499,#162500,#162501,#162502,#162503,#162504,#162505,
#162506,#162507,#162508,#162509,#162510,#162511,#162512,#162513,#162514,
#162515,#162516,#162517,#162518,#162519,#162520,#162521,#162522,#162523,
#162524,#162525,#162526,#162527,#162528,#162529,#162530,#162531,#162532,
#162533,#162534,#162535,#162536,#162537,#162538),.UNSPECIFIED.,.F.,.F.,
(4,2,2,2,2,2,2,2,2,2,2,2,2,2,2,2,2,2,2,2,2,2,2,2,2,2,2,2,2,2,2,2,2,2,2,
2,2,2,2,2,2,2,2,2,2,2,2,2,2,2,2,2,2,2,2,2,2,2,2,2,2,2,2,2,2,2,2,2,2,2,2,
2,2,2,2,2,2,2,2,2,2,2,2,2,2,2,2,2,2,2,2,2,2,2,2,2,2,2,2,2,2,2,2,4),(-11.684044174322,
-11.6723367729996,-11.6578121804501,-11.6213110169713,-11.4659961518821,
-11.3949588913602,-11.3405391976892,-11.3088570747923,-11.2795126353998,
-11.2386456144045,-11.0885755866662,-11.0180390006996,-10.9740204899463,
-10.9540047134165,-10.9371921425277,-10.9116799180412,-10.772104244175,
-10.6924075600857,-10.6348193273248,-10.602676986944,-10.5734840389483,
-10.5338417896757,-10.416174179528,-10.3233755606539,-10.2720432235089,
-10.2362551585611,-10.2183719028399,-10.2028080433849,-10.1792891894372,
-10.0955321491061,-9.99682485798081,-9.92575976392989,-9.87132523251124,
-9.8396397759129,-9.81029529297017,-9.76943338184275,-9.61926762710395,
-9.54877801758719,-9.50477660009966,-9.48476302813906,-9.46794918087568,
-9.44243051234741,-9.30281954225911,-9.22314464713178,-9.16556541387518,
-9.13342385207994,-9.10422944144975,-9.064581790491,-8.94666604649448,-8.85258545643525,
-8.80212773470256,-8.76675706925275,-8.74894916912009,-8.73353607961527,
-8.71000687037493,-8.62634021065093,-8.52762996553284,-8.4565241472155,
-8.40206817624361,-8.37037821353963,-8.34103413103857,-8.30018054264639,
-8.14987483177597,-8.07945594751373,-8.03548056449599,-8.01547057214582,
-7.99865508565373,-7.9731272329097,-7.83346309061008,-7.75382343831422,
-7.69625920008055,-7.6641194132818,-7.6349232418721,-7.59526788858234,-7.47694539865929,
-7.36353796539349,-7.32380079443192,-7.29388946418653,-7.27712283294249,
-7.26097107435698,-7.23413817200323,-7.07433090077473,-6.98158545707883,
-6.93020696410078,-6.89906512256474,-6.86980261427119,-6.82751420994756,
-6.70813042045763,-6.61894713689106,-6.56861078422214,-6.54768760660895,
-6.53104358260768,-6.50707032200526,-6.42785900488293,-6.30717218959642,
-6.27246012230937,-6.2217530119573,-6.19078642066411,-6.16142784615645,
-6.11862909549268,-5.93063288332504,-5.84217227257886,-5.81867682705061,
-5.80673691874591),.UNSPECIFIED.);
#30126=B_SPLINE_CURVE_WITH_KNOTS('',3,(#162539,#162540,#162541,#162542,
#162543,#162544,#162545,#162546,#162547,#162548,#162549,#162550,#162551,
#162552,#162553,#162554,#162555,#162556,#162557,#162558,#162559,#162560,
#162561,#162562,#162563,#162564,#162565,#162566,#162567,#162568,#162569,
#162570,#162571,#162572,#162573,#162574,#162575,#162576,#162577,#162578,
#162579,#162580,#162581,#162582,#162583,#162584,#162585,#162586,#162587,
#162588,#162589,#162590,#162591,#162592,#162593,#162594,#162595,#162596,
#162597,#162598,#162599,#162600,#162601,#162602,#162603,#162604,#162605,
#162606,#162607,#162608,#162609,#162610,#162611,#162612,#162613,#162614,
#162615,#162616,#162617,#162618,#162619,#162620,#162621,#162622,#162623,
#162624,#162625,#162626,#162627,#162628,#162629,#162630,#162631,#162632,
#162633,#162634,#162635,#162636,#162637,#162638,#162639,#162640,#162641,
#162642,#162643,#162644,#162645,#162646,#162647,#162648,#162649,#162650,
#162651,#162652,#162653,#162654,#162655,#162656,#162657,#162658,#162659,
#162660,#162661,#162662,#162663,#162664,#162665,#162666,#162667,#162668,
#162669,#162670,#162671,#162672,#162673,#162674,#162675,#162676,#162677,
#162678,#162679,#162680,#162681,#162682,#162683,#162684,#162685,#162686,
#162687,#162688,#162689,#162690,#162691,#162692,#162693,#162694,#162695,
#162696,#162697,#162698,#162699,#162700,#162701,#162702,#162703,#162704,
#162705,#162706,#162707,#162708,#162709,#162710,#162711,#162712,#162713,
#162714,#162715,#162716,#162717,#162718,#162719,#162720,#162721,#162722,
#162723,#162724,#162725,#162726,#162727,#162728,#162729,#162730,#162731,
#162732,#162733,#162734,#162735,#162736,#162737,#162738,#162739,#162740,
#162741,#162742,#162743,#162744),.UNSPECIFIED.,.F.,.F.,(4,2,2,2,2,2,2,2,
2,2,2,2,2,2,2,2,2,2,2,2,2,2,2,2,2,2,2,2,2,2,2,2,2,2,2,2,2,2,2,2,2,2,2,2,
2,2,2,2,2,2,2,2,2,2,2,2,2,2,2,2,2,2,2,2,2,2,2,2,2,2,2,2,2,2,2,2,2,2,2,2,
2,2,2,2,2,2,2,2,2,2,2,2,2,2,2,2,2,2,2,2,2,2,4),(-23.511361333244,-23.4993972146998,
-23.4758809979245,-23.3920650137635,-23.2933538790571,-23.222311663882,
-23.1678881812097,-23.1362038578463,-23.1068573834604,-23.0659875336822,
-22.9159070008107,-22.8453655716136,-22.8013440258702,-22.7813268635726,
-22.7645131254748,-22.7389991251823,-22.5994137366634,-22.5197115478179,
-22.4621193305488,-22.4299747619663,-22.4007797880389,-22.3611347842271,
-22.2434587686312,-22.1506513293291,-22.0993169410328,-22.0635271110743,
-22.0456427443577,-22.0300777615743,-22.0065569877358,-21.9227978044795,
-21.8240836745711,-21.7530120351075,-21.6985728996921,-21.6668850982125,
-21.6375386358784,-21.5966742949601,-21.4464924060745,-21.3760009976888,
-21.3319976895833,-21.3119829078351,-21.2951678475892,-21.2696470548108,
-21.1300244121076,-21.0503455467186,-20.9927630125642,-20.9606193364621,
-20.9314228664848,-20.8917722001421,-20.7738322732462,-20.6796670929825,
-20.629259794319,-20.593912562184,-20.5761081420522,-20.5606923997099,-20.5371509363203,
-20.4535496666785,-20.3548327100082,-20.2836961859723,-20.2292232392401,
-20.1975287401617,-20.1681835203225,-20.1273335473972,-19.9769278678421,
-19.906552344578,-19.862592066368,-19.8425834801576,-19.8257660978533,-19.8002309315131,
-19.6605226063899,-19.5809037486191,-19.5233472487528,-19.4912071878676,
-19.46200841687,-19.4223458305632,-19.2344315517932,-19.1392170953403,-19.1154216534419,
-19.0998135406436,-19.0820475230388,-19.046913153152,-18.9069936528118,
-18.8239247364213,-18.7636645823629,-18.730965971671,-18.7019078955318,
-18.6640356065842,-18.5570298547274,-18.4687890467565,-18.4216257184478,
-18.3876755479274,-18.3693757380058,-18.3538804018095,-18.3259541867317,
-18.1495305957111,-18.0659447479598,-18.030177836169,-18.0013209655792,
-17.9667538391989,-17.8946472335103,-17.7511154568425,-17.6684221208536,
-17.6452400522391,-17.6336516764103),.UNSPECIFIED.);
#30127=B_SPLINE_CURVE_WITH_KNOTS('',3,(#162747,#162748,#162749,#162750,
#162751,#162752,#162753,#162754,#162755,#162756,#162757,#162758,#162759,
#162760,#162761,#162762,#162763,#162764,#162765,#162766,#162767,#162768,
#162769,#162770,#162771,#162772,#162773,#162774,#162775,#162776,#162777,
#162778,#162779,#162780,#162781,#162782,#162783,#162784,#162785,#162786,
#162787,#162788,#162789,#162790,#162791,#162792,#162793,#162794,#162795,
#162796,#162797,#162798,#162799,#162800,#162801,#162802,#162803,#162804,
#162805,#162806,#162807,#162808,#162809,#162810,#162811,#162812,#162813,
#162814,#162815,#162816,#162817,#162818,#162819,#162820,#162821,#162822,
#162823,#162824,#162825,#162826,#162827,#162828,#162829,#162830,#162831,
#162832,#162833,#162834,#162835,#162836,#162837,#162838,#162839,#162840,
#162841,#162842,#162843,#162844,#162845,#162846,#162847,#162848,#162849,
#162850,#162851,#162852,#162853,#162854,#162855,#162856,#162857,#162858,
#162859,#162860,#162861,#162862,#162863,#162864,#162865,#162866,#162867,
#162868,#162869,#162870,#162871,#162872,#162873,#162874,#162875,#162876,
#162877,#162878,#162879,#162880,#162881,#162882,#162883,#162884,#162885,
#162886,#162887,#162888,#162889,#162890,#162891,#162892,#162893,#162894,
#162895,#162896,#162897,#162898,#162899,#162900,#162901,#162902,#162903,
#162904,#162905,#162906,#162907,#162908,#162909,#162910,#162911,#162912,
#162913,#162914,#162915,#162916,#162917,#162918,#162919,#162920,#162921,
#162922,#162923,#162924,#162925,#162926,#162927,#162928,#162929,#162930,
#162931,#162932,#162933,#162934,#162935,#162936,#162937,#162938,#162939,
#162940,#162941,#162942,#162943,#162944,#162945,#162946,#162947,#162948,
#162949,#162950,#162951,#162952,#162953,#162954),.UNSPECIFIED.,.F.,.F.,
(4,2,2,2,2,2,2,2,2,2,2,2,2,2,2,2,2,2,2,2,2,2,2,2,2,2,2,2,2,2,2,2,2,2,2,
2,2,2,2,2,2,2,2,2,2,2,2,2,2,2,2,2,2,2,2,2,2,2,2,2,2,2,2,2,2,2,2,2,2,2,2,
2,2,2,2,2,2,2,2,2,2,2,2,2,2,2,2,2,2,2,2,2,2,2,2,2,2,2,2,2,2,2,2,4),(-17.6336516764103,
-17.6297243330596,-17.6116808244776,-17.5750059161433,-17.4367864941327,
-17.3541262239905,-17.2940543692883,-17.2613882223578,-17.2323243674471,
-17.1943943599489,-17.0846814014701,-16.9816201130654,-16.927367862535,
-16.9059448670352,-16.8893486613693,-16.8660531557983,-16.7953573344822,
-16.7864150354094,-16.6649414585775,-16.630115600003,-16.5792969587153,
-16.5483100156811,-16.5189610220922,-16.4762299426034,-16.3119485845575,
-16.2098416083641,-16.1810552057561,-16.1645128975227,-16.1481695117954,
-16.1203707252606,-15.9660810541342,-15.8691700519801,-15.8180199551347,
-15.7869176839933,-15.7576318254445,-15.7151968440132,-15.6025722476219,
-15.5087784758488,-15.4570725237245,-15.4359686611406,-15.419344216166,
-15.3956253670958,-15.3202983293306,-15.1964086399864,-15.1612416528181,
-15.1100918324008,-15.0790470775991,-15.0497297623631,-15.0072044449991,
-14.8406561679522,-14.7400623849715,-14.7114372462249,-14.6949272684309,
-14.6805627321891,-14.654893180657,-14.50694225317,-14.3855500321139,-14.3415261726698,
-14.3116722146673,-14.2809387669368,-14.2315816356588,-14.1688167976056,
-14.0691049340051,-13.9938446919914,-13.9701305813156,-13.9535065294856,
-13.9323991956418,-13.880665938317,-13.7867761558958,-13.6743063607204,
-13.631870689576,-13.6025846942315,-13.5714824819395,-13.5203332368778,
-13.4233565715843,-13.2691331244168,-13.2413190829432,-13.2249726282854,
-13.2084334966322,-13.1796632703288,-13.077707529614,-12.9132272038271,
-12.8705149485744,-12.8411688075139,-12.8101764854403,-12.7593277508794,
-12.7244708632311,-12.6027868669078,-12.5586556269274,-12.5149929475945,
-12.4950303927588,-12.4782009101954,-12.4525739862569,-12.4208646084837,
-12.3484411713795,-12.2017213702071,-12.1606457739916,-12.1312685777191,
-12.099653925335,-12.0456331388895,-11.8143378152777,-11.7775768940125,
-11.7595172858016,-11.7555598459133),.UNSPECIFIED.);
#30128=B_SPLINE_CURVE_WITH_KNOTS('',3,(#162957,#162958,#162959,#162960,
#162961,#162962,#162963,#162964,#162965,#162966,#162967,#162968,#162969,
#162970,#162971,#162972,#162973,#162974,#162975,#162976,#162977,#162978,
#162979,#162980,#162981,#162982,#162983,#162984,#162985,#162986,#162987,
#162988,#162989,#162990,#162991,#162992,#162993,#162994,#162995,#162996,
#162997,#162998,#162999,#163000,#163001,#163002,#163003,#163004,#163005,
#163006,#163007,#163008,#163009,#163010,#163011,#163012,#163013,#163014,
#163015,#163016,#163017,#163018,#163019,#163020,#163021,#163022,#163023,
#163024,#163025,#163026,#163027,#163028,#163029,#163030,#163031,#163032,
#163033,#163034,#163035,#163036,#163037,#163038,#163039,#163040,#163041,
#163042,#163043,#163044,#163045,#163046,#163047,#163048,#163049,#163050,
#163051,#163052,#163053,#163054,#163055,#163056,#163057,#163058,#163059,
#163060,#163061,#163062,#163063,#163064,#163065,#163066,#163067,#163068,
#163069,#163070,#163071,#163072,#163073,#163074,#163075,#163076,#163077,
#163078,#163079,#163080,#163081,#163082,#163083,#163084,#163085,#163086,
#163087,#163088,#163089,#163090,#163091,#163092,#163093,#163094,#163095,
#163096,#163097,#163098,#163099,#163100,#163101,#163102,#163103,#163104,
#163105,#163106,#163107,#163108,#163109,#163110,#163111,#163112,#163113,
#163114,#163115,#163116,#163117,#163118,#163119,#163120,#163121,#163122,
#163123,#163124,#163125,#163126,#163127,#163128,#163129,#163130,#163131,
#163132,#163133,#163134,#163135,#163136,#163137,#163138,#163139,#163140,
#163141,#163142,#163143,#163144,#163145,#163146,#163147,#163148,#163149,
#163150,#163151,#163152,#163153,#163154,#163155,#163156,#163157,#163158,
#163159,#163160,#163161,#163162),.UNSPECIFIED.,.F.,.F.,(4,2,2,2,2,2,2,2,
2,2,2,2,2,2,2,2,2,2,2,2,2,2,2,2,2,2,2,2,2,2,2,2,2,2,2,2,2,2,2,2,2,2,2,2,
2,2,2,2,2,2,2,2,2,2,2,2,2,2,2,2,2,2,2,2,2,2,2,2,2,2,2,2,2,2,2,2,2,2,2,2,
2,2,2,2,2,2,2,2,2,2,2,2,2,2,2,2,2,2,2,2,2,2,4),(-5.87747899666309,-5.87157346505971,
-5.85248314543527,-5.80954203483998,-5.7417957919028,-5.5608213270671,-5.5201349499391,
-5.49079992027863,-5.45907652088146,-5.40398214713538,-5.32972990832103,
-5.18388223059086,-5.15664816033201,-5.13974869721203,-5.12056346370538,
-5.08166576675479,-4.96471618283776,-4.84727000182852,-4.80935360609149,
-4.78029242579081,-4.74762140467953,-4.68751512230553,-4.60477716464133,
-4.46624328632409,-4.42985298043581,-4.4118607071297,-4.39633043336306,
-4.37304374410558,-4.28852092165992,-4.14412811602476,-4.0740255911769,
-4.03975577928991,-4.01116499979379,-3.97519554604315,-3.8897194987258,
-3.78910941156182,-3.70831001718957,-3.68410127974098,-3.66743607545008,
-3.64666970556103,-3.59749286246434,-3.51203828177267,-3.38728278927883,
-3.34503190946236,-3.31577494615111,-3.28462199156079,-3.23318206344992,
-3.14058837404119,-2.98069440326973,-2.95387314181897,-2.937723617619,-2.92095388779108,
-2.89102741751659,-2.85126289552927,-2.73768112991984,-2.61959869869359,
-2.5799480763157,-2.55075237876615,-2.51861023214061,-2.46103313057068,
-2.38136459778146,-2.24171758855171,-2.2161946518779,-2.19937971442438,
-2.17936694154875,-2.1353740560491,-2.06490903203982,-1.91470678954435,
-1.87384699542792,-1.84450183315419,-1.81281363412142,-1.75836912301625,
-1.68728513927099,-1.58856462092969,-1.50482238591236,-1.48129984342857,
-1.46573494246526,-1.44785213223697,-1.41206920115665,-1.36074929016381,
-1.26793889032233,-1.15027252609476,-1.11062990544292,-1.08143591754672,
-1.04929168040641,-0.99169818777239,-0.911991451022073,-0.772399803164502,
-0.746886891767463,-0.730073653166686,-0.710056749975434,-0.666034554412352,
-0.595490216808555,-0.445442481013401,-0.404573231916604,-0.375227423474463,
-0.343543965431134,-0.289122676732243,-0.21808301763149,-0.0627325530217655,
-0.02623614266319,-0.0117124008606042,-1.00000000102796E-6),
 .UNSPECIFIED.);
#30129=B_SPLINE_CURVE_WITH_KNOTS('',3,(#163167,#163168,#163169,#163170,
#163171,#163172,#163173,#163174,#163175,#163176,#163177,#163178,#163179,
#163180,#163181,#163182,#163183,#163184,#163185,#163186,#163187,#163188,
#163189,#163190,#163191,#163192,#163193,#163194,#163195,#163196,#163197,
#163198,#163199,#163200,#163201,#163202,#163203,#163204,#163205,#163206,
#163207,#163208,#163209,#163210,#163211,#163212,#163213,#163214,#163215,
#163216,#163217,#163218,#163219,#163220,#163221,#163222,#163223,#163224,
#163225,#163226,#163227,#163228,#163229,#163230,#163231,#163232,#163233,
#163234,#163235,#163236,#163237,#163238,#163239,#163240,#163241,#163242,
#163243,#163244,#163245,#163246,#163247,#163248,#163249,#163250,#163251,
#163252,#163253,#163254,#163255,#163256,#163257,#163258,#163259,#163260,
#163261,#163262,#163263,#163264,#163265,#163266,#163267,#163268,#163269,
#163270,#163271,#163272,#163273,#163274,#163275,#163276,#163277,#163278,
#163279,#163280,#163281,#163282,#163283,#163284,#163285,#163286,#163287,
#163288,#163289,#163290,#163291,#163292,#163293,#163294,#163295,#163296,
#163297,#163298,#163299,#163300,#163301,#163302,#163303,#163304,#163305,
#163306,#163307,#163308,#163309,#163310,#163311,#163312,#163313,#163314,
#163315,#163316,#163317,#163318,#163319,#163320,#163321,#163322,#163323,
#163324,#163325,#163326,#163327,#163328,#163329,#163330,#163331,#163332,
#163333,#163334,#163335,#163336,#163337,#163338,#163339,#163340,#163341,
#163342,#163343,#163344,#163345,#163346,#163347,#163348,#163349,#163350,
#163351,#163352,#163353,#163354,#163355,#163356,#163357,#163358,#163359,
#163360,#163361,#163362),.UNSPECIFIED.,.F.,.F.,(4,2,2,2,2,2,2,2,2,2,2,2,
2,2,2,2,2,2,2,2,2,2,2,2,2,2,2,2,2,2,2,2,2,2,2,2,2,2,2,2,2,2,2,2,2,2,2,2,
2,2,2,2,2,2,2,2,2,2,2,2,2,2,2,2,2,2,2,2,2,2,2,2,2,2,2,2,2,2,2,2,2,2,2,2,
2,2,2,2,2,2,2,2,2,2,2,2,2,4),(-11.7554193354896,-11.7397043632071,-11.7123004815342,
-11.6224226329561,-11.4373214846833,-11.3972516385993,-11.3680038502512,
-11.3360446056121,-11.2795437262896,-11.2022552555165,-11.0575886767294,
-11.0324815767214,-11.015720652302,-10.9954932470459,-10.950073918821,-10.8757255179483,
-10.7323508256304,-10.6911203504236,-10.6617252978838,-10.6301725220565,
-10.5764779266283,-10.3341276308243,-10.3038299096669,-10.2869872280702,
-10.2708941245356,-10.2443610789862,-10.1377258901351,-9.9739783796236,
-9.9312112972648,-9.90185904001811,-9.87088633993241,-9.82013679359398,
-9.78537996755567,-9.66438133917026,-9.58618606974665,-9.5619483554948,
-9.54528130209995,-9.52453598057058,-9.47550615798171,-9.39050927554147,
-9.26523325924768,-9.22293054516803,-9.19366725491827,-9.16253205978628,
-9.11118379427364,-8.86425618552492,-8.83412626996381,-8.81731620087078,
-8.80119737244526,-8.77453432150838,-8.66029891333827,-8.50548966811694,
-8.46221896920077,-8.43278589735234,-8.40194360743511,-8.35195177820095,
-8.28797649513853,-8.1881217207662,-8.11486396452449,-8.09140312005425,
-8.07479768206906,-8.0535049396504,-8.00030373832085,-7.90117681883251,
-7.78622750901807,-7.74828129370964,-7.71921680515702,-7.68656181833748,
-7.62654998195761,-7.54401711520464,-7.4063189996342,-7.36915394529351,
-7.3510242746613,-7.33553417289989,-7.31253040254177,-7.23269484403501,
-7.09052336097322,-7.01526138710406,-6.98024657890108,-6.9513993988035,
-6.91612418334169,-6.83681859754211,-6.68649309196766,-6.64000070015146,
-6.61881803077876,-6.60387345672411,-6.58153213344665,-6.51891702391052,
-6.37632972261265,-6.30508437756925,-6.27084803666434,-6.24197681600633,
-6.20582826182792,-6.12182666386515,-5.96475121216872,-5.90828696392928,
-5.88688495602323,-5.87747899666309),.UNSPECIFIED.);
#30130=B_SPLINE_CURVE_WITH_KNOTS('',3,(#163363,#163364,#163365,#163366,
#163367,#163368,#163369,#163370,#163371,#163372,#163373,#163374,#163375,
#163376,#163377,#163378,#163379,#163380,#163381,#163382,#163383,#163384,
#163385,#163386,#163387,#163388,#163389,#163390,#163391,#163392,#163393,
#163394,#163395,#163396,#163397,#163398,#163399,#163400,#163401,#163402,
#163403,#163404,#163405,#163406,#163407,#163408,#163409,#163410,#163411,
#163412,#163413,#163414,#163415,#163416,#163417,#163418,#163419,#163420,
#163421,#163422,#163423,#163424,#163425,#163426,#163427,#163428,#163429,
#163430,#163431,#163432,#163433,#163434,#163435,#163436,#163437,#163438,
#163439,#163440,#163441,#163442,#163443,#163444,#163445,#163446,#163447,
#163448,#163449,#163450,#163451,#163452,#163453,#163454,#163455,#163456,
#163457,#163458,#163459,#163460,#163461,#163462,#163463,#163464,#163465,
#163466,#163467,#163468,#163469,#163470,#163471,#163472,#163473,#163474,
#163475,#163476,#163477,#163478,#163479,#163480,#163481,#163482,#163483,
#163484,#163485,#163486,#163487,#163488,#163489,#163490,#163491,#163492,
#163493,#163494,#163495,#163496,#163497,#163498,#163499,#163500,#163501,
#163502,#163503,#163504,#163505,#163506,#163507,#163508,#163509,#163510,
#163511,#163512,#163513,#163514,#163515,#163516,#163517,#163518,#163519,
#163520,#163521,#163522,#163523,#163524,#163525,#163526,#163527,#163528,
#163529,#163530,#163531,#163532,#163533,#163534,#163535,#163536,#163537,
#163538,#163539,#163540,#163541,#163542,#163543,#163544,#163545,#163546,
#163547,#163548,#163549,#163550,#163551,#163552,#163553,#163554,#163555,
#163556,#163557,#163558,#163559,#163560,#163561,#163562,#163563,#163564,
#163565,#163566,#163567,#163568),.UNSPECIFIED.,.F.,.F.,(4,2,2,2,2,2,2,2,
2,2,2,2,2,2,2,2,2,2,2,2,2,2,2,2,2,2,2,2,2,2,2,2,2,2,2,2,2,2,2,2,2,2,2,2,
2,2,2,2,2,2,2,2,2,2,2,2,2,2,2,2,2,2,2,2,2,2,2,2,2,2,2,2,2,2,2,2,2,2,2,2,
2,2,2,2,2,2,2,2,2,2,2,2,2,2,2,2,2,2,2,2,2,2,4),(-11.7555598459133,-11.7440048067695,
-11.720851736883,-11.638659223459,-11.4953665694064,-11.4227083740445,-11.3880596555871,
-11.3592030410641,-11.3235236457627,-11.2407482262352,-11.0700802910848,
-11.0383780099431,-11.0205040090326,-11.0024721687282,-10.9699455702908,
-10.9256322936732,-10.7740119075505,-10.7099728002658,-10.6767884487821,
-10.6478103432566,-10.6101592509722,-10.5120284451198,-10.4250797153776,
-10.3301968685769,-10.3021758802065,-10.2857871637331,-10.2692906627363,
-10.2407356533069,-10.1407993755448,-9.97324266646984,-9.93081799300448,
-9.90151489474412,-9.87043899193725,-9.81911755145721,-9.78377384073625,
-9.65861981349754,-9.58575417153447,-9.56169656834753,-9.54504351230296,
-9.5241730780038,-9.47424208902618,-9.38638792719994,-9.26501304267273,
-9.22276472422519,-9.19350551792324,-9.16234684096919,-9.110888961732,-9.01770518171239,
-8.85868257304902,-8.8317053223883,-8.81552408718923,-8.79879050856922,
-8.76905203613641,-8.72963687788532,-8.61820280554415,-8.49733444467963,
-8.45764792686622,-8.42844487004975,-8.39631271403875,-8.3388109906517,
-8.25931711823037,-8.11940588144879,-8.09384484094786,-8.07702334324308,
-8.05702598803933,-8.01314304416159,-7.94297521434756,-7.79218740176557,
-7.75136442710309,-7.72202168256262,-7.69031479211883,-7.63577899031293,
-7.5645206967366,-7.46578969299074,-7.38269289579539,-7.35900554606823,
-7.34356717687921,-7.32582497937522,-7.29082160692587,-7.24112945306772,
-7.14593443646003,-7.02778013672203,-6.9881251327,-6.95892680798051,-6.92678233802362,
-6.86920288508827,-6.78953331989904,-6.64986690084062,-6.62434048946161,
-6.60752394225729,-6.58751010528971,-6.54351767881986,-6.4730578617152,
-6.32282194091014,-6.28196012859145,-6.25261265899417,-6.2209212087621,
-6.16646900481442,-6.09537301881674,-5.99664407705398,-5.91290865712216,
-5.88938277793605,-5.87740991053728),.UNSPECIFIED.);
#30131=B_SPLINE_CURVE_WITH_KNOTS('',3,(#163573,#163574,#163575,#163576,
#163577,#163578,#163579,#163580,#163581,#163582,#163583,#163584,#163585,
#163586,#163587,#163588,#163589,#163590,#163591,#163592,#163593,#163594,
#163595,#163596,#163597,#163598,#163599,#163600,#163601,#163602,#163603,
#163604,#163605,#163606,#163607,#163608,#163609,#163610,#163611,#163612,
#163613,#163614,#163615,#163616,#163617,#163618,#163619,#163620,#163621,
#163622,#163623,#163624,#163625,#163626,#163627,#163628,#163629,#163630,
#163631,#163632,#163633,#163634,#163635,#163636,#163637,#163638,#163639,
#163640,#163641,#163642,#163643,#163644,#163645,#163646,#163647,#163648,
#163649,#163650,#163651,#163652,#163653,#163654,#163655,#163656,#163657,
#163658,#163659,#163660,#163661,#163662,#163663,#163664,#163665,#163666,
#163667,#163668,#163669,#163670,#163671,#163672,#163673,#163674,#163675,
#163676,#163677,#163678,#163679,#163680,#163681,#163682,#163683,#163684,
#163685,#163686,#163687,#163688,#163689,#163690,#163691,#163692,#163693,
#163694,#163695,#163696,#163697,#163698,#163699,#163700,#163701,#163702,
#163703,#163704,#163705,#163706,#163707,#163708,#163709,#163710,#163711,
#163712,#163713,#163714,#163715,#163716,#163717,#163718,#163719,#163720,
#163721,#163722,#163723,#163724,#163725,#163726,#163727,#163728,#163729,
#163730,#163731,#163732,#163733,#163734,#163735,#163736,#163737,#163738,
#163739,#163740,#163741,#163742,#163743,#163744,#163745,#163746,#163747,
#163748,#163749,#163750,#163751,#163752,#163753,#163754,#163755,#163756,
#163757,#163758,#163759,#163760,#163761,#163762,#163763,#163764,#163765,
#163766,#163767,#163768,#163769,#163770,#163771,#163772),.UNSPECIFIED.,
 .F.,.F.,(4,2,2,2,2,2,2,2,2,2,2,2,2,2,2,2,2,2,2,2,2,2,2,2,2,2,2,2,2,2,2,
2,2,2,2,2,2,2,2,2,2,2,2,2,2,2,2,2,2,2,2,2,2,2,2,2,2,2,2,2,2,2,2,2,2,2,2,
2,2,2,2,2,2,2,2,2,2,2,2,2,2,2,2,2,2,2,2,2,2,2,2,2,2,2,2,2,2,2,2,4),(-17.6325413712744,
-17.6173187457267,-17.5904856539766,-17.4593952055629,-17.3626719016611,
-17.2965513353061,-17.2628975944784,-17.2339877545232,-17.1970562833595,
-17.1096153606531,-16.9866238803363,-16.9456921605042,-16.9149211009742,
-16.89722700416,-16.8790024480916,-16.8454419442937,-16.6774854446449,-16.5951359694173,
-16.5595115378792,-16.5306635546779,-16.4959833036162,-16.4230634716081,
-16.2799158071296,-16.1979903684606,-16.1748579249094,-16.159351597272,
-16.1412896347085,-16.1044983710977,-15.9664384603955,-15.8838265873493,
-15.8237812112649,-15.7911238400417,-15.762064995908,-15.7241374690325,
-15.6077611350589,-15.4903145511018,-15.4510846007422,-15.4318445322676,
-15.4149715433235,-15.387893779987,-15.2412814902409,-15.1673191911459,
-15.1123642372609,-15.0806678097385,-15.0513283384161,-15.0105871103192,
-14.8035043822286,-14.7516665127793,-14.7156392273614,-14.697713275884,
-14.6821643154854,-14.6587417864808,-14.5775135039217,-14.4344046562726,
-14.3622961518627,-14.3273191292728,-14.2984747582599,-14.2631678401768,
-14.1835735132702,-14.0317209167044,-13.9865811168811,-13.9656290196518,
-13.9489901467216,-13.925063527677,-13.8408484917158,-13.6623672802532,
-13.6250349005944,-13.5960376800389,-13.5630417581693,-13.5009852778125,
-13.4139140657653,-13.2642609992235,-13.2387213061367,-13.2243802532728,
-13.2078391596062,-13.1790510099162,-13.0769001636591,-12.9127536585608,
-12.8700218757182,-12.8406761560905,-12.8096957282282,-12.7588959517633,
-12.7240867360307,-12.6027175415787,-12.5250678189431,-12.5008241580527,
-12.484157186304,-12.4634173481096,-12.4144228007699,-12.3295333231515,
-12.2041551846857,-12.1618359118408,-12.1325711761753,-12.1014427265716,
-12.0501266293664,-11.9578768100303,-11.7971824674383,-11.770504412013,
-11.7559673807982,-11.7554193354896),.UNSPECIFIED.);
#30132=B_SPLINE_CURVE_WITH_KNOTS('',3,(#163774,#163775,#163776,#163777,
#163778,#163779,#163780,#163781,#163782,#163783,#163784,#163785,#163786,
#163787,#163788,#163789,#163790,#163791,#163792,#163793,#163794,#163795,
#163796,#163797,#163798,#163799,#163800,#163801,#163802,#163803,#163804,
#163805,#163806,#163807,#163808,#163809,#163810,#163811,#163812,#163813,
#163814,#163815,#163816,#163817,#163818,#163819,#163820,#163821,#163822,
#163823,#163824,#163825,#163826,#163827,#163828,#163829,#163830,#163831,
#163832,#163833,#163834,#163835,#163836,#163837,#163838,#163839,#163840,
#163841,#163842,#163843,#163844,#163845,#163846,#163847,#163848,#163849,
#163850,#163851,#163852,#163853,#163854,#163855,#163856,#163857,#163858,
#163859,#163860,#163861,#163862,#163863,#163864,#163865,#163866,#163867,
#163868,#163869,#163870,#163871,#163872,#163873,#163874,#163875,#163876,
#163877,#163878,#163879,#163880,#163881,#163882,#163883,#163884,#163885,
#163886,#163887,#163888,#163889,#163890,#163891,#163892,#163893,#163894,
#163895,#163896,#163897,#163898,#163899,#163900,#163901,#163902,#163903,
#163904,#163905,#163906,#163907,#163908,#163909,#163910,#163911,#163912,
#163913,#163914,#163915,#163916,#163917,#163918,#163919,#163920,#163921,
#163922,#163923,#163924,#163925,#163926,#163927,#163928,#163929,#163930,
#163931,#163932,#163933,#163934,#163935,#163936,#163937,#163938,#163939,
#163940,#163941,#163942,#163943,#163944,#163945,#163946,#163947,#163948,
#163949,#163950,#163951,#163952,#163953,#163954,#163955,#163956,#163957,
#163958,#163959,#163960,#163961,#163962,#163963,#163964,#163965,#163966,
#163967,#163968,#163969,#163970,#163971,#163972,#163973,#163974,#163975,
#163976,#163977,#163978,#163979,#163980,#163981,#163982,#163983,#163984,
#163985),.UNSPECIFIED.,.F.,.F.,(4,2,2,2,2,2,2,2,2,2,2,2,2,2,2,2,2,2,2,2,
2,2,2,2,2,2,2,2,2,2,2,2,2,2,2,2,2,2,2,2,2,2,2,2,2,2,2,2,2,2,2,2,2,2,2,2,
2,2,2,2,2,2,2,2,2,2,2,2,2,2,2,2,2,2,2,2,2,2,2,2,2,2,2,2,2,2,2,2,2,2,2,2,
2,2,2,2,2,2,2,2,2,2,2,2,2,4),(-5.87740991053728,-5.87381634389079,-5.85593259626545,
-5.82014988976725,-5.76883250195084,-5.67600323296091,-5.55832568302647,
-5.51867964714232,-5.4894831557696,-5.45733617317984,-5.39973779655696,
-5.32002434367809,-5.18042059592695,-5.1549054723282,-5.13809078986479,
-5.11807218524499,-5.07404630556962,-5.00349615672977,-4.8534351379586,
-4.812562417678,-4.78321409938624,-4.75152791616519,-4.69710190387738,-4.62605603914143,
-4.52732961968957,-4.44348970680189,-4.41997195299682,-4.4044070877698,
-4.38652049228867,-4.35072022791597,-4.29936522418603,-4.20660022685623,
-4.08893228353677,-4.04928748385735,-4.02009183715372,-3.98794572217029,
-3.93034870130074,-3.85063688066746,-3.71103790495148,-3.68552365771353,
-3.66870947346294,-3.64869136252443,-3.60466624131641,-3.53411678403665,
-3.38406246324267,-3.34319073573122,-3.31384322885109,-3.28215800891038,
-3.22773389296099,-3.15669072814478,-3.05796711401422,-2.97412817625273,
-2.95061115117794,-2.93519943267184,-2.91738499773655,-2.88198087389371,
-2.83145493570879,-2.73748120548732,-2.6195895690735,-2.57994205599912,
-2.55074675201768,-2.51860323799425,-2.46101795597002,-2.38133107091658,
-2.24170745971876,-2.21618866822998,-2.19937427274828,-2.17935940028968,
-2.13535287861461,-2.06485158880524,-1.91471635824081,-1.8738518013772,
-1.84450597083593,-1.81281948687812,-1.75838467887102,-1.68731964167472,
-1.58859899517801,-1.50481364012982,-1.48129449819807,-1.46573010873508,
-1.44784576290461,-1.41205434491034,-1.36071658586461,-1.26793430907094,
-1.15027077968689,-1.11062820157249,-1.08143421502927,-1.04928995090465,
-0.991696319260591,-0.911989278801862,-0.772397971886967,-0.746885124704753,
-0.730071892244856,-0.710054950998422,-0.666032522475088,-0.595487572620013,
-0.445440918675119,-0.404571584945724,-0.375225760690415,-0.343542325363129,
-0.289121185952612,-0.218081824129735,-0.0627285934085948,-0.0262342865270621,
-0.011711063373005,-1.00000000198032E-6),.UNSPECIFIED.);
#30133=B_SPLINE_CURVE_WITH_KNOTS('',3,(#163986,#163987,#163988,#163989),
 .UNSPECIFIED.,.F.,.F.,(4,4),(-12.3895192570164,-12.3895147069527),
 .UNSPECIFIED.);
#30134=B_SPLINE_CURVE_WITH_KNOTS('',3,(#163994,#163995,#163996,#163997,
#163998,#163999,#164000,#164001,#164002,#164003,#164004,#164005,#164006,
#164007,#164008,#164009,#164010,#164011,#164012,#164013,#164014,#164015,
#164016,#164017,#164018,#164019,#164020,#164021,#164022,#164023,#164024,
#164025,#164026,#164027,#164028,#164029,#164030,#164031,#164032,#164033,
#164034,#164035,#164036,#164037,#164038,#164039,#164040,#164041,#164042,
#164043,#164044,#164045,#164046,#164047,#164048,#164049,#164050,#164051,
#164052,#164053,#164054,#164055,#164056,#164057,#164058,#164059,#164060,
#164061,#164062,#164063,#164064,#164065,#164066,#164067,#164068,#164069,
#164070,#164071,#164072,#164073,#164074,#164075,#164076,#164077,#164078,
#164079,#164080,#164081,#164082,#164083,#164084,#164085,#164086,#164087,
#164088,#164089,#164090,#164091,#164092,#164093,#164094,#164095,#164096,
#164097,#164098,#164099,#164100,#164101,#164102,#164103,#164104,#164105,
#164106,#164107,#164108,#164109,#164110,#164111,#164112,#164113,#164114,
#164115,#164116,#164117,#164118,#164119,#164120,#164121,#164122,#164123,
#164124,#164125,#164126,#164127,#164128,#164129,#164130,#164131,#164132,
#164133,#164134,#164135,#164136,#164137,#164138,#164139,#164140,#164141,
#164142,#164143,#164144,#164145,#164146,#164147,#164148,#164149,#164150,
#164151,#164152,#164153,#164154,#164155,#164156,#164157,#164158,#164159,
#164160,#164161,#164162,#164163,#164164,#164165,#164166,#164167,#164168,
#164169,#164170,#164171,#164172,#164173,#164174,#164175,#164176,#164177,
#164178,#164179,#164180,#164181,#164182,#164183,#164184,#164185,#164186,
#164187,#164188,#164189,#164190,#164191,#164192,#164193,#164194,#164195,
#164196,#164197,#164198,#164199,#164200,#164201,#164202,#164203,#164204,
#164205),.UNSPECIFIED.,.F.,.F.,(4,2,2,2,2,2,2,2,2,2,2,2,2,2,2,2,2,2,2,2,
2,2,2,2,2,2,2,2,2,2,2,2,2,2,2,2,2,2,2,2,2,2,2,2,2,2,2,2,2,2,2,2,2,2,2,2,
2,2,2,2,2,2,2,2,2,2,2,2,2,2,2,2,2,2,2,2,2,2,2,2,2,2,2,2,2,2,2,2,2,2,2,2,
2,2,2,2,2,2,2,2,2,2,2,2,2,4),(-23.5087927899511,-23.4968313698322,-23.4733204154092,
-23.389522330444,-23.290833133669,-23.2198070544226,-23.1653958453539,-23.1337185956986,
-23.1043786318951,-23.0635177792145,-22.9134718397736,-22.8429454197137,
-22.7989334068048,-22.7789206549434,-22.7621106639869,-22.7366024110544,
-22.5970484570337,-22.5173636578392,-22.4597840963954,-22.4276466482817,
-22.3984581704448,-22.3588220335695,-22.2411753725644,-22.1484200315698,
-22.0970770954317,-22.0612857337457,-22.043403627955,-22.0278426792721,
-22.0043309391874,-21.9205308578202,-21.8218385050015,-21.7508098285477,
-21.6963967121042,-21.6647184193347,-21.6353775280291,-21.5945154493004,
-21.4444635489012,-21.3739355004649,-21.3299223152833,-21.3099089593149,
-21.2930984210289,-21.2675892800697,-21.1280304760964,-21.0483434323024,
-20.9907621643042,-20.958623710459,-20.9294342919689,-20.8897968349208,
-20.7721434073732,-20.6793555736253,-20.6280297185314,-20.5922461116202,
-20.5743650417727,-20.5588030561401,-20.5352869931688,-20.4515407559718,
-20.3528454009096,-20.2817886006594,-20.2273604978313,-20.195678845116,
-20.1663379205417,-20.1254810247372,-19.9753323695748,-19.9048518541056,
-19.8608559714563,-19.8408448522938,-19.8240330293425,-19.7985173807911,
-19.6589229238285,-19.5792579494841,-19.5216858060394,-19.4895481517101,
-19.4603572646099,-19.4207143584248,-19.302809919845,-19.2087262937014,
-19.1582846275073,-19.1229230165088,-19.1051181396125,-19.0897066218821,
-19.0661782991244,-18.9825364446692,-18.8838381644915,-18.8127353675039,
-18.7582831250707,-18.7265964880695,-18.6972561479971,-18.6564088951883,
-18.5061019142493,-18.4357020284634,-18.3917359069127,-18.3717289409319,
-18.3549153292737,-18.329389359514,-18.1897347780319,-18.1101103762315,
-18.0525556034341,-18.0204201202029,-17.9912273562865,-17.9515758407652,
-17.8332048197293,-17.7198606513816,-17.6801363305922,-17.650232961444,
-17.6334692206125,-17.6325413712744),.UNSPECIFIED.);
#30135=B_SPLINE_CURVE_WITH_KNOTS('',3,(#164206,#164207,#164208,#164209,
#164210,#164211,#164212,#164213,#164214,#164215,#164216,#164217,#164218,
#164219,#164220,#164221,#164222,#164223,#164224,#164225,#164226,#164227,
#164228,#164229,#164230,#164231,#164232,#164233,#164234,#164235,#164236,
#164237,#164238,#164239,#164240,#164241,#164242,#164243,#164244,#164245,
#164246,#164247,#164248,#164249,#164250,#164251,#164252,#164253,#164254,
#164255,#164256,#164257,#164258,#164259,#164260,#164261,#164262,#164263,
#164264,#164265,#164266,#164267,#164268,#164269,#164270,#164271,#164272,
#164273,#164274,#164275,#164276,#164277,#164278,#164279,#164280,#164281,
#164282,#164283,#164284,#164285,#164286,#164287,#164288,#164289,#164290,
#164291,#164292,#164293,#164294,#164295,#164296,#164297,#164298,#164299,
#164300,#164301,#164302,#164303,#164304,#164305,#164306,#164307,#164308,
#164309,#164310,#164311,#164312,#164313,#164314,#164315,#164316,#164317,
#164318,#164319,#164320,#164321,#164322,#164323,#164324,#164325,#164326,
#164327,#164328,#164329,#164330,#164331,#164332,#164333,#164334,#164335,
#164336,#164337,#164338,#164339,#164340,#164341,#164342,#164343,#164344,
#164345,#164346,#164347,#164348,#164349,#164350,#164351,#164352,#164353,
#164354,#164355,#164356,#164357,#164358,#164359,#164360,#164361,#164362,
#164363,#164364,#164365,#164366,#164367,#164368,#164369,#164370,#164371,
#164372,#164373,#164374,#164375,#164376,#164377,#164378,#164379,#164380,
#164381,#164382,#164383,#164384,#164385,#164386,#164387,#164388,#164389,
#164390,#164391,#164392,#164393,#164394,#164395,#164396,#164397,#164398,
#164399,#164400,#164401,#164402,#164403,#164404,#164405,#164406,#164407,
#164408,#164409,#164410,#164411,#164412,#164413,#164414,#164415,#164416,
#164417),.UNSPECIFIED.,.F.,.F.,(4,2,2,2,2,2,2,2,2,2,2,2,2,2,2,2,2,2,2,2,
2,2,2,2,2,2,2,2,2,2,2,2,2,2,2,2,2,2,2,2,2,2,2,2,2,2,2,2,2,2,2,2,2,2,2,2,
2,2,2,2,2,2,2,2,2,2,2,2,2,2,2,2,2,2,2,2,2,2,2,2,2,2,2,2,2,2,2,2,2,2,2,2,
2,2,2,2,2,2,2,2,2,2,2,2,2,4),(-12.3895147069527,-12.377807257671,-12.3632813542591,
-12.3267754286178,-12.1714619301749,-12.1004236322622,-12.0460030633795,
-12.014320365083,-11.9849753549371,-11.9441074748392,-11.7940357195205,
-11.7234971735021,-11.6794775922804,-11.6594613985178,-11.642648516205,
-11.6171358753871,-11.4775579155955,-11.397859412922,-11.3402699488588,
-11.3081269733203,-11.2789334750683,-11.2392905204773,-11.1216236031218,
-11.028852099042,-10.9775004647937,-10.9417030101661,-10.9238178400865,
-10.9082542111278,-10.8847384017566,-10.8009244242619,-10.702215098039,
-10.6311739600063,-10.5767513591747,-10.5450675955751,-10.5157216662698,
-10.4748526208287,-10.3247740369237,-10.2542343319478,-10.2102137547144,
-10.1901969838709,-10.1733835471008,-10.1478699644682,-10.0082868665789,
-9.92858634718545,-9.87099527794653,-9.83885131344926,-9.80965686943057,
-9.77001255569823,-9.65233662531578,-9.55951046683855,-9.50818996136906,
-9.4724069399824,-9.45452401270246,-9.4389589417329,-9.41543612792821,-9.33170680362448,
-9.23299455169726,-9.16191201462924,-9.10746762671221,-9.07577929839688,
-9.04643380002528,-9.0055732668675,-8.85535106321629,-8.7848842268555,-8.74089047733835,
-8.72087740837846,-8.70406230594376,-8.67853931489024,-8.53890406411337,
-8.45923850498894,-8.40166230375907,-8.36952009599412,-8.34032390293436,
-8.30067194889025,-8.18261088356668,-8.08785230533081,-8.03785700456833,
-8.00270826578259,-7.98494028438201,-7.96951250192704,-7.9458893753669,
-7.86262072124033,-7.76390596017912,-7.69268698263105,-7.63817216266634,
-7.60647064912219,-7.57712887290436,-7.53630054769812,-7.38561225972224,
-7.31539114302896,-7.27148935423217,-7.25149001879428,-7.23467061448617,
-7.2091182507377,-7.06928624042655,-6.98976200267619,-6.93224810822009,
-6.90011556261007,-6.87091528493107,-6.83123751778278,-6.71128806744215,
-6.59914285794704,-6.55961080606437,-6.52980993051937,-6.51306470671676,
-6.51219502816774),.UNSPECIFIED.);
#30136=B_SPLINE_CURVE_WITH_KNOTS('',3,(#164424,#164425,#164426,#164427,
#164428,#164429,#164430,#164431,#164432,#164433,#164434,#164435,#164436,
#164437,#164438,#164439,#164440,#164441,#164442,#164443,#164444,#164445,
#164446,#164447,#164448,#164449,#164450,#164451,#164452,#164453,#164454,
#164455,#164456,#164457,#164458,#164459,#164460,#164461,#164462,#164463,
#164464,#164465,#164466,#164467,#164468,#164469,#164470,#164471,#164472,
#164473,#164474,#164475,#164476,#164477,#164478,#164479,#164480,#164481,
#164482,#164483,#164484,#164485,#164486,#164487,#164488,#164489,#164490,
#164491,#164492,#164493,#164494,#164495,#164496,#164497,#164498,#164499,
#164500,#164501,#164502,#164503,#164504,#164505,#164506,#164507,#164508,
#164509,#164510,#164511,#164512,#164513,#164514,#164515,#164516,#164517,
#164518,#164519,#164520,#164521,#164522,#164523,#164524,#164525,#164526,
#164527,#164528,#164529,#164530,#164531,#164532,#164533,#164534,#164535,
#164536,#164537,#164538,#164539,#164540,#164541,#164542,#164543,#164544,
#164545,#164546,#164547,#164548,#164549,#164550,#164551,#164552,#164553,
#164554,#164555,#164556,#164557,#164558,#164559,#164560,#164561,#164562,
#164563,#164564,#164565,#164566,#164567,#164568,#164569,#164570,#164571,
#164572,#164573,#164574,#164575,#164576,#164577,#164578,#164579,#164580,
#164581,#164582,#164583,#164584,#164585,#164586,#164587,#164588,#164589,
#164590,#164591,#164592,#164593,#164594,#164595,#164596,#164597,#164598,
#164599,#164600,#164601,#164602,#164603,#164604,#164605,#164606,#164607,
#164608,#164609,#164610,#164611,#164612,#164613,#164614,#164615,#164616,
#164617,#164618,#164619,#164620,#164621,#164622,#164623,#164624,#164625,
#164626,#164627),.UNSPECIFIED.,.F.,.F.,(4,2,2,2,2,2,2,2,2,2,2,2,2,2,2,2,
2,2,2,2,2,2,2,2,2,2,2,2,2,2,2,2,2,2,2,2,2,2,2,2,2,2,2,2,2,2,2,2,2,2,2,2,
2,2,2,2,2,2,2,2,2,2,2,2,2,2,2,2,2,2,2,2,2,2,2,2,2,2,2,2,2,2,2,2,2,2,2,2,
2,2,2,2,2,2,2,2,2,2,2,2,2,4),(-29.154596735575,-29.0680469775082,-29.0366008769626,
-29.009649364794,-28.980358946728,-28.9398354719708,-28.7890301469152,-28.718512760047,
-28.6745063857758,-28.6544961985365,-28.6376883621472,-28.6121833791968,
-28.4726473149498,-28.392972725798,-28.3354005428435,-28.3032672134614,
-28.2740824766732,-28.2344514203136,-28.1168198660072,-28.0240766912348,
-27.9727401591336,-27.9369533008584,-27.9190734718067,-27.9035145225909,
-27.8800058295461,-27.7962157970364,-27.6975360912537,-27.6265168456998,
-27.572110870966,-27.5404366680126,-27.5110995257468,-27.4702426019138,
-27.3202111034496,-27.2496914600294,-27.2056836775571,-27.1856728499932,
-27.1688644757543,-27.143358676646,-27.0038181472543,-26.9241410085203,
-26.8665669832593,-26.8344326256126,-26.8052469549149,-26.7656146303642,
-26.647979311855,-26.555233169304,-26.5038949944387,-26.4681069909873,-26.4502265897825,
-26.4346671426812,-26.4111576973591,-26.3273649835731,-26.2286821200446,
-26.1576606018781,-26.1032528861554,-26.0715776696288,-26.0422395885759,
-26.0013813573234,-25.8513450578567,-25.7808231578136,-25.7368139670951,
-25.7168024991859,-25.69999358708,-25.6744869717877,-25.534941977107,-25.4552622887116,
-25.3976864210865,-25.3655510351428,-25.3363644305056,-25.2967308377232,
-25.1790917548905,-25.0863426444483,-25.0350028267789,-24.9992136781203,
-24.9813327047451,-24.9657727597423,-24.9422625621174,-24.8584671670318,
-24.7597811456606,-24.6887573547836,-24.6343478980047,-24.6026716678716,
-24.5733326480036,-24.5324731092984,-24.3824320085824,-24.3119078518984,
-24.26789725291,-24.2478851446385,-24.231075694648,-24.2055682631395,-24.0660188029948,
-23.9863365648802,-23.9287588548426,-23.8966224405704,-23.8674349019629,
-23.8278000409034,-23.7101571933654,-23.6174051123933,-23.566063653479,
-23.5302733603428,-23.5123918149171,-23.5087927899511),.UNSPECIFIED.);
#30137=B_SPLINE_CURVE_WITH_KNOTS('',3,(#164628,#164629,#164630,#164631,
#164632,#164633,#164634,#164635,#164636,#164637,#164638,#164639,#164640,
#164641,#164642,#164643,#164644,#164645,#164646,#164647,#164648,#164649,
#164650,#164651,#164652,#164653,#164654,#164655,#164656,#164657,#164658,
#164659,#164660,#164661,#164662,#164663,#164664,#164665,#164666,#164667,
#164668,#164669,#164670,#164671,#164672,#164673,#164674,#164675,#164676,
#164677,#164678,#164679,#164680,#164681,#164682,#164683,#164684,#164685,
#164686,#164687,#164688,#164689,#164690,#164691,#164692,#164693,#164694,
#164695,#164696,#164697,#164698,#164699,#164700,#164701,#164702,#164703,
#164704,#164705,#164706,#164707,#164708,#164709,#164710,#164711,#164712,
#164713,#164714,#164715,#164716,#164717,#164718,#164719,#164720,#164721,
#164722,#164723,#164724,#164725,#164726,#164727,#164728,#164729,#164730,
#164731,#164732,#164733,#164734,#164735,#164736,#164737,#164738,#164739,
#164740,#164741,#164742,#164743,#164744,#164745,#164746,#164747,#164748,
#164749,#164750,#164751,#164752,#164753,#164754,#164755,#164756,#164757,
#164758,#164759,#164760,#164761,#164762,#164763,#164764,#164765,#164766,
#164767,#164768,#164769,#164770,#164771,#164772,#164773,#164774,#164775,
#164776,#164777,#164778,#164779,#164780,#164781,#164782,#164783,#164784,
#164785,#164786,#164787,#164788,#164789,#164790,#164791,#164792,#164793,
#164794,#164795,#164796,#164797,#164798,#164799,#164800,#164801,#164802,
#164803,#164804,#164805,#164806,#164807,#164808,#164809,#164810,#164811,
#164812,#164813,#164814,#164815,#164816,#164817,#164818,#164819,#164820,
#164821,#164822,#164823,#164824,#164825,#164826,#164827,#164828,#164829),
 .UNSPECIFIED.,.F.,.F.,(4,2,2,2,2,2,2,2,2,2,2,2,2,2,2,2,2,2,2,2,2,2,2,2,
2,2,2,2,2,2,2,2,2,2,2,2,2,2,2,2,2,2,2,2,2,2,2,2,2,2,2,2,2,2,2,2,2,2,2,2,
2,2,2,2,2,2,2,2,2,2,2,2,2,2,2,2,2,2,2,2,2,2,2,2,2,2,2,2,2,2,2,2,2,2,2,2,
2,2,2,2,4),(-6.51219502816774,-6.49689472217411,-6.46997129052892,-6.33929047170556,
-6.1947859721142,-6.1544204919948,-6.12512902835179,-6.09328081973178,-6.0374576478002,
-5.96164855254946,-5.82372445141555,-5.79375782895583,-5.77621192813791,
-5.75779046594482,-5.72318471319209,-5.67467744732633,-5.49150139516094,
-5.44913881236605,-5.41986448638267,-5.38874266249544,-5.33748016546924,
-5.27244324153535,-5.16593489972955,-5.07913909304673,-5.05515738971787,
-5.0396742219655,-5.02205748198278,-4.98772940484716,-4.93942033450216,
-4.75043426596149,-4.6977392235594,-4.66636225158126,-4.63688499827377,
-4.59510699534641,-4.56898087592549,-4.49447943642386,-4.34936201571812,
-4.32198775929466,-4.30506608009003,-4.28593306721165,-4.2473386632098,
-4.13084640770648,-4.01243634219351,-3.97453782714609,-3.94547904169831,
-3.91279926357094,-3.85263912610603,-3.76978323189877,-3.63075714172454,
-3.5948194464321,-3.57690857557399,-3.56135272833126,-3.53789146688165,
-3.45009573499749,-3.26259524537362,-3.21925017479097,-3.18980575538939,
-3.15898330002587,-3.10910265272203,-3.04533935388429,-2.94551417146924,
-2.87306010393177,-2.84904131658227,-2.83239378132126,-2.81150257496362,
-2.76140175815404,-2.67298551663729,-2.55248337600327,-2.51022340991007,
-2.48096579391245,-2.44981682268409,-2.39839539525427,-2.30730525960288,
-2.14514366857188,-2.11871346457313,-2.10421914390871,-2.08789929894286,
-2.06021402931002,-1.96797504792757,-1.78729165291815,-1.74656534219371,
-1.71722549523362,-1.68551857864315,-1.63051638189085,-1.55645807035467,
-1.41006063025761,-1.38293344364847,-1.36605133247423,-1.34682686522701,
-1.30769669162197,-1.1903996757451,-1.07369608520175,-1.03576984837626,
-1.00670841764685,-0.974044489441254,-0.913975528066767,-0.8313170466221,
-0.693102441749089,-0.656423357532267,-0.638380021990908,-0.634450996246336),
 .UNSPECIFIED.);
#30138=B_SPLINE_CURVE_WITH_KNOTS('',3,(#164835,#164836,#164837,#164838,
#164839,#164840,#164841,#164842,#164843,#164844,#164845,#164846,#164847,
#164848,#164849,#164850,#164851,#164852,#164853,#164854,#164855,#164856,
#164857,#164858,#164859,#164860,#164861,#164862,#164863,#164864,#164865,
#164866,#164867,#164868,#164869,#164870,#164871,#164872,#164873,#164874,
#164875,#164876,#164877,#164878,#164879,#164880,#164881,#164882,#164883,
#164884,#164885,#164886,#164887,#164888,#164889,#164890,#164891,#164892,
#164893,#164894,#164895,#164896,#164897,#164898,#164899,#164900,#164901,
#164902,#164903,#164904,#164905,#164906,#164907,#164908,#164909,#164910,
#164911,#164912,#164913,#164914,#164915,#164916,#164917,#164918,#164919,
#164920,#164921,#164922,#164923,#164924,#164925,#164926,#164927,#164928,
#164929,#164930,#164931,#164932,#164933,#164934,#164935,#164936,#164937,
#164938,#164939,#164940,#164941,#164942,#164943,#164944,#164945,#164946,
#164947,#164948,#164949,#164950,#164951,#164952,#164953,#164954,#164955,
#164956,#164957,#164958,#164959,#164960,#164961,#164962,#164963,#164964,
#164965,#164966,#164967,#164968,#164969,#164970,#164971,#164972),
 .UNSPECIFIED.,.F.,.F.,(4,2,2,2,2,2,2,2,2,2,2,2,2,2,2,2,2,2,2,2,2,2,2,2,
2,2,2,2,2,2,2,2,2,2,2,2,2,2,2,2,2,2,2,2,2,2,2,2,2,2,2,2,2,2,2,2,2,2,2,2,
2,2,2,2,2,2,2,2,4),(-3.2456129003934,-3.24151973927817,-3.23300392887545,
-3.21464854915612,-3.13705852807635,-2.9528080579948,-2.89330519802188,
-2.87273145681729,-2.85933340186152,-2.84651462975601,-2.82887122294633,
-2.78603698053238,-2.72313221862484,-2.63586417862452,-2.53328362850053,
-2.51288600487319,-2.50369709015821,-2.49660483534415,-2.48825976819539,
-2.47268283796893,-2.35265936259145,-2.19298651208667,-2.16604760658548,
-2.1498637084089,-2.13722877649194,-2.12336785393765,-2.10063386868242,
-2.01050169504874,-1.90468427825519,-1.78700536024996,-1.7664172081085,
-1.75838355622291,-1.75176386535067,-1.74460349259306,-1.73282431405224,
-1.68904423506647,-1.60068618089287,-1.41986982946812,-1.38883000707498,
-1.37303502142016,-1.36047465266443,-1.34624116192914,-1.32175821863759,
-1.18262002171282,-1.03751793083754,-1.0189995758897,-1.01006323001346,
-1.00299723872,-0.994331961508112,-0.97719335369875,-0.954503392578678,
-0.897355449029842,-0.698170085462727,-0.672255062571138,-0.656192979047803,
-0.643606184760003,-0.629535838183939,-0.605829791594677,-0.499755432290025,
-0.405721615865298,-0.294140531709845,-0.273972105360895,-0.265761711513818,
-0.259098271344394,-0.252019846976943,-0.240611437057429,-0.200849659954101,
-0.125463182742716,-0.000228192652907022),.UNSPECIFIED.);
#30139=B_SPLINE_CURVE_WITH_KNOTS('',3,(#164975,#164976,#164977,#164978,
#164979,#164980,#164981,#164982,#164983,#164984,#164985,#164986,#164987,
#164988,#164989,#164990,#164991,#164992,#164993,#164994,#164995,#164996,
#164997,#164998,#164999,#165000,#165001,#165002,#165003,#165004,#165005,
#165006,#165007,#165008,#165009,#165010,#165011,#165012,#165013,#165014,
#165015,#165016,#165017,#165018,#165019,#165020,#165021,#165022,#165023,
#165024,#165025,#165026,#165027,#165028,#165029,#165030,#165031,#165032,
#165033,#165034,#165035,#165036,#165037,#165038,#165039,#165040,#165041,
#165042,#165043,#165044,#165045,#165046,#165047,#165048,#165049,#165050,
#165051,#165052,#165053,#165054,#165055,#165056,#165057,#165058,#165059,
#165060,#165061,#165062,#165063,#165064,#165065,#165066,#165067,#165068,
#165069,#165070,#165071,#165072,#165073,#165074,#165075,#165076,#165077,
#165078,#165079,#165080,#165081,#165082,#165083,#165084,#165085,#165086,
#165087,#165088,#165089,#165090,#165091,#165092,#165093,#165094,#165095,
#165096,#165097,#165098,#165099,#165100,#165101,#165102),.UNSPECIFIED.,
 .F.,.F.,(4,2,2,2,2,2,2,2,2,2,2,2,2,2,2,2,2,2,2,2,2,2,2,2,2,2,2,2,2,2,2,
2,2,2,2,2,2,2,2,2,2,2,2,2,2,2,2,2,2,2,2,2,2,2,2,2,2,2,2,2,2,2,2,4),(-20.6404265031114,
-20.5538188837533,-20.5366027537719,-20.5238741986076,-20.5110137403867,
-20.4992592678507,-20.4833663937635,-20.443525073977,-20.3505999831602,
-20.2477399606774,-20.2003627857329,-20.180268831843,-20.1646632979875,
-20.1563126916547,-20.1492219223327,-20.1400427117604,-20.1196965355734,
-20.0187640405624,-19.9332601172847,-19.8682796548066,-19.8244542175184,
-19.8066584598254,-19.7938137729206,-19.780463457377,-19.7601125918741,
-19.7024760434826,-19.5158994343518,-19.4383141633649,-19.4199601864392,
-19.4114450723809,-19.4049018792084,-19.3972056083733,-19.3833544735927,
-19.313452632251,-19.1726005317205,-19.0709030414189,-19.0417266274786,
-19.0265093092129,-19.0152021534447,-19.0009872434407,-18.9765899308292,
-18.8482124631035,-18.7550463745566,-18.7076579169902,-18.6782100025422,
-18.6674952982743,-18.6601941239403,-18.6534402627088,-18.6417779835096,
-18.6077638334634,-18.5659273946448,-18.4453233307968,-18.3774261007886,
-18.3322356165173,-18.3142332752973,-18.301351351476,-18.2896227119443,
-18.2708315619069,-18.2241038488764,-18.023334188905,-17.945581828206,-17.9272086899218,
-17.9186899223837,-17.9145909763123),.UNSPECIFIED.);
#30140=B_SPLINE_CURVE_WITH_KNOTS('',3,(#165107,#165108,#165109,#165110,
#165111,#165112,#165113,#165114,#165115,#165116,#165117,#165118,#165119,
#165120,#165121,#165122,#165123,#165124,#165125,#165126,#165127,#165128,
#165129,#165130,#165131,#165132,#165133,#165134,#165135,#165136,#165137,
#165138,#165139,#165140,#165141,#165142,#165143,#165144,#165145,#165146,
#165147,#165148,#165149,#165150,#165151,#165152,#165153,#165154,#165155,
#165156,#165157,#165158,#165159,#165160,#165161,#165162,#165163,#165164,
#165165,#165166,#165167,#165168,#165169,#165170,#165171,#165172,#165173,
#165174,#165175,#165176,#165177,#165178,#165179,#165180,#165181,#165182,
#165183,#165184,#165185,#165186,#165187,#165188,#165189,#165190,#165191,
#165192,#165193,#165194,#165195,#165196,#165197,#165198,#165199,#165200,
#165201,#165202,#165203,#165204,#165205,#165206,#165207,#165208,#165209,
#165210,#165211,#165212,#165213,#165214,#165215,#165216,#165217,#165218,
#165219,#165220,#165221,#165222,#165223,#165224,#165225,#165226,#165227,
#165228,#165229,#165230,#165231,#165232,#165233,#165234,#165235,#165236,
#165237,#165238,#165239,#165240,#165241,#165242,#165243,#165244,#165245,
#165246,#165247,#165248,#165249,#165250,#165251,#165252,#165253,#165254,
#165255,#165256,#165257,#165258,#165259,#165260,#165261,#165262,#165263,
#165264,#165265,#165266,#165267,#165268,#165269,#165270,#165271,#165272,
#165273,#165274,#165275,#165276,#165277,#165278,#165279,#165280,#165281,
#165282,#165283,#165284,#165285,#165286,#165287,#165288,#165289,#165290,
#165291,#165292,#165293,#165294,#165295,#165296,#165297,#165298,#165299,
#165300,#165301,#165302,#165303,#165304,#165305,#165306,#165307,#165308,
#165309,#165310,#165311,#165312,#165313,#165314,#165315,#165316,#165317,
#165318,#165319,#165320,#165321,#165322,#165323,#165324,#165325,#165326,
#165327,#165328,#165329,#165330,#165331,#165332,#165333,#165334,#165335,
#165336,#165337,#165338,#165339,#165340,#165341,#165342,#165343,#165344,
#165345,#165346,#165347,#165348,#165349,#165350,#165351,#165352,#165353,
#165354,#165355,#165356,#165357,#165358,#165359,#165360,#165361,#165362,
#165363,#165364,#165365,#165366,#165367,#165368),.UNSPECIFIED.,.F.,.F.,
(4,2,2,2,2,2,2,2,2,2,2,2,2,2,2,2,2,2,2,2,2,2,2,2,2,2,2,2,2,2,2,2,2,2,2,
2,2,2,2,2,2,2,2,2,2,2,2,2,2,2,2,2,2,2,2,2,2,2,2,2,2,2,2,2,2,2,2,2,2,2,2,
2,2,2,2,2,2,2,2,2,2,2,2,2,2,2,2,2,2,2,2,2,2,2,2,2,2,2,2,2,2,2,2,2,2,2,2,
2,2,2,2,2,2,2,2,2,2,2,2,2,2,2,2,2,2,2,2,2,2,2,4),(-9.21748158827845,-9.21382472857645,
-9.20555010398746,-9.19226665746033,-9.08755739849233,-8.91019214907064,
-8.86181086810311,-8.84276324903766,-8.83098746131698,-8.81814313254699,
-8.80035991220493,-8.75663018859442,-8.69185628427859,-8.60704520878716,
-8.50506244227701,-8.48467657989922,-8.47548919028004,-8.46839643428287,
-8.46004874080444,-8.44446181290621,-8.32379220608945,-8.16484608717407,
-8.1378515091685,-8.12165092296186,-8.10901261910952,-8.09515781045967,
-8.0724564945001,-7.98281494607982,-7.87666389084958,-7.75872555223543,
-7.73813633891077,-7.73010201566733,-7.72348167155071,-7.71632046338717,
-7.70453966708904,-7.66075062345517,-7.5723683063852,-7.39145494653566,
-7.36047267593528,-7.34468856583957,-7.33212801135452,-7.31788486353923,
-7.29336115763615,-7.15172956036571,-7.00959248101371,-6.99079374299124,
-6.9818031416346,-6.97473458651297,-6.96611549471299,-6.94920905223148,
-6.92691915070103,-6.87134369617109,-6.68734580804887,-6.64781616132574,
-6.63203215980734,-6.62030286023555,-6.60741590293669,-6.58939729735798,
-6.54429661423769,-6.47795241799782,-6.3801374681796,-6.26582878573395,
-6.24560893993672,-6.23738911415706,-6.23072274995958,-6.22364722066697,
-6.21225423137606,-6.17265924039142,-6.09778395559222,-5.91021013481413,
-5.87184439771556,-5.85618008270338,-5.84447963852268,-5.83156765660398,
-5.81340717427366,-5.76715521131481,-5.6969415960481,-5.56013740382126,
-5.50779235098627,-5.49427484489502,-5.48637114686605,-5.47916739440721,
-5.46899522993174,-5.44329686608043,-5.40422697089216,-5.30154519405414,
-5.16939500832562,-5.14495830728065,-5.130733968207,-5.11942656235678,-5.10421827374453,
-5.07509171248983,-4.97376105119414,-4.83335887206876,-4.76256814021437,
-4.74867875224038,-4.74097340161693,-4.73443047191177,-4.72592605206858,
-4.70763247322185,-4.63058636455537,-4.43098599274847,-4.3827660741241,
-4.36374392954782,-4.35197342868982,-4.33912660745904,-4.32132461119646,
-4.27746619415442,-4.21241844540731,-4.12696444880667,-4.02604803005594,
-4.00570078156937,-3.99652078718055,-3.98942928108482,-3.98107764425874,
-3.96546978382914,-3.94537271838847,-3.89798711802878,-3.80481214765171,
-3.6764259104078,-3.65202668378943,-3.63781060333696,-3.62650248684246,
-3.61128383069372,-3.58210472001241,-3.4803963523489,-3.3395213464396,-3.26961286108437,
-3.25576043951311,-3.24806348956315,-3.2456129003934),.UNSPECIFIED.);
#30141=B_SPLINE_CURVE_WITH_KNOTS('',3,(#165369,#165370,#165371,#165372,
#165373,#165374,#165375,#165376,#165377,#165378,#165379,#165380,#165381,
#165382,#165383,#165384,#165385,#165386,#165387,#165388,#165389,#165390,
#165391,#165392,#165393,#165394,#165395,#165396,#165397,#165398,#165399,
#165400,#165401,#165402,#165403,#165404,#165405,#165406,#165407,#165408,
#165409,#165410,#165411,#165412,#165413,#165414,#165415,#165416,#165417,
#165418,#165419,#165420,#165421,#165422,#165423,#165424,#165425,#165426,
#165427,#165428,#165429,#165430,#165431,#165432,#165433,#165434,#165435,
#165436,#165437,#165438,#165439,#165440,#165441,#165442,#165443,#165444,
#165445,#165446,#165447,#165448,#165449,#165450,#165451,#165452,#165453,
#165454,#165455,#165456,#165457,#165458,#165459,#165460,#165461,#165462,
#165463,#165464,#165465,#165466,#165467,#165468,#165469,#165470,#165471,
#165472,#165473,#165474,#165475,#165476,#165477,#165478,#165479,#165480,
#165481,#165482,#165483,#165484,#165485,#165486,#165487,#165488,#165489,
#165490,#165491,#165492,#165493,#165494,#165495,#165496,#165497,#165498,
#165499,#165500,#165501,#165502,#165503,#165504,#165505,#165506,#165507,
#165508,#165509,#165510,#165511,#165512,#165513,#165514,#165515,#165516,
#165517,#165518,#165519,#165520,#165521,#165522,#165523,#165524,#165525,
#165526,#165527,#165528,#165529,#165530,#165531,#165532,#165533,#165534,
#165535,#165536,#165537,#165538,#165539,#165540,#165541,#165542,#165543,
#165544,#165545,#165546,#165547,#165548,#165549,#165550,#165551,#165552,
#165553,#165554,#165555,#165556,#165557,#165558,#165559,#165560,#165561,
#165562,#165563,#165564,#165565,#165566,#165567,#165568,#165569,#165570,
#165571,#165572,#165573,#165574,#165575,#165576,#165577,#165578,#165579,
#165580,#165581,#165582,#165583,#165584,#165585,#165586,#165587,#165588,
#165589,#165590,#165591,#165592,#165593,#165594,#165595,#165596,#165597,
#165598,#165599,#165600,#165601,#165602,#165603,#165604,#165605,#165606,
#165607,#165608,#165609,#165610,#165611,#165612,#165613,#165614,#165615,
#165616,#165617,#165618,#165619,#165620,#165621,#165622,#165623,#165624,
#165625,#165626,#165627,#165628,#165629,#165630,#165631,#165632),
 .UNSPECIFIED.,.F.,.F.,(4,2,2,2,2,2,2,2,2,2,2,2,2,2,2,2,2,2,2,2,2,2,2,2,
2,2,2,2,2,2,2,2,2,2,2,2,2,2,2,2,2,2,2,2,2,2,2,2,2,2,2,2,2,2,2,2,2,2,2,2,
2,2,2,2,2,2,2,2,2,2,2,2,2,2,2,2,2,2,2,2,2,2,2,2,2,2,2,2,2,2,2,2,2,2,2,2,
2,2,2,2,2,2,2,2,2,2,2,2,2,2,2,2,2,2,2,2,2,2,2,2,2,2,2,2,2,2,2,2,2,2,2,4),
(-17.9145909763123,-17.9121463149229,-17.9044523773332,-17.8906120035617,
-17.8209721505478,-17.6800253356371,-17.5781715345178,-17.54897299257,-17.5337510479476,
-17.5224432866508,-17.5082313166204,-17.4838484557573,-17.3562463996887,
-17.2096147603588,-17.1840722578969,-17.1739245593704,-17.1667253213257,
-17.1588122855645,-17.1452501576726,-17.0922772504089,-16.9568654998564,
-16.8862532631213,-16.8398218323326,-16.8216360627537,-16.8087201634212,
-16.7970255318323,-16.7813829594699,-16.7431418448027,-16.5554414631575,
-16.4805350359567,-16.44093113087,-16.4295378614113,-16.4224626400556,-16.4157969688591,
-16.407578422791,-16.3873637604223,-16.2732260223652,-16.1759908051098,
-16.1092168867775,-16.063908043945,-16.045858903648,-16.032967121291,-16.0196881544029,
-15.9996738026445,-15.9441875189247,-15.7934054825846,-15.7083435345649,
-15.6887186401988,-15.6795730555433,-15.6731710144705,-15.6649712812535,
-15.6504804351063,-15.5781271396811,-15.4490463168124,-15.3875712717742,
-15.3454305202164,-15.327896376873,-15.315096658422,-15.3016643759991,-15.2809279154852,
-15.2199961674478,-15.0375383776727,-14.9599290406113,-14.9415717234541,
-14.9330556653237,-14.9265120238059,-14.9188155523938,-14.9049648168994,
-14.8350890776082,-14.6942153229771,-14.5924951584541,-14.563314626739,
-14.5480958880551,-14.5367879748653,-14.5225725022773,-14.4981752146796,
-14.3698760047884,-14.2769009697618,-14.2293264238139,-14.2091768931081,
-14.1935376486409,-14.1851795551169,-14.178089090624,-14.1689186335417,
-14.1486238867513,-14.0491287473219,-13.96599195866,-13.8986326047346,-13.8536902543354,
-13.8357241923833,-13.8228481238843,-13.8111112307353,-13.7922769922941,
-13.7452785462086,-13.5244599296396,-13.4587110752116,-13.445452469443,
-13.43796725459,-13.431386335647,-13.4226838224456,-13.4027832550075,-13.2605232472613,
-13.1476410845656,-13.1048876281172,-13.072374830324,-13.0565009335129,
-13.0439321930748,-13.0297469209276,-13.0054930521031,-12.8877696989127,
-12.7638180454279,-12.7286386699555,-12.7048203340245,-12.694945031054,
-12.6877878228131,-12.679748777692,-12.6656090121849,-12.6035138427132,
-12.4753422918281,-12.4065313559282,-12.3609185071692,-12.3428520073658,
-12.3299572223299,-12.3182390812238,-12.3025011560222,-12.2633670807237,
-12.0765034759226,-12.001805440768,-11.9622690274271,-11.9508816527243,
-11.943807305019,-11.9431123563756),.UNSPECIFIED.);
#30142=B_SPLINE_CURVE_WITH_KNOTS('',3,(#165637,#165638,#165639,#165640,
#165641,#165642,#165643,#165644,#165645,#165646,#165647,#165648,#165649,
#165650,#165651,#165652,#165653,#165654,#165655,#165656,#165657,#165658,
#165659,#165660,#165661,#165662,#165663,#165664,#165665,#165666,#165667,
#165668,#165669,#165670,#165671,#165672,#165673,#165674,#165675,#165676,
#165677,#165678,#165679,#165680,#165681,#165682,#165683,#165684,#165685,
#165686,#165687,#165688,#165689,#165690,#165691,#165692,#165693,#165694,
#165695,#165696,#165697,#165698,#165699,#165700,#165701,#165702,#165703,
#165704,#165705,#165706,#165707,#165708,#165709,#165710,#165711,#165712,
#165713,#165714,#165715,#165716,#165717,#165718,#165719,#165720,#165721,
#165722,#165723,#165724,#165725,#165726,#165727,#165728,#165729,#165730,
#165731,#165732,#165733,#165734,#165735,#165736,#165737,#165738,#165739,
#165740,#165741,#165742,#165743,#165744,#165745,#165746,#165747,#165748,
#165749,#165750,#165751,#165752,#165753,#165754,#165755,#165756,#165757,
#165758,#165759,#165760,#165761,#165762,#165763,#165764,#165765,#165766,
#165767,#165768,#165769,#165770,#165771,#165772,#165773,#165774,#165775,
#165776,#165777,#165778,#165779,#165780,#165781,#165782,#165783,#165784,
#165785,#165786,#165787,#165788,#165789,#165790,#165791,#165792,#165793,
#165794,#165795,#165796,#165797,#165798,#165799,#165800,#165801,#165802,
#165803,#165804,#165805,#165806,#165807,#165808,#165809,#165810,#165811,
#165812,#165813,#165814,#165815,#165816,#165817,#165818,#165819,#165820,
#165821,#165822,#165823,#165824,#165825,#165826,#165827,#165828,#165829,
#165830,#165831,#165832,#165833,#165834,#165835,#165836,#165837,#165838,
#165839,#165840,#165841,#165842,#165843,#165844,#165845,#165846,#165847,
#165848,#165849,#165850,#165851,#165852,#165853,#165854,#165855,#165856,
#165857,#165858,#165859,#165860,#165861,#165862,#165863,#165864,#165865,
#165866,#165867,#165868,#165869,#165870,#165871,#165872,#165873,#165874,
#165875,#165876,#165877,#165878,#165879,#165880,#165881,#165882,#165883,
#165884,#165885,#165886,#165887,#165888,#165889,#165890,#165891,#165892,
#165893,#165894),.UNSPECIFIED.,.F.,.F.,(4,2,2,2,2,2,2,2,2,2,2,2,2,2,2,2,
2,2,2,2,2,2,2,2,2,2,2,2,2,2,2,2,2,2,2,2,2,2,2,2,2,2,2,2,2,2,2,2,2,2,2,2,
2,2,2,2,2,2,2,2,2,2,2,2,2,2,2,2,2,2,2,2,2,2,2,2,2,2,2,2,2,2,2,2,2,2,2,2,
2,2,2,2,2,2,2,2,2,2,2,2,2,2,2,2,2,2,2,2,2,2,2,2,2,2,2,2,2,2,2,2,2,2,2,2,
2,2,2,2,4),(-15.1894918505391,-15.1870416113486,-15.1793449807329,-15.1654935784906,
-15.0956024288551,-14.9547347015735,-14.8530224898747,-14.8238430395983,
-14.8086244993549,-14.7973165838072,-14.7831009124023,-14.7587027856351,
-14.630360052036,-14.5372855031732,-14.4898030161241,-14.4696791059428,
-14.454055252677,-14.4457003681928,-14.4386094579693,-14.4294344476659,
-14.4091143926754,-14.3088148987986,-14.2245001378627,-14.1583731650709,
-14.1140060255117,-14.0961267125243,-14.0832662687304,-14.0715119973594,
-14.055623424675,-14.0159071042666,-13.8297933552427,-13.7552867640185,
-13.7158143430029,-13.7044335377081,-13.697360822426,-13.6906930729186,
-13.6824673822671,-13.6622128678422,-13.5463875921862,-13.4437057197943,
-13.3812049502699,-13.3380028272016,-13.3202768897009,-13.3074427391972,
-13.2956541141949,-13.279625563326,-13.2389695955077,-13.0360789886683,
-12.9938057328544,-12.9666215028766,-12.9562264642999,-12.9489840600123,
-12.9411684396504,-12.9280538875842,-12.8802722446436,-12.7580389718178,
-12.6446841141885,-12.6143616073319,-12.5989223745428,-12.5863880816962,
-12.5719003467737,-12.5469281275898,-12.4053145989166,-12.3029797615794,
-12.2271850700113,-12.2134714137552,-12.2058879386375,-12.1993269724132,
-12.1907856736944,-12.1717946060692,-12.0175252796335,-11.9120985255636,
-11.850578002158,-11.8304076522327,-11.817093934446,-11.8043690444182,-11.7865383770859,
-11.7457246786345,-11.5444433204555,-11.5013100213407,-11.4737357750924,
-11.4632838017366,-11.4560310320658,-11.4482361697524,-11.4352167257948,
-11.3885284613779,-11.2436700442378,-11.1743561017675,-11.1285126424949,
-11.1104117471717,-11.0975103862839,-11.0857983146814,-11.0700866097557,
-11.0314408922365,-10.8441545081836,-10.7693489375529,-10.7297765622723,
-10.7183854673745,-10.7113101760597,-10.704643235399,-10.6964218823539,
-10.6761942862667,-10.5615499096762,-10.4627030421729,-10.3637923074457,
-10.3404874588252,-10.3265022755237,-10.313895769996,-10.2976747381143,
-10.2712173056198,-10.1051474455863,-9.99192088572466,-9.97554911063105,
-9.96703865407043,-9.95996315371423,-9.95084044521359,-9.93134226763777,
-9.79865177725536,-9.64905950282259,-9.6243062037698,-9.61001368715274,
-9.59745903772131,-9.58174779079974,-9.55008366237157,-9.3726918540088,
-9.24337589625386,-9.22823720114878,-9.22035297280733,-9.21748158827845),
 .UNSPECIFIED.);
#30143=B_SPLINE_CURVE_WITH_KNOTS('',3,(#165895,#165896,#165897,#165898,
#165899,#165900,#165901,#165902,#165903,#165904,#165905,#165906,#165907,
#165908,#165909,#165910,#165911,#165912,#165913,#165914,#165915,#165916,
#165917,#165918,#165919,#165920,#165921,#165922,#165923,#165924,#165925,
#165926,#165927,#165928,#165929,#165930,#165931,#165932,#165933,#165934,
#165935,#165936,#165937,#165938,#165939,#165940,#165941,#165942,#165943,
#165944,#165945,#165946,#165947,#165948,#165949,#165950,#165951,#165952,
#165953,#165954,#165955,#165956,#165957,#165958,#165959,#165960,#165961,
#165962,#165963,#165964,#165965,#165966,#165967,#165968,#165969,#165970,
#165971,#165972,#165973,#165974,#165975,#165976,#165977,#165978,#165979,
#165980,#165981,#165982,#165983,#165984,#165985,#165986,#165987,#165988,
#165989,#165990,#165991,#165992,#165993,#165994,#165995,#165996,#165997,
#165998,#165999,#166000,#166001,#166002,#166003,#166004,#166005,#166006,
#166007,#166008,#166009,#166010,#166011,#166012,#166013,#166014,#166015,
#166016,#166017,#166018,#166019,#166020,#166021,#166022,#166023,#166024,
#166025,#166026,#166027,#166028,#166029,#166030,#166031,#166032,#166033,
#166034,#166035,#166036,#166037,#166038,#166039,#166040,#166041,#166042,
#166043,#166044,#166045,#166046,#166047,#166048,#166049,#166050,#166051,
#166052,#166053,#166054,#166055,#166056,#166057,#166058,#166059,#166060,
#166061,#166062,#166063,#166064,#166065,#166066,#166067,#166068,#166069,
#166070,#166071,#166072,#166073,#166074,#166075,#166076,#166077,#166078,
#166079,#166080,#166081,#166082,#166083,#166084,#166085,#166086,#166087,
#166088,#166089,#166090,#166091,#166092,#166093,#166094,#166095,#166096,
#166097,#166098,#166099,#166100,#166101,#166102,#166103,#166104,#166105,
#166106,#166107,#166108,#166109,#166110,#166111,#166112,#166113,#166114,
#166115,#166116,#166117,#166118,#166119,#166120,#166121,#166122,#166123,
#166124,#166125,#166126,#166127,#166128,#166129,#166130,#166131,#166132,
#166133,#166134,#166135,#166136,#166137,#166138,#166139,#166140,#166141,
#166142,#166143,#166144,#166145,#166146),.UNSPECIFIED.,.F.,.F.,(4,2,2,2,
2,2,2,2,2,2,2,2,2,2,2,2,2,2,2,2,2,2,2,2,2,2,2,2,2,2,2,2,2,2,2,2,2,2,2,2,
2,2,2,2,2,2,2,2,2,2,2,2,2,2,2,2,2,2,2,2,2,2,2,2,2,2,2,2,2,2,2,2,2,2,2,2,
2,2,2,2,2,2,2,2,2,2,2,2,2,2,2,2,2,2,2,2,2,2,2,2,2,2,2,2,2,2,2,2,2,2,2,2,
2,2,2,2,2,2,2,2,2,2,2,2,2,4),(-11.9431123563756,-11.9371400945385,-11.9289172128653,
-11.9086800441113,-11.7935921533514,-11.6937260935414,-11.5961479228807,
-11.5729244680541,-11.5589570921374,-11.5463470432184,-11.5300939069081,
-11.5035247186011,-11.3389085811387,-11.2244999409633,-11.2080933282744,
-11.1995758733406,-11.1925011265811,-11.1833878091642,-11.163939126086,
-11.0289354641812,-10.8816233132815,-10.8568526541824,-10.8425566844538,
-10.8300028599394,-10.8142977371823,-10.7826638439394,-10.6049158771398,
-10.4759113732513,-10.4607769398394,-10.4528937237041,-10.4463656172844,
-10.4380902808621,-10.4248040481589,-10.3201645482951,-10.1429649225121,
-10.0944200747842,-10.0753480613444,-10.0635681277133,-10.0507278873983,
-10.0329662673887,-9.98937506419385,-9.92489190637708,-9.83947252087029,
-9.73761962873634,-9.71723787208984,-9.70805136989529,-9.70095887054295,
-9.69261095916566,-9.67702232298835,-9.55619263636395,-9.39744205095968,
-9.37043487760053,-9.3542309551249,-9.34159248032378,-9.32773995372433,
-9.30504806897216,-9.21553396853199,-9.10930686262019,-8.99130820639629,
-8.97071987207343,-8.9626858184261,-8.95606566791012,-8.94890463241116,
-8.93712405068992,-8.89333496225985,-8.8049507937886,-8.62404902692935,
-8.59306706635493,-8.57728327829012,-8.5647230588297,-8.55048037517143,
-8.52595768399791,-8.38435368020825,-8.24219256233126,-8.22339668294539,
-8.21440677514545,-8.20733843167372,-8.19871918972571,-8.18181129598609,
-8.15951872072812,-8.10393200279178,-7.91985797885726,-7.88039864853292,
-7.86462621735444,-7.85289991712386,-7.84001077378147,-7.82197876899257,
-7.77678742211517,-7.71025611290615,-7.61268765976083,-7.49845077059258,
-7.47823291956886,-7.47001356919396,-7.46334745266185,-7.45627201130869,
-7.4448788503633,-7.40527997835284,-7.3303917020678,-7.14276316507474,-7.10445327262611,
-7.08879861871029,-7.07710069280272,-7.06418683841725,-7.0460148300962,
-6.99968191063227,-6.92928866499938,-6.79311596066494,-6.74047763658306,
-6.72693901068511,-6.7190308384122,-6.71182913972786,-6.70166840345522,
-6.6760433499676,-6.52931785629973,-6.4019090495025,-6.37752900447575,-6.3633171389559,
-6.35200863497734,-6.33678461469793,-6.30757837164564,-6.20567478274499,
-6.06469422378829,-5.99511169331124,-5.9812730275737,-5.97357921617743,
-5.97113581786257),.UNSPECIFIED.);
#30144=B_SPLINE_CURVE_WITH_KNOTS('',3,(#166152,#166153,#166154,#166155,
#166156,#166157,#166158,#166159,#166160,#166161,#166162,#166163,#166164,
#166165,#166166,#166167,#166168,#166169,#166170,#166171,#166172,#166173,
#166174,#166175,#166176,#166177,#166178,#166179,#166180,#166181,#166182,
#166183,#166184,#166185,#166186,#166187,#166188,#166189,#166190,#166191,
#166192,#166193,#166194,#166195,#166196,#166197,#166198,#166199,#166200,
#166201,#166202,#166203,#166204,#166205,#166206,#166207,#166208,#166209,
#166210,#166211,#166212,#166213,#166214,#166215,#166216,#166217,#166218,
#166219,#166220,#166221,#166222,#166223,#166224,#166225,#166226,#166227,
#166228,#166229,#166230,#166231,#166232,#166233,#166234,#166235,#166236,
#166237,#166238,#166239,#166240,#166241,#166242,#166243,#166244,#166245,
#166246,#166247,#166248,#166249,#166250,#166251,#166252,#166253,#166254,
#166255,#166256,#166257,#166258,#166259,#166260,#166261,#166262,#166263,
#166264,#166265,#166266,#166267,#166268,#166269,#166270,#166271,#166272,
#166273,#166274,#166275,#166276,#166277,#166278,#166279,#166280,#166281),
 .UNSPECIFIED.,.F.,.F.,(4,2,2,2,2,2,2,2,2,2,2,2,2,2,2,2,2,2,2,2,2,2,2,2,
2,2,2,2,2,2,2,2,2,2,2,2,2,2,2,2,2,2,2,2,2,2,2,2,2,2,2,2,2,2,2,2,2,2,2,2,
2,2,2,2,4),(-2.98559501155222,-2.98150198114167,-2.97298644258405,-2.95463164891737,
-2.87704410593891,-2.69279950536456,-2.63329855246361,-2.6127254688512,
-2.59932784173563,-2.58650947868206,-2.56886663441153,-2.52603375527301,
-2.46313099303798,-2.37586575689804,-2.27328847636493,-2.25289150371308,
-2.24370288227929,-2.23661085383845,-2.22826605306425,-2.21268962008674,
-2.09266997970115,-1.93300222104418,-1.90606417573725,-1.88988079422555,
-1.87724626561229,-1.86338578543205,-1.84065252559053,-1.75052322562678,
-1.6447091884978,-1.60221390767052,-1.59627120130252,-1.51738924746365,
-1.50320025983768,-1.49542858053529,-1.48889345528827,-1.48048152497209,
-1.46267647594869,-1.38981484332574,-1.22508601237974,-1.1449703970151,
-1.12220342944022,-1.10833580321562,-1.09570342214667,-1.07926100385269,
-1.04359994854982,-0.909885413282459,-0.7793738821061,-0.75972942411144,
-0.750580439955319,-0.743504377630477,-0.73501714993527,-0.718754160922146,
-0.608988500037552,-0.438698349799292,-0.412595483209955,-0.396478855141943,
-0.383886264642389,-0.369847521045809,-0.346287165374704,-0.242897536326381,
-0.1472765080372,-0.0299220292933785,-0.0125922719991535,-0.00561123964068375,
-9.99999651085659E-7),.UNSPECIFIED.);
#30145=B_SPLINE_CURVE_WITH_KNOTS('',3,(#166282,#166283,#166284,#166285,
#166286,#166287,#166288,#166289,#166290,#166291,#166292,#166293,#166294,
#166295,#166296,#166297,#166298,#166299,#166300,#166301,#166302,#166303,
#166304,#166305,#166306,#166307,#166308,#166309,#166310,#166311,#166312,
#166313,#166314,#166315,#166316,#166317,#166318,#166319,#166320,#166321,
#166322,#166323,#166324,#166325,#166326,#166327,#166328,#166329,#166330,
#166331,#166332,#166333,#166334,#166335,#166336,#166337,#166338,#166339,
#166340,#166341,#166342,#166343,#166344,#166345,#166346,#166347,#166348,
#166349,#166350,#166351,#166352,#166353,#166354,#166355,#166356,#166357,
#166358,#166359,#166360,#166361,#166362,#166363,#166364,#166365,#166366,
#166367,#166368,#166369,#166370,#166371,#166372,#166373,#166374,#166375,
#166376,#166377,#166378,#166379,#166380,#166381,#166382,#166383,#166384,
#166385,#166386,#166387,#166388,#166389,#166390,#166391,#166392,#166393,
#166394,#166395,#166396,#166397,#166398,#166399,#166400,#166401,#166402,
#166403,#166404,#166405,#166406,#166407,#166408,#166409,#166410,#166411),
 .UNSPECIFIED.,.F.,.F.,(4,2,2,2,2,2,2,2,2,2,2,2,2,2,2,2,2,2,2,2,2,2,2,2,
2,2,2,2,2,2,2,2,2,2,2,2,2,2,2,2,2,2,2,2,2,2,2,2,2,2,2,2,2,2,2,2,2,2,2,2,
2,2,2,2,4),(-18.1752349093479,-18.1694917945602,-18.1622828023296,-18.1443097264025,
-17.9872703263121,-17.8830902947781,-17.8220212711318,-17.8019035257271,
-17.7886017324481,-17.7758716274271,-17.7580056736581,-17.7169856263102,
-17.5342909142115,-17.4794120198481,-17.4573025911209,-17.4405020101241,
-17.4319049037613,-17.4248361097276,-17.4158219926332,-17.3968965427577,
-17.254827872475,-17.1133639183328,-17.0888453045179,-17.0746042249777,
-17.062044963451,-17.0462617705439,-17.0152790027055,-16.8344193773344,
-16.7460153965524,-16.7022220974958,-16.6904417728106,-16.6832811659422,
-16.6766616260191,-16.6686285405048,-16.6480438794491,-16.5336006504433,
-16.4358128480918,-16.3694654431122,-16.3243638435582,-16.306345979109,
-16.2934599031709,-16.2801724230947,-16.2601171578566,-16.2043216964771,
-16.053818098587,-15.9688583704556,-15.9492442538141,-15.9401006618835,
-15.9336988464382,-15.9254977628865,-15.9110009495152,-15.8384879693636,
-15.7095382702265,-15.6480862356229,-15.6059566916617,-15.588424302149,
-15.575624865703,-15.5621919813025,-15.5414527579674,-15.4804967773218,
-15.298057267305,-15.2204573774013,-15.2021011181322,-15.1935852478966,
-15.1894918505391),.UNSPECIFIED.);
#30146=B_SPLINE_CURVE_WITH_KNOTS('',3,(#166413,#166414,#166415,#166416,
#166417,#166418,#166419,#166420,#166421,#166422,#166423,#166424,#166425,
#166426,#166427,#166428,#166429,#166430,#166431,#166432,#166433,#166434,
#166435,#166436,#166437,#166438,#166439,#166440,#166441,#166442,#166443,
#166444,#166445,#166446,#166447,#166448,#166449,#166450,#166451,#166452,
#166453,#166454,#166455,#166456,#166457,#166458,#166459,#166460,#166461,
#166462,#166463,#166464,#166465,#166466,#166467,#166468,#166469,#166470,
#166471,#166472,#166473,#166474,#166475,#166476,#166477,#166478,#166479,
#166480,#166481,#166482,#166483,#166484,#166485,#166486,#166487,#166488,
#166489,#166490,#166491,#166492,#166493,#166494,#166495,#166496,#166497,
#166498,#166499,#166500,#166501,#166502,#166503,#166504,#166505,#166506,
#166507,#166508,#166509,#166510,#166511,#166512,#166513,#166514,#166515,
#166516,#166517,#166518,#166519,#166520,#166521,#166522,#166523,#166524,
#166525,#166526,#166527,#166528,#166529,#166530,#166531,#166532,#166533,
#166534,#166535,#166536,#166537,#166538,#166539,#166540,#166541,#166542,
#166543,#166544,#166545,#166546,#166547,#166548,#166549,#166550,#166551,
#166552,#166553,#166554,#166555,#166556,#166557,#166558,#166559,#166560,
#166561,#166562,#166563,#166564,#166565,#166566,#166567,#166568,#166569,
#166570,#166571,#166572,#166573,#166574,#166575,#166576,#166577,#166578,
#166579,#166580,#166581,#166582,#166583,#166584,#166585,#166586,#166587,
#166588,#166589,#166590,#166591,#166592,#166593,#166594,#166595,#166596,
#166597,#166598,#166599,#166600,#166601,#166602,#166603,#166604,#166605,
#166606,#166607,#166608,#166609,#166610,#166611,#166612,#166613,#166614,
#166615,#166616,#166617,#166618,#166619,#166620,#166621,#166622,#166623,
#166624,#166625,#166626,#166627,#166628,#166629,#166630,#166631,#166632,
#166633,#166634,#166635,#166636,#166637,#166638,#166639,#166640,#166641,
#166642,#166643,#166644,#166645,#166646,#166647,#166648,#166649,#166650,
#166651,#166652,#166653,#166654,#166655,#166656,#166657,#166658,#166659,
#166660,#166661,#166662,#166663,#166664,#166665,#166666,#166667,#166668,
#166669,#166670,#166671,#166672,#166673,#166674,#166675,#166676,#166677,
#166678),.UNSPECIFIED.,.F.,.F.,(4,2,2,2,2,2,2,2,2,2,2,2,2,2,2,2,2,2,2,2,
2,2,2,2,2,2,2,2,2,2,2,2,2,2,2,2,2,2,2,2,2,2,2,2,2,2,2,2,2,2,2,2,2,2,2,2,
2,2,2,2,2,2,2,2,2,2,2,2,2,2,2,2,2,2,2,2,2,2,2,2,2,2,2,2,2,2,2,2,2,2,2,2,
2,2,2,2,2,2,2,2,2,2,2,2,2,2,2,2,2,2,2,2,2,2,2,2,2,2,2,2,2,2,2,2,2,2,2,2,
2,2,2,2,4),(-5.97113581786257,-5.96703516979956,-5.95851512437902,-5.9401366653248,
-5.8623426411769,-5.67954037707069,-5.61906809617788,-5.5983835578764,-5.58496217941587,
-5.57215643449029,-5.55458773859438,-5.51222895885169,-5.45030598444822,
-5.32232734328591,-5.24963238058043,-5.23512860741096,-5.22692591591118,
-5.22052431017789,-5.21138293579274,-5.19178101938982,-5.10693781792056,
-4.95674925962414,-4.90060919842211,-4.88050875704274,-4.86721179174308,
-4.8543318046417,-4.83634786235152,-4.79147080793593,-4.72558345883557,
-4.62720144626423,-4.5127253977237,-4.49250319162965,-4.48428327588057,
-4.47761719599568,-4.47054242167573,-4.45915145950253,-4.41957201846929,
-4.34474076754283,-4.15733451499403,-4.11882946199004,-4.10314234331012,
-4.09143700121037,-4.07853160422073,-4.06040325175182,-4.01436513329425,
-3.9446202562311,-3.80040739830392,-3.75378202972391,-3.74076905044114,
-3.73297613354094,-3.72572357546339,-3.71526964393254,-3.68767708447693,
-3.64450161772212,-3.45373144808359,-3.40531056592493,-3.38630582224035,
-3.37453779336924,-3.36168818876024,-3.34387079864031,-3.30007636261581,
-3.23638595947187,-3.1354675928041,-3.01989215553245,-2.9996451505462,-2.99142112221163,
-2.98475415599664,-2.97768154624234,-2.96629962408355,-2.92680969770483,
-2.85224733950829,-2.66590006190023,-2.62642566076004,-2.61057760629896,
-2.59883380587266,-2.58596582012182,-2.56804044398435,-2.52336307863607,
-2.45657025500021,-2.37292868558626,-2.27303609761326,-2.25273281200869,
-2.24356123296528,-2.23647112674232,-2.22811494126773,-2.21248301115083,
-2.19234534653522,-2.14481167510858,-2.051809674463,-1.92350792031644,-1.89911234172393,
-1.88489790562532,-1.87359083876238,-1.85837326087575,-1.82919505514916,
-1.72748290480389,-1.586610633051,-1.51673444542262,-1.50288442203188,-1.49518845044274,
-1.48864529902065,-1.48012996563862,-1.46177451981791,-1.38417588128721,
-1.20175612220662,-1.14081352461235,-1.12007688325711,-1.10664522153314,
-1.09384662500304,-1.0763148685492,-1.03418426671125,-0.972727660312583,
-0.843740801965002,-0.771211454106194,-0.756755952869671,-0.748564527438784,
-0.741446658718512,-0.731858433097371,-0.709753312347637,-0.67796812890868,
-0.576744370466088,-0.442416394878315,-0.411551338029357,-0.395803965344789,
-0.383248489665609,-0.368984292072017,-0.344374807045077,-0.217516004833518,
-0.0706040303832338,-0.0216738259340477,-0.00982584924864139,-0.00454025443351554,
-9.99999878459334E-7),.UNSPECIFIED.);
#30147=B_SPLINE_CURVE_WITH_KNOTS('',3,(#166679,#166680,#166681,#166682),
 .UNSPECIFIED.,.F.,.F.,(4,4),(-18.8333370051235,-18.8333271884725),
 .UNSPECIFIED.);
#30148=B_SPLINE_CURVE_WITH_KNOTS('',3,(#166687,#166688,#166689,#166690,
#166691,#166692,#166693,#166694,#166695,#166696,#166697,#166698,#166699,
#166700,#166701,#166702,#166703,#166704,#166705,#166706,#166707,#166708,
#166709,#166710,#166711,#166712,#166713,#166714,#166715,#166716,#166717,
#166718,#166719,#166720,#166721,#166722,#166723,#166724,#166725,#166726,
#166727,#166728,#166729,#166730,#166731,#166732,#166733,#166734,#166735,
#166736,#166737,#166738,#166739,#166740,#166741,#166742,#166743,#166744,
#166745,#166746,#166747,#166748,#166749,#166750,#166751,#166752,#166753,
#166754,#166755,#166756,#166757,#166758,#166759,#166760,#166761,#166762,
#166763,#166764,#166765,#166766,#166767,#166768,#166769,#166770,#166771,
#166772,#166773,#166774,#166775,#166776,#166777,#166778,#166779,#166780,
#166781,#166782,#166783,#166784,#166785,#166786,#166787,#166788,#166789,
#166790,#166791,#166792,#166793,#166794,#166795,#166796,#166797,#166798,
#166799,#166800,#166801,#166802,#166803,#166804,#166805,#166806,#166807,
#166808,#166809,#166810,#166811,#166812,#166813,#166814,#166815,#166816,
#166817,#166818,#166819,#166820,#166821,#166822,#166823,#166824,#166825,
#166826,#166827,#166828,#166829,#166830,#166831,#166832,#166833,#166834,
#166835,#166836,#166837,#166838,#166839,#166840,#166841,#166842,#166843,
#166844,#166845,#166846,#166847,#166848,#166849,#166850,#166851,#166852,
#166853,#166854,#166855,#166856,#166857,#166858,#166859,#166860,#166861,
#166862,#166863,#166864,#166865,#166866,#166867,#166868,#166869,#166870,
#166871,#166872,#166873,#166874,#166875,#166876,#166877,#166878,#166879,
#166880,#166881,#166882,#166883,#166884,#166885,#166886,#166887,#166888,
#166889,#166890,#166891,#166892,#166893,#166894,#166895,#166896,#166897,
#166898,#166899,#166900,#166901,#166902,#166903,#166904,#166905,#166906,
#166907,#166908,#166909,#166910,#166911,#166912,#166913,#166914,#166915,
#166916,#166917,#166918,#166919,#166920,#166921,#166922,#166923,#166924,
#166925,#166926,#166927,#166928,#166929,#166930,#166931,#166932,#166933,
#166934,#166935,#166936,#166937,#166938,#166939,#166940,#166941,#166942,
#166943,#166944,#166945,#166946,#166947,#166948),.UNSPECIFIED.,.F.,.F.,
(4,2,2,2,2,2,2,2,2,2,2,2,2,2,2,2,2,2,2,2,2,2,2,2,2,2,2,2,2,2,2,2,2,2,2,
2,2,2,2,2,2,2,2,2,2,2,2,2,2,2,2,2,2,2,2,2,2,2,2,2,2,2,2,2,2,2,2,2,2,2,2,
2,2,2,2,2,2,2,2,2,2,2,2,2,2,2,2,2,2,2,2,2,2,2,2,2,2,2,2,2,2,2,2,2,2,2,2,
2,2,2,2,2,2,2,2,2,2,2,2,2,2,2,2,2,2,2,2,2,2,2,4),(-8.95728479359192,-8.95319472449675,
-8.94468023383271,-8.92633397429123,-8.84883028474799,-8.66233517595378,
-8.60452255113426,-8.58414805233119,-8.57079131157462,-8.55794712790372,
-8.54016299966128,-8.49642508642479,-8.43163306182336,-8.34684859799388,
-8.24487810698112,-8.22449313291941,-8.215306077125,-8.20821354925228,-8.19986608835073,
-8.18427950485201,-8.06360244357754,-7.90467452639556,-7.87767987699411,
-7.86147954027321,-7.84884159944553,-7.83498735981955,-7.81228737062127,
-7.72265732029666,-7.61650411289081,-7.49856511562014,-7.47797657330771,
-7.4699425069411,-7.46332237256215,-7.45616138878537,-7.44438095692343,
-7.40059321091551,-7.31221339382306,-7.13130619173945,-7.10032486236829,
-7.08454124288637,-7.07198108414554,-7.05773839078626,-7.03321548194083,
-6.89158995899938,-6.74945547485728,-6.73065748832695,-6.72166720088065,
-6.71459887002994,-6.70598002412953,-6.68907398587613,-6.66678456595408,
-6.61121000187179,-6.42721250257005,-6.38768873538252,-6.37190597674247,
-6.36017722647903,-6.34729050649113,-6.3292715422203,-6.28416615324382,
-6.2178114586612,-6.12001578804295,-6.00571535221424,-5.9854962422321,-5.97727669281131,
-5.97061054338669,-5.96353523018159,-5.95214256758366,-5.91254848917706,
-5.83767454670796,-5.65010258573478,-5.61174177655313,-5.5960785818475,
-5.58437865598323,-5.57146693088284,-5.55330620761518,-5.50705014156774,
-5.43682646825714,-5.30006812615573,-5.2477056193848,-5.23418713840763,
-5.22628338385167,-5.21907998035943,-5.20890886608527,-5.1832160667927,
-5.14415746687846,-5.04146737251542,-4.90931636189658,-4.88488043077842,
-4.87065654056488,-4.85934949190088,-4.84414168417916,-4.81501604558257,
-4.71368860411346,-4.57329089134552,-4.50250234339957,-4.48861339196056,
-4.48090828422289,-4.47436556122808,-4.46586141066861,-4.44756841324618,
-4.37052476982206,-4.17093079682548,-4.12271230327394,-4.10369074462931,
-4.09192061287048,-4.07907419965218,-4.06127277836163,-4.0174158295572,
-3.95237031059405,-3.86691882248367,-3.76600549780537,-3.74565888803279,
-3.73647918287974,-3.7293879006948,-3.72103652814687,-3.70542916306244,
-3.68533273633539,-3.63794864683019,-3.54477660405748,-3.41639441498623,
-3.39199595887229,-3.37778032739539,-3.36647256806141,-3.35125439261519,
-3.3220762037064,-3.22037104968136,-3.07950049421774,-3.00959421440906,
-2.99574223024993,-2.98804552337654,-2.98559501155222),.UNSPECIFIED.);
#30149=B_SPLINE_CURVE_WITH_KNOTS('',3,(#166949,#166950,#166951,#166952,
#166953,#166954,#166955,#166956,#166957,#166958,#166959,#166960,#166961,
#166962,#166963,#166964,#166965,#166966,#166967,#166968,#166969,#166970,
#166971,#166972,#166973,#166974,#166975,#166976,#166977,#166978,#166979,
#166980,#166981,#166982,#166983,#166984,#166985,#166986,#166987,#166988,
#166989,#166990,#166991,#166992,#166993,#166994,#166995,#166996,#166997,
#166998,#166999,#167000,#167001,#167002,#167003,#167004,#167005,#167006,
#167007,#167008,#167009,#167010,#167011,#167012,#167013,#167014,#167015,
#167016,#167017,#167018,#167019,#167020,#167021,#167022,#167023,#167024,
#167025,#167026,#167027,#167028,#167029,#167030,#167031,#167032,#167033,
#167034,#167035,#167036,#167037,#167038,#167039,#167040,#167041,#167042,
#167043,#167044,#167045,#167046,#167047,#167048,#167049,#167050,#167051,
#167052,#167053,#167054,#167055,#167056,#167057,#167058,#167059,#167060,
#167061,#167062,#167063,#167064,#167065,#167066,#167067,#167068,#167069,
#167070,#167071,#167072,#167073,#167074,#167075,#167076,#167077,#167078,
#167079,#167080,#167081,#167082,#167083,#167084,#167085,#167086,#167087,
#167088,#167089,#167090,#167091,#167092,#167093,#167094,#167095,#167096,
#167097,#167098,#167099,#167100,#167101,#167102,#167103,#167104,#167105,
#167106,#167107,#167108,#167109,#167110,#167111,#167112,#167113,#167114,
#167115,#167116,#167117,#167118,#167119,#167120,#167121,#167122,#167123,
#167124,#167125,#167126,#167127,#167128,#167129,#167130,#167131,#167132,
#167133,#167134,#167135,#167136,#167137,#167138,#167139,#167140,#167141,
#167142,#167143,#167144,#167145,#167146,#167147,#167148,#167149,#167150,
#167151,#167152,#167153,#167154,#167155,#167156,#167157,#167158,#167159,
#167160,#167161,#167162,#167163,#167164,#167165,#167166,#167167,#167168,
#167169,#167170,#167171,#167172,#167173,#167174,#167175,#167176,#167177,
#167178,#167179,#167180,#167181,#167182,#167183,#167184,#167185,#167186,
#167187,#167188,#167189,#167190,#167191,#167192,#167193,#167194,#167195,
#167196,#167197,#167198,#167199,#167200,#167201,#167202,#167203,#167204,
#167205,#167206),.UNSPECIFIED.,.F.,.F.,(4,2,2,2,2,2,2,2,2,2,2,2,2,2,2,2,
2,2,2,2,2,2,2,2,2,2,2,2,2,2,2,2,2,2,2,2,2,2,2,2,2,2,2,2,2,2,2,2,2,2,2,2,
2,2,2,2,2,2,2,2,2,2,2,2,2,2,2,2,2,2,2,2,2,2,2,2,2,2,2,2,2,2,2,2,2,2,2,2,
2,2,2,2,2,2,2,2,2,2,2,2,2,2,2,2,2,2,2,2,2,2,2,2,2,2,2,2,2,2,2,2,2,2,2,2,
2,2,2,2,4),(-18.8333271884725,-18.8275940477612,-18.8203839697781,-18.8024196795371,
-18.6453570392404,-18.5411895733732,-18.4801256944877,-18.460008870824,
-18.4467075020269,-18.4339776683675,-18.4161118680451,-18.375091133818,
-18.1923737134745,-18.1375160076914,-18.1154122623847,-18.0986151018949,
-18.0900188208057,-18.0829501757085,-18.0739355756863,-18.0550068553597,
-17.9129861507796,-17.771488224752,-17.7469696911682,-17.7327288580406,
-17.720169932425,-17.7043873196533,-17.6734062048385,-17.492540611656,-17.404145715695,
-17.3603555239855,-17.3485756734211,-17.3414152873433,-17.3347958973036,
-17.3267629383907,-17.3061783015708,-17.1911532016556,-17.091763619604,
-17.0267286513643,-16.9822694059548,-16.9643495926245,-16.9514815782364,
-16.9397344228996,-16.9238730979679,-16.8842277090151,-16.7005117606719,
-16.6449853395928,-16.6227088785986,-16.6058107651318,-16.597193892138,
-16.5901259991452,-16.5811347858343,-16.5623299166487,-16.4203128318417,
-16.2786154058817,-16.2540932728942,-16.2398513787375,-16.2272921284468,
-16.2115099216185,-16.1805322523859,-15.9996063329079,-15.9112437615492,
-15.8674624103931,-15.855683074692,-15.8485226543329,-15.841902953222,-15.8338693319389,
-15.8132814509296,-15.6956110629582,-15.5898043085768,-15.4996663502823,
-15.4769319562555,-15.4630709099522,-15.450435944843,-15.434252114158,-15.4073135534577,
-15.2476220380605,-15.1276041320696,-15.1120270662866,-15.103681946473,
-15.0965896569689,-15.0874007136488,-15.0670030768978,-14.9644159953963,
-14.8771844477364,-14.8142680640235,-14.7714278774235,-14.753783490814,
-14.7409644926401,-14.7275666328729,-14.7069940650418,-14.6475023361526,
-14.4632269531374,-14.3856347370723,-14.3672790928821,-14.3587631990604,
-14.3522194038388,-14.3445224214826,-14.3306699983082,-14.2607614060004,
-14.1198964716473,-14.0181897845375,-13.9890107076789,-13.9737919930991,
-13.9624837967593,-13.9482675746057,-13.9238679997972,-13.7954778226951,
-13.7023011561734,-13.6549102029061,-13.6348116213243,-13.6192029026326,
-13.6108510494741,-13.6037595108128,-13.5945796676636,-13.5742334846981,
-13.4733444630476,-13.3879432573216,-13.3228519253627,-13.2789724969996,
-13.2611672051614,-13.2483197197274,-13.2365497775743,-13.2175311549447,
-13.1693351315456,-12.9697029535102,-12.8926450250858,-12.8743500572872,
-12.8658453317366,-12.8617719349234),.UNSPECIFIED.);
#30150=B_SPLINE_CURVE_WITH_KNOTS('',3,(#167211,#167212,#167213,#167214,
#167215,#167216,#167217,#167218,#167219,#167220,#167221,#167222,#167223,
#167224,#167225,#167226,#167227,#167228,#167229,#167230,#167231,#167232,
#167233,#167234,#167235,#167236,#167237,#167238,#167239,#167240,#167241,
#167242,#167243,#167244,#167245,#167246,#167247,#167248,#167249,#167250,
#167251,#167252,#167253,#167254,#167255,#167256,#167257,#167258,#167259,
#167260,#167261,#167262,#167263,#167264,#167265,#167266,#167267,#167268,
#167269,#167270,#167271,#167272,#167273,#167274,#167275,#167276,#167277,
#167278,#167279,#167280,#167281,#167282,#167283,#167284,#167285,#167286,
#167287,#167288,#167289,#167290,#167291,#167292,#167293,#167294,#167295,
#167296,#167297,#167298,#167299,#167300,#167301,#167302,#167303,#167304,
#167305,#167306,#167307,#167308,#167309,#167310,#167311,#167312,#167313,
#167314,#167315,#167316,#167317,#167318,#167319,#167320,#167321,#167322,
#167323,#167324,#167325,#167326,#167327,#167328,#167329,#167330,#167331,
#167332,#167333,#167334,#167335,#167336,#167337,#167338,#167339,#167340,
#167341,#167342,#167343,#167344,#167345,#167346,#167347,#167348,#167349,
#167350,#167351,#167352,#167353,#167354,#167355,#167356,#167357,#167358,
#167359,#167360,#167361,#167362,#167363,#167364,#167365,#167366,#167367,
#167368,#167369,#167370,#167371,#167372,#167373,#167374,#167375,#167376,
#167377,#167378,#167379,#167380,#167381,#167382,#167383,#167384,#167385,
#167386,#167387,#167388,#167389,#167390,#167391,#167392,#167393,#167394,
#167395,#167396,#167397,#167398,#167399,#167400,#167401,#167402,#167403,
#167404,#167405,#167406,#167407,#167408,#167409,#167410,#167411,#167412,
#167413,#167414,#167415,#167416,#167417,#167418,#167419,#167420,#167421,
#167422,#167423,#167424,#167425,#167426,#167427,#167428,#167429,#167430,
#167431,#167432,#167433,#167434,#167435,#167436,#167437,#167438,#167439,
#167440,#167441,#167442,#167443,#167444,#167445,#167446,#167447,#167448,
#167449,#167450,#167451,#167452,#167453,#167454,#167455,#167456,#167457,
#167458,#167459,#167460,#167461,#167462,#167463,#167464,#167465,#167466),
 .UNSPECIFIED.,.F.,.F.,(4,2,2,2,2,2,2,2,2,2,2,2,2,2,2,2,2,2,2,2,2,2,2,2,
2,2,2,2,2,2,2,2,2,2,2,2,2,2,2,2,2,2,2,2,2,2,2,2,2,2,2,2,2,2,2,2,2,2,2,2,
2,2,2,2,2,2,2,2,2,2,2,2,2,2,2,2,2,2,2,2,2,2,2,2,2,2,2,2,2,2,2,2,2,2,2,2,
2,2,2,2,2,2,2,2,2,2,2,2,2,2,2,2,2,2,2,2,2,2,2,2,2,2,2,2,2,2,2,4),(-14.9292022091245,
-14.923567848276,-14.9155341105952,-14.8949460842086,-14.7772119848963,
-14.6713208808229,-14.5813074281692,-14.5585814134627,-14.5447220021843,
-14.532086278869,-14.5158983704316,-14.4889460233737,-14.3294359857361,
-14.2092587418778,-14.1936792881916,-14.1853335696015,-14.1782412028746,
-14.1690527018714,-14.1486581371181,-14.0462436492217,-13.9591442328379,
-13.8960387366708,-13.8531072092446,-13.8354483602321,-13.8226266564347,
-13.8108252555576,-13.7916316878714,-13.7422707253191,-13.5444346773123,
-13.4671801679223,-13.4488627636572,-13.4403538635117,-13.4338105149843,
-13.4261082427384,-13.4122327471416,-13.3417770796311,-13.2011855204261,
-13.0997264424969,-13.0705816646625,-13.055369630315,-13.0440618000276,
-13.0298400228771,-13.0054156065968,-12.8753958462801,-12.778500397953,
-12.7345197398789,-12.7065653235143,-12.6960588499837,-12.6887963047187,
-12.6810213838878,-12.6680920382948,-12.6224112606043,-12.4766601981801,
-12.4071756784451,-12.3612548710066,-12.3431429768141,-12.330239929755,
-12.3185304465873,-12.3028283856362,-12.2642382658227,-12.0768994616907,
-12.0020816544984,-11.9625057608874,-11.951114588555,-11.9440394418029,
-11.9373728006283,-11.9291519853375,-11.908926530449,-11.7943512630132,
-11.6956862626441,-11.6300243870223,-11.5852562952438,-11.5672881231649,
-11.5544103051328,-11.5426710915306,-11.5238338682072,-11.4765392065805,
-11.2819867366182,-11.2401878322433,-11.2132200192572,-11.2028566142301,
-11.1956196884502,-11.1877918092086,-11.1746219634921,-11.126199909589,
-11.0044460772341,-10.8913054656154,-10.8610086976045,-10.8455742764201,
-10.8330399416849,-10.8185477591444,-10.7935568043138,-10.6486808977673,
-10.4995747290421,-10.4683272210659,-10.4575045034846,-10.4512436687114,
-10.4445376682149,-10.4349039388764,-10.4098576410527,-10.2759531399225,
-10.1197007614083,-10.0868019207057,-10.070854188857,-10.0582776597712,
-10.0441369193296,-10.0200926579586,-9.8991450338858,-9.7823285925319,-9.72702940003429,
-9.71330714876304,-9.70535850075845,-9.69817116751192,-9.68810144970114,
-9.66306661532859,-9.51695087688235,-9.38814289118255,-9.36373472735201,
-9.34951606401935,-9.33820730175752,-9.32298959921333,-9.29381865170373,
-9.19217652373736,-9.05135798675799,-8.98129727795255,-8.96743769117316,
-8.95973879369766,-8.95728479359192),.UNSPECIFIED.);
#30151=B_SPLINE_CURVE_WITH_KNOTS('',3,(#167467,#167468,#167469,#167470,
#167471,#167472,#167473,#167474,#167475,#167476,#167477,#167478,#167479,
#167480,#167481,#167482,#167483,#167484,#167485,#167486,#167487,#167488,
#167489,#167490,#167491,#167492,#167493,#167494,#167495,#167496,#167497,
#167498,#167499,#167500,#167501,#167502,#167503,#167504,#167505,#167506,
#167507,#167508,#167509,#167510,#167511,#167512,#167513,#167514,#167515,
#167516,#167517,#167518,#167519,#167520,#167521,#167522,#167523,#167524,
#167525,#167526,#167527,#167528,#167529,#167530,#167531,#167532,#167533,
#167534,#167535,#167536,#167537,#167538,#167539,#167540,#167541,#167542,
#167543,#167544,#167545,#167546,#167547,#167548,#167549,#167550,#167551,
#167552,#167553,#167554,#167555,#167556,#167557,#167558,#167559,#167560,
#167561,#167562,#167563,#167564,#167565,#167566,#167567,#167568,#167569,
#167570,#167571,#167572,#167573,#167574,#167575,#167576,#167577,#167578,
#167579,#167580,#167581,#167582,#167583,#167584,#167585,#167586,#167587,
#167588,#167589,#167590,#167591,#167592,#167593,#167594,#167595,#167596,
#167597,#167598,#167599,#167600,#167601,#167602,#167603,#167604,#167605,
#167606,#167607,#167608,#167609,#167610,#167611,#167612,#167613,#167614,
#167615,#167616,#167617,#167618,#167619,#167620,#167621,#167622,#167623,
#167624,#167625,#167626,#167627,#167628,#167629,#167630,#167631,#167632,
#167633,#167634,#167635,#167636,#167637,#167638,#167639,#167640,#167641,
#167642,#167643,#167644,#167645,#167646,#167647,#167648,#167649,#167650,
#167651,#167652,#167653,#167654,#167655,#167656,#167657,#167658,#167659,
#167660,#167661,#167662,#167663,#167664,#167665,#167666,#167667,#167668,
#167669,#167670,#167671,#167672,#167673,#167674,#167675,#167676,#167677,
#167678,#167679,#167680,#167681,#167682,#167683,#167684,#167685,#167686,
#167687,#167688,#167689,#167690,#167691,#167692,#167693,#167694,#167695,
#167696,#167697,#167698,#167699,#167700,#167701,#167702,#167703,#167704,
#167705,#167706,#167707,#167708,#167709,#167710,#167711,#167712,#167713,
#167714,#167715,#167716,#167717,#167718,#167719,#167720,#167721,#167722,
#167723,#167724,#167725,#167726),.UNSPECIFIED.,.F.,.F.,(4,2,2,2,2,2,2,2,
2,2,2,2,2,2,2,2,2,2,2,2,2,2,2,2,2,2,2,2,2,2,2,2,2,2,2,2,2,2,2,2,2,2,2,2,
2,2,2,2,2,2,2,2,2,2,2,2,2,2,2,2,2,2,2,2,2,2,2,2,2,2,2,2,2,2,2,2,2,2,2,2,
2,2,2,2,2,2,2,2,2,2,2,2,2,2,2,2,2,2,2,2,2,2,2,2,2,2,2,2,2,2,2,2,2,2,2,2,
2,2,2,2,2,2,2,2,2,2,2,2,2,4),(-12.8617719349234,-12.8593023241814,-12.8515970655534,
-12.8377082814962,-12.7669327203902,-12.6265298016717,-12.5251956232254,
-12.49606833127,-12.4808598072358,-12.4695522810842,-12.4553278686535,-12.4308912403472,
-12.2991307505065,-12.1995197234588,-12.1583227167709,-12.1316317780818,
-12.1213096379905,-12.1140801976905,-12.10623694004,-12.0929959929273,-12.043773588809,
-11.9016248725565,-11.8324692487148,-11.7866985870222,-11.7686087890099,
-11.7557097663079,-11.7439960831697,-11.7282766155344,-11.6895828141384,
-11.5023558809494,-11.4275661604878,-11.3879994857,-11.3766091817801,-11.3695342066581,
-11.3628674155391,-11.3546460937897,-11.3344178309401,-11.2197183683731,
-11.1207216231782,-11.0553340160798,-11.0107002159779,-10.9927524665652,
-10.9798783126377,-10.9681349984893,-10.9522932121648,-10.9127736872259,
-10.7083497078901,-10.6659936754757,-10.6387714549941,-10.6283706075608,
-10.6211269577052,-10.6133130587186,-10.6002072217801,-10.5525305406158,
-10.4302114902307,-10.3168161925509,-10.2864881132567,-10.2710474189525,
-10.2585125939678,-10.2440249727032,-10.2190547818093,-10.0776537287402,
-9.97574544739281,-9.899336844425,-9.88559839442322,-9.87800941917835,-9.87144911684368,
-9.86291555704555,-9.8446590378013,-9.68403702367608,-9.58244682924576,
-9.5223222386069,-9.50231115753956,-9.48903031329043,-9.4762839175659,-9.45833352891559,
-9.41682296164706,-9.35477089637641,-9.22897195441992,-9.15454515242283,
-9.13989428577581,-9.13165811439528,-9.12526143896965,-9.11616746861413,
-9.09682227198179,-9.01438845433282,-8.87050666068671,-8.80699307239601,
-8.7860572217461,-8.77258364035977,-8.75980291871828,-8.74239063754349,
-8.70115789900073,-8.56483678196901,-8.41530816135717,-8.3959393881213,
-8.38733031481535,-8.38076111016192,-8.37321974237346,-8.35970258424534,
-8.28855502052216,-8.18353147904001,-8.03964364301497,-8.01465295388328,
-8.00016073279213,-7.98762625014456,-7.97219150134397,-7.94189362359652,
-7.82874507750857,-7.70697846726183,-7.65856242753242,-7.64539296358926,
-7.63756511240549,-7.63032804522553,-7.61996420972807,-7.59299394905434,
-7.55119024130368,-7.3565467777315,-7.30933025176023,-7.2905047541494,-7.27876750651671,
-7.26588756893653,-7.24790841281392,-7.20306912679643,-7.13726129300237,
-7.03876501592092,-6.92424400669048,-6.90401931289166,-6.89579856302506,
-6.88983016741359),.UNSPECIFIED.);
#30152=B_SPLINE_CURVE_WITH_KNOTS('',3,(#167731,#167732,#167733,#167734,
#167735,#167736,#167737,#167738,#167739,#167740,#167741,#167742,#167743,
#167744,#167745,#167746,#167747,#167748,#167749,#167750,#167751,#167752,
#167753,#167754,#167755,#167756,#167757,#167758,#167759,#167760,#167761,
#167762,#167763,#167764,#167765,#167766,#167767,#167768,#167769,#167770,
#167771,#167772,#167773,#167774,#167775,#167776,#167777,#167778,#167779,
#167780,#167781,#167782,#167783,#167784,#167785,#167786,#167787,#167788,
#167789,#167790,#167791,#167792,#167793,#167794,#167795,#167796,#167797,
#167798,#167799,#167800,#167801,#167802,#167803,#167804,#167805,#167806,
#167807,#167808,#167809,#167810,#167811,#167812,#167813,#167814,#167815,
#167816,#167817,#167818,#167819,#167820,#167821,#167822,#167823,#167824,
#167825,#167826,#167827,#167828,#167829,#167830,#167831,#167832,#167833,
#167834,#167835,#167836,#167837,#167838,#167839,#167840,#167841,#167842,
#167843,#167844,#167845,#167846,#167847,#167848,#167849,#167850,#167851,
#167852,#167853,#167854,#167855,#167856,#167857,#167858,#167859,#167860,
#167861,#167862,#167863,#167864,#167865,#167866,#167867,#167868,#167869,
#167870,#167871,#167872,#167873,#167874,#167875,#167876,#167877,#167878,
#167879,#167880,#167881,#167882,#167883,#167884,#167885,#167886,#167887,
#167888,#167889,#167890,#167891,#167892,#167893,#167894,#167895,#167896,
#167897,#167898,#167899,#167900,#167901,#167902,#167903,#167904,#167905,
#167906,#167907,#167908,#167909,#167910,#167911,#167912,#167913,#167914,
#167915,#167916,#167917,#167918,#167919,#167920,#167921,#167922,#167923,
#167924,#167925,#167926,#167927,#167928,#167929,#167930,#167931,#167932,
#167933,#167934,#167935,#167936,#167937,#167938,#167939,#167940,#167941,
#167942,#167943,#167944,#167945,#167946,#167947,#167948,#167949,#167950,
#167951,#167952,#167953,#167954,#167955,#167956,#167957,#167958,#167959,
#167960,#167961,#167962,#167963,#167964,#167965,#167966,#167967,#167968,
#167969,#167970,#167971,#167972,#167973,#167974,#167975,#167976,#167977,
#167978,#167979,#167980,#167981,#167982,#167983,#167984,#167985,#167986,
#167987,#167988,#167989,#167990),.UNSPECIFIED.,.F.,.F.,(4,2,2,2,2,2,2,2,
2,2,2,2,2,2,2,2,2,2,2,2,2,2,2,2,2,2,2,2,2,2,2,2,2,2,2,2,2,2,2,2,2,2,2,2,
2,2,2,2,2,2,2,2,2,2,2,2,2,2,2,2,2,2,2,2,2,2,2,2,2,2,2,2,2,2,2,2,2,2,2,2,
2,2,2,2,2,2,2,2,2,2,2,2,2,2,2,2,2,2,2,2,2,2,2,2,2,2,2,2,2,2,2,2,2,2,2,2,
2,2,2,2,2,2,2,2,2,2,2,2,2,4),(-20.9006012202032,-20.9001713274698,-20.8931717655193,
-20.8821215261626,-20.8491311403437,-20.6723703761679,-20.5554857242621,
-20.5312640626005,-20.5170832713651,-20.5045162344918,-20.4886402304745,
-20.46335858551,-20.2855464468007,-20.2606342106676,-20.2051108428453,-20.1828357216655,
-20.1659386604881,-20.1573223608734,-20.1502549590852,-20.1412643971362,
-20.1224609782449,-19.9804519675184,-19.8387658755263,-19.8142454645421,
-19.8000045625636,-19.7874461825262,-19.7716650630128,-19.7406895076086,
-19.5597765529035,-19.4714198381321,-19.427641443944,-19.4158629181493,
-19.4087029927893,-19.4020837514475,-19.394050690327,-19.3734642567595,
-19.2557971422429,-19.1499911356937,-19.0598695108081,-19.0371373970091,
-19.0232774638021,-19.0106433339887,-18.9944603255084,-18.9675225755179,
-18.8078568045629,-18.6878347478868,-18.6722585963133,-18.6639140204238,
-18.6568222275419,-18.6476339708278,-18.6272380245924,-18.524672664206,
-18.4373387556432,-18.3744826699684,-18.3316724264722,-18.3140334760254,
-18.30121609886,-18.2894116798905,-18.2701973403491,-18.2206891858261,-18.02308286435,
-17.9458270936638,-17.9275103897592,-17.9190020728669,-17.9124592911764,
-17.9047578257945,-17.8908841094032,-17.8204478463093,-17.6798613297729,
-17.578405869207,-17.5492629245707,-17.5340520893621,-17.5227452498584,
-17.5085248488967,-17.4841031272564,-17.3541406182398,-17.2572377856411,
-17.2132418255269,-17.1852813098867,-17.1747745418703,-17.1675124160736,
-17.159738620634,-17.1468124030856,-17.1011576398705,-16.9554451076541,
-16.8859350592151,-16.8400038759811,-16.8218914626414,-16.8089891702259,
-16.7972811244549,-16.7815821181825,-16.7427129174984,-16.5555966950846,
-16.4808374821355,-16.4412822773744,-16.4298937963868,-16.4228196488019,
-16.4161533791638,-16.4079324339744,-16.3877038028021,-16.2729139990718,
-16.1736785289361,-16.1085075153986,-16.0639811768673,-16.0460508824072,
-16.033180786685,-16.0214354292174,-16.00558215487,-15.9659871155828,-15.7822086477371,
-15.7266708932671,-15.7043913636228,-15.6874913849516,-15.6788740340354,
-15.6718060178269,-15.6628149885053,-15.6440116358243,-15.5019690116316,
-15.3602881984508,-15.3357658661288,-15.3215237544323,-15.3089642519043,
-15.293181647654,-15.2622029365615,-15.0812788830013,-14.9929111169226,
-14.9491279008498,-14.9373482475801,-14.9301876685023,-14.9292022091245),
 .UNSPECIFIED.);
#30153=B_SPLINE_CURVE_WITH_KNOTS('',3,(#167991,#167992,#167993,#167994,
#167995,#167996,#167997,#167998,#167999,#168000,#168001,#168002,#168003,
#168004,#168005,#168006,#168007,#168008,#168009,#168010,#168011,#168012,
#168013,#168014,#168015,#168016,#168017,#168018,#168019,#168020,#168021,
#168022,#168023,#168024,#168025,#168026,#168027,#168028,#168029,#168030,
#168031,#168032,#168033,#168034,#168035,#168036,#168037,#168038,#168039,
#168040,#168041,#168042,#168043,#168044,#168045,#168046,#168047,#168048,
#168049,#168050,#168051,#168052,#168053,#168054,#168055,#168056,#168057,
#168058,#168059,#168060,#168061,#168062,#168063,#168064,#168065,#168066,
#168067,#168068,#168069,#168070,#168071,#168072,#168073,#168074,#168075,
#168076,#168077,#168078,#168079,#168080,#168081,#168082,#168083,#168084,
#168085,#168086,#168087,#168088,#168089,#168090,#168091,#168092,#168093,
#168094,#168095,#168096,#168097,#168098,#168099,#168100,#168101,#168102,
#168103,#168104,#168105,#168106,#168107,#168108,#168109,#168110,#168111,
#168112,#168113,#168114,#168115,#168116,#168117,#168118,#168119,#168120,
#168121,#168122,#168123,#168124,#168125,#168126,#168127,#168128,#168129,
#168130,#168131,#168132,#168133,#168134,#168135,#168136,#168137,#168138,
#168139,#168140,#168141,#168142,#168143,#168144,#168145,#168146,#168147,
#168148,#168149,#168150,#168151,#168152,#168153,#168154,#168155,#168156,
#168157,#168158,#168159,#168160,#168161,#168162,#168163,#168164,#168165,
#168166,#168167,#168168,#168169,#168170,#168171,#168172,#168173,#168174,
#168175,#168176,#168177,#168178,#168179,#168180,#168181,#168182,#168183,
#168184,#168185,#168186,#168187,#168188,#168189,#168190,#168191,#168192,
#168193,#168194,#168195,#168196,#168197,#168198,#168199,#168200,#168201,
#168202,#168203,#168204,#168205,#168206,#168207,#168208,#168209,#168210,
#168211,#168212,#168213,#168214,#168215,#168216,#168217,#168218,#168219,
#168220,#168221,#168222,#168223,#168224,#168225,#168226,#168227,#168228,
#168229,#168230,#168231,#168232,#168233,#168234,#168235,#168236,#168237,
#168238,#168239,#168240,#168241,#168242,#168243,#168244,#168245,#168246,
#168247,#168248,#168249,#168250,#168251,#168252),.UNSPECIFIED.,.F.,.F.,
(4,2,2,2,2,2,2,2,2,2,2,2,2,2,2,2,2,2,2,2,2,2,2,2,2,2,2,2,2,2,2,2,2,2,2,
2,2,2,2,2,2,2,2,2,2,2,2,2,2,2,2,2,2,2,2,2,2,2,2,2,2,2,2,2,2,2,2,2,2,2,2,
2,2,2,2,2,2,2,2,2,2,2,2,2,2,2,2,2,2,2,2,2,2,2,2,2,2,2,2,2,2,2,2,2,2,2,2,
2,2,2,2,2,2,2,2,2,2,2,2,2,2,2,2,2,2,2,2,2,2,2,4),(-6.88983016741359,-6.88913187945072,
-6.88205655671293,-6.87066487676115,-6.83108467296479,-6.75625495688335,
-6.56886418117328,-6.53027002139335,-6.51459700351551,-6.50289434311178,
-6.48998415268692,-6.4718342803467,-6.42565615619463,-6.35560590871231,
-6.21578913304267,-6.16583993697248,-6.15250743531802,-6.1446440885681,
-6.13742341550088,-6.12715205788757,-6.10080113134887,-6.06033902727961,
-5.95983271440256,-5.82778172939104,-5.80334462110304,-5.78912002043135,
-5.77781239346956,-5.76260379046175,-5.73347656809926,-5.63214325597553,
-5.49173722693558,-5.4209469594796,-5.40705737814925,-5.39935189510391,
-5.39280883646972,-5.38430422767557,-5.36601016540622,-5.28896143768228,
-5.08935389687434,-5.04113647014719,-5.0221144770105,-5.01034384103868,
-4.99749669163258,-4.97969390512581,-4.93583173165814,-4.87077658430402,
-4.78532759720732,-4.6844124882172,-4.66406498299851,-4.6548848352987,-4.6477931940593,
-4.63944137778573,-4.62383313110876,-4.60373553696183,-4.55634851930268,
-4.46317227607844,-4.33478378698708,-4.31038409151202,-4.2961677363078,
-4.28485940041794,-4.26964044790941,-4.24046076520245,-4.13875038094999,
-3.9978726072158,-3.92796285072478,-3.91411016406304,-3.90641306564974,
-3.89986918837637,-3.89135321171877,-3.87299747003301,-3.79540589136508,
-3.6111522481167,-3.55164796341351,-3.53107379195006,-3.51767547057735,
-3.50485645359576,-3.48721272592217,-3.44437778906765,-3.38147208978702,
-3.29420172201006,-3.19161934222916,-3.17122132608957,-3.16203223373006,
-3.15493984144054,-3.14659461208925,-3.13101737798728,-3.01099143845297,
-2.85131565252643,-2.82437621305624,-2.80819199776416,-2.79555682039172,
-2.78169563072154,-2.7589612123388,-2.66882740144109,-2.56300786050056,
-2.4453266069816,-2.42473805582632,-2.41670424819144,-2.41008442896301,
-2.40292391733999,-2.39114451031011,-2.34736358150708,-2.25900381099065,
-2.07808271695856,-2.04710499079443,-2.03132262104751,-2.01876317554152,
-2.00452099006845,-1.9799981858713,-1.83829539055137,-1.69626853256855,
-1.67746325548576,-1.66847186983495,-1.66140385800443,-1.6527868476265,
-1.63588850664463,-1.61361192701009,-1.55808564607875,-1.37436955231147,
-1.33472785306068,-1.31886697147818,-1.30711978196907,-1.29425137666648,
-1.27633036569073,-1.23186467230361,-1.16681634436809,-1.06744511505669,
-0.952573777543494,-0.93234314610872,-0.924121854583241,-0.918151647035043),
 .UNSPECIFIED.);
#30154=B_SPLINE_CURVE_WITH_KNOTS('',3,(#168257,#168258,#168259,#168260,
#168261,#168262,#168263,#168264,#168265,#168266,#168267,#168268,#168269,
#168270,#168271,#168272,#168273,#168274,#168275,#168276,#168277,#168278),
 .UNSPECIFIED.,.F.,.F.,(4,2,2,2,2,2,2,2,2,2,4),(5.94644245477199,6.60767518318918,
7.16805975801899,7.45354600572087,8.24302433165703,8.85682530139938,9.73093935598426,
10.4069887989121,10.7296063241796,11.5427165923998,12.1931059899322),
 .UNSPECIFIED.);
#30155=B_SPLINE_CURVE_WITH_KNOTS('',3,(#168285,#168286,#168287,#168288,
#168289,#168290,#168291,#168292,#168293,#168294,#168295,#168296,#168297,
#168298,#168299,#168300,#168301,#168302,#168303,#168304,#168305,#168306,
#168307,#168308,#168309,#168310,#168311,#168312,#168313,#168314,#168315,
#168316,#168317,#168318,#168319,#168320,#168321,#168322,#168323,#168324,
#168325,#168326,#168327,#168328,#168329,#168330,#168331,#168332,#168333,
#168334,#168335,#168336,#168337,#168338,#168339,#168340,#168341,#168342,
#168343,#168344,#168345,#168346,#168347,#168348,#168349,#168350,#168351,
#168352,#168353,#168354,#168355,#168356,#168357,#168358,#168359,#168360,
#168361,#168362,#168363,#168364,#168365,#168366,#168367,#168368,#168369,
#168370,#168371,#168372,#168373,#168374,#168375,#168376,#168377,#168378,
#168379,#168380,#168381,#168382,#168383,#168384,#168385,#168386,#168387,
#168388,#168389,#168390,#168391,#168392,#168393,#168394,#168395,#168396,
#168397,#168398,#168399,#168400,#168401,#168402,#168403,#168404,#168405,
#168406,#168407,#168408,#168409,#168410,#168411,#168412,#168413,#168414,
#168415,#168416,#168417,#168418,#168419,#168420,#168421,#168422,#168423,
#168424,#168425,#168426,#168427,#168428,#168429,#168430,#168431,#168432,
#168433,#168434,#168435,#168436,#168437,#168438,#168439,#168440,#168441,
#168442,#168443,#168444,#168445,#168446,#168447,#168448,#168449,#168450,
#168451,#168452,#168453,#168454),.UNSPECIFIED.,.F.,.F.,(4,2,2,2,2,2,2,2,
2,2,2,2,2,2,2,2,2,2,2,2,2,2,2,2,2,2,2,2,2,2,2,2,2,2,2,2,2,2,2,2,2,2,2,2,
2,2,2,2,2,2,2,2,2,2,2,2,2,2,2,2,2,2,2,2,2,2,2,2,2,2,2,2,2,2,2,2,2,2,2,2,
2,2,2,2,4),(6.28535341527715,6.2882021757388,6.29605541836851,6.31102864908079,
6.43737275494601,6.63842224468773,6.66961171887247,6.68545158990087,6.69801645538159,
6.71220958836953,6.7364685902245,6.85630095703125,6.94659497629758,6.99453804280581,
7.04788912249746,7.06155273754703,7.06949213793895,7.07666834134776,7.08667011430709,
7.11120329448208,7.1476244638425,7.27630821386669,7.40475824841285,7.42926164513167,
7.44364646837022,7.45618756100137,7.47174426974938,7.50255643735899,7.61491829777165,
7.77285165013532,7.83346066295643,7.84687487291156,7.85447634465023,7.86036935737998,
7.8686049787064,7.88546936373978,8.02338035809764,8.20747132524815,8.24052449108624,
8.25651548122264,8.26909538961242,8.28319562460639,8.3070237362241,8.41671539152207,
8.54804794796548,8.61753783005534,8.63199261912393,8.64018895056254,8.64658274565332,
8.65566809018836,8.6749299946092,8.75544417864585,8.95913615221126,8.99437645690017,
9.01058745452713,9.02322647636245,9.03706252120184,9.05965723658158,9.14635359296998,
9.34916066368639,9.40547507906998,9.41862132410928,9.42616183785918,9.43206403156523,
9.44038584770225,9.45769282285902,9.54606472904573,9.68702931575528,9.79297945277671,
9.81732212763114,9.83167508673994,9.84421940676834,9.85982122175962,9.89090303956229,
10.0085276021679,10.1331155412817,10.1902336610209,10.2041589880414,10.2121554877834,
10.2193127852824,10.2291918164983,10.2529662604549,10.2878607508683,10.4008697061023,
10.5463583837695),.UNSPECIFIED.);
#30156=B_SPLINE_CURVE_WITH_KNOTS('',3,(#168457,#168458,#168459,#168460,
#168461,#168462,#168463,#168464,#168465,#168466,#168467,#168468,#168469,
#168470,#168471,#168472,#168473,#168474,#168475,#168476,#168477,#168478,
#168479,#168480,#168481,#168482,#168483,#168484,#168485,#168486,#168487,
#168488,#168489,#168490,#168491,#168492,#168493,#168494,#168495,#168496,
#168497,#168498,#168499,#168500,#168501,#168502,#168503,#168504,#168505,
#168506,#168507,#168508,#168509,#168510,#168511,#168512,#168513,#168514,
#168515,#168516,#168517,#168518,#168519,#168520,#168521,#168522,#168523,
#168524,#168525,#168526,#168527,#168528,#168529,#168530,#168531,#168532,
#168533,#168534,#168535,#168536,#168537,#168538,#168539,#168540,#168541,
#168542,#168543,#168544,#168545,#168546,#168547,#168548,#168549,#168550,
#168551,#168552,#168553,#168554,#168555,#168556,#168557,#168558,#168559,
#168560,#168561,#168562,#168563,#168564,#168565,#168566,#168567,#168568,
#168569,#168570,#168571,#168572,#168573,#168574,#168575,#168576,#168577,
#168578,#168579,#168580,#168581,#168582,#168583,#168584,#168585,#168586,
#168587,#168588,#168589,#168590,#168591,#168592,#168593,#168594,#168595,
#168596,#168597,#168598,#168599,#168600,#168601,#168602,#168603,#168604,
#168605,#168606,#168607,#168608,#168609,#168610,#168611,#168612,#168613,
#168614,#168615,#168616,#168617,#168618,#168619,#168620,#168621,#168622,
#168623,#168624,#168625,#168626),.UNSPECIFIED.,.F.,.F.,(4,2,2,2,2,2,2,2,
2,2,2,2,2,2,2,2,2,2,2,2,2,2,2,2,2,2,2,2,2,2,2,2,2,2,2,2,2,2,2,2,2,2,2,2,
2,2,2,2,2,2,2,2,2,2,2,2,2,2,2,2,2,2,2,2,2,2,2,2,2,2,2,2,2,2,2,2,2,2,2,2,
2,2,2,2,4),(1.00000001185263E-6,0.150101630938482,0.170066194866638,0.179282640036017,
0.186361094252854,0.194748588751972,0.210058493834735,0.316330590351473,
0.435034177154938,0.521604396572538,0.544106270412088,0.557919985969065,
0.570565783326518,0.586820611551792,0.622241305541521,0.84800481608078,
0.913931869336241,0.950727236159845,0.961855658571001,0.968875094076227,
0.975562470997592,0.983858611106606,1.00475445095198,1.12080859978613,1.21725245728034,
1.33448460862351,1.3589192729214,1.37315386374228,1.38571315148011,1.40149051951235,
1.43347410104357,1.58431113222412,1.64004883439538,1.72963380932092,1.74455462876196,
1.75276600851946,1.75987086077602,1.76919159027147,1.79028359486636,1.9026442337869,
2.00292651393419,2.06259211451374,2.10406030440563,2.12151597717192,2.13430430318827,
2.14614602816371,2.16554724661403,2.21600599884866,2.41998820713048,2.48550210351074,
2.52214600587198,2.53325856796103,2.54027469808609,2.5469647451392,2.55527026966158,
2.5762216464443,2.69549981884673,2.81463287731623,2.90837872677946,2.9314844011882,
2.94543206021137,2.958044291966,2.97431291194609,3.00088446214869,3.20676318283083,
3.29314567079042,3.31305386420129,3.32226044982287,3.32933874691901,3.33773489966039,
3.35308167124301,3.46207783141478,3.5408332891298,3.661231340971,3.68551358051179,
3.69971254026873,3.71227789042278,3.72811210673465,3.76034118921313,3.95468021994065,
3.98625084726419,4.08243792313468,4.10007838852451,4.10846490510006,4.11237294021447),
 .UNSPECIFIED.);
#30157=B_SPLINE_CURVE_WITH_KNOTS('',3,(#168631,#168632,#168633,#168634,
#168635,#168636,#168637,#168638,#168639,#168640,#168641,#168642,#168643,
#168644,#168645,#168646,#168647,#168648,#168649,#168650,#168651,#168652,
#168653,#168654,#168655,#168656,#168657,#168658,#168659,#168660,#168661,
#168662,#168663,#168664,#168665,#168666,#168667,#168668,#168669,#168670,
#168671,#168672,#168673,#168674,#168675,#168676,#168677,#168678,#168679,
#168680,#168681,#168682,#168683,#168684,#168685,#168686,#168687,#168688,
#168689,#168690,#168691,#168692,#168693,#168694,#168695,#168696,#168697,
#168698,#168699,#168700,#168701,#168702,#168703,#168704,#168705,#168706,
#168707,#168708,#168709,#168710,#168711,#168712,#168713,#168714,#168715,
#168716,#168717,#168718,#168719,#168720,#168721,#168722,#168723,#168724,
#168725,#168726,#168727,#168728,#168729,#168730,#168731,#168732,#168733,
#168734,#168735,#168736,#168737,#168738,#168739,#168740,#168741,#168742,
#168743,#168744,#168745,#168746,#168747,#168748,#168749,#168750,#168751,
#168752,#168753,#168754,#168755,#168756,#168757,#168758,#168759,#168760,
#168761,#168762,#168763,#168764,#168765,#168766,#168767,#168768,#168769,
#168770,#168771,#168772,#168773,#168774,#168775,#168776,#168777,#168778,
#168779,#168780,#168781,#168782,#168783,#168784,#168785,#168786,#168787,
#168788,#168789,#168790,#168791,#168792,#168793,#168794,#168795,#168796,
#168797,#168798,#168799,#168800,#168801,#168802,#168803,#168804,#168805,
#168806,#168807,#168808,#168809,#168810,#168811,#168812,#168813,#168814,
#168815,#168816,#168817,#168818,#168819,#168820,#168821,#168822,#168823,
#168824,#168825,#168826,#168827,#168828,#168829,#168830,#168831,#168832,
#168833,#168834,#168835,#168836,#168837,#168838,#168839,#168840,#168841,
#168842,#168843,#168844,#168845,#168846,#168847,#168848,#168849,#168850,
#168851,#168852,#168853,#168854,#168855,#168856,#168857,#168858,#168859,
#168860,#168861,#168862,#168863,#168864,#168865,#168866,#168867,#168868,
#168869,#168870,#168871,#168872,#168873,#168874,#168875,#168876,#168877,
#168878,#168879,#168880,#168881,#168882,#168883,#168884,#168885,#168886,
#168887,#168888,#168889,#168890,#168891,#168892,#168893,#168894,#168895,
#168896,#168897,#168898,#168899,#168900,#168901,#168902),.UNSPECIFIED.,
 .F.,.F.,(4,2,2,2,2,2,2,2,2,2,2,2,2,2,2,2,2,2,2,2,2,2,2,2,2,2,2,2,2,2,2,
2,2,2,2,2,2,2,2,2,2,2,2,2,2,2,2,2,2,2,2,2,2,2,2,2,2,2,2,2,2,2,2,2,2,2,2,
2,2,2,2,2,2,2,2,2,2,2,2,2,2,2,2,2,2,2,2,2,2,2,2,2,2,2,2,2,2,2,2,2,2,2,2,
2,2,2,2,2,2,2,2,2,2,2,2,2,2,2,2,2,2,2,2,2,2,2,2,2,2,2,2,2,2,2,2,4),(9.99999999287575E-7,
0.00579850576153826,0.0130944527428375,0.0312216908045841,0.163439922679926,
0.283087003150158,0.339763914128201,0.380142608406775,0.397437276560381,
0.410198455738976,0.422080475513747,0.441697421133798,0.493971521459607,
0.676471733323956,0.753758194362052,0.772650638227882,0.781665847663628,
0.788051868319968,0.796296770705438,0.81096749919682,0.885366770739691,
1.01994513665708,1.08770771085909,1.13312676587809,1.15119793582843,1.16409485308743,
1.1758052929941,1.19150611991899,1.22216538739257,1.3900571992775,1.48397377965424,
1.5485818796735,1.56183522765093,1.56932203819386,1.57589345274377,1.58453343338458,
1.60404586310083,1.76897444173588,1.9080950100385,1.9506200734075,1.96826493692671,
1.98108579046468,1.99447300352144,2.01498659070443,2.07385730127611,2.24945901727584,
2.3253583410306,2.34408872720265,2.35307295373937,2.35945578029628,2.36772302362599,
2.38249325130372,2.45845701526486,2.59112407090777,2.65899065332678,2.7044588852972,
2.72253748740991,2.73543581242198,2.7471449159159,2.7628400386619,2.80128879284624,
3.00159230559794,3.02120568491813,3.08719297854698,3.12401020127794,3.13514080317366,
3.14216062614208,3.14884751616431,3.15714215977869,3.17802955164812,3.30232441387236,
3.41284103904473,3.47702967743191,3.52128993031315,3.53920839103398,3.55207833050819,
3.5638205452224,3.58266524932496,3.62972081729748,3.81840317907358,3.89636745759488,
3.91533878679841,3.92436925730299,3.93075713430037,3.93899184877964,3.95361631767279,
4.02580908780727,4.16285994804546,4.23052055026061,4.27589195482301,4.29395642310159,
4.30685250034773,4.31856482546026,4.3342721450285,4.36495623236491,4.52847566179826,
4.59036293734492,4.65786274620942,4.69523138105016,4.70642031242063,4.71345305817074,
4.72013168762499,4.72839469380622,4.748843539932,4.89135152044875,5.01667084527042,
5.0625835962627,5.09701600028071,5.1132662608486,5.12587601579613,5.13983170110593,
5.16298891662328,5.24872203885499,5.2729098659224,5.40421699200536,5.41407604116132,
5.47550495518287,5.48954889310835,5.49765233942526,5.50478027069231,5.51445064472022,
5.53697449813832,5.56940984470954,5.67197838103664,5.82120496738593,5.85324470132735,
5.86903283780541,5.88159303574035,5.89582048127871,5.92022221704508,6.03674823352164,
6.17586231118275,6.26019775401805,6.27341835675887,6.28167831501583,6.28535341527715),
 .UNSPECIFIED.);
#30158=B_SPLINE_CURVE_WITH_KNOTS('',3,(#168903,#168904,#168905,#168906,
#168907,#168908,#168909,#168910,#168911,#168912,#168913,#168914,#168915,
#168916,#168917,#168918,#168919,#168920,#168921,#168922,#168923,#168924,
#168925,#168926,#168927,#168928,#168929,#168930,#168931,#168932,#168933,
#168934,#168935,#168936,#168937,#168938,#168939,#168940,#168941,#168942,
#168943,#168944,#168945,#168946,#168947,#168948,#168949,#168950,#168951,
#168952,#168953,#168954,#168955,#168956,#168957,#168958,#168959,#168960,
#168961,#168962,#168963,#168964,#168965,#168966,#168967,#168968,#168969,
#168970,#168971,#168972,#168973,#168974,#168975,#168976,#168977,#168978,
#168979,#168980,#168981,#168982,#168983,#168984,#168985,#168986,#168987,
#168988,#168989,#168990,#168991,#168992,#168993,#168994,#168995,#168996,
#168997,#168998,#168999,#169000,#169001,#169002,#169003,#169004,#169005,
#169006,#169007,#169008,#169009,#169010,#169011,#169012,#169013,#169014,
#169015,#169016,#169017,#169018,#169019,#169020,#169021,#169022,#169023,
#169024,#169025,#169026,#169027,#169028,#169029,#169030,#169031,#169032,
#169033,#169034,#169035,#169036,#169037,#169038,#169039,#169040,#169041,
#169042,#169043,#169044,#169045,#169046,#169047,#169048,#169049,#169050,
#169051,#169052,#169053,#169054,#169055,#169056,#169057,#169058,#169059,
#169060,#169061,#169062,#169063,#169064,#169065,#169066,#169067,#169068,
#169069,#169070,#169071,#169072,#169073,#169074,#169075,#169076,#169077,
#169078,#169079,#169080,#169081,#169082,#169083,#169084,#169085,#169086,
#169087,#169088,#169089,#169090,#169091,#169092,#169093,#169094,#169095,
#169096,#169097,#169098,#169099,#169100,#169101,#169102,#169103,#169104,
#169105,#169106,#169107,#169108,#169109,#169110,#169111,#169112,#169113,
#169114,#169115,#169116,#169117,#169118,#169119,#169120,#169121,#169122,
#169123,#169124,#169125,#169126,#169127,#169128,#169129,#169130,#169131,
#169132,#169133,#169134,#169135,#169136,#169137,#169138,#169139,#169140,
#169141,#169142,#169143,#169144,#169145,#169146,#169147,#169148,#169149,
#169150,#169151,#169152,#169153,#169154),.UNSPECIFIED.,.F.,.F.,(4,2,2,2,
2,2,2,2,2,2,2,2,2,2,2,2,2,2,2,2,2,2,2,2,2,2,2,2,2,2,2,2,2,2,2,2,2,2,2,2,
2,2,2,2,2,2,2,2,2,2,2,2,2,2,2,2,2,2,2,2,2,2,2,2,2,2,2,2,2,2,2,2,2,2,2,2,
2,2,2,2,2,2,2,2,2,2,2,2,2,2,2,2,2,2,2,2,2,2,2,2,2,2,2,2,2,2,2,2,2,2,2,2,
2,2,2,2,2,2,2,2,2,2,2,2,2,4),(4.11237294021447,4.11499671540717,4.12275024725038,
4.13683830501483,4.20978481128889,4.35604088880456,4.46691615971153,4.49752961927095,
4.51304796272934,4.52558752430315,4.54000297149108,4.56463849871281,4.70111758557034,
4.82312637138642,4.85861870830937,4.88269262212078,4.89262103687441,4.89978637009214,
4.90776066981282,4.92158188465078,4.97712479566213,5.12304864411524,5.23352835707963,
5.25739535856455,5.27150488114816,5.28408466278652,5.30006401991669,5.333050898281,
5.5181062787572,5.65345504765757,5.67143550863331,5.67988672844655,5.6864234272891,
5.69412908227144,5.70800319637131,5.77711412488523,5.934056353816,6.04921965618755,
6.07355850453487,6.08777303761054,6.1003361048332,6.11614692858305,6.14830104965685,
6.28008600210841,6.42798092955698,6.45365732446582,6.46383937666132,6.47104577798304,
6.47890933151204,6.49222419299424,6.54163787607225,6.69229401929071,6.80493120638159,
6.82889626978474,6.84302694337066,6.85560310826527,6.87154732706019,6.90434975836392,
7.09179331270864,7.22950648522972,7.2446744633357,7.25256853281062,7.25909094906039,
7.26730456963467,7.28036948296626,7.35908002395987,7.50405901090792,7.62067937323755,
7.64508719825605,7.65931671199228,7.67187784592876,7.6876659723343,7.71970146956426,
7.86898929485801,7.97152845851285,8.00395985205691,8.0264822770266,8.03615289547914,
8.04328135068401,8.05138578328401,8.06543225656834,8.12688992260981,8.15132715251319,
8.2596074085133,8.37615632891564,8.40028841541381,8.4144552245251,8.42702575626741,
8.44291177725569,8.4754092597276,8.66657758043566,8.80098951246528,8.81619630230322,
8.82409848938872,8.83062069222283,8.83882534150094,8.85186014475097,8.92965837482495,
9.07493776300742,9.19218121001687,9.21661824665642,9.23085422137612,9.24341473125934,
9.25919363608272,9.29118033834613,9.44306193458432,9.54367339790887,9.57577175484967,
9.59812209770917,9.60776344964721,9.6148881825251,9.62300890999991,9.63712669646708,
9.69989933794189,9.8206613702415,9.94708314232956,9.97157566291891,9.98582009690826,
9.99837945079697,10.0141445049674,10.0460144784218,10.2807586240382,10.3693192933289,
10.386629671906,10.394952971852,10.398744700606),.UNSPECIFIED.);
#30159=B_SPLINE_CURVE_WITH_KNOTS('',3,(#169159,#169160,#169161,#169162,
#169163,#169164,#169165,#169166,#169167,#169168,#169169,#169170,#169171,
#169172,#169173,#169174,#169175,#169176,#169177,#169178,#169179,#169180,
#169181,#169182,#169183,#169184,#169185,#169186,#169187,#169188,#169189,
#169190,#169191,#169192,#169193,#169194,#169195,#169196,#169197,#169198,
#169199,#169200,#169201,#169202,#169203,#169204,#169205,#169206,#169207,
#169208,#169209,#169210,#169211,#169212,#169213,#169214,#169215,#169216,
#169217,#169218,#169219,#169220,#169221,#169222,#169223,#169224,#169225,
#169226,#169227,#169228,#169229,#169230,#169231,#169232,#169233,#169234,
#169235,#169236,#169237,#169238,#169239,#169240,#169241,#169242,#169243,
#169244,#169245,#169246,#169247,#169248,#169249,#169250,#169251,#169252,
#169253,#169254,#169255,#169256,#169257,#169258,#169259,#169260,#169261,
#169262,#169263,#169264,#169265,#169266,#169267,#169268,#169269,#169270,
#169271,#169272,#169273,#169274,#169275,#169276,#169277,#169278,#169279,
#169280,#169281,#169282,#169283,#169284,#169285,#169286,#169287,#169288,
#169289,#169290,#169291,#169292,#169293,#169294,#169295,#169296,#169297,
#169298,#169299,#169300,#169301,#169302,#169303,#169304,#169305,#169306,
#169307,#169308,#169309,#169310,#169311,#169312,#169313,#169314,#169315,
#169316,#169317,#169318,#169319,#169320,#169321,#169322,#169323,#169324,
#169325,#169326,#169327,#169328,#169329,#169330,#169331,#169332,#169333,
#169334,#169335,#169336,#169337,#169338,#169339,#169340,#169341,#169342,
#169343,#169344,#169345,#169346,#169347,#169348,#169349,#169350,#169351,
#169352,#169353,#169354,#169355,#169356,#169357,#169358,#169359,#169360,
#169361,#169362,#169363,#169364,#169365,#169366,#169367,#169368,#169369,
#169370,#169371,#169372,#169373,#169374,#169375,#169376,#169377,#169378,
#169379,#169380,#169381,#169382,#169383,#169384,#169385,#169386,#169387,
#169388,#169389,#169390,#169391,#169392,#169393,#169394,#169395,#169396,
#169397,#169398,#169399,#169400,#169401,#169402,#169403,#169404,#169405,
#169406,#169407,#169408,#169409,#169410),.UNSPECIFIED.,.F.,.F.,(4,2,2,2,
2,2,2,2,2,2,2,2,2,2,2,2,2,2,2,2,2,2,2,2,2,2,2,2,2,2,2,2,2,2,2,2,2,2,2,2,
2,2,2,2,2,2,2,2,2,2,2,2,2,2,2,2,2,2,2,2,2,2,2,2,2,2,2,2,2,2,2,2,2,2,2,2,
2,2,2,2,2,2,2,2,2,2,2,2,2,2,2,2,2,2,2,2,2,2,2,2,2,2,2,2,2,2,2,2,2,2,2,2,
2,2,2,2,2,2,2,2,2,2,2,2,2,4),(17.0758907305399,17.0798166350792,17.0882129209521,
17.105905153377,17.2444158663091,17.426428078424,17.459622874717,17.4756414594216,
17.4882250997439,17.5023107956712,17.5260684540758,17.6342620918617,17.7654974805742,
17.8365209489007,17.8510995376378,17.8593241227922,17.8657138629315,17.8747595927644,
17.8938100934201,17.9724594159901,18.1722338642068,18.2108072615323,18.2265118770991,
18.2382237784594,18.2511231586535,18.2692007711738,18.3144950827931,18.3807542873899,
18.4889661851832,18.6118628459642,18.6328859914446,18.6412077212122,18.647901962198,
18.6549114403332,18.6659943338251,18.7023633466317,18.7671353237329,18.9999060308964,
19.0318809578003,19.047665143945,19.0602248040117,19.0744536190217,19.0988787402169,
19.223344276648,19.3402849661336,19.4084121406566,19.42279793497,19.4309787255063,
19.4373752639112,19.4464838998575,19.4658693135521,19.5474830491216,19.5843922286228,
19.7569805605909,19.7845790192998,19.8009653554527,19.8136297031117,19.8273820175657,
19.8495890327939,19.9313998380183,20.106038918756,20.193591928415,20.2069032270294,
20.2151902137928,20.2217152871771,20.2295458143085,20.2444105787853,20.361350433356,
20.5655089110364,20.6012945033035,20.6176145467569,20.6302695062486,20.6440514222814,
20.666406735545,20.7516291900446,20.8565065700056,20.9694213497286,20.9905136728443,
20.9998340943112,21.0069385234827,21.0151491862314,21.0300681730316,21.1196154049678,
21.1748681507587,21.3261318313632,21.3581709385152,21.3739583841935,21.386517859895,
21.400744303133,21.425143854543,21.5416471411628,21.6785621967833,21.7649847628388,
21.7782658435484,21.7865436391079,21.7930680104112,21.8009055493004,21.8158047600009,
21.935410808731,22.1449971702972,22.1724889157877,22.1888602393926,22.2015222615868,
22.215279162764,22.2375203072286,22.3212395471551,22.5391114964196,22.560925794966,
22.5697953674184,22.576994920778,22.5846989944394,22.5972913076029,22.6436473705236,
22.7390977572285,22.8979241991219,22.929780157148,22.9455322610994,22.9580885575351,
22.9723380812627,22.9968448691232,23.1156962121063,23.261330431272,23.3360193182187,
23.3505702488122,23.3566815208642,23.3617662463869),.UNSPECIFIED.);
#30160=B_SPLINE_CURVE_WITH_KNOTS('',3,(#169411,#169412,#169413,#169414,
#169415,#169416,#169417,#169418,#169419,#169420,#169421,#169422,#169423,
#169424,#169425,#169426,#169427,#169428,#169429,#169430,#169431,#169432,
#169433,#169434,#169435,#169436,#169437,#169438,#169439,#169440,#169441,
#169442,#169443,#169444,#169445,#169446,#169447,#169448,#169449,#169450,
#169451,#169452,#169453,#169454,#169455,#169456,#169457,#169458,#169459,
#169460,#169461,#169462,#169463,#169464,#169465,#169466,#169467,#169468,
#169469,#169470,#169471,#169472,#169473,#169474,#169475,#169476,#169477,
#169478,#169479,#169480,#169481,#169482,#169483,#169484,#169485,#169486,
#169487,#169488,#169489,#169490,#169491,#169492,#169493,#169494,#169495,
#169496,#169497,#169498,#169499,#169500,#169501,#169502,#169503,#169504,
#169505,#169506,#169507,#169508,#169509,#169510,#169511,#169512,#169513,
#169514,#169515,#169516,#169517,#169518,#169519,#169520,#169521,#169522,
#169523,#169524,#169525,#169526,#169527,#169528,#169529,#169530,#169531,
#169532,#169533,#169534,#169535,#169536,#169537,#169538,#169539,#169540,
#169541,#169542,#169543,#169544,#169545,#169546,#169547,#169548,#169549,
#169550,#169551,#169552,#169553,#169554,#169555,#169556,#169557,#169558,
#169559,#169560,#169561,#169562,#169563,#169564,#169565,#169566,#169567,
#169568,#169569,#169570,#169571,#169572,#169573,#169574,#169575,#169576,
#169577,#169578,#169579,#169580,#169581,#169582,#169583,#169584,#169585,
#169586,#169587,#169588,#169589,#169590,#169591,#169592,#169593,#169594,
#169595,#169596,#169597,#169598,#169599,#169600,#169601,#169602,#169603,
#169604,#169605,#169606,#169607,#169608,#169609,#169610,#169611,#169612,
#169613,#169614,#169615,#169616,#169617,#169618,#169619,#169620,#169621,
#169622,#169623,#169624,#169625,#169626,#169627,#169628,#169629,#169630,
#169631,#169632,#169633,#169634,#169635,#169636,#169637,#169638,#169639,
#169640,#169641,#169642,#169643,#169644,#169645,#169646,#169647,#169648,
#169649,#169650,#169651,#169652,#169653,#169654,#169655,#169656,#169657,
#169658,#169659,#169660,#169661,#169662,#169663,#169664,#169665,#169666,
#169667,#169668,#169669,#169670),.UNSPECIFIED.,.F.,.F.,(4,2,2,2,2,2,2,2,
2,2,2,2,2,2,2,2,2,2,2,2,2,2,2,2,2,2,2,2,2,2,2,2,2,2,2,2,2,2,2,2,2,2,2,2,
2,2,2,2,2,2,2,2,2,2,2,2,2,2,2,2,2,2,2,2,2,2,2,2,2,2,2,2,2,2,2,2,2,2,2,2,
2,2,2,2,2,2,2,2,2,2,2,2,2,2,2,2,2,2,2,2,2,2,2,2,2,2,2,2,2,2,2,2,2,2,2,2,
2,2,2,2,2,2,2,2,2,2,2,2,2,4),(10.398744700606,10.4008561584502,10.4083978533202,
10.4215459790634,10.4778645782516,10.6496659209323,10.7641546126389,10.7884619920227,
10.8026701973569,10.8152349241933,10.8310575500151,10.8632705603044,11.0088451550061,
11.0685600676601,11.1590578976249,11.1740069389689,11.182224918033,11.1893295347377,
11.1986423962117,11.2196860193964,11.327127566098,11.4158727801605,11.4854634052821,
11.5308828072108,11.5494481126179,11.5623104951733,11.5754331156023,11.5946552612859,
11.6480146641304,11.7315857755624,11.9235202464166,11.952807537667,11.9633754704451,
11.9695883861885,11.9763187987357,11.986074391225,12.0118732800191,12.147869975836,
12.3201550382873,12.353828534035,12.3699385514725,12.3825334417738,12.3965691445339,
12.4200906361679,12.5236149349893,12.5892513133597,12.7216981890727,12.7420272310879,
12.7513541844365,12.7584605687789,12.7666698894368,12.7815779544907,12.8706802567874,
12.9156870915836,13.0788730815012,13.1098152906864,13.125595675421,13.1381566642025,
13.1523924342078,13.176827232678,13.2940113866893,13.4359751234392,13.4373849778119,
13.5170347572255,13.5301293116592,13.5383520503394,13.5448751221521,13.5527620192768,
13.5678942446418,13.7029026680166,13.8935507814303,13.9260940669884,13.9419891557434,
13.9545608964675,13.9687227709009,13.9928307458483,14.108782208555,14.2101541347645,
14.3013796617016,14.3166829553153,14.3250697110483,14.3321494089144,14.3413698938271,
14.3613520087862,14.4484221221795,14.5996623324507,14.6677741203912,14.6892948812208,
14.7028983303647,14.7156186369075,14.7326491796368,14.7714528188204,14.9085920463417,
15.0756709768052,15.0983213867863,15.1078750838088,15.1145012819586,15.1216269857896,
15.1332347905824,15.1748225824595,15.254629643548,15.4546686420783,15.4933965839387,
15.5091400695916,15.5208618855114,15.5337512176802,15.5517737548373,15.5968598132321,
15.6639151023815,15.75527402183,15.8641882624848,15.8852646694166,15.8945831053084,
15.9016881703043,15.9099021298115,15.9248331507426,16.0147265192899,16.0733653851664,
16.2207298875367,16.252893513232,16.2687063176727,16.2812697411125,16.2954833809431,
16.3198174413809,16.4348764186703,16.5931907105774,16.661136587772,16.6749536492156,
16.6826465666522,16.6851291404356),.UNSPECIFIED.);
#30161=B_SPLINE_CURVE_WITH_KNOTS('',3,(#169675,#169676,#169677,#169678,
#169679,#169680,#169681,#169682,#169683,#169684,#169685,#169686,#169687,
#169688,#169689,#169690,#169691,#169692,#169693,#169694,#169695,#169696,
#169697,#169698,#169699,#169700,#169701,#169702,#169703,#169704,#169705,
#169706,#169707,#169708,#169709,#169710,#169711,#169712,#169713,#169714,
#169715,#169716,#169717,#169718,#169719,#169720,#169721,#169722,#169723,
#169724,#169725,#169726,#169727,#169728,#169729,#169730,#169731,#169732,
#169733,#169734,#169735,#169736,#169737,#169738,#169739,#169740,#169741,
#169742,#169743,#169744,#169745,#169746,#169747,#169748,#169749,#169750,
#169751,#169752,#169753,#169754,#169755,#169756,#169757,#169758,#169759,
#169760,#169761,#169762,#169763,#169764,#169765,#169766,#169767,#169768,
#169769,#169770,#169771,#169772,#169773,#169774,#169775,#169776,#169777,
#169778,#169779,#169780,#169781,#169782,#169783,#169784,#169785,#169786,
#169787,#169788,#169789,#169790,#169791,#169792,#169793,#169794,#169795,
#169796,#169797,#169798,#169799,#169800,#169801,#169802,#169803,#169804,
#169805,#169806,#169807,#169808,#169809,#169810,#169811,#169812,#169813,
#169814,#169815,#169816,#169817,#169818,#169819,#169820,#169821,#169822,
#169823,#169824,#169825,#169826,#169827,#169828,#169829,#169830,#169831,
#169832,#169833,#169834,#169835,#169836,#169837,#169838,#169839,#169840,
#169841,#169842,#169843,#169844,#169845,#169846,#169847,#169848,#169849,
#169850,#169851,#169852,#169853,#169854,#169855,#169856,#169857,#169858,
#169859,#169860,#169861,#169862,#169863,#169864,#169865,#169866,#169867,
#169868,#169869,#169870,#169871,#169872,#169873,#169874,#169875,#169876,
#169877,#169878,#169879,#169880,#169881,#169882,#169883,#169884,#169885,
#169886,#169887,#169888,#169889,#169890,#169891,#169892,#169893,#169894,
#169895,#169896,#169897,#169898,#169899,#169900,#169901,#169902,#169903,
#169904,#169905,#169906,#169907,#169908,#169909,#169910,#169911,#169912,
#169913,#169914,#169915,#169916,#169917,#169918,#169919,#169920,#169921,
#169922,#169923,#169924,#169925,#169926,#169927,#169928,#169929,#169930,
#169931,#169932),.UNSPECIFIED.,.F.,.F.,(4,2,2,2,2,2,2,2,2,2,2,2,2,2,2,2,
2,2,2,2,2,2,2,2,2,2,2,2,2,2,2,2,2,2,2,2,2,2,2,2,2,2,2,2,2,2,2,2,2,2,2,2,
2,2,2,2,2,2,2,2,2,2,2,2,2,2,2,2,2,2,2,2,2,2,2,2,2,2,2,2,2,2,2,2,2,2,2,2,
2,2,2,2,2,2,2,2,2,2,2,2,2,2,2,2,2,2,2,2,2,2,2,2,2,2,2,2,2,2,2,2,2,2,2,2,
2,2,2,2,4),(10.7898186351041,10.7921918032135,10.7998388212371,10.81345228456,
10.8774594094187,11.0730362515152,11.1297095366792,11.1700874911333,11.1873832545396,
11.2001457554164,11.212029370956,11.2316498044645,11.2839383106706,11.4490478245626,
11.5412621511017,11.5617799221726,11.5710981300933,11.5781225898265,11.5864135061441,
11.6012871678741,11.6806489981361,11.8469704721643,11.9155152772257,11.9370845669454,
11.9506979558565,11.9634133058162,11.9804155693687,12.0190575894802,12.1584082443195,
12.329256882272,12.3481323806516,12.356791095682,12.3633655219846,12.3708426765423,
12.3840494355145,12.447782440295,12.5678857268475,12.7240782105056,12.7495763548337,
12.7641899982491,12.776595107701,12.791806092072,12.8209212843122,12.923312511244,
13.0847249400031,13.1260740585857,13.1386353954765,13.1463332793623,13.1536224450291,
13.1642608951442,13.1930339260669,13.2384968635326,13.3428181055496,13.4806114046105,
13.5052647290925,13.5196842057074,13.5322234380873,13.5477364300346,13.5783227669092,
13.6889965649581,13.836999880382,13.9085375802838,13.9225654133134,13.9303055077478,
13.9368386191739,13.9452430332507,13.9629770823624,14.0929601954303,14.2846050717009,
14.3170628758517,14.3329410859518,14.3455106299147,14.3596818144301,14.3838350793634,
14.5009185353507,14.6114904867803,14.6766888519298,14.7020986700663,14.7125218106092,
14.7196989835066,14.7274475075633,14.7402394020425,14.7889374272439,14.8932704507135,
14.9027599775658,15.0399758877475,15.0721676908585,15.0879855904972,15.1005491202281,
15.1147586884187,15.1390752337641,15.2537823369036,15.4198558817108,15.4810594717459,
15.4945173671567,15.5021291215348,15.5086158320848,15.5171670899168,15.5356813053504,
15.6137538003989,15.7923997336184,15.8725197194364,15.8953818904609,15.909276893723,
15.9219020955858,15.9382735080365,15.9734247060353,16.0211412591509,16.1631561245004,
16.2189479944778,16.2677062901924,16.2809645850439,16.2888156350195,16.2960271150681,
16.3062395469988,16.3321140375229,16.4801830654789,16.6236315158137,16.6482764948441,
16.6626938420286,16.6752328748452,16.6907477502608,16.7213449429958,16.8321021951556,
16.9793319257277,17.0514845874532,17.0655384951259,17.0732842839512,17.0758907305399),
 .UNSPECIFIED.);
#30162=B_SPLINE_CURVE_WITH_KNOTS('',3,(#169933,#169934,#169935,#169936,
#169937,#169938,#169939,#169940,#169941,#169942,#169943,#169944,#169945,
#169946,#169947,#169948,#169949,#169950,#169951,#169952,#169953,#169954,
#169955,#169956,#169957,#169958,#169959,#169960,#169961,#169962,#169963,
#169964,#169965,#169966,#169967,#169968,#169969,#169970,#169971,#169972,
#169973,#169974,#169975,#169976,#169977,#169978,#169979,#169980,#169981,
#169982,#169983,#169984,#169985,#169986,#169987,#169988,#169989,#169990,
#169991,#169992,#169993,#169994,#169995,#169996,#169997,#169998,#169999,
#170000,#170001,#170002,#170003,#170004,#170005,#170006,#170007,#170008,
#170009,#170010,#170011,#170012,#170013,#170014,#170015,#170016,#170017,
#170018,#170019,#170020,#170021,#170022,#170023,#170024,#170025,#170026,
#170027,#170028,#170029,#170030,#170031,#170032,#170033,#170034,#170035,
#170036,#170037,#170038,#170039,#170040,#170041,#170042,#170043,#170044,
#170045,#170046,#170047,#170048,#170049,#170050,#170051,#170052,#170053,
#170054,#170055,#170056,#170057,#170058,#170059,#170060,#170061,#170062,
#170063,#170064,#170065,#170066,#170067,#170068,#170069,#170070,#170071,
#170072,#170073,#170074,#170075,#170076,#170077,#170078,#170079,#170080,
#170081,#170082,#170083,#170084,#170085,#170086,#170087,#170088,#170089,
#170090,#170091,#170092,#170093,#170094,#170095,#170096,#170097,#170098,
#170099,#170100,#170101,#170102,#170103,#170104,#170105,#170106,#170107,
#170108,#170109,#170110,#170111,#170112,#170113,#170114,#170115,#170116,
#170117,#170118,#170119,#170120,#170121,#170122,#170123,#170124,#170125,
#170126,#170127,#170128,#170129,#170130,#170131,#170132,#170133,#170134,
#170135,#170136,#170137,#170138,#170139,#170140,#170141,#170142,#170143,
#170144,#170145,#170146,#170147,#170148,#170149,#170150,#170151,#170152,
#170153,#170154,#170155,#170156,#170157,#170158,#170159,#170160,#170161,
#170162,#170163,#170164,#170165,#170166,#170167,#170168,#170169,#170170,
#170171,#170172,#170173,#170174,#170175,#170176,#170177,#170178,#170179,
#170180,#170181,#170182,#170183,#170184,#170185,#170186,#170187,#170188),
 .UNSPECIFIED.,.F.,.F.,(4,2,2,2,2,2,2,2,2,2,2,2,2,2,2,2,2,2,2,2,2,2,2,2,
2,2,2,2,2,2,2,2,2,2,2,2,2,2,2,2,2,2,2,2,2,2,2,2,2,2,2,2,2,2,2,2,2,2,2,2,
2,2,2,2,2,2,2,2,2,2,2,2,2,2,2,2,2,2,2,2,2,2,2,2,2,2,2,2,2,2,2,2,2,2,2,2,
2,2,2,2,2,2,2,2,2,2,2,2,2,2,2,2,2,2,2,2,2,2,2,2,2,2,2,2,2,2,2,4),(16.6851291404356,
16.6891848353774,16.6976541060233,16.7157297009885,16.7900676343414,16.9900542918037,
17.056157653,17.0775654245892,17.0911462205749,17.1038750923964,17.1209649827791,
17.1602148900421,17.2155519530881,17.3153895467823,17.4358812228311,17.4568460367297,
17.4661446911833,17.4732473216251,17.4814735682872,17.496462703809,17.5883925759467,
17.6345856849508,17.7924757253217,17.8245046154945,17.8402912599175,17.8528520126454,
17.8670819451238,17.8914926423306,18.0081858277598,18.1534869576225,18.2317990716855,
18.2448506723089,18.253060198381,18.2595823246727,18.2674796199095,18.2826637129226,
18.4205221558987,18.6077739697828,18.6405916646402,18.6565385726394,18.6691147560217,
18.6832432446556,18.7071991515676,18.8196430282876,18.972893324294,19.0202446257863,
19.0333793978062,19.0412032996922,19.0484266834284,19.0587079185179,19.0850340229593,
19.2335282765803,19.3759126711263,19.4005697015907,19.4149897167684,19.427528439784,
19.4430395413321,19.473617927943,19.5842368592339,19.732684080907,19.8038603693889,
19.81787226502,19.8256086440089,19.8321418802572,19.8405506491336,19.8583084044284,
19.9653030926738,20.1544009353061,20.2038026128688,20.2230463201509,20.2348594163614,
20.2476692402974,20.2652494181708,20.3074917502285,20.3687021764774,20.4668259401795,
20.5787090711882,20.5997997406627,20.6091203243637,20.6162252571657,20.6244369547715,
20.6393588895596,20.7289719790186,20.7850143526512,20.9356988003089,20.9675777789258,
20.9833351182327,20.9958927941399,21.0101408919735,21.0346376318975,21.153229725294,
21.3107695392435,21.3758874242494,21.3895594649733,21.3972194484067,21.403761318284,
21.4122763457042,21.4305972497696,21.5070129869486,21.6834220473702,21.7670890648905,
21.7902759958697,21.8042410602935,21.8168489584327,21.8330837738811,21.8674914735401,
21.9138749148698,22.0321362705211,22.1501942121107,22.1712311239756,22.1805422020978,
22.1876459674459,22.1958635653018,22.2108133481679,22.3013794266412,22.3608920329085,
22.506580892971,22.5387878367801,22.5546082666932,22.5671715977257,22.5813785937464,
22.6056848362693,22.7201936103805,22.8619754129453,22.9442317078442,22.9594782998301,
22.9657894059735,22.970999517308),.UNSPECIFIED.);
#30163=B_SPLINE_CURVE_WITH_KNOTS('',3,(#170193,#170194,#170195,#170196,
#170197,#170198,#170199,#170200,#170201,#170202,#170203,#170204,#170205,
#170206,#170207,#170208,#170209,#170210,#170211,#170212,#170213,#170214,
#170215,#170216,#170217,#170218,#170219,#170220,#170221,#170222,#170223,
#170224,#170225,#170226,#170227,#170228,#170229,#170230,#170231,#170232,
#170233,#170234,#170235,#170236,#170237,#170238,#170239,#170240,#170241,
#170242,#170243,#170244,#170245,#170246,#170247,#170248,#170249,#170250,
#170251,#170252,#170253,#170254,#170255,#170256,#170257,#170258,#170259,
#170260,#170261,#170262,#170263,#170264,#170265,#170266,#170267,#170268,
#170269,#170270,#170271,#170272,#170273,#170274,#170275,#170276,#170277,
#170278,#170279,#170280,#170281,#170282,#170283,#170284,#170285,#170286,
#170287,#170288,#170289,#170290,#170291,#170292,#170293,#170294,#170295,
#170296,#170297,#170298,#170299,#170300,#170301,#170302,#170303,#170304,
#170305,#170306,#170307,#170308,#170309,#170310,#170311,#170312,#170313,
#170314,#170315,#170316,#170317,#170318,#170319,#170320,#170321,#170322,
#170323,#170324,#170325,#170326,#170327,#170328,#170329,#170330,#170331,
#170332,#170333,#170334,#170335,#170336,#170337,#170338,#170339,#170340,
#170341,#170342,#170343,#170344,#170345,#170346,#170347,#170348,#170349,
#170350,#170351,#170352,#170353,#170354,#170355,#170356,#170357,#170358,
#170359,#170360,#170361,#170362,#170363,#170364,#170365,#170366,#170367,
#170368,#170369,#170370,#170371,#170372,#170373,#170374,#170375,#170376,
#170377,#170378,#170379,#170380,#170381,#170382,#170383,#170384,#170385,
#170386,#170387,#170388,#170389,#170390,#170391,#170392,#170393,#170394,
#170395,#170396,#170397,#170398,#170399,#170400,#170401,#170402,#170403,
#170404,#170405,#170406,#170407,#170408,#170409,#170410,#170411,#170412,
#170413,#170414,#170415,#170416,#170417,#170418,#170419,#170420,#170421,
#170422,#170423,#170424,#170425,#170426,#170427,#170428,#170429,#170430,
#170431,#170432,#170433,#170434,#170435,#170436,#170437,#170438,#170439,
#170440,#170441,#170442,#170443,#170444,#170445,#170446,#170447,#170448,
#170449,#170450,#170451,#170452,#170453,#170454),.UNSPECIFIED.,.F.,.F.,
(4,2,2,2,2,2,2,2,2,2,2,2,2,2,2,2,2,2,2,2,2,2,2,2,2,2,2,2,2,2,2,2,2,2,2,
2,2,2,2,2,2,2,2,2,2,2,2,2,2,2,2,2,2,2,2,2,2,2,2,2,2,2,2,2,2,2,2,2,2,2,2,
2,2,2,2,2,2,2,2,2,2,2,2,2,2,2,2,2,2,2,2,2,2,2,2,2,2,2,2,2,2,2,2,2,2,2,2,
2,2,2,2,2,2,2,2,2,2,2,2,2,2,2,2,2,2,2,2,2,2,2,4),(4.50400203993545,4.50783078879762,
4.51617336957014,4.52967085577925,4.645661358127,4.66484391224903,4.77745340529264,
4.83969458000058,4.88296902407783,4.90073353901219,4.91357602962783,4.92535018303914,
4.94131179144098,4.98143819914888,5.17618136231952,5.23614973539588,5.27093510019915,
5.2823494982435,5.2897967772644,5.29639604111083,5.30547187381965,5.32850840604712,
5.47934159114501,5.60233834905262,5.64028225564697,5.6571486018372,5.66984239122988,
5.68351052058056,5.70532610630803,5.77509730238163,5.94562219603879,6.05030002355518,
6.06495719017102,6.07274448292501,6.07927301024529,6.08761480270507,6.10110926187093,
6.19816676464921,6.32365119136852,6.44056041220587,6.46498059683818,6.47921227426936,
6.4917722981847,6.50755500072208,6.5395651185537,6.69182664965174,6.74620444512316,
6.83569768772053,6.85061606014671,6.85882703442838,6.86593216358815,6.87525405511605,
6.89635192810502,7.01005492593952,7.13548735728464,7.18032138194295,7.21385502669898,
7.22992740954191,7.24251670474267,7.25657182177177,7.28017407340108,7.36995511210761,
7.54036075213862,7.61599982243425,7.63422947861459,7.6427274651935,7.64926788325522,
7.65693982831498,7.67066474042213,7.73679428780625,7.89388882437003,8.01188767967951,
8.03635792186589,8.05060041377246,8.06315900594515,8.07892529048758,8.11085007986573,
8.26434403883236,8.31769085454703,8.4071230587894,8.42203966058159,8.43025027784888,
8.43735551002728,8.44667806092502,8.46777955236474,8.58210897290625,8.68624202648577,
8.77090635592798,8.79322136798927,8.80699539494234,8.81965430041978,8.83599510682316,
8.86337577700412,9.07391539198163,9.19282037175703,9.20771235395789,9.21554900316822,
9.22207434434218,9.23035554118649,9.2436461332262,9.33104565818227,9.33430254033697,
9.46662507022681,9.58349671221414,9.6079159795697,9.62214784846763,9.63470847622948,
9.65049251760594,9.6825074199498,9.83408467373633,9.8891052812609,9.97864442223905,
9.99356469161716,10.0017762878928,10.0088816737712,10.0182035439249,10.03929991615,
10.152482068856,10.2783117601934,10.3232211169318,10.3567978592978,10.3728787422926,
10.3854694458644,10.3995207130716,10.4231033872177,10.5125759737873,10.6832927165416,
10.7589755972446,10.7772108283276,10.7857100808537,10.7898186351041),
 .UNSPECIFIED.);
#30164=B_SPLINE_CURVE_WITH_KNOTS('',3,(#170455,#170456,#170457,#170458,
#170459,#170460,#170461,#170462,#170463,#170464,#170465,#170466,#170467,
#170468,#170469,#170470,#170471,#170472,#170473,#170474,#170475,#170476,
#170477,#170478,#170479,#170480,#170481,#170482,#170483,#170484,#170485,
#170486,#170487,#170488,#170489,#170490,#170491,#170492,#170493,#170494,
#170495,#170496,#170497,#170498,#170499,#170500,#170501,#170502,#170503,
#170504,#170505,#170506,#170507,#170508,#170509,#170510,#170511,#170512,
#170513,#170514,#170515,#170516,#170517,#170518,#170519,#170520,#170521,
#170522,#170523,#170524,#170525,#170526,#170527,#170528,#170529,#170530,
#170531,#170532,#170533,#170534,#170535,#170536,#170537,#170538,#170539,
#170540,#170541,#170542,#170543,#170544,#170545,#170546,#170547,#170548,
#170549,#170550,#170551,#170552,#170553,#170554,#170555,#170556,#170557,
#170558,#170559,#170560,#170561,#170562,#170563,#170564,#170565,#170566,
#170567,#170568,#170569,#170570,#170571,#170572,#170573,#170574,#170575,
#170576,#170577,#170578,#170579,#170580,#170581,#170582,#170583,#170584,
#170585,#170586,#170587,#170588,#170589,#170590,#170591,#170592,#170593,
#170594,#170595,#170596,#170597,#170598,#170599,#170600,#170601,#170602,
#170603,#170604,#170605,#170606,#170607,#170608,#170609,#170610,#170611,
#170612,#170613,#170614,#170615,#170616,#170617,#170618,#170619,#170620,
#170621,#170622,#170623,#170624,#170625,#170626,#170627,#170628,#170629,
#170630,#170631,#170632,#170633,#170634,#170635,#170636,#170637,#170638,
#170639,#170640,#170641,#170642,#170643,#170644,#170645,#170646,#170647,
#170648,#170649,#170650,#170651,#170652,#170653,#170654,#170655,#170656,
#170657,#170658,#170659,#170660,#170661,#170662,#170663,#170664,#170665,
#170666,#170667,#170668,#170669,#170670,#170671,#170672,#170673,#170674,
#170675,#170676,#170677,#170678,#170679,#170680,#170681,#170682,#170683,
#170684,#170685,#170686,#170687,#170688,#170689,#170690,#170691,#170692,
#170693,#170694,#170695,#170696,#170697,#170698,#170699,#170700,#170701,
#170702,#170703,#170704,#170705,#170706,#170707,#170708,#170709,#170710,
#170711,#170712,#170713,#170714),.UNSPECIFIED.,.F.,.F.,(4,2,2,2,2,2,2,2,
2,2,2,2,2,2,2,2,2,2,2,2,2,2,2,2,2,2,2,2,2,2,2,2,2,2,2,2,2,2,2,2,2,2,2,2,
2,2,2,2,2,2,2,2,2,2,2,2,2,2,2,2,2,2,2,2,2,2,2,2,2,2,2,2,2,2,2,2,2,2,2,2,
2,2,2,2,2,2,2,2,2,2,2,2,2,2,2,2,2,2,2,2,2,2,2,2,2,2,2,2,2,2,2,2,2,2,2,2,
2,2,2,2,2,2,2,2,2,2,2,2,2,4),(9.99999999314102E-7,0.00521187694995086,0.0115243780586715,
0.0267764289715423,0.109101741016729,0.250843391215176,0.365307860432174,
0.389610755024793,0.403816410484198,0.416378925485257,0.432198823705125,
0.464406488465193,0.609941514961661,0.669861994045137,0.760150764001163,
0.775091551278359,0.783306881601369,0.790410465265545,0.799723570901651,
0.820774205379463,0.935181085531112,1.05604958818247,1.1029796647841,1.13769227386817,
1.15398250233226,1.16659640651649,1.18053067832399,1.20357838282418,1.2855080131829,
1.46234388816903,1.54006507023998,1.55853763968509,1.56708060882173,1.57356588606699,
1.5811817213839,1.59465978182557,1.65623642278592,1.82186528698761,1.93658062216615,
1.9608956522277,1.97510393887553,1.98766609565137,2.00348194636585,2.03566844989071,
2.17227750047059,2.31077637813875,2.33978744715114,2.35045844852665,2.35775323319897,
2.36543933592666,2.37794986739516,2.41882190395879,2.45513570201323,2.5920602532835,
2.69320597781548,2.71659414321804,2.73059928129607,2.74319738742964,2.75935406837429,
2.79328673569503,2.96175212978104,3.01795359068554,3.11761975813416,3.13216655731193,
3.13993029434479,3.14646027338732,3.15483108021548,3.1684242830127,3.27159172098514,
3.39073081656475,3.50766257455933,3.53208242695173,3.54631338335822,3.55887245508663,
3.57465353985711,3.60665887413866,3.76464241422557,3.86054773413309,3.89180580933521,
3.91371783832301,3.92328279764401,3.93039703745322,3.938558985752,3.95286180535382,
4.01904292745739,4.16220513375268,4.23014815079747,4.27565233493159,4.29373623108368,
4.3066354453395,4.3198978121195,4.33980939688194,4.39373370619213,4.57844285303776,
4.68387023636065,4.70156430183261,4.70996049778992,4.71649232258913,4.72423694408111,
4.73828744444111,4.81038147503658,4.95767073515514,5.06841665922256,5.09901083576851,
5.11452427933853,5.12706219853634,5.14147831364645,5.16612130980634,5.30330060422524,
5.40494466480211,5.47538811634404,5.48956928721446,5.49762129629522,5.50476222644121,
5.51452917883596,5.53762667411542,5.5711815501957,5.68048559906794,5.82074929137883,
5.85296115228007,5.86878205667884,5.88134489166568,5.8955503991264,5.91985176371621,
6.03427857298967,6.20680983655509,6.26247544082628,6.27557884477625,6.28310963195874,
6.28519602509786),.UNSPECIFIED.);
#30165=B_SPLINE_CURVE_WITH_KNOTS('',3,(#170720,#170721,#170722,#170723,
#170724,#170725,#170726,#170727,#170728,#170729,#170730,#170731,#170732,
#170733,#170734,#170735,#170736,#170737,#170738,#170739,#170740,#170741,
#170742,#170743,#170744,#170745,#170746,#170747,#170748,#170749,#170750,
#170751,#170752,#170753,#170754,#170755,#170756,#170757,#170758,#170759,
#170760,#170761,#170762,#170763,#170764,#170765,#170766,#170767,#170768,
#170769,#170770,#170771,#170772,#170773,#170774,#170775,#170776,#170777,
#170778,#170779,#170780,#170781,#170782,#170783,#170784,#170785,#170786,
#170787,#170788,#170789,#170790,#170791,#170792,#170793,#170794,#170795,
#170796,#170797,#170798,#170799,#170800,#170801,#170802,#170803,#170804,
#170805,#170806,#170807,#170808,#170809,#170810,#170811,#170812,#170813,
#170814,#170815,#170816,#170817,#170818,#170819,#170820,#170821,#170822,
#170823,#170824,#170825,#170826,#170827,#170828,#170829,#170830,#170831,
#170832,#170833,#170834,#170835,#170836,#170837,#170838,#170839,#170840,
#170841,#170842,#170843,#170844,#170845,#170846,#170847,#170848,#170849,
#170850,#170851,#170852,#170853,#170854,#170855,#170856,#170857,#170858,
#170859,#170860,#170861,#170862,#170863,#170864,#170865,#170866,#170867,
#170868,#170869,#170870,#170871,#170872,#170873),.UNSPECIFIED.,.F.,.F.,
(4,2,2,2,2,2,2,2,2,2,2,2,2,2,2,2,2,2,2,2,2,2,2,2,2,2,2,2,2,2,2,2,2,2,2,
2,2,2,2,2,2,2,2,2,2,2,2,2,2,2,2,2,2,2,2,2,2,2,2,2,2,2,2,2,2,2,2,2,2,2,2,
2,2,2,2,2,4),(6.44324130749359,6.45009989945945,6.46952174069895,6.51371948633358,
6.58264731915039,6.78450170032278,6.83051898716609,6.86078018873499,6.8909498277508,
6.93660137164695,6.99185200670286,7.12821205945386,7.21188928495002,7.23668756456504,
7.25341893997957,7.27328405056241,7.31537886060976,7.44333783601869,7.57348204528162,
7.61342556797451,7.64267743466213,7.67449810850209,7.72894478014473,7.8378171049123,
7.98611714158222,8.02850948778931,8.04763977263604,8.06135457370724,8.08107703485136,
8.12721051481373,8.20091774318204,8.4031357171896,8.44549529415767,8.47482898268042,
8.50573768590399,8.55550330556311,8.58880282586661,8.69495127610468,8.81377919504479,
8.84302264517212,8.86049944932598,8.8787284981319,8.91179996796876,8.95645174496428,
9.09585729472496,9.18897227904853,9.22661307320286,9.25566055395916,9.28823312004371,
9.34679551122857,9.42440073750344,9.52759101876076,9.62646011006886,9.65106087315707,
9.66667331032369,9.68373228491427,9.71477075757884,9.75606528653478,9.87174019916766,
10.0039500133767,10.0508708182577,10.0812947528742,10.1113136944997,10.1561082457514,
10.2825312016657,10.4279124024802,10.4552930886508,10.4707408756368,10.4888420793433,
10.5212606070798,10.6089376933129,10.7915881430545,10.832893936256,10.8623412354449,
10.8892975116174,10.9193612832434,10.9565256385629),.UNSPECIFIED.);
#30166=B_SPLINE_CURVE_WITH_KNOTS('',3,(#170876,#170877,#170878,#170879,
#170880,#170881,#170882,#170883,#170884,#170885,#170886,#170887,#170888,
#170889,#170890,#170891,#170892,#170893,#170894,#170895,#170896,#170897,
#170898,#170899,#170900,#170901,#170902,#170903,#170904,#170905,#170906,
#170907,#170908,#170909,#170910,#170911,#170912,#170913,#170914,#170915,
#170916,#170917,#170918,#170919,#170920,#170921,#170922,#170923,#170924,
#170925,#170926,#170927,#170928,#170929,#170930,#170931,#170932,#170933,
#170934,#170935,#170936,#170937,#170938,#170939,#170940,#170941,#170942,
#170943,#170944,#170945,#170946,#170947,#170948,#170949,#170950,#170951,
#170952,#170953,#170954,#170955,#170956,#170957,#170958,#170959,#170960,
#170961,#170962,#170963,#170964,#170965,#170966,#170967,#170968,#170969,
#170970,#170971,#170972,#170973,#170974,#170975,#170976,#170977,#170978,
#170979,#170980,#170981,#170982,#170983,#170984,#170985,#170986,#170987,
#170988,#170989,#170990,#170991,#170992,#170993,#170994,#170995,#170996,
#170997,#170998,#170999,#171000,#171001,#171002,#171003,#171004,#171005,
#171006,#171007,#171008,#171009,#171010,#171011,#171012,#171013),
 .UNSPECIFIED.,.F.,.F.,(4,2,2,2,2,2,2,2,2,2,2,2,2,2,2,2,2,2,2,2,2,2,2,2,
2,2,2,2,2,2,2,2,2,2,2,2,2,2,2,2,2,2,2,2,2,2,2,2,2,2,2,2,2,2,2,2,2,2,2,2,
2,2,2,2,2,2,2,2,4),(9.99999999894808E-7,0.0130525840280033,0.0250471003602153,
0.0423664309872074,0.0710432677210413,0.192633457570409,0.34076010321594,
0.384889710270354,0.414795624627185,0.445362477788186,0.493057746807944,
0.643693335011998,0.744750679568014,0.800416149366004,0.821461677838465,
0.83672923651018,0.855615531649739,0.896541970431237,1.04634851009296,1.16347119594112,
1.21379636485514,1.24485044205548,1.27410460991681,1.30938174994106,1.41967247131201,
1.54331898859052,1.58575137558574,1.61764879222985,1.63564784065184,1.65115457186324,
1.67889521792463,1.84512752293783,1.92455612337491,1.95224397680292,1.99600296939021,
2.02584569639317,2.0528694479377,2.09755771731233,2.30039509475668,2.37043808010399,
2.41509540238138,2.43458941151924,2.44981412633709,2.4697518945745,2.51413855687589,
2.76157189397774,2.81903983964568,2.85141405184491,2.88050549044656,2.91852224989909,
3.01334438430698,3.15056968303968,3.19493301374123,3.22785352038779,3.24605297969566,
3.26355178142859,3.29291102618676,3.45045501550115,3.53302930270614,3.59299173898179,
3.62572446262663,3.65474162204956,3.69206239054126,3.78016692247768,3.80006553634604,
3.95104662110329,4.01888554269364,4.04128254128481,4.05239777510564),
 .UNSPECIFIED.);
#30167=B_SPLINE_CURVE_WITH_KNOTS('',3,(#171018,#171019,#171020,#171021,
#171022,#171023,#171024,#171025,#171026,#171027,#171028,#171029,#171030,
#171031,#171032,#171033,#171034,#171035,#171036,#171037,#171038,#171039,
#171040,#171041,#171042,#171043,#171044,#171045,#171046,#171047,#171048,
#171049,#171050,#171051,#171052,#171053,#171054,#171055,#171056,#171057,
#171058,#171059,#171060,#171061,#171062,#171063,#171064,#171065,#171066,
#171067,#171068,#171069,#171070,#171071,#171072,#171073,#171074,#171075,
#171076,#171077,#171078,#171079,#171080,#171081,#171082,#171083,#171084,
#171085,#171086,#171087,#171088,#171089,#171090,#171091,#171092,#171093,
#171094,#171095,#171096,#171097,#171098,#171099,#171100,#171101,#171102,
#171103,#171104,#171105,#171106,#171107,#171108,#171109,#171110,#171111,
#171112,#171113,#171114,#171115,#171116,#171117,#171118,#171119,#171120,
#171121,#171122,#171123,#171124,#171125,#171126,#171127,#171128,#171129,
#171130,#171131,#171132,#171133,#171134,#171135,#171136,#171137,#171138,
#171139,#171140,#171141,#171142,#171143,#171144,#171145,#171146,#171147,
#171148,#171149,#171150,#171151,#171152,#171153,#171154,#171155,#171156,
#171157,#171158,#171159,#171160,#171161,#171162,#171163,#171164,#171165,
#171166,#171167,#171168,#171169,#171170,#171171,#171172,#171173,#171174,
#171175,#171176,#171177,#171178,#171179,#171180,#171181,#171182,#171183,
#171184,#171185,#171186,#171187,#171188,#171189,#171190,#171191,#171192,
#171193,#171194,#171195,#171196,#171197,#171198,#171199,#171200,#171201,
#171202,#171203,#171204,#171205,#171206,#171207,#171208,#171209,#171210,
#171211,#171212,#171213,#171214,#171215,#171216,#171217,#171218,#171219,
#171220,#171221,#171222,#171223,#171224,#171225,#171226,#171227,#171228,
#171229,#171230,#171231),.UNSPECIFIED.,.F.,.F.,(4,2,2,2,2,2,2,2,2,2,2,2,
2,2,2,2,2,2,2,2,2,2,2,2,2,2,2,2,2,2,2,2,2,2,2,2,2,2,2,2,2,2,2,2,2,2,2,2,
2,2,2,2,2,2,2,2,2,2,2,2,2,2,2,2,2,2,2,2,2,2,2,2,2,2,2,2,2,2,2,2,2,2,2,2,
2,2,2,2,2,2,2,2,2,2,2,2,2,2,2,2,2,2,2,2,2,2,4),(1.00000000121357E-6,0.0132985295892812,
0.0305000676118254,0.0775692256728027,0.240329177579876,0.317940181801879,
0.376505573386614,0.409079332936633,0.438127542992531,0.475768834166774,
0.568885314201447,0.708281105687855,0.752931035956093,0.786002062687976,
0.804231354419126,0.821708779458675,0.850954001770212,0.969779811205238,
1.07594614121046,1.10924966352201,1.15901958569497,1.18992963621842,1.219263685806,
1.26162217598733,1.46383810972887,1.53753889267239,1.56989739314913,1.5958354235727,
1.61185803830954,1.62857798714354,1.65793469577569,1.82894800314684,1.93570299071125,
1.99023923088798,2.02207672419668,2.05132329240569,2.09122617743967,2.21166682806551,
2.32613966015929,2.36711268145982,2.39822254302645,2.41606553077769,2.4316703550286,
2.45999901482697,2.59492100741736,2.7349024933847,2.77744414123908,2.80708613984153,
2.83804419215404,2.88785350445539,3.08662018715367,3.15275155788358,3.19577430269898,
3.21500758194648,3.2302454924629,3.25047873061391,3.29661415563424,3.5422014322881,
3.59928708186249,3.631591986514,3.66070082358628,3.69885666652083,3.79747243719323,
3.93139357911008,3.97531070010754,4.00799669647732,4.02615048001158,4.04368532504206,
4.07323084518633,4.17822468056961,4.29310811558839,4.32796978894856,4.37932841061905,
4.41052714031691,4.43970790316327,4.48109097958902,4.62179856396732,4.74007571658718,
4.78181922664451,4.81310234910538,4.83021039824333,4.84579753539331,4.87025488503379,
4.96231649282271,5.11014528919533,5.16899375117321,5.21725337041476,5.24792388189464,
5.27740809051997,5.32078858951301,5.47828530244555,5.59181491813238,5.62120983726276,
5.63871586987435,5.65690714073263,5.68978405857206,5.73406431524519,5.87065192694529,
5.96620333617338,6.00425804766391,6.03335479769658,6.06571117634368,6.12307795036316,
6.3700061840772,6.41485391950567,6.43487189935052,6.44324130749359),
 .UNSPECIFIED.);
#30168=B_SPLINE_CURVE_WITH_KNOTS('',3,(#171232,#171233,#171234,#171235,
#171236,#171237,#171238,#171239,#171240,#171241,#171242,#171243,#171244,
#171245,#171246,#171247,#171248,#171249,#171250,#171251,#171252,#171253,
#171254,#171255,#171256,#171257,#171258,#171259,#171260,#171261,#171262,
#171263,#171264,#171265,#171266,#171267,#171268,#171269,#171270,#171271,
#171272,#171273,#171274,#171275,#171276,#171277,#171278,#171279,#171280,
#171281,#171282,#171283,#171284,#171285,#171286,#171287,#171288,#171289,
#171290,#171291,#171292,#171293,#171294,#171295,#171296,#171297,#171298,
#171299,#171300,#171301,#171302,#171303,#171304,#171305,#171306,#171307,
#171308,#171309,#171310,#171311,#171312,#171313,#171314,#171315,#171316,
#171317,#171318,#171319,#171320,#171321,#171322,#171323,#171324,#171325,
#171326,#171327,#171328,#171329,#171330,#171331,#171332,#171333,#171334,
#171335,#171336,#171337,#171338,#171339,#171340,#171341,#171342,#171343,
#171344,#171345,#171346,#171347,#171348,#171349,#171350,#171351,#171352,
#171353,#171354,#171355,#171356,#171357,#171358,#171359,#171360,#171361,
#171362,#171363,#171364,#171365,#171366,#171367,#171368,#171369,#171370,
#171371,#171372,#171373,#171374,#171375,#171376,#171377,#171378,#171379,
#171380,#171381,#171382,#171383,#171384,#171385,#171386,#171387,#171388,
#171389,#171390,#171391,#171392,#171393,#171394,#171395,#171396,#171397,
#171398,#171399,#171400,#171401,#171402,#171403,#171404,#171405,#171406,
#171407,#171408,#171409,#171410,#171411,#171412,#171413,#171414,#171415,
#171416,#171417,#171418,#171419,#171420,#171421,#171422,#171423,#171424,
#171425,#171426,#171427,#171428,#171429,#171430,#171431,#171432,#171433,
#171434,#171435,#171436,#171437,#171438,#171439,#171440,#171441,#171442,
#171443),.UNSPECIFIED.,.F.,.F.,(4,2,2,2,2,2,2,2,2,2,2,2,2,2,2,2,2,2,2,2,
2,2,2,2,2,2,2,2,2,2,2,2,2,2,2,2,2,2,2,2,2,2,2,2,2,2,2,2,2,2,2,2,2,2,2,2,
2,2,2,2,2,2,2,2,2,2,2,2,2,2,2,2,2,2,2,2,2,2,2,2,2,2,2,2,2,2,2,2,2,2,2,2,
2,2,2,2,2,2,2,2,2,2,2,2,2,4),(4.05239777510564,4.05669631670699,4.07474633851778,
4.11093866250766,4.26584683425855,4.37831229643335,4.43228498905449,4.46401679397778,
4.49329763725746,4.53346068528141,4.72136923542866,4.7887627863517,4.83240337843136,
4.85252224128053,4.86919630816024,4.89353311098095,4.97224055757222,5.11298425432336,
5.16895743666786,5.21503078211746,5.24527378241042,5.27545830392223,5.32105479858966,
5.49217779118691,5.62009465225304,5.64716561778583,5.66341526327337,5.67985805846434,
5.70786619889621,5.85628026117951,5.99387218746446,6.04520914801298,6.07645108367382,
6.10593901988633,6.14750875484144,6.32568276461725,6.39712219394073,6.44239362779474,
6.46277280506414,6.47940028866236,6.50330774927925,6.57565196846024,6.68032886790893,
6.77136600383769,6.82166771010724,6.85267401853342,6.88195296346427,6.92396857806303,
7.12842560393073,7.20118416663039,7.23329968825024,7.25909217247564,7.27508598783313,
7.29184467424206,7.32139292930927,7.45773062558618,7.5685713966976,7.61991187333395,
7.66362259442563,7.69347684144813,7.72050184056222,7.76526263232103,7.88528335382165,
7.99189141685828,8.03150313511859,8.06186693922171,8.07956174812618,8.0952715064761,
8.12421574543822,8.27870822290594,8.39568712496389,8.4392540033007,8.46906416428899,
8.49611927663557,8.54100630939177,8.72358332366881,8.80651700789685,8.84114464854317,
8.868422612394,8.88471481574657,8.901112591712,8.92890207034066,9.0830228697413,
9.23064667717671,9.27435570711325,9.30420923578343,9.33123385761761,9.37599469200737,
9.4967220998385,9.62391582345146,9.66552184744801,9.68530456554423,9.70205609939084,
9.72701089006405,9.81416045760381,9.94776797301862,10.0025472904076,10.047920929013,
10.0780412027337,10.1083527593252,10.1546524015123,10.3132481468407,10.4106500529436,
10.4651792677483,10.4860798856037,10.4952223301995),.UNSPECIFIED.);
#30169=B_SPLINE_CURVE_WITH_KNOTS('',3,(#171448,#171449,#171450,#171451,
#171452,#171453,#171454,#171455,#171456,#171457,#171458,#171459,#171460,
#171461,#171462,#171463,#171464,#171465,#171466,#171467,#171468,#171469,
#171470,#171471,#171472,#171473,#171474,#171475,#171476,#171477,#171478,
#171479,#171480,#171481,#171482,#171483,#171484,#171485,#171486,#171487,
#171488,#171489,#171490,#171491,#171492,#171493,#171494,#171495,#171496,
#171497,#171498,#171499,#171500,#171501,#171502,#171503,#171504,#171505,
#171506,#171507,#171508,#171509,#171510,#171511,#171512,#171513,#171514,
#171515,#171516,#171517,#171518,#171519,#171520,#171521,#171522,#171523,
#171524,#171525,#171526,#171527,#171528,#171529,#171530,#171531,#171532,
#171533,#171534,#171535,#171536,#171537,#171538,#171539,#171540,#171541,
#171542,#171543,#171544,#171545,#171546,#171547,#171548,#171549,#171550,
#171551,#171552,#171553,#171554,#171555,#171556,#171557,#171558,#171559,
#171560,#171561,#171562,#171563,#171564,#171565,#171566,#171567,#171568,
#171569,#171570,#171571,#171572,#171573,#171574,#171575,#171576,#171577,
#171578,#171579,#171580,#171581,#171582,#171583,#171584,#171585,#171586,
#171587,#171588,#171589,#171590,#171591,#171592,#171593,#171594,#171595,
#171596,#171597,#171598,#171599,#171600,#171601,#171602,#171603,#171604,
#171605,#171606,#171607,#171608,#171609,#171610,#171611,#171612,#171613,
#171614,#171615,#171616,#171617,#171618,#171619,#171620,#171621,#171622,
#171623,#171624,#171625,#171626,#171627,#171628,#171629,#171630,#171631,
#171632,#171633,#171634,#171635,#171636,#171637,#171638,#171639,#171640,
#171641,#171642,#171643,#171644,#171645,#171646,#171647,#171648,#171649,
#171650,#171651,#171652,#171653,#171654,#171655,#171656,#171657,#171658,
#171659,#171660,#171661,#171662,#171663,#171664,#171665,#171666,#171667,
#171668,#171669,#171670,#171671,#171672,#171673,#171674,#171675),
 .UNSPECIFIED.,.F.,.F.,(4,2,2,2,2,2,2,2,2,2,2,2,2,2,2,2,2,2,2,2,2,2,2,2,
2,2,2,2,2,2,2,2,2,2,2,2,2,2,2,2,2,2,2,2,2,2,2,2,2,2,2,2,2,2,2,2,2,2,2,2,
2,2,2,2,2,2,2,2,2,2,2,2,2,2,2,2,2,2,2,2,2,2,2,2,2,2,2,2,2,2,2,2,2,2,2,2,
2,2,2,2,2,2,2,2,2,2,2,2,2,2,2,2,2,4),(19.7725472889628,19.7745630841054,
19.7916200476201,19.8226511599206,19.8639329635955,19.9795410716252,20.1118258377354,
20.1587444018553,20.1891668403298,20.2191842746196,20.2639765147832,20.3903925148979,
20.5357674478223,20.5631467123286,20.5785937213992,20.5966940425543,20.6291110480684,
20.6725208085203,20.8028168600046,20.814012064891,20.9073302683404,20.94498528383,
20.9740327647176,21.0065941451291,21.0651024941645,21.1426041463908,21.2457967031782,
21.3448266654611,21.369429300689,21.3850413381192,21.4020980314289,21.4331286521571,
21.4744098018785,21.5900160785627,21.7222987490248,21.7692165698878,21.7996385264272,
21.829655485198,21.8744470157887,22.0008610132948,22.1462336432735,22.1736124740533,
22.1890592384218,22.207159272843,22.2395757648267,22.2829848376073,22.4132788250151,
22.4244738525792,22.5177905777285,22.5554449967101,22.584492017446,22.6170528820414,
22.6755603042281,22.7530607287287,22.8562516508049,22.9552800443077,22.979882289796,
22.9954940799104,23.0125505030194,23.0435806321822,23.0848611279569,23.2004655732939,
23.3327461482097,23.3796632258316,23.4100847004467,23.4401011837089,23.4848920047424,
23.6113039996843,23.7566743267646,23.7840527238278,23.7994992434982,23.8175989911895,
23.8500149696512,23.8934233547716,24.0237152781391,24.0349101283707,24.128225375247,
24.1658791977297,24.1949257583198,24.2274861071055,24.2859926024538,24.3634917992416,
24.466681086628,24.5657079113769,24.590309767131,24.6059213099325,24.6229774628435,
24.6540071004445,24.6952869422768,24.8108895562715,24.9431680356764,24.9900843700649,
25.0205053627607,25.0505213705191,25.0953114820017,25.2217214743951,25.3670894986047,
25.394467461955,25.409913736931,25.4280131978972,25.4604286628444,25.5038363603156,
25.6341262196795,25.6453208925587,25.7386346611949,25.7762878871884,25.8053339876401,
25.8378938206237,25.8963993891451,25.9738973582341,26.1364067009837,26.1837594997724,
26.2010247288919,26.214356777113),.UNSPECIFIED.);
#30170=B_SPLINE_CURVE_WITH_KNOTS('',3,(#171676,#171677,#171678,#171679,
#171680,#171681,#171682,#171683,#171684,#171685,#171686,#171687,#171688,
#171689,#171690,#171691,#171692,#171693,#171694,#171695,#171696,#171697,
#171698,#171699,#171700,#171701,#171702,#171703,#171704,#171705,#171706,
#171707,#171708,#171709,#171710,#171711,#171712,#171713,#171714,#171715,
#171716,#171717,#171718,#171719,#171720,#171721,#171722,#171723,#171724,
#171725,#171726,#171727,#171728,#171729,#171730,#171731,#171732,#171733,
#171734,#171735,#171736,#171737,#171738,#171739,#171740,#171741,#171742,
#171743,#171744,#171745,#171746,#171747,#171748,#171749,#171750,#171751,
#171752,#171753,#171754,#171755,#171756,#171757,#171758,#171759,#171760,
#171761,#171762,#171763,#171764,#171765,#171766,#171767,#171768,#171769,
#171770,#171771,#171772,#171773,#171774,#171775,#171776,#171777,#171778,
#171779,#171780,#171781,#171782,#171783,#171784,#171785,#171786,#171787,
#171788,#171789,#171790,#171791,#171792,#171793,#171794,#171795,#171796,
#171797,#171798,#171799,#171800,#171801,#171802,#171803,#171804,#171805,
#171806,#171807,#171808,#171809,#171810,#171811,#171812,#171813,#171814,
#171815,#171816,#171817,#171818,#171819,#171820,#171821,#171822,#171823,
#171824,#171825,#171826,#171827,#171828,#171829,#171830,#171831,#171832,
#171833,#171834,#171835,#171836,#171837,#171838,#171839,#171840,#171841,
#171842,#171843,#171844,#171845,#171846,#171847,#171848,#171849,#171850,
#171851,#171852,#171853,#171854,#171855,#171856,#171857,#171858,#171859,
#171860,#171861,#171862,#171863,#171864,#171865,#171866,#171867,#171868,
#171869,#171870,#171871,#171872,#171873,#171874,#171875,#171876,#171877,
#171878,#171879,#171880,#171881,#171882,#171883,#171884,#171885,#171886,
#171887),.UNSPECIFIED.,.F.,.F.,(4,2,2,2,2,2,2,2,2,2,2,2,2,2,2,2,2,2,2,2,
2,2,2,2,2,2,2,2,2,2,2,2,2,2,2,2,2,2,2,2,2,2,2,2,2,2,2,2,2,2,2,2,2,2,2,2,
2,2,2,2,2,2,2,2,2,2,2,2,2,2,2,2,2,2,2,2,2,2,2,2,2,2,2,2,2,2,2,2,2,2,2,2,
2,2,2,2,2,2,2,2,2,2,2,2,2,4),(10.4952223301995,10.5011982931848,10.5201141668262,
10.5612176483542,10.710837565267,10.8203497273949,10.8747647732625,10.9065791759548,
10.9358323362552,10.9757890810257,11.1048464791224,11.2127858288314,11.2526351230995,
11.283129772312,11.3008502417718,11.3165402711789,11.3453708443362,11.5000195295456,
11.6170390156557,11.6606110326317,11.6904219297176,11.7211151365107,11.7695005285895,
11.828562249715,11.9776778622939,12.0680464038359,12.0924593207554,12.1080383104008,
12.1251609048322,12.1565187049553,12.1984009800228,12.3174927727997,12.4571046596959,
12.498499574189,12.5276815076566,12.5588752114482,12.6102098212781,12.6450479632141,
12.759799544636,12.8649609089739,12.8945062003926,12.9120406790426,12.9301937411356,
12.9628779515214,13.006792733061,13.1406938104117,13.2393422058225,13.277498416277,
13.3066065516965,13.3389096759854,13.3959895172866,13.6415455398334,13.6876856772709,
13.7079192110452,13.7231566936277,13.7423884942477,13.7854045169452,13.8515218100554,
14.0502772104686,14.1001091521979,14.1310707122562,14.1607090457987,14.2032327874398,
14.3423846151305,14.4786192579758,14.5066981968369,14.5222606947975,14.540167348806,
14.5715997902277,14.6131688489649,14.7312876623688,14.847328371507,14.8870639054878,
14.9162870388762,14.9481909710892,15.003091530125,15.1070660983584,15.281143780499,
15.3099583083846,15.3265670217133,15.342674080297,15.3690401714997,15.493534994602,
15.6700149594369,15.7153427746451,15.7454795322935,15.775773039985,15.8221301669671,
15.8785897321692,16.0224155298113,16.0974217418858,16.1215490604885,16.1381996504406,
16.1584426685227,16.2028543121936,16.2721398430011,16.4553927504788,16.4962505619495,
16.5256311179101,16.5571081893088,16.6097086821471,16.7383535874396,16.893752455785,
16.9215410247633,16.9379384083926,16.9381046579605),.UNSPECIFIED.);
#30171=B_SPLINE_CURVE_WITH_KNOTS('',3,(#171892,#171893,#171894,#171895,
#171896,#171897,#171898,#171899,#171900,#171901,#171902,#171903,#171904,
#171905,#171906,#171907,#171908,#171909,#171910,#171911,#171912,#171913,
#171914,#171915,#171916,#171917,#171918,#171919,#171920,#171921,#171922,
#171923,#171924,#171925,#171926,#171927,#171928,#171929,#171930,#171931,
#171932,#171933,#171934,#171935,#171936,#171937,#171938,#171939,#171940,
#171941,#171942,#171943,#171944,#171945,#171946,#171947,#171948,#171949,
#171950,#171951,#171952,#171953,#171954,#171955,#171956,#171957,#171958,
#171959,#171960,#171961,#171962,#171963,#171964,#171965,#171966,#171967,
#171968,#171969,#171970,#171971,#171972,#171973,#171974,#171975,#171976,
#171977,#171978,#171979,#171980,#171981,#171982,#171983,#171984,#171985,
#171986,#171987,#171988,#171989,#171990,#171991,#171992,#171993,#171994,
#171995,#171996,#171997,#171998,#171999,#172000,#172001,#172002,#172003,
#172004,#172005,#172006,#172007,#172008,#172009,#172010,#172011,#172012,
#172013,#172014,#172015,#172016,#172017,#172018,#172019,#172020,#172021,
#172022,#172023,#172024,#172025,#172026,#172027,#172028,#172029,#172030,
#172031,#172032,#172033,#172034,#172035,#172036,#172037,#172038,#172039,
#172040,#172041,#172042,#172043,#172044,#172045,#172046,#172047,#172048,
#172049,#172050,#172051,#172052,#172053,#172054,#172055,#172056,#172057,
#172058,#172059,#172060,#172061,#172062,#172063,#172064,#172065,#172066,
#172067,#172068,#172069,#172070,#172071,#172072,#172073,#172074,#172075,
#172076,#172077,#172078,#172079,#172080,#172081,#172082,#172083,#172084,
#172085,#172086,#172087,#172088,#172089,#172090,#172091,#172092,#172093,
#172094,#172095,#172096,#172097,#172098,#172099,#172100,#172101,#172102,
#172103,#172104,#172105,#172106,#172107,#172108,#172109,#172110,#172111,
#172112,#172113,#172114,#172115,#172116,#172117),.UNSPECIFIED.,.F.,.F.,
(4,2,2,2,2,2,2,2,2,2,2,2,2,2,2,2,2,2,2,2,2,2,2,2,2,2,2,2,2,2,2,2,2,2,2,
2,2,2,2,2,2,2,2,2,2,2,2,2,2,2,2,2,2,2,2,2,2,2,2,2,2,2,2,2,2,2,2,2,2,2,2,
2,2,2,2,2,2,2,2,2,2,2,2,2,2,2,2,2,2,2,2,2,2,2,2,2,2,2,2,2,2,2,2,2,2,2,2,
2,2,2,2,2,4),(13.3303028304434,13.3458863286888,13.3725516882644,13.4061359908023,
13.4847270614522,13.6759450464462,13.7198704120896,13.7467739054654,13.7767481029321,
13.8212814221794,13.9456252700599,14.0937325303308,14.1210689909734,14.1365098200614,
14.1546244755228,14.1871107313086,14.2306501286573,14.3618496144961,14.3712773604203,
14.4651102512911,14.5028139166799,14.5318685537057,14.5644070577876,14.622780848882,
14.7000165668204,14.803240976931,14.9027378911907,14.9273515713224,14.9429662990634,
14.9600209165184,14.9910377049003,15.0322924891111,15.1477404423996,15.2802530093577,
15.3271739658346,15.3575978832191,15.3876167246649,15.4324109611222,15.5588318702412,
15.7042153453161,15.7315958150163,15.7470435444722,15.7651447582422,15.7975634600849,
15.8409755746499,15.9712798357069,15.9824693531093,16.0757950332109,16.1134520915238,
16.1425009857032,16.1750637847203,16.2335741805707,16.3110780713012,16.4142756827816,
16.5133128430796,16.5379167027833,16.5535294938141,16.5705869832614,16.6016189978069,
16.642901958538,16.758512847704,16.8908030274003,16.9377230865701,16.9681464938793,
16.9981648836962,17.0429585488897,17.1693785651203,17.3147581392816,17.3421382747194,
17.3575857754761,17.3756866731555,17.4081047119725,17.4515158567751,17.5818160724451,
17.5930115847522,17.6863327831989,17.7239889995254,17.75303740547,17.7855998215379,
17.8441100275484,17.9216141358451,18.0248099792089,18.1238431139926,18.1484465329417,
18.1640590675117,18.1811163037496,18.2121479117771,18.2534303745975,18.3690403249464,
18.5013272165901,18.5482465312657,18.5786694564029,18.6086873708738,18.6534803275609,
18.7798983498586,18.9252756084132,18.9526553108944,18.968102567067,18.9862031777716,
19.0186207018643,19.0620311567516,19.1923292926769,19.2035246762882,19.2968443727149,
19.3344999905819,19.3635479361403,19.3961098374245,19.454619122368,19.5321220142945,
19.6353162218491,19.7343477684474,19.7589507972439,19.7725472889628),
 .UNSPECIFIED.);
#30172=B_SPLINE_CURVE_WITH_KNOTS('',3,(#172118,#172119,#172120,#172121,
#172122,#172123,#172124,#172125,#172126,#172127,#172128,#172129,#172130,
#172131,#172132,#172133,#172134,#172135,#172136,#172137,#172138,#172139,
#172140,#172141,#172142,#172143,#172144,#172145,#172146,#172147,#172148,
#172149,#172150,#172151,#172152,#172153,#172154,#172155,#172156,#172157,
#172158,#172159,#172160,#172161,#172162,#172163,#172164,#172165,#172166,
#172167,#172168,#172169,#172170,#172171,#172172,#172173,#172174,#172175,
#172176,#172177,#172178,#172179,#172180,#172181,#172182,#172183,#172184,
#172185,#172186,#172187,#172188,#172189,#172190,#172191,#172192,#172193,
#172194,#172195,#172196,#172197,#172198,#172199,#172200,#172201,#172202,
#172203,#172204,#172205,#172206,#172207,#172208,#172209,#172210,#172211,
#172212,#172213,#172214,#172215,#172216,#172217,#172218,#172219,#172220,
#172221,#172222,#172223,#172224,#172225,#172226,#172227,#172228,#172229,
#172230,#172231,#172232,#172233,#172234,#172235,#172236,#172237,#172238,
#172239,#172240,#172241,#172242,#172243,#172244,#172245,#172246,#172247,
#172248,#172249,#172250,#172251,#172252,#172253,#172254,#172255,#172256,
#172257,#172258,#172259,#172260,#172261,#172262,#172263,#172264,#172265,
#172266,#172267,#172268,#172269,#172270,#172271,#172272,#172273,#172274,
#172275,#172276,#172277,#172278,#172279,#172280,#172281,#172282,#172283,
#172284,#172285,#172286,#172287,#172288,#172289,#172290,#172291,#172292,
#172293,#172294,#172295,#172296,#172297,#172298,#172299,#172300,#172301,
#172302,#172303,#172304,#172305,#172306,#172307,#172308,#172309,#172310,
#172311,#172312,#172313,#172314,#172315,#172316,#172317,#172318,#172319,
#172320,#172321,#172322,#172323,#172324,#172325,#172326,#172327,#172328,
#172329,#172330,#172331),.UNSPECIFIED.,.F.,.F.,(4,2,2,2,2,2,2,2,2,2,2,2,
2,2,2,2,2,2,2,2,2,2,2,2,2,2,2,2,2,2,2,2,2,2,2,2,2,2,2,2,2,2,2,2,2,2,2,2,
2,2,2,2,2,2,2,2,2,2,2,2,2,2,2,2,2,2,2,2,2,2,2,2,2,2,2,2,2,2,2,2,2,2,2,2,
2,2,2,2,2,2,2,2,2,2,2,2,2,2,2,2,2,2,2,2,2,2,4),(16.9381046579605,16.9542302905378,
16.9815079559571,17.0161358369833,17.0990705756198,17.281663301635,17.326549864848,
17.3536045109049,17.3834139473609,17.4269794760336,17.5439546486233,17.6984511933568,
17.7273810036705,17.7430880273296,17.7607854896951,17.7911643203876,17.8308041244526,
17.9375671978045,18.0682962903425,18.1082285607795,18.1374781231329,18.1693017554341,
18.2237682312351,18.3321706252319,18.4795226022105,18.5228614178865,18.5421452229526,
18.5573792669162,18.5779107226447,18.6296544540729,18.7185914269492,18.890953761646,
18.9364903724993,18.9666642333328,18.9969183204702,19.0430541862303,19.0991338405693,
19.2405506256492,19.3184585592705,19.3427372301077,19.3594046237519,19.3795573368572,
19.4234070666597,19.4913104405511,19.6779605326234,19.7183153435066,19.7476231003178,
19.7792817711919,19.8328603398126,19.9634779221162,20.1149427588734,20.1428266872479,
20.1592436514563,20.1755166479756,20.2027028788878,20.3198431657269,20.5031939377934,
20.5480098810489,20.5750529876773,20.6048731800791,20.6485048061577,20.676078352161,
20.7550230088709,20.8598185225424,20.9290951282174,20.9533949765663,20.9700643472372,
20.9902035745078,21.0339724360505,21.1016797315993,21.2888092142557,21.3290899043742,
21.3583864408186,21.3900715902998,21.4437966655168,21.5550304345355,21.7058183901195,
21.7457737084136,21.764493496282,21.7797795670898,21.8010575967874,21.8586169404002,
21.9660703604165,22.1095203892109,22.1563819667218,22.1867943136484,22.2168211546372,
22.2616659667345,22.3885012027066,22.5332116036451,22.5606623169395,22.5761210114605,
22.5942007575406,22.6265121584786,22.6697225955412,22.7986257088523,22.8159852915396,
22.9057314308541,22.9430815651382,22.9720955805802,23.0048273479192,23.064282535774,
23.1436545541524,23.3102516102636,23.3521031003166,23.3680703288497,23.3806731202454),
 .UNSPECIFIED.);
#30173=B_SPLINE_CURVE_WITH_KNOTS('',3,(#172334,#172335,#172336,#172337,
#172338,#172339,#172340,#172341,#172342,#172343,#172344,#172345,#172346,
#172347,#172348,#172349,#172350,#172351,#172352,#172353,#172354,#172355,
#172356,#172357,#172358,#172359,#172360,#172361,#172362,#172363,#172364,
#172365,#172366,#172367,#172368,#172369,#172370,#172371,#172372,#172373,
#172374,#172375,#172376,#172377,#172378,#172379,#172380,#172381,#172382,
#172383,#172384,#172385,#172386,#172387,#172388,#172389,#172390,#172391,
#172392,#172393,#172394,#172395,#172396,#172397,#172398,#172399,#172400,
#172401,#172402,#172403,#172404,#172405,#172406,#172407,#172408,#172409,
#172410,#172411,#172412,#172413,#172414,#172415,#172416,#172417,#172418,
#172419,#172420,#172421,#172422,#172423,#172424,#172425,#172426,#172427,
#172428,#172429,#172430,#172431,#172432,#172433,#172434,#172435,#172436,
#172437,#172438,#172439,#172440,#172441,#172442,#172443,#172444,#172445,
#172446,#172447,#172448,#172449,#172450,#172451,#172452,#172453,#172454,
#172455,#172456,#172457,#172458,#172459,#172460,#172461,#172462,#172463,
#172464,#172465,#172466,#172467,#172468,#172469,#172470,#172471,#172472,
#172473,#172474,#172475,#172476,#172477,#172478,#172479,#172480,#172481,
#172482,#172483,#172484,#172485,#172486,#172487,#172488,#172489,#172490,
#172491,#172492,#172493,#172494,#172495,#172496,#172497,#172498,#172499,
#172500,#172501,#172502,#172503,#172504,#172505,#172506,#172507,#172508,
#172509,#172510,#172511,#172512,#172513,#172514,#172515,#172516,#172517,
#172518,#172519,#172520,#172521,#172522,#172523,#172524,#172525,#172526,
#172527,#172528,#172529,#172530,#172531,#172532,#172533,#172534,#172535,
#172536,#172537,#172538,#172539,#172540,#172541,#172542,#172543,#172544,
#172545,#172546,#172547),.UNSPECIFIED.,.F.,.F.,(4,2,2,2,2,2,2,2,2,2,2,2,
2,2,2,2,2,2,2,2,2,2,2,2,2,2,2,2,2,2,2,2,2,2,2,2,2,2,2,2,2,2,2,2,2,2,2,2,
2,2,2,2,2,2,2,2,2,2,2,2,2,2,2,2,2,2,2,2,2,2,2,2,2,2,2,2,2,2,2,2,2,2,2,2,
2,2,2,2,2,2,2,2,2,2,2,2,2,2,2,2,2,2,2,2,2,2,4),(9.99999998048566E-7,0.00834286144590505,
0.0177640667967872,0.0443704512860533,0.221553904266857,0.324776256047929,
0.379415729592964,0.411272071436925,0.440511894327933,0.480366880991184,
0.670334133764149,0.736926102996499,0.780236264571233,0.800302085622393,
0.816988116744412,0.841420562650441,0.919654749145134,1.06060638730221,
1.1166147636061,1.16270935329757,1.19295728388864,1.22314016131068,1.26872095420009,
1.47289041591499,1.54092443341236,1.58475036792778,1.60411311821516,1.61934395744352,
1.63942842626298,1.68466555767539,1.93119791592704,1.98848249191259,2.02082404286317,
2.0499245319029,2.08800904734668,2.18426336945691,2.32021421986361,2.36440785725355,
2.39723956796959,2.41542206247379,2.43293496630915,2.4623655809095,2.57485795209346,
2.68491529535448,2.75605909595906,2.79060108383157,2.81944402763495,2.85487328097934,
2.93073928908664,2.97254590531705,3.12096301605404,3.16720229429947,3.20086986220605,
3.21844505952338,3.23383104101312,3.25707899360891,3.32983882344906,3.49408295297215,
3.55547920711643,3.60522732965993,3.63617422684778,3.66548738009172,3.70103665451084,
3.8950751093854,3.95978285991415,4.00230356596832,4.02223977402358,4.0389546510325,
4.06362143231028,4.14508193895005,4.28328645306604,4.33884742264124,4.38468072972562,
4.41488280468269,4.44511197082407,4.49094911775094,4.65784511985492,4.75011904504832,
4.78685643259309,4.815353005971,4.83189707030005,4.84805919618089,4.87469627736907,
5.04137366155528,5.16197423512273,5.21402548464954,5.24540195989211,5.27482963215457,
5.3159927581544,5.49713950832766,5.56730735531076,5.61207477474198,5.63237534482196,
5.64901726063103,5.67305448454816,5.74695604356235,5.89178865167136,5.94840797686942,
5.9948584944394,6.02517022769549,6.05529422481561,6.1005414456489,6.27842455005587,
6.36402201393951,6.4146057232201,6.43497826388505,6.44334884079168),
 .UNSPECIFIED.);
#30174=B_SPLINE_CURVE_WITH_KNOTS('',3,(#172550,#172551,#172552,#172553,
#172554,#172555,#172556,#172557,#172558,#172559,#172560,#172561,#172562,
#172563,#172564,#172565,#172566,#172567,#172568,#172569,#172570,#172571,
#172572,#172573,#172574,#172575,#172576,#172577,#172578,#172579,#172580,
#172581,#172582,#172583,#172584,#172585,#172586,#172587,#172588,#172589,
#172590,#172591,#172592,#172593,#172594,#172595,#172596,#172597,#172598,
#172599,#172600,#172601,#172602,#172603,#172604,#172605,#172606,#172607,
#172608,#172609,#172610,#172611,#172612,#172613,#172614,#172615,#172616,
#172617,#172618,#172619,#172620,#172621,#172622,#172623,#172624,#172625,
#172626,#172627,#172628,#172629,#172630,#172631,#172632,#172633,#172634,
#172635,#172636,#172637,#172638,#172639,#172640,#172641,#172642,#172643,
#172644,#172645,#172646,#172647,#172648,#172649,#172650,#172651,#172652,
#172653,#172654,#172655,#172656,#172657,#172658,#172659,#172660,#172661,
#172662,#172663,#172664,#172665,#172666,#172667,#172668,#172669,#172670,
#172671,#172672,#172673,#172674,#172675,#172676,#172677,#172678,#172679,
#172680,#172681,#172682,#172683,#172684,#172685,#172686,#172687,#172688,
#172689,#172690,#172691,#172692,#172693,#172694,#172695,#172696,#172697,
#172698,#172699,#172700,#172701,#172702,#172703,#172704,#172705,#172706,
#172707,#172708,#172709,#172710,#172711,#172712,#172713,#172714,#172715,
#172716,#172717,#172718,#172719,#172720,#172721,#172722,#172723,#172724,
#172725,#172726,#172727,#172728,#172729,#172730,#172731,#172732,#172733,
#172734,#172735,#172736,#172737,#172738,#172739,#172740,#172741,#172742,
#172743,#172744,#172745,#172746,#172747,#172748,#172749,#172750,#172751,
#172752,#172753,#172754,#172755,#172756,#172757,#172758,#172759,#172760,
#172761,#172762,#172763,#172764,#172765),.UNSPECIFIED.,.F.,.F.,(4,2,2,2,
2,2,2,2,2,2,2,2,2,2,2,2,2,2,2,2,2,2,2,2,2,2,2,2,2,2,2,2,2,2,2,2,2,2,2,2,
2,2,2,2,2,2,2,2,2,2,2,2,2,2,2,2,2,2,2,2,2,2,2,2,2,2,2,2,2,2,2,2,2,2,2,2,
2,2,2,2,2,2,2,2,2,2,2,2,2,2,2,2,2,2,2,2,2,2,2,2,2,2,2,2,2,2,2,4),(6.8874084212544,
6.8931476979918,6.91193457522707,6.95227471359089,7.10269181429562,7.21258566515954,
7.26698091127184,7.29879233467828,7.32804777647773,7.36801574908982,7.49612765992609,
7.60475441792588,7.64472596340581,7.67528814179571,7.6930223285844,7.70870312128107,
7.73747796699285,7.87094346979186,8.01151058958166,8.05406317889222,8.08370690190195,
8.11466188078627,8.1644548820903,8.36323289561284,8.4293761871952,8.47240398190068,
8.49163805792286,8.50687588749096,8.52710810825527,8.57323741716685,8.81883048471187,
8.87591736430399,8.90822245361849,8.93733117746541,8.97548646279464,9.07408042293343,
9.20801948114663,9.25193901682701,9.284626268699,9.30278027668346,9.32031488611257,
9.34985929740095,9.45473430520403,9.569698342345,9.60457381044061,9.6559463214887,
9.6871475416497,9.71632703695402,9.75770205494782,9.89901768809575,10.0168511978477,
10.0585188144546,10.0897607296006,10.1068605476429,10.122451904686,10.1469331931645,
10.2422392832044,10.3452626589476,10.4250348771085,10.4846916825598,10.5174611178321,
10.5464706291868,10.5837619496263,10.6729396529996,10.6911461266842,10.8199600911317,
10.8631582851443,10.8954641080057,10.913543601221,10.9290042253279,10.9564621737753,
11.101154215805,11.2280278623349,11.2728797275263,11.3029093124564,11.3333228775806,
11.3801831351613,11.5231030291366,11.6309462642744,11.6886188773855,11.7099114723339,
11.7251997742406,11.7439118613215,11.7838177072938,11.9346844582464,12.0447904378391,
12.0991709762353,12.1309790482828,12.160234475402,12.2002073852251,12.3274474868857,
12.4367031745351,12.4767846487415,12.5074069829761,12.5251527368355,12.5408242511039,
12.56954680696,12.7303728832813,12.8255731826283,12.8770870522267,12.9083137430622,
12.937480647036,12.9787745915852,13.1086034429492,13.2847225008811,13.3131830449594,
13.3297191004029,13.3303028304434),.UNSPECIFIED.);
#30175=B_SPLINE_CURVE_WITH_KNOTS('',3,(#172770,#172771,#172772,#172773,
#172774,#172775,#172776,#172777,#172778,#172779,#172780,#172781,#172782,
#172783,#172784,#172785,#172786,#172787,#172788,#172789,#172790,#172791,
#172792,#172793,#172794,#172795,#172796,#172797,#172798,#172799,#172800,
#172801,#172802,#172803,#172804,#172805,#172806,#172807,#172808,#172809,
#172810,#172811,#172812,#172813,#172814,#172815,#172816,#172817,#172818,
#172819,#172820,#172821,#172822,#172823,#172824,#172825,#172826,#172827,
#172828,#172829,#172830,#172831,#172832,#172833,#172834,#172835,#172836,
#172837,#172838,#172839,#172840,#172841,#172842,#172843,#172844,#172845,
#172846,#172847,#172848,#172849,#172850,#172851,#172852,#172853,#172854,
#172855,#172856,#172857,#172858,#172859,#172860,#172861,#172862,#172863,
#172864,#172865,#172866,#172867,#172868,#172869,#172870,#172871,#172872,
#172873,#172874,#172875,#172876,#172877,#172878,#172879,#172880,#172881,
#172882,#172883,#172884,#172885,#172886,#172887,#172888,#172889,#172890,
#172891,#172892,#172893,#172894,#172895,#172896,#172897,#172898,#172899,
#172900,#172901,#172902,#172903,#172904,#172905,#172906,#172907,#172908,
#172909,#172910,#172911,#172912,#172913,#172914,#172915,#172916,#172917,
#172918,#172919,#172920,#172921,#172922,#172923,#172924,#172925,#172926,
#172927,#172928,#172929,#172930,#172931,#172932,#172933,#172934,#172935,
#172936,#172937,#172938,#172939,#172940,#172941,#172942,#172943,#172944,
#172945,#172946,#172947,#172948,#172949,#172950,#172951,#172952,#172953,
#172954,#172955,#172956,#172957,#172958,#172959,#172960,#172961,#172962,
#172963,#172964,#172965,#172966,#172967,#172968,#172969,#172970,#172971,
#172972,#172973,#172974,#172975,#172976,#172977,#172978,#172979,#172980,
#172981,#172982,#172983,#172984,#172985,#172986,#172987,#172988,#172989),
 .UNSPECIFIED.,.F.,.F.,(4,2,2,2,2,2,2,2,2,2,2,2,2,2,2,2,2,2,2,2,2,2,2,2,
2,2,2,2,2,2,2,2,2,2,2,2,2,2,2,2,2,2,2,2,2,2,2,2,2,2,2,2,2,2,2,2,2,2,2,2,
2,2,2,2,2,2,2,2,2,2,2,2,2,2,2,2,2,2,2,2,2,2,2,2,2,2,2,2,2,2,2,2,2,2,2,2,
2,2,2,2,2,2,2,2,2,2,2,2,2,4),(0.444473727037554,0.44569666576656,0.462457412279222,
0.492014020454777,0.628329929449259,0.739182942359156,0.790527183277837,
0.834240640537556,0.864096106430243,0.891121802638194,0.935882755657428,
1.05763238444124,1.18434537221623,1.22560492572548,1.24532970898227,1.26209779708942,
1.28717017897574,1.37652478081576,1.50837964394317,1.54592545196543,1.59994381909527,
1.63162659240943,1.66093134393032,1.7011771809382,1.81597295936036,1.95640075266018,
2.02212106258482,2.04430825171449,2.05969560079507,2.07786089714591,2.11467755976525,
2.29598519843079,2.37334946652739,2.43178921120935,2.46434054448088,2.49339387246809,
2.53107763597037,2.6246989682917,2.63523112299089,2.76576497900819,2.80920998407807,
2.84164689624057,2.85975234835858,2.87519915604307,2.90257021858942,3.0481565985851,
3.17446229849664,3.21924399553585,3.24926185225053,3.27613078212855,3.31982889901256,
3.51276298776419,3.59054732950157,3.62393340306708,3.65048220980924,3.66662635419815,
3.68319110718666,3.71178954442697,3.85235133245311,4.01206874999574,4.05577982322363,
4.08563447664817,4.11265994735563,4.15742177377,4.2775826652578,4.38409014260239,
4.42368407807875,4.45403819762537,4.47173127926597,4.48744280901574,4.51639634910409,
4.6049069265807,4.73187270442656,4.76869064443234,4.82199715813846,4.85355035898922,
4.88290365767978,4.92349119774373,5.03921135224957,5.21878780455633,5.25457793594768,
5.272554326443,5.28798876060115,5.30691252884742,5.35880973149051,5.51742213530823,
5.59482048757793,5.65327780260943,5.68583250404732,5.7148854397096,5.75256384255149,
5.84612289040229,5.85546426649575,5.98699907233347,6.03058577321119,6.06309777725836,
6.0812180662375,6.09665706722825,6.12397891103025,6.27063851247635,6.39617504209887,
6.4408606715366,6.47086214161049,6.50131068343722,6.54835923024429,6.69508442948009,
6.79989183914482,6.85668284467142,6.8778684731313,6.8874084212544),
 .UNSPECIFIED.);
#30176=B_SPLINE_CURVE_WITH_KNOTS('',3,(#172990,#172991,#172992,#172993,
#172994,#172995,#172996,#172997,#172998,#172999,#173000,#173001,#173002,
#173003,#173004,#173005,#173006,#173007,#173008,#173009,#173010,#173011,
#173012,#173013,#173014,#173015,#173016,#173017,#173018,#173019,#173020,
#173021,#173022,#173023,#173024,#173025,#173026,#173027,#173028,#173029,
#173030,#173031,#173032,#173033,#173034,#173035,#173036,#173037,#173038,
#173039,#173040,#173041,#173042,#173043,#173044,#173045,#173046,#173047,
#173048,#173049,#173050,#173051,#173052,#173053,#173054,#173055,#173056,
#173057,#173058,#173059,#173060,#173061,#173062,#173063,#173064,#173065,
#173066,#173067,#173068,#173069,#173070,#173071,#173072,#173073,#173074,
#173075,#173076,#173077,#173078,#173079,#173080,#173081,#173082,#173083,
#173084,#173085,#173086,#173087,#173088,#173089,#173090,#173091,#173092,
#173093,#173094,#173095,#173096,#173097,#173098,#173099,#173100,#173101,
#173102,#173103,#173104,#173105,#173106,#173107,#173108,#173109,#173110,
#173111,#173112,#173113,#173114,#173115,#173116,#173117,#173118,#173119,
#173120,#173121,#173122,#173123,#173124,#173125,#173126,#173127,#173128,
#173129,#173130,#173131,#173132,#173133,#173134,#173135,#173136,#173137,
#173138,#173139,#173140,#173141,#173142,#173143,#173144,#173145,#173146,
#173147,#173148,#173149,#173150,#173151,#173152,#173153,#173154,#173155,
#173156,#173157,#173158,#173159,#173160,#173161,#173162,#173163,#173164,
#173165,#173166,#173167,#173168,#173169,#173170,#173171,#173172,#173173,
#173174,#173175,#173176,#173177,#173178,#173179,#173180,#173181,#173182,
#173183,#173184,#173185,#173186,#173187,#173188,#173189,#173190,#173191,
#173192,#173193,#173194,#173195,#173196,#173197,#173198,#173199,#173200,
#173201),.UNSPECIFIED.,.F.,.F.,(4,2,2,2,2,2,2,2,2,2,2,2,2,2,2,2,2,2,2,2,
2,2,2,2,2,2,2,2,2,2,2,2,2,2,2,2,2,2,2,2,2,2,2,2,2,2,2,2,2,2,2,2,2,2,2,2,
2,2,2,2,2,2,2,2,2,2,2,2,2,2,2,2,2,2,2,2,2,2,2,2,2,2,2,2,2,2,2,2,2,2,2,2,
2,2,2,2,2,2,2,2,2,2,2,2,2,4),(6.44334884079168,6.45020661119763,6.46962829037362,
6.51382335570583,6.66036685340636,6.78577784535818,6.83120544377829,6.86136155765678,
6.89163898631733,6.93789674469328,6.99418382632804,7.1368919406878,7.21319192619572,
7.23742255677102,7.25408559679794,7.2742692991809,7.31830497201757,7.38666050837615,
7.57221427647539,7.61273808710649,7.64207177564436,7.6736714254471,7.72692292198614,
7.97430722930759,8.02454260163753,8.04331673182283,8.05872399488782,8.07680814039745,
8.11317957995387,8.16477632272232,8.36548425929763,8.42747741939418,8.46100201245027,
8.48990698799265,8.52663010527001,8.6142051062479,8.78865428560555,8.83380175441251,
8.85416243677422,8.87079439690745,8.89473536845016,8.97120891903685,9.0662520061906,
9.18490175020454,9.22474828480411,9.25398845615285,9.28585119258864,9.34051816110509,
9.44264250555622,9.6200699409606,9.64830880663657,9.6648002157263,9.68100899289069,
9.70787455058517,9.83759081362432,10.0071875525531,10.0528712137266,10.0830735221571,
10.1133043724582,10.1592969213707,10.2151287991287,10.3549877822516,10.4344870168673,
10.4590162143119,10.4757144924983,10.4957273242045,10.5387102019195,10.6045155043423,
10.7965513012817,10.8321923609652,10.8615262268871,10.8924393597251,10.9420025825363,
11.0030780687583,11.1650954388579,11.2402967619581,11.2637538045953,11.2791729209072,
11.2966600310387,11.329869563942,11.3752292103597,11.5170414657339,11.6304658632159,
11.6705671218966,11.6998511283669,11.731589488876,11.7859175753562,11.9149149054604,
12.0359141003639,12.0651286074155,12.0826003724143,12.1008378806642,12.1339502525029,
12.1786794885646,12.3186733571335,12.4111894815271,12.4487858940284,12.4778293853812,
12.5104283916848,12.5691324033298,12.6470142965126,12.7362314298784,12.8392947638747,
12.8688111094762,12.8855635427888,12.8867645288586),.UNSPECIFIED.);
#30177=B_SPLINE_CURVE_WITH_KNOTS('',3,(#173232,#173233,#173234,#173235,
#173236,#173237,#173238,#173239,#173240,#173241,#173242,#173243,#173244,
#173245,#173246,#173247,#173248,#173249,#173250,#173251,#173252,#173253,
#173254,#173255,#173256,#173257,#173258,#173259,#173260,#173261,#173262,
#173263,#173264,#173265,#173266,#173267,#173268,#173269,#173270,#173271),
 .UNSPECIFIED.,.F.,.F.,(4,2,2,2,2,2,2,2,2,2,2,2,2,2,2,2,2,2,2,4),(12.8867645288586,
12.9015623774001,12.9273795904343,12.9595366430601,13.0324541294685,13.2369391272014,
13.2788483163085,13.3081109800271,13.339149325778,13.3896247662921,13.43390330168,
13.451409382202,13.4562541410545,13.5522040596861,13.6466306131858,13.6758263086521,
13.693294127577,13.7085327834317,13.7271129613633,13.7835751351093),
 .UNSPECIFIED.);
#30178=B_SPLINE_CURVE_WITH_KNOTS('',3,(#173274,#173275,#173276,#173277,
#173278,#173279,#173280,#173281,#173282,#173283,#173284,#173285,#173286,
#173287,#173288,#173289,#173290,#173291),.UNSPECIFIED.,.F.,.F.,(4,2,2,2,
2,2,2,2,4),(1.00000000165542E-6,0.0153017020044519,0.0305119587961849,0.0583363701016362,
0.103708540329548,0.274366722756818,0.403915594495088,0.429703415281917,
0.444473727037554),.UNSPECIFIED.);
#30179=B_SPLINE_CURVE_WITH_KNOTS('',3,(#173314,#173315,#173316,#173317,
#173318,#173319,#173320,#173321,#173322,#173323,#173324,#173325,#173326,
#173327,#173328,#173329,#173330,#173331,#173332,#173333,#173334,#173335,
#173336,#173337,#173338,#173339,#173340,#173341,#173342,#173343,#173344,
#173345,#173346,#173347,#173348,#173349,#173350,#173351,#173352,#173353,
#173354,#173355,#173356,#173357,#173358,#173359,#173360,#173361,#173362,
#173363,#173364,#173365,#173366,#173367,#173368,#173369,#173370,#173371,
#173372,#173373,#173374,#173375,#173376,#173377,#173378,#173379,#173380,
#173381,#173382,#173383,#173384,#173385,#173386,#173387,#173388,#173389,
#173390,#173391,#173392,#173393,#173394,#173395,#173396,#173397,#173398,
#173399,#173400,#173401,#173402,#173403,#173404,#173405,#173406,#173407,
#173408,#173409,#173410,#173411,#173412,#173413,#173414,#173415,#173416,
#173417,#173418,#173419,#173420,#173421,#173422,#173423,#173424,#173425,
#173426,#173427,#173428,#173429,#173430,#173431,#173432,#173433,#173434,
#173435,#173436,#173437,#173438,#173439,#173440,#173441,#173442,#173443,
#173444,#173445,#173446,#173447,#173448,#173449,#173450,#173451,#173452,
#173453,#173454,#173455,#173456,#173457,#173458,#173459,#173460,#173461,
#173462,#173463,#173464,#173465,#173466,#173467,#173468,#173469,#173470,
#173471,#173472,#173473,#173474,#173475,#173476,#173477,#173478,#173479,
#173480,#173481,#173482,#173483,#173484,#173485,#173486,#173487,#173488,
#173489,#173490,#173491,#173492,#173493,#173494,#173495,#173496,#173497,
#173498,#173499,#173500,#173501,#173502,#173503,#173504,#173505,#173506,
#173507,#173508,#173509,#173510,#173511),.UNSPECIFIED.,.F.,.F.,(4,2,2,2,
2,2,2,2,2,2,2,2,2,2,2,2,2,2,2,2,2,2,2,2,2,2,2,2,2,2,2,2,2,2,2,2,2,2,2,2,
2,2,2,2,2,2,2,2,2,2,2,2,2,2,2,2,2,2,2,2,2,2,2,2,2,2,2,2,2,2,2,2,2,2,2,2,
2,2,2,2,2,2,2,2,2,2,2,2,2,2,2,2,2,2,2,2,2,2,4),(6.28519602509786,6.28901353086328,
6.2973498731085,6.31473179191909,6.42061492088043,6.605250658758,6.65926549255974,
6.67919017382771,6.69245539621225,6.70535294312242,6.72342705860252,6.76886510629959,
6.83666704283505,6.97041023924232,7.04545627146495,7.06019146936096,7.06845088399039,
7.07483484998806,7.08382997653377,7.10261711445801,7.17900000490521,7.36327396446623,
7.41502638214024,7.43456662500351,7.44643453864809,7.45920520306252,7.47655660759406,
7.51727707013666,7.57459858058148,7.77668831880739,7.83375294956289,7.84694800156893,
7.85449967082409,7.86040009869791,7.86870581179625,7.88592945551878,8.02473005738236,
8.2071975499987,8.24036039948964,8.25637220524566,8.26895431395015,8.28304224537606,
8.30681334748901,8.41531234773116,8.54652830008896,8.61723628696111,8.63180153041676,
8.64002274575152,8.6464124487705,8.65546147724681,8.6745314739972,8.7533573826537,
8.95342346288724,8.99164092946578,9.00728489469574,9.01898174064997,9.03189436830331,
9.05004724167751,9.09584396633112,9.16312306337085,9.27024738630931,9.32485842043261,
9.4031696771062,9.41621986821084,9.42442840472778,9.43094967347004,9.43884584386771,
9.45402753468027,9.59186406686353,9.77909615207739,9.81190911692872,9.82785384375041,
9.84042835903054,9.85455502825018,9.87850798525611,9.99094178889568,10.1313997308747,
10.1898738032537,10.2038850793348,10.2118999816578,10.219051102569,10.2288907422188,
10.2524276058154,10.2868502454306,10.4016740345544,10.5349748157314,10.5671441261324,
10.5829564142464,10.5955179364463,10.6097278392607,10.6340515108208,10.748959280512,
10.9316121773167,10.955771170825,10.9826093996835,10.9926127145221,10.9993377269722,
11.0044125226315,11.0097303272946),.UNSPECIFIED.);
#30180=B_SPLINE_CURVE_WITH_KNOTS('',3,(#173514,#173515,#173516,#173517,
#173518,#173519,#173520,#173521,#173522,#173523,#173524,#173525,#173526,
#173527,#173528,#173529,#173530,#173531,#173532,#173533,#173534,#173535,
#173536,#173537,#173538,#173539,#173540,#173541,#173542,#173543,#173544,
#173545,#173546,#173547,#173548,#173549,#173550,#173551,#173552,#173553,
#173554,#173555,#173556,#173557,#173558,#173559,#173560,#173561,#173562,
#173563,#173564,#173565,#173566,#173567,#173568,#173569,#173570,#173571,
#173572,#173573,#173574,#173575,#173576,#173577,#173578,#173579,#173580,
#173581,#173582,#173583,#173584,#173585,#173586,#173587,#173588,#173589,
#173590,#173591,#173592,#173593,#173594,#173595,#173596,#173597,#173598,
#173599,#173600,#173601,#173602,#173603,#173604,#173605,#173606,#173607,
#173608,#173609,#173610,#173611,#173612,#173613,#173614,#173615,#173616,
#173617,#173618,#173619,#173620,#173621,#173622,#173623,#173624,#173625,
#173626,#173627,#173628,#173629,#173630,#173631,#173632,#173633,#173634,
#173635,#173636,#173637,#173638,#173639,#173640,#173641,#173642,#173643,
#173644,#173645,#173646,#173647,#173648,#173649,#173650,#173651,#173652,
#173653,#173654,#173655,#173656,#173657,#173658,#173659,#173660,#173661,
#173662,#173663,#173664,#173665,#173666,#173667,#173668,#173669,#173670,
#173671,#173672,#173673,#173674,#173675,#173676,#173677,#173678,#173679,
#173680,#173681,#173682,#173683,#173684,#173685,#173686,#173687,#173688,
#173689,#173690,#173691,#173692,#173693,#173694,#173695,#173696,#173697,
#173698,#173699),.UNSPECIFIED.,.F.,.F.,(4,2,2,2,2,2,2,2,2,2,2,2,2,2,2,2,
2,2,2,2,2,2,2,2,2,2,2,2,2,2,2,2,2,2,2,2,2,2,2,2,2,2,2,2,2,2,2,2,2,2,2,2,
2,2,2,2,2,2,2,2,2,2,2,2,2,2,2,2,2,2,2,2,2,2,2,2,2,2,2,2,2,2,2,2,2,2,2,2,
2,2,2,2,4),(0.000200536233982881,0.138417303990259,0.172812251864514,0.189055178724505,
0.201663628280664,0.215622323018577,0.238795084007953,0.324791897898088,
0.349164011317468,0.483038165431939,0.529190380219428,0.558082580182329,
0.568846010764633,0.576158804245789,0.583816249184777,0.596196363279018,
0.635879329593167,0.793951507471554,0.910369046537782,0.934492994205679,
0.94865676861636,0.961225662802842,0.977111037346156,1.0096123392182,1.24008206304933,
1.3058522261296,1.34258968533793,1.35371178764923,1.36072973518842,1.36741786276578,
1.37571719549323,1.39663294066603,1.51392738001782,1.61206476455402,1.72656329446571,
1.75086856488995,1.76507508092252,1.77763803902874,1.79345806928563,1.82566447178002,
1.9713069348334,2.03119738309361,2.12142743581017,2.13636698783731,2.14458225005192,
2.15168618158042,2.16100026055674,2.18205518653002,2.28996921622105,2.37950931646946,
2.48292581799482,2.50643889609789,2.52047141804266,2.53306459706185,2.5491740066023,
2.58285221788166,2.75592853625272,2.891621210336,2.91699655937253,2.92668873863429,
2.93340629854986,2.94050355968752,2.95198503164026,2.98830085870527,3.14322440438076,
3.27340149106296,3.31308653581341,3.33026555465513,3.34300828421071,3.3565533039302,
3.37780663550806,3.44338973399375,3.61294020032678,3.66745629889736,3.70008460904966,
3.71123548842394,3.71862697381515,3.72526996051674,3.73633943994479,3.76590845038749,
3.91302234215016,4.03116695838225,4.06893198951861,4.08576711212521,4.09845597275285,
4.11213655269138,4.13401086864785,4.20431447764165,4.37437172967117,4.47886302722555,
4.49351606379445,4.50130236743711,4.50400203993545),.UNSPECIFIED.);
#30181=B_SPLINE_CURVE_WITH_KNOTS('',3,(#173703,#173704,#173705,#173706,
#173707,#173708),.UNSPECIFIED.,.F.,.F.,(4,2,4),(-0.262354516905103,-0.131154285438883,
-9.9978299089587E-7),.UNSPECIFIED.);
#30182=B_SPLINE_CURVE_WITH_KNOTS('',3,(#173710,#173711,#173712,#173713,
#173714,#173715,#173716,#173717,#173718,#173719,#173720,#173721,#173722,
#173723,#173724,#173725),.UNSPECIFIED.,.F.,.F.,(4,2,2,2,2,2,2,4),(9.99999994500671E-7,
0.369172740514888,0.675655915500258,1.11184046459798,1.56416421463315,2.08483397497198,
2.35023008390774,2.63088244313733),.UNSPECIFIED.);
#30183=B_SPLINE_CURVE_WITH_KNOTS('',3,(#173727,#173728,#173729,#173730,
#173731,#173732,#173733,#173734,#173735,#173736,#173737,#173738,#173739,
#173740,#173741,#173742,#173743,#173744,#173745,#173746,#173747,#173748),
 .UNSPECIFIED.,.F.,.F.,(4,2,2,2,2,2,2,2,2,2,4),(2.63088244313733,2.69546818234403,
3.0348688318089,3.19115119671758,3.55687823384515,3.99038170602948,4.20896941662107,
4.74902248620587,5.2734511797038,5.85070004788538,6.57223423227542),
 .UNSPECIFIED.);
#30184=B_SPLINE_CURVE_WITH_KNOTS('',3,(#173752,#173753,#173754,#173755,
#173756,#173757,#173758,#173759,#173760,#173761,#173762,#173763,#173764,
#173765,#173766,#173767,#173768,#173769,#173770,#173771,#173772,#173773,
#173774,#173775),.UNSPECIFIED.,.F.,.F.,(4,2,2,2,2,2,2,2,2,2,2,4),(2.75893124092028,
3.47129380746993,3.91475560027265,4.62575754639855,5.13958137759193,5.62273924852717,
6.07205236472011,6.47892216149857,6.92327779350677,7.28438064116319,7.53542186624699,
7.78890090561998),.UNSPECIFIED.);
#30185=B_SPLINE_CURVE_WITH_KNOTS('',3,(#173779,#173780,#173781,#173782,
#173783,#173784,#173785,#173786,#173787,#173788,#173789,#173790,#173791,
#173792),.UNSPECIFIED.,.F.,.F.,(4,2,2,2,2,2,4),(9.99999998254383E-7,0.400379609020636,
0.849460616516701,1.36345993017091,1.96278107846063,2.643590982597,2.75893124092028),
 .UNSPECIFIED.);
#30186=B_SPLINE_CURVE_WITH_KNOTS('',3,(#173827,#173828,#173829,#173830,
#173831,#173832,#173833,#173834,#173835,#173836,#173837,#173838,#173839,
#173840,#173841,#173842,#173843,#173844),.UNSPECIFIED.,.F.,.F.,(4,2,2,2,
2,2,2,2,4),(0.00026697786525906,0.248328138175261,0.378660605109992,0.616962714032332,
1.00025039751551,1.28920300639177,1.42688012206986,1.9141195649657,2.27710571623716),
 .UNSPECIFIED.);
#30187=B_SPLINE_CURVE_WITH_KNOTS('',3,(#173845,#173846,#173847,#173848,
#173849,#173850,#173851,#173852,#173853,#173854,#173855,#173856,#173857,
#173858,#173859,#173860,#173861,#173862,#173863,#173864,#173865,#173866,
#173867,#173868,#173869,#173870,#173871,#173872,#173873,#173874,#173875,
#173876,#173877,#173878),.UNSPECIFIED.,.F.,.F.,(4,2,2,2,2,2,2,2,2,2,2,2,
2,2,2,2,4),(1.00000001235279E-6,0.284067726320766,0.475326776009137,0.748904955936679,
1.14607740629631,1.50603295057684,1.93520778592777,2.3935701797541,2.90506409166115,
3.44391786134405,3.87621012480206,4.36338426004738,4.55553335566627,5.1694239011698,
5.65334987446971,5.87721795904605,5.94644245477199),.UNSPECIFIED.);
#30188=B_SPLINE_CURVE_WITH_KNOTS('',3,(#173881,#173882,#173883,#173884,
#173885,#173886,#173887,#173888,#173889,#173890,#173891,#173892,#173893,
#173894,#173895,#173896,#173897,#173898,#173899,#173900,#173901,#173902,
#173903,#173904,#173905,#173906,#173907,#173908,#173909,#173910,#173911,
#173912,#173913,#173914),.UNSPECIFIED.,.F.,.F.,(4,2,2,2,2,2,2,2,2,2,2,2,
2,2,2,2,4),(2.42138039423514,2.94917661332815,3.69054276678486,4.50082126956817,
5.42793599331964,6.36346209958375,7.33447465668507,7.84009893881512,9.16241399297696,
10.3457374091789,11.9263428378431,13.3309430649595,14.0568928218673,15.8227739100455,
17.3107175510575,19.078104485536,20.8484436842247),.UNSPECIFIED.);
#30189=B_SPLINE_CURVE_WITH_KNOTS('',3,(#173915,#173916,#173917,#173918,
#173919,#173920,#173921,#173922,#173923,#173924,#173925,#173926,#173927,
#173928,#173929,#173930,#173931,#173932),.UNSPECIFIED.,.F.,.F.,(4,2,2,2,
2,2,2,2,4),(-3.11844708417124,-2.64468204992212,-2.24234014729625,-1.61104523883494,
-1.0918992231367,-0.789389280194095,-0.622416825135047,-0.261781713236578,
-9.99995018347022E-7),.UNSPECIFIED.);
#30190=B_SPLINE_CURVE_WITH_KNOTS('',3,(#173933,#173934,#173935,#173936,
#173937,#173938,#173939,#173940,#173941,#173942,#173943,#173944,#173945,
#173946),.UNSPECIFIED.,.F.,.F.,(4,2,2,2,2,2,4),(9.99999998881322E-7,0.263909788184675,
0.673262348384023,1.16230828562023,1.70456174986609,2.30630414009246,2.42138039423514),
 .UNSPECIFIED.);
#30191=B_SPLINE_CURVE_WITH_KNOTS('',3,(#173951,#173952,#173953,#173954,
#173955,#173956,#173957,#173958,#173959,#173960,#173961,#173962,#173963,
#173964,#173965,#173966,#173967,#173968,#173969,#173970,#173971,#173972,
#173973,#173974,#173975,#173976,#173977,#173978,#173979,#173980,#173981,
#173982,#173983,#173984,#173985,#173986,#173987,#173988,#173989,#173990,
#173991,#173992,#173993,#173994),.UNSPECIFIED.,.F.,.F.,(4,2,2,2,2,2,2,2,
2,2,2,2,2,2,2,2,2,2,2,2,2,4),(-0.918151647035043,-0.917455501213576,-0.910381510809376,
-0.898993721060337,-0.859445308085101,-0.784707091077987,-0.585182429345266,
-0.554177150673725,-0.538389469005455,-0.525829981835348,-0.51159222440807,
-0.487088487493674,-0.387504063757192,-0.286760142516632,-0.202034274519989,
-0.184112852766584,-0.175292583613589,-0.16822888003932,-0.159455088186085,
-0.141770058164199,-0.118131103261592,-9.99999999917733E-7),
 .UNSPECIFIED.);
#30192=B_SPLINE_CURVE_WITH_KNOTS('',3,(#173995,#173996,#173997,#173998,
#173999,#174000,#174001,#174002,#174003,#174004,#174005,#174006,#174007,
#174008,#174009,#174010,#174011,#174012,#174013,#174014,#174015,#174016,
#174017,#174018),.UNSPECIFIED.,.F.,.F.,(4,2,2,2,2,2,2,2,2,2,2,4),(-21.2972205327464,
-21.2900945455965,-21.2827776382084,-21.2687259488357,-21.2442239997285,
-21.1220249620756,-21.0309934027925,-20.990754061758,-20.9453911008694,
-20.917065047827,-20.9069670168058,-20.9006012202032),.UNSPECIFIED.);
#30193=B_SPLINE_CURVE_WITH_KNOTS('',3,(#174020,#174021,#174022,#174023,
#174024,#174025,#174026,#174027,#174028,#174029,#174030,#174031,#174032,
#174033,#174034,#174035,#174036,#174037,#174038,#174039),.UNSPECIFIED.,
 .F.,.F.,(4,2,2,2,2,2,2,2,2,4),(-0.634450996246336,-0.622865914713776,-0.599688377221672,
-0.517041024851767,-0.319266063390083,-0.277934609428317,-0.248507740710781,
-0.217016410888511,-0.184161387630576,-1.00000001346245E-6),
 .UNSPECIFIED.);
#30194=B_SPLINE_CURVE_WITH_KNOTS('',3,(#174771,#174772,#174773,#174774,
#174775,#174776,#174777,#174778,#174779,#174780,#174781,#174782,#174783,
#174784,#174785,#174786,#174787,#174788,#174789,#174790,#174791,#174792,
#174793,#174794,#174795,#174796,#174797,#174798,#174799,#174800,#174801,
#174802,#174803,#174804,#174805,#174806,#174807,#174808,#174809,#174810),
 .UNSPECIFIED.,.F.,.F.,(4,2,2,2,2,2,2,2,2,2,2,2,2,2,2,2,2,2,2,4),(16.4121932386951,
16.5930208425103,16.8461078239737,17.0995968965712,17.3585819104816,17.5388688400622,
17.7351706126336,17.9578257108876,18.1560633677355,18.4119469970658,18.5365531367551,
18.7858967699952,19.0446361984666,19.2963636739384,19.55282938767,19.7628209649916,
19.9947900143882,20.2506006554381,20.3828496027218,20.5152088298456),
 .UNSPECIFIED.);
#30195=B_SPLINE_CURVE_WITH_KNOTS('',3,(#174812,#174813,#174814,#174815,
#174816,#174817,#174818,#174819,#174820,#174821,#174822,#174823,#174824,
#174825,#174826,#174827,#174828,#174829,#174830,#174831,#174832,#174833,
#174834,#174835,#174836,#174837,#174838,#174839,#174840,#174841,#174842,
#174843,#174844,#174845),.UNSPECIFIED.,.F.,.F.,(4,2,2,2,2,2,2,2,2,2,2,2,
2,2,2,2,4),(-3.6474313045369,-3.33257853570554,-3.227803824618,-2.94609671662879,
-2.68640335638716,-2.43382900975872,-2.07865629233525,-1.82329744429604,
-1.69779781579172,-1.49131358643697,-1.27057756142443,-1.11563261308778,
-0.88437607370081,-0.690814598987342,-0.518873862845574,-0.260515535696464,
-0.000141823912015449),.UNSPECIFIED.);
#30196=B_SPLINE_CURVE_WITH_KNOTS('',3,(#174848,#174849,#174850,#174851,
#174852,#174853,#174854,#174855,#174856,#174857,#174858,#174859,#174860,
#174861,#174862,#174863,#174864,#174865,#174866,#174867,#174868,#174869,
#174870,#174871,#174872,#174873,#174874,#174875,#174876,#174877,#174878,
#174879,#174880,#174881,#174882,#174883,#174884,#174885,#174886,#174887,
#174888,#174889,#174890,#174891,#174892,#174893,#174894,#174895,#174896,
#174897,#174898,#174899,#174900,#174901,#174902,#174903,#174904,#174905,
#174906,#174907,#174908,#174909,#174910,#174911,#174912,#174913,#174914,
#174915,#174916,#174917,#174918,#174919,#174920,#174921,#174922,#174923),
 .UNSPECIFIED.,.F.,.F.,(4,2,2,2,2,2,2,2,2,2,2,2,2,2,2,2,2,2,2,2,2,2,2,2,
2,2,2,2,2,2,2,2,2,2,2,2,2,4),(0.00016549378706301,0.131853006236288,0.261698990576789,
0.517935066297707,0.716387983891709,0.935197434746891,1.10002486633248,
1.35980835922816,1.48446952560043,1.71312228306834,1.93117096309254,2.15262213646806,
2.32001636811431,2.54132664418812,2.66830819062656,2.92738142725857,3.15039093059539,
3.40877332402121,3.5279082179231,3.78654252090004,3.91245989974845,4.17113821618592,
4.39785287753683,4.52271772135692,4.75314615630485,5.01177835618428,5.26798072414789,
5.52059832272264,5.77934187635112,6.01221566186675,6.2089902580178,6.43228727960982,
6.55702649342403,6.85144774364401,7.05924514976984,7.31290959162113,7.56649104411875,
7.75004480391499),.UNSPECIFIED.);
#30197=B_SPLINE_CURVE_WITH_KNOTS('',3,(#174928,#174929,#174930,#174931,
#174932,#174933,#174934,#174935,#174936,#174937,#174938,#174939,#174940,
#174941,#174942,#174943,#174944,#174945,#174946,#174947,#174948,#174949,
#174950,#174951,#174952,#174953,#174954,#174955,#174956,#174957,#174958,
#174959,#174960,#174961,#174962,#174963,#174964,#174965,#174966,#174967,
#174968,#174969,#174970,#174971,#174972,#174973,#174974,#174975,#174976,
#174977,#174978,#174979,#174980,#174981,#174982,#174983,#174984,#174985,
#174986,#174987,#174988,#174989,#174990,#174991,#174992,#174993,#174994,
#174995,#174996,#174997,#174998,#174999,#175000,#175001,#175002,#175003,
#175004,#175005,#175006,#175007,#175008,#175009),.UNSPECIFIED.,.F.,.F.,
(4,2,2,2,2,2,2,2,2,2,2,2,2,2,2,2,2,2,2,2,2,2,2,2,2,2,2,2,2,2,2,2,2,2,2,
2,2,2,2,2,4),(8.20592890423442,8.38225901240072,8.58683139065276,8.84279381561286,
9.0951465132682,9.35392458008801,9.58374870993814,9.78041991532572,10.0036274478047,
10.2573713007949,10.3819176450443,10.6913316732546,10.8165222413783,11.0495245517201,
11.3082425310969,11.4351743696995,11.6938511186544,11.9424279723859,12.069447778218,
12.1989595233584,12.4572536185707,12.7210408379567,12.8463169911851,13.0577955603349,
13.3169325646344,13.442420483011,13.6682306643446,13.8691273183975,14.1287661136922,
14.2540792835159,14.4824506400339,14.6773644422413,14.8960058930337,15.1180021367018,
15.3775153577096,15.5047943278521,15.7168300382009,15.9908120819898,16.1159914931326,
16.3579030196544,16.4121932386951),.UNSPECIFIED.);
#30198=B_SPLINE_CURVE_WITH_KNOTS('',3,(#175010,#175011,#175012,#175013,
#175014,#175015,#175016,#175017,#175018,#175019,#175020,#175021,#175022,
#175023,#175024,#175025,#175026,#175027,#175028,#175029,#175030,#175031,
#175032,#175033,#175034,#175035,#175036,#175037,#175038,#175039,#175040,
#175041,#175042,#175043,#175044,#175045,#175046,#175047,#175048,#175049,
#175050,#175051,#175052,#175053,#175054,#175055,#175056,#175057,#175058,
#175059,#175060,#175061,#175062,#175063,#175064,#175065,#175066,#175067,
#175068,#175069,#175070,#175071,#175072,#175073,#175074,#175075,#175076,
#175077,#175078,#175079,#175080,#175081,#175082,#175083,#175084,#175085,
#175086,#175087,#175088,#175089),.UNSPECIFIED.,.F.,.F.,(4,2,2,2,2,2,2,2,
2,2,2,2,2,2,2,2,2,2,2,2,2,2,2,2,2,2,2,2,2,2,2,2,2,2,2,2,2,2,2,4),(7.75004480391499,
7.82559307735231,8.02118525258592,8.28072501906034,8.53379530147537,8.78758376914345,
9.04716113331003,9.26718216598056,9.48610231574621,9.68024537017959,9.90991871172859,
10.0351114292772,10.2947553276189,10.4946157112935,10.7212580175289,10.8466614421288,
11.1058000116479,11.315608428921,11.5469143693834,11.6982130176188,11.9566159027608,
12.0810892128377,12.3325158027635,12.5428800202823,12.7596011729384,13.018863254076,
13.2712859568414,13.5242570694265,13.7833183753977,13.9461601162603,14.1487791549318,
14.4077051927678,14.6664417651085,14.7937668432316,14.9917838884636,15.2409388250797,
15.365460191223,15.692537035722,15.8184776621585,15.9564624294639),
 .UNSPECIFIED.);
#30199=B_SPLINE_CURVE_WITH_KNOTS('',3,(#175095,#175096,#175097,#175098,
#175099,#175100,#175101,#175102,#175103,#175104),.UNSPECIFIED.,.F.,.F.,
(4,2,2,2,4),(0.00012251398680704,0.222884378529215,0.446676969347221,0.675563919564766,
0.912296554340543),.UNSPECIFIED.);
#30200=B_SPLINE_CURVE_WITH_KNOTS('',3,(#175106,#175107,#175108,#175109),
 .UNSPECIFIED.,.F.,.F.,(4,4),(0.,1.),.UNSPECIFIED.);
#30201=B_SPLINE_CURVE_WITH_KNOTS('',3,(#175110,#175111,#175112,#175113,
#175114,#175115,#175116,#175117,#175118,#175119),.UNSPECIFIED.,.F.,.F.,
(4,2,2,2,4),(-0.912452539736231,-0.684829823365555,-0.456379958242761,-0.343466785291313,
-6.86284440254452E-5),.UNSPECIFIED.);
#30202=B_SPLINE_CURVE_WITH_KNOTS('',3,(#175125,#175126,#175127,#175128,
#175129,#175130,#175131,#175132,#175133,#175134,#175135,#175136,#175137,
#175138,#175139,#175140,#175141,#175142,#175143,#175144,#175145,#175146,
#175147,#175148,#175149,#175150,#175151,#175152,#175153,#175154,#175155,
#175156,#175157,#175158,#175159,#175160,#175161,#175162,#175163,#175164),
 .UNSPECIFIED.,.F.,.F.,(4,2,2,2,2,2,2,2,2,2,2,2,2,2,2,2,2,2,2,4),(-3.85213857003362,
-3.81351780802066,-3.57037494324692,-3.33336412591946,-3.0942360656147,
-2.85103108402327,-2.66918050910776,-2.42599071864031,-2.18949413218482,
-1.95059174770184,-1.70741763335434,-1.54072919441616,-1.29745630963647,
-1.1796044847409,-0.936390049858489,-0.746647776807323,-0.564050922972708,
-0.425460046457917,-0.21305312129021,-9.9999999880751E-7),.UNSPECIFIED.);
#30203=B_SPLINE_CURVE_WITH_KNOTS('',3,(#175166,#175167,#175168,#175169,
#175170,#175171,#175172,#175173,#175174,#175175),.UNSPECIFIED.,.F.,.F.,
(4,2,2,2,4),(-0.856199781211949,-0.642101402330201,-0.428204524303596,-0.321759740087164,
0.),.UNSPECIFIED.);
#30204=B_SPLINE_CURVE_WITH_KNOTS('',3,(#175177,#175178,#175179,#175180,
#175181,#175182,#175183,#175184,#175185,#175186),.UNSPECIFIED.,.F.,.F.,
(4,2,2,2,4),(-1.24857216709431,-0.938370073706321,-0.624319392609352,-0.314072407460326,
-1.91505823752094E-6),.UNSPECIFIED.);
#30205=B_SPLINE_CURVE_WITH_KNOTS('',3,(#175190,#175191,#175192,#175193,
#175194,#175195,#175196,#175197,#175198,#175199),.UNSPECIFIED.,.F.,.F.,
(4,2,2,2,4),(-1.24672715675223,-0.93314257651352,-0.623377583747238,-0.309803734768785,
-7.91147253157414E-5),.UNSPECIFIED.);
#30206=B_SPLINE_CURVE_WITH_KNOTS('',3,(#175201,#175202,#175203,#175204,
#175205,#175206,#175207,#175208,#175209,#175210),.UNSPECIFIED.,.F.,.F.,
(4,2,2,2,4),(-0.85620344504851,-0.534443747738202,-0.427999096338968,-0.214103034436511,
-6.19686688838123E-6),.UNSPECIFIED.);
#30207=B_SPLINE_CURVE_WITH_KNOTS('',3,(#175212,#175213,#175214,#175215,
#175216,#175217,#175218,#175219,#175220,#175221,#175222,#175223,#175224,
#175225,#175226,#175227,#175228,#175229,#175230,#175231,#175232,#175233,
#175234,#175235,#175236,#175237,#175238,#175239,#175240,#175241,#175242,
#175243,#175244,#175245,#175246,#175247,#175248,#175249,#175250,#175251),
 .UNSPECIFIED.,.F.,.F.,(4,2,2,2,2,2,2,2,2,2,2,2,2,2,2,2,2,2,2,4),(-22.6866943890527,
-22.5303032047481,-22.3763846167728,-22.0766259920643,-21.874826864479,
-21.6366463018233,-21.4013557329154,-21.1773704733836,-20.9343396078115,
-20.8169433024953,-20.606787502898,-20.3635497033644,-20.2099007632458,
-19.9667622500637,-19.8236447234393,-19.5805449222105,-19.4401009849293,
-19.1970125819126,-19.0572964760453,-18.834521337081),.UNSPECIFIED.);
#30208=B_SPLINE_CURVE_WITH_KNOTS('',3,(#175255,#175256,#175257,#175258,
#175259,#175260,#175261,#175262,#175263,#175264,#175265,#175266,#175267,
#175268,#175269,#175270,#175271,#175272,#175273,#175274,#175275,#175276,
#175277,#175278,#175279,#175280,#175281,#175282,#175283,#175284,#175285,
#175286,#175287,#175288,#175289,#175290,#175291,#175292,#175293,#175294,
#175295,#175296,#175297,#175298,#175299,#175300,#175301,#175302,#175303,
#175304,#175305,#175306,#175307,#175308,#175309,#175310,#175311,#175312,
#175313,#175314,#175315,#175316,#175317,#175318,#175319,#175320,#175321,
#175322,#175323,#175324,#175325,#175326,#175327,#175328,#175329,#175330),
 .UNSPECIFIED.,.F.,.F.,(4,2,2,2,2,2,2,2,2,2,2,2,2,2,2,2,2,2,2,2,2,2,2,2,
2,2,2,2,2,2,2,2,2,2,2,2,2,4),(-18.834521337081,-18.8142112428211,-18.6930610625541,
-18.4498270202033,-18.2105484733472,-17.9729461594295,-17.7431487367217,
-17.5442087098032,-17.4253111128454,-17.1905951849816,-16.9473337588043,
-16.7732130783734,-16.5300185480996,-16.2909841113175,-16.0542185594088,
-15.8253352177396,-15.6305501116955,-15.3873225387848,-15.1480794265471,
-14.9107046837507,-14.6809797436391,-14.4834330965413,-14.2402014100838,
-14.0009428884633,-13.7634982178047,-13.5337512383856,-13.3357958936231,
-13.0925628681154,-12.853301565187,-12.6158460453357,-12.3726617626798,
-12.1855926241435,-11.9423727181238,-11.8245607822377,-11.5812786032023,
-11.3433366492245,-11.2260753874151,-11.1297961553119),.UNSPECIFIED.);
#30209=B_SPLINE_CURVE_WITH_KNOTS('',3,(#175335,#175336,#175337,#175338,
#175339,#175340,#175341,#175342,#175343,#175344,#175345,#175346,#175347,
#175348,#175349,#175350,#175351,#175352,#175353,#175354,#175355,#175356,
#175357,#175358,#175359,#175360,#175361,#175362,#175363,#175364,#175365,
#175366,#175367,#175368,#175369,#175370,#175371,#175372,#175373,#175374,
#175375,#175376,#175377,#175378,#175379,#175380,#175381,#175382,#175383,
#175384,#175385,#175386,#175387,#175388,#175389,#175390,#175391,#175392,
#175393,#175394,#175395,#175396,#175397,#175398,#175399,#175400,#175401,
#175402,#175403,#175404,#175405,#175406,#175407,#175408,#175409,#175410,
#175411,#175412,#175413,#175414),.UNSPECIFIED.,.F.,.F.,(4,2,2,2,2,2,2,2,
2,2,2,2,2,2,2,2,2,2,2,2,2,2,2,2,2,2,2,2,2,2,2,2,2,2,2,2,2,2,2,4),(-11.556536076899,
-11.4599091059737,-11.3426764930753,-11.1047897385837,-10.8615067205227,
-10.7436737873529,-10.5004512226842,-10.3121637978976,-10.0689968772169,
-9.83134858415051,-9.59206264015326,-9.34882015260983,-9.22766368519635,
-8.9845680610119,-8.843924548653,-8.6008153678,-8.45696131749682,-8.21380668176722,
-8.05705534469272,-7.81379525350039,-7.69704438167437,-7.45394461400543,
-7.31199668399831,-7.06886954234882,-6.91997962388108,-6.67677155065413,
-6.49576195805203,-6.25255623119234,-6.01622745272294,-5.77741013639552,
-5.53424261099661,-5.37197812846586,-5.12870441503673,-5.0113059354371,
-4.76813077786016,-4.60232369259186,-4.35904771161803,-4.24128069760431,
-3.99807056728671,-3.85213857003362),.UNSPECIFIED.);
#30210=B_SPLINE_CURVE_WITH_KNOTS('',3,(#175415,#175416,#175417,#175418,
#175419,#175420,#175421,#175422,#175423,#175424,#175425,#175426,#175427,
#175428,#175429,#175430,#175431,#175432,#175433,#175434,#175435,#175436,
#175437,#175438,#175439,#175440,#175441,#175442,#175443,#175444,#175445,
#175446,#175447,#175448,#175449,#175450,#175451,#175452,#175453,#175454,
#175455,#175456,#175457,#175458,#175459,#175460,#175461,#175462,#175463,
#175464,#175465,#175466,#175467,#175468,#175469,#175470,#175471,#175472,
#175473,#175474,#175475,#175476,#175477,#175478,#175479,#175480,#175481,
#175482,#175483,#175484,#175485,#175486,#175487,#175488,#175489,#175490),
 .UNSPECIFIED.,.F.,.F.,(4,2,2,2,2,2,2,2,2,2,2,2,2,2,2,2,2,2,2,2,2,2,2,2,
2,2,2,2,2,2,2,2,2,2,2,2,2,4),(-11.1297961553119,-10.9829100940662,-10.8230475417878,
-10.5797749840848,-10.4626462024022,-10.2194975040537,-10.0647874730273,
-9.82153667980929,-9.60379690366332,-9.48630400015833,-9.25101963163764,
-9.02527872492806,-8.78940634808324,-8.55085145790989,-8.30771488641139,
-8.15596340970547,-7.91273314934468,-7.71509397891962,-7.48536686971287,
-7.24797705560601,-7.00873489582634,-6.76550808682275,-6.57009088441412,
-6.34046536874229,-6.1034716395441,-5.86434868796832,-5.62114284806789,
-5.43991081232665,-5.19671060384064,-4.96033806115533,-4.72149865938757,
-4.47833071347064,-4.31490529075738,-4.07163241624487,-3.95410997527723,
-3.71092437494605,-3.53930859415792,-3.4252187051346),.UNSPECIFIED.);
#30211=B_SPLINE_CURVE_WITH_KNOTS('',3,(#175495,#175496,#175497,#175498,
#175499,#175500,#175501,#175502,#175503,#175504,#175505,#175506,#175507,
#175508,#175509,#175510,#175511,#175512,#175513,#175514,#175515,#175516,
#175517,#175518,#175519,#175520,#175521,#175522,#175523,#175524,#175525,
#175526,#175527,#175528,#175529,#175530,#175531,#175532,#175533,#175534,
#175535,#175536,#175537,#175538,#175539,#175540,#175541,#175542,#175543,
#175544,#175545,#175546,#175547,#175548,#175549,#175550,#175551,#175552,
#175553,#175554,#175555,#175556,#175557,#175558,#175559,#175560,#175561,
#175562,#175563,#175564,#175565,#175566,#175567,#175568,#175569,#175570,
#175571,#175572,#175573,#175574,#175575,#175576),.UNSPECIFIED.,.F.,.F.,
(4,2,2,2,2,2,2,2,2,2,2,2,2,2,2,2,2,2,2,2,2,2,2,2,2,2,2,2,2,2,2,2,2,2,2,
2,2,2,2,2,4),(-19.2607415147143,-19.2489929067448,-19.0136586011244,-18.7895409073619,
-18.5497501962804,-18.4323267611571,-18.2193903806131,-17.9761525636568,
-17.857981437046,-17.6147127766078,-17.4445175126809,-17.2013362482858,
-17.054552499899,-16.9362847960168,-16.6680676760938,-16.4249963674093,
-16.2863690742156,-16.0432880999595,-15.9221398697641,-15.6789072259686,
-15.4396337893472,-15.2020777881446,-14.9722964554593,-14.7736460914282,
-14.5304165486609,-14.3785045838873,-14.1353690015121,-14.0183188143693,
-13.7750525066905,-13.6158393249603,-13.3726799597151,-13.2554372067625,
-13.0451087988904,-12.858355020038,-12.6151371326671,-12.465210290949,-12.2220782456079,
-12.1050826480636,-11.8618144997283,-11.7030704694281,-11.556536076899),
 .UNSPECIFIED.);
#30212=B_SPLINE_CURVE_WITH_KNOTS('',3,(#175578,#175579,#175580,#175581,
#175582,#175583,#175584,#175585,#175586,#175587,#175588,#175589,#175590,
#175591,#175592,#175593,#175594,#175595,#175596,#175597,#175598,#175599,
#175600,#175601,#175602,#175603,#175604,#175605,#175606,#175607,#175608,
#175609),.UNSPECIFIED.,.F.,.F.,(4,2,2,2,2,2,2,2,2,2,2,2,2,2,2,4),(-3.4252187051346,
-3.296042216674,-3.17775013519778,-2.9345032039866,-2.82052273167594,-2.58476260927433,
-2.37502283991358,-2.13188994584829,-1.89482091514807,-1.65567382322027,
-1.41246801058212,-1.22857993508971,-0.985427993245079,-0.748545735313343,
-0.373606352085642,-8.37234906265989E-5),.UNSPECIFIED.);
#30213=B_SPLINE_CURVE_WITH_KNOTS('',3,(#175610,#175611,#175612,#175613,
#175614,#175615,#175616,#175617,#175618,#175619,#175620,#175621,#175622,
#175623,#175624,#175625,#175626,#175627,#175628,#175629,#175630,#175631,
#175632,#175633,#175634,#175635,#175636,#175637,#175638,#175639,#175640,
#175641,#175642,#175643,#175644,#175645,#175646,#175647,#175648,#175649,
#175650,#175651,#175652,#175653,#175654,#175655),.UNSPECIFIED.,.F.,.F.,
(4,2,2,2,2,2,2,2,2,2,2,2,2,2,2,2,2,2,2,2,2,2,4),(-15.8342194625049,-15.6977127043355,
-15.5773804110908,-15.3642468765764,-15.09931918308,-14.9294000167655,-14.7206652063124,
-14.486715371738,-14.3080704995446,-14.2094573881803,-13.9895882638501,
-13.8413026265143,-13.5246285120497,-13.2854001451967,-13.0588788494565,
-12.8566029430652,-12.6243630241051,-12.4564523076755,-12.2472506528897,
-12.0126776113488,-11.8406732046349,-11.6300509401454,-11.5541786166363),
 .UNSPECIFIED.);
#30214=B_SPLINE_CURVE_WITH_KNOTS('',3,(#175661,#175662,#175663,#175664,
#175665,#175666,#175667,#175668,#175669,#175670,#175671,#175672,#175673,
#175674,#175675,#175676,#175677,#175678,#175679,#175680,#175681,#175682,
#175683,#175684,#175685,#175686,#175687,#175688,#175689,#175690,#175691,
#175692),.UNSPECIFIED.,.F.,.F.,(4,2,2,2,2,2,2,2,2,2,2,2,2,2,2,4),(-4.28434131557169,
-4.09277740304251,-3.61917124043791,-3.44763569882389,-3.18732168462545,
-2.69760137878484,-2.47655354496899,-2.23097942144452,-1.99516744125324,
-1.79887978653663,-1.30903271099472,-1.1395483035054,-0.874036589805563,
-0.50662520338749,-0.275259912498234,-6.25946676278E-5),.UNSPECIFIED.);
#30215=B_SPLINE_CURVE_WITH_KNOTS('',3,(#175693,#175694,#175695,#175696,
#175697,#175698,#175699,#175700,#175701,#175702,#175703,#175704,#175705,
#175706,#175707,#175708,#175709,#175710,#175711,#175712,#175713,#175714,
#175715,#175716,#175717,#175718,#175719,#175720,#175721,#175722,#175723,
#175724,#175725,#175726,#175727,#175728,#175729,#175730),.UNSPECIFIED.,
 .F.,.F.,(4,2,2,2,2,2,2,2,2,2,2,2,2,2,2,2,2,2,4),(-22.6845908560294,-22.56357533318,
-22.4433332062268,-22.2076672947508,-22.0518282119736,-21.8491460788328,
-21.6061246150425,-21.488733935936,-21.2790179348323,-21.0357861008617,
-20.917655920078,-20.6743899393749,-20.5046475501176,-20.261470665812,-20.1147815859423,
-19.8716721347519,-19.7302899931803,-19.4872020908436,-19.2607415147143),
 .UNSPECIFIED.);
#30216=B_SPLINE_CURVE_WITH_KNOTS('',3,(#175731,#175732,#175733,#175734,
#175735,#175736,#175737,#175738,#175739,#175740,#175741,#175742,#175743,
#175744,#175745,#175746,#175747,#175748,#175749,#175750,#175751,#175752,
#175753,#175754,#175755,#175756,#175757,#175758,#175759,#175760,#175761,
#175762,#175763,#175764,#175765,#175766,#175767,#175768,#175769,#175770,
#175771,#175772,#175773,#175774,#175775,#175776,#175777,#175778,#175779,
#175780,#175781,#175782,#175783,#175784,#175785,#175786,#175787,#175788,
#175789,#175790,#175791,#175792,#175793,#175794,#175795,#175796,#175797,
#175798,#175799,#175800,#175801,#175802,#175803,#175804,#175805,#175806,
#175807,#175808,#175809,#175810,#175811,#175812),.UNSPECIFIED.,.F.,.F.,
(4,2,2,2,2,2,2,2,2,2,2,2,2,2,2,2,2,2,2,2,2,2,2,2,2,2,2,2,2,2,2,2,2,2,2,
2,2,2,2,2,4),(-11.5541786166363,-11.3950854156062,-11.2096775121344,-11.0043226829807,
-10.8500288973595,-10.6890213298879,-10.5864939249941,-10.3829386240887,
-10.2358179688788,-10.0716509837532,-9.89159841404206,-9.65709860754171,
-9.50826552548869,-9.38376704948463,-9.17323910044889,-8.94728758877424,
-8.72851366280805,-8.52549599229854,-8.29298891156297,-8.12584946479877,
-7.91594018917861,-7.70031586754289,-7.49769126456504,-7.18422374900822,
-6.97475394587394,-6.80146565745864,-6.56728466583071,-6.35934118054618,
-6.18839009038117,-5.9560804906308,-5.75359007713891,-5.52928078721657,
-5.31018117475273,-5.10068372756452,-4.93164167344563,-4.70453244843515,
-4.49159153330761,-4.34455457508952,-4.20783168701383,-3.97233424177691,
-3.85128105488488),.UNSPECIFIED.);
#30217=B_SPLINE_CURVE_WITH_KNOTS('',3,(#175819,#175820,#175821,#175822,
#175823,#175824,#175825,#175826),.UNSPECIFIED.,.F.,.F.,(4,2,2,4),(-12.5667441018124,
-12.3948644827148,-12.2315918217553,-11.9950102098449),.UNSPECIFIED.);
#30218=B_SPLINE_CURVE_WITH_KNOTS('',3,(#175834,#175835,#175836,#175837,
#175838,#175839,#175840,#175841,#175842,#175843,#175844,#175845,#175846,
#175847,#175848,#175849,#175850,#175851,#175852,#175853,#175854,#175855,
#175856,#175857,#175858,#175859,#175860,#175861,#175862,#175863,#175864,
#175865,#175866,#175867,#175868,#175869,#175870,#175871,#175872,#175873,
#175874,#175875,#175876,#175877,#175878,#175879,#175880,#175881,#175882,
#175883,#175884,#175885,#175886,#175887,#175888,#175889,#175890,#175891,
#175892,#175893),.UNSPECIFIED.,.F.,.F.,(4,2,2,2,2,2,2,2,2,2,2,2,2,2,2,2,
2,2,2,2,2,2,2,2,2,2,2,2,2,4),(-11.9950102098449,-11.9174453923583,-11.7508299267779,
-11.3974252645589,-11.14570121458,-10.9105100626791,-10.6766139949695,-10.1854286940875,
-10.0159923559882,-9.84730729538404,-9.50844590120323,-9.01935539408419,
-8.86994604666456,-8.62945896795752,-8.37107887875824,-7.87982978978599,
-7.6994348954704,-7.35438717316835,-7.09964540659805,-6.78873130182614,
-6.5189806395568,-6.28324949672827,-6.04828226034808,-5.82497750860391,
-5.35946271865167,-5.19008739133567,-4.91855369030482,-4.5495935508187,
-4.31459941285212,-4.28434131557169),.UNSPECIFIED.);
#30219=B_SPLINE_CURVE_WITH_KNOTS('',3,(#175895,#175896,#175897,#175898,
#175899,#175900,#175901,#175902,#175903,#175904,#175905,#175906,#175907,
#175908,#175909,#175910,#175911,#175912,#175913,#175914,#175915,#175916,
#175917,#175918,#175919,#175920,#175921,#175922,#175923,#175924,#175925,
#175926,#175927,#175928,#175929,#175930,#175931,#175932,#175933,#175934,
#175935,#175936,#175937,#175938,#175939,#175940,#175941,#175942),
 .UNSPECIFIED.,.F.,.F.,(4,2,2,2,2,2,2,2,2,2,2,2,2,2,2,2,2,2,2,2,2,2,2,4),
(-3.85128105488488,-3.79021381602281,-3.62604742867229,-3.47891163529719,
-3.27535403509337,-3.17283585566507,-3.01183230825087,-2.85751291683218,
-2.65215108768188,-2.46499690997713,-2.22947181361531,-2.01689531266768,
-1.86831310131458,-1.73170963183605,-1.50097799364476,-1.31366423476826,
-1.14712140893274,-1.00476385207455,-0.802106911930033,-0.57926903885878,
-0.353938107479744,-0.181471048650026,-0.108959320929375,-1.00000000013978E-6),
 .UNSPECIFIED.);
#30220=B_SPLINE_CURVE_WITH_KNOTS('',3,(#175944,#175945,#175946,#175947,
#175948,#175949,#175950,#175951,#175952,#175953,#175954,#175955,#175956,
#175957,#175958,#175959,#175960,#175961),.UNSPECIFIED.,.F.,.F.,(4,2,2,2,
2,2,2,2,4),(-1.56872780698315,-1.4440306336282,-1.12597350523365,-0.975660481160978,
-0.784391357145661,-0.591408591724091,-0.401362373433468,-0.0876302679175364,
-4.3266993764275E-5),.UNSPECIFIED.);
#30221=B_SPLINE_CURVE_WITH_KNOTS('',3,(#175964,#175965,#175966,#175967,
#175968,#175969,#175970,#175971,#175972,#175973,#175974,#175975,#175976,
#175977,#175978,#175979,#175980,#175981,#175982,#175983,#175984,#175985,
#175986,#175987,#175988,#175989,#175990,#175991,#175992,#175993,#175994,
#175995,#175996,#175997,#175998,#175999,#176000,#176001,#176002,#176003,
#176004,#176005,#176006,#176007,#176008,#176009,#176010,#176011,#176012,
#176013,#176014,#176015,#176016,#176017,#176018,#176019,#176020,#176021,
#176022,#176023,#176024,#176025,#176026,#176027,#176028,#176029,#176030,
#176031,#176032,#176033,#176034,#176035,#176036,#176037,#176038,#176039,
#176040,#176041,#176042,#176043,#176044,#176045),.UNSPECIFIED.,.F.,.F.,
(4,2,2,2,2,2,2,2,2,2,2,2,2,2,2,2,2,2,2,2,2,2,2,2,2,2,2,2,2,2,2,2,2,2,2,
2,2,2,2,2,4),(9.99999996770772E-7,0.216096709673407,0.429552939762468,0.571271952022262,
0.755836106170213,1.01820485320077,1.21703629447801,1.44716350412417,1.64325668657453,
1.84994165032243,2.04724835673668,2.22529775200564,2.48438121460585,2.63947162473055,
2.89870671827172,3.04835514620737,3.17388312085714,3.45727180697445,3.6684611276535,
3.85144843842677,4.11123903335375,4.36451230583652,4.61753038314871,4.86090458780383,
5.0908854501483,5.31127319319499,5.50839114872044,5.73729202430653,5.86251219157969,
6.12172543232554,6.3278151707646,6.45314931926401,6.71822856253032,6.97657492212759,
7.1060792710105,7.23313600922317,7.48178953492956,7.74046648497742,7.86739147753993,
8.12610096263681,8.20592890423442),.UNSPECIFIED.);
#30222=B_SPLINE_CURVE_WITH_KNOTS('',3,(#176046,#176047,#176048,#176049,
#176050,#176051,#176052,#176053,#176054,#176055,#176056,#176057,#176058,
#176059,#176060,#176061,#176062,#176063,#176064,#176065,#176066,#176067,
#176068,#176069,#176070,#176071,#176072,#176073,#176074,#176075,#176076,
#176077,#176078,#176079,#176080,#176081,#176082,#176083,#176084,#176085,
#176086,#176087,#176088,#176089,#176090,#176091,#176092,#176093,#176094,
#176095,#176096,#176097,#176098,#176099,#176100,#176101,#176102,#176103,
#176104,#176105,#176106,#176107,#176108,#176109,#176110,#176111,#176112,
#176113,#176114,#176115,#176116,#176117,#176118,#176119,#176120,#176121,
#176122,#176123,#176124,#176125,#176126,#176127,#176128,#176129),
 .UNSPECIFIED.,.F.,.F.,(4,2,2,2,2,2,2,2,2,2,2,2,2,2,2,2,2,2,2,2,2,2,2,2,
2,2,2,2,2,2,2,2,2,2,2,2,2,2,2,2,2,4),(15.9564624294639,15.9706790833614,
16.2291128145473,16.3883470222381,16.6013963628145,16.8272802503908,17.0859867465911,
17.2118389039018,17.4705312770014,17.6971467409743,17.8221896050243,18.0699274003179,
18.3291189666377,18.4560722250234,18.677144832226,18.8380375686119,19.0633228435152,
19.2690179009758,19.4884396484015,19.6419673542867,19.9017917209588,20.0763305486744,
20.2904388264911,20.5396306120903,20.6645338341068,20.9229592234423,21.1820326854096,
21.3095426955538,21.5133942780727,21.7723438890345,21.8970975613754,22.1291363525681,
22.3287446861619,22.5911219866707,22.7158489770712,22.9425177394998,23.1403660822531,
23.3884095378057,23.5767981126961,23.7214216510108,23.9407025478493,24.1621317186099),
 .UNSPECIFIED.);
#30223=B_SPLINE_CURVE_WITH_KNOTS('',3,(#176133,#176134,#176135,#176136,
#176137,#176138,#176139,#176140,#176141,#176142,#176143,#176144,#176145,
#176146,#176147,#176148),.UNSPECIFIED.,.F.,.F.,(4,2,2,2,2,2,2,4),(-5.34036980583782,
-5.1030202497345,-4.85331064879726,-4.37225443792772,-3.88453013968305,
-3.63186010168836,-3.38655743616596,-3.33078402932135),.UNSPECIFIED.);
#30224=B_SPLINE_CURVE_WITH_KNOTS('',3,(#176152,#176153,#176154,#176155,
#176156,#176157,#176158,#176159,#176160,#176161,#176162,#176163,#176164,
#176165,#176166,#176167,#176168,#176169,#176170,#176171,#176172,#176173),
 .UNSPECIFIED.,.F.,.F.,(4,2,2,2,2,2,2,2,2,2,4),(-3.33078402932135,-3.1457787811171,
-2.66969336894367,-2.42517438029747,-2.18777430400242,-1.69235110047304,
-1.45012215012257,-1.21210349141667,-0.975414798511056,-0.48839821058214,
-4.75981067057991E-5),.UNSPECIFIED.);
#30225=B_SPLINE_CURVE_WITH_KNOTS('',3,(#176175,#176176,#176177,#176178,
#176179,#176180,#176181,#176182,#176183,#176184,#176185,#176186,#176187,
#176188,#176189,#176190,#176191,#176192,#176193,#176194,#176195,#176196,
#176197,#176198,#176199,#176200,#176201,#176202,#176203,#176204,#176205,
#176206,#176207,#176208,#176209,#176210,#176211,#176212,#176213,#176214,
#176215,#176216,#176217,#176218,#176219,#176220,#176221,#176222,#176223,
#176224,#176225,#176226,#176227,#176228,#176229,#176230,#176231,#176232,
#176233,#176234,#176235,#176236,#176237,#176238,#176239,#176240,#176241),
 .UNSPECIFIED.,.F.,.F.,(4,3,3,3,3,3,3,3,3,3,3,3,3,3,3,3,3,3,3,3,3,3,4),
(0.,0.0532797188798471,0.106117363864542,0.124999999999999,0.176897081798013,
0.229324525544414,0.249999999999997,0.30186133202288,0.353569755832338,
0.405192326669397,0.456691995603922,0.499999999999998,0.55129671836749,
0.60294632648651,0.65479461109988,0.70698774344366,0.749999999999999,0.803309497919045,
0.856238158519042,0.875,0.929869764524203,0.984191399199238,0.999999665677159),
 .UNSPECIFIED.);
#30226=B_SPLINE_CURVE_WITH_KNOTS('',3,(#176243,#176244,#176245,#176246,
#176247,#176248,#176249,#176250,#176251,#176252),.UNSPECIFIED.,.F.,.F.,
(4,2,2,2,4),(-1.36676107014523,-1.02924695186398,-0.680886324591757,-0.344531536147177,
-6.48039110289688E-5),.UNSPECIFIED.);
#30227=B_SPLINE_CURVE_WITH_KNOTS('',3,(#176253,#176254,#176255,#176256),
 .UNSPECIFIED.,.F.,.F.,(4,4),(-0.000734763449220644,0.),.UNSPECIFIED.);
#30228=B_SPLINE_CURVE_WITH_KNOTS('',3,(#176506,#176507,#176508,#176509,
#176510,#176511,#176512,#176513,#176514,#176515,#176516,#176517,#176518,
#176519,#176520,#176521,#176522,#176523,#176524,#176525,#176526,#176527,
#176528,#176529,#176530,#176531,#176532,#176533,#176534,#176535,#176536,
#176537,#176538,#176539,#176540,#176541,#176542,#176543,#176544,#176545,
#176546,#176547,#176548,#176549,#176550,#176551,#176552,#176553,#176554,
#176555,#176556,#176557,#176558,#176559,#176560,#176561,#176562,#176563,
#176564,#176565,#176566,#176567,#176568,#176569,#176570,#176571,#176572,
#176573,#176574,#176575,#176576,#176577,#176578,#176579,#176580,#176581,
#176582,#176583,#176584,#176585,#176586,#176587,#176588,#176589,#176590,
#176591,#176592,#176593,#176594,#176595,#176596,#176597,#176598,#176599,
#176600,#176601,#176602,#176603,#176604,#176605,#176606,#176607,#176608,
#176609,#176610,#176611,#176612,#176613,#176614,#176615,#176616,#176617,
#176618,#176619,#176620,#176621,#176622,#176623,#176624,#176625,#176626,
#176627,#176628,#176629,#176630,#176631,#176632,#176633,#176634,#176635,
#176636,#176637,#176638,#176639,#176640,#176641,#176642,#176643,#176644,
#176645,#176646,#176647,#176648,#176649,#176650,#176651,#176652,#176653,
#176654,#176655,#176656,#176657,#176658,#176659,#176660,#176661,#176662,
#176663,#176664,#176665,#176666,#176667,#176668,#176669,#176670,#176671,
#176672,#176673,#176674,#176675,#176676,#176677,#176678,#176679,#176680,
#176681,#176682,#176683,#176684,#176685,#176686,#176687,#176688,#176689,
#176690,#176691,#176692,#176693,#176694,#176695,#176696,#176697,#176698,
#176699,#176700,#176701,#176702,#176703,#176704,#176705,#176706,#176707,
#176708,#176709,#176710,#176711,#176712,#176713,#176714,#176715,#176716,
#176717,#176718,#176719,#176720,#176721,#176722,#176723,#176724,#176725,
#176726,#176727,#176728,#176729,#176730,#176731,#176732,#176733,#176734,
#176735,#176736,#176737,#176738,#176739,#176740,#176741,#176742,#176743,
#176744,#176745,#176746,#176747,#176748,#176749,#176750,#176751,#176752,
#176753,#176754,#176755,#176756,#176757,#176758,#176759,#176760,#176761,
#176762,#176763,#176764,#176765,#176766,#176767,#176768,#176769,#176770,
#176771),.UNSPECIFIED.,.F.,.F.,(4,2,2,2,2,2,2,2,2,2,2,2,2,2,2,2,2,2,2,2,
2,2,2,2,2,2,2,2,2,2,2,2,2,2,2,2,2,2,2,2,2,2,2,2,2,2,2,2,2,2,2,2,2,2,2,2,
2,2,2,2,2,2,2,2,2,2,2,2,2,2,2,2,2,2,2,2,2,2,2,2,2,2,2,2,2,2,2,2,2,2,2,2,
2,2,2,2,2,2,2,2,2,2,2,2,2,2,2,2,2,2,2,2,2,2,2,2,2,2,2,2,2,2,2,2,2,2,2,2,
2,2,2,2,4),(0.00790828593609008,0.135265930619079,0.267467598036355,0.533750941535481,
0.880175746938389,1.1338405443315,1.41070844372411,1.59304779965695,1.75172475124652,
1.94683177568559,2.11230163182156,2.21836502601455,2.42774980582893,2.62554209451856,
2.76879627869621,2.84874851608012,2.95782638710911,3.1420718245399,3.25663249533483,
3.37303209236669,3.45626245649945,3.52892154030204,3.68573723948832,3.80006718543718,
3.88555502975854,4.0320423160462,4.10567934099106,4.17075031359099,4.33697733739522,
4.47525084585826,4.54230650264742,4.69174783611453,4.75810010013034,4.81934275757705,
4.98087758791925,5.06503448417813,5.13211067183557,5.30211215786814,5.38411998545328,
5.44913118286113,5.62478643836323,5.6979080046166,5.76285686104845,5.91135455861418,
6.04924818147376,6.11297581444621,6.23609931889428,6.31387423831546,6.38379383181836,
6.5431982006822,6.65173531534229,6.73360986229017,6.84907769003456,6.96565700724283,
7.06231030062707,7.25738516515829,7.36934772486594,7.49480537614529,7.61574046453119,
7.85193160654754,7.97320619022983,8.08119356140715,8.19959932847115,8.5129309706179,
8.65863771376222,8.89993699829434,9.15208629185396,9.39091843112858,9.89069339159353,
10.1407981290889,10.5878862308056,10.6956897527359,10.9247151895919,11.1721558027748,
11.3026325812458,11.4126909898134,11.5387554878034,11.7749564773706,11.8944454341237,
12.0206020487927,12.1515122339321,12.3960074971869,12.4881436837981,12.6185243384004,
12.6893649949368,12.8337678291243,13.000390380818,13.0719084854457,13.1514103473186,
13.29001535684,13.3604822047163,13.4504758627378,13.6181390237592,13.6835566992388,
13.7534189922822,13.9354044526173,14.0011047363716,14.0851743832152,14.2450851183931,
14.3093195873102,14.3835274618411,14.5778616591905,14.6415990299127,14.7210498163087,
14.8716723114075,14.9401038812815,15.0236827439956,15.2210626466111,15.2872680425288,
15.3680469481223,15.5054195894244,15.5905449268311,15.7067042853767,15.8567162573542,
15.9290186069713,16.035971248706,16.1380071526865,16.2541495814732,16.4512230290027,
16.5501048959706,16.6242393523664,16.6962956772534,16.8009353513907,16.9202921968447,
17.1807747200293,17.2823328953094,17.4399142909722,17.6184675397991,17.8672454811379,
17.9911585604127,18.2371160348155,18.5095082696298,18.7892894936131),
 .UNSPECIFIED.);
#30229=B_SPLINE_CURVE_WITH_KNOTS('',3,(#176913,#176914,#176915,#176916,
#176917,#176918,#176919,#176920,#176921,#176922,#176923,#176924,#176925,
#176926,#176927,#176928,#176929,#176930,#176931,#176932,#176933,#176934,
#176935,#176936,#176937,#176938,#176939,#176940,#176941,#176942,#176943,
#176944,#176945,#176946,#176947,#176948,#176949,#176950,#176951,#176952,
#176953,#176954,#176955,#176956,#176957,#176958,#176959,#176960,#176961,
#176962,#176963,#176964,#176965,#176966,#176967,#176968,#176969,#176970,
#176971,#176972,#176973,#176974,#176975,#176976,#176977,#176978,#176979,
#176980,#176981,#176982,#176983,#176984,#176985,#176986,#176987,#176988,
#176989,#176990,#176991,#176992,#176993,#176994),.UNSPECIFIED.,.F.,.F.,
(4,2,2,2,2,2,2,2,2,2,2,2,2,2,2,2,2,2,2,2,2,2,2,2,2,2,2,2,2,2,2,2,2,2,2,
2,2,2,2,2,4),(-14.2732703759233,-13.8912273375714,-13.6142499111935,-13.3975932237184,
-13.1227155432504,-12.7070233843852,-12.382403721359,-12.1293949736052,
-11.8703642014978,-11.5353850377401,-11.1414389161118,-10.8461410004745,
-10.5760851451527,-10.2292125849178,-9.73704557043714,-9.39335342119085,
-9.12378600305438,-8.81489519476552,-8.39716574474396,-8.04541518664136,
-7.7772102046378,-7.50917494412834,-7.15370825667384,-6.69461619344525,
-6.35436303694603,-6.06376512695785,-5.6829615871504,-5.09892163725548,
-4.68369409177525,-4.3593566671839,-4.01204603447841,-3.53687730817834,
-3.08826224434253,-2.75857559248875,-2.45520533882891,-2.06641699456192,
-1.51781117594086,-1.13911402161876,-0.846466340154513,-0.481778164862169,
-7.79037809214993E-5),.UNSPECIFIED.);
#30230=B_SPLINE_CURVE_WITH_KNOTS('',3,(#177263,#177264,#177265,#177266,
#177267,#177268),.UNSPECIFIED.,.F.,.F.,(4,2,4),(-0.0902565459305608,-0.0451906733529908,
-0.000194550672436811),.UNSPECIFIED.);
#30231=B_SPLINE_CURVE_WITH_KNOTS('',3,(#177290,#177291,#177292,#177293,
#177294,#177295,#177296,#177297,#177298,#177299,#177300,#177301,#177302,
#177303,#177304,#177305,#177306,#177307,#177308,#177309,#177310,#177311,
#177312,#177313,#177314,#177315,#177316,#177317,#177318,#177319,#177320,
#177321,#177322,#177323,#177324,#177325,#177326,#177327,#177328,#177329,
#177330,#177331,#177332,#177333,#177334,#177335,#177336,#177337,#177338,
#177339,#177340,#177341,#177342,#177343,#177344,#177345,#177346,#177347),
 .UNSPECIFIED.,.F.,.F.,(4,3,3,3,3,3,3,3,3,3,3,3,3,3,3,3,3,3,3,4),(-1.28896142245236,
-1.09309231307544,-1.04016081898322,-0.9801834909399,-0.885023600728055,
-0.791562904179352,-0.670254571060442,-0.644748735287768,-0.634093103877705,
-0.626279232157149,-0.469588976340557,-0.352102611119503,-0.310009489205423,
-0.249406568727739,-0.188707985006066,-0.17575239527642,-0.142257802210763,
-0.0813352071442708,-0.0211767799228357,-1.50340976189325E-6),
 .UNSPECIFIED.);
#30232=B_SPLINE_CURVE_WITH_KNOTS('',3,(#177372,#177373,#177374,#177375,
#177376,#177377,#177378,#177379,#177380,#177381,#177382,#177383,#177384,
#177385,#177386,#177387,#177388,#177389,#177390,#177391,#177392,#177393,
#177394,#177395,#177396,#177397,#177398,#177399,#177400,#177401,#177402,
#177403,#177404,#177405,#177406,#177407,#177408,#177409,#177410,#177411,
#177412,#177413,#177414,#177415,#177416,#177417,#177418,#177419,#177420,
#177421,#177422,#177423,#177424,#177425,#177426,#177427,#177428,#177429),
 .UNSPECIFIED.,.F.,.F.,(4,3,3,3,3,3,3,3,3,3,3,3,3,3,3,3,3,3,3,4),(0.000196331256316104,
0.195854367373606,0.245817836587432,0.308742496769627,0.403496982747047,
0.491306783782293,0.608890768308108,0.644062191156899,0.654689003664205,
0.654735110821007,0.813710421230246,0.932829188307881,0.979410739453054,
1.03972898458091,1.1001348124034,1.11172797209159,1.14748205288158,1.20898204679902,
1.26971077107191,1.29001475424264),.UNSPECIFIED.);
#30233=B_SPLINE_CURVE_WITH_KNOTS('',3,(#177450,#177451,#177452,#177453,
#177454,#177455),.UNSPECIFIED.,.F.,.F.,(4,2,4),(-0.0900560505430899,-0.0451018402846952,
-1.01924371517976E-5),.UNSPECIFIED.);
#30234=B_SPLINE_CURVE_WITH_KNOTS('',3,(#178001,#178002,#178003,#178004,
#178005,#178006,#178007,#178008,#178009,#178010,#178011,#178012,#178013,
#178014,#178015,#178016,#178017,#178018,#178019,#178020,#178021,#178022,
#178023,#178024,#178025,#178026,#178027,#178028,#178029,#178030,#178031,
#178032,#178033,#178034,#178035,#178036,#178037,#178038,#178039,#178040,
#178041,#178042),.UNSPECIFIED.,.F.,.F.,(4,2,2,2,2,2,2,2,2,2,2,2,2,2,2,2,
2,2,2,2,4),(16.411939559148,16.5276993648978,16.7898103993412,16.9146234716417,
17.1336164713817,17.331869283095,17.5558277390514,17.7571272017244,17.9098817122033,
18.1686635086661,18.3330413380558,18.5331993144161,18.7925278924566,19.0512622565918,
19.1783118587244,19.3819635677508,19.6487024603407,19.7552464035092,20.0145823158284,
20.2601584579687,20.5148551545717),.UNSPECIFIED.);
#30235=B_SPLINE_CURVE_WITH_KNOTS('',3,(#178044,#178045,#178046,#178047,
#178048,#178049,#178050,#178051,#178052,#178053,#178054,#178055,#178056,
#178057,#178058,#178059,#178060,#178061,#178062,#178063,#178064,#178065,
#178066,#178067,#178068,#178069,#178070,#178071,#178072,#178073,#178074,
#178075,#178076,#178077),.UNSPECIFIED.,.F.,.F.,(4,2,2,2,2,2,2,2,2,2,2,2,
2,2,2,2,4),(-3.64743130453341,-3.33257853567476,-3.22780382457832,-2.94609671661996,
-2.68640335637872,-2.43382900975111,-2.07865629233289,-1.823297444294,-1.69779781578983,
-1.49131358643798,-1.2705775614283,-1.11563261310354,-0.884376073702807,
-0.690814598996595,-0.518873862852227,-0.260515535699254,-0.000141823912015393),
 .UNSPECIFIED.);
#30236=B_SPLINE_CURVE_WITH_KNOTS('',3,(#178080,#178081,#178082,#178083,
#178084,#178085,#178086,#178087,#178088,#178089,#178090,#178091,#178092,
#178093,#178094,#178095,#178096,#178097,#178098,#178099,#178100,#178101,
#178102,#178103,#178104,#178105,#178106,#178107,#178108,#178109,#178110,
#178111,#178112,#178113,#178114,#178115,#178116,#178117,#178118,#178119,
#178120,#178121,#178122,#178123,#178124,#178125,#178126,#178127,#178128,
#178129,#178130,#178131,#178132,#178133,#178134,#178135,#178136,#178137,
#178138,#178139,#178140,#178141,#178142,#178143,#178144,#178145,#178146,
#178147,#178148,#178149,#178150,#178151),.UNSPECIFIED.,.F.,.F.,(4,2,2,2,
2,2,2,2,2,2,2,2,2,2,2,2,2,2,2,2,2,2,2,2,2,2,2,2,2,2,2,2,2,2,2,4),(0.000165493788789278,
0.133572515359782,0.265070417066448,0.525261541659564,0.718250836461765,
0.939262619734119,1.10101308860442,1.36078600247732,1.61438552821345,1.86608480335074,
2.10918592858206,2.36534540858103,2.49037418921662,2.71408475481147,2.97308494587933,
3.09890243561411,3.35779973017724,3.57542031480175,3.79208623060398,4.04882373567806,
4.30051979229931,4.55920852636254,4.81123563101406,5.01845678813855,5.27455044290403,
5.52645653972308,5.76250743234395,6.00874266289446,6.20633919438028,6.3337050145735,
6.59244105306261,6.85126540653577,7.05793450067292,7.31164686257427,7.56543499053437,
7.75024417698323),.UNSPECIFIED.);
#30237=B_SPLINE_CURVE_WITH_KNOTS('',3,(#178156,#178157,#178158,#178159,
#178160,#178161,#178162,#178163,#178164,#178165,#178166,#178167,#178168,
#178169,#178170,#178171,#178172,#178173,#178174,#178175,#178176,#178177,
#178178,#178179,#178180,#178181,#178182,#178183,#178184,#178185,#178186,
#178187,#178188,#178189,#178190,#178191,#178192,#178193,#178194,#178195,
#178196,#178197,#178198,#178199,#178200,#178201,#178202,#178203,#178204,
#178205,#178206,#178207,#178208,#178209,#178210,#178211,#178212,#178213,
#178214,#178215,#178216,#178217,#178218,#178219,#178220,#178221,#178222,
#178223,#178224,#178225,#178226,#178227,#178228,#178229,#178230,#178231,
#178232,#178233,#178234,#178235,#178236,#178237),.UNSPECIFIED.,.F.,.F.,
(4,2,2,2,2,2,2,2,2,2,2,2,2,2,2,2,2,2,2,2,2,2,2,2,2,2,2,2,2,2,2,2,2,2,2,
2,2,2,2,2,4),(8.20599054997932,8.35079045388701,8.60924481411329,8.75465398952731,
8.95626211349646,9.21554237835956,9.34443315214084,9.58153550224463,9.77860946937124,
10.0041117166618,10.2579350567844,10.3824872891584,10.6879416879749,10.8130137052272,
11.0351748170972,11.2420075009466,11.4004731687472,11.6129596147629,11.8470240825678,
12.0601025163729,12.2237306704323,12.4823623009414,12.6947479399234,12.8195512556543,
13.0784335443201,13.3076522799465,13.4323904647595,13.6664221203585,13.8636547400886,
14.0842574617044,14.3120516628972,14.5550127212924,14.8073205727347,15.0605117862674,
15.3202978529829,15.4883699770317,15.7022609398385,15.8985108557244,16.1077929373567,
16.3226600726361,16.411939559148),.UNSPECIFIED.);
#30238=B_SPLINE_CURVE_WITH_KNOTS('',3,(#178238,#178239,#178240,#178241,
#178242,#178243,#178244,#178245,#178246,#178247,#178248,#178249,#178250,
#178251,#178252,#178253,#178254,#178255,#178256,#178257,#178258,#178259,
#178260,#178261,#178262,#178263,#178264,#178265,#178266,#178267,#178268,
#178269,#178270,#178271,#178272,#178273,#178274,#178275,#178276,#178277,
#178278,#178279,#178280,#178281,#178282,#178283,#178284,#178285,#178286,
#178287,#178288,#178289,#178290,#178291,#178292,#178293,#178294,#178295,
#178296,#178297,#178298,#178299,#178300,#178301,#178302,#178303,#178304,
#178305,#178306,#178307,#178308,#178309,#178310,#178311,#178312,#178313,
#178314,#178315,#178316,#178317),.UNSPECIFIED.,.F.,.F.,(4,2,2,2,2,2,2,2,
2,2,2,2,2,2,2,2,2,2,2,2,2,2,2,2,2,2,2,2,2,2,2,2,2,2,2,2,2,2,2,4),(7.75024417698323,
7.82451593103171,8.02113898697175,8.28067309482283,8.53374289089235,8.78755898378574,
9.04712635066033,9.26728651955331,9.48617872391405,9.68037806711142,9.90991948493791,
10.0351210994055,10.2947590347315,10.4947121782736,10.7212623316305,10.8466717851503,
11.1058046174447,11.3157786202329,11.5462098319442,11.6980972601113,11.9564972275347,
12.0809855194537,12.3324431280832,12.5428274659398,12.7594848200696,13.0187426511126,
13.2711191413954,13.5240636571919,13.7831182451389,13.9451540287318,14.1483747254047,
14.4416992472351,14.5664190762602,14.7966381602951,14.9957380443166,15.260658195038,
15.3855066671222,15.5901676955325,15.848864838421,15.9563811041735),
 .UNSPECIFIED.);
#30239=B_SPLINE_CURVE_WITH_KNOTS('',3,(#178323,#178324,#178325,#178326,
#178327,#178328,#178329,#178330,#178331,#178332),.UNSPECIFIED.,.F.,.F.,
(4,2,2,2,4),(0.000122513986806074,0.222884378529465,0.446676969347694,0.675563919565001,
0.912296554340542),.UNSPECIFIED.);
#30240=B_SPLINE_CURVE_WITH_KNOTS('',3,(#178334,#178335,#178336,#178337),
 .UNSPECIFIED.,.F.,.F.,(4,4),(0.,1.),.UNSPECIFIED.);
#30241=B_SPLINE_CURVE_WITH_KNOTS('',3,(#178338,#178339,#178340,#178341,
#178342,#178343,#178344,#178345,#178346,#178347),.UNSPECIFIED.,.F.,.F.,
(4,2,2,2,4),(-0.912452539736376,-0.684829823365645,-0.456379958242787,-0.343466785291317,
-6.86284440253819E-5),.UNSPECIFIED.);
#30242=B_SPLINE_CURVE_WITH_KNOTS('',3,(#178353,#178354,#178355,#178356,
#178357,#178358,#178359,#178360,#178361,#178362,#178363,#178364,#178365,
#178366,#178367,#178368,#178369,#178370,#178371,#178372,#178373,#178374,
#178375,#178376,#178377,#178378,#178379,#178380,#178381,#178382,#178383,
#178384,#178385,#178386,#178387,#178388,#178389,#178390,#178391,#178392,
#178393,#178394,#178395,#178396),.UNSPECIFIED.,.F.,.F.,(4,2,2,2,2,2,2,2,
2,2,2,2,2,2,2,2,2,2,2,2,2,4),(-3.85203272472586,-3.81068214158194,-3.60033621336808,
-3.48309143663605,-3.23993317549133,-3.0806350821531,-2.83736961014879,
-2.72030932217897,-2.47717399183909,-2.32489351843059,-2.08166265518047,
-1.96051566916432,-1.71743905866922,-1.44667552022466,-1.3282758343242,
-1.17213639367387,-0.928887044086265,-0.812271660099406,-0.610350351616681,
-0.31037347820266,-0.156424378504126,-9.99999996142975E-7),
 .UNSPECIFIED.);
#30243=B_SPLINE_CURVE_WITH_KNOTS('',3,(#178398,#178399,#178400,#178401,
#178402,#178403,#178404,#178405,#178406,#178407),.UNSPECIFIED.,.F.,.F.,
(4,2,2,2,4),(-0.856199781212238,-0.642101402330389,-0.428204524303658,-0.321759740087186,
0.),.UNSPECIFIED.);
#30244=B_SPLINE_CURVE_WITH_KNOTS('',3,(#178409,#178410,#178411,#178412,
#178413,#178414,#178415,#178416,#178417,#178418),.UNSPECIFIED.,.F.,.F.,
(4,2,2,2,4),(-1.24857216709389,-0.938370073705948,-0.624319392609061,-0.31407240746023,
-1.91505823160449E-6),.UNSPECIFIED.);
#30245=B_SPLINE_CURVE_WITH_KNOTS('',3,(#178422,#178423,#178424,#178425,
#178426,#178427,#178428,#178429,#178430,#178431),.UNSPECIFIED.,.F.,.F.,
(4,2,2,2,4),(-1.24672715675234,-0.933142576513486,-0.623377583747118,-0.309803734768733,
-7.91147252940148E-5),.UNSPECIFIED.);
#30246=B_SPLINE_CURVE_WITH_KNOTS('',3,(#178433,#178434,#178435,#178436,
#178437,#178438,#178439,#178440,#178441,#178442),.UNSPECIFIED.,.F.,.F.,
(4,2,2,2,4),(-0.85620344504763,-0.534443747738016,-0.427999096338903,-0.214103034436443,
-6.19686689110128E-6),.UNSPECIFIED.);
#30247=B_SPLINE_CURVE_WITH_KNOTS('',3,(#178444,#178445,#178446,#178447,
#178448,#178449,#178450,#178451,#178452,#178453,#178454,#178455,#178456,
#178457,#178458,#178459,#178460,#178461,#178462,#178463,#178464,#178465,
#178466,#178467,#178468,#178469,#178470,#178471,#178472,#178473,#178474,
#178475,#178476,#178477,#178478,#178479,#178480,#178481,#178482,#178483,
#178484,#178485),.UNSPECIFIED.,.F.,.F.,(4,2,2,2,2,2,2,2,2,2,2,2,2,2,2,2,
2,2,2,2,4),(-22.6856736757846,-22.4729484327686,-22.2608902357116,-22.1224645885887,
-21.9401656304958,-21.6971390197663,-21.5797484468213,-21.3707797129937,
-21.1275346348255,-20.9740534912599,-20.7309072529524,-20.6138113800813,
-20.3705385067576,-20.2109568292684,-19.9677909680696,-19.8232856164035,
-19.5801706501752,-19.4393531223485,-19.1962535931423,-18.9580519542603,
-18.8335546705084),.UNSPECIFIED.);
#30248=B_SPLINE_CURVE_WITH_KNOTS('',3,(#178489,#178490,#178491,#178492,
#178493,#178494,#178495,#178496,#178497,#178498,#178499,#178500,#178501,
#178502,#178503,#178504,#178505,#178506,#178507,#178508,#178509,#178510,
#178511,#178512,#178513,#178514,#178515,#178516,#178517,#178518,#178519,
#178520,#178521,#178522,#178523,#178524,#178525,#178526,#178527,#178528,
#178529,#178530,#178531,#178532,#178533,#178534,#178535,#178536,#178537,
#178538,#178539,#178540,#178541,#178542,#178543,#178544,#178545,#178546,
#178547,#178548,#178549,#178550,#178551,#178552,#178553,#178554,#178555,
#178556,#178557,#178558,#178559,#178560,#178561,#178562,#178563,#178564,
#178565,#178566),.UNSPECIFIED.,.F.,.F.,(4,2,2,2,2,2,2,2,2,2,2,2,2,2,2,2,
2,2,2,2,2,2,2,2,2,2,2,2,2,2,2,2,2,2,2,2,2,2,4),(-18.8335546705084,-18.7227357997547,
-18.4794804275072,-18.3029946229965,-18.0597884772514,-17.9421642824665,
-17.6988795154385,-17.5345187053728,-17.2913374272366,-17.1457737280561,
-16.9026517389328,-16.6642788314431,-16.3365927448224,-16.2192214989655,
-15.9859590265659,-15.7503815683893,-15.512436383961,-15.2774941236952,
-15.0545123299144,-14.811474357221,-14.6940767755213,-14.4845852214616,
-14.2413335075011,-14.0877730700931,-13.9694005212358,-13.6992966442092,
-13.4562052826424,-13.33505073917,-13.0918047666125,-12.8525232134558,-12.6150000024995,
-12.3718115009665,-12.1843740433989,-11.941143292846,-11.8233203791244,
-11.5800278639557,-11.3420914658496,-11.2248334089522,-11.1284471789905),
 .UNSPECIFIED.);
#30249=B_SPLINE_CURVE_WITH_KNOTS('',3,(#178571,#178572,#178573,#178574,
#178575,#178576,#178577,#178578,#178579,#178580,#178581,#178582,#178583,
#178584,#178585,#178586,#178587,#178588,#178589,#178590,#178591,#178592,
#178593,#178594,#178595,#178596,#178597,#178598,#178599,#178600,#178601,
#178602,#178603,#178604,#178605,#178606,#178607,#178608,#178609,#178610,
#178611,#178612,#178613,#178614,#178615,#178616,#178617,#178618,#178619,
#178620,#178621,#178622,#178623,#178624,#178625,#178626,#178627,#178628,
#178629,#178630,#178631,#178632,#178633,#178634,#178635,#178636,#178637,
#178638,#178639,#178640,#178641,#178642,#178643,#178644,#178645,#178646,
#178647,#178648),.UNSPECIFIED.,.F.,.F.,(4,2,2,2,2,2,2,2,2,2,2,2,2,2,2,2,
2,2,2,2,2,2,2,2,2,2,2,2,2,2,2,2,2,2,2,2,2,2,4),(-11.5566456717678,-11.4598611162991,
-11.3426388598562,-11.1047720742011,-10.8614846878278,-10.7436406873222,
-10.5004129844007,-10.3115727442124,-10.0919136118381,-9.97374824847428,
-9.73049762835425,-9.51862735066146,-9.40121052478211,-9.15814875252158,
-8.93140561123793,-8.6952260136082,-8.45648843501656,-8.21332578494614,
-8.05479937138979,-7.81152977304203,-7.69455898882562,-7.45142845787144,
-7.30240675633191,-7.05919460455083,-6.87747816562279,-6.63427898704334,
-6.39780330111834,-6.15890783331182,-5.91572809274957,-5.74977652524943,
-5.50649627086529,-5.38871321866122,-5.14549760697054,-4.96012413551749,
-4.716995797981,-4.4798366946526,-4.24065538165822,-3.99743850082616,-3.85203272472586),
 .UNSPECIFIED.);
#30250=B_SPLINE_CURVE_WITH_KNOTS('',3,(#178649,#178650,#178651,#178652,
#178653,#178654,#178655,#178656,#178657,#178658,#178659,#178660,#178661,
#178662,#178663,#178664,#178665,#178666,#178667,#178668,#178669,#178670,
#178671,#178672,#178673,#178674,#178675,#178676,#178677,#178678,#178679,
#178680,#178681,#178682,#178683,#178684,#178685,#178686,#178687,#178688,
#178689,#178690,#178691,#178692,#178693,#178694,#178695,#178696,#178697,
#178698,#178699,#178700,#178701,#178702,#178703,#178704,#178705,#178706,
#178707,#178708,#178709,#178710,#178711,#178712,#178713,#178714,#178715,
#178716,#178717,#178718,#178719,#178720,#178721,#178722,#178723,#178724,
#178725,#178726,#178727,#178728,#178729,#178730,#178731,#178732),
 .UNSPECIFIED.,.F.,.F.,(4,2,2,2,2,2,2,2,2,2,2,2,2,2,2,2,2,2,2,2,2,2,2,2,
2,2,2,2,2,2,2,2,2,2,2,2,2,2,2,2,2,4),(-11.1284471789905,-10.9816587208291,
-10.8221212812395,-10.5788393403607,-10.4617444480828,-10.2185900739436,
-10.0653161343258,-9.82206320327862,-9.61454252856661,-9.49715897724724,
-9.18835062284835,-9.06994520510295,-8.91395148058202,-8.67068666495257,
-8.55470868504613,-8.31162166341757,-8.04192503012683,-7.92357624744711,
-7.77151825007441,-7.52827892879812,-7.40712771267413,-7.16404476106431,
-6.89478333943309,-6.77645862986625,-6.62598533905963,-6.38276068494049,
-6.19286058726435,-5.97177573631606,-5.85343274268845,-5.61017529353358,
-5.49377026376138,-5.25068435595605,-5.11190848598995,-4.86883056632006,
-4.59961981470766,-4.48129985821881,-4.33099374628005,-4.0877753196181,
-3.89883471810049,-3.67904334786015,-3.56086407502634,-3.42395895046783),
 .UNSPECIFIED.);
#30251=B_SPLINE_CURVE_WITH_KNOTS('',3,(#178737,#178738,#178739,#178740,
#178741,#178742,#178743,#178744,#178745,#178746,#178747,#178748,#178749,
#178750,#178751,#178752,#178753,#178754,#178755,#178756,#178757,#178758,
#178759,#178760,#178761,#178762,#178763,#178764,#178765,#178766,#178767,
#178768,#178769,#178770,#178771,#178772,#178773,#178774,#178775,#178776,
#178777,#178778,#178779,#178780,#178781,#178782,#178783,#178784,#178785,
#178786,#178787,#178788,#178789,#178790,#178791,#178792,#178793,#178794,
#178795,#178796,#178797,#178798,#178799,#178800,#178801,#178802,#178803,
#178804,#178805,#178806,#178807,#178808,#178809,#178810,#178811,#178812,
#178813,#178814),.UNSPECIFIED.,.F.,.F.,(4,2,2,2,2,2,2,2,2,2,2,2,2,2,2,2,
2,2,2,2,2,2,2,2,2,2,2,2,2,2,2,2,2,2,2,2,2,2,4),(-19.2614576637728,-19.1356789719326,
-18.9731201279323,-18.7299508942672,-18.584783367083,-18.3416704020533,
-18.2006804311134,-17.9575847946136,-17.8177162848732,-17.5746255386636,
-17.3364643703782,-17.0110447446521,-16.893675924676,-16.6601686346933,
-16.4246089396369,-16.2865539568494,-16.0434714014953,-15.9223218853332,
-15.6790861072034,-15.439812074119,-15.2022771564619,-14.972500515759,-14.7740011427573,
-14.5307675167468,-14.3788774059206,-14.2605320044324,-13.9908835424712,
-13.74780064827,-13.5097367539058,-13.2746224555694,-13.0313626288571,-12.8556969244336,
-12.612493001893,-12.464613656871,-12.2214846886535,-12.1045468764796,-11.8612760424733,
-11.7030254218495,-11.5566456717678),.UNSPECIFIED.);
#30252=B_SPLINE_CURVE_WITH_KNOTS('',3,(#178816,#178817,#178818,#178819,
#178820,#178821,#178822,#178823,#178824,#178825,#178826,#178827,#178828,
#178829,#178830,#178831,#178832,#178833,#178834,#178835,#178836,#178837,
#178838,#178839,#178840,#178841,#178842,#178843,#178844,#178845,#178846,
#178847,#178848,#178849,#178850,#178851,#178852,#178853,#178854,#178855),
 .UNSPECIFIED.,.F.,.F.,(4,2,2,2,2,2,2,2,2,2,2,2,2,2,2,2,2,2,2,4),(-3.42395895046783,
-3.31762163229697,-3.10420599987773,-2.98677630963011,-2.74955318449751,
-2.52785333895686,-2.40944089100547,-2.16618638678871,-2.04940406440818,
-1.8063065177699,-1.66329915599726,-1.42016381120343,-1.26694861534978,
-1.02371503625448,-0.9025623522204,-0.659474909044351,-0.518219698477484,
-0.260456869351534,-0.130812079682504,-8.37234198767857E-5),
 .UNSPECIFIED.);
#30253=B_SPLINE_CURVE_WITH_KNOTS('',3,(#178856,#178857,#178858,#178859,
#178860,#178861,#178862,#178863,#178864,#178865,#178866,#178867,#178868,
#178869,#178870,#178871,#178872,#178873,#178874,#178875,#178876,#178877,
#178878,#178879,#178880,#178881,#178882,#178883,#178884,#178885,#178886,
#178887,#178888,#178889,#178890,#178891,#178892,#178893,#178894,#178895,
#178896,#178897,#178898,#178899,#178900,#178901),.UNSPECIFIED.,.F.,.F.,
(4,2,2,2,2,2,2,2,2,2,2,2,2,2,2,2,2,2,2,2,2,2,4),(-15.8354657754405,-15.6407458592451,
-15.4634984810298,-15.224746948074,-15.0754563288153,-14.9781844851558,
-14.4958306045442,-14.302961113374,-14.0985025945051,-13.8652929473164,
-13.6951623652772,-13.4855741019692,-13.2508958722351,-13.078530665073,
-12.8679347864287,-12.6329351583833,-12.4473201408781,-12.2420452632793,
-12.0880584712123,-11.9269121240055,-11.8242338140593,-11.6207006516122,
-11.5542914416033),.UNSPECIFIED.);
#30254=B_SPLINE_CURVE_WITH_KNOTS('',3,(#178907,#178908,#178909,#178910,
#178911,#178912,#178913,#178914,#178915,#178916,#178917,#178918,#178919,
#178920,#178921,#178922,#178923,#178924,#178925,#178926,#178927,#178928,
#178929,#178930,#178931,#178932,#178933,#178934,#178935,#178936,#178937,
#178938),.UNSPECIFIED.,.F.,.F.,(4,2,2,2,2,2,2,2,2,2,2,2,2,2,2,4),(-4.28434131558935,
-4.09277740390565,-3.61917123484337,-3.44763570279824,-3.18732168422942,
-2.69760137829887,-2.47655354440947,-2.23097941886294,-1.99516743825397,
-1.79887979205484,-1.30903271526569,-1.139548317617,-0.874036586908317,
-0.506625225075278,-0.275259934209563,-6.25946676274787E-5),
 .UNSPECIFIED.);
#30255=B_SPLINE_CURVE_WITH_KNOTS('',3,(#178939,#178940,#178941,#178942,
#178943,#178944,#178945,#178946,#178947,#178948,#178949,#178950,#178951,
#178952,#178953,#178954,#178955,#178956,#178957,#178958,#178959,#178960,
#178961,#178962,#178963,#178964,#178965,#178966,#178967,#178968,#178969,
#178970,#178971,#178972,#178973,#178974,#178975,#178976),.UNSPECIFIED.,
 .F.,.F.,(4,2,2,2,2,2,2,2,2,2,2,2,2,2,2,2,2,2,4),(-22.6854834825577,-22.56281589728,
-22.4409718299283,-22.2016930444766,-22.0443790072972,-21.8011428851532,
-21.6479506659735,-21.4048125035339,-21.166216579999,-20.9302791714888,
-20.7043149936291,-20.5112109918504,-20.2679881685403,-20.1500823996117,
-19.9068055479873,-19.7395638044544,-19.4963842851851,-19.3789539628455,
-19.2614576637728),.UNSPECIFIED.);
#30256=B_SPLINE_CURVE_WITH_KNOTS('',3,(#178977,#178978,#178979,#178980,
#178981,#178982,#178983,#178984,#178985,#178986,#178987,#178988,#178989,
#178990,#178991,#178992,#178993,#178994,#178995,#178996,#178997,#178998,
#178999,#179000,#179001,#179002,#179003,#179004,#179005,#179006,#179007,
#179008,#179009,#179010,#179011,#179012,#179013,#179014,#179015,#179016,
#179017,#179018,#179019,#179020,#179021,#179022,#179023,#179024,#179025,
#179026,#179027,#179028,#179029,#179030,#179031,#179032,#179033,#179034,
#179035,#179036,#179037,#179038,#179039,#179040,#179041,#179042,#179043,
#179044,#179045,#179046,#179047,#179048,#179049,#179050,#179051,#179052,
#179053,#179054,#179055,#179056,#179057,#179058,#179059,#179060),
 .UNSPECIFIED.,.F.,.F.,(4,2,2,2,2,2,2,2,2,2,2,2,2,2,2,2,2,2,2,2,2,2,2,2,
2,2,2,2,2,2,2,2,2,2,2,2,2,2,2,2,2,4),(-11.5542914416033,-11.4737373012928,
-11.309482051677,-11.12712473689,-10.8918422034198,-10.755109644318,-10.6080076524658,
-10.395068669024,-10.1594521898136,-9.97180536976226,-9.7665090044771,-9.61243658395786,
-9.45133180206899,-9.34869787814915,-9.14516201698245,-8.91245253192468,
-8.73952193900105,-8.531902825353,-8.29781529126438,-8.12528871999226,-7.9156016238263,
-7.70024882936839,-7.49762229510223,-7.18415226895485,-6.97468363629993,
-6.80124038036845,-6.56701043783358,-6.35892698651081,-6.18711460646771,
-5.95441407950802,-5.75090105180435,-5.64822728207524,-5.48708701340564,
-5.33311721246657,-5.12786052318682,-4.9400333125358,-4.70438356181232,
-4.49131096231414,-4.34481309486669,-4.20821925860371,-3.97021584717785,
-3.8512796228323),.UNSPECIFIED.);
#30257=B_SPLINE_CURVE_WITH_KNOTS('',3,(#179067,#179068,#179069,#179070,
#179071,#179072,#179073,#179074),.UNSPECIFIED.,.F.,.F.,(4,2,2,4),(-12.5667440997737,
-12.3948646496968,-12.2315921270525,-11.9950102079231),.UNSPECIFIED.);
#30258=B_SPLINE_CURVE_WITH_KNOTS('',3,(#179082,#179083,#179084,#179085,
#179086,#179087,#179088,#179089,#179090,#179091,#179092,#179093,#179094,
#179095,#179096,#179097,#179098,#179099,#179100,#179101,#179102,#179103,
#179104,#179105,#179106,#179107,#179108,#179109,#179110,#179111,#179112,
#179113,#179114,#179115,#179116,#179117,#179118,#179119,#179120,#179121,
#179122,#179123,#179124,#179125,#179126,#179127,#179128,#179129,#179130,
#179131,#179132,#179133,#179134,#179135,#179136,#179137,#179138,#179139,
#179140,#179141),.UNSPECIFIED.,.F.,.F.,(4,2,2,2,2,2,2,2,2,2,2,2,2,2,2,2,
2,2,2,2,2,2,2,2,2,2,2,2,2,4),(-11.9950102079231,-11.9174457962354,-11.7508295781321,
-11.3974253956048,-11.145701176373,-10.9105100206839,-10.6766139857417,
-10.1854286855557,-10.015992362905,-9.84730729815986,-9.50844590171839,
-9.01935539446705,-8.86994604617293,-8.62945896761266,-8.37107887868964,
-7.87982978971591,-7.69943489551864,-7.3543871731509,-7.09964540660761,
-6.78873130182666,-6.51898063956417,-6.28324949673751,-6.04828226035897,
-5.82497750860756,-5.35946271870781,-5.19008739124356,-4.91855369036197,
-4.54959355051724,-4.31459941253855,-4.28434131558935),.UNSPECIFIED.);
#30259=B_SPLINE_CURVE_WITH_KNOTS('',3,(#179143,#179144,#179145,#179146,
#179147,#179148,#179149,#179150,#179151,#179152,#179153,#179154,#179155,
#179156,#179157,#179158,#179159,#179160,#179161,#179162,#179163,#179164,
#179165,#179166,#179167,#179168,#179169,#179170,#179171,#179172,#179173,
#179174,#179175,#179176,#179177,#179178,#179179,#179180,#179181,#179182,
#179183,#179184,#179185,#179186,#179187,#179188,#179189,#179190),
 .UNSPECIFIED.,.F.,.F.,(4,2,2,2,2,2,2,2,2,2,2,2,2,2,2,2,2,2,2,2,2,2,2,4),
(-3.8512796228323,-3.7901986030621,-3.62600036533853,-3.478932106501,-3.27538901373182,
-3.17281013873208,-3.01175246892729,-2.85756470629415,-2.65224064392687,
-2.46482663385682,-2.22925087842699,-2.01648262408061,-1.86870024940216,
-1.73196153851578,-1.4991536801006,-1.3141785407599,-1.14882249401481,-1.00412990208225,
-0.801059083462348,-0.582700972005783,-0.355531059708101,-0.182241705505865,
-0.109215112418338,-9.99999998363421E-7),.UNSPECIFIED.);
#30260=B_SPLINE_CURVE_WITH_KNOTS('',3,(#179192,#179193,#179194,#179195,
#179196,#179197,#179198,#179199,#179200,#179201,#179202,#179203,#179204,
#179205,#179206,#179207,#179208,#179209),.UNSPECIFIED.,.F.,.F.,(4,2,2,2,
2,2,2,2,4),(-1.56872780698428,-1.44403063362972,-1.12597350523431,-0.975660481161639,
-0.784391357146069,-0.59140859172425,-0.401362373433348,-0.087630267916436,
-4.32669937617874E-5),.UNSPECIFIED.);
#30261=B_SPLINE_CURVE_WITH_KNOTS('',3,(#179212,#179213,#179214,#179215,
#179216,#179217,#179218,#179219,#179220,#179221,#179222,#179223,#179224,
#179225,#179226,#179227,#179228,#179229,#179230,#179231,#179232,#179233,
#179234,#179235,#179236,#179237,#179238,#179239,#179240,#179241,#179242,
#179243,#179244,#179245,#179246,#179247,#179248,#179249,#179250,#179251,
#179252,#179253,#179254,#179255,#179256,#179257,#179258,#179259,#179260,
#179261,#179262,#179263,#179264,#179265,#179266,#179267,#179268,#179269,
#179270,#179271,#179272,#179273,#179274,#179275,#179276,#179277,#179278,
#179279,#179280,#179281,#179282,#179283,#179284,#179285,#179286,#179287,
#179288,#179289,#179290,#179291),.UNSPECIFIED.,.F.,.F.,(4,2,2,2,2,2,2,2,
2,2,2,2,2,2,2,2,2,2,2,2,2,2,2,2,2,2,2,2,2,2,2,2,2,2,2,2,2,2,2,4),(1.00000000916034E-6,
0.213754930701631,0.424652319564036,0.565040153296804,0.748075759262127,
1.05142999748217,1.25223264793173,1.50715507366388,1.76061269237607,2.01941808507526,
2.26964944794214,2.47651392626711,2.73003327533967,2.98431110662871,3.24346008377567,
3.50188237345356,3.6267924102787,3.8729079603262,4.08710371160095,4.28624559950554,
4.41150404599036,4.68071417586692,4.89967370396659,5.07419479348004,5.29610569553035,
5.47890193858856,5.70169182511378,5.91354244510472,6.13506182294941,6.26094691361958,
6.51995060806452,6.73927748471563,6.96718021692218,7.11944389614993,7.3777879311047,
7.50229063002226,7.76088809123817,7.96057223441664,8.08559790968841,8.20599054997932),
 .UNSPECIFIED.);
#30262=B_SPLINE_CURVE_WITH_KNOTS('',3,(#179292,#179293,#179294,#179295,
#179296,#179297,#179298,#179299,#179300,#179301,#179302,#179303,#179304,
#179305,#179306,#179307,#179308,#179309,#179310,#179311,#179312,#179313,
#179314,#179315,#179316,#179317,#179318,#179319,#179320,#179321,#179322,
#179323,#179324,#179325,#179326,#179327,#179328,#179329,#179330,#179331,
#179332,#179333,#179334,#179335,#179336,#179337,#179338,#179339,#179340,
#179341,#179342,#179343,#179344,#179345,#179346,#179347,#179348,#179349,
#179350,#179351,#179352,#179353,#179354,#179355,#179356,#179357,#179358,
#179359,#179360,#179361,#179362,#179363,#179364,#179365,#179366,#179367,
#179368,#179369,#179370,#179371,#179372,#179373),.UNSPECIFIED.,.F.,.F.,
(4,2,2,2,2,2,2,2,2,2,2,2,2,2,2,2,2,2,2,2,2,2,2,2,2,2,2,2,2,2,2,2,2,2,2,
2,2,2,2,2,4),(15.9563811041735,15.9737975928771,16.188144625583,16.4403174813183,
16.6990099245498,16.9507148240286,17.2074066749168,17.4259263304847,17.6367507053452,
17.8957326470844,18.0212038054511,18.2460623414005,18.436300514819,18.6585432543082,
18.8698740658398,19.0932433887016,19.286315914036,19.5142197774173,19.6388520817395,
19.8986455059131,20.0628063040985,20.2809247137134,20.4746673369814,20.6873209945832,
20.8803418454722,21.0898020808175,21.2889726415437,21.4941317239042,21.7182599168424,
21.9192434783725,22.173550582982,22.2982001664574,22.5570948821,22.8158110382015,
22.9431610993941,23.1412950840882,23.3935731392472,23.5807736260057,23.724556486473,
23.9421164922607,24.1619673706865),.UNSPECIFIED.);
#30263=B_SPLINE_CURVE_WITH_KNOTS('',3,(#179377,#179378,#179379,#179380,
#179381,#179382,#179383,#179384,#179385,#179386,#179387,#179388,#179389,
#179390,#179391,#179392),.UNSPECIFIED.,.F.,.F.,(4,2,2,2,2,2,2,4),(-5.3403698058518,
-5.10302024972618,-4.85331064876673,-4.3722544378929,-3.88453013965518,
-3.63186010165686,-3.38655743613479,-3.33078402932654),.UNSPECIFIED.);
#30264=B_SPLINE_CURVE_WITH_KNOTS('',3,(#179396,#179397,#179398,#179399,
#179400,#179401,#179402,#179403,#179404,#179405,#179406,#179407,#179408,
#179409,#179410,#179411,#179412,#179413,#179414,#179415,#179416,#179417),
 .UNSPECIFIED.,.F.,.F.,(4,2,2,2,2,2,2,2,2,2,4),(-3.33078402932654,-3.14577878108155,
-2.6696933689128,-2.42517438026941,-2.18777430397266,-1.69235110044299,
-1.45012215009031,-1.21210349138623,-0.975414798478184,-0.488398210557989,
-4.75981067121614E-5),.UNSPECIFIED.);
#30265=B_SPLINE_CURVE_WITH_KNOTS('',3,(#179419,#179420,#179421,#179422,
#179423,#179424,#179425,#179426,#179427,#179428,#179429,#179430,#179431,
#179432,#179433,#179434,#179435,#179436,#179437,#179438,#179439,#179440,
#179441,#179442,#179443,#179444,#179445,#179446,#179447,#179448,#179449,
#179450,#179451,#179452,#179453,#179454,#179455,#179456,#179457,#179458,
#179459,#179460,#179461,#179462,#179463,#179464,#179465,#179466,#179467,
#179468,#179469,#179470,#179471,#179472,#179473,#179474,#179475,#179476,
#179477,#179478,#179479,#179480,#179481,#179482,#179483,#179484,#179485),
 .UNSPECIFIED.,.F.,.F.,(4,3,3,3,3,3,3,3,3,3,3,3,3,3,3,3,3,3,3,3,3,3,4),
(0.,0.0532797188796114,0.106117363864123,0.125,0.176897081798127,0.229324525544369,
0.25,0.301861332022725,0.353569755832101,0.405192326669166,0.456691995603618,
0.499999999999999,0.551296718367494,0.602946326486467,0.654794611099575,
0.706987743443309,0.749999999999998,0.803309497918933,0.856238158518513,
0.874999999999999,0.929869764525177,0.984191399200626,0.999999665677158),
 .UNSPECIFIED.);
#30266=B_SPLINE_CURVE_WITH_KNOTS('',3,(#179487,#179488,#179489,#179490,
#179491,#179492,#179493,#179494,#179495,#179496),.UNSPECIFIED.,.F.,.F.,
(4,2,2,2,4),(-1.36676107014535,-1.02924695186405,-0.680886324591822,-0.34453153614729,
-6.48039110316922E-5),.UNSPECIFIED.);
#30267=B_SPLINE_CURVE_WITH_KNOTS('',3,(#179497,#179498,#179499,#179500),
 .UNSPECIFIED.,.F.,.F.,(4,4),(-0.000734763449235485,0.),.UNSPECIFIED.);
#30268=B_SPLINE_CURVE_WITH_KNOTS('',3,(#179750,#179751,#179752,#179753,
#179754,#179755,#179756,#179757,#179758,#179759,#179760,#179761,#179762,
#179763,#179764,#179765,#179766,#179767,#179768,#179769,#179770,#179771,
#179772,#179773,#179774,#179775,#179776,#179777,#179778,#179779,#179780,
#179781,#179782,#179783,#179784,#179785,#179786,#179787,#179788,#179789,
#179790,#179791,#179792,#179793,#179794,#179795,#179796,#179797,#179798,
#179799,#179800,#179801,#179802,#179803,#179804,#179805,#179806,#179807,
#179808,#179809,#179810,#179811,#179812,#179813,#179814,#179815,#179816,
#179817,#179818,#179819,#179820,#179821,#179822,#179823,#179824,#179825,
#179826,#179827,#179828,#179829,#179830,#179831,#179832,#179833,#179834,
#179835,#179836,#179837,#179838,#179839,#179840,#179841,#179842,#179843,
#179844,#179845,#179846,#179847,#179848,#179849,#179850,#179851,#179852,
#179853,#179854,#179855,#179856,#179857,#179858,#179859,#179860,#179861,
#179862,#179863,#179864,#179865,#179866,#179867,#179868,#179869,#179870,
#179871,#179872,#179873,#179874,#179875,#179876,#179877,#179878,#179879,
#179880,#179881,#179882,#179883,#179884,#179885,#179886,#179887,#179888,
#179889,#179890,#179891,#179892,#179893,#179894,#179895,#179896,#179897,
#179898,#179899,#179900,#179901,#179902,#179903,#179904,#179905,#179906,
#179907,#179908,#179909,#179910,#179911,#179912,#179913,#179914,#179915,
#179916,#179917,#179918,#179919,#179920,#179921,#179922,#179923,#179924,
#179925,#179926,#179927,#179928,#179929,#179930,#179931,#179932,#179933,
#179934,#179935,#179936,#179937,#179938,#179939,#179940,#179941,#179942,
#179943,#179944,#179945,#179946,#179947,#179948,#179949,#179950,#179951,
#179952,#179953,#179954,#179955,#179956,#179957,#179958,#179959,#179960,
#179961,#179962,#179963,#179964,#179965,#179966,#179967,#179968,#179969,
#179970,#179971,#179972,#179973,#179974,#179975,#179976,#179977,#179978,
#179979,#179980,#179981,#179982,#179983,#179984,#179985,#179986,#179987,
#179988,#179989,#179990,#179991,#179992,#179993,#179994,#179995,#179996,
#179997,#179998,#179999,#180000,#180001,#180002,#180003,#180004,#180005,
#180006,#180007,#180008,#180009,#180010,#180011,#180012,#180013,#180014,
#180015),.UNSPECIFIED.,.F.,.F.,(4,2,2,2,2,2,2,2,2,2,2,2,2,2,2,2,2,2,2,2,
2,2,2,2,2,2,2,2,2,2,2,2,2,2,2,2,2,2,2,2,2,2,2,2,2,2,2,2,2,2,2,2,2,2,2,2,
2,2,2,2,2,2,2,2,2,2,2,2,2,2,2,2,2,2,2,2,2,2,2,2,2,2,2,2,2,2,2,2,2,2,2,2,
2,2,2,2,2,2,2,2,2,2,2,2,2,2,2,2,2,2,2,2,2,2,2,2,2,2,2,2,2,2,2,2,2,2,2,2,
2,2,2,2,4),(0.00790828593611698,0.135265930291889,0.267467597358619,0.533750940167357,
0.88017574947923,1.13384054666904,1.41070844498502,1.59304811912023,1.75172514557715,
1.94683197777222,2.11230898000431,2.2183789781365,2.42776377877795,2.62555120627117,
2.76879848422111,2.84874922368211,2.95782682962964,3.14207307762776,3.25663406363165,
3.37303424343138,3.45626456111032,3.52892374114935,3.6857389432425,3.80006939109491,
3.88555748851367,4.03204550791092,4.10568247069694,4.17075352363226,4.33697990742952,
4.47525429526118,4.54231004104649,4.69175162177885,4.75810401002136,4.81934676172847,
4.98088188776317,5.06503890354536,5.1321151904307,5.30211693017162,5.38412488189451,
5.44913617798401,5.62479169811705,5.69791337660177,5.76286233196133,5.91136026020286,
6.04925408777556,6.11298181775794,6.23610551115398,6.31388054876702,6.38380024863477,
6.5432048593396,6.65174213941674,6.73361681103904,6.84908481495156,6.96566430926586,
7.06231774977973,7.25739291090475,7.36935564096079,7.49481348313,7.61574875549503,
7.85194025684748,7.97321502503676,8.08120256050554,8.19960850771165,8.51294062655963,
8.65864759138126,8.89994724302448,9.15209692020237,9.39092942283465,9.8907051436538,
10.1408102616569,10.5878990435705,10.6957027295127,10.9247285148082,11.1721695044457,
11.3026464814219,11.4127050574303,11.5387697472141,11.7749710961387,11.8944602329429,
12.0206170420862,12.1515274285258,12.3960230599727,12.488159385815,12.6185402384999,
12.6893810027722,12.8337840499673,13.0004068655612,13.0719250791122,13.1514270639328,
13.2900322788783,13.360499232878,13.4504930252814,13.6181564670971,13.6835742421503,
13.7534366573758,13.9354223495435,14.0011227284056,14.0851924898259,14.2451036661492,
14.3093382614856,14.3835463997154,14.5778804557065,14.6416178904133,14.7210686769463,
14.8716856282844,14.940114896237,15.0236871260087,15.2210857305321,15.2872921270163,
15.3680758518447,15.5054362572902,15.590558560566,15.7067094494271,15.8567404575721,
15.9290430710459,16.035996173057,16.1380191692964,16.2541464373657,16.4511595599156,
16.5500800259854,16.6242233687588,16.6963137053059,16.8009540412491,16.9203081431285,
17.1808011324626,17.282359025085,17.4399399592422,17.6184937765128,17.8672726158994,
17.9911861104215,18.2371444098655,18.5095375574028,18.789319718825),
 .UNSPECIFIED.);
#30269=B_SPLINE_CURVE_WITH_KNOTS('',3,(#180157,#180158,#180159,#180160,
#180161,#180162,#180163,#180164,#180165,#180166,#180167,#180168,#180169,
#180170,#180171,#180172,#180173,#180174,#180175,#180176,#180177,#180178,
#180179,#180180,#180181,#180182,#180183,#180184,#180185,#180186,#180187,
#180188,#180189,#180190,#180191,#180192,#180193,#180194,#180195,#180196,
#180197,#180198,#180199,#180200,#180201,#180202,#180203,#180204,#180205,
#180206,#180207,#180208,#180209,#180210,#180211,#180212,#180213,#180214,
#180215,#180216,#180217,#180218,#180219,#180220,#180221,#180222,#180223,
#180224,#180225,#180226,#180227,#180228,#180229,#180230,#180231,#180232,
#180233,#180234,#180235,#180236,#180237,#180238),.UNSPECIFIED.,.F.,.F.,
(4,2,2,2,2,2,2,2,2,2,2,2,2,2,2,2,2,2,2,2,2,2,2,2,2,2,2,2,2,2,2,2,2,2,2,
2,2,2,2,2,4),(-14.2732703758709,-13.8912273375201,-13.6142499111422,-13.3975932236668,
-13.1227155431991,-12.7070233843363,-12.382403721312,-12.1293949735596,
-11.8703642014538,-11.535385037698,-11.1414389160712,-10.8461410004354,
-10.5760851451155,-10.229212584883,-9.73704557040598,-9.39335342116224,
-9.12378600302777,-8.81489519474117,-8.39716574472202,-8.04541518662001,
-7.77721020461666,-7.50917494410743,-7.15370825665347,-6.694616193426,-6.35436303692717,
-6.06376512693916,-5.68296158713199,-5.09892163723771,-4.68369409175826,
-4.35935666716764,-4.01204603446286,-3.53687730816414,-3.0882622443312,
-2.75857559247952,-2.45520533882133,-2.06641699455647,-1.51781117593839,
-1.13911402161754,-0.846466340153964,-0.481778164862173,-7.79037809220391E-5),
 .UNSPECIFIED.);
#30270=B_SPLINE_CURVE_WITH_KNOTS('',3,(#180507,#180508,#180509,#180510,
#180511,#180512),.UNSPECIFIED.,.F.,.F.,(4,2,4),(-0.0902565102820884,-0.0451906624768086,
-0.000194550672140855),.UNSPECIFIED.);
#30271=B_SPLINE_CURVE_WITH_KNOTS('',3,(#180534,#180535,#180536,#180537,
#180538,#180539,#180540,#180541,#180542,#180543,#180544,#180545,#180546,
#180547,#180548,#180549,#180550,#180551,#180552,#180553,#180554,#180555,
#180556,#180557,#180558,#180559,#180560,#180561,#180562,#180563,#180564,
#180565,#180566,#180567,#180568,#180569,#180570,#180571,#180572,#180573,
#180574,#180575,#180576,#180577,#180578,#180579,#180580,#180581,#180582,
#180583,#180584,#180585,#180586,#180587,#180588,#180589,#180590,#180591),
 .UNSPECIFIED.,.F.,.F.,(4,3,3,3,3,3,3,3,3,3,3,3,3,3,3,3,3,3,3,4),(-1.28896142244996,
-1.09309231306789,-1.04016081898117,-0.980183490937908,-0.885023600722137,
-0.791562904177703,-0.670254571147595,-0.644748735286477,-0.63409310387645,
-0.626279232155984,-0.469588976339915,-0.352102611119142,-0.310009489205054,
-0.249406568724682,-0.188707985000504,-0.175752395276352,-0.142257802210724,
-0.0813352071390198,-0.0211767799124928,-1.50340975617814E-6),
 .UNSPECIFIED.);
#30272=B_SPLINE_CURVE_WITH_KNOTS('',3,(#180616,#180617,#180618,#180619,
#180620,#180621,#180622,#180623,#180624,#180625,#180626,#180627,#180628,
#180629,#180630,#180631,#180632,#180633,#180634,#180635,#180636,#180637,
#180638,#180639,#180640,#180641,#180642,#180643,#180644,#180645,#180646,
#180647,#180648,#180649,#180650,#180651,#180652,#180653,#180654,#180655,
#180656,#180657,#180658,#180659,#180660,#180661,#180662,#180663,#180664,
#180665,#180666,#180667,#180668,#180669,#180670,#180671,#180672,#180673),
 .UNSPECIFIED.,.F.,.F.,(4,3,3,3,3,3,3,3,3,3,3,3,3,3,3,3,3,3,3,4),(0.000196331256314133,
0.195854367371089,0.245817836587428,0.308742496769599,0.403496982746037,
0.491306783782198,0.608890768221054,0.644062191156574,0.654689003663857,
0.65473511082066,0.81371042122958,0.932829188307031,0.979410739452192,1.03972898457711,
1.10013481239701,1.11172797209075,1.14748205288075,1.20898204679883,1.26971077107247,
1.29001475424187),.UNSPECIFIED.);
#30273=B_SPLINE_CURVE_WITH_KNOTS('',3,(#180694,#180695,#180696,#180697,
#180698,#180699),.UNSPECIFIED.,.F.,.F.,(4,2,4),(-0.0900560308119693,-0.0451018328691558,
-1.01924371514621E-5),.UNSPECIFIED.);
#30274=B_SPLINE_CURVE_WITH_KNOTS('',3,(#181128,#181129,#181130,#181131,
#181132,#181133,#181134,#181135,#181136,#181137,#181138,#181139,#181140,
#181141,#181142,#181143,#181144,#181145,#181146,#181147,#181148,#181149,
#181150,#181151,#181152,#181153,#181154,#181155,#181156,#181157,#181158,
#181159,#181160,#181161,#181162,#181163,#181164,#181165,#181166,#181167,
#181168,#181169,#181170,#181171,#181172,#181173,#181174,#181175,#181176,
#181177,#181178,#181179,#181180,#181181,#181182,#181183,#181184,#181185,
#181186,#181187,#181188,#181189,#181190,#181191,#181192,#181193,#181194,
#181195,#181196,#181197,#181198,#181199,#181200,#181201,#181202,#181203,
#181204,#181205,#181206,#181207,#181208,#181209,#181210,#181211,#181212,
#181213,#181214,#181215,#181216,#181217,#181218,#181219,#181220,#181221,
#181222,#181223,#181224,#181225,#181226,#181227,#181228,#181229,#181230,
#181231,#181232,#181233,#181234,#181235,#181236,#181237),.UNSPECIFIED.,
 .F.,.F.,(4,2,2,2,2,2,2,2,2,2,2,2,2,2,2,2,2,2,2,2,2,2,2,2,2,2,2,2,2,2,2,
2,2,2,2,2,2,2,2,2,2,2,2,2,2,2,2,2,2,2,2,2,2,2,4),(-2.0374264169892,-2.03325723873566,
-2.01852518698755,-1.98019546730744,-1.89910957670444,-1.8473559268582,
-1.82181501438801,-1.8000221301294,-1.77132035516003,-1.73779453405823,
-1.65621553961038,-1.62324600384763,-1.60802171249166,-1.59508722455329,
-1.57328737753901,-1.54369621600048,-1.43275430172482,-1.40641781973598,
-1.3848882552916,-1.35742036745476,-1.2746876774316,-1.19931109475228,-1.18126032660081,
-1.16953462805175,-1.15525014334195,-1.12077741049727,-1.05645337488967,
-0.986844591638145,-0.96000395932419,-0.938279265882365,-0.911240690812327,
-0.880604952539318,-0.816126256851267,-0.76177602608691,-0.745553142489823,
-0.733025997958031,-0.713891980393471,-0.689464491039709,-0.623696595424254,
-0.566646952663267,-0.540885267446727,-0.519111084586999,-0.490775715375377,
-0.413973876129471,-0.333776908151955,-0.316301768502787,-0.304639059444405,
-0.290026744158241,-0.252788348082332,-0.176955717799064,-0.119916186580509,
-0.093942455038947,-0.0721880153941974,-0.0510648498280456,-0.000149360373092413),
 .UNSPECIFIED.);
#30275=B_SPLINE_CURVE_WITH_KNOTS('',3,(#181240,#181241,#181242,#181243,
#181244,#181245,#181246,#181247,#181248,#181249,#181250,#181251,#181252,
#181253,#181254,#181255,#181256,#181257,#181258,#181259,#181260,#181261,
#181262,#181263,#181264,#181265,#181266,#181267,#181268,#181269,#181270,
#181271,#181272,#181273,#181274,#181275,#181276,#181277,#181278,#181279,
#181280,#181281,#181282,#181283,#181284,#181285,#181286,#181287,#181288,
#181289,#181290,#181291,#181292,#181293,#181294,#181295,#181296,#181297,
#181298,#181299,#181300,#181301,#181302,#181303,#181304,#181305,#181306,
#181307,#181308,#181309,#181310,#181311,#181312,#181313,#181314,#181315),
 .UNSPECIFIED.,.F.,.F.,(4,2,2,2,2,2,2,2,2,2,2,2,2,2,2,2,2,2,2,2,2,2,2,2,
2,2,2,2,2,2,2,2,2,2,2,2,2,4),(-11.0420177746592,-10.9599397421387,-10.9398938962619,
-10.923237123713,-10.9106052415203,-10.8947670479531,-10.8078828554248,
-10.7438996772105,-10.718208157378,-10.6964285618455,-10.6684886275246,
-10.5730160503389,-10.5086930824629,-10.4924060260972,-10.4808258283884,
-10.4656213586583,-10.4259108932372,-10.3590662985945,-10.2972473633837,
-10.2713228294197,-10.2495656322461,-10.2219108414823,-10.1537182957188,
-10.1005077442629,-10.0783068470237,-10.0604069299075,-10.0478241035653,
-10.0302281109333,-9.95833483875728,-9.88365573874688,-9.85656659541233,
-9.83484229672353,-9.80805159221074,-9.741502251406,-9.67479042103899,-9.63969737588758,
-9.6253365275997,-9.62176322384599),.UNSPECIFIED.);
#30276=B_SPLINE_CURVE_WITH_KNOTS('',3,(#181320,#181321,#181322,#181323,
#181324,#181325,#181326,#181327,#181328,#181329,#181330,#181331,#181332,
#181333,#181334,#181335,#181336,#181337,#181338,#181339,#181340,#181341,
#181342,#181343,#181344,#181345,#181346,#181347,#181348,#181349,#181350,
#181351,#181352,#181353,#181354,#181355,#181356,#181357,#181358,#181359,
#181360,#181361,#181362,#181363,#181364,#181365,#181366,#181367,#181368,
#181369,#181370,#181371,#181372,#181373,#181374,#181375,#181376,#181377,
#181378,#181379,#181380,#181381,#181382,#181383,#181384,#181385,#181386,
#181387,#181388,#181389,#181390,#181391,#181392,#181393,#181394,#181395,
#181396,#181397,#181398,#181399,#181400,#181401,#181402,#181403,#181404,
#181405,#181406,#181407,#181408,#181409,#181410,#181411,#181412,#181413,
#181414,#181415,#181416,#181417,#181418,#181419,#181420,#181421,#181422,
#181423,#181424,#181425,#181426,#181427,#181428,#181429,#181430,#181431,
#181432,#181433,#181434,#181435,#181436,#181437,#181438,#181439,#181440,
#181441,#181442,#181443,#181444,#181445,#181446,#181447,#181448,#181449,
#181450,#181451,#181452,#181453,#181454,#181455,#181456,#181457,#181458,
#181459,#181460,#181461,#181462,#181463,#181464,#181465,#181466,#181467,
#181468,#181469,#181470,#181471,#181472,#181473,#181474,#181475,#181476,
#181477,#181478,#181479,#181480,#181481,#181482,#181483,#181484,#181485,
#181486,#181487,#181488,#181489,#181490,#181491,#181492,#181493,#181494,
#181495,#181496,#181497,#181498,#181499,#181500,#181501),.UNSPECIFIED.,
 .F.,.F.,(4,2,2,2,2,2,2,2,2,2,2,2,2,2,2,2,2,2,2,2,2,2,2,2,2,2,2,2,2,2,2,
2,2,2,2,2,2,2,2,2,2,2,2,2,2,2,2,2,2,2,2,2,2,2,2,2,2,2,2,2,2,2,2,2,2,2,2,
2,2,2,2,2,2,2,2,2,2,2,2,2,2,2,2,2,2,2,2,2,2,2,4),(-5.49514095832648,-5.49479992473117,
-5.4820584180547,-5.45783766717952,-5.32910650724132,-5.29327873109851,
-5.27057092541286,-5.24752547378678,-5.20900193213987,-5.15508416570214,
-5.08711236100685,-5.06926421126503,-5.05668133832967,-5.03903409214227,
-4.97994615985857,-4.89316178777948,-4.86585298026823,-4.84412509360188,
-4.8175347032467,-4.74555196018678,-4.6567371781831,-4.63879628292061,-4.62708350973762,
-4.61274018657622,-4.57779243715063,-4.51164856045253,-4.44461999984613,
-4.41773445466564,-4.39600985688239,-4.36901756354521,-4.29343048511146,
-4.22225763360175,-4.20461264184201,-4.19202980445917,-4.1741794951694,
-4.15206701369583,-4.09929898265307,-4.03042520549459,-4.00278967559688,
-3.98103278125623,-3.95509190484458,-3.89308759144006,-3.82620275634084,
-3.78665450219168,-3.77148423019889,-3.7599021211164,-3.74357271272327,
-3.6768433017597,-3.58444871147446,-3.55629077886608,-3.53449449496795,
-3.50895308800941,-3.44738813407108,-3.37754034248968,-3.34859811288362,
-3.33456473684734,-3.32095844719234,-3.29475388264289,-3.25528548292294,
-3.16310634592479,-3.1362527942936,-3.1145276481891,-3.08750362661562,-3.05726646565273,
-2.9971538208965,-2.92816109205382,-2.91012982645738,-2.89840655169761,
-2.88411199446826,-2.84955770748755,-2.78492463024832,-2.71575655695739,
-2.68890888665255,-2.66718444560362,-2.64015373933234,-2.62408225637449,
-2.6010943112649,-2.51599344191209,-2.48792465828078,-2.47261609198703,
-2.45971084992899,-2.43812581613357,-2.4089703937702,-2.30143419560341,
-2.2738713464661,-2.25211855318578,-2.22612269040889,-2.16343062428365,
-2.0621869162582,-2.04490192589283,-2.0374264169892),.UNSPECIFIED.);
#30277=B_SPLINE_CURVE_WITH_KNOTS('',3,(#181502,#181503,#181504,#181505,
#181506,#181507,#181508,#181509,#181510,#181511,#181512,#181513,#181514,
#181515,#181516,#181517,#181518,#181519,#181520,#181521,#181522,#181523,
#181524,#181525,#181526,#181527,#181528,#181529,#181530,#181531,#181532,
#181533,#181534,#181535,#181536,#181537,#181538,#181539,#181540,#181541,
#181542,#181543,#181544,#181545,#181546,#181547,#181548,#181549,#181550,
#181551,#181552,#181553,#181554,#181555,#181556,#181557,#181558,#181559,
#181560,#181561,#181562,#181563,#181564,#181565,#181566,#181567,#181568,
#181569,#181570,#181571,#181572,#181573,#181574,#181575,#181576,#181577,
#181578,#181579,#181580,#181581,#181582,#181583,#181584,#181585,#181586,
#181587,#181588,#181589,#181590,#181591,#181592,#181593,#181594,#181595,
#181596,#181597,#181598,#181599,#181600,#181601,#181602,#181603,#181604,
#181605,#181606,#181607,#181608,#181609,#181610,#181611,#181612,#181613,
#181614,#181615,#181616,#181617,#181618,#181619,#181620,#181621,#181622,
#181623,#181624,#181625,#181626,#181627,#181628,#181629,#181630,#181631,
#181632,#181633,#181634,#181635,#181636,#181637,#181638,#181639,#181640,
#181641,#181642,#181643,#181644,#181645,#181646,#181647,#181648,#181649,
#181650,#181651,#181652,#181653,#181654,#181655,#181656,#181657,#181658,
#181659,#181660,#181661,#181662,#181663,#181664,#181665,#181666,#181667,
#181668,#181669,#181670,#181671,#181672,#181673,#181674,#181675,#181676,
#181677,#181678,#181679),.UNSPECIFIED.,.F.,.F.,(4,2,2,2,2,2,2,2,2,2,2,2,
2,2,2,2,2,2,2,2,2,2,2,2,2,2,2,2,2,2,2,2,2,2,2,2,2,2,2,2,2,2,2,2,2,2,2,2,
2,2,2,2,2,2,2,2,2,2,2,2,2,2,2,2,2,2,2,2,2,2,2,2,2,2,2,2,2,2,2,2,2,2,2,2,
2,2,2,2,4),(-9.62176322384599,-9.61362793664136,-9.59572068391397,-9.51842556037379,
-9.43864125932449,-9.41068969274724,-9.3889379954071,-9.36289536573885,
-9.29603888750942,-9.21996859001137,-9.1990239946575,-9.18620176302793,
-9.17061958148039,-9.13357698038007,-9.0557120872312,-9.02273687179219,
-8.9943474525171,-8.97257599227928,-8.94683145156729,-8.89339699252227,
-8.81415845666444,-8.77620113787093,-8.76150967376524,-8.74985971603038,
-8.73251307255491,-8.6388488468192,-8.57001675505747,-8.54359818107113,
-8.52186669522419,-8.49436302458913,-8.41214561447724,-8.36754232123613,
-8.34719712953825,-8.33036481139516,-8.3177486818033,-8.30208368864063,
-8.2570642930598,-8.18778763062589,-8.15624359064142,-8.12867597788388,
-8.10694230403665,-8.08057669381003,-8.01636404010515,-7.94695688957519,
-7.91119382815484,-7.89675209882627,-7.88505957115733,-7.86729663388556,
-7.77608614635548,-7.7058864190148,-7.67938958125659,-7.65765989890923,
-7.63024603986514,-7.54551338030752,-7.48324689940725,-7.46622800531952,
-7.45362464997324,-7.43813235833985,-7.35698949434093,-7.29194643889332,
-7.2643374505598,-7.24260214694485,-7.21627009228013,-7.15987645830453,
-7.0843738374995,-7.04720640187818,-7.03260202344148,-7.02093811517747,
-7.00345032242073,-6.91062255393296,-6.84132138876095,-6.81487464097661,
-6.79314319744251,-6.76567040428183,-6.6824952859288,-6.62038536131578,
-6.60266652125036,-6.59008399296299,-6.57230887829423,-6.50314991168874,
-6.44984717547513,-6.41157111664384,-6.38856109819059,-6.36582284170627,
-6.32979323434818,-6.22610083519746,-6.1840247938677,-6.16892022716619,
-6.16419090700929),.UNSPECIFIED.);
#30278=B_SPLINE_CURVE_WITH_KNOTS('',3,(#181684,#181685,#181686,#181687,
#181688,#181689,#181690,#181691,#181692,#181693,#181694,#181695,#181696,
#181697,#181698,#181699,#181700,#181701,#181702,#181703,#181704,#181705,
#181706,#181707,#181708,#181709,#181710,#181711,#181712,#181713,#181714,
#181715,#181716,#181717,#181718,#181719,#181720,#181721,#181722,#181723,
#181724,#181725,#181726,#181727,#181728,#181729,#181730,#181731,#181732,
#181733,#181734,#181735,#181736,#181737,#181738,#181739,#181740,#181741,
#181742,#181743,#181744,#181745,#181746,#181747,#181748,#181749,#181750,
#181751,#181752,#181753,#181754,#181755,#181756,#181757,#181758,#181759,
#181760,#181761,#181762,#181763,#181764,#181765,#181766,#181767,#181768,
#181769,#181770,#181771,#181772,#181773,#181774,#181775,#181776,#181777,
#181778,#181779,#181780,#181781,#181782,#181783,#181784,#181785,#181786,
#181787,#181788,#181789,#181790,#181791,#181792,#181793,#181794,#181795,
#181796,#181797,#181798,#181799,#181800,#181801,#181802,#181803,#181804,
#181805,#181806,#181807,#181808,#181809,#181810,#181811,#181812,#181813,
#181814,#181815,#181816,#181817,#181818,#181819,#181820,#181821,#181822,
#181823,#181824,#181825,#181826,#181827,#181828,#181829,#181830,#181831,
#181832,#181833,#181834,#181835,#181836,#181837,#181838,#181839,#181840,
#181841,#181842,#181843,#181844,#181845,#181846,#181847,#181848,#181849,
#181850,#181851,#181852,#181853,#181854,#181855,#181856,#181857,#181858,
#181859,#181860,#181861,#181862,#181863),.UNSPECIFIED.,.F.,.F.,(4,2,2,2,
2,2,2,2,2,2,2,2,2,2,2,2,2,2,2,2,2,2,2,2,2,2,2,2,2,2,2,2,2,2,2,2,2,2,2,2,
2,2,2,2,2,2,2,2,2,2,2,2,2,2,2,2,2,2,2,2,2,2,2,2,2,2,2,2,2,2,2,2,2,2,2,2,
2,2,2,2,2,2,2,2,2,2,2,2,2,4),(-8.95293752943051,-8.94466494354158,-8.92662197800537,
-8.85140677799895,-8.76782829419565,-8.74060822603189,-8.71888012097177,
-8.69221316947022,-8.59829581946537,-8.55954665453933,-8.53363450953526,
-8.52007436829822,-8.50598418094776,-8.47666325842438,-8.40693709867059,
-8.34573803375985,-8.3202210493761,-8.29842109397278,-8.27022466722885,
-8.17852621903307,-8.11350566802394,-8.09609202761019,-8.08443504838779,
-8.06978400359294,-8.03557577626809,-7.9677493481306,-7.90077116864638,
-7.87446608172774,-7.85272892927623,-7.82508518180479,-7.74631650503349,
-7.67782123813631,-7.66117979312411,-7.64854509816135,-7.63268837932748,
-7.54589169709742,-7.49549495842685,-7.46452090650524,-7.44250916966715,
-7.41810679218684,-7.3705817815995,-7.28285829705504,-7.24327831287026,
-7.22841471876788,-7.21678624917497,-7.19969685725232,-7.11505580885114,
-7.06299158652229,-7.02447733489016,-7.00136172911433,-6.97871046342424,
-6.94294481590786,-6.85516535904935,-6.82460801210217,-6.80233839225203,
-6.78933775608357,-6.77428575018232,-6.74244047489071,-6.65967307752173,
-6.62598048187553,-6.59718374005725,-6.57538301579716,-6.54989939096632,
-6.4985783186988,-6.41697460141405,-6.37854004035094,-6.36379609332515,
-6.35215234412663,-6.33488366309922,-6.24073183913631,-6.17215875911867,
-6.14575354115085,-6.12401954842903,-6.09649473247129,-6.014824666104,-5.96989123714106,
-5.949468300581,-5.93259009325537,-5.91997627037338,-5.90435207184409,-5.81614839584029,
-5.76634897365184,-5.73548326381252,-5.71348384115434,-5.68903794321173,
-5.64117931219174,-5.5538610027468,-5.52634787091137,-5.50572248954911,
-5.49514095832648),.UNSPECIFIED.);
#30279=B_SPLINE_CURVE_WITH_KNOTS('',3,(#181864,#181865,#181866,#181867,
#181868,#181869,#181870,#181871,#181872,#181873,#181874,#181875,#181876,
#181877,#181878,#181879,#181880,#181881,#181882,#181883,#181884,#181885,
#181886,#181887,#181888,#181889,#181890,#181891,#181892,#181893,#181894,
#181895,#181896,#181897,#181898,#181899,#181900,#181901,#181902,#181903,
#181904,#181905,#181906,#181907,#181908,#181909,#181910,#181911,#181912,
#181913,#181914,#181915,#181916,#181917,#181918,#181919,#181920,#181921,
#181922,#181923,#181924,#181925,#181926,#181927,#181928,#181929,#181930,
#181931,#181932,#181933,#181934,#181935,#181936,#181937,#181938,#181939,
#181940,#181941,#181942,#181943,#181944,#181945,#181946,#181947,#181948,
#181949,#181950,#181951,#181952,#181953,#181954,#181955,#181956,#181957,
#181958,#181959,#181960,#181961,#181962,#181963,#181964,#181965,#181966,
#181967,#181968,#181969,#181970,#181971,#181972,#181973,#181974,#181975,
#181976,#181977,#181978,#181979,#181980,#181981,#181982,#181983,#181984,
#181985,#181986,#181987,#181988,#181989,#181990,#181991,#181992,#181993,
#181994,#181995,#181996,#181997,#181998,#181999,#182000,#182001,#182002,
#182003,#182004,#182005,#182006,#182007,#182008,#182009,#182010,#182011,
#182012,#182013,#182014,#182015,#182016,#182017,#182018,#182019,#182020,
#182021,#182022,#182023,#182024,#182025,#182026,#182027,#182028,#182029,
#182030,#182031,#182032,#182033,#182034,#182035,#182036,#182037,#182038,
#182039,#182040,#182041),.UNSPECIFIED.,.F.,.F.,(4,2,2,2,2,2,2,2,2,2,2,2,
2,2,2,2,2,2,2,2,2,2,2,2,2,2,2,2,2,2,2,2,2,2,2,2,2,2,2,2,2,2,2,2,2,2,2,2,
2,2,2,2,2,2,2,2,2,2,2,2,2,2,2,2,2,2,2,2,2,2,2,2,2,2,2,2,2,2,2,2,2,2,2,2,
2,2,2,2,4),(-6.16419090700929,-6.15731653447364,-6.14056411527924,-6.05198636916046,
-6.00171152973909,-5.96400099653716,-5.94100788492888,-5.91825471481642,
-5.88177258492111,-5.79423701631445,-5.76426476526426,-5.74227876310545,
-5.729318475769,-5.71416447629465,-5.68167403647096,-5.59960405095324,-5.57696442385519,
-5.5432407280318,-5.52087753886471,-5.49733579815858,-5.45596877366023,
-5.39706516156768,-5.32593660424819,-5.30797910093004,-5.29626443354325,
-5.28193019596578,-5.24705607251649,-5.18119784704434,-5.11376429792051,
-5.08688666352897,-5.06516213418457,-5.03816192426049,-4.96406673182427,
-4.8911901173433,-4.87533543247579,-4.86270167510026,-4.84606012737471,
-4.78147443569736,-4.6983674121006,-4.6708938077729,-4.64916272843381,-4.62271754523909,
-4.55344583906296,-4.46054973531814,-4.44307173244349,-4.43140896996955,
-4.41679899584926,-4.37957931765812,-4.30383060078425,-4.24703356049772,
-4.22094740206581,-4.1994093214977,-4.17162085822899,-4.10513259025917,
-4.02543486564442,-4.00867574916312,-3.99607562882306,-3.97758032318802,
-3.92190701584802,-3.83312939794508,-3.80596068411184,-3.78423510539483,
-3.75751770667088,-3.6826934328211,-3.59484351663941,-3.57798109323278,
-3.56637050500942,-3.55134849971937,-3.51015111117681,-3.41254225725811,
-3.37251827322652,-3.34917679648139,-3.32669312229479,-3.29209838160418,
-3.24721117712543,-3.1596699041009,-3.14330180894059,-3.13063545158538,
-3.11115330335491,-3.08608005778132,-3.01605958134592,-2.96332610827766,
-2.93796238003775,-2.91614401066078,-2.88720122760286,-2.81504547153266,
-2.73079590200839,-2.71376506241483,-2.70657200810638),.UNSPECIFIED.);
#30280=B_SPLINE_CURVE_WITH_KNOTS('',3,(#182046,#182047,#182048,#182049,
#182050,#182051,#182052,#182053,#182054,#182055,#182056,#182057,#182058,
#182059,#182060,#182061,#182062,#182063),.UNSPECIFIED.,.F.,.F.,(4,2,2,2,
2,2,2,2,4),(3.80158966705551,3.91441070971229,4.3189896343053,4.69887283496923,
5.04702075342428,5.38197377559302,5.74008106147176,5.97805601036782,6.26584118659148),
 .UNSPECIFIED.);
#30281=B_SPLINE_CURVE_WITH_KNOTS('',3,(#182070,#182071,#182072,#182073,
#182074,#182075,#182076,#182077,#182078,#182079,#182080,#182081,#182082,
#182083,#182084,#182085,#182086,#182087,#182088,#182089,#182090,#182091,
#182092,#182093,#182094,#182095,#182096,#182097,#182098,#182099,#182100,
#182101,#182102,#182103,#182104,#182105,#182106,#182107,#182108,#182109,
#182110,#182111,#182112,#182113,#182114,#182115,#182116,#182117,#182118,
#182119,#182120,#182121,#182122,#182123,#182124,#182125,#182126,#182127,
#182128,#182129,#182130,#182131,#182132,#182133,#182134,#182135,#182136,
#182137,#182138,#182139,#182140,#182141,#182142,#182143,#182144,#182145,
#182146,#182147),.UNSPECIFIED.,.F.,.F.,(4,2,2,2,2,2,2,2,2,2,2,2,2,2,2,2,
2,2,2,2,2,2,2,2,2,2,2,2,2,2,2,2,2,2,2,2,2,2,4),(6.88948415565909,6.89141801458342,
6.90474021311763,6.93177588713481,6.97221514823743,7.08776936697473,7.11769020949234,
7.13962540316573,7.16415849604642,7.21203763277651,7.29039380168267,7.33921802785112,
7.35560423878488,7.36816059809641,7.3862691115726,7.45046823029671,7.54624104871021,
7.57432106142301,7.59611687794412,7.62140064381964,7.67372768818048,7.76255670421757,
7.81014142349575,7.82459371238885,7.83623675695614,7.85051909614518,7.88377441630314,
7.94084361064966,8.02992242379317,8.06017844583965,8.08215257062765,8.10653377932961,
8.15328396329187,8.22131431393986,8.27667423996549,8.29572185013062,8.30814872058125,
8.32014034829938,8.34523528310529),.UNSPECIFIED.);
#30282=B_SPLINE_CURVE_WITH_KNOTS('',3,(#182150,#182151,#182152,#182153,
#182154,#182155,#182156,#182157,#182158,#182159,#182160,#182161,#182162,
#182163,#182164,#182165,#182166,#182167,#182168,#182169,#182170,#182171,
#182172,#182173,#182174,#182175,#182176,#182177,#182178,#182179,#182180,
#182181,#182182,#182183,#182184,#182185,#182186,#182187,#182188,#182189,
#182190,#182191,#182192,#182193,#182194,#182195,#182196,#182197,#182198,
#182199,#182200,#182201,#182202,#182203,#182204,#182205),.UNSPECIFIED.,
 .F.,.F.,(4,2,2,2,2,2,2,2,2,2,2,2,2,2,2,2,2,2,2,2,2,2,2,2,2,2,2,4),(1.00000001712619E-6,
0.0947119972862606,0.109535172509233,0.122857363566205,0.134658169476671,
0.153906771232427,0.234207439936081,0.296649708059561,0.340368572332069,
0.364427318761554,0.386499398388915,0.412681983689554,0.517013231527544,
0.57373595734596,0.590623080685259,0.603169022656912,0.621031899335483,
0.711114334859672,0.785685359291965,0.812534065126885,0.834250299145937,
0.86086282768967,0.920548379689519,0.926540857549104,1.0078403703309,1.04760215944455,
1.0626981323893,1.06776182258593),.UNSPECIFIED.);
#30283=B_SPLINE_CURVE_WITH_KNOTS('',3,(#182210,#182211,#182212,#182213,
#182214,#182215,#182216,#182217,#182218,#182219,#182220,#182221,#182222,
#182223,#182224,#182225,#182226,#182227,#182228,#182229,#182230,#182231,
#182232,#182233,#182234,#182235,#182236,#182237,#182238,#182239,#182240,
#182241,#182242,#182243,#182244,#182245,#182246,#182247,#182248,#182249,
#182250,#182251,#182252,#182253,#182254,#182255,#182256,#182257,#182258,
#182259,#182260,#182261,#182262,#182263,#182264,#182265,#182266,#182267,
#182268,#182269,#182270,#182271,#182272,#182273,#182274,#182275,#182276,
#182277,#182278,#182279,#182280,#182281,#182282,#182283,#182284,#182285,
#182286,#182287,#182288,#182289,#182290,#182291,#182292,#182293,#182294,
#182295,#182296,#182297,#182298,#182299,#182300,#182301,#182302,#182303,
#182304,#182305,#182306,#182307,#182308,#182309,#182310,#182311,#182312,
#182313,#182314,#182315,#182316,#182317,#182318,#182319,#182320,#182321,
#182322,#182323,#182324,#182325,#182326,#182327,#182328,#182329,#182330,
#182331,#182332,#182333,#182334,#182335,#182336,#182337,#182338,#182339,
#182340,#182341,#182342,#182343,#182344,#182345,#182346,#182347,#182348,
#182349,#182350,#182351,#182352,#182353,#182354,#182355,#182356,#182357,
#182358,#182359,#182360,#182361,#182362,#182363,#182364,#182365,#182366,
#182367,#182368,#182369,#182370,#182371,#182372,#182373,#182374,#182375,
#182376,#182377,#182378,#182379,#182380,#182381,#182382,#182383,#182384,
#182385,#182386,#182387,#182388,#182389,#182390,#182391,#182392,#182393,
#182394,#182395,#182396,#182397,#182398,#182399),.UNSPECIFIED.,.F.,.F.,
(4,2,2,2,2,2,2,2,2,2,2,2,2,2,2,2,2,2,2,2,2,2,2,2,2,2,2,2,2,2,2,2,2,2,2,
2,2,2,2,2,2,2,2,2,2,2,2,2,2,2,2,2,2,2,2,2,2,2,2,2,2,2,2,2,2,2,2,2,2,2,2,
2,2,2,2,2,2,2,2,2,2,2,2,2,2,2,2,2,2,2,2,2,2,2,4),(3.11744395882936,3.12694151309502,
3.14579754015536,3.24459640843926,3.30628076311852,3.34053666865373,3.36308156246976,
3.38623505328776,3.42464055749654,3.5202847142483,3.56776294756924,3.58408491513238,
3.59667182302396,3.61220276931054,3.67683258823788,3.74351999935887,3.7877598262854,
3.81179123517777,3.83387831942606,3.86004480977197,3.96913524517012,4.01490588650292,
4.04412676213954,4.05780824464263,4.06947278689076,4.08782109592327,4.17268601614708,
4.25777089488721,4.28810886071105,4.31009463674667,4.33444400400631,4.38094817055307,
4.45459771554067,4.50649591984476,4.52470157414305,4.5372638493657,4.55387211568767,
4.60544171108894,4.72285039684045,4.74921521875177,4.76876842552846,4.79477459882673,
4.85313308550783,4.97268136874961,4.9928818035547,5.00377846445466,5.01636385097906,
5.03928727157169,5.07083044565121,5.13298455450813,5.20705851567379,5.23460909473655,
5.25637191982548,5.2820048772336,5.33933355425583,5.41053597534993,5.4515007565642,
5.46715927407271,5.47976014339252,5.49596056164844,5.54191540591792,5.64133736785147,
5.67866939863431,5.70165617682956,5.72433342209488,5.75942599766235,5.80332579814885,
5.87225678500807,5.92345674406103,5.93979175548642,5.95135294957844,5.96627996610724,
6.00455883449701,6.07943996231504,6.15042525690114,6.17811953207395,6.19986266661448,
6.22573949973217,6.28563697419499,6.35590403733274,6.39677568424294,6.41294399314959,
6.42551768899698,6.44392129981866,6.46673152154306,6.52040099614958,6.60158366471143,
6.62777382705719,6.64984804132894,6.67390457814773,6.71760477527127,6.77999880564105,
6.86036549578554,6.87961643495318,6.88948415565909),.UNSPECIFIED.);
#30284=B_SPLINE_CURVE_WITH_KNOTS('',3,(#182400,#182401,#182402,#182403,
#182404,#182405,#182406,#182407,#182408,#182409,#182410,#182411,#182412,
#182413,#182414,#182415,#182416,#182417,#182418,#182419,#182420,#182421,
#182422,#182423,#182424,#182425,#182426,#182427,#182428,#182429,#182430,
#182431,#182432,#182433,#182434,#182435,#182436,#182437,#182438,#182439,
#182440,#182441,#182442,#182443,#182444,#182445,#182446,#182447,#182448,
#182449,#182450,#182451,#182452,#182453,#182454,#182455,#182456,#182457,
#182458,#182459,#182460,#182461,#182462,#182463,#182464,#182465,#182466,
#182467,#182468,#182469,#182470,#182471,#182472,#182473,#182474,#182475,
#182476,#182477,#182478,#182479,#182480,#182481,#182482,#182483,#182484,
#182485,#182486,#182487,#182488,#182489,#182490,#182491,#182492,#182493,
#182494,#182495,#182496,#182497,#182498,#182499,#182500,#182501,#182502,
#182503,#182504,#182505,#182506,#182507,#182508,#182509,#182510,#182511,
#182512,#182513,#182514,#182515,#182516,#182517,#182518,#182519,#182520,
#182521,#182522,#182523,#182524,#182525,#182526,#182527,#182528,#182529,
#182530,#182531,#182532,#182533,#182534,#182535,#182536,#182537,#182538,
#182539,#182540,#182541,#182542,#182543,#182544,#182545,#182546,#182547,
#182548,#182549,#182550,#182551,#182552,#182553,#182554,#182555,#182556,
#182557,#182558,#182559,#182560,#182561,#182562,#182563,#182564,#182565,
#182566,#182567,#182568,#182569,#182570,#182571,#182572,#182573,#182574,
#182575,#182576,#182577,#182578,#182579,#182580,#182581,#182582,#182583,
#182584,#182585,#182586,#182587),.UNSPECIFIED.,.F.,.F.,(4,2,2,2,2,2,2,2,
2,2,2,2,2,2,2,2,2,2,2,2,2,2,2,2,2,2,2,2,2,2,2,2,2,2,2,2,2,2,2,2,2,2,2,2,
2,2,2,2,2,2,2,2,2,2,2,2,2,2,2,2,2,2,2,2,2,2,2,2,2,2,2,2,2,2,2,2,2,2,2,2,
2,2,2,2,2,2,2,2,2,2,2,2,2,4),(1.06776182258593,1.07424788354723,1.09037184154246,
1.13945079036451,1.2270035492851,1.27899909195985,1.30424012793862,1.32604164394563,
1.3541890587477,1.44889705400479,1.51321247283617,1.53167700348148,1.54425451446089,
1.56037901360682,1.60109455708781,1.67451960508606,1.73219945160084,1.75786609105852,
1.77962428141715,1.80712543760684,1.88626840594513,1.95481635508634,1.99147171609752,
2.00620231139152,2.01778094040984,2.03437793173402,2.08423345261758,2.17045781598089,
2.22209877833376,2.24729351920513,2.26910145791718,2.29732302490004,2.39064538694898,
2.45651016745175,2.47480704713921,2.48737389968575,2.50361875572393,2.54471688484202,
2.61843298859145,2.67537943962706,2.70097303378857,2.72273790630625,2.75033781881128,
2.8680181519061,2.91025725622607,2.93805260894651,2.95150230303917,2.96324978649333,
2.9821578899495,3.08066359977336,3.14194758412427,3.17649896256903,3.19909030348181,
3.22218229194078,3.26019178363487,3.36213004842725,3.40501331314863,3.42094058353768,
3.43357995091236,3.45277606974348,3.51769337946013,3.58144858110792,3.60200392198475,
3.63399817820798,3.65618344693286,3.67996223747849,3.72188229728814,3.83069624635579,
3.87536641780213,3.8909616664111,3.90249964789073,3.9178018861172,3.95775315380778,
4.02782764509861,4.07794464122129,4.11619913461445,4.13938862233777,4.16164538356313,
4.1956754392536,4.23845769308302,4.34315482837855,4.36118053643026,4.37373407659236,
4.39048715927313,4.44452015701052,4.5586118465161,4.58514890648456,4.60686784061629,
4.63379679261957,4.70191902674089,4.771251252303,4.81766625531918,4.83203831894305,
4.83979364673243),.UNSPECIFIED.);
#30285=B_SPLINE_CURVE_WITH_KNOTS('',3,(#182614,#182615,#182616,#182617,
#182618,#182619,#182620,#182621,#182622,#182623),.UNSPECIFIED.,.F.,.F.,
(4,3,3,4),(0.,0.466042421267126,0.940249856436761,1.),.UNSPECIFIED.);
#30286=B_SPLINE_CURVE_WITH_KNOTS('',3,(#182635,#182636,#182637,#182638,
#182639,#182640,#182641,#182642,#182643,#182644,#182645,#182646,#182647,
#182648,#182649,#182650,#182651,#182652,#182653,#182654,#182655,#182656,
#182657,#182658,#182659,#182660,#182661,#182662,#182663,#182664,#182665,
#182666,#182667,#182668,#182669,#182670,#182671,#182672,#182673,#182674,
#182675,#182676,#182677,#182678,#182679,#182680,#182681,#182682,#182683,
#182684,#182685,#182686,#182687,#182688,#182689,#182690,#182691,#182692,
#182693,#182694,#182695,#182696,#182697,#182698,#182699,#182700,#182701,
#182702,#182703,#182704,#182705,#182706,#182707,#182708,#182709,#182710,
#182711,#182712,#182713,#182714,#182715,#182716,#182717,#182718,#182719,
#182720,#182721,#182722,#182723,#182724,#182725,#182726,#182727,#182728,
#182729,#182730,#182731,#182732,#182733,#182734,#182735,#182736,#182737,
#182738,#182739,#182740,#182741,#182742,#182743,#182744,#182745,#182746,
#182747,#182748,#182749,#182750,#182751,#182752,#182753,#182754,#182755,
#182756,#182757,#182758,#182759,#182760,#182761,#182762,#182763,#182764,
#182765,#182766,#182767,#182768,#182769,#182770,#182771,#182772,#182773,
#182774,#182775,#182776,#182777,#182778,#182779,#182780,#182781,#182782,
#182783,#182784,#182785,#182786,#182787,#182788,#182789,#182790,#182791,
#182792,#182793,#182794,#182795,#182796,#182797,#182798,#182799,#182800,
#182801,#182802,#182803,#182804,#182805,#182806,#182807,#182808,#182809,
#182810),.UNSPECIFIED.,.F.,.F.,(4,2,2,2,2,2,2,2,2,2,2,2,2,2,2,2,2,2,2,2,
2,2,2,2,2,2,2,2,2,2,2,2,2,2,2,2,2,2,2,2,2,2,2,2,2,2,2,2,2,2,2,2,2,2,2,2,
2,2,2,2,2,2,2,2,2,2,2,2,2,2,2,2,2,2,2,2,2,2,2,2,2,2,2,2,2,2,2,4),(4.83979364673243,
4.84367014322603,4.85802029975688,4.89176076265798,4.9503386380513,5.03714167429101,
5.06744736122364,5.0894287373729,5.11379099582578,5.16039299666449,5.23436606903538,
5.28708932448838,5.30469658181848,5.31723609741978,5.33435263414912,5.3971999728895,
5.49763805243059,5.52530333933724,5.54706898097428,5.57263536588406,5.62720509399079,
5.72548818007443,5.76272841944928,5.77763157651974,5.78917837969072,5.80522127391578,
5.85530303480364,5.95717195261677,5.99938153238094,6.02320564045918,6.04537037249978,
6.07721790956922,6.09763102156905,6.16061416364242,6.22686448743711,6.24599901729141,
6.25863210695444,6.274596068554,6.31787131798,6.42250893271361,6.45878788619945,
6.48161023218432,6.50443757194009,6.54046997542785,6.58616209400338,6.65534263176113,
6.70335009057412,6.71783260264344,6.72948023359561,6.74373813814339,6.77681903931524,
6.83335381360029,6.9232754924118,6.95350270842544,6.97547332750822,6.99986701859546,
7.04670943674406,7.12148632426097,7.17495111535607,7.19154073776591,7.20408600217487,
7.22193927577781,7.2437988308098,7.29316361060375,7.38155535794701,7.40997901253632,
7.43180435601276,7.45687485781199,7.5075866571292,7.59047867266803,7.64469907080788,
7.66142826971883,7.67301707905495,7.68765387073351,7.72356600357138,7.78941553209505,
7.86553410640628,7.89603339619037,7.91803699914874,7.94231427265443,7.98830867777345,
8.06032117887829,8.11302803706241,8.13198929278981,8.14460558454549,8.16067628809637,
8.2051332456036,8.32330225647707),.UNSPECIFIED.);
#30287=B_SPLINE_CURVE_WITH_KNOTS('',3,(#182813,#182814,#182815,#182816,
#182817,#182818,#182819,#182820,#182821,#182822,#182823,#182824,#182825,
#182826,#182827,#182828,#182829,#182830,#182831,#182832,#182833,#182834,
#182835,#182836,#182837,#182838,#182839,#182840,#182841,#182842,#182843,
#182844,#182845,#182846,#182847,#182848,#182849,#182850,#182851,#182852,
#182853,#182854,#182855,#182856,#182857,#182858,#182859,#182860,#182861,
#182862,#182863,#182864,#182865,#182866,#182867,#182868,#182869,#182870,
#182871,#182872,#182873,#182874,#182875,#182876,#182877,#182878,#182879,
#182880,#182881,#182882,#182883,#182884,#182885,#182886,#182887,#182888,
#182889,#182890,#182891,#182892,#182893,#182894,#182895,#182896,#182897,
#182898,#182899,#182900,#182901,#182902,#182903,#182904,#182905,#182906,
#182907,#182908,#182909,#182910,#182911,#182912,#182913,#182914,#182915,
#182916,#182917,#182918,#182919,#182920,#182921,#182922,#182923,#182924,
#182925,#182926,#182927,#182928,#182929,#182930,#182931,#182932,#182933,
#182934,#182935,#182936,#182937,#182938,#182939,#182940,#182941,#182942,
#182943,#182944,#182945,#182946,#182947,#182948,#182949,#182950,#182951,
#182952,#182953,#182954,#182955,#182956,#182957,#182958,#182959,#182960,
#182961,#182962,#182963,#182964,#182965,#182966,#182967,#182968,#182969,
#182970,#182971,#182972),.UNSPECIFIED.,.F.,.F.,(4,2,2,2,2,2,2,2,2,2,2,2,
2,2,2,2,2,2,2,2,2,2,2,2,2,2,2,2,2,2,2,2,2,2,2,2,2,2,2,2,2,2,2,2,2,2,2,2,
2,2,2,2,2,2,2,2,2,2,2,2,2,2,2,2,2,2,2,2,2,2,2,2,2,2,2,2,2,2,2,4),(0.000225337909139367,
0.0292717095416562,0.0505239070880682,0.0751504710126493,0.119984405057097,
0.222628091878377,0.267192334550033,0.282776676146931,0.294313533193336,
0.309623314590521,0.349645533055194,0.419702387883073,0.476031974073537,
0.510940415084872,0.533587424214121,0.556607355965541,0.594159068655156,
0.690053826025381,0.738607405494358,0.755009621309299,0.767587828478025,
0.78303625440397,0.832973737062743,0.909671379078525,0.957079771885631,
0.981550402261636,1.00350136931844,1.03355831363916,1.14829431806412,1.1890215181048,
1.21618042059942,1.22952351576019,1.24131581869561,1.26050889790246,1.34195804753588,
1.43121477359485,1.46053881398604,1.4824100984169,1.50724122817928,1.55743393075515,
1.5783724429731,1.64795120208137,1.67372298916354,1.6937833995583,1.70651884828274,
1.72197251917669,1.75543462582521,1.82719833229392,1.89367459809474,1.92007460444182,
1.94179461045165,1.96886675656026,2.03221009135532,2.11430237212839,2.15423737604396,
2.16935263342085,2.18090146087354,2.19700260542734,2.24578624585707,2.33359222314304,
2.38565465677845,2.41090453658282,2.43270506830581,2.46083903427388,2.55577376470094,
2.61990655913048,2.63836773569775,2.65094509986822,2.66707215988022,2.71091140333411,
2.78317198810242,2.83937087960711,2.86488791011897,2.88666018259058,2.91436577524644,
3.03128114050773,3.07381474163023,3.10173217448532,3.11520207107795,3.11744395882936),
 .UNSPECIFIED.);
#30288=B_SPLINE_CURVE_WITH_KNOTS('',3,(#182976,#182977,#182978,#182979,
#182980,#182981),.UNSPECIFIED.,.F.,.F.,(4,2,4),(1.45420179664634,1.60034795961777,
1.7792155245964),.UNSPECIFIED.);
#30289=B_SPLINE_CURVE_WITH_KNOTS('',3,(#182985,#182986,#182987,#182988,
#182989,#182990,#182991,#182992,#182993,#182994,#182995,#182996,#182997,
#182998,#182999,#183000,#183001,#183002,#183003,#183004,#183005,#183006,
#183007,#183008,#183009,#183010),.UNSPECIFIED.,.F.,.F.,(4,2,2,2,2,2,2,2,
2,2,2,2,4),(1.00000001384073E-6,0.147496320872454,0.27627744997771,0.416495853131057,
0.550555574701638,0.664844786569313,0.796386308624163,0.911514817984701,
1.04112230610171,1.1590206206347,1.29683959014132,1.43253712595453,1.45420179664634),
 .UNSPECIFIED.);
#30290=B_SPLINE_CURVE_WITH_KNOTS('',3,(#183034,#183035,#183036,#183037,
#183038,#183039,#183040,#183041),.UNSPECIFIED.,.F.,.F.,(4,2,2,4),(-0.422074901515015,
-0.379068128351578,-0.282387357989601,-0.250738867764476),.UNSPECIFIED.);
#30291=B_SPLINE_CURVE_WITH_KNOTS('',3,(#183046,#183047,#183048,#183049,
#183050,#183051,#183052),.UNSPECIFIED.,.F.,.F.,(4,3,4),(-0.0851792640752978,
0.,0.0851792640752318),.UNSPECIFIED.);
#30292=B_SPLINE_CURVE_WITH_KNOTS('',3,(#183059,#183060,#183061,#183062,
#183063,#183064,#183065,#183066,#183067,#183068,#183069,#183070,#183071,
#183072,#183073,#183074,#183075),.UNSPECIFIED.,.F.,.F.,(4,2,2,2,1,2,2,2,
4),(0.691841692846147,0.730361481240391,0.749621375437511,0.754436348986791,
0.759251322536071,0.768881269634628,0.845920846423085,0.922960423211543,
1.),.UNSPECIFIED.);
#30293=B_SPLINE_CURVE_WITH_KNOTS('',3,(#183076,#183077,#183078,#183079,
#183080,#183081,#183082,#183083,#183084,#183085,#183086,#183087,#183088,
#183089,#183090,#183091,#183092,#183093,#183094,#183095,#183096,#183097,
#183098,#183099,#183100,#183101,#183102,#183103,#183104,#183105,#183106,
#183107,#183108,#183109,#183110,#183111,#183112,#183113,#183114,#183115,
#183116,#183117,#183118,#183119,#183120,#183121,#183122,#183123,#183124,
#183125,#183126,#183127,#183128,#183129,#183130,#183131,#183132,#183133,
#183134,#183135,#183136,#183137,#183138,#183139,#183140,#183141,#183142,
#183143,#183144,#183145,#183146,#183147,#183148,#183149,#183150,#183151,
#183152,#183153,#183154,#183155,#183156,#183157,#183158,#183159,#183160),
 .UNSPECIFIED.,.F.,.F.,(4,3,3,3,3,3,3,3,3,3,3,3,3,3,3,3,3,3,3,3,3,3,3,3,
3,3,3,3,4),(0.,0.0480329457521728,0.0955923583820344,0.142452410367028,
0.172960423211526,0.227007917172798,0.280795071156351,0.334180568678605,
0.345920846423051,0.391773667569033,0.432401058028814,0.475641163831695,
0.497261216733136,0.502746609445371,0.508071243183858,0.51888126963458,
0.542844921349788,0.567150056988716,0.591940455940715,0.605361481240375,
0.616171507691099,0.621576520916459,0.624279027529142,0.626981534141824,
0.642242401576597,0.648601587043266,0.663892977132314,0.679172488710331,
0.691841689138341),.UNSPECIFIED.);
#30294=B_SPLINE_CURVE_WITH_KNOTS('',3,(#183161,#183162,#183163,#183164,
#183165,#183166,#183167,#183168,#183169,#183170,#183171,#183172,#183173,
#183174,#183175,#183176,#183177,#183178,#183179,#183180,#183181,#183182,
#183183,#183184),.UNSPECIFIED.,.F.,.F.,(4,2,2,2,2,2,2,2,2,2,2,4),(1.00000001309674E-6,
0.129224229604342,0.241263601967655,0.496076308060944,0.797054408048329,
1.12551872852194,1.51457617341985,1.9211054184316,2.48023648950879,2.94600632909222,
3.4283141418049,3.80158966705551),.UNSPECIFIED.);
#30295=B_SPLINE_CURVE_WITH_KNOTS('',3,(#183190,#183191,#183192,#183193,
#183194,#183195,#183196,#183197,#183198,#183199,#183200,#183201,#183202,
#183203,#183204,#183205,#183206,#183207,#183208,#183209,#183210,#183211,
#183212,#183213,#183214,#183215,#183216,#183217,#183218,#183219,#183220,
#183221,#183222,#183223,#183224,#183225,#183226,#183227,#183228,#183229,
#183230,#183231,#183232,#183233,#183234,#183235,#183236,#183237,#183238,
#183239,#183240,#183241,#183242,#183243,#183244,#183245,#183246,#183247,
#183248,#183249,#183250,#183251,#183252,#183253,#183254,#183255,#183256,
#183257,#183258,#183259,#183260,#183261,#183262,#183263,#183264,#183265,
#183266,#183267,#183268,#183269,#183270,#183271,#183272,#183273,#183274,
#183275,#183276,#183277,#183278,#183279,#183280,#183281,#183282,#183283,
#183284,#183285,#183286,#183287,#183288,#183289,#183290,#183291,#183292,
#183293,#183294,#183295,#183296,#183297,#183298,#183299,#183300,#183301,
#183302,#183303,#183304,#183305,#183306,#183307,#183308,#183309,#183310,
#183311,#183312,#183313,#183314,#183315,#183316,#183317,#183318,#183319,
#183320,#183321,#183322,#183323,#183324,#183325,#183326,#183327,#183328,
#183329,#183330,#183331,#183332,#183333),.UNSPECIFIED.,.F.,.F.,(4,2,2,2,
2,2,2,2,2,2,2,2,2,2,2,2,2,2,2,2,2,2,2,2,2,2,2,2,2,2,2,2,2,2,2,2,2,2,2,2,
2,2,2,2,2,2,2,2,2,2,2,2,2,2,2,2,2,2,2,2,2,2,2,2,2,2,2,2,2,2,2,4),(-2.70657200810638,
-2.70214184710763,-2.68723936465603,-2.64726736463653,-2.55727944885561,
-2.51159438667173,-2.48743895240915,-2.46534998566859,-2.43371879553524,
-2.41324657383308,-2.34693664433086,-2.29546775853098,-2.27919589566977,
-2.26667452046651,-2.24761514929512,-2.22332511326117,-2.15842203129561,
-2.100283970418,-2.07450170525313,-2.05272929755366,-2.02442294882669,-1.95492881376122,
-1.86554060462523,-1.84891352543864,-1.83731748462922,-1.82211690291699,
-1.77896342050705,-1.66685971268145,-1.63563287714678,-1.6135740399562,
-1.58931660936387,-1.541621602447,-1.45740584130219,-1.42569639648637,-1.41126743469913,
-1.39795078874467,-1.37357931312205,-1.30288363529104,-1.23665700931164,
-1.2106035121226,-1.1888514958355,-1.16091132341498,-1.12915158688185,-1.06214283552152,
-1.00473805161412,-0.98636319840359,-0.974597196061126,-0.960477052669798,
-0.927287673755786,-0.867607488061156,-0.797545140108554,-0.768454686778253,
-0.746624285458318,-0.721349851053767,-0.663411959843093,-0.568693706683454,
-0.553023634158854,-0.54040672331115,-0.523578440895917,-0.503240896751126,
-0.45867043084094,-0.376406353474949,-0.348904053221221,-0.327171805956353,
-0.300750127078341,-0.231888909936616,-0.138442844373473,-0.120995821362398,
-0.109335903594524,-0.0947063495243196,-0.0748468037826614,-1.00000001657108E-6),
 .UNSPECIFIED.);
#30296=B_SPLINE_CURVE_WITH_KNOTS('',3,(#183334,#183335,#183336,#183337,
#183338,#183339,#183340,#183341,#183342,#183343,#183344,#183345,#183346,
#183347,#183348,#183349,#183350,#183351,#183352,#183353,#183354,#183355,
#183356,#183357,#183358,#183359,#183360,#183361,#183362,#183363,#183364,
#183365,#183366,#183367,#183368,#183369,#183370,#183371,#183372,#183373,
#183374,#183375,#183376,#183377,#183378,#183379,#183380,#183381,#183382,
#183383,#183384,#183385,#183386,#183387,#183388,#183389,#183390,#183391,
#183392,#183393,#183394,#183395,#183396,#183397,#183398,#183399,#183400,
#183401,#183402,#183403,#183404,#183405,#183406,#183407,#183408,#183409,
#183410,#183411,#183412,#183413,#183414,#183415,#183416,#183417,#183418,
#183419,#183420,#183421,#183422,#183423,#183424,#183425,#183426,#183427,
#183428,#183429,#183430,#183431,#183432,#183433,#183434,#183435,#183436,
#183437,#183438,#183439,#183440,#183441,#183442,#183443),.UNSPECIFIED.,
 .F.,.F.,(4,2,2,2,2,2,2,2,2,2,2,2,2,2,2,2,2,2,2,2,2,2,2,2,2,2,2,2,2,2,2,
2,2,2,2,2,2,2,2,2,2,2,2,2,2,2,2,2,2,2,2,2,2,2,4),(-11.0525898219334,-10.9451955405454,
-10.9175376166771,-10.8958004433713,-10.8695079718537,-10.8058361867022,
-10.7358477644187,-10.6999437907365,-10.6854850563783,-10.6737953686814,
-10.6560609945434,-10.5646795309562,-10.4945715412295,-10.468079086281,
-10.446348643571,-10.4189280801612,-10.33433506663,-10.2718010737687,-10.2548428267076,
-10.2422351870229,-10.2266867142584,-10.144336853529,-10.0977280708593,
-10.0810002635724,-10.0532562691983,-10.0315155882965,-10.0052916010387,
-9.94867170022827,-9.8730873610219,-9.83590140699322,-9.82129460438642,
-9.80963062924863,-9.79214544329891,-9.7116523592644,-9.63517351316824,
-9.60684048441813,-9.58506591829065,-9.55930136163698,-9.5022068778219,
-9.43646311463777,-9.41203817947794,-9.39290563146559,-9.3803783558284,
-9.3641536887642,-9.30976579535966,-9.24532094133244,-9.21469225226209,
-9.18765718227209,-9.16593182042167,-9.13908611089903,-9.06964232827476,
-9.00518783627803,-8.97067935807782,-8.95639002715814,-8.95293752943051),
 .UNSPECIFIED.);
#30297=B_SPLINE_CURVE_WITH_KNOTS('',3,(#183732,#183733,#183734,#183735,
#183736,#183737,#183738,#183739,#183740,#183741),.UNSPECIFIED.,.F.,.F.,
(4,3,3,4),(0.,0.466042421235165,0.94024985640319,1.),.UNSPECIFIED.);
#30298=B_SPLINE_CURVE_WITH_KNOTS('',3,(#183813,#183814,#183815,#183816,
#183817,#183818,#183819,#183820),.UNSPECIFIED.,.F.,.F.,(4,2,2,4),(1.98093781570329E-5,
0.435125302348886,0.651412660622268,0.869568218310475),.UNSPECIFIED.);
#30299=B_SPLINE_CURVE_WITH_KNOTS('',3,(#183826,#183827,#183828,#183829,
#183830,#183831,#183832,#183833,#183834,#183835,#183836,#183837,#183838,
#183839,#183840,#183841,#183842,#183843,#183844,#183845,#183846,#183847,
#183848,#183849,#183850,#183851,#183852,#183853,#183854,#183855,#183856,
#183857,#183858,#183859,#183860,#183861,#183862,#183863,#183864,#183865,
#183866,#183867,#183868,#183869,#183870,#183871,#183872,#183873,#183874,
#183875,#183876,#183877,#183878,#183879,#183880,#183881,#183882,#183883,
#183884,#183885,#183886,#183887,#183888,#183889,#183890,#183891,#183892,
#183893,#183894,#183895,#183896,#183897,#183898,#183899,#183900,#183901,
#183902,#183903,#183904,#183905,#183906,#183907),.UNSPECIFIED.,.F.,.F.,
(4,2,2,2,2,2,2,2,2,2,2,2,2,2,2,2,2,2,2,2,2,2,2,2,2,2,2,2,2,2,2,2,2,2,2,
2,2,2,2,2,4),(-25.3488773908543,-25.2117579765738,-25.0765301219692,-24.8121844159216,
-24.6100474871139,-24.4348153226359,-24.1591117730323,-23.9801715480672,
-23.7098723062826,-23.3436886097765,-23.124093349834,-22.9301004485503,
-22.713789244769,-22.5178484117983,-22.3445885926295,-22.1365517072343,
-21.9617467722256,-21.6860606757945,-21.5039208682341,-21.3209414773744,
-21.1435380906266,-20.8678762695796,-20.6933425591195,-20.4219590279459,
-20.0473764685859,-19.8294686500964,-19.6344958137531,-19.4185809489582,
-19.2224066058403,-19.0491319032085,-18.841195416967,-18.6663874275954,
-18.3907086523902,-18.2086415850464,-18.0255307566173,-17.8481495826963,
-17.5724951826215,-17.39794550316,-17.1265746270368,-16.7520562837938,-16.6093578201488),
 .UNSPECIFIED.);
#30300=B_SPLINE_CURVE_WITH_KNOTS('',3,(#183910,#183911,#183912,#183913,
#183914,#183915,#183916,#183917,#183918,#183919,#183920,#183921,#183922,
#183923,#183924,#183925,#183926,#183927,#183928,#183929,#183930,#183931,
#183932,#183933,#183934,#183935,#183936,#183937,#183938,#183939,#183940,
#183941,#183942,#183943,#183944,#183945,#183946,#183947,#183948,#183949,
#183950,#183951,#183952,#183953,#183954,#183955,#183956,#183957,#183958,
#183959,#183960,#183961,#183962,#183963),.UNSPECIFIED.,.F.,.F.,(4,2,2,2,
2,2,2,2,2,2,2,2,2,2,2,2,2,2,2,2,2,2,2,2,2,2,4),(6.63472946974546E-5,0.119852469453836,
0.240332488052986,0.471018335111722,0.81956291339417,1.09565454106518,1.45232143744692,
1.76752908522675,2.11369209864303,2.3742079135105,2.92100550850285,3.10718760089758,
3.45781086818677,3.68161712065895,4.03562600471986,4.40380054033367,4.58503323789667,
5.13378113052651,5.39299395323343,5.73656971192001,6.01538708479495,6.35675532647042,
6.57106600077119,7.02865050751105,7.31409315488209,7.65074778062276,8.07357000628427),
 .UNSPECIFIED.);
#30301=B_SPLINE_CURVE_WITH_KNOTS('',3,(#183968,#183969,#183970,#183971,
#183972,#183973,#183974,#183975,#183976,#183977,#183978,#183979,#183980,
#183981,#183982,#183983,#183984,#183985,#183986,#183987,#183988,#183989,
#183990,#183991,#183992,#183993,#183994,#183995,#183996,#183997,#183998,
#183999,#184000,#184001,#184002,#184003,#184004,#184005,#184006,#184007,
#184008,#184009,#184010,#184011,#184012,#184013,#184014,#184015,#184016,
#184017,#184018,#184019,#184020,#184021,#184022,#184023,#184024,#184025,
#184026,#184027,#184028,#184029,#184030,#184031,#184032,#184033,#184034,
#184035,#184036,#184037,#184038,#184039,#184040,#184041,#184042,#184043,
#184044,#184045,#184046,#184047,#184048,#184049,#184050,#184051,#184052,
#184053),.UNSPECIFIED.,.F.,.F.,(4,2,2,2,2,2,2,2,2,2,2,2,2,2,2,2,2,2,2,2,
2,2,2,2,2,2,2,2,2,2,2,2,2,2,2,2,2,2,2,2,2,2,4),(-16.6093578201488,-16.5792653081084,
-16.3688617948715,-16.1942583158352,-15.9185937912375,-15.7341679467037,
-15.510329013096,-15.3337592978338,-15.1376405428431,-14.9617442945232,
-14.6860653778253,-14.5088808638798,-14.2381796190777,-13.8692442892602,
-13.6966458427509,-13.4851560245841,-13.3106424775729,-13.0349964870432,
-12.8479009746796,-12.6740346954215,-12.5002332859473,-12.3138240226037,
-12.0381735405829,-11.8636493211966,-11.6522937409599,-11.4796727640309,
-11.110050570064,-10.8392528782752,-10.6624476167363,-10.4372172998725,
-10.2537939564926,-9.97812630303468,-9.80345503736936,-9.59390281924938,
-9.42095531055332,-9.22887410887228,-9.00592036679354,-8.73026742422095,
-8.5488309202539,-8.38217370714925,-8.1948770877202,-7.91922350740144,-7.87061597992456),
 .UNSPECIFIED.);
#30302=B_SPLINE_CURVE_WITH_KNOTS('',3,(#184054,#184055,#184056,#184057,
#184058,#184059,#184060,#184061,#184062,#184063,#184064,#184065,#184066,
#184067,#184068,#184069,#184070,#184071,#184072,#184073,#184074,#184075,
#184076,#184077,#184078,#184079,#184080,#184081,#184082,#184083,#184084,
#184085,#184086,#184087,#184088,#184089,#184090,#184091,#184092,#184093,
#184094,#184095,#184096,#184097,#184098,#184099,#184100,#184101,#184102,
#184103,#184104,#184105,#184106,#184107,#184108,#184109,#184110,#184111,
#184112,#184113,#184114,#184115,#184116,#184117,#184118,#184119,#184120,
#184121,#184122,#184123,#184124,#184125,#184126,#184127,#184128,#184129,
#184130,#184131,#184132,#184133,#184134,#184135,#184136,#184137,#184138,
#184139,#184140,#184141,#184142,#184143,#184144,#184145,#184146,#184147,
#184148,#184149,#184150,#184151,#184152,#184153,#184154,#184155,#184156,
#184157,#184158,#184159,#184160,#184161),.UNSPECIFIED.,.F.,.F.,(4,2,2,2,
2,2,2,2,2,2,2,2,2,2,2,2,2,2,2,2,2,2,2,2,2,2,2,2,2,2,2,2,2,2,2,2,2,2,2,2,
2,2,2,2,2,2,2,2,2,2,2,2,2,4),(-8.73899861150267,-8.69914480337356,-8.54464421100673,
-8.39572763166509,-8.23116510095003,-8.04330833686929,-7.89530357788577,
-7.71444490512931,-7.63218540045482,-7.34190189330136,-7.18731818512391,
-7.03875298532148,-6.87440872067566,-6.68634926779794,-6.53835803539044,
-6.3574461866764,-6.27519062631498,-5.98491286681858,-5.83033369014256,
-5.68177659125073,-5.51744048167933,-5.32938533228556,-5.18139964121957,
-5.00049251951509,-4.91823952559342,-4.627971678843,-4.47339685583356,-4.32484684565646,
-4.16051662597844,-3.9724686670833,-3.82448853460015,-3.64358883675198,
-3.56134283666075,-3.27107437284463,-3.11651405924174,-2.96793565491532,
-2.80344671651332,-2.6155305073513,-2.46749047947249,-2.28682286631188,
-2.20469916989341,-1.91428724602398,-1.76006360631775,-1.61059279284905,
-1.52984381579783,-1.23251915858275,-1.07535085998026,-0.928129335387397,
-0.845106454401542,-0.561534774960734,-0.41156192518634,-0.314806053587988,
-0.213628494228944,-4.30320540010522E-5),.UNSPECIFIED.);
#30303=B_SPLINE_CURVE_WITH_KNOTS('',3,(#184168,#184169,#184170,#184171,
#184172,#184173,#184174,#184175,#184176,#184177,#184178,#184179,#184180,
#184181,#184182,#184183,#184184,#184185,#184186,#184187,#184188,#184189,
#184190,#184191,#184192,#184193,#184194,#184195,#184196,#184197,#184198,
#184199,#184200,#184201,#184202,#184203,#184204,#184205,#184206,#184207,
#184208,#184209,#184210,#184211,#184212,#184213,#184214,#184215,#184216,
#184217,#184218,#184219,#184220,#184221,#184222,#184223,#184224,#184225,
#184226,#184227,#184228,#184229,#184230,#184231,#184232,#184233,#184234,
#184235,#184236,#184237,#184238,#184239,#184240,#184241),.UNSPECIFIED.,
 .F.,.F.,(4,2,2,2,2,2,2,2,2,2,2,2,2,2,2,2,2,2,2,2,2,2,2,2,2,2,2,2,2,2,2,
2,2,2,2,2,4),(-7.87061597992456,-7.74470628455937,-7.53319093454486,-7.36059066540921,
-6.99174256274364,-6.72104629906109,-6.54380121348743,-6.26811290449752,
-6.0922320395682,-5.8959050199953,-5.719400421899,-5.49597956919839,-5.31123334622609,
-5.03556141350746,-4.86096963377401,-4.65034766871294,-4.47758950715269,
-4.10414504573837,-3.83287387892188,-3.65788145499446,-3.44503513096825,
-3.25094276997586,-2.97525557236685,-2.80045632747259,-2.59234243153645,
-2.41909859753841,-2.22334257313634,-2.00672459368894,-1.81352307443079,
-1.59254980365457,-1.23297515385466,-0.963874962372695,-0.779853288355305,
-0.585014064424859,-0.293134115374441,-0.147808546265094,-9.31271228427911E-6),
 .UNSPECIFIED.);
#30304=B_SPLINE_CURVE_WITH_KNOTS('',3,(#184242,#184243,#184244,#184245,
#184246,#184247,#184248,#184249,#184250,#184251,#184252,#184253,#184254,
#184255,#184256,#184257,#184258,#184259,#184260,#184261,#184262,#184263,
#184264,#184265,#184266,#184267,#184268,#184269,#184270,#184271,#184272,
#184273,#184274,#184275,#184276,#184277,#184278,#184279,#184280,#184281,
#184282,#184283,#184284,#184285,#184286,#184287,#184288,#184289,#184290,
#184291,#184292,#184293,#184294,#184295,#184296,#184297,#184298,#184299,
#184300,#184301,#184302,#184303,#184304,#184305,#184306,#184307,#184308,
#184309,#184310,#184311,#184312,#184313,#184314,#184315,#184316,#184317,
#184318,#184319,#184320,#184321,#184322,#184323,#184324,#184325,#184326,
#184327,#184328,#184329,#184330,#184331,#184332,#184333,#184334,#184335,
#184336,#184337,#184338,#184339,#184340,#184341,#184342,#184343,#184344,
#184345,#184346,#184347),.UNSPECIFIED.,.F.,.F.,(4,2,2,2,2,2,2,2,2,2,2,2,
2,2,2,2,2,2,2,2,2,2,2,2,2,2,2,2,2,2,2,2,2,2,2,2,2,2,2,2,2,2,2,2,2,2,2,2,
2,2,2,2,4),(-17.4782773446469,-17.3145507638988,-17.2323097895944,-17.0514231256051,
-16.9034535217882,-16.7154162229866,-16.5510957447174,-16.4025567378387,
-16.2479928964372,-15.9577428595964,-15.8754948526675,-15.6946006751635,
-15.5466254429558,-15.3585808507769,-15.1942544180056,-15.045708273596,
-14.8911399994233,-14.6008798764381,-14.5186292733015,-14.3377298054029,
-14.1897490289545,-14.0016983511229,-13.8373654025521,-13.6888138885248,
-13.5342402921702,-13.2439697088235,-13.1617163401424,-12.9808071777748,
-12.8328216847827,-12.6447522100799,-12.4804258903256,-12.3318894677204,
-12.1773052701961,-11.886991386448,-11.8047439638111,-11.62342288253,-11.4754890658908,
-11.2859093990368,-11.1230831642647,-10.9770480843857,-10.8218072863131,
-10.5274988371903,-10.4462882197963,-10.2870405659291,-10.1350158954007,
-9.86489557230041,-9.77667896000119,-9.58326202343803,-9.43586173011933,
-9.22167535505261,-9.0712847440584,-8.98887090232673,-8.73899861150267),
 .UNSPECIFIED.);
#30305=B_SPLINE_CURVE_WITH_KNOTS('',3,(#184367,#184368,#184369,#184370,
#184371,#184372,#184373,#184374,#184375,#184376,#184377,#184378,#184379,
#184380,#184381,#184382,#184383,#184384),.UNSPECIFIED.,.F.,.F.,(4,2,2,2,
2,2,2,2,4),(0.118255944796295,0.150196749040088,0.182137553283882,0.210325561008924,
0.238513568733966,0.266701576459009,0.294889584184051,0.326830388427845,
0.358771192671638),.UNSPECIFIED.);
#30306=B_SPLINE_CURVE_WITH_KNOTS('',3,(#184388,#184389,#184390,#184391,
#184392,#184393,#184394,#184395,#184396,#184397,#184398,#184399,#184400,
#184401,#184402,#184403,#184404,#184405),.UNSPECIFIED.,.F.,.F.,(4,2,2,2,
2,2,2,2,4),(-0.357545008588623,-0.325833280361292,-0.294121552133961,-0.265932611678201,
-0.237743671222442,-0.209554730766682,-0.181365790310923,-0.149654062083592,
-0.117942333856262),.UNSPECIFIED.);
#30307=B_SPLINE_CURVE_WITH_KNOTS('',3,(#184410,#184411,#184412,#184413,
#184414,#184415,#184416,#184417,#184418,#184419,#184420,#184421,#184422,
#184423,#184424,#184425,#184426,#184427),.UNSPECIFIED.,.F.,.F.,(4,2,2,2,
2,2,2,2,4),(-0.357545008588621,-0.325833280361291,-0.29412155213396,-0.265932611678201,
-0.237743671222441,-0.209554730766681,-0.181365790310922,-0.149654062083591,
-0.117942333856259),.UNSPECIFIED.);
#30308=B_SPLINE_CURVE_WITH_KNOTS('',3,(#184431,#184432,#184433,#184434,
#184435,#184436,#184437,#184438,#184439,#184440,#184441,#184442,#184443,
#184444,#184445,#184446,#184447,#184448),.UNSPECIFIED.,.F.,.F.,(4,2,2,2,
2,2,2,2,4),(-0.358783917084611,-0.327792365271302,-0.296800813457993,-0.26765719109598,
-0.238513568733966,-0.210325561008924,-0.182137553283882,-0.150196749040089,
-0.118255944796295),.UNSPECIFIED.);
#30309=B_SPLINE_CURVE_WITH_KNOTS('',3,(#184456,#184457,#184458,#184459,
#184460,#184461,#184462,#184463,#184464,#184465,#184466,#184467,#184468,
#184469,#184470,#184471,#184472,#184473,#184474),.UNSPECIFIED.,.F.,.F.,
(4,2,2,2,3,2,2,2,4),(-0.120257623937773,-0.0883168196939601,-0.0563760154501472,
-0.0281880077250899,-3.25711679849405E-14,0.0281880077250248,0.0563760154500821,
0.0883168196938949,0.120257623937708),.UNSPECIFIED.);
#30310=B_SPLINE_CURVE_WITH_KNOTS('',3,(#184486,#184487,#184488,#184489,
#184490,#184491,#184492,#184493,#184494,#184495,#184496,#184497,#184498,
#184499,#184500,#184501,#184502,#184503),.UNSPECIFIED.,.F.,.F.,(4,2,2,2,
2,2,2,2,4),(-0.358786911659494,-0.3268461074157,-0.294905303171906,-0.266717295446863,
-0.238529287721821,-0.209385665359807,-0.180242042997794,-0.149250491184484,
-0.118258939371175),.UNSPECIFIED.);
#30311=B_SPLINE_CURVE_WITH_KNOTS('',3,(#184506,#184507,#184508,#184509,
#184510,#184511,#184512,#184513,#184514,#184515,#184516,#184517,#184518,
#184519,#184520,#184521,#184522,#184523,#184524),.UNSPECIFIED.,.F.,.F.,
(4,2,2,2,3,2,2,2,4),(-0.120257623937686,-0.0883168196938895,-0.0563760154500934,
-0.0281880077250492,-5.10702591327572E-15,0.0281880077250392,0.0563760154500835,
0.0883168196938795,0.120257623937675),.UNSPECIFIED.);
#30312=B_SPLINE_CURVE_WITH_KNOTS('',3,(#184529,#184530,#184531,#184532,
#184533,#184534,#184535,#184536,#184537,#184538,#184539,#184540,#184541,
#184542,#184543,#184544,#184545,#184546),.UNSPECIFIED.,.F.,.F.,(4,2,2,2,
2,2,2,2,4),(-0.358783917084615,-0.327792365271305,-0.296800813457996,-0.267657191095982,
-0.238513568733968,-0.210325561008926,-0.182137553283884,-0.150196749040089,
-0.118255944796295),.UNSPECIFIED.);
#30313=B_SPLINE_CURVE_WITH_KNOTS('',3,(#184549,#184550,#184551,#184552,
#184553,#184554,#184555,#184556,#184557,#184558,#184559,#184560,#184561,
#184562,#184563,#184564,#184565,#184566,#184567),.UNSPECIFIED.,.F.,.F.,
(4,2,2,2,3,2,2,2,4),(0.356772508105138,0.388713312348931,0.420654116592725,
0.448842124317767,0.477030132042809,0.505218139767852,0.533406147492894,
0.565346951736688,0.597287755980482),.UNSPECIFIED.);
#30314=B_SPLINE_CURVE_WITH_KNOTS('',3,(#184571,#184572,#184573,#184574,
#184575,#184576,#184577,#184578,#184579,#184580,#184581,#184582,#184583,
#184584,#184585,#184586,#184587,#184588,#184589),.UNSPECIFIED.,.F.,.F.,
(4,2,2,2,3,2,2,2,4),(0.35677250810512,0.388713312348932,0.420654116592744,
0.448842124317802,0.477030132042859,0.505218139767916,0.533406147492973,
0.565346951736786,0.597287755980598),.UNSPECIFIED.);
#30315=B_SPLINE_CURVE_WITH_KNOTS('',3,(#184594,#184595,#184596,#184597,
#184598,#184599,#184600,#184601,#184602,#184603,#184604,#184605,#184606,
#184607,#184608,#184609,#184610,#184611),.UNSPECIFIED.,.F.,.F.,(4,2,2,2,
2,2,2,2,4),(-0.357556076431055,-0.326734510063867,-0.29591294369668,-0.266828307459561,
-0.237743671222443,-0.209554730766684,-0.181365790310925,-0.149654062083593,
-0.117942333856261),.UNSPECIFIED.);
#30316=B_SPLINE_CURVE_WITH_KNOTS('',3,(#184618,#184619,#184620,#184621,
#184622,#184623,#184624,#184625,#184626,#184627,#184628,#184629,#184630,
#184631,#184632,#184633,#184634,#184635),.UNSPECIFIED.,.F.,.F.,(4,2,2,2,
2,2,2,2,4),(-0.357558765732128,-0.325847037504796,-0.294135309277465,-0.265946368821705,
-0.237757428365946,-0.208672792128828,-0.17958815589171,-0.148766589524522,
-0.117945023157334),.UNSPECIFIED.);
#30317=B_SPLINE_CURVE_WITH_KNOTS('',3,(#184645,#184646,#184647,#184648,
#184649,#184650,#184651,#184652,#184653,#184654,#184655,#184656,#184657,
#184658,#184659,#184660,#184661,#184662,#184663),.UNSPECIFIED.,.F.,.F.,
(4,2,2,2,3,2,2,2,4),(-0.119801337366205,-0.0880896091388694,-0.0563778809115339,
-0.0281889404557727,-1.15601972439094E-14,0.02818894045575,0.0563778809115115,
0.0880896091388471,0.119801337366183),.UNSPECIFIED.);
#30318=B_SPLINE_CURVE_WITH_KNOTS('',3,(#184675,#184676,#184677,#184678,
#184679,#184680,#184681,#184682,#184683,#184684,#184685,#184686,#184687,
#184688,#184689,#184690,#184691,#184692,#184693),.UNSPECIFIED.,.F.,.F.,
(4,2,2,2,3,2,2,2,4),(-0.119812405208569,-0.0889908388413916,-0.0581692724742138,
-0.0290846362371043,5.25968157916168E-15,0.0281889404557555,0.0563778809115058,
0.0880896091388275,0.119801337366149),.UNSPECIFIED.);
#30319=B_SPLINE_CURVE_WITH_KNOTS('',3,(#184698,#184699,#184700,#184701,
#184702,#184703,#184704,#184705,#184706,#184707,#184708,#184709,#184710,
#184711,#184712,#184713,#184714,#184715,#184716),.UNSPECIFIED.,.F.,.F.,
(4,2,2,2,3,2,2,2,4),(-0.119801337366148,-0.0880896091388235,-0.0563778809114992,
-0.028188940455747,5.14865927669916E-15,0.0290846362371171,0.0581692724742291,
0.0889908388414093,0.11981240520859),.UNSPECIFIED.);
#30320=B_SPLINE_CURVE_WITH_KNOTS('',3,(#184721,#184722,#184723,#184724,
#184725,#184726,#184727,#184728,#184729,#184730,#184731,#184732,#184733,
#184734,#184735,#184736,#184737,#184738,#184739),.UNSPECIFIED.,.F.,.F.,
(4,2,2,2,3,2,2,2,4),(-0.119801337366183,-0.0880896091388476,-0.0563778809115119,
-0.0281889404557501,1.15879528195251E-14,0.0281889404557729,0.0563778809115343,
0.08808960913887,0.119801337366206),.UNSPECIFIED.);
#30321=B_SPLINE_CURVE_WITH_KNOTS('',3,(#184812,#184813,#184814,#184815,
#184816,#184817,#184818,#184819,#184820,#184821,#184822,#184823,#184824,
#184825,#184826,#184827,#184828,#184829,#184830,#184831,#184832,#184833,
#184834,#184835,#184836,#184837,#184838,#184839,#184840,#184841,#184842,
#184843,#184844,#184845,#184846,#184847,#184848,#184849,#184850,#184851,
#184852,#184853,#184854,#184855,#184856,#184857,#184858,#184859,#184860,
#184861,#184862,#184863,#184864,#184865,#184866,#184867),.UNSPECIFIED.,
 .F.,.F.,(4,2,2,2,2,2,2,2,2,2,2,2,2,2,2,2,2,2,2,2,2,2,2,2,2,2,2,4),(1.00000000824441E-6,
0.275071439947967,0.543589949820334,0.726708281005337,0.964982097293981,
1.23327523189536,1.50260089643556,1.77224618743942,2.03912144009645,2.30999928062765,
2.57411052670835,2.84582268677525,3.10783768543331,3.37967001978092,3.6453167716663,
3.9093743140936,4.17506210086737,4.43697141321252,4.70280662599637,4.96284365192071,
5.09444162419176,5.36127414381699,5.62123954982782,5.88473753210837,6.10516180647631,
6.44201482456383,6.60698025662302,6.77613368119588),.UNSPECIFIED.);
#30322=B_SPLINE_CURVE_WITH_KNOTS('',3,(#184871,#184872,#184873,#184874,
#184875,#184876,#184877,#184878,#184879,#184880,#184881,#184882,#184883,
#184884,#184885,#184886,#184887,#184888,#184889,#184890,#184891,#184892,
#184893,#184894,#184895,#184896,#184897,#184898,#184899,#184900,#184901),
 .UNSPECIFIED.,.F.,.F.,(4,3,3,3,3,3,3,3,3,3,4),(0.,0.0699423398648104,0.139991703689476,
0.15887188919288,0.241543521732975,0.317743778385759,0.397179722982199,
0.476615667578639,0.551702197147984,0.590430876649392,0.635487556771519),
 .UNSPECIFIED.);
#30323=B_SPLINE_CURVE_WITH_KNOTS('',3,(#184902,#184903,#184904,#184905,
#184906,#184907),.UNSPECIFIED.,.F.,.F.,(4,2,4),(0.635487559214341,0.817743778385759,
1.),.UNSPECIFIED.);
#30324=B_SPLINE_CURVE_WITH_KNOTS('',3,(#185056,#185057,#185058,#185059,
#185060,#185061,#185062,#185063,#185064,#185065,#185066,#185067,#185068,
#185069,#185070,#185071,#185072,#185073,#185074,#185075,#185076,#185077,
#185078,#185079,#185080,#185081,#185082,#185083,#185084,#185085,#185086,
#185087,#185088,#185089,#185090,#185091,#185092,#185093,#185094,#185095,
#185096,#185097,#185098,#185099,#185100,#185101,#185102,#185103,#185104,
#185105,#185106,#185107,#185108,#185109,#185110,#185111,#185112,#185113,
#185114,#185115,#185116,#185117,#185118,#185119,#185120,#185121,#185122,
#185123,#185124,#185125,#185126,#185127,#185128,#185129,#185130,#185131,
#185132,#185133,#185134,#185135,#185136,#185137,#185138,#185139,#185140,
#185141,#185142,#185143,#185144,#185145,#185146,#185147,#185148,#185149,
#185150,#185151,#185152,#185153,#185154,#185155,#185156,#185157,#185158,
#185159,#185160,#185161,#185162,#185163,#185164,#185165,#185166,#185167,
#185168,#185169,#185170,#185171,#185172,#185173,#185174,#185175,#185176,
#185177,#185178,#185179,#185180,#185181,#185182,#185183,#185184,#185185,
#185186,#185187,#185188,#185189,#185190,#185191,#185192,#185193,#185194,
#185195,#185196,#185197,#185198,#185199,#185200,#185201,#185202,#185203,
#185204,#185205,#185206,#185207,#185208,#185209,#185210,#185211,#185212,
#185213,#185214,#185215,#185216,#185217,#185218,#185219,#185220,#185221,
#185222,#185223,#185224,#185225,#185226,#185227,#185228,#185229,#185230,
#185231,#185232,#185233,#185234,#185235,#185236,#185237,#185238,#185239,
#185240,#185241,#185242,#185243,#185244,#185245,#185246,#185247,#185248,
#185249,#185250,#185251,#185252,#185253,#185254,#185255,#185256,#185257,
#185258,#185259,#185260,#185261,#185262,#185263,#185264,#185265,#185266,
#185267,#185268,#185269,#185270,#185271,#185272,#185273,#185274,#185275,
#185276,#185277,#185278,#185279,#185280,#185281,#185282,#185283,#185284,
#185285,#185286,#185287,#185288,#185289,#185290,#185291,#185292,#185293,
#185294,#185295,#185296,#185297,#185298,#185299,#185300,#185301,#185302,
#185303,#185304,#185305,#185306,#185307,#185308,#185309,#185310,#185311,
#185312,#185313,#185314,#185315,#185316,#185317,#185318,#185319,#185320,
#185321,#185322,#185323,#185324,#185325,#185326,#185327,#185328,#185329,
#185330,#185331,#185332,#185333,#185334,#185335,#185336,#185337,#185338,
#185339,#185340,#185341,#185342,#185343,#185344,#185345,#185346,#185347,
#185348,#185349,#185350,#185351,#185352,#185353,#185354,#185355,#185356,
#185357,#185358,#185359,#185360,#185361,#185362,#185363,#185364,#185365,
#185366,#185367,#185368,#185369,#185370,#185371,#185372,#185373,#185374,
#185375,#185376,#185377,#185378,#185379,#185380,#185381,#185382,#185383,
#185384,#185385,#185386,#185387,#185388,#185389,#185390,#185391,#185392,
#185393,#185394,#185395,#185396,#185397,#185398,#185399,#185400,#185401,
#185402,#185403,#185404,#185405,#185406,#185407,#185408,#185409,#185410,
#185411,#185412,#185413,#185414,#185415,#185416,#185417,#185418,#185419,
#185420,#185421,#185422,#185423,#185424,#185425,#185426,#185427,#185428,
#185429,#185430,#185431,#185432,#185433,#185434,#185435,#185436,#185437,
#185438,#185439,#185440,#185441,#185442,#185443,#185444,#185445,#185446,
#185447,#185448,#185449,#185450,#185451,#185452,#185453,#185454,#185455,
#185456,#185457,#185458,#185459,#185460,#185461,#185462,#185463,#185464,
#185465,#185466,#185467,#185468,#185469,#185470,#185471,#185472,#185473,
#185474,#185475,#185476,#185477,#185478,#185479),.UNSPECIFIED.,.F.,.F.,
(4,2,2,2,2,2,2,2,2,2,2,2,2,2,2,2,2,2,2,2,2,2,2,2,2,2,2,2,2,2,2,2,2,2,2,
2,2,2,2,2,2,2,2,2,2,2,2,2,2,2,2,2,2,2,2,2,2,2,2,2,2,2,2,2,2,2,2,2,2,2,2,
2,2,2,2,2,2,2,2,2,2,2,2,2,2,2,2,2,2,2,2,2,2,2,2,2,2,2,2,2,2,2,2,2,2,2,2,
2,2,2,2,2,2,2,2,2,2,2,2,2,2,2,2,2,2,2,2,2,2,2,2,2,2,2,2,2,2,2,2,2,2,2,2,
2,2,2,2,2,2,2,2,2,2,2,2,2,2,2,2,2,2,2,2,2,2,2,2,2,2,2,2,2,2,2,2,2,2,2,2,
2,2,2,2,2,2,2,2,2,2,2,2,2,2,2,2,2,2,2,2,2,2,2,2,2,2,2,2,2,2,2,2,4),(0.000164533515203592,
0.15574788143604,0.300311425412708,0.569373761758525,0.79618657880448,0.922541857226,
0.988904254887107,1.0653692971268,1.25210389344582,1.42535492735896,1.50265916110143,
1.58851742855532,1.66019897681292,1.7154790824507,1.77355589777661,1.95475787098224,
2.04862650077206,2.12027287069596,2.17286295576569,2.2595637445942,2.34255832444489,
2.38071228733387,2.42149276767208,2.47124766457881,2.6150539169351,2.75087412291449,
2.80056720175112,2.84167674733784,2.98305280903366,3.07138278232828,3.10632890237946,
3.14629868941928,3.22861226113931,3.36258398098612,3.43849932049605,3.47714516706065,
3.51392785473813,3.6117878053805,3.70836592068353,3.76794458464598,3.79962609632322,
3.83743317455229,3.94227692301846,4.04709614636816,4.11179326352921,4.14572233491239,
4.18359857780085,4.2847010418534,4.38923781641045,4.45343794502814,4.48682377962691,
4.52149832706062,4.59643350613506,4.71314948116913,4.76039791117649,4.79937613171105,
4.83531193373953,4.89766444205739,5.05424405055733,5.13467567943698,5.173180257863,
5.20800344399481,5.34491460624367,5.43934749892766,5.47878821833075,5.52559040811516,
5.69013077490027,5.77544264138173,5.8379652638945,5.87889902859667,5.92624035708248,
6.04473759572682,6.09274842224217,6.14285502964907,6.19964912006544,6.36932165795769,
6.46449491795829,6.53568224943887,6.58612340023522,6.68154754770684,6.78172409066983,
6.85266260775808,7.08411900047799,7.18340018586257,7.26475716566072,7.34592524358762,
7.44742089527027,7.57757375930111,7.75796056009403,7.97929905302474,8.09228581444125,
8.61092620220196,8.74282270043409,8.99753184305009,9.23459888874445,9.36815206661486,
9.43329508924799,9.50767505195354,9.73032389966636,9.8365758432595,9.92238613205742,
9.99555986248376,10.0676642998935,10.1467995025813,10.198486501858,10.2778943711568,
10.3930873678413,10.5270230683069,10.5865851703363,10.6386106779327,10.6882622302918,
10.8052544371083,10.851675060425,10.8938848923791,10.9627076822763,11.1735165890948,
11.2332315816838,11.274511843921,11.3258318815358,11.4433870595462,11.5176797599669,
11.5528679247441,11.5915777257815,11.6720238231879,11.8279526244865,11.8919536687505,
11.9287288660531,11.9675433985747,12.014254075755,12.1301965112121,12.2053125480792,
12.2394501915855,12.273327920918,12.3405513281499,12.4550836863104,12.5460185108539,
12.5832819421439,12.6173385791642,12.6864705035049,12.8086815512044,12.8894377209578,
12.9260334996992,12.9579593879317,13.0214163878057,13.1308924188965,13.2132216960653,
13.2493968551011,13.2873945418515,13.3639203976739,13.5033029393173,13.5807831965947,
13.619109048039,13.6543434044654,13.7602592767141,13.8745338706366,13.9152694853788,
13.9596948201189,14.0508765813697,14.2367980478715,14.2906477020263,14.3309772172887,
14.3914972781408,14.5048023767773,14.56371883741,14.6153600973738,14.6966447505308,
14.818385443839,14.9499347785817,15.0060265353982,15.05981889999,15.127586751363,
15.2245099254412,15.2973100920515,15.4691547722829,15.6527398494129,15.7273552713701,
15.7908427662886,15.9217598306892,16.0990554913762,16.4443175652378,16.5617592512692,
17.0838742715074,17.1932159661468,17.3259554357176,17.6060135285824,17.7357461921405,
17.8427816548078,17.9152772018098,18.0124495522896,18.1509017133738,18.296623164564,
18.3725042626396,18.4559825970312,18.5838321615931,18.6358492486316,18.7210910207846,
18.8555132024386,18.9686220505528,19.024120219767,19.0762897095534,19.1802134193937,
19.2520770089242,19.2932612111306,19.3373941271067,19.4249263100775,19.5932635977254,
19.6592373098822,19.7004586930598,19.7463549783324,19.9232344224063,19.9501361012415,
19.9622891784342),.UNSPECIFIED.);
#30325=B_SPLINE_CURVE_WITH_KNOTS('',3,(#185481,#185482,#185483,#185484,
#185485,#185486,#185487,#185488,#185489,#185490,#185491,#185492,#185493,
#185494),.UNSPECIFIED.,.F.,.F.,(4,2,2,2,2,2,4),(2.32621539683198E-5,0.400098729001259,
0.799101480288672,1.34105949117882,1.70265074241555,1.91405386469819,2.12102518490325),
 .UNSPECIFIED.);
#30326=B_SPLINE_CURVE_WITH_KNOTS('',3,(#185496,#185497,#185498,#185499),
 .UNSPECIFIED.,.F.,.F.,(4,4),(0.,0.00660405994458262),.UNSPECIFIED.);
#30327=B_SPLINE_CURVE_WITH_KNOTS('',3,(#185500,#185501,#185502,#185503,
#185504,#185505,#185506,#185507,#185508,#185509,#185510,#185511),
 .UNSPECIFIED.,.F.,.F.,(4,2,2,2,2,4),(-18.1421165145352,-17.9925634623113,
-17.9105025327825,-17.7593505375724,-17.6048012785571,-17.4782773446469),
 .UNSPECIFIED.);
#30328=B_SPLINE_CURVE_WITH_KNOTS('',3,(#185592,#185593,#185594,#185595,
#185596,#185597,#185598,#185599,#185600,#185601,#185602,#185603,#185604,
#185605,#185606,#185607,#185608,#185609,#185610,#185611,#185612,#185613,
#185614,#185615,#185616,#185617,#185618,#185619,#185620,#185621,#185622,
#185623,#185624,#185625,#185626,#185627,#185628,#185629,#185630,#185631,
#185632,#185633,#185634,#185635,#185636,#185637,#185638,#185639,#185640,
#185641,#185642,#185643,#185644,#185645,#185646,#185647,#185648,#185649,
#185650,#185651,#185652,#185653,#185654,#185655,#185656,#185657,#185658,
#185659,#185660,#185661,#185662,#185663,#185664,#185665,#185666,#185667),
 .UNSPECIFIED.,.F.,.F.,(4,2,2,2,2,2,2,2,2,2,2,2,2,2,2,2,2,2,2,2,2,2,2,2,
2,2,2,2,2,2,2,2,2,2,2,2,2,4),(9.5121277628468E-5,0.249595276786102,0.402925412314556,
0.521282340890639,0.751084079383089,1.01658038578886,1.25339646377788,1.50485759578655,
1.610531239197,1.88100328567676,2.1163995971987,2.29305069595439,2.53046871405044,
2.69847868939906,2.96099769965047,3.18389439258267,3.71587281309874,3.92336136867365,
4.12173585205318,4.37630183981309,4.57630326379367,4.67864799639467,4.89141453502725,
5.14664142545471,5.37623130030702,5.71415099752245,5.97637698865336,6.23695400971814,
6.75820129659731,7.01668233427012,7.20065892246672,7.45676982547489,7.98061722365381,
8.24162856837933,8.36890312771966,8.8427719861429,9.08125032492622,9.32032447711697),
 .UNSPECIFIED.);
#30329=B_SPLINE_CURVE_WITH_KNOTS('',3,(#185669,#185670,#185671,#185672,
#185673,#185674,#185675,#185676,#185677,#185678,#185679,#185680,#185681,
#185682,#185683,#185684,#185685,#185686,#185687,#185688,#185689,#185690,
#185691,#185692,#185693,#185694,#185695,#185696,#185697,#185698,#185699,
#185700,#185701,#185702,#185703,#185704,#185705,#185706,#185707,#185708,
#185709,#185710,#185711,#185712,#185713,#185714,#185715,#185716,#185717,
#185718,#185719,#185720,#185721,#185722,#185723,#185724,#185725,#185726,
#185727,#185728,#185729,#185730,#185731,#185732,#185733,#185734,#185735,
#185736,#185737,#185738,#185739,#185740,#185741,#185742,#185743,#185744,
#185745,#185746,#185747,#185748,#185749,#185750,#185751,#185752,#185753,
#185754,#185755,#185756,#185757,#185758,#185759,#185760,#185761,#185762,
#185763,#185764,#185765,#185766,#185767,#185768,#185769,#185770,#185771,
#185772,#185773,#185774,#185775,#185776,#185777,#185778,#185779,#185780,
#185781,#185782,#185783,#185784,#185785,#185786,#185787,#185788,#185789,
#185790,#185791,#185792),.UNSPECIFIED.,.F.,.F.,(4,3,3,3,3,3,3,3,3,3,3,3,
3,3,3,3,3,3,3,3,3,3,3,3,3,3,3,3,3,3,3,3,3,3,3,3,3,3,3,3,3,4),(0.,0.0276914053910685,
0.0664920742418303,0.106600634168667,0.145179304224856,0.175451960403814,
0.183883838061466,0.190699425235669,0.218730858025732,0.239809569979581,
0.247513314271047,0.252696050322163,0.292154019225632,0.331863658139455,
0.371731219090931,0.387360553656524,0.427049658799308,0.467428988434914,
0.485094945150492,0.49455817189996,0.499129004833813,0.502646411513384,
0.541484936161962,0.580472912016988,0.619451931615742,0.658127145790832,
0.681122858545679,0.686905028775457,0.692898726594125,0.719841435153799,
0.734962865518979,0.742523580701569,0.746492661689958,0.74924581130424,
0.750084295884158,0.788114818739895,0.826614366988998,0.86547301495562,
0.90460707319013,0.943746161219805,0.982674727452436,1.),.UNSPECIFIED.);
#30330=B_SPLINE_CURVE_WITH_KNOTS('',3,(#185794,#185795,#185796,#185797),
 .UNSPECIFIED.,.F.,.F.,(4,4),(-0.000360640939376314,0.),.UNSPECIFIED.);
#30331=B_SPLINE_CURVE_WITH_KNOTS('',3,(#185798,#185799,#185800,#185801,
#185802,#185803,#185804,#185805,#185806,#185807,#185808,#185809,#185810,
#185811,#185812,#185813,#185814,#185815,#185816,#185817,#185818,#185819,
#185820,#185821,#185822,#185823,#185824,#185825,#185826,#185827,#185828,
#185829,#185830,#185831,#185832,#185833,#185834,#185835,#185836,#185837,
#185838,#185839,#185840,#185841,#185842,#185843,#185844,#185845,#185846,
#185847,#185848,#185849,#185850,#185851,#185852,#185853,#185854,#185855,
#185856,#185857,#185858,#185859,#185860,#185861,#185862,#185863,#185864,
#185865,#185866,#185867),.UNSPECIFIED.,.F.,.F.,(4,2,2,2,2,2,2,2,2,2,2,2,
2,2,2,2,2,2,2,2,2,2,2,2,2,2,2,2,2,2,2,2,2,2,4),(-6.70530344949381,-6.3523661180227,
-6.21616553242361,-6.05570076631061,-5.86324644351769,-5.75752630293958,
-5.57746835957856,-5.32503153778005,-5.11610470936969,-4.90230388945836,
-4.79773619952221,-4.58648071047068,-4.39330135932084,-4.2188712833661,
-4.11297408472852,-3.97677726421539,-3.84549117665225,-3.71129611429485,
-3.58847537704995,-3.462789093206,-3.26206199633315,-3.11034685614292,-2.83007851493899,
-2.35622475827822,-2.16802485780617,-1.93367740396821,-1.80677119945566,
-1.61140432188186,-1.47961053146882,-1.23439747229975,-1.04314403571828,
-0.901677225570379,-0.45467837226067,-0.229205497357456,-0.00019735943205006),
 .UNSPECIFIED.);
#30332=B_SPLINE_CURVE_WITH_KNOTS('',3,(#186009,#186010,#186011,#186012,
#186013,#186014,#186015,#186016,#186017,#186018,#186019,#186020,#186021,
#186022,#186023,#186024,#186025,#186026,#186027,#186028,#186029,#186030,
#186031,#186032,#186033,#186034,#186035,#186036,#186037,#186038,#186039,
#186040,#186041,#186042,#186043,#186044,#186045,#186046,#186047,#186048,
#186049,#186050,#186051,#186052,#186053,#186054,#186055,#186056,#186057,
#186058,#186059,#186060,#186061,#186062,#186063,#186064,#186065,#186066,
#186067,#186068,#186069,#186070,#186071,#186072,#186073,#186074,#186075,
#186076,#186077,#186078,#186079,#186080,#186081,#186082,#186083,#186084,
#186085,#186086,#186087,#186088,#186089,#186090,#186091,#186092,#186093,
#186094,#186095,#186096,#186097,#186098,#186099,#186100,#186101,#186102,
#186103,#186104,#186105,#186106,#186107,#186108,#186109,#186110,#186111,
#186112,#186113,#186114,#186115,#186116,#186117,#186118,#186119,#186120,
#186121,#186122,#186123,#186124,#186125,#186126,#186127,#186128,#186129,
#186130,#186131,#186132,#186133,#186134,#186135,#186136,#186137,#186138,
#186139,#186140,#186141,#186142,#186143,#186144,#186145,#186146,#186147,
#186148,#186149,#186150,#186151,#186152,#186153,#186154,#186155,#186156,
#186157,#186158,#186159,#186160,#186161,#186162,#186163,#186164,#186165,
#186166,#186167,#186168,#186169,#186170,#186171,#186172,#186173,#186174,
#186175,#186176,#186177,#186178,#186179,#186180,#186181,#186182,#186183,
#186184,#186185,#186186,#186187,#186188,#186189,#186190,#186191,#186192,
#186193,#186194,#186195,#186196,#186197,#186198,#186199,#186200,#186201,
#186202,#186203,#186204,#186205,#186206,#186207,#186208,#186209,#186210,
#186211,#186212,#186213,#186214,#186215,#186216,#186217,#186218,#186219,
#186220,#186221,#186222,#186223,#186224,#186225,#186226,#186227,#186228,
#186229,#186230,#186231,#186232,#186233,#186234,#186235,#186236,#186237,
#186238,#186239,#186240,#186241,#186242,#186243,#186244,#186245,#186246,
#186247,#186248,#186249,#186250,#186251,#186252,#186253,#186254,#186255,
#186256,#186257,#186258,#186259,#186260,#186261,#186262,#186263,#186264,
#186265,#186266,#186267,#186268,#186269,#186270,#186271,#186272,#186273,
#186274,#186275,#186276,#186277,#186278,#186279,#186280,#186281,#186282,
#186283,#186284,#186285,#186286,#186287,#186288,#186289,#186290,#186291,
#186292,#186293,#186294,#186295,#186296,#186297,#186298,#186299,#186300,
#186301,#186302,#186303,#186304,#186305,#186306,#186307,#186308,#186309,
#186310,#186311,#186312,#186313,#186314,#186315,#186316,#186317,#186318,
#186319,#186320,#186321,#186322,#186323,#186324,#186325,#186326,#186327,
#186328,#186329,#186330,#186331,#186332,#186333,#186334,#186335,#186336,
#186337,#186338,#186339,#186340,#186341,#186342,#186343,#186344,#186345,
#186346,#186347,#186348,#186349,#186350,#186351,#186352,#186353,#186354,
#186355,#186356,#186357,#186358,#186359,#186360,#186361,#186362,#186363,
#186364,#186365,#186366,#186367,#186368,#186369,#186370,#186371,#186372,
#186373,#186374,#186375,#186376,#186377,#186378,#186379,#186380,#186381,
#186382,#186383,#186384,#186385,#186386,#186387,#186388,#186389,#186390,
#186391,#186392,#186393,#186394,#186395,#186396,#186397,#186398,#186399,
#186400,#186401,#186402,#186403,#186404,#186405,#186406,#186407,#186408,
#186409,#186410,#186411,#186412,#186413,#186414,#186415,#186416,#186417,
#186418,#186419,#186420,#186421,#186422,#186423,#186424,#186425,#186426,
#186427,#186428),.UNSPECIFIED.,.F.,.F.,(4,2,2,2,2,2,2,2,2,2,2,2,2,2,2,2,
2,2,2,2,2,2,2,2,2,2,2,2,2,2,2,2,2,2,2,2,2,2,2,2,2,2,2,2,2,2,2,2,2,2,2,2,
2,2,2,2,2,2,2,2,2,2,2,2,2,2,2,2,2,2,2,2,2,2,2,2,2,2,2,2,2,2,2,2,2,2,2,2,
2,2,2,2,2,2,2,2,2,2,2,2,2,2,2,2,2,2,2,2,2,2,2,2,2,2,2,2,2,2,2,2,2,2,2,2,
2,2,2,2,2,2,2,2,2,2,2,2,2,2,2,2,2,2,2,2,2,2,2,2,2,2,2,2,2,2,2,2,2,2,2,2,
2,2,2,2,2,2,2,2,2,2,2,2,2,2,2,2,2,2,2,2,2,2,2,2,2,2,2,2,2,2,2,2,2,2,2,2,
2,2,2,2,2,2,2,2,2,2,2,2,2,4),(-21.8329251448155,-21.6443827645098,-21.5732407549653,
-21.4937793564471,-21.3036935948802,-21.1950255432799,-21.1302502295424,
-21.0062043365996,-20.8956464117004,-20.8495843915274,-20.7926915242238,
-20.6645775558975,-20.586408714092,-20.461637530838,-20.3595427854041,-20.1985602066991,
-20.1453544408803,-20.1043960712606,-19.9756229159482,-19.88814467434,-19.7911012649131,
-19.6507351841967,-19.5093899344014,-19.453489464351,-19.4080492880456,
-19.3489994344965,-19.2040163537948,-19.1434388099925,-19.0805936762193,
-18.979017836747,-18.8094306948228,-18.7128296685487,-18.6460413514842,
-18.4771673378652,-18.3721213587991,-18.3156755479724,-18.178125879852,
-18.0491151473622,-17.9981253909182,-17.8584086914978,-17.6688254349913,
-17.5859758529825,-17.499684076209,-17.3848610015013,-17.3166647400089,
-17.2760782035752,-17.1634007314228,-16.9970020382501,-16.8804829120801,
-16.7477798300899,-16.6501523196607,-16.5908288232001,-16.5497170959436,
-16.4140180509483,-16.3021699235238,-16.2150863070732,-16.0601667092189,
-15.9286097189282,-15.8821907279592,-15.8348094666183,-15.6531777111572,
-15.5555277630453,-15.4953667835224,-15.3410430155883,-15.2004015569117,
-15.1344094696977,-14.9371678957363,-14.8106943984559,-14.7503347499441,
-14.5949231760321,-14.4884550179283,-14.4425584435066,-14.3184945675219,
-14.1167954208962,-14.0221544659323,-13.9217386657594,-13.8199513853057,
-13.7569930854452,-13.7172190677987,-13.5899115647471,-13.4860952228305,
-13.3750486109775,-13.2342883034089,-13.1168722215261,-13.0613073120677,
-13.0168955754192,-12.9641889276144,-12.8257016274758,-12.7630104237111,
-12.6931293473043,-12.5847956599781,-12.3954142745935,-12.3361766735367,
-12.2835030511139,-12.0937418228578,-11.989663675477,-11.9333618005977,
-11.7821776465091,-11.650065948291,-11.5942783726521,-11.4372704510442,
-11.2704115699778,-11.1981389409495,-11.1116287657827,-10.9954416907346,
-10.943180460361,-10.8982455627616,-10.8381247965561,-10.7311394039421,
-10.5639880855157,-10.4583057422459,-10.3283572843291,-10.2186298399277,
-10.1786771935202,-10.1232450305456,-10.0430232151756,-9.92337233040851,
-9.82627804394939,-9.65433544558044,-9.51106261477267,-9.46485794953245,
-9.40667614441514,-9.18485385318469,-9.12078871442883,-8.96331818580267,
-8.79330185738388,-8.7314749974436,-8.60391771326453,-8.45958860209339,
-8.39713249969306,-8.32340459424354,-8.2095325045695,-8.12349454627661,
-8.06899666183474,-7.97971801445844,-7.75403315050388,-7.66186828080559,
-7.5850840797206,-7.49406962693947,-7.39953238386288,-7.35521010723848,
-7.30425096509559,-7.07833953163658,-6.96035821501014,-6.83011103593677,
-6.68586967100914,-6.64055674783179,-6.59308766991904,-6.53375843097421,
-6.35873389077308,-6.27162098010247,-6.07877227115871,-5.94418030597099,
-5.89639674667542,-5.78250149271391,-5.63100810747453,-5.57357436413799,
-5.46781284842467,-5.29426621008378,-5.22427614936901,-5.13033477719018,
-4.97823105212994,-4.87430784643472,-4.81377783645382,-4.75822182974962,
-4.6332498800261,-4.55442529116533,-4.50942665398307,-4.42683325193232,
-4.1847708687164,-4.08929937501717,-3.98367052808113,-3.8364247733426,-3.79671297631128,
-3.73331902314079,-3.62334590164148,-3.50865127727065,-3.39372167724177,
-3.22019220688821,-3.11571682197365,-3.07415734032848,-3.00045509449745,
-2.86858467446023,-2.79450504880198,-2.71346183938156,-2.61417115195599,
-2.3937657849274,-2.33641916099488,-2.2671746271922,-2.10622552046567,-2.04086190697162,
-1.97500729742979,-1.88805238173785,-1.7243916329033,-1.66967464879849,
-1.50861406559062,-1.34057573516499,-1.26894107176565,-1.16016163255503,
-1.02030806014582,-0.976593745862524,-0.915928188220698,-0.8064189356607,
-0.646691593117389,-0.542287460916897,-0.401621152798373,-0.299052515077757,
-0.258763143589947,-0.203698819625743,-0.0115231415835987),
 .UNSPECIFIED.);
#30333=B_SPLINE_CURVE_WITH_KNOTS('',3,(#186430,#186431,#186432,#186433,
#186434,#186435,#186436,#186437,#186438,#186439,#186440,#186441,#186442,
#186443,#186444,#186445,#186446,#186447,#186448,#186449,#186450,#186451,
#186452,#186453,#186454,#186455,#186456,#186457,#186458,#186459,#186460,
#186461,#186462,#186463,#186464,#186465,#186466,#186467,#186468,#186469,
#186470,#186471,#186472,#186473,#186474,#186475,#186476,#186477,#186478,
#186479,#186480,#186481,#186482,#186483,#186484,#186485,#186486,#186487,
#186488,#186489,#186490,#186491,#186492,#186493,#186494,#186495,#186496,
#186497,#186498,#186499,#186500,#186501,#186502,#186503,#186504,#186505,
#186506,#186507,#186508,#186509,#186510,#186511,#186512,#186513,#186514,
#186515,#186516,#186517,#186518,#186519,#186520,#186521,#186522,#186523,
#186524,#186525,#186526,#186527,#186528,#186529,#186530,#186531,#186532,
#186533,#186534,#186535,#186536,#186537,#186538,#186539,#186540,#186541,
#186542,#186543,#186544,#186545,#186546,#186547,#186548,#186549,#186550,
#186551,#186552,#186553,#186554,#186555,#186556,#186557,#186558,#186559,
#186560,#186561,#186562,#186563,#186564,#186565,#186566,#186567,#186568,
#186569,#186570,#186571,#186572,#186573,#186574,#186575,#186576,#186577,
#186578,#186579,#186580),.UNSPECIFIED.,.F.,.F.,(4,3,3,3,3,3,3,3,3,3,3,3,
3,3,3,3,3,3,3,3,3,3,3,3,3,3,3,3,3,3,3,3,3,3,3,3,3,3,3,3,3,3,3,3,3,3,3,3,
3,3,4),(0.,0.0392866652558998,0.0785456651531797,0.0880372583011311,0.0920278542607797,
0.0956231269293492,0.112912484515642,0.122437251525716,0.124969665134475,
0.127473761529773,0.164063235736105,0.200668571059852,0.227798128282118,
0.24236056777765,0.248093420263772,0.252685719858583,0.297930728075632,
0.343215831814716,0.365856436119722,0.383101361047376,0.417705028837983,
0.443984982286002,0.46862243864352,0.471549913649985,0.488617603051972,
0.499949749118747,0.502163791399289,0.545535599660173,0.588876763877804,
0.620040203893865,0.624334132892357,0.628034909772857,0.667089344334197,
0.677782778063702,0.685552586199097,0.690858618578248,0.716899516151074,
0.74283750634619,0.747597535630855,0.750418042766665,0.789527071692462,
0.801691374770918,0.81061815205851,0.816126459479278,0.838184284006286,
0.85757334010825,0.874944966513778,0.879852174093526,0.919450746518562,
0.959062655278241,0.993296732821997),.UNSPECIFIED.);
#30334=B_SPLINE_CURVE_WITH_KNOTS('',3,(#186581,#186582,#186583,#186584),
 .UNSPECIFIED.,.F.,.F.,(4,4),(0.,0.00140322528949482),.UNSPECIFIED.);
#30335=B_SPLINE_CURVE_WITH_KNOTS('',3,(#186616,#186617,#186618,#186619),
 .UNSPECIFIED.,.F.,.F.,(4,4),(0.,0.00269304460844964),.UNSPECIFIED.);
#30336=B_SPLINE_CURVE_WITH_KNOTS('',3,(#186620,#186621,#186622,#186623,
#186624,#186625,#186626,#186627,#186628,#186629,#186630,#186631,#186632,
#186633),.UNSPECIFIED.,.F.,.F.,(4,2,2,2,2,2,4),(0.000161979881089482,0.400873717312025,
0.801763578870112,1.29477100198553,1.7630975899284,2.11375019375441,2.46863362347642),
 .UNSPECIFIED.);
#30337=B_SPLINE_CURVE_WITH_KNOTS('',3,(#186981,#186982,#186983,#186984,
#186985,#186986),.UNSPECIFIED.,.F.,.F.,(4,2,4),(-0.194208713167773,-0.0971361853452758,
-3.86117433745282E-5),.UNSPECIFIED.);
#30338=B_SPLINE_CURVE_WITH_KNOTS('',3,(#187064,#187065,#187066,#187067,
#187068,#187069),.UNSPECIFIED.,.F.,.F.,(4,2,4),(-0.194199485947135,-0.0971172181367527,
-0.00177501603400677),.UNSPECIFIED.);
#30339=B_SPLINE_CURVE_WITH_KNOTS('',3,(#187070,#187071,#187072,#187073),
 .UNSPECIFIED.,.F.,.F.,(4,4),(-0.00170970345529554,0.),.UNSPECIFIED.);
#30340=B_SPLINE_CURVE_WITH_KNOTS('',3,(#203972,#203973,#203974,#203975,
#203976,#203977,#203978,#203979,#203980,#203981,#203982,#203983,#203984,
#203985,#203986,#203987,#203988,#203989,#203990,#203991,#203992,#203993,
#203994,#203995,#203996,#203997,#203998,#203999,#204000,#204001,#204002,
#204003,#204004,#204005,#204006,#204007,#204008,#204009,#204010,#204011,
#204012,#204013,#204014,#204015,#204016,#204017,#204018,#204019,#204020,
#204021,#204022,#204023,#204024,#204025,#204026,#204027,#204028,#204029,
#204030,#204031,#204032,#204033,#204034,#204035),.UNSPECIFIED.,.F.,.F.,
(4,2,2,2,2,2,2,2,2,2,2,2,2,2,2,2,2,2,2,2,2,2,2,2,2,2,2,2,2,2,2,4),(-23.4687033631746,
-23.3852838488551,-23.2308554847859,-23.0393647019256,-22.8498155999754,
-22.652833031898,-22.315915647242,-22.1130911030338,-21.9105460832706,-21.8118793336342,
-21.502550365139,-21.4036127891307,-21.0871228937064,-20.9089890751837,
-20.7563727831538,-20.5652998484044,-20.3758816924102,-20.1791368906873,
-19.7735353482811,-19.3679961261668,-19.0912031493949,-18.8269861994187,
-18.682485974505,-18.4754244900494,-18.3751033651293,-18.1841021938767,
-18.0344520619974,-17.8766239737055,-17.6844266758722,-17.4946282500565,
-17.2972509069455,-17.0172746992294),.UNSPECIFIED.);
#30341=B_SPLINE_CURVE_WITH_KNOTS('',3,(#204042,#204043,#204044,#204045,
#204046,#204047,#204048,#204049,#204050,#204051,#204052,#204053,#204054,
#204055,#204056,#204057,#204058,#204059,#204060,#204061,#204062,#204063),
 .UNSPECIFIED.,.F.,.F.,(4,2,2,2,2,2,2,2,2,2,4),(-25.3610794444717,-25.215820953514,
-25.0739186005887,-24.7915033253179,-24.6197089966247,-24.4661941325765,
-24.2748584769765,-24.0853564193073,-23.8884542762642,-23.5522025045507,
-23.4687033631746),.UNSPECIFIED.);
#30342=B_SPLINE_CURVE_WITH_KNOTS('',3,(#204065,#204066,#204067,#204068,
#204069,#204070,#204071,#204072,#204073,#204074,#204075,#204076),
 .UNSPECIFIED.,.F.,.F.,(4,2,2,2,2,4),(0.,0.250779295927707,0.498420132328089,
0.665822634254374,0.997622742450792,1.33240355331691),.UNSPECIFIED.);
#30343=B_SPLINE_CURVE_WITH_KNOTS('',3,(#204078,#204079,#204080,#204081,
#204082,#204083,#204084,#204085,#204086,#204087),.UNSPECIFIED.,.F.,.F.,
(4,2,2,2,4),(1.00000001498937E-6,0.17890870313992,0.360010001015776,0.541048047587083,
0.720025159562802),.UNSPECIFIED.);
#30344=B_SPLINE_CURVE_WITH_KNOTS('',3,(#204091,#204092,#204093,#204094,
#204095,#204096,#204097,#204098,#204099,#204100),.UNSPECIFIED.,.F.,.F.,
(4,2,2,2,4),(9.72076722375712E-6,0.1792358276481,0.360521578492281,0.541895207425263,
0.721026938707022),.UNSPECIFIED.);
#30345=B_SPLINE_CURVE_WITH_KNOTS('',3,(#204102,#204103,#204104,#204105,
#204106,#204107,#204108,#204109,#204110,#204111,#204112,#204113),
 .UNSPECIFIED.,.F.,.F.,(4,2,2,2,2,4),(4.89083575497185E-5,0.33528796581701,
0.667578151924638,0.835217190795273,1.08321230565051,1.33434816674587),
 .UNSPECIFIED.);
#30346=B_SPLINE_CURVE_WITH_KNOTS('',3,(#204114,#204115,#204116,#204117,
#204118,#204119,#204120,#204121,#204122,#204123,#204124,#204125,#204126,
#204127,#204128,#204129,#204130,#204131,#204132,#204133,#204134,#204135,
#204136,#204137),.UNSPECIFIED.,.F.,.F.,(4,2,2,2,2,2,2,2,2,2,2,4),(-1.8922192761269,
-1.82208104036279,-1.72310272792682,-1.57263894437134,-1.37868950925003,
-1.09799372962318,-0.944358317890287,-0.741461864009143,-0.570015728206036,
-0.287462712367492,-0.145517952353573,-0.000222633823225556),
 .UNSPECIFIED.);
#30347=B_SPLINE_CURVE_WITH_KNOTS('',3,(#204142,#204143,#204144,#204145,
#204146,#204147,#204148,#204149,#204150,#204151,#204152,#204153,#204154,
#204155,#204156,#204157,#204158,#204159,#204160,#204161,#204162,#204163,
#204164,#204165,#204166,#204167,#204168,#204169,#204170,#204171,#204172,
#204173,#204174,#204175,#204176,#204177,#204178,#204179,#204180,#204181,
#204182,#204183,#204184,#204185,#204186,#204187,#204188,#204189,#204190,
#204191,#204192,#204193,#204194,#204195,#204196,#204197,#204198,#204199,
#204200,#204201,#204202,#204203,#204204,#204205,#204206,#204207,#204208,
#204209,#204210,#204211),.UNSPECIFIED.,.F.,.F.,(4,2,2,2,2,2,2,2,2,2,2,2,
2,2,2,2,2,2,2,2,2,2,2,2,2,2,2,2,2,2,2,2,2,2,4),(-17.0172746992294,-16.9570341593048,
-16.792101803634,-16.6373190264763,-16.4457456987925,-16.2561661420914,
-16.0591346632691,-15.7218448464861,-15.5190147192512,-15.3164628814597,
-15.1613876841587,-15.0618956354682,-14.6562439169265,-14.2510449276501,
-14.0643280509466,-13.9112414278334,-13.7081367905437,-13.549089547108,
-13.2661265111997,-13.0733681568302,-12.9227481717328,-12.8230280772896,
-12.6800940302714,-12.5372991613764,-12.3424755693224,-12.2420612363616,
-12.0263381283204,-11.8746885503234,-11.6898041466877,-11.487305003181,
-11.1798393325958,-11.000772028645,-10.7623483749487,-10.5732527961531,
-10.5668376876055),.UNSPECIFIED.);
#30348=B_SPLINE_CURVE_WITH_KNOTS('',3,(#204212,#204213,#204214,#204215,
#204216,#204217,#204218,#204219,#204220,#204221,#204222,#204223,#204224,
#204225,#204226,#204227,#204228,#204229,#204230,#204231,#204232,#204233,
#204234,#204235,#204236,#204237,#204238,#204239,#204240,#204241,#204242,
#204243,#204244,#204245,#204246,#204247,#204248,#204249,#204250,#204251,
#204252,#204253,#204254,#204255,#204256,#204257,#204258,#204259,#204260,
#204261,#204262,#204263,#204264,#204265,#204266,#204267,#204268,#204269,
#204270,#204271,#204272,#204273,#204274,#204275,#204276,#204277,#204278,
#204279),.UNSPECIFIED.,.F.,.F.,(4,2,2,2,2,2,2,2,2,2,2,2,2,2,2,2,2,2,2,2,
2,2,2,2,2,2,2,2,2,2,2,2,2,4),(-8.34223146287018,-8.2437468689296,-8.1445331304528,
-8.00277428460089,-7.90363519637987,-7.75312469070092,-7.55950114862038,
-7.27821172189581,-7.123201953391,-6.92024992819774,-6.75401545855723,-6.41641697923769,
-6.21935513267499,-6.02975645077751,-5.83812241235353,-5.68302985602848,
-5.51983283504851,-5.17607855273823,-4.77054981706035,-4.57406021893795,
-4.3847652397882,-4.19413112242747,-4.04325574447564,-3.8525494370582,-3.56528972580251,
-3.39427279588752,-3.12386295022243,-2.92760142092666,-2.73840859284267,
-2.55306289660506,-2.40680761858462,-2.16930160980798,-1.96607832439979,
-1.8922192761269),.UNSPECIFIED.);
#30349=B_SPLINE_CURVE_WITH_KNOTS('',3,(#204284,#204285,#204286,#204287,
#204288,#204289,#204290,#204291,#204292,#204293,#204294,#204295,#204296,
#204297,#204298,#204299,#204300,#204301,#204302,#204303,#204304,#204305,
#204306,#204307,#204308,#204309,#204310,#204311,#204312,#204313,#204314,
#204315,#204316,#204317,#204318,#204319,#204320,#204321,#204322,#204323,
#204324,#204325,#204326,#204327,#204328,#204329,#204330,#204331,#204332,
#204333,#204334,#204335,#204336,#204337,#204338,#204339,#204340,#204341,
#204342,#204343,#204344,#204345,#204346,#204347),.UNSPECIFIED.,.F.,.F.,
(4,2,2,2,2,2,2,2,2,2,2,2,2,2,2,2,2,2,2,2,2,2,2,2,2,2,2,2,2,2,2,4),(-10.5668376876055,
-10.3695145546731,-10.209549091418,-10.0687533668579,-9.96852459979405,
-9.81829531262626,-9.62238319389152,-9.41979214179699,-9.16391241020837,
-8.89180940188572,-8.69451601949468,-8.5047725837468,-8.3127197684882,-8.15558944526667,
-8.00275113624896,-7.81574606685221,-7.41056799669842,-7.00492097173905,
-6.90542366392111,-6.74999661874291,-6.43214336167413,-6.3331580848781,
-6.13066135698989,-5.81906147311646,-5.63291565467514,-5.47685015982526,
-5.27386467844866,-5.11127794339281,-4.7662573920237,-4.3606919703882,-4.164031884149,
-4.11510768846113),.UNSPECIFIED.);
#30350=B_SPLINE_CURVE_WITH_KNOTS('',3,(#204348,#204349,#204350,#204351,
#204352,#204353,#204354,#204355,#204356,#204357,#204358,#204359,#204360,
#204361,#204362,#204363,#204364,#204365,#204366,#204367,#204368,#204369,
#204370,#204371,#204372,#204373,#204374,#204375,#204376,#204377,#204378,
#204379,#204380,#204381,#204382,#204383,#204384,#204385,#204386,#204387,
#204388,#204389,#204390,#204391,#204392,#204393,#204394,#204395,#204396,
#204397,#204398,#204399,#204400,#204401,#204402,#204403,#204404,#204405,
#204406,#204407,#204408,#204409,#204410,#204411,#204412,#204413),
 .UNSPECIFIED.,.F.,.F.,(4,2,2,2,2,2,2,2,2,2,2,2,2,2,2,2,2,2,2,2,2,2,2,2,
2,2,2,2,2,2,2,2,4),(-14.7941896039958,-14.7907288342538,-14.6014565735193,
-14.4050047082297,-13.999485821835,-13.6559995232801,-13.4926811791532,
-13.3376171268456,-13.1187143338417,-13.0182737576245,-12.8221486482289,
-12.6797078495678,-12.5371531258208,-12.437175717494,-12.2865086245459,
-12.0941605946292,-11.8104011366496,-11.6492897792206,-11.4461076163316,
-11.299077152733,-11.1046903401399,-11.0042879555534,-10.789600296376,-10.6389655833835,
-10.4463614481799,-10.1631164110068,-10.0033311713694,-9.80020187469263,
-9.64934811132958,-9.45988021821959,-9.05486186397317,-8.64923209009487,
-8.34223146287018),.UNSPECIFIED.);
#30351=B_SPLINE_CURVE_WITH_KNOTS('',3,(#204419,#204420,#204421,#204422,
#204423,#204424,#204425,#204426,#204427,#204428,#204429,#204430,#204431,
#204432,#204433,#204434,#204435,#204436,#204437,#204438,#204439,#204440,
#204441,#204442,#204443,#204444),.UNSPECIFIED.,.F.,.F.,(4,2,2,2,2,2,2,2,
2,2,2,2,4),(-25.358128575953,-25.2282057716136,-25.1006369562764,-24.8605143713168,
-24.6990322666366,-24.4301037612475,-24.1855417081035,-23.9829494758163,
-23.7841984111289,-23.6343112149622,-23.4204024134121,-23.2450169133133,
-23.0216689529943),.UNSPECIFIED.);
#30352=B_SPLINE_CURVE_WITH_KNOTS('',3,(#204445,#204446,#204447,#204448,
#204449,#204450,#204451,#204452,#204453,#204454,#204455,#204456,#204457,
#204458,#204459,#204460,#204461,#204462,#204463,#204464,#204465,#204466,
#204467,#204468,#204469,#204470,#204471,#204472,#204473,#204474,#204475,
#204476,#204477,#204478,#204479,#204480,#204481,#204482,#204483,#204484),
 .UNSPECIFIED.,.F.,.F.,(4,2,2,2,2,2,2,2,2,2,2,2,2,2,2,2,2,2,2,4),(-4.11510768846113,
-3.97465611214066,-3.78372531762154,-3.63167160766886,-3.44970718078692,
-3.13906620947007,-3.04035407326069,-2.72332235910956,-2.62436848539607,
-2.42186942376738,-2.2191087758114,-2.01653460754979,-1.63854808421647,
-1.23292144483628,-0.827416533095915,-0.728204201083642,-0.586019509433464,
-0.293840301528918,-0.148831020870704,-5.5569436307398E-6),
 .UNSPECIFIED.);
#30353=B_SPLINE_CURVE_WITH_KNOTS('',3,(#204485,#204486,#204487,#204488,
#204489,#204490,#204491,#204492,#204493,#204494,#204495,#204496,#204497,
#204498,#204499,#204500,#204501,#204502,#204503,#204504,#204505,#204506,
#204507,#204508,#204509,#204510,#204511,#204512,#204513,#204514,#204515,
#204516,#204517,#204518,#204519,#204520,#204521,#204522,#204523,#204524,
#204525,#204526,#204527,#204528,#204529,#204530,#204531,#204532,#204533,
#204534,#204535,#204536,#204537,#204538,#204539,#204540,#204541,#204542,
#204543,#204544,#204545,#204546,#204547,#204548,#204549,#204550),
 .UNSPECIFIED.,.F.,.F.,(4,2,2,2,2,2,2,2,2,2,2,2,2,2,2,2,2,2,2,2,2,2,2,2,
2,2,2,2,2,2,2,2,4),(-21.2441617485895,-21.070587928597,-20.9234573689237,
-20.8241336310768,-20.4185450674067,-20.0459830102852,-19.8434197686704,
-19.6692135233886,-19.4663449269589,-19.2438763143868,-19.0963949961391,
-18.90938123838,-18.7201711314077,-18.5238604605068,-18.1923834699827,-18.0229719748758,
-17.8689758692299,-17.5844471973557,-17.3819988020371,-17.2827921156069,
-17.0133277526635,-16.7668635407395,-16.6212559306274,-16.4125806174337,
-16.3122464198425,-16.1205036043305,-15.9714483969571,-15.7683020315977,
-15.6079042345084,-15.324423539191,-15.1319451009706,-14.9813001926369,
-14.7941896039958),.UNSPECIFIED.);
#30354=B_SPLINE_CURVE_WITH_KNOTS('',3,(#204555,#204556,#204557,#204558,
#204559,#204560,#204561,#204562,#204563,#204564,#204565,#204566,#204567,
#204568,#204569,#204570,#204571,#204572,#204573,#204574,#204575,#204576,
#204577,#204578,#204579,#204580,#204581,#204582,#204583,#204584,#204585,
#204586,#204587,#204588,#204589,#204590,#204591,#204592,#204593,#204594,
#204595,#204596,#204597,#204598,#204599,#204600,#204601,#204602,#204603,
#204604,#204605,#204606,#204607,#204608,#204609,#204610,#204611,#204612,
#204613,#204614,#204615,#204616,#204617,#204618,#204619,#204620,#204621,
#204622),.UNSPECIFIED.,.F.,.F.,(4,2,2,2,2,2,2,2,2,2,2,2,2,2,2,2,2,2,2,2,
2,2,2,2,2,2,2,2,2,2,2,2,2,4),(-23.0216689529943,-22.9399958735644,-22.7375037591772,
-22.5521572389522,-22.4005761281261,-22.1849223594256,-22.0845124981317,
-21.8897176262462,-21.6961038208106,-21.4935285235385,-21.3206979684953,
-21.1178183959759,-20.9646317914223,-20.6841456784191,-20.490099223666,
-20.3396486032863,-20.2408119398105,-20.048836819849,-19.8462725323272,
-19.6730062813175,-19.5196477425073,-19.3284088871973,-19.1389480903071,
-18.9421137731765,-18.5365182788126,-18.2626806906338,-18.0031887816691,
-17.8006076556692,-17.6055964822867,-17.4552678130184,-17.2409037369228,
-17.0654526175782,-16.7603904867758,-16.572626139466),.UNSPECIFIED.);
#30355=B_SPLINE_CURVE_WITH_KNOTS('',3,(#204624,#204625,#204626,#204627,
#204628,#204629,#204630,#204631,#204632,#204633,#204634,#204635,#204636,
#204637,#204638,#204639,#204640,#204641,#204642,#204643,#204644,#204645,
#204646,#204647,#204648,#204649,#204650,#204651,#204652,#204653,#204654,
#204655,#204656,#204657,#204658,#204659,#204660,#204661,#204662,#204663),
 .UNSPECIFIED.,.F.,.F.,(4,2,2,2,2,2,2,2,2,2,2,2,2,2,2,2,2,2,2,4),(-25.3597291394773,
-25.2285499994245,-25.099819969673,-24.8569096210103,-24.6946723481893,
-24.3848163488543,-24.2859059766642,-23.9700785764519,-23.7915143928961,
-23.6389722847768,-23.4479188760001,-23.2585105543305,-23.0617791374454,
-22.6561917407724,-22.3106553070311,-22.1617955868105,-22.0624360532406,
-21.6568261998587,-21.2513780415546,-21.2441617485895),.UNSPECIFIED.);
#30356=B_SPLINE_CURVE_WITH_KNOTS('',3,(#204664,#204665,#204666,#204667,
#204668,#204669,#204670,#204671,#204672,#204673,#204674,#204675,#204676,
#204677,#204678,#204679,#204680,#204681,#204682,#204683,#204684,#204685,
#204686,#204687,#204688,#204689),.UNSPECIFIED.,.F.,.F.,(4,2,2,2,2,2,2,2,
2,2,2,2,4),(-2.33658628848224,-2.10644543766237,-1.91798466615612,-1.74806681040746,
-1.47807527992586,-1.28215067339681,-1.09308272844972,-0.889352076714527,
-0.730281318729365,-0.586371993056161,-0.293984893799743,-0.14890606456612,
-5.55694363607431E-6),.UNSPECIFIED.);
#30357=B_SPLINE_CURVE_WITH_KNOTS('',3,(#204694,#204695,#204696,#204697,
#204698,#204699,#204700,#204701,#204702,#204703,#204704,#204705,#204706,
#204707,#204708,#204709,#204710,#204711,#204712,#204713,#204714,#204715,
#204716,#204717,#204718,#204719,#204720,#204721,#204722,#204723,#204724,
#204725,#204726,#204727,#204728,#204729,#204730,#204731,#204732,#204733,
#204734,#204735,#204736,#204737,#204738,#204739,#204740,#204741,#204742,
#204743,#204744,#204745,#204746,#204747,#204748,#204749,#204750,#204751,
#204752,#204753,#204754,#204755,#204756,#204757,#204758,#204759),
 .UNSPECIFIED.,.F.,.F.,(4,2,2,2,2,2,2,2,2,2,2,2,2,2,2,2,2,2,2,2,2,2,2,2,
2,2,2,2,2,2,2,2,4),(-16.572626139466,-16.5579064723409,-16.4588708780629,
-16.189728250312,-16.0236918146546,-15.8358602520613,-15.6400498510376,
-15.3125659356413,-15.1409698691107,-14.987336698355,-14.7960302402308,
-14.6065447833013,-14.4096696235586,-14.0040574873121,-13.7301365342186,
-13.4704980259158,-13.2679112814905,-13.0729287155005,-12.9225917833455,
-12.8244358269876,-12.6792390808328,-12.5343267001255,-12.3468510891694,
-11.941714258584,-11.5360819504349,-11.4365769701358,-11.2806264452415,
-10.964592008435,-10.8656781544007,-10.5558023852578,-10.4571215809503,
-10.1390736746432,-10.1206942749107),.UNSPECIFIED.);
#30358=B_SPLINE_CURVE_WITH_KNOTS('',3,(#204760,#204761,#204762,#204763,
#204764,#204765,#204766,#204767,#204768,#204769,#204770,#204771,#204772,
#204773,#204774,#204775,#204776,#204777,#204778,#204779,#204780,#204781,
#204782,#204783,#204784,#204785,#204786,#204787,#204788,#204789,#204790,
#204791,#204792,#204793,#204794,#204795,#204796,#204797,#204798,#204799,
#204800,#204801,#204802,#204803,#204804,#204805,#204806,#204807,#204808,
#204809,#204810,#204811,#204812,#204813,#204814,#204815,#204816,#204817,
#204818,#204819,#204820,#204821,#204822,#204823,#204824,#204825,#204826,
#204827),.UNSPECIFIED.,.F.,.F.,(4,2,2,2,2,2,2,2,2,2,2,2,2,2,2,2,2,2,2,2,
2,2,2,2,2,2,2,2,2,2,2,2,2,4),(-8.78547365602618,-8.69348451276142,-8.5041269058269,
-8.31327657074127,-8.16156881945659,-7.97709475252234,-7.77459226543236,
-7.46494243339529,-7.28228169534135,-7.14413707085143,-6.94154150864123,
-6.69020367748547,-6.41969738046043,-6.22336323422511,-6.03413591023072,
-5.84650660349539,-5.69854632462125,-5.48123669444399,-5.27845229594527,
-5.09164011359389,-4.88915281314924,-4.59150589507809,-4.42554170215773,
-4.2606008691664,-4.05800247084799,-3.80526013087876,-3.53432581759653,
-3.33769514728129,-3.14832978216314,-2.95745696485319,-2.80566562102031,
-2.62178165020044,-2.41927475517814,-2.33658628848224),.UNSPECIFIED.);
#30359=B_SPLINE_CURVE_WITH_KNOTS('',3,(#204832,#204833,#204834,#204835,
#204836,#204837,#204838,#204839,#204840,#204841,#204842,#204843,#204844,
#204845,#204846,#204847,#204848,#204849,#204850,#204851,#204852,#204853,
#204854,#204855,#204856,#204857,#204858,#204859,#204860,#204861,#204862,
#204863,#204864,#204865,#204866,#204867,#204868,#204869,#204870,#204871,
#204872,#204873,#204874,#204875,#204876,#204877,#204878,#204879,#204880,
#204881,#204882,#204883,#204884,#204885,#204886,#204887,#204888,#204889,
#204890,#204891,#204892,#204893,#204894,#204895),.UNSPECIFIED.,.F.,.F.,
(4,2,2,2,2,2,2,2,2,2,2,2,2,2,2,2,2,2,2,2,2,2,2,2,2,2,2,2,2,2,2,4),(-10.1206942749107,
-10.0400839521642,-9.83759471021484,-9.52699477320647,-9.34264981477488,
-9.19621348106729,-8.99352683439908,-8.79166491131934,-8.5890659650105,
-8.35566614364774,-8.15254681303885,-8.0011384430874,-7.81236926147717,
-7.40730673342809,-7.00167445589182,-6.90213798484658,-6.74473748892279,
-6.43338739195136,-6.33464876950753,-6.01857571089482,-5.91965836156433,
-5.60981558607575,-5.51113398519595,-5.19302395275696,-5.09402985252356,
-4.8915360684116,-4.58119198016509,-4.39730850756027,-4.25322027900818,
-4.05057562847383,-3.83652325505148,-3.66932922096601),.UNSPECIFIED.);
#30360=B_SPLINE_CURVE_WITH_KNOTS('',3,(#204896,#204897,#204898,#204899,
#204900,#204901,#204902,#204903,#204904,#204905,#204906,#204907,#204908,
#204909,#204910,#204911,#204912,#204913,#204914,#204915,#204916,#204917,
#204918,#204919,#204920,#204921,#204922,#204923,#204924,#204925,#204926,
#204927,#204928,#204929,#204930,#204931,#204932,#204933,#204934,#204935,
#204936,#204937,#204938,#204939,#204940,#204941,#204942,#204943,#204944,
#204945,#204946,#204947,#204948,#204949,#204950,#204951,#204952,#204953,
#204954,#204955,#204956,#204957,#204958,#204959,#204960,#204961,#204962,
#204963),.UNSPECIFIED.,.F.,.F.,(4,2,2,2,2,2,2,2,2,2,2,2,2,2,2,2,2,2,2,2,
2,2,2,2,2,2,2,2,2,2,2,2,2,4),(-15.2358584380909,-14.8883885392091,-14.728212944849,
-14.5251956127154,-14.3683968473714,-14.182115397803,-13.9864134048351,
-13.6598620632904,-13.4877215195534,-13.3341662488961,-13.1166141821009,
-13.0161814909876,-12.8205979419664,-12.6780030352916,-12.5352842902373,
-12.435411099845,-12.2847577367461,-12.0922290363848,-11.8087984536162,
-11.6485680946771,-11.4454108591613,-11.2958281511512,-11.1047309033229,
-11.0044031080027,-10.7971359215093,-10.6524992354358,-10.3905358718725,
-10.1152482405395,-9.70960192401104,-9.51214685878303,-9.32229105452583,
-9.22401521382655,-8.8901013239156,-8.78547365602618),.UNSPECIFIED.);
#30361=B_SPLINE_CURVE_WITH_KNOTS('',3,(#204969,#204970,#204971,#204972,
#204973,#204974,#204975,#204976,#204977,#204978,#204979,#204980,#204981,
#204982,#204983,#204984,#204985,#204986,#204987,#204988,#204989,#204990,
#204991,#204992),.UNSPECIFIED.,.F.,.F.,(4,2,2,2,2,2,2,2,2,2,2,4),(5.07374035525052E-5,
0.196063149027679,0.390967942257574,0.792252129422216,1.19229882428634,
1.39196195962885,1.59087444470586,1.78833640693344,1.98791847080214,2.18776996778451,
2.48510060443421,2.78256740042434),.UNSPECIFIED.);
#30362=B_SPLINE_CURVE_WITH_KNOTS('',3,(#204993,#204994,#204995,#204996,
#204997,#204998,#204999,#205000,#205001,#205002,#205003,#205004,#205005,
#205006,#205007,#205008,#205009,#205010,#205011,#205012,#205013,#205014,
#205015,#205016,#205017,#205018,#205019,#205020,#205021,#205022,#205023,
#205024,#205025,#205026,#205027,#205028,#205029,#205030),.UNSPECIFIED.,
 .F.,.F.,(4,2,2,2,2,2,2,2,2,2,2,2,2,2,2,2,2,2,4),(-3.66932922096601,-3.63379619948926,
-3.43837159610714,-3.23577904909041,-2.97792121223131,-2.70491838769706,
-2.29941172035685,-2.10299660590446,-1.91373585149283,-1.72322993852301,
-1.57285025595175,-1.37821359396355,-1.09875040975318,-0.947825149927794,
-0.745015350883296,-0.562989317652314,-0.284735747904233,-0.144100026768447,
-1.91474371047745E-5),.UNSPECIFIED.);
#30363=B_SPLINE_CURVE_WITH_KNOTS('',3,(#205031,#205032,#205033,#205034,
#205035,#205036,#205037,#205038,#205039,#205040,#205041,#205042,#205043,
#205044,#205045,#205046,#205047,#205048,#205049,#205050,#205051,#205052,
#205053,#205054,#205055,#205056,#205057,#205058,#205059,#205060,#205061,
#205062,#205063,#205064,#205065,#205066,#205067,#205068,#205069,#205070,
#205071,#205072,#205073,#205074,#205075,#205076,#205077,#205078,#205079,
#205080,#205081,#205082,#205083,#205084,#205085,#205086,#205087,#205088,
#205089,#205090,#205091,#205092),.UNSPECIFIED.,.F.,.F.,(4,2,2,2,2,2,2,2,
2,2,2,2,2,2,2,2,2,2,2,2,2,2,2,2,2,2,2,2,2,2,4),(-21.689764260827,-21.5004354920718,
-21.4014712593995,-21.0843183727269,-20.9856029012984,-20.675026378304,
-20.576123130789,-20.2605890177469,-20.1044705304227,-20.0049574917496,
-19.599311014219,-19.2223904560661,-19.0198129778767,-18.8170498102401,
-18.6145467724549,-18.5155815017818,-18.1983732976846,-18.0996606679563,
-17.7891316225265,-17.6314561471473,-17.5319132563183,-17.1262842576294,
-16.7212408715178,-16.5321987154693,-16.3809997804679,-16.2235136125589,
-16.031384250264,-15.8416120625211,-15.6442728268669,-15.2386130816602,
-15.2358584380909),.UNSPECIFIED.);
#30364=B_SPLINE_CURVE_WITH_KNOTS('',3,(#205098,#205099,#205100,#205101,
#205102,#205103,#205104,#205105),.UNSPECIFIED.,.F.,.F.,(4,2,2,4),(9.21790452011069,
9.43188320060596,9.73296466447981,10.0352832224195),.UNSPECIFIED.);
#30365=B_SPLINE_CURVE_WITH_KNOTS('',3,(#205111,#205112,#205113,#205114,
#205115,#205116,#205117,#205118,#205119,#205120,#205121,#205122,#205123,
#205124,#205125,#205126,#205127,#205128,#205129,#205130,#205131,#205132,
#205133,#205134,#205135,#205136,#205137,#205138,#205139,#205140,#205141,
#205142,#205143,#205144,#205145,#205146,#205147,#205148,#205149,#205150,
#205151,#205152,#205153,#205154,#205155,#205156,#205157,#205158,#205159,
#205160,#205161,#205162,#205163,#205164,#205165,#205166,#205167,#205168,
#205169,#205170,#205171,#205172,#205173,#205174),.UNSPECIFIED.,.F.,.F.,
(4,2,2,2,2,2,2,2,2,2,2,2,2,2,2,2,2,2,2,2,2,2,2,2,2,2,2,2,2,2,2,4),(1.03510113506635,
1.42190076144482,1.65975570624358,1.90918310386553,2.03534477977229,2.54453754089879,
2.78186254656011,3.03265366633356,3.15880260896223,3.66811591822015,3.9093765188749,
4.15314502279335,4.27935426029752,4.78786109189824,5.01857442700664,5.24596204488937,
5.53988512634698,5.76236179366713,6.26691663032822,6.39333733950275,6.62191123079057,
6.74582667446146,6.99053079452599,7.33725916007856,7.58275600969113,7.82878226923088,
8.05831356871582,8.32996067834969,8.55807863234559,9.0659946634424,9.1922346984401,
9.21790452011069),.UNSPECIFIED.);
#30366=B_SPLINE_CURVE_WITH_KNOTS('',3,(#205178,#205179,#205180,#205181),
 .UNSPECIFIED.,.F.,.F.,(4,4),(0.,0.000545808001568916),.UNSPECIFIED.);
#30367=B_SPLINE_CURVE_WITH_KNOTS('',3,(#205183,#205184,#205185,#205186,
#205187,#205188,#205189,#205190,#205191,#205192,#205193,#205194,#205195,
#205196,#205197,#205198,#205199,#205200,#205201,#205202,#205203,#205204,
#205205,#205206,#205207,#205208,#205209,#205210,#205211,#205212),
 .UNSPECIFIED.,.F.,.F.,(4,2,2,2,2,2,2,2,2,2,2,2,2,2,4),(0.,0.161665978883775,
0.323391460360772,0.526063184698653,0.925852633975413,1.05183001042864,
1.56958669063238,1.76531286768935,1.96277562636044,2.47502393525148,2.70447577935272,
3.02961056722481,3.22205209759142,3.37599328488627,3.53032372881095),
 .UNSPECIFIED.);
#30368=B_SPLINE_CURVE_WITH_KNOTS('',3,(#205213,#205214,#205215,#205216,
#205217,#205218,#205219,#205220,#205221,#205222,#205223,#205224,#205225,
#205226,#205227,#205228,#205229,#205230,#205231,#205232,#205233,#205234,
#205235,#205236,#205237,#205238,#205239,#205240),.UNSPECIFIED.,.F.,.F.,
(4,2,2,2,2,2,2,2,2,2,2,2,2,4),(-4.09286724239512,-3.809817967321,-3.64049485149474,
-3.12585719629425,-2.93571507424271,-2.57217968239084,-2.39990451051648,
-1.88602332786757,-1.68187581713282,-1.33960776342174,-1.16853206857936,
-0.653965814988459,-0.343366468889826,-1.00000001346245E-6),
 .UNSPECIFIED.);
#30369=B_SPLINE_CURVE_WITH_KNOTS('',3,(#205246,#205247,#205248,#205249,
#205250,#205251,#205252,#205253,#205254,#205255,#205256,#205257,#205258,
#205259,#205260,#205261,#205262,#205263,#205264,#205265,#205266,#205267,
#205268,#205269,#205270,#205271,#205272,#205273,#205274,#205275,#205276,
#205277,#205278,#205279,#205280,#205281,#205282,#205283,#205284,#205285,
#205286,#205287,#205288,#205289,#205290,#205291,#205292,#205293,#205294,
#205295,#205296,#205297,#205298,#205299,#205300,#205301,#205302,#205303,
#205304,#205305,#205306,#205307,#205308,#205309,#205310,#205311,#205312,
#205313),.UNSPECIFIED.,.F.,.F.,(4,2,2,2,2,2,2,2,2,2,2,2,2,2,2,2,2,2,2,2,
2,2,2,2,2,2,2,2,2,2,2,2,2,4),(19.9487996122062,20.142855664464,20.3820278485055,
20.6144155244437,20.7885129097536,21.0464983427962,21.346008746776,21.4714454550556,
21.6929535544609,21.9237633529913,22.2093771833086,22.3344845972046,22.5904306859218,
22.8486338537469,22.9737744527411,23.2243002103828,23.4635057336823,23.6958961400256,
23.8701093935839,24.1280890660469,24.4283422020099,24.5537978750225,24.7778505729301,
25.0089108086963,25.3110493184325,25.4365629915189,25.6675530044301,25.9257492918385,
26.0506057192989,26.3016248087996,26.5596650416896,26.8209909987335,26.954995010501,
27.0898578193234),.UNSPECIFIED.);
#30370=B_SPLINE_CURVE_WITH_KNOTS('',3,(#205314,#205315,#205316,#205317,
#205318,#205319,#205320,#205321,#205322,#205323,#205324,#205325),
 .UNSPECIFIED.,.F.,.F.,(4,2,2,2,2,4),(4.25269675076831E-5,0.255194498558364,
0.508955632320006,0.799301344136182,0.91256206172092,1.03510113506635),
 .UNSPECIFIED.);
#30371=B_SPLINE_CURVE_WITH_KNOTS('',3,(#205326,#205327,#205328,#205329,
#205330,#205331,#205332,#205333,#205334,#205335,#205336,#205337,#205338,
#205339,#205340,#205341,#205342,#205343,#205344,#205345,#205346,#205347,
#205348,#205349,#205350,#205351,#205352,#205353,#205354,#205355,#205356,
#205357,#205358,#205359,#205360,#205361,#205362,#205363,#205364,#205365,
#205366,#205367,#205368,#205369,#205370,#205371,#205372,#205373,#205374,
#205375,#205376,#205377,#205378,#205379,#205380,#205381,#205382,#205383),
 .UNSPECIFIED.,.F.,.F.,(4,2,2,2,2,2,2,2,2,2,2,2,2,2,2,2,2,2,2,2,2,2,2,2,
2,2,2,2,4),(-12.2749063733074,-12.1187904451948,-11.8798089113104,-11.5535691718836,
-11.3094012788877,-10.8019635842849,-10.6138794912441,-10.2280063178699,
-10.0105009951333,-9.68641783018162,-9.41284063967618,-8.97177822450054,
-8.76888849823266,-8.36889877655667,-8.24292592734775,-7.88568962568576,
-7.63571172493582,-7.27227457659428,-7.02175834137767,-6.65613264294611,
-6.26737152351897,-6.07660330010159,-5.57048100512442,-5.3257325836551,
-4.99778399629202,-4.71802225801622,-4.39296620643604,-4.16592791232279,
-4.09286724239512),.UNSPECIFIED.);
#30372=B_SPLINE_CURVE_WITH_KNOTS('',3,(#205388,#205389,#205390,#205391,
#205392,#205393,#205394,#205395,#205396,#205397,#205398,#205399,#205400,
#205401,#205402,#205403,#205404,#205405,#205406,#205407,#205408,#205409,
#205410,#205411,#205412,#205413,#205414,#205415,#205416,#205417,#205418,
#205419,#205420,#205421,#205422,#205423,#205424,#205425,#205426,#205427,
#205428,#205429,#205430,#205431,#205432,#205433,#205434,#205435,#205436,
#205437,#205438,#205439,#205440,#205441,#205442,#205443,#205444,#205445,
#205446,#205447,#205448,#205449,#205450,#205451,#205452,#205453,#205454,
#205455,#205456,#205457,#205458,#205459,#205460,#205461,#205462,#205463,
#205464,#205465),.UNSPECIFIED.,.F.,.F.,(4,2,2,2,2,2,2,2,2,2,2,2,2,2,2,2,
2,2,2,2,2,2,2,2,2,2,2,2,2,2,2,2,2,2,2,2,2,2,4),(11.7724815045368,11.9880232082335,
12.2186987115618,12.4765421102483,12.6019106871588,12.8601182538573,13.0971443443364,
13.328594358856,13.5448091327034,13.7614888636755,13.9929278017894,14.2301122870459,
14.488318743795,14.6137006386228,14.8715479886744,15.1029029510991,15.3611256858989,
15.4860272745404,15.7370133629348,15.992357545874,16.2505543540056,16.3760124056608,
16.6338779445043,16.8697402281887,17.1279511122735,17.2532293185732,17.503512257197,
17.7339521368796,17.9649654333985,18.2644048003711,18.3898427277393,18.6110955292288,
18.8419052284847,19.1259978968563,19.2510812383165,19.5089682466988,19.7671789135495,
19.8923237629256,19.9487996122062),.UNSPECIFIED.);
#30373=B_SPLINE_CURVE_WITH_KNOTS('',3,(#205467,#205468,#205469,#205470,
#205471,#205472,#205473,#205474,#205475,#205476,#205477,#205478),
 .UNSPECIFIED.,.F.,.F.,(4,2,2,2,2,4),(-13.3097623343318,-13.0506231758963,
-12.7981080529111,-12.6277705686398,-12.4570074402762,-12.2749063733074),
 .UNSPECIFIED.);
#30374=B_SPLINE_CURVE_WITH_KNOTS('',3,(#205479,#205480,#205481,#205482,
#205483,#205484,#205485,#205486,#205487,#205488,#205489,#205490,#205491,
#205492,#205493,#205494,#205495,#205496,#205497,#205498,#205499,#205500,
#205501,#205502,#205503,#205504,#205505,#205506,#205507,#205508,#205509,
#205510,#205511,#205512,#205513,#205514,#205515,#205516,#205517,#205518,
#205519,#205520,#205521,#205522,#205523,#205524,#205525,#205526,#205527,
#205528,#205529,#205530,#205531,#205532,#205533,#205534,#205535,#205536,
#205537,#205538,#205539,#205540,#205541,#205542,#205543,#205544,#205545,
#205546,#205547,#205548),.UNSPECIFIED.,.F.,.F.,(4,2,2,2,2,2,2,2,2,2,2,2,
2,2,2,2,2,2,2,2,2,2,2,2,2,2,2,2,2,2,2,2,2,2,4),(-7.14122009963437,-7.10127310707761,
-6.97636086161089,-6.76788215683646,-6.51626329539109,-6.26141374359471,
-6.00319987140726,-5.87811140533219,-5.62747313366361,-5.38458271921353,
-5.12636745030447,-5.00151505431046,-4.75046058999399,-4.49223192810647,
-4.23405928698162,-4.10848089710744,-3.85059081999491,-3.5842634917128,
-3.33942218792414,-3.08877078337361,-2.96290962115914,-2.66718399600173,
-2.54184986425145,-2.31676961113023,-2.08596597217156,-1.80509407491701,
-1.68006608005489,-1.42222650442997,-1.16402119388851,-1.03914810583125,
-0.788143072776472,-0.530949948001708,-0.269269866189475,-0.135098326930044,
-6.79217263228586E-5),.UNSPECIFIED.);
#30375=B_SPLINE_CURVE_WITH_KNOTS('',3,(#205553,#205554,#205555,#205556,
#205557,#205558,#205559,#205560,#205561,#205562,#205563,#205564,#205565,
#205566,#205567,#205568,#205569,#205570,#205571,#205572,#205573,#205574,
#205575,#205576,#205577,#205578,#205579,#205580,#205581,#205582,#205583,
#205584,#205585,#205586,#205587,#205588,#205589,#205590,#205591,#205592,
#205593,#205594,#205595,#205596,#205597,#205598,#205599,#205600,#205601,
#205602,#205603,#205604,#205605,#205606,#205607,#205608,#205609,#205610,
#205611,#205612,#205613,#205614,#205615,#205616,#205617,#205618,#205619,
#205620,#205621,#205622,#205623,#205624,#205625,#205626,#205627,#205628,
#205629,#205630,#205631,#205632),.UNSPECIFIED.,.F.,.F.,(4,2,2,2,2,2,2,2,
2,2,2,2,2,2,2,2,2,2,2,2,2,2,2,2,2,2,2,2,2,2,2,2,2,2,2,2,2,2,2,4),(3.59627226695956,
3.6820600167183,3.80682696477215,4.06503601396435,4.32286613510125,4.44787779959693,
4.72748981290888,4.85322792225321,5.10340879996836,5.34812827344507,5.61203495282972,
5.86991733555808,5.99546211326746,6.25364136016089,6.49309994339892,6.75097551172211,
6.87648804579222,7.13467380487495,7.37367211565911,7.63154747763148,7.7986701016379,
8.03053802827694,8.2746699170043,8.39982470434024,8.68749696161902,8.94546076267652,
9.11758260107282,9.34982456475858,9.59575501121538,9.84716629837951,10.0584626241018,
10.1833748416066,10.4528951173875,10.7108031723359,10.8364283644821,11.0945998805693,
11.3538735001863,11.6049615553723,11.7298011915162,11.7724815045368),
 .UNSPECIFIED.);
#30376=B_SPLINE_CURVE_WITH_KNOTS('',3,(#205633,#205634,#205635,#205636,
#205637,#205638,#205639,#205640,#205641,#205642,#205643,#205644,#205645,
#205646,#205647,#205648,#205649,#205650,#205651,#205652,#205653,#205654,
#205655,#205656,#205657,#205658,#205659,#205660,#205661,#205662,#205663,
#205664,#205665,#205666,#205667,#205668,#205669,#205670,#205671,#205672,
#205673,#205674,#205675,#205676,#205677,#205678,#205679,#205680,#205681,
#205682,#205683,#205684,#205685,#205686,#205687,#205688,#205689,#205690,
#205691,#205692,#205693,#205694,#205695,#205696,#205697,#205698,#205699,
#205700,#205701,#205702,#205703,#205704,#205705,#205706,#205707,#205708),
 .UNSPECIFIED.,.F.,.F.,(4,2,2,2,2,2,2,2,2,2,2,2,2,2,2,2,2,2,2,2,2,2,2,2,
2,2,2,2,2,2,2,2,2,2,2,2,2,4),(-15.317600608495,-15.1056219580742,-14.8722513427225,
-14.6143963369378,-14.4889800020028,-14.2307783488225,-13.99312958769,-13.7617239607727,
-13.544813767322,-13.328495618661,-13.0970771655347,-12.8596184019178,-12.601415245543,
-12.4760144538482,-12.2181639986697,-11.9856237537738,-11.7274032423102,
-11.6023998741531,-11.3515970506217,-11.1029633060686,-10.8447459947707,
-10.7196010603171,-10.4690595259377,-10.2297444117701,-9.9973186109037,
-9.82280774939264,-9.56481055125628,-9.26273553467217,-9.13721415315108,
-8.90657398144562,-8.64835908946668,-8.52352550164255,-8.27243999430361,
-8.01300468974959,-7.75484166851552,-7.6292129323572,-7.3713101840488,-7.14122009963437),
 .UNSPECIFIED.);
#30377=B_SPLINE_CURVE_WITH_KNOTS('',3,(#205714,#205715,#205716,#205717,
#205718,#205719,#205720,#205721,#205722,#205723,#205724,#205725,#205726,
#205727,#205728,#205729,#205730,#205731,#205732,#205733,#205734,#205735,
#205736,#205737,#205738,#205739,#205740,#205741,#205742,#205743,#205744,
#205745,#205746,#205747,#205748,#205749,#205750,#205751,#205752,#205753,
#205754,#205755,#205756,#205757,#205758,#205759),.UNSPECIFIED.,.F.,.F.,
(4,2,2,2,2,2,2,2,2,2,2,2,2,2,2,2,2,2,2,2,2,2,4),(-27.0910624136568,-26.9485297956287,
-26.8071562305741,-26.5294229406298,-26.3120852980215,-26.0764565382135,
-25.8991731920804,-25.6664808600428,-25.4263379769398,-25.1757865161133,
-25.013524286709,-24.8875050591639,-24.6363094106816,-24.3912847026917,
-24.1219528354226,-23.8909880111037,-23.6725325990257,-23.438024623467,
-23.2587214500234,-23.1324894158539,-22.7613668132535,-22.6364211647448,
-22.5113746151152),.UNSPECIFIED.);
#30378=B_SPLINE_CURVE_WITH_KNOTS('',3,(#205760,#205761,#205762,#205763,
#205764,#205765,#205766,#205767,#205768,#205769,#205770,#205771,#205772,
#205773,#205774,#205775,#205776,#205777,#205778,#205779,#205780,#205781,
#205782,#205783,#205784,#205785,#205786,#205787,#205788,#205789,#205790,
#205791,#205792,#205793,#205794,#205795),.UNSPECIFIED.,.F.,.F.,(4,2,2,2,
2,2,2,2,2,2,2,2,2,2,2,2,2,4),(6.63670082959331E-6,0.138847337507348,0.276650112027392,
0.546239332473065,0.724776399663302,0.98298432656475,1.22509099349884,1.47570301961592,
1.60079692900476,1.8590027850634,2.11687597018492,2.24194740912891,2.52544615201078,
2.78338592312406,2.90917826586352,3.16729181898307,3.43087394279093,3.59627226695956),
 .UNSPECIFIED.);
#30379=B_SPLINE_CURVE_WITH_KNOTS('',3,(#205796,#205797,#205798,#205799,
#205800,#205801,#205802,#205803,#205804,#205805,#205806,#205807,#205808,
#205809,#205810,#205811,#205812,#205813,#205814,#205815,#205816,#205817,
#205818,#205819,#205820,#205821,#205822,#205823,#205824,#205825,#205826,
#205827,#205828,#205829,#205830,#205831,#205832,#205833,#205834,#205835,
#205836,#205837,#205838,#205839,#205840,#205841,#205842,#205843,#205844,
#205845,#205846,#205847,#205848,#205849,#205850,#205851,#205852,#205853,
#205854,#205855,#205856,#205857,#205858,#205859,#205860,#205861,#205862,
#205863,#205864,#205865,#205866,#205867,#205868,#205869,#205870,#205871,
#205872,#205873,#205874,#205875),.UNSPECIFIED.,.F.,.F.,(4,2,2,2,2,2,2,2,
2,2,2,2,2,2,2,2,2,2,2,2,2,2,2,2,2,2,2,2,2,2,2,2,2,2,2,2,2,2,2,4),(-23.4937717245981,
-23.4149622474878,-23.2518531829715,-23.0202626120369,-22.7851106159285,
-22.5346906323585,-22.4094834242548,-22.151270805228,-21.9013492411497,
-21.6505124378202,-21.5255288848259,-21.2673100902392,-21.0094439097838,
-20.7573343531256,-20.5557090153031,-20.4307869371161,-20.1594159310078,
-19.9015048799453,-19.7758559447382,-19.5176942020619,-19.2578307792033,
-19.0067304919821,-18.8819009556285,-18.623682631028,-18.3812729116814,
-18.1306445818583,-18.0055462446488,-17.7473293917388,-17.5136733528107,
-17.2558191980766,-17.1303989826605,-16.8721999568476,-16.6176890754392,
-16.3667268578538,-16.2418132831234,-15.9835923810468,-15.7395918633547,
-15.488916783225,-15.363841527225,-15.317600608495),.UNSPECIFIED.);
#30380=B_SPLINE_CURVE_WITH_KNOTS('',3,(#205880,#205881,#205882,#205883,
#205884,#205885,#205886,#205887,#205888,#205889,#205890,#205891,#205892,
#205893,#205894,#205895,#205896,#205897,#205898,#205899,#205900,#205901,
#205902,#205903,#205904,#205905,#205906,#205907,#205908,#205909,#205910,
#205911,#205912,#205913,#205914,#205915,#205916,#205917,#205918,#205919,
#205920,#205921,#205922,#205923,#205924,#205925,#205926,#205927,#205928,
#205929,#205930,#205931,#205932,#205933,#205934,#205935,#205936,#205937,
#205938,#205939,#205940,#205941,#205942,#205943,#205944,#205945,#205946,
#205947,#205948,#205949,#205950,#205951,#205952,#205953,#205954,#205955,
#205956,#205957),.UNSPECIFIED.,.F.,.F.,(4,2,2,2,2,2,2,2,2,2,2,2,2,2,2,2,
2,2,2,2,2,2,2,2,2,2,2,2,2,2,2,2,2,2,2,2,2,2,4),(-22.5113746151152,-22.3622013116186,
-22.2365061539233,-21.9295000211994,-21.8035549222477,-21.5526094311646,
-21.3076712345341,-21.039790083002,-20.7818879132803,-20.6562842093903,
-20.3981100668058,-20.1393696152133,-19.8882954198129,-19.763446951026,
-19.5052254143252,-19.2624813513231,-19.0118407093092,-18.8867459155375,
-18.6285258780502,-18.3809498202434,-18.1301741601724,-18.0051528863069,
-17.7469311137219,-17.4890562011227,-17.2369979097946,-17.0345635881456,
-16.9096411105631,-16.63842716538,-16.3805132473707,-16.2548647611498,-15.9966991588529,
-15.7368835496313,-15.4857812656124,-15.3609492874221,-15.1027275466364,
-14.8721471489679,-14.6143039871265,-14.4889361920765,-14.3348679765578),
 .UNSPECIFIED.);
#30381=B_SPLINE_CURVE_WITH_KNOTS('',3,(#205959,#205960,#205961,#205962,
#205963,#205964,#205965,#205966,#205967,#205968,#205969,#205970,#205971,
#205972,#205973,#205974,#205975,#205976,#205977,#205978,#205979,#205980,
#205981,#205982,#205983,#205984,#205985,#205986,#205987,#205988,#205989,
#205990,#205991,#205992,#205993,#205994),.UNSPECIFIED.,.F.,.F.,(4,2,2,2,
2,2,2,2,2,2,2,2,2,2,2,2,2,4),(-27.0899870889368,-26.9530598593633,-26.8171091942596,
-26.5516008514074,-26.3748538499552,-26.1166597858708,-25.8789718218379,
-25.6475129080143,-25.4306415300505,-25.3052641631091,-25.0079344600063,
-24.776962792956,-24.5470734614413,-24.2968096085422,-24.1326327675215,
-23.9009712650346,-23.6653943076616,-23.4937717245981),.UNSPECIFIED.);
#30382=B_SPLINE_CURVE_WITH_KNOTS('',3,(#205995,#205996,#205997,#205998,
#205999,#206000,#206001,#206002,#206003,#206004,#206005,#206006,#206007,
#206008,#206009,#206010,#206011,#206012,#206013,#206014,#206015,#206016,
#206017,#206018,#206019,#206020,#206021,#206022,#206023,#206024,#206025,
#206026,#206027,#206028,#206029,#206030,#206031,#206032,#206033,#206034,
#206035,#206036,#206037,#206038,#206039,#206040),.UNSPECIFIED.,.F.,.F.,
(4,2,2,2,2,2,2,2,2,2,2,2,2,2,2,2,2,2,2,2,2,2,4),(-4.57954798347794,-4.51040613143666,
-4.27892855829839,-4.11745185319605,-3.86677760228649,-3.62237827806238,
-3.36416946717782,-3.23924161777639,-2.98832792653369,-2.73518719314125,
-2.4769938688065,-2.35164184692701,-2.09381583051975,-1.86367735928636,
-1.60547069925905,-1.4806851661486,-1.22953536858346,-0.967443934401527,
-0.709310837623982,-0.533692325490634,-0.270605510121337,-0.135776812330919,
-3.84812749395499E-6),.UNSPECIFIED.);
#30383=B_SPLINE_CURVE_WITH_KNOTS('',3,(#206045,#206046,#206047,#206048,
#206049,#206050,#206051,#206052,#206053,#206054,#206055,#206056,#206057,
#206058,#206059,#206060,#206061,#206062,#206063,#206064,#206065,#206066,
#206067,#206068,#206069,#206070,#206071,#206072,#206073,#206074,#206075,
#206076,#206077,#206078,#206079,#206080,#206081,#206082,#206083,#206084,
#206085,#206086,#206087,#206088,#206089,#206090,#206091,#206092,#206093,
#206094,#206095,#206096,#206097,#206098,#206099,#206100,#206101,#206102,
#206103,#206104,#206105,#206106,#206107,#206108,#206109,#206110,#206111,
#206112,#206113,#206114,#206115,#206116,#206117,#206118,#206119,#206120,
#206121,#206122),.UNSPECIFIED.,.F.,.F.,(4,2,2,2,2,2,2,2,2,2,2,2,2,2,2,2,
2,2,2,2,2,2,2,2,2,2,2,2,2,2,2,2,2,2,2,2,2,2,4),(-14.3348679765578,-14.2307291371401,
-13.9937264081978,-13.7622752350275,-13.5460663942738,-13.3293994027905,
-13.0979594006491,-12.8607996474343,-12.6025935681271,-12.4772150610294,
-12.2193696239954,-11.9881213265458,-11.7298995835503,-11.605008893432,
-11.3540079235617,-11.0980479583536,-10.8398545998019,-10.7143709190112,
-10.4564996619228,-10.2189743116877,-9.96077385475969,-9.83536896601102,
-9.57751937674932,-9.3446829071744,-9.08646492332606,-8.96143705944965,
-8.71068232766445,-8.4637182852313,-8.2055010592925,-8.08043922563878,-7.8297466815448,
-7.58501360152563,-7.32679533589724,-7.20184622275508,-6.95095231324976,
-6.69888065047845,-6.44067411083485,-6.31536707642487,-6.15860212849669),
 .UNSPECIFIED.);
#30384=B_SPLINE_CURVE_WITH_KNOTS('',3,(#206123,#206124,#206125,#206126,
#206127,#206128,#206129,#206130,#206131,#206132,#206133,#206134,#206135,
#206136,#206137,#206138,#206139,#206140,#206141,#206142,#206143,#206144,
#206145,#206146,#206147,#206148,#206149,#206150,#206151,#206152,#206153,
#206154,#206155,#206156,#206157,#206158,#206159,#206160,#206161,#206162,
#206163,#206164,#206165,#206166,#206167,#206168,#206169,#206170,#206171,
#206172,#206173,#206174,#206175,#206176,#206177,#206178,#206179,#206180,
#206181,#206182,#206183,#206184,#206185,#206186,#206187,#206188,#206189,
#206190,#206191,#206192,#206193,#206194,#206195,#206196,#206197,#206198,
#206199,#206200),.UNSPECIFIED.,.F.,.F.,(4,2,2,2,2,2,2,2,2,2,2,2,2,2,2,2,
2,2,2,2,2,2,2,2,2,2,2,2,2,2,2,2,2,2,2,2,2,2,4),(-12.7553611554937,-12.6017145941975,
-12.4763762122337,-12.2185474892998,-11.9893326254508,-11.7567223866939,
-11.5798310036023,-11.3436886696159,-11.1266310767901,-10.895255140734,
-10.6572994907987,-10.3991097311077,-10.2736757350015,-10.0158250513052,
-9.78107512198834,-9.52286890232859,-9.39768468763165,-9.14723654608586,
-8.91085699546733,-8.67905773239113,-8.51279779148808,-8.25494725044977,
-8.01983611288601,-7.76163292372143,-7.63642023060741,-7.38603097600229,
-7.15161907456632,-6.92015153602238,-6.75884077192061,-6.50814063174183,
-6.26282945460571,-6.00462037579504,-5.87964569336017,-5.62881318350843,
-5.37869162359585,-5.12048884010234,-4.99527739343617,-4.74488656402094,
-4.57954798347794),.UNSPECIFIED.);
#30385=B_SPLINE_CURVE_WITH_KNOTS('',3,(#206209,#206210,#206211,#206212,
#206213,#206214),.UNSPECIFIED.,.F.,.F.,(4,2,4),(1.00000001053189E-6,0.291982877240883,
0.583963182531396),.UNSPECIFIED.);
#30386=B_SPLINE_CURVE_WITH_KNOTS('',3,(#206218,#206219,#206220,#206221,
#206222,#206223),.UNSPECIFIED.,.F.,.F.,(4,2,4),(1.18860081555568E-5,0.292247563585408,
0.584494052040901),.UNSPECIFIED.);
#30387=B_SPLINE_CURVE_WITH_KNOTS('',3,(#206227,#206228,#206229,#206230,
#206231,#206232,#206233,#206234,#206235,#206236,#206237,#206238,#206239,
#206240,#206241,#206242,#206243,#206244,#206245,#206246,#206247,#206248,
#206249,#206250,#206251,#206252,#206253,#206254,#206255,#206256,#206257,
#206258,#206259,#206260,#206261,#206262,#206263,#206264,#206265,#206266,
#206267,#206268,#206269,#206270,#206271,#206272,#206273,#206274,#206275,
#206276,#206277,#206278,#206279,#206280,#206281,#206282,#206283,#206284,
#206285,#206286),.UNSPECIFIED.,.F.,.F.,(4,2,2,2,2,2,2,2,2,2,2,2,2,2,2,2,
2,2,2,2,2,2,2,2,2,2,2,2,2,4),(-27.088923764392,-26.950639491994,-26.8133525669105,
-26.544907036575,-26.3668620021181,-26.108660746686,-25.8508123833913,-25.7257678773642,
-25.4436361357283,-25.1857075525708,-25.0145798547139,-24.8884489823397,
-24.5204161698867,-24.3954710664388,-24.1209093810336,-23.86300038075,-23.6932540021783,
-23.461206206101,-23.2161229095314,-22.9647484897821,-22.7531956056424,
-22.6282932069822,-22.3588407689814,-22.1009488738442,-21.9753313793407,
-21.717177140173,-21.4579376178504,-21.2068654511702,-21.082032595878,-20.9312459291626),
 .UNSPECIFIED.);
#30388=B_SPLINE_CURVE_WITH_KNOTS('',3,(#206287,#206288,#206289,#206290,
#206291,#206292,#206293,#206294,#206295,#206296,#206297,#206298,#206299,
#206300),.UNSPECIFIED.,.F.,.F.,(4,2,2,2,2,2,4),(0.,0.254132792260243,0.504072118513533,
1.01015766536926,1.26037994975052,1.64270580735409,2.01988313929201),
 .UNSPECIFIED.);
#30389=B_SPLINE_CURVE_WITH_KNOTS('',3,(#206305,#206306,#206307,#206308),
 .UNSPECIFIED.,.F.,.F.,(4,4),(-0.00220042394823992,0.),.UNSPECIFIED.);
#30390=B_SPLINE_CURVE_WITH_KNOTS('',3,(#206310,#206311,#206312,#206313,
#206314,#206315,#206316,#206317,#206318,#206319,#206320,#206321,#206322,
#206323,#206324,#206325,#206326,#206327,#206328,#206329,#206330,#206331,
#206332,#206333,#206334,#206335,#206336,#206337,#206338,#206339,#206340,
#206341,#206342,#206343,#206344,#206345,#206346,#206347,#206348,#206349,
#206350,#206351,#206352,#206353,#206354,#206355),.UNSPECIFIED.,.F.,.F.,
(4,2,2,2,2,2,2,2,2,2,2,2,2,2,2,2,2,2,2,2,2,2,4),(3.77495847620787E-5,0.239786601820601,
0.486605707253356,0.970538667061549,1.45703768164805,1.71085426685705,1.9510783074641,
2.07349206054835,2.55160936918151,2.80110529120666,3.03699522422384,3.28275824999066,
3.52002970929671,3.76617821420918,4.00121882590241,4.49262572156392,4.61272242555606,
4.85423743096944,5.08785380877291,5.57193736666279,6.05829820485225,6.18384427889897,
6.56939833044204),.UNSPECIFIED.);
#30391=B_SPLINE_CURVE_WITH_KNOTS('',3,(#206358,#206359,#206360,#206361,
#206362,#206363,#206364,#206365,#206366,#206367,#206368,#206369,#206370,
#206371,#206372,#206373,#206374,#206375,#206376,#206377,#206378,#206379,
#206380,#206381,#206382,#206383,#206384,#206385,#206386,#206387,#206388,
#206389,#206390,#206391,#206392,#206393,#206394,#206395,#206396,#206397,
#206398,#206399,#206400,#206401,#206402,#206403,#206404,#206405,#206406,
#206407,#206408,#206409,#206410,#206411,#206412,#206413,#206414,#206415),
 .UNSPECIFIED.,.F.,.F.,(4,3,3,3,3,3,3,3,3,3,3,3,3,3,3,3,3,3,3,4),(0.,0.0577023232576086,
0.115555621115906,0.173492165360545,0.231551782116938,0.25,0.307569756346692,
0.365075787326178,0.422538236884358,0.479957516808789,0.537334036195474,
0.594651018367717,0.651929822766841,0.709155453145986,0.75,0.807257177142689,
0.864351407537183,0.921347999936588,0.978207659355297,0.999999816562461),
 .UNSPECIFIED.);
#30392=B_SPLINE_CURVE_WITH_KNOTS('',3,(#206421,#206422,#206423,#206424),
 .UNSPECIFIED.,.F.,.F.,(4,4),(-6.83645232667685E-6,-1.00000001587719E-6),
 .UNSPECIFIED.);
#30393=B_SPLINE_CURVE_WITH_KNOTS('',3,(#206426,#206427,#206428,#206429,
#206430,#206431,#206432,#206433,#206434,#206435,#206436,#206437),
 .UNSPECIFIED.,.F.,.F.,(4,2,2,2,2,4),(0.000339869836820149,0.296752020291076,
0.39447181405845,0.493164400823495,0.639110988050355,0.788070724201917),
 .UNSPECIFIED.);
#30394=B_SPLINE_CURVE_WITH_KNOTS('',3,(#206440,#206441,#206442,#206443,
#206444,#206445,#206446,#206447,#206448,#206449,#206450,#206451),
 .UNSPECIFIED.,.F.,.F.,(4,2,2,2,2,4),(-0.787810247909609,-0.491424601924294,
-0.393707156562174,-0.29503529184239,-0.149115943288715,-9.76537854778592E-5),
 .UNSPECIFIED.);
#30395=B_SPLINE_CURVE_WITH_KNOTS('',3,(#206454,#206455,#206456,#206457,
#206458,#206459,#206460,#206461,#206462,#206463,#206464,#206465,#206466,
#206467,#206468,#206469,#206470,#206471,#206472,#206473,#206474,#206475,
#206476,#206477,#206478,#206479,#206480,#206481,#206482,#206483,#206484,
#206485,#206486,#206487,#206488,#206489,#206490,#206491,#206492,#206493,
#206494,#206495,#206496,#206497,#206498,#206499,#206500,#206501,#206502,
#206503,#206504,#206505,#206506,#206507,#206508,#206509,#206510,#206511,
#206512,#206513,#206514,#206515,#206516,#206517,#206518,#206519),
 .UNSPECIFIED.,.F.,.F.,(4,2,2,2,2,2,2,2,2,2,2,2,2,2,2,2,2,2,2,2,2,2,2,2,
2,2,2,2,2,2,2,2,4),(-20.0251822700621,-19.783399253692,-19.7027995529101,
-19.3819220086887,-19.2335279991671,-19.0806295483898,-18.9217357990387,
-18.8325340301694,-18.6562482399521,-18.4948478066825,-18.3256422331843,
-18.173550209753,-17.9918384866733,-17.8262128753862,-17.7375272992725,
-17.5586636565654,-17.3917395152,-17.2468299270429,-17.0904651127749,-16.9212870128186,
-16.7510701900917,-16.4818730929832,-16.3432229200778,-16.1264751872471,
-15.947096589243,-15.7717268657687,-15.6306011902255,-15.4602842612329,
-15.2908239990938,-15.1162436454238,-14.756984936882,-14.3959660136892,
-14.3036677916835),.UNSPECIFIED.);
#30396=B_SPLINE_CURVE_WITH_KNOTS('',3,(#206522,#206523,#206524,#206525,
#206526,#206527,#206528,#206529,#206530,#206531,#206532,#206533,#206534,
#206535,#206536,#206537,#206538,#206539,#206540,#206541,#206542,#206543,
#206544,#206545,#206546,#206547,#206548,#206549,#206550,#206551,#206552,
#206553,#206554,#206555,#206556,#206557,#206558,#206559,#206560,#206561,
#206562,#206563,#206564,#206565,#206566,#206567,#206568,#206569,#206570,
#206571,#206572,#206573,#206574,#206575,#206576,#206577,#206578,#206579,
#206580,#206581,#206582,#206583,#206584,#206585),.UNSPECIFIED.,.F.,.F.,
(4,2,2,2,2,2,2,2,2,2,2,2,2,2,2,2,2,2,2,2,2,2,2,2,2,2,2,2,2,2,2,4),(-5.72191210760107,
-5.41349515739714,-5.05567096156071,-4.96749892296319,-4.81840590942988,
-4.63859224637836,-4.45820907173672,-4.18760610519457,-4.09983054832184,
-3.79969878315938,-3.44429584089838,-3.27068421004476,-3.10024231552191,
-2.92994627866288,-2.76951740584553,-2.62353240632635,-2.46635235484725,
-2.28748261501643,-2.19879437053061,-2.03356792410285,-1.85427977681009,
-1.70336284067883,-1.51995057865207,-1.36630179602626,-1.19012013778883,
-1.10095232118681,-0.94005746713909,-0.759230972609438,-0.616488683133836,
-0.385776320856448,-0.195646578274231,-6.83645232667685E-6),
 .UNSPECIFIED.);
#30397=B_SPLINE_CURVE_WITH_KNOTS('',3,(#206590,#206591,#206592,#206593,
#206594,#206595,#206596,#206597,#206598,#206599,#206600,#206601,#206602,
#206603,#206604,#206605,#206606,#206607,#206608,#206609,#206610,#206611,
#206612,#206613,#206614,#206615,#206616,#206617,#206618,#206619,#206620,
#206621,#206622,#206623,#206624,#206625,#206626,#206627,#206628,#206629,
#206630,#206631,#206632,#206633,#206634,#206635,#206636,#206637,#206638,
#206639,#206640,#206641,#206642,#206643,#206644,#206645,#206646,#206647,
#206648,#206649,#206650,#206651,#206652,#206653,#206654,#206655,#206656,
#206657,#206658,#206659,#206660,#206661,#206662,#206663),.UNSPECIFIED.,
 .F.,.F.,(4,2,2,2,2,2,2,2,2,2,2,2,2,2,2,2,2,2,2,2,2,2,2,2,2,2,2,2,2,2,2,
2,2,2,2,2,4),(-11.4417380987961,-11.3553364651864,-11.1774160383949,-11.0372075791858,
-10.8667631656153,-10.6973773346602,-10.5226016322737,-10.2477974621797,
-10.0995357553595,-10.0114468986988,-9.65549049338967,-9.48138958945092,
-9.31089325773942,-9.14006813818346,-8.98157553049582,-8.82713166956379,
-8.68104046619338,-8.50127889414351,-8.41281799829901,-8.24999629874056,
-8.08982187212831,-7.94014904278731,-7.62303054035336,-7.5348458585733,
-7.39685004091648,-7.21874574487305,-7.04217836617445,-6.95300076868866,
-6.79472871579089,-6.63547366518565,-6.48774654885689,-6.31196696168113,
-6.22263750831177,-6.07312396277187,-5.9302570348509,-5.7687427317654,-5.72191210760107),
 .UNSPECIFIED.);
#30398=B_SPLINE_CURVE_WITH_KNOTS('',3,(#206664,#206665,#206666,#206667,
#206668,#206669,#206670,#206671,#206672,#206673,#206674,#206675,#206676,
#206677,#206678,#206679,#206680,#206681,#206682,#206683,#206684,#206685,
#206686,#206687,#206688,#206689,#206690,#206691,#206692,#206693,#206694,
#206695,#206696,#206697,#206698,#206699,#206700,#206701,#206702,#206703,
#206704,#206705,#206706,#206707,#206708,#206709,#206710,#206711,#206712,
#206713,#206714,#206715,#206716,#206717,#206718,#206719,#206720,#206721,
#206722,#206723,#206724,#206725,#206726,#206727,#206728,#206729,#206730,
#206731,#206732,#206733),.UNSPECIFIED.,.F.,.F.,(4,2,2,2,2,2,2,2,2,2,2,2,
2,2,2,2,2,2,2,2,2,2,2,2,2,2,2,2,2,2,2,2,2,2,4),(-14.3036677916835,-14.0340394295821,
-13.7520315188632,-13.5974111949159,-13.4400684067818,-13.3508209983375,
-13.1749381983995,-12.9996246650309,-12.8581361268037,-12.7010224181862,
-12.5108779886259,-12.3442110009737,-12.2554161351745,-12.07716356736,-11.9192026641883,
-11.76735048996,-11.6082372190042,-11.5197094013378,-11.3400263407629,-11.1895026213211,
-11.0407835689815,-10.8835502767979,-10.7128843788238,-10.5424684480171,
-10.3684595925684,-10.0124870321069,-9.92436933678178,-9.76328708361137,
-9.58305914112651,-9.3895913390335,-9.20952067832326,-9.04285406091558,
-8.78771294563985,-8.61662518543304,-8.58288598458152),.UNSPECIFIED.);
#30399=B_SPLINE_CURVE_WITH_KNOTS('',3,(#206738,#206739,#206740,#206741,
#206742,#206743,#206744,#206745,#206746,#206747,#206748,#206749,#206750,
#206751,#206752,#206753,#206754,#206755,#206756,#206757,#206758,#206759,
#206760,#206761,#206762,#206763,#206764,#206765,#206766,#206767,#206768,
#206769,#206770,#206771,#206772,#206773,#206774,#206775,#206776,#206777,
#206778,#206779,#206780,#206781,#206782,#206783,#206784,#206785,#206786,
#206787,#206788,#206789,#206790,#206791,#206792,#206793,#206794,#206795,
#206796,#206797,#206798,#206799,#206800,#206801,#206802,#206803,#206804,
#206805,#206806,#206807,#206808,#206809),.UNSPECIFIED.,.F.,.F.,(4,2,2,2,
2,2,2,2,2,2,2,2,2,2,2,2,2,2,2,2,2,2,2,2,2,2,2,2,2,2,2,2,2,2,2,4),(-17.1620566513902,
-17.0701997094641,-16.904359851517,-16.73085642586,-16.4591336747313,-16.3106797711992,
-16.2225325965221,-15.864752733382,-15.5094655368914,-15.350730421272,-15.206575755354,
-15.0564334242206,-14.9671036987014,-14.7913228671624,-14.6434878566294,
-14.4840597819354,-14.3255899820278,-14.2364158793949,-14.0597959539414,
-13.8817212505758,-13.7015961877199,-13.5488101428796,-13.3943208444835,
-13.2307006383988,-13.1420687705111,-12.9628774862974,-12.7987939786307,
-12.6529353983322,-12.4973750820984,-12.3038931681488,-12.1420166067712,
-12.0583227818685,-11.8789515515351,-11.7435506383085,-11.5348041836882,
-11.4417380987961),.UNSPECIFIED.);
#30400=B_SPLINE_CURVE_WITH_KNOTS('',3,(#206810,#206811,#206812,#206813,
#206814,#206815,#206816,#206817,#206818,#206819,#206820,#206821,#206822,
#206823,#206824,#206825,#206826,#206827,#206828,#206829,#206830,#206831,
#206832,#206833,#206834,#206835,#206836,#206837,#206838,#206839,#206840,
#206841,#206842,#206843,#206844,#206845,#206846,#206847,#206848,#206849,
#206850,#206851,#206852,#206853,#206854,#206855,#206856,#206857,#206858,
#206859,#206860,#206861,#206862,#206863,#206864,#206865,#206866,#206867,
#206868,#206869,#206870,#206871,#206872,#206873,#206874,#206875,#206876,
#206877),.UNSPECIFIED.,.F.,.F.,(4,2,2,2,2,2,2,2,2,2,2,2,2,2,2,2,2,2,2,2,
2,2,2,2,2,2,2,2,2,2,2,2,2,4),(-8.58288598458152,-8.46851059617028,-8.31821013384429,
-8.03138467818614,-7.67593192574583,-7.58797629524239,-7.43061142801808,
-7.25095832007405,-7.16241149566316,-7.004909138247,-6.86028525748937,-6.69154418576299,
-6.51323022248577,-6.42445253407658,-6.25733786057316,-6.06457571797289,
-5.90460532302624,-5.74822811543796,-5.59531793438502,-5.41934787698796,
-5.33009193009703,-5.17355970644515,-5.02475475717209,-4.87451797166454,
-4.69873282775091,-4.51879651590067,-4.16262955435834,-3.80463506979839,
-3.7166292175596,-3.56433073312492,-3.29214753994671,-3.11861456496206,
-2.95246910301541,-2.8610678083529),.UNSPECIFIED.);
#30401=B_SPLINE_CURVE_WITH_KNOTS('',3,(#206883,#206884,#206885,#206886),
 .UNSPECIFIED.,.F.,.F.,(4,4),(-9.10624753604124E-6,-1.00000002245526E-6),
 .UNSPECIFIED.);
#30402=B_SPLINE_CURVE_WITH_KNOTS('',3,(#206888,#206889,#206890,#206891,
#206892,#206893,#206894,#206895),.UNSPECIFIED.,.F.,.F.,(4,2,2,4),(0.000264654385573201,
0.197179255479995,0.294830977384857,0.393932741177773),.UNSPECIFIED.);
#30403=B_SPLINE_CURVE_WITH_KNOTS('',3,(#206898,#206899,#206900,#206901,
#206902,#206903,#206904,#206905),.UNSPECIFIED.,.F.,.F.,(4,2,2,4),(-0.393859367021486,
-0.195155499306153,-0.0984062565036703,-0.000187054781717022),
 .UNSPECIFIED.);
#30404=B_SPLINE_CURVE_WITH_KNOTS('',3,(#206908,#206909,#206910,#206911,
#206912,#206913,#206914,#206915,#206916,#206917,#206918,#206919,#206920,
#206921,#206922,#206923,#206924,#206925,#206926,#206927,#206928,#206929,
#206930,#206931,#206932,#206933,#206934,#206935,#206936,#206937,#206938,
#206939,#206940,#206941,#206942,#206943,#206944,#206945,#206946,#206947,
#206948,#206949,#206950,#206951,#206952,#206953,#206954,#206955,#206956,
#206957,#206958,#206959,#206960,#206961,#206962,#206963,#206964,#206965,
#206966,#206967,#206968,#206969,#206970,#206971,#206972,#206973),
 .UNSPECIFIED.,.F.,.F.,(4,2,2,2,2,2,2,2,2,2,2,2,2,2,2,2,2,2,2,2,2,2,2,2,
2,2,2,2,2,2,2,2,4),(-20.0261911591635,-19.7901934295335,-19.5560940283505,
-19.4036395436267,-19.2565931006169,-19.1672547768,-18.9914680343798,-18.8452477477883,
-18.7102619323775,-18.5409811946449,-18.3351165290447,-18.1682508621197,
-17.9965602320071,-17.8266219334632,-17.608983519323,-17.4393211233688,
-17.3507328805447,-17.1721276112691,-17.0229918399559,-16.8616276503751,
-16.7018749905528,-16.531682353722,-16.3612915040967,-16.1877446686152,
-15.8323524409229,-15.5329897781126,-15.4452006269922,-15.1739016223424,
-14.993531276491,-14.813721299713,-14.6606761967681,-14.5726633728389,-14.30529387033),
 .UNSPECIFIED.);
#30405=B_SPLINE_CURVE_WITH_KNOTS('',3,(#206976,#206977,#206978,#206979,
#206980,#206981,#206982,#206983,#206984,#206985,#206986,#206987,#206988,
#206989,#206990,#206991,#206992,#206993,#206994,#206995,#206996,#206997,
#206998,#206999,#207000,#207001,#207002,#207003,#207004,#207005,#207006,
#207007,#207008,#207009,#207010,#207011,#207012,#207013,#207014,#207015,
#207016,#207017,#207018,#207019,#207020,#207021,#207022,#207023,#207024,
#207025,#207026,#207027,#207028,#207029,#207030,#207031,#207032,#207033,
#207034,#207035,#207036,#207037,#207038,#207039),.UNSPECIFIED.,.F.,.F.,
(4,2,2,2,2,2,2,2,2,2,2,2,2,2,2,2,2,2,2,2,2,2,2,2,2,2,2,2,2,2,2,4),(-5.72211617364862,
-5.45144606650527,-5.3633052520705,-5.21572875839572,-4.94204657011516,
-4.7684701239606,-4.60105176610644,-4.41970948295995,-4.27072885820464,
-4.12114797529049,-3.82944484156022,-3.47369830924017,-3.29998251974305,
-3.1295246180773,-2.95909462929261,-2.79532532558971,-2.63619886337304,
-2.48604117540911,-2.17544688801221,-2.08746385928504,-1.93484205763217,
-1.76012459250849,-1.58397517528309,-1.49481489335935,-1.33338753263079,
-1.1490392729983,-1.00494293849868,-0.801857008033588,-0.664088345956647,
-0.335938630733057,-0.252209855432774,-9.10624753604124E-6),
 .UNSPECIFIED.);
#30406=B_SPLINE_CURVE_WITH_KNOTS('',3,(#207044,#207045,#207046,#207047,
#207048,#207049,#207050,#207051,#207052,#207053,#207054,#207055,#207056,
#207057,#207058,#207059,#207060,#207061,#207062,#207063,#207064,#207065,
#207066,#207067,#207068,#207069,#207070,#207071,#207072,#207073,#207074,
#207075,#207076,#207077,#207078,#207079,#207080,#207081,#207082,#207083,
#207084,#207085,#207086,#207087,#207088,#207089,#207090,#207091,#207092,
#207093,#207094,#207095,#207096,#207097,#207098,#207099,#207100,#207101,
#207102,#207103,#207104,#207105),.UNSPECIFIED.,.F.,.F.,(4,2,2,2,2,2,2,2,
2,2,2,2,2,2,2,2,2,2,2,2,2,2,2,2,2,2,2,2,2,2,4),(-11.4453555711932,-11.2868526815436,
-10.9283028098601,-10.5679594860918,-10.3092878491564,-10.1011704626875,
-10.0136956633507,-9.83704715036268,-9.74840954808365,-9.6037178358129,
-9.30695121065821,-8.95089887793476,-8.77626913462526,-8.60529767077106,
-8.43340752041267,-8.26372948570216,-8.14556017964418,-7.97486491658098,
-7.79763042634811,-7.70867088721176,-7.54222343817563,-7.34448119580206,
-7.18264701373627,-7.00152016368675,-6.85719439430696,-6.64009268403691,
-6.50065906693968,-6.32149308911038,-6.16486393792819,-5.80935272002635,
-5.72211617364862),.UNSPECIFIED.);
#30407=B_SPLINE_CURVE_WITH_KNOTS('',3,(#207106,#207107,#207108,#207109,
#207110,#207111,#207112,#207113,#207114,#207115,#207116,#207117,#207118,
#207119,#207120,#207121,#207122,#207123,#207124,#207125,#207126,#207127,
#207128,#207129,#207130,#207131,#207132,#207133,#207134,#207135,#207136,
#207137,#207138,#207139,#207140,#207141,#207142,#207143,#207144,#207145,
#207146,#207147,#207148,#207149,#207150,#207151,#207152,#207153,#207154,
#207155,#207156,#207157,#207158,#207159,#207160,#207161,#207162,#207163,
#207164,#207165,#207166,#207167),.UNSPECIFIED.,.F.,.F.,(4,2,2,2,2,2,2,2,
2,2,2,2,2,2,2,2,2,2,2,2,2,2,2,2,2,2,2,2,2,2,4),(-14.30529387033,-14.214635198436,
-13.8584617770324,-13.6785499880908,-13.5027518196477,-13.3546092672862,
-13.2001155595787,-13.0453669138218,-12.956086461402,-12.7800997287169,
-12.6232959758484,-12.4961681013161,-12.3267364071978,-12.1226954065264,
-11.9540253642301,-11.7562548269082,-11.5881848396705,-11.4172301653806,
-11.2466872819809,-11.0725892239989,-10.7163691877442,-10.436500748924,
-10.2781001697233,-10.1895252680676,-10.0128939376982,-9.92540538050117,
-9.7221803864745,-9.46331745376698,-9.10309646813805,-8.74493137208567,
-8.5824306122609),.UNSPECIFIED.);
#30408=B_SPLINE_CURVE_WITH_KNOTS('',3,(#207172,#207173,#207174,#207175,
#207176,#207177,#207178,#207179,#207180,#207181,#207182,#207183,#207184,
#207185,#207186,#207187,#207188,#207189,#207190,#207191,#207192,#207193,
#207194,#207195,#207196,#207197,#207198,#207199,#207200,#207201,#207202,
#207203,#207204,#207205,#207206,#207207,#207208,#207209,#207210,#207211,
#207212,#207213,#207214,#207215,#207216,#207217,#207218,#207219,#207220,
#207221,#207222,#207223,#207224,#207225,#207226,#207227,#207228,#207229,
#207230,#207231,#207232,#207233,#207234,#207235,#207236,#207237,#207238,
#207239,#207240,#207241,#207242,#207243,#207244,#207245),.UNSPECIFIED.,
 .F.,.F.,(4,2,2,2,2,2,2,2,2,2,2,2,2,2,2,2,2,2,2,2,2,2,2,2,2,2,2,2,2,2,2,
2,2,2,2,2,4),(-17.166235588483,-17.1290620281814,-16.8564247638492,-16.7081866111978,
-16.6200472505132,-16.262216084275,-15.9068054388724,-15.7503880717279,
-15.6001841980369,-15.4518261553452,-15.3624610849156,-15.1866414162631,
-15.0348927644298,-14.8800867026375,-14.7224140652765,-14.6332233584554,
-14.4565822398736,-14.2784347564555,-14.0983608695542,-13.944597984781,
-13.7912875839889,-13.6280294912066,-13.5393862977335,-13.3601858785979,
-13.2005980542115,-13.0781456483354,-12.9084210492395,-12.823102902181,
-12.735600182679,-12.5645357834063,-12.3901511907983,-12.1044488364628,
-11.9461820660416,-11.8015524326663,-11.6310593138553,-11.4613677768082,
-11.4453555711932),.UNSPECIFIED.);
#30409=B_SPLINE_CURVE_WITH_KNOTS('',3,(#207246,#207247,#207248,#207249,
#207250,#207251,#207252,#207253,#207254,#207255,#207256,#207257,#207258,
#207259,#207260,#207261,#207262,#207263,#207264,#207265,#207266,#207267,
#207268,#207269,#207270,#207271,#207272,#207273,#207274,#207275,#207276,
#207277,#207278,#207279,#207280,#207281,#207282,#207283,#207284,#207285,
#207286,#207287,#207288,#207289,#207290,#207291,#207292,#207293,#207294,
#207295,#207296,#207297,#207298,#207299,#207300,#207301,#207302,#207303,
#207304,#207305,#207306,#207307,#207308,#207309,#207310,#207311,#207312,
#207313),.UNSPECIFIED.,.F.,.F.,(4,2,2,2,2,2,2,2,2,2,2,2,2,2,2,2,2,2,2,2,
2,2,2,2,2,2,2,2,2,2,2,2,2,4),(-8.5824306122609,-8.57103770819693,-8.40325571514215,
-8.23587731607054,-8.09807718898508,-7.87804323785844,-7.74008814103692,
-7.55930879121377,-7.26215386073682,-6.906151748955,-6.73157115865593,-6.56061385975624,
-6.38879209803198,-6.21911161776177,-5.99012880275868,-5.90238817036819,
-5.71544395322699,-5.56262175016414,-5.3827312589457,-5.29369993625239,
-5.12458390792792,-5.00403736786862,-4.84033276501113,-4.6645241502789,
-4.57516300392967,-4.42711804071362,-4.27509016740412,-4.1199929652534,
-3.7645535559046,-3.40672055774514,-3.3185896395958,-3.17024067651289,-2.89755199278977,
-2.8604020772222),.UNSPECIFIED.);
#30410=B_SPLINE_CURVE_WITH_KNOTS('',3,(#207319,#207320,#207321,#207322),
 .UNSPECIFIED.,.F.,.F.,(4,4),(0.000166910408725463,0.000172246164436567),
 .UNSPECIFIED.);
#30411=B_SPLINE_CURVE_WITH_KNOTS('',3,(#207324,#207325,#207326,#207327,
#207328,#207329),.UNSPECIFIED.,.F.,.F.,(4,2,4),(0.000158868425727158,0.234718202342811,
0.469154050604624),.UNSPECIFIED.);
#30412=B_SPLINE_CURVE_WITH_KNOTS('',3,(#207336,#207337,#207338,#207339,
#207340,#207341,#207342,#207343,#207344,#207345,#207346,#207347,#207348,
#207349,#207350,#207351,#207352,#207353,#207354,#207355,#207356,#207357,
#207358,#207359,#207360,#207361,#207362,#207363,#207364,#207365,#207366,
#207367,#207368,#207369,#207370,#207371,#207372,#207373,#207374,#207375,
#207376,#207377,#207378,#207379,#207380,#207381,#207382,#207383,#207384,
#207385,#207386,#207387,#207388,#207389,#207390,#207391,#207392,#207393,
#207394,#207395,#207396,#207397,#207398,#207399,#207400,#207401,#207402,
#207403,#207404,#207405,#207406,#207407,#207408,#207409),.UNSPECIFIED.,
 .F.,.F.,(4,2,2,2,2,2,2,2,2,2,2,2,2,2,2,2,2,2,2,2,2,2,2,2,2,2,2,2,2,2,2,
2,2,2,2,2,4),(-6.99961622965257,-6.96391578728215,-6.73460522677822,-6.49987907509467,
-6.27549114934176,-6.16171354295781,-5.9319207685918,-5.69736222847282,
-5.47298362661363,-5.35906532128113,-5.1290559345853,-4.89456581019745,
-4.67025576664923,-4.55618747183648,-4.32637094188848,-4.09174449679306,
-3.8675865506281,-3.75343209190301,-3.52419107187844,-3.25370641558361,
-3.13975920840176,-2.95251199520079,-2.72382611475827,-2.44530613821909,
-2.33128288872491,-2.00859486011215,-1.89364040439153,-1.73174264476915,
-1.50515816911957,-1.24787775884641,-1.13380587579145,-0.958202539565173,
-0.729140507942947,-0.494185151112094,-0.250153069066657,-0.125295117691977,
-0.000535240498741617),.UNSPECIFIED.);
#30413=B_SPLINE_CURVE_WITH_KNOTS('',3,(#207412,#207413,#207414,#207415,
#207416,#207417,#207418,#207419,#207420,#207421,#207422,#207423,#207424,
#207425,#207426,#207427,#207428,#207429,#207430,#207431,#207432,#207433,
#207434,#207435,#207436,#207437,#207438,#207439,#207440,#207441,#207442,
#207443,#207444,#207445,#207446,#207447,#207448,#207449,#207450,#207451,
#207452,#207453,#207454,#207455,#207456,#207457,#207458,#207459,#207460,
#207461,#207462,#207463,#207464,#207465,#207466,#207467,#207468,#207469,
#207470,#207471,#207472,#207473,#207474,#207475,#207476,#207477,#207478,
#207479,#207480,#207481,#207482,#207483),.UNSPECIFIED.,.F.,.F.,(4,2,2,2,
2,2,2,2,2,2,2,2,2,2,2,2,2,2,2,2,2,2,2,2,2,2,2,2,2,2,2,2,2,2,2,4),(-24.6761488606007,
-24.5536439797374,-24.4309909429808,-24.1916221027102,-23.9565240762551,
-23.7281632573065,-23.6142884178381,-23.390153971156,-23.1549002339024,
-23.0406665683764,-22.7725487102365,-22.6579276896609,-22.4304762591835,
-22.2063853627223,-21.9629289515731,-21.7352875834566,-21.5770834181909,
-21.4624147721794,-21.2334477924476,-21.0093471006007,-20.7550531474735,
-20.525866361529,-20.3726134692837,-20.2580599272056,-19.938146030468,-19.7071268961134,
-19.4776001634708,-19.1298823887128,-19.0156965246622,-18.7922790652087,
-18.567360532056,-18.3326914807233,-18.2184489417264,-17.9944926139954,
-17.7699051708102,-17.6762610095338),.UNSPECIFIED.);
#30414=B_SPLINE_CURVE_WITH_KNOTS('',3,(#207488,#207489,#207490,#207491,
#207492,#207493,#207494,#207495,#207496,#207497,#207498,#207499,#207500,
#207501,#207502,#207503,#207504,#207505,#207506,#207507,#207508,#207509,
#207510,#207511,#207512,#207513,#207514,#207515,#207516,#207517,#207518,
#207519,#207520,#207521,#207522,#207523,#207524,#207525,#207526,#207527,
#207528,#207529,#207530,#207531,#207532,#207533,#207534,#207535,#207536,
#207537,#207538,#207539,#207540,#207541,#207542,#207543,#207544,#207545,
#207546,#207547,#207548,#207549,#207550,#207551,#207552,#207553,#207554,
#207555,#207556,#207557,#207558,#207559,#207560,#207561,#207562,#207563),
 .UNSPECIFIED.,.F.,.F.,(4,2,2,2,2,2,2,2,2,2,2,2,2,2,2,2,2,2,2,2,2,2,2,2,
2,2,2,2,2,2,2,2,2,2,2,2,2,4),(-14.4468995549683,-14.3338230138911,-14.1049853155161,
-13.9911346407241,-13.7668625729503,-13.5317910990408,-13.3034542451472,
-13.1121055062976,-12.9980663688873,-12.7755786428509,-12.5511637402028,
-12.3376524508539,-12.1169631347962,-11.89244615783,-11.7786512059243,-11.5484712642546,
-11.2576695020677,-11.1435363437395,-10.8691017091229,-10.7551201682166,
-10.4083152994627,-10.1772149624584,-9.94805105254814,-9.63178517014678,
-9.51704203555597,-9.36866156248235,-9.14039244722859,-8.9051388454019,
-8.68103340781509,-8.56718342498947,-8.33883211661612,-8.10371161990445,
-7.87945222661585,-7.76569166175392,-7.53692932536058,-7.30199255339616,
-7.07763708918854,-6.99961622965257),.UNSPECIFIED.);
#30415=B_SPLINE_CURVE_WITH_KNOTS('',3,(#207564,#207565,#207566,#207567,
#207568,#207569,#207570,#207571,#207572,#207573,#207574,#207575,#207576,
#207577,#207578,#207579,#207580,#207581,#207582,#207583,#207584,#207585,
#207586,#207587,#207588,#207589,#207590,#207591,#207592,#207593,#207594,
#207595,#207596,#207597,#207598,#207599,#207600,#207601,#207602,#207603,
#207604,#207605,#207606,#207607,#207608,#207609,#207610,#207611,#207612,
#207613,#207614,#207615,#207616,#207617,#207618,#207619,#207620,#207621,
#207622,#207623,#207624,#207625,#207626,#207627,#207628,#207629,#207630,
#207631,#207632,#207633,#207634,#207635,#207636,#207637,#207638,#207639,
#207640,#207641),.UNSPECIFIED.,.F.,.F.,(4,2,2,2,2,2,2,2,2,2,2,2,2,2,2,2,
2,2,2,2,2,2,2,2,2,2,2,2,2,2,2,2,2,2,2,2,2,2,4),(-17.6762610095338,-17.5419908579114,
-17.3131157857729,-17.1992573974253,-16.9749636654749,-16.7398785388768,
-16.5115085298758,-16.3975830001727,-16.1734076813033,-15.9381503008392,
-15.7100545893463,-15.5960347950023,-15.3720110876936,-15.1366797103947,
-14.9084672287798,-14.7578872231388,-14.6431928204129,-14.414883927883,
-14.1907508768027,-13.9437496450835,-13.8294506512664,-13.5267457198042,
-13.412662900829,-13.1289422646053,-12.898879177942,-12.7849725900379,-12.5605070969637,
-12.3388849321193,-12.1230679108322,-11.8986867387086,-11.6758968209308,
-11.5618217668304,-11.3774685411443,-11.1487011126834,-10.9136767675669,
-10.6892651770141,-10.4651893114796,-10.3509213635975,-10.2287171917464),
 .UNSPECIFIED.);
#30416=B_SPLINE_CURVE_WITH_KNOTS('',3,(#207646,#207647,#207648,#207649,
#207650,#207651,#207652,#207653,#207654,#207655,#207656,#207657,#207658,
#207659,#207660,#207661,#207662,#207663,#207664,#207665,#207666,#207667,
#207668,#207669,#207670,#207671,#207672,#207673,#207674,#207675,#207676,
#207677,#207678,#207679,#207680,#207681,#207682,#207683,#207684,#207685,
#207686,#207687,#207688,#207689,#207690,#207691,#207692,#207693,#207694,
#207695,#207696,#207697,#207698,#207699,#207700,#207701,#207702,#207703,
#207704,#207705,#207706,#207707,#207708,#207709,#207710,#207711,#207712,
#207713,#207714,#207715,#207716,#207717,#207718,#207719,#207720,#207721),
 .UNSPECIFIED.,.F.,.F.,(4,2,2,2,2,2,2,2,2,2,2,2,2,2,2,2,2,2,2,2,2,2,2,2,
2,2,2,2,2,2,2,2,2,2,2,2,2,4),(-21.8941006277626,-21.780740412087,-21.545887927874,
-21.4315987982601,-21.1966662763011,-20.9720787002586,-20.7868693665202,
-20.5619196383158,-20.3833365915359,-20.2680385408366,-19.9362331764476,
-19.8221772895811,-19.5618881397594,-19.3352647253081,-19.1728063081744,
-19.0579504591606,-18.8293134558212,-18.6050181008145,-18.348427763471,
-18.1198963356815,-18.0055357561925,-17.7815590670609,-17.5793331813053,
-17.3442776335965,-17.1710180856163,-17.0563086033263,-16.7283892268032,
-16.4972731113214,-16.2678539132103,-15.9217722116351,-15.8075940171985,
-15.5841696373609,-15.3592839501101,-15.1246300414118,-15.0103952794729,
-14.7864374327893,-14.5618787393385,-14.4468995549683),.UNSPECIFIED.);
#30417=B_SPLINE_CURVE_WITH_KNOTS('',3,(#207722,#207723,#207724,#207725,
#207726,#207727,#207728,#207729,#207730,#207731,#207732,#207733,#207734,
#207735,#207736,#207737,#207738,#207739,#207740,#207741,#207742,#207743,
#207744,#207745,#207746,#207747,#207748,#207749,#207750,#207751,#207752,
#207753,#207754,#207755,#207756,#207757,#207758,#207759,#207760,#207761,
#207762,#207763,#207764,#207765,#207766,#207767,#207768,#207769,#207770,
#207771,#207772,#207773,#207774,#207775,#207776,#207777,#207778,#207779,
#207780,#207781,#207782,#207783,#207784,#207785,#207786,#207787,#207788,
#207789,#207790,#207791,#207792,#207793,#207794,#207795,#207796,#207797,
#207798,#207799),.UNSPECIFIED.,.F.,.F.,(4,2,2,2,2,2,2,2,2,2,2,2,2,2,2,2,
2,2,2,2,2,2,2,2,2,2,2,2,2,2,2,2,2,2,2,2,2,2,4),(-10.2287171917464,-10.1161007911178,
-9.89141055980067,-9.6678705935114,-9.55364216626409,-9.23717401805758,
-9.12262327489105,-8.88796410295785,-8.66393856533794,-8.5491156077035,
-8.3209369932818,-8.0592223034357,-7.94507330386266,-7.62969963912177,-7.51523207325705,
-7.23314021509567,-7.11877209325123,-6.85536329826687,-6.74132701173776,
-6.41901820793362,-6.30428383308501,-6.13938890573675,-5.90463023907916,
-5.74450993837472,-5.51737633472601,-5.26681979415362,-5.04220502816595,
-4.81376837806515,-4.69871024394659,-4.53568257856599,-4.30924644403034,
-4.04662489230807,-3.9323967044129,-3.69737473426783,-3.47297320997549,
-3.24926425480023,-3.13503985545589,-2.90021146096247,-2.78095249520184),
 .UNSPECIFIED.);
#30418=B_SPLINE_CURVE_WITH_KNOTS('',3,(#207805,#207806,#207807,#207808),
 .UNSPECIFIED.,.F.,.F.,(4,4),(-2.9809807408467E-6,-9.99999997800541E-7),
 .UNSPECIFIED.);
#30419=B_SPLINE_CURVE_WITH_KNOTS('',3,(#207810,#207811,#207812,#207813,
#207814,#207815,#207816,#207817,#207818,#207819,#207820,#207821,#207822,
#207823,#207824,#207825,#207826,#207827,#207828,#207829,#207830,#207831,
#207832,#207833),.UNSPECIFIED.,.F.,.F.,(4,2,2,2,2,2,2,2,2,2,2,4),(-1.88511749360749,
-1.67932546370318,-1.47452695473615,-1.33807794357269,-1.10356671114348,
-0.989276200715796,-0.873916730130468,-0.661501517586868,-0.498025260970523,
-0.252000037949951,-0.126229715468468,-0.0002548003213796),
 .UNSPECIFIED.);
#30420=B_SPLINE_CURVE_WITH_KNOTS('',3,(#207836,#207837,#207838,#207839,
#207840,#207841,#207842,#207843,#207844,#207845,#207846,#207847,#207848,
#207849,#207850,#207851,#207852,#207853,#207854,#207855,#207856,#207857),
 .UNSPECIFIED.,.F.,.F.,(4,2,2,2,2,2,2,2,2,2,4),(5.98718350647653E-5,0.203932709927811,
0.406516261468775,0.541488095383762,0.718522052217883,0.942619519328388,
1.17051888563054,1.39440958810362,1.63674335451152,1.76079483716854,1.88502497314767),
 .UNSPECIFIED.);
#30421=B_SPLINE_CURVE_WITH_KNOTS('',3,(#207860,#207861,#207862,#207863,
#207864,#207865,#207866,#207867,#207868,#207869,#207870,#207871,#207872,
#207873,#207874,#207875,#207876,#207877,#207878,#207879,#207880,#207881,
#207882,#207883,#207884,#207885,#207886,#207887,#207888,#207889,#207890,
#207891,#207892,#207893,#207894,#207895,#207896,#207897,#207898,#207899,
#207900,#207901,#207902,#207903,#207904,#207905,#207906,#207907,#207908,
#207909,#207910,#207911,#207912,#207913,#207914,#207915,#207916,#207917,
#207918,#207919,#207920,#207921,#207922,#207923,#207924,#207925,#207926,
#207927,#207928,#207929,#207930,#207931,#207932,#207933,#207934,#207935),
 .UNSPECIFIED.,.F.,.F.,(4,2,2,2,2,2,2,2,2,2,2,2,2,2,2,2,2,2,2,2,2,2,2,2,
2,2,2,2,2,2,2,2,2,2,2,2,2,4),(-22.7898778497251,-22.5769609640614,-22.3695124452767,
-22.2312330244057,-21.9516446289458,-21.7229229900236,-21.5359972853678,
-21.4220437741558,-21.1514317382949,-20.9221716042284,-20.808009654741,
-20.5838347309842,-20.3491911828098,-20.1193525791475,-20.0052765391877,
-19.7809474046369,-19.5464387603694,-19.3164055772272,-19.2024801658494,
-18.9780819391374,-18.7435052159597,-18.5136887949594,-18.3999053854775,
-18.1754991758094,-17.9407566335972,-17.7114241829266,-17.5976984882579,
-17.3733273241935,-17.1399839200798,-16.9113426684198,-16.7974862500793,
-16.5732417254602,-16.3380788243774,-16.1098509568817,-15.9959077981696,
-15.7718116070002,-15.5365143255446,-15.3427013025877),.UNSPECIFIED.);
#30422=B_SPLINE_CURVE_WITH_KNOTS('',3,(#207938,#207939,#207940,#207941,
#207942,#207943,#207944,#207945,#207946,#207947,#207948,#207949,#207950,
#207951,#207952,#207953,#207954,#207955,#207956,#207957,#207958,#207959,
#207960,#207961,#207962,#207963,#207964,#207965,#207966,#207967,#207968,
#207969,#207970,#207971,#207972,#207973,#207974,#207975,#207976,#207977,
#207978,#207979,#207980,#207981,#207982,#207983,#207984,#207985,#207986,
#207987,#207988,#207989,#207990,#207991,#207992,#207993,#207994,#207995,
#207996,#207997,#207998,#207999,#208000,#208001,#208002,#208003,#208004,
#208005,#208006,#208007,#208008,#208009,#208010,#208011,#208012,#208013,
#208014,#208015),.UNSPECIFIED.,.F.,.F.,(4,2,2,2,2,2,2,2,2,2,2,2,2,2,2,2,
2,2,2,2,2,2,2,2,2,2,2,2,2,2,2,2,2,2,2,2,2,2,4),(-7.44716700303765,-7.38821906924776,
-7.27428145715534,-7.06688827855258,-6.83996772069574,-6.62191392601838,
-6.39766012445358,-6.17371232000397,-6.05949518821232,-5.8245461642506,
-5.60000112988346,-5.37668289458153,-5.26247364391113,-5.02769031769412,
-4.80274782323196,-4.56791504903113,-4.45364256518003,-4.21899719582635,
-3.99432645102175,-3.7701326911471,-3.65593332336233,-3.33757632247385,
-3.22304872331591,-2.94112313631895,-2.8267168206034,-2.56242098741452,
-2.44830716819401,-2.14282098982722,-2.02851425171739,-1.77636422371573,
-1.66241821220455,-1.44250391547649,-1.20765092501976,-1.03094059547456,
-0.796125839660265,-0.602228919090577,-0.45287392841626,-0.226871301920059,
-2.9809807408467E-6),.UNSPECIFIED.);
#30423=B_SPLINE_CURVE_WITH_KNOTS('',3,(#208020,#208021,#208022,#208023,
#208024,#208025,#208026,#208027,#208028,#208029,#208030,#208031,#208032,
#208033,#208034,#208035,#208036,#208037,#208038,#208039,#208040,#208041,
#208042,#208043,#208044,#208045,#208046,#208047,#208048,#208049,#208050,
#208051,#208052,#208053,#208054,#208055,#208056,#208057,#208058,#208059,
#208060,#208061,#208062,#208063,#208064,#208065,#208066,#208067,#208068,
#208069,#208070,#208071,#208072,#208073,#208074,#208075,#208076,#208077,
#208078,#208079,#208080,#208081,#208082,#208083,#208084,#208085,#208086,
#208087,#208088,#208089,#208090,#208091,#208092,#208093,#208094,#208095,
#208096,#208097),.UNSPECIFIED.,.F.,.F.,(4,2,2,2,2,2,2,2,2,2,2,2,2,2,2,2,
2,2,2,2,2,2,2,2,2,2,2,2,2,2,2,2,2,2,2,2,2,2,4),(-14.8946700477258,-14.8517362223534,
-14.6214125150804,-14.4352051146492,-14.3210509902728,-14.0979141027459,
-13.8728253741749,-13.638230718361,-13.5240136865351,-13.3002647009627,
-13.0755452699733,-12.8408118139435,-12.7265409496863,-12.4916521557968,
-12.2667033382962,-12.0523755399774,-11.8242444978479,-11.6248243519107,
-11.3949567393001,-11.2807671494687,-11.1004347878287,-10.8697045571671,
-10.635190741098,-10.4104612772714,-10.1861089283667,-10.0719981856532,
-9.73942527197504,-9.62457831078745,-9.43460635965954,-9.19962189879514,
-9.0854757521845,-8.85637593762672,-8.5832741345898,-8.4693089289279,-8.28989617589463,
-8.06088048439594,-7.75546279704184,-7.64098328995621,-7.44716700303765),
 .UNSPECIFIED.);
#30424=B_SPLINE_CURVE_WITH_KNOTS('',3,(#208098,#208099,#208100,#208101,
#208102,#208103,#208104,#208105,#208106,#208107,#208108,#208109,#208110,
#208111,#208112,#208113,#208114,#208115,#208116,#208117,#208118,#208119,
#208120,#208121,#208122,#208123,#208124,#208125,#208126,#208127,#208128,
#208129,#208130,#208131,#208132,#208133,#208134,#208135,#208136,#208137,
#208138,#208139,#208140,#208141,#208142,#208143,#208144,#208145,#208146,
#208147,#208148,#208149,#208150,#208151,#208152,#208153,#208154,#208155,
#208156,#208157,#208158,#208159,#208160,#208161,#208162,#208163,#208164,
#208165,#208166,#208167,#208168,#208169,#208170,#208171,#208172,#208173,
#208174,#208175,#208176,#208177),.UNSPECIFIED.,.F.,.F.,(4,2,2,2,2,2,2,2,
2,2,2,2,2,2,2,2,2,2,2,2,2,2,2,2,2,2,2,2,2,2,2,2,2,2,2,2,2,2,2,4),(-15.3427013025877,
-15.308377083126,-15.1198299572003,-15.0058773390422,-14.7827804020896,
-14.5479713358685,-14.3128246478954,-14.1989229240919,-13.936125651035,
-13.7072754352123,-13.5929916628281,-13.3689291282708,-13.1682327373279,
-13.0533139372504,-12.7176624551363,-12.6035535375263,-12.3792784911725,
-12.1545198581629,-11.9200025711672,-11.6892296049746,-11.509552355854,
-11.3953619097248,-11.1654843733141,-10.9653174025646,-10.7372355087874,
-10.5246262139959,-10.2996083571961,-10.1000341502175,-9.87582954799773,
-9.76159792532465,-9.53286039336265,-9.30541050113956,-9.08104214635054,
-8.96713906917654,-8.73727439389497,-8.50274606740872,-8.27841007432963,
-8.16435618488069,-7.93445330201098,-7.89546626363725),.UNSPECIFIED.);
#30425=B_SPLINE_CURVE_WITH_KNOTS('',3,(#208182,#208183,#208184,#208185,
#208186,#208187,#208188,#208189,#208190,#208191,#208192,#208193,#208194,
#208195,#208196,#208197,#208198,#208199,#208200,#208201,#208202,#208203,
#208204,#208205,#208206,#208207,#208208,#208209,#208210,#208211,#208212,
#208213,#208214,#208215,#208216,#208217,#208218,#208219,#208220,#208221,
#208222,#208223,#208224,#208225,#208226,#208227,#208228,#208229,#208230,
#208231,#208232,#208233,#208234,#208235,#208236,#208237,#208238,#208239,
#208240,#208241,#208242,#208243,#208244,#208245,#208246,#208247,#208248,
#208249,#208250,#208251,#208252,#208253,#208254,#208255,#208256,#208257),
 .UNSPECIFIED.,.F.,.F.,(4,2,2,2,2,2,2,2,2,2,2,2,2,2,2,2,2,2,2,2,2,2,2,2,
2,2,2,2,2,2,2,2,2,2,2,2,2,4),(-22.342212772346,-22.0873250974015,-21.8590935717735,
-21.7442773051237,-21.5202809959495,-21.2856618803179,-21.0576420432068,
-20.8981008541047,-20.6717097349625,-20.5014524842998,-20.3863957461922,
-20.05201737793,-19.9378145342768,-19.7146260410002,-19.4900223022936,-19.2551146528616,
-19.1409019380648,-18.9170712445363,-18.6927764342657,-18.4576614111678,
-18.2290862188997,-18.0472275704511,-17.9332151496194,-17.7100946558276,
-17.4858717510111,-17.2679229347136,-17.1536153204947,-16.8551315088828,
-16.7410621886897,-16.4741067334556,-16.3596892939691,-16.0508381737592,
-15.9367797235592,-15.654535714996,-15.4246277315006,-15.310679005235,-15.0862764825703,
-14.8946700477258),.UNSPECIFIED.);
#30426=B_SPLINE_CURVE_WITH_KNOTS('',3,(#208258,#208259,#208260,#208261,
#208262,#208263,#208264,#208265,#208266,#208267,#208268,#208269,#208270,
#208271,#208272,#208273,#208274,#208275,#208276,#208277,#208278,#208279,
#208280,#208281,#208282,#208283,#208284,#208285,#208286,#208287,#208288,
#208289,#208290,#208291,#208292,#208293,#208294,#208295,#208296,#208297,
#208298,#208299,#208300,#208301,#208302,#208303,#208304,#208305,#208306,
#208307,#208308,#208309,#208310,#208311,#208312,#208313,#208314,#208315,
#208316,#208317,#208318,#208319,#208320,#208321,#208322,#208323,#208324,
#208325,#208326,#208327,#208328,#208329,#208330,#208331,#208332,#208333,
#208334,#208335),.UNSPECIFIED.,.F.,.F.,(4,2,2,2,2,2,2,2,2,2,2,2,2,2,2,2,
2,2,2,2,2,2,2,2,2,2,2,2,2,2,2,2,2,2,2,2,2,2,4),(-7.89546626363725,-7.69990956786955,
-7.47567575446496,-7.3615016075955,-7.13198331357449,-6.86609849690881,
-6.75212893118196,-6.54990280206718,-6.32194913420725,-6.07666857325898,
-5.8525875973681,-5.6246458581589,-5.51001025855811,-5.22814394054347,-5.11358386940624,
-4.8533923353295,-4.73932613652158,-4.40650160285151,-4.29116066157497,
-4.10963949560704,-3.88487417100665,-3.68607608359745,-3.46186854734996,
-3.34774564045541,-3.1194968319031,-2.90576828195544,-2.68074515135746,
-2.44588963266135,-2.33163405919186,-2.0969520638675,-1.87218683011271,
-1.64853553127989,-1.53433709317659,-1.20205134984514,-1.08724650032732,
-0.913804339188073,-0.687370374613069,-0.51437072350683,-0.448073224698156),
 .UNSPECIFIED.);
#30427=B_SPLINE_CURVE_WITH_KNOTS('',3,(#208343,#208344,#208345,#208346),
 .UNSPECIFIED.,.F.,.F.,(4,4),(0.,0.000776497202964865),.UNSPECIFIED.);
#30428=B_SPLINE_CURVE_WITH_KNOTS('',3,(#208348,#208349,#208350,#208351,
#208352,#208353,#208354,#208355,#208356,#208357,#208358,#208359,#208360,
#208361,#208362,#208363,#208364,#208365,#208366,#208367,#208368,#208369,
#208370,#208371,#208372,#208373,#208374,#208375,#208376,#208377),
 .UNSPECIFIED.,.F.,.F.,(4,2,2,2,2,2,2,2,2,2,2,2,2,2,4),(-2.58819132413446,
-2.36273572464036,-2.13741551586263,-1.98563553180927,-1.79408322231075,
-1.60046605723319,-1.40804760753452,-1.31130466449971,-1.11849752052555,
-0.921488213499352,-0.727078362402644,-0.545763875761525,-0.273849840655809,
-0.136429802224172,-1.19577251067637E-5),.UNSPECIFIED.);
#30429=B_SPLINE_CURVE_WITH_KNOTS('',3,(#208379,#208380,#208381,#208382,
#208383,#208384,#208385,#208386,#208387,#208388,#208389,#208390,#208391,
#208392,#208393,#208394,#208395,#208396,#208397,#208398,#208399,#208400,
#208401,#208402,#208403,#208404,#208405,#208406,#208407,#208408,#208409,
#208410,#208411,#208412),.UNSPECIFIED.,.F.,.F.,(4,2,2,2,2,2,2,2,2,2,2,2,
2,2,2,2,4),(-2.54573725987018,-2.37476608201991,-2.20211346082218,-2.08770172421983,
-1.93349297075943,-1.75019087472518,-1.56693226938438,-1.47443768915391,
-1.29039242591634,-1.19762811175987,-1.0130459107736,-0.825229741583941,
-0.638712708813757,-0.479166346939911,-0.240379360899738,-0.119773973838457,
-2.99430650133206E-6),.UNSPECIFIED.);
#30430=B_SPLINE_CURVE_WITH_KNOTS('',3,(#208415,#208416,#208417,#208418,
#208419,#208420,#208421,#208422,#208423,#208424,#208425,#208426,#208427,
#208428,#208429,#208430,#208431,#208432,#208433,#208434,#208435,#208436,
#208437,#208438,#208439,#208440,#208441,#208442,#208443,#208444,#208445,
#208446,#208447,#208448,#208449,#208450,#208451),.UNSPECIFIED.,.F.,.F.,
(4,3,3,3,3,3,3,3,3,3,3,3,4),(0.,0.0940528831804072,0.188071722346433,0.282046558286573,
0.375986938965022,0.469884151166603,0.5,0.59354846011734,0.686978341974529,
0.780242306989359,0.873402721161719,0.966421835499807,0.999999946312435),
 .UNSPECIFIED.);
#30431=B_SPLINE_CURVE_WITH_KNOTS('',3,(#208454,#208455,#208456,#208457,
#208458,#208459,#208460,#208461,#208462,#208463,#208464,#208465),
 .UNSPECIFIED.,.F.,.F.,(4,2,2,2,2,4),(1.4160226947081E-5,0.103268302452664,
0.209393167484997,0.42464682943301,0.531127353777131,0.94850884172664),
 .UNSPECIFIED.);
#30432=B_SPLINE_CURVE_WITH_KNOTS('',3,(#208474,#208475,#208476,#208477,
#208478,#208479,#208480,#208481),.UNSPECIFIED.,.F.,.F.,(4,2,2,4),(-0.448073224698156,
-0.259160404724375,-0.130320776825101,-0.000536776125191383),
 .UNSPECIFIED.);
#30433=B_SPLINE_CURVE_WITH_KNOTS('',3,(#208482,#208483,#208484,#208485,
#208486,#208487,#208488,#208489),.UNSPECIFIED.,.F.,.F.,(4,2,2,4),(-22.7900378045853,
-22.4589932577425,-22.3488734903167,-22.342212772346),.UNSPECIFIED.);
#30434=B_SPLINE_CURVE_WITH_KNOTS('',3,(#208492,#208493,#208494,#208495,
#208496,#208497,#208498,#208499,#208500,#208501,#208502,#208503,#208504,
#208505,#208506,#208507,#208508,#208509,#208510,#208511,#208512,#208513,
#208514,#208515,#208516,#208517,#208518,#208519,#208520,#208521,#208522,
#208523),.UNSPECIFIED.,.F.,.F.,(4,2,2,2,2,2,2,2,2,2,2,2,2,2,2,4),(-2.78095249520184,
-2.67548166760889,-2.4524117649796,-2.33820932010235,-1.99663964164419,
-1.88152145310964,-1.68782733522852,-1.46342179217326,-1.34957851491786,
-1.1195579922506,-0.885063164301947,-0.66070119563241,-0.497943683992526,
-0.25136918885441,-0.126361115412786,-0.000333910245350815),
 .UNSPECIFIED.);
#30435=B_SPLINE_CURVE_WITH_KNOTS('',3,(#208526,#208527,#208528,#208529,
#208530,#208531,#208532,#208533,#208534,#208535,#208536,#208537,#208538,
#208539,#208540,#208541,#208542,#208543,#208544,#208545,#208546,#208547,
#208548,#208549,#208550,#208551,#208552,#208553,#208554,#208555,#208556,
#208557),.UNSPECIFIED.,.F.,.F.,(4,2,2,2,2,2,2,2,2,2,2,2,2,2,2,4),(-24.6744529274319,
-24.5441174497078,-24.4149402545385,-24.1589241813401,-23.9872705046797,
-23.7608090756699,-23.5877304959073,-23.4729377236922,-23.1408069622114,
-23.0266185261872,-22.8029811384122,-22.5782347091128,-22.3435721538024,
-22.229327493513,-22.0051981112948,-21.8941006277626),.UNSPECIFIED.);
#30436=B_SPLINE_CURVE_WITH_KNOTS('',3,(#208561,#208562,#208563,#208564,
#208565,#208566,#208567,#208568,#208569,#208570,#208571),.UNSPECIFIED.,
 .F.,.F.,(4,2,3,2,4),(-0.707920522022904,-0.389439958817395,0.,0.389439958817396,
0.707920522023273),.UNSPECIFIED.);
#30437=B_SPLINE_CURVE_WITH_KNOTS('',3,(#208575,#208576,#208577,#208578,
#208579,#208580,#208581,#208582,#208583,#208584,#208585),.UNSPECIFIED.,
 .F.,.F.,(4,2,3,2,4),(-0.704027076636135,-0.390169294707907,0.,0.390169294707907,
0.573011129927055),.UNSPECIFIED.);
#30438=B_SPLINE_CURVE_WITH_KNOTS('',3,(#208587,#208588,#208589,#208590),
 .UNSPECIFIED.,.F.,.F.,(4,4),(0.573011129927055,0.704038599815001),
 .UNSPECIFIED.);
#30439=B_SPLINE_CURVE_WITH_KNOTS('',3,(#208596,#208597,#208598,#208599,
#208600,#208601,#208602,#208603,#208604,#208605,#208606,#208607,#208608,
#208609,#208610,#208611,#208612,#208613,#208614,#208615,#208616,#208617,
#208618,#208619,#208620,#208621,#208622,#208623,#208624,#208625,#208626,
#208627,#208628,#208629,#208630,#208631),.UNSPECIFIED.,.F.,.F.,(4,2,2,2,
2,2,2,2,2,2,2,2,2,2,2,2,2,4),(-2.69278601163599,-2.48949828257243,-2.28229533337829,
-2.14458879630755,-1.96754811547389,-1.79103983134423,-1.61387421528426,
-1.43688712002345,-1.34835665175354,-1.25978242305215,-1.08286142570342,
-0.905901114542216,-0.728942624529302,-0.640388431956018,-0.480377748967097,
-0.240145438538195,-0.120091889664005,-0.000154281172380586),
 .UNSPECIFIED.);
#30440=B_SPLINE_CURVE_WITH_KNOTS('',3,(#208632,#208633,#208634,#208635,
#208636,#208637,#208638,#208639,#208640,#208641,#208642,#208643,#208644,
#208645,#208646,#208647,#208648,#208649,#208650,#208651,#208652,#208653,
#208654,#208655,#208656,#208657,#208658,#208659,#208660,#208661,#208662,
#208663),.UNSPECIFIED.,.F.,.F.,(4,2,2,2,2,2,2,2,2,2,2,2,2,2,2,4),(-2.46530051632041,
-2.26819680103668,-2.0711954618087,-1.93999090652036,-1.76308472873804,
-1.58642929790919,-1.40948483540281,-1.23270430940088,-1.05614800855081,
-0.879169642198454,-0.70232687435545,-0.525413854333788,-0.394197725784304,
-0.197144745652711,-0.098600755514457,-0.00026354035724065),
 .UNSPECIFIED.);
#30441=B_SPLINE_CURVE_WITH_KNOTS('',3,(#208665,#208666,#208667,#208668,
#208669,#208670,#208671,#208672,#208673,#208674,#208675,#208676,#208677,
#208678,#208679,#208680,#208681,#208682,#208683,#208684,#208685,#208686,
#208687,#208688,#208689,#208690),.UNSPECIFIED.,.F.,.F.,(4,2,2,2,2,2,2,2,
2,2,2,2,4),(0.000318650702430989,0.313346654756281,0.619041496227019,0.795573539849274,
0.972003501309865,1.14847338462624,1.32604214603395,1.68155740636289,1.85805892632572,
2.01000672201703,2.23835919370013,2.35285672004845,2.46729888736451),
 .UNSPECIFIED.);
#30442=B_SPLINE_CURVE_WITH_KNOTS('',3,(#208691,#208692,#208693,#208694,
#208695,#208696,#208697,#208698,#208699,#208700,#208701,#208702,#208703,
#208704,#208705,#208706,#208707,#208708,#208709,#208710,#208711,#208712,
#208713,#208714,#208715,#208716,#208717,#208718,#208719,#208720,#208721,
#208722,#208723,#208724),.UNSPECIFIED.,.F.,.F.,(4,2,2,2,2,2,2,2,2,2,2,2,
2,2,2,2,4),(0.000172246164436567,0.137421022141082,0.274393772366344,0.548014374963287,
0.723403918543801,0.900115220230536,1.07657539273742,1.2530000195469,1.43023283105391,
1.78627983687558,1.87475797459756,2.05193109982066,2.14050606857681,2.31698437617588,
2.58688830258845,2.72343273743266,2.86001317919873),.UNSPECIFIED.);
#30443=B_SPLINE_CURVE_WITH_KNOTS('',3,(#208727,#208728,#208729,#208730,
#208731,#208732,#208733,#208734,#208735,#208736,#208737,#208738,#208739,
#208740,#208741,#208742,#208743,#208744,#208745,#208746,#208747,#208748,
#208749,#208750,#208751,#208752,#208753,#208754,#208755,#208756,#208757,
#208758,#208759,#208760),.UNSPECIFIED.,.F.,.F.,(4,2,2,2,2,2,2,2,2,2,2,2,
2,2,2,2,4),(-2.8604020772222,-2.72399588747906,-2.55750044548352,-2.37620089410916,
-2.22874860029063,-2.08275318086539,-1.92798249835796,-1.83854814703534,
-1.62320721676794,-1.45286930809083,-1.28281138427904,-1.1241953649196,
-0.967800004567202,-0.815712191339319,-0.636830671478215,-0.323116638129756,
-9.999999992516E-7),.UNSPECIFIED.);
#30444=B_SPLINE_CURVE_WITH_KNOTS('',3,(#208761,#208762,#208763,#208764,
#208765,#208766,#208767,#208768,#208769,#208770,#208771,#208772,#208773,
#208774,#208775,#208776,#208777,#208778,#208779,#208780,#208781,#208782,
#208783,#208784),.UNSPECIFIED.,.F.,.F.,(4,2,2,2,2,2,2,2,2,2,2,4),(-2.07371028241749,
-1.89670800669829,-1.71936907534134,-1.60400157839947,-1.44968076203279,
-1.09401343926072,-0.738422470297299,-0.650645320698835,-0.49885496807562,
-0.251161098077026,-0.127294929010069,-0.000361776623960997),
 .UNSPECIFIED.);
#30445=B_SPLINE_CURVE_WITH_KNOTS('',3,(#208786,#208787,#208788,#208789,
#208790,#208791,#208792,#208793,#208794,#208795,#208796,#208797,#208798,
#208799,#208800,#208801,#208802,#208803,#208804,#208805,#208806,#208807,
#208808,#208809,#208810,#208811),.UNSPECIFIED.,.F.,.F.,(4,2,2,2,2,2,2,2,
2,2,2,2,4),(0.000219774120001982,0.128265976878421,0.255769893159645,0.493856419136348,
0.651486942309498,0.821726852996698,1.03589976718762,1.25551703969407,1.39399885601373,
1.57317372451604,1.8211861086334,1.94515901785526,2.07223113354374),
 .UNSPECIFIED.);
#30446=B_SPLINE_CURVE_WITH_KNOTS('',3,(#208812,#208813,#208814,#208815,
#208816,#208817,#208818,#208819,#208820,#208821,#208822,#208823,#208824,
#208825,#208826,#208827,#208828,#208829,#208830,#208831,#208832,#208833,
#208834,#208835,#208836,#208837,#208838,#208839,#208840,#208841,#208842,
#208843,#208844,#208845),.UNSPECIFIED.,.F.,.F.,(4,2,2,2,2,2,2,2,2,2,2,2,
2,2,2,2,4),(-20.0267697459016,-19.7034013542535,-19.3891929917687,-19.2102906022386,
-19.0571883022074,-18.9019968771614,-18.7436220861097,-18.5735973213373,
-18.4032735363198,-18.1880846617368,-18.0986525161132,-17.9441161047557,
-17.7977744331096,-17.6503832691351,-17.4690817117426,-17.3026231029396,
-17.166235588483),.UNSPECIFIED.);
#30447=B_SPLINE_CURVE_WITH_KNOTS('',3,(#208848,#208849,#208850,#208851,
#208852,#208853,#208854,#208855,#208856,#208857,#208858,#208859,#208860,
#208861,#208862,#208863,#208864,#208865,#208866,#208867,#208868,#208869,
#208870,#208871,#208872,#208873,#208874,#208875,#208876,#208877,#208878,
#208879),.UNSPECIFIED.,.F.,.F.,(4,2,2,2,2,2,2,2,2,2,2,2,2,2,2,4),(-2.8610678083529,
-2.77118001727313,-2.62423597662898,-2.47550480424851,-2.17505208121599,
-1.8194196555836,-1.64521569280835,-1.4743719964416,-1.30309359694003,-1.1333766862558,
-0.917899747742497,-0.74777190157107,-0.576876204814989,-0.435632361078004,
-0.28735165256909,-9.99999999695689E-7),.UNSPECIFIED.);
#30448=B_SPLINE_CURVE_WITH_KNOTS('',3,(#208881,#208882,#208883,#208884,
#208885,#208886,#208887,#208888,#208889,#208890,#208891,#208892,#208893,
#208894,#208895,#208896,#208897,#208898,#208899,#208900,#208901,#208902),
 .UNSPECIFIED.,.F.,.F.,(4,2,2,2,2,2,2,2,2,2,4),(-1.6783918973356,-1.54864602744031,
-1.41972171226195,-1.17041428893027,-1.02310065652554,-0.854629785345839,
-0.705938566731539,-0.530158415550069,-0.26465166379874,-0.13428370906012,
-0.00063552929898788),.UNSPECIFIED.);
#30449=B_SPLINE_CURVE_WITH_KNOTS('',3,(#208904,#208905,#208906,#208907),
 .UNSPECIFIED.,.F.,.F.,(4,4),(0.,1.),.UNSPECIFIED.);
#30450=B_SPLINE_CURVE_WITH_KNOTS('',3,(#208909,#208910,#208911,#208912,
#208913,#208914,#208915,#208916,#208917,#208918,#208919,#208920,#208921,
#208922,#208923,#208924,#208925,#208926,#208927,#208928,#208929,#208930),
 .UNSPECIFIED.,.F.,.F.,(4,2,2,2,2,2,2,2,2,2,4),(0.000147978863487718,0.132665880139302,
0.264039836415925,0.521001553776919,0.701578774201878,0.83899587449096,
1.11207159356816,1.25225787140647,1.45962584134195,1.56800447112712,1.67810387049899),
 .UNSPECIFIED.);
#30451=B_SPLINE_CURVE_WITH_KNOTS('',3,(#208931,#208932,#208933,#208934,
#208935,#208936,#208937,#208938,#208939,#208940,#208941,#208942,#208943,
#208944,#208945,#208946,#208947,#208948,#208949,#208950,#208951,#208952,
#208953,#208954,#208955,#208956,#208957,#208958,#208959,#208960,#208961,
#208962),.UNSPECIFIED.,.F.,.F.,(4,2,2,2,2,2,2,2,2,2,2,2,2,2,2,4),(-20.0228897850774,
-19.7547732797997,-19.6058056189287,-19.4708760835207,-19.2549323436283,
-19.0852647002444,-18.8857336685939,-18.7179066463893,-18.5469453747283,
-18.3762608119982,-18.2022424489253,-17.8465788019333,-17.5488974776113,
-17.3980719908646,-17.2515164719589,-17.1620566513902),.UNSPECIFIED.);
#30452=B_SPLINE_CURVE_WITH_KNOTS('',3,(#208992,#208993,#208994,#208995,
#208996,#208997,#208998,#208999,#209000,#209001,#209002,#209003,#209004,
#209005,#209006,#209007,#209008,#209009,#209010),.UNSPECIFIED.,.F.,.F.,
(4,3,3,3,3,3,4),(0.,0.188384660261452,0.240000922766572,0.500001230410849,
0.760001538055127,0.945884007376155,0.999999610267735),.UNSPECIFIED.);
#30453=B_SPLINE_CURVE_WITH_KNOTS('',3,(#209013,#209014,#209015,#209016,
#209017,#209018,#209019,#209020,#209021,#209022,#209023,#209024,#209025,
#209026),.UNSPECIFIED.,.F.,.F.,(4,2,2,2,2,2,4),(0.000337787465763639,0.284976578385995,
0.575874331198097,0.935643861114864,1.30221214423588,1.60875324692267,1.91914645332358),
 .UNSPECIFIED.);
#30454=B_SPLINE_CURVE_WITH_KNOTS('',3,(#209297,#209298,#209299,#209300,
#209301,#209302,#209303,#209304,#209305,#209306,#209307,#209308,#209309,
#209310,#209311,#209312,#209313,#209314,#209315,#209316,#209317,#209318,
#209319,#209320,#209321,#209322,#209323,#209324,#209325,#209326,#209327,
#209328,#209329,#209330,#209331,#209332,#209333,#209334),.UNSPECIFIED.,
 .F.,.F.,(4,2,2,2,2,2,2,2,2,2,2,2,2,2,2,2,2,2,4),(-25.3605959634744,-25.2299176631067,
-25.1016543086936,-24.859881463169,-24.6979355907445,-24.3835783247934,
-24.2847913992405,-23.9723612276356,-23.8735088087347,-23.5593401804643,
-23.4605396458714,-23.1477400987566,-22.9907821446129,-22.8912511255084,
-22.4856054757622,-22.1082880433666,-21.9057075956864,-21.7029412164806,
-21.689764260827),.UNSPECIFIED.);
#30455=B_SPLINE_CURVE_WITH_KNOTS('',3,(#209604,#209605,#209606,#209607,
#209608,#209609),.UNSPECIFIED.,.F.,.F.,(4,2,4),(1.30310740020753E-6,0.0653973385639156,
0.130262424727681),.UNSPECIFIED.);
#30456=B_SPLINE_CURVE_WITH_KNOTS('',3,(#209638,#209639,#209640,#209641,
#209642,#209643),.UNSPECIFIED.,.F.,.F.,(4,2,4),(-0.0180566566914832,-0.00903372775874852,
-8.36277988998135E-7),.UNSPECIFIED.);
#30457=B_SPLINE_CURVE_WITH_KNOTS('',3,(#209645,#209646,#209647,#209648,
#209649,#209650),.UNSPECIFIED.,.F.,.F.,(4,2,4),(-0.0180610510695298,-0.00903269966892605,
-5.26550410692647E-6),.UNSPECIFIED.);
#30458=B_SPLINE_CURVE_WITH_KNOTS('',3,(#209679,#209680,#209681,#209682,
#209683,#209684),.UNSPECIFIED.,.F.,.F.,(4,2,4),(0.000679919887194027,0.0656077343225083,
0.130948244492649),.UNSPECIFIED.);
#30459=B_SPLINE_CURVE_WITH_KNOTS('',3,(#210299,#210300,#210301,#210302,
#210303,#210304),.UNSPECIFIED.,.F.,.F.,(4,2,4),(1.37679443180464E-6,0.132788624167646,
0.261946710422712),.UNSPECIFIED.);
#30460=B_SPLINE_CURVE_WITH_KNOTS('',3,(#210305,#210306,#210307,#210308,
#210309,#210310),.UNSPECIFIED.,.F.,.F.,(4,2,4),(9.69834488243248E-6,0.0602748062235942,
0.119740503039534),.UNSPECIFIED.);
#30461=B_SPLINE_CURVE_WITH_KNOTS('',3,(#210323,#210324,#210325,#210326,
#210327,#210328,#210329,#210330,#210331,#210332),.UNSPECIFIED.,.F.,.F.,
(4,2,2,2,4),(2.46055889067629,2.77696986044635,3.16672845187631,3.55648704330627,
3.87289801307632),.UNSPECIFIED.);
#30462=B_SPLINE_CURVE_WITH_KNOTS('',3,(#210334,#210335,#210336,#210337,
#210338,#210339),.UNSPECIFIED.,.F.,.F.,(4,2,4),(3.76834231838167E-5,0.27701452139551,
0.555926380958724),.UNSPECIFIED.);
#30463=B_SPLINE_CURVE_WITH_KNOTS('',3,(#210369,#210370,#210371,#210372,
#210373,#210374,#210375,#210376,#210377,#210378,#210379,#210380,#210381,
#210382,#210383,#210384,#210385,#210386,#210387),.UNSPECIFIED.,.F.,.F.,
(4,3,3,3,3,3,4),(0.,0.176916349750736,0.240000637218415,0.500000956530079,
0.760001275841745,0.935051760779978,0.999999692665182),.UNSPECIFIED.);
#30464=B_SPLINE_CURVE_WITH_KNOTS('',3,(#210390,#210391,#210392,#210393,
#210394,#210395,#210396,#210397,#210398,#210399,#210400,#210401,#210402,
#210403),.UNSPECIFIED.,.F.,.F.,(4,2,2,2,2,2,4),(0.000167093672002118,0.369844031545408,
0.745935182508687,1.21004916822787,1.6809812805177,2.07272751301276,2.4680790456475),
 .UNSPECIFIED.);
#30465=B_SPLINE_CURVE_WITH_KNOTS('',3,(#210545,#210546,#210547,#210548,
#210549,#210550,#210551,#210552,#210553,#210554,#210555,#210556,#210557,
#210558,#210559,#210560,#210561,#210562,#210563,#210564,#210565,#210566,
#210567,#210568,#210569,#210570,#210571,#210572,#210573,#210574,#210575,
#210576,#210577,#210578,#210579,#210580,#210581,#210582,#210583,#210584,
#210585,#210586,#210587,#210588,#210589,#210590,#210591,#210592,#210593,
#210594,#210595,#210596,#210597,#210598,#210599,#210600,#210601,#210602,
#210603,#210604,#210605,#210606,#210607,#210608,#210609,#210610,#210611,
#210612,#210613,#210614,#210615,#210616,#210617,#210618,#210619,#210620,
#210621,#210622,#210623,#210624,#210625,#210626,#210627,#210628,#210629,
#210630,#210631,#210632,#210633,#210634,#210635,#210636,#210637,#210638,
#210639,#210640,#210641,#210642,#210643,#210644,#210645,#210646,#210647,
#210648,#210649,#210650,#210651,#210652,#210653,#210654,#210655,#210656,
#210657,#210658,#210659,#210660,#210661,#210662,#210663,#210664,#210665,
#210666,#210667,#210668,#210669,#210670,#210671,#210672,#210673,#210674,
#210675,#210676,#210677,#210678,#210679,#210680,#210681,#210682,#210683,
#210684,#210685,#210686,#210687,#210688,#210689,#210690,#210691,#210692,
#210693,#210694,#210695,#210696,#210697,#210698,#210699,#210700,#210701,
#210702,#210703,#210704,#210705,#210706,#210707,#210708,#210709,#210710,
#210711,#210712,#210713,#210714,#210715,#210716,#210717,#210718,#210719,
#210720,#210721,#210722,#210723,#210724,#210725,#210726,#210727,#210728,
#210729,#210730,#210731,#210732,#210733,#210734,#210735,#210736,#210737,
#210738,#210739,#210740,#210741,#210742,#210743,#210744,#210745,#210746,
#210747,#210748,#210749,#210750),.UNSPECIFIED.,.F.,.F.,(4,2,2,2,2,2,2,2,
2,2,2,2,2,2,2,2,2,2,2,2,2,2,2,2,2,2,2,2,2,2,2,2,2,2,2,2,2,2,2,2,2,2,2,2,
2,2,2,2,2,2,2,2,2,2,2,2,2,2,2,2,2,2,2,2,2,2,2,2,2,2,2,2,2,2,2,2,2,2,2,2,
2,2,2,2,2,2,2,2,2,2,2,2,2,2,2,2,2,2,2,2,2,2,4),(0.00107990835998589,0.0329071537590182,
0.195893328033104,0.355153898355014,0.434988215509004,0.642816516674076,
0.737569287381765,0.908716883124716,0.993153014695592,1.18963661548505,
1.28754502534697,1.47339632996793,1.55811137750697,1.76173951263956,1.85370473288822,
2.02895304659489,2.11938121696687,2.33665348563873,2.4229728740814,2.59661267496729,
2.68840363087139,2.90216045936439,2.98711838103119,3.1734242939562,3.26349749387919,
3.45824610570519,3.54619696517821,3.73710767095252,3.83188019060896,4.03301640764842,
4.1174764626154,4.30305199918925,4.40238831686129,4.60868154531538,4.68987410516886,
4.87477538174019,4.97656143336439,5.17614663824206,5.25912879747928,5.44612356898342,
5.55060337109826,5.7420288787186,5.82728553412066,6.01648422296294,6.12403067649721,
6.30698556070633,6.39486121220803,6.59463365048308,6.70174065578835,6.86827502056953,
6.957226649254,7.16281963592479,7.27369262076292,7.43009960965057,7.5220123839873,
7.70970084821241,7.83380812566714,7.98940531492064,8.08401416975494,8.26759687546506,
8.40024551700738,8.54235987947,8.63766384309952,8.81511758034529,9.02203998410492,
9.12411504839395,9.27578319432331,9.43003056609417,9.6064767873789,9.70887427476012,
9.85136721032997,10.0286666133371,10.1832040076769,10.2906557504572,10.4409835687639,
10.7071639933474,10.8497640564256,11.0174209495745,11.3445265446232,11.4731243770269,
11.6129658838983,11.9583938225873,12.0723592156197,12.2439881908159,12.4769173317724,
12.6198592275825,12.7939302219618,13.0253846296432,13.188025339889,13.3844928168393,
13.6178785486688,13.7866824791461,14.047968468405,14.5213773907695,14.7566219201825,
14.8883214848249,15.2208691883029,15.4554942000865,15.9304221828407,16.0434638694231,
16.5048987708617,16.8936209742175,17.2855462784105),.UNSPECIFIED.);
#30466=B_SPLINE_CURVE_WITH_KNOTS('',3,(#210752,#210753,#210754,#210755,
#210756,#210757,#210758,#210759,#210760,#210761,#210762,#210763,#210764,
#210765,#210766,#210767,#210768,#210769,#210770,#210771,#210772,#210773,
#210774,#210775,#210776,#210777,#210778,#210779,#210780,#210781,#210782,
#210783,#210784,#210785,#210786,#210787,#210788,#210789,#210790,#210791,
#210792,#210793,#210794,#210795,#210796,#210797,#210798,#210799,#210800,
#210801,#210802,#210803,#210804,#210805,#210806,#210807,#210808,#210809,
#210810,#210811,#210812,#210813,#210814,#210815,#210816,#210817,#210818,
#210819,#210820,#210821,#210822,#210823,#210824,#210825,#210826,#210827,
#210828,#210829,#210830,#210831,#210832,#210833,#210834,#210835,#210836),
 .UNSPECIFIED.,.F.,.F.,(4,3,3,3,3,3,3,3,3,3,3,3,3,3,3,3,3,3,3,3,3,3,3,3,
3,3,3,3,4),(0.,0.047552339646909,0.0945933459078274,0.141741666696633,0.18879608789237,
0.236701745213095,0.246392852639966,0.250474334099904,0.297627468266538,
0.344829936104484,0.380418717175272,0.427580266713761,0.474808467386502,
0.496867832817848,0.502907306283412,0.549192807164965,0.595728951546223,
0.642323912201335,0.688682512723011,0.723451463114268,0.738537131268896,
0.747378843505563,0.752846656310363,0.801913023150851,0.827758314288039,
0.876702333074763,0.925834305036086,0.974954869278943,0.999217082393029),
 .UNSPECIFIED.);
#30467=B_SPLINE_CURVE_WITH_KNOTS('',3,(#210838,#210839,#210840,#210841),
 .UNSPECIFIED.,.F.,.F.,(4,4),(-0.000244606540981952,0.),.UNSPECIFIED.);
#30468=B_SPLINE_CURVE_WITH_KNOTS('',3,(#210842,#210843,#210844,#210845,
#210846,#210847,#210848,#210849,#210850,#210851,#210852,#210853,#210854,
#210855,#210856,#210857,#210858,#210859,#210860,#210861,#210862,#210863,
#210864,#210865,#210866,#210867,#210868,#210869,#210870,#210871,#210872,
#210873,#210874,#210875,#210876,#210877,#210878,#210879,#210880,#210881,
#210882,#210883,#210884,#210885,#210886,#210887,#210888,#210889,#210890,
#210891,#210892,#210893,#210894,#210895,#210896,#210897,#210898,#210899,
#210900,#210901,#210902,#210903,#210904,#210905,#210906,#210907,#210908,
#210909,#210910,#210911,#210912,#210913,#210914,#210915,#210916,#210917,
#210918,#210919,#210920,#210921,#210922,#210923,#210924,#210925,#210926,
#210927,#210928,#210929,#210930,#210931,#210932,#210933,#210934,#210935,
#210936,#210937,#210938,#210939,#210940,#210941,#210942,#210943,#210944,
#210945,#210946,#210947,#210948,#210949,#210950,#210951,#210952,#210953,
#210954,#210955,#210956,#210957,#210958,#210959,#210960,#210961,#210962,
#210963,#210964,#210965,#210966,#210967,#210968,#210969,#210970,#210971,
#210972,#210973,#210974,#210975,#210976,#210977,#210978,#210979,#210980,
#210981,#210982,#210983,#210984,#210985,#210986,#210987,#210988,#210989,
#210990,#210991,#210992,#210993,#210994,#210995,#210996,#210997,#210998,
#210999,#211000,#211001,#211002,#211003,#211004,#211005,#211006,#211007,
#211008,#211009,#211010,#211011,#211012,#211013,#211014,#211015,#211016,
#211017,#211018,#211019),.UNSPECIFIED.,.F.,.F.,(4,2,2,2,2,2,2,2,2,2,2,2,
2,2,2,2,2,2,2,2,2,2,2,2,2,2,2,2,2,2,2,2,2,2,2,2,2,2,2,2,2,2,2,2,2,2,2,2,
2,2,2,2,2,2,2,2,2,2,2,2,2,2,2,2,2,2,2,2,2,2,2,2,2,2,2,2,2,2,2,2,2,2,2,2,
2,2,2,2,4),(-17.8874346104741,-17.5294919406818,-17.186048243618,-16.9295394703044,
-16.8092492886893,-16.1896824714199,-15.8340272539635,-15.2083864407959,
-14.9204681111906,-14.3899595901558,-14.1556344485288,-13.9783598067019,
-13.7492496008297,-13.5994074640869,-13.4666029323457,-13.36660794238,-13.154214154486,
-12.9906873703296,-12.887536511039,-12.7359106835424,-12.5879560881589,
-12.4262389067138,-12.325210118249,-12.1497599741407,-12.0316602780003,
-11.844332676878,-11.7509492084952,-11.5889580967691,-11.4836693199961,
-11.2966545631598,-11.192487027676,-11.0521608686276,-10.9450814860788,
-10.7612433258855,-10.6366324078592,-10.4865596856504,-10.346504062992,
-10.1283588143909,-10.0182524554306,-9.89616481205125,-9.58905421185916,
-9.07549190179132,-8.68076130995556,-8.46605691773842,-8.01018323272566,
-7.6210762100739,-7.24137219648118,-6.65939456135951,-6.42566825698983,
-6.19571944234743,-5.93321022345773,-5.81507259108846,-5.6394297626821,
-5.45310433689612,-5.2600764092861,-5.15380952310406,-5.03637349809631,
-4.82334403415801,-4.68443024678171,-4.54527121636483,-4.4172699568073,
-4.24519534314461,-4.1387700467407,-4.00127907201438,-3.88561719144662,
-3.73605126424484,-3.64032051175329,-3.46696552173688,-3.36568283466442,
-3.21304464574596,-3.10894067512593,-2.93016448528719,-2.83463383876123,
-2.67405588966363,-2.53885135281782,-2.39350009266653,-2.2994834121646,
-2.13842813199443,-1.95939869234199,-1.82841008968958,-1.69294839797772,
-1.5518629856045,-1.33346072700906,-1.18729433138863,-0.994382017820723,
-0.767650200558565,-0.680987224726351,-0.341206102852212,-0.000193437912456803),
 .UNSPECIFIED.);
#30469=B_SPLINE_CURVE_WITH_KNOTS('',3,(#211289,#211290,#211291,#211292,
#211293,#211294),.UNSPECIFIED.,.F.,.F.,(4,2,4),(-0.131003728994287,-0.0656099055372978,
-3.86587579667962E-6),.UNSPECIFIED.);
#30470=B_SPLINE_CURVE_WITH_KNOTS('',3,(#211296,#211297,#211298,#211299,
#211300,#211301,#211302,#211303,#211304,#211305,#211306,#211307,#211308,
#211309,#211310,#211311,#211312,#211313,#211314,#211315,#211316,#211317,
#211318,#211319,#211320,#211321,#211322,#211323,#211324,#211325,#211326,
#211327,#211328,#211329,#211330,#211331,#211332,#211333,#211334,#211335,
#211336,#211337,#211338,#211339,#211340,#211341,#211342,#211343,#211344,
#211345,#211346,#211347,#211348,#211349,#211350,#211351,#211352,#211353),
 .UNSPECIFIED.,.F.,.F.,(4,2,2,2,2,2,2,2,2,2,2,2,2,2,2,2,2,2,2,2,2,2,2,2,
2,2,2,2,4),(-6.15860212849669,-6.06515038114135,-5.83681474701059,-5.60593974251633,
-5.31433449222845,-5.18909714071076,-4.9413569458906,-4.68314415669207,
-4.55804547761989,-4.30742774828901,-4.06523839474389,-3.80702431616562,
-3.68220920617004,-3.43109416439227,-3.17048590815028,-2.91233401200879,
-2.78665746308759,-2.52874309402958,-2.25501193498755,-2.13006946787647,
-1.75457334893578,-1.62820215757801,-1.43603946055039,-1.20517175944087,
-0.920799061189383,-0.807044726910511,-0.445490300674665,-0.334664291987655,
-3.49174065404852E-5),.UNSPECIFIED.);
#30471=B_SPLINE_CURVE_WITH_KNOTS('',3,(#211382,#211383,#211384,#211385,
#211386,#211387),.UNSPECIFIED.,.F.,.F.,(4,2,4),(-0.0180614175475543,-0.00903747414230311,
-8.04914190790971E-7),.UNSPECIFIED.);
#30472=B_SPLINE_CURVE_WITH_KNOTS('',3,(#211388,#211389,#211390,#211391,
#211392,#211393,#211394,#211395,#211396,#211397,#211398,#211399,#211400,
#211401),.UNSPECIFIED.,.F.,.F.,(4,2,2,2,2,2,4),(1.00000038869935E-6,0.377507126467116,
0.760172295625594,1.01061719312917,1.51716116734711,1.76732387692719,2.02167921549907),
 .UNSPECIFIED.);
#30473=B_SPLINE_CURVE_WITH_KNOTS('',3,(#211403,#211404,#211405,#211406,
#211407,#211408),.UNSPECIFIED.,.F.,.F.,(4,2,4),(-0.0180670199973744,-0.00903616121666639,
-6.43699294978515E-6),.UNSPECIFIED.);
#30474=B_SPLINE_CURVE_WITH_KNOTS('',3,(#211437,#211438,#211439,#211440,
#211441,#211442),.UNSPECIFIED.,.F.,.F.,(4,2,4),(-0.131007272486104,-0.0654519130722608,
-7.32542528862561E-6),.UNSPECIFIED.);
#30475=B_SPLINE_CURVE_WITH_KNOTS('',3,(#211711,#211712,#211713,#211714,
#211715,#211716,#211717,#211718,#211719,#211720,#211721,#211722,#211723,
#211724,#211725,#211726,#211727,#211728,#211729,#211730,#211731,#211732,
#211733,#211734,#211735,#211736,#211737,#211738,#211739,#211740,#211741,
#211742,#211743,#211744,#211745,#211746,#211747,#211748,#211749,#211750,
#211751,#211752,#211753,#211754,#211755,#211756,#211757,#211758,#211759,
#211760,#211761,#211762,#211763,#211764,#211765,#211766,#211767,#211768,
#211769,#211770,#211771,#211772,#211773,#211774,#211775,#211776,#211777,
#211778,#211779,#211780,#211781,#211782,#211783,#211784,#211785,#211786,
#211787,#211788),.UNSPECIFIED.,.F.,.F.,(4,2,2,2,2,2,2,2,2,2,2,2,2,2,2,2,
2,2,2,2,2,2,2,2,2,2,2,2,2,2,2,2,2,2,2,2,2,2,4),(-20.9312459291626,-20.8238269097937,
-20.5931648525945,-20.3353373519583,-20.1701043049685,-19.9383799110844,
-19.702397418043,-19.451963635314,-19.3267742859618,-19.0685720740393,-18.8337543042022,
-18.5759062577988,-18.4504717029174,-18.1922860321218,-17.9373418768597,
-17.6863787711074,-17.5614775151041,-17.3032678569112,-17.0594109215148,
-16.8087504776042,-16.6471745738218,-16.4156901290353,-16.1896876711962,
-16.0642108166878,-15.7633972745444,-15.5054078770155,-15.3311008092168,
-15.0986958752912,-14.8699701821476,-14.6121430096181,-14.4868124487622,
-14.2286099369188,-13.9920525360736,-13.7605761499709,-13.5444790500576,
-13.3280590731181,-13.0965913797703,-12.8599164248024,-12.7553611554937),
 .UNSPECIFIED.);
#30476=B_SPLINE_CURVE_WITH_KNOTS('',3,(#212200,#212201,#212202,#212203,
#212204,#212205),.UNSPECIFIED.,.F.,.F.,(4,2,4),(-0.344875729523264,-0.172579825677985,
-3.94566552320122E-5),.UNSPECIFIED.);
#30477=B_SPLINE_CURVE_WITH_KNOTS('',3,(#212206,#212207,#212208,#212209),
 .UNSPECIFIED.,.F.,.F.,(4,4),(-0.000257082057276752,0.),.UNSPECIFIED.);
#30478=B_SPLINE_CURVE_WITH_KNOTS('',3,(#212621,#212622,#212623,#212624,
#212625,#212626),.UNSPECIFIED.,.F.,.F.,(4,2,4),(-0.344703474824345,-0.172091835354049,
-0.00130738802397509),.UNSPECIFIED.);
#30479=B_SPLINE_CURVE_WITH_KNOTS('',3,(#212627,#212628,#212629,#212630),
 .UNSPECIFIED.,.F.,.F.,(4,4),(-0.00138054251324295,0.),.UNSPECIFIED.);
#30480=B_SPLINE_CURVE_WITH_KNOTS('',3,(#212657,#212658,#212659,#212660,
#212661,#212662),.UNSPECIFIED.,.F.,.F.,(4,2,4),(0.000411407934210648,0.132395690524123,
0.265296797891605),.UNSPECIFIED.);
#30481=B_SPLINE_CURVE_WITH_KNOTS('',3,(#212665,#212666,#212667,#212668),
 .UNSPECIFIED.,.F.,.F.,(4,4),(0.,0.000434666445632145),.UNSPECIFIED.);
#30482=B_SPLINE_CURVE_WITH_KNOTS('',3,(#212670,#212671,#212672,#212673,
#212674,#212675,#212676,#212677,#212678,#212679,#212680,#212681,#212682,
#212683,#212684,#212685,#212686,#212687,#212688,#212689,#212690,#212691),
 .UNSPECIFIED.,.F.,.F.,(4,2,2,2,2,2,2,2,2,2,4),(0.,0.144173778921579,0.288103676995469,
0.573727861047774,0.772563733388318,1.17379786176643,1.57506737125788,1.77392881725764,
1.91671525972644,2.13148394854954,2.34639580468694),.UNSPECIFIED.);
#30483=B_SPLINE_CURVE_WITH_KNOTS('',3,(#212692,#212693,#212694,#212695),
 .UNSPECIFIED.,.F.,.F.,(4,4),(4.93459806199749E-5,5.07374035525052E-5),
 .UNSPECIFIED.);
#30484=B_SPLINE_CURVE_WITH_KNOTS('',3,(#212774,#212775,#212776,#212777,
#212778,#212779,#212780,#212781,#212782,#212783),.UNSPECIFIED.,.F.,.F.,
(4,2,2,2,4),(2.44487072892702,2.76003095423418,3.15004164386436,3.54005233349455,
3.85521255880171),.UNSPECIFIED.);
#30485=B_SPLINE_CURVE_WITH_KNOTS('',3,(#212795,#212796,#212797,#212798,
#212799,#212800,#212801,#212802,#212803,#212804,#212805,#212806,#212807,
#212808,#212809,#212810,#212811,#212812,#212813,#212814,#212815,#212816,
#212817,#212818,#212819,#212820,#212821,#212822,#212823,#212824,#212825,
#212826,#212827,#212828,#212829,#212830,#212831,#212832,#212833,#212834,
#212835,#212836,#212837,#212838,#212839,#212840,#212841,#212842,#212843,
#212844,#212845,#212846,#212847,#212848,#212849,#212850,#212851,#212852,
#212853,#212854,#212855,#212856,#212857,#212858),.UNSPECIFIED.,.F.,.F.,
(4,2,2,2,2,2,2,2,2,2,2,2,2,2,2,2,2,2,2,2,2,2,2,2,2,2,2,2,2,2,2,4),(-23.4655815117522,
-23.3821633536412,-23.2277363527294,-23.0362474977428,-22.8467003384102,
-22.649719777506,-22.3128056337548,-22.1099831860358,-21.9074402590789,
-21.8087745346896,-21.4994489052755,-21.4005123478419,-21.0840256137525,
-20.9058937064287,-20.7532789815947,-20.562208019526,-20.3727918208678,
-20.1760490515299,-19.7704517016932,-19.3649166721905,-19.0881265530438,
-18.8239123291825,-18.6794135983185,-18.4723542547888,-18.37203416693,-18.1810349703384,
-18.0313863852817,-17.8735599285529,-17.6813646175406,-17.4915681537435,
-17.2941928509983,-17.0142195375219),.UNSPECIFIED.);
#30486=B_SPLINE_CURVE_WITH_KNOTS('',3,(#212865,#212866,#212867,#212868,
#212869,#212870,#212871,#212872,#212873,#212874,#212875,#212876,#212877,
#212878,#212879,#212880,#212881,#212882,#212883,#212884,#212885,#212886),
 .UNSPECIFIED.,.F.,.F.,(4,2,2,2,2,2,2,2,2,2,4),(-25.3579380604563,-25.2126790926101,
-25.0707763793626,-24.7883580752298,-24.6165805135713,-24.4630647928614,
-24.2717305560932,-24.0822302806376,-23.8853298566005,-23.5490789423312,
-23.4655815117522),.UNSPECIFIED.);
#30487=B_SPLINE_CURVE_WITH_KNOTS('',3,(#212888,#212889,#212890,#212891,
#212892,#212893,#212894,#212895,#212896,#212897,#212898,#212899),
 .UNSPECIFIED.,.F.,.F.,(4,2,2,2,2,4),(0.,0.250779295927683,0.498420132327997,
0.665822634254242,0.997622742450503,1.3324035533165),.UNSPECIFIED.);
#30488=B_SPLINE_CURVE_WITH_KNOTS('',3,(#212901,#212902,#212903,#212904,
#212905,#212906,#212907,#212908,#212909,#212910),.UNSPECIFIED.,.F.,.F.,
(4,2,2,2,4),(1.00000001185067E-6,0.17890870313989,0.360010001015589,0.541048047586756,
0.720025159562407),.UNSPECIFIED.);
#30489=B_SPLINE_CURVE_WITH_KNOTS('',3,(#212914,#212915,#212916,#212917,
#212918,#212919,#212920,#212921,#212922,#212923),.UNSPECIFIED.,.F.,.F.,
(4,2,2,2,4),(9.72076722368276E-6,0.179235827648045,0.360521578492218,0.541895207425194,
0.721026938706915),.UNSPECIFIED.);
#30490=B_SPLINE_CURVE_WITH_KNOTS('',3,(#212925,#212926,#212927,#212928,
#212929,#212930,#212931,#212932,#212933,#212934,#212935,#212936),
 .UNSPECIFIED.,.F.,.F.,(4,2,2,2,2,4),(4.89083575544467E-5,0.335287965816992,
0.667578151924596,0.835217190795273,1.08321230565055,1.334348166746),
 .UNSPECIFIED.);
#30491=B_SPLINE_CURVE_WITH_KNOTS('',3,(#212937,#212938,#212939,#212940,
#212941,#212942,#212943,#212944,#212945,#212946,#212947,#212948,#212949,
#212950,#212951,#212952,#212953,#212954,#212955,#212956,#212957,#212958),
 .UNSPECIFIED.,.F.,.F.,(4,2,2,2,2,2,2,2,2,2,4),(-1.89255759737355,-1.80353521663288,
-1.60097725222907,-1.3981474008695,-1.05868693104851,-0.86140418669837,
-0.671667910335707,-0.508679971146122,-0.262571560520725,-0.132568711431051,
-0.000222633785011576),.UNSPECIFIED.);
#30492=B_SPLINE_CURVE_WITH_KNOTS('',3,(#212963,#212964,#212965,#212966,
#212967,#212968,#212969,#212970,#212971,#212972,#212973,#212974,#212975,
#212976,#212977,#212978,#212979,#212980,#212981,#212982,#212983,#212984,
#212985,#212986,#212987,#212988,#212989,#212990,#212991,#212992,#212993,
#212994,#212995,#212996,#212997,#212998,#212999,#213000,#213001,#213002,
#213003,#213004,#213005,#213006,#213007,#213008,#213009,#213010,#213011,
#213012,#213013,#213014,#213015,#213016,#213017,#213018,#213019,#213020,
#213021,#213022,#213023,#213024,#213025,#213026,#213027,#213028,#213029,
#213030,#213031,#213032),.UNSPECIFIED.,.F.,.F.,(4,2,2,2,2,2,2,2,2,2,2,2,
2,2,2,2,2,2,2,2,2,2,2,2,2,2,2,2,2,2,2,2,2,2,4),(-17.0142195375219,-16.9539796203354,
-16.7890489696158,-16.6342677925073,-16.4426964451876,-16.2531188482399,
-16.0560894062044,-15.7188030761123,-15.5159750456067,-15.3134253016677,
-15.1583517074344,-15.0588606872297,-14.6532131620584,-14.2480183614723,
-14.0613034149302,-13.9082183743288,-13.7051158366063,-13.5460702373005,
-13.263110126487,-13.0703537647283,-12.9197353366452,-12.820016273049,-12.6770837035873,
-12.5342903108104,-12.3394687327371,-12.2390554377965,-12.0233345598109,
-11.8716865495169,-11.6868040567647,-11.4843070065672,-11.1768445161315,
-10.9977790660545,-10.7593578972188,-10.5702642746217,-10.5638492065124),
 .UNSPECIFIED.);
#30493=B_SPLINE_CURVE_WITH_KNOTS('',3,(#213033,#213034,#213035,#213036,
#213037,#213038,#213039,#213040,#213041,#213042,#213043,#213044,#213045,
#213046,#213047,#213048,#213049,#213050,#213051,#213052,#213053,#213054,
#213055,#213056,#213057,#213058,#213059,#213060,#213061,#213062,#213063,
#213064,#213065,#213066,#213067,#213068,#213069,#213070,#213071,#213072,
#213073,#213074,#213075,#213076,#213077,#213078,#213079,#213080,#213081,
#213082,#213083,#213084,#213085,#213086,#213087,#213088,#213089,#213090,
#213091,#213092,#213093,#213094,#213095,#213096,#213097,#213098),
 .UNSPECIFIED.,.F.,.F.,(4,2,2,2,2,2,2,2,2,2,2,2,2,2,2,2,2,2,2,2,2,2,2,2,
2,2,2,2,2,2,2,2,4),(-8.34439189346545,-8.24590534832181,-8.14668971659077,
-8.0049280196085,-7.90578734244284,-7.75527402355542,-7.56164635479124,
-7.28035238806601,-7.12534157358082,-6.92238574982098,-6.75614142420925,
-6.4185497256095,-6.22148570635503,-6.03188435919294,-5.84024949079621,
-5.68516707862395,-5.52189531741973,-5.17828352388869,-4.77275280538589,
-4.57628006212064,-4.38699097039336,-4.19638854892432,-4.0456449408773,
-3.85387561061917,-3.56891093370617,-3.36522566092619,-3.20822221584918,
-3.05476221089561,-2.86850590511233,-2.4632747529187,-2.05761577697304,
-1.95813288497916,-1.89255759737355),.UNSPECIFIED.);
#30494=B_SPLINE_CURVE_WITH_KNOTS('',3,(#213103,#213104,#213105,#213106,
#213107,#213108,#213109,#213110,#213111,#213112,#213113,#213114,#213115,
#213116,#213117,#213118,#213119,#213120,#213121,#213122,#213123,#213124,
#213125,#213126,#213127,#213128,#213129,#213130,#213131,#213132,#213133,
#213134,#213135,#213136,#213137,#213138,#213139,#213140,#213141,#213142,
#213143,#213144,#213145,#213146,#213147,#213148,#213149,#213150,#213151,
#213152,#213153,#213154,#213155,#213156,#213157,#213158,#213159,#213160,
#213161,#213162,#213163,#213164,#213165,#213166,#213167,#213168),
 .UNSPECIFIED.,.F.,.F.,(4,2,2,2,2,2,2,2,2,2,2,2,2,2,2,2,2,2,2,2,2,2,2,2,
2,2,2,2,2,2,2,2,4),(-10.5638492065124,-10.3665281400106,-10.2065643589849,
-10.0657701952293,-9.96554246102645,-9.81531484461045,-9.61940377013227,
-9.41681481261266,-9.16094167265437,-8.88884314638493,-8.69155264734285,
-8.50181173061584,-8.30976242994707,-8.15264143083408,-7.99976837552985,
-7.81280965557528,-7.40763311197167,-7.00199007004737,-6.90249478182624,
-6.7471184359148,-6.42909757011231,-6.33010686318968,-6.12761283321231,
-5.81684026459228,-5.63219570194093,-5.48423490732585,-5.28150664967726,
-5.08689708330431,-4.80741352692034,-4.6564265426323,-4.45361226970384,
-4.27215445416353,-4.11333321794941),.UNSPECIFIED.);
#30495=B_SPLINE_CURVE_WITH_KNOTS('',3,(#213169,#213170,#213171,#213172,
#213173,#213174,#213175,#213176,#213177,#213178,#213179,#213180,#213181,
#213182,#213183,#213184,#213185,#213186,#213187,#213188,#213189,#213190,
#213191,#213192,#213193,#213194,#213195,#213196,#213197,#213198,#213199,
#213200,#213201,#213202,#213203,#213204,#213205,#213206,#213207,#213208,
#213209,#213210,#213211,#213212,#213213,#213214,#213215,#213216,#213217,
#213218,#213219,#213220,#213221,#213222,#213223,#213224,#213225,#213226,
#213227,#213228,#213229,#213230,#213231,#213232,#213233,#213234),
 .UNSPECIFIED.,.F.,.F.,(4,2,2,2,2,2,2,2,2,2,2,2,2,2,2,2,2,2,2,2,2,2,2,2,
2,2,2,2,2,2,2,2,4),(-14.7964729471967,-14.7930121131524,-14.6037362465881,
-14.4072806385629,-14.0017540267854,-13.6582611829268,-13.4949397283514,
-13.3398727218517,-13.1209657585198,-13.0205232688638,-12.8243944231431,
-12.6819509109363,-12.5393934714743,-12.4394141585229,-12.2887441952975,
-12.0963925010855,-11.8126276373192,-11.6515132105288,-11.448327176925,
-11.3012939126661,-11.1069033964773,-11.0064990991705,-10.7918073490527,
-10.6411697653991,-10.4485619690297,-10.1653115199523,-10.005523195632,
-9.80239002765117,-9.65153351059004,-9.46206185717822,-9.05703579811716,
-8.65139829862876,-8.34439189346545),.UNSPECIFIED.);
#30496=B_SPLINE_CURVE_WITH_KNOTS('',3,(#213240,#213241,#213242,#213243,
#213244,#213245,#213246,#213247,#213248,#213249,#213250,#213251,#213252,
#213253,#213254,#213255,#213256,#213257,#213258,#213259,#213260,#213261,
#213262,#213263,#213264,#213265,#213266,#213267),.UNSPECIFIED.,.F.,.F.,
(4,2,2,2,2,2,2,2,2,2,2,2,2,4),(-25.3599939626477,-25.2110052268727,-25.0658395881092,
-24.7731830676316,-24.6302233121548,-24.4709374768147,-24.2672182293805,
-24.0781558955,-23.8400128244761,-23.6610071037644,-23.353579459936,-23.1510946673596,
-23.0520783263848,-23.0237218553495),.UNSPECIFIED.);
#30497=B_SPLINE_CURVE_WITH_KNOTS('',3,(#213268,#213269,#213270,#213271,
#213272,#213273,#213274,#213275,#213276,#213277,#213278,#213279,#213280,
#213281,#213282,#213283,#213284,#213285,#213286,#213287,#213288,#213289,
#213290,#213291,#213292,#213293,#213294,#213295,#213296,#213297,#213298,
#213299,#213300,#213301,#213302,#213303,#213304,#213305,#213306,#213307,
#213308,#213309,#213310,#213311),.UNSPECIFIED.,.F.,.F.,(4,2,2,2,2,2,2,2,
2,2,2,2,2,2,2,2,2,2,2,2,2,4),(-4.11333321794941,-3.96076191479785,-3.86202062745145,
-3.54599574300317,-3.44707915710504,-3.13716544626074,-3.03848011624721,
-2.72045780085061,-2.62146595892779,-2.41896937024694,-2.10817748977627,
-1.92349758118348,-1.77537722483771,-1.5726426679254,-1.37872992888174,
-1.09796693044656,-0.944179154417269,-0.741277533053446,-0.570394112429525,
-0.287612371759698,-0.145595795194013,-5.55694362388068E-6),
 .UNSPECIFIED.);
#30498=B_SPLINE_CURVE_WITH_KNOTS('',3,(#213312,#213313,#213314,#213315,
#213316,#213317,#213318,#213319,#213320,#213321,#213322,#213323,#213324,
#213325,#213326,#213327,#213328,#213329,#213330,#213331,#213332,#213333,
#213334,#213335,#213336,#213337,#213338,#213339,#213340,#213341,#213342,
#213343,#213344,#213345,#213346,#213347,#213348,#213349,#213350,#213351,
#213352,#213353,#213354,#213355,#213356,#213357,#213358,#213359,#213360,
#213361,#213362,#213363,#213364,#213365,#213366,#213367,#213368,#213369,
#213370,#213371,#213372,#213373,#213374,#213375,#213376,#213377),
 .UNSPECIFIED.,.F.,.F.,(4,2,2,2,2,2,2,2,2,2,2,2,2,2,2,2,2,2,2,2,2,2,2,2,
2,2,2,2,2,2,2,2,4),(-21.2462595254853,-21.0130526317412,-20.6600149992664,
-20.5011090444902,-20.2980763381775,-20.0685171116799,-19.8659046223187,
-19.6629317394128,-19.4602424779167,-19.2488692412891,-19.1003391764158,
-18.9119956891045,-18.7227658705206,-18.5264138806326,-18.1946275381072,
-18.0253752742207,-17.8713489015093,-17.586778234647,-17.384325934204,-17.2851176679844,
-17.0156489622446,-16.7691855010582,-16.6235747431412,-16.414894933244,
-16.3145588184473,-16.1228121116564,-15.9737542503545,-15.7706040124235,
-15.610203095414,-15.3267169747295,-15.1342348821604,-14.9835871024164,
-14.7964729471967),.UNSPECIFIED.);
#30499=B_SPLINE_CURVE_WITH_KNOTS('',3,(#213382,#213383,#213384,#213385,
#213386,#213387,#213388,#213389,#213390,#213391,#213392,#213393,#213394,
#213395,#213396,#213397,#213398,#213399,#213400,#213401,#213402,#213403,
#213404,#213405,#213406,#213407,#213408,#213409,#213410,#213411,#213412,
#213413,#213414,#213415,#213416,#213417,#213418,#213419,#213420,#213421,
#213422,#213423,#213424,#213425,#213426,#213427,#213428,#213429,#213430,
#213431,#213432,#213433,#213434,#213435,#213436,#213437,#213438,#213439,
#213440,#213441,#213442,#213443),.UNSPECIFIED.,.F.,.F.,(4,2,2,2,2,2,2,2,
2,2,2,2,2,2,2,2,2,2,2,2,2,2,2,2,2,2,2,2,2,2,4),(-23.0237218553495,-22.7829578146256,
-22.53985611019,-22.3372736023383,-22.1979623272724,-22.0150657011536,-21.7052985547119,
-21.5028125493589,-21.4038147651851,-21.085595223343,-20.9085658857745,
-20.7057289281245,-20.5536435482767,-20.3682264157039,-20.1726079358586,
-19.8466166265223,-19.6741889045732,-19.5206951783369,-19.3294245802063,
-19.1399535116033,-18.9431008723126,-18.5375013263223,-18.2636250828212,
-18.004062687006,-17.801480911653,-17.6064861128457,-17.4561549159828,-17.2417879958575,
-17.0663359785854,-16.7612726574011,-16.5735077595754),.UNSPECIFIED.);
#30500=B_SPLINE_CURVE_WITH_KNOTS('',3,(#213445,#213446,#213447,#213448,
#213449,#213450,#213451,#213452,#213453,#213454,#213455,#213456,#213457,
#213458,#213459,#213460,#213461,#213462,#213463,#213464,#213465,#213466,
#213467,#213468,#213469,#213470,#213471,#213472,#213473,#213474,#213475,
#213476,#213477,#213478,#213479,#213480,#213481,#213482,#213483,#213484,
#213485,#213486),.UNSPECIFIED.,.F.,.F.,(4,2,2,2,2,2,2,2,2,2,2,2,2,2,2,2,
2,2,2,2,4),(-25.3598482220487,-25.2134211082989,-25.0706251162533,-24.7853399490412,
-24.6208618383294,-24.4178851639507,-24.2622830408013,-23.9807185207273,
-23.7872130499894,-23.5844639595727,-23.3696718488658,-23.1670170319282,
-22.9595539400521,-22.7568765161118,-22.5470207421421,-22.3983316917044,
-22.2097930130438,-22.0205546305087,-21.8241908375456,-21.418680597865,
-21.2462595254853),.UNSPECIFIED.);
#30501=B_SPLINE_CURVE_WITH_KNOTS('',3,(#213487,#213488,#213489,#213490,
#213491,#213492,#213493,#213494,#213495,#213496,#213497,#213498,#213499,
#213500,#213501,#213502,#213503,#213504,#213505,#213506,#213507,#213508,
#213509,#213510,#213511,#213512,#213513,#213514),.UNSPECIFIED.,.F.,.F.,
(4,2,2,2,2,2,2,2,2,2,2,2,2,4),(-2.33721822141003,-2.31110570753062,-2.21223251201049,
-1.90071971511215,-1.80197161402924,-1.48609808399419,-1.38718479643066,
-1.076992667329,-0.978293896948929,-0.660945421098482,-0.499220557990324,
-0.258250015726861,-0.130322448606808,-5.55694360169744E-6),
 .UNSPECIFIED.);
#30502=B_SPLINE_CURVE_WITH_KNOTS('',3,(#213519,#213520,#213521,#213522,
#213523,#213524,#213525,#213526,#213527,#213528,#213529,#213530,#213531,
#213532,#213533,#213534,#213535,#213536,#213537,#213538,#213539,#213540,
#213541,#213542,#213543,#213544,#213545,#213546,#213547,#213548,#213549,
#213550,#213551,#213552,#213553,#213554,#213555,#213556,#213557,#213558,
#213559,#213560,#213561,#213562,#213563,#213564,#213565,#213566,#213567,
#213568,#213569,#213570,#213571,#213572,#213573,#213574,#213575,#213576,
#213577,#213578,#213579,#213580,#213581,#213582,#213583,#213584),
 .UNSPECIFIED.,.F.,.F.,(4,2,2,2,2,2,2,2,2,2,2,2,2,2,2,2,2,2,2,2,2,2,2,2,
2,2,2,2,2,2,2,2,4),(-16.5735077595754,-16.558788014462,-16.4597521147959,
-16.1906086541584,-16.0245717260025,-15.8367395841997,-15.6409285758089,
-15.313443646354,-15.1418470460958,-14.9882133987819,-14.7969063470367,
-14.6074203021057,-14.410544531441,-14.0049311364927,-13.7310093334175,
-13.4713700195003,-13.2687826464027,-13.0737994753134,-12.923462076633,
-12.8253058156821,-12.68010861894,-12.5351957885283,-12.3477195958187,-11.9425815080008,
-11.5369479410831,-11.437442651998,-11.2814916431801,-10.9654562255593,
-10.8665420645695,-10.5566653339251,-10.4579842233931,-10.1399353299562,
-10.1215558732796),.UNSPECIFIED.);
#30503=B_SPLINE_CURVE_WITH_KNOTS('',3,(#213585,#213586,#213587,#213588,
#213589,#213590,#213591,#213592,#213593,#213594,#213595,#213596,#213597,
#213598,#213599,#213600,#213601,#213602,#213603,#213604,#213605,#213606,
#213607,#213608,#213609,#213610,#213611,#213612,#213613,#213614,#213615,
#213616,#213617,#213618,#213619,#213620,#213621,#213622,#213623,#213624,
#213625,#213626,#213627,#213628,#213629,#213630,#213631,#213632,#213633,
#213634,#213635,#213636,#213637,#213638,#213639,#213640,#213641,#213642,
#213643,#213644,#213645,#213646,#213647,#213648,#213649,#213650),
 .UNSPECIFIED.,.F.,.F.,(4,2,2,2,2,2,2,2,2,2,2,2,2,2,2,2,2,2,2,2,2,2,2,2,
2,2,2,2,2,2,2,2,4),(-8.78646590511648,-8.69447764122115,-8.50512180829162,
-8.31427326472456,-8.16256695330588,-7.97809447067373,-7.77559387977924,
-7.46594770522954,-7.28328997819737,-7.14515274060527,-6.94255908319348,
-6.69117979097634,-6.42066375919234,-6.2243223411716,-6.03509287700676,
-5.84714336525967,-5.69892935521848,-5.48430236760396,-5.28156262317273,
-5.08768687858614,-4.80685766016851,-4.65291432428607,-4.44999718079432,
-4.27993773196351,-3.9496315087519,-3.75346099655457,-3.56430030673111,
-3.38227916274677,-3.23818448040399,-2.96662657818636,-2.82057795462476,
-2.58018133296781,-2.33721822141003),.UNSPECIFIED.);
#30504=B_SPLINE_CURVE_WITH_KNOTS('',3,(#213655,#213656,#213657,#213658,
#213659,#213660,#213661,#213662,#213663,#213664,#213665,#213666,#213667,
#213668,#213669,#213670,#213671,#213672,#213673,#213674,#213675,#213676,
#213677,#213678,#213679,#213680,#213681,#213682,#213683,#213684,#213685,
#213686,#213687,#213688,#213689,#213690,#213691,#213692,#213693,#213694,
#213695,#213696,#213697,#213698,#213699,#213700,#213701,#213702,#213703,
#213704,#213705,#213706,#213707,#213708,#213709,#213710,#213711,#213712,
#213713,#213714,#213715,#213716,#213717,#213718),.UNSPECIFIED.,.F.,.F.,
(4,2,2,2,2,2,2,2,2,2,2,2,2,2,2,2,2,2,2,2,2,2,2,2,2,2,2,2,2,2,2,4),(-10.1215558732796,
-10.0409453002839,-9.83845542996561,-9.52785452984907,-9.34350900069316,
-9.19707221940522,-8.99438494390757,-8.7925223606963,-8.58992278550474,
-8.35652235900569,-8.15340240102332,-8.0019933378063,-7.81322384890866,
-7.40816004464301,-7.00252650556468,-6.90298973191125,-6.74558906250778,
-6.43423701736284,-6.33549805144709,-6.01942533379578,-5.92050772757459,
-5.61066228809942,-5.51198031710246,-5.1938716118372,-5.09487729173345,
-4.89238287118889,-4.58202669110098,-4.39812304091263,-4.2539365260713,
-4.05128954032214,-3.83776873148533,-3.67017174968231),.UNSPECIFIED.);
#30505=B_SPLINE_CURVE_WITH_KNOTS('',3,(#213719,#213720,#213721,#213722,
#213723,#213724,#213725,#213726,#213727,#213728,#213729,#213730,#213731,
#213732,#213733,#213734,#213735,#213736,#213737,#213738,#213739,#213740,
#213741,#213742,#213743,#213744,#213745,#213746,#213747,#213748,#213749,
#213750,#213751,#213752,#213753,#213754,#213755,#213756,#213757,#213758,
#213759,#213760,#213761,#213762,#213763,#213764,#213765,#213766,#213767,
#213768,#213769,#213770,#213771,#213772,#213773,#213774,#213775,#213776,
#213777,#213778,#213779,#213780,#213781,#213782,#213783,#213784,#213785,
#213786),.UNSPECIFIED.,.F.,.F.,(4,2,2,2,2,2,2,2,2,2,2,2,2,2,2,2,2,2,2,2,
2,2,2,2,2,2,2,2,2,2,2,2,2,4),(-15.2367903044136,-14.8893236437563,-14.7291495722032,
-14.5261341402795,-14.3693368356338,-14.1830571286185,-13.9873569675475,
-13.6608086821188,-13.4886697502539,-13.3351159169796,-13.1175658866552,
-13.0171341357064,-12.8215524175462,-12.6789588457294,-12.536241436693,
-12.4363691812245,-12.2857172284162,-12.0931903303355,-11.8097624008203,
-11.6495335418658,-11.4463782081366,-11.2967969002635,-11.1057014414873,
-11.0053745853545,-10.7981093394651,-10.6534740075858,-10.391513092408,
-10.116228035644,-9.71058551650308,-9.51313229873795,-9.32327827108487,
-9.22500334979002,-8.89109260896205,-8.78646590511648),.UNSPECIFIED.);
#30506=B_SPLINE_CURVE_WITH_KNOTS('',3,(#213792,#213793,#213794,#213795,
#213796,#213797,#213798,#213799,#213800,#213801,#213802,#213803,#213804,
#213805,#213806,#213807,#213808,#213809,#213810,#213811,#213812,#213813,
#213814,#213815),.UNSPECIFIED.,.F.,.F.,(4,2,2,2,2,2,2,2,2,2,2,4),(5.07374035434672E-5,
0.19606314902765,0.390967942257509,0.792252129422002,1.19229882428601,1.39196195962845,
1.5908744447054,1.78833640693294,1.98791847080156,2.18776996778386,2.48510060443345,
2.78256740042348),.UNSPECIFIED.);
#30507=B_SPLINE_CURVE_WITH_KNOTS('',3,(#213816,#213817,#213818,#213819,
#213820,#213821,#213822,#213823,#213824,#213825,#213826,#213827,#213828,
#213829,#213830,#213831,#213832,#213833,#213834,#213835,#213836,#213837,
#213838,#213839,#213840,#213841,#213842,#213843,#213844,#213845,#213846,
#213847,#213848,#213849,#213850,#213851),.UNSPECIFIED.,.F.,.F.,(4,2,2,2,
2,2,2,2,2,2,2,2,2,2,2,2,2,4),(-3.67017174968231,-3.635048745841,-3.43815758420685,
-3.23556456026557,-2.98357247568108,-2.7128797384741,-2.51641098932753,
-2.32712518426374,-2.13652722295863,-1.98578976714053,-1.79398833616895,
-1.50909393296523,-1.30541347022808,-1.14838131573872,-0.99497187110547,
-0.808745254833481,-0.403515045478468,-1.91474428097279E-5),
 .UNSPECIFIED.);
#30508=B_SPLINE_CURVE_WITH_KNOTS('',3,(#213852,#213853,#213854,#213855,
#213856,#213857,#213858,#213859,#213860,#213861,#213862,#213863,#213864,
#213865,#213866,#213867,#213868,#213869,#213870,#213871,#213872,#213873,
#213874,#213875,#213876,#213877,#213878,#213879,#213880,#213881,#213882,
#213883,#213884,#213885,#213886,#213887,#213888,#213889,#213890,#213891,
#213892,#213893,#213894,#213895,#213896,#213897,#213898,#213899,#213900,
#213901,#213902,#213903,#213904,#213905,#213906,#213907,#213908,#213909,
#213910,#213911,#213912,#213913),.UNSPECIFIED.,.F.,.F.,(4,2,2,2,2,2,2,2,
2,2,2,2,2,2,2,2,2,2,2,2,2,2,2,2,2,2,2,2,2,2,4),(-21.6906362475869,-21.5013896141299,
-21.4024213539677,-21.0851404732035,-20.9864295651607,-20.6759526794773,
-20.5770475261363,-20.2614416858976,-20.1053469575417,-20.0058352989294,
-19.600192486939,-19.2232859369709,-19.020710368846,-18.8179491194557,-18.6154479835255,
-18.5164835795067,-18.1992767642662,-18.1005651025437,-17.7900401315637,
-17.6323657521275,-17.5328237855654,-17.127198587604,-16.722159016726,-16.5331182952159,
-16.3819210436559,-16.2244362917703,-16.0323087166128,-15.8425383011383,
-15.6452009065229,-15.2395449589195,-15.2367903044136),.UNSPECIFIED.);
#30509=B_SPLINE_CURVE_WITH_KNOTS('',3,(#213919,#213920,#213921,#213922,
#213923,#213924,#213925,#213926),.UNSPECIFIED.,.F.,.F.,(4,2,2,4),(9.21790452008223,
9.4318832005907,9.73296466445621,10.0352832223881),.UNSPECIFIED.);
#30510=B_SPLINE_CURVE_WITH_KNOTS('',3,(#213932,#213933,#213934,#213935,
#213936,#213937,#213938,#213939,#213940,#213941,#213942,#213943,#213944,
#213945,#213946,#213947,#213948,#213949,#213950,#213951,#213952,#213953,
#213954,#213955,#213956,#213957,#213958,#213959,#213960,#213961,#213962,
#213963,#213964,#213965,#213966,#213967,#213968,#213969,#213970,#213971,
#213972,#213973,#213974,#213975,#213976,#213977,#213978,#213979,#213980,
#213981,#213982,#213983,#213984,#213985,#213986,#213987,#213988,#213989,
#213990,#213991,#213992,#213993,#213994,#213995),.UNSPECIFIED.,.F.,.F.,
(4,2,2,2,2,2,2,2,2,2,2,2,2,2,2,2,2,2,2,2,2,2,2,2,2,2,2,2,2,2,2,4),(1.03510113506669,
1.42190076144609,1.65975570624457,1.90918310386495,2.03534477977157,2.54453754089686,
2.78186254655865,3.03265366633092,3.15880260895928,3.66811591821521,3.90937651886798,
4.15314502278736,4.27935426029102,4.78786109188973,5.01857442699673,5.24596204487806,
5.53988512633587,5.76236179365467,6.26691663031345,6.39333733948748,6.62191123077583,
6.74582667444504,6.99053079450849,7.33725916006411,7.58275600967597,7.8287822692156,
8.05831356870385,8.32996067829968,8.55807863230822,9.06599466340575,9.19223469840276,
9.21790452008223),.UNSPECIFIED.);
#30511=B_SPLINE_CURVE_WITH_KNOTS('',3,(#213999,#214000,#214001,#214002),
 .UNSPECIFIED.,.F.,.F.,(4,4),(0.,0.00054580800139321),.UNSPECIFIED.);
#30512=B_SPLINE_CURVE_WITH_KNOTS('',3,(#214004,#214005,#214006,#214007,
#214008,#214009,#214010,#214011,#214012,#214013,#214014,#214015,#214016,
#214017,#214018,#214019,#214020,#214021,#214022,#214023,#214024,#214025,
#214026,#214027,#214028,#214029,#214030,#214031,#214032,#214033),
 .UNSPECIFIED.,.F.,.F.,(4,2,2,2,2,2,2,2,2,2,2,2,2,2,4),(0.,0.16166597888304,
0.323391460359401,0.526063184698531,0.925852633976886,1.05183001043014,
1.56958669063404,1.76531286769044,1.96277562636095,2.47502393525251,2.70447577935253,
3.02961056722522,3.22205209758851,3.37599328488597,3.53032372881347),
 .UNSPECIFIED.);
#30513=B_SPLINE_CURVE_WITH_KNOTS('',3,(#214034,#214035,#214036,#214037,
#214038,#214039,#214040,#214041,#214042,#214043,#214044,#214045,#214046,
#214047,#214048,#214049,#214050,#214051,#214052,#214053,#214054,#214055,
#214056,#214057,#214058,#214059,#214060,#214061),.UNSPECIFIED.,.F.,.F.,
(4,2,2,2,2,2,2,2,2,2,2,2,2,4),(-4.0928672423958,-3.80981796722786,-3.64049485155161,
-3.12585719634299,-2.93571507444881,-2.5721796822949,-2.39990451027257,
-1.88602332766581,-1.68187581621743,-1.33960776333701,-1.16853206863454,
-0.653965815035966,-0.343366468922743,-1.00000000013978E-6),
 .UNSPECIFIED.);
#30514=B_SPLINE_CURVE_WITH_KNOTS('',3,(#214067,#214068,#214069,#214070,
#214071,#214072,#214073,#214074,#214075,#214076,#214077,#214078,#214079,
#214080,#214081,#214082,#214083,#214084,#214085,#214086,#214087,#214088,
#214089,#214090,#214091,#214092,#214093,#214094,#214095,#214096,#214097,
#214098,#214099,#214100,#214101,#214102,#214103,#214104,#214105,#214106,
#214107,#214108,#214109,#214110,#214111,#214112,#214113,#214114,#214115,
#214116,#214117,#214118,#214119,#214120,#214121,#214122,#214123,#214124,
#214125,#214126,#214127,#214128,#214129,#214130,#214131,#214132),
 .UNSPECIFIED.,.F.,.F.,(4,2,2,2,2,2,2,2,2,2,2,2,2,2,2,2,2,2,2,2,2,2,2,2,
2,2,2,2,2,2,2,2,4),(19.9501840521356,20.2039213034323,20.3287580909671,
20.5798677055414,20.8396508055159,21.0978253952488,21.2234763844211,21.4813984877127,
21.7524924853527,21.8774181480447,22.0805108449731,22.3325329071134,22.5904208234137,
22.8486507412779,22.9737051239086,23.2244367307076,23.4701290954001,23.7283594100504,
23.8533638265947,24.1041849116098,24.3531282121589,24.6113545063552,24.736519792903,
24.9870430282304,25.2253775519541,25.4575680251568,25.6291332729475,25.8870963905533,
26.1714349415304,26.2852130171025,26.6471257924219,26.7579086160256,27.092373191068),
 .UNSPECIFIED.);
#30515=B_SPLINE_CURVE_WITH_KNOTS('',3,(#214133,#214134,#214135,#214136,
#214137,#214138,#214139,#214140,#214141,#214142,#214143,#214144),
 .UNSPECIFIED.,.F.,.F.,(4,2,2,2,2,4),(4.25269675018496E-5,0.255194498557652,
0.508955632318599,0.799301344137275,0.912562061722119,1.03510113506669),
 .UNSPECIFIED.);
#30516=B_SPLINE_CURVE_WITH_KNOTS('',3,(#214145,#214146,#214147,#214148,
#214149,#214150,#214151,#214152,#214153,#214154,#214155,#214156,#214157,
#214158,#214159,#214160,#214161,#214162,#214163,#214164,#214165,#214166,
#214167,#214168,#214169,#214170,#214171,#214172,#214173,#214174,#214175,
#214176,#214177,#214178,#214179,#214180,#214181,#214182,#214183,#214184,
#214185,#214186,#214187,#214188,#214189,#214190,#214191,#214192,#214193,
#214194,#214195,#214196,#214197,#214198,#214199,#214200,#214201,#214202),
 .UNSPECIFIED.,.F.,.F.,(4,2,2,2,2,2,2,2,2,2,2,2,2,2,2,2,2,2,2,2,2,2,2,2,
2,2,2,2,4),(-12.2749063736218,-12.1187900791705,-11.879808815597,-11.5535690996991,
-11.3094012187778,-10.8019634959954,-10.6138794600607,-10.2280063491379,
-10.0105010044501,-9.68641783911147,-9.41284064170808,-8.97177822363525,
-8.76888849795534,-8.36889877677119,-8.24292592755194,-7.88568962577202,
-7.63571172501066,-7.27227457662365,-7.02175834140347,-6.65613264295677,
-6.26737152351143,-6.0766033000751,-5.57048100510707,-5.32573258363369,
-4.99778399626186,-4.71802225787336,-4.39296620626389,-4.16592791266086,
-4.0928672423958),.UNSPECIFIED.);
#30517=B_SPLINE_CURVE_WITH_KNOTS('',3,(#214207,#214208,#214209,#214210,
#214211,#214212,#214213,#214214,#214215,#214216,#214217,#214218,#214219,
#214220,#214221,#214222,#214223,#214224,#214225,#214226,#214227,#214228,
#214229,#214230,#214231,#214232,#214233,#214234,#214235,#214236,#214237,
#214238,#214239,#214240,#214241,#214242,#214243,#214244,#214245,#214246,
#214247,#214248,#214249,#214250,#214251,#214252,#214253,#214254,#214255,
#214256,#214257,#214258,#214259,#214260,#214261,#214262,#214263,#214264,
#214265,#214266,#214267,#214268,#214269,#214270,#214271,#214272,#214273,
#214274,#214275,#214276,#214277,#214278,#214279,#214280,#214281,#214282,
#214283,#214284),.UNSPECIFIED.,.F.,.F.,(4,2,2,2,2,2,2,2,2,2,2,2,2,2,2,2,
2,2,2,2,2,2,2,2,2,2,2,2,2,2,2,2,2,2,2,2,2,2,4),(11.7734600023717,11.9982362050268,
12.2288307658104,12.4791354655245,12.6044197106843,12.8626497232774,13.0985045059271,
13.3300569078068,13.5460652655509,13.7620013704151,13.9935561404502,14.2293816155567,
14.4876118366438,14.6128950196291,14.8632050686861,15.093950803072,15.3250057131515,
15.6256039597299,15.7510855597561,15.9762377203391,16.2075321392228,16.3655548549729,
16.6167748241098,16.8807332018033,17.1388659369982,17.2646851086345,17.5226540391788,
17.8073718259425,17.932474738288,18.1903879181091,18.4486148820817,18.5738163564277,
18.8242739157131,19.0602709056961,19.2920160693179,19.4572439568824,19.7150957671442,
19.9456909285047,19.9501840521356),.UNSPECIFIED.);
#30518=B_SPLINE_CURVE_WITH_KNOTS('',3,(#214286,#214287,#214288,#214289,
#214290,#214291,#214292,#214293,#214294,#214295,#214296,#214297),
 .UNSPECIFIED.,.F.,.F.,(4,2,2,2,2,4),(-13.3097623354321,-13.0506230872222,
-12.7981078626377,-12.6277703233625,-12.4570073448961,-12.2749063736218),
 .UNSPECIFIED.);
#30519=B_SPLINE_CURVE_WITH_KNOTS('',3,(#214298,#214299,#214300,#214301,
#214302,#214303,#214304,#214305,#214306,#214307,#214308,#214309,#214310,
#214311,#214312,#214313,#214314,#214315,#214316,#214317,#214318,#214319,
#214320,#214321,#214322,#214323,#214324,#214325,#214326,#214327,#214328,
#214329,#214330,#214331,#214332,#214333,#214334,#214335,#214336,#214337,
#214338,#214339,#214340,#214341,#214342,#214343,#214344,#214345,#214346,
#214347,#214348,#214349,#214350,#214351,#214352,#214353,#214354,#214355,
#214356,#214357,#214358,#214359,#214360,#214361,#214362,#214363,#214364,
#214365,#214366,#214367),.UNSPECIFIED.,.F.,.F.,(4,2,2,2,2,2,2,2,2,2,2,2,
2,2,2,2,2,2,2,2,2,2,2,2,2,2,2,2,2,2,2,2,2,2,4),(-7.14121730581807,-7.10127190196412,
-6.97635927806433,-6.76787273732327,-6.51625363264104,-6.26142709012785,
-6.00321238811012,-5.87812473396963,-5.62748345688499,-5.38451315576289,
-5.12629705305085,-5.00144012143128,-4.75039183957789,-4.49242993202835,
-4.23425457712158,-4.10868711407363,-3.85079913174379,-3.58528178243477,
-3.34048377236277,-3.08998645698157,-2.96416702950007,-2.67402819920963,
-2.548826428631,-2.29286226189582,-2.03468181880128,-1.90920364004217,-1.65134503451085,
-1.41375102191269,-1.15556492024653,-1.03016186674223,-0.772326080524892,
-0.538863998804044,-0.273114657421419,-0.137051040303161,-6.79217266545488E-5),
 .UNSPECIFIED.);
#30520=B_SPLINE_CURVE_WITH_KNOTS('',3,(#214372,#214373,#214374,#214375,
#214376,#214377,#214378,#214379,#214380,#214381,#214382,#214383,#214384,
#214385,#214386,#214387,#214388,#214389,#214390,#214391,#214392,#214393,
#214394,#214395,#214396,#214397,#214398,#214399,#214400,#214401,#214402,
#214403,#214404,#214405,#214406,#214407,#214408,#214409,#214410,#214411,
#214412,#214413,#214414,#214415,#214416,#214417,#214418,#214419,#214420,
#214421,#214422,#214423,#214424,#214425,#214426,#214427,#214428,#214429,
#214430,#214431,#214432,#214433,#214434,#214435,#214436,#214437,#214438,
#214439,#214440,#214441,#214442,#214443,#214444,#214445,#214446,#214447,
#214448,#214449),.UNSPECIFIED.,.F.,.F.,(4,2,2,2,2,2,2,2,2,2,2,2,2,2,2,2,
2,2,2,2,2,2,2,2,2,2,2,2,2,2,2,2,2,2,2,2,2,2,4),(3.59637852778132,3.77812667911342,
4.02304674635722,4.29062104873451,4.54852148405871,4.67411990136732,4.93229550742404,
5.17248737133136,5.43037080611408,5.55589702810278,5.81408617301148,6.07101155670248,
6.32203927006553,6.44691570930367,6.70513880893479,6.95581693593773,7.08095057279958,
7.36746835221977,7.62543238824665,7.79735490426262,7.92350791987667,8.29187981987286,
8.41683743990179,8.69138966599333,8.94932139764217,9.07501539189821,9.33317961110474,
9.59405572704114,9.71924899120621,10.0085573244635,10.2394175420354,10.4671044593678,
10.5924380553917,10.8877072565187,11.1186536449452,11.341727853923,11.4671925064493,
11.7671943111698,11.7734600023717),.UNSPECIFIED.);
#30521=B_SPLINE_CURVE_WITH_KNOTS('',3,(#214450,#214451,#214452,#214453,
#214454,#214455,#214456,#214457,#214458,#214459,#214460,#214461,#214462,
#214463,#214464,#214465,#214466,#214467,#214468,#214469,#214470,#214471,
#214472,#214473,#214474,#214475,#214476,#214477,#214478,#214479,#214480,
#214481,#214482,#214483,#214484,#214485,#214486,#214487,#214488,#214489,
#214490,#214491,#214492,#214493,#214494,#214495,#214496,#214497,#214498,
#214499,#214500,#214501,#214502,#214503,#214504,#214505,#214506,#214507,
#214508,#214509,#214510,#214511,#214512,#214513,#214514,#214515,#214516,
#214517,#214518,#214519,#214520,#214521,#214522,#214523,#214524,#214525),
 .UNSPECIFIED.,.F.,.F.,(4,2,2,2,2,2,2,2,2,2,2,2,2,2,2,2,2,2,2,2,2,2,2,2,
2,2,2,2,2,2,2,2,2,2,2,2,2,4),(-15.3176231869007,-15.1056438788204,-14.8722725390337,
-14.614416732992,-14.489000008823,-14.2307975543113,-13.9931480555956,-13.7617417105088,
-13.5448308438595,-13.3285120238497,-13.097092852516,-12.8596333519296,
-12.6014293942186,-12.47602821334,-12.218176957919,-11.9856359912747,-11.7274146784205,
-11.602410922309,-11.3516073204166,-11.1029728045464,-10.8447546918672,
-10.7196093690404,-10.4690670570721,-10.2297511991479,-9.99732467670149,
-9.82281327047037,-9.56481527159159,-9.26273929783766,-9.1372175261113,
-8.90657656378107,-8.6483608703652,-8.52352688836427,-8.27244061302118,
-8.01300493924838,-7.75484111316192,-7.62921200516085,-7.37130846105036,
-7.14121730581807),.UNSPECIFIED.);
#30522=B_SPLINE_CURVE_WITH_KNOTS('',3,(#214531,#214532,#214533,#214534,
#214535,#214536,#214537,#214538,#214539,#214540,#214541,#214542,#214543,
#214544,#214545,#214546,#214547,#214548,#214549,#214550,#214551,#214552,
#214553,#214554,#214555,#214556,#214557,#214558,#214559,#214560,#214561,
#214562,#214563,#214564,#214565,#214566,#214567,#214568,#214569,#214570,
#214571,#214572,#214573,#214574,#214575,#214576),.UNSPECIFIED.,.F.,.F.,
(4,2,2,2,2,2,2,2,2,2,2,2,2,2,2,2,2,2,2,2,2,2,4),(-27.0906254788674,-26.9501859108409,
-26.8108374409825,-26.5377652063263,-26.314814384877,-26.2047766401236,
-25.8436700170918,-25.7187168828716,-25.4433658352626,-25.1854571453625,
-25.0155712252688,-24.8894553916724,-24.5219127449176,-24.3969666928096,
-24.1223476036517,-23.891498454964,-23.671986020183,-23.4378392902655,-23.2579366145597,
-23.1316996181331,-22.7603654578437,-22.6354219479875,-22.5104081169932),
 .UNSPECIFIED.);
#30523=B_SPLINE_CURVE_WITH_KNOTS('',3,(#214577,#214578,#214579,#214580,
#214581,#214582,#214583,#214584,#214585,#214586,#214587,#214588,#214589,
#214590,#214591,#214592,#214593,#214594,#214595,#214596,#214597,#214598,
#214599,#214600,#214601,#214602,#214603,#214604,#214605,#214606,#214607,
#214608,#214609,#214610,#214611,#214612),.UNSPECIFIED.,.F.,.F.,(4,2,2,2,
2,2,2,2,2,2,2,2,2,2,2,2,2,4),(6.63670101017275E-6,0.255164148591463,0.5026236995069,
0.769207716988034,1.02708819460434,1.19522482133063,1.42721465689468,1.68501797683759,
1.80999390851426,2.08699717987714,2.21271380182159,2.46280904639482,2.70750797272155,
2.97099701514689,3.09660781343983,3.40130864969258,3.52723844382287,3.59637852778132),
 .UNSPECIFIED.);
#30524=B_SPLINE_CURVE_WITH_KNOTS('',3,(#214613,#214614,#214615,#214616,
#214617,#214618,#214619,#214620,#214621,#214622,#214623,#214624,#214625,
#214626,#214627,#214628,#214629,#214630,#214631,#214632,#214633,#214634,
#214635,#214636,#214637,#214638,#214639,#214640,#214641,#214642,#214643,
#214644,#214645,#214646,#214647,#214648,#214649,#214650,#214651,#214652,
#214653,#214654,#214655,#214656,#214657,#214658,#214659,#214660,#214661,
#214662,#214663,#214664,#214665,#214666,#214667,#214668,#214669,#214670,
#214671,#214672,#214673,#214674,#214675,#214676,#214677,#214678,#214679,
#214680,#214681,#214682,#214683,#214684,#214685,#214686,#214687,#214688,
#214689,#214690,#214691,#214692),.UNSPECIFIED.,.F.,.F.,(4,2,2,2,2,2,2,2,
2,2,2,2,2,2,2,2,2,2,2,2,2,2,2,2,2,2,2,2,2,2,2,2,2,2,2,2,2,2,2,4),(-23.4938196648925,
-23.4149340907595,-23.2518796395597,-23.0202919717034,-22.7851614155846,
-22.5347413007983,-22.4095333736385,-22.1513199685413,-21.9013907117378,
-21.6505529411977,-21.5255691067719,-21.2673495098011,-21.0094825445456,
-20.7573720460851,-20.5557484524118,-20.4308259828129,-20.1594536607042,
-19.901541807629,-19.7758924762591,-19.5177299337117,-19.2578655533035,
-19.0067644829067,-18.8819345614844,-18.6237154355237,-18.3813050082189,
-18.1306759018197,-18.0055771756941,-17.7473595214231,-17.5137027493023,
-17.2558477942795,-17.1304271894833,-16.8722273623606,-16.6177156880087,
-16.3667526914773,-16.2418387291235,-15.9836170256549,-15.7396157516227,
-15.4889398935453,-15.3638642493586,-15.3176231869007),.UNSPECIFIED.);
#30525=B_SPLINE_CURVE_WITH_KNOTS('',3,(#214697,#214698,#214699,#214700,
#214701,#214702,#214703,#214704,#214705,#214706,#214707,#214708,#214709,
#214710,#214711,#214712,#214713,#214714,#214715,#214716,#214717,#214718,
#214719,#214720,#214721,#214722,#214723,#214724,#214725,#214726,#214727,
#214728,#214729,#214730,#214731,#214732,#214733,#214734,#214735,#214736,
#214737,#214738,#214739,#214740,#214741,#214742,#214743,#214744,#214745,
#214746,#214747,#214748,#214749,#214750,#214751,#214752,#214753,#214754,
#214755,#214756,#214757,#214758,#214759,#214760,#214761,#214762,#214763,
#214764,#214765,#214766,#214767,#214768,#214769,#214770,#214771,#214772,
#214773,#214774),.UNSPECIFIED.,.F.,.F.,(4,2,2,2,2,2,2,2,2,2,2,2,2,2,2,2,
2,2,2,2,2,2,2,2,2,2,2,2,2,2,2,2,2,2,2,2,2,2,4),(-22.5104081169932,-22.3612307693209,
-22.2355377097177,-21.9285413116893,-21.8025981562684,-21.551656587909,
-21.306722143075,-21.0388457213177,-20.7809474596957,-20.6553456671694,
-20.397175432749,-20.1384391189269,-19.8873687315545,-19.7625221501105,
-19.5043045239689,-19.2615640724446,-19.0109272243863,-18.8858343260698,
-18.6276181991213,-18.3800459105684,-18.1292740488693,-18.0042546680597,
-17.7460368060689,-17.4881657987609,-17.236111325147,-17.0336800623867,
-16.9087594766789,-16.6375496402009,-16.3796396281236,-16.2539930447797,
-15.9958313522177,-15.7360196781561,-15.4849211969179,-15.3600911092144,
-15.1018732790179,-14.8712963732557,-14.6134571162699,-14.4880912198269,
-14.334025337542),.UNSPECIFIED.);
#30526=B_SPLINE_CURVE_WITH_KNOTS('',3,(#214776,#214777,#214778,#214779,
#214780,#214781,#214782,#214783,#214784,#214785,#214786,#214787,#214788,
#214789,#214790,#214791,#214792,#214793,#214794,#214795,#214796,#214797,
#214798,#214799,#214800,#214801,#214802,#214803,#214804,#214805,#214806,
#214807,#214808,#214809,#214810,#214811),.UNSPECIFIED.,.F.,.F.,(4,2,2,2,
2,2,2,2,2,2,2,2,2,2,2,2,2,4),(-27.089958399627,-26.952979419026,-26.8169785957911,
-26.5513613453522,-26.3745643085782,-26.1163666107755,-25.87887336021,-25.647399127963,
-25.431082688021,-25.1956028474001,-25.0178025030768,-24.7851132908777,
-24.5557298449793,-24.2978969360107,-24.1329631967999,-23.9012495356808,
-23.6653755408411,-23.4938196648925),.UNSPECIFIED.);
#30527=B_SPLINE_CURVE_WITH_KNOTS('',3,(#214812,#214813,#214814,#214815,
#214816,#214817,#214818,#214819,#214820,#214821,#214822,#214823,#214824,
#214825,#214826,#214827,#214828,#214829,#214830,#214831,#214832,#214833,
#214834,#214835,#214836,#214837,#214838,#214839,#214840,#214841,#214842,
#214843,#214844,#214845,#214846,#214847,#214848,#214849,#214850,#214851,
#214852,#214853,#214854,#214855,#214856,#214857),.UNSPECIFIED.,.F.,.F.,
(4,2,2,2,2,2,2,2,2,2,2,2,2,2,2,2,2,2,2,2,2,2,4),(-4.5795509234186,-4.50984625011772,
-4.27825488944027,-4.1149876509827,-3.86459297117082,-3.62991131288588,
-3.39840441911819,-3.23643616951018,-2.98583978245699,-2.74413559559504,
-2.48592991455161,-2.36114402600808,-2.10999536200624,-1.84777195661155,
-1.589644744617,-1.46390699951972,-1.20598373740661,-0.927127338164872,
-0.812594909757223,-0.606764161622401,-0.304527926094519,-0.153020088801399,
-3.84812749945382E-6),.UNSPECIFIED.);
#30528=B_SPLINE_CURVE_WITH_KNOTS('',3,(#214862,#214863,#214864,#214865,
#214866,#214867,#214868,#214869,#214870,#214871,#214872,#214873,#214874,
#214875,#214876,#214877,#214878,#214879,#214880,#214881,#214882,#214883,
#214884,#214885,#214886,#214887,#214888,#214889,#214890,#214891,#214892,
#214893,#214894,#214895,#214896,#214897,#214898,#214899,#214900,#214901,
#214902,#214903,#214904,#214905,#214906,#214907,#214908,#214909,#214910,
#214911,#214912,#214913,#214914,#214915,#214916,#214917,#214918,#214919,
#214920,#214921,#214922,#214923,#214924,#214925,#214926,#214927,#214928,
#214929,#214930,#214931,#214932,#214933,#214934,#214935,#214936,#214937,
#214938,#214939),.UNSPECIFIED.,.F.,.F.,(4,2,2,2,2,2,2,2,2,2,2,2,2,2,2,2,
2,2,2,2,2,2,2,2,2,2,2,2,2,2,2,2,2,2,2,2,2,2,4),(-14.334025337542,-14.2298880752575,
-13.9928889355398,-13.7614412675403,-13.5452357011143,-13.3285719908861,
-13.0971354937459,-12.8599793321159,-12.601777163161,-12.4764005548312,
-12.2185590226874,-11.9873142271819,-11.7290963947761,-11.6042075960275,
-11.3532104274166,-11.0972543394135,-10.8390648910172,-10.7135831106281,
-10.4557157588316,-10.2181940081271,-9.95999746144929,-9.83459447204947,
-9.57674878778774,-9.34391585468663,-9.08570178135842,-8.96067581182445,
-8.70992487595289,-8.4629645160084,-8.20475120064606,-8.07969125810166,
-7.82900251582835,-7.58427333026132,-7.32605897513911,-7.201111763903,-6.95022163718091,
-6.69815316779949,-6.43995054050984,-6.31464537487433,-6.15788331278694),
 .UNSPECIFIED.);
#30529=B_SPLINE_CURVE_WITH_KNOTS('',3,(#214940,#214941,#214942,#214943,
#214944,#214945,#214946,#214947,#214948,#214949,#214950,#214951,#214952,
#214953,#214954,#214955,#214956,#214957,#214958,#214959,#214960,#214961,
#214962,#214963,#214964,#214965,#214966,#214967,#214968,#214969,#214970,
#214971,#214972,#214973,#214974,#214975,#214976,#214977,#214978,#214979,
#214980,#214981,#214982,#214983,#214984,#214985,#214986,#214987,#214988,
#214989,#214990,#214991,#214992,#214993,#214994,#214995,#214996,#214997,
#214998,#214999,#215000,#215001,#215002,#215003,#215004,#215005,#215006,
#215007,#215008,#215009,#215010,#215011,#215012,#215013,#215014,#215015,
#215016,#215017),.UNSPECIFIED.,.F.,.F.,(4,2,2,2,2,2,2,2,2,2,2,2,2,2,2,2,
2,2,2,2,2,2,2,2,2,2,2,2,2,2,2,2,2,2,2,2,2,2,4),(-12.7553010434687,-12.6016556768374,
-12.4763182694624,-12.218491551322,-11.9892784696402,-11.7566700395306,
-11.5797800311709,-11.3436395338856,-11.1265836305225,-10.895209493342,
-10.6572556971099,-10.3990679449927,-10.2736349244766,-10.0157862458109,
-9.78103815707203,-9.52283394508956,-9.39765070502228,-9.14720450848217,
-8.91082671304611,-8.67902923702854,-8.51277037102089,-8.25492183080519,
-8.01981155397926,-7.76161037628427,-7.63639857901851,-7.38601142426069,
-7.15160657277073,-6.9201416220309,-6.75884469323388,-6.50814457860648,
-6.26276625595113,-6.00455921046281,-5.87958199057688,-5.62875764298286,
-5.37886593938861,-5.12066465996931,-4.99546505972988,-4.74505487654086,
-4.5795509234186),.UNSPECIFIED.);
#30530=B_SPLINE_CURVE_WITH_KNOTS('',3,(#215026,#215027,#215028,#215029,
#215030,#215031),.UNSPECIFIED.,.F.,.F.,(4,2,4),(1.00000001154634E-6,0.291982877240899,
0.583963182531403),.UNSPECIFIED.);
#30531=B_SPLINE_CURVE_WITH_KNOTS('',3,(#215035,#215036,#215037,#215038,
#215039,#215040),.UNSPECIFIED.,.F.,.F.,(4,2,4),(1.18860081512343E-5,0.292247563585459,
0.584494052040958),.UNSPECIFIED.);
#30532=B_SPLINE_CURVE_WITH_KNOTS('',3,(#215044,#215045,#215046,#215047,
#215048,#215049,#215050,#215051,#215052,#215053,#215054,#215055,#215056,
#215057,#215058,#215059,#215060,#215061,#215062,#215063,#215064,#215065,
#215066,#215067,#215068,#215069,#215070,#215071,#215072,#215073,#215074,
#215075,#215076,#215077,#215078,#215079,#215080,#215081,#215082,#215083,
#215084,#215085,#215086,#215087,#215088,#215089,#215090,#215091,#215092,
#215093,#215094,#215095,#215096,#215097,#215098,#215099,#215100,#215101,
#215102,#215103),.UNSPECIFIED.,.F.,.F.,(4,2,2,2,2,2,2,2,2,2,2,2,2,2,2,2,
2,2,2,2,2,2,2,2,2,2,2,2,2,4),(-27.0887410610092,-26.9511925330194,-26.8146181657615,
-26.5477430484365,-26.3703867926432,-26.1121969470036,-25.8619181368252,
-25.61109070341,-25.486127317508,-25.2279323061975,-24.9957522036846,-24.7379286430516,
-24.6125451134737,-24.3543677958648,-24.1004364568259,-23.9752344396555,
-23.6847558007391,-23.4539116075989,-23.2606464300677,-23.1342701225633,
-22.7584338658159,-22.633498574235,-22.3598177762354,-22.1019137699259,
-21.9762419243061,-21.7181016904069,-21.4575171051022,-21.2064122614871,
-21.0816012437997,-20.9311220871695),.UNSPECIFIED.);
#30533=B_SPLINE_CURVE_WITH_KNOTS('',3,(#215104,#215105,#215106,#215107,
#215108,#215109,#215110,#215111,#215112,#215113,#215114,#215115,#215116,
#215117),.UNSPECIFIED.,.F.,.F.,(4,2,2,2,2,2,4),(0.,0.254132792260232,0.504072118513429,
1.01015766536903,1.26037994975016,1.64270580735333,2.01988313929097),
 .UNSPECIFIED.);
#30534=B_SPLINE_CURVE_WITH_KNOTS('',3,(#215122,#215123,#215124,#215125),
 .UNSPECIFIED.,.F.,.F.,(4,4),(-0.00220042394831986,0.),.UNSPECIFIED.);
#30535=B_SPLINE_CURVE_WITH_KNOTS('',3,(#215127,#215128,#215129,#215130,
#215131,#215132,#215133,#215134,#215135,#215136,#215137,#215138,#215139,
#215140,#215141,#215142,#215143,#215144,#215145,#215146,#215147,#215148,
#215149,#215150,#215151,#215152,#215153,#215154,#215155,#215156,#215157,
#215158,#215159,#215160,#215161,#215162,#215163,#215164,#215165,#215166,
#215167,#215168,#215169,#215170,#215171,#215172),.UNSPECIFIED.,.F.,.F.,
(4,2,2,2,2,2,2,2,2,2,2,2,2,2,2,2,2,2,2,2,2,2,4),(3.77495847628064E-5,0.239786601820375,
0.486605707252922,0.970538667060806,1.45703768164762,1.71085426685665,1.9510783074637,
2.07349206054796,2.55160936918131,2.80110529120643,3.03699522422359,3.28275824999043,
3.52002970929651,3.76617821420921,4.00121882590256,4.49262572156428,4.61272242555652,
4.85423743097051,5.08785380877439,5.57193736666521,6.05829820485534,6.18384427890247,
6.56939833044695),.UNSPECIFIED.);
#30536=B_SPLINE_CURVE_WITH_KNOTS('',3,(#215175,#215176,#215177,#215178,
#215179,#215180,#215181,#215182,#215183,#215184,#215185,#215186,#215187,
#215188,#215189,#215190,#215191,#215192,#215193,#215194,#215195,#215196,
#215197,#215198,#215199,#215200,#215201,#215202,#215203,#215204,#215205,
#215206,#215207,#215208,#215209,#215210,#215211,#215212,#215213,#215214,
#215215,#215216,#215217,#215218,#215219,#215220,#215221,#215222,#215223,
#215224,#215225,#215226,#215227,#215228,#215229,#215230,#215231,#215232),
 .UNSPECIFIED.,.F.,.F.,(4,3,3,3,3,3,3,3,3,3,3,3,3,3,3,3,3,3,3,4),(0.,0.0577023232573194,
0.115555621115559,0.173492165360459,0.231551782116688,0.25,0.307569756346389,
0.36507578732566,0.422538236883637,0.479957516807691,0.537334036195806,
0.594651018367979,0.651929822767017,0.709155453145963,0.75,0.807257177143259,
0.864351407537752,0.921347999937229,0.97820765935611,0.999999816562462),
 .UNSPECIFIED.);
#30537=B_SPLINE_CURVE_WITH_KNOTS('',3,(#215238,#215239,#215240,#215241),
 .UNSPECIFIED.,.F.,.F.,(4,4),(-6.83645233358743E-6,-1.00000001751477E-6),
 .UNSPECIFIED.);
#30538=B_SPLINE_CURVE_WITH_KNOTS('',3,(#215243,#215244,#215245,#215246,
#215247,#215248,#215249,#215250,#215251,#215252,#215253,#215254),
 .UNSPECIFIED.,.F.,.F.,(4,2,2,2,2,4),(0.000339869836819791,0.29675202029107,
0.394471814058443,0.493164400823471,0.639110988050242,0.788070724201746),
 .UNSPECIFIED.);
#30539=B_SPLINE_CURVE_WITH_KNOTS('',3,(#215257,#215258,#215259,#215260,
#215261,#215262,#215263,#215264,#215265,#215266,#215267,#215268),
 .UNSPECIFIED.,.F.,.F.,(4,2,2,2,2,4),(-0.787810247908823,-0.491424601923884,
-0.393707156561869,-0.295035291842161,-0.149115943288589,-9.76537854817782E-5),
 .UNSPECIFIED.);
#30540=B_SPLINE_CURVE_WITH_KNOTS('',3,(#215271,#215272,#215273,#215274,
#215275,#215276,#215277,#215278,#215279,#215280,#215281,#215282,#215283,
#215284,#215285,#215286,#215287,#215288,#215289,#215290,#215291,#215292,
#215293,#215294,#215295,#215296,#215297,#215298,#215299,#215300,#215301,
#215302,#215303,#215304,#215305,#215306,#215307,#215308,#215309,#215310,
#215311,#215312,#215313,#215314,#215315,#215316,#215317,#215318,#215319,
#215320,#215321,#215322,#215323,#215324,#215325,#215326,#215327,#215328,
#215329,#215330,#215331,#215332,#215333,#215334,#215335,#215336,#215337,
#215338,#215339,#215340),.UNSPECIFIED.,.F.,.F.,(4,2,2,2,2,2,2,2,2,2,2,2,
2,2,2,2,2,2,2,2,2,2,2,2,2,2,2,2,2,2,2,2,2,2,4),(-20.0196235340061,-19.8157278920515,
-19.6158545518425,-19.4425763978127,-19.2852028557817,-19.1959685061364,
-19.0203362825393,-18.8728424835519,-18.7345184196789,-18.5651733062971,
-18.3584086465096,-18.1897342242108,-18.1009133571369,-17.9231088860798,
-17.7687386604926,-17.6127844006329,-17.4523655002313,-17.3638013379125,
-17.1842840455061,-17.0221648541842,-16.9027716802059,-16.7343479146783,
-16.5301402266849,-16.3682944213952,-16.1638372797701,-16.0746707278444,
-15.9189413862097,-15.8312910721691,-15.5641446602286,-15.3837526745358,
-15.2039523974867,-15.0498956541389,-14.9618693672449,-14.6038541971235,
-14.2994391167293),.UNSPECIFIED.);
#30541=B_SPLINE_CURVE_WITH_KNOTS('',3,(#215343,#215344,#215345,#215346,
#215347,#215348,#215349,#215350,#215351,#215352,#215353,#215354,#215355,
#215356,#215357,#215358,#215359,#215360,#215361,#215362,#215363,#215364,
#215365,#215366,#215367,#215368,#215369,#215370,#215371,#215372,#215373,
#215374,#215375,#215376,#215377,#215378,#215379,#215380,#215381,#215382,
#215383,#215384,#215385,#215386,#215387,#215388,#215389,#215390,#215391,
#215392,#215393,#215394,#215395,#215396,#215397,#215398,#215399,#215400,
#215401,#215402,#215403,#215404,#215405,#215406,#215407,#215408,#215409,
#215410),.UNSPECIFIED.,.F.,.F.,(4,2,2,2,2,2,2,2,2,2,2,2,2,2,2,2,2,2,2,2,
2,2,2,2,2,2,2,2,2,2,2,2,2,4),(-5.72098192612602,-5.4140289061323,-5.056101730372,
-4.96798087881037,-4.819769206694,-4.54633567752282,-4.37277702978704,-4.20554432130538,
-4.0478229434517,-3.91343223942507,-3.5963260817461,-3.50785527543515,-3.35735778939112,
-3.20580694022997,-3.02615489172175,-2.84949295160721,-2.76019692805457,
-2.56673230648565,-2.40566688978276,-2.2464078740048,-2.09440523942289,
-1.91421338925738,-1.73650461422533,-1.55941996019895,-1.47033771435364,
-1.31006776518604,-1.14767795859055,-0.999884460342694,-0.824207561520106,
-0.734963617853822,-0.578056733648994,-0.420047611278566,-0.211187702725621,
-6.83645233358743E-6),.UNSPECIFIED.);
#30542=B_SPLINE_CURVE_WITH_KNOTS('',3,(#215415,#215416,#215417,#215418,
#215419,#215420,#215421,#215422,#215423,#215424,#215425,#215426,#215427,
#215428,#215429,#215430,#215431,#215432,#215433,#215434,#215435,#215436,
#215437,#215438,#215439,#215440,#215441,#215442,#215443,#215444,#215445,
#215446,#215447,#215448,#215449,#215450,#215451,#215452,#215453,#215454,
#215455,#215456,#215457,#215458,#215459,#215460,#215461,#215462,#215463,
#215464,#215465,#215466,#215467,#215468,#215469,#215470,#215471,#215472,
#215473,#215474,#215475,#215476,#215477,#215478,#215479,#215480,#215481,
#215482,#215483,#215484,#215485,#215486),.UNSPECIFIED.,.F.,.F.,(4,2,2,2,
2,2,2,2,2,2,2,2,2,2,2,2,2,2,2,2,2,2,2,2,2,2,2,2,2,2,2,2,2,2,2,4),(-11.4412093673078,
-11.338051198562,-11.1891609467898,-11.1010562826919,-10.7866246366731,
-10.6066561084781,-10.4268423987289,-10.2467065997548,-10.098678538798,
-10.0105929109292,-9.65463874041737,-9.48052854819771,-9.31002440202757,
-9.13918288304346,-8.98055225874758,-8.82546188245068,-8.67973574012756,
-8.49997454609656,-8.41152390733726,-8.24811344358312,-8.07358642266137,
-7.92464560938184,-7.70469009445336,-7.55442719254641,-7.35785242194359,
-7.20795195047273,-6.90068692991203,-6.81290801551602,-6.64908308538578,
-6.49018627923697,-6.31439124792872,-6.22502211673781,-6.07787970006461,
-5.9211138364368,-5.76964709342306,-5.72098192612602),.UNSPECIFIED.);
#30543=B_SPLINE_CURVE_WITH_KNOTS('',3,(#215487,#215488,#215489,#215490,
#215491,#215492,#215493,#215494,#215495,#215496,#215497,#215498,#215499,
#215500,#215501,#215502,#215503,#215504,#215505,#215506,#215507,#215508,
#215509,#215510,#215511,#215512,#215513,#215514,#215515,#215516,#215517,
#215518,#215519,#215520,#215521,#215522,#215523,#215524,#215525,#215526,
#215527,#215528,#215529,#215530,#215531,#215532,#215533,#215534,#215535,
#215536,#215537,#215538,#215539,#215540,#215541,#215542,#215543,#215544,
#215545,#215546,#215547,#215548,#215549,#215550,#215551,#215552,#215553,
#215554,#215555,#215556,#215557,#215558,#215559,#215560),.UNSPECIFIED.,
 .F.,.F.,(4,2,2,2,2,2,2,2,2,2,2,2,2,2,2,2,2,2,2,2,2,2,2,2,2,2,2,2,2,2,2,
2,2,2,2,2,4),(-14.2994391167293,-14.2477501603601,-14.0678479146357,-13.892033039284,
-13.7449994332337,-13.5933261734264,-13.4364967134449,-13.3472472844073,
-13.1713477116733,-12.9929134291802,-12.8495266728997,-12.6946660563486,
-12.50714685734,-12.3408887659613,-12.2520944775663,-12.0738427041846,-11.9100950504764,
-11.762543263869,-11.6043231736101,-11.5157857281393,-11.3361551841859,
-11.1826312112805,-11.0366836994984,-10.8800924293092,-10.709523970501,
-10.5391611197758,-10.3652159760863,-10.0092725080805,-9.92114808123932,
-9.76123299805315,-9.58102608277333,-9.38455674435135,-9.20446141623579,
-9.04465508227102,-8.77152473193952,-8.59818150590377,-8.58008361725819),
 .UNSPECIFIED.);
#30544=B_SPLINE_CURVE_WITH_KNOTS('',3,(#215565,#215566,#215567,#215568,
#215569,#215570,#215571,#215572,#215573,#215574,#215575,#215576,#215577,
#215578,#215579,#215580,#215581,#215582,#215583,#215584,#215585,#215586,
#215587,#215588,#215589,#215590,#215591,#215592,#215593,#215594,#215595,
#215596,#215597,#215598,#215599,#215600,#215601,#215602,#215603,#215604,
#215605,#215606,#215607,#215608,#215609,#215610,#215611,#215612,#215613,
#215614,#215615,#215616,#215617,#215618,#215619,#215620,#215621,#215622,
#215623,#215624,#215625,#215626,#215627,#215628,#215629,#215630,#215631,
#215632,#215633,#215634),.UNSPECIFIED.,.F.,.F.,(4,2,2,2,2,2,2,2,2,2,2,2,
2,2,2,2,2,2,2,2,2,2,2,2,2,2,2,2,2,2,2,2,2,2,4),(-17.1619514598514,-17.0707998436542,
-16.9045145666629,-16.7309852587693,-16.4586010792192,-16.309900328499,
-16.221783342895,-15.8639724075797,-15.5085207792211,-15.355192371691,-15.2006223540609,
-15.0529932168943,-14.9636273693785,-14.7878315671842,-14.6292399631429,
-14.4801068549128,-14.3234633590855,-14.1304499920554,-13.9645679910772,
-13.8756157382424,-13.6982985297934,-13.5306753108811,-13.3696744824731,
-13.2167356928649,-13.0331390496967,-12.868276309184,-12.6976058536657,
-12.5270153994763,-12.3098536115514,-12.144439553079,-12.0660876907221,
-11.9201930773019,-11.8318736328062,-11.5176804116582,-11.4412093673078),
 .UNSPECIFIED.);
#30545=B_SPLINE_CURVE_WITH_KNOTS('',3,(#215635,#215636,#215637,#215638,
#215639,#215640,#215641,#215642,#215643,#215644,#215645,#215646,#215647,
#215648,#215649,#215650,#215651,#215652,#215653,#215654,#215655,#215656,
#215657,#215658,#215659,#215660,#215661,#215662,#215663,#215664,#215665,
#215666,#215667,#215668,#215669,#215670,#215671,#215672,#215673,#215674,
#215675,#215676,#215677,#215678,#215679,#215680,#215681,#215682,#215683,
#215684,#215685,#215686,#215687,#215688,#215689,#215690,#215691,#215692,
#215693,#215694,#215695,#215696,#215697,#215698,#215699,#215700,#215701,
#215702,#215703,#215704,#215705,#215706),.UNSPECIFIED.,.F.,.F.,(4,2,2,2,
2,2,2,2,2,2,2,2,2,2,2,2,2,2,2,2,2,2,2,2,2,2,2,2,2,2,2,2,2,2,2,4),(-8.58008361725819,
-8.4286097990283,-8.26279364651665,-8.12156683079037,-7.91613144710299,
-7.7770878294328,-7.60612693118763,-7.51786059374663,-7.355334811172,-7.17383932316611,
-7.02447968816001,-6.83757625395707,-6.68626101237962,-6.50602979938285,
-6.32854906868142,-6.15109686754141,-6.06207677134911,-5.90122486412687,
-5.73980986202818,-5.59047106699529,-5.41469586981278,-5.32548902221139,
-5.16583815293916,-4.98252592676009,-4.84153082561947,-4.61168690966548,
-4.47290134245129,-4.25386145852119,-4.12105436091202,-3.80495585716246,
-3.71697908525877,-3.56653413552749,-3.29029346081404,-3.1165390136774,
-2.94720715469032,-2.86068452297866),.UNSPECIFIED.);
#30546=B_SPLINE_CURVE_WITH_KNOTS('',3,(#215712,#215713,#215714,#215715),
 .UNSPECIFIED.,.F.,.F.,(4,4),(-9.10624732692347E-6,-9.99999999714383E-7),
 .UNSPECIFIED.);
#30547=B_SPLINE_CURVE_WITH_KNOTS('',3,(#215717,#215718,#215719,#215720,
#215721,#215722,#215723,#215724),.UNSPECIFIED.,.F.,.F.,(4,2,2,4),(0.000264654385577618,
0.197179255479982,0.294830977384805,0.393932741177781),.UNSPECIFIED.);
#30548=B_SPLINE_CURVE_WITH_KNOTS('',3,(#215727,#215728,#215729,#215730,
#215731,#215732,#215733,#215734),.UNSPECIFIED.,.F.,.F.,(4,2,2,4),(-0.393859367022616,
-0.195155498856749,-0.0984062562737634,-0.000187054781780563),
 .UNSPECIFIED.);
#30549=B_SPLINE_CURVE_WITH_KNOTS('',3,(#215737,#215738,#215739,#215740,
#215741,#215742,#215743,#215744,#215745,#215746,#215747,#215748,#215749,
#215750,#215751,#215752,#215753,#215754,#215755,#215756,#215757,#215758,
#215759,#215760,#215761,#215762,#215763,#215764,#215765,#215766,#215767,
#215768,#215769,#215770,#215771,#215772,#215773,#215774,#215775,#215776,
#215777,#215778,#215779,#215780,#215781,#215782,#215783,#215784,#215785,
#215786,#215787,#215788,#215789,#215790,#215791,#215792,#215793,#215794,
#215795,#215796,#215797,#215798,#215799,#215800,#215801,#215802),
 .UNSPECIFIED.,.F.,.F.,(4,2,2,2,2,2,2,2,2,2,2,2,2,2,2,2,2,2,2,2,2,2,2,2,
2,2,2,2,2,2,2,2,4),(-20.0265413516697,-19.7916844706762,-19.5590662266383,
-19.4024008232342,-19.256032447578,-19.166686445916,-18.9909052667409,-18.8210922306707,
-18.6737831612299,-18.521576051052,-18.3315039514708,-18.1668536215511,
-17.995500173617,-17.8256557704653,-17.609225679366,-17.4395698378931,-17.3509823357291,
-17.1723670573172,-17.0230846436569,-16.8620577093886,-16.7023795041317,
-16.5322074361327,-16.3618316254644,-16.1883018411768,-15.8329332221974,
-15.5336648716409,-15.4458799425158,-15.1745299152678,-14.9941718872728,
-14.8143733476338,-14.6613652206745,-14.5733584986169,-14.3060169149355),
 .UNSPECIFIED.);
#30550=B_SPLINE_CURVE_WITH_KNOTS('',3,(#215805,#215806,#215807,#215808,
#215809,#215810,#215811,#215812,#215813,#215814,#215815,#215816,#215817,
#215818,#215819,#215820,#215821,#215822,#215823,#215824,#215825,#215826,
#215827,#215828,#215829,#215830,#215831,#215832,#215833,#215834,#215835,
#215836,#215837,#215838,#215839,#215840,#215841,#215842,#215843,#215844,
#215845,#215846,#215847,#215848,#215849,#215850,#215851,#215852,#215853,
#215854,#215855,#215856,#215857,#215858,#215859,#215860,#215861,#215862,
#215863,#215864,#215865,#215866,#215867,#215868,#215869,#215870,#215871,
#215872,#215873,#215874),.UNSPECIFIED.,.F.,.F.,(4,2,2,2,2,2,2,2,2,2,2,2,
2,2,2,2,2,2,2,2,2,2,2,2,2,2,2,2,2,2,2,2,2,2,4),(-5.72061718523155,-5.45327902906014,
-5.36526221058928,-5.21232654173221,-4.94148501082312,-4.76805599127904,
-4.60257504126808,-4.45597704073809,-4.27635443196831,-4.11908377830053,
-3.82844746279641,-3.47270207454062,-3.29904824307419,-3.12863076631413,
-2.95830433805699,-2.79525046268999,-2.63930549851454,-2.48756465643266,
-2.30737197039185,-2.12968316227983,-1.95260099959419,-1.86352213387736,
-1.70295441302047,-1.55476562448681,-1.39890926825175,-1.22301319224729,
-1.1336969300927,-0.981472937761808,-0.835350461991401,-0.756826061006568,
-0.597584350396601,-0.38942460359425,-0.19920936171246,-0.100488991555656,
-9.10624732692347E-6),.UNSPECIFIED.);
#30551=B_SPLINE_CURVE_WITH_KNOTS('',3,(#215879,#215880,#215881,#215882,
#215883,#215884,#215885,#215886,#215887,#215888,#215889,#215890,#215891,
#215892,#215893,#215894,#215895,#215896,#215897,#215898,#215899,#215900,
#215901,#215902,#215903,#215904,#215905,#215906,#215907,#215908,#215909,
#215910,#215911,#215912,#215913,#215914,#215915,#215916,#215917,#215918,
#215919,#215920,#215921,#215922,#215923,#215924,#215925,#215926,#215927,
#215928,#215929,#215930,#215931,#215932,#215933,#215934,#215935,#215936,
#215937,#215938,#215939,#215940,#215941,#215942,#215943,#215944,#215945,
#215946,#215947,#215948),.UNSPECIFIED.,.F.,.F.,(4,2,2,2,2,2,2,2,2,2,2,2,
2,2,2,2,2,2,2,2,2,2,2,2,2,2,2,2,2,2,2,2,2,2,4),(-11.4419881045767,-11.2813757427722,
-10.9230195600775,-10.5627315202554,-10.3040525988962,-10.0984733872441,
-10.0109954258154,-9.83436174340115,-9.74575772244497,-9.60239614232087,
-9.52573747390332,-9.35709163921518,-9.23242885839426,-9.0787523283877,
-8.8991056633472,-8.81056299647559,-8.65235325948151,-8.50488912061725,
-8.34098326812671,-8.16271885955965,-8.07392192693336,-7.90764130003375,
-7.72001379955113,-7.56506656821126,-7.42215076339577,-7.24369481826094,
-7.06777708120355,-6.97852418519129,-6.82191574427426,-6.67154336340269,
-6.52324657455666,-6.34744501943803,-6.16753233716479,-5.8113316468472,
-5.72061718523155),.UNSPECIFIED.);
#30552=B_SPLINE_CURVE_WITH_KNOTS('',3,(#215949,#215950,#215951,#215952,
#215953,#215954,#215955,#215956,#215957,#215958,#215959,#215960,#215961,
#215962,#215963,#215964,#215965,#215966,#215967,#215968,#215969,#215970,
#215971,#215972,#215973,#215974,#215975,#215976,#215977,#215978,#215979,
#215980,#215981,#215982,#215983,#215984,#215985,#215986,#215987,#215988,
#215989,#215990,#215991,#215992,#215993,#215994,#215995,#215996,#215997,
#215998,#215999,#216000,#216001,#216002,#216003,#216004,#216005,#216006,
#216007,#216008,#216009,#216010),.UNSPECIFIED.,.F.,.F.,(4,2,2,2,2,2,2,2,
2,2,2,2,2,2,2,2,2,2,2,2,2,2,2,2,2,2,2,2,2,2,4),(-14.3060169149355,-14.2153533605477,
-13.8592013666033,-13.6793010719143,-13.5035148376052,-13.3553481442817,
-13.2008977678138,-13.0461650598207,-12.9568903328304,-12.7809148780731,
-12.6240853619038,-12.4969981438777,-12.3275773000993,-12.1235583172129,
-11.954900463041,-11.7571435569065,-11.5890846229911,-11.4181410921951,
-11.2476093170342,-11.0735226012537,-10.7173257541303,-10.4374746893783,
-10.279085066303,-10.1905159431329,-10.0138961142132,-9.92641324896063,
-9.72320254008456,-9.46435634533218,-9.10415884290171,-8.74601715292997,
-8.58352616457983),.UNSPECIFIED.);
#30553=B_SPLINE_CURVE_WITH_KNOTS('',3,(#216015,#216016,#216017,#216018,
#216019,#216020,#216021,#216022,#216023,#216024,#216025,#216026,#216027,
#216028,#216029,#216030,#216031,#216032,#216033,#216034,#216035,#216036,
#216037,#216038,#216039,#216040,#216041,#216042,#216043,#216044,#216045,
#216046,#216047,#216048,#216049,#216050,#216051,#216052,#216053,#216054,
#216055,#216056,#216057,#216058,#216059,#216060,#216061,#216062,#216063,
#216064,#216065,#216066,#216067,#216068,#216069,#216070,#216071,#216072,
#216073,#216074,#216075,#216076,#216077,#216078,#216079,#216080,#216081,
#216082),.UNSPECIFIED.,.F.,.F.,(4,2,2,2,2,2,2,2,2,2,2,2,2,2,2,2,2,2,2,2,
2,2,2,2,2,2,2,2,2,2,2,2,2,4),(-17.1637028159425,-17.060980079838,-16.9731277708488,
-16.7039506772942,-16.6158780571909,-16.2579619756541,-15.902163184888,
-15.7222693652696,-15.5464068666462,-15.4013221879371,-15.2469926384159,
-15.0895045273709,-15.0002592668443,-14.8243372318778,-14.6499630540693,
-14.4989074383824,-14.4109524992573,-14.0991443530046,-13.9481908664376,
-13.7545715781592,-13.6668395980893,-13.3716646622225,-13.2255092730848,
-13.0815190750491,-12.9115779913326,-12.6477158018356,-12.5071502928206,
-12.2921387977884,-12.1128676892355,-11.9372023629355,-11.7950742363449,
-11.6250873609284,-11.455560653579,-11.4419881045767),.UNSPECIFIED.);
#30554=B_SPLINE_CURVE_WITH_KNOTS('',3,(#216083,#216084,#216085,#216086,
#216087,#216088,#216089,#216090,#216091,#216092,#216093,#216094,#216095,
#216096,#216097,#216098,#216099,#216100,#216101,#216102,#216103,#216104,
#216105,#216106,#216107,#216108,#216109,#216110,#216111,#216112,#216113,
#216114,#216115,#216116,#216117,#216118,#216119,#216120,#216121,#216122,
#216123,#216124,#216125,#216126,#216127,#216128,#216129,#216130,#216131,
#216132,#216133,#216134,#216135,#216136,#216137,#216138,#216139,#216140,
#216141,#216142,#216143,#216144,#216145,#216146,#216147,#216148),
 .UNSPECIFIED.,.F.,.F.,(4,2,2,2,2,2,2,2,2,2,2,2,2,2,2,2,2,2,2,2,2,2,2,2,
2,2,2,2,2,2,2,2,4),(-8.58352616457983,-8.57213493872926,-8.4043656780315,
-8.23701159034506,-8.09922963062936,-7.8790859158866,-7.74110042947993,
-7.56032808455996,-7.26345493070519,-6.90746919946779,-6.73291365888483,
-6.56197986053401,-6.39019403814515,-6.2205243571735,-5.9923600289844,-5.90464672861176,
-5.71406901099162,-5.56250424947646,-5.38258318234043,-5.20398838814573,
-5.02796851980871,-4.93869431385693,-4.78385613976576,-4.62994880217048,
-4.48093247543028,-4.30514646512333,-4.12522809790341,-3.76913166638306,
-3.41116858385401,-3.32315902178704,-3.17015858971904,-2.99032705055544,
-2.86193028654911),.UNSPECIFIED.);
#30555=B_SPLINE_CURVE_WITH_KNOTS('',3,(#216154,#216155,#216156,#216157),
 .UNSPECIFIED.,.F.,.F.,(4,4),(0.000166910408644729,0.000172246164355015),
 .UNSPECIFIED.);
#30556=B_SPLINE_CURVE_WITH_KNOTS('',3,(#216159,#216160,#216161,#216162,
#216163,#216164),.UNSPECIFIED.,.F.,.F.,(4,2,4),(0.00015886842573906,0.234718197189778,
0.469154050605007),.UNSPECIFIED.);
#30557=B_SPLINE_CURVE_WITH_KNOTS('',3,(#216171,#216172,#216173,#216174,
#216175,#216176,#216177,#216178,#216179,#216180,#216181,#216182,#216183,
#216184,#216185,#216186,#216187,#216188,#216189,#216190,#216191,#216192,
#216193,#216194,#216195,#216196,#216197,#216198,#216199,#216200,#216201,
#216202,#216203,#216204,#216205,#216206,#216207,#216208,#216209,#216210,
#216211,#216212,#216213,#216214,#216215,#216216,#216217,#216218,#216219,
#216220,#216221,#216222,#216223,#216224,#216225,#216226,#216227,#216228,
#216229,#216230,#216231,#216232,#216233,#216234,#216235,#216236,#216237,
#216238,#216239,#216240,#216241,#216242,#216243,#216244),.UNSPECIFIED.,
 .F.,.F.,(4,2,2,2,2,2,2,2,2,2,2,2,2,2,2,2,2,2,2,2,2,2,2,2,2,2,2,2,2,2,2,
2,2,2,2,2,4),(-6.99964291132138,-6.96394858937547,-6.73463545641311,-6.49990723450948,
-6.27551710468842,-6.16173884786356,-5.93194349327878,-5.69738288218128,
-5.47300205903081,-5.35908307540296,-5.12907111679914,-4.89457892018263,
-4.67026667804598,-4.55619766722167,-4.32637859683717,-4.09175009325455,
-3.86759000101173,-3.75343478832399,-3.52419127870063,-3.25368513389825,
-3.13973680388134,-2.95254528949578,-2.72385358337876,-2.4451494752902,
-2.33112321801767,-2.0093121095651,-1.89438301602845,-1.73461634653569,
-1.50777243640498,-1.2869037055871,-1.06277033526056,-0.948922951171791,
-0.720534931469837,-0.485452231856019,-0.245885103670598,-0.123137748004486,
-0.00053524047117373),.UNSPECIFIED.);
#30558=B_SPLINE_CURVE_WITH_KNOTS('',3,(#216247,#216248,#216249,#216250,
#216251,#216252,#216253,#216254,#216255,#216256,#216257,#216258,#216259,
#216260,#216261,#216262,#216263,#216264,#216265,#216266,#216267,#216268,
#216269,#216270,#216271,#216272,#216273,#216274,#216275,#216276,#216277,
#216278,#216279,#216280,#216281,#216282,#216283,#216284,#216285,#216286,
#216287,#216288,#216289,#216290,#216291,#216292,#216293,#216294,#216295,
#216296,#216297,#216298,#216299,#216300,#216301,#216302,#216303,#216304,
#216305,#216306,#216307,#216308,#216309,#216310,#216311,#216312,#216313,
#216314,#216315,#216316,#216317,#216318),.UNSPECIFIED.,.F.,.F.,(4,2,2,2,
2,2,2,2,2,2,2,2,2,2,2,2,2,2,2,2,2,2,2,2,2,2,2,2,2,2,2,2,2,2,2,4),(-24.6757663477501,
-24.5533436654801,-24.4307711038346,-24.1915697619018,-23.9564679661864,
-23.7281366468575,-23.6142452247218,-23.3901168444522,-23.1548585281943,
-23.040619601695,-22.7722458466604,-22.6576238849321,-22.4301674660062,
-22.206076808646,-21.9625811024712,-21.7349429828328,-21.5767302857709,
-21.4620624951134,-21.2330970713377,-21.0089981637414,-20.7547023533752,
-20.5255173717378,-20.3722665776375,-20.2577140022871,-19.937803146283,
-19.7067859523919,-19.4772611387739,-19.1295462031688,-19.015361295707,
-18.7919457097124,-18.5670290601582,-18.332361974679,-18.2181203927842,
-17.9941659427034,-17.76958038057,-17.675937012053),.UNSPECIFIED.);
#30559=B_SPLINE_CURVE_WITH_KNOTS('',3,(#216323,#216324,#216325,#216326,
#216327,#216328,#216329,#216330,#216331,#216332,#216333,#216334,#216335,
#216336,#216337,#216338,#216339,#216340,#216341,#216342,#216343,#216344,
#216345,#216346,#216347,#216348,#216349,#216350,#216351,#216352,#216353,
#216354,#216355,#216356,#216357,#216358,#216359,#216360,#216361,#216362,
#216363,#216364,#216365,#216366,#216367,#216368,#216369,#216370,#216371,
#216372,#216373,#216374,#216375,#216376,#216377,#216378,#216379,#216380,
#216381,#216382,#216383,#216384,#216385,#216386,#216387,#216388,#216389,
#216390,#216391,#216392,#216393,#216394,#216395,#216396,#216397,#216398),
 .UNSPECIFIED.,.F.,.F.,(4,2,2,2,2,2,2,2,2,2,2,2,2,2,2,2,2,2,2,2,2,2,2,2,
2,2,2,2,2,2,2,2,2,2,2,2,2,4),(-14.4469920765838,-14.3339145542341,-14.1050748344662,
-13.9912231520843,-13.7669491019276,-13.5318755495119,-13.3035366786338,
-13.1121862203767,-12.9981460748547,-12.7756563829289,-12.5512394960465,
-12.3377263279076,-12.1170350634801,-11.8925161013489,-11.7787201437416,
-11.5485381666371,-11.2577338092456,-11.1435996416612,-10.8691626700202,
-10.7551801220181,-10.4083716979756,-10.1772692913796,-9.94810338992655,
-9.63183711218707,-9.51709302956755,-9.36871627394153,-9.14044456903546,
-8.9051890107586,-8.68108149544486,-8.56723085598633,-8.33887699025705,
-8.10375453299894,-7.87949303584005,-7.76573182405683,-7.53696692993187,
-7.30202815163844,-7.07767053099068,-6.99964291132138),.UNSPECIFIED.);
#30560=B_SPLINE_CURVE_WITH_KNOTS('',3,(#216399,#216400,#216401,#216402,
#216403,#216404,#216405,#216406,#216407,#216408,#216409,#216410,#216411,
#216412,#216413,#216414,#216415,#216416,#216417,#216418,#216419,#216420,
#216421,#216422,#216423,#216424,#216425,#216426,#216427,#216428,#216429,
#216430,#216431,#216432,#216433,#216434,#216435,#216436,#216437,#216438,
#216439,#216440,#216441,#216442,#216443,#216444,#216445,#216446,#216447,
#216448,#216449,#216450,#216451,#216452,#216453,#216454,#216455,#216456,
#216457,#216458,#216459,#216460,#216461,#216462,#216463,#216464,#216465,
#216466,#216467,#216468,#216469,#216470,#216471,#216472,#216473,#216474,
#216475,#216476),.UNSPECIFIED.,.F.,.F.,(4,2,2,2,2,2,2,2,2,2,2,2,2,2,2,2,
2,2,2,2,2,2,2,2,2,2,2,2,2,2,2,2,2,2,2,2,2,2,4),(-17.675937012053,-17.541667988348,
-17.3127948338258,-17.1989373991103,-16.9746455461691,-16.7395623888719,
-16.5111942932525,-16.3972697177496,-16.173096276875,-15.937840867139,-15.7097470667384,
-15.5957282273868,-15.3717063968006,-15.1363769908546,-14.9081664213362,
-14.7575876744846,-14.6428942325424,-14.4145872524929,-14.1904560789865,
-13.9434569157579,-13.8291588794412,-13.5264564835631,-13.4123746202815,
-13.1286563608922,-12.8985952015119,-12.784689567824,-12.5602259551404,
-12.3386056468598,-12.1227904334969,-11.8984111410574,-11.6756230896314,
-11.5615489911593,-11.3771973098817,-11.1484317978468,-10.9134094215749,
-10.68899971096,-10.4649257225573,-10.35065873192,-10.22845558376),
 .UNSPECIFIED.);
#30561=B_SPLINE_CURVE_WITH_KNOTS('',3,(#216481,#216482,#216483,#216484,
#216485,#216486,#216487,#216488,#216489,#216490,#216491,#216492,#216493,
#216494,#216495,#216496,#216497,#216498,#216499,#216500,#216501,#216502,
#216503,#216504,#216505,#216506,#216507,#216508,#216509,#216510,#216511,
#216512,#216513,#216514,#216515,#216516,#216517,#216518,#216519,#216520,
#216521,#216522,#216523,#216524,#216525,#216526,#216527,#216528,#216529,
#216530,#216531,#216532,#216533,#216534,#216535,#216536,#216537,#216538,
#216539,#216540,#216541,#216542,#216543,#216544,#216545,#216546,#216547,
#216548,#216549,#216550,#216551,#216552,#216553,#216554,#216555,#216556),
 .UNSPECIFIED.,.F.,.F.,(4,2,2,2,2,2,2,2,2,2,2,2,2,2,2,2,2,2,2,2,2,2,2,2,
2,2,2,2,2,2,2,2,2,2,2,2,2,4),(-21.8943047423385,-21.7758651347812,-21.5410515033964,
-21.4268285997185,-21.2030184270806,-20.9786575429375,-20.7625105893418,
-20.6478936288047,-20.3698911794026,-20.2550588086357,-19.9389522360808,
-19.8248572046001,-19.5625496742136,-19.3359762790518,-19.1730889945457,
-19.0582271151876,-18.829574401143,-18.6052712102383,-18.3485145033467,
-18.1199766319641,-18.0056172240497,-17.7816376834012,-17.5794451870502,
-17.3443875772851,-17.1711327726157,-17.0564223246057,-16.7285022822342,
-16.4973841529025,-16.2679629029584,-15.9218777080356,-15.8076985043827,
-15.5842721602659,-15.3593844814189,-15.1247284981361,-15.0104927267103,
-14.7865329091102,-14.5619722283021,-14.4469920765838),.UNSPECIFIED.);
#30562=B_SPLINE_CURVE_WITH_KNOTS('',3,(#216557,#216558,#216559,#216560,
#216561,#216562,#216563,#216564,#216565,#216566,#216567,#216568,#216569,
#216570,#216571,#216572,#216573,#216574,#216575,#216576,#216577,#216578,
#216579,#216580,#216581,#216582,#216583,#216584,#216585,#216586,#216587,
#216588,#216589,#216590,#216591,#216592,#216593,#216594,#216595,#216596,
#216597,#216598,#216599,#216600,#216601,#216602,#216603,#216604,#216605,
#216606,#216607,#216608,#216609,#216610,#216611,#216612,#216613,#216614,
#216615,#216616,#216617,#216618,#216619,#216620,#216621,#216622,#216623,
#216624,#216625,#216626,#216627,#216628,#216629,#216630,#216631,#216632,
#216633,#216634),.UNSPECIFIED.,.F.,.F.,(4,2,2,2,2,2,2,2,2,2,2,2,2,2,2,2,
2,2,2,2,2,2,2,2,2,2,2,2,2,2,2,2,2,2,2,2,2,2,4),(-10.22845558376,-10.1158401265768,
-9.89115177753051,-9.66761368388471,-9.55338621355086,-9.23692071620921,
-9.122370932652,-8.88771372650107,-8.66369006558576,-8.54886806983543,-8.3206913669332,
-8.05897886871758,-7.94483082538692,-7.62945980835995,-7.51499320151402,
-7.23290372901667,-7.11853656580412,-6.855130090617,-6.74109476064902,-6.41878779605464,
-6.30405435983148,-6.13915860379677,-5.90440188687171,-5.74427454092565,
-5.51714392881869,-5.26655270450146,-5.04193707803073,-4.81349746352477,
-4.6984382894124,-4.53524967574988,-4.30883411100736,-4.0454369895731,-3.93119365547195,
-3.69615849635357,-3.47178830981662,-3.24790775411328,-3.13367035284959,
-2.89883668306189,-2.78075214770189),.UNSPECIFIED.);
#30563=B_SPLINE_CURVE_WITH_KNOTS('',3,(#216640,#216641,#216642,#216643),
 .UNSPECIFIED.,.F.,.F.,(4,4),(-2.98098074791244E-6,-9.99999995798516E-7),
 .UNSPECIFIED.);
#30564=B_SPLINE_CURVE_WITH_KNOTS('',3,(#216645,#216646,#216647,#216648,
#216649,#216650,#216651,#216652,#216653,#216654,#216655,#216656,#216657,
#216658,#216659,#216660,#216661,#216662,#216663,#216664,#216665,#216666,
#216667,#216668),.UNSPECIFIED.,.F.,.F.,(4,2,2,2,2,2,2,2,2,2,2,4),(-1.88511749361157,
-1.67932546304624,-1.47452695338293,-1.33807794175079,-1.10356670932426,
-0.989276198914495,-0.873916728340471,-0.661501516222309,-0.498025259869575,
-0.252000037418745,-0.126229715199769,-0.000254800321387329),
 .UNSPECIFIED.);
#30565=B_SPLINE_CURVE_WITH_KNOTS('',3,(#216671,#216672,#216673,#216674,
#216675,#216676,#216677,#216678,#216679,#216680,#216681,#216682,#216683,
#216684,#216685,#216686,#216687,#216688,#216689,#216690,#216691,#216692),
 .UNSPECIFIED.,.F.,.F.,(4,2,2,2,2,2,2,2,2,2,4),(5.98718350673662E-5,0.203932709927782,
0.406516261468655,0.541488095383629,0.718522052217718,0.942619519328621,
1.17051888563091,1.39440958810066,1.63674335451055,1.76079483716829,1.88502497314799),
 .UNSPECIFIED.);
#30566=B_SPLINE_CURVE_WITH_KNOTS('',3,(#216695,#216696,#216697,#216698,
#216699,#216700,#216701,#216702,#216703,#216704,#216705,#216706,#216707,
#216708,#216709,#216710,#216711,#216712,#216713,#216714,#216715,#216716,
#216717,#216718,#216719,#216720,#216721,#216722,#216723,#216724,#216725,
#216726,#216727,#216728,#216729,#216730,#216731,#216732,#216733,#216734,
#216735,#216736,#216737,#216738,#216739,#216740,#216741,#216742,#216743,
#216744,#216745,#216746,#216747,#216748,#216749,#216750,#216751,#216752,
#216753,#216754,#216755,#216756,#216757,#216758,#216759,#216760,#216761,
#216762,#216763,#216764,#216765,#216766,#216767,#216768,#216769,#216770,
#216771,#216772),.UNSPECIFIED.,.F.,.F.,(4,2,2,2,2,2,2,2,2,2,2,2,2,2,2,2,
2,2,2,2,2,2,2,2,2,2,2,2,2,2,2,2,2,2,2,2,2,2,4),(-22.7887754871925,-22.5737853607563,
-22.3645912829662,-22.2250703698579,-21.9520105528446,-21.7234422036205,
-21.5344458228471,-21.4205033205513,-21.1505966646988,-20.9213671507031,
-20.8072028928257,-20.5830474551358,-20.3484175287191,-20.1186112362477,
-20.0045315383634,-19.7802237481903,-19.5457292550042,-19.315729471641,
-19.2017990774839,-18.9774229981112,-18.7428603593495,-18.5130776936426,
-18.3992883308069,-18.1749036431537,-17.9401751152226,-17.7108762627284,
-17.5971442416489,-17.3727928848634,-17.1391574499357,-16.9105229740035,
-16.79667802978,-16.5724458853296,-16.3394723212058,-16.111442940754,-15.9973964286305,
-15.7733306583291,-15.5380042916193,-15.4237362863445,-15.342147766727),
 .UNSPECIFIED.);
#30567=B_SPLINE_CURVE_WITH_KNOTS('',3,(#216775,#216776,#216777,#216778,
#216779,#216780,#216781,#216782,#216783,#216784,#216785,#216786,#216787,
#216788,#216789,#216790,#216791,#216792,#216793,#216794,#216795,#216796,
#216797,#216798,#216799,#216800,#216801,#216802,#216803,#216804,#216805,
#216806,#216807,#216808,#216809,#216810,#216811,#216812,#216813,#216814,
#216815,#216816,#216817,#216818,#216819,#216820,#216821,#216822,#216823,
#216824,#216825,#216826,#216827,#216828,#216829,#216830,#216831,#216832,
#216833,#216834,#216835,#216836,#216837,#216838,#216839,#216840,#216841,
#216842,#216843,#216844,#216845,#216846,#216847,#216848,#216849,#216850,
#216851,#216852),.UNSPECIFIED.,.F.,.F.,(4,2,2,2,2,2,2,2,2,2,2,2,2,2,2,2,
2,2,2,2,2,2,2,2,2,2,2,2,2,2,2,2,2,2,2,2,2,2,4),(-7.44718343892512,-7.36240446244989,
-7.24805819005065,-7.02308065474895,-6.79889962536361,-6.68521835702744,
-6.456593568243,-6.22151211684303,-5.9971659350046,-5.7732432646884,-5.65900294954311,
-5.42412826474149,-5.19948668701251,-4.97616348979199,-4.86194591875158,
-4.62722551562504,-4.40217320669064,-4.16739074652333,-4.0531419222947,
-3.81856601393786,-3.59383807002767,-3.36961197351575,-3.25544477485063,
-2.92967683372141,-2.81502248789315,-2.65144118011975,-2.423646930303,-2.14811559177375,
-2.03388722384771,-1.78699119824193,-1.56303399023159,-1.33478382184713,
-1.22030231366281,-0.942135255595247,-0.827820820338569,-0.584107166585578,
-0.439444762624892,-0.221298301331629,-2.98098074791244E-6),
 .UNSPECIFIED.);
#30568=B_SPLINE_CURVE_WITH_KNOTS('',3,(#216857,#216858,#216859,#216860,
#216861,#216862,#216863,#216864,#216865,#216866,#216867,#216868,#216869,
#216870,#216871,#216872,#216873,#216874,#216875,#216876,#216877,#216878,
#216879,#216880,#216881,#216882,#216883,#216884,#216885,#216886,#216887,
#216888,#216889,#216890,#216891,#216892,#216893,#216894,#216895,#216896,
#216897,#216898,#216899,#216900,#216901,#216902,#216903,#216904,#216905,
#216906,#216907,#216908,#216909,#216910,#216911,#216912,#216913,#216914,
#216915,#216916,#216917,#216918,#216919,#216920,#216921,#216922,#216923,
#216924,#216925,#216926,#216927,#216928,#216929,#216930,#216931,#216932,
#216933,#216934),.UNSPECIFIED.,.F.,.F.,(4,2,2,2,2,2,2,2,2,2,2,2,2,2,2,2,
2,2,2,2,2,2,2,2,2,2,2,2,2,2,2,2,2,2,2,2,2,2,4),(-14.8947554416205,-14.8555328238902,
-14.6255932266936,-14.5115483148371,-14.2871917339874,-14.0526532288194,
-13.8227502409632,-13.7088584582275,-13.4844700238339,-13.2568809816448,
-13.0280884043627,-12.9138754281338,-12.689658624793,-12.4904413403656,
-12.2654119085154,-12.0529319801525,-11.8248485904798,-11.6246180764855,
-11.3947343862561,-11.280540944454,-11.1009100249439,-10.8701321621013,
-10.6356115829466,-10.4108478312659,-10.186578073999,-10.0724663873352,
-9.73649474395671,-9.62156564200684,-9.41972195006705,-9.19568899880307,
-9.08133069845105,-8.85261827817306,-8.59523573549692,-8.37092206998091,
-8.14210122680411,-8.02723354700109,-7.86215740024421,-7.63576125229907,
-7.44718343892512),.UNSPECIFIED.);
#30569=B_SPLINE_CURVE_WITH_KNOTS('',3,(#216935,#216936,#216937,#216938,
#216939,#216940,#216941,#216942,#216943,#216944,#216945,#216946,#216947,
#216948,#216949,#216950,#216951,#216952,#216953,#216954,#216955,#216956,
#216957,#216958,#216959,#216960,#216961,#216962,#216963,#216964,#216965,
#216966,#216967,#216968,#216969,#216970,#216971,#216972,#216973,#216974,
#216975,#216976,#216977,#216978,#216979,#216980,#216981,#216982,#216983,
#216984,#216985,#216986,#216987,#216988,#216989,#216990,#216991,#216992,
#216993,#216994,#216995,#216996,#216997,#216998,#216999,#217000,#217001,
#217002,#217003,#217004,#217005,#217006,#217007,#217008,#217009,#217010,
#217011,#217012),.UNSPECIFIED.,.F.,.F.,(4,2,2,2,2,2,2,2,2,2,2,2,2,2,2,2,
2,2,2,2,2,2,2,2,2,2,2,2,2,2,2,2,2,2,2,2,2,2,4),(-15.342147766727,-15.1529720065065,
-15.0383703444976,-14.810809948066,-14.586751207086,-14.3429750891665,-14.1152058277465,
-13.9570672325687,-13.8424259697976,-13.6133621923892,-13.3892883641721,
-13.1714179393148,-13.0564020234404,-12.716404767469,-12.6023018240209,
-12.3781455868867,-12.1533575609804,-11.9188469906034,-11.6880294779991,
-11.509248903507,-11.3950609040316,-11.165177855366,-10.963986090416,-10.7359806575178,
-10.5257207831069,-10.3006120053153,-10.0657543218304,-9.9515117616543,
-9.71678726270671,-9.49192700742318,-9.26870398584334,-9.15450428638233,
-8.80897988487314,-8.69389321850089,-8.4777887626932,-8.25370904546708,
-8.02408547888485,-7.90947386498692,-7.89471088538268),.UNSPECIFIED.);
#30570=B_SPLINE_CURVE_WITH_KNOTS('',3,(#217017,#217018,#217019,#217020,
#217021,#217022,#217023,#217024,#217025,#217026,#217027,#217028,#217029,
#217030,#217031,#217032,#217033,#217034,#217035,#217036,#217037,#217038,
#217039,#217040,#217041,#217042,#217043,#217044,#217045,#217046,#217047,
#217048,#217049,#217050,#217051,#217052,#217053,#217054,#217055,#217056,
#217057,#217058,#217059,#217060,#217061,#217062,#217063,#217064,#217065,
#217066,#217067,#217068,#217069,#217070,#217071,#217072,#217073,#217074,
#217075,#217076,#217077,#217078,#217079,#217080,#217081,#217082,#217083,
#217084,#217085,#217086,#217087,#217088,#217089,#217090,#217091,#217092,
#217093,#217094),.UNSPECIFIED.,.F.,.F.,(4,2,2,2,2,2,2,2,2,2,2,2,2,2,2,2,
2,2,2,2,2,2,2,2,2,2,2,2,2,2,2,2,2,2,2,2,2,2,4),(-22.3420595105916,-22.3087706117589,
-22.1501209153067,-21.9431458113864,-21.7193635049408,-21.4944800880326,
-21.2599207185237,-21.1456978247876,-20.9213787890152,-20.6967842790541,
-20.4620796048301,-20.3477868290561,-20.1129279053258,-19.8881009482717,
-19.6532740453404,-19.5390667997237,-19.315609140037,-19.0911533599053,
-18.8561460335345,-18.741939321533,-18.5067222121917,-18.2821685233984,
-18.0715067743307,-17.9570526515047,-17.6559632223792,-17.5418483339653,
-17.2763985394528,-17.1618752207304,-16.9343481155266,-16.7103507009649,
-16.4662542480478,-16.2380547179748,-16.0388216827039,-15.924846808128,
-15.6580555001392,-15.4285045183689,-15.314337636522,-15.090086051584,-14.8947554416205),
 .UNSPECIFIED.);
#30571=B_SPLINE_CURVE_WITH_KNOTS('',3,(#217095,#217096,#217097,#217098,
#217099,#217100,#217101,#217102,#217103,#217104,#217105,#217106,#217107,
#217108,#217109,#217110,#217111,#217112,#217113,#217114,#217115,#217116,
#217117,#217118,#217119,#217120,#217121,#217122,#217123,#217124,#217125,
#217126,#217127,#217128,#217129,#217130,#217131,#217132,#217133,#217134,
#217135,#217136,#217137,#217138,#217139,#217140,#217141,#217142,#217143,
#217144,#217145,#217146,#217147,#217148,#217149,#217150,#217151,#217152,
#217153,#217154,#217155,#217156,#217157,#217158,#217159,#217160,#217161,
#217162,#217163,#217164,#217165,#217166,#217167,#217168,#217169,#217170,
#217171,#217172),.UNSPECIFIED.,.F.,.F.,(4,2,2,2,2,2,2,2,2,2,2,2,2,2,2,2,
2,2,2,2,2,2,2,2,2,2,2,2,2,2,2,2,2,2,2,2,2,2,4),(-7.89471088538268,-7.7513446470039,
-7.52274813975883,-7.27356060895527,-7.04945125083501,-6.82000660796923,
-6.70532977234191,-6.54058473742381,-6.3057493848618,-6.14534762068587,
-5.91799925641447,-5.66491089523042,-5.55102496010023,-5.3375198753743,
-5.11108617476756,-4.84273060467716,-4.72849634427378,-4.49323939229272,
-4.2691188750551,-4.15523017770918,-3.92691048583833,-3.69180245193583,
-3.46753946147414,-3.35373345582603,-3.12496264585747,-2.89005372862249,
-2.66571673663732,-2.55193417606568,-2.32261364211153,-2.08792618496844,
-1.8635724908039,-1.74971746957993,-1.51994827839982,-1.28540978867085,
-1.06107669190666,-0.947078264469952,-0.717152631942884,-0.482651609103955,
-0.448047571937242),.UNSPECIFIED.);
#30572=B_SPLINE_CURVE_WITH_KNOTS('',3,(#217180,#217181,#217182,#217183),
 .UNSPECIFIED.,.F.,.F.,(4,4),(0.,0.000776497203231734),.UNSPECIFIED.);
#30573=B_SPLINE_CURVE_WITH_KNOTS('',3,(#217185,#217186,#217187,#217188,
#217189,#217190,#217191,#217192,#217193,#217194,#217195,#217196,#217197,
#217198,#217199,#217200,#217201,#217202,#217203,#217204,#217205,#217206,
#217207,#217208,#217209,#217210,#217211,#217212,#217213,#217214),
 .UNSPECIFIED.,.F.,.F.,(4,2,2,2,2,2,2,2,2,2,2,2,2,2,4),(-2.58819132413352,
-2.3627357246396,-2.13741551586203,-1.98563553180878,-1.79408322231036,
-1.60046605723288,-1.40804760753431,-1.31130466449952,-1.11849752052538,
-0.921488213499259,-0.727078362402504,-0.545763875761456,-0.273849840655846,
-0.136429802224194,-1.19577251124937E-5),.UNSPECIFIED.);
#30574=B_SPLINE_CURVE_WITH_KNOTS('',3,(#217216,#217217,#217218,#217219,
#217220,#217221,#217222,#217223,#217224,#217225,#217226,#217227,#217228,
#217229,#217230,#217231,#217232,#217233,#217234,#217235,#217236,#217237,
#217238,#217239,#217240,#217241,#217242,#217243,#217244,#217245,#217246,
#217247,#217248,#217249),.UNSPECIFIED.,.F.,.F.,(4,2,2,2,2,2,2,2,2,2,2,2,
2,2,2,2,4),(-2.54573725986498,-2.37476608201507,-2.20211346081785,-2.08770172421587,
-1.93349297075605,-1.75019087472256,-1.56693226938244,-1.47443768915228,
-1.29039242591535,-1.19762811175894,-1.01304591077278,-0.825229741583214,
-0.638712708813142,-0.47916634693947,-0.24037936089956,-0.119773973838393,
-2.99430650417543E-6),.UNSPECIFIED.);
#30575=B_SPLINE_CURVE_WITH_KNOTS('',3,(#217252,#217253,#217254,#217255,
#217256,#217257,#217258,#217259,#217260,#217261,#217262,#217263,#217264,
#217265,#217266,#217267,#217268,#217269,#217270,#217271,#217272,#217273,
#217274,#217275,#217276,#217277,#217278,#217279,#217280,#217281,#217282,
#217283,#217284,#217285,#217286,#217287,#217288),.UNSPECIFIED.,.F.,.F.,
(4,3,3,3,3,3,3,3,3,3,3,3,4),(0.,0.0940528831804161,0.188071722346358,0.282046558286538,
0.375986938964542,0.469884151166454,0.5,0.593548460116691,0.686978341973026,
0.780242306988025,0.873402721160576,0.966421835499172,0.999999946312436),
 .UNSPECIFIED.);
#30576=B_SPLINE_CURVE_WITH_KNOTS('',3,(#217291,#217292,#217293,#217294,
#217295,#217296,#217297,#217298,#217299,#217300,#217301,#217302),
 .UNSPECIFIED.,.F.,.F.,(4,2,2,2,2,4),(1.41602269427444E-5,0.103268302452876,
0.209393167485349,0.424646829433195,0.5311273537776,0.948508841723998),
 .UNSPECIFIED.);
#30577=B_SPLINE_CURVE_WITH_KNOTS('',3,(#217311,#217312,#217313,#217314,
#217315,#217316,#217317,#217318),.UNSPECIFIED.,.F.,.F.,(4,2,2,4),(-0.448047571937242,
-0.24397532728341,-0.122603630859418,-0.000536776025982476),
 .UNSPECIFIED.);
#30578=B_SPLINE_CURVE_WITH_KNOTS('',3,(#217319,#217320,#217321,#217322,
#217323,#217324,#217325,#217326),.UNSPECIFIED.,.F.,.F.,(4,2,2,4),(-22.7895799823983,
-22.6678389417462,-22.5467817476268,-22.3420595105916),.UNSPECIFIED.);
#30579=B_SPLINE_CURVE_WITH_KNOTS('',3,(#217329,#217330,#217331,#217332,
#217333,#217334,#217335,#217336,#217337,#217338,#217339,#217340,#217341,
#217342,#217343,#217344,#217345,#217346,#217347,#217348,#217349,#217350,
#217351,#217352,#217353,#217354,#217355,#217356,#217357,#217358,#217359,
#217360),.UNSPECIFIED.,.F.,.F.,(4,2,2,2,2,2,2,2,2,2,2,2,2,2,2,4),(-2.78075214770189,
-2.67416520655263,-2.45088006356431,-2.33666972312661,-2.10198688626357,
-1.87689522479149,-1.64214565828053,-1.52791483266349,-1.29337178707801,
-1.06862921741881,-0.844459861678536,-0.739641881971006,-0.55627135957414,
-0.278570352687516,-0.140184550502981,-0.000333910314163745),
 .UNSPECIFIED.);
#30580=B_SPLINE_CURVE_WITH_KNOTS('',3,(#217363,#217364,#217365,#217366,
#217367,#217368,#217369,#217370,#217371,#217372,#217373,#217374,#217375,
#217376,#217377,#217378,#217379,#217380,#217381,#217382,#217383,#217384,
#217385,#217386,#217387,#217388,#217389,#217390,#217391,#217392,#217393,
#217394),.UNSPECIFIED.,.F.,.F.,(4,2,2,2,2,2,2,2,2,2,2,2,2,2,2,4),(-24.6745311376285,
-24.5346323571423,-24.3961991428265,-24.1183826232944,-23.9348941546191,
-23.8300338079026,-23.6059502628919,-23.3811973449391,-23.146667341407,
-23.0324471264885,-22.7977120868547,-22.5726065945869,-22.3379394752642,
-22.22374090337,-22.0005377731445,-21.8943047423385),.UNSPECIFIED.);
#30581=B_SPLINE_CURVE_WITH_KNOTS('',3,(#217398,#217399,#217400,#217401,
#217402,#217403,#217404,#217405,#217406,#217407,#217408),.UNSPECIFIED.,
 .F.,.F.,(4,2,3,2,4),(-0.707920522022895,-0.389439958817396,0.,0.389439958817396,
0.707920522023277),.UNSPECIFIED.);
#30582=B_SPLINE_CURVE_WITH_KNOTS('',3,(#217412,#217413,#217414,#217415,
#217416,#217417,#217418,#217419,#217420,#217421,#217422),.UNSPECIFIED.,
 .F.,.F.,(4,2,3,2,4),(-0.704072833963995,-0.391088299603276,0.,0.390169294707907,
0.573011129927049),.UNSPECIFIED.);
#30583=B_SPLINE_CURVE_WITH_KNOTS('',3,(#217424,#217425,#217426,#217427),
 .UNSPECIFIED.,.F.,.F.,(4,4),(0.573011129927049,0.704038599815),
 .UNSPECIFIED.);
#30584=B_SPLINE_CURVE_WITH_KNOTS('',3,(#217433,#217434,#217435,#217436,
#217437,#217438,#217439,#217440,#217441,#217442,#217443,#217444,#217445,
#217446,#217447,#217448,#217449,#217450,#217451,#217452,#217453,#217454,
#217455,#217456,#217457,#217458,#217459,#217460,#217461,#217462,#217463,
#217464,#217465,#217466,#217467,#217468),.UNSPECIFIED.,.F.,.F.,(4,2,2,2,
2,2,2,2,2,2,2,2,2,2,2,2,2,4),(-2.69278601163302,-2.48949828256942,-2.2822953333751,
-2.14458879630419,-1.96754811547026,-1.79103983134041,-1.61387421528028,
-1.4368871200193,-1.34835665174934,-1.25978242304794,-1.08286142569904,
-0.905901114537669,-0.728942624524571,-0.640388431951228,-0.480377748963507,
-0.24014543853639,-0.120091889663099,-0.000154281167704561),
 .UNSPECIFIED.);
#30585=B_SPLINE_CURVE_WITH_KNOTS('',3,(#217469,#217470,#217471,#217472,
#217473,#217474,#217475,#217476,#217477,#217478,#217479,#217480,#217481,
#217482,#217483,#217484,#217485,#217486,#217487,#217488,#217489,#217490,
#217491,#217492,#217493,#217494,#217495,#217496,#217497,#217498,#217499,
#217500),.UNSPECIFIED.,.F.,.F.,(4,2,2,2,2,2,2,2,2,2,2,2,2,2,2,4),(-2.46530051632309,
-2.26819680103626,-2.07119546180983,-1.93999090652251,-1.76308472874,-1.58642929791097,
-1.40948483540438,-1.23270430940226,-1.05614800855202,-0.879169642199461,
-0.702326874356245,-0.525413854334426,-0.394197725784808,-0.197144745652885,
-0.0986007555144971,-0.000263540357241407),.UNSPECIFIED.);
#30586=B_SPLINE_CURVE_WITH_KNOTS('',3,(#217502,#217503,#217504,#217505,
#217506,#217507,#217508,#217509,#217510,#217511,#217512,#217513,#217514,
#217515,#217516,#217517,#217518,#217519,#217520,#217521,#217522,#217523,
#217524,#217525),.UNSPECIFIED.,.F.,.F.,(4,2,2,2,2,2,2,2,2,2,2,4),(0.000318649964459465,
0.216450635165624,0.43221115121817,0.575746846605652,0.931054759121386,
1.28597766699898,1.46245055330704,1.63929983860731,1.81580252156612,1.97755622729653,
2.22237862591288,2.46755233424745),.UNSPECIFIED.);
#30587=B_SPLINE_CURVE_WITH_KNOTS('',3,(#217526,#217527,#217528,#217529,
#217530,#217531,#217532,#217533,#217534,#217535,#217536,#217537,#217538,
#217539,#217540,#217541,#217542,#217543,#217544,#217545,#217546,#217547,
#217548,#217549,#217550,#217551,#217552,#217553,#217554,#217555,#217556,
#217557,#217558,#217559),.UNSPECIFIED.,.F.,.F.,(4,2,2,2,2,2,2,2,2,2,2,2,
2,2,2,2,4),(0.000172246164355015,0.137421045642985,0.274393819056073,0.548014470689402,
0.723404022606042,0.900115325731667,1.07657549560485,1.25300012233027,1.43023293239451,
1.78627993866689,1.87475807665471,2.05193119898048,2.14050616753244,2.31698447474687,
2.58688835542286,2.72343276379947,2.8600131789018),.UNSPECIFIED.);
#30588=B_SPLINE_CURVE_WITH_KNOTS('',3,(#217562,#217563,#217564,#217565,
#217566,#217567,#217568,#217569,#217570,#217571,#217572,#217573,#217574,
#217575,#217576,#217577,#217578,#217579,#217580,#217581,#217582,#217583,
#217584,#217585,#217586,#217587,#217588,#217589,#217590,#217591),
 .UNSPECIFIED.,.F.,.F.,(4,2,2,2,2,2,2,2,2,2,2,2,2,2,4),(-2.86193028654911,
-2.80997689806081,-2.53859155289255,-2.45079675084397,-2.1519918870356,
-1.79660795427829,-1.62313020729879,-1.45278636887481,-1.28271379788856,
-1.12400310249263,-0.967139554823996,-0.815414409998087,-0.636542489421722,
-0.323024007865446,-9.999999992516E-7),.UNSPECIFIED.);
#30589=B_SPLINE_CURVE_WITH_KNOTS('',3,(#217592,#217593,#217594,#217595,
#217596,#217597,#217598,#217599,#217600,#217601,#217602,#217603,#217604,
#217605,#217606,#217607,#217608,#217609,#217610,#217611,#217612,#217613,
#217614,#217615),.UNSPECIFIED.,.F.,.F.,(4,2,2,2,2,2,2,2,2,2,2,4),(-2.07371028242565,
-1.89670800614931,-1.71936907413992,-1.6040015767827,-1.44968076011158,
-1.09401343727901,-0.738422468249123,-0.650645318605829,-0.498854971265117,
-0.251161099398345,-0.127294929695514,-0.000361776623968905),
 .UNSPECIFIED.);
#30590=B_SPLINE_CURVE_WITH_KNOTS('',3,(#217617,#217618,#217619,#217620,
#217621,#217622,#217623,#217624,#217625,#217626,#217627,#217628,#217629,
#217630,#217631,#217632,#217633,#217634,#217635,#217636,#217637,#217638,
#217639,#217640,#217641,#217642),.UNSPECIFIED.,.F.,.F.,(4,2,2,2,2,2,2,2,
2,2,2,2,4),(0.000219774119996971,0.128265976878325,0.255769893159544,0.493856419136537,
0.651486942309664,0.821726852996873,1.03589976718783,1.25551703969422,1.3939988560134,
1.57317372451587,1.82118610863373,1.94515901785584,2.07223113354457),
 .UNSPECIFIED.);
#30591=B_SPLINE_CURVE_WITH_KNOTS('',3,(#217643,#217644,#217645,#217646,
#217647,#217648,#217649,#217650,#217651,#217652,#217653,#217654,#217655,
#217656,#217657,#217658,#217659,#217660,#217661,#217662,#217663,#217664,
#217665,#217666,#217667,#217668,#217669,#217670,#217671,#217672),
 .UNSPECIFIED.,.F.,.F.,(4,2,2,2,2,2,2,2,2,2,2,2,2,2,4),(-20.0257156012565,
-19.7027546279237,-19.3893986009445,-19.210538838357,-19.0591308279729,
-18.9074787091117,-18.7457793362987,-18.5752767544231,-18.404751196263,
-18.2310130985394,-17.8756055227173,-17.573445592098,-17.4857146330988,
-17.2174499967721,-17.1637028159425),.UNSPECIFIED.);
#30592=B_SPLINE_CURVE_WITH_KNOTS('',3,(#217675,#217676,#217677,#217678,
#217679,#217680,#217681,#217682,#217683,#217684,#217685,#217686,#217687,
#217688,#217689,#217690,#217691,#217692,#217693,#217694,#217695,#217696,
#217697,#217698,#217699,#217700,#217701,#217702,#217703,#217704,#217705,
#217706,#217707,#217708),.UNSPECIFIED.,.F.,.F.,(4,2,2,2,2,2,2,2,2,2,2,2,
2,2,2,2,4),(-2.86068452297866,-2.77773294211803,-2.63630062493424,-2.44865158052864,
-2.18043666205413,-1.82474834886011,-1.65128159569772,-1.4809693172972,
-1.31094241874573,-1.14993202613478,-0.990511201393968,-0.838687969453853,
-0.65849182006884,-0.576298702112474,-0.435211787338084,-0.287957514444663,
-9.99999996587064E-7),.UNSPECIFIED.);
#30593=B_SPLINE_CURVE_WITH_KNOTS('',3,(#217710,#217711,#217712,#217713,
#217714,#217715,#217716,#217717,#217718,#217719,#217720,#217721,#217722,
#217723,#217724,#217725,#217726,#217727,#217728,#217729,#217730,#217731),
 .UNSPECIFIED.,.F.,.F.,(4,2,2,2,2,2,2,2,2,2,4),(-1.678391897345,-1.54864602532634,
-1.419721708183,-1.17041427886277,-1.02310064103662,-0.854629816400835,
-0.705938572535618,-0.530158421676784,-0.264651666630037,-0.134283710524161,
-0.000635529299139109),.UNSPECIFIED.);
#30594=B_SPLINE_CURVE_WITH_KNOTS('',3,(#217733,#217734,#217735,#217736),
 .UNSPECIFIED.,.F.,.F.,(4,4),(0.,1.),.UNSPECIFIED.);
#30595=B_SPLINE_CURVE_WITH_KNOTS('',3,(#217738,#217739,#217740,#217741,
#217742,#217743,#217744,#217745,#217746,#217747,#217748,#217749,#217750,
#217751,#217752,#217753,#217754,#217755,#217756,#217757,#217758,#217759),
 .UNSPECIFIED.,.F.,.F.,(4,2,2,2,2,2,2,2,2,2,4),(0.000147978863462259,0.132665880132235,
0.264039836401641,0.521001553758146,0.701578774182686,0.838995874465286,
1.11207159352395,1.25225787136096,1.4596258412934,1.56800447107715,1.67810387044742),
 .UNSPECIFIED.);
#30596=B_SPLINE_CURVE_WITH_KNOTS('',3,(#217760,#217761,#217762,#217763,
#217764,#217765,#217766,#217767,#217768,#217769,#217770,#217771,#217772,
#217773,#217774,#217775,#217776,#217777,#217778,#217779,#217780,#217781,
#217782,#217783,#217784,#217785,#217786,#217787,#217788,#217789,#217790,
#217791,#217792,#217793),.UNSPECIFIED.,.F.,.F.,(4,2,2,2,2,2,2,2,2,2,2,2,
2,2,2,2,4),(-20.0226821886523,-19.730263650116,-19.5909631962108,-19.4511634053081,
-19.3697072643866,-19.2822426050699,-19.1116277510905,-18.8907000615668,
-18.7210061060888,-18.5495596781661,-18.3786443708691,-18.2043541297755,
-17.8487913077471,-17.5467363732741,-17.3992244973413,-17.252074015242,
-17.1619514598514),.UNSPECIFIED.);
#30597=B_SPLINE_CURVE_WITH_KNOTS('',3,(#217823,#217824,#217825,#217826,
#217827,#217828,#217829,#217830,#217831,#217832,#217833,#217834,#217835,
#217836,#217837,#217838,#217839,#217840,#217841),.UNSPECIFIED.,.F.,.F.,
(4,3,3,3,3,3,4),(3.59311864544389E-15,0.188384660190751,0.240000922766575,
0.50000123041085,0.760001538055125,0.945884007472818,0.999999610267735),
 .UNSPECIFIED.);
#30598=B_SPLINE_CURVE_WITH_KNOTS('',3,(#217844,#217845,#217846,#217847,
#217848,#217849,#217850,#217851,#217852,#217853,#217854,#217855,#217856,
#217857),.UNSPECIFIED.,.F.,.F.,(4,2,2,2,2,2,4),(0.000337787465768249,0.284976578385984,
0.575874331198088,0.935643861114886,1.30221214423596,1.60875324692279,1.91914645332376),
 .UNSPECIFIED.);
#30599=B_SPLINE_CURVE_WITH_KNOTS('',3,(#218128,#218129,#218130,#218131,
#218132,#218133,#218134,#218135,#218136,#218137,#218138,#218139,#218140,
#218141,#218142,#218143,#218144,#218145,#218146,#218147,#218148,#218149,
#218150,#218151,#218152,#218153,#218154,#218155,#218156,#218157,#218158,
#218159,#218160,#218161,#218162,#218163,#218164,#218165),.UNSPECIFIED.,
 .F.,.F.,(4,2,2,2,2,2,2,2,2,2,2,2,2,2,2,2,2,2,4),(-25.3607679059522,-25.2146555775584,
-25.0721549022585,-24.7878117742293,-24.6209012665101,-24.4665570964828,
-24.2750293060982,-24.0854606330825,-23.8884468545564,-23.5513161309177,
-23.3484860585261,-23.1459344345172,-22.9908242973992,-22.8913313630438,
-22.4856788944898,-22.1092331654096,-21.9066557467446,-21.7038929328105,
-21.6906362475869),.UNSPECIFIED.);
#30600=B_SPLINE_CURVE_WITH_KNOTS('',3,(#218435,#218436,#218437,#218438,
#218439,#218440),.UNSPECIFIED.,.F.,.F.,(4,2,4),(1.30310740493471E-6,0.0653973299358593,
0.130262396001019),.UNSPECIFIED.);
#30601=B_SPLINE_CURVE_WITH_KNOTS('',3,(#218469,#218470,#218471,#218472,
#218473,#218474),.UNSPECIFIED.,.F.,.F.,(4,2,4),(-0.0180566566914932,-0.00903372775810624,
-8.36277994474979E-7),.UNSPECIFIED.);
#30602=B_SPLINE_CURVE_WITH_KNOTS('',3,(#218476,#218477,#218478,#218479,
#218480,#218481),.UNSPECIFIED.,.F.,.F.,(4,2,4),(-0.0180610510695405,-0.0090326996689314,
-5.26550411017056E-6),.UNSPECIFIED.);
#30603=B_SPLINE_CURVE_WITH_KNOTS('',3,(#218510,#218511,#218512,#218513,
#218514,#218515),.UNSPECIFIED.,.F.,.F.,(4,2,4),(0.000679919885625248,0.0656077246252304,
0.130948216318226),.UNSPECIFIED.);
#30604=B_SPLINE_CURVE_WITH_KNOTS('',3,(#219130,#219131,#219132,#219133,
#219134,#219135),.UNSPECIFIED.,.F.,.F.,(4,2,4),(1.37679441807117E-6,0.132788624167673,
0.261946710422657),.UNSPECIFIED.);
#30605=B_SPLINE_CURVE_WITH_KNOTS('',3,(#219136,#219137,#219138,#219139,
#219140,#219141),.UNSPECIFIED.,.F.,.F.,(4,2,4),(9.69834487247414E-6,0.0602748062236532,
0.119740503039193),.UNSPECIFIED.);
#30606=B_SPLINE_CURVE_WITH_KNOTS('',3,(#219154,#219155,#219156,#219157,
#219158,#219159,#219160,#219161,#219162,#219163),.UNSPECIFIED.,.F.,.F.,
(4,2,2,2,4),(2.4605588906763,2.77696986044635,3.16672845187631,3.55648704330627,
3.87289801307633),.UNSPECIFIED.);
#30607=B_SPLINE_CURVE_WITH_KNOTS('',3,(#219165,#219166,#219167,#219168,
#219169,#219170),.UNSPECIFIED.,.F.,.F.,(4,2,4),(3.76834231800082E-5,0.277014521395569,
0.555926380959157),.UNSPECIFIED.);
#30608=B_SPLINE_CURVE_WITH_KNOTS('',3,(#219200,#219201,#219202,#219203,
#219204,#219205,#219206,#219207,#219208,#219209,#219210,#219211,#219212,
#219213,#219214,#219215,#219216,#219217,#219218),.UNSPECIFIED.,.F.,.F.,
(4,3,3,3,3,3,4),(0.,0.176916349798396,0.240000637218418,0.500000956530085,
0.760001275841753,0.935051760841337,0.999999692665191),.UNSPECIFIED.);
#30609=B_SPLINE_CURVE_WITH_KNOTS('',3,(#219221,#219222,#219223,#219224,
#219225,#219226,#219227,#219228,#219229,#219230,#219231,#219232,#219233,
#219234),.UNSPECIFIED.,.F.,.F.,(4,2,2,2,2,2,4),(0.000167093672000697,0.369844031545414,
0.745935182508726,1.21004916822793,1.6809812805178,2.07272751301291,2.46807904564772),
 .UNSPECIFIED.);
#30610=B_SPLINE_CURVE_WITH_KNOTS('',3,(#219376,#219377,#219378,#219379,
#219380,#219381,#219382,#219383,#219384,#219385,#219386,#219387,#219388,
#219389,#219390,#219391,#219392,#219393,#219394,#219395,#219396,#219397,
#219398,#219399,#219400,#219401,#219402,#219403,#219404,#219405,#219406,
#219407,#219408,#219409,#219410,#219411,#219412,#219413,#219414,#219415,
#219416,#219417,#219418,#219419,#219420,#219421,#219422,#219423,#219424,
#219425,#219426,#219427,#219428,#219429,#219430,#219431,#219432,#219433,
#219434,#219435,#219436,#219437,#219438,#219439,#219440,#219441,#219442,
#219443,#219444,#219445,#219446,#219447,#219448,#219449,#219450,#219451,
#219452,#219453,#219454,#219455,#219456,#219457,#219458,#219459,#219460,
#219461,#219462,#219463,#219464,#219465,#219466,#219467,#219468,#219469,
#219470,#219471,#219472,#219473,#219474,#219475,#219476,#219477,#219478,
#219479,#219480,#219481,#219482,#219483,#219484,#219485,#219486,#219487,
#219488,#219489,#219490,#219491,#219492,#219493,#219494,#219495,#219496,
#219497,#219498,#219499,#219500,#219501,#219502,#219503,#219504,#219505,
#219506,#219507,#219508,#219509,#219510,#219511,#219512,#219513,#219514,
#219515,#219516,#219517,#219518,#219519,#219520,#219521,#219522,#219523,
#219524,#219525,#219526,#219527,#219528,#219529,#219530,#219531,#219532,
#219533,#219534,#219535,#219536,#219537,#219538,#219539,#219540,#219541,
#219542,#219543,#219544,#219545,#219546,#219547,#219548,#219549,#219550,
#219551,#219552,#219553,#219554,#219555,#219556,#219557,#219558,#219559,
#219560,#219561,#219562,#219563,#219564,#219565,#219566,#219567,#219568,
#219569,#219570,#219571,#219572,#219573,#219574,#219575,#219576,#219577,
#219578,#219579),.UNSPECIFIED.,.F.,.F.,(4,2,2,2,2,2,2,2,2,2,2,2,2,2,2,2,
2,2,2,2,2,2,2,2,2,2,2,2,2,2,2,2,2,2,2,2,2,2,2,2,2,2,2,2,2,2,2,2,2,2,2,2,
2,2,2,2,2,2,2,2,2,2,2,2,2,2,2,2,2,2,2,2,2,2,2,2,2,2,2,2,2,2,2,2,2,2,2,2,
2,2,2,2,2,2,2,2,2,2,2,2,2,4),(0.00107990836000404,0.0329071535296479,0.195893327983235,
0.355153899134427,0.434988215969284,0.642816515067203,0.737569286405069,
0.908716883287997,0.993153014806632,1.18963661554878,1.28754502541362,1.47339633011078,
1.55811137762964,1.76173951289927,1.85370473309428,2.02895304676804,2.11938121712701,
2.33665348572374,2.42297287419884,2.59661267513458,2.68840363105108,2.90216045958087,
2.987118381251,3.17342429417755,3.26349749411226,3.45824610590557,3.54619696540934,
3.73710767122859,3.83188019089672,4.03301640796955,4.11747646294057,4.30305199952714,
4.40238831720826,4.60868154567945,4.68987410554116,4.87477538213013,4.97656143376426,
5.17614663866258,5.25912879790943,5.44612356943043,5.55060337155454,5.74202887918956,
5.82728553459735,6.01648422346557,6.12403067700903,6.30698556123304,6.3948612127417,
6.59463365103844,6.70174065635423,6.86827502115102,6.95722664984312,7.16281963653449,
7.27369262138387,7.43009961028706,7.52201238463309,7.70970084887526,7.83380812634278,
7.98940531561225,8.08401417045588,8.26759687618598,8.40024551773955,8.54235988021463,
8.63766384385343,8.81511758111811,9.02203998489799,9.12411504919588,9.27578319513838,
9.43003056692406,9.6064767882247,9.70887427561559,9.85136721119973,10.0286666142249,
10.1832040085792,10.2906557513719,10.4409835696911,10.7071639943014,10.8497640573907,
11.0174209505587,11.3437940692132,11.4716454362162,11.6108663252812,11.9469480845909,
12.0272146927954,12.2685798563405,12.5116906256741,12.6535479256158,12.8550753169041,
13.2724871383448,13.4494739492565,13.619028692563,13.8159480124215,14.1806924721594,
14.3608390254965,14.4645640031877,14.7164986862713,14.8965371123671,15.2222169253479,
15.3963408756932,15.575785343045,15.9915006951352,16.2407971147128,16.4907160008511),
 .UNSPECIFIED.);
#30611=B_SPLINE_CURVE_WITH_KNOTS('',3,(#219581,#219582,#219583,#219584,
#219585,#219586,#219587,#219588,#219589,#219590,#219591,#219592,#219593,
#219594,#219595,#219596,#219597,#219598,#219599,#219600,#219601,#219602,
#219603,#219604,#219605,#219606,#219607,#219608,#219609,#219610,#219611,
#219612,#219613,#219614,#219615,#219616,#219617,#219618,#219619,#219620,
#219621,#219622,#219623,#219624,#219625,#219626,#219627,#219628,#219629,
#219630,#219631,#219632,#219633,#219634,#219635,#219636,#219637,#219638,
#219639,#219640,#219641,#219642,#219643,#219644,#219645,#219646,#219647,
#219648,#219649,#219650,#219651,#219652,#219653,#219654,#219655,#219656,
#219657,#219658,#219659,#219660,#219661,#219662,#219663,#219664,#219665),
 .UNSPECIFIED.,.F.,.F.,(4,3,3,3,3,3,3,3,3,3,3,3,3,3,3,3,3,3,3,3,3,3,3,3,
3,3,3,3,4),(0.,0.0475523396469734,0.0945933459100679,0.141741666700758,
0.188796087897991,0.23670174521744,0.246392852642554,0.25047433411042,0.297627468238015,
0.344829936037007,0.380418717175787,0.427580266675554,0.474808467309134,
0.496867832745316,0.502907306312494,0.549192807169434,0.595728951526263,
0.642323912157344,0.688682512690019,0.723451463089525,0.738537131197933,
0.747378842105526,0.752846656127323,0.801913022967692,0.827758314288042,
0.876702333074787,0.92583430503612,0.974954869279015,0.999217082393009),
 .UNSPECIFIED.);
#30612=B_SPLINE_CURVE_WITH_KNOTS('',3,(#219667,#219668,#219669,#219670),
 .UNSPECIFIED.,.F.,.F.,(4,4),(-0.000244606540982073,0.),.UNSPECIFIED.);
#30613=B_SPLINE_CURVE_WITH_KNOTS('',3,(#219671,#219672,#219673,#219674,
#219675,#219676,#219677,#219678,#219679,#219680,#219681,#219682,#219683,
#219684,#219685,#219686,#219687,#219688,#219689,#219690,#219691,#219692,
#219693,#219694,#219695,#219696,#219697,#219698,#219699,#219700,#219701,
#219702,#219703,#219704,#219705,#219706,#219707,#219708,#219709,#219710,
#219711,#219712,#219713,#219714,#219715,#219716,#219717,#219718,#219719,
#219720,#219721,#219722,#219723,#219724,#219725,#219726,#219727,#219728,
#219729,#219730,#219731,#219732,#219733,#219734,#219735,#219736,#219737,
#219738,#219739,#219740,#219741,#219742,#219743,#219744,#219745,#219746,
#219747,#219748,#219749,#219750,#219751,#219752,#219753,#219754,#219755,
#219756,#219757,#219758,#219759,#219760,#219761,#219762,#219763,#219764,
#219765,#219766,#219767,#219768,#219769,#219770,#219771,#219772,#219773,
#219774,#219775,#219776,#219777,#219778,#219779,#219780,#219781,#219782,
#219783,#219784,#219785,#219786,#219787,#219788,#219789,#219790,#219791,
#219792,#219793,#219794,#219795,#219796,#219797,#219798,#219799,#219800,
#219801,#219802,#219803,#219804,#219805,#219806,#219807,#219808,#219809,
#219810,#219811,#219812,#219813,#219814,#219815,#219816,#219817,#219818,
#219819,#219820,#219821,#219822,#219823,#219824,#219825,#219826,#219827,
#219828,#219829,#219830,#219831,#219832,#219833,#219834,#219835,#219836,
#219837,#219838,#219839,#219840,#219841,#219842,#219843,#219844,#219845,
#219846,#219847,#219848),.UNSPECIFIED.,.F.,.F.,(4,2,2,2,2,2,2,2,2,2,2,2,
2,2,2,2,2,2,2,2,2,2,2,2,2,2,2,2,2,2,2,2,2,2,2,2,2,2,2,2,2,2,2,2,2,2,2,2,
2,2,2,2,2,2,2,2,2,2,2,2,2,2,2,2,2,2,2,2,2,2,2,2,2,2,2,2,2,2,2,2,2,2,2,2,
2,2,2,2,4),(-17.8874346102476,-17.5294919404532,-17.186048243388,-16.9295394700842,
-16.809249288478,-16.1896824712227,-15.8340272537738,-15.2083864406208,
-14.9204681110229,-14.3899595900006,-14.1556344483798,-13.9783598065547,
-13.7492496006877,-13.5994074639487,-13.4666029322114,-13.366607942251,
-13.1542141543599,-12.9906873702076,-12.8875365109189,-12.735910683424,
-12.5879560880447,-12.4262389066032,-12.3252101181408,-12.1497599740358,
-12.0316602778982,-11.8443326767789,-11.7509492083987,-11.5889580966796,
-11.4836693199074,-11.2966545630751,-11.1924870275934,-11.0521608685493,
-10.9450814860021,-10.7612433258151,-10.6366324077902,-10.486559685584,
-10.3465040629413,-10.1283588143423,-10.018252455382,-9.89616481200024,
-9.58905421181,-9.07549190175552,-8.68076130992365,-8.46605691770783,-8.01018323269793,
-7.62107621005051,-7.24137219646125,-6.65939456134288,-6.42566825697358,
-6.19571944233163,-5.93321022343852,-5.81507259106976,-5.63942976266636,
-5.45310433687737,-5.26007640926833,-5.15380952307374,-5.03637349809843,
-4.82334403415963,-4.68443024677056,-4.54527121635446,-4.41726995679759,
-4.2451953431367,-4.13877004673389,-4.00127907200663,-3.88561719143933,
-3.73605126423849,-3.64032051174758,-3.46696552173283,-3.36568283466282,
-3.21304464574176,-3.10894067512282,-2.9301644852829,-2.83463383875695,
-2.67405588965988,-2.53885135281524,-2.39350009266555,-2.2994834121668,
-2.13842813199059,-1.95939869233589,-1.8284100896886,-1.69294839797854,
-1.55186298560815,-1.33346072701374,-1.18729433138974,-0.99438201782296,
-0.767650200561418,-0.680987224727819,-0.341206102852197,-0.000193437912458331),
 .UNSPECIFIED.);
#30614=B_SPLINE_CURVE_WITH_KNOTS('',3,(#220118,#220119,#220120,#220121,
#220122,#220123),.UNSPECIFIED.,.F.,.F.,(4,2,4),(-0.1310037054835,-0.0656099052540244,
-3.86587579881701E-6),.UNSPECIFIED.);
#30615=B_SPLINE_CURVE_WITH_KNOTS('',3,(#220125,#220126,#220127,#220128,
#220129,#220130,#220131,#220132,#220133,#220134,#220135,#220136,#220137,
#220138,#220139,#220140,#220141,#220142,#220143,#220144,#220145,#220146,
#220147,#220148,#220149,#220150,#220151,#220152,#220153,#220154,#220155,
#220156,#220157,#220158,#220159,#220160,#220161,#220162,#220163,#220164,
#220165,#220166,#220167,#220168,#220169,#220170,#220171,#220172,#220173,
#220174,#220175,#220176,#220177,#220178,#220179,#220180,#220181,#220182,
#220183,#220184),.UNSPECIFIED.,.F.,.F.,(4,2,2,2,2,2,2,2,2,2,2,2,2,2,2,2,
2,2,2,2,2,2,2,2,2,2,2,2,2,4),(-6.15788331278694,-6.06443252815276,-5.83610230741255,
-5.60523089161273,-5.31363699842867,-5.18840170216816,-4.94062642991686,
-4.68241759985902,-4.557318904294,-4.30670853548563,-4.0646490808404,-3.80643899426189,
-3.68163245799914,-3.43051020036923,-3.16947422123254,-2.91133046902137,
-2.78563835863885,-2.52772346543546,-2.25261630655297,-2.12766163183034,
-1.76426794976545,-1.63827805735133,-1.47827926244735,-1.22738320571347,
-0.974993743424404,-0.716796513895058,-0.539736803061585,-0.273532248004654,
-0.137263400187583,-3.49173976057398E-5),.UNSPECIFIED.);
#30616=B_SPLINE_CURVE_WITH_KNOTS('',3,(#220213,#220214,#220215,#220216,
#220217,#220218),.UNSPECIFIED.,.F.,.F.,(4,2,4),(-0.0180614175475569,-0.00903747414230207,
-8.0491419894641E-7),.UNSPECIFIED.);
#30617=B_SPLINE_CURVE_WITH_KNOTS('',3,(#220219,#220220,#220221,#220222,
#220223,#220224,#220225,#220226,#220227,#220228,#220229,#220230,#220231,
#220232),.UNSPECIFIED.,.F.,.F.,(4,2,2,2,2,2,4),(1.00000038962293E-6,0.377507126467076,
0.760172295625583,1.01061719312921,1.51716116734717,1.76732387692728,2.02167921549914),
 .UNSPECIFIED.);
#30618=B_SPLINE_CURVE_WITH_KNOTS('',3,(#220234,#220235,#220236,#220237,
#220238,#220239),.UNSPECIFIED.,.F.,.F.,(4,2,4),(-0.0180670199973735,-0.00903616121666685,
-6.43699295097665E-6),.UNSPECIFIED.);
#30619=B_SPLINE_CURVE_WITH_KNOTS('',3,(#220268,#220269,#220270,#220271,
#220272,#220273),.UNSPECIFIED.,.F.,.F.,(4,2,4),(-0.131007313205517,-0.0654519306470199,
-7.32542529301984E-6),.UNSPECIFIED.);
#30620=B_SPLINE_CURVE_WITH_KNOTS('',3,(#220542,#220543,#220544,#220545,
#220546,#220547,#220548,#220549,#220550,#220551,#220552,#220553,#220554,
#220555,#220556,#220557,#220558,#220559,#220560,#220561,#220562,#220563,
#220564,#220565,#220566,#220567,#220568,#220569,#220570,#220571,#220572,
#220573,#220574,#220575,#220576,#220577,#220578,#220579,#220580,#220581,
#220582,#220583,#220584,#220585,#220586,#220587,#220588,#220589,#220590,
#220591,#220592,#220593,#220594,#220595,#220596,#220597,#220598,#220599,
#220600,#220601,#220602,#220603,#220604,#220605,#220606,#220607,#220608,
#220609,#220610,#220611,#220612,#220613,#220614,#220615,#220616,#220617,
#220618,#220619),.UNSPECIFIED.,.F.,.F.,(4,2,2,2,2,2,2,2,2,2,2,2,2,2,2,2,
2,2,2,2,2,2,2,2,2,2,2,2,2,2,2,2,2,2,2,2,2,2,4),(-20.9311220871695,-20.8233977585101,
-20.5929681913972,-20.3351437643928,-20.1699664773702,-19.9382476421245,
-19.7022880772898,-19.4518568542575,-19.326668163532,-19.0684679733444,
-18.833648144018,-18.5758020857754,-18.450368441215,-18.1921847851807,-17.9372411480242,
-17.6862799548196,-17.5613796926949,-17.3031720422929,-17.0593174409058,
-16.808658958332,-16.6470842308963,-16.4156015810085,-16.1896008615369,
-16.0641249825309,-15.7633137741317,-15.505326382634,-15.3310206693453,
-15.0986175424629,-14.8698936276518,-14.6120684599034,-14.486738873575,
-14.2285383694322,-13.9919828079423,-13.7605082217295,-13.5444128021083,
-13.3279945079624,-13.096528614438,-12.859855499747,-12.7553010434687),
 .UNSPECIFIED.);
#30621=B_SPLINE_CURVE_WITH_KNOTS('',3,(#221031,#221032,#221033,#221034,
#221035,#221036),.UNSPECIFIED.,.F.,.F.,(4,2,4),(-0.344875729523311,-0.172579825678003,
-3.94566552332552E-5),.UNSPECIFIED.);
#30622=B_SPLINE_CURVE_WITH_KNOTS('',3,(#221037,#221038,#221039,#221040),
 .UNSPECIFIED.,.F.,.F.,(4,4),(-0.00025708205727752,0.),.UNSPECIFIED.);
#30623=B_SPLINE_CURVE_WITH_KNOTS('',3,(#221452,#221453,#221454,#221455,
#221456,#221457),.UNSPECIFIED.,.F.,.F.,(4,2,4),(-0.344703474824423,-0.172091835354088,
-0.00130738802393666),.UNSPECIFIED.);
#30624=B_SPLINE_CURVE_WITH_KNOTS('',3,(#221458,#221459,#221460,#221461),
 .UNSPECIFIED.,.F.,.F.,(4,4),(-0.00138054251313501,0.),.UNSPECIFIED.);
#30625=B_SPLINE_CURVE_WITH_KNOTS('',3,(#221488,#221489,#221490,#221491,
#221492,#221493),.UNSPECIFIED.,.F.,.F.,(4,2,4),(0.000411407934197906,0.132395690524123,
0.265296797891781),.UNSPECIFIED.);
#30626=B_SPLINE_CURVE_WITH_KNOTS('',3,(#221496,#221497,#221498,#221499),
 .UNSPECIFIED.,.F.,.F.,(4,4),(0.,0.000434666445788224),.UNSPECIFIED.);
#30627=B_SPLINE_CURVE_WITH_KNOTS('',3,(#221501,#221502,#221503,#221504,
#221505,#221506,#221507,#221508,#221509,#221510,#221511,#221512,#221513,
#221514,#221515,#221516,#221517,#221518,#221519,#221520,#221521,#221522),
 .UNSPECIFIED.,.F.,.F.,(4,2,2,2,2,2,2,2,2,2,4),(0.,0.144173778921629,0.288103676995556,
0.573727861047887,0.772563733388475,1.17379786176671,1.5750673712583,1.77392881725809,
1.91671525972691,2.13148394855007,2.34639580468754),.UNSPECIFIED.);
#30628=B_SPLINE_CURVE_WITH_KNOTS('',3,(#221523,#221524,#221525,#221526),
 .UNSPECIFIED.,.F.,.F.,(4,4),(4.93459806213273E-5,5.07374035434672E-5),
 .UNSPECIFIED.);
#30629=B_SPLINE_CURVE_WITH_KNOTS('',3,(#221605,#221606,#221607,#221608,
#221609,#221610,#221611,#221612,#221613,#221614),.UNSPECIFIED.,.F.,.F.,
(4,2,2,2,4),(2.44487072892702,2.76003095423418,3.15004164386436,3.5418883593805,
3.8553044918496),.UNSPECIFIED.);
#30630=CIRCLE('',#79485,1.5);
#30631=CIRCLE('',#79486,1.5);
#30632=CIRCLE('',#79487,1.500000002703);
#30633=CIRCLE('',#79493,1.50000004292401);
#30634=CIRCLE('',#79494,1.5);
#30635=CIRCLE('',#79495,1.5);
#30636=CIRCLE('',#79501,20.5);
#30637=CIRCLE('',#79505,9.47898844935865);
#30638=CIRCLE('',#79508,20.5);
#30639=CIRCLE('',#79510,1.5);
#30640=CIRCLE('',#79513,9.52146805877686);
#30641=CIRCLE('',#79516,8.39999999999999);
#30642=CIRCLE('',#79520,8.4);
#30643=CIRCLE('',#79523,8.4);
#30644=CIRCLE('',#79529,17.);
#30645=CIRCLE('',#79531,16.375);
#30646=CIRCLE('',#79532,16.375);
#30647=CIRCLE('',#79535,16.375);
#30648=CIRCLE('',#79536,16.5);
#30649=CIRCLE('',#79537,29.9999999999995);
#30650=CIRCLE('',#79538,19.);
#30651=CIRCLE('',#79540,20.5);
#30652=CIRCLE('',#79541,20.5);
#30653=CIRCLE('',#79542,20.5);
#30654=CIRCLE('',#79544,1.499999982843);
#30655=CIRCLE('',#79545,1.5);
#30656=CIRCLE('',#79546,1.499999982843);
#30657=CIRCLE('',#79547,1.5);
#30658=CIRCLE('',#79548,1.5);
#30659=CIRCLE('',#79550,11.);
#30660=CIRCLE('',#79552,1.5);
#30661=CIRCLE('',#79553,1.469693767054);
#30662=CIRCLE('',#79554,1.50000000000001);
#30663=CIRCLE('',#79556,9.50000000000099);
#30664=CIRCLE('',#79557,10.0995446485457);
#30665=CIRCLE('',#79559,10.5);
#30666=CIRCLE('',#79560,10.5);
#30667=CIRCLE('',#79561,10.5);
#30668=CIRCLE('',#79563,10.99999310643);
#30669=CIRCLE('',#79564,0.5);
#30670=CIRCLE('',#79566,11.25);
#30671=CIRCLE('',#79567,11.25);
#30672=CIRCLE('',#79568,11.25);
#30673=CIRCLE('',#79570,11.7499940828);
#30674=CIRCLE('',#79571,0.5);
#30675=CIRCLE('',#79573,11.);
#30676=CIRCLE('',#79574,0.500000000000001);
#30677=CIRCLE('',#79575,10.5);
#30678=CIRCLE('',#79576,0.5);
#30679=CIRCLE('',#79580,21.);
#30680=CIRCLE('',#79583,10.5);
#30681=CIRCLE('',#79584,0.5);
#30682=CIRCLE('',#79585,0.500000000000001);
#30683=CIRCLE('',#79588,1.499999986109);
#30684=CIRCLE('',#79589,1.5);
#30685=CIRCLE('',#79590,1.499999986109);
#30686=CIRCLE('',#79591,1.5);
#30687=CIRCLE('',#79592,1.5);
#30688=CIRCLE('',#79594,9.50000000000099);
#30689=CIRCLE('',#79595,9.50000000000101);
#30690=CIRCLE('',#79597,8.249990255698);
#30691=CIRCLE('',#79598,0.5);
#30692=CIRCLE('',#79599,7.75);
#30693=CIRCLE('',#79600,7.75);
#30694=CIRCLE('',#79602,7.75);
#30695=CIRCLE('',#79604,6.5);
#30696=CIRCLE('',#79605,6.5);
#30697=CIRCLE('',#79606,6.5);
#30698=CIRCLE('',#79608,9.5);
#30699=CIRCLE('',#79609,9.5);
#30700=CIRCLE('',#79610,9.5);
#30701=CIRCLE('',#79611,9.5);
#30702=CIRCLE('',#79613,13.5);
#30703=CIRCLE('',#79614,13.5);
#30704=CIRCLE('',#79615,13.5);
#30705=CIRCLE('',#79617,14.0995393127475);
#30706=CIRCLE('',#79619,14.5);
#30707=CIRCLE('',#79620,14.5);
#30708=CIRCLE('',#79622,7.25);
#30709=CIRCLE('',#79628,6.5);
#30710=CIRCLE('',#79629,6.5);
#30711=CIRCLE('',#79630,0.5);
#30712=CIRCLE('',#79631,6.999991969209);
#30713=CIRCLE('',#79633,6.5);
#30714=CIRCLE('',#79635,5.5);
#30715=CIRCLE('',#79636,6.09968496709595);
#30716=CIRCLE('',#79637,5.5);
#30717=CIRCLE('',#79639,5.5);
#30718=CIRCLE('',#79640,5.5);
#30719=CIRCLE('',#79643,9.5);
#30720=CIRCLE('',#79645,37.5);
#30721=CIRCLE('',#79646,37.5);
#30722=CIRCLE('',#79649,16.);
#30723=CIRCLE('',#79650,16.);
#30724=CIRCLE('',#79651,16.);
#30725=CIRCLE('',#79654,17.);
#30726=CIRCLE('',#79655,17.175);
#30727=CIRCLE('',#79658,9.999992241343);
#30728=CIRCLE('',#79659,0.5);
#30729=CIRCLE('',#79660,9.49999999999999);
#30730=CIRCLE('',#79661,9.49999999999999);
#30731=CIRCLE('',#79663,9.49999999999999);
#30732=CIRCLE('',#79665,8.999610558584);
#30733=CIRCLE('',#79668,12.);
#30734=CIRCLE('',#79670,37.5);
#30735=CIRCLE('',#79671,37.5);
#30736=CIRCLE('',#79673,8.5);
#30737=CIRCLE('',#79675,10.25);
#30738=CIRCLE('',#79676,10.25);
#30739=CIRCLE('',#79678,11.75);
#30740=CIRCLE('',#79679,11.75);
#30741=CIRCLE('',#79680,11.75);
#30742=CIRCLE('',#79682,11.25);
#30743=CIRCLE('',#79684,7.75000000000001);
#30744=CIRCLE('',#79685,7.75000000000001);
#30745=CIRCLE('',#79686,7.75000000000001);
#30746=CIRCLE('',#79687,7.75000000000001);
#30747=CIRCLE('',#79690,7.95);
#30748=CIRCLE('',#79692,9.49999999999999);
#30749=CIRCLE('',#79693,9.49999999999999);
#30750=CIRCLE('',#79694,0.5);
#30751=CIRCLE('',#79695,10.);
#30752=CIRCLE('',#79697,9.49999999999999);
#30753=CIRCLE('',#79699,8.99961055858501);
#30754=CIRCLE('',#79701,8.4);
#30755=CIRCLE('',#79703,12.);
#30756=CIRCLE('',#79705,37.5);
#30757=CIRCLE('',#79706,37.5);
#30758=CIRCLE('',#79708,8.5);
#30759=CIRCLE('',#79710,10.25);
#30760=CIRCLE('',#79711,10.25);
#30761=CIRCLE('',#79713,11.75);
#30762=CIRCLE('',#79714,11.75);
#30763=CIRCLE('',#79715,11.75);
#30764=CIRCLE('',#79717,11.25);
#30765=CIRCLE('',#79719,7.75000000000001);
#30766=CIRCLE('',#79720,7.75000000000001);
#30767=CIRCLE('',#79721,7.75000000000001);
#30768=CIRCLE('',#79722,7.75000000000001);
#30769=CIRCLE('',#79725,7.95);
#30770=CIRCLE('',#79736,1.5);
#30771=CIRCLE('',#79737,1.5);
#30772=CIRCLE('',#79738,9.499999338856);
#30773=CIRCLE('',#79739,9.50002077009014);
#30774=CIRCLE('',#79741,18.5);
#30775=CIRCLE('',#79743,1.5);
#30776=CIRCLE('',#79744,1.499999950122);
#30777=CIRCLE('',#79747,1.);
#30778=CIRCLE('',#79749,1.);
#30779=CIRCLE('',#79751,20.5);
#30780=CIRCLE('',#79752,1.00001318723944);
#30781=CIRCLE('',#79754,1.5);
#30782=CIRCLE('',#79756,20.5);
#30783=CIRCLE('',#79758,0.999999999999988);
#30784=CIRCLE('',#79759,1.50000050755152);
#30785=CIRCLE('',#79760,1.5);
#30786=CIRCLE('',#79761,9.49592460421503);
#30787=CIRCLE('',#79763,1.5);
#30788=CIRCLE('',#79764,27.5);
#30789=CIRCLE('',#79765,1.5);
#30790=CIRCLE('',#79766,25.999999939);
#30791=CIRCLE('',#79768,1.5);
#30792=CIRCLE('',#79769,6.999999373843);
#30793=CIRCLE('',#79771,1.5);
#30794=CIRCLE('',#79772,27.5);
#30795=CIRCLE('',#79773,25.999999939);
#30796=CIRCLE('',#79774,9.499992460383);
#30797=CIRCLE('',#79777,67.5000000000001);
#30798=CIRCLE('',#79778,1.5);
#30799=CIRCLE('',#79779,66.);
#30800=CIRCLE('',#79781,3.999998543283);
#30801=CIRCLE('',#79782,35.99999881413);
#30802=CIRCLE('',#79784,1.5);
#30803=CIRCLE('',#79785,1.5);
#30804=CIRCLE('',#79787,0.999969185525436);
#30805=CIRCLE('',#79788,1.67878043484372);
#30806=CIRCLE('',#79790,36.);
#30807=CIRCLE('',#79791,3.99999530486);
#30808=CIRCLE('',#79793,1.5);
#30809=CIRCLE('',#79794,5.5);
#30810=CIRCLE('',#79797,5.5);
#30811=CIRCLE('',#79798,1.5);
#30812=CIRCLE('',#79799,3.99999479023);
#30813=CIRCLE('',#79801,35.99999988417);
#30814=CIRCLE('',#79802,3.999994788468);
#30815=CIRCLE('',#79804,1.5);
#30816=CIRCLE('',#79805,5.5);
#30817=CIRCLE('',#79809,1.5);
#30818=CIRCLE('',#79810,5.5);
#30819=CIRCLE('',#79816,37.5);
#30820=CIRCLE('',#79818,37.5);
#30821=CIRCLE('',#79821,7.49975097307099);
#30822=CIRCLE('',#79822,7.49996549760091);
#30823=CIRCLE('',#79823,7.499998842876);
#30824=CIRCLE('',#79824,7.4998364236414);
#30825=CIRCLE('',#79825,7.49981706173728);
#30826=CIRCLE('',#79826,7.50005935914293);
#30827=CIRCLE('',#79827,0.899997806293704);
#30828=CIRCLE('',#79828,0.8999999261735);
#30829=CIRCLE('',#79829,0.899996702628005);
#30830=CIRCLE('',#79830,0.899999963985599);
#30831=CIRCLE('',#79831,0.89999753573199);
#30832=CIRCLE('',#79832,0.900009083862835);
#30833=CIRCLE('',#79845,1.5);
#30834=CIRCLE('',#79846,1.5);
#30835=CIRCLE('',#79847,1.500044106112);
#30836=CIRCLE('',#79849,1.);
#30837=CIRCLE('',#79850,1.00000010883301);
#30838=CIRCLE('',#79852,1.);
#30839=CIRCLE('',#79854,1.5);
#30840=CIRCLE('',#79855,1.00000410138919);
#30841=CIRCLE('',#79859,1.5);
#30842=CIRCLE('',#79860,1.499999948802);
#30843=CIRCLE('',#79862,18.5);
#30844=CIRCLE('',#79864,20.5);
#30845=CIRCLE('',#79866,20.5);
#30846=CIRCLE('',#79867,9.5000384206471);
#30847=CIRCLE('',#79868,9.49986806483473);
#30848=CIRCLE('',#79869,9.50751370143532);
#30849=CIRCLE('',#79870,1.5);
#30850=CIRCLE('',#79871,0.9999958303961);
#30851=CIRCLE('',#79872,2.60851153982772);
#30852=CIRCLE('',#79873,1.68163933950004);
#30853=CIRCLE('',#79875,3.999995304826);
#30854=CIRCLE('',#79876,36.);
#30855=CIRCLE('',#79879,1.5);
#30856=CIRCLE('',#79880,1.5);
#30857=CIRCLE('',#79882,35.9999988124);
#30858=CIRCLE('',#79883,3.999998543287);
#30859=CIRCLE('',#79884,66.);
#30860=CIRCLE('',#79886,1.5);
#30861=CIRCLE('',#79887,67.5);
#30862=CIRCLE('',#79889,9.49998316126555);
#30863=CIRCLE('',#79891,1.5);
#30864=CIRCLE('',#79892,27.5);
#30865=CIRCLE('',#79893,1.5);
#30866=CIRCLE('',#79894,25.9999999388);
#30867=CIRCLE('',#79896,1.5);
#30868=CIRCLE('',#79897,6.999999378975);
#30869=CIRCLE('',#79899,1.5);
#30870=CIRCLE('',#79900,27.5);
#30871=CIRCLE('',#79901,25.9999999388);
#30872=CIRCLE('',#79904,1.5);
#30873=CIRCLE('',#79905,5.5);
#30874=CIRCLE('',#79909,1.5);
#30875=CIRCLE('',#79911,5.5);
#30876=CIRCLE('',#79915,5.5);
#30877=CIRCLE('',#79916,1.5);
#30878=CIRCLE('',#79917,3.999994788468);
#30879=CIRCLE('',#79919,35.99999988437);
#30880=CIRCLE('',#79920,3.99999479023);
#30881=CIRCLE('',#79922,1.5);
#30882=CIRCLE('',#79923,5.5);
#30883=CIRCLE('',#79927,37.5);
#30884=CIRCLE('',#79929,37.5);
#30885=CIRCLE('',#79931,7.49963123500319);
#30886=CIRCLE('',#79932,7.49983642367189);
#30887=CIRCLE('',#79933,7.4995737213981);
#30888=CIRCLE('',#79934,7.49996421205067);
#30889=CIRCLE('',#79935,7.49815090357793);
#30890=CIRCLE('',#79936,7.50024364842026);
#30891=CIRCLE('',#79937,0.899999997921601);
#30892=CIRCLE('',#79938,0.900001968871443);
#30893=CIRCLE('',#79939,0.899995896073665);
#30894=CIRCLE('',#79940,0.900004054655721);
#30895=CIRCLE('',#79941,0.899997812495222);
#30896=CIRCLE('',#79948,3.);
#30897=CIRCLE('',#79949,66.50000548541);
#30898=CIRCLE('',#79950,4.499997824719);
#30899=CIRCLE('',#79951,36.49999892491);
#30900=CIRCLE('',#79952,0.499990522764298);
#30901=CIRCLE('',#79954,0.4999905099229);
#30902=CIRCLE('',#79955,36.49999890351);
#30903=CIRCLE('',#79956,4.499997824561);
#30904=CIRCLE('',#79957,66.50000546274);
#30905=CIRCLE('',#79958,3.);
#30906=CIRCLE('',#79964,1.49999970075033);
#30907=CIRCLE('',#79965,1.49999998655821);
#30908=CIRCLE('',#79966,1.50016116215603);
#30909=CIRCLE('',#79969,15.5);
#30910=CIRCLE('',#79970,15.5);
#30911=CIRCLE('',#79972,15.5);
#30912=CIRCLE('',#79973,15.5);
#30913=CIRCLE('',#79975,5.498378496899);
#30914=CIRCLE('',#79977,5.498378496898);
#30915=CIRCLE('',#79978,10.50000198938);
#30916=CIRCLE('',#79980,1.);
#30917=CIRCLE('',#79982,1.);
#30918=CIRCLE('',#79983,10.5002831444245);
#30919=CIRCLE('',#79984,1.499999996972);
#30920=CIRCLE('',#79987,1.49997521686421);
#30921=CIRCLE('',#79988,1.50041791440912);
#30922=CIRCLE('',#79990,1.50000397930881);
#30923=CIRCLE('',#79991,1.50000460950488);
#30924=CIRCLE('',#79995,0.999998640941429);
#30925=CIRCLE('',#79998,0.999998603408247);
#30926=CIRCLE('',#80001,0.999995569663453);
#30927=CIRCLE('',#80003,1.);
#30928=CIRCLE('',#80004,1.);
#30929=CIRCLE('',#80006,67.5);
#30930=CIRCLE('',#80007,1.);
#30931=CIRCLE('',#80009,5.5);
#30932=CIRCLE('',#80011,5.5);
#30933=CIRCLE('',#80013,1.);
#30934=CIRCLE('',#80014,1.);
#30935=CIRCLE('',#80016,20.5);
#30936=CIRCLE('',#80019,1.5);
#30937=CIRCLE('',#80020,1.5);
#30938=CIRCLE('',#80021,10.5003945400646);
#30939=CIRCLE('',#80023,14.);
#30940=CIRCLE('',#80025,15.5);
#30941=CIRCLE('',#80026,15.5);
#30942=CIRCLE('',#80028,1.49990933380908);
#30943=CIRCLE('',#80029,13.99999933141);
#30944=CIRCLE('',#80030,1.4999999963081);
#30945=CIRCLE('',#80032,8.01643786925901);
#30946=CIRCLE('',#80033,1.49999999641083);
#30947=CIRCLE('',#80034,9.516437378118);
#30948=CIRCLE('',#80038,8.33645645579341);
#30949=CIRCLE('',#80043,7.999967894592);
#30950=CIRCLE('',#80046,0.300014002256891);
#30951=CIRCLE('',#80047,0.299999949983396);
#30952=CIRCLE('',#80051,12.0017324877834);
#30953=CIRCLE('',#80052,12.0017324881221);
#30954=CIRCLE('',#80059,0.299999960727201);
#30955=CIRCLE('',#80060,0.300014841061868);
#30956=CIRCLE('',#80065,7.99999976356479);
#30957=CIRCLE('',#80073,1.49999999999999);
#30958=CIRCLE('',#80074,1.50000000099398);
#30959=CIRCLE('',#80076,3.89386562528717);
#30960=CIRCLE('',#80077,1.50004717292849);
#30961=CIRCLE('',#80081,1.50005062266532);
#30962=CIRCLE('',#80083,15.5);
#30963=CIRCLE('',#80084,15.5);
#30964=CIRCLE('',#80085,1.49999999999785);
#30965=CIRCLE('',#80088,5.498378496899);
#30966=CIRCLE('',#80090,4.498380133177);
#30967=CIRCLE('',#80092,14.50000004627);
#30968=CIRCLE('',#80093,0.99996090845702);
#30969=CIRCLE('',#80095,0.999999999999999);
#30970=CIRCLE('',#80096,0.999998041963027);
#30971=CIRCLE('',#80098,14.50000488242);
#30972=CIRCLE('',#80099,1.);
#30973=CIRCLE('',#80102,0.999262032196716);
#30974=CIRCLE('',#80103,0.999999996008301);
#30975=CIRCLE('',#80105,14.50000488338);
#30976=CIRCLE('',#80106,1.00007468229929);
#30977=CIRCLE('',#80107,1.000000000272);
#30978=CIRCLE('',#80110,0.999975226270856);
#30979=CIRCLE('',#80112,14.50000004257);
#30980=CIRCLE('',#80113,0.999999999999993);
#30981=CIRCLE('',#80115,5.498378496898);
#30982=CIRCLE('',#80118,27.6468278765);
#30983=CIRCLE('',#80123,27.64683059909);
#30984=CIRCLE('',#80124,1.5);
#30985=CIRCLE('',#80125,1.5);
#30986=CIRCLE('',#80126,1.5);
#30987=CIRCLE('',#80127,1.50000003977618);
#30988=CIRCLE('',#80128,1.5);
#30989=CIRCLE('',#80129,3.88721692441433);
#30990=CIRCLE('',#80130,1.50002159187886);
#30991=CIRCLE('',#80132,26.64680776781);
#30992=CIRCLE('',#80134,26.64680492934);
#30993=CIRCLE('',#80141,9.50000000000099);
#30994=CIRCLE('',#80144,9.500000000001);
#30995=CIRCLE('',#80145,9.500000000001);
#30996=CIRCLE('',#80147,2.449482268868);
#30997=CIRCLE('',#80148,10.55050311408);
#30998=CIRCLE('',#80149,10.49985738567);
#30999=CIRCLE('',#80151,10.49988903328);
#31000=CIRCLE('',#80152,10.55050536419);
#31001=CIRCLE('',#80153,2.449485998643);
#31002=CIRCLE('',#80155,1.00004538195426);
#31003=CIRCLE('',#80156,11.5);
#31004=CIRCLE('',#80157,0.999999999999998);
#31005=CIRCLE('',#80158,1.00001406525855);
#31006=CIRCLE('',#80161,11.5);
#31007=CIRCLE('',#80164,13.99999938228);
#31008=CIRCLE('',#80166,0.999998820674145);
#31009=CIRCLE('',#80167,1.00000976363729);
#31010=CIRCLE('',#80168,0.999999855249661);
#31011=CIRCLE('',#80171,11.53030601499);
#31012=CIRCLE('',#80172,1.);
#31013=CIRCLE('',#80178,1.5);
#31014=CIRCLE('',#80179,1.5);
#31015=CIRCLE('',#80180,1.5);
#31016=CIRCLE('',#80181,1.469693696648);
#31017=CIRCLE('',#80183,0.999999999999999);
#31018=CIRCLE('',#80185,11.53030595098);
#31019=CIRCLE('',#80187,13.00000023588);
#31020=CIRCLE('',#80191,13.00000024132);
#31021=CIRCLE('',#80193,1.5);
#31022=CIRCLE('',#80195,1.5);
#31023=CIRCLE('',#80196,1.5);
#31024=CIRCLE('',#80200,1.5000306953952);
#31025=CIRCLE('',#80204,1.500000156322);
#31026=CIRCLE('',#80208,10.4988998342525);
#31027=CIRCLE('',#80209,1.5);
#31028=CIRCLE('',#80211,10.49999854524);
#31029=CIRCLE('',#80213,15.);
#31030=CIRCLE('',#80214,15.);
#31031=CIRCLE('',#80215,4.99999999388658);
#31032=CIRCLE('',#80216,4.99999999999388);
#31033=CIRCLE('',#80217,4.99999968198887);
#31034=CIRCLE('',#80218,5.00000000000995);
#31035=CIRCLE('',#80220,5.00000474327103);
#31036=CIRCLE('',#80221,4.99999999999405);
#31037=CIRCLE('',#80222,4.9999996844452);
#31038=CIRCLE('',#80224,4.99999968385975);
#31039=CIRCLE('',#80225,4.99999999999802);
#31040=CIRCLE('',#80226,5.00000000000122);
#31041=CIRCLE('',#80228,40.);
#31042=CIRCLE('',#80229,0.5);
#31043=CIRCLE('',#80230,39.5);
#31044=CIRCLE('',#80231,0.5);
#31045=CIRCLE('',#80232,40.);
#31046=CIRCLE('',#80235,8.);
#31047=CIRCLE('',#80236,8.);
#31048=CIRCLE('',#80238,40.);
#31049=CIRCLE('',#80240,0.5);
#31050=CIRCLE('',#80241,39.5);
#31051=CIRCLE('',#80242,0.500000000000001);
#31052=CIRCLE('',#80243,40.);
#31053=CIRCLE('',#80246,8.);
#31054=CIRCLE('',#80247,8.);
#31055=CIRCLE('',#80248,4.99999999991307);
#31056=CIRCLE('',#80249,5.00000000000412);
#31057=CIRCLE('',#80250,4.9999996846577);
#31058=CIRCLE('',#80251,4.999999999992);
#31059=CIRCLE('',#80252,4.99999999400135);
#31060=CIRCLE('',#80253,4.99999999999915);
#31061=CIRCLE('',#80254,5.00000000000267);
#31062=CIRCLE('',#80255,4.99999968222069);
#31063=CIRCLE('',#80256,4.99999968215304);
#31064=CIRCLE('',#80257,4.99999999999966);
#31065=CIRCLE('',#80259,15.);
#31066=CIRCLE('',#80260,15.);
#31067=CIRCLE('',#80265,7.5);
#31068=CIRCLE('',#80266,0.5);
#31069=CIRCLE('',#80268,29.5);
#31070=CIRCLE('',#80269,30.);
#31071=CIRCLE('',#80271,30.);
#31072=CIRCLE('',#80272,0.500000000000002);
#31073=CIRCLE('',#80273,29.5);
#31074=CIRCLE('',#80275,7.5);
#31075=CIRCLE('',#80278,6.999999985528);
#31076=CIRCLE('',#80280,30.);
#31077=CIRCLE('',#80282,30.);
#31078=CIRCLE('',#80283,6.9999999999976);
#31079=CIRCLE('',#80285,0.500000000000002);
#31080=CIRCLE('',#80286,29.5);
#31081=CIRCLE('',#80288,29.5);
#31082=CIRCLE('',#80289,0.5);
#31083=CIRCLE('',#80291,7.5);
#31084=CIRCLE('',#80293,7.5);
#31085=CIRCLE('',#80296,8.00000000037468);
#31086=CIRCLE('',#80298,6.0000000000044);
#31087=CIRCLE('',#80299,6.00000000004738);
#31088=CIRCLE('',#80300,6.00000000068573);
#31089=CIRCLE('',#80302,5.99998574891701);
#31090=CIRCLE('',#80303,6.00000003035761);
#31091=CIRCLE('',#80305,6.00000000004975);
#31092=CIRCLE('',#80306,6.00000000004976);
#31093=CIRCLE('',#80308,13.);
#31094=CIRCLE('',#80309,13.);
#31095=CIRCLE('',#80314,10.0997825859452);
#31096=CIRCLE('',#80317,1.5);
#31097=CIRCLE('',#80318,1.5);
#31098=CIRCLE('',#80320,1.5);
#31099=CIRCLE('',#80321,31.6373353297717);
#31100=CIRCLE('',#80322,1.500000028483);
#31101=CIRCLE('',#80327,1.5);
#31102=CIRCLE('',#80329,1.5);
#31103=CIRCLE('',#80330,1.5);
#31104=CIRCLE('',#80335,1.500000033965);
#31105=CIRCLE('',#80336,31.6434611407195);
#31106=CIRCLE('',#80337,1.49999999939402);
#31107=CIRCLE('',#80338,1.5);
#31108=CIRCLE('',#80344,1.5);
#31109=CIRCLE('',#80346,0.999995633686306);
#31110=CIRCLE('',#80348,67.5);
#31111=CIRCLE('',#80350,1.5);
#31112=CIRCLE('',#80351,1.5);
#31113=CIRCLE('',#80353,1.5);
#31114=CIRCLE('',#80354,1.5);
#31115=CIRCLE('',#80356,1.5);
#31116=CIRCLE('',#80358,1.);
#31117=CIRCLE('',#80362,1.5);
#31118=CIRCLE('',#80363,10.5004492687665);
#31119=CIRCLE('',#80366,14.);
#31120=CIRCLE('',#80372,1.00000780008503);
#31121=CIRCLE('',#80374,1.49987422447354);
#31122=CIRCLE('',#80377,20.5);
#31123=CIRCLE('',#80381,21.5);
#31124=CIRCLE('',#80382,21.);
#31125=CIRCLE('',#80383,21.5);
#31126=CIRCLE('',#80386,21.5);
#31127=CIRCLE('',#80390,20.);
#31128=CIRCLE('',#80392,20.);
#31129=CIRCLE('',#80393,20.);
#31130=CIRCLE('',#80398,20.74940226558);
#31131=CIRCLE('',#80401,1.5);
#31132=CIRCLE('',#80402,18.49999990017);
#31133=CIRCLE('',#80404,1.367013312824);
#31134=CIRCLE('',#80405,1.50000000000001);
#31135=CIRCLE('',#80407,1.50000000000001);
#31136=CIRCLE('',#80408,1.367013312824);
#31137=CIRCLE('',#80410,2.15);
#31138=CIRCLE('',#80413,19.);
#31139=CIRCLE('',#80414,19.);
#31140=CIRCLE('',#80416,17.5);
#31141=CIRCLE('',#80418,17.5);
#31142=CIRCLE('',#80421,19.);
#31143=CIRCLE('',#80422,17.5);
#31144=CIRCLE('',#80424,19.);
#31145=CIRCLE('',#80427,17.5);
#31146=CIRCLE('',#80431,1.);
#31147=CIRCLE('',#80432,1.367013307544);
#31148=CIRCLE('',#80435,0.999999999999999);
#31149=CIRCLE('',#80436,1.367013307544);
#31150=CIRCLE('',#80439,1.50000000000001);
#31151=CIRCLE('',#80440,1.50000000000001);
#31152=CIRCLE('',#80442,1.50000000000001);
#31153=CIRCLE('',#80443,2.866767200355);
#31154=CIRCLE('',#80445,1.50000000000001);
#31155=CIRCLE('',#80447,1.50000000000001);
#31156=CIRCLE('',#80448,2.866767200355);
#31157=CIRCLE('',#80450,1.50000000000001);
#31158=CIRCLE('',#80452,1.50000000000001);
#31159=CIRCLE('',#80453,1.367013307544);
#31160=CIRCLE('',#80454,2.866767200355);
#31161=CIRCLE('',#80456,0.999999999999999);
#31162=CIRCLE('',#80459,0.6329865970941);
#31163=CIRCLE('',#80462,260.049496473139);
#31164=CIRCLE('',#80463,263.669169655306);
#31165=CIRCLE('',#80470,0.632986597024199);
#31166=CIRCLE('',#80472,1.50000000000001);
#31167=CIRCLE('',#80474,1.367013307544);
#31168=CIRCLE('',#80475,2.866767200355);
#31169=CIRCLE('',#80477,1.);
#31170=CIRCLE('',#80495,0.99994027564094);
#31171=CIRCLE('',#80496,1.00013699839423);
#31172=CIRCLE('',#80497,1.00004072258415);
#31173=CIRCLE('',#80498,2.99994768942185);
#31174=CIRCLE('',#80499,2.99994973931572);
#31175=CIRCLE('',#80501,3.00000436884464);
#31176=CIRCLE('',#80502,2.99998510560444);
#31177=CIRCLE('',#80504,0.999982594817338);
#31178=CIRCLE('',#80505,0.99999946824157);
#31179=CIRCLE('',#80506,0.999999991421499);
#31180=CIRCLE('',#80509,2.999999936398);
#31181=CIRCLE('',#80510,2.999999257509);
#31182=CIRCLE('',#80511,2.999979963362);
#31183=CIRCLE('',#80515,3.000001934398);
#31184=CIRCLE('',#80516,3.00003905154638);
#31185=CIRCLE('',#80517,2.99998878091108);
#31186=CIRCLE('',#80519,3.00001995803758);
#31187=CIRCLE('',#80524,9.35);
#31188=CIRCLE('',#80531,9.35);
#31189=CIRCLE('',#80533,9.49999999999999);
#31190=CIRCLE('',#80541,9.49999999999999);
#31191=CIRCLE('',#80543,10.);
#31192=CIRCLE('',#80549,10.25);
#31193=CIRCLE('',#80556,7.25);
#31194=CIRCLE('',#80558,10.25);
#31195=CIRCLE('',#80560,9.25);
#31196=CIRCLE('',#80561,9.25);
#31197=CIRCLE('',#80562,9.25);
#31198=CIRCLE('',#80564,11.);
#31199=CIRCLE('',#80565,11.);
#31200=CIRCLE('',#80567,9.15);
#31201=CIRCLE('',#80568,9.15);
#31202=CIRCLE('',#80570,10.);
#31203=CIRCLE('',#80572,9.35);
#31204=CIRCLE('',#80574,9.50000000000001);
#31205=CIRCLE('',#80575,91.074321383489);
#31206=CIRCLE('',#80577,7.75);
#31207=CIRCLE('',#80578,7.75);
#31208=CIRCLE('',#80579,7.75);
#31209=CIRCLE('',#80581,6.5);
#31210=CIRCLE('',#80582,6.5);
#31211=CIRCLE('',#80584,6.75);
#31212=CIRCLE('',#80585,0.25);
#31213=CIRCLE('',#80587,0.5);
#31214=CIRCLE('',#80588,8.25);
#31215=CIRCLE('',#80590,4.);
#31216=CIRCLE('',#80591,4.);
#31217=CIRCLE('',#80593,9.49999999999999);
#31218=CIRCLE('',#80595,9.25);
#31219=CIRCLE('',#80602,4.);
#31220=CIRCLE('',#80603,4.);
#31221=CIRCLE('',#80622,9.49999999999999);
#31222=CIRCLE('',#80623,0.25);
#31223=CIRCLE('',#80624,10.);
#31224=CIRCLE('',#80626,11.);
#31225=CIRCLE('',#80627,0.25);
#31226=CIRCLE('',#80628,11.5);
#31227=CIRCLE('',#80630,12.1);
#31228=CIRCLE('',#80631,12.1);
#31229=CIRCLE('',#80632,12.1);
#31230=CIRCLE('',#80633,12.1);
#31231=CIRCLE('',#80634,12.1);
#31232=CIRCLE('',#80635,12.1);
#31233=CIRCLE('',#80636,12.1);
#31234=CIRCLE('',#80637,12.1);
#31235=CIRCLE('',#80639,11.5);
#31236=CIRCLE('',#80640,0.25);
#31237=CIRCLE('',#80641,11.);
#31238=CIRCLE('',#80643,10.);
#31239=CIRCLE('',#80644,0.25);
#31240=CIRCLE('',#80645,9.49999999999999);
#31241=CIRCLE('',#80647,7.50000000000001);
#31242=CIRCLE('',#80648,7.50000000000001);
#31243=CIRCLE('',#80650,1.5);
#31244=CIRCLE('',#80651,1.5);
#31245=CIRCLE('',#80653,1.49999999999999);
#31246=CIRCLE('',#80654,1.49999999999999);
#31247=CIRCLE('',#80657,1.5);
#31248=CIRCLE('',#80659,1.5);
#31249=CIRCLE('',#80672,12.25);
#31250=CIRCLE('',#80677,12.25);
#31251=CIRCLE('',#80679,10.5);
#31252=CIRCLE('',#80680,10.5);
#31253=CIRCLE('',#80682,12.25);
#31254=CIRCLE('',#80685,13.25000025523);
#31255=CIRCLE('',#80687,16.);
#31256=CIRCLE('',#80688,16.);
#31257=CIRCLE('',#80689,16.);
#31258=CIRCLE('',#80690,16.);
#31259=CIRCLE('',#80691,16.);
#31260=CIRCLE('',#80692,14.);
#31261=CIRCLE('',#80693,16.);
#31262=CIRCLE('',#80694,16.);
#31263=CIRCLE('',#80696,16.);
#31264=CIRCLE('',#80697,16.);
#31265=CIRCLE('',#80698,16.);
#31266=CIRCLE('',#80699,16.);
#31267=CIRCLE('',#80700,16.);
#31268=CIRCLE('',#80701,14.);
#31269=CIRCLE('',#80702,16.);
#31270=CIRCLE('',#80703,16.);
#31271=CIRCLE('',#80721,9.49999999999999);
#31272=CIRCLE('',#80722,0.25);
#31273=CIRCLE('',#80723,10.);
#31274=CIRCLE('',#80725,11.);
#31275=CIRCLE('',#80726,0.25);
#31276=CIRCLE('',#80727,11.5);
#31277=CIRCLE('',#80729,12.1);
#31278=CIRCLE('',#80730,12.1);
#31279=CIRCLE('',#80731,12.1);
#31280=CIRCLE('',#80732,12.1);
#31281=CIRCLE('',#80733,12.1);
#31282=CIRCLE('',#80734,12.1);
#31283=CIRCLE('',#80735,12.1);
#31284=CIRCLE('',#80736,12.1);
#31285=CIRCLE('',#80738,11.5);
#31286=CIRCLE('',#80739,0.25);
#31287=CIRCLE('',#80740,11.);
#31288=CIRCLE('',#80742,10.);
#31289=CIRCLE('',#80743,0.25);
#31290=CIRCLE('',#80744,9.49999999999999);
#31291=CIRCLE('',#80746,7.50000000000001);
#31292=CIRCLE('',#80747,7.50000000000001);
#31293=CIRCLE('',#80749,1.5);
#31294=CIRCLE('',#80750,1.5);
#31295=CIRCLE('',#80752,1.49999999999999);
#31296=CIRCLE('',#80753,1.49999999999999);
#31297=CIRCLE('',#80756,1.5);
#31298=CIRCLE('',#80758,1.5);
#31299=CIRCLE('',#80768,26.49999955823);
#31300=CIRCLE('',#80769,1.);
#31301=CIRCLE('',#80770,27.5);
#31302=CIRCLE('',#80772,27.5);
#31303=CIRCLE('',#80774,12.4);
#31304=CIRCLE('',#80775,12.4);
#31305=CIRCLE('',#80777,2.);
#31306=CIRCLE('',#80778,2.);
#31307=CIRCLE('',#80780,27.);
#31308=CIRCLE('',#80781,0.5);
#31309=CIRCLE('',#80782,26.5);
#31310=CIRCLE('',#80784,27.);
#31311=CIRCLE('',#80786,15.93867390024);
#31312=CIRCLE('',#80787,14.68867390024);
#31313=CIRCLE('',#80791,14.5);
#31314=CIRCLE('',#80793,15.75);
#31315=CIRCLE('',#80801,12.25);
#31316=CIRCLE('',#80806,12.25);
#31317=CIRCLE('',#80808,10.5);
#31318=CIRCLE('',#80809,10.5);
#31319=CIRCLE('',#80811,12.25);
#31320=CIRCLE('',#80814,13.25000025523);
#31321=CIRCLE('',#80816,16.);
#31322=CIRCLE('',#80817,16.);
#31323=CIRCLE('',#80818,16.);
#31324=CIRCLE('',#80819,16.);
#31325=CIRCLE('',#80820,16.);
#31326=CIRCLE('',#80821,14.);
#31327=CIRCLE('',#80822,16.);
#31328=CIRCLE('',#80823,16.);
#31329=CIRCLE('',#80825,16.);
#31330=CIRCLE('',#80826,16.);
#31331=CIRCLE('',#80827,16.);
#31332=CIRCLE('',#80828,16.);
#31333=CIRCLE('',#80829,16.);
#31334=CIRCLE('',#80830,14.);
#31335=CIRCLE('',#80831,16.);
#31336=CIRCLE('',#80832,16.);
#31337=CIRCLE('',#80850,2.05000000000001);
#31338=CIRCLE('',#80851,2.05);
#31339=CIRCLE('',#80852,2.05);
#31340=CIRCLE('',#80856,5.5);
#31341=CIRCLE('',#80860,5.5);
#31342=CIRCLE('',#80862,6.);
#31343=CIRCLE('',#80865,7.);
#31344=CIRCLE('',#80866,7.);
#31345=CIRCLE('',#80867,7.);
#31346=CIRCLE('',#80868,7.);
#31347=CIRCLE('',#80869,7.);
#31348=CIRCLE('',#80870,7.);
#31349=CIRCLE('',#80872,6.5);
#31350=CIRCLE('',#80874,5.25);
#31351=CIRCLE('',#80875,5.25);
#31352=CIRCLE('',#80877,6.);
#31353=CIRCLE('',#80879,5.5);
#31354=CIRCLE('',#80880,155.44481082364);
#31355=CIRCLE('',#80882,4.4);
#31356=CIRCLE('',#80883,4.4);
#31357=CIRCLE('',#80884,4.4);
#31358=CIRCLE('',#80886,2.55);
#31359=CIRCLE('',#80887,2.55);
#31360=CIRCLE('',#80888,2.55);
#31361=CIRCLE('',#80889,2.55);
#31362=CIRCLE('',#80891,3.05);
#31363=CIRCLE('',#80893,3.05);
#31364=CIRCLE('',#80895,5.5);
#31365=CIRCLE('',#80897,4.9);
#31366=CIRCLE('',#80900,6.47238979616113);
#31367=CIRCLE('',#80901,6.47238979616116);
#31368=CIRCLE('',#80903,0.959420631745662);
#31369=CIRCLE('',#80904,6.47238979616113);
#31370=CIRCLE('',#80906,6.47238979616113);
#31371=CIRCLE('',#80908,9.);
#31372=CIRCLE('',#80909,9.);
#31373=CIRCLE('',#80910,9.);
#31374=CIRCLE('',#80912,9.99999999999999);
#31375=CIRCLE('',#80913,10.);
#31376=CIRCLE('',#80914,10.);
#31377=CIRCLE('',#80916,9.49999999999999);
#31378=CIRCLE('',#80917,0.5);
#31379=CIRCLE('',#80919,9.50000000000001);
#31380=CIRCLE('',#80920,0.5);
#31381=CIRCLE('',#80922,0.5);
#31382=CIRCLE('',#80924,7.99999999999999);
#31383=CIRCLE('',#80925,7.99999999999999);
#31384=CIRCLE('',#80927,0.5);
#31385=CIRCLE('',#80928,7.5);
#31386=CIRCLE('',#80930,4.);
#31387=CIRCLE('',#80931,4.);
#31388=CIRCLE('',#80933,2.30850939467147);
#31389=CIRCLE('',#80934,2.30850939467147);
#31390=CIRCLE('',#80949,6.5);
#31391=CIRCLE('',#80953,26.49999955823);
#31392=CIRCLE('',#80954,1.);
#31393=CIRCLE('',#80955,27.5);
#31394=CIRCLE('',#80957,27.5);
#31395=CIRCLE('',#80959,12.4);
#31396=CIRCLE('',#80960,12.4);
#31397=CIRCLE('',#80962,2.);
#31398=CIRCLE('',#80963,2.);
#31399=CIRCLE('',#80965,27.);
#31400=CIRCLE('',#80966,0.5);
#31401=CIRCLE('',#80967,26.5);
#31402=CIRCLE('',#80969,27.);
#31403=CIRCLE('',#80971,15.93867390024);
#31404=CIRCLE('',#80972,14.68867390024);
#31405=CIRCLE('',#80976,14.5);
#31406=CIRCLE('',#80978,15.75);
#31407=CIRCLE('',#80983,13.9);
#31408=CIRCLE('',#80985,13.9);
#31409=CIRCLE('',#80988,13.9);
#31410=CIRCLE('',#80990,11.58843628952);
#31411=CIRCLE('',#80991,11.69981713671);
#31412=CIRCLE('',#80992,11.58843628952);
#31413=CIRCLE('',#80994,0.7);
#31414=CIRCLE('',#80995,11.40026076189);
#31415=CIRCLE('',#80997,1.3);
#31416=CIRCLE('',#80998,11.05);
#31417=CIRCLE('',#81002,11.05);
#31418=CIRCLE('',#81003,11.05);
#31419=CIRCLE('',#81004,11.05);
#31420=CIRCLE('',#81005,11.05);
#31421=CIRCLE('',#81006,11.05);
#31422=CIRCLE('',#81007,11.05);
#31423=CIRCLE('',#81008,11.05);
#31424=CIRCLE('',#81009,11.05);
#31425=CIRCLE('',#81010,11.05);
#31426=CIRCLE('',#81011,11.05);
#31427=CIRCLE('',#81012,11.05);
#31428=CIRCLE('',#81016,11.35);
#31429=CIRCLE('',#81017,11.35);
#31430=CIRCLE('',#81018,11.35);
#31431=CIRCLE('',#81019,11.35);
#31432=CIRCLE('',#81020,11.35);
#31433=CIRCLE('',#81021,11.35);
#31434=CIRCLE('',#81022,11.35);
#31435=CIRCLE('',#81023,11.35);
#31436=CIRCLE('',#81024,11.35);
#31437=CIRCLE('',#81025,11.35);
#31438=CIRCLE('',#81026,11.35);
#31439=CIRCLE('',#81027,11.35);
#31440=CIRCLE('',#81029,10.84999988564);
#31441=CIRCLE('',#81030,0.5);
#31442=CIRCLE('',#81032,9.84999999999999);
#31443=CIRCLE('',#81033,9.84999999999999);
#31444=CIRCLE('',#81035,10.15);
#31445=CIRCLE('',#81036,10.15);
#31446=CIRCLE('',#81038,1.);
#31447=CIRCLE('',#81039,11.6194313553);
#31448=CIRCLE('',#81041,1.);
#31449=CIRCLE('',#81042,11.88825353763);
#31450=CIRCLE('',#81043,11.88825353763);
#31451=CIRCLE('',#81045,12.);
#31452=CIRCLE('',#81047,12.25);
#31453=CIRCLE('',#81048,12.25);
#31454=CIRCLE('',#81050,12.75);
#31455=CIRCLE('',#81051,12.75);
#31456=CIRCLE('',#81053,13.1);
#31457=CIRCLE('',#81054,13.1);
#31458=CIRCLE('',#81056,13.7);
#31459=CIRCLE('',#81057,13.7);
#31460=CIRCLE('',#81058,13.7);
#31461=CIRCLE('',#81059,13.7);
#31462=CIRCLE('',#81060,13.7);
#31463=CIRCLE('',#81061,13.7);
#31464=CIRCLE('',#81063,13.4);
#31465=CIRCLE('',#81065,12.75);
#31466=CIRCLE('',#81066,12.75);
#31467=CIRCLE('',#81069,13.2);
#31468=CIRCLE('',#81071,13.2);
#31469=CIRCLE('',#81077,13.9);
#31470=CIRCLE('',#81083,13.07481294348);
#31471=CIRCLE('',#81085,15.44456161589);
#31472=CIRCLE('',#81086,15.74486371827);
#31473=CIRCLE('',#81088,13.39778838118);
#31474=CIRCLE('',#81089,13.04356099794);
#31475=CIRCLE('',#81091,15.75914761359);
#31476=CIRCLE('',#81092,15.45912298634);
#31477=CIRCLE('',#81094,8.729046339664);
#31478=CIRCLE('',#81096,13.07481294348);
#31479=CIRCLE('',#81098,15.36666793768);
#31480=CIRCLE('',#81099,15.66846302312);
#31481=CIRCLE('',#81101,13.39778838118);
#31482=CIRCLE('',#81102,13.04356099794);
#31483=CIRCLE('',#81104,15.71466619139);
#31484=CIRCLE('',#81105,15.41377577062);
#31485=CIRCLE('',#81107,8.729046339664);
#31486=CIRCLE('',#81109,13.04356099794);
#31487=CIRCLE('',#81110,13.39778838118);
#31488=CIRCLE('',#81112,15.52741876511);
#31489=CIRCLE('',#81114,13.07481294348);
#31490=CIRCLE('',#81116,15.3030873848);
#31491=CIRCLE('',#81117,15.60611205608);
#31492=CIRCLE('',#81119,8.72904633966399);
#31493=CIRCLE('',#81121,15.45912298634);
#31494=CIRCLE('',#81122,15.75914761359);
#31495=CIRCLE('',#81124,13.62844391363);
#31496=CIRCLE('',#81125,13.96784641621);
#31497=CIRCLE('',#81127,15.44456161589);
#31498=CIRCLE('',#81128,15.74486371827);
#31499=CIRCLE('',#81130,13.34857608537);
#31500=CIRCLE('',#81131,13.69491633808);
#31501=CIRCLE('',#81133,15.41377577062);
#31502=CIRCLE('',#81134,15.71466619139);
#31503=CIRCLE('',#81136,13.62844391363);
#31504=CIRCLE('',#81137,13.96784641621);
#31505=CIRCLE('',#81139,15.36666793768);
#31506=CIRCLE('',#81140,15.66846302312);
#31507=CIRCLE('',#81142,13.34857608537);
#31508=CIRCLE('',#81143,13.69491633808);
#31509=CIRCLE('',#81145,15.3030873848);
#31510=CIRCLE('',#81146,15.60611205608);
#31511=CIRCLE('',#81148,13.62844391363);
#31512=CIRCLE('',#81149,13.96784641621);
#31513=CIRCLE('',#81151,15.22282771061);
#31514=CIRCLE('',#81152,15.52741876511);
#31515=CIRCLE('',#81154,13.34857608537);
#31516=CIRCLE('',#81155,13.69491633808);
#31517=CIRCLE('',#81157,13.62844391363);
#31518=CIRCLE('',#81158,13.96784641621);
#31519=CIRCLE('',#81160,15.01114530963);
#31520=CIRCLE('',#81161,15.31994561044);
#31521=CIRCLE('',#81163,13.34857608537);
#31522=CIRCLE('',#81164,13.69491633808);
#31523=CIRCLE('',#81166,15.12562340887);
#31524=CIRCLE('',#81167,15.4321331483);
#31525=CIRCLE('',#81169,13.69491633808);
#31526=CIRCLE('',#81171,14.72869592011);
#31527=CIRCLE('',#81172,15.0432953008);
#31528=CIRCLE('',#81174,13.96784641621);
#31529=CIRCLE('',#81175,13.62844391363);
#31530=CIRCLE('',#81177,15.19048167462);
#31531=CIRCLE('',#81178,14.87899470754);
#31532=CIRCLE('',#81180,8.729046339664);
#31533=CIRCLE('',#81182,13.1066579839);
#31534=CIRCLE('',#81183,13.45922484792);
#31535=CIRCLE('',#81185,15.28837739941);
#31536=CIRCLE('',#81186,15.59168796208);
#31537=CIRCLE('',#81188,13.14156510873);
#31538=CIRCLE('',#81190,15.20475200412);
#31539=CIRCLE('',#81191,15.50969804693);
#31540=CIRCLE('',#81193,8.729046339664);
#31541=CIRCLE('',#81195,13.1066579839);
#31542=CIRCLE('',#81196,13.45922484792);
#31543=CIRCLE('',#81198,15.40566400734);
#31544=CIRCLE('',#81199,15.70670982437);
#31545=CIRCLE('',#81201,13.14156510873);
#31546=CIRCLE('',#81203,15.35527542921);
#31547=CIRCLE('',#81204,15.65729010739);
#31548=CIRCLE('',#81206,8.729046339664);
#31549=CIRCLE('',#81208,13.1066579839);
#31550=CIRCLE('',#81209,13.45922484792);
#31551=CIRCLE('',#81211,15.45750573369);
#31552=CIRCLE('',#81212,15.75756115352);
#31553=CIRCLE('',#81214,12.78023800666);
#31554=CIRCLE('',#81215,13.14156510873);
#31555=CIRCLE('',#81217,15.43970477396);
#31556=CIRCLE('',#81218,15.7400995393);
#31557=CIRCLE('',#81220,8.729046339664);
#31558=CIRCLE('',#81222,13.1066579839);
#31559=CIRCLE('',#81223,13.45922484792);
#31560=CIRCLE('',#81225,15.44456161589);
#31561=CIRCLE('',#81226,15.74486371827);
#31562=CIRCLE('',#81228,12.78023800666);
#31563=CIRCLE('',#81229,13.14156510873);
#31564=CIRCLE('',#81231,15.45912298634);
#31565=CIRCLE('',#81232,15.75914761359);
#31566=CIRCLE('',#81234,13.1066579839);
#31567=CIRCLE('',#81235,13.45922484792);
#31568=CIRCLE('',#81237,15.36666793768);
#31569=CIRCLE('',#81238,15.66846302312);
#31570=CIRCLE('',#81240,13.14156510873);
#31571=CIRCLE('',#81242,15.41377577062);
#31572=CIRCLE('',#81243,15.71466619139);
#31573=CIRCLE('',#81245,8.72904633966401);
#31574=CIRCLE('',#81247,13.1066579839);
#31575=CIRCLE('',#81248,13.45922484792);
#31576=CIRCLE('',#81250,15.22282771061);
#31577=CIRCLE('',#81251,15.52741876511);
#31578=CIRCLE('',#81253,13.14156510873);
#31579=CIRCLE('',#81255,15.3030873848);
#31580=CIRCLE('',#81256,15.60611205608);
#31581=CIRCLE('',#81258,8.729046339664);
#31582=CIRCLE('',#81260,13.1066579839);
#31583=CIRCLE('',#81261,13.45922484792);
#31584=CIRCLE('',#81263,15.3030873848);
#31585=CIRCLE('',#81264,15.60611205608);
#31586=CIRCLE('',#81266,13.14156510873);
#31587=CIRCLE('',#81268,15.22282771061);
#31588=CIRCLE('',#81269,15.52741876511);
#31589=CIRCLE('',#81271,8.729046339664);
#31590=CIRCLE('',#81273,13.1066579839);
#31591=CIRCLE('',#81274,13.45922484792);
#31592=CIRCLE('',#81276,15.41377577062);
#31593=CIRCLE('',#81277,15.71466619139);
#31594=CIRCLE('',#81279,13.14156510873);
#31595=CIRCLE('',#81281,15.36666793768);
#31596=CIRCLE('',#81282,15.66846302312);
#31597=CIRCLE('',#81284,8.729046339664);
#31598=CIRCLE('',#81286,15.45912298634);
#31599=CIRCLE('',#81287,15.75914761359);
#31600=CIRCLE('',#81289,12.78023800666);
#31601=CIRCLE('',#81290,13.14156510873);
#31602=CIRCLE('',#81292,15.44456161589);
#31603=CIRCLE('',#81293,15.74486371827);
#31604=CIRCLE('',#81295,13.1066579839);
#31605=CIRCLE('',#81296,13.45922484792);
#31606=CIRCLE('',#81298,15.45912298634);
#31607=CIRCLE('',#81299,15.75914761359);
#31608=CIRCLE('',#81301,14.1185864557);
#31609=CIRCLE('',#81302,14.4464782389);
#31610=CIRCLE('',#81304,15.44456161589);
#31611=CIRCLE('',#81305,15.74486371827);
#31612=CIRCLE('',#81307,13.88468521454);
#31613=CIRCLE('',#81308,14.21797220095);
#31614=CIRCLE('',#81310,15.41377577062);
#31615=CIRCLE('',#81311,15.71466619139);
#31616=CIRCLE('',#81313,14.1185864557);
#31617=CIRCLE('',#81314,14.4464782389);
#31618=CIRCLE('',#81316,15.36666793768);
#31619=CIRCLE('',#81317,15.66846302312);
#31620=CIRCLE('',#81319,13.88468521454);
#31621=CIRCLE('',#81320,14.21797220095);
#31622=CIRCLE('',#81322,15.3030873848);
#31623=CIRCLE('',#81323,15.60611205608);
#31624=CIRCLE('',#81325,14.1185864557);
#31625=CIRCLE('',#81326,14.4464782389);
#31626=CIRCLE('',#81328,15.22282771061);
#31627=CIRCLE('',#81329,15.52741876511);
#31628=CIRCLE('',#81331,13.88468521454);
#31629=CIRCLE('',#81332,14.21797220095);
#31630=CIRCLE('',#81334,15.12562340887);
#31631=CIRCLE('',#81335,15.4321331483);
#31632=CIRCLE('',#81337,14.1185864557);
#31633=CIRCLE('',#81338,14.4464782389);
#31634=CIRCLE('',#81340,15.01114530963);
#31635=CIRCLE('',#81341,15.31994561044);
#31636=CIRCLE('',#81343,13.88468521454);
#31637=CIRCLE('',#81344,14.21797220095);
#31638=CIRCLE('',#81346,14.87899470754);
#31639=CIRCLE('',#81347,15.19048167462);
#31640=CIRCLE('',#81349,14.1185864557);
#31641=CIRCLE('',#81350,14.4464782389);
#31642=CIRCLE('',#81352,14.72869592011);
#31643=CIRCLE('',#81353,15.0432953008);
#31644=CIRCLE('',#81355,13.88468521454);
#31645=CIRCLE('',#81356,14.21797220095);
#31646=CIRCLE('',#81358,14.87786051511);
#31647=CIRCLE('',#81359,14.55968693025);
#31648=CIRCLE('',#81361,14.4464782389);
#31649=CIRCLE('',#81362,14.1185864557);
#31650=CIRCLE('',#81364,14.37130764777);
#31651=CIRCLE('',#81365,14.69356095393);
#31652=CIRCLE('',#81367,14.21797220095);
#31653=CIRCLE('',#81368,13.88468521454);
#31654=CIRCLE('',#81370,8.72904633966401);
#31655=CIRCLE('',#81372,13.68153805341);
#31656=CIRCLE('',#81373,14.01965525635);
#31657=CIRCLE('',#81375,14.8504034796);
#31658=CIRCLE('',#81376,15.16247781555);
#31659=CIRCLE('',#81378,13.75139023906);
#31660=CIRCLE('',#81380,14.6964105654);
#31661=CIRCLE('',#81381,15.01168656437);
#31662=CIRCLE('',#81383,8.729046339664);
#31663=CIRCLE('',#81385,13.68153805341);
#31664=CIRCLE('',#81386,14.01965525635);
#31665=CIRCLE('',#81388,15.10412140798);
#31666=CIRCLE('',#81389,15.41105880551);
#31667=CIRCLE('',#81391,13.40650899776);
#31668=CIRCLE('',#81392,13.75139023906);
#31669=CIRCLE('',#81394,14.98614304973);
#31670=CIRCLE('',#81395,15.29544813031);
#31671=CIRCLE('',#81397,13.68153805341);
#31672=CIRCLE('',#81398,14.01965525635);
#31673=CIRCLE('',#81400,15.28837739941);
#31674=CIRCLE('',#81401,15.59168796208);
#31675=CIRCLE('',#81403,13.40650899776);
#31676=CIRCLE('',#81404,13.75139023906);
#31677=CIRCLE('',#81406,15.20475200412);
#31678=CIRCLE('',#81407,15.50969804693);
#31679=CIRCLE('',#81409,13.68153805341);
#31680=CIRCLE('',#81410,14.01965525635);
#31681=CIRCLE('',#81412,15.40566400734);
#31682=CIRCLE('',#81413,15.70670982437);
#31683=CIRCLE('',#81415,13.40650899776);
#31684=CIRCLE('',#81416,13.75139023906);
#31685=CIRCLE('',#81418,15.35527542921);
#31686=CIRCLE('',#81419,15.65729010739);
#31687=CIRCLE('',#81421,13.68153805341);
#31688=CIRCLE('',#81422,14.01965525635);
#31689=CIRCLE('',#81424,15.45750573369);
#31690=CIRCLE('',#81425,15.75756115352);
#31691=CIRCLE('',#81427,13.40650899776);
#31692=CIRCLE('',#81428,13.75139023906);
#31693=CIRCLE('',#81430,15.43970477396);
#31694=CIRCLE('',#81431,15.7400995393);
#31695=CIRCLE('',#81433,13.68153805341);
#31696=CIRCLE('',#81434,14.01965525635);
#31697=CIRCLE('',#81436,15.44456161589);
#31698=CIRCLE('',#81437,15.74486371827);
#31699=CIRCLE('',#81439,13.40650899776);
#31700=CIRCLE('',#81440,13.75139023906);
#31701=CIRCLE('',#81442,15.45912298634);
#31702=CIRCLE('',#81443,15.75914761359);
#31703=CIRCLE('',#81445,13.68153805341);
#31704=CIRCLE('',#81446,14.01965525635);
#31705=CIRCLE('',#81448,15.36666793768);
#31706=CIRCLE('',#81449,15.66846302312);
#31707=CIRCLE('',#81451,13.40650899776);
#31708=CIRCLE('',#81452,13.75139023906);
#31709=CIRCLE('',#81454,15.41377577062);
#31710=CIRCLE('',#81455,15.71466619139);
#31711=CIRCLE('',#81457,13.68153805341);
#31712=CIRCLE('',#81458,14.01965525635);
#31713=CIRCLE('',#81460,15.22282771061);
#31714=CIRCLE('',#81461,15.52741876511);
#31715=CIRCLE('',#81463,13.40650899776);
#31716=CIRCLE('',#81464,13.75139023906);
#31717=CIRCLE('',#81466,15.3030873848);
#31718=CIRCLE('',#81467,15.60611205608);
#31719=CIRCLE('',#81469,13.68153805341);
#31720=CIRCLE('',#81470,14.01965525635);
#31721=CIRCLE('',#81472,15.01114530963);
#31722=CIRCLE('',#81473,15.31994561044);
#31723=CIRCLE('',#81475,13.40650899776);
#31724=CIRCLE('',#81476,13.75139023906);
#31725=CIRCLE('',#81478,15.12562340887);
#31726=CIRCLE('',#81479,15.4321331483);
#31727=CIRCLE('',#81481,13.68153805341);
#31728=CIRCLE('',#81482,14.01965525635);
#31729=CIRCLE('',#81484,14.72869592011);
#31730=CIRCLE('',#81485,15.0432953008);
#31731=CIRCLE('',#81487,13.75139023906);
#31732=CIRCLE('',#81489,14.87899470754);
#31733=CIRCLE('',#81490,15.19048167462);
#31734=CIRCLE('',#81492,8.729046339664);
#31735=CIRCLE('',#81494,13.68153805341);
#31736=CIRCLE('',#81495,14.01965525635);
#31737=CIRCLE('',#81497,14.87899470754);
#31738=CIRCLE('',#81498,15.19048167462);
#31739=CIRCLE('',#81500,13.75139023906);
#31740=CIRCLE('',#81502,14.72869592011);
#31741=CIRCLE('',#81503,15.0432953008);
#31742=CIRCLE('',#81505,8.72904633966401);
#31743=CIRCLE('',#81507,15.12562340887);
#31744=CIRCLE('',#81508,15.4321331483);
#31745=CIRCLE('',#81510,13.40650899776);
#31746=CIRCLE('',#81511,13.75139023906);
#31747=CIRCLE('',#81513,15.01114530963);
#31748=CIRCLE('',#81514,15.31994561044);
#31749=CIRCLE('',#81516,13.68153805341);
#31750=CIRCLE('',#81517,14.01965525635);
#31751=CIRCLE('',#81519,15.3030873848);
#31752=CIRCLE('',#81520,15.60611205608);
#31753=CIRCLE('',#81522,13.40650899776);
#31754=CIRCLE('',#81523,13.75139023906);
#31755=CIRCLE('',#81525,15.22282771061);
#31756=CIRCLE('',#81526,15.52741876511);
#31757=CIRCLE('',#81528,13.68153805341);
#31758=CIRCLE('',#81529,14.01965525635);
#31759=CIRCLE('',#81531,15.41377577062);
#31760=CIRCLE('',#81532,15.71466619139);
#31761=CIRCLE('',#81534,13.40650899776);
#31762=CIRCLE('',#81535,13.75139023906);
#31763=CIRCLE('',#81537,15.36666793768);
#31764=CIRCLE('',#81538,15.66846302312);
#31765=CIRCLE('',#81540,13.68153805341);
#31766=CIRCLE('',#81541,14.01965525635);
#31767=CIRCLE('',#81543,15.45912298634);
#31768=CIRCLE('',#81544,15.75914761359);
#31769=CIRCLE('',#81546,13.40650899776);
#31770=CIRCLE('',#81547,13.75139023906);
#31771=CIRCLE('',#81549,15.44456161589);
#31772=CIRCLE('',#81550,15.74486371827);
#31773=CIRCLE('',#81552,13.68153805341);
#31774=CIRCLE('',#81553,14.01965525635);
#31775=CIRCLE('',#81555,15.45912298634);
#31776=CIRCLE('',#81556,15.75914761359);
#31777=CIRCLE('',#81558,14.52358370055);
#31778=CIRCLE('',#81559,14.84253123652);
#31779=CIRCLE('',#81561,15.44456161589);
#31780=CIRCLE('',#81562,15.74486371827);
#31781=CIRCLE('',#81564,14.33124152008);
#31782=CIRCLE('',#81565,14.65437591667);
#31783=CIRCLE('',#81567,15.41377577062);
#31784=CIRCLE('',#81568,15.71466619139);
#31785=CIRCLE('',#81570,14.52358370055);
#31786=CIRCLE('',#81571,14.84253123652);
#31787=CIRCLE('',#81573,15.36666793768);
#31788=CIRCLE('',#81574,15.66846302312);
#31789=CIRCLE('',#81576,14.33124152008);
#31790=CIRCLE('',#81577,14.65437591667);
#31791=CIRCLE('',#81579,15.3030873848);
#31792=CIRCLE('',#81580,15.60611205608);
#31793=CIRCLE('',#81582,14.52358370055);
#31794=CIRCLE('',#81583,14.84253123652);
#31795=CIRCLE('',#81585,15.22282771061);
#31796=CIRCLE('',#81586,15.52741876511);
#31797=CIRCLE('',#81588,14.33124152008);
#31798=CIRCLE('',#81589,14.65437591667);
#31799=CIRCLE('',#81591,15.12562340887);
#31800=CIRCLE('',#81592,15.4321331483);
#31801=CIRCLE('',#81594,14.52358370055);
#31802=CIRCLE('',#81595,14.84253123652);
#31803=CIRCLE('',#81597,15.01114530963);
#31804=CIRCLE('',#81598,15.31994561044);
#31805=CIRCLE('',#81600,14.33124152008);
#31806=CIRCLE('',#81601,14.65437591667);
#31807=CIRCLE('',#81603,14.87899470754);
#31808=CIRCLE('',#81604,15.19048167462);
#31809=CIRCLE('',#81606,14.52358370055);
#31810=CIRCLE('',#81607,14.84253123652);
#31811=CIRCLE('',#81609,14.72869592011);
#31812=CIRCLE('',#81610,15.0432953008);
#31813=CIRCLE('',#81612,14.33124152008);
#31814=CIRCLE('',#81613,14.65437591667);
#31815=CIRCLE('',#81615,14.55968693025);
#31816=CIRCLE('',#81616,14.87786051511);
#31817=CIRCLE('',#81618,14.52358370055);
#31818=CIRCLE('',#81619,14.84253123652);
#31819=CIRCLE('',#81621,14.37130764777);
#31820=CIRCLE('',#81622,14.69356095393);
#31821=CIRCLE('',#81624,14.33124152008);
#31822=CIRCLE('',#81625,14.65437591667);
#31823=CIRCLE('',#81627,8.729046339664);
#31824=CIRCLE('',#81629,14.16278516066);
#31825=CIRCLE('',#81630,14.48967679098);
#31826=CIRCLE('',#81632,14.52358370055);
#31827=CIRCLE('',#81633,14.84253123652);
#31828=CIRCLE('',#81635,13.93321511737);
#31829=CIRCLE('',#81636,14.26536832707);
#31830=CIRCLE('',#81638,14.33124152008);
#31831=CIRCLE('',#81639,14.65437591667);
#31832=CIRCLE('',#81641,14.16278516066);
#31833=CIRCLE('',#81642,14.48967679098);
#31834=CIRCLE('',#81644,14.8504034796);
#31835=CIRCLE('',#81645,15.16247781555);
#31836=CIRCLE('',#81647,13.93321511737);
#31837=CIRCLE('',#81648,14.26536832707);
#31838=CIRCLE('',#81650,14.6964105654);
#31839=CIRCLE('',#81651,15.01168656437);
#31840=CIRCLE('',#81653,14.16278516066);
#31841=CIRCLE('',#81654,14.48967679098);
#31842=CIRCLE('',#81656,15.10412140798);
#31843=CIRCLE('',#81657,15.41105880551);
#31844=CIRCLE('',#81659,13.93321511737);
#31845=CIRCLE('',#81660,14.26536832707);
#31846=CIRCLE('',#81662,14.98614304973);
#31847=CIRCLE('',#81663,15.29544813031);
#31848=CIRCLE('',#81665,14.16278516066);
#31849=CIRCLE('',#81666,14.48967679098);
#31850=CIRCLE('',#81668,15.28837739941);
#31851=CIRCLE('',#81669,15.59168796208);
#31852=CIRCLE('',#81671,13.93321511737);
#31853=CIRCLE('',#81672,14.26536832707);
#31854=CIRCLE('',#81674,15.20475200412);
#31855=CIRCLE('',#81675,15.50969804693);
#31856=CIRCLE('',#81677,14.16278516066);
#31857=CIRCLE('',#81678,14.48967679098);
#31858=CIRCLE('',#81680,15.40566400734);
#31859=CIRCLE('',#81681,15.70670982437);
#31860=CIRCLE('',#81683,13.93321511737);
#31861=CIRCLE('',#81684,14.26536832707);
#31862=CIRCLE('',#81686,15.35527542921);
#31863=CIRCLE('',#81687,15.65729010739);
#31864=CIRCLE('',#81689,14.16278516066);
#31865=CIRCLE('',#81690,14.48967679098);
#31866=CIRCLE('',#81692,15.45750573369);
#31867=CIRCLE('',#81693,15.75756115352);
#31868=CIRCLE('',#81695,13.93321511737);
#31869=CIRCLE('',#81696,14.26536832707);
#31870=CIRCLE('',#81698,15.43970477396);
#31871=CIRCLE('',#81699,15.7400995393);
#31872=CIRCLE('',#81701,14.16278516066);
#31873=CIRCLE('',#81702,14.48967679098);
#31874=CIRCLE('',#81704,15.44456161589);
#31875=CIRCLE('',#81705,15.74486371827);
#31876=CIRCLE('',#81707,13.93321511737);
#31877=CIRCLE('',#81708,14.26536832707);
#31878=CIRCLE('',#81710,15.45912298634);
#31879=CIRCLE('',#81711,15.75914761359);
#31880=CIRCLE('',#81713,14.16278516066);
#31881=CIRCLE('',#81714,14.48967679098);
#31882=CIRCLE('',#81716,15.36666793768);
#31883=CIRCLE('',#81717,15.66846302312);
#31884=CIRCLE('',#81719,13.93321511737);
#31885=CIRCLE('',#81720,14.26536832707);
#31886=CIRCLE('',#81722,15.41377577062);
#31887=CIRCLE('',#81723,15.71466619139);
#31888=CIRCLE('',#81725,14.16278516066);
#31889=CIRCLE('',#81726,14.48967679098);
#31890=CIRCLE('',#81728,15.22282771061);
#31891=CIRCLE('',#81729,15.52741876511);
#31892=CIRCLE('',#81731,13.93321511737);
#31893=CIRCLE('',#81732,14.26536832707);
#31894=CIRCLE('',#81734,15.3030873848);
#31895=CIRCLE('',#81735,15.60611205608);
#31896=CIRCLE('',#81737,14.16278516066);
#31897=CIRCLE('',#81738,14.48967679098);
#31898=CIRCLE('',#81740,15.01114530963);
#31899=CIRCLE('',#81741,15.31994561044);
#31900=CIRCLE('',#81743,13.93321511737);
#31901=CIRCLE('',#81744,14.26536832707);
#31902=CIRCLE('',#81746,15.12562340887);
#31903=CIRCLE('',#81747,15.4321331483);
#31904=CIRCLE('',#81749,14.16278516066);
#31905=CIRCLE('',#81750,14.48967679098);
#31906=CIRCLE('',#81752,14.72869592011);
#31907=CIRCLE('',#81753,15.0432953008);
#31908=CIRCLE('',#81755,13.93321511737);
#31909=CIRCLE('',#81756,14.26536832707);
#31910=CIRCLE('',#81758,14.87899470754);
#31911=CIRCLE('',#81759,15.19048167462);
#31912=CIRCLE('',#81761,14.55968693025);
#31913=CIRCLE('',#81762,14.87786051511);
#31914=CIRCLE('',#81764,14.16278516066);
#31915=CIRCLE('',#81765,14.48967679098);
#31916=CIRCLE('',#81767,14.37130764777);
#31917=CIRCLE('',#81768,14.69356095393);
#31918=CIRCLE('',#81770,13.93321511737);
#31919=CIRCLE('',#81771,14.26536832707);
#31920=CIRCLE('',#81773,8.72904633966401);
#31921=CIRCLE('',#81775,14.16278516066);
#31922=CIRCLE('',#81776,14.48967679098);
#31923=CIRCLE('',#81778,14.55968693025);
#31924=CIRCLE('',#81779,14.87786051511);
#31925=CIRCLE('',#81781,13.93321511737);
#31926=CIRCLE('',#81782,14.26536832707);
#31927=CIRCLE('',#81784,14.37130764777);
#31928=CIRCLE('',#81785,14.69356095393);
#31929=CIRCLE('',#81787,8.72904633966401);
#31930=CIRCLE('',#81789,14.87899470754);
#31931=CIRCLE('',#81790,15.19048167462);
#31932=CIRCLE('',#81792,13.93321511737);
#31933=CIRCLE('',#81793,14.26536832707);
#31934=CIRCLE('',#81795,14.72869592011);
#31935=CIRCLE('',#81796,15.0432953008);
#31936=CIRCLE('',#81798,14.16278516066);
#31937=CIRCLE('',#81799,14.48967679098);
#31938=CIRCLE('',#81801,15.12562340887);
#31939=CIRCLE('',#81802,15.4321331483);
#31940=CIRCLE('',#81804,13.93321511737);
#31941=CIRCLE('',#81805,14.26536832707);
#31942=CIRCLE('',#81807,15.01114530963);
#31943=CIRCLE('',#81808,15.31994561044);
#31944=CIRCLE('',#81810,14.16278516066);
#31945=CIRCLE('',#81811,14.48967679098);
#31946=CIRCLE('',#81813,15.3030873848);
#31947=CIRCLE('',#81814,15.60611205608);
#31948=CIRCLE('',#81816,13.93321511737);
#31949=CIRCLE('',#81817,14.26536832707);
#31950=CIRCLE('',#81819,15.22282771061);
#31951=CIRCLE('',#81820,15.52741876511);
#31952=CIRCLE('',#81822,14.16278516066);
#31953=CIRCLE('',#81823,14.48967679098);
#31954=CIRCLE('',#81825,15.41377577062);
#31955=CIRCLE('',#81826,15.71466619139);
#31956=CIRCLE('',#81828,13.93321511737);
#31957=CIRCLE('',#81829,14.26536832707);
#31958=CIRCLE('',#81831,15.36666793768);
#31959=CIRCLE('',#81832,15.66846302312);
#31960=CIRCLE('',#81834,14.16278516066);
#31961=CIRCLE('',#81835,14.48967679098);
#31962=CIRCLE('',#81837,15.45912298634);
#31963=CIRCLE('',#81838,15.75914761359);
#31964=CIRCLE('',#81840,13.93321511737);
#31965=CIRCLE('',#81841,14.26536832707);
#31966=CIRCLE('',#81843,15.44456161589);
#31967=CIRCLE('',#81844,15.74486371827);
#31968=CIRCLE('',#81846,14.16278516066);
#31969=CIRCLE('',#81847,14.48967679098);
#31970=CIRCLE('',#81849,15.45912298634);
#31971=CIRCLE('',#81850,15.75914761359);
#31972=CIRCLE('',#81852,14.8504034796);
#31973=CIRCLE('',#81853,15.16247781555);
#31974=CIRCLE('',#81855,15.44456161589);
#31975=CIRCLE('',#81856,15.74486371827);
#31976=CIRCLE('',#81858,14.6964105654);
#31977=CIRCLE('',#81859,15.01168656437);
#31978=CIRCLE('',#81861,15.41377577062);
#31979=CIRCLE('',#81862,15.71466619139);
#31980=CIRCLE('',#81864,14.8504034796);
#31981=CIRCLE('',#81865,15.16247781555);
#31982=CIRCLE('',#81867,15.36666793768);
#31983=CIRCLE('',#81868,15.66846302312);
#31984=CIRCLE('',#81870,14.6964105654);
#31985=CIRCLE('',#81871,15.01168656437);
#31986=CIRCLE('',#81873,15.3030873848);
#31987=CIRCLE('',#81874,15.60611205608);
#31988=CIRCLE('',#81876,14.8504034796);
#31989=CIRCLE('',#81877,15.16247781555);
#31990=CIRCLE('',#81879,15.22282771061);
#31991=CIRCLE('',#81880,15.52741876511);
#31992=CIRCLE('',#81882,14.6964105654);
#31993=CIRCLE('',#81883,15.01168656437);
#31994=CIRCLE('',#81885,15.12562340887);
#31995=CIRCLE('',#81886,15.4321331483);
#31996=CIRCLE('',#81888,14.8504034796);
#31997=CIRCLE('',#81889,15.16247781555);
#31998=CIRCLE('',#81891,15.01114530963);
#31999=CIRCLE('',#81892,15.31994561044);
#32000=CIRCLE('',#81894,14.6964105654);
#32001=CIRCLE('',#81895,15.01168656437);
#32002=CIRCLE('',#81897,14.87899470754);
#32003=CIRCLE('',#81898,15.19048167462);
#32004=CIRCLE('',#81900,14.8504034796);
#32005=CIRCLE('',#81901,15.16247781555);
#32006=CIRCLE('',#81903,14.72869592011);
#32007=CIRCLE('',#81904,15.0432953008);
#32008=CIRCLE('',#81906,14.6964105654);
#32009=CIRCLE('',#81907,15.01168656437);
#32010=CIRCLE('',#81909,14.55968693025);
#32011=CIRCLE('',#81910,14.87786051511);
#32012=CIRCLE('',#81912,14.8504034796);
#32013=CIRCLE('',#81913,15.16247781555);
#32014=CIRCLE('',#81915,14.37130764777);
#32015=CIRCLE('',#81916,14.69356095393);
#32016=CIRCLE('',#81918,14.6964105654);
#32017=CIRCLE('',#81919,15.01168656437);
#32018=CIRCLE('',#81921,14.55968693025);
#32019=CIRCLE('',#81922,14.87786051511);
#32020=CIRCLE('',#81924,15.10412140798);
#32021=CIRCLE('',#81925,15.41105880551);
#32022=CIRCLE('',#81927,14.37130764777);
#32023=CIRCLE('',#81928,14.69356095393);
#32024=CIRCLE('',#81930,14.98614304973);
#32025=CIRCLE('',#81931,15.29544813031);
#32026=CIRCLE('',#81933,14.55968693025);
#32027=CIRCLE('',#81934,14.87786051511);
#32028=CIRCLE('',#81936,15.28837739941);
#32029=CIRCLE('',#81937,15.59168796208);
#32030=CIRCLE('',#81939,14.37130764777);
#32031=CIRCLE('',#81940,14.69356095393);
#32032=CIRCLE('',#81942,15.20475200412);
#32033=CIRCLE('',#81943,15.50969804693);
#32034=CIRCLE('',#81945,14.55968693025);
#32035=CIRCLE('',#81946,14.87786051511);
#32036=CIRCLE('',#81948,15.40566400734);
#32037=CIRCLE('',#81949,15.70670982437);
#32038=CIRCLE('',#81951,14.37130764777);
#32039=CIRCLE('',#81952,14.69356095393);
#32040=CIRCLE('',#81954,15.35527542921);
#32041=CIRCLE('',#81955,15.65729010739);
#32042=CIRCLE('',#81957,14.55968693025);
#32043=CIRCLE('',#81958,14.87786051511);
#32044=CIRCLE('',#81960,15.45750573369);
#32045=CIRCLE('',#81961,15.75756115352);
#32046=CIRCLE('',#81963,14.37130764777);
#32047=CIRCLE('',#81964,14.69356095393);
#32048=CIRCLE('',#81966,15.43970477396);
#32049=CIRCLE('',#81967,15.7400995393);
#32050=CIRCLE('',#81969,14.55968693025);
#32051=CIRCLE('',#81970,14.87786051511);
#32052=CIRCLE('',#81972,15.44456161589);
#32053=CIRCLE('',#81973,15.74486371827);
#32054=CIRCLE('',#81975,14.37130764777);
#32055=CIRCLE('',#81976,14.69356095393);
#32056=CIRCLE('',#81978,15.45912298634);
#32057=CIRCLE('',#81979,15.75914761359);
#32058=CIRCLE('',#81981,14.55968693025);
#32059=CIRCLE('',#81982,14.87786051511);
#32060=CIRCLE('',#81984,15.36666793768);
#32061=CIRCLE('',#81985,15.66846302312);
#32062=CIRCLE('',#81987,14.37130764777);
#32063=CIRCLE('',#81988,14.69356095393);
#32064=CIRCLE('',#81990,15.41377577062);
#32065=CIRCLE('',#81991,15.71466619139);
#32066=CIRCLE('',#81993,14.55968693025);
#32067=CIRCLE('',#81994,14.87786051511);
#32068=CIRCLE('',#81996,15.22282771061);
#32069=CIRCLE('',#81997,15.52741876511);
#32070=CIRCLE('',#81999,14.37130764777);
#32071=CIRCLE('',#82000,14.69356095393);
#32072=CIRCLE('',#82002,15.3030873848);
#32073=CIRCLE('',#82003,15.60611205608);
#32074=CIRCLE('',#82005,14.55968693025);
#32075=CIRCLE('',#82006,14.87786051511);
#32076=CIRCLE('',#82008,15.01114530963);
#32077=CIRCLE('',#82009,15.31994561044);
#32078=CIRCLE('',#82011,14.37130764777);
#32079=CIRCLE('',#82012,14.69356095393);
#32080=CIRCLE('',#82014,15.12562340887);
#32081=CIRCLE('',#82015,15.4321331483);
#32082=CIRCLE('',#82017,14.55968693025);
#32083=CIRCLE('',#82018,14.87786051511);
#32084=CIRCLE('',#82020,14.72869592011);
#32085=CIRCLE('',#82021,15.0432953008);
#32086=CIRCLE('',#82023,14.37130764777);
#32087=CIRCLE('',#82024,14.69356095393);
#32088=CIRCLE('',#82026,14.87899470754);
#32089=CIRCLE('',#82027,15.19048167462);
#32090=CIRCLE('',#82029,14.55968693025);
#32091=CIRCLE('',#82030,14.87786051511);
#32092=CIRCLE('',#82032,14.37130764777);
#32093=CIRCLE('',#82033,14.69356095393);
#32094=CIRCLE('',#82035,14.37130764777);
#32095=CIRCLE('',#82036,14.69356095393);
#32096=CIRCLE('',#82038,14.55968693025);
#32097=CIRCLE('',#82039,14.87786051511);
#32098=CIRCLE('',#82041,14.87899470754);
#32099=CIRCLE('',#82042,15.19048167462);
#32100=CIRCLE('',#82044,14.37130764777);
#32101=CIRCLE('',#82045,14.69356095393);
#32102=CIRCLE('',#82047,14.72869592011);
#32103=CIRCLE('',#82048,15.0432953008);
#32104=CIRCLE('',#82050,14.55968693025);
#32105=CIRCLE('',#82051,14.87786051511);
#32106=CIRCLE('',#82053,15.12562340887);
#32107=CIRCLE('',#82054,15.4321331483);
#32108=CIRCLE('',#82056,14.37130764777);
#32109=CIRCLE('',#82057,14.69356095393);
#32110=CIRCLE('',#82059,15.01114530963);
#32111=CIRCLE('',#82060,15.31994561044);
#32112=CIRCLE('',#82062,14.55968693025);
#32113=CIRCLE('',#82063,14.87786051511);
#32114=CIRCLE('',#82065,15.3030873848);
#32115=CIRCLE('',#82066,15.60611205608);
#32116=CIRCLE('',#82068,14.37130764777);
#32117=CIRCLE('',#82069,14.69356095393);
#32118=CIRCLE('',#82071,15.22282771061);
#32119=CIRCLE('',#82072,15.52741876511);
#32120=CIRCLE('',#82074,14.55968693025);
#32121=CIRCLE('',#82075,14.87786051511);
#32122=CIRCLE('',#82077,15.41377577062);
#32123=CIRCLE('',#82078,15.71466619139);
#32124=CIRCLE('',#82080,14.37130764777);
#32125=CIRCLE('',#82081,14.69356095393);
#32126=CIRCLE('',#82083,15.36666793768);
#32127=CIRCLE('',#82084,15.66846302312);
#32128=CIRCLE('',#82086,14.55968693025);
#32129=CIRCLE('',#82087,14.87786051511);
#32130=CIRCLE('',#82089,15.45912298634);
#32131=CIRCLE('',#82090,15.75914761359);
#32132=CIRCLE('',#82092,14.37130764777);
#32133=CIRCLE('',#82093,14.69356095393);
#32134=CIRCLE('',#82095,15.44456161589);
#32135=CIRCLE('',#82096,15.74486371827);
#32136=CIRCLE('',#82098,14.55968693025);
#32137=CIRCLE('',#82099,14.87786051511);
#32138=CIRCLE('',#82101,15.10412140798);
#32139=CIRCLE('',#82102,15.41105880551);
#32140=CIRCLE('',#82104,15.44456161589);
#32141=CIRCLE('',#82105,15.74486371827);
#32142=CIRCLE('',#82107,14.98614304973);
#32143=CIRCLE('',#82108,15.29544813031);
#32144=CIRCLE('',#82110,15.45912298634);
#32145=CIRCLE('',#82111,15.75914761359);
#32146=CIRCLE('',#82113,15.41377577062);
#32147=CIRCLE('',#82114,15.71466619139);
#32148=CIRCLE('',#82116,15.10412140798);
#32149=CIRCLE('',#82117,15.41105880551);
#32150=CIRCLE('',#82119,15.36666793768);
#32151=CIRCLE('',#82120,15.66846302312);
#32152=CIRCLE('',#82122,14.98614304973);
#32153=CIRCLE('',#82123,15.29544813031);
#32154=CIRCLE('',#82125,15.3030873848);
#32155=CIRCLE('',#82126,15.60611205608);
#32156=CIRCLE('',#82128,15.10412140798);
#32157=CIRCLE('',#82129,15.41105880551);
#32158=CIRCLE('',#82131,15.22282771061);
#32159=CIRCLE('',#82132,15.52741876511);
#32160=CIRCLE('',#82134,14.98614304973);
#32161=CIRCLE('',#82135,15.29544813031);
#32162=CIRCLE('',#82137,15.12562340887);
#32163=CIRCLE('',#82138,15.4321331483);
#32164=CIRCLE('',#82140,15.10412140798);
#32165=CIRCLE('',#82141,15.41105880551);
#32166=CIRCLE('',#82143,15.01114530963);
#32167=CIRCLE('',#82144,15.31994561044);
#32168=CIRCLE('',#82146,14.98614304973);
#32169=CIRCLE('',#82147,15.29544813031);
#32170=CIRCLE('',#82149,14.87899470754);
#32171=CIRCLE('',#82150,15.19048167462);
#32172=CIRCLE('',#82152,15.10412140798);
#32173=CIRCLE('',#82153,15.41105880551);
#32174=CIRCLE('',#82155,14.72869592011);
#32175=CIRCLE('',#82156,15.0432953008);
#32176=CIRCLE('',#82158,14.98614304973);
#32177=CIRCLE('',#82159,15.29544813031);
#32178=CIRCLE('',#82161,14.87899470754);
#32179=CIRCLE('',#82162,15.19048167462);
#32180=CIRCLE('',#82164,15.28837739941);
#32181=CIRCLE('',#82165,15.59168796208);
#32182=CIRCLE('',#82167,14.72869592011);
#32183=CIRCLE('',#82168,15.0432953008);
#32184=CIRCLE('',#82170,15.20475200412);
#32185=CIRCLE('',#82171,15.50969804693);
#32186=CIRCLE('',#82173,14.87899470754);
#32187=CIRCLE('',#82174,15.19048167462);
#32188=CIRCLE('',#82176,15.40566400734);
#32189=CIRCLE('',#82177,15.70670982437);
#32190=CIRCLE('',#82179,14.72869592011);
#32191=CIRCLE('',#82180,15.0432953008);
#32192=CIRCLE('',#82182,15.35527542921);
#32193=CIRCLE('',#82183,15.65729010739);
#32194=CIRCLE('',#82185,14.87899470754);
#32195=CIRCLE('',#82186,15.19048167462);
#32196=CIRCLE('',#82188,15.45750573369);
#32197=CIRCLE('',#82189,15.75756115352);
#32198=CIRCLE('',#82191,14.72869592011);
#32199=CIRCLE('',#82192,15.0432953008);
#32200=CIRCLE('',#82194,15.43970477396);
#32201=CIRCLE('',#82195,15.7400995393);
#32202=CIRCLE('',#82197,14.87899470754);
#32203=CIRCLE('',#82198,15.19048167462);
#32204=CIRCLE('',#82200,15.44456161589);
#32205=CIRCLE('',#82201,15.74486371827);
#32206=CIRCLE('',#82203,14.72869592011);
#32207=CIRCLE('',#82204,15.0432953008);
#32208=CIRCLE('',#82206,15.45912298634);
#32209=CIRCLE('',#82207,15.75914761359);
#32210=CIRCLE('',#82209,14.87899470754);
#32211=CIRCLE('',#82210,15.19048167462);
#32212=CIRCLE('',#82212,15.36666793768);
#32213=CIRCLE('',#82213,15.66846302312);
#32214=CIRCLE('',#82215,14.72869592011);
#32215=CIRCLE('',#82216,15.0432953008);
#32216=CIRCLE('',#82218,15.41377577062);
#32217=CIRCLE('',#82219,15.71466619139);
#32218=CIRCLE('',#82221,14.87899470754);
#32219=CIRCLE('',#82222,15.19048167462);
#32220=CIRCLE('',#82224,15.22282771061);
#32221=CIRCLE('',#82225,15.52741876511);
#32222=CIRCLE('',#82227,14.72869592011);
#32223=CIRCLE('',#82228,15.0432953008);
#32224=CIRCLE('',#82230,15.3030873848);
#32225=CIRCLE('',#82231,15.60611205608);
#32226=CIRCLE('',#82233,14.87899470754);
#32227=CIRCLE('',#82234,15.19048167462);
#32228=CIRCLE('',#82236,15.01114530963);
#32229=CIRCLE('',#82237,15.31994561044);
#32230=CIRCLE('',#82239,14.72869592011);
#32231=CIRCLE('',#82240,15.0432953008);
#32232=CIRCLE('',#82242,15.12562340887);
#32233=CIRCLE('',#82243,15.4321331483);
#32234=CIRCLE('',#82245,14.87899470754);
#32235=CIRCLE('',#82246,15.19048167462);
#32236=CIRCLE('',#82248,14.72869592011);
#32237=CIRCLE('',#82249,15.0432953008);
#32238=CIRCLE('',#82251,14.72869592011);
#32239=CIRCLE('',#82252,15.0432953008);
#32240=CIRCLE('',#82254,14.87899470754);
#32241=CIRCLE('',#82255,15.19048167462);
#32242=CIRCLE('',#82257,15.12562340887);
#32243=CIRCLE('',#82258,15.4321331483);
#32244=CIRCLE('',#82260,14.72869592011);
#32245=CIRCLE('',#82261,15.0432953008);
#32246=CIRCLE('',#82263,15.01114530963);
#32247=CIRCLE('',#82264,15.31994561044);
#32248=CIRCLE('',#82266,14.87899470754);
#32249=CIRCLE('',#82267,15.19048167462);
#32250=CIRCLE('',#82269,15.3030873848);
#32251=CIRCLE('',#82270,15.60611205608);
#32252=CIRCLE('',#82272,14.72869592011);
#32253=CIRCLE('',#82273,15.0432953008);
#32254=CIRCLE('',#82275,15.22282771061);
#32255=CIRCLE('',#82276,15.52741876511);
#32256=CIRCLE('',#82278,14.87899470754);
#32257=CIRCLE('',#82279,15.19048167462);
#32258=CIRCLE('',#82281,15.41377577062);
#32259=CIRCLE('',#82282,15.71466619139);
#32260=CIRCLE('',#82284,14.72869592011);
#32261=CIRCLE('',#82285,15.0432953008);
#32262=CIRCLE('',#82287,15.36666793768);
#32263=CIRCLE('',#82288,15.66846302312);
#32264=CIRCLE('',#82290,14.87899470754);
#32265=CIRCLE('',#82291,15.19048167462);
#32266=CIRCLE('',#82293,15.45912298634);
#32267=CIRCLE('',#82294,15.75914761359);
#32268=CIRCLE('',#82296,14.72869592011);
#32269=CIRCLE('',#82297,15.0432953008);
#32270=CIRCLE('',#82299,15.44456161589);
#32271=CIRCLE('',#82300,15.74486371827);
#32272=CIRCLE('',#82302,14.87899470754);
#32273=CIRCLE('',#82303,15.19048167462);
#32274=CIRCLE('',#82305,15.45912298634);
#32275=CIRCLE('',#82306,15.75914761359);
#32276=CIRCLE('',#82308,15.28837739941);
#32277=CIRCLE('',#82309,15.59168796208);
#32278=CIRCLE('',#82311,15.44456161589);
#32279=CIRCLE('',#82312,15.74486371827);
#32280=CIRCLE('',#82314,15.20475200412);
#32281=CIRCLE('',#82315,15.50969804693);
#32282=CIRCLE('',#82317,15.41377577062);
#32283=CIRCLE('',#82318,15.71466619139);
#32284=CIRCLE('',#82320,15.28837739941);
#32285=CIRCLE('',#82321,15.59168796208);
#32286=CIRCLE('',#82323,15.36666793768);
#32287=CIRCLE('',#82324,15.66846302312);
#32288=CIRCLE('',#82326,15.20475200412);
#32289=CIRCLE('',#82327,15.50969804693);
#32290=CIRCLE('',#82329,15.3030873848);
#32291=CIRCLE('',#82330,15.60611205608);
#32292=CIRCLE('',#82332,15.28837739941);
#32293=CIRCLE('',#82333,15.59168796208);
#32294=CIRCLE('',#82335,15.22282771061);
#32295=CIRCLE('',#82336,15.52741876511);
#32296=CIRCLE('',#82338,15.20475200412);
#32297=CIRCLE('',#82339,15.50969804693);
#32298=CIRCLE('',#82341,15.12562340887);
#32299=CIRCLE('',#82342,15.4321331483);
#32300=CIRCLE('',#82344,15.28837739941);
#32301=CIRCLE('',#82345,15.59168796208);
#32302=CIRCLE('',#82347,15.01114530963);
#32303=CIRCLE('',#82348,15.31994561044);
#32304=CIRCLE('',#82350,15.20475200412);
#32305=CIRCLE('',#82351,15.50969804693);
#32306=CIRCLE('',#82353,15.12562340887);
#32307=CIRCLE('',#82354,15.4321331483);
#32308=CIRCLE('',#82356,15.40566400734);
#32309=CIRCLE('',#82357,15.70670982437);
#32310=CIRCLE('',#82359,15.01114530963);
#32311=CIRCLE('',#82360,15.31994561044);
#32312=CIRCLE('',#82362,15.35527542921);
#32313=CIRCLE('',#82363,15.65729010739);
#32314=CIRCLE('',#82365,15.12562340887);
#32315=CIRCLE('',#82366,15.4321331483);
#32316=CIRCLE('',#82368,15.45750573369);
#32317=CIRCLE('',#82369,15.75756115352);
#32318=CIRCLE('',#82371,15.01114530963);
#32319=CIRCLE('',#82372,15.31994561044);
#32320=CIRCLE('',#82374,15.43970477396);
#32321=CIRCLE('',#82375,15.7400995393);
#32322=CIRCLE('',#82377,15.12562340887);
#32323=CIRCLE('',#82378,15.4321331483);
#32324=CIRCLE('',#82380,15.44456161589);
#32325=CIRCLE('',#82381,15.74486371827);
#32326=CIRCLE('',#82383,15.01114530963);
#32327=CIRCLE('',#82384,15.31994561044);
#32328=CIRCLE('',#82386,15.45912298634);
#32329=CIRCLE('',#82387,15.75914761359);
#32330=CIRCLE('',#82389,15.12562340887);
#32331=CIRCLE('',#82390,15.4321331483);
#32332=CIRCLE('',#82392,15.36666793768);
#32333=CIRCLE('',#82393,15.66846302312);
#32334=CIRCLE('',#82395,15.01114530963);
#32335=CIRCLE('',#82396,15.31994561044);
#32336=CIRCLE('',#82398,15.41377577062);
#32337=CIRCLE('',#82399,15.71466619139);
#32338=CIRCLE('',#82401,15.12562340887);
#32339=CIRCLE('',#82402,15.4321331483);
#32340=CIRCLE('',#82404,15.22282771061);
#32341=CIRCLE('',#82405,15.52741876511);
#32342=CIRCLE('',#82407,15.01114530963);
#32343=CIRCLE('',#82408,15.31994561044);
#32344=CIRCLE('',#82410,15.3030873848);
#32345=CIRCLE('',#82411,15.60611205608);
#32346=CIRCLE('',#82413,15.12562340887);
#32347=CIRCLE('',#82414,15.4321331483);
#32348=CIRCLE('',#82416,15.01114530963);
#32349=CIRCLE('',#82417,15.31994561044);
#32350=CIRCLE('',#82419,15.01114530963);
#32351=CIRCLE('',#82420,15.31994561044);
#32352=CIRCLE('',#82422,15.12562340887);
#32353=CIRCLE('',#82423,15.4321331483);
#32354=CIRCLE('',#82425,15.3030873848);
#32355=CIRCLE('',#82426,15.60611205608);
#32356=CIRCLE('',#82428,15.01114530963);
#32357=CIRCLE('',#82429,15.31994561044);
#32358=CIRCLE('',#82431,15.22282771061);
#32359=CIRCLE('',#82432,15.52741876511);
#32360=CIRCLE('',#82434,15.12562340887);
#32361=CIRCLE('',#82435,15.4321331483);
#32362=CIRCLE('',#82437,15.41377577062);
#32363=CIRCLE('',#82438,15.71466619139);
#32364=CIRCLE('',#82440,15.01114530963);
#32365=CIRCLE('',#82441,15.31994561044);
#32366=CIRCLE('',#82443,15.36666793768);
#32367=CIRCLE('',#82444,15.66846302312);
#32368=CIRCLE('',#82446,15.12562340887);
#32369=CIRCLE('',#82447,15.4321331483);
#32370=CIRCLE('',#82449,15.45912298634);
#32371=CIRCLE('',#82450,15.75914761359);
#32372=CIRCLE('',#82452,15.01114530963);
#32373=CIRCLE('',#82453,15.31994561044);
#32374=CIRCLE('',#82455,15.44456161589);
#32375=CIRCLE('',#82456,15.74486371827);
#32376=CIRCLE('',#82458,15.12562340887);
#32377=CIRCLE('',#82459,15.4321331483);
#32378=CIRCLE('',#82461,15.45912298634);
#32379=CIRCLE('',#82462,15.75914761359);
#32380=CIRCLE('',#82464,15.40566400734);
#32381=CIRCLE('',#82465,15.70670982437);
#32382=CIRCLE('',#82467,15.44456161589);
#32383=CIRCLE('',#82468,15.74486371827);
#32384=CIRCLE('',#82470,15.35527542921);
#32385=CIRCLE('',#82471,15.65729010739);
#32386=CIRCLE('',#82473,15.41377577062);
#32387=CIRCLE('',#82474,15.71466619139);
#32388=CIRCLE('',#82476,15.40566400734);
#32389=CIRCLE('',#82477,15.70670982437);
#32390=CIRCLE('',#82479,15.36666793768);
#32391=CIRCLE('',#82480,15.66846302312);
#32392=CIRCLE('',#82482,15.35527542921);
#32393=CIRCLE('',#82483,15.65729010739);
#32394=CIRCLE('',#82485,15.3030873848);
#32395=CIRCLE('',#82486,15.60611205608);
#32396=CIRCLE('',#82488,15.40566400734);
#32397=CIRCLE('',#82489,15.70670982437);
#32398=CIRCLE('',#82491,15.22282771061);
#32399=CIRCLE('',#82492,15.52741876511);
#32400=CIRCLE('',#82494,15.35527542921);
#32401=CIRCLE('',#82495,15.65729010739);
#32402=CIRCLE('',#82497,15.3030873848);
#32403=CIRCLE('',#82498,15.60611205608);
#32404=CIRCLE('',#82500,15.45750573369);
#32405=CIRCLE('',#82501,15.75756115352);
#32406=CIRCLE('',#82503,15.22282771061);
#32407=CIRCLE('',#82504,15.52741876511);
#32408=CIRCLE('',#82506,15.43970477396);
#32409=CIRCLE('',#82507,15.7400995393);
#32410=CIRCLE('',#82509,15.3030873848);
#32411=CIRCLE('',#82510,15.60611205608);
#32412=CIRCLE('',#82512,15.44456161589);
#32413=CIRCLE('',#82513,15.74486371827);
#32414=CIRCLE('',#82515,15.22282771061);
#32415=CIRCLE('',#82516,15.52741876511);
#32416=CIRCLE('',#82518,15.45912298634);
#32417=CIRCLE('',#82519,15.75914761359);
#32418=CIRCLE('',#82521,15.3030873848);
#32419=CIRCLE('',#82522,15.60611205608);
#32420=CIRCLE('',#82524,15.36666793768);
#32421=CIRCLE('',#82525,15.66846302312);
#32422=CIRCLE('',#82527,15.22282771061);
#32423=CIRCLE('',#82528,15.52741876511);
#32424=CIRCLE('',#82530,15.41377577062);
#32425=CIRCLE('',#82531,15.71466619139);
#32426=CIRCLE('',#82533,15.3030873848);
#32427=CIRCLE('',#82534,15.60611205608);
#32428=CIRCLE('',#82536,15.22282771061);
#32429=CIRCLE('',#82537,15.52741876511);
#32430=CIRCLE('',#82539,15.22282771061);
#32431=CIRCLE('',#82540,15.52741876511);
#32432=CIRCLE('',#82542,15.3030873848);
#32433=CIRCLE('',#82543,15.60611205608);
#32434=CIRCLE('',#82545,15.41377577062);
#32435=CIRCLE('',#82546,15.71466619139);
#32436=CIRCLE('',#82548,15.22282771061);
#32437=CIRCLE('',#82549,15.52741876511);
#32438=CIRCLE('',#82551,15.36666793768);
#32439=CIRCLE('',#82552,15.66846302312);
#32440=CIRCLE('',#82554,15.3030873848);
#32441=CIRCLE('',#82555,15.60611205608);
#32442=CIRCLE('',#82557,15.45912298634);
#32443=CIRCLE('',#82558,15.75914761359);
#32444=CIRCLE('',#82560,15.22282771061);
#32445=CIRCLE('',#82561,15.52741876511);
#32446=CIRCLE('',#82563,15.44456161589);
#32447=CIRCLE('',#82564,15.74486371827);
#32448=CIRCLE('',#82566,15.3030873848);
#32449=CIRCLE('',#82567,15.60611205608);
#32450=CIRCLE('',#82569,15.45912298634);
#32451=CIRCLE('',#82570,15.75914761359);
#32452=CIRCLE('',#82572,15.45750573369);
#32453=CIRCLE('',#82573,15.75756115352);
#32454=CIRCLE('',#82575,15.44456161589);
#32455=CIRCLE('',#82576,15.74486371827);
#32456=CIRCLE('',#82578,15.43970477396);
#32457=CIRCLE('',#82579,15.7400995393);
#32458=CIRCLE('',#82581,15.41377577062);
#32459=CIRCLE('',#82582,15.71466619139);
#32460=CIRCLE('',#82584,15.45750573369);
#32461=CIRCLE('',#82585,15.75756115352);
#32462=CIRCLE('',#82587,15.36666793768);
#32463=CIRCLE('',#82588,15.66846302312);
#32464=CIRCLE('',#82590,15.43970477396);
#32465=CIRCLE('',#82591,15.7400995393);
#32466=CIRCLE('',#82593,15.41377577062);
#32467=CIRCLE('',#82594,15.71466619139);
#32468=CIRCLE('',#82596,15.44456161589);
#32469=CIRCLE('',#82597,15.74486371827);
#32470=CIRCLE('',#82599,15.36666793768);
#32471=CIRCLE('',#82600,15.66846302312);
#32472=CIRCLE('',#82602,15.45912298634);
#32473=CIRCLE('',#82603,15.75914761359);
#32474=CIRCLE('',#82605,15.41377577062);
#32475=CIRCLE('',#82606,15.71466619139);
#32476=CIRCLE('',#82608,15.36666793768);
#32477=CIRCLE('',#82609,15.66846302312);
#32478=CIRCLE('',#82611,15.36666793768);
#32479=CIRCLE('',#82612,15.66846302312);
#32480=CIRCLE('',#82614,15.41377577062);
#32481=CIRCLE('',#82615,15.71466619139);
#32482=CIRCLE('',#82617,15.45912298634);
#32483=CIRCLE('',#82618,15.75914761359);
#32484=CIRCLE('',#82620,15.36666793768);
#32485=CIRCLE('',#82621,15.66846302312);
#32486=CIRCLE('',#82623,15.44456161589);
#32487=CIRCLE('',#82624,15.74486371827);
#32488=CIRCLE('',#82626,15.41377577062);
#32489=CIRCLE('',#82627,15.71466619139);
#32490=CIRCLE('',#82629,13.04356099794);
#32491=CIRCLE('',#82630,13.39778838118);
#32492=CIRCLE('',#82632,15.3030873848);
#32493=CIRCLE('',#82633,15.60611205608);
#32494=CIRCLE('',#82635,13.07481294348);
#32495=CIRCLE('',#82637,15.52741876511);
#32496=CIRCLE('',#82639,8.729046339664);
#32497=CIRCLE('',#82641,13.04356099794);
#32498=CIRCLE('',#82642,13.39778838118);
#32499=CIRCLE('',#82644,15.41377577062);
#32500=CIRCLE('',#82645,15.71466619139);
#32501=CIRCLE('',#82647,13.07481294348);
#32502=CIRCLE('',#82649,15.36666793768);
#32503=CIRCLE('',#82650,15.66846302312);
#32504=CIRCLE('',#82652,8.72904633966401);
#32505=CIRCLE('',#82654,13.04356099794);
#32506=CIRCLE('',#82655,13.39778838118);
#32507=CIRCLE('',#82657,15.45912298634);
#32508=CIRCLE('',#82658,15.75914761359);
#32509=CIRCLE('',#82660,13.07481294348);
#32510=CIRCLE('',#82662,15.44456161589);
#32511=CIRCLE('',#82663,15.74486371827);
#32512=CIRCLE('',#82665,8.729046339664);
#32513=CIRCLE('',#82667,13.04356099794);
#32514=CIRCLE('',#82668,13.39778838118);
#32515=CIRCLE('',#82670,15.43970477396);
#32516=CIRCLE('',#82671,15.7400995393);
#32517=CIRCLE('',#82673,13.07481294348);
#32518=CIRCLE('',#82675,15.45750573369);
#32519=CIRCLE('',#82676,15.75756115352);
#32520=CIRCLE('',#82678,8.729046339664);
#32521=CIRCLE('',#82680,13.04356099794);
#32522=CIRCLE('',#82681,13.39778838118);
#32523=CIRCLE('',#82683,15.35527542921);
#32524=CIRCLE('',#82684,15.65729010739);
#32525=CIRCLE('',#82686,13.07481294348);
#32526=CIRCLE('',#82688,15.40566400734);
#32527=CIRCLE('',#82689,15.70670982437);
#32528=CIRCLE('',#82691,8.729046339664);
#32529=CIRCLE('',#82693,13.04356099794);
#32530=CIRCLE('',#82694,13.39778838118);
#32531=CIRCLE('',#82696,15.50969804693);
#32532=CIRCLE('',#82698,13.07481294348);
#32533=CIRCLE('',#82700,15.28837739941);
#32534=CIRCLE('',#82701,15.59168796208);
#32535=CIRCLE('',#82703,8.729046339664);
#32536=CIRCLE('',#82705,15.28837739941);
#32537=CIRCLE('',#82706,15.59168796208);
#32538=CIRCLE('',#82708,13.07481294348);
#32539=CIRCLE('',#82710,15.50969804693);
#32540=CIRCLE('',#82712,13.04356099794);
#32541=CIRCLE('',#82713,13.39778838118);
#32542=CIRCLE('',#82715,8.729046339664);
#32543=CIRCLE('',#82717,13.04356099794);
#32544=CIRCLE('',#82718,13.39778838118);
#32545=CIRCLE('',#82720,15.40566400734);
#32546=CIRCLE('',#82721,15.70670982437);
#32547=CIRCLE('',#82723,13.07481294348);
#32548=CIRCLE('',#82725,15.35527542921);
#32549=CIRCLE('',#82726,15.65729010739);
#32550=CIRCLE('',#82728,8.729046339664);
#32551=CIRCLE('',#82730,13.04356099794);
#32552=CIRCLE('',#82731,13.39778838118);
#32553=CIRCLE('',#82733,15.45750573369);
#32554=CIRCLE('',#82734,15.75756115352);
#32555=CIRCLE('',#82736,13.07481294348);
#32556=CIRCLE('',#82738,15.43970477396);
#32557=CIRCLE('',#82739,15.7400995393);
#32558=CIRCLE('',#82741,8.729046339664);
#32559=CIRCLE('',#82743,13.62844391363);
#32560=CIRCLE('',#82744,13.96784641621);
#32561=CIRCLE('',#82746,14.87899470754);
#32562=CIRCLE('',#82747,15.19048167462);
#32563=CIRCLE('',#82749,13.69491633808);
#32564=CIRCLE('',#82751,14.72869592011);
#32565=CIRCLE('',#82752,15.0432953008);
#32566=CIRCLE('',#82754,8.729046339664);
#32567=CIRCLE('',#82756,13.34857608537);
#32568=CIRCLE('',#82757,13.69491633808);
#32569=CIRCLE('',#82759,15.01114530963);
#32570=CIRCLE('',#82760,15.31994561044);
#32571=CIRCLE('',#82762,13.62844391363);
#32572=CIRCLE('',#82763,13.96784641621);
#32573=CIRCLE('',#82765,15.12562340887);
#32574=CIRCLE('',#82766,15.4321331483);
#32575=CIRCLE('',#82768,13.34857608537);
#32576=CIRCLE('',#82769,13.69491633808);
#32577=CIRCLE('',#82771,15.22282771061);
#32578=CIRCLE('',#82772,15.52741876511);
#32579=CIRCLE('',#82774,13.62844391363);
#32580=CIRCLE('',#82775,13.96784641621);
#32581=CIRCLE('',#82777,15.3030873848);
#32582=CIRCLE('',#82778,15.60611205608);
#32583=CIRCLE('',#82780,13.34857608537);
#32584=CIRCLE('',#82781,13.69491633808);
#32585=CIRCLE('',#82783,15.36666793768);
#32586=CIRCLE('',#82784,15.66846302312);
#32587=CIRCLE('',#82786,13.62844391363);
#32588=CIRCLE('',#82787,13.96784641621);
#32589=CIRCLE('',#82789,15.41377577062);
#32590=CIRCLE('',#82790,15.71466619139);
#32591=CIRCLE('',#82792,13.34857608537);
#32592=CIRCLE('',#82793,13.69491633808);
#32593=CIRCLE('',#82795,15.44456161589);
#32594=CIRCLE('',#82796,15.74486371827);
#32595=CIRCLE('',#82798,13.62844391363);
#32596=CIRCLE('',#82799,13.96784641621);
#32597=CIRCLE('',#82801,15.45912298634);
#32598=CIRCLE('',#82802,15.75914761359);
#32599=CIRCLE('',#82804,13.34857608537);
#32600=CIRCLE('',#82805,13.69491633808);
#32601=CIRCLE('',#82807,15.45750573369);
#32602=CIRCLE('',#82808,15.75756115352);
#32603=CIRCLE('',#82810,13.62844391363);
#32604=CIRCLE('',#82811,13.96784641621);
#32605=CIRCLE('',#82813,15.43970477396);
#32606=CIRCLE('',#82814,15.7400995393);
#32607=CIRCLE('',#82816,13.34857608537);
#32608=CIRCLE('',#82817,13.69491633808);
#32609=CIRCLE('',#82819,15.40566400734);
#32610=CIRCLE('',#82820,15.70670982437);
#32611=CIRCLE('',#82822,13.62844391363);
#32612=CIRCLE('',#82823,13.96784641621);
#32613=CIRCLE('',#82825,15.35527542921);
#32614=CIRCLE('',#82826,15.65729010739);
#32615=CIRCLE('',#82828,13.34857608537);
#32616=CIRCLE('',#82829,13.69491633808);
#32617=CIRCLE('',#82831,15.28837739941);
#32618=CIRCLE('',#82832,15.59168796208);
#32619=CIRCLE('',#82834,13.62844391363);
#32620=CIRCLE('',#82835,13.96784641621);
#32621=CIRCLE('',#82837,15.20475200412);
#32622=CIRCLE('',#82838,15.50969804693);
#32623=CIRCLE('',#82840,13.34857608537);
#32624=CIRCLE('',#82841,13.69491633808);
#32625=CIRCLE('',#82843,15.10412140798);
#32626=CIRCLE('',#82844,15.41105880551);
#32627=CIRCLE('',#82846,13.62844391363);
#32628=CIRCLE('',#82847,13.96784641621);
#32629=CIRCLE('',#82849,14.98614304973);
#32630=CIRCLE('',#82850,15.29544813031);
#32631=CIRCLE('',#82852,13.62844391363);
#32632=CIRCLE('',#82853,13.96784641621);
#32633=CIRCLE('',#82855,15.01168656437);
#32634=CIRCLE('',#82857,13.69491633808);
#32635=CIRCLE('',#82859,14.8504034796);
#32636=CIRCLE('',#82860,15.16247781555);
#32637=CIRCLE('',#82862,8.729046339664);
#32638=CIRCLE('',#82864,14.8504034796);
#32639=CIRCLE('',#82865,15.16247781555);
#32640=CIRCLE('',#82867,13.69491633808);
#32641=CIRCLE('',#82869,15.01168656437);
#32642=CIRCLE('',#82871,13.62844391363);
#32643=CIRCLE('',#82872,13.96784641621);
#32644=CIRCLE('',#82874,8.729046339664);
#32645=CIRCLE('',#82876,13.62844391363);
#32646=CIRCLE('',#82877,13.96784641621);
#32647=CIRCLE('',#82879,15.10412140798);
#32648=CIRCLE('',#82880,15.41105880551);
#32649=CIRCLE('',#82882,13.34857608537);
#32650=CIRCLE('',#82883,13.69491633808);
#32651=CIRCLE('',#82885,14.98614304973);
#32652=CIRCLE('',#82886,15.29544813031);
#32653=CIRCLE('',#82888,15.20475200412);
#32654=CIRCLE('',#82889,15.50969804693);
#32655=CIRCLE('',#82891,13.62844391363);
#32656=CIRCLE('',#82892,13.96784641621);
#32657=CIRCLE('',#82894,15.28837739941);
#32658=CIRCLE('',#82895,15.59168796208);
#32659=CIRCLE('',#82897,13.34857608537);
#32660=CIRCLE('',#82898,13.69491633808);
#32661=CIRCLE('',#82900,15.35527542921);
#32662=CIRCLE('',#82901,15.65729010739);
#32663=CIRCLE('',#82903,13.62844391363);
#32664=CIRCLE('',#82904,13.96784641621);
#32665=CIRCLE('',#82906,15.40566400734);
#32666=CIRCLE('',#82907,15.70670982437);
#32667=CIRCLE('',#82909,13.34857608537);
#32668=CIRCLE('',#82910,13.69491633808);
#32669=CIRCLE('',#82912,15.43970477396);
#32670=CIRCLE('',#82913,15.7400995393);
#32671=CIRCLE('',#82915,13.62844391363);
#32672=CIRCLE('',#82916,13.96784641621);
#32673=CIRCLE('',#82918,15.45750573369);
#32674=CIRCLE('',#82919,15.75756115352);
#32675=CIRCLE('',#82921,13.34857608537);
#32676=CIRCLE('',#82922,13.69491633808);
#32677=CIRCLE('',#82924,15.45750573369);
#32678=CIRCLE('',#82925,15.75756115352);
#32679=CIRCLE('',#82927,13.1066579839);
#32680=CIRCLE('',#82928,13.45922484792);
#32681=CIRCLE('',#82930,15.43970477396);
#32682=CIRCLE('',#82931,15.7400995393);
#32683=CIRCLE('',#82933,12.78023800666);
#32684=CIRCLE('',#82934,13.14156510873);
#32685=CIRCLE('',#82936,8.729046339664);
#32686=CIRCLE('',#82938,13.1066579839);
#32687=CIRCLE('',#82939,13.45922484792);
#32688=CIRCLE('',#82941,15.35527542921);
#32689=CIRCLE('',#82942,15.65729010739);
#32690=CIRCLE('',#82944,13.14156510873);
#32691=CIRCLE('',#82946,15.40566400734);
#32692=CIRCLE('',#82947,15.70670982437);
#32693=CIRCLE('',#82949,8.729046339664);
#32694=CIRCLE('',#82951,13.1066579839);
#32695=CIRCLE('',#82952,13.45922484792);
#32696=CIRCLE('',#82954,15.20475200412);
#32697=CIRCLE('',#82955,15.50969804693);
#32698=CIRCLE('',#82957,13.14156510873);
#32699=CIRCLE('',#82959,15.28837739941);
#32700=CIRCLE('',#82960,15.59168796208);
#32701=CIRCLE('',#82962,8.729046339664);
#32702=CIRCLE('',#82964,14.1185864557);
#32703=CIRCLE('',#82965,14.4464782389);
#32704=CIRCLE('',#82967,14.55968693025);
#32705=CIRCLE('',#82968,14.87786051511);
#32706=CIRCLE('',#82970,13.88468521454);
#32707=CIRCLE('',#82971,14.21797220095);
#32708=CIRCLE('',#82973,14.37130764777);
#32709=CIRCLE('',#82974,14.69356095393);
#32710=CIRCLE('',#82976,8.72904633966401);
#32711=CIRCLE('',#82978,13.88468521454);
#32712=CIRCLE('',#82979,14.21797220095);
#32713=CIRCLE('',#82981,14.72869592011);
#32714=CIRCLE('',#82982,15.0432953008);
#32715=CIRCLE('',#82984,14.1185864557);
#32716=CIRCLE('',#82985,14.4464782389);
#32717=CIRCLE('',#82987,14.87899470754);
#32718=CIRCLE('',#82988,15.19048167462);
#32719=CIRCLE('',#82990,13.88468521454);
#32720=CIRCLE('',#82991,14.21797220095);
#32721=CIRCLE('',#82993,15.01114530963);
#32722=CIRCLE('',#82994,15.31994561044);
#32723=CIRCLE('',#82996,14.1185864557);
#32724=CIRCLE('',#82997,14.4464782389);
#32725=CIRCLE('',#82999,15.12562340887);
#32726=CIRCLE('',#83000,15.4321331483);
#32727=CIRCLE('',#83002,13.88468521454);
#32728=CIRCLE('',#83003,14.21797220095);
#32729=CIRCLE('',#83005,15.22282771061);
#32730=CIRCLE('',#83006,15.52741876511);
#32731=CIRCLE('',#83008,14.1185864557);
#32732=CIRCLE('',#83009,14.4464782389);
#32733=CIRCLE('',#83011,15.3030873848);
#32734=CIRCLE('',#83012,15.60611205608);
#32735=CIRCLE('',#83014,13.88468521454);
#32736=CIRCLE('',#83015,14.21797220095);
#32737=CIRCLE('',#83017,15.36666793768);
#32738=CIRCLE('',#83018,15.66846302312);
#32739=CIRCLE('',#83020,14.1185864557);
#32740=CIRCLE('',#83021,14.4464782389);
#32741=CIRCLE('',#83023,15.41377577062);
#32742=CIRCLE('',#83024,15.71466619139);
#32743=CIRCLE('',#83026,13.88468521454);
#32744=CIRCLE('',#83027,14.21797220095);
#32745=CIRCLE('',#83029,15.44456161589);
#32746=CIRCLE('',#83030,15.74486371827);
#32747=CIRCLE('',#83032,14.1185864557);
#32748=CIRCLE('',#83033,14.4464782389);
#32749=CIRCLE('',#83035,15.45912298634);
#32750=CIRCLE('',#83036,15.75914761359);
#32751=CIRCLE('',#83038,13.88468521454);
#32752=CIRCLE('',#83039,14.21797220095);
#32753=CIRCLE('',#83041,15.45750573369);
#32754=CIRCLE('',#83042,15.75756115352);
#32755=CIRCLE('',#83044,14.1185864557);
#32756=CIRCLE('',#83045,14.4464782389);
#32757=CIRCLE('',#83047,15.43970477396);
#32758=CIRCLE('',#83048,15.7400995393);
#32759=CIRCLE('',#83050,13.88468521454);
#32760=CIRCLE('',#83051,14.21797220095);
#32761=CIRCLE('',#83053,15.40566400734);
#32762=CIRCLE('',#83054,15.70670982437);
#32763=CIRCLE('',#83056,14.1185864557);
#32764=CIRCLE('',#83057,14.4464782389);
#32765=CIRCLE('',#83059,15.35527542921);
#32766=CIRCLE('',#83060,15.65729010739);
#32767=CIRCLE('',#83062,13.88468521454);
#32768=CIRCLE('',#83063,14.21797220095);
#32769=CIRCLE('',#83065,15.28837739941);
#32770=CIRCLE('',#83066,15.59168796208);
#32771=CIRCLE('',#83068,14.1185864557);
#32772=CIRCLE('',#83069,14.4464782389);
#32773=CIRCLE('',#83071,15.20475200412);
#32774=CIRCLE('',#83072,15.50969804693);
#32775=CIRCLE('',#83074,13.88468521454);
#32776=CIRCLE('',#83075,14.21797220095);
#32777=CIRCLE('',#83077,15.10412140798);
#32778=CIRCLE('',#83078,15.41105880551);
#32779=CIRCLE('',#83080,14.1185864557);
#32780=CIRCLE('',#83081,14.4464782389);
#32781=CIRCLE('',#83083,14.98614304973);
#32782=CIRCLE('',#83084,15.29544813031);
#32783=CIRCLE('',#83086,13.88468521454);
#32784=CIRCLE('',#83087,14.21797220095);
#32785=CIRCLE('',#83089,14.8504034796);
#32786=CIRCLE('',#83090,15.16247781555);
#32787=CIRCLE('',#83092,14.1185864557);
#32788=CIRCLE('',#83093,14.4464782389);
#32789=CIRCLE('',#83095,14.6964105654);
#32790=CIRCLE('',#83096,15.01168656437);
#32791=CIRCLE('',#83098,14.52358370055);
#32792=CIRCLE('',#83099,14.84253123652);
#32793=CIRCLE('',#83101,14.1185864557);
#32794=CIRCLE('',#83102,14.4464782389);
#32795=CIRCLE('',#83104,14.33124152008);
#32796=CIRCLE('',#83105,14.65437591667);
#32797=CIRCLE('',#83107,13.88468521454);
#32798=CIRCLE('',#83108,14.21797220095);
#32799=CIRCLE('',#83110,8.729046339664);
#32800=CIRCLE('',#83112,14.1185864557);
#32801=CIRCLE('',#83113,14.4464782389);
#32802=CIRCLE('',#83115,14.52358370055);
#32803=CIRCLE('',#83116,14.84253123652);
#32804=CIRCLE('',#83118,13.88468521454);
#32805=CIRCLE('',#83119,14.21797220095);
#32806=CIRCLE('',#83121,14.33124152008);
#32807=CIRCLE('',#83122,14.65437591667);
#32808=CIRCLE('',#83124,8.729046339664);
#32809=CIRCLE('',#83126,14.6964105654);
#32810=CIRCLE('',#83127,15.01168656437);
#32811=CIRCLE('',#83129,14.1185864557);
#32812=CIRCLE('',#83130,14.4464782389);
#32813=CIRCLE('',#83132,14.8504034796);
#32814=CIRCLE('',#83133,15.16247781555);
#32815=CIRCLE('',#83135,13.88468521454);
#32816=CIRCLE('',#83136,14.21797220095);
#32817=CIRCLE('',#83138,14.98614304973);
#32818=CIRCLE('',#83139,15.29544813031);
#32819=CIRCLE('',#83141,14.1185864557);
#32820=CIRCLE('',#83142,14.4464782389);
#32821=CIRCLE('',#83144,15.10412140798);
#32822=CIRCLE('',#83145,15.41105880551);
#32823=CIRCLE('',#83147,13.88468521454);
#32824=CIRCLE('',#83148,14.21797220095);
#32825=CIRCLE('',#83150,15.20475200412);
#32826=CIRCLE('',#83151,15.50969804693);
#32827=CIRCLE('',#83153,14.1185864557);
#32828=CIRCLE('',#83154,14.4464782389);
#32829=CIRCLE('',#83156,15.28837739941);
#32830=CIRCLE('',#83157,15.59168796208);
#32831=CIRCLE('',#83159,13.88468521454);
#32832=CIRCLE('',#83160,14.21797220095);
#32833=CIRCLE('',#83162,15.35527542921);
#32834=CIRCLE('',#83163,15.65729010739);
#32835=CIRCLE('',#83165,14.1185864557);
#32836=CIRCLE('',#83166,14.4464782389);
#32837=CIRCLE('',#83168,15.40566400734);
#32838=CIRCLE('',#83169,15.70670982437);
#32839=CIRCLE('',#83171,13.88468521454);
#32840=CIRCLE('',#83172,14.21797220095);
#32841=CIRCLE('',#83174,15.43970477396);
#32842=CIRCLE('',#83175,15.7400995393);
#32843=CIRCLE('',#83177,14.1185864557);
#32844=CIRCLE('',#83178,14.4464782389);
#32845=CIRCLE('',#83180,15.45750573369);
#32846=CIRCLE('',#83181,15.75756115352);
#32847=CIRCLE('',#83183,13.88468521454);
#32848=CIRCLE('',#83184,14.21797220095);
#32849=CIRCLE('',#83186,15.43970477396);
#32850=CIRCLE('',#83187,15.7400995393);
#32851=CIRCLE('',#83189,13.40650899776);
#32852=CIRCLE('',#83190,13.75139023906);
#32853=CIRCLE('',#83192,15.45750573369);
#32854=CIRCLE('',#83193,15.75756115352);
#32855=CIRCLE('',#83195,13.68153805341);
#32856=CIRCLE('',#83196,14.01965525635);
#32857=CIRCLE('',#83198,15.35527542921);
#32858=CIRCLE('',#83199,15.65729010739);
#32859=CIRCLE('',#83201,13.40650899776);
#32860=CIRCLE('',#83202,13.75139023906);
#32861=CIRCLE('',#83204,15.40566400734);
#32862=CIRCLE('',#83205,15.70670982437);
#32863=CIRCLE('',#83207,13.68153805341);
#32864=CIRCLE('',#83208,14.01965525635);
#32865=CIRCLE('',#83210,15.20475200412);
#32866=CIRCLE('',#83211,15.50969804693);
#32867=CIRCLE('',#83213,13.40650899776);
#32868=CIRCLE('',#83214,13.75139023906);
#32869=CIRCLE('',#83216,15.28837739941);
#32870=CIRCLE('',#83217,15.59168796208);
#32871=CIRCLE('',#83219,13.68153805341);
#32872=CIRCLE('',#83220,14.01965525635);
#32873=CIRCLE('',#83222,14.98614304973);
#32874=CIRCLE('',#83223,15.29544813031);
#32875=CIRCLE('',#83225,13.40650899776);
#32876=CIRCLE('',#83226,13.75139023906);
#32877=CIRCLE('',#83228,15.10412140798);
#32878=CIRCLE('',#83229,15.41105880551);
#32879=CIRCLE('',#83231,13.68153805341);
#32880=CIRCLE('',#83232,14.01965525635);
#32881=CIRCLE('',#83234,13.68153805341);
#32882=CIRCLE('',#83235,14.01965525635);
#32883=CIRCLE('',#83237,14.6964105654);
#32884=CIRCLE('',#83238,15.01168656437);
#32885=CIRCLE('',#83240,13.75139023906);
#32886=CIRCLE('',#83242,14.8504034796);
#32887=CIRCLE('',#83243,15.16247781555);
#32888=CIRCLE('',#83245,8.729046339664);
#32889=CIRCLE('',#83247,14.52358370055);
#32890=CIRCLE('',#83248,14.84253123652);
#32891=CIRCLE('',#83250,14.16278516066);
#32892=CIRCLE('',#83251,14.48967679098);
#32893=CIRCLE('',#83253,14.33124152008);
#32894=CIRCLE('',#83254,14.65437591667);
#32895=CIRCLE('',#83256,13.93321511737);
#32896=CIRCLE('',#83257,14.26536832707);
#32897=CIRCLE('',#83259,8.72904633966401);
#32898=CIRCLE('',#83261,14.33124152008);
#32899=CIRCLE('',#83262,14.65437591667);
#32900=CIRCLE('',#83264,14.37130764777);
#32901=CIRCLE('',#83265,14.69356095393);
#32902=CIRCLE('',#83267,14.52358370055);
#32903=CIRCLE('',#83268,14.84253123652);
#32904=CIRCLE('',#83270,14.55968693025);
#32905=CIRCLE('',#83271,14.87786051511);
#32906=CIRCLE('',#83273,14.33124152008);
#32907=CIRCLE('',#83274,14.65437591667);
#32908=CIRCLE('',#83276,14.72869592011);
#32909=CIRCLE('',#83277,15.0432953008);
#32910=CIRCLE('',#83279,14.52358370055);
#32911=CIRCLE('',#83280,14.84253123652);
#32912=CIRCLE('',#83282,14.87899470754);
#32913=CIRCLE('',#83283,15.19048167462);
#32914=CIRCLE('',#83285,14.33124152008);
#32915=CIRCLE('',#83286,14.65437591667);
#32916=CIRCLE('',#83288,15.01114530963);
#32917=CIRCLE('',#83289,15.31994561044);
#32918=CIRCLE('',#83291,14.52358370055);
#32919=CIRCLE('',#83292,14.84253123652);
#32920=CIRCLE('',#83294,15.12562340887);
#32921=CIRCLE('',#83295,15.4321331483);
#32922=CIRCLE('',#83297,14.33124152008);
#32923=CIRCLE('',#83298,14.65437591667);
#32924=CIRCLE('',#83300,15.22282771061);
#32925=CIRCLE('',#83301,15.52741876511);
#32926=CIRCLE('',#83303,14.52358370055);
#32927=CIRCLE('',#83304,14.84253123652);
#32928=CIRCLE('',#83306,15.3030873848);
#32929=CIRCLE('',#83307,15.60611205608);
#32930=CIRCLE('',#83309,14.33124152008);
#32931=CIRCLE('',#83310,14.65437591667);
#32932=CIRCLE('',#83312,15.36666793768);
#32933=CIRCLE('',#83313,15.66846302312);
#32934=CIRCLE('',#83315,14.52358370055);
#32935=CIRCLE('',#83316,14.84253123652);
#32936=CIRCLE('',#83318,15.41377577062);
#32937=CIRCLE('',#83319,15.71466619139);
#32938=CIRCLE('',#83321,14.33124152008);
#32939=CIRCLE('',#83322,14.65437591667);
#32940=CIRCLE('',#83324,15.44456161589);
#32941=CIRCLE('',#83325,15.74486371827);
#32942=CIRCLE('',#83327,14.52358370055);
#32943=CIRCLE('',#83328,14.84253123652);
#32944=CIRCLE('',#83330,15.45912298634);
#32945=CIRCLE('',#83331,15.75914761359);
#32946=CIRCLE('',#83333,14.33124152008);
#32947=CIRCLE('',#83334,14.65437591667);
#32948=CIRCLE('',#83336,15.45750573369);
#32949=CIRCLE('',#83337,15.75756115352);
#32950=CIRCLE('',#83339,14.52358370055);
#32951=CIRCLE('',#83340,14.84253123652);
#32952=CIRCLE('',#83342,15.43970477396);
#32953=CIRCLE('',#83343,15.7400995393);
#32954=CIRCLE('',#83345,14.33124152008);
#32955=CIRCLE('',#83346,14.65437591667);
#32956=CIRCLE('',#83348,15.40566400734);
#32957=CIRCLE('',#83349,15.70670982437);
#32958=CIRCLE('',#83351,14.52358370055);
#32959=CIRCLE('',#83352,14.84253123652);
#32960=CIRCLE('',#83354,15.35527542921);
#32961=CIRCLE('',#83355,15.65729010739);
#32962=CIRCLE('',#83357,14.33124152008);
#32963=CIRCLE('',#83358,14.65437591667);
#32964=CIRCLE('',#83360,15.28837739941);
#32965=CIRCLE('',#83361,15.59168796208);
#32966=CIRCLE('',#83363,14.52358370055);
#32967=CIRCLE('',#83364,14.84253123652);
#32968=CIRCLE('',#83366,15.20475200412);
#32969=CIRCLE('',#83367,15.50969804693);
#32970=CIRCLE('',#83369,14.33124152008);
#32971=CIRCLE('',#83370,14.65437591667);
#32972=CIRCLE('',#83372,15.10412140798);
#32973=CIRCLE('',#83373,15.41105880551);
#32974=CIRCLE('',#83375,14.52358370055);
#32975=CIRCLE('',#83376,14.84253123652);
#32976=CIRCLE('',#83378,14.98614304973);
#32977=CIRCLE('',#83379,15.29544813031);
#32978=CIRCLE('',#83381,14.33124152008);
#32979=CIRCLE('',#83382,14.65437591667);
#32980=CIRCLE('',#83384,14.8504034796);
#32981=CIRCLE('',#83385,15.16247781555);
#32982=CIRCLE('',#83387,14.52358370055);
#32983=CIRCLE('',#83388,14.84253123652);
#32984=CIRCLE('',#83390,14.6964105654);
#32985=CIRCLE('',#83391,15.01168656437);
#32986=CIRCLE('',#83393,14.33124152008);
#32987=CIRCLE('',#83394,14.65437591667);
#32988=CIRCLE('',#83396,14.52358370055);
#32989=CIRCLE('',#83397,14.84253123652);
#32990=CIRCLE('',#83399,14.52358370055);
#32991=CIRCLE('',#83400,14.84253123652);
#32992=CIRCLE('',#83402,14.33124152008);
#32993=CIRCLE('',#83403,14.65437591667);
#32994=CIRCLE('',#83405,14.6964105654);
#32995=CIRCLE('',#83406,15.01168656437);
#32996=CIRCLE('',#83408,14.52358370055);
#32997=CIRCLE('',#83409,14.84253123652);
#32998=CIRCLE('',#83411,14.8504034796);
#32999=CIRCLE('',#83412,15.16247781555);
#33000=CIRCLE('',#83414,14.33124152008);
#33001=CIRCLE('',#83415,14.65437591667);
#33002=CIRCLE('',#83417,14.98614304973);
#33003=CIRCLE('',#83418,15.29544813031);
#33004=CIRCLE('',#83420,14.52358370055);
#33005=CIRCLE('',#83421,14.84253123652);
#33006=CIRCLE('',#83423,15.10412140798);
#33007=CIRCLE('',#83424,15.41105880551);
#33008=CIRCLE('',#83426,14.33124152008);
#33009=CIRCLE('',#83427,14.65437591667);
#33010=CIRCLE('',#83429,15.20475200412);
#33011=CIRCLE('',#83430,15.50969804693);
#33012=CIRCLE('',#83432,14.52358370055);
#33013=CIRCLE('',#83433,14.84253123652);
#33014=CIRCLE('',#83435,15.28837739941);
#33015=CIRCLE('',#83436,15.59168796208);
#33016=CIRCLE('',#83438,14.33124152008);
#33017=CIRCLE('',#83439,14.65437591667);
#33018=CIRCLE('',#83441,15.35527542921);
#33019=CIRCLE('',#83442,15.65729010739);
#33020=CIRCLE('',#83444,14.52358370055);
#33021=CIRCLE('',#83445,14.84253123652);
#33022=CIRCLE('',#83447,15.40566400734);
#33023=CIRCLE('',#83448,15.70670982437);
#33024=CIRCLE('',#83450,14.33124152008);
#33025=CIRCLE('',#83451,14.65437591667);
#33026=CIRCLE('',#83453,15.43970477396);
#33027=CIRCLE('',#83454,15.7400995393);
#33028=CIRCLE('',#83456,14.52358370055);
#33029=CIRCLE('',#83457,14.84253123652);
#33030=CIRCLE('',#83459,15.45750573369);
#33031=CIRCLE('',#83460,15.75756115352);
#33032=CIRCLE('',#83462,14.33124152008);
#33033=CIRCLE('',#83463,14.65437591667);
#33034=CIRCLE('',#83465,15.43970477396);
#33035=CIRCLE('',#83466,15.7400995393);
#33036=CIRCLE('',#83468,13.93321511737);
#33037=CIRCLE('',#83469,14.26536832707);
#33038=CIRCLE('',#83471,15.45750573369);
#33039=CIRCLE('',#83472,15.75756115352);
#33040=CIRCLE('',#83474,14.16278516066);
#33041=CIRCLE('',#83475,14.48967679098);
#33042=CIRCLE('',#83477,15.35527542921);
#33043=CIRCLE('',#83478,15.65729010739);
#33044=CIRCLE('',#83480,13.93321511737);
#33045=CIRCLE('',#83481,14.26536832707);
#33046=CIRCLE('',#83483,15.40566400734);
#33047=CIRCLE('',#83484,15.70670982437);
#33048=CIRCLE('',#83486,14.16278516066);
#33049=CIRCLE('',#83487,14.48967679098);
#33050=CIRCLE('',#83489,15.20475200412);
#33051=CIRCLE('',#83490,15.50969804693);
#33052=CIRCLE('',#83492,13.93321511737);
#33053=CIRCLE('',#83493,14.26536832707);
#33054=CIRCLE('',#83495,15.28837739941);
#33055=CIRCLE('',#83496,15.59168796208);
#33056=CIRCLE('',#83498,14.16278516066);
#33057=CIRCLE('',#83499,14.48967679098);
#33058=CIRCLE('',#83501,14.98614304973);
#33059=CIRCLE('',#83502,15.29544813031);
#33060=CIRCLE('',#83504,13.93321511737);
#33061=CIRCLE('',#83505,14.26536832707);
#33062=CIRCLE('',#83507,15.10412140798);
#33063=CIRCLE('',#83508,15.41105880551);
#33064=CIRCLE('',#83510,14.16278516066);
#33065=CIRCLE('',#83511,14.48967679098);
#33066=CIRCLE('',#83513,14.6964105654);
#33067=CIRCLE('',#83514,15.01168656437);
#33068=CIRCLE('',#83516,13.93321511737);
#33069=CIRCLE('',#83517,14.26536832707);
#33070=CIRCLE('',#83519,14.8504034796);
#33071=CIRCLE('',#83520,15.16247781555);
#33072=CIRCLE('',#83522,14.16278516066);
#33073=CIRCLE('',#83523,14.48967679098);
#33074=CIRCLE('',#83525,14.6964105654);
#33075=CIRCLE('',#83526,15.01168656437);
#33076=CIRCLE('',#83528,14.37130764777);
#33077=CIRCLE('',#83529,14.69356095393);
#33078=CIRCLE('',#83531,14.8504034796);
#33079=CIRCLE('',#83532,15.16247781555);
#33080=CIRCLE('',#83534,14.55968693025);
#33081=CIRCLE('',#83535,14.87786051511);
#33082=CIRCLE('',#83537,14.6964105654);
#33083=CIRCLE('',#83538,15.01168656437);
#33084=CIRCLE('',#83540,14.72869592011);
#33085=CIRCLE('',#83541,15.0432953008);
#33086=CIRCLE('',#83543,14.8504034796);
#33087=CIRCLE('',#83544,15.16247781555);
#33088=CIRCLE('',#83546,14.87899470754);
#33089=CIRCLE('',#83547,15.19048167462);
#33090=CIRCLE('',#83549,14.6964105654);
#33091=CIRCLE('',#83550,15.01168656437);
#33092=CIRCLE('',#83552,15.01114530963);
#33093=CIRCLE('',#83553,15.31994561044);
#33094=CIRCLE('',#83555,14.8504034796);
#33095=CIRCLE('',#83556,15.16247781555);
#33096=CIRCLE('',#83558,15.12562340887);
#33097=CIRCLE('',#83559,15.4321331483);
#33098=CIRCLE('',#83561,14.6964105654);
#33099=CIRCLE('',#83562,15.01168656437);
#33100=CIRCLE('',#83564,15.22282771061);
#33101=CIRCLE('',#83565,15.52741876511);
#33102=CIRCLE('',#83567,14.8504034796);
#33103=CIRCLE('',#83568,15.16247781555);
#33104=CIRCLE('',#83570,15.3030873848);
#33105=CIRCLE('',#83571,15.60611205608);
#33106=CIRCLE('',#83573,14.6964105654);
#33107=CIRCLE('',#83574,15.01168656437);
#33108=CIRCLE('',#83576,15.36666793768);
#33109=CIRCLE('',#83577,15.66846302312);
#33110=CIRCLE('',#83579,14.8504034796);
#33111=CIRCLE('',#83580,15.16247781555);
#33112=CIRCLE('',#83582,15.41377577062);
#33113=CIRCLE('',#83583,15.71466619139);
#33114=CIRCLE('',#83585,14.6964105654);
#33115=CIRCLE('',#83586,15.01168656437);
#33116=CIRCLE('',#83588,15.44456161589);
#33117=CIRCLE('',#83589,15.74486371827);
#33118=CIRCLE('',#83591,14.8504034796);
#33119=CIRCLE('',#83592,15.16247781555);
#33120=CIRCLE('',#83594,15.45912298634);
#33121=CIRCLE('',#83595,15.75914761359);
#33122=CIRCLE('',#83597,14.6964105654);
#33123=CIRCLE('',#83598,15.01168656437);
#33124=CIRCLE('',#83600,15.45750573369);
#33125=CIRCLE('',#83601,15.75756115352);
#33126=CIRCLE('',#83603,14.8504034796);
#33127=CIRCLE('',#83604,15.16247781555);
#33128=CIRCLE('',#83606,15.43970477396);
#33129=CIRCLE('',#83607,15.7400995393);
#33130=CIRCLE('',#83609,14.6964105654);
#33131=CIRCLE('',#83610,15.01168656437);
#33132=CIRCLE('',#83612,15.40566400734);
#33133=CIRCLE('',#83613,15.70670982437);
#33134=CIRCLE('',#83615,14.8504034796);
#33135=CIRCLE('',#83616,15.16247781555);
#33136=CIRCLE('',#83618,15.35527542921);
#33137=CIRCLE('',#83619,15.65729010739);
#33138=CIRCLE('',#83621,14.6964105654);
#33139=CIRCLE('',#83622,15.01168656437);
#33140=CIRCLE('',#83624,15.28837739941);
#33141=CIRCLE('',#83625,15.59168796208);
#33142=CIRCLE('',#83627,14.8504034796);
#33143=CIRCLE('',#83628,15.16247781555);
#33144=CIRCLE('',#83630,15.20475200412);
#33145=CIRCLE('',#83631,15.50969804693);
#33146=CIRCLE('',#83633,14.6964105654);
#33147=CIRCLE('',#83634,15.01168656437);
#33148=CIRCLE('',#83636,15.10412140798);
#33149=CIRCLE('',#83637,15.41105880551);
#33150=CIRCLE('',#83639,14.8504034796);
#33151=CIRCLE('',#83640,15.16247781555);
#33152=CIRCLE('',#83642,14.98614304973);
#33153=CIRCLE('',#83643,15.29544813031);
#33154=CIRCLE('',#83645,14.6964105654);
#33155=CIRCLE('',#83646,15.01168656437);
#33156=CIRCLE('',#83648,14.8504034796);
#33157=CIRCLE('',#83649,15.16247781555);
#33158=CIRCLE('',#83651,14.8504034796);
#33159=CIRCLE('',#83652,15.16247781555);
#33160=CIRCLE('',#83654,14.6964105654);
#33161=CIRCLE('',#83655,15.01168656437);
#33162=CIRCLE('',#83657,14.98614304973);
#33163=CIRCLE('',#83658,15.29544813031);
#33164=CIRCLE('',#83660,14.8504034796);
#33165=CIRCLE('',#83661,15.16247781555);
#33166=CIRCLE('',#83663,15.10412140798);
#33167=CIRCLE('',#83664,15.41105880551);
#33168=CIRCLE('',#83666,14.6964105654);
#33169=CIRCLE('',#83667,15.01168656437);
#33170=CIRCLE('',#83669,15.20475200412);
#33171=CIRCLE('',#83670,15.50969804693);
#33172=CIRCLE('',#83672,14.8504034796);
#33173=CIRCLE('',#83673,15.16247781555);
#33174=CIRCLE('',#83675,15.28837739941);
#33175=CIRCLE('',#83676,15.59168796208);
#33176=CIRCLE('',#83678,14.6964105654);
#33177=CIRCLE('',#83679,15.01168656437);
#33178=CIRCLE('',#83681,15.35527542921);
#33179=CIRCLE('',#83682,15.65729010739);
#33180=CIRCLE('',#83684,14.8504034796);
#33181=CIRCLE('',#83685,15.16247781555);
#33182=CIRCLE('',#83687,15.40566400734);
#33183=CIRCLE('',#83688,15.70670982437);
#33184=CIRCLE('',#83690,14.6964105654);
#33185=CIRCLE('',#83691,15.01168656437);
#33186=CIRCLE('',#83693,15.43970477396);
#33187=CIRCLE('',#83694,15.7400995393);
#33188=CIRCLE('',#83696,14.8504034796);
#33189=CIRCLE('',#83697,15.16247781555);
#33190=CIRCLE('',#83699,15.45750573369);
#33191=CIRCLE('',#83700,15.75756115352);
#33192=CIRCLE('',#83702,14.6964105654);
#33193=CIRCLE('',#83703,15.01168656437);
#33194=CIRCLE('',#83705,15.43970477396);
#33195=CIRCLE('',#83706,15.7400995393);
#33196=CIRCLE('',#83708,14.37130764777);
#33197=CIRCLE('',#83709,14.69356095393);
#33198=CIRCLE('',#83711,15.45750573369);
#33199=CIRCLE('',#83712,15.75756115352);
#33200=CIRCLE('',#83714,14.55968693025);
#33201=CIRCLE('',#83715,14.87786051511);
#33202=CIRCLE('',#83717,15.35527542921);
#33203=CIRCLE('',#83718,15.65729010739);
#33204=CIRCLE('',#83720,14.37130764777);
#33205=CIRCLE('',#83721,14.69356095393);
#33206=CIRCLE('',#83723,15.40566400734);
#33207=CIRCLE('',#83724,15.70670982437);
#33208=CIRCLE('',#83726,14.55968693025);
#33209=CIRCLE('',#83727,14.87786051511);
#33210=CIRCLE('',#83729,15.20475200412);
#33211=CIRCLE('',#83730,15.50969804693);
#33212=CIRCLE('',#83732,14.37130764777);
#33213=CIRCLE('',#83733,14.69356095393);
#33214=CIRCLE('',#83735,15.28837739941);
#33215=CIRCLE('',#83736,15.59168796208);
#33216=CIRCLE('',#83738,14.55968693025);
#33217=CIRCLE('',#83739,14.87786051511);
#33218=CIRCLE('',#83741,14.98614304973);
#33219=CIRCLE('',#83742,15.29544813031);
#33220=CIRCLE('',#83744,14.37130764777);
#33221=CIRCLE('',#83745,14.69356095393);
#33222=CIRCLE('',#83747,15.10412140798);
#33223=CIRCLE('',#83748,15.41105880551);
#33224=CIRCLE('',#83750,14.55968693025);
#33225=CIRCLE('',#83751,14.87786051511);
#33226=CIRCLE('',#83753,14.98614304973);
#33227=CIRCLE('',#83754,15.29544813031);
#33228=CIRCLE('',#83756,14.72869592011);
#33229=CIRCLE('',#83757,15.0432953008);
#33230=CIRCLE('',#83759,15.10412140798);
#33231=CIRCLE('',#83760,15.41105880551);
#33232=CIRCLE('',#83762,14.87899470754);
#33233=CIRCLE('',#83763,15.19048167462);
#33234=CIRCLE('',#83765,14.98614304973);
#33235=CIRCLE('',#83766,15.29544813031);
#33236=CIRCLE('',#83768,15.01114530963);
#33237=CIRCLE('',#83769,15.31994561044);
#33238=CIRCLE('',#83771,15.10412140798);
#33239=CIRCLE('',#83772,15.41105880551);
#33240=CIRCLE('',#83774,15.12562340887);
#33241=CIRCLE('',#83775,15.4321331483);
#33242=CIRCLE('',#83777,14.98614304973);
#33243=CIRCLE('',#83778,15.29544813031);
#33244=CIRCLE('',#83780,15.22282771061);
#33245=CIRCLE('',#83781,15.52741876511);
#33246=CIRCLE('',#83783,15.10412140798);
#33247=CIRCLE('',#83784,15.41105880551);
#33248=CIRCLE('',#83786,15.3030873848);
#33249=CIRCLE('',#83787,15.60611205608);
#33250=CIRCLE('',#83789,14.98614304973);
#33251=CIRCLE('',#83790,15.29544813031);
#33252=CIRCLE('',#83792,15.36666793768);
#33253=CIRCLE('',#83793,15.66846302312);
#33254=CIRCLE('',#83795,15.10412140798);
#33255=CIRCLE('',#83796,15.41105880551);
#33256=CIRCLE('',#83798,15.41377577062);
#33257=CIRCLE('',#83799,15.71466619139);
#33258=CIRCLE('',#83801,14.98614304973);
#33259=CIRCLE('',#83802,15.29544813031);
#33260=CIRCLE('',#83804,15.44456161589);
#33261=CIRCLE('',#83805,15.74486371827);
#33262=CIRCLE('',#83807,15.10412140798);
#33263=CIRCLE('',#83808,15.41105880551);
#33264=CIRCLE('',#83810,15.45912298634);
#33265=CIRCLE('',#83811,15.75914761359);
#33266=CIRCLE('',#83813,14.98614304973);
#33267=CIRCLE('',#83814,15.29544813031);
#33268=CIRCLE('',#83816,15.45750573369);
#33269=CIRCLE('',#83817,15.75756115352);
#33270=CIRCLE('',#83819,15.10412140798);
#33271=CIRCLE('',#83820,15.41105880551);
#33272=CIRCLE('',#83822,15.43970477396);
#33273=CIRCLE('',#83823,15.7400995393);
#33274=CIRCLE('',#83825,14.98614304973);
#33275=CIRCLE('',#83826,15.29544813031);
#33276=CIRCLE('',#83828,15.40566400734);
#33277=CIRCLE('',#83829,15.70670982437);
#33278=CIRCLE('',#83831,15.10412140798);
#33279=CIRCLE('',#83832,15.41105880551);
#33280=CIRCLE('',#83834,15.35527542921);
#33281=CIRCLE('',#83835,15.65729010739);
#33282=CIRCLE('',#83837,14.98614304973);
#33283=CIRCLE('',#83838,15.29544813031);
#33284=CIRCLE('',#83840,15.28837739941);
#33285=CIRCLE('',#83841,15.59168796208);
#33286=CIRCLE('',#83843,15.10412140798);
#33287=CIRCLE('',#83844,15.41105880551);
#33288=CIRCLE('',#83846,15.20475200412);
#33289=CIRCLE('',#83847,15.50969804693);
#33290=CIRCLE('',#83849,14.98614304973);
#33291=CIRCLE('',#83850,15.29544813031);
#33292=CIRCLE('',#83852,15.10412140798);
#33293=CIRCLE('',#83853,15.41105880551);
#33294=CIRCLE('',#83855,15.10412140798);
#33295=CIRCLE('',#83856,15.41105880551);
#33296=CIRCLE('',#83858,14.98614304973);
#33297=CIRCLE('',#83859,15.29544813031);
#33298=CIRCLE('',#83861,15.20475200412);
#33299=CIRCLE('',#83862,15.50969804693);
#33300=CIRCLE('',#83864,15.10412140798);
#33301=CIRCLE('',#83865,15.41105880551);
#33302=CIRCLE('',#83867,15.28837739941);
#33303=CIRCLE('',#83868,15.59168796208);
#33304=CIRCLE('',#83870,14.98614304973);
#33305=CIRCLE('',#83871,15.29544813031);
#33306=CIRCLE('',#83873,15.35527542921);
#33307=CIRCLE('',#83874,15.65729010739);
#33308=CIRCLE('',#83876,15.10412140798);
#33309=CIRCLE('',#83877,15.41105880551);
#33310=CIRCLE('',#83879,15.40566400734);
#33311=CIRCLE('',#83880,15.70670982437);
#33312=CIRCLE('',#83882,14.98614304973);
#33313=CIRCLE('',#83883,15.29544813031);
#33314=CIRCLE('',#83885,15.10412140798);
#33315=CIRCLE('',#83886,15.41105880551);
#33316=CIRCLE('',#83888,15.45750573369);
#33317=CIRCLE('',#83889,15.75756115352);
#33318=CIRCLE('',#83891,14.98614304973);
#33319=CIRCLE('',#83892,15.29544813031);
#33320=CIRCLE('',#83894,15.43970477396);
#33321=CIRCLE('',#83895,15.7400995393);
#33322=CIRCLE('',#83897,15.43970477396);
#33323=CIRCLE('',#83898,15.7400995393);
#33324=CIRCLE('',#83900,14.72869592011);
#33325=CIRCLE('',#83901,15.0432953008);
#33326=CIRCLE('',#83903,15.45750573369);
#33327=CIRCLE('',#83904,15.75756115352);
#33328=CIRCLE('',#83906,14.87899470754);
#33329=CIRCLE('',#83907,15.19048167462);
#33330=CIRCLE('',#83909,15.35527542921);
#33331=CIRCLE('',#83910,15.65729010739);
#33332=CIRCLE('',#83912,14.72869592011);
#33333=CIRCLE('',#83913,15.0432953008);
#33334=CIRCLE('',#83915,15.40566400734);
#33335=CIRCLE('',#83916,15.70670982437);
#33336=CIRCLE('',#83918,14.87899470754);
#33337=CIRCLE('',#83919,15.19048167462);
#33338=CIRCLE('',#83921,15.20475200412);
#33339=CIRCLE('',#83922,15.50969804693);
#33340=CIRCLE('',#83924,14.72869592011);
#33341=CIRCLE('',#83925,15.0432953008);
#33342=CIRCLE('',#83927,15.28837739941);
#33343=CIRCLE('',#83928,15.59168796208);
#33344=CIRCLE('',#83930,14.87899470754);
#33345=CIRCLE('',#83931,15.19048167462);
#33346=CIRCLE('',#83933,15.20475200412);
#33347=CIRCLE('',#83934,15.50969804693);
#33348=CIRCLE('',#83936,15.01114530963);
#33349=CIRCLE('',#83937,15.31994561044);
#33350=CIRCLE('',#83939,15.28837739941);
#33351=CIRCLE('',#83940,15.59168796208);
#33352=CIRCLE('',#83942,15.12562340887);
#33353=CIRCLE('',#83943,15.4321331483);
#33354=CIRCLE('',#83945,15.20475200412);
#33355=CIRCLE('',#83946,15.50969804693);
#33356=CIRCLE('',#83948,15.22282771061);
#33357=CIRCLE('',#83949,15.52741876511);
#33358=CIRCLE('',#83951,15.28837739941);
#33359=CIRCLE('',#83952,15.59168796208);
#33360=CIRCLE('',#83954,15.3030873848);
#33361=CIRCLE('',#83955,15.60611205608);
#33362=CIRCLE('',#83957,15.20475200412);
#33363=CIRCLE('',#83958,15.50969804693);
#33364=CIRCLE('',#83960,15.36666793768);
#33365=CIRCLE('',#83961,15.66846302312);
#33366=CIRCLE('',#83963,15.28837739941);
#33367=CIRCLE('',#83964,15.59168796208);
#33368=CIRCLE('',#83966,15.41377577062);
#33369=CIRCLE('',#83967,15.71466619139);
#33370=CIRCLE('',#83969,15.20475200412);
#33371=CIRCLE('',#83970,15.50969804693);
#33372=CIRCLE('',#83972,15.44456161589);
#33373=CIRCLE('',#83973,15.74486371827);
#33374=CIRCLE('',#83975,15.28837739941);
#33375=CIRCLE('',#83976,15.59168796208);
#33376=CIRCLE('',#83978,15.45912298634);
#33377=CIRCLE('',#83979,15.75914761359);
#33378=CIRCLE('',#83981,15.20475200412);
#33379=CIRCLE('',#83982,15.50969804693);
#33380=CIRCLE('',#83984,15.45750573369);
#33381=CIRCLE('',#83985,15.75756115352);
#33382=CIRCLE('',#83987,15.28837739941);
#33383=CIRCLE('',#83988,15.59168796208);
#33384=CIRCLE('',#83990,15.43970477396);
#33385=CIRCLE('',#83991,15.7400995393);
#33386=CIRCLE('',#83993,15.20475200412);
#33387=CIRCLE('',#83994,15.50969804693);
#33388=CIRCLE('',#83996,15.40566400734);
#33389=CIRCLE('',#83997,15.70670982437);
#33390=CIRCLE('',#83999,15.28837739941);
#33391=CIRCLE('',#84000,15.59168796208);
#33392=CIRCLE('',#84002,15.35527542921);
#33393=CIRCLE('',#84003,15.65729010739);
#33394=CIRCLE('',#84005,15.20475200412);
#33395=CIRCLE('',#84006,15.50969804693);
#33396=CIRCLE('',#84008,15.28837739941);
#33397=CIRCLE('',#84009,15.59168796208);
#33398=CIRCLE('',#84011,15.28837739941);
#33399=CIRCLE('',#84012,15.59168796208);
#33400=CIRCLE('',#84014,15.20475200412);
#33401=CIRCLE('',#84015,15.50969804693);
#33402=CIRCLE('',#84017,15.35527542921);
#33403=CIRCLE('',#84018,15.65729010739);
#33404=CIRCLE('',#84020,15.28837739941);
#33405=CIRCLE('',#84021,15.59168796208);
#33406=CIRCLE('',#84023,15.40566400734);
#33407=CIRCLE('',#84024,15.70670982437);
#33408=CIRCLE('',#84026,15.20475200412);
#33409=CIRCLE('',#84027,15.50969804693);
#33410=CIRCLE('',#84029,15.43970477396);
#33411=CIRCLE('',#84030,15.7400995393);
#33412=CIRCLE('',#84032,15.28837739941);
#33413=CIRCLE('',#84033,15.59168796208);
#33414=CIRCLE('',#84035,15.45750573369);
#33415=CIRCLE('',#84036,15.75756115352);
#33416=CIRCLE('',#84038,15.20475200412);
#33417=CIRCLE('',#84039,15.50969804693);
#33418=CIRCLE('',#84041,15.43970477396);
#33419=CIRCLE('',#84042,15.7400995393);
#33420=CIRCLE('',#84044,15.01114530963);
#33421=CIRCLE('',#84045,15.31994561044);
#33422=CIRCLE('',#84047,15.45750573369);
#33423=CIRCLE('',#84048,15.75756115352);
#33424=CIRCLE('',#84050,15.12562340887);
#33425=CIRCLE('',#84051,15.4321331483);
#33426=CIRCLE('',#84053,15.35527542921);
#33427=CIRCLE('',#84054,15.65729010739);
#33428=CIRCLE('',#84056,15.01114530963);
#33429=CIRCLE('',#84057,15.31994561044);
#33430=CIRCLE('',#84059,15.40566400734);
#33431=CIRCLE('',#84060,15.70670982437);
#33432=CIRCLE('',#84062,15.12562340887);
#33433=CIRCLE('',#84063,15.4321331483);
#33434=CIRCLE('',#84065,15.35527542921);
#33435=CIRCLE('',#84066,15.65729010739);
#33436=CIRCLE('',#84068,15.22282771061);
#33437=CIRCLE('',#84069,15.52741876511);
#33438=CIRCLE('',#84071,15.40566400734);
#33439=CIRCLE('',#84072,15.70670982437);
#33440=CIRCLE('',#84074,15.3030873848);
#33441=CIRCLE('',#84075,15.60611205608);
#33442=CIRCLE('',#84077,15.35527542921);
#33443=CIRCLE('',#84078,15.65729010739);
#33444=CIRCLE('',#84080,15.36666793768);
#33445=CIRCLE('',#84081,15.66846302312);
#33446=CIRCLE('',#84083,15.40566400734);
#33447=CIRCLE('',#84084,15.70670982437);
#33448=CIRCLE('',#84086,15.41377577062);
#33449=CIRCLE('',#84087,15.71466619139);
#33450=CIRCLE('',#84089,15.35527542921);
#33451=CIRCLE('',#84090,15.65729010739);
#33452=CIRCLE('',#84092,15.44456161589);
#33453=CIRCLE('',#84093,15.74486371827);
#33454=CIRCLE('',#84095,15.40566400734);
#33455=CIRCLE('',#84096,15.70670982437);
#33456=CIRCLE('',#84098,15.45912298634);
#33457=CIRCLE('',#84099,15.75914761359);
#33458=CIRCLE('',#84101,15.35527542921);
#33459=CIRCLE('',#84102,15.65729010739);
#33460=CIRCLE('',#84104,15.45750573369);
#33461=CIRCLE('',#84105,15.75756115352);
#33462=CIRCLE('',#84107,15.40566400734);
#33463=CIRCLE('',#84108,15.70670982437);
#33464=CIRCLE('',#84110,15.43970477396);
#33465=CIRCLE('',#84111,15.7400995393);
#33466=CIRCLE('',#84113,15.35527542921);
#33467=CIRCLE('',#84114,15.65729010739);
#33468=CIRCLE('',#84116,15.40566400734);
#33469=CIRCLE('',#84117,15.70670982437);
#33470=CIRCLE('',#84119,15.40566400734);
#33471=CIRCLE('',#84120,15.70670982437);
#33472=CIRCLE('',#84122,15.35527542921);
#33473=CIRCLE('',#84123,15.65729010739);
#33474=CIRCLE('',#84125,15.43970477396);
#33475=CIRCLE('',#84126,15.7400995393);
#33476=CIRCLE('',#84128,15.40566400734);
#33477=CIRCLE('',#84129,15.70670982437);
#33478=CIRCLE('',#84131,15.45750573369);
#33479=CIRCLE('',#84132,15.75756115352);
#33480=CIRCLE('',#84134,15.35527542921);
#33481=CIRCLE('',#84135,15.65729010739);
#33482=CIRCLE('',#84137,15.43970477396);
#33483=CIRCLE('',#84138,15.7400995393);
#33484=CIRCLE('',#84140,15.22282771061);
#33485=CIRCLE('',#84141,15.52741876511);
#33486=CIRCLE('',#84143,15.45750573369);
#33487=CIRCLE('',#84144,15.75756115352);
#33488=CIRCLE('',#84146,15.3030873848);
#33489=CIRCLE('',#84147,15.60611205608);
#33490=CIRCLE('',#84149,15.43970477396);
#33491=CIRCLE('',#84150,15.7400995393);
#33492=CIRCLE('',#84152,15.36666793768);
#33493=CIRCLE('',#84153,15.66846302312);
#33494=CIRCLE('',#84155,15.45750573369);
#33495=CIRCLE('',#84156,15.75756115352);
#33496=CIRCLE('',#84158,15.41377577062);
#33497=CIRCLE('',#84159,15.71466619139);
#33498=CIRCLE('',#84161,15.43970477396);
#33499=CIRCLE('',#84162,15.7400995393);
#33500=CIRCLE('',#84164,15.44456161589);
#33501=CIRCLE('',#84165,15.74486371827);
#33502=CIRCLE('',#84167,15.45750573369);
#33503=CIRCLE('',#84168,15.75756115352);
#33504=CIRCLE('',#84170,15.45912298634);
#33505=CIRCLE('',#84171,15.75914761359);
#33506=CIRCLE('',#84173,15.43970477396);
#33507=CIRCLE('',#84174,15.7400995393);
#33508=CIRCLE('',#84176,15.45750573369);
#33509=CIRCLE('',#84177,15.75756115352);
#33510=CIRCLE('',#84179,15.45750573369);
#33511=CIRCLE('',#84180,15.75756115352);
#33512=CIRCLE('',#84182,15.43970477396);
#33513=CIRCLE('',#84183,15.7400995393);
#33514=CIRCLE('',#85950,9.152185531336);
#33515=CIRCLE('',#85952,15.45912298634);
#33516=CIRCLE('',#85953,15.44456161589);
#33517=CIRCLE('',#85954,15.44456161589);
#33518=CIRCLE('',#85955,15.45912298634);
#33519=CIRCLE('',#85957,15.75914761359);
#33520=CIRCLE('',#85959,15.74486371827);
#33521=CIRCLE('',#85961,15.74486371827);
#33522=CIRCLE('',#85963,15.75914761359);
#33523=CIRCLE('',#85965,9.25);
#33524=CIRCLE('',#85969,10.25);
#33525=CIRCLE('',#85970,10.25);
#33526=CIRCLE('',#85979,13.);
#33527=CIRCLE('',#85981,13.);
#33528=CIRCLE('',#85989,13.);
#33529=CIRCLE('',#85990,13.);
#33530=CIRCLE('',#85992,12.00000442428);
#33531=CIRCLE('',#86002,9.08769033371916);
#33532=CIRCLE('',#86004,4.9028521085786);
#33533=CIRCLE('',#86012,10.25);
#33534=CIRCLE('',#86013,9.250003127107);
#33535=CIRCLE('',#86015,10.25);
#33536=CIRCLE('',#86021,11.4812930575157);
#33537=CIRCLE('',#86024,9.08769033371916);
#33538=CIRCLE('',#86029,66.65911415553);
#33539=CIRCLE('',#86030,66.65911415553);
#33540=CIRCLE('',#86031,67.66415225213);
#33541=CIRCLE('',#86033,68.);
#33542=CIRCLE('',#86034,67.66415225213);
#33543=CIRCLE('',#86039,10.5);
#33544=CIRCLE('',#86040,10.5);
#33545=CIRCLE('',#86041,10.5);
#33546=CIRCLE('',#86043,11.0000062575399);
#33547=CIRCLE('',#86047,7.75);
#33548=CIRCLE('',#86049,7.75);
#33549=CIRCLE('',#86051,8.249994983965);
#33550=CIRCLE('',#86055,66.65911415553);
#33551=CIRCLE('',#86056,67.);
#33552=CIRCLE('',#86061,10.25);
#33553=CIRCLE('',#86062,10.25);
#33554=CIRCLE('',#86071,13.);
#33555=CIRCLE('',#86073,13.);
#33556=CIRCLE('',#86081,13.);
#33557=CIRCLE('',#86082,13.);
#33558=CIRCLE('',#86084,12.00000442428);
#33559=CIRCLE('',#86094,9.08769033371916);
#33560=CIRCLE('',#86096,4.90285210866692);
#33561=CIRCLE('',#86104,10.25);
#33562=CIRCLE('',#86105,9.250003127107);
#33563=CIRCLE('',#86107,10.25);
#33564=CIRCLE('',#86113,11.4812930573653);
#33565=CIRCLE('',#86116,9.08769033371916);
#33566=CIRCLE('',#86121,66.65911415553);
#33567=CIRCLE('',#86122,66.65911415553);
#33568=CIRCLE('',#86123,67.66415225213);
#33569=CIRCLE('',#86125,68.);
#33570=CIRCLE('',#86126,67.66415225213);
#33571=CIRCLE('',#86131,10.5);
#33572=CIRCLE('',#86132,10.5);
#33573=CIRCLE('',#86133,10.5);
#33574=CIRCLE('',#86135,11.0000062575399);
#33575=CIRCLE('',#86139,7.75);
#33576=CIRCLE('',#86141,7.75);
#33577=CIRCLE('',#86143,8.249994983965);
#33578=CIRCLE('',#86147,66.65911415553);
#33579=CIRCLE('',#86148,67.);
#33580=VERTEX_POINT('',#106598);
#33581=VERTEX_POINT('',#106599);
#33582=VERTEX_POINT('',#106601);
#33583=VERTEX_POINT('',#106603);
#33584=VERTEX_POINT('',#106612);
#33585=VERTEX_POINT('',#106614);
#33586=VERTEX_POINT('',#106653);
#33587=VERTEX_POINT('',#106752);
#33588=VERTEX_POINT('',#106878);
#33589=VERTEX_POINT('',#106879);
#33590=VERTEX_POINT('',#106881);
#33591=VERTEX_POINT('',#106883);
#33592=VERTEX_POINT('',#106927);
#33593=VERTEX_POINT('',#106947);
#33594=VERTEX_POINT('',#106949);
#33595=VERTEX_POINT('',#107028);
#33596=VERTEX_POINT('',#107154);
#33597=VERTEX_POINT('',#107155);
#33598=VERTEX_POINT('',#107168);
#33599=VERTEX_POINT('',#107191);
#33600=VERTEX_POINT('',#107193);
#33601=VERTEX_POINT('',#107206);
#33602=VERTEX_POINT('',#107208);
#33603=VERTEX_POINT('',#107299);
#33604=VERTEX_POINT('',#107300);
#33605=VERTEX_POINT('',#107332);
#33606=VERTEX_POINT('',#107442);
#33607=VERTEX_POINT('',#107577);
#33608=VERTEX_POINT('',#108207);
#33609=VERTEX_POINT('',#108208);
#33610=VERTEX_POINT('',#108210);
#33611=VERTEX_POINT('',#108233);
#33612=VERTEX_POINT('',#108246);
#33613=VERTEX_POINT('',#108253);
#33614=VERTEX_POINT('',#108266);
#33615=VERTEX_POINT('',#108281);
#33616=VERTEX_POINT('',#108282);
#33617=VERTEX_POINT('',#108284);
#33618=VERTEX_POINT('',#108617);
#33619=VERTEX_POINT('',#108635);
#33620=VERTEX_POINT('',#109123);
#33621=VERTEX_POINT('',#109124);
#33622=VERTEX_POINT('',#109126);
#33623=VERTEX_POINT('',#109171);
#33624=VERTEX_POINT('',#109198);
#33625=VERTEX_POINT('',#109253);
#33626=VERTEX_POINT('',#109255);
#33627=VERTEX_POINT('',#109264);
#33628=VERTEX_POINT('',#109324);
#33629=VERTEX_POINT('',#109325);
#33630=VERTEX_POINT('',#109379);
#33631=VERTEX_POINT('',#109439);
#33632=VERTEX_POINT('',#109440);
#33633=VERTEX_POINT('',#109442);
#33634=VERTEX_POINT('',#109455);
#33635=VERTEX_POINT('',#109457);
#33636=VERTEX_POINT('',#109489);
#33637=VERTEX_POINT('',#109490);
#33638=VERTEX_POINT('',#109544);
#33639=VERTEX_POINT('',#109602);
#33640=VERTEX_POINT('',#109603);
#33641=VERTEX_POINT('',#109605);
#33642=VERTEX_POINT('',#109630);
#33643=VERTEX_POINT('',#109679);
#33644=VERTEX_POINT('',#109680);
#33645=VERTEX_POINT('',#109682);
#33646=VERTEX_POINT('',#109723);
#33647=VERTEX_POINT('',#109766);
#33648=VERTEX_POINT('',#109767);
#33649=VERTEX_POINT('',#109994);
#33650=VERTEX_POINT('',#109995);
#33651=VERTEX_POINT('',#110220);
#33652=VERTEX_POINT('',#110221);
#33653=VERTEX_POINT('',#110452);
#33654=VERTEX_POINT('',#110453);
#33655=VERTEX_POINT('',#110455);
#33656=VERTEX_POINT('',#110484);
#33657=VERTEX_POINT('',#110485);
#33658=VERTEX_POINT('',#110487);
#33659=VERTEX_POINT('',#110566);
#33660=VERTEX_POINT('',#110568);
#33661=VERTEX_POINT('',#110647);
#33662=VERTEX_POINT('',#110649);
#33663=VERTEX_POINT('',#110785);
#33664=VERTEX_POINT('',#110786);
#33665=VERTEX_POINT('',#111045);
#33666=VERTEX_POINT('',#111046);
#33667=VERTEX_POINT('',#111048);
#33668=VERTEX_POINT('',#111151);
#33669=VERTEX_POINT('',#111298);
#33670=VERTEX_POINT('',#111300);
#33671=VERTEX_POINT('',#111304);
#33672=VERTEX_POINT('',#111305);
#33673=VERTEX_POINT('',#111307);
#33674=VERTEX_POINT('',#111314);
#33675=VERTEX_POINT('',#111321);
#33676=VERTEX_POINT('',#111330);
#33677=VERTEX_POINT('',#111337);
#33678=VERTEX_POINT('',#111342);
#33679=VERTEX_POINT('',#111349);
#33680=VERTEX_POINT('',#111360);
#33681=VERTEX_POINT('',#111365);
#33682=VERTEX_POINT('',#111367);
#33683=VERTEX_POINT('',#111387);
#33684=VERTEX_POINT('',#111389);
#33685=VERTEX_POINT('',#111394);
#33686=VERTEX_POINT('',#111405);
#33687=VERTEX_POINT('',#111412);
#33688=VERTEX_POINT('',#111417);
#33689=VERTEX_POINT('',#111425);
#33690=VERTEX_POINT('',#111434);
#33691=VERTEX_POINT('',#111448);
#33692=VERTEX_POINT('',#111449);
#33693=VERTEX_POINT('',#111451);
#33694=VERTEX_POINT('',#111453);
#33695=VERTEX_POINT('',#111455);
#33696=VERTEX_POINT('',#111459);
#33697=VERTEX_POINT('',#111460);
#33698=VERTEX_POINT('',#111462);
#33699=VERTEX_POINT('',#111464);
#33700=VERTEX_POINT('',#111481);
#33701=VERTEX_POINT('',#111494);
#33702=VERTEX_POINT('',#111495);
#33703=VERTEX_POINT('',#111497);
#33704=VERTEX_POINT('',#111529);
#33705=VERTEX_POINT('',#111570);
#33706=VERTEX_POINT('',#111574);
#33707=VERTEX_POINT('',#111575);
#33708=VERTEX_POINT('',#111577);
#33709=VERTEX_POINT('',#111579);
#33710=VERTEX_POINT('',#111583);
#33711=VERTEX_POINT('',#111584);
#33712=VERTEX_POINT('',#111586);
#33713=VERTEX_POINT('',#111591);
#33714=VERTEX_POINT('',#111595);
#33715=VERTEX_POINT('',#111596);
#33716=VERTEX_POINT('',#111598);
#33717=VERTEX_POINT('',#111603);
#33718=VERTEX_POINT('',#111607);
#33719=VERTEX_POINT('',#111608);
#33720=VERTEX_POINT('',#111610);
#33721=VERTEX_POINT('',#111612);
#33722=VERTEX_POINT('',#111616);
#33723=VERTEX_POINT('',#111617);
#33724=VERTEX_POINT('',#111624);
#33725=VERTEX_POINT('',#111653);
#33726=VERTEX_POINT('',#111654);
#33727=VERTEX_POINT('',#111716);
#33728=VERTEX_POINT('',#111898);
#33729=VERTEX_POINT('',#111978);
#33730=VERTEX_POINT('',#112004);
#33731=VERTEX_POINT('',#112047);
#33732=VERTEX_POINT('',#112055);
#33733=VERTEX_POINT('',#112234);
#33734=VERTEX_POINT('',#112253);
#33735=VERTEX_POINT('',#112255);
#33736=VERTEX_POINT('',#112258);
#33737=VERTEX_POINT('',#112260);
#33738=VERTEX_POINT('',#112370);
#33739=VERTEX_POINT('',#112451);
#33740=VERTEX_POINT('',#112459);
#33741=VERTEX_POINT('',#112674);
#33742=VERTEX_POINT('',#112703);
#33743=VERTEX_POINT('',#112726);
#33744=VERTEX_POINT('',#112934);
#33745=VERTEX_POINT('',#112935);
#33746=VERTEX_POINT('',#112940);
#33747=VERTEX_POINT('',#112941);
#33748=VERTEX_POINT('',#113000);
#33749=VERTEX_POINT('',#113101);
#33750=VERTEX_POINT('',#113127);
#33751=VERTEX_POINT('',#113129);
#33752=VERTEX_POINT('',#113152);
#33753=VERTEX_POINT('',#113211);
#33754=VERTEX_POINT('',#113312);
#33755=VERTEX_POINT('',#113324);
#33756=VERTEX_POINT('',#113349);
#33757=VERTEX_POINT('',#113350);
#33758=VERTEX_POINT('',#113352);
#33759=VERTEX_POINT('',#113354);
#33760=VERTEX_POINT('',#113356);
#33761=VERTEX_POINT('',#113361);
#33762=VERTEX_POINT('',#113363);
#33763=VERTEX_POINT('',#113370);
#33764=VERTEX_POINT('',#113379);
#33765=VERTEX_POINT('',#113381);
#33766=VERTEX_POINT('',#113383);
#33767=VERTEX_POINT('',#113387);
#33768=VERTEX_POINT('',#113391);
#33769=VERTEX_POINT('',#113393);
#33770=VERTEX_POINT('',#113395);
#33771=VERTEX_POINT('',#113397);
#33772=VERTEX_POINT('',#113410);
#33773=VERTEX_POINT('',#113411);
#33774=VERTEX_POINT('',#113413);
#33775=VERTEX_POINT('',#113428);
#33776=VERTEX_POINT('',#113430);
#33777=VERTEX_POINT('',#113433);
#33778=VERTEX_POINT('',#113450);
#33779=VERTEX_POINT('',#113452);
#33780=VERTEX_POINT('',#113454);
#33781=VERTEX_POINT('',#113458);
#33782=VERTEX_POINT('',#113462);
#33783=VERTEX_POINT('',#113464);
#33784=VERTEX_POINT('',#113468);
#33785=VERTEX_POINT('',#113470);
#33786=VERTEX_POINT('',#113472);
#33787=VERTEX_POINT('',#113474);
#33788=VERTEX_POINT('',#113491);
#33789=VERTEX_POINT('',#113493);
#33790=VERTEX_POINT('',#113495);
#33791=VERTEX_POINT('',#113514);
#33792=VERTEX_POINT('',#113515);
#33793=VERTEX_POINT('',#113518);
#33794=VERTEX_POINT('',#113522);
#33795=VERTEX_POINT('',#113526);
#33796=VERTEX_POINT('',#113527);
#33797=VERTEX_POINT('',#113529);
#33798=VERTEX_POINT('',#113534);
#33799=VERTEX_POINT('',#113535);
#33800=VERTEX_POINT('',#113540);
#33801=VERTEX_POINT('',#113541);
#33802=VERTEX_POINT('',#113543);
#33803=VERTEX_POINT('',#113599);
#33804=VERTEX_POINT('',#113660);
#33805=VERTEX_POINT('',#113661);
#33806=VERTEX_POINT('',#113663);
#33807=VERTEX_POINT('',#113665);
#33808=VERTEX_POINT('',#113926);
#33809=VERTEX_POINT('',#113927);
#33810=VERTEX_POINT('',#113929);
#33811=VERTEX_POINT('',#113936);
#33812=VERTEX_POINT('',#113938);
#33813=VERTEX_POINT('',#113959);
#33814=VERTEX_POINT('',#114226);
#33815=VERTEX_POINT('',#114228);
#33816=VERTEX_POINT('',#114230);
#33817=VERTEX_POINT('',#114234);
#33818=VERTEX_POINT('',#114238);
#33819=VERTEX_POINT('',#114239);
#33820=VERTEX_POINT('',#114274);
#33821=VERTEX_POINT('',#114281);
#33822=VERTEX_POINT('',#114290);
#33823=VERTEX_POINT('',#114319);
#33824=VERTEX_POINT('',#114413);
#33825=VERTEX_POINT('',#114414);
#33826=VERTEX_POINT('',#114461);
#33827=VERTEX_POINT('',#114505);
#33828=VERTEX_POINT('',#114672);
#33829=VERTEX_POINT('',#114812);
#33830=VERTEX_POINT('',#114856);
#33831=VERTEX_POINT('',#114913);
#33832=VERTEX_POINT('',#114916);
#33833=VERTEX_POINT('',#115068);
#33834=VERTEX_POINT('',#115276);
#33835=VERTEX_POINT('',#115277);
#33836=VERTEX_POINT('',#115279);
#33837=VERTEX_POINT('',#115281);
#33838=VERTEX_POINT('',#115283);
#33839=VERTEX_POINT('',#115285);
#33840=VERTEX_POINT('',#115416);
#33841=VERTEX_POINT('',#115457);
#33842=VERTEX_POINT('',#115458);
#33843=VERTEX_POINT('',#115460);
#33844=VERTEX_POINT('',#115462);
#33845=VERTEX_POINT('',#115530);
#33846=VERTEX_POINT('',#115606);
#33847=VERTEX_POINT('',#115608);
#33848=VERTEX_POINT('',#115612);
#33849=VERTEX_POINT('',#115613);
#33850=VERTEX_POINT('',#115615);
#33851=VERTEX_POINT('',#115620);
#33852=VERTEX_POINT('',#115624);
#33853=VERTEX_POINT('',#115625);
#33854=VERTEX_POINT('',#115627);
#33855=VERTEX_POINT('',#115629);
#33856=VERTEX_POINT('',#115634);
#33857=VERTEX_POINT('',#115635);
#33858=VERTEX_POINT('',#115639);
#33859=VERTEX_POINT('',#115643);
#33860=VERTEX_POINT('',#115647);
#33861=VERTEX_POINT('',#115652);
#33862=VERTEX_POINT('',#115656);
#33863=VERTEX_POINT('',#115664);
#33864=VERTEX_POINT('',#115668);
#33865=VERTEX_POINT('',#115669);
#33866=VERTEX_POINT('',#115672);
#33867=VERTEX_POINT('',#115676);
#33868=VERTEX_POINT('',#115680);
#33869=VERTEX_POINT('',#115697);
#33870=VERTEX_POINT('',#115716);
#33871=VERTEX_POINT('',#115718);
#33872=VERTEX_POINT('',#115732);
#33873=VERTEX_POINT('',#115757);
#33874=VERTEX_POINT('',#115764);
#33875=VERTEX_POINT('',#115779);
#33876=VERTEX_POINT('',#115780);
#33877=VERTEX_POINT('',#115827);
#33878=VERTEX_POINT('',#115934);
#33879=VERTEX_POINT('',#116035);
#33880=VERTEX_POINT('',#116092);
#33881=VERTEX_POINT('',#116095);
#33882=VERTEX_POINT('',#116247);
#33883=VERTEX_POINT('',#116273);
#33884=VERTEX_POINT('',#116557);
#33885=VERTEX_POINT('',#116639);
#33886=VERTEX_POINT('',#116640);
#33887=VERTEX_POINT('',#116669);
#33888=VERTEX_POINT('',#116706);
#33889=VERTEX_POINT('',#116708);
#33890=VERTEX_POINT('',#116710);
#33891=VERTEX_POINT('',#116712);
#33892=VERTEX_POINT('',#116716);
#33893=VERTEX_POINT('',#116717);
#33894=VERTEX_POINT('',#116727);
#33895=VERTEX_POINT('',#116747);
#33896=VERTEX_POINT('',#116749);
#33897=VERTEX_POINT('',#116753);
#33898=VERTEX_POINT('',#116755);
#33899=VERTEX_POINT('',#116759);
#33900=VERTEX_POINT('',#116760);
#33901=VERTEX_POINT('',#116762);
#33902=VERTEX_POINT('',#116767);
#33903=VERTEX_POINT('',#116771);
#33904=VERTEX_POINT('',#116772);
#33905=VERTEX_POINT('',#116774);
#33906=VERTEX_POINT('',#116776);
#33907=VERTEX_POINT('',#116781);
#33908=VERTEX_POINT('',#116782);
#33909=VERTEX_POINT('',#116786);
#33910=VERTEX_POINT('',#116790);
#33911=VERTEX_POINT('',#116794);
#33912=VERTEX_POINT('',#116799);
#33913=VERTEX_POINT('',#116803);
#33914=VERTEX_POINT('',#116811);
#33915=VERTEX_POINT('',#116815);
#33916=VERTEX_POINT('',#116816);
#33917=VERTEX_POINT('',#116818);
#33918=VERTEX_POINT('',#116820);
#33919=VERTEX_POINT('',#116822);
#33920=VERTEX_POINT('',#116824);
#33921=VERTEX_POINT('',#116842);
#33922=VERTEX_POINT('',#116843);
#33923=VERTEX_POINT('',#116845);
#33924=VERTEX_POINT('',#116847);
#33925=VERTEX_POINT('',#116882);
#33926=VERTEX_POINT('',#116883);
#33927=VERTEX_POINT('',#116945);
#33928=VERTEX_POINT('',#117049);
#33929=VERTEX_POINT('',#117051);
#33930=VERTEX_POINT('',#117060);
#33931=VERTEX_POINT('',#117062);
#33932=VERTEX_POINT('',#117108);
#33933=VERTEX_POINT('',#117112);
#33934=VERTEX_POINT('',#117114);
#33935=VERTEX_POINT('',#117116);
#33936=VERTEX_POINT('',#117171);
#33937=VERTEX_POINT('',#117230);
#33938=VERTEX_POINT('',#117299);
#33939=VERTEX_POINT('',#117356);
#33940=VERTEX_POINT('',#117360);
#33941=VERTEX_POINT('',#117361);
#33942=VERTEX_POINT('',#117406);
#33943=VERTEX_POINT('',#117407);
#33944=VERTEX_POINT('',#117489);
#33945=VERTEX_POINT('',#117490);
#33946=VERTEX_POINT('',#117503);
#33947=VERTEX_POINT('',#117505);
#33948=VERTEX_POINT('',#117510);
#33949=VERTEX_POINT('',#117512);
#33950=VERTEX_POINT('',#117615);
#33951=VERTEX_POINT('',#117616);
#33952=VERTEX_POINT('',#117680);
#33953=VERTEX_POINT('',#117775);
#33954=VERTEX_POINT('',#117913);
#33955=VERTEX_POINT('',#117922);
#33956=VERTEX_POINT('',#118017);
#33957=VERTEX_POINT('',#118198);
#33958=VERTEX_POINT('',#118200);
#33959=VERTEX_POINT('',#118202);
#33960=VERTEX_POINT('',#118206);
#33961=VERTEX_POINT('',#118210);
#33962=VERTEX_POINT('',#118211);
#33963=VERTEX_POINT('',#118239);
#33964=VERTEX_POINT('',#118363);
#33965=VERTEX_POINT('',#118539);
#33966=VERTEX_POINT('',#118720);
#33967=VERTEX_POINT('',#118957);
#33968=VERTEX_POINT('',#118959);
#33969=VERTEX_POINT('',#118963);
#33970=VERTEX_POINT('',#118970);
#33971=VERTEX_POINT('',#118996);
#33972=VERTEX_POINT('',#119000);
#33973=VERTEX_POINT('',#119359);
#33974=VERTEX_POINT('',#119361);
#33975=VERTEX_POINT('',#119365);
#33976=VERTEX_POINT('',#119369);
#33977=VERTEX_POINT('',#119498);
#33978=VERTEX_POINT('',#119625);
#33979=VERTEX_POINT('',#119650);
#33980=VERTEX_POINT('',#119771);
#33981=VERTEX_POINT('',#119805);
#33982=VERTEX_POINT('',#119870);
#33983=VERTEX_POINT('',#119872);
#33984=VERTEX_POINT('',#119913);
#33985=VERTEX_POINT('',#119973);
#33986=VERTEX_POINT('',#120090);
#33987=VERTEX_POINT('',#120386);
#33988=VERTEX_POINT('',#120452);
#33989=VERTEX_POINT('',#120536);
#33990=VERTEX_POINT('',#120635);
#33991=VERTEX_POINT('',#121905);
#33992=VERTEX_POINT('',#121906);
#33993=VERTEX_POINT('',#122084);
#33994=VERTEX_POINT('',#122356);
#33995=VERTEX_POINT('',#122649);
#33996=VERTEX_POINT('',#123070);
#33997=VERTEX_POINT('',#123593);
#33998=VERTEX_POINT('',#123594);
#33999=VERTEX_POINT('',#123596);
#34000=VERTEX_POINT('',#123598);
#34001=VERTEX_POINT('',#123600);
#34002=VERTEX_POINT('',#123602);
#34003=VERTEX_POINT('',#123651);
#34004=VERTEX_POINT('',#123652);
#34005=VERTEX_POINT('',#123702);
#34006=VERTEX_POINT('',#123741);
#34007=VERTEX_POINT('',#123742);
#34008=VERTEX_POINT('',#123744);
#34009=VERTEX_POINT('',#123746);
#34010=VERTEX_POINT('',#123809);
#34011=VERTEX_POINT('',#123910);
#34012=VERTEX_POINT('',#123912);
#34013=VERTEX_POINT('',#124096);
#34014=VERTEX_POINT('',#124097);
#34015=VERTEX_POINT('',#124099);
#34016=VERTEX_POINT('',#124261);
#34017=VERTEX_POINT('',#124262);
#34018=VERTEX_POINT('',#124360);
#34019=VERTEX_POINT('',#124361);
#34020=VERTEX_POINT('',#124363);
#34021=VERTEX_POINT('',#124365);
#34022=VERTEX_POINT('',#124420);
#34023=VERTEX_POINT('',#124421);
#34024=VERTEX_POINT('',#124432);
#34025=VERTEX_POINT('',#124434);
#34026=VERTEX_POINT('',#124461);
#34027=VERTEX_POINT('',#124468);
#34028=VERTEX_POINT('',#124534);
#34029=VERTEX_POINT('',#124655);
#34030=VERTEX_POINT('',#124659);
#34031=VERTEX_POINT('',#124660);
#34032=VERTEX_POINT('',#124707);
#34033=VERTEX_POINT('',#124714);
#34034=VERTEX_POINT('',#124718);
#34035=VERTEX_POINT('',#124725);
#34036=VERTEX_POINT('',#124842);
#34037=VERTEX_POINT('',#125047);
#34038=VERTEX_POINT('',#125048);
#34039=VERTEX_POINT('',#125109);
#34040=VERTEX_POINT('',#125110);
#34041=VERTEX_POINT('',#125115);
#34042=VERTEX_POINT('',#125410);
#34043=VERTEX_POINT('',#125412);
#34044=VERTEX_POINT('',#125416);
#34045=VERTEX_POINT('',#125509);
#34046=VERTEX_POINT('',#125685);
#34047=VERTEX_POINT('',#125893);
#34048=VERTEX_POINT('',#125898);
#34049=VERTEX_POINT('',#125963);
#34050=VERTEX_POINT('',#125965);
#34051=VERTEX_POINT('',#125967);
#34052=VERTEX_POINT('',#125971);
#34053=VERTEX_POINT('',#125975);
#34054=VERTEX_POINT('',#125976);
#34055=VERTEX_POINT('',#126216);
#34056=VERTEX_POINT('',#126218);
#34057=VERTEX_POINT('',#126222);
#34058=VERTEX_POINT('',#126226);
#34059=VERTEX_POINT('',#126230);
#34060=VERTEX_POINT('',#126357);
#34061=VERTEX_POINT('',#126372);
#34062=VERTEX_POINT('',#126389);
#34063=VERTEX_POINT('',#126411);
#34064=VERTEX_POINT('',#126533);
#34065=VERTEX_POINT('',#126611);
#34066=VERTEX_POINT('',#126613);
#34067=VERTEX_POINT('',#126618);
#34068=VERTEX_POINT('',#126730);
#34069=VERTEX_POINT('',#126973);
#34070=VERTEX_POINT('',#127057);
#34071=VERTEX_POINT('',#127144);
#34072=VERTEX_POINT('',#127205);
#34073=VERTEX_POINT('',#127390);
#34074=VERTEX_POINT('',#128608);
#34075=VERTEX_POINT('',#128623);
#34076=VERTEX_POINT('',#128692);
#34077=VERTEX_POINT('',#128798);
#34078=VERTEX_POINT('',#129092);
#34079=VERTEX_POINT('',#129503);
#34080=VERTEX_POINT('',#130321);
#34081=VERTEX_POINT('',#130322);
#34082=VERTEX_POINT('',#130324);
#34083=VERTEX_POINT('',#130326);
#34084=VERTEX_POINT('',#130328);
#34085=VERTEX_POINT('',#130330);
#34086=VERTEX_POINT('',#130332);
#34087=VERTEX_POINT('',#130334);
#34088=VERTEX_POINT('',#130336);
#34089=VERTEX_POINT('',#130340);
#34090=VERTEX_POINT('',#130341);
#34091=VERTEX_POINT('',#130343);
#34092=VERTEX_POINT('',#130345);
#34093=VERTEX_POINT('',#130347);
#34094=VERTEX_POINT('',#130349);
#34095=VERTEX_POINT('',#130351);
#34096=VERTEX_POINT('',#130353);
#34097=VERTEX_POINT('',#130355);
#34098=VERTEX_POINT('',#130359);
#34099=VERTEX_POINT('',#130361);
#34100=VERTEX_POINT('',#130365);
#34101=VERTEX_POINT('',#130367);
#34102=VERTEX_POINT('',#130371);
#34103=VERTEX_POINT('',#130373);
#34104=VERTEX_POINT('',#130375);
#34105=VERTEX_POINT('',#130403);
#34106=VERTEX_POINT('',#130404);
#34107=VERTEX_POINT('',#130406);
#34108=VERTEX_POINT('',#130460);
#34109=VERTEX_POINT('',#130543);
#34110=VERTEX_POINT('',#130577);
#34111=VERTEX_POINT('',#130582);
#34112=VERTEX_POINT('',#130596);
#34113=VERTEX_POINT('',#130598);
#34114=VERTEX_POINT('',#130600);
#34115=VERTEX_POINT('',#130613);
#34116=VERTEX_POINT('',#130615);
#34117=VERTEX_POINT('',#130827);
#34118=VERTEX_POINT('',#131000);
#34119=VERTEX_POINT('',#131010);
#34120=VERTEX_POINT('',#131015);
#34121=VERTEX_POINT('',#131017);
#34122=VERTEX_POINT('',#131030);
#34123=VERTEX_POINT('',#131032);
#34124=VERTEX_POINT('',#131034);
#34125=VERTEX_POINT('',#131053);
#34126=VERTEX_POINT('',#131157);
#34127=VERTEX_POINT('',#131159);
#34128=VERTEX_POINT('',#131161);
#34129=VERTEX_POINT('',#131189);
#34130=VERTEX_POINT('',#131191);
#34131=VERTEX_POINT('',#131258);
#34132=VERTEX_POINT('',#131314);
#34133=VERTEX_POINT('',#131322);
#34134=VERTEX_POINT('',#131324);
#34135=VERTEX_POINT('',#131348);
#34136=VERTEX_POINT('',#131350);
#34137=VERTEX_POINT('',#131524);
#34138=VERTEX_POINT('',#131535);
#34139=VERTEX_POINT('',#131582);
#34140=VERTEX_POINT('',#131584);
#34141=VERTEX_POINT('',#131865);
#34142=VERTEX_POINT('',#131876);
#34143=VERTEX_POINT('',#131880);
#34144=VERTEX_POINT('',#131891);
#34145=VERTEX_POINT('',#132049);
#34146=VERTEX_POINT('',#132056);
#34147=VERTEX_POINT('',#132383);
#34148=VERTEX_POINT('',#132385);
#34149=VERTEX_POINT('',#132487);
#34150=VERTEX_POINT('',#132489);
#34151=VERTEX_POINT('',#132585);
#34152=VERTEX_POINT('',#132586);
#34153=VERTEX_POINT('',#132588);
#34154=VERTEX_POINT('',#132727);
#34155=VERTEX_POINT('',#132847);
#34156=VERTEX_POINT('',#132848);
#34157=VERTEX_POINT('',#132850);
#34158=VERTEX_POINT('',#132915);
#34159=VERTEX_POINT('',#132916);
#34160=VERTEX_POINT('',#132918);
#34161=VERTEX_POINT('',#132965);
#34162=VERTEX_POINT('',#133060);
#34163=VERTEX_POINT('',#133061);
#34164=VERTEX_POINT('',#133090);
#34165=VERTEX_POINT('',#133153);
#34166=VERTEX_POINT('',#133154);
#34167=VERTEX_POINT('',#133156);
#34168=VERTEX_POINT('',#133206);
#34169=VERTEX_POINT('',#133211);
#34170=VERTEX_POINT('',#133213);
#34171=VERTEX_POINT('',#133248);
#34172=VERTEX_POINT('',#133322);
#34173=VERTEX_POINT('',#133333);
#34174=VERTEX_POINT('',#133377);
#34175=VERTEX_POINT('',#133414);
#34176=VERTEX_POINT('',#133452);
#34177=VERTEX_POINT('',#133458);
#34178=VERTEX_POINT('',#133468);
#34179=VERTEX_POINT('',#133469);
#34180=VERTEX_POINT('',#133471);
#34181=VERTEX_POINT('',#133474);
#34182=VERTEX_POINT('',#133608);
#34183=VERTEX_POINT('',#133771);
#34184=VERTEX_POINT('',#133848);
#34185=VERTEX_POINT('',#133979);
#34186=VERTEX_POINT('',#134347);
#34187=VERTEX_POINT('',#134348);
#34188=VERTEX_POINT('',#134410);
#34189=VERTEX_POINT('',#134412);
#34190=VERTEX_POINT('',#134435);
#34191=VERTEX_POINT('',#134437);
#34192=VERTEX_POINT('',#134562);
#34193=VERTEX_POINT('',#134564);
#34194=VERTEX_POINT('',#134569);
#34195=VERTEX_POINT('',#134582);
#34196=VERTEX_POINT('',#134584);
#34197=VERTEX_POINT('',#134696);
#34198=VERTEX_POINT('',#134698);
#34199=VERTEX_POINT('',#134702);
#34200=VERTEX_POINT('',#134707);
#34201=VERTEX_POINT('',#134709);
#34202=VERTEX_POINT('',#134711);
#34203=VERTEX_POINT('',#134715);
#34204=VERTEX_POINT('',#134904);
#34205=VERTEX_POINT('',#135034);
#34206=VERTEX_POINT('',#135062);
#34207=VERTEX_POINT('',#135215);
#34208=VERTEX_POINT('',#135220);
#34209=VERTEX_POINT('',#135395);
#34210=VERTEX_POINT('',#135397);
#34211=VERTEX_POINT('',#135399);
#34212=VERTEX_POINT('',#135576);
#34213=VERTEX_POINT('',#135605);
#34214=VERTEX_POINT('',#135607);
#34215=VERTEX_POINT('',#135611);
#34216=VERTEX_POINT('',#135613);
#34217=VERTEX_POINT('',#135615);
#34218=VERTEX_POINT('',#135617);
#34219=VERTEX_POINT('',#135621);
#34220=VERTEX_POINT('',#135622);
#34221=VERTEX_POINT('',#135624);
#34222=VERTEX_POINT('',#135626);
#34223=VERTEX_POINT('',#135628);
#34224=VERTEX_POINT('',#135632);
#34225=VERTEX_POINT('',#135643);
#34226=VERTEX_POINT('',#136405);
#34227=VERTEX_POINT('',#136521);
#34228=VERTEX_POINT('',#136819);
#34229=VERTEX_POINT('',#136834);
#34230=VERTEX_POINT('',#137188);
#34231=VERTEX_POINT('',#137834);
#34232=VERTEX_POINT('',#137847);
#34233=VERTEX_POINT('',#137849);
#34234=VERTEX_POINT('',#137881);
#34235=VERTEX_POINT('',#137894);
#34236=VERTEX_POINT('',#137896);
#34237=VERTEX_POINT('',#137933);
#34238=VERTEX_POINT('',#138649);
#34239=VERTEX_POINT('',#138665);
#34240=VERTEX_POINT('',#138667);
#34241=VERTEX_POINT('',#138704);
#34242=VERTEX_POINT('',#138940);
#34243=VERTEX_POINT('',#138986);
#34244=VERTEX_POINT('',#139024);
#34245=VERTEX_POINT('',#139065);
#34246=VERTEX_POINT('',#139067);
#34247=VERTEX_POINT('',#139142);
#34248=VERTEX_POINT('',#139466);
#34249=VERTEX_POINT('',#139468);
#34250=VERTEX_POINT('',#140049);
#34251=VERTEX_POINT('',#140176);
#34252=VERTEX_POINT('',#140244);
#34253=VERTEX_POINT('',#140440);
#34254=VERTEX_POINT('',#140441);
#34255=VERTEX_POINT('',#140536);
#34256=VERTEX_POINT('',#140547);
#34257=VERTEX_POINT('',#140593);
#34258=VERTEX_POINT('',#140648);
#34259=VERTEX_POINT('',#140698);
#34260=VERTEX_POINT('',#140705);
#34261=VERTEX_POINT('',#140806);
#34262=VERTEX_POINT('',#140904);
#34263=VERTEX_POINT('',#140911);
#34264=VERTEX_POINT('',#140964);
#34265=VERTEX_POINT('',#141028);
#34266=VERTEX_POINT('',#141094);
#34267=VERTEX_POINT('',#141096);
#34268=VERTEX_POINT('',#141402);
#34269=VERTEX_POINT('',#141461);
#34270=VERTEX_POINT('',#141478);
#34271=VERTEX_POINT('',#142789);
#34272=VERTEX_POINT('',#142794);
#34273=VERTEX_POINT('',#142796);
#34274=VERTEX_POINT('',#142939);
#34275=VERTEX_POINT('',#142941);
#34276=VERTEX_POINT('',#142964);
#34277=VERTEX_POINT('',#142966);
#34278=VERTEX_POINT('',#143053);
#34279=VERTEX_POINT('',#143055);
#34280=VERTEX_POINT('',#143110);
#34281=VERTEX_POINT('',#143240);
#34282=VERTEX_POINT('',#143251);
#34283=VERTEX_POINT('',#143256);
#34284=VERTEX_POINT('',#143263);
#34285=VERTEX_POINT('',#143301);
#34286=VERTEX_POINT('',#143310);
#34287=VERTEX_POINT('',#143353);
#34288=VERTEX_POINT('',#143480);
#34289=VERTEX_POINT('',#143523);
#34290=VERTEX_POINT('',#143584);
#34291=VERTEX_POINT('',#143688);
#34292=VERTEX_POINT('',#143748);
#34293=VERTEX_POINT('',#143791);
#34294=VERTEX_POINT('',#143852);
#34295=VERTEX_POINT('',#143895);
#34296=VERTEX_POINT('',#143971);
#34297=VERTEX_POINT('',#143975);
#34298=VERTEX_POINT('',#143984);
#34299=VERTEX_POINT('',#143993);
#34300=VERTEX_POINT('',#144003);
#34301=VERTEX_POINT('',#144004);
#34302=VERTEX_POINT('',#144011);
#34303=VERTEX_POINT('',#144020);
#34304=VERTEX_POINT('',#144056);
#34305=VERTEX_POINT('',#144096);
#34306=VERTEX_POINT('',#144122);
#34307=VERTEX_POINT('',#144159);
#34308=VERTEX_POINT('',#144173);
#34309=VERTEX_POINT('',#144210);
#34310=VERTEX_POINT('',#144326);
#34311=VERTEX_POINT('',#144331);
#34312=VERTEX_POINT('',#144372);
#34313=VERTEX_POINT('',#144374);
#34314=VERTEX_POINT('',#144545);
#34315=VERTEX_POINT('',#144682);
#34316=VERTEX_POINT('',#144873);
#34317=VERTEX_POINT('',#144950);
#34318=VERTEX_POINT('',#145130);
#34319=VERTEX_POINT('',#145256);
#34320=VERTEX_POINT('',#145296);
#34321=VERTEX_POINT('',#145304);
#34322=VERTEX_POINT('',#145333);
#34323=VERTEX_POINT('',#145362);
#34324=VERTEX_POINT('',#145408);
#34325=VERTEX_POINT('',#145409);
#34326=VERTEX_POINT('',#145413);
#34327=VERTEX_POINT('',#145414);
#34328=VERTEX_POINT('',#145416);
#34329=VERTEX_POINT('',#145499);
#34330=VERTEX_POINT('',#145501);
#34331=VERTEX_POINT('',#145575);
#34332=VERTEX_POINT('',#145590);
#34333=VERTEX_POINT('',#145594);
#34334=VERTEX_POINT('',#145596);
#34335=VERTEX_POINT('',#145598);
#34336=VERTEX_POINT('',#145600);
#34337=VERTEX_POINT('',#145619);
#34338=VERTEX_POINT('',#145621);
#34339=VERTEX_POINT('',#145627);
#34340=VERTEX_POINT('',#145629);
#34341=VERTEX_POINT('',#145633);
#34342=VERTEX_POINT('',#145635);
#34343=VERTEX_POINT('',#145702);
#34344=VERTEX_POINT('',#145799);
#34345=VERTEX_POINT('',#145833);
#34346=VERTEX_POINT('',#145835);
#34347=VERTEX_POINT('',#145855);
#34348=VERTEX_POINT('',#145886);
#34349=VERTEX_POINT('',#146034);
#34350=VERTEX_POINT('',#146167);
#34351=VERTEX_POINT('',#146226);
#34352=VERTEX_POINT('',#146298);
#34353=VERTEX_POINT('',#146300);
#34354=VERTEX_POINT('',#146311);
#34355=VERTEX_POINT('',#146321);
#34356=VERTEX_POINT('',#146332);
#34357=VERTEX_POINT('',#146334);
#34358=VERTEX_POINT('',#146342);
#34359=VERTEX_POINT('',#146352);
#34360=VERTEX_POINT('',#146363);
#34361=VERTEX_POINT('',#146365);
#34362=VERTEX_POINT('',#146369);
#34363=VERTEX_POINT('',#146461);
#34364=VERTEX_POINT('',#146508);
#34365=VERTEX_POINT('',#146609);
#34366=VERTEX_POINT('',#146611);
#34367=VERTEX_POINT('',#146617);
#34368=VERTEX_POINT('',#146657);
#34369=VERTEX_POINT('',#146908);
#34370=VERTEX_POINT('',#146912);
#34371=VERTEX_POINT('',#146913);
#34372=VERTEX_POINT('',#146915);
#34373=VERTEX_POINT('',#146959);
#34374=VERTEX_POINT('',#147097);
#34375=VERTEX_POINT('',#147114);
#34376=VERTEX_POINT('',#147263);
#34377=VERTEX_POINT('',#147265);
#34378=VERTEX_POINT('',#147400);
#34379=VERTEX_POINT('',#147407);
#34380=VERTEX_POINT('',#147443);
#34381=VERTEX_POINT('',#147450);
#34382=VERTEX_POINT('',#147573);
#34383=VERTEX_POINT('',#147576);
#34384=VERTEX_POINT('',#147611);
#34385=VERTEX_POINT('',#147713);
#34386=VERTEX_POINT('',#147715);
#34387=VERTEX_POINT('',#147782);
#34388=VERTEX_POINT('',#147783);
#34389=VERTEX_POINT('',#148079);
#34390=VERTEX_POINT('',#148248);
#34391=VERTEX_POINT('',#148253);
#34392=VERTEX_POINT('',#148450);
#34393=VERTEX_POINT('',#148456);
#34394=VERTEX_POINT('',#148485);
#34395=VERTEX_POINT('',#148486);
#34396=VERTEX_POINT('',#148488);
#34397=VERTEX_POINT('',#148499);
#34398=VERTEX_POINT('',#148501);
#34399=VERTEX_POINT('',#148506);
#34400=VERTEX_POINT('',#148558);
#34401=VERTEX_POINT('',#148560);
#34402=VERTEX_POINT('',#148582);
#34403=VERTEX_POINT('',#148644);
#34404=VERTEX_POINT('',#148765);
#34405=VERTEX_POINT('',#149134);
#34406=VERTEX_POINT('',#149207);
#34407=VERTEX_POINT('',#149528);
#34408=VERTEX_POINT('',#149580);
#34409=VERTEX_POINT('',#149623);
#34410=VERTEX_POINT('',#149726);
#34411=VERTEX_POINT('',#149817);
#34412=VERTEX_POINT('',#149819);
#34413=VERTEX_POINT('',#149821);
#34414=VERTEX_POINT('',#149823);
#34415=VERTEX_POINT('',#149829);
#34416=VERTEX_POINT('',#149864);
#34417=VERTEX_POINT('',#149866);
#34418=VERTEX_POINT('',#149868);
#34419=VERTEX_POINT('',#149953);
#34420=VERTEX_POINT('',#149955);
#34421=VERTEX_POINT('',#149959);
#34422=VERTEX_POINT('',#149960);
#34423=VERTEX_POINT('',#149984);
#34424=VERTEX_POINT('',#149985);
#34425=VERTEX_POINT('',#150075);
#34426=VERTEX_POINT('',#150077);
#34427=VERTEX_POINT('',#150079);
#34428=VERTEX_POINT('',#150083);
#34429=VERTEX_POINT('',#150084);
#34430=VERTEX_POINT('',#150147);
#34431=VERTEX_POINT('',#150149);
#34432=VERTEX_POINT('',#150151);
#34433=VERTEX_POINT('',#150201);
#34434=VERTEX_POINT('',#150203);
#34435=VERTEX_POINT('',#150256);
#34436=VERTEX_POINT('',#150276);
#34437=VERTEX_POINT('',#150278);
#34438=VERTEX_POINT('',#150407);
#34439=VERTEX_POINT('',#150618);
#34440=VERTEX_POINT('',#150706);
#34441=VERTEX_POINT('',#150803);
#34442=VERTEX_POINT('',#150831);
#34443=VERTEX_POINT('',#150853);
#34444=VERTEX_POINT('',#150955);
#34445=VERTEX_POINT('',#151163);
#34446=VERTEX_POINT('',#151353);
#34447=VERTEX_POINT('',#151361);
#34448=VERTEX_POINT('',#151702);
#34449=VERTEX_POINT('',#151881);
#34450=VERTEX_POINT('',#152219);
#34451=VERTEX_POINT('',#152430);
#34452=VERTEX_POINT('',#152887);
#34453=VERTEX_POINT('',#153252);
#34454=VERTEX_POINT('',#153256);
#34455=VERTEX_POINT('',#153281);
#34456=VERTEX_POINT('',#153443);
#34457=VERTEX_POINT('',#153674);
#34458=VERTEX_POINT('',#153685);
#34459=VERTEX_POINT('',#153863);
#34460=VERTEX_POINT('',#153874);
#34461=VERTEX_POINT('',#153984);
#34462=VERTEX_POINT('',#154098);
#34463=VERTEX_POINT('',#154116);
#34464=VERTEX_POINT('',#154194);
#34465=VERTEX_POINT('',#154222);
#34466=VERTEX_POINT('',#154250);
#34467=VERTEX_POINT('',#154331);
#34468=VERTEX_POINT('',#154338);
#34469=VERTEX_POINT('',#154404);
#34470=VERTEX_POINT('',#154514);
#34471=VERTEX_POINT('',#154628);
#34472=VERTEX_POINT('',#154827);
#34473=VERTEX_POINT('',#154830);
#34474=VERTEX_POINT('',#154834);
#34475=VERTEX_POINT('',#154840);
#34476=VERTEX_POINT('',#154950);
#34477=VERTEX_POINT('',#154957);
#34478=VERTEX_POINT('',#154965);
#34479=VERTEX_POINT('',#155003);
#34480=VERTEX_POINT('',#155075);
#34481=VERTEX_POINT('',#155148);
#34482=VERTEX_POINT('',#155153);
#34483=VERTEX_POINT('',#155483);
#34484=VERTEX_POINT('',#155617);
#34485=VERTEX_POINT('',#155721);
#34486=VERTEX_POINT('',#155980);
#34487=VERTEX_POINT('',#156250);
#34488=VERTEX_POINT('',#156807);
#34489=VERTEX_POINT('',#156865);
#34490=VERTEX_POINT('',#156998);
#34491=VERTEX_POINT('',#157254);
#34492=VERTEX_POINT('',#157362);
#34493=VERTEX_POINT('',#158207);
#34494=VERTEX_POINT('',#158208);
#34495=VERTEX_POINT('',#158210);
#34496=VERTEX_POINT('',#158251);
#34497=VERTEX_POINT('',#158253);
#34498=VERTEX_POINT('',#158296);
#34499=VERTEX_POINT('',#158297);
#34500=VERTEX_POINT('',#158317);
#34501=VERTEX_POINT('',#158441);
#34502=VERTEX_POINT('',#158443);
#34503=VERTEX_POINT('',#158462);
#34504=VERTEX_POINT('',#158464);
#34505=VERTEX_POINT('',#158466);
#34506=VERTEX_POINT('',#158488);
#34507=VERTEX_POINT('',#158499);
#34508=VERTEX_POINT('',#158629);
#34509=VERTEX_POINT('',#158630);
#34510=VERTEX_POINT('',#158647);
#34511=VERTEX_POINT('',#158664);
#34512=VERTEX_POINT('',#158666);
#34513=VERTEX_POINT('',#158681);
#34514=VERTEX_POINT('',#158712);
#34515=VERTEX_POINT('',#158713);
#34516=VERTEX_POINT('',#158715);
#34517=VERTEX_POINT('',#158717);
#34518=VERTEX_POINT('',#158719);
#34519=VERTEX_POINT('',#158738);
#34520=VERTEX_POINT('',#158740);
#34521=VERTEX_POINT('',#158766);
#34522=VERTEX_POINT('',#158768);
#34523=VERTEX_POINT('',#158772);
#34524=VERTEX_POINT('',#158776);
#34525=VERTEX_POINT('',#158777);
#34526=VERTEX_POINT('',#158806);
#34527=VERTEX_POINT('',#158812);
#34528=VERTEX_POINT('',#158862);
#34529=VERTEX_POINT('',#158866);
#34530=VERTEX_POINT('',#158867);
#34531=VERTEX_POINT('',#158873);
#34532=VERTEX_POINT('',#158902);
#34533=VERTEX_POINT('',#158904);
#34534=VERTEX_POINT('',#158995);
#34535=VERTEX_POINT('',#158996);
#34536=VERTEX_POINT('',#159025);
#34537=VERTEX_POINT('',#159057);
#34538=VERTEX_POINT('',#159058);
#34539=VERTEX_POINT('',#159060);
#34540=VERTEX_POINT('',#159062);
#34541=VERTEX_POINT('',#159066);
#34542=VERTEX_POINT('',#159068);
#34543=VERTEX_POINT('',#159072);
#34544=VERTEX_POINT('',#159076);
#34545=VERTEX_POINT('',#159082);
#34546=VERTEX_POINT('',#159083);
#34547=VERTEX_POINT('',#159085);
#34548=VERTEX_POINT('',#159087);
#34549=VERTEX_POINT('',#159091);
#34550=VERTEX_POINT('',#159093);
#34551=VERTEX_POINT('',#159097);
#34552=VERTEX_POINT('',#159101);
#34553=VERTEX_POINT('',#159107);
#34554=VERTEX_POINT('',#159108);
#34555=VERTEX_POINT('',#159110);
#34556=VERTEX_POINT('',#159112);
#34557=VERTEX_POINT('',#159116);
#34558=VERTEX_POINT('',#159118);
#34559=VERTEX_POINT('',#159122);
#34560=VERTEX_POINT('',#159124);
#34561=VERTEX_POINT('',#159128);
#34562=VERTEX_POINT('',#159130);
#34563=VERTEX_POINT('',#159134);
#34564=VERTEX_POINT('',#159136);
#34565=VERTEX_POINT('',#159140);
#34566=VERTEX_POINT('',#159142);
#34567=VERTEX_POINT('',#159146);
#34568=VERTEX_POINT('',#159150);
#34569=VERTEX_POINT('',#159154);
#34570=VERTEX_POINT('',#159158);
#34571=VERTEX_POINT('',#159162);
#34572=VERTEX_POINT('',#159163);
#34573=VERTEX_POINT('',#159168);
#34574=VERTEX_POINT('',#159172);
#34575=VERTEX_POINT('',#159174);
#34576=VERTEX_POINT('',#159333);
#34577=VERTEX_POINT('',#159400);
#34578=VERTEX_POINT('',#159402);
#34579=VERTEX_POINT('',#159509);
#34580=VERTEX_POINT('',#159511);
#34581=VERTEX_POINT('',#159515);
#34582=VERTEX_POINT('',#159575);
#34583=VERTEX_POINT('',#159678);
#34584=VERTEX_POINT('',#159683);
#34585=VERTEX_POINT('',#159690);
#34586=VERTEX_POINT('',#159694);
#34587=VERTEX_POINT('',#159702);
#34588=VERTEX_POINT('',#159703);
#34589=VERTEX_POINT('',#159705);
#34590=VERTEX_POINT('',#159707);
#34591=VERTEX_POINT('',#159709);
#34592=VERTEX_POINT('',#159711);
#34593=VERTEX_POINT('',#159713);
#34594=VERTEX_POINT('',#159715);
#34595=VERTEX_POINT('',#159719);
#34596=VERTEX_POINT('',#159721);
#34597=VERTEX_POINT('',#159725);
#34598=VERTEX_POINT('',#159729);
#34599=VERTEX_POINT('',#159733);
#34600=VERTEX_POINT('',#159737);
#34601=VERTEX_POINT('',#159741);
#34602=VERTEX_POINT('',#159745);
#34603=VERTEX_POINT('',#159800);
#34604=VERTEX_POINT('',#159802);
#34605=VERTEX_POINT('',#159823);
#34606=VERTEX_POINT('',#159846);
#34607=VERTEX_POINT('',#159869);
#34608=VERTEX_POINT('',#159877);
#34609=VERTEX_POINT('',#159935);
#34610=VERTEX_POINT('',#160082);
#34611=VERTEX_POINT('',#160224);
#34612=VERTEX_POINT('',#160331);
#34613=VERTEX_POINT('',#160499);
#34614=VERTEX_POINT('',#160556);
#34615=VERTEX_POINT('',#160663);
#34616=VERTEX_POINT('',#160674);
#34617=VERTEX_POINT('',#160676);
#34618=VERTEX_POINT('',#160864);
#34619=VERTEX_POINT('',#160883);
#34620=VERTEX_POINT('',#160978);
#34621=VERTEX_POINT('',#161428);
#34622=VERTEX_POINT('',#161430);
#34623=VERTEX_POINT('',#161939);
#34624=VERTEX_POINT('',#161940);
#34625=VERTEX_POINT('',#161942);
#34626=VERTEX_POINT('',#162145);
#34627=VERTEX_POINT('',#162328);
#34628=VERTEX_POINT('',#162329);
#34629=VERTEX_POINT('',#162746);
#34630=VERTEX_POINT('',#162955);
#34631=VERTEX_POINT('',#163164);
#34632=VERTEX_POINT('',#163165);
#34633=VERTEX_POINT('',#163570);
#34634=VERTEX_POINT('',#163571);
#34635=VERTEX_POINT('',#163773);
#34636=VERTEX_POINT('',#163991);
#34637=VERTEX_POINT('',#163992);
#34638=VERTEX_POINT('',#164419);
#34639=VERTEX_POINT('',#164420);
#34640=VERTEX_POINT('',#164422);
#34641=VERTEX_POINT('',#164831);
#34642=VERTEX_POINT('',#164832);
#34643=VERTEX_POINT('',#164834);
#34644=VERTEX_POINT('',#164973);
#34645=VERTEX_POINT('',#165104);
#34646=VERTEX_POINT('',#165105);
#34647=VERTEX_POINT('',#165634);
#34648=VERTEX_POINT('',#165635);
#34649=VERTEX_POINT('',#166148);
#34650=VERTEX_POINT('',#166149);
#34651=VERTEX_POINT('',#166151);
#34652=VERTEX_POINT('',#166412);
#34653=VERTEX_POINT('',#166684);
#34654=VERTEX_POINT('',#166685);
#34655=VERTEX_POINT('',#167208);
#34656=VERTEX_POINT('',#167209);
#34657=VERTEX_POINT('',#167728);
#34658=VERTEX_POINT('',#167729);
#34659=VERTEX_POINT('',#168254);
#34660=VERTEX_POINT('',#168255);
#34661=VERTEX_POINT('',#168281);
#34662=VERTEX_POINT('',#168282);
#34663=VERTEX_POINT('',#168284);
#34664=VERTEX_POINT('',#168455);
#34665=VERTEX_POINT('',#168628);
#34666=VERTEX_POINT('',#168629);
#34667=VERTEX_POINT('',#169156);
#34668=VERTEX_POINT('',#169157);
#34669=VERTEX_POINT('',#169672);
#34670=VERTEX_POINT('',#169673);
#34671=VERTEX_POINT('',#170190);
#34672=VERTEX_POINT('',#170191);
#34673=VERTEX_POINT('',#170716);
#34674=VERTEX_POINT('',#170717);
#34675=VERTEX_POINT('',#170719);
#34676=VERTEX_POINT('',#170874);
#34677=VERTEX_POINT('',#171015);
#34678=VERTEX_POINT('',#171016);
#34679=VERTEX_POINT('',#171445);
#34680=VERTEX_POINT('',#171446);
#34681=VERTEX_POINT('',#171889);
#34682=VERTEX_POINT('',#171890);
#34683=VERTEX_POINT('',#172333);
#34684=VERTEX_POINT('',#172548);
#34685=VERTEX_POINT('',#172767);
#34686=VERTEX_POINT('',#172768);
#34687=VERTEX_POINT('',#173203);
#34688=VERTEX_POINT('',#173204);
#34689=VERTEX_POINT('',#173208);
#34690=VERTEX_POINT('',#173212);
#34691=VERTEX_POINT('',#173216);
#34692=VERTEX_POINT('',#173219);
#34693=VERTEX_POINT('',#173223);
#34694=VERTEX_POINT('',#173231);
#34695=VERTEX_POINT('',#173272);
#34696=VERTEX_POINT('',#173293);
#34697=VERTEX_POINT('',#173295);
#34698=VERTEX_POINT('',#173297);
#34699=VERTEX_POINT('',#173301);
#34700=VERTEX_POINT('',#173303);
#34701=VERTEX_POINT('',#173307);
#34702=VERTEX_POINT('',#173309);
#34703=VERTEX_POINT('',#173313);
#34704=VERTEX_POINT('',#173512);
#34705=VERTEX_POINT('',#173701);
#34706=VERTEX_POINT('',#173709);
#34707=VERTEX_POINT('',#173750);
#34708=VERTEX_POINT('',#173751);
#34709=VERTEX_POINT('',#173776);
#34710=VERTEX_POINT('',#173795);
#34711=VERTEX_POINT('',#173796);
#34712=VERTEX_POINT('',#173798);
#34713=VERTEX_POINT('',#173803);
#34714=VERTEX_POINT('',#173805);
#34715=VERTEX_POINT('',#173809);
#34716=VERTEX_POINT('',#173813);
#34717=VERTEX_POINT('',#173817);
#34718=VERTEX_POINT('',#173818);
#34719=VERTEX_POINT('',#173820);
#34720=VERTEX_POINT('',#173822);
#34721=VERTEX_POINT('',#173880);
#34722=VERTEX_POINT('',#173947);
#34723=VERTEX_POINT('',#174617);
#34724=VERTEX_POINT('',#174619);
#34725=VERTEX_POINT('',#174623);
#34726=VERTEX_POINT('',#174625);
#34727=VERTEX_POINT('',#174629);
#34728=VERTEX_POINT('',#174631);
#34729=VERTEX_POINT('',#174635);
#34730=VERTEX_POINT('',#174637);
#34731=VERTEX_POINT('',#174641);
#34732=VERTEX_POINT('',#174643);
#34733=VERTEX_POINT('',#174647);
#34734=VERTEX_POINT('',#174649);
#34735=VERTEX_POINT('',#174658);
#34736=VERTEX_POINT('',#174659);
#34737=VERTEX_POINT('',#174661);
#34738=VERTEX_POINT('',#174663);
#34739=VERTEX_POINT('',#174665);
#34740=VERTEX_POINT('',#174667);
#34741=VERTEX_POINT('',#174688);
#34742=VERTEX_POINT('',#174690);
#34743=VERTEX_POINT('',#174694);
#34744=VERTEX_POINT('',#174696);
#34745=VERTEX_POINT('',#174700);
#34746=VERTEX_POINT('',#174702);
#34747=VERTEX_POINT('',#174704);
#34748=VERTEX_POINT('',#174706);
#34749=VERTEX_POINT('',#174708);
#34750=VERTEX_POINT('',#174710);
#34751=VERTEX_POINT('',#174712);
#34752=VERTEX_POINT('',#174714);
#34753=VERTEX_POINT('',#174716);
#34754=VERTEX_POINT('',#174718);
#34755=VERTEX_POINT('',#174720);
#34756=VERTEX_POINT('',#174722);
#34757=VERTEX_POINT('',#174724);
#34758=VERTEX_POINT('',#174726);
#34759=VERTEX_POINT('',#174730);
#34760=VERTEX_POINT('',#174732);
#34761=VERTEX_POINT('',#174736);
#34762=VERTEX_POINT('',#174738);
#34763=VERTEX_POINT('',#174742);
#34764=VERTEX_POINT('',#174744);
#34765=VERTEX_POINT('',#174767);
#34766=VERTEX_POINT('',#174768);
#34767=VERTEX_POINT('',#174770);
#34768=VERTEX_POINT('',#174811);
#34769=VERTEX_POINT('',#174846);
#34770=VERTEX_POINT('',#174925);
#34771=VERTEX_POINT('',#174926);
#34772=VERTEX_POINT('',#175091);
#34773=VERTEX_POINT('',#175092);
#34774=VERTEX_POINT('',#175094);
#34775=VERTEX_POINT('',#175105);
#34776=VERTEX_POINT('',#175121);
#34777=VERTEX_POINT('',#175122);
#34778=VERTEX_POINT('',#175124);
#34779=VERTEX_POINT('',#175165);
#34780=VERTEX_POINT('',#175176);
#34781=VERTEX_POINT('',#175187);
#34782=VERTEX_POINT('',#175189);
#34783=VERTEX_POINT('',#175200);
#34784=VERTEX_POINT('',#175211);
#34785=VERTEX_POINT('',#175252);
#34786=VERTEX_POINT('',#175332);
#34787=VERTEX_POINT('',#175333);
#34788=VERTEX_POINT('',#175492);
#34789=VERTEX_POINT('',#175493);
#34790=VERTEX_POINT('',#175577);
#34791=VERTEX_POINT('',#175657);
#34792=VERTEX_POINT('',#175658);
#34793=VERTEX_POINT('',#175660);
#34794=VERTEX_POINT('',#175814);
#34795=VERTEX_POINT('',#175815);
#34796=VERTEX_POINT('',#175817);
#34797=VERTEX_POINT('',#175828);
#34798=VERTEX_POINT('',#175830);
#34799=VERTEX_POINT('',#175894);
#34800=VERTEX_POINT('',#175943);
#34801=VERTEX_POINT('',#176131);
#34802=VERTEX_POINT('',#176132);
#34803=VERTEX_POINT('',#176149);
#34804=VERTEX_POINT('',#176174);
#34805=VERTEX_POINT('',#176242);
#34806=VERTEX_POINT('',#176258);
#34807=VERTEX_POINT('',#176259);
#34808=VERTEX_POINT('',#176263);
#34809=VERTEX_POINT('',#176265);
#34810=VERTEX_POINT('',#176269);
#34811=VERTEX_POINT('',#176271);
#34812=VERTEX_POINT('',#176275);
#34813=VERTEX_POINT('',#176277);
#34814=VERTEX_POINT('',#176281);
#34815=VERTEX_POINT('',#176283);
#34816=VERTEX_POINT('',#176287);
#34817=VERTEX_POINT('',#176289);
#34818=VERTEX_POINT('',#176292);
#34819=VERTEX_POINT('',#176294);
#34820=VERTEX_POINT('',#176300);
#34821=VERTEX_POINT('',#176301);
#34822=VERTEX_POINT('',#176305);
#34823=VERTEX_POINT('',#176307);
#34824=VERTEX_POINT('',#176311);
#34825=VERTEX_POINT('',#176313);
#34826=VERTEX_POINT('',#176317);
#34827=VERTEX_POINT('',#176319);
#34828=VERTEX_POINT('',#176323);
#34829=VERTEX_POINT('',#176325);
#34830=VERTEX_POINT('',#176329);
#34831=VERTEX_POINT('',#176331);
#34832=VERTEX_POINT('',#176334);
#34833=VERTEX_POINT('',#176336);
#34834=VERTEX_POINT('',#177868);
#34835=VERTEX_POINT('',#177870);
#34836=VERTEX_POINT('',#177874);
#34837=VERTEX_POINT('',#177876);
#34838=VERTEX_POINT('',#177880);
#34839=VERTEX_POINT('',#177882);
#34840=VERTEX_POINT('',#177884);
#34841=VERTEX_POINT('',#177886);
#34842=VERTEX_POINT('',#177888);
#34843=VERTEX_POINT('',#177890);
#34844=VERTEX_POINT('',#177892);
#34845=VERTEX_POINT('',#177894);
#34846=VERTEX_POINT('',#177896);
#34847=VERTEX_POINT('',#177898);
#34848=VERTEX_POINT('',#177900);
#34849=VERTEX_POINT('',#177902);
#34850=VERTEX_POINT('',#177904);
#34851=VERTEX_POINT('',#177906);
#34852=VERTEX_POINT('',#177910);
#34853=VERTEX_POINT('',#177912);
#34854=VERTEX_POINT('',#177916);
#34855=VERTEX_POINT('',#177918);
#34856=VERTEX_POINT('',#177922);
#34857=VERTEX_POINT('',#177924);
#34858=VERTEX_POINT('',#177947);
#34859=VERTEX_POINT('',#177949);
#34860=VERTEX_POINT('',#177953);
#34861=VERTEX_POINT('',#177957);
#34862=VERTEX_POINT('',#177958);
#34863=VERTEX_POINT('',#177960);
#34864=VERTEX_POINT('',#177962);
#34865=VERTEX_POINT('',#177969);
#34866=VERTEX_POINT('',#177971);
#34867=VERTEX_POINT('',#177975);
#34868=VERTEX_POINT('',#177979);
#34869=VERTEX_POINT('',#177981);
#34870=VERTEX_POINT('',#177987);
#34871=VERTEX_POINT('',#177990);
#34872=VERTEX_POINT('',#177997);
#34873=VERTEX_POINT('',#177998);
#34874=VERTEX_POINT('',#178000);
#34875=VERTEX_POINT('',#178043);
#34876=VERTEX_POINT('',#178078);
#34877=VERTEX_POINT('',#178153);
#34878=VERTEX_POINT('',#178154);
#34879=VERTEX_POINT('',#178319);
#34880=VERTEX_POINT('',#178320);
#34881=VERTEX_POINT('',#178322);
#34882=VERTEX_POINT('',#178333);
#34883=VERTEX_POINT('',#178349);
#34884=VERTEX_POINT('',#178350);
#34885=VERTEX_POINT('',#178352);
#34886=VERTEX_POINT('',#178397);
#34887=VERTEX_POINT('',#178408);
#34888=VERTEX_POINT('',#178419);
#34889=VERTEX_POINT('',#178421);
#34890=VERTEX_POINT('',#178432);
#34891=VERTEX_POINT('',#178443);
#34892=VERTEX_POINT('',#178486);
#34893=VERTEX_POINT('',#178568);
#34894=VERTEX_POINT('',#178569);
#34895=VERTEX_POINT('',#178734);
#34896=VERTEX_POINT('',#178735);
#34897=VERTEX_POINT('',#178815);
#34898=VERTEX_POINT('',#178903);
#34899=VERTEX_POINT('',#178904);
#34900=VERTEX_POINT('',#178906);
#34901=VERTEX_POINT('',#179062);
#34902=VERTEX_POINT('',#179063);
#34903=VERTEX_POINT('',#179065);
#34904=VERTEX_POINT('',#179076);
#34905=VERTEX_POINT('',#179078);
#34906=VERTEX_POINT('',#179142);
#34907=VERTEX_POINT('',#179191);
#34908=VERTEX_POINT('',#179375);
#34909=VERTEX_POINT('',#179376);
#34910=VERTEX_POINT('',#179393);
#34911=VERTEX_POINT('',#179418);
#34912=VERTEX_POINT('',#179486);
#34913=VERTEX_POINT('',#179502);
#34914=VERTEX_POINT('',#179503);
#34915=VERTEX_POINT('',#179507);
#34916=VERTEX_POINT('',#179509);
#34917=VERTEX_POINT('',#179513);
#34918=VERTEX_POINT('',#179515);
#34919=VERTEX_POINT('',#179519);
#34920=VERTEX_POINT('',#179521);
#34921=VERTEX_POINT('',#179525);
#34922=VERTEX_POINT('',#179527);
#34923=VERTEX_POINT('',#179531);
#34924=VERTEX_POINT('',#179533);
#34925=VERTEX_POINT('',#179536);
#34926=VERTEX_POINT('',#179538);
#34927=VERTEX_POINT('',#179544);
#34928=VERTEX_POINT('',#179545);
#34929=VERTEX_POINT('',#179549);
#34930=VERTEX_POINT('',#179551);
#34931=VERTEX_POINT('',#179555);
#34932=VERTEX_POINT('',#179557);
#34933=VERTEX_POINT('',#179561);
#34934=VERTEX_POINT('',#179563);
#34935=VERTEX_POINT('',#179567);
#34936=VERTEX_POINT('',#179569);
#34937=VERTEX_POINT('',#179573);
#34938=VERTEX_POINT('',#179575);
#34939=VERTEX_POINT('',#179578);
#34940=VERTEX_POINT('',#179580);
#34941=VERTEX_POINT('',#181112);
#34942=VERTEX_POINT('',#181114);
#34943=VERTEX_POINT('',#181116);
#34944=VERTEX_POINT('',#181120);
#34945=VERTEX_POINT('',#181124);
#34946=VERTEX_POINT('',#181125);
#34947=VERTEX_POINT('',#181127);
#34948=VERTEX_POINT('',#181238);
#34949=VERTEX_POINT('',#181317);
#34950=VERTEX_POINT('',#181318);
#34951=VERTEX_POINT('',#181681);
#34952=VERTEX_POINT('',#181682);
#34953=VERTEX_POINT('',#182043);
#34954=VERTEX_POINT('',#182044);
#34955=VERTEX_POINT('',#182066);
#34956=VERTEX_POINT('',#182067);
#34957=VERTEX_POINT('',#182069);
#34958=VERTEX_POINT('',#182148);
#34959=VERTEX_POINT('',#182207);
#34960=VERTEX_POINT('',#182208);
#34961=VERTEX_POINT('',#182589);
#34962=VERTEX_POINT('',#182591);
#34963=VERTEX_POINT('',#182593);
#34964=VERTEX_POINT('',#182595);
#34965=VERTEX_POINT('',#182597);
#34966=VERTEX_POINT('',#182599);
#34967=VERTEX_POINT('',#182601);
#34968=VERTEX_POINT('',#182603);
#34969=VERTEX_POINT('',#182605);
#34970=VERTEX_POINT('',#182607);
#34971=VERTEX_POINT('',#182611);
#34972=VERTEX_POINT('',#182612);
#34973=VERTEX_POINT('',#182628);
#34974=VERTEX_POINT('',#182630);
#34975=VERTEX_POINT('',#182634);
#34976=VERTEX_POINT('',#182811);
#34977=VERTEX_POINT('',#182974);
#34978=VERTEX_POINT('',#182975);
#34979=VERTEX_POINT('',#182982);
#34980=VERTEX_POINT('',#183013);
#34981=VERTEX_POINT('',#183014);
#34982=VERTEX_POINT('',#183016);
#34983=VERTEX_POINT('',#183021);
#34984=VERTEX_POINT('',#183022);
#34985=VERTEX_POINT('',#183024);
#34986=VERTEX_POINT('',#183026);
#34987=VERTEX_POINT('',#183028);
#34988=VERTEX_POINT('',#183030);
#34989=VERTEX_POINT('',#183042);
#34990=VERTEX_POINT('',#183053);
#34991=VERTEX_POINT('',#183058);
#34992=VERTEX_POINT('',#183186);
#34993=VERTEX_POINT('',#183445);
#34994=VERTEX_POINT('',#183447);
#34995=VERTEX_POINT('',#183451);
#34996=VERTEX_POINT('',#183455);
#34997=VERTEX_POINT('',#183459);
#34998=VERTEX_POINT('',#183460);
#34999=VERTEX_POINT('',#183462);
#35000=VERTEX_POINT('',#183467);
#35001=VERTEX_POINT('',#183469);
#35002=VERTEX_POINT('',#183471);
#35003=VERTEX_POINT('',#183475);
#35004=VERTEX_POINT('',#183479);
#35005=VERTEX_POINT('',#183485);
#35006=VERTEX_POINT('',#183487);
#35007=VERTEX_POINT('',#183491);
#35008=VERTEX_POINT('',#183495);
#35009=VERTEX_POINT('',#183497);
#35010=VERTEX_POINT('',#183501);
#35011=VERTEX_POINT('',#183503);
#35012=VERTEX_POINT('',#183731);
#35013=VERTEX_POINT('',#183746);
#35014=VERTEX_POINT('',#183759);
#35015=VERTEX_POINT('',#183761);
#35016=VERTEX_POINT('',#183765);
#35017=VERTEX_POINT('',#183769);
#35018=VERTEX_POINT('',#183770);
#35019=VERTEX_POINT('',#183772);
#35020=VERTEX_POINT('',#183774);
#35021=VERTEX_POINT('',#183781);
#35022=VERTEX_POINT('',#183783);
#35023=VERTEX_POINT('',#183787);
#35024=VERTEX_POINT('',#183791);
#35025=VERTEX_POINT('',#183793);
#35026=VERTEX_POINT('',#183799);
#35027=VERTEX_POINT('',#183802);
#35028=VERTEX_POINT('',#183809);
#35029=VERTEX_POINT('',#183810);
#35030=VERTEX_POINT('',#183812);
#35031=VERTEX_POINT('',#183823);
#35032=VERTEX_POINT('',#183824);
#35033=VERTEX_POINT('',#183908);
#35034=VERTEX_POINT('',#183965);
#35035=VERTEX_POINT('',#183966);
#35036=VERTEX_POINT('',#184163);
#35037=VERTEX_POINT('',#184164);
#35038=VERTEX_POINT('',#184166);
#35039=VERTEX_POINT('',#184349);
#35040=VERTEX_POINT('',#184350);
#35041=VERTEX_POINT('',#184352);
#35042=VERTEX_POINT('',#184357);
#35043=VERTEX_POINT('',#184361);
#35044=VERTEX_POINT('',#184365);
#35045=VERTEX_POINT('',#184366);
#35046=VERTEX_POINT('',#184385);
#35047=VERTEX_POINT('',#184387);
#35048=VERTEX_POINT('',#184408);
#35049=VERTEX_POINT('',#184409);
#35050=VERTEX_POINT('',#184428);
#35051=VERTEX_POINT('',#184430);
#35052=VERTEX_POINT('',#184451);
#35053=VERTEX_POINT('',#184453);
#35054=VERTEX_POINT('',#184455);
#35055=VERTEX_POINT('',#184475);
#35056=VERTEX_POINT('',#184477);
#35057=VERTEX_POINT('',#184482);
#35058=VERTEX_POINT('',#184483);
#35059=VERTEX_POINT('',#184485);
#35060=VERTEX_POINT('',#184504);
#35061=VERTEX_POINT('',#184525);
#35062=VERTEX_POINT('',#184526);
#35063=VERTEX_POINT('',#184528);
#35064=VERTEX_POINT('',#184547);
#35065=VERTEX_POINT('',#184568);
#35066=VERTEX_POINT('',#184570);
#35067=VERTEX_POINT('',#184592);
#35068=VERTEX_POINT('',#184593);
#35069=VERTEX_POINT('',#184615);
#35070=VERTEX_POINT('',#184617);
#35071=VERTEX_POINT('',#184638);
#35072=VERTEX_POINT('',#184640);
#35073=VERTEX_POINT('',#184642);
#35074=VERTEX_POINT('',#184644);
#35075=VERTEX_POINT('',#184664);
#35076=VERTEX_POINT('',#184666);
#35077=VERTEX_POINT('',#184671);
#35078=VERTEX_POINT('',#184673);
#35079=VERTEX_POINT('',#184694);
#35080=VERTEX_POINT('',#184696);
#35081=VERTEX_POINT('',#184717);
#35082=VERTEX_POINT('',#184719);
#35083=VERTEX_POINT('',#184741);
#35084=VERTEX_POINT('',#184745);
#35085=VERTEX_POINT('',#184747);
#35086=VERTEX_POINT('',#184751);
#35087=VERTEX_POINT('',#184753);
#35088=VERTEX_POINT('',#184757);
#35089=VERTEX_POINT('',#184761);
#35090=VERTEX_POINT('',#184763);
#35091=VERTEX_POINT('',#184767);
#35092=VERTEX_POINT('',#184771);
#35093=VERTEX_POINT('',#184773);
#35094=VERTEX_POINT('',#184777);
#35095=VERTEX_POINT('',#184779);
#35096=VERTEX_POINT('',#184783);
#35097=VERTEX_POINT('',#184785);
#35098=VERTEX_POINT('',#184789);
#35099=VERTEX_POINT('',#184790);
#35100=VERTEX_POINT('',#184792);
#35101=VERTEX_POINT('',#184794);
#35102=VERTEX_POINT('',#184796);
#35103=VERTEX_POINT('',#184798);
#35104=VERTEX_POINT('',#184800);
#35105=VERTEX_POINT('',#184802);
#35106=VERTEX_POINT('',#184804);
#35107=VERTEX_POINT('',#184807);
#35108=VERTEX_POINT('',#184811);
#35109=VERTEX_POINT('',#184868);
#35110=VERTEX_POINT('',#184870);
#35111=VERTEX_POINT('',#184909);
#35112=VERTEX_POINT('',#184911);
#35113=VERTEX_POINT('',#185054);
#35114=VERTEX_POINT('',#185055);
#35115=VERTEX_POINT('',#185480);
#35116=VERTEX_POINT('',#185495);
#35117=VERTEX_POINT('',#185589);
#35118=VERTEX_POINT('',#185591);
#35119=VERTEX_POINT('',#185668);
#35120=VERTEX_POINT('',#185793);
#35121=VERTEX_POINT('',#186008);
#35122=VERTEX_POINT('',#186429);
#35123=VERTEX_POINT('',#186586);
#35124=VERTEX_POINT('',#186591);
#35125=VERTEX_POINT('',#186597);
#35126=VERTEX_POINT('',#186603);
#35127=VERTEX_POINT('',#186615);
#35128=VERTEX_POINT('',#187063);
#35129=VERTEX_POINT('',#187078);
#35130=VERTEX_POINT('',#187079);
#35131=VERTEX_POINT('',#187081);
#35132=VERTEX_POINT('',#187083);
#35133=VERTEX_POINT('',#187087);
#35134=VERTEX_POINT('',#187089);
#35135=VERTEX_POINT('',#187091);
#35136=VERTEX_POINT('',#187095);
#35137=VERTEX_POINT('',#187097);
#35138=VERTEX_POINT('',#187102);
#35139=VERTEX_POINT('',#187108);
#35140=VERTEX_POINT('',#187109);
#35141=VERTEX_POINT('',#187111);
#35142=VERTEX_POINT('',#187113);
#35143=VERTEX_POINT('',#187117);
#35144=VERTEX_POINT('',#187118);
#35145=VERTEX_POINT('',#187120);
#35146=VERTEX_POINT('',#187125);
#35147=VERTEX_POINT('',#187127);
#35148=VERTEX_POINT('',#187132);
#35149=VERTEX_POINT('',#187138);
#35150=VERTEX_POINT('',#187139);
#35151=VERTEX_POINT('',#187141);
#35152=VERTEX_POINT('',#187143);
#35153=VERTEX_POINT('',#187147);
#35154=VERTEX_POINT('',#187148);
#35155=VERTEX_POINT('',#187153);
#35156=VERTEX_POINT('',#187154);
#35157=VERTEX_POINT('',#187159);
#35158=VERTEX_POINT('',#187166);
#35159=VERTEX_POINT('',#187167);
#35160=VERTEX_POINT('',#187169);
#35161=VERTEX_POINT('',#187171);
#35162=VERTEX_POINT('',#187175);
#35163=VERTEX_POINT('',#187176);
#35164=VERTEX_POINT('',#187181);
#35165=VERTEX_POINT('',#187182);
#35166=VERTEX_POINT('',#187190);
#35167=VERTEX_POINT('',#187191);
#35168=VERTEX_POINT('',#187193);
#35169=VERTEX_POINT('',#187195);
#35170=VERTEX_POINT('',#187199);
#35171=VERTEX_POINT('',#187200);
#35172=VERTEX_POINT('',#187205);
#35173=VERTEX_POINT('',#187206);
#35174=VERTEX_POINT('',#187214);
#35175=VERTEX_POINT('',#187215);
#35176=VERTEX_POINT('',#187217);
#35177=VERTEX_POINT('',#187219);
#35178=VERTEX_POINT('',#187223);
#35179=VERTEX_POINT('',#187224);
#35180=VERTEX_POINT('',#187229);
#35181=VERTEX_POINT('',#187230);
#35182=VERTEX_POINT('',#187238);
#35183=VERTEX_POINT('',#187239);
#35184=VERTEX_POINT('',#187241);
#35185=VERTEX_POINT('',#187243);
#35186=VERTEX_POINT('',#187247);
#35187=VERTEX_POINT('',#187248);
#35188=VERTEX_POINT('',#187253);
#35189=VERTEX_POINT('',#187254);
#35190=VERTEX_POINT('',#187262);
#35191=VERTEX_POINT('',#187263);
#35192=VERTEX_POINT('',#187265);
#35193=VERTEX_POINT('',#187267);
#35194=VERTEX_POINT('',#187271);
#35195=VERTEX_POINT('',#187272);
#35196=VERTEX_POINT('',#187274);
#35197=VERTEX_POINT('',#187279);
#35198=VERTEX_POINT('',#187281);
#35199=VERTEX_POINT('',#187286);
#35200=VERTEX_POINT('',#187292);
#35201=VERTEX_POINT('',#187293);
#35202=VERTEX_POINT('',#187295);
#35203=VERTEX_POINT('',#187297);
#35204=VERTEX_POINT('',#187301);
#35205=VERTEX_POINT('',#187302);
#35206=VERTEX_POINT('',#187304);
#35207=VERTEX_POINT('',#187309);
#35208=VERTEX_POINT('',#187310);
#35209=VERTEX_POINT('',#187315);
#35210=VERTEX_POINT('',#187322);
#35211=VERTEX_POINT('',#187323);
#35212=VERTEX_POINT('',#187325);
#35213=VERTEX_POINT('',#187327);
#35214=VERTEX_POINT('',#187331);
#35215=VERTEX_POINT('',#187332);
#35216=VERTEX_POINT('',#187334);
#35217=VERTEX_POINT('',#187339);
#35218=VERTEX_POINT('',#187340);
#35219=VERTEX_POINT('',#187345);
#35220=VERTEX_POINT('',#187352);
#35221=VERTEX_POINT('',#187353);
#35222=VERTEX_POINT('',#187355);
#35223=VERTEX_POINT('',#187357);
#35224=VERTEX_POINT('',#187361);
#35225=VERTEX_POINT('',#187362);
#35226=VERTEX_POINT('',#187367);
#35227=VERTEX_POINT('',#187368);
#35228=VERTEX_POINT('',#187370);
#35229=VERTEX_POINT('',#187375);
#35230=VERTEX_POINT('',#187382);
#35231=VERTEX_POINT('',#187383);
#35232=VERTEX_POINT('',#187385);
#35233=VERTEX_POINT('',#187387);
#35234=VERTEX_POINT('',#187391);
#35235=VERTEX_POINT('',#187392);
#35236=VERTEX_POINT('',#187397);
#35237=VERTEX_POINT('',#187398);
#35238=VERTEX_POINT('',#187406);
#35239=VERTEX_POINT('',#187407);
#35240=VERTEX_POINT('',#187409);
#35241=VERTEX_POINT('',#187411);
#35242=VERTEX_POINT('',#187415);
#35243=VERTEX_POINT('',#187416);
#35244=VERTEX_POINT('',#187418);
#35245=VERTEX_POINT('',#187423);
#35246=VERTEX_POINT('',#187424);
#35247=VERTEX_POINT('',#187429);
#35248=VERTEX_POINT('',#187436);
#35249=VERTEX_POINT('',#187437);
#35250=VERTEX_POINT('',#187439);
#35251=VERTEX_POINT('',#187441);
#35252=VERTEX_POINT('',#187445);
#35253=VERTEX_POINT('',#187446);
#35254=VERTEX_POINT('',#187448);
#35255=VERTEX_POINT('',#187453);
#35256=VERTEX_POINT('',#187454);
#35257=VERTEX_POINT('',#187459);
#35258=VERTEX_POINT('',#187466);
#35259=VERTEX_POINT('',#187467);
#35260=VERTEX_POINT('',#187469);
#35261=VERTEX_POINT('',#187471);
#35262=VERTEX_POINT('',#187475);
#35263=VERTEX_POINT('',#187476);
#35264=VERTEX_POINT('',#187478);
#35265=VERTEX_POINT('',#187483);
#35266=VERTEX_POINT('',#187484);
#35267=VERTEX_POINT('',#187489);
#35268=VERTEX_POINT('',#187496);
#35269=VERTEX_POINT('',#187497);
#35270=VERTEX_POINT('',#187499);
#35271=VERTEX_POINT('',#187501);
#35272=VERTEX_POINT('',#187505);
#35273=VERTEX_POINT('',#187506);
#35274=VERTEX_POINT('',#187508);
#35275=VERTEX_POINT('',#187513);
#35276=VERTEX_POINT('',#187514);
#35277=VERTEX_POINT('',#187519);
#35278=VERTEX_POINT('',#187526);
#35279=VERTEX_POINT('',#187527);
#35280=VERTEX_POINT('',#187529);
#35281=VERTEX_POINT('',#187531);
#35282=VERTEX_POINT('',#187535);
#35283=VERTEX_POINT('',#187536);
#35284=VERTEX_POINT('',#187541);
#35285=VERTEX_POINT('',#187542);
#35286=VERTEX_POINT('',#187550);
#35287=VERTEX_POINT('',#187551);
#35288=VERTEX_POINT('',#187553);
#35289=VERTEX_POINT('',#187555);
#35290=VERTEX_POINT('',#187559);
#35291=VERTEX_POINT('',#187560);
#35292=VERTEX_POINT('',#187565);
#35293=VERTEX_POINT('',#187566);
#35294=VERTEX_POINT('',#187574);
#35295=VERTEX_POINT('',#187575);
#35296=VERTEX_POINT('',#187577);
#35297=VERTEX_POINT('',#187579);
#35298=VERTEX_POINT('',#187583);
#35299=VERTEX_POINT('',#187584);
#35300=VERTEX_POINT('',#187589);
#35301=VERTEX_POINT('',#187590);
#35302=VERTEX_POINT('',#187598);
#35303=VERTEX_POINT('',#187599);
#35304=VERTEX_POINT('',#187601);
#35305=VERTEX_POINT('',#187603);
#35306=VERTEX_POINT('',#187607);
#35307=VERTEX_POINT('',#187608);
#35308=VERTEX_POINT('',#187613);
#35309=VERTEX_POINT('',#187614);
#35310=VERTEX_POINT('',#187622);
#35311=VERTEX_POINT('',#187623);
#35312=VERTEX_POINT('',#187625);
#35313=VERTEX_POINT('',#187627);
#35314=VERTEX_POINT('',#187631);
#35315=VERTEX_POINT('',#187632);
#35316=VERTEX_POINT('',#187637);
#35317=VERTEX_POINT('',#187638);
#35318=VERTEX_POINT('',#187646);
#35319=VERTEX_POINT('',#187647);
#35320=VERTEX_POINT('',#187649);
#35321=VERTEX_POINT('',#187651);
#35322=VERTEX_POINT('',#187655);
#35323=VERTEX_POINT('',#187656);
#35324=VERTEX_POINT('',#187661);
#35325=VERTEX_POINT('',#187662);
#35326=VERTEX_POINT('',#187670);
#35327=VERTEX_POINT('',#187671);
#35328=VERTEX_POINT('',#187673);
#35329=VERTEX_POINT('',#187675);
#35330=VERTEX_POINT('',#187679);
#35331=VERTEX_POINT('',#187681);
#35332=VERTEX_POINT('',#187685);
#35333=VERTEX_POINT('',#187686);
#35334=VERTEX_POINT('',#187689);
#35335=VERTEX_POINT('',#187694);
#35336=VERTEX_POINT('',#187700);
#35337=VERTEX_POINT('',#187701);
#35338=VERTEX_POINT('',#187703);
#35339=VERTEX_POINT('',#187705);
#35340=VERTEX_POINT('',#187709);
#35341=VERTEX_POINT('',#187710);
#35342=VERTEX_POINT('',#187712);
#35343=VERTEX_POINT('',#187717);
#35344=VERTEX_POINT('',#187718);
#35345=VERTEX_POINT('',#187723);
#35346=VERTEX_POINT('',#187730);
#35347=VERTEX_POINT('',#187731);
#35348=VERTEX_POINT('',#187733);
#35349=VERTEX_POINT('',#187735);
#35350=VERTEX_POINT('',#187739);
#35351=VERTEX_POINT('',#187740);
#35352=VERTEX_POINT('',#187745);
#35353=VERTEX_POINT('',#187746);
#35354=VERTEX_POINT('',#187754);
#35355=VERTEX_POINT('',#187755);
#35356=VERTEX_POINT('',#187757);
#35357=VERTEX_POINT('',#187759);
#35358=VERTEX_POINT('',#187763);
#35359=VERTEX_POINT('',#187764);
#35360=VERTEX_POINT('',#187769);
#35361=VERTEX_POINT('',#187770);
#35362=VERTEX_POINT('',#187778);
#35363=VERTEX_POINT('',#187779);
#35364=VERTEX_POINT('',#187781);
#35365=VERTEX_POINT('',#187783);
#35366=VERTEX_POINT('',#187787);
#35367=VERTEX_POINT('',#187788);
#35368=VERTEX_POINT('',#187793);
#35369=VERTEX_POINT('',#187794);
#35370=VERTEX_POINT('',#187802);
#35371=VERTEX_POINT('',#187803);
#35372=VERTEX_POINT('',#187805);
#35373=VERTEX_POINT('',#187807);
#35374=VERTEX_POINT('',#187811);
#35375=VERTEX_POINT('',#187812);
#35376=VERTEX_POINT('',#187817);
#35377=VERTEX_POINT('',#187818);
#35378=VERTEX_POINT('',#187826);
#35379=VERTEX_POINT('',#187827);
#35380=VERTEX_POINT('',#187829);
#35381=VERTEX_POINT('',#187831);
#35382=VERTEX_POINT('',#187835);
#35383=VERTEX_POINT('',#187836);
#35384=VERTEX_POINT('',#187841);
#35385=VERTEX_POINT('',#187842);
#35386=VERTEX_POINT('',#187850);
#35387=VERTEX_POINT('',#187851);
#35388=VERTEX_POINT('',#187853);
#35389=VERTEX_POINT('',#187855);
#35390=VERTEX_POINT('',#187859);
#35391=VERTEX_POINT('',#187860);
#35392=VERTEX_POINT('',#187865);
#35393=VERTEX_POINT('',#187866);
#35394=VERTEX_POINT('',#187874);
#35395=VERTEX_POINT('',#187875);
#35396=VERTEX_POINT('',#187877);
#35397=VERTEX_POINT('',#187879);
#35398=VERTEX_POINT('',#187883);
#35399=VERTEX_POINT('',#187884);
#35400=VERTEX_POINT('',#187889);
#35401=VERTEX_POINT('',#187890);
#35402=VERTEX_POINT('',#187898);
#35403=VERTEX_POINT('',#187899);
#35404=VERTEX_POINT('',#187901);
#35405=VERTEX_POINT('',#187903);
#35406=VERTEX_POINT('',#187907);
#35407=VERTEX_POINT('',#187908);
#35408=VERTEX_POINT('',#187913);
#35409=VERTEX_POINT('',#187914);
#35410=VERTEX_POINT('',#187922);
#35411=VERTEX_POINT('',#187923);
#35412=VERTEX_POINT('',#187925);
#35413=VERTEX_POINT('',#187927);
#35414=VERTEX_POINT('',#187931);
#35415=VERTEX_POINT('',#187932);
#35416=VERTEX_POINT('',#187934);
#35417=VERTEX_POINT('',#187939);
#35418=VERTEX_POINT('',#187940);
#35419=VERTEX_POINT('',#187945);
#35420=VERTEX_POINT('',#187952);
#35421=VERTEX_POINT('',#187953);
#35422=VERTEX_POINT('',#187955);
#35423=VERTEX_POINT('',#187957);
#35424=VERTEX_POINT('',#187961);
#35425=VERTEX_POINT('',#187962);
#35426=VERTEX_POINT('',#187964);
#35427=VERTEX_POINT('',#187969);
#35428=VERTEX_POINT('',#187970);
#35429=VERTEX_POINT('',#187975);
#35430=VERTEX_POINT('',#187982);
#35431=VERTEX_POINT('',#187983);
#35432=VERTEX_POINT('',#187985);
#35433=VERTEX_POINT('',#187987);
#35434=VERTEX_POINT('',#187991);
#35435=VERTEX_POINT('',#187992);
#35436=VERTEX_POINT('',#187997);
#35437=VERTEX_POINT('',#187998);
#35438=VERTEX_POINT('',#188006);
#35439=VERTEX_POINT('',#188007);
#35440=VERTEX_POINT('',#188009);
#35441=VERTEX_POINT('',#188011);
#35442=VERTEX_POINT('',#188015);
#35443=VERTEX_POINT('',#188016);
#35444=VERTEX_POINT('',#188021);
#35445=VERTEX_POINT('',#188022);
#35446=VERTEX_POINT('',#188030);
#35447=VERTEX_POINT('',#188031);
#35448=VERTEX_POINT('',#188033);
#35449=VERTEX_POINT('',#188035);
#35450=VERTEX_POINT('',#188039);
#35451=VERTEX_POINT('',#188040);
#35452=VERTEX_POINT('',#188045);
#35453=VERTEX_POINT('',#188046);
#35454=VERTEX_POINT('',#188054);
#35455=VERTEX_POINT('',#188055);
#35456=VERTEX_POINT('',#188057);
#35457=VERTEX_POINT('',#188059);
#35458=VERTEX_POINT('',#188063);
#35459=VERTEX_POINT('',#188064);
#35460=VERTEX_POINT('',#188069);
#35461=VERTEX_POINT('',#188070);
#35462=VERTEX_POINT('',#188078);
#35463=VERTEX_POINT('',#188079);
#35464=VERTEX_POINT('',#188081);
#35465=VERTEX_POINT('',#188083);
#35466=VERTEX_POINT('',#188087);
#35467=VERTEX_POINT('',#188088);
#35468=VERTEX_POINT('',#188093);
#35469=VERTEX_POINT('',#188094);
#35470=VERTEX_POINT('',#188102);
#35471=VERTEX_POINT('',#188103);
#35472=VERTEX_POINT('',#188105);
#35473=VERTEX_POINT('',#188107);
#35474=VERTEX_POINT('',#188111);
#35475=VERTEX_POINT('',#188112);
#35476=VERTEX_POINT('',#188117);
#35477=VERTEX_POINT('',#188118);
#35478=VERTEX_POINT('',#188126);
#35479=VERTEX_POINT('',#188127);
#35480=VERTEX_POINT('',#188129);
#35481=VERTEX_POINT('',#188131);
#35482=VERTEX_POINT('',#188135);
#35483=VERTEX_POINT('',#188136);
#35484=VERTEX_POINT('',#188141);
#35485=VERTEX_POINT('',#188142);
#35486=VERTEX_POINT('',#188150);
#35487=VERTEX_POINT('',#188151);
#35488=VERTEX_POINT('',#188153);
#35489=VERTEX_POINT('',#188155);
#35490=VERTEX_POINT('',#188159);
#35491=VERTEX_POINT('',#188160);
#35492=VERTEX_POINT('',#188165);
#35493=VERTEX_POINT('',#188166);
#35494=VERTEX_POINT('',#188174);
#35495=VERTEX_POINT('',#188175);
#35496=VERTEX_POINT('',#188177);
#35497=VERTEX_POINT('',#188179);
#35498=VERTEX_POINT('',#188183);
#35499=VERTEX_POINT('',#188184);
#35500=VERTEX_POINT('',#188189);
#35501=VERTEX_POINT('',#188190);
#35502=VERTEX_POINT('',#188198);
#35503=VERTEX_POINT('',#188199);
#35504=VERTEX_POINT('',#188201);
#35505=VERTEX_POINT('',#188203);
#35506=VERTEX_POINT('',#188207);
#35507=VERTEX_POINT('',#188208);
#35508=VERTEX_POINT('',#188213);
#35509=VERTEX_POINT('',#188214);
#35510=VERTEX_POINT('',#188222);
#35511=VERTEX_POINT('',#188223);
#35512=VERTEX_POINT('',#188225);
#35513=VERTEX_POINT('',#188229);
#35514=VERTEX_POINT('',#188230);
#35515=VERTEX_POINT('',#188232);
#35516=VERTEX_POINT('',#188234);
#35517=VERTEX_POINT('',#188238);
#35518=VERTEX_POINT('',#188239);
#35519=VERTEX_POINT('',#188244);
#35520=VERTEX_POINT('',#188252);
#35521=VERTEX_POINT('',#188253);
#35522=VERTEX_POINT('',#188255);
#35523=VERTEX_POINT('',#188257);
#35524=VERTEX_POINT('',#188261);
#35525=VERTEX_POINT('',#188262);
#35526=VERTEX_POINT('',#188267);
#35527=VERTEX_POINT('',#188268);
#35528=VERTEX_POINT('',#188276);
#35529=VERTEX_POINT('',#188277);
#35530=VERTEX_POINT('',#188279);
#35531=VERTEX_POINT('',#188281);
#35532=VERTEX_POINT('',#188285);
#35533=VERTEX_POINT('',#188286);
#35534=VERTEX_POINT('',#188291);
#35535=VERTEX_POINT('',#188292);
#35536=VERTEX_POINT('',#188300);
#35537=VERTEX_POINT('',#188301);
#35538=VERTEX_POINT('',#188303);
#35539=VERTEX_POINT('',#188305);
#35540=VERTEX_POINT('',#188309);
#35541=VERTEX_POINT('',#188310);
#35542=VERTEX_POINT('',#188315);
#35543=VERTEX_POINT('',#188316);
#35544=VERTEX_POINT('',#188324);
#35545=VERTEX_POINT('',#188325);
#35546=VERTEX_POINT('',#188327);
#35547=VERTEX_POINT('',#188329);
#35548=VERTEX_POINT('',#188333);
#35549=VERTEX_POINT('',#188334);
#35550=VERTEX_POINT('',#188339);
#35551=VERTEX_POINT('',#188340);
#35552=VERTEX_POINT('',#188348);
#35553=VERTEX_POINT('',#188349);
#35554=VERTEX_POINT('',#188351);
#35555=VERTEX_POINT('',#188353);
#35556=VERTEX_POINT('',#188357);
#35557=VERTEX_POINT('',#188358);
#35558=VERTEX_POINT('',#188363);
#35559=VERTEX_POINT('',#188364);
#35560=VERTEX_POINT('',#188372);
#35561=VERTEX_POINT('',#188373);
#35562=VERTEX_POINT('',#188375);
#35563=VERTEX_POINT('',#188377);
#35564=VERTEX_POINT('',#188381);
#35565=VERTEX_POINT('',#188382);
#35566=VERTEX_POINT('',#188387);
#35567=VERTEX_POINT('',#188388);
#35568=VERTEX_POINT('',#188396);
#35569=VERTEX_POINT('',#188397);
#35570=VERTEX_POINT('',#188399);
#35571=VERTEX_POINT('',#188401);
#35572=VERTEX_POINT('',#188405);
#35573=VERTEX_POINT('',#188406);
#35574=VERTEX_POINT('',#188411);
#35575=VERTEX_POINT('',#188412);
#35576=VERTEX_POINT('',#188420);
#35577=VERTEX_POINT('',#188421);
#35578=VERTEX_POINT('',#188423);
#35579=VERTEX_POINT('',#188425);
#35580=VERTEX_POINT('',#188429);
#35581=VERTEX_POINT('',#188430);
#35582=VERTEX_POINT('',#188435);
#35583=VERTEX_POINT('',#188436);
#35584=VERTEX_POINT('',#188444);
#35585=VERTEX_POINT('',#188445);
#35586=VERTEX_POINT('',#188447);
#35587=VERTEX_POINT('',#188449);
#35588=VERTEX_POINT('',#188453);
#35589=VERTEX_POINT('',#188454);
#35590=VERTEX_POINT('',#188459);
#35591=VERTEX_POINT('',#188460);
#35592=VERTEX_POINT('',#188468);
#35593=VERTEX_POINT('',#188469);
#35594=VERTEX_POINT('',#188471);
#35595=VERTEX_POINT('',#188473);
#35596=VERTEX_POINT('',#188477);
#35597=VERTEX_POINT('',#188478);
#35598=VERTEX_POINT('',#188483);
#35599=VERTEX_POINT('',#188484);
#35600=VERTEX_POINT('',#188492);
#35601=VERTEX_POINT('',#188493);
#35602=VERTEX_POINT('',#188495);
#35603=VERTEX_POINT('',#188497);
#35604=VERTEX_POINT('',#188501);
#35605=VERTEX_POINT('',#188502);
#35606=VERTEX_POINT('',#188507);
#35607=VERTEX_POINT('',#188508);
#35608=VERTEX_POINT('',#188510);
#35609=VERTEX_POINT('',#188515);
#35610=VERTEX_POINT('',#188522);
#35611=VERTEX_POINT('',#188523);
#35612=VERTEX_POINT('',#188525);
#35613=VERTEX_POINT('',#188527);
#35614=VERTEX_POINT('',#188531);
#35615=VERTEX_POINT('',#188532);
#35616=VERTEX_POINT('',#188537);
#35617=VERTEX_POINT('',#188538);
#35618=VERTEX_POINT('',#188540);
#35619=VERTEX_POINT('',#188545);
#35620=VERTEX_POINT('',#188552);
#35621=VERTEX_POINT('',#188553);
#35622=VERTEX_POINT('',#188555);
#35623=VERTEX_POINT('',#188557);
#35624=VERTEX_POINT('',#188561);
#35625=VERTEX_POINT('',#188562);
#35626=VERTEX_POINT('',#188567);
#35627=VERTEX_POINT('',#188568);
#35628=VERTEX_POINT('',#188576);
#35629=VERTEX_POINT('',#188577);
#35630=VERTEX_POINT('',#188579);
#35631=VERTEX_POINT('',#188581);
#35632=VERTEX_POINT('',#188585);
#35633=VERTEX_POINT('',#188586);
#35634=VERTEX_POINT('',#188591);
#35635=VERTEX_POINT('',#188592);
#35636=VERTEX_POINT('',#188600);
#35637=VERTEX_POINT('',#188601);
#35638=VERTEX_POINT('',#188603);
#35639=VERTEX_POINT('',#188605);
#35640=VERTEX_POINT('',#188609);
#35641=VERTEX_POINT('',#188610);
#35642=VERTEX_POINT('',#188615);
#35643=VERTEX_POINT('',#188616);
#35644=VERTEX_POINT('',#188624);
#35645=VERTEX_POINT('',#188625);
#35646=VERTEX_POINT('',#188627);
#35647=VERTEX_POINT('',#188629);
#35648=VERTEX_POINT('',#188633);
#35649=VERTEX_POINT('',#188634);
#35650=VERTEX_POINT('',#188639);
#35651=VERTEX_POINT('',#188640);
#35652=VERTEX_POINT('',#188648);
#35653=VERTEX_POINT('',#188649);
#35654=VERTEX_POINT('',#188651);
#35655=VERTEX_POINT('',#188653);
#35656=VERTEX_POINT('',#188657);
#35657=VERTEX_POINT('',#188658);
#35658=VERTEX_POINT('',#188663);
#35659=VERTEX_POINT('',#188664);
#35660=VERTEX_POINT('',#188672);
#35661=VERTEX_POINT('',#188673);
#35662=VERTEX_POINT('',#188675);
#35663=VERTEX_POINT('',#188677);
#35664=VERTEX_POINT('',#188681);
#35665=VERTEX_POINT('',#188682);
#35666=VERTEX_POINT('',#188687);
#35667=VERTEX_POINT('',#188688);
#35668=VERTEX_POINT('',#188696);
#35669=VERTEX_POINT('',#188697);
#35670=VERTEX_POINT('',#188699);
#35671=VERTEX_POINT('',#188701);
#35672=VERTEX_POINT('',#188705);
#35673=VERTEX_POINT('',#188706);
#35674=VERTEX_POINT('',#188711);
#35675=VERTEX_POINT('',#188712);
#35676=VERTEX_POINT('',#188720);
#35677=VERTEX_POINT('',#188721);
#35678=VERTEX_POINT('',#188723);
#35679=VERTEX_POINT('',#188725);
#35680=VERTEX_POINT('',#188729);
#35681=VERTEX_POINT('',#188730);
#35682=VERTEX_POINT('',#188735);
#35683=VERTEX_POINT('',#188736);
#35684=VERTEX_POINT('',#188744);
#35685=VERTEX_POINT('',#188745);
#35686=VERTEX_POINT('',#188747);
#35687=VERTEX_POINT('',#188749);
#35688=VERTEX_POINT('',#188753);
#35689=VERTEX_POINT('',#188754);
#35690=VERTEX_POINT('',#188759);
#35691=VERTEX_POINT('',#188760);
#35692=VERTEX_POINT('',#188768);
#35693=VERTEX_POINT('',#188769);
#35694=VERTEX_POINT('',#188771);
#35695=VERTEX_POINT('',#188773);
#35696=VERTEX_POINT('',#188777);
#35697=VERTEX_POINT('',#188778);
#35698=VERTEX_POINT('',#188783);
#35699=VERTEX_POINT('',#188784);
#35700=VERTEX_POINT('',#188792);
#35701=VERTEX_POINT('',#188793);
#35702=VERTEX_POINT('',#188795);
#35703=VERTEX_POINT('',#188797);
#35704=VERTEX_POINT('',#188801);
#35705=VERTEX_POINT('',#188802);
#35706=VERTEX_POINT('',#188807);
#35707=VERTEX_POINT('',#188808);
#35708=VERTEX_POINT('',#188816);
#35709=VERTEX_POINT('',#188817);
#35710=VERTEX_POINT('',#188819);
#35711=VERTEX_POINT('',#188821);
#35712=VERTEX_POINT('',#188825);
#35713=VERTEX_POINT('',#188826);
#35714=VERTEX_POINT('',#188831);
#35715=VERTEX_POINT('',#188832);
#35716=VERTEX_POINT('',#188840);
#35717=VERTEX_POINT('',#188841);
#35718=VERTEX_POINT('',#188843);
#35719=VERTEX_POINT('',#188845);
#35720=VERTEX_POINT('',#188849);
#35721=VERTEX_POINT('',#188850);
#35722=VERTEX_POINT('',#188855);
#35723=VERTEX_POINT('',#188856);
#35724=VERTEX_POINT('',#188864);
#35725=VERTEX_POINT('',#188865);
#35726=VERTEX_POINT('',#188867);
#35727=VERTEX_POINT('',#188869);
#35728=VERTEX_POINT('',#188873);
#35729=VERTEX_POINT('',#188874);
#35730=VERTEX_POINT('',#188879);
#35731=VERTEX_POINT('',#188880);
#35732=VERTEX_POINT('',#188888);
#35733=VERTEX_POINT('',#188889);
#35734=VERTEX_POINT('',#188891);
#35735=VERTEX_POINT('',#188893);
#35736=VERTEX_POINT('',#188897);
#35737=VERTEX_POINT('',#188898);
#35738=VERTEX_POINT('',#188903);
#35739=VERTEX_POINT('',#188904);
#35740=VERTEX_POINT('',#188912);
#35741=VERTEX_POINT('',#188913);
#35742=VERTEX_POINT('',#188915);
#35743=VERTEX_POINT('',#188917);
#35744=VERTEX_POINT('',#188921);
#35745=VERTEX_POINT('',#188922);
#35746=VERTEX_POINT('',#188927);
#35747=VERTEX_POINT('',#188928);
#35748=VERTEX_POINT('',#188936);
#35749=VERTEX_POINT('',#188937);
#35750=VERTEX_POINT('',#188939);
#35751=VERTEX_POINT('',#188941);
#35752=VERTEX_POINT('',#188945);
#35753=VERTEX_POINT('',#188946);
#35754=VERTEX_POINT('',#188951);
#35755=VERTEX_POINT('',#188952);
#35756=VERTEX_POINT('',#188960);
#35757=VERTEX_POINT('',#188961);
#35758=VERTEX_POINT('',#188963);
#35759=VERTEX_POINT('',#188965);
#35760=VERTEX_POINT('',#188969);
#35761=VERTEX_POINT('',#188970);
#35762=VERTEX_POINT('',#188975);
#35763=VERTEX_POINT('',#188976);
#35764=VERTEX_POINT('',#188984);
#35765=VERTEX_POINT('',#188985);
#35766=VERTEX_POINT('',#188987);
#35767=VERTEX_POINT('',#188989);
#35768=VERTEX_POINT('',#188993);
#35769=VERTEX_POINT('',#188994);
#35770=VERTEX_POINT('',#188999);
#35771=VERTEX_POINT('',#189000);
#35772=VERTEX_POINT('',#189008);
#35773=VERTEX_POINT('',#189009);
#35774=VERTEX_POINT('',#189011);
#35775=VERTEX_POINT('',#189013);
#35776=VERTEX_POINT('',#189017);
#35777=VERTEX_POINT('',#189018);
#35778=VERTEX_POINT('',#189023);
#35779=VERTEX_POINT('',#189024);
#35780=VERTEX_POINT('',#189032);
#35781=VERTEX_POINT('',#189033);
#35782=VERTEX_POINT('',#189035);
#35783=VERTEX_POINT('',#189037);
#35784=VERTEX_POINT('',#189041);
#35785=VERTEX_POINT('',#189042);
#35786=VERTEX_POINT('',#189047);
#35787=VERTEX_POINT('',#189048);
#35788=VERTEX_POINT('',#189056);
#35789=VERTEX_POINT('',#189057);
#35790=VERTEX_POINT('',#189059);
#35791=VERTEX_POINT('',#189061);
#35792=VERTEX_POINT('',#189065);
#35793=VERTEX_POINT('',#189066);
#35794=VERTEX_POINT('',#189071);
#35795=VERTEX_POINT('',#189072);
#35796=VERTEX_POINT('',#189080);
#35797=VERTEX_POINT('',#189081);
#35798=VERTEX_POINT('',#189083);
#35799=VERTEX_POINT('',#189085);
#35800=VERTEX_POINT('',#189089);
#35801=VERTEX_POINT('',#189090);
#35802=VERTEX_POINT('',#189095);
#35803=VERTEX_POINT('',#189096);
#35804=VERTEX_POINT('',#189104);
#35805=VERTEX_POINT('',#189105);
#35806=VERTEX_POINT('',#189107);
#35807=VERTEX_POINT('',#189109);
#35808=VERTEX_POINT('',#189113);
#35809=VERTEX_POINT('',#189114);
#35810=VERTEX_POINT('',#189119);
#35811=VERTEX_POINT('',#189120);
#35812=VERTEX_POINT('',#189128);
#35813=VERTEX_POINT('',#189129);
#35814=VERTEX_POINT('',#189131);
#35815=VERTEX_POINT('',#189133);
#35816=VERTEX_POINT('',#189137);
#35817=VERTEX_POINT('',#189138);
#35818=VERTEX_POINT('',#189143);
#35819=VERTEX_POINT('',#189144);
#35820=VERTEX_POINT('',#189152);
#35821=VERTEX_POINT('',#189153);
#35822=VERTEX_POINT('',#189155);
#35823=VERTEX_POINT('',#189157);
#35824=VERTEX_POINT('',#189161);
#35825=VERTEX_POINT('',#189162);
#35826=VERTEX_POINT('',#189167);
#35827=VERTEX_POINT('',#189168);
#35828=VERTEX_POINT('',#189176);
#35829=VERTEX_POINT('',#189177);
#35830=VERTEX_POINT('',#189179);
#35831=VERTEX_POINT('',#189181);
#35832=VERTEX_POINT('',#189185);
#35833=VERTEX_POINT('',#189186);
#35834=VERTEX_POINT('',#189191);
#35835=VERTEX_POINT('',#189192);
#35836=VERTEX_POINT('',#189200);
#35837=VERTEX_POINT('',#189201);
#35838=VERTEX_POINT('',#189203);
#35839=VERTEX_POINT('',#189205);
#35840=VERTEX_POINT('',#189209);
#35841=VERTEX_POINT('',#189210);
#35842=VERTEX_POINT('',#189215);
#35843=VERTEX_POINT('',#189216);
#35844=VERTEX_POINT('',#189224);
#35845=VERTEX_POINT('',#189225);
#35846=VERTEX_POINT('',#189227);
#35847=VERTEX_POINT('',#189229);
#35848=VERTEX_POINT('',#189233);
#35849=VERTEX_POINT('',#189234);
#35850=VERTEX_POINT('',#189239);
#35851=VERTEX_POINT('',#189240);
#35852=VERTEX_POINT('',#189248);
#35853=VERTEX_POINT('',#189249);
#35854=VERTEX_POINT('',#189251);
#35855=VERTEX_POINT('',#189253);
#35856=VERTEX_POINT('',#189257);
#35857=VERTEX_POINT('',#189258);
#35858=VERTEX_POINT('',#189263);
#35859=VERTEX_POINT('',#189264);
#35860=VERTEX_POINT('',#189272);
#35861=VERTEX_POINT('',#189273);
#35862=VERTEX_POINT('',#189275);
#35863=VERTEX_POINT('',#189277);
#35864=VERTEX_POINT('',#189281);
#35865=VERTEX_POINT('',#189282);
#35866=VERTEX_POINT('',#189287);
#35867=VERTEX_POINT('',#189288);
#35868=VERTEX_POINT('',#189296);
#35869=VERTEX_POINT('',#189297);
#35870=VERTEX_POINT('',#189299);
#35871=VERTEX_POINT('',#189301);
#35872=VERTEX_POINT('',#189305);
#35873=VERTEX_POINT('',#189306);
#35874=VERTEX_POINT('',#189311);
#35875=VERTEX_POINT('',#189312);
#35876=VERTEX_POINT('',#189320);
#35877=VERTEX_POINT('',#189321);
#35878=VERTEX_POINT('',#189323);
#35879=VERTEX_POINT('',#189325);
#35880=VERTEX_POINT('',#189329);
#35881=VERTEX_POINT('',#189330);
#35882=VERTEX_POINT('',#189335);
#35883=VERTEX_POINT('',#189336);
#35884=VERTEX_POINT('',#189344);
#35885=VERTEX_POINT('',#189345);
#35886=VERTEX_POINT('',#189347);
#35887=VERTEX_POINT('',#189349);
#35888=VERTEX_POINT('',#189353);
#35889=VERTEX_POINT('',#189354);
#35890=VERTEX_POINT('',#189359);
#35891=VERTEX_POINT('',#189360);
#35892=VERTEX_POINT('',#189368);
#35893=VERTEX_POINT('',#189369);
#35894=VERTEX_POINT('',#189371);
#35895=VERTEX_POINT('',#189373);
#35896=VERTEX_POINT('',#189377);
#35897=VERTEX_POINT('',#189378);
#35898=VERTEX_POINT('',#189383);
#35899=VERTEX_POINT('',#189384);
#35900=VERTEX_POINT('',#189392);
#35901=VERTEX_POINT('',#189393);
#35902=VERTEX_POINT('',#189395);
#35903=VERTEX_POINT('',#189397);
#35904=VERTEX_POINT('',#189401);
#35905=VERTEX_POINT('',#189402);
#35906=VERTEX_POINT('',#189407);
#35907=VERTEX_POINT('',#189408);
#35908=VERTEX_POINT('',#189416);
#35909=VERTEX_POINT('',#189417);
#35910=VERTEX_POINT('',#189419);
#35911=VERTEX_POINT('',#189421);
#35912=VERTEX_POINT('',#189425);
#35913=VERTEX_POINT('',#189426);
#35914=VERTEX_POINT('',#189431);
#35915=VERTEX_POINT('',#189432);
#35916=VERTEX_POINT('',#189440);
#35917=VERTEX_POINT('',#189441);
#35918=VERTEX_POINT('',#189443);
#35919=VERTEX_POINT('',#189445);
#35920=VERTEX_POINT('',#189449);
#35921=VERTEX_POINT('',#189450);
#35922=VERTEX_POINT('',#189455);
#35923=VERTEX_POINT('',#189456);
#35924=VERTEX_POINT('',#189464);
#35925=VERTEX_POINT('',#189465);
#35926=VERTEX_POINT('',#189467);
#35927=VERTEX_POINT('',#189469);
#35928=VERTEX_POINT('',#189473);
#35929=VERTEX_POINT('',#189474);
#35930=VERTEX_POINT('',#189479);
#35931=VERTEX_POINT('',#189480);
#35932=VERTEX_POINT('',#189488);
#35933=VERTEX_POINT('',#189489);
#35934=VERTEX_POINT('',#189491);
#35935=VERTEX_POINT('',#189493);
#35936=VERTEX_POINT('',#189497);
#35937=VERTEX_POINT('',#189498);
#35938=VERTEX_POINT('',#189503);
#35939=VERTEX_POINT('',#189504);
#35940=VERTEX_POINT('',#189512);
#35941=VERTEX_POINT('',#189513);
#35942=VERTEX_POINT('',#189515);
#35943=VERTEX_POINT('',#189517);
#35944=VERTEX_POINT('',#189521);
#35945=VERTEX_POINT('',#189522);
#35946=VERTEX_POINT('',#189527);
#35947=VERTEX_POINT('',#189528);
#35948=VERTEX_POINT('',#189536);
#35949=VERTEX_POINT('',#189537);
#35950=VERTEX_POINT('',#189539);
#35951=VERTEX_POINT('',#189541);
#35952=VERTEX_POINT('',#189545);
#35953=VERTEX_POINT('',#189546);
#35954=VERTEX_POINT('',#189551);
#35955=VERTEX_POINT('',#189552);
#35956=VERTEX_POINT('',#189560);
#35957=VERTEX_POINT('',#189561);
#35958=VERTEX_POINT('',#189563);
#35959=VERTEX_POINT('',#189565);
#35960=VERTEX_POINT('',#189569);
#35961=VERTEX_POINT('',#189570);
#35962=VERTEX_POINT('',#189575);
#35963=VERTEX_POINT('',#189576);
#35964=VERTEX_POINT('',#189584);
#35965=VERTEX_POINT('',#189585);
#35966=VERTEX_POINT('',#189587);
#35967=VERTEX_POINT('',#189589);
#35968=VERTEX_POINT('',#189593);
#35969=VERTEX_POINT('',#189594);
#35970=VERTEX_POINT('',#189599);
#35971=VERTEX_POINT('',#189600);
#35972=VERTEX_POINT('',#189608);
#35973=VERTEX_POINT('',#189609);
#35974=VERTEX_POINT('',#189611);
#35975=VERTEX_POINT('',#189613);
#35976=VERTEX_POINT('',#189617);
#35977=VERTEX_POINT('',#189618);
#35978=VERTEX_POINT('',#189623);
#35979=VERTEX_POINT('',#189624);
#35980=VERTEX_POINT('',#189632);
#35981=VERTEX_POINT('',#189633);
#35982=VERTEX_POINT('',#189635);
#35983=VERTEX_POINT('',#189637);
#35984=VERTEX_POINT('',#189641);
#35985=VERTEX_POINT('',#189642);
#35986=VERTEX_POINT('',#189647);
#35987=VERTEX_POINT('',#189648);
#35988=VERTEX_POINT('',#189656);
#35989=VERTEX_POINT('',#189657);
#35990=VERTEX_POINT('',#189659);
#35991=VERTEX_POINT('',#189661);
#35992=VERTEX_POINT('',#189665);
#35993=VERTEX_POINT('',#189666);
#35994=VERTEX_POINT('',#189671);
#35995=VERTEX_POINT('',#189672);
#35996=VERTEX_POINT('',#189680);
#35997=VERTEX_POINT('',#189681);
#35998=VERTEX_POINT('',#189683);
#35999=VERTEX_POINT('',#189685);
#36000=VERTEX_POINT('',#189689);
#36001=VERTEX_POINT('',#189690);
#36002=VERTEX_POINT('',#189695);
#36003=VERTEX_POINT('',#189696);
#36004=VERTEX_POINT('',#189704);
#36005=VERTEX_POINT('',#189705);
#36006=VERTEX_POINT('',#189707);
#36007=VERTEX_POINT('',#189709);
#36008=VERTEX_POINT('',#189713);
#36009=VERTEX_POINT('',#189714);
#36010=VERTEX_POINT('',#189719);
#36011=VERTEX_POINT('',#189720);
#36012=VERTEX_POINT('',#189728);
#36013=VERTEX_POINT('',#189729);
#36014=VERTEX_POINT('',#189731);
#36015=VERTEX_POINT('',#189733);
#36016=VERTEX_POINT('',#189737);
#36017=VERTEX_POINT('',#189738);
#36018=VERTEX_POINT('',#189743);
#36019=VERTEX_POINT('',#189744);
#36020=VERTEX_POINT('',#189752);
#36021=VERTEX_POINT('',#189753);
#36022=VERTEX_POINT('',#189755);
#36023=VERTEX_POINT('',#189757);
#36024=VERTEX_POINT('',#189761);
#36025=VERTEX_POINT('',#189762);
#36026=VERTEX_POINT('',#189767);
#36027=VERTEX_POINT('',#189768);
#36028=VERTEX_POINT('',#189776);
#36029=VERTEX_POINT('',#189777);
#36030=VERTEX_POINT('',#189779);
#36031=VERTEX_POINT('',#189781);
#36032=VERTEX_POINT('',#189785);
#36033=VERTEX_POINT('',#189786);
#36034=VERTEX_POINT('',#189791);
#36035=VERTEX_POINT('',#189792);
#36036=VERTEX_POINT('',#189800);
#36037=VERTEX_POINT('',#189801);
#36038=VERTEX_POINT('',#189803);
#36039=VERTEX_POINT('',#189805);
#36040=VERTEX_POINT('',#189809);
#36041=VERTEX_POINT('',#189810);
#36042=VERTEX_POINT('',#189815);
#36043=VERTEX_POINT('',#189816);
#36044=VERTEX_POINT('',#189824);
#36045=VERTEX_POINT('',#189825);
#36046=VERTEX_POINT('',#189827);
#36047=VERTEX_POINT('',#189829);
#36048=VERTEX_POINT('',#189833);
#36049=VERTEX_POINT('',#189834);
#36050=VERTEX_POINT('',#189839);
#36051=VERTEX_POINT('',#189840);
#36052=VERTEX_POINT('',#189848);
#36053=VERTEX_POINT('',#189849);
#36054=VERTEX_POINT('',#189851);
#36055=VERTEX_POINT('',#189853);
#36056=VERTEX_POINT('',#189857);
#36057=VERTEX_POINT('',#189858);
#36058=VERTEX_POINT('',#189863);
#36059=VERTEX_POINT('',#189864);
#36060=VERTEX_POINT('',#189872);
#36061=VERTEX_POINT('',#189873);
#36062=VERTEX_POINT('',#189875);
#36063=VERTEX_POINT('',#189877);
#36064=VERTEX_POINT('',#189881);
#36065=VERTEX_POINT('',#189882);
#36066=VERTEX_POINT('',#189887);
#36067=VERTEX_POINT('',#189888);
#36068=VERTEX_POINT('',#189896);
#36069=VERTEX_POINT('',#189897);
#36070=VERTEX_POINT('',#189899);
#36071=VERTEX_POINT('',#189901);
#36072=VERTEX_POINT('',#189905);
#36073=VERTEX_POINT('',#189906);
#36074=VERTEX_POINT('',#189911);
#36075=VERTEX_POINT('',#189912);
#36076=VERTEX_POINT('',#189920);
#36077=VERTEX_POINT('',#189921);
#36078=VERTEX_POINT('',#189923);
#36079=VERTEX_POINT('',#189925);
#36080=VERTEX_POINT('',#189929);
#36081=VERTEX_POINT('',#189930);
#36082=VERTEX_POINT('',#189935);
#36083=VERTEX_POINT('',#189936);
#36084=VERTEX_POINT('',#189944);
#36085=VERTEX_POINT('',#189945);
#36086=VERTEX_POINT('',#189947);
#36087=VERTEX_POINT('',#189949);
#36088=VERTEX_POINT('',#189953);
#36089=VERTEX_POINT('',#189954);
#36090=VERTEX_POINT('',#189959);
#36091=VERTEX_POINT('',#189960);
#36092=VERTEX_POINT('',#189968);
#36093=VERTEX_POINT('',#189969);
#36094=VERTEX_POINT('',#189971);
#36095=VERTEX_POINT('',#189973);
#36096=VERTEX_POINT('',#189977);
#36097=VERTEX_POINT('',#189978);
#36098=VERTEX_POINT('',#189983);
#36099=VERTEX_POINT('',#189984);
#36100=VERTEX_POINT('',#189992);
#36101=VERTEX_POINT('',#189993);
#36102=VERTEX_POINT('',#189995);
#36103=VERTEX_POINT('',#189997);
#36104=VERTEX_POINT('',#190001);
#36105=VERTEX_POINT('',#190002);
#36106=VERTEX_POINT('',#190007);
#36107=VERTEX_POINT('',#190008);
#36108=VERTEX_POINT('',#190016);
#36109=VERTEX_POINT('',#190017);
#36110=VERTEX_POINT('',#190019);
#36111=VERTEX_POINT('',#190021);
#36112=VERTEX_POINT('',#190025);
#36113=VERTEX_POINT('',#190026);
#36114=VERTEX_POINT('',#190031);
#36115=VERTEX_POINT('',#190032);
#36116=VERTEX_POINT('',#190040);
#36117=VERTEX_POINT('',#190041);
#36118=VERTEX_POINT('',#190043);
#36119=VERTEX_POINT('',#190045);
#36120=VERTEX_POINT('',#190049);
#36121=VERTEX_POINT('',#190050);
#36122=VERTEX_POINT('',#190055);
#36123=VERTEX_POINT('',#190056);
#36124=VERTEX_POINT('',#190064);
#36125=VERTEX_POINT('',#190065);
#36126=VERTEX_POINT('',#190067);
#36127=VERTEX_POINT('',#190069);
#36128=VERTEX_POINT('',#190073);
#36129=VERTEX_POINT('',#190074);
#36130=VERTEX_POINT('',#190079);
#36131=VERTEX_POINT('',#190080);
#36132=VERTEX_POINT('',#190088);
#36133=VERTEX_POINT('',#190089);
#36134=VERTEX_POINT('',#190091);
#36135=VERTEX_POINT('',#190093);
#36136=VERTEX_POINT('',#190097);
#36137=VERTEX_POINT('',#190098);
#36138=VERTEX_POINT('',#190103);
#36139=VERTEX_POINT('',#190104);
#36140=VERTEX_POINT('',#190112);
#36141=VERTEX_POINT('',#190113);
#36142=VERTEX_POINT('',#190115);
#36143=VERTEX_POINT('',#190117);
#36144=VERTEX_POINT('',#190121);
#36145=VERTEX_POINT('',#190122);
#36146=VERTEX_POINT('',#190127);
#36147=VERTEX_POINT('',#190128);
#36148=VERTEX_POINT('',#190136);
#36149=VERTEX_POINT('',#190137);
#36150=VERTEX_POINT('',#190139);
#36151=VERTEX_POINT('',#190141);
#36152=VERTEX_POINT('',#190145);
#36153=VERTEX_POINT('',#190146);
#36154=VERTEX_POINT('',#190151);
#36155=VERTEX_POINT('',#190152);
#36156=VERTEX_POINT('',#190160);
#36157=VERTEX_POINT('',#190161);
#36158=VERTEX_POINT('',#190163);
#36159=VERTEX_POINT('',#190165);
#36160=VERTEX_POINT('',#190169);
#36161=VERTEX_POINT('',#190170);
#36162=VERTEX_POINT('',#190175);
#36163=VERTEX_POINT('',#190176);
#36164=VERTEX_POINT('',#190184);
#36165=VERTEX_POINT('',#190185);
#36166=VERTEX_POINT('',#190187);
#36167=VERTEX_POINT('',#190189);
#36168=VERTEX_POINT('',#190193);
#36169=VERTEX_POINT('',#190194);
#36170=VERTEX_POINT('',#190199);
#36171=VERTEX_POINT('',#190200);
#36172=VERTEX_POINT('',#190208);
#36173=VERTEX_POINT('',#190209);
#36174=VERTEX_POINT('',#190211);
#36175=VERTEX_POINT('',#190213);
#36176=VERTEX_POINT('',#190217);
#36177=VERTEX_POINT('',#190218);
#36178=VERTEX_POINT('',#190223);
#36179=VERTEX_POINT('',#190224);
#36180=VERTEX_POINT('',#190232);
#36181=VERTEX_POINT('',#190233);
#36182=VERTEX_POINT('',#190235);
#36183=VERTEX_POINT('',#190237);
#36184=VERTEX_POINT('',#190241);
#36185=VERTEX_POINT('',#190242);
#36186=VERTEX_POINT('',#190244);
#36187=VERTEX_POINT('',#190249);
#36188=VERTEX_POINT('',#190250);
#36189=VERTEX_POINT('',#190260);
#36190=VERTEX_POINT('',#190261);
#36191=VERTEX_POINT('',#190263);
#36192=VERTEX_POINT('',#190265);
#36193=VERTEX_POINT('',#190269);
#36194=VERTEX_POINT('',#190270);
#36195=VERTEX_POINT('',#190272);
#36196=VERTEX_POINT('',#190277);
#36197=VERTEX_POINT('',#190278);
#36198=VERTEX_POINT('',#190283);
#36199=VERTEX_POINT('',#190290);
#36200=VERTEX_POINT('',#190291);
#36201=VERTEX_POINT('',#190293);
#36202=VERTEX_POINT('',#190295);
#36203=VERTEX_POINT('',#190299);
#36204=VERTEX_POINT('',#190300);
#36205=VERTEX_POINT('',#190302);
#36206=VERTEX_POINT('',#190307);
#36207=VERTEX_POINT('',#190308);
#36208=VERTEX_POINT('',#190313);
#36209=VERTEX_POINT('',#190320);
#36210=VERTEX_POINT('',#190321);
#36211=VERTEX_POINT('',#190323);
#36212=VERTEX_POINT('',#190325);
#36213=VERTEX_POINT('',#190329);
#36214=VERTEX_POINT('',#190330);
#36215=VERTEX_POINT('',#190332);
#36216=VERTEX_POINT('',#190337);
#36217=VERTEX_POINT('',#190338);
#36218=VERTEX_POINT('',#190343);
#36219=VERTEX_POINT('',#190350);
#36220=VERTEX_POINT('',#190351);
#36221=VERTEX_POINT('',#190353);
#36222=VERTEX_POINT('',#190355);
#36223=VERTEX_POINT('',#190359);
#36224=VERTEX_POINT('',#190360);
#36225=VERTEX_POINT('',#190362);
#36226=VERTEX_POINT('',#190367);
#36227=VERTEX_POINT('',#190368);
#36228=VERTEX_POINT('',#190373);
#36229=VERTEX_POINT('',#190380);
#36230=VERTEX_POINT('',#190381);
#36231=VERTEX_POINT('',#190383);
#36232=VERTEX_POINT('',#190385);
#36233=VERTEX_POINT('',#190387);
#36234=VERTEX_POINT('',#190391);
#36235=VERTEX_POINT('',#190392);
#36236=VERTEX_POINT('',#190397);
#36237=VERTEX_POINT('',#190398);
#36238=VERTEX_POINT('',#190403);
#36239=VERTEX_POINT('',#190410);
#36240=VERTEX_POINT('',#190411);
#36241=VERTEX_POINT('',#190413);
#36242=VERTEX_POINT('',#190415);
#36243=VERTEX_POINT('',#190417);
#36244=VERTEX_POINT('',#190421);
#36245=VERTEX_POINT('',#190422);
#36246=VERTEX_POINT('',#190427);
#36247=VERTEX_POINT('',#190428);
#36248=VERTEX_POINT('',#190433);
#36249=VERTEX_POINT('',#190440);
#36250=VERTEX_POINT('',#190441);
#36251=VERTEX_POINT('',#190443);
#36252=VERTEX_POINT('',#190445);
#36253=VERTEX_POINT('',#190449);
#36254=VERTEX_POINT('',#190450);
#36255=VERTEX_POINT('',#190452);
#36256=VERTEX_POINT('',#190457);
#36257=VERTEX_POINT('',#190458);
#36258=VERTEX_POINT('',#190463);
#36259=VERTEX_POINT('',#190470);
#36260=VERTEX_POINT('',#190471);
#36261=VERTEX_POINT('',#190473);
#36262=VERTEX_POINT('',#190475);
#36263=VERTEX_POINT('',#190479);
#36264=VERTEX_POINT('',#190480);
#36265=VERTEX_POINT('',#190482);
#36266=VERTEX_POINT('',#190487);
#36267=VERTEX_POINT('',#190488);
#36268=VERTEX_POINT('',#190493);
#36269=VERTEX_POINT('',#190500);
#36270=VERTEX_POINT('',#190501);
#36271=VERTEX_POINT('',#190503);
#36272=VERTEX_POINT('',#190505);
#36273=VERTEX_POINT('',#190509);
#36274=VERTEX_POINT('',#190510);
#36275=VERTEX_POINT('',#190512);
#36276=VERTEX_POINT('',#190517);
#36277=VERTEX_POINT('',#190518);
#36278=VERTEX_POINT('',#190523);
#36279=VERTEX_POINT('',#190530);
#36280=VERTEX_POINT('',#190531);
#36281=VERTEX_POINT('',#190533);
#36282=VERTEX_POINT('',#190535);
#36283=VERTEX_POINT('',#190539);
#36284=VERTEX_POINT('',#190540);
#36285=VERTEX_POINT('',#190545);
#36286=VERTEX_POINT('',#190546);
#36287=VERTEX_POINT('',#190554);
#36288=VERTEX_POINT('',#190555);
#36289=VERTEX_POINT('',#190557);
#36290=VERTEX_POINT('',#190559);
#36291=VERTEX_POINT('',#190563);
#36292=VERTEX_POINT('',#190564);
#36293=VERTEX_POINT('',#190569);
#36294=VERTEX_POINT('',#190570);
#36295=VERTEX_POINT('',#190578);
#36296=VERTEX_POINT('',#190579);
#36297=VERTEX_POINT('',#190581);
#36298=VERTEX_POINT('',#190583);
#36299=VERTEX_POINT('',#190587);
#36300=VERTEX_POINT('',#190588);
#36301=VERTEX_POINT('',#190593);
#36302=VERTEX_POINT('',#190594);
#36303=VERTEX_POINT('',#190602);
#36304=VERTEX_POINT('',#190603);
#36305=VERTEX_POINT('',#190605);
#36306=VERTEX_POINT('',#190607);
#36307=VERTEX_POINT('',#190611);
#36308=VERTEX_POINT('',#190612);
#36309=VERTEX_POINT('',#190617);
#36310=VERTEX_POINT('',#190618);
#36311=VERTEX_POINT('',#190626);
#36312=VERTEX_POINT('',#190627);
#36313=VERTEX_POINT('',#190629);
#36314=VERTEX_POINT('',#190631);
#36315=VERTEX_POINT('',#190635);
#36316=VERTEX_POINT('',#190636);
#36317=VERTEX_POINT('',#190641);
#36318=VERTEX_POINT('',#190642);
#36319=VERTEX_POINT('',#190650);
#36320=VERTEX_POINT('',#190651);
#36321=VERTEX_POINT('',#190653);
#36322=VERTEX_POINT('',#190655);
#36323=VERTEX_POINT('',#190659);
#36324=VERTEX_POINT('',#190660);
#36325=VERTEX_POINT('',#190665);
#36326=VERTEX_POINT('',#190666);
#36327=VERTEX_POINT('',#190674);
#36328=VERTEX_POINT('',#190675);
#36329=VERTEX_POINT('',#190677);
#36330=VERTEX_POINT('',#190679);
#36331=VERTEX_POINT('',#190683);
#36332=VERTEX_POINT('',#190684);
#36333=VERTEX_POINT('',#190689);
#36334=VERTEX_POINT('',#190690);
#36335=VERTEX_POINT('',#190698);
#36336=VERTEX_POINT('',#190699);
#36337=VERTEX_POINT('',#190701);
#36338=VERTEX_POINT('',#190703);
#36339=VERTEX_POINT('',#190707);
#36340=VERTEX_POINT('',#190708);
#36341=VERTEX_POINT('',#190713);
#36342=VERTEX_POINT('',#190714);
#36343=VERTEX_POINT('',#190722);
#36344=VERTEX_POINT('',#190723);
#36345=VERTEX_POINT('',#190725);
#36346=VERTEX_POINT('',#190727);
#36347=VERTEX_POINT('',#190729);
#36348=VERTEX_POINT('',#190733);
#36349=VERTEX_POINT('',#190734);
#36350=VERTEX_POINT('',#190739);
#36351=VERTEX_POINT('',#190740);
#36352=VERTEX_POINT('',#190745);
#36353=VERTEX_POINT('',#190752);
#36354=VERTEX_POINT('',#190753);
#36355=VERTEX_POINT('',#190755);
#36356=VERTEX_POINT('',#190757);
#36357=VERTEX_POINT('',#190759);
#36358=VERTEX_POINT('',#190763);
#36359=VERTEX_POINT('',#190764);
#36360=VERTEX_POINT('',#190769);
#36361=VERTEX_POINT('',#190770);
#36362=VERTEX_POINT('',#190775);
#36363=VERTEX_POINT('',#190782);
#36364=VERTEX_POINT('',#190783);
#36365=VERTEX_POINT('',#190785);
#36366=VERTEX_POINT('',#190787);
#36367=VERTEX_POINT('',#190791);
#36368=VERTEX_POINT('',#190792);
#36369=VERTEX_POINT('',#190797);
#36370=VERTEX_POINT('',#190798);
#36371=VERTEX_POINT('',#190806);
#36372=VERTEX_POINT('',#190807);
#36373=VERTEX_POINT('',#190809);
#36374=VERTEX_POINT('',#190811);
#36375=VERTEX_POINT('',#190815);
#36376=VERTEX_POINT('',#190816);
#36377=VERTEX_POINT('',#190821);
#36378=VERTEX_POINT('',#190822);
#36379=VERTEX_POINT('',#190830);
#36380=VERTEX_POINT('',#190831);
#36381=VERTEX_POINT('',#190833);
#36382=VERTEX_POINT('',#190835);
#36383=VERTEX_POINT('',#190839);
#36384=VERTEX_POINT('',#190840);
#36385=VERTEX_POINT('',#190845);
#36386=VERTEX_POINT('',#190846);
#36387=VERTEX_POINT('',#190854);
#36388=VERTEX_POINT('',#190855);
#36389=VERTEX_POINT('',#190857);
#36390=VERTEX_POINT('',#190859);
#36391=VERTEX_POINT('',#190863);
#36392=VERTEX_POINT('',#190864);
#36393=VERTEX_POINT('',#190869);
#36394=VERTEX_POINT('',#190870);
#36395=VERTEX_POINT('',#190878);
#36396=VERTEX_POINT('',#190879);
#36397=VERTEX_POINT('',#190881);
#36398=VERTEX_POINT('',#190883);
#36399=VERTEX_POINT('',#190887);
#36400=VERTEX_POINT('',#190888);
#36401=VERTEX_POINT('',#190893);
#36402=VERTEX_POINT('',#190894);
#36403=VERTEX_POINT('',#190896);
#36404=VERTEX_POINT('',#190901);
#36405=VERTEX_POINT('',#190908);
#36406=VERTEX_POINT('',#190909);
#36407=VERTEX_POINT('',#190911);
#36408=VERTEX_POINT('',#190913);
#36409=VERTEX_POINT('',#190917);
#36410=VERTEX_POINT('',#190918);
#36411=VERTEX_POINT('',#190920);
#36412=VERTEX_POINT('',#190925);
#36413=VERTEX_POINT('',#190926);
#36414=VERTEX_POINT('',#190931);
#36415=VERTEX_POINT('',#190938);
#36416=VERTEX_POINT('',#190939);
#36417=VERTEX_POINT('',#190941);
#36418=VERTEX_POINT('',#190943);
#36419=VERTEX_POINT('',#190947);
#36420=VERTEX_POINT('',#190948);
#36421=VERTEX_POINT('',#190950);
#36422=VERTEX_POINT('',#190955);
#36423=VERTEX_POINT('',#190956);
#36424=VERTEX_POINT('',#190961);
#36425=VERTEX_POINT('',#190968);
#36426=VERTEX_POINT('',#190969);
#36427=VERTEX_POINT('',#190971);
#36428=VERTEX_POINT('',#190973);
#36429=VERTEX_POINT('',#190977);
#36430=VERTEX_POINT('',#190978);
#36431=VERTEX_POINT('',#190983);
#36432=VERTEX_POINT('',#190984);
#36433=VERTEX_POINT('',#190986);
#36434=VERTEX_POINT('',#190991);
#36435=VERTEX_POINT('',#190998);
#36436=VERTEX_POINT('',#190999);
#36437=VERTEX_POINT('',#191001);
#36438=VERTEX_POINT('',#191003);
#36439=VERTEX_POINT('',#191007);
#36440=VERTEX_POINT('',#191008);
#36441=VERTEX_POINT('',#191013);
#36442=VERTEX_POINT('',#191014);
#36443=VERTEX_POINT('',#191022);
#36444=VERTEX_POINT('',#191023);
#36445=VERTEX_POINT('',#191025);
#36446=VERTEX_POINT('',#191027);
#36447=VERTEX_POINT('',#191031);
#36448=VERTEX_POINT('',#191032);
#36449=VERTEX_POINT('',#191037);
#36450=VERTEX_POINT('',#191038);
#36451=VERTEX_POINT('',#191046);
#36452=VERTEX_POINT('',#191047);
#36453=VERTEX_POINT('',#191049);
#36454=VERTEX_POINT('',#191051);
#36455=VERTEX_POINT('',#191055);
#36456=VERTEX_POINT('',#191056);
#36457=VERTEX_POINT('',#191061);
#36458=VERTEX_POINT('',#191062);
#36459=VERTEX_POINT('',#191070);
#36460=VERTEX_POINT('',#191071);
#36461=VERTEX_POINT('',#191073);
#36462=VERTEX_POINT('',#191075);
#36463=VERTEX_POINT('',#191079);
#36464=VERTEX_POINT('',#191080);
#36465=VERTEX_POINT('',#191085);
#36466=VERTEX_POINT('',#191086);
#36467=VERTEX_POINT('',#191094);
#36468=VERTEX_POINT('',#191095);
#36469=VERTEX_POINT('',#191097);
#36470=VERTEX_POINT('',#191099);
#36471=VERTEX_POINT('',#191103);
#36472=VERTEX_POINT('',#191104);
#36473=VERTEX_POINT('',#191109);
#36474=VERTEX_POINT('',#191110);
#36475=VERTEX_POINT('',#191118);
#36476=VERTEX_POINT('',#191119);
#36477=VERTEX_POINT('',#191121);
#36478=VERTEX_POINT('',#191123);
#36479=VERTEX_POINT('',#191127);
#36480=VERTEX_POINT('',#191128);
#36481=VERTEX_POINT('',#191133);
#36482=VERTEX_POINT('',#191134);
#36483=VERTEX_POINT('',#191142);
#36484=VERTEX_POINT('',#191143);
#36485=VERTEX_POINT('',#191145);
#36486=VERTEX_POINT('',#191147);
#36487=VERTEX_POINT('',#191151);
#36488=VERTEX_POINT('',#191152);
#36489=VERTEX_POINT('',#191157);
#36490=VERTEX_POINT('',#191158);
#36491=VERTEX_POINT('',#191166);
#36492=VERTEX_POINT('',#191167);
#36493=VERTEX_POINT('',#191169);
#36494=VERTEX_POINT('',#191171);
#36495=VERTEX_POINT('',#191175);
#36496=VERTEX_POINT('',#191176);
#36497=VERTEX_POINT('',#191181);
#36498=VERTEX_POINT('',#191182);
#36499=VERTEX_POINT('',#191190);
#36500=VERTEX_POINT('',#191191);
#36501=VERTEX_POINT('',#191193);
#36502=VERTEX_POINT('',#191195);
#36503=VERTEX_POINT('',#191199);
#36504=VERTEX_POINT('',#191200);
#36505=VERTEX_POINT('',#191205);
#36506=VERTEX_POINT('',#191206);
#36507=VERTEX_POINT('',#191214);
#36508=VERTEX_POINT('',#191215);
#36509=VERTEX_POINT('',#191217);
#36510=VERTEX_POINT('',#191219);
#36511=VERTEX_POINT('',#191223);
#36512=VERTEX_POINT('',#191224);
#36513=VERTEX_POINT('',#191229);
#36514=VERTEX_POINT('',#191230);
#36515=VERTEX_POINT('',#191238);
#36516=VERTEX_POINT('',#191239);
#36517=VERTEX_POINT('',#191241);
#36518=VERTEX_POINT('',#191243);
#36519=VERTEX_POINT('',#191247);
#36520=VERTEX_POINT('',#191248);
#36521=VERTEX_POINT('',#191253);
#36522=VERTEX_POINT('',#191254);
#36523=VERTEX_POINT('',#191256);
#36524=VERTEX_POINT('',#191261);
#36525=VERTEX_POINT('',#191268);
#36526=VERTEX_POINT('',#191269);
#36527=VERTEX_POINT('',#191271);
#36528=VERTEX_POINT('',#191273);
#36529=VERTEX_POINT('',#191277);
#36530=VERTEX_POINT('',#191278);
#36531=VERTEX_POINT('',#191283);
#36532=VERTEX_POINT('',#191284);
#36533=VERTEX_POINT('',#191286);
#36534=VERTEX_POINT('',#191291);
#36535=VERTEX_POINT('',#191298);
#36536=VERTEX_POINT('',#191299);
#36537=VERTEX_POINT('',#191301);
#36538=VERTEX_POINT('',#191303);
#36539=VERTEX_POINT('',#191307);
#36540=VERTEX_POINT('',#191308);
#36541=VERTEX_POINT('',#191313);
#36542=VERTEX_POINT('',#191314);
#36543=VERTEX_POINT('',#191322);
#36544=VERTEX_POINT('',#191323);
#36545=VERTEX_POINT('',#191325);
#36546=VERTEX_POINT('',#191327);
#36547=VERTEX_POINT('',#191331);
#36548=VERTEX_POINT('',#191332);
#36549=VERTEX_POINT('',#191337);
#36550=VERTEX_POINT('',#191338);
#36551=VERTEX_POINT('',#191346);
#36552=VERTEX_POINT('',#191347);
#36553=VERTEX_POINT('',#191349);
#36554=VERTEX_POINT('',#191351);
#36555=VERTEX_POINT('',#191355);
#36556=VERTEX_POINT('',#191356);
#36557=VERTEX_POINT('',#191361);
#36558=VERTEX_POINT('',#191362);
#36559=VERTEX_POINT('',#191370);
#36560=VERTEX_POINT('',#191371);
#36561=VERTEX_POINT('',#191373);
#36562=VERTEX_POINT('',#191375);
#36563=VERTEX_POINT('',#191379);
#36564=VERTEX_POINT('',#191380);
#36565=VERTEX_POINT('',#191385);
#36566=VERTEX_POINT('',#191386);
#36567=VERTEX_POINT('',#191394);
#36568=VERTEX_POINT('',#191395);
#36569=VERTEX_POINT('',#191397);
#36570=VERTEX_POINT('',#191399);
#36571=VERTEX_POINT('',#191403);
#36572=VERTEX_POINT('',#191404);
#36573=VERTEX_POINT('',#191409);
#36574=VERTEX_POINT('',#191410);
#36575=VERTEX_POINT('',#191418);
#36576=VERTEX_POINT('',#191419);
#36577=VERTEX_POINT('',#191421);
#36578=VERTEX_POINT('',#191423);
#36579=VERTEX_POINT('',#191427);
#36580=VERTEX_POINT('',#191428);
#36581=VERTEX_POINT('',#191433);
#36582=VERTEX_POINT('',#191434);
#36583=VERTEX_POINT('',#191442);
#36584=VERTEX_POINT('',#191443);
#36585=VERTEX_POINT('',#191445);
#36586=VERTEX_POINT('',#191447);
#36587=VERTEX_POINT('',#191451);
#36588=VERTEX_POINT('',#191452);
#36589=VERTEX_POINT('',#191457);
#36590=VERTEX_POINT('',#191458);
#36591=VERTEX_POINT('',#191466);
#36592=VERTEX_POINT('',#191467);
#36593=VERTEX_POINT('',#191469);
#36594=VERTEX_POINT('',#191471);
#36595=VERTEX_POINT('',#191475);
#36596=VERTEX_POINT('',#191476);
#36597=VERTEX_POINT('',#191481);
#36598=VERTEX_POINT('',#191482);
#36599=VERTEX_POINT('',#191490);
#36600=VERTEX_POINT('',#191491);
#36601=VERTEX_POINT('',#191493);
#36602=VERTEX_POINT('',#191495);
#36603=VERTEX_POINT('',#191499);
#36604=VERTEX_POINT('',#191500);
#36605=VERTEX_POINT('',#191505);
#36606=VERTEX_POINT('',#191506);
#36607=VERTEX_POINT('',#191514);
#36608=VERTEX_POINT('',#191515);
#36609=VERTEX_POINT('',#191517);
#36610=VERTEX_POINT('',#191519);
#36611=VERTEX_POINT('',#191523);
#36612=VERTEX_POINT('',#191524);
#36613=VERTEX_POINT('',#191526);
#36614=VERTEX_POINT('',#191531);
#36615=VERTEX_POINT('',#191532);
#36616=VERTEX_POINT('',#191537);
#36617=VERTEX_POINT('',#191544);
#36618=VERTEX_POINT('',#191545);
#36619=VERTEX_POINT('',#191547);
#36620=VERTEX_POINT('',#191549);
#36621=VERTEX_POINT('',#191553);
#36622=VERTEX_POINT('',#191554);
#36623=VERTEX_POINT('',#191559);
#36624=VERTEX_POINT('',#191560);
#36625=VERTEX_POINT('',#191562);
#36626=VERTEX_POINT('',#191567);
#36627=VERTEX_POINT('',#191574);
#36628=VERTEX_POINT('',#191575);
#36629=VERTEX_POINT('',#191577);
#36630=VERTEX_POINT('',#191579);
#36631=VERTEX_POINT('',#191583);
#36632=VERTEX_POINT('',#191584);
#36633=VERTEX_POINT('',#191589);
#36634=VERTEX_POINT('',#191590);
#36635=VERTEX_POINT('',#191598);
#36636=VERTEX_POINT('',#191599);
#36637=VERTEX_POINT('',#191601);
#36638=VERTEX_POINT('',#191603);
#36639=VERTEX_POINT('',#191607);
#36640=VERTEX_POINT('',#191608);
#36641=VERTEX_POINT('',#191613);
#36642=VERTEX_POINT('',#191614);
#36643=VERTEX_POINT('',#191622);
#36644=VERTEX_POINT('',#191623);
#36645=VERTEX_POINT('',#191625);
#36646=VERTEX_POINT('',#191627);
#36647=VERTEX_POINT('',#191631);
#36648=VERTEX_POINT('',#191632);
#36649=VERTEX_POINT('',#191637);
#36650=VERTEX_POINT('',#191638);
#36651=VERTEX_POINT('',#191646);
#36652=VERTEX_POINT('',#191647);
#36653=VERTEX_POINT('',#191649);
#36654=VERTEX_POINT('',#191651);
#36655=VERTEX_POINT('',#191655);
#36656=VERTEX_POINT('',#191656);
#36657=VERTEX_POINT('',#191661);
#36658=VERTEX_POINT('',#191662);
#36659=VERTEX_POINT('',#191670);
#36660=VERTEX_POINT('',#191671);
#36661=VERTEX_POINT('',#191673);
#36662=VERTEX_POINT('',#191675);
#36663=VERTEX_POINT('',#191679);
#36664=VERTEX_POINT('',#191680);
#36665=VERTEX_POINT('',#191685);
#36666=VERTEX_POINT('',#191686);
#36667=VERTEX_POINT('',#191694);
#36668=VERTEX_POINT('',#191695);
#36669=VERTEX_POINT('',#191697);
#36670=VERTEX_POINT('',#191699);
#36671=VERTEX_POINT('',#191703);
#36672=VERTEX_POINT('',#191704);
#36673=VERTEX_POINT('',#191709);
#36674=VERTEX_POINT('',#191710);
#36675=VERTEX_POINT('',#191718);
#36676=VERTEX_POINT('',#191719);
#36677=VERTEX_POINT('',#191721);
#36678=VERTEX_POINT('',#191723);
#36679=VERTEX_POINT('',#191727);
#36680=VERTEX_POINT('',#191728);
#36681=VERTEX_POINT('',#191733);
#36682=VERTEX_POINT('',#191734);
#36683=VERTEX_POINT('',#191742);
#36684=VERTEX_POINT('',#191743);
#36685=VERTEX_POINT('',#191745);
#36686=VERTEX_POINT('',#191747);
#36687=VERTEX_POINT('',#191751);
#36688=VERTEX_POINT('',#191752);
#36689=VERTEX_POINT('',#191757);
#36690=VERTEX_POINT('',#191758);
#36691=VERTEX_POINT('',#191766);
#36692=VERTEX_POINT('',#191767);
#36693=VERTEX_POINT('',#191769);
#36694=VERTEX_POINT('',#191771);
#36695=VERTEX_POINT('',#191775);
#36696=VERTEX_POINT('',#191776);
#36697=VERTEX_POINT('',#191781);
#36698=VERTEX_POINT('',#191782);
#36699=VERTEX_POINT('',#191790);
#36700=VERTEX_POINT('',#191791);
#36701=VERTEX_POINT('',#191793);
#36702=VERTEX_POINT('',#191795);
#36703=VERTEX_POINT('',#191799);
#36704=VERTEX_POINT('',#191800);
#36705=VERTEX_POINT('',#191805);
#36706=VERTEX_POINT('',#191806);
#36707=VERTEX_POINT('',#191814);
#36708=VERTEX_POINT('',#191815);
#36709=VERTEX_POINT('',#191817);
#36710=VERTEX_POINT('',#191819);
#36711=VERTEX_POINT('',#191823);
#36712=VERTEX_POINT('',#191824);
#36713=VERTEX_POINT('',#191829);
#36714=VERTEX_POINT('',#191830);
#36715=VERTEX_POINT('',#191838);
#36716=VERTEX_POINT('',#191839);
#36717=VERTEX_POINT('',#191841);
#36718=VERTEX_POINT('',#191843);
#36719=VERTEX_POINT('',#191847);
#36720=VERTEX_POINT('',#191848);
#36721=VERTEX_POINT('',#191853);
#36722=VERTEX_POINT('',#191854);
#36723=VERTEX_POINT('',#191862);
#36724=VERTEX_POINT('',#191863);
#36725=VERTEX_POINT('',#191865);
#36726=VERTEX_POINT('',#191867);
#36727=VERTEX_POINT('',#191871);
#36728=VERTEX_POINT('',#191872);
#36729=VERTEX_POINT('',#191877);
#36730=VERTEX_POINT('',#191878);
#36731=VERTEX_POINT('',#191886);
#36732=VERTEX_POINT('',#191887);
#36733=VERTEX_POINT('',#191889);
#36734=VERTEX_POINT('',#191891);
#36735=VERTEX_POINT('',#191895);
#36736=VERTEX_POINT('',#191896);
#36737=VERTEX_POINT('',#191901);
#36738=VERTEX_POINT('',#191902);
#36739=VERTEX_POINT('',#191910);
#36740=VERTEX_POINT('',#191911);
#36741=VERTEX_POINT('',#191913);
#36742=VERTEX_POINT('',#191915);
#36743=VERTEX_POINT('',#191919);
#36744=VERTEX_POINT('',#191920);
#36745=VERTEX_POINT('',#191925);
#36746=VERTEX_POINT('',#191926);
#36747=VERTEX_POINT('',#191934);
#36748=VERTEX_POINT('',#191935);
#36749=VERTEX_POINT('',#191937);
#36750=VERTEX_POINT('',#191939);
#36751=VERTEX_POINT('',#191943);
#36752=VERTEX_POINT('',#191944);
#36753=VERTEX_POINT('',#191949);
#36754=VERTEX_POINT('',#191950);
#36755=VERTEX_POINT('',#191958);
#36756=VERTEX_POINT('',#191959);
#36757=VERTEX_POINT('',#191961);
#36758=VERTEX_POINT('',#191963);
#36759=VERTEX_POINT('',#191967);
#36760=VERTEX_POINT('',#191968);
#36761=VERTEX_POINT('',#191973);
#36762=VERTEX_POINT('',#191974);
#36763=VERTEX_POINT('',#191982);
#36764=VERTEX_POINT('',#191983);
#36765=VERTEX_POINT('',#191985);
#36766=VERTEX_POINT('',#191987);
#36767=VERTEX_POINT('',#191991);
#36768=VERTEX_POINT('',#191992);
#36769=VERTEX_POINT('',#191997);
#36770=VERTEX_POINT('',#191998);
#36771=VERTEX_POINT('',#192006);
#36772=VERTEX_POINT('',#192007);
#36773=VERTEX_POINT('',#192009);
#36774=VERTEX_POINT('',#192011);
#36775=VERTEX_POINT('',#192015);
#36776=VERTEX_POINT('',#192016);
#36777=VERTEX_POINT('',#192021);
#36778=VERTEX_POINT('',#192022);
#36779=VERTEX_POINT('',#192030);
#36780=VERTEX_POINT('',#192031);
#36781=VERTEX_POINT('',#192033);
#36782=VERTEX_POINT('',#192035);
#36783=VERTEX_POINT('',#192039);
#36784=VERTEX_POINT('',#192040);
#36785=VERTEX_POINT('',#192045);
#36786=VERTEX_POINT('',#192046);
#36787=VERTEX_POINT('',#192054);
#36788=VERTEX_POINT('',#192055);
#36789=VERTEX_POINT('',#192057);
#36790=VERTEX_POINT('',#192059);
#36791=VERTEX_POINT('',#192063);
#36792=VERTEX_POINT('',#192064);
#36793=VERTEX_POINT('',#192069);
#36794=VERTEX_POINT('',#192070);
#36795=VERTEX_POINT('',#192078);
#36796=VERTEX_POINT('',#192079);
#36797=VERTEX_POINT('',#192081);
#36798=VERTEX_POINT('',#192083);
#36799=VERTEX_POINT('',#192087);
#36800=VERTEX_POINT('',#192088);
#36801=VERTEX_POINT('',#192093);
#36802=VERTEX_POINT('',#192094);
#36803=VERTEX_POINT('',#192102);
#36804=VERTEX_POINT('',#192103);
#36805=VERTEX_POINT('',#192105);
#36806=VERTEX_POINT('',#192107);
#36807=VERTEX_POINT('',#192111);
#36808=VERTEX_POINT('',#192112);
#36809=VERTEX_POINT('',#192117);
#36810=VERTEX_POINT('',#192118);
#36811=VERTEX_POINT('',#192126);
#36812=VERTEX_POINT('',#192127);
#36813=VERTEX_POINT('',#192129);
#36814=VERTEX_POINT('',#192131);
#36815=VERTEX_POINT('',#192135);
#36816=VERTEX_POINT('',#192136);
#36817=VERTEX_POINT('',#192141);
#36818=VERTEX_POINT('',#192142);
#36819=VERTEX_POINT('',#192150);
#36820=VERTEX_POINT('',#192151);
#36821=VERTEX_POINT('',#192153);
#36822=VERTEX_POINT('',#192155);
#36823=VERTEX_POINT('',#192159);
#36824=VERTEX_POINT('',#192160);
#36825=VERTEX_POINT('',#192165);
#36826=VERTEX_POINT('',#192166);
#36827=VERTEX_POINT('',#192174);
#36828=VERTEX_POINT('',#192175);
#36829=VERTEX_POINT('',#192177);
#36830=VERTEX_POINT('',#192179);
#36831=VERTEX_POINT('',#192183);
#36832=VERTEX_POINT('',#192184);
#36833=VERTEX_POINT('',#192189);
#36834=VERTEX_POINT('',#192190);
#36835=VERTEX_POINT('',#192198);
#36836=VERTEX_POINT('',#192199);
#36837=VERTEX_POINT('',#192201);
#36838=VERTEX_POINT('',#192203);
#36839=VERTEX_POINT('',#192207);
#36840=VERTEX_POINT('',#192208);
#36841=VERTEX_POINT('',#192213);
#36842=VERTEX_POINT('',#192214);
#36843=VERTEX_POINT('',#192222);
#36844=VERTEX_POINT('',#192223);
#36845=VERTEX_POINT('',#192225);
#36846=VERTEX_POINT('',#192227);
#36847=VERTEX_POINT('',#192231);
#36848=VERTEX_POINT('',#192232);
#36849=VERTEX_POINT('',#192237);
#36850=VERTEX_POINT('',#192238);
#36851=VERTEX_POINT('',#192246);
#36852=VERTEX_POINT('',#192247);
#36853=VERTEX_POINT('',#192249);
#36854=VERTEX_POINT('',#192251);
#36855=VERTEX_POINT('',#192255);
#36856=VERTEX_POINT('',#192256);
#36857=VERTEX_POINT('',#192261);
#36858=VERTEX_POINT('',#192262);
#36859=VERTEX_POINT('',#192270);
#36860=VERTEX_POINT('',#192271);
#36861=VERTEX_POINT('',#192273);
#36862=VERTEX_POINT('',#192275);
#36863=VERTEX_POINT('',#192279);
#36864=VERTEX_POINT('',#192280);
#36865=VERTEX_POINT('',#192285);
#36866=VERTEX_POINT('',#192286);
#36867=VERTEX_POINT('',#192294);
#36868=VERTEX_POINT('',#192295);
#36869=VERTEX_POINT('',#192297);
#36870=VERTEX_POINT('',#192299);
#36871=VERTEX_POINT('',#192303);
#36872=VERTEX_POINT('',#192304);
#36873=VERTEX_POINT('',#192309);
#36874=VERTEX_POINT('',#192310);
#36875=VERTEX_POINT('',#192318);
#36876=VERTEX_POINT('',#192319);
#36877=VERTEX_POINT('',#192321);
#36878=VERTEX_POINT('',#192323);
#36879=VERTEX_POINT('',#192327);
#36880=VERTEX_POINT('',#192328);
#36881=VERTEX_POINT('',#192333);
#36882=VERTEX_POINT('',#192334);
#36883=VERTEX_POINT('',#192342);
#36884=VERTEX_POINT('',#192343);
#36885=VERTEX_POINT('',#192345);
#36886=VERTEX_POINT('',#192347);
#36887=VERTEX_POINT('',#192351);
#36888=VERTEX_POINT('',#192352);
#36889=VERTEX_POINT('',#192357);
#36890=VERTEX_POINT('',#192358);
#36891=VERTEX_POINT('',#192366);
#36892=VERTEX_POINT('',#192367);
#36893=VERTEX_POINT('',#192369);
#36894=VERTEX_POINT('',#192371);
#36895=VERTEX_POINT('',#192375);
#36896=VERTEX_POINT('',#192376);
#36897=VERTEX_POINT('',#192381);
#36898=VERTEX_POINT('',#192382);
#36899=VERTEX_POINT('',#192390);
#36900=VERTEX_POINT('',#192391);
#36901=VERTEX_POINT('',#192393);
#36902=VERTEX_POINT('',#192395);
#36903=VERTEX_POINT('',#192399);
#36904=VERTEX_POINT('',#192400);
#36905=VERTEX_POINT('',#192405);
#36906=VERTEX_POINT('',#192406);
#36907=VERTEX_POINT('',#192414);
#36908=VERTEX_POINT('',#192415);
#36909=VERTEX_POINT('',#192417);
#36910=VERTEX_POINT('',#192419);
#36911=VERTEX_POINT('',#192423);
#36912=VERTEX_POINT('',#192424);
#36913=VERTEX_POINT('',#192429);
#36914=VERTEX_POINT('',#192430);
#36915=VERTEX_POINT('',#192438);
#36916=VERTEX_POINT('',#192439);
#36917=VERTEX_POINT('',#192441);
#36918=VERTEX_POINT('',#192443);
#36919=VERTEX_POINT('',#192447);
#36920=VERTEX_POINT('',#192448);
#36921=VERTEX_POINT('',#192453);
#36922=VERTEX_POINT('',#192454);
#36923=VERTEX_POINT('',#192462);
#36924=VERTEX_POINT('',#192463);
#36925=VERTEX_POINT('',#192465);
#36926=VERTEX_POINT('',#192467);
#36927=VERTEX_POINT('',#192471);
#36928=VERTEX_POINT('',#192472);
#36929=VERTEX_POINT('',#192477);
#36930=VERTEX_POINT('',#192478);
#36931=VERTEX_POINT('',#192486);
#36932=VERTEX_POINT('',#192487);
#36933=VERTEX_POINT('',#192489);
#36934=VERTEX_POINT('',#192491);
#36935=VERTEX_POINT('',#192495);
#36936=VERTEX_POINT('',#192496);
#36937=VERTEX_POINT('',#192501);
#36938=VERTEX_POINT('',#192502);
#36939=VERTEX_POINT('',#192510);
#36940=VERTEX_POINT('',#192511);
#36941=VERTEX_POINT('',#192513);
#36942=VERTEX_POINT('',#192515);
#36943=VERTEX_POINT('',#192519);
#36944=VERTEX_POINT('',#192520);
#36945=VERTEX_POINT('',#192525);
#36946=VERTEX_POINT('',#192526);
#36947=VERTEX_POINT('',#192534);
#36948=VERTEX_POINT('',#192535);
#36949=VERTEX_POINT('',#192537);
#36950=VERTEX_POINT('',#192539);
#36951=VERTEX_POINT('',#192543);
#36952=VERTEX_POINT('',#192544);
#36953=VERTEX_POINT('',#192549);
#36954=VERTEX_POINT('',#192550);
#36955=VERTEX_POINT('',#192558);
#36956=VERTEX_POINT('',#192559);
#36957=VERTEX_POINT('',#192561);
#36958=VERTEX_POINT('',#192563);
#36959=VERTEX_POINT('',#192567);
#36960=VERTEX_POINT('',#192568);
#36961=VERTEX_POINT('',#192573);
#36962=VERTEX_POINT('',#192574);
#36963=VERTEX_POINT('',#192582);
#36964=VERTEX_POINT('',#192583);
#36965=VERTEX_POINT('',#192585);
#36966=VERTEX_POINT('',#192587);
#36967=VERTEX_POINT('',#192591);
#36968=VERTEX_POINT('',#192592);
#36969=VERTEX_POINT('',#192597);
#36970=VERTEX_POINT('',#192598);
#36971=VERTEX_POINT('',#192606);
#36972=VERTEX_POINT('',#192607);
#36973=VERTEX_POINT('',#192609);
#36974=VERTEX_POINT('',#192611);
#36975=VERTEX_POINT('',#192615);
#36976=VERTEX_POINT('',#192616);
#36977=VERTEX_POINT('',#192621);
#36978=VERTEX_POINT('',#192622);
#36979=VERTEX_POINT('',#192630);
#36980=VERTEX_POINT('',#192631);
#36981=VERTEX_POINT('',#192633);
#36982=VERTEX_POINT('',#192635);
#36983=VERTEX_POINT('',#192639);
#36984=VERTEX_POINT('',#192640);
#36985=VERTEX_POINT('',#192645);
#36986=VERTEX_POINT('',#192646);
#36987=VERTEX_POINT('',#192654);
#36988=VERTEX_POINT('',#192655);
#36989=VERTEX_POINT('',#192657);
#36990=VERTEX_POINT('',#192659);
#36991=VERTEX_POINT('',#192663);
#36992=VERTEX_POINT('',#192664);
#36993=VERTEX_POINT('',#192669);
#36994=VERTEX_POINT('',#192670);
#36995=VERTEX_POINT('',#192678);
#36996=VERTEX_POINT('',#192679);
#36997=VERTEX_POINT('',#192681);
#36998=VERTEX_POINT('',#192683);
#36999=VERTEX_POINT('',#192687);
#37000=VERTEX_POINT('',#192688);
#37001=VERTEX_POINT('',#192693);
#37002=VERTEX_POINT('',#192694);
#37003=VERTEX_POINT('',#192702);
#37004=VERTEX_POINT('',#192703);
#37005=VERTEX_POINT('',#192705);
#37006=VERTEX_POINT('',#192707);
#37007=VERTEX_POINT('',#192711);
#37008=VERTEX_POINT('',#192712);
#37009=VERTEX_POINT('',#192717);
#37010=VERTEX_POINT('',#192718);
#37011=VERTEX_POINT('',#192726);
#37012=VERTEX_POINT('',#192727);
#37013=VERTEX_POINT('',#192729);
#37014=VERTEX_POINT('',#192731);
#37015=VERTEX_POINT('',#192735);
#37016=VERTEX_POINT('',#192736);
#37017=VERTEX_POINT('',#192741);
#37018=VERTEX_POINT('',#192742);
#37019=VERTEX_POINT('',#192750);
#37020=VERTEX_POINT('',#192751);
#37021=VERTEX_POINT('',#192753);
#37022=VERTEX_POINT('',#192755);
#37023=VERTEX_POINT('',#192759);
#37024=VERTEX_POINT('',#192760);
#37025=VERTEX_POINT('',#192765);
#37026=VERTEX_POINT('',#192766);
#37027=VERTEX_POINT('',#192774);
#37028=VERTEX_POINT('',#192775);
#37029=VERTEX_POINT('',#192777);
#37030=VERTEX_POINT('',#192779);
#37031=VERTEX_POINT('',#192783);
#37032=VERTEX_POINT('',#192784);
#37033=VERTEX_POINT('',#192789);
#37034=VERTEX_POINT('',#192790);
#37035=VERTEX_POINT('',#192798);
#37036=VERTEX_POINT('',#192799);
#37037=VERTEX_POINT('',#192801);
#37038=VERTEX_POINT('',#192803);
#37039=VERTEX_POINT('',#192807);
#37040=VERTEX_POINT('',#192808);
#37041=VERTEX_POINT('',#192813);
#37042=VERTEX_POINT('',#192814);
#37043=VERTEX_POINT('',#192822);
#37044=VERTEX_POINT('',#192823);
#37045=VERTEX_POINT('',#192825);
#37046=VERTEX_POINT('',#192827);
#37047=VERTEX_POINT('',#192831);
#37048=VERTEX_POINT('',#192832);
#37049=VERTEX_POINT('',#192837);
#37050=VERTEX_POINT('',#192838);
#37051=VERTEX_POINT('',#192846);
#37052=VERTEX_POINT('',#192847);
#37053=VERTEX_POINT('',#192849);
#37054=VERTEX_POINT('',#192851);
#37055=VERTEX_POINT('',#192855);
#37056=VERTEX_POINT('',#192856);
#37057=VERTEX_POINT('',#192861);
#37058=VERTEX_POINT('',#192862);
#37059=VERTEX_POINT('',#192870);
#37060=VERTEX_POINT('',#192871);
#37061=VERTEX_POINT('',#192873);
#37062=VERTEX_POINT('',#192875);
#37063=VERTEX_POINT('',#192879);
#37064=VERTEX_POINT('',#192880);
#37065=VERTEX_POINT('',#192885);
#37066=VERTEX_POINT('',#192886);
#37067=VERTEX_POINT('',#192894);
#37068=VERTEX_POINT('',#192895);
#37069=VERTEX_POINT('',#192897);
#37070=VERTEX_POINT('',#192899);
#37071=VERTEX_POINT('',#192903);
#37072=VERTEX_POINT('',#192904);
#37073=VERTEX_POINT('',#192909);
#37074=VERTEX_POINT('',#192910);
#37075=VERTEX_POINT('',#192918);
#37076=VERTEX_POINT('',#192919);
#37077=VERTEX_POINT('',#192921);
#37078=VERTEX_POINT('',#192923);
#37079=VERTEX_POINT('',#192927);
#37080=VERTEX_POINT('',#192928);
#37081=VERTEX_POINT('',#192933);
#37082=VERTEX_POINT('',#192934);
#37083=VERTEX_POINT('',#192942);
#37084=VERTEX_POINT('',#192943);
#37085=VERTEX_POINT('',#192945);
#37086=VERTEX_POINT('',#192947);
#37087=VERTEX_POINT('',#192951);
#37088=VERTEX_POINT('',#192952);
#37089=VERTEX_POINT('',#192957);
#37090=VERTEX_POINT('',#192958);
#37091=VERTEX_POINT('',#192966);
#37092=VERTEX_POINT('',#192967);
#37093=VERTEX_POINT('',#192969);
#37094=VERTEX_POINT('',#192971);
#37095=VERTEX_POINT('',#192975);
#37096=VERTEX_POINT('',#192976);
#37097=VERTEX_POINT('',#192981);
#37098=VERTEX_POINT('',#192982);
#37099=VERTEX_POINT('',#192990);
#37100=VERTEX_POINT('',#192991);
#37101=VERTEX_POINT('',#192993);
#37102=VERTEX_POINT('',#192995);
#37103=VERTEX_POINT('',#192999);
#37104=VERTEX_POINT('',#193000);
#37105=VERTEX_POINT('',#193005);
#37106=VERTEX_POINT('',#193006);
#37107=VERTEX_POINT('',#193014);
#37108=VERTEX_POINT('',#193015);
#37109=VERTEX_POINT('',#193017);
#37110=VERTEX_POINT('',#193019);
#37111=VERTEX_POINT('',#193023);
#37112=VERTEX_POINT('',#193024);
#37113=VERTEX_POINT('',#193029);
#37114=VERTEX_POINT('',#193030);
#37115=VERTEX_POINT('',#193038);
#37116=VERTEX_POINT('',#193039);
#37117=VERTEX_POINT('',#193041);
#37118=VERTEX_POINT('',#193043);
#37119=VERTEX_POINT('',#193047);
#37120=VERTEX_POINT('',#193048);
#37121=VERTEX_POINT('',#193053);
#37122=VERTEX_POINT('',#193054);
#37123=VERTEX_POINT('',#193062);
#37124=VERTEX_POINT('',#193063);
#37125=VERTEX_POINT('',#193065);
#37126=VERTEX_POINT('',#193067);
#37127=VERTEX_POINT('',#193071);
#37128=VERTEX_POINT('',#193072);
#37129=VERTEX_POINT('',#193077);
#37130=VERTEX_POINT('',#193078);
#37131=VERTEX_POINT('',#193086);
#37132=VERTEX_POINT('',#193087);
#37133=VERTEX_POINT('',#193089);
#37134=VERTEX_POINT('',#193091);
#37135=VERTEX_POINT('',#193095);
#37136=VERTEX_POINT('',#193096);
#37137=VERTEX_POINT('',#193101);
#37138=VERTEX_POINT('',#193102);
#37139=VERTEX_POINT('',#193110);
#37140=VERTEX_POINT('',#193111);
#37141=VERTEX_POINT('',#193113);
#37142=VERTEX_POINT('',#193115);
#37143=VERTEX_POINT('',#193119);
#37144=VERTEX_POINT('',#193120);
#37145=VERTEX_POINT('',#193125);
#37146=VERTEX_POINT('',#193126);
#37147=VERTEX_POINT('',#193134);
#37148=VERTEX_POINT('',#193135);
#37149=VERTEX_POINT('',#193137);
#37150=VERTEX_POINT('',#193139);
#37151=VERTEX_POINT('',#193143);
#37152=VERTEX_POINT('',#193144);
#37153=VERTEX_POINT('',#193149);
#37154=VERTEX_POINT('',#193150);
#37155=VERTEX_POINT('',#193158);
#37156=VERTEX_POINT('',#193159);
#37157=VERTEX_POINT('',#193161);
#37158=VERTEX_POINT('',#193163);
#37159=VERTEX_POINT('',#193167);
#37160=VERTEX_POINT('',#193168);
#37161=VERTEX_POINT('',#193173);
#37162=VERTEX_POINT('',#193174);
#37163=VERTEX_POINT('',#193182);
#37164=VERTEX_POINT('',#193183);
#37165=VERTEX_POINT('',#193185);
#37166=VERTEX_POINT('',#193187);
#37167=VERTEX_POINT('',#193191);
#37168=VERTEX_POINT('',#193192);
#37169=VERTEX_POINT('',#193197);
#37170=VERTEX_POINT('',#193198);
#37171=VERTEX_POINT('',#193206);
#37172=VERTEX_POINT('',#193207);
#37173=VERTEX_POINT('',#193209);
#37174=VERTEX_POINT('',#193211);
#37175=VERTEX_POINT('',#193215);
#37176=VERTEX_POINT('',#193216);
#37177=VERTEX_POINT('',#193221);
#37178=VERTEX_POINT('',#193222);
#37179=VERTEX_POINT('',#193230);
#37180=VERTEX_POINT('',#193231);
#37181=VERTEX_POINT('',#193233);
#37182=VERTEX_POINT('',#193235);
#37183=VERTEX_POINT('',#193239);
#37184=VERTEX_POINT('',#193240);
#37185=VERTEX_POINT('',#193245);
#37186=VERTEX_POINT('',#193246);
#37187=VERTEX_POINT('',#193254);
#37188=VERTEX_POINT('',#193255);
#37189=VERTEX_POINT('',#193257);
#37190=VERTEX_POINT('',#193259);
#37191=VERTEX_POINT('',#193263);
#37192=VERTEX_POINT('',#193264);
#37193=VERTEX_POINT('',#193269);
#37194=VERTEX_POINT('',#193270);
#37195=VERTEX_POINT('',#193278);
#37196=VERTEX_POINT('',#193279);
#37197=VERTEX_POINT('',#193281);
#37198=VERTEX_POINT('',#193283);
#37199=VERTEX_POINT('',#193287);
#37200=VERTEX_POINT('',#193288);
#37201=VERTEX_POINT('',#193293);
#37202=VERTEX_POINT('',#193294);
#37203=VERTEX_POINT('',#193302);
#37204=VERTEX_POINT('',#193303);
#37205=VERTEX_POINT('',#193305);
#37206=VERTEX_POINT('',#193307);
#37207=VERTEX_POINT('',#193311);
#37208=VERTEX_POINT('',#193312);
#37209=VERTEX_POINT('',#193317);
#37210=VERTEX_POINT('',#193318);
#37211=VERTEX_POINT('',#193326);
#37212=VERTEX_POINT('',#193327);
#37213=VERTEX_POINT('',#193329);
#37214=VERTEX_POINT('',#193331);
#37215=VERTEX_POINT('',#193335);
#37216=VERTEX_POINT('',#193336);
#37217=VERTEX_POINT('',#193341);
#37218=VERTEX_POINT('',#193342);
#37219=VERTEX_POINT('',#193350);
#37220=VERTEX_POINT('',#193351);
#37221=VERTEX_POINT('',#193353);
#37222=VERTEX_POINT('',#193355);
#37223=VERTEX_POINT('',#193359);
#37224=VERTEX_POINT('',#193360);
#37225=VERTEX_POINT('',#193365);
#37226=VERTEX_POINT('',#193366);
#37227=VERTEX_POINT('',#193374);
#37228=VERTEX_POINT('',#193375);
#37229=VERTEX_POINT('',#193377);
#37230=VERTEX_POINT('',#193379);
#37231=VERTEX_POINT('',#193383);
#37232=VERTEX_POINT('',#193384);
#37233=VERTEX_POINT('',#193389);
#37234=VERTEX_POINT('',#193390);
#37235=VERTEX_POINT('',#193398);
#37236=VERTEX_POINT('',#193399);
#37237=VERTEX_POINT('',#193401);
#37238=VERTEX_POINT('',#193403);
#37239=VERTEX_POINT('',#193407);
#37240=VERTEX_POINT('',#193408);
#37241=VERTEX_POINT('',#193413);
#37242=VERTEX_POINT('',#193414);
#37243=VERTEX_POINT('',#193423);
#37244=VERTEX_POINT('',#193424);
#37245=VERTEX_POINT('',#193426);
#37246=VERTEX_POINT('',#193428);
#37247=VERTEX_POINT('',#193432);
#37248=VERTEX_POINT('',#193433);
#37249=VERTEX_POINT('',#193438);
#37250=VERTEX_POINT('',#193439);
#37251=VERTEX_POINT('',#193447);
#37252=VERTEX_POINT('',#193448);
#37253=VERTEX_POINT('',#193450);
#37254=VERTEX_POINT('',#193452);
#37255=VERTEX_POINT('',#193456);
#37256=VERTEX_POINT('',#193457);
#37257=VERTEX_POINT('',#193462);
#37258=VERTEX_POINT('',#193463);
#37259=VERTEX_POINT('',#193471);
#37260=VERTEX_POINT('',#193472);
#37261=VERTEX_POINT('',#193474);
#37262=VERTEX_POINT('',#193476);
#37263=VERTEX_POINT('',#193480);
#37264=VERTEX_POINT('',#193481);
#37265=VERTEX_POINT('',#193486);
#37266=VERTEX_POINT('',#193487);
#37267=VERTEX_POINT('',#193495);
#37268=VERTEX_POINT('',#193496);
#37269=VERTEX_POINT('',#193498);
#37270=VERTEX_POINT('',#193500);
#37271=VERTEX_POINT('',#193504);
#37272=VERTEX_POINT('',#193505);
#37273=VERTEX_POINT('',#193510);
#37274=VERTEX_POINT('',#193511);
#37275=VERTEX_POINT('',#193519);
#37276=VERTEX_POINT('',#193520);
#37277=VERTEX_POINT('',#193522);
#37278=VERTEX_POINT('',#193524);
#37279=VERTEX_POINT('',#193528);
#37280=VERTEX_POINT('',#193529);
#37281=VERTEX_POINT('',#193534);
#37282=VERTEX_POINT('',#193535);
#37283=VERTEX_POINT('',#193543);
#37284=VERTEX_POINT('',#193544);
#37285=VERTEX_POINT('',#193546);
#37286=VERTEX_POINT('',#193548);
#37287=VERTEX_POINT('',#193552);
#37288=VERTEX_POINT('',#193553);
#37289=VERTEX_POINT('',#193558);
#37290=VERTEX_POINT('',#193559);
#37291=VERTEX_POINT('',#193567);
#37292=VERTEX_POINT('',#193568);
#37293=VERTEX_POINT('',#193570);
#37294=VERTEX_POINT('',#193572);
#37295=VERTEX_POINT('',#193576);
#37296=VERTEX_POINT('',#193577);
#37297=VERTEX_POINT('',#193582);
#37298=VERTEX_POINT('',#193583);
#37299=VERTEX_POINT('',#193591);
#37300=VERTEX_POINT('',#193592);
#37301=VERTEX_POINT('',#193594);
#37302=VERTEX_POINT('',#193596);
#37303=VERTEX_POINT('',#193600);
#37304=VERTEX_POINT('',#193601);
#37305=VERTEX_POINT('',#193606);
#37306=VERTEX_POINT('',#193607);
#37307=VERTEX_POINT('',#193615);
#37308=VERTEX_POINT('',#193616);
#37309=VERTEX_POINT('',#193618);
#37310=VERTEX_POINT('',#193620);
#37311=VERTEX_POINT('',#193624);
#37312=VERTEX_POINT('',#193625);
#37313=VERTEX_POINT('',#193630);
#37314=VERTEX_POINT('',#193631);
#37315=VERTEX_POINT('',#193639);
#37316=VERTEX_POINT('',#193640);
#37317=VERTEX_POINT('',#193642);
#37318=VERTEX_POINT('',#193644);
#37319=VERTEX_POINT('',#193648);
#37320=VERTEX_POINT('',#193649);
#37321=VERTEX_POINT('',#193654);
#37322=VERTEX_POINT('',#193655);
#37323=VERTEX_POINT('',#193663);
#37324=VERTEX_POINT('',#193664);
#37325=VERTEX_POINT('',#193666);
#37326=VERTEX_POINT('',#193668);
#37327=VERTEX_POINT('',#193672);
#37328=VERTEX_POINT('',#193673);
#37329=VERTEX_POINT('',#193678);
#37330=VERTEX_POINT('',#193679);
#37331=VERTEX_POINT('',#193687);
#37332=VERTEX_POINT('',#193688);
#37333=VERTEX_POINT('',#193690);
#37334=VERTEX_POINT('',#193692);
#37335=VERTEX_POINT('',#193696);
#37336=VERTEX_POINT('',#193697);
#37337=VERTEX_POINT('',#193702);
#37338=VERTEX_POINT('',#193703);
#37339=VERTEX_POINT('',#193711);
#37340=VERTEX_POINT('',#193712);
#37341=VERTEX_POINT('',#193714);
#37342=VERTEX_POINT('',#193716);
#37343=VERTEX_POINT('',#193720);
#37344=VERTEX_POINT('',#193721);
#37345=VERTEX_POINT('',#193726);
#37346=VERTEX_POINT('',#193727);
#37347=VERTEX_POINT('',#193735);
#37348=VERTEX_POINT('',#193736);
#37349=VERTEX_POINT('',#193738);
#37350=VERTEX_POINT('',#193740);
#37351=VERTEX_POINT('',#193744);
#37352=VERTEX_POINT('',#193745);
#37353=VERTEX_POINT('',#193750);
#37354=VERTEX_POINT('',#193751);
#37355=VERTEX_POINT('',#193759);
#37356=VERTEX_POINT('',#193760);
#37357=VERTEX_POINT('',#193762);
#37358=VERTEX_POINT('',#193764);
#37359=VERTEX_POINT('',#193768);
#37360=VERTEX_POINT('',#193769);
#37361=VERTEX_POINT('',#193774);
#37362=VERTEX_POINT('',#193775);
#37363=VERTEX_POINT('',#193783);
#37364=VERTEX_POINT('',#193784);
#37365=VERTEX_POINT('',#193786);
#37366=VERTEX_POINT('',#193788);
#37367=VERTEX_POINT('',#193792);
#37368=VERTEX_POINT('',#193793);
#37369=VERTEX_POINT('',#193798);
#37370=VERTEX_POINT('',#193799);
#37371=VERTEX_POINT('',#193807);
#37372=VERTEX_POINT('',#193808);
#37373=VERTEX_POINT('',#193810);
#37374=VERTEX_POINT('',#193812);
#37375=VERTEX_POINT('',#193816);
#37376=VERTEX_POINT('',#193817);
#37377=VERTEX_POINT('',#193822);
#37378=VERTEX_POINT('',#193823);
#37379=VERTEX_POINT('',#193831);
#37380=VERTEX_POINT('',#193832);
#37381=VERTEX_POINT('',#193834);
#37382=VERTEX_POINT('',#193836);
#37383=VERTEX_POINT('',#193840);
#37384=VERTEX_POINT('',#193841);
#37385=VERTEX_POINT('',#193846);
#37386=VERTEX_POINT('',#193847);
#37387=VERTEX_POINT('',#193855);
#37388=VERTEX_POINT('',#193856);
#37389=VERTEX_POINT('',#193858);
#37390=VERTEX_POINT('',#193860);
#37391=VERTEX_POINT('',#193864);
#37392=VERTEX_POINT('',#193865);
#37393=VERTEX_POINT('',#193870);
#37394=VERTEX_POINT('',#193871);
#37395=VERTEX_POINT('',#193879);
#37396=VERTEX_POINT('',#193880);
#37397=VERTEX_POINT('',#193882);
#37398=VERTEX_POINT('',#193884);
#37399=VERTEX_POINT('',#193888);
#37400=VERTEX_POINT('',#193889);
#37401=VERTEX_POINT('',#193894);
#37402=VERTEX_POINT('',#193895);
#37403=VERTEX_POINT('',#193903);
#37404=VERTEX_POINT('',#193904);
#37405=VERTEX_POINT('',#193906);
#37406=VERTEX_POINT('',#193908);
#37407=VERTEX_POINT('',#193912);
#37408=VERTEX_POINT('',#193913);
#37409=VERTEX_POINT('',#193918);
#37410=VERTEX_POINT('',#193919);
#37411=VERTEX_POINT('',#193927);
#37412=VERTEX_POINT('',#193928);
#37413=VERTEX_POINT('',#193930);
#37414=VERTEX_POINT('',#193932);
#37415=VERTEX_POINT('',#193936);
#37416=VERTEX_POINT('',#193937);
#37417=VERTEX_POINT('',#193942);
#37418=VERTEX_POINT('',#193943);
#37419=VERTEX_POINT('',#193951);
#37420=VERTEX_POINT('',#193952);
#37421=VERTEX_POINT('',#193954);
#37422=VERTEX_POINT('',#193956);
#37423=VERTEX_POINT('',#193960);
#37424=VERTEX_POINT('',#193961);
#37425=VERTEX_POINT('',#193966);
#37426=VERTEX_POINT('',#193967);
#37427=VERTEX_POINT('',#193975);
#37428=VERTEX_POINT('',#193976);
#37429=VERTEX_POINT('',#193978);
#37430=VERTEX_POINT('',#193980);
#37431=VERTEX_POINT('',#193984);
#37432=VERTEX_POINT('',#193985);
#37433=VERTEX_POINT('',#193990);
#37434=VERTEX_POINT('',#193991);
#37435=VERTEX_POINT('',#193999);
#37436=VERTEX_POINT('',#194000);
#37437=VERTEX_POINT('',#194002);
#37438=VERTEX_POINT('',#194004);
#37439=VERTEX_POINT('',#194008);
#37440=VERTEX_POINT('',#194009);
#37441=VERTEX_POINT('',#194014);
#37442=VERTEX_POINT('',#194015);
#37443=VERTEX_POINT('',#194023);
#37444=VERTEX_POINT('',#194024);
#37445=VERTEX_POINT('',#194026);
#37446=VERTEX_POINT('',#194028);
#37447=VERTEX_POINT('',#194032);
#37448=VERTEX_POINT('',#194033);
#37449=VERTEX_POINT('',#194038);
#37450=VERTEX_POINT('',#194039);
#37451=VERTEX_POINT('',#194047);
#37452=VERTEX_POINT('',#194048);
#37453=VERTEX_POINT('',#194050);
#37454=VERTEX_POINT('',#194052);
#37455=VERTEX_POINT('',#194056);
#37456=VERTEX_POINT('',#194057);
#37457=VERTEX_POINT('',#194062);
#37458=VERTEX_POINT('',#194063);
#37459=VERTEX_POINT('',#194071);
#37460=VERTEX_POINT('',#194072);
#37461=VERTEX_POINT('',#194074);
#37462=VERTEX_POINT('',#194076);
#37463=VERTEX_POINT('',#194080);
#37464=VERTEX_POINT('',#194081);
#37465=VERTEX_POINT('',#194086);
#37466=VERTEX_POINT('',#194087);
#37467=VERTEX_POINT('',#194095);
#37468=VERTEX_POINT('',#194096);
#37469=VERTEX_POINT('',#194098);
#37470=VERTEX_POINT('',#194100);
#37471=VERTEX_POINT('',#194104);
#37472=VERTEX_POINT('',#194105);
#37473=VERTEX_POINT('',#194110);
#37474=VERTEX_POINT('',#194111);
#37475=VERTEX_POINT('',#194119);
#37476=VERTEX_POINT('',#194120);
#37477=VERTEX_POINT('',#194122);
#37478=VERTEX_POINT('',#194124);
#37479=VERTEX_POINT('',#194128);
#37480=VERTEX_POINT('',#194129);
#37481=VERTEX_POINT('',#194134);
#37482=VERTEX_POINT('',#194135);
#37483=VERTEX_POINT('',#194143);
#37484=VERTEX_POINT('',#194144);
#37485=VERTEX_POINT('',#194146);
#37486=VERTEX_POINT('',#194148);
#37487=VERTEX_POINT('',#194152);
#37488=VERTEX_POINT('',#194153);
#37489=VERTEX_POINT('',#194158);
#37490=VERTEX_POINT('',#194159);
#37491=VERTEX_POINT('',#194167);
#37492=VERTEX_POINT('',#194168);
#37493=VERTEX_POINT('',#194170);
#37494=VERTEX_POINT('',#194172);
#37495=VERTEX_POINT('',#194176);
#37496=VERTEX_POINT('',#194177);
#37497=VERTEX_POINT('',#194182);
#37498=VERTEX_POINT('',#194183);
#37499=VERTEX_POINT('',#194191);
#37500=VERTEX_POINT('',#194192);
#37501=VERTEX_POINT('',#194194);
#37502=VERTEX_POINT('',#194196);
#37503=VERTEX_POINT('',#194200);
#37504=VERTEX_POINT('',#194201);
#37505=VERTEX_POINT('',#194206);
#37506=VERTEX_POINT('',#194207);
#37507=VERTEX_POINT('',#194215);
#37508=VERTEX_POINT('',#194216);
#37509=VERTEX_POINT('',#194218);
#37510=VERTEX_POINT('',#194220);
#37511=VERTEX_POINT('',#194224);
#37512=VERTEX_POINT('',#194225);
#37513=VERTEX_POINT('',#194230);
#37514=VERTEX_POINT('',#194231);
#37515=VERTEX_POINT('',#194239);
#37516=VERTEX_POINT('',#194240);
#37517=VERTEX_POINT('',#194242);
#37518=VERTEX_POINT('',#194244);
#37519=VERTEX_POINT('',#194248);
#37520=VERTEX_POINT('',#194249);
#37521=VERTEX_POINT('',#194254);
#37522=VERTEX_POINT('',#194255);
#37523=VERTEX_POINT('',#194263);
#37524=VERTEX_POINT('',#194264);
#37525=VERTEX_POINT('',#194266);
#37526=VERTEX_POINT('',#194268);
#37527=VERTEX_POINT('',#194272);
#37528=VERTEX_POINT('',#194273);
#37529=VERTEX_POINT('',#194278);
#37530=VERTEX_POINT('',#194279);
#37531=VERTEX_POINT('',#194287);
#37532=VERTEX_POINT('',#194288);
#37533=VERTEX_POINT('',#194290);
#37534=VERTEX_POINT('',#194292);
#37535=VERTEX_POINT('',#194296);
#37536=VERTEX_POINT('',#194297);
#37537=VERTEX_POINT('',#194302);
#37538=VERTEX_POINT('',#194303);
#37539=VERTEX_POINT('',#194311);
#37540=VERTEX_POINT('',#194312);
#37541=VERTEX_POINT('',#194314);
#37542=VERTEX_POINT('',#194316);
#37543=VERTEX_POINT('',#194320);
#37544=VERTEX_POINT('',#194321);
#37545=VERTEX_POINT('',#194326);
#37546=VERTEX_POINT('',#194327);
#37547=VERTEX_POINT('',#194335);
#37548=VERTEX_POINT('',#194336);
#37549=VERTEX_POINT('',#194338);
#37550=VERTEX_POINT('',#194340);
#37551=VERTEX_POINT('',#194344);
#37552=VERTEX_POINT('',#194345);
#37553=VERTEX_POINT('',#194350);
#37554=VERTEX_POINT('',#194351);
#37555=VERTEX_POINT('',#194359);
#37556=VERTEX_POINT('',#194360);
#37557=VERTEX_POINT('',#194362);
#37558=VERTEX_POINT('',#194364);
#37559=VERTEX_POINT('',#194368);
#37560=VERTEX_POINT('',#194369);
#37561=VERTEX_POINT('',#194374);
#37562=VERTEX_POINT('',#194375);
#37563=VERTEX_POINT('',#194383);
#37564=VERTEX_POINT('',#194384);
#37565=VERTEX_POINT('',#194386);
#37566=VERTEX_POINT('',#194388);
#37567=VERTEX_POINT('',#194392);
#37568=VERTEX_POINT('',#194393);
#37569=VERTEX_POINT('',#194398);
#37570=VERTEX_POINT('',#194399);
#37571=VERTEX_POINT('',#194407);
#37572=VERTEX_POINT('',#194408);
#37573=VERTEX_POINT('',#194410);
#37574=VERTEX_POINT('',#194412);
#37575=VERTEX_POINT('',#194416);
#37576=VERTEX_POINT('',#194417);
#37577=VERTEX_POINT('',#194422);
#37578=VERTEX_POINT('',#194423);
#37579=VERTEX_POINT('',#194431);
#37580=VERTEX_POINT('',#194432);
#37581=VERTEX_POINT('',#194434);
#37582=VERTEX_POINT('',#194436);
#37583=VERTEX_POINT('',#194440);
#37584=VERTEX_POINT('',#194441);
#37585=VERTEX_POINT('',#194446);
#37586=VERTEX_POINT('',#194447);
#37587=VERTEX_POINT('',#194455);
#37588=VERTEX_POINT('',#194456);
#37589=VERTEX_POINT('',#194458);
#37590=VERTEX_POINT('',#194460);
#37591=VERTEX_POINT('',#194464);
#37592=VERTEX_POINT('',#194465);
#37593=VERTEX_POINT('',#194470);
#37594=VERTEX_POINT('',#194471);
#37595=VERTEX_POINT('',#194479);
#37596=VERTEX_POINT('',#194480);
#37597=VERTEX_POINT('',#194482);
#37598=VERTEX_POINT('',#194484);
#37599=VERTEX_POINT('',#194488);
#37600=VERTEX_POINT('',#194489);
#37601=VERTEX_POINT('',#194494);
#37602=VERTEX_POINT('',#194495);
#37603=VERTEX_POINT('',#194503);
#37604=VERTEX_POINT('',#194504);
#37605=VERTEX_POINT('',#194506);
#37606=VERTEX_POINT('',#194508);
#37607=VERTEX_POINT('',#194512);
#37608=VERTEX_POINT('',#194513);
#37609=VERTEX_POINT('',#194518);
#37610=VERTEX_POINT('',#194519);
#37611=VERTEX_POINT('',#194527);
#37612=VERTEX_POINT('',#194528);
#37613=VERTEX_POINT('',#194530);
#37614=VERTEX_POINT('',#194532);
#37615=VERTEX_POINT('',#194536);
#37616=VERTEX_POINT('',#194537);
#37617=VERTEX_POINT('',#194542);
#37618=VERTEX_POINT('',#194543);
#37619=VERTEX_POINT('',#194551);
#37620=VERTEX_POINT('',#194552);
#37621=VERTEX_POINT('',#194554);
#37622=VERTEX_POINT('',#194556);
#37623=VERTEX_POINT('',#194560);
#37624=VERTEX_POINT('',#194561);
#37625=VERTEX_POINT('',#194566);
#37626=VERTEX_POINT('',#194567);
#37627=VERTEX_POINT('',#194575);
#37628=VERTEX_POINT('',#194576);
#37629=VERTEX_POINT('',#194578);
#37630=VERTEX_POINT('',#194580);
#37631=VERTEX_POINT('',#194584);
#37632=VERTEX_POINT('',#194585);
#37633=VERTEX_POINT('',#194590);
#37634=VERTEX_POINT('',#194591);
#37635=VERTEX_POINT('',#194599);
#37636=VERTEX_POINT('',#194600);
#37637=VERTEX_POINT('',#194602);
#37638=VERTEX_POINT('',#194604);
#37639=VERTEX_POINT('',#194608);
#37640=VERTEX_POINT('',#194609);
#37641=VERTEX_POINT('',#194614);
#37642=VERTEX_POINT('',#194615);
#37643=VERTEX_POINT('',#194623);
#37644=VERTEX_POINT('',#194624);
#37645=VERTEX_POINT('',#194626);
#37646=VERTEX_POINT('',#194628);
#37647=VERTEX_POINT('',#194632);
#37648=VERTEX_POINT('',#194633);
#37649=VERTEX_POINT('',#194638);
#37650=VERTEX_POINT('',#194639);
#37651=VERTEX_POINT('',#194647);
#37652=VERTEX_POINT('',#194648);
#37653=VERTEX_POINT('',#194650);
#37654=VERTEX_POINT('',#194652);
#37655=VERTEX_POINT('',#194656);
#37656=VERTEX_POINT('',#194657);
#37657=VERTEX_POINT('',#194662);
#37658=VERTEX_POINT('',#194663);
#37659=VERTEX_POINT('',#194671);
#37660=VERTEX_POINT('',#194672);
#37661=VERTEX_POINT('',#194674);
#37662=VERTEX_POINT('',#194676);
#37663=VERTEX_POINT('',#194680);
#37664=VERTEX_POINT('',#194681);
#37665=VERTEX_POINT('',#194686);
#37666=VERTEX_POINT('',#194687);
#37667=VERTEX_POINT('',#194695);
#37668=VERTEX_POINT('',#194696);
#37669=VERTEX_POINT('',#194698);
#37670=VERTEX_POINT('',#194700);
#37671=VERTEX_POINT('',#194704);
#37672=VERTEX_POINT('',#194705);
#37673=VERTEX_POINT('',#194710);
#37674=VERTEX_POINT('',#194711);
#37675=VERTEX_POINT('',#194719);
#37676=VERTEX_POINT('',#194720);
#37677=VERTEX_POINT('',#194722);
#37678=VERTEX_POINT('',#194724);
#37679=VERTEX_POINT('',#194728);
#37680=VERTEX_POINT('',#194729);
#37681=VERTEX_POINT('',#194734);
#37682=VERTEX_POINT('',#194735);
#37683=VERTEX_POINT('',#194743);
#37684=VERTEX_POINT('',#194744);
#37685=VERTEX_POINT('',#194746);
#37686=VERTEX_POINT('',#194748);
#37687=VERTEX_POINT('',#194752);
#37688=VERTEX_POINT('',#194753);
#37689=VERTEX_POINT('',#194758);
#37690=VERTEX_POINT('',#194759);
#37691=VERTEX_POINT('',#194767);
#37692=VERTEX_POINT('',#194768);
#37693=VERTEX_POINT('',#194770);
#37694=VERTEX_POINT('',#194772);
#37695=VERTEX_POINT('',#194776);
#37696=VERTEX_POINT('',#194777);
#37697=VERTEX_POINT('',#194782);
#37698=VERTEX_POINT('',#194783);
#37699=VERTEX_POINT('',#194791);
#37700=VERTEX_POINT('',#194792);
#37701=VERTEX_POINT('',#194794);
#37702=VERTEX_POINT('',#194796);
#37703=VERTEX_POINT('',#194800);
#37704=VERTEX_POINT('',#194801);
#37705=VERTEX_POINT('',#194806);
#37706=VERTEX_POINT('',#194807);
#37707=VERTEX_POINT('',#194815);
#37708=VERTEX_POINT('',#194816);
#37709=VERTEX_POINT('',#194818);
#37710=VERTEX_POINT('',#194820);
#37711=VERTEX_POINT('',#194824);
#37712=VERTEX_POINT('',#194825);
#37713=VERTEX_POINT('',#194830);
#37714=VERTEX_POINT('',#194831);
#37715=VERTEX_POINT('',#194839);
#37716=VERTEX_POINT('',#194840);
#37717=VERTEX_POINT('',#194842);
#37718=VERTEX_POINT('',#194844);
#37719=VERTEX_POINT('',#194848);
#37720=VERTEX_POINT('',#194849);
#37721=VERTEX_POINT('',#194854);
#37722=VERTEX_POINT('',#194855);
#37723=VERTEX_POINT('',#194863);
#37724=VERTEX_POINT('',#194864);
#37725=VERTEX_POINT('',#194866);
#37726=VERTEX_POINT('',#194868);
#37727=VERTEX_POINT('',#194872);
#37728=VERTEX_POINT('',#194873);
#37729=VERTEX_POINT('',#194878);
#37730=VERTEX_POINT('',#194879);
#37731=VERTEX_POINT('',#194887);
#37732=VERTEX_POINT('',#194888);
#37733=VERTEX_POINT('',#194890);
#37734=VERTEX_POINT('',#194892);
#37735=VERTEX_POINT('',#194896);
#37736=VERTEX_POINT('',#194897);
#37737=VERTEX_POINT('',#194902);
#37738=VERTEX_POINT('',#194903);
#37739=VERTEX_POINT('',#194911);
#37740=VERTEX_POINT('',#194912);
#37741=VERTEX_POINT('',#194914);
#37742=VERTEX_POINT('',#194916);
#37743=VERTEX_POINT('',#194920);
#37744=VERTEX_POINT('',#194921);
#37745=VERTEX_POINT('',#194926);
#37746=VERTEX_POINT('',#194927);
#37747=VERTEX_POINT('',#194935);
#37748=VERTEX_POINT('',#194936);
#37749=VERTEX_POINT('',#194938);
#37750=VERTEX_POINT('',#194940);
#37751=VERTEX_POINT('',#194944);
#37752=VERTEX_POINT('',#194945);
#37753=VERTEX_POINT('',#194950);
#37754=VERTEX_POINT('',#194951);
#37755=VERTEX_POINT('',#194959);
#37756=VERTEX_POINT('',#194960);
#37757=VERTEX_POINT('',#194962);
#37758=VERTEX_POINT('',#194964);
#37759=VERTEX_POINT('',#194968);
#37760=VERTEX_POINT('',#194969);
#37761=VERTEX_POINT('',#194974);
#37762=VERTEX_POINT('',#194975);
#37763=VERTEX_POINT('',#194983);
#37764=VERTEX_POINT('',#194984);
#37765=VERTEX_POINT('',#194986);
#37766=VERTEX_POINT('',#194988);
#37767=VERTEX_POINT('',#194992);
#37768=VERTEX_POINT('',#194993);
#37769=VERTEX_POINT('',#194998);
#37770=VERTEX_POINT('',#194999);
#37771=VERTEX_POINT('',#195007);
#37772=VERTEX_POINT('',#195008);
#37773=VERTEX_POINT('',#195010);
#37774=VERTEX_POINT('',#195012);
#37775=VERTEX_POINT('',#195016);
#37776=VERTEX_POINT('',#195017);
#37777=VERTEX_POINT('',#195022);
#37778=VERTEX_POINT('',#195023);
#37779=VERTEX_POINT('',#195031);
#37780=VERTEX_POINT('',#195032);
#37781=VERTEX_POINT('',#195034);
#37782=VERTEX_POINT('',#195036);
#37783=VERTEX_POINT('',#195040);
#37784=VERTEX_POINT('',#195041);
#37785=VERTEX_POINT('',#195046);
#37786=VERTEX_POINT('',#195047);
#37787=VERTEX_POINT('',#195055);
#37788=VERTEX_POINT('',#195056);
#37789=VERTEX_POINT('',#195058);
#37790=VERTEX_POINT('',#195060);
#37791=VERTEX_POINT('',#195064);
#37792=VERTEX_POINT('',#195065);
#37793=VERTEX_POINT('',#195070);
#37794=VERTEX_POINT('',#195071);
#37795=VERTEX_POINT('',#195079);
#37796=VERTEX_POINT('',#195080);
#37797=VERTEX_POINT('',#195082);
#37798=VERTEX_POINT('',#195084);
#37799=VERTEX_POINT('',#195088);
#37800=VERTEX_POINT('',#195089);
#37801=VERTEX_POINT('',#195094);
#37802=VERTEX_POINT('',#195095);
#37803=VERTEX_POINT('',#195103);
#37804=VERTEX_POINT('',#195104);
#37805=VERTEX_POINT('',#195106);
#37806=VERTEX_POINT('',#195108);
#37807=VERTEX_POINT('',#195112);
#37808=VERTEX_POINT('',#195113);
#37809=VERTEX_POINT('',#195118);
#37810=VERTEX_POINT('',#195119);
#37811=VERTEX_POINT('',#195127);
#37812=VERTEX_POINT('',#195128);
#37813=VERTEX_POINT('',#195130);
#37814=VERTEX_POINT('',#195132);
#37815=VERTEX_POINT('',#195136);
#37816=VERTEX_POINT('',#195137);
#37817=VERTEX_POINT('',#195142);
#37818=VERTEX_POINT('',#195143);
#37819=VERTEX_POINT('',#195151);
#37820=VERTEX_POINT('',#195152);
#37821=VERTEX_POINT('',#195154);
#37822=VERTEX_POINT('',#195156);
#37823=VERTEX_POINT('',#195160);
#37824=VERTEX_POINT('',#195161);
#37825=VERTEX_POINT('',#195166);
#37826=VERTEX_POINT('',#195167);
#37827=VERTEX_POINT('',#195175);
#37828=VERTEX_POINT('',#195176);
#37829=VERTEX_POINT('',#195178);
#37830=VERTEX_POINT('',#195180);
#37831=VERTEX_POINT('',#195184);
#37832=VERTEX_POINT('',#195185);
#37833=VERTEX_POINT('',#195190);
#37834=VERTEX_POINT('',#195191);
#37835=VERTEX_POINT('',#195199);
#37836=VERTEX_POINT('',#195200);
#37837=VERTEX_POINT('',#195202);
#37838=VERTEX_POINT('',#195204);
#37839=VERTEX_POINT('',#195208);
#37840=VERTEX_POINT('',#195209);
#37841=VERTEX_POINT('',#195214);
#37842=VERTEX_POINT('',#195215);
#37843=VERTEX_POINT('',#195223);
#37844=VERTEX_POINT('',#195224);
#37845=VERTEX_POINT('',#195226);
#37846=VERTEX_POINT('',#195228);
#37847=VERTEX_POINT('',#195232);
#37848=VERTEX_POINT('',#195233);
#37849=VERTEX_POINT('',#195238);
#37850=VERTEX_POINT('',#195239);
#37851=VERTEX_POINT('',#195247);
#37852=VERTEX_POINT('',#195248);
#37853=VERTEX_POINT('',#195250);
#37854=VERTEX_POINT('',#195252);
#37855=VERTEX_POINT('',#195256);
#37856=VERTEX_POINT('',#195257);
#37857=VERTEX_POINT('',#195262);
#37858=VERTEX_POINT('',#195263);
#37859=VERTEX_POINT('',#195271);
#37860=VERTEX_POINT('',#195272);
#37861=VERTEX_POINT('',#195274);
#37862=VERTEX_POINT('',#195276);
#37863=VERTEX_POINT('',#195280);
#37864=VERTEX_POINT('',#195281);
#37865=VERTEX_POINT('',#195286);
#37866=VERTEX_POINT('',#195287);
#37867=VERTEX_POINT('',#195295);
#37868=VERTEX_POINT('',#195296);
#37869=VERTEX_POINT('',#195298);
#37870=VERTEX_POINT('',#195300);
#37871=VERTEX_POINT('',#195304);
#37872=VERTEX_POINT('',#195305);
#37873=VERTEX_POINT('',#195310);
#37874=VERTEX_POINT('',#195311);
#37875=VERTEX_POINT('',#195319);
#37876=VERTEX_POINT('',#195320);
#37877=VERTEX_POINT('',#195322);
#37878=VERTEX_POINT('',#195324);
#37879=VERTEX_POINT('',#195328);
#37880=VERTEX_POINT('',#195329);
#37881=VERTEX_POINT('',#195334);
#37882=VERTEX_POINT('',#195335);
#37883=VERTEX_POINT('',#195343);
#37884=VERTEX_POINT('',#195344);
#37885=VERTEX_POINT('',#195346);
#37886=VERTEX_POINT('',#195348);
#37887=VERTEX_POINT('',#195352);
#37888=VERTEX_POINT('',#195353);
#37889=VERTEX_POINT('',#195358);
#37890=VERTEX_POINT('',#195359);
#37891=VERTEX_POINT('',#195367);
#37892=VERTEX_POINT('',#195368);
#37893=VERTEX_POINT('',#195370);
#37894=VERTEX_POINT('',#195372);
#37895=VERTEX_POINT('',#195376);
#37896=VERTEX_POINT('',#195377);
#37897=VERTEX_POINT('',#195382);
#37898=VERTEX_POINT('',#195383);
#37899=VERTEX_POINT('',#195391);
#37900=VERTEX_POINT('',#195392);
#37901=VERTEX_POINT('',#195394);
#37902=VERTEX_POINT('',#195396);
#37903=VERTEX_POINT('',#195400);
#37904=VERTEX_POINT('',#195401);
#37905=VERTEX_POINT('',#195406);
#37906=VERTEX_POINT('',#195407);
#37907=VERTEX_POINT('',#195415);
#37908=VERTEX_POINT('',#195416);
#37909=VERTEX_POINT('',#195418);
#37910=VERTEX_POINT('',#195420);
#37911=VERTEX_POINT('',#195424);
#37912=VERTEX_POINT('',#195425);
#37913=VERTEX_POINT('',#195430);
#37914=VERTEX_POINT('',#195431);
#37915=VERTEX_POINT('',#195439);
#37916=VERTEX_POINT('',#195440);
#37917=VERTEX_POINT('',#195442);
#37918=VERTEX_POINT('',#195444);
#37919=VERTEX_POINT('',#195448);
#37920=VERTEX_POINT('',#195449);
#37921=VERTEX_POINT('',#195454);
#37922=VERTEX_POINT('',#195455);
#37923=VERTEX_POINT('',#195463);
#37924=VERTEX_POINT('',#195464);
#37925=VERTEX_POINT('',#195466);
#37926=VERTEX_POINT('',#195468);
#37927=VERTEX_POINT('',#195472);
#37928=VERTEX_POINT('',#195473);
#37929=VERTEX_POINT('',#195478);
#37930=VERTEX_POINT('',#195479);
#37931=VERTEX_POINT('',#195487);
#37932=VERTEX_POINT('',#195488);
#37933=VERTEX_POINT('',#195490);
#37934=VERTEX_POINT('',#195492);
#37935=VERTEX_POINT('',#195496);
#37936=VERTEX_POINT('',#195497);
#37937=VERTEX_POINT('',#195502);
#37938=VERTEX_POINT('',#195503);
#37939=VERTEX_POINT('',#195511);
#37940=VERTEX_POINT('',#195512);
#37941=VERTEX_POINT('',#195514);
#37942=VERTEX_POINT('',#195516);
#37943=VERTEX_POINT('',#195520);
#37944=VERTEX_POINT('',#195521);
#37945=VERTEX_POINT('',#195526);
#37946=VERTEX_POINT('',#195527);
#37947=VERTEX_POINT('',#195535);
#37948=VERTEX_POINT('',#195536);
#37949=VERTEX_POINT('',#195538);
#37950=VERTEX_POINT('',#195540);
#37951=VERTEX_POINT('',#195544);
#37952=VERTEX_POINT('',#195545);
#37953=VERTEX_POINT('',#195550);
#37954=VERTEX_POINT('',#195551);
#37955=VERTEX_POINT('',#195559);
#37956=VERTEX_POINT('',#195560);
#37957=VERTEX_POINT('',#195562);
#37958=VERTEX_POINT('',#195564);
#37959=VERTEX_POINT('',#195568);
#37960=VERTEX_POINT('',#195569);
#37961=VERTEX_POINT('',#195574);
#37962=VERTEX_POINT('',#195575);
#37963=VERTEX_POINT('',#195583);
#37964=VERTEX_POINT('',#195584);
#37965=VERTEX_POINT('',#195586);
#37966=VERTEX_POINT('',#195588);
#37967=VERTEX_POINT('',#195592);
#37968=VERTEX_POINT('',#195593);
#37969=VERTEX_POINT('',#195598);
#37970=VERTEX_POINT('',#195599);
#37971=VERTEX_POINT('',#195607);
#37972=VERTEX_POINT('',#195608);
#37973=VERTEX_POINT('',#195610);
#37974=VERTEX_POINT('',#195612);
#37975=VERTEX_POINT('',#195616);
#37976=VERTEX_POINT('',#195617);
#37977=VERTEX_POINT('',#195622);
#37978=VERTEX_POINT('',#195623);
#37979=VERTEX_POINT('',#195631);
#37980=VERTEX_POINT('',#195632);
#37981=VERTEX_POINT('',#195634);
#37982=VERTEX_POINT('',#195636);
#37983=VERTEX_POINT('',#195640);
#37984=VERTEX_POINT('',#195641);
#37985=VERTEX_POINT('',#195646);
#37986=VERTEX_POINT('',#195647);
#37987=VERTEX_POINT('',#195655);
#37988=VERTEX_POINT('',#195656);
#37989=VERTEX_POINT('',#195658);
#37990=VERTEX_POINT('',#195660);
#37991=VERTEX_POINT('',#195664);
#37992=VERTEX_POINT('',#195665);
#37993=VERTEX_POINT('',#195670);
#37994=VERTEX_POINT('',#195671);
#37995=VERTEX_POINT('',#195679);
#37996=VERTEX_POINT('',#195680);
#37997=VERTEX_POINT('',#195682);
#37998=VERTEX_POINT('',#195684);
#37999=VERTEX_POINT('',#195688);
#38000=VERTEX_POINT('',#195689);
#38001=VERTEX_POINT('',#195694);
#38002=VERTEX_POINT('',#195695);
#38003=VERTEX_POINT('',#195703);
#38004=VERTEX_POINT('',#195704);
#38005=VERTEX_POINT('',#195706);
#38006=VERTEX_POINT('',#195708);
#38007=VERTEX_POINT('',#195712);
#38008=VERTEX_POINT('',#195713);
#38009=VERTEX_POINT('',#195718);
#38010=VERTEX_POINT('',#195719);
#38011=VERTEX_POINT('',#195727);
#38012=VERTEX_POINT('',#195728);
#38013=VERTEX_POINT('',#195730);
#38014=VERTEX_POINT('',#195732);
#38015=VERTEX_POINT('',#195736);
#38016=VERTEX_POINT('',#195737);
#38017=VERTEX_POINT('',#195742);
#38018=VERTEX_POINT('',#195743);
#38019=VERTEX_POINT('',#195751);
#38020=VERTEX_POINT('',#195752);
#38021=VERTEX_POINT('',#195754);
#38022=VERTEX_POINT('',#195756);
#38023=VERTEX_POINT('',#195760);
#38024=VERTEX_POINT('',#195761);
#38025=VERTEX_POINT('',#195766);
#38026=VERTEX_POINT('',#195767);
#38027=VERTEX_POINT('',#195775);
#38028=VERTEX_POINT('',#195776);
#38029=VERTEX_POINT('',#195778);
#38030=VERTEX_POINT('',#195780);
#38031=VERTEX_POINT('',#195784);
#38032=VERTEX_POINT('',#195785);
#38033=VERTEX_POINT('',#195790);
#38034=VERTEX_POINT('',#195791);
#38035=VERTEX_POINT('',#195799);
#38036=VERTEX_POINT('',#195800);
#38037=VERTEX_POINT('',#195802);
#38038=VERTEX_POINT('',#195804);
#38039=VERTEX_POINT('',#195808);
#38040=VERTEX_POINT('',#195809);
#38041=VERTEX_POINT('',#195814);
#38042=VERTEX_POINT('',#195815);
#38043=VERTEX_POINT('',#195823);
#38044=VERTEX_POINT('',#195824);
#38045=VERTEX_POINT('',#195826);
#38046=VERTEX_POINT('',#195828);
#38047=VERTEX_POINT('',#195832);
#38048=VERTEX_POINT('',#195833);
#38049=VERTEX_POINT('',#195838);
#38050=VERTEX_POINT('',#195839);
#38051=VERTEX_POINT('',#195847);
#38052=VERTEX_POINT('',#195848);
#38053=VERTEX_POINT('',#195850);
#38054=VERTEX_POINT('',#195852);
#38055=VERTEX_POINT('',#195856);
#38056=VERTEX_POINT('',#195857);
#38057=VERTEX_POINT('',#195862);
#38058=VERTEX_POINT('',#195863);
#38059=VERTEX_POINT('',#195871);
#38060=VERTEX_POINT('',#195872);
#38061=VERTEX_POINT('',#195874);
#38062=VERTEX_POINT('',#195876);
#38063=VERTEX_POINT('',#195880);
#38064=VERTEX_POINT('',#195881);
#38065=VERTEX_POINT('',#195886);
#38066=VERTEX_POINT('',#195887);
#38067=VERTEX_POINT('',#195895);
#38068=VERTEX_POINT('',#195896);
#38069=VERTEX_POINT('',#195898);
#38070=VERTEX_POINT('',#195900);
#38071=VERTEX_POINT('',#195904);
#38072=VERTEX_POINT('',#195905);
#38073=VERTEX_POINT('',#195910);
#38074=VERTEX_POINT('',#195911);
#38075=VERTEX_POINT('',#195919);
#38076=VERTEX_POINT('',#195920);
#38077=VERTEX_POINT('',#195922);
#38078=VERTEX_POINT('',#195924);
#38079=VERTEX_POINT('',#195928);
#38080=VERTEX_POINT('',#195929);
#38081=VERTEX_POINT('',#195934);
#38082=VERTEX_POINT('',#195935);
#38083=VERTEX_POINT('',#195943);
#38084=VERTEX_POINT('',#195944);
#38085=VERTEX_POINT('',#195946);
#38086=VERTEX_POINT('',#195948);
#38087=VERTEX_POINT('',#195952);
#38088=VERTEX_POINT('',#195953);
#38089=VERTEX_POINT('',#195958);
#38090=VERTEX_POINT('',#195959);
#38091=VERTEX_POINT('',#195967);
#38092=VERTEX_POINT('',#195968);
#38093=VERTEX_POINT('',#195970);
#38094=VERTEX_POINT('',#195972);
#38095=VERTEX_POINT('',#195976);
#38096=VERTEX_POINT('',#195977);
#38097=VERTEX_POINT('',#195982);
#38098=VERTEX_POINT('',#195983);
#38099=VERTEX_POINT('',#195991);
#38100=VERTEX_POINT('',#195992);
#38101=VERTEX_POINT('',#195994);
#38102=VERTEX_POINT('',#195996);
#38103=VERTEX_POINT('',#196000);
#38104=VERTEX_POINT('',#196001);
#38105=VERTEX_POINT('',#196006);
#38106=VERTEX_POINT('',#196007);
#38107=VERTEX_POINT('',#196015);
#38108=VERTEX_POINT('',#196016);
#38109=VERTEX_POINT('',#196018);
#38110=VERTEX_POINT('',#196020);
#38111=VERTEX_POINT('',#196024);
#38112=VERTEX_POINT('',#196025);
#38113=VERTEX_POINT('',#196030);
#38114=VERTEX_POINT('',#196031);
#38115=VERTEX_POINT('',#196039);
#38116=VERTEX_POINT('',#196040);
#38117=VERTEX_POINT('',#196042);
#38118=VERTEX_POINT('',#196044);
#38119=VERTEX_POINT('',#196048);
#38120=VERTEX_POINT('',#196049);
#38121=VERTEX_POINT('',#196054);
#38122=VERTEX_POINT('',#196055);
#38123=VERTEX_POINT('',#196063);
#38124=VERTEX_POINT('',#196064);
#38125=VERTEX_POINT('',#196066);
#38126=VERTEX_POINT('',#196068);
#38127=VERTEX_POINT('',#196072);
#38128=VERTEX_POINT('',#196073);
#38129=VERTEX_POINT('',#196078);
#38130=VERTEX_POINT('',#196079);
#38131=VERTEX_POINT('',#196087);
#38132=VERTEX_POINT('',#196088);
#38133=VERTEX_POINT('',#196090);
#38134=VERTEX_POINT('',#196092);
#38135=VERTEX_POINT('',#196096);
#38136=VERTEX_POINT('',#196097);
#38137=VERTEX_POINT('',#196102);
#38138=VERTEX_POINT('',#196103);
#38139=VERTEX_POINT('',#196111);
#38140=VERTEX_POINT('',#196112);
#38141=VERTEX_POINT('',#196114);
#38142=VERTEX_POINT('',#196116);
#38143=VERTEX_POINT('',#196120);
#38144=VERTEX_POINT('',#196121);
#38145=VERTEX_POINT('',#196126);
#38146=VERTEX_POINT('',#196127);
#38147=VERTEX_POINT('',#196135);
#38148=VERTEX_POINT('',#196136);
#38149=VERTEX_POINT('',#196138);
#38150=VERTEX_POINT('',#196140);
#38151=VERTEX_POINT('',#196144);
#38152=VERTEX_POINT('',#196145);
#38153=VERTEX_POINT('',#196150);
#38154=VERTEX_POINT('',#196151);
#38155=VERTEX_POINT('',#196159);
#38156=VERTEX_POINT('',#196160);
#38157=VERTEX_POINT('',#196162);
#38158=VERTEX_POINT('',#196164);
#38159=VERTEX_POINT('',#196168);
#38160=VERTEX_POINT('',#196169);
#38161=VERTEX_POINT('',#196174);
#38162=VERTEX_POINT('',#196175);
#38163=VERTEX_POINT('',#196183);
#38164=VERTEX_POINT('',#196184);
#38165=VERTEX_POINT('',#196186);
#38166=VERTEX_POINT('',#196188);
#38167=VERTEX_POINT('',#196192);
#38168=VERTEX_POINT('',#196193);
#38169=VERTEX_POINT('',#196198);
#38170=VERTEX_POINT('',#196199);
#38171=VERTEX_POINT('',#196207);
#38172=VERTEX_POINT('',#196208);
#38173=VERTEX_POINT('',#196210);
#38174=VERTEX_POINT('',#196212);
#38175=VERTEX_POINT('',#196216);
#38176=VERTEX_POINT('',#196217);
#38177=VERTEX_POINT('',#196222);
#38178=VERTEX_POINT('',#196223);
#38179=VERTEX_POINT('',#196231);
#38180=VERTEX_POINT('',#196232);
#38181=VERTEX_POINT('',#196234);
#38182=VERTEX_POINT('',#196236);
#38183=VERTEX_POINT('',#196240);
#38184=VERTEX_POINT('',#196241);
#38185=VERTEX_POINT('',#196246);
#38186=VERTEX_POINT('',#196247);
#38187=VERTEX_POINT('',#196255);
#38188=VERTEX_POINT('',#196256);
#38189=VERTEX_POINT('',#196258);
#38190=VERTEX_POINT('',#196260);
#38191=VERTEX_POINT('',#196264);
#38192=VERTEX_POINT('',#196265);
#38193=VERTEX_POINT('',#196270);
#38194=VERTEX_POINT('',#196271);
#38195=VERTEX_POINT('',#196279);
#38196=VERTEX_POINT('',#196280);
#38197=VERTEX_POINT('',#196282);
#38198=VERTEX_POINT('',#196284);
#38199=VERTEX_POINT('',#196288);
#38200=VERTEX_POINT('',#196289);
#38201=VERTEX_POINT('',#196294);
#38202=VERTEX_POINT('',#196295);
#38203=VERTEX_POINT('',#196303);
#38204=VERTEX_POINT('',#196304);
#38205=VERTEX_POINT('',#196306);
#38206=VERTEX_POINT('',#196308);
#38207=VERTEX_POINT('',#196312);
#38208=VERTEX_POINT('',#196313);
#38209=VERTEX_POINT('',#196318);
#38210=VERTEX_POINT('',#196319);
#38211=VERTEX_POINT('',#196327);
#38212=VERTEX_POINT('',#196328);
#38213=VERTEX_POINT('',#196330);
#38214=VERTEX_POINT('',#196332);
#38215=VERTEX_POINT('',#196336);
#38216=VERTEX_POINT('',#196337);
#38217=VERTEX_POINT('',#196342);
#38218=VERTEX_POINT('',#196343);
#38219=VERTEX_POINT('',#196351);
#38220=VERTEX_POINT('',#196352);
#38221=VERTEX_POINT('',#196354);
#38222=VERTEX_POINT('',#196356);
#38223=VERTEX_POINT('',#196360);
#38224=VERTEX_POINT('',#196361);
#38225=VERTEX_POINT('',#196366);
#38226=VERTEX_POINT('',#196367);
#38227=VERTEX_POINT('',#196375);
#38228=VERTEX_POINT('',#196376);
#38229=VERTEX_POINT('',#196378);
#38230=VERTEX_POINT('',#196380);
#38231=VERTEX_POINT('',#196384);
#38232=VERTEX_POINT('',#196385);
#38233=VERTEX_POINT('',#196390);
#38234=VERTEX_POINT('',#196391);
#38235=VERTEX_POINT('',#196399);
#38236=VERTEX_POINT('',#196400);
#38237=VERTEX_POINT('',#196402);
#38238=VERTEX_POINT('',#196404);
#38239=VERTEX_POINT('',#196408);
#38240=VERTEX_POINT('',#196409);
#38241=VERTEX_POINT('',#196414);
#38242=VERTEX_POINT('',#196415);
#38243=VERTEX_POINT('',#196423);
#38244=VERTEX_POINT('',#196424);
#38245=VERTEX_POINT('',#196426);
#38246=VERTEX_POINT('',#196428);
#38247=VERTEX_POINT('',#196432);
#38248=VERTEX_POINT('',#196433);
#38249=VERTEX_POINT('',#196438);
#38250=VERTEX_POINT('',#196439);
#38251=VERTEX_POINT('',#196447);
#38252=VERTEX_POINT('',#196448);
#38253=VERTEX_POINT('',#196450);
#38254=VERTEX_POINT('',#196452);
#38255=VERTEX_POINT('',#196456);
#38256=VERTEX_POINT('',#196457);
#38257=VERTEX_POINT('',#196462);
#38258=VERTEX_POINT('',#196463);
#38259=VERTEX_POINT('',#196471);
#38260=VERTEX_POINT('',#196472);
#38261=VERTEX_POINT('',#196474);
#38262=VERTEX_POINT('',#196476);
#38263=VERTEX_POINT('',#196480);
#38264=VERTEX_POINT('',#196481);
#38265=VERTEX_POINT('',#196486);
#38266=VERTEX_POINT('',#196487);
#38267=VERTEX_POINT('',#196495);
#38268=VERTEX_POINT('',#196496);
#38269=VERTEX_POINT('',#196498);
#38270=VERTEX_POINT('',#196500);
#38271=VERTEX_POINT('',#196504);
#38272=VERTEX_POINT('',#196505);
#38273=VERTEX_POINT('',#196510);
#38274=VERTEX_POINT('',#196511);
#38275=VERTEX_POINT('',#196519);
#38276=VERTEX_POINT('',#196520);
#38277=VERTEX_POINT('',#196522);
#38278=VERTEX_POINT('',#196524);
#38279=VERTEX_POINT('',#196528);
#38280=VERTEX_POINT('',#196529);
#38281=VERTEX_POINT('',#196534);
#38282=VERTEX_POINT('',#196535);
#38283=VERTEX_POINT('',#196543);
#38284=VERTEX_POINT('',#196544);
#38285=VERTEX_POINT('',#196546);
#38286=VERTEX_POINT('',#196548);
#38287=VERTEX_POINT('',#196552);
#38288=VERTEX_POINT('',#196553);
#38289=VERTEX_POINT('',#196558);
#38290=VERTEX_POINT('',#196559);
#38291=VERTEX_POINT('',#196567);
#38292=VERTEX_POINT('',#196568);
#38293=VERTEX_POINT('',#196570);
#38294=VERTEX_POINT('',#196572);
#38295=VERTEX_POINT('',#196576);
#38296=VERTEX_POINT('',#196577);
#38297=VERTEX_POINT('',#196582);
#38298=VERTEX_POINT('',#196583);
#38299=VERTEX_POINT('',#196591);
#38300=VERTEX_POINT('',#196592);
#38301=VERTEX_POINT('',#196594);
#38302=VERTEX_POINT('',#196596);
#38303=VERTEX_POINT('',#196600);
#38304=VERTEX_POINT('',#196601);
#38305=VERTEX_POINT('',#196606);
#38306=VERTEX_POINT('',#196607);
#38307=VERTEX_POINT('',#196615);
#38308=VERTEX_POINT('',#196616);
#38309=VERTEX_POINT('',#196618);
#38310=VERTEX_POINT('',#196620);
#38311=VERTEX_POINT('',#196624);
#38312=VERTEX_POINT('',#196625);
#38313=VERTEX_POINT('',#196630);
#38314=VERTEX_POINT('',#196631);
#38315=VERTEX_POINT('',#196639);
#38316=VERTEX_POINT('',#196640);
#38317=VERTEX_POINT('',#196642);
#38318=VERTEX_POINT('',#196644);
#38319=VERTEX_POINT('',#196648);
#38320=VERTEX_POINT('',#196649);
#38321=VERTEX_POINT('',#196654);
#38322=VERTEX_POINT('',#196655);
#38323=VERTEX_POINT('',#196663);
#38324=VERTEX_POINT('',#196664);
#38325=VERTEX_POINT('',#196666);
#38326=VERTEX_POINT('',#196668);
#38327=VERTEX_POINT('',#196672);
#38328=VERTEX_POINT('',#196673);
#38329=VERTEX_POINT('',#196678);
#38330=VERTEX_POINT('',#196679);
#38331=VERTEX_POINT('',#196687);
#38332=VERTEX_POINT('',#196688);
#38333=VERTEX_POINT('',#196690);
#38334=VERTEX_POINT('',#196692);
#38335=VERTEX_POINT('',#196696);
#38336=VERTEX_POINT('',#196697);
#38337=VERTEX_POINT('',#196702);
#38338=VERTEX_POINT('',#196703);
#38339=VERTEX_POINT('',#196711);
#38340=VERTEX_POINT('',#196712);
#38341=VERTEX_POINT('',#196714);
#38342=VERTEX_POINT('',#196716);
#38343=VERTEX_POINT('',#196720);
#38344=VERTEX_POINT('',#196721);
#38345=VERTEX_POINT('',#196726);
#38346=VERTEX_POINT('',#196727);
#38347=VERTEX_POINT('',#196735);
#38348=VERTEX_POINT('',#196736);
#38349=VERTEX_POINT('',#196738);
#38350=VERTEX_POINT('',#196740);
#38351=VERTEX_POINT('',#196744);
#38352=VERTEX_POINT('',#196745);
#38353=VERTEX_POINT('',#196750);
#38354=VERTEX_POINT('',#196751);
#38355=VERTEX_POINT('',#196759);
#38356=VERTEX_POINT('',#196760);
#38357=VERTEX_POINT('',#196762);
#38358=VERTEX_POINT('',#196764);
#38359=VERTEX_POINT('',#196768);
#38360=VERTEX_POINT('',#196769);
#38361=VERTEX_POINT('',#196774);
#38362=VERTEX_POINT('',#196775);
#38363=VERTEX_POINT('',#196783);
#38364=VERTEX_POINT('',#196784);
#38365=VERTEX_POINT('',#196786);
#38366=VERTEX_POINT('',#196788);
#38367=VERTEX_POINT('',#196792);
#38368=VERTEX_POINT('',#196793);
#38369=VERTEX_POINT('',#196798);
#38370=VERTEX_POINT('',#196799);
#38371=VERTEX_POINT('',#196807);
#38372=VERTEX_POINT('',#196808);
#38373=VERTEX_POINT('',#196810);
#38374=VERTEX_POINT('',#196812);
#38375=VERTEX_POINT('',#196816);
#38376=VERTEX_POINT('',#196817);
#38377=VERTEX_POINT('',#196822);
#38378=VERTEX_POINT('',#196823);
#38379=VERTEX_POINT('',#196831);
#38380=VERTEX_POINT('',#196832);
#38381=VERTEX_POINT('',#196834);
#38382=VERTEX_POINT('',#196836);
#38383=VERTEX_POINT('',#196840);
#38384=VERTEX_POINT('',#196841);
#38385=VERTEX_POINT('',#196846);
#38386=VERTEX_POINT('',#196847);
#38387=VERTEX_POINT('',#196855);
#38388=VERTEX_POINT('',#196856);
#38389=VERTEX_POINT('',#196858);
#38390=VERTEX_POINT('',#196860);
#38391=VERTEX_POINT('',#196864);
#38392=VERTEX_POINT('',#196865);
#38393=VERTEX_POINT('',#196870);
#38394=VERTEX_POINT('',#196871);
#38395=VERTEX_POINT('',#196879);
#38396=VERTEX_POINT('',#196880);
#38397=VERTEX_POINT('',#196882);
#38398=VERTEX_POINT('',#196884);
#38399=VERTEX_POINT('',#196888);
#38400=VERTEX_POINT('',#196889);
#38401=VERTEX_POINT('',#196894);
#38402=VERTEX_POINT('',#196895);
#38403=VERTEX_POINT('',#196903);
#38404=VERTEX_POINT('',#196904);
#38405=VERTEX_POINT('',#196906);
#38406=VERTEX_POINT('',#196908);
#38407=VERTEX_POINT('',#196912);
#38408=VERTEX_POINT('',#196913);
#38409=VERTEX_POINT('',#196918);
#38410=VERTEX_POINT('',#196919);
#38411=VERTEX_POINT('',#196927);
#38412=VERTEX_POINT('',#196928);
#38413=VERTEX_POINT('',#196930);
#38414=VERTEX_POINT('',#196932);
#38415=VERTEX_POINT('',#196936);
#38416=VERTEX_POINT('',#196937);
#38417=VERTEX_POINT('',#196942);
#38418=VERTEX_POINT('',#196943);
#38419=VERTEX_POINT('',#196951);
#38420=VERTEX_POINT('',#196952);
#38421=VERTEX_POINT('',#196954);
#38422=VERTEX_POINT('',#196956);
#38423=VERTEX_POINT('',#196960);
#38424=VERTEX_POINT('',#196961);
#38425=VERTEX_POINT('',#196966);
#38426=VERTEX_POINT('',#196967);
#38427=VERTEX_POINT('',#196975);
#38428=VERTEX_POINT('',#196976);
#38429=VERTEX_POINT('',#196978);
#38430=VERTEX_POINT('',#196980);
#38431=VERTEX_POINT('',#196984);
#38432=VERTEX_POINT('',#196985);
#38433=VERTEX_POINT('',#196990);
#38434=VERTEX_POINT('',#196991);
#38435=VERTEX_POINT('',#196999);
#38436=VERTEX_POINT('',#197000);
#38437=VERTEX_POINT('',#197002);
#38438=VERTEX_POINT('',#197004);
#38439=VERTEX_POINT('',#197008);
#38440=VERTEX_POINT('',#197009);
#38441=VERTEX_POINT('',#197014);
#38442=VERTEX_POINT('',#197015);
#38443=VERTEX_POINT('',#197023);
#38444=VERTEX_POINT('',#197024);
#38445=VERTEX_POINT('',#197026);
#38446=VERTEX_POINT('',#197028);
#38447=VERTEX_POINT('',#197032);
#38448=VERTEX_POINT('',#197033);
#38449=VERTEX_POINT('',#197038);
#38450=VERTEX_POINT('',#197039);
#38451=VERTEX_POINT('',#197047);
#38452=VERTEX_POINT('',#197048);
#38453=VERTEX_POINT('',#197050);
#38454=VERTEX_POINT('',#197052);
#38455=VERTEX_POINT('',#197056);
#38456=VERTEX_POINT('',#197057);
#38457=VERTEX_POINT('',#197062);
#38458=VERTEX_POINT('',#197063);
#38459=VERTEX_POINT('',#197071);
#38460=VERTEX_POINT('',#197072);
#38461=VERTEX_POINT('',#197074);
#38462=VERTEX_POINT('',#197076);
#38463=VERTEX_POINT('',#197080);
#38464=VERTEX_POINT('',#197081);
#38465=VERTEX_POINT('',#197086);
#38466=VERTEX_POINT('',#197087);
#38467=VERTEX_POINT('',#197095);
#38468=VERTEX_POINT('',#197096);
#38469=VERTEX_POINT('',#197098);
#38470=VERTEX_POINT('',#197100);
#38471=VERTEX_POINT('',#197104);
#38472=VERTEX_POINT('',#197105);
#38473=VERTEX_POINT('',#197110);
#38474=VERTEX_POINT('',#197111);
#38475=VERTEX_POINT('',#197119);
#38476=VERTEX_POINT('',#197120);
#38477=VERTEX_POINT('',#197122);
#38478=VERTEX_POINT('',#197124);
#38479=VERTEX_POINT('',#197128);
#38480=VERTEX_POINT('',#197129);
#38481=VERTEX_POINT('',#197134);
#38482=VERTEX_POINT('',#197135);
#38483=VERTEX_POINT('',#197143);
#38484=VERTEX_POINT('',#197144);
#38485=VERTEX_POINT('',#197146);
#38486=VERTEX_POINT('',#197148);
#38487=VERTEX_POINT('',#197152);
#38488=VERTEX_POINT('',#197153);
#38489=VERTEX_POINT('',#197158);
#38490=VERTEX_POINT('',#197159);
#38491=VERTEX_POINT('',#197167);
#38492=VERTEX_POINT('',#197168);
#38493=VERTEX_POINT('',#197170);
#38494=VERTEX_POINT('',#197172);
#38495=VERTEX_POINT('',#197176);
#38496=VERTEX_POINT('',#197177);
#38497=VERTEX_POINT('',#197182);
#38498=VERTEX_POINT('',#197183);
#38499=VERTEX_POINT('',#197191);
#38500=VERTEX_POINT('',#197192);
#38501=VERTEX_POINT('',#197194);
#38502=VERTEX_POINT('',#197196);
#38503=VERTEX_POINT('',#197200);
#38504=VERTEX_POINT('',#197201);
#38505=VERTEX_POINT('',#197206);
#38506=VERTEX_POINT('',#197207);
#38507=VERTEX_POINT('',#197215);
#38508=VERTEX_POINT('',#197216);
#38509=VERTEX_POINT('',#197218);
#38510=VERTEX_POINT('',#197220);
#38511=VERTEX_POINT('',#197224);
#38512=VERTEX_POINT('',#197225);
#38513=VERTEX_POINT('',#197230);
#38514=VERTEX_POINT('',#197231);
#38515=VERTEX_POINT('',#197239);
#38516=VERTEX_POINT('',#197240);
#38517=VERTEX_POINT('',#197242);
#38518=VERTEX_POINT('',#197244);
#38519=VERTEX_POINT('',#197248);
#38520=VERTEX_POINT('',#197249);
#38521=VERTEX_POINT('',#197254);
#38522=VERTEX_POINT('',#197255);
#38523=VERTEX_POINT('',#197263);
#38524=VERTEX_POINT('',#197264);
#38525=VERTEX_POINT('',#197266);
#38526=VERTEX_POINT('',#197268);
#38527=VERTEX_POINT('',#197272);
#38528=VERTEX_POINT('',#197273);
#38529=VERTEX_POINT('',#197278);
#38530=VERTEX_POINT('',#197279);
#38531=VERTEX_POINT('',#197287);
#38532=VERTEX_POINT('',#197288);
#38533=VERTEX_POINT('',#197290);
#38534=VERTEX_POINT('',#197292);
#38535=VERTEX_POINT('',#197296);
#38536=VERTEX_POINT('',#197297);
#38537=VERTEX_POINT('',#197302);
#38538=VERTEX_POINT('',#197303);
#38539=VERTEX_POINT('',#197311);
#38540=VERTEX_POINT('',#197312);
#38541=VERTEX_POINT('',#197314);
#38542=VERTEX_POINT('',#197316);
#38543=VERTEX_POINT('',#197320);
#38544=VERTEX_POINT('',#197321);
#38545=VERTEX_POINT('',#197326);
#38546=VERTEX_POINT('',#197327);
#38547=VERTEX_POINT('',#197335);
#38548=VERTEX_POINT('',#197336);
#38549=VERTEX_POINT('',#197338);
#38550=VERTEX_POINT('',#197340);
#38551=VERTEX_POINT('',#197344);
#38552=VERTEX_POINT('',#197345);
#38553=VERTEX_POINT('',#197350);
#38554=VERTEX_POINT('',#197351);
#38555=VERTEX_POINT('',#197359);
#38556=VERTEX_POINT('',#197360);
#38557=VERTEX_POINT('',#197362);
#38558=VERTEX_POINT('',#197364);
#38559=VERTEX_POINT('',#197368);
#38560=VERTEX_POINT('',#197369);
#38561=VERTEX_POINT('',#197374);
#38562=VERTEX_POINT('',#197375);
#38563=VERTEX_POINT('',#197383);
#38564=VERTEX_POINT('',#197384);
#38565=VERTEX_POINT('',#197386);
#38566=VERTEX_POINT('',#197388);
#38567=VERTEX_POINT('',#197392);
#38568=VERTEX_POINT('',#197393);
#38569=VERTEX_POINT('',#197398);
#38570=VERTEX_POINT('',#197399);
#38571=VERTEX_POINT('',#197407);
#38572=VERTEX_POINT('',#197408);
#38573=VERTEX_POINT('',#197410);
#38574=VERTEX_POINT('',#197412);
#38575=VERTEX_POINT('',#197416);
#38576=VERTEX_POINT('',#197417);
#38577=VERTEX_POINT('',#197422);
#38578=VERTEX_POINT('',#197423);
#38579=VERTEX_POINT('',#197431);
#38580=VERTEX_POINT('',#197432);
#38581=VERTEX_POINT('',#197434);
#38582=VERTEX_POINT('',#197436);
#38583=VERTEX_POINT('',#197440);
#38584=VERTEX_POINT('',#197441);
#38585=VERTEX_POINT('',#197446);
#38586=VERTEX_POINT('',#197447);
#38587=VERTEX_POINT('',#197455);
#38588=VERTEX_POINT('',#197456);
#38589=VERTEX_POINT('',#197458);
#38590=VERTEX_POINT('',#197460);
#38591=VERTEX_POINT('',#197464);
#38592=VERTEX_POINT('',#197465);
#38593=VERTEX_POINT('',#197470);
#38594=VERTEX_POINT('',#197471);
#38595=VERTEX_POINT('',#197479);
#38596=VERTEX_POINT('',#197480);
#38597=VERTEX_POINT('',#197482);
#38598=VERTEX_POINT('',#197484);
#38599=VERTEX_POINT('',#197488);
#38600=VERTEX_POINT('',#197489);
#38601=VERTEX_POINT('',#197494);
#38602=VERTEX_POINT('',#197495);
#38603=VERTEX_POINT('',#197503);
#38604=VERTEX_POINT('',#197504);
#38605=VERTEX_POINT('',#197506);
#38606=VERTEX_POINT('',#197508);
#38607=VERTEX_POINT('',#197512);
#38608=VERTEX_POINT('',#197513);
#38609=VERTEX_POINT('',#197518);
#38610=VERTEX_POINT('',#197519);
#38611=VERTEX_POINT('',#197527);
#38612=VERTEX_POINT('',#197528);
#38613=VERTEX_POINT('',#197530);
#38614=VERTEX_POINT('',#197532);
#38615=VERTEX_POINT('',#197536);
#38616=VERTEX_POINT('',#197537);
#38617=VERTEX_POINT('',#197542);
#38618=VERTEX_POINT('',#197543);
#38619=VERTEX_POINT('',#197551);
#38620=VERTEX_POINT('',#197552);
#38621=VERTEX_POINT('',#197554);
#38622=VERTEX_POINT('',#197556);
#38623=VERTEX_POINT('',#197560);
#38624=VERTEX_POINT('',#197561);
#38625=VERTEX_POINT('',#197566);
#38626=VERTEX_POINT('',#197567);
#38627=VERTEX_POINT('',#197575);
#38628=VERTEX_POINT('',#197576);
#38629=VERTEX_POINT('',#197578);
#38630=VERTEX_POINT('',#197580);
#38631=VERTEX_POINT('',#197584);
#38632=VERTEX_POINT('',#197585);
#38633=VERTEX_POINT('',#197590);
#38634=VERTEX_POINT('',#197591);
#38635=VERTEX_POINT('',#197599);
#38636=VERTEX_POINT('',#197600);
#38637=VERTEX_POINT('',#197602);
#38638=VERTEX_POINT('',#197604);
#38639=VERTEX_POINT('',#197608);
#38640=VERTEX_POINT('',#197609);
#38641=VERTEX_POINT('',#197614);
#38642=VERTEX_POINT('',#197615);
#38643=VERTEX_POINT('',#197623);
#38644=VERTEX_POINT('',#197624);
#38645=VERTEX_POINT('',#197626);
#38646=VERTEX_POINT('',#197628);
#38647=VERTEX_POINT('',#197632);
#38648=VERTEX_POINT('',#197633);
#38649=VERTEX_POINT('',#197638);
#38650=VERTEX_POINT('',#197639);
#38651=VERTEX_POINT('',#197647);
#38652=VERTEX_POINT('',#197648);
#38653=VERTEX_POINT('',#197650);
#38654=VERTEX_POINT('',#197652);
#38655=VERTEX_POINT('',#197656);
#38656=VERTEX_POINT('',#197657);
#38657=VERTEX_POINT('',#197662);
#38658=VERTEX_POINT('',#197663);
#38659=VERTEX_POINT('',#197671);
#38660=VERTEX_POINT('',#197672);
#38661=VERTEX_POINT('',#197674);
#38662=VERTEX_POINT('',#197676);
#38663=VERTEX_POINT('',#197680);
#38664=VERTEX_POINT('',#197681);
#38665=VERTEX_POINT('',#197686);
#38666=VERTEX_POINT('',#197687);
#38667=VERTEX_POINT('',#197695);
#38668=VERTEX_POINT('',#197696);
#38669=VERTEX_POINT('',#197698);
#38670=VERTEX_POINT('',#197700);
#38671=VERTEX_POINT('',#197704);
#38672=VERTEX_POINT('',#197705);
#38673=VERTEX_POINT('',#197710);
#38674=VERTEX_POINT('',#197711);
#38675=VERTEX_POINT('',#197719);
#38676=VERTEX_POINT('',#197720);
#38677=VERTEX_POINT('',#197722);
#38678=VERTEX_POINT('',#197724);
#38679=VERTEX_POINT('',#197728);
#38680=VERTEX_POINT('',#197729);
#38681=VERTEX_POINT('',#197734);
#38682=VERTEX_POINT('',#197735);
#38683=VERTEX_POINT('',#197743);
#38684=VERTEX_POINT('',#197744);
#38685=VERTEX_POINT('',#197746);
#38686=VERTEX_POINT('',#197748);
#38687=VERTEX_POINT('',#197752);
#38688=VERTEX_POINT('',#197753);
#38689=VERTEX_POINT('',#197758);
#38690=VERTEX_POINT('',#197759);
#38691=VERTEX_POINT('',#197767);
#38692=VERTEX_POINT('',#197768);
#38693=VERTEX_POINT('',#197770);
#38694=VERTEX_POINT('',#197772);
#38695=VERTEX_POINT('',#197776);
#38696=VERTEX_POINT('',#197777);
#38697=VERTEX_POINT('',#197782);
#38698=VERTEX_POINT('',#197783);
#38699=VERTEX_POINT('',#197791);
#38700=VERTEX_POINT('',#197792);
#38701=VERTEX_POINT('',#197794);
#38702=VERTEX_POINT('',#197796);
#38703=VERTEX_POINT('',#197800);
#38704=VERTEX_POINT('',#197801);
#38705=VERTEX_POINT('',#197806);
#38706=VERTEX_POINT('',#197807);
#38707=VERTEX_POINT('',#197815);
#38708=VERTEX_POINT('',#197816);
#38709=VERTEX_POINT('',#197818);
#38710=VERTEX_POINT('',#197820);
#38711=VERTEX_POINT('',#197824);
#38712=VERTEX_POINT('',#197825);
#38713=VERTEX_POINT('',#197830);
#38714=VERTEX_POINT('',#197831);
#38715=VERTEX_POINT('',#197839);
#38716=VERTEX_POINT('',#197840);
#38717=VERTEX_POINT('',#197842);
#38718=VERTEX_POINT('',#197844);
#38719=VERTEX_POINT('',#197848);
#38720=VERTEX_POINT('',#197849);
#38721=VERTEX_POINT('',#197854);
#38722=VERTEX_POINT('',#197855);
#38723=VERTEX_POINT('',#197863);
#38724=VERTEX_POINT('',#197864);
#38725=VERTEX_POINT('',#197866);
#38726=VERTEX_POINT('',#197868);
#38727=VERTEX_POINT('',#197872);
#38728=VERTEX_POINT('',#197873);
#38729=VERTEX_POINT('',#197878);
#38730=VERTEX_POINT('',#197879);
#38731=VERTEX_POINT('',#197887);
#38732=VERTEX_POINT('',#197888);
#38733=VERTEX_POINT('',#197890);
#38734=VERTEX_POINT('',#197892);
#38735=VERTEX_POINT('',#197896);
#38736=VERTEX_POINT('',#197897);
#38737=VERTEX_POINT('',#197902);
#38738=VERTEX_POINT('',#197903);
#38739=VERTEX_POINT('',#197911);
#38740=VERTEX_POINT('',#197912);
#38741=VERTEX_POINT('',#197914);
#38742=VERTEX_POINT('',#197916);
#38743=VERTEX_POINT('',#197920);
#38744=VERTEX_POINT('',#197921);
#38745=VERTEX_POINT('',#197926);
#38746=VERTEX_POINT('',#197927);
#38747=VERTEX_POINT('',#197935);
#38748=VERTEX_POINT('',#197936);
#38749=VERTEX_POINT('',#197938);
#38750=VERTEX_POINT('',#197940);
#38751=VERTEX_POINT('',#197944);
#38752=VERTEX_POINT('',#197945);
#38753=VERTEX_POINT('',#197950);
#38754=VERTEX_POINT('',#197951);
#38755=VERTEX_POINT('',#197959);
#38756=VERTEX_POINT('',#197960);
#38757=VERTEX_POINT('',#197962);
#38758=VERTEX_POINT('',#197964);
#38759=VERTEX_POINT('',#197968);
#38760=VERTEX_POINT('',#197969);
#38761=VERTEX_POINT('',#197974);
#38762=VERTEX_POINT('',#197975);
#38763=VERTEX_POINT('',#197983);
#38764=VERTEX_POINT('',#197984);
#38765=VERTEX_POINT('',#197986);
#38766=VERTEX_POINT('',#197988);
#38767=VERTEX_POINT('',#197992);
#38768=VERTEX_POINT('',#197993);
#38769=VERTEX_POINT('',#197998);
#38770=VERTEX_POINT('',#197999);
#38771=VERTEX_POINT('',#198007);
#38772=VERTEX_POINT('',#198008);
#38773=VERTEX_POINT('',#198010);
#38774=VERTEX_POINT('',#198012);
#38775=VERTEX_POINT('',#198016);
#38776=VERTEX_POINT('',#198017);
#38777=VERTEX_POINT('',#198022);
#38778=VERTEX_POINT('',#198023);
#38779=VERTEX_POINT('',#198031);
#38780=VERTEX_POINT('',#198032);
#38781=VERTEX_POINT('',#198034);
#38782=VERTEX_POINT('',#198036);
#38783=VERTEX_POINT('',#198040);
#38784=VERTEX_POINT('',#198041);
#38785=VERTEX_POINT('',#198046);
#38786=VERTEX_POINT('',#198047);
#38787=VERTEX_POINT('',#198055);
#38788=VERTEX_POINT('',#198056);
#38789=VERTEX_POINT('',#198058);
#38790=VERTEX_POINT('',#198060);
#38791=VERTEX_POINT('',#198064);
#38792=VERTEX_POINT('',#198065);
#38793=VERTEX_POINT('',#198070);
#38794=VERTEX_POINT('',#198071);
#38795=VERTEX_POINT('',#198079);
#38796=VERTEX_POINT('',#198080);
#38797=VERTEX_POINT('',#198082);
#38798=VERTEX_POINT('',#198084);
#38799=VERTEX_POINT('',#198088);
#38800=VERTEX_POINT('',#198089);
#38801=VERTEX_POINT('',#198094);
#38802=VERTEX_POINT('',#198095);
#38803=VERTEX_POINT('',#198103);
#38804=VERTEX_POINT('',#198104);
#38805=VERTEX_POINT('',#198106);
#38806=VERTEX_POINT('',#198108);
#38807=VERTEX_POINT('',#198112);
#38808=VERTEX_POINT('',#198113);
#38809=VERTEX_POINT('',#198118);
#38810=VERTEX_POINT('',#198119);
#38811=VERTEX_POINT('',#198127);
#38812=VERTEX_POINT('',#198128);
#38813=VERTEX_POINT('',#198130);
#38814=VERTEX_POINT('',#198132);
#38815=VERTEX_POINT('',#198136);
#38816=VERTEX_POINT('',#198137);
#38817=VERTEX_POINT('',#198142);
#38818=VERTEX_POINT('',#198143);
#38819=VERTEX_POINT('',#198151);
#38820=VERTEX_POINT('',#198152);
#38821=VERTEX_POINT('',#198154);
#38822=VERTEX_POINT('',#198156);
#38823=VERTEX_POINT('',#198160);
#38824=VERTEX_POINT('',#198161);
#38825=VERTEX_POINT('',#198166);
#38826=VERTEX_POINT('',#198167);
#38827=VERTEX_POINT('',#198175);
#38828=VERTEX_POINT('',#198176);
#38829=VERTEX_POINT('',#198178);
#38830=VERTEX_POINT('',#198180);
#38831=VERTEX_POINT('',#198184);
#38832=VERTEX_POINT('',#198185);
#38833=VERTEX_POINT('',#198190);
#38834=VERTEX_POINT('',#198191);
#38835=VERTEX_POINT('',#198199);
#38836=VERTEX_POINT('',#198200);
#38837=VERTEX_POINT('',#198202);
#38838=VERTEX_POINT('',#198204);
#38839=VERTEX_POINT('',#198208);
#38840=VERTEX_POINT('',#198209);
#38841=VERTEX_POINT('',#198214);
#38842=VERTEX_POINT('',#198215);
#38843=VERTEX_POINT('',#198223);
#38844=VERTEX_POINT('',#198224);
#38845=VERTEX_POINT('',#198226);
#38846=VERTEX_POINT('',#198228);
#38847=VERTEX_POINT('',#198232);
#38848=VERTEX_POINT('',#198233);
#38849=VERTEX_POINT('',#198238);
#38850=VERTEX_POINT('',#198239);
#38851=VERTEX_POINT('',#198247);
#38852=VERTEX_POINT('',#198248);
#38853=VERTEX_POINT('',#198250);
#38854=VERTEX_POINT('',#198252);
#38855=VERTEX_POINT('',#198256);
#38856=VERTEX_POINT('',#198257);
#38857=VERTEX_POINT('',#198262);
#38858=VERTEX_POINT('',#198263);
#38859=VERTEX_POINT('',#198271);
#38860=VERTEX_POINT('',#198272);
#38861=VERTEX_POINT('',#198274);
#38862=VERTEX_POINT('',#198276);
#38863=VERTEX_POINT('',#198280);
#38864=VERTEX_POINT('',#198281);
#38865=VERTEX_POINT('',#198286);
#38866=VERTEX_POINT('',#198287);
#38867=VERTEX_POINT('',#198295);
#38868=VERTEX_POINT('',#198296);
#38869=VERTEX_POINT('',#198298);
#38870=VERTEX_POINT('',#198300);
#38871=VERTEX_POINT('',#198304);
#38872=VERTEX_POINT('',#198305);
#38873=VERTEX_POINT('',#198310);
#38874=VERTEX_POINT('',#198311);
#38875=VERTEX_POINT('',#198319);
#38876=VERTEX_POINT('',#198320);
#38877=VERTEX_POINT('',#198322);
#38878=VERTEX_POINT('',#198324);
#38879=VERTEX_POINT('',#198328);
#38880=VERTEX_POINT('',#198329);
#38881=VERTEX_POINT('',#198334);
#38882=VERTEX_POINT('',#198335);
#38883=VERTEX_POINT('',#198343);
#38884=VERTEX_POINT('',#198344);
#38885=VERTEX_POINT('',#198346);
#38886=VERTEX_POINT('',#198348);
#38887=VERTEX_POINT('',#198352);
#38888=VERTEX_POINT('',#198353);
#38889=VERTEX_POINT('',#198358);
#38890=VERTEX_POINT('',#198359);
#38891=VERTEX_POINT('',#198367);
#38892=VERTEX_POINT('',#198368);
#38893=VERTEX_POINT('',#198370);
#38894=VERTEX_POINT('',#198372);
#38895=VERTEX_POINT('',#198376);
#38896=VERTEX_POINT('',#198377);
#38897=VERTEX_POINT('',#198382);
#38898=VERTEX_POINT('',#198383);
#38899=VERTEX_POINT('',#198391);
#38900=VERTEX_POINT('',#198392);
#38901=VERTEX_POINT('',#198394);
#38902=VERTEX_POINT('',#198396);
#38903=VERTEX_POINT('',#198400);
#38904=VERTEX_POINT('',#198401);
#38905=VERTEX_POINT('',#198406);
#38906=VERTEX_POINT('',#198407);
#38907=VERTEX_POINT('',#198415);
#38908=VERTEX_POINT('',#198416);
#38909=VERTEX_POINT('',#198418);
#38910=VERTEX_POINT('',#198420);
#38911=VERTEX_POINT('',#198424);
#38912=VERTEX_POINT('',#198425);
#38913=VERTEX_POINT('',#198430);
#38914=VERTEX_POINT('',#198431);
#38915=VERTEX_POINT('',#198439);
#38916=VERTEX_POINT('',#198440);
#38917=VERTEX_POINT('',#198442);
#38918=VERTEX_POINT('',#198444);
#38919=VERTEX_POINT('',#198448);
#38920=VERTEX_POINT('',#198449);
#38921=VERTEX_POINT('',#198454);
#38922=VERTEX_POINT('',#198455);
#38923=VERTEX_POINT('',#198463);
#38924=VERTEX_POINT('',#198464);
#38925=VERTEX_POINT('',#198466);
#38926=VERTEX_POINT('',#198468);
#38927=VERTEX_POINT('',#198472);
#38928=VERTEX_POINT('',#198473);
#38929=VERTEX_POINT('',#198478);
#38930=VERTEX_POINT('',#198479);
#38931=VERTEX_POINT('',#198487);
#38932=VERTEX_POINT('',#198488);
#38933=VERTEX_POINT('',#198490);
#38934=VERTEX_POINT('',#198492);
#38935=VERTEX_POINT('',#198496);
#38936=VERTEX_POINT('',#198497);
#38937=VERTEX_POINT('',#198502);
#38938=VERTEX_POINT('',#198503);
#38939=VERTEX_POINT('',#198511);
#38940=VERTEX_POINT('',#198512);
#38941=VERTEX_POINT('',#198514);
#38942=VERTEX_POINT('',#198516);
#38943=VERTEX_POINT('',#198520);
#38944=VERTEX_POINT('',#198521);
#38945=VERTEX_POINT('',#198526);
#38946=VERTEX_POINT('',#198527);
#38947=VERTEX_POINT('',#198535);
#38948=VERTEX_POINT('',#198536);
#38949=VERTEX_POINT('',#198538);
#38950=VERTEX_POINT('',#198540);
#38951=VERTEX_POINT('',#198544);
#38952=VERTEX_POINT('',#198545);
#38953=VERTEX_POINT('',#198550);
#38954=VERTEX_POINT('',#198551);
#38955=VERTEX_POINT('',#198559);
#38956=VERTEX_POINT('',#198560);
#38957=VERTEX_POINT('',#198562);
#38958=VERTEX_POINT('',#198564);
#38959=VERTEX_POINT('',#198568);
#38960=VERTEX_POINT('',#198569);
#38961=VERTEX_POINT('',#198574);
#38962=VERTEX_POINT('',#198575);
#38963=VERTEX_POINT('',#198583);
#38964=VERTEX_POINT('',#198584);
#38965=VERTEX_POINT('',#198586);
#38966=VERTEX_POINT('',#198588);
#38967=VERTEX_POINT('',#198592);
#38968=VERTEX_POINT('',#198593);
#38969=VERTEX_POINT('',#198598);
#38970=VERTEX_POINT('',#198599);
#38971=VERTEX_POINT('',#198607);
#38972=VERTEX_POINT('',#198608);
#38973=VERTEX_POINT('',#198610);
#38974=VERTEX_POINT('',#198612);
#38975=VERTEX_POINT('',#198616);
#38976=VERTEX_POINT('',#198617);
#38977=VERTEX_POINT('',#198622);
#38978=VERTEX_POINT('',#198623);
#38979=VERTEX_POINT('',#198631);
#38980=VERTEX_POINT('',#198632);
#38981=VERTEX_POINT('',#198634);
#38982=VERTEX_POINT('',#198636);
#38983=VERTEX_POINT('',#198640);
#38984=VERTEX_POINT('',#198641);
#38985=VERTEX_POINT('',#198646);
#38986=VERTEX_POINT('',#198647);
#38987=VERTEX_POINT('',#198655);
#38988=VERTEX_POINT('',#198656);
#38989=VERTEX_POINT('',#198658);
#38990=VERTEX_POINT('',#198660);
#38991=VERTEX_POINT('',#198664);
#38992=VERTEX_POINT('',#198665);
#38993=VERTEX_POINT('',#198670);
#38994=VERTEX_POINT('',#198671);
#38995=VERTEX_POINT('',#198679);
#38996=VERTEX_POINT('',#198680);
#38997=VERTEX_POINT('',#198682);
#38998=VERTEX_POINT('',#198684);
#38999=VERTEX_POINT('',#198688);
#39000=VERTEX_POINT('',#198689);
#39001=VERTEX_POINT('',#198694);
#39002=VERTEX_POINT('',#198695);
#39003=VERTEX_POINT('',#198703);
#39004=VERTEX_POINT('',#198704);
#39005=VERTEX_POINT('',#198706);
#39006=VERTEX_POINT('',#198708);
#39007=VERTEX_POINT('',#198712);
#39008=VERTEX_POINT('',#198713);
#39009=VERTEX_POINT('',#198718);
#39010=VERTEX_POINT('',#198719);
#39011=VERTEX_POINT('',#198727);
#39012=VERTEX_POINT('',#198728);
#39013=VERTEX_POINT('',#198730);
#39014=VERTEX_POINT('',#198732);
#39015=VERTEX_POINT('',#198736);
#39016=VERTEX_POINT('',#198737);
#39017=VERTEX_POINT('',#198742);
#39018=VERTEX_POINT('',#198743);
#39019=VERTEX_POINT('',#198751);
#39020=VERTEX_POINT('',#198752);
#39021=VERTEX_POINT('',#198754);
#39022=VERTEX_POINT('',#198756);
#39023=VERTEX_POINT('',#198760);
#39024=VERTEX_POINT('',#198761);
#39025=VERTEX_POINT('',#198766);
#39026=VERTEX_POINT('',#198767);
#39027=VERTEX_POINT('',#198775);
#39028=VERTEX_POINT('',#198776);
#39029=VERTEX_POINT('',#198778);
#39030=VERTEX_POINT('',#198780);
#39031=VERTEX_POINT('',#198784);
#39032=VERTEX_POINT('',#198785);
#39033=VERTEX_POINT('',#198790);
#39034=VERTEX_POINT('',#198791);
#39035=VERTEX_POINT('',#198799);
#39036=VERTEX_POINT('',#198800);
#39037=VERTEX_POINT('',#198802);
#39038=VERTEX_POINT('',#198804);
#39039=VERTEX_POINT('',#198808);
#39040=VERTEX_POINT('',#198809);
#39041=VERTEX_POINT('',#198814);
#39042=VERTEX_POINT('',#198815);
#39043=VERTEX_POINT('',#198823);
#39044=VERTEX_POINT('',#198824);
#39045=VERTEX_POINT('',#198826);
#39046=VERTEX_POINT('',#198828);
#39047=VERTEX_POINT('',#198832);
#39048=VERTEX_POINT('',#198833);
#39049=VERTEX_POINT('',#198838);
#39050=VERTEX_POINT('',#198839);
#39051=VERTEX_POINT('',#198847);
#39052=VERTEX_POINT('',#198848);
#39053=VERTEX_POINT('',#198850);
#39054=VERTEX_POINT('',#198852);
#39055=VERTEX_POINT('',#198856);
#39056=VERTEX_POINT('',#198857);
#39057=VERTEX_POINT('',#198862);
#39058=VERTEX_POINT('',#198863);
#39059=VERTEX_POINT('',#198871);
#39060=VERTEX_POINT('',#198872);
#39061=VERTEX_POINT('',#198874);
#39062=VERTEX_POINT('',#198876);
#39063=VERTEX_POINT('',#198880);
#39064=VERTEX_POINT('',#198881);
#39065=VERTEX_POINT('',#198886);
#39066=VERTEX_POINT('',#198887);
#39067=VERTEX_POINT('',#198895);
#39068=VERTEX_POINT('',#198896);
#39069=VERTEX_POINT('',#198898);
#39070=VERTEX_POINT('',#198900);
#39071=VERTEX_POINT('',#198904);
#39072=VERTEX_POINT('',#198905);
#39073=VERTEX_POINT('',#198910);
#39074=VERTEX_POINT('',#198911);
#39075=VERTEX_POINT('',#198919);
#39076=VERTEX_POINT('',#198920);
#39077=VERTEX_POINT('',#198922);
#39078=VERTEX_POINT('',#198924);
#39079=VERTEX_POINT('',#198928);
#39080=VERTEX_POINT('',#198929);
#39081=VERTEX_POINT('',#198934);
#39082=VERTEX_POINT('',#198935);
#39083=VERTEX_POINT('',#198943);
#39084=VERTEX_POINT('',#198944);
#39085=VERTEX_POINT('',#198946);
#39086=VERTEX_POINT('',#198948);
#39087=VERTEX_POINT('',#198952);
#39088=VERTEX_POINT('',#198953);
#39089=VERTEX_POINT('',#198958);
#39090=VERTEX_POINT('',#198959);
#39091=VERTEX_POINT('',#198967);
#39092=VERTEX_POINT('',#198968);
#39093=VERTEX_POINT('',#198970);
#39094=VERTEX_POINT('',#198972);
#39095=VERTEX_POINT('',#198976);
#39096=VERTEX_POINT('',#198977);
#39097=VERTEX_POINT('',#198982);
#39098=VERTEX_POINT('',#198983);
#39099=VERTEX_POINT('',#198991);
#39100=VERTEX_POINT('',#198992);
#39101=VERTEX_POINT('',#198994);
#39102=VERTEX_POINT('',#198996);
#39103=VERTEX_POINT('',#199000);
#39104=VERTEX_POINT('',#199001);
#39105=VERTEX_POINT('',#199006);
#39106=VERTEX_POINT('',#199007);
#39107=VERTEX_POINT('',#199015);
#39108=VERTEX_POINT('',#199016);
#39109=VERTEX_POINT('',#199018);
#39110=VERTEX_POINT('',#199020);
#39111=VERTEX_POINT('',#199024);
#39112=VERTEX_POINT('',#199025);
#39113=VERTEX_POINT('',#199030);
#39114=VERTEX_POINT('',#199031);
#39115=VERTEX_POINT('',#199039);
#39116=VERTEX_POINT('',#199040);
#39117=VERTEX_POINT('',#199042);
#39118=VERTEX_POINT('',#199044);
#39119=VERTEX_POINT('',#199048);
#39120=VERTEX_POINT('',#199049);
#39121=VERTEX_POINT('',#199054);
#39122=VERTEX_POINT('',#199055);
#39123=VERTEX_POINT('',#199063);
#39124=VERTEX_POINT('',#199064);
#39125=VERTEX_POINT('',#199066);
#39126=VERTEX_POINT('',#199068);
#39127=VERTEX_POINT('',#199072);
#39128=VERTEX_POINT('',#199073);
#39129=VERTEX_POINT('',#199078);
#39130=VERTEX_POINT('',#199079);
#39131=VERTEX_POINT('',#199087);
#39132=VERTEX_POINT('',#199088);
#39133=VERTEX_POINT('',#199090);
#39134=VERTEX_POINT('',#199092);
#39135=VERTEX_POINT('',#199096);
#39136=VERTEX_POINT('',#199097);
#39137=VERTEX_POINT('',#199102);
#39138=VERTEX_POINT('',#199103);
#39139=VERTEX_POINT('',#199111);
#39140=VERTEX_POINT('',#199112);
#39141=VERTEX_POINT('',#199114);
#39142=VERTEX_POINT('',#199116);
#39143=VERTEX_POINT('',#199120);
#39144=VERTEX_POINT('',#199121);
#39145=VERTEX_POINT('',#199126);
#39146=VERTEX_POINT('',#199127);
#39147=VERTEX_POINT('',#199135);
#39148=VERTEX_POINT('',#199136);
#39149=VERTEX_POINT('',#199138);
#39150=VERTEX_POINT('',#199140);
#39151=VERTEX_POINT('',#199144);
#39152=VERTEX_POINT('',#199145);
#39153=VERTEX_POINT('',#199150);
#39154=VERTEX_POINT('',#199151);
#39155=VERTEX_POINT('',#199159);
#39156=VERTEX_POINT('',#199160);
#39157=VERTEX_POINT('',#199162);
#39158=VERTEX_POINT('',#199164);
#39159=VERTEX_POINT('',#199168);
#39160=VERTEX_POINT('',#199169);
#39161=VERTEX_POINT('',#199174);
#39162=VERTEX_POINT('',#199175);
#39163=VERTEX_POINT('',#199183);
#39164=VERTEX_POINT('',#199184);
#39165=VERTEX_POINT('',#199186);
#39166=VERTEX_POINT('',#199188);
#39167=VERTEX_POINT('',#199192);
#39168=VERTEX_POINT('',#199193);
#39169=VERTEX_POINT('',#199198);
#39170=VERTEX_POINT('',#199199);
#39171=VERTEX_POINT('',#199207);
#39172=VERTEX_POINT('',#199208);
#39173=VERTEX_POINT('',#199210);
#39174=VERTEX_POINT('',#199212);
#39175=VERTEX_POINT('',#199216);
#39176=VERTEX_POINT('',#199217);
#39177=VERTEX_POINT('',#199222);
#39178=VERTEX_POINT('',#199223);
#39179=VERTEX_POINT('',#199231);
#39180=VERTEX_POINT('',#199232);
#39181=VERTEX_POINT('',#199234);
#39182=VERTEX_POINT('',#199236);
#39183=VERTEX_POINT('',#199240);
#39184=VERTEX_POINT('',#199241);
#39185=VERTEX_POINT('',#199246);
#39186=VERTEX_POINT('',#199247);
#39187=VERTEX_POINT('',#199255);
#39188=VERTEX_POINT('',#199256);
#39189=VERTEX_POINT('',#199258);
#39190=VERTEX_POINT('',#199260);
#39191=VERTEX_POINT('',#199264);
#39192=VERTEX_POINT('',#199265);
#39193=VERTEX_POINT('',#199270);
#39194=VERTEX_POINT('',#199271);
#39195=VERTEX_POINT('',#199279);
#39196=VERTEX_POINT('',#199280);
#39197=VERTEX_POINT('',#199282);
#39198=VERTEX_POINT('',#199284);
#39199=VERTEX_POINT('',#199288);
#39200=VERTEX_POINT('',#199289);
#39201=VERTEX_POINT('',#199294);
#39202=VERTEX_POINT('',#199295);
#39203=VERTEX_POINT('',#199303);
#39204=VERTEX_POINT('',#199304);
#39205=VERTEX_POINT('',#199306);
#39206=VERTEX_POINT('',#199308);
#39207=VERTEX_POINT('',#199312);
#39208=VERTEX_POINT('',#199313);
#39209=VERTEX_POINT('',#199318);
#39210=VERTEX_POINT('',#199319);
#39211=VERTEX_POINT('',#199327);
#39212=VERTEX_POINT('',#199328);
#39213=VERTEX_POINT('',#199330);
#39214=VERTEX_POINT('',#199332);
#39215=VERTEX_POINT('',#199336);
#39216=VERTEX_POINT('',#199337);
#39217=VERTEX_POINT('',#199342);
#39218=VERTEX_POINT('',#199343);
#39219=VERTEX_POINT('',#199351);
#39220=VERTEX_POINT('',#199352);
#39221=VERTEX_POINT('',#199354);
#39222=VERTEX_POINT('',#199356);
#39223=VERTEX_POINT('',#199360);
#39224=VERTEX_POINT('',#199361);
#39225=VERTEX_POINT('',#199366);
#39226=VERTEX_POINT('',#199367);
#39227=VERTEX_POINT('',#199375);
#39228=VERTEX_POINT('',#199376);
#39229=VERTEX_POINT('',#199378);
#39230=VERTEX_POINT('',#199380);
#39231=VERTEX_POINT('',#199384);
#39232=VERTEX_POINT('',#199385);
#39233=VERTEX_POINT('',#199390);
#39234=VERTEX_POINT('',#199391);
#39235=VERTEX_POINT('',#199399);
#39236=VERTEX_POINT('',#199400);
#39237=VERTEX_POINT('',#199402);
#39238=VERTEX_POINT('',#199404);
#39239=VERTEX_POINT('',#199408);
#39240=VERTEX_POINT('',#199409);
#39241=VERTEX_POINT('',#199414);
#39242=VERTEX_POINT('',#199415);
#39243=VERTEX_POINT('',#199423);
#39244=VERTEX_POINT('',#199424);
#39245=VERTEX_POINT('',#199426);
#39246=VERTEX_POINT('',#199428);
#39247=VERTEX_POINT('',#199432);
#39248=VERTEX_POINT('',#199433);
#39249=VERTEX_POINT('',#199438);
#39250=VERTEX_POINT('',#199439);
#39251=VERTEX_POINT('',#199447);
#39252=VERTEX_POINT('',#199448);
#39253=VERTEX_POINT('',#199450);
#39254=VERTEX_POINT('',#199452);
#39255=VERTEX_POINT('',#199456);
#39256=VERTEX_POINT('',#199457);
#39257=VERTEX_POINT('',#199462);
#39258=VERTEX_POINT('',#199463);
#39259=VERTEX_POINT('',#199471);
#39260=VERTEX_POINT('',#199472);
#39261=VERTEX_POINT('',#199474);
#39262=VERTEX_POINT('',#199476);
#39263=VERTEX_POINT('',#199480);
#39264=VERTEX_POINT('',#199481);
#39265=VERTEX_POINT('',#199486);
#39266=VERTEX_POINT('',#199487);
#39267=VERTEX_POINT('',#199495);
#39268=VERTEX_POINT('',#199496);
#39269=VERTEX_POINT('',#199498);
#39270=VERTEX_POINT('',#199500);
#39271=VERTEX_POINT('',#199504);
#39272=VERTEX_POINT('',#199505);
#39273=VERTEX_POINT('',#199510);
#39274=VERTEX_POINT('',#199511);
#39275=VERTEX_POINT('',#199519);
#39276=VERTEX_POINT('',#199520);
#39277=VERTEX_POINT('',#199522);
#39278=VERTEX_POINT('',#199524);
#39279=VERTEX_POINT('',#199528);
#39280=VERTEX_POINT('',#199529);
#39281=VERTEX_POINT('',#199534);
#39282=VERTEX_POINT('',#199535);
#39283=VERTEX_POINT('',#199543);
#39284=VERTEX_POINT('',#199544);
#39285=VERTEX_POINT('',#199546);
#39286=VERTEX_POINT('',#199548);
#39287=VERTEX_POINT('',#199552);
#39288=VERTEX_POINT('',#199553);
#39289=VERTEX_POINT('',#199558);
#39290=VERTEX_POINT('',#199559);
#39291=VERTEX_POINT('',#199567);
#39292=VERTEX_POINT('',#199568);
#39293=VERTEX_POINT('',#199570);
#39294=VERTEX_POINT('',#199572);
#39295=VERTEX_POINT('',#199576);
#39296=VERTEX_POINT('',#199577);
#39297=VERTEX_POINT('',#199582);
#39298=VERTEX_POINT('',#199583);
#39299=VERTEX_POINT('',#199591);
#39300=VERTEX_POINT('',#199592);
#39301=VERTEX_POINT('',#199594);
#39302=VERTEX_POINT('',#199596);
#39303=VERTEX_POINT('',#199600);
#39304=VERTEX_POINT('',#199601);
#39305=VERTEX_POINT('',#199606);
#39306=VERTEX_POINT('',#199607);
#39307=VERTEX_POINT('',#199615);
#39308=VERTEX_POINT('',#199616);
#39309=VERTEX_POINT('',#199618);
#39310=VERTEX_POINT('',#199620);
#39311=VERTEX_POINT('',#199624);
#39312=VERTEX_POINT('',#199625);
#39313=VERTEX_POINT('',#199630);
#39314=VERTEX_POINT('',#199631);
#39315=VERTEX_POINT('',#199639);
#39316=VERTEX_POINT('',#199640);
#39317=VERTEX_POINT('',#199642);
#39318=VERTEX_POINT('',#199644);
#39319=VERTEX_POINT('',#199648);
#39320=VERTEX_POINT('',#199649);
#39321=VERTEX_POINT('',#199654);
#39322=VERTEX_POINT('',#199655);
#39323=VERTEX_POINT('',#199663);
#39324=VERTEX_POINT('',#199664);
#39325=VERTEX_POINT('',#199666);
#39326=VERTEX_POINT('',#199668);
#39327=VERTEX_POINT('',#199672);
#39328=VERTEX_POINT('',#199673);
#39329=VERTEX_POINT('',#199678);
#39330=VERTEX_POINT('',#199679);
#39331=VERTEX_POINT('',#199687);
#39332=VERTEX_POINT('',#199688);
#39333=VERTEX_POINT('',#199690);
#39334=VERTEX_POINT('',#199692);
#39335=VERTEX_POINT('',#199696);
#39336=VERTEX_POINT('',#199697);
#39337=VERTEX_POINT('',#199702);
#39338=VERTEX_POINT('',#199703);
#39339=VERTEX_POINT('',#199711);
#39340=VERTEX_POINT('',#199712);
#39341=VERTEX_POINT('',#199714);
#39342=VERTEX_POINT('',#199716);
#39343=VERTEX_POINT('',#199720);
#39344=VERTEX_POINT('',#199721);
#39345=VERTEX_POINT('',#199726);
#39346=VERTEX_POINT('',#199727);
#39347=VERTEX_POINT('',#199735);
#39348=VERTEX_POINT('',#199736);
#39349=VERTEX_POINT('',#199738);
#39350=VERTEX_POINT('',#199740);
#39351=VERTEX_POINT('',#199744);
#39352=VERTEX_POINT('',#199745);
#39353=VERTEX_POINT('',#199750);
#39354=VERTEX_POINT('',#199751);
#39355=VERTEX_POINT('',#199759);
#39356=VERTEX_POINT('',#199760);
#39357=VERTEX_POINT('',#199762);
#39358=VERTEX_POINT('',#199764);
#39359=VERTEX_POINT('',#199768);
#39360=VERTEX_POINT('',#199769);
#39361=VERTEX_POINT('',#199774);
#39362=VERTEX_POINT('',#199775);
#39363=VERTEX_POINT('',#199783);
#39364=VERTEX_POINT('',#199784);
#39365=VERTEX_POINT('',#199786);
#39366=VERTEX_POINT('',#199788);
#39367=VERTEX_POINT('',#199792);
#39368=VERTEX_POINT('',#199793);
#39369=VERTEX_POINT('',#199798);
#39370=VERTEX_POINT('',#199799);
#39371=VERTEX_POINT('',#199807);
#39372=VERTEX_POINT('',#199808);
#39373=VERTEX_POINT('',#199810);
#39374=VERTEX_POINT('',#199812);
#39375=VERTEX_POINT('',#199816);
#39376=VERTEX_POINT('',#199817);
#39377=VERTEX_POINT('',#199822);
#39378=VERTEX_POINT('',#199823);
#39379=VERTEX_POINT('',#199831);
#39380=VERTEX_POINT('',#199832);
#39381=VERTEX_POINT('',#199834);
#39382=VERTEX_POINT('',#199836);
#39383=VERTEX_POINT('',#199840);
#39384=VERTEX_POINT('',#199841);
#39385=VERTEX_POINT('',#199846);
#39386=VERTEX_POINT('',#199847);
#39387=VERTEX_POINT('',#199855);
#39388=VERTEX_POINT('',#199856);
#39389=VERTEX_POINT('',#199858);
#39390=VERTEX_POINT('',#199860);
#39391=VERTEX_POINT('',#199864);
#39392=VERTEX_POINT('',#199865);
#39393=VERTEX_POINT('',#199870);
#39394=VERTEX_POINT('',#199871);
#39395=VERTEX_POINT('',#199879);
#39396=VERTEX_POINT('',#199880);
#39397=VERTEX_POINT('',#199882);
#39398=VERTEX_POINT('',#199884);
#39399=VERTEX_POINT('',#199888);
#39400=VERTEX_POINT('',#199889);
#39401=VERTEX_POINT('',#199894);
#39402=VERTEX_POINT('',#199895);
#39403=VERTEX_POINT('',#199903);
#39404=VERTEX_POINT('',#199904);
#39405=VERTEX_POINT('',#199906);
#39406=VERTEX_POINT('',#199908);
#39407=VERTEX_POINT('',#199912);
#39408=VERTEX_POINT('',#199913);
#39409=VERTEX_POINT('',#199918);
#39410=VERTEX_POINT('',#199919);
#39411=VERTEX_POINT('',#199927);
#39412=VERTEX_POINT('',#199928);
#39413=VERTEX_POINT('',#199930);
#39414=VERTEX_POINT('',#199932);
#39415=VERTEX_POINT('',#199936);
#39416=VERTEX_POINT('',#199937);
#39417=VERTEX_POINT('',#199942);
#39418=VERTEX_POINT('',#199943);
#39419=VERTEX_POINT('',#199951);
#39420=VERTEX_POINT('',#199952);
#39421=VERTEX_POINT('',#199954);
#39422=VERTEX_POINT('',#199956);
#39423=VERTEX_POINT('',#199960);
#39424=VERTEX_POINT('',#199961);
#39425=VERTEX_POINT('',#199966);
#39426=VERTEX_POINT('',#199967);
#39427=VERTEX_POINT('',#199975);
#39428=VERTEX_POINT('',#199976);
#39429=VERTEX_POINT('',#199978);
#39430=VERTEX_POINT('',#199980);
#39431=VERTEX_POINT('',#199984);
#39432=VERTEX_POINT('',#199985);
#39433=VERTEX_POINT('',#199990);
#39434=VERTEX_POINT('',#199991);
#39435=VERTEX_POINT('',#199999);
#39436=VERTEX_POINT('',#200000);
#39437=VERTEX_POINT('',#200002);
#39438=VERTEX_POINT('',#200004);
#39439=VERTEX_POINT('',#200008);
#39440=VERTEX_POINT('',#200009);
#39441=VERTEX_POINT('',#200014);
#39442=VERTEX_POINT('',#200015);
#39443=VERTEX_POINT('',#200023);
#39444=VERTEX_POINT('',#200024);
#39445=VERTEX_POINT('',#200026);
#39446=VERTEX_POINT('',#200028);
#39447=VERTEX_POINT('',#200032);
#39448=VERTEX_POINT('',#200033);
#39449=VERTEX_POINT('',#200038);
#39450=VERTEX_POINT('',#200039);
#39451=VERTEX_POINT('',#200047);
#39452=VERTEX_POINT('',#200048);
#39453=VERTEX_POINT('',#200050);
#39454=VERTEX_POINT('',#200052);
#39455=VERTEX_POINT('',#200056);
#39456=VERTEX_POINT('',#200057);
#39457=VERTEX_POINT('',#200062);
#39458=VERTEX_POINT('',#200063);
#39459=VERTEX_POINT('',#200071);
#39460=VERTEX_POINT('',#200072);
#39461=VERTEX_POINT('',#200074);
#39462=VERTEX_POINT('',#200076);
#39463=VERTEX_POINT('',#200080);
#39464=VERTEX_POINT('',#200081);
#39465=VERTEX_POINT('',#200086);
#39466=VERTEX_POINT('',#200087);
#39467=VERTEX_POINT('',#200095);
#39468=VERTEX_POINT('',#200096);
#39469=VERTEX_POINT('',#200098);
#39470=VERTEX_POINT('',#200100);
#39471=VERTEX_POINT('',#200104);
#39472=VERTEX_POINT('',#200105);
#39473=VERTEX_POINT('',#200110);
#39474=VERTEX_POINT('',#200111);
#39475=VERTEX_POINT('',#200119);
#39476=VERTEX_POINT('',#200120);
#39477=VERTEX_POINT('',#200122);
#39478=VERTEX_POINT('',#200124);
#39479=VERTEX_POINT('',#200128);
#39480=VERTEX_POINT('',#200129);
#39481=VERTEX_POINT('',#200134);
#39482=VERTEX_POINT('',#200135);
#39483=VERTEX_POINT('',#200143);
#39484=VERTEX_POINT('',#200144);
#39485=VERTEX_POINT('',#200146);
#39486=VERTEX_POINT('',#200148);
#39487=VERTEX_POINT('',#200152);
#39488=VERTEX_POINT('',#200153);
#39489=VERTEX_POINT('',#200158);
#39490=VERTEX_POINT('',#200159);
#39491=VERTEX_POINT('',#200167);
#39492=VERTEX_POINT('',#200168);
#39493=VERTEX_POINT('',#200170);
#39494=VERTEX_POINT('',#200172);
#39495=VERTEX_POINT('',#200176);
#39496=VERTEX_POINT('',#200177);
#39497=VERTEX_POINT('',#200182);
#39498=VERTEX_POINT('',#200183);
#39499=VERTEX_POINT('',#200191);
#39500=VERTEX_POINT('',#200192);
#39501=VERTEX_POINT('',#200194);
#39502=VERTEX_POINT('',#200196);
#39503=VERTEX_POINT('',#200200);
#39504=VERTEX_POINT('',#200201);
#39505=VERTEX_POINT('',#200206);
#39506=VERTEX_POINT('',#200207);
#39507=VERTEX_POINT('',#200215);
#39508=VERTEX_POINT('',#200216);
#39509=VERTEX_POINT('',#200218);
#39510=VERTEX_POINT('',#200220);
#39511=VERTEX_POINT('',#200224);
#39512=VERTEX_POINT('',#200225);
#39513=VERTEX_POINT('',#200230);
#39514=VERTEX_POINT('',#200231);
#39515=VERTEX_POINT('',#200239);
#39516=VERTEX_POINT('',#200240);
#39517=VERTEX_POINT('',#200242);
#39518=VERTEX_POINT('',#200244);
#39519=VERTEX_POINT('',#200248);
#39520=VERTEX_POINT('',#200249);
#39521=VERTEX_POINT('',#200254);
#39522=VERTEX_POINT('',#200255);
#39523=VERTEX_POINT('',#200263);
#39524=VERTEX_POINT('',#200264);
#39525=VERTEX_POINT('',#200266);
#39526=VERTEX_POINT('',#200268);
#39527=VERTEX_POINT('',#200272);
#39528=VERTEX_POINT('',#200273);
#39529=VERTEX_POINT('',#200278);
#39530=VERTEX_POINT('',#200279);
#39531=VERTEX_POINT('',#200287);
#39532=VERTEX_POINT('',#200288);
#39533=VERTEX_POINT('',#200290);
#39534=VERTEX_POINT('',#200292);
#39535=VERTEX_POINT('',#200296);
#39536=VERTEX_POINT('',#200297);
#39537=VERTEX_POINT('',#200302);
#39538=VERTEX_POINT('',#200303);
#39539=VERTEX_POINT('',#200311);
#39540=VERTEX_POINT('',#200312);
#39541=VERTEX_POINT('',#200314);
#39542=VERTEX_POINT('',#200316);
#39543=VERTEX_POINT('',#200320);
#39544=VERTEX_POINT('',#200321);
#39545=VERTEX_POINT('',#200326);
#39546=VERTEX_POINT('',#200327);
#39547=VERTEX_POINT('',#200335);
#39548=VERTEX_POINT('',#200336);
#39549=VERTEX_POINT('',#200338);
#39550=VERTEX_POINT('',#200340);
#39551=VERTEX_POINT('',#200344);
#39552=VERTEX_POINT('',#200345);
#39553=VERTEX_POINT('',#200350);
#39554=VERTEX_POINT('',#200351);
#39555=VERTEX_POINT('',#200359);
#39556=VERTEX_POINT('',#200360);
#39557=VERTEX_POINT('',#200362);
#39558=VERTEX_POINT('',#200364);
#39559=VERTEX_POINT('',#200368);
#39560=VERTEX_POINT('',#200369);
#39561=VERTEX_POINT('',#200374);
#39562=VERTEX_POINT('',#200375);
#39563=VERTEX_POINT('',#200383);
#39564=VERTEX_POINT('',#200384);
#39565=VERTEX_POINT('',#200386);
#39566=VERTEX_POINT('',#200388);
#39567=VERTEX_POINT('',#200392);
#39568=VERTEX_POINT('',#200393);
#39569=VERTEX_POINT('',#200398);
#39570=VERTEX_POINT('',#200399);
#39571=VERTEX_POINT('',#200407);
#39572=VERTEX_POINT('',#200408);
#39573=VERTEX_POINT('',#200410);
#39574=VERTEX_POINT('',#200412);
#39575=VERTEX_POINT('',#200416);
#39576=VERTEX_POINT('',#200417);
#39577=VERTEX_POINT('',#200422);
#39578=VERTEX_POINT('',#200423);
#39579=VERTEX_POINT('',#200431);
#39580=VERTEX_POINT('',#200432);
#39581=VERTEX_POINT('',#200434);
#39582=VERTEX_POINT('',#200436);
#39583=VERTEX_POINT('',#200440);
#39584=VERTEX_POINT('',#200441);
#39585=VERTEX_POINT('',#200446);
#39586=VERTEX_POINT('',#200447);
#39587=VERTEX_POINT('',#200455);
#39588=VERTEX_POINT('',#200456);
#39589=VERTEX_POINT('',#200458);
#39590=VERTEX_POINT('',#200460);
#39591=VERTEX_POINT('',#200464);
#39592=VERTEX_POINT('',#200465);
#39593=VERTEX_POINT('',#200470);
#39594=VERTEX_POINT('',#200471);
#39595=VERTEX_POINT('',#200479);
#39596=VERTEX_POINT('',#200480);
#39597=VERTEX_POINT('',#200482);
#39598=VERTEX_POINT('',#200484);
#39599=VERTEX_POINT('',#200488);
#39600=VERTEX_POINT('',#200489);
#39601=VERTEX_POINT('',#200494);
#39602=VERTEX_POINT('',#200495);
#39603=VERTEX_POINT('',#200503);
#39604=VERTEX_POINT('',#200504);
#39605=VERTEX_POINT('',#200506);
#39606=VERTEX_POINT('',#200508);
#39607=VERTEX_POINT('',#200512);
#39608=VERTEX_POINT('',#200513);
#39609=VERTEX_POINT('',#200518);
#39610=VERTEX_POINT('',#200519);
#39611=VERTEX_POINT('',#200527);
#39612=VERTEX_POINT('',#200528);
#39613=VERTEX_POINT('',#200530);
#39614=VERTEX_POINT('',#200532);
#39615=VERTEX_POINT('',#200536);
#39616=VERTEX_POINT('',#200537);
#39617=VERTEX_POINT('',#200542);
#39618=VERTEX_POINT('',#200543);
#39619=VERTEX_POINT('',#200551);
#39620=VERTEX_POINT('',#200552);
#39621=VERTEX_POINT('',#200554);
#39622=VERTEX_POINT('',#200556);
#39623=VERTEX_POINT('',#200560);
#39624=VERTEX_POINT('',#200561);
#39625=VERTEX_POINT('',#200566);
#39626=VERTEX_POINT('',#200567);
#39627=VERTEX_POINT('',#200575);
#39628=VERTEX_POINT('',#200576);
#39629=VERTEX_POINT('',#200578);
#39630=VERTEX_POINT('',#200580);
#39631=VERTEX_POINT('',#200584);
#39632=VERTEX_POINT('',#200585);
#39633=VERTEX_POINT('',#200590);
#39634=VERTEX_POINT('',#200591);
#39635=VERTEX_POINT('',#200599);
#39636=VERTEX_POINT('',#200600);
#39637=VERTEX_POINT('',#200602);
#39638=VERTEX_POINT('',#200604);
#39639=VERTEX_POINT('',#200608);
#39640=VERTEX_POINT('',#200609);
#39641=VERTEX_POINT('',#200614);
#39642=VERTEX_POINT('',#200615);
#39643=VERTEX_POINT('',#200623);
#39644=VERTEX_POINT('',#200624);
#39645=VERTEX_POINT('',#200626);
#39646=VERTEX_POINT('',#200628);
#39647=VERTEX_POINT('',#200632);
#39648=VERTEX_POINT('',#200633);
#39649=VERTEX_POINT('',#200638);
#39650=VERTEX_POINT('',#200639);
#39651=VERTEX_POINT('',#200647);
#39652=VERTEX_POINT('',#200648);
#39653=VERTEX_POINT('',#200650);
#39654=VERTEX_POINT('',#200652);
#39655=VERTEX_POINT('',#200656);
#39656=VERTEX_POINT('',#200657);
#39657=VERTEX_POINT('',#200662);
#39658=VERTEX_POINT('',#200663);
#39659=VERTEX_POINT('',#200671);
#39660=VERTEX_POINT('',#200672);
#39661=VERTEX_POINT('',#200674);
#39662=VERTEX_POINT('',#200676);
#39663=VERTEX_POINT('',#200680);
#39664=VERTEX_POINT('',#200681);
#39665=VERTEX_POINT('',#200686);
#39666=VERTEX_POINT('',#200687);
#39667=VERTEX_POINT('',#200695);
#39668=VERTEX_POINT('',#200696);
#39669=VERTEX_POINT('',#200698);
#39670=VERTEX_POINT('',#200700);
#39671=VERTEX_POINT('',#200704);
#39672=VERTEX_POINT('',#200705);
#39673=VERTEX_POINT('',#200710);
#39674=VERTEX_POINT('',#200711);
#39675=VERTEX_POINT('',#200719);
#39676=VERTEX_POINT('',#200720);
#39677=VERTEX_POINT('',#200722);
#39678=VERTEX_POINT('',#200724);
#39679=VERTEX_POINT('',#200728);
#39680=VERTEX_POINT('',#200729);
#39681=VERTEX_POINT('',#200734);
#39682=VERTEX_POINT('',#200735);
#39683=VERTEX_POINT('',#200743);
#39684=VERTEX_POINT('',#200744);
#39685=VERTEX_POINT('',#200746);
#39686=VERTEX_POINT('',#200748);
#39687=VERTEX_POINT('',#200752);
#39688=VERTEX_POINT('',#200753);
#39689=VERTEX_POINT('',#200758);
#39690=VERTEX_POINT('',#200759);
#39691=VERTEX_POINT('',#200767);
#39692=VERTEX_POINT('',#200768);
#39693=VERTEX_POINT('',#200770);
#39694=VERTEX_POINT('',#200772);
#39695=VERTEX_POINT('',#200776);
#39696=VERTEX_POINT('',#200777);
#39697=VERTEX_POINT('',#200782);
#39698=VERTEX_POINT('',#200783);
#39699=VERTEX_POINT('',#200791);
#39700=VERTEX_POINT('',#200792);
#39701=VERTEX_POINT('',#200794);
#39702=VERTEX_POINT('',#200796);
#39703=VERTEX_POINT('',#200800);
#39704=VERTEX_POINT('',#200801);
#39705=VERTEX_POINT('',#200806);
#39706=VERTEX_POINT('',#200807);
#39707=VERTEX_POINT('',#200815);
#39708=VERTEX_POINT('',#200816);
#39709=VERTEX_POINT('',#200818);
#39710=VERTEX_POINT('',#200820);
#39711=VERTEX_POINT('',#200824);
#39712=VERTEX_POINT('',#200825);
#39713=VERTEX_POINT('',#200830);
#39714=VERTEX_POINT('',#200831);
#39715=VERTEX_POINT('',#200839);
#39716=VERTEX_POINT('',#200840);
#39717=VERTEX_POINT('',#200842);
#39718=VERTEX_POINT('',#200844);
#39719=VERTEX_POINT('',#200848);
#39720=VERTEX_POINT('',#200849);
#39721=VERTEX_POINT('',#200854);
#39722=VERTEX_POINT('',#200855);
#39723=VERTEX_POINT('',#200863);
#39724=VERTEX_POINT('',#200864);
#39725=VERTEX_POINT('',#200866);
#39726=VERTEX_POINT('',#200868);
#39727=VERTEX_POINT('',#200872);
#39728=VERTEX_POINT('',#200873);
#39729=VERTEX_POINT('',#200878);
#39730=VERTEX_POINT('',#200879);
#39731=VERTEX_POINT('',#200887);
#39732=VERTEX_POINT('',#200888);
#39733=VERTEX_POINT('',#200890);
#39734=VERTEX_POINT('',#200892);
#39735=VERTEX_POINT('',#200896);
#39736=VERTEX_POINT('',#200897);
#39737=VERTEX_POINT('',#200902);
#39738=VERTEX_POINT('',#200903);
#39739=VERTEX_POINT('',#200911);
#39740=VERTEX_POINT('',#200912);
#39741=VERTEX_POINT('',#200914);
#39742=VERTEX_POINT('',#200916);
#39743=VERTEX_POINT('',#200920);
#39744=VERTEX_POINT('',#200921);
#39745=VERTEX_POINT('',#200926);
#39746=VERTEX_POINT('',#200927);
#39747=VERTEX_POINT('',#200935);
#39748=VERTEX_POINT('',#200936);
#39749=VERTEX_POINT('',#200938);
#39750=VERTEX_POINT('',#200940);
#39751=VERTEX_POINT('',#200944);
#39752=VERTEX_POINT('',#200945);
#39753=VERTEX_POINT('',#200950);
#39754=VERTEX_POINT('',#200951);
#39755=VERTEX_POINT('',#200959);
#39756=VERTEX_POINT('',#200960);
#39757=VERTEX_POINT('',#200962);
#39758=VERTEX_POINT('',#200964);
#39759=VERTEX_POINT('',#200968);
#39760=VERTEX_POINT('',#200969);
#39761=VERTEX_POINT('',#200974);
#39762=VERTEX_POINT('',#200975);
#39763=VERTEX_POINT('',#200983);
#39764=VERTEX_POINT('',#200984);
#39765=VERTEX_POINT('',#200986);
#39766=VERTEX_POINT('',#200988);
#39767=VERTEX_POINT('',#200992);
#39768=VERTEX_POINT('',#200993);
#39769=VERTEX_POINT('',#200998);
#39770=VERTEX_POINT('',#200999);
#39771=VERTEX_POINT('',#201007);
#39772=VERTEX_POINT('',#201008);
#39773=VERTEX_POINT('',#201010);
#39774=VERTEX_POINT('',#201012);
#39775=VERTEX_POINT('',#201016);
#39776=VERTEX_POINT('',#201017);
#39777=VERTEX_POINT('',#201022);
#39778=VERTEX_POINT('',#201023);
#39779=VERTEX_POINT('',#201031);
#39780=VERTEX_POINT('',#201032);
#39781=VERTEX_POINT('',#201034);
#39782=VERTEX_POINT('',#201036);
#39783=VERTEX_POINT('',#201040);
#39784=VERTEX_POINT('',#201041);
#39785=VERTEX_POINT('',#201046);
#39786=VERTEX_POINT('',#201047);
#39787=VERTEX_POINT('',#201055);
#39788=VERTEX_POINT('',#201056);
#39789=VERTEX_POINT('',#201058);
#39790=VERTEX_POINT('',#201060);
#39791=VERTEX_POINT('',#201064);
#39792=VERTEX_POINT('',#201065);
#39793=VERTEX_POINT('',#201070);
#39794=VERTEX_POINT('',#201071);
#39795=VERTEX_POINT('',#201079);
#39796=VERTEX_POINT('',#201080);
#39797=VERTEX_POINT('',#201082);
#39798=VERTEX_POINT('',#201084);
#39799=VERTEX_POINT('',#201088);
#39800=VERTEX_POINT('',#201089);
#39801=VERTEX_POINT('',#201094);
#39802=VERTEX_POINT('',#201095);
#39803=VERTEX_POINT('',#201103);
#39804=VERTEX_POINT('',#201104);
#39805=VERTEX_POINT('',#201106);
#39806=VERTEX_POINT('',#201108);
#39807=VERTEX_POINT('',#201112);
#39808=VERTEX_POINT('',#201113);
#39809=VERTEX_POINT('',#201118);
#39810=VERTEX_POINT('',#201119);
#39811=VERTEX_POINT('',#201127);
#39812=VERTEX_POINT('',#201128);
#39813=VERTEX_POINT('',#201130);
#39814=VERTEX_POINT('',#201132);
#39815=VERTEX_POINT('',#201136);
#39816=VERTEX_POINT('',#201137);
#39817=VERTEX_POINT('',#201142);
#39818=VERTEX_POINT('',#201143);
#39819=VERTEX_POINT('',#201151);
#39820=VERTEX_POINT('',#201152);
#39821=VERTEX_POINT('',#201154);
#39822=VERTEX_POINT('',#201156);
#39823=VERTEX_POINT('',#201160);
#39824=VERTEX_POINT('',#201161);
#39825=VERTEX_POINT('',#201166);
#39826=VERTEX_POINT('',#201167);
#39827=VERTEX_POINT('',#201175);
#39828=VERTEX_POINT('',#201176);
#39829=VERTEX_POINT('',#201178);
#39830=VERTEX_POINT('',#201180);
#39831=VERTEX_POINT('',#201184);
#39832=VERTEX_POINT('',#201185);
#39833=VERTEX_POINT('',#201190);
#39834=VERTEX_POINT('',#201191);
#39835=VERTEX_POINT('',#201199);
#39836=VERTEX_POINT('',#201200);
#39837=VERTEX_POINT('',#201202);
#39838=VERTEX_POINT('',#201204);
#39839=VERTEX_POINT('',#201208);
#39840=VERTEX_POINT('',#201209);
#39841=VERTEX_POINT('',#201214);
#39842=VERTEX_POINT('',#201215);
#39843=VERTEX_POINT('',#201223);
#39844=VERTEX_POINT('',#201224);
#39845=VERTEX_POINT('',#201226);
#39846=VERTEX_POINT('',#201228);
#39847=VERTEX_POINT('',#201232);
#39848=VERTEX_POINT('',#201233);
#39849=VERTEX_POINT('',#201238);
#39850=VERTEX_POINT('',#201239);
#39851=VERTEX_POINT('',#201247);
#39852=VERTEX_POINT('',#201248);
#39853=VERTEX_POINT('',#201250);
#39854=VERTEX_POINT('',#201252);
#39855=VERTEX_POINT('',#201256);
#39856=VERTEX_POINT('',#201257);
#39857=VERTEX_POINT('',#201262);
#39858=VERTEX_POINT('',#201263);
#39859=VERTEX_POINT('',#201271);
#39860=VERTEX_POINT('',#201272);
#39861=VERTEX_POINT('',#201274);
#39862=VERTEX_POINT('',#201276);
#39863=VERTEX_POINT('',#201280);
#39864=VERTEX_POINT('',#201281);
#39865=VERTEX_POINT('',#201286);
#39866=VERTEX_POINT('',#201287);
#39867=VERTEX_POINT('',#201295);
#39868=VERTEX_POINT('',#201296);
#39869=VERTEX_POINT('',#201298);
#39870=VERTEX_POINT('',#201300);
#39871=VERTEX_POINT('',#201304);
#39872=VERTEX_POINT('',#201305);
#39873=VERTEX_POINT('',#201310);
#39874=VERTEX_POINT('',#201311);
#39875=VERTEX_POINT('',#201319);
#39876=VERTEX_POINT('',#201320);
#39877=VERTEX_POINT('',#201322);
#39878=VERTEX_POINT('',#201324);
#39879=VERTEX_POINT('',#201328);
#39880=VERTEX_POINT('',#201329);
#39881=VERTEX_POINT('',#201334);
#39882=VERTEX_POINT('',#201335);
#39883=VERTEX_POINT('',#201343);
#39884=VERTEX_POINT('',#201344);
#39885=VERTEX_POINT('',#201346);
#39886=VERTEX_POINT('',#201348);
#39887=VERTEX_POINT('',#201352);
#39888=VERTEX_POINT('',#201353);
#39889=VERTEX_POINT('',#201358);
#39890=VERTEX_POINT('',#201359);
#39891=VERTEX_POINT('',#201367);
#39892=VERTEX_POINT('',#201368);
#39893=VERTEX_POINT('',#201370);
#39894=VERTEX_POINT('',#201372);
#39895=VERTEX_POINT('',#201376);
#39896=VERTEX_POINT('',#201377);
#39897=VERTEX_POINT('',#201382);
#39898=VERTEX_POINT('',#201383);
#39899=VERTEX_POINT('',#201391);
#39900=VERTEX_POINT('',#201392);
#39901=VERTEX_POINT('',#201394);
#39902=VERTEX_POINT('',#201396);
#39903=VERTEX_POINT('',#201400);
#39904=VERTEX_POINT('',#201401);
#39905=VERTEX_POINT('',#201406);
#39906=VERTEX_POINT('',#201407);
#39907=VERTEX_POINT('',#201415);
#39908=VERTEX_POINT('',#201416);
#39909=VERTEX_POINT('',#201418);
#39910=VERTEX_POINT('',#201420);
#39911=VERTEX_POINT('',#201424);
#39912=VERTEX_POINT('',#201425);
#39913=VERTEX_POINT('',#201430);
#39914=VERTEX_POINT('',#201431);
#39915=VERTEX_POINT('',#201439);
#39916=VERTEX_POINT('',#201440);
#39917=VERTEX_POINT('',#201442);
#39918=VERTEX_POINT('',#201444);
#39919=VERTEX_POINT('',#201448);
#39920=VERTEX_POINT('',#201449);
#39921=VERTEX_POINT('',#201454);
#39922=VERTEX_POINT('',#201455);
#39923=VERTEX_POINT('',#201463);
#39924=VERTEX_POINT('',#201464);
#39925=VERTEX_POINT('',#201466);
#39926=VERTEX_POINT('',#201468);
#39927=VERTEX_POINT('',#201472);
#39928=VERTEX_POINT('',#201473);
#39929=VERTEX_POINT('',#201478);
#39930=VERTEX_POINT('',#201479);
#39931=VERTEX_POINT('',#201487);
#39932=VERTEX_POINT('',#201488);
#39933=VERTEX_POINT('',#201490);
#39934=VERTEX_POINT('',#201492);
#39935=VERTEX_POINT('',#201496);
#39936=VERTEX_POINT('',#201497);
#39937=VERTEX_POINT('',#201502);
#39938=VERTEX_POINT('',#201503);
#39939=VERTEX_POINT('',#201511);
#39940=VERTEX_POINT('',#201512);
#39941=VERTEX_POINT('',#201514);
#39942=VERTEX_POINT('',#201516);
#39943=VERTEX_POINT('',#201520);
#39944=VERTEX_POINT('',#201521);
#39945=VERTEX_POINT('',#201526);
#39946=VERTEX_POINT('',#201527);
#39947=VERTEX_POINT('',#201535);
#39948=VERTEX_POINT('',#201536);
#39949=VERTEX_POINT('',#201538);
#39950=VERTEX_POINT('',#201540);
#39951=VERTEX_POINT('',#201544);
#39952=VERTEX_POINT('',#201545);
#39953=VERTEX_POINT('',#201550);
#39954=VERTEX_POINT('',#201551);
#39955=VERTEX_POINT('',#201559);
#39956=VERTEX_POINT('',#201560);
#39957=VERTEX_POINT('',#201562);
#39958=VERTEX_POINT('',#201564);
#39959=VERTEX_POINT('',#201568);
#39960=VERTEX_POINT('',#201569);
#39961=VERTEX_POINT('',#201574);
#39962=VERTEX_POINT('',#201575);
#39963=VERTEX_POINT('',#201583);
#39964=VERTEX_POINT('',#201584);
#39965=VERTEX_POINT('',#201586);
#39966=VERTEX_POINT('',#201588);
#39967=VERTEX_POINT('',#201592);
#39968=VERTEX_POINT('',#201593);
#39969=VERTEX_POINT('',#201598);
#39970=VERTEX_POINT('',#201599);
#39971=VERTEX_POINT('',#201607);
#39972=VERTEX_POINT('',#201608);
#39973=VERTEX_POINT('',#201610);
#39974=VERTEX_POINT('',#201612);
#39975=VERTEX_POINT('',#201616);
#39976=VERTEX_POINT('',#201617);
#39977=VERTEX_POINT('',#201622);
#39978=VERTEX_POINT('',#201623);
#39979=VERTEX_POINT('',#201631);
#39980=VERTEX_POINT('',#201632);
#39981=VERTEX_POINT('',#201634);
#39982=VERTEX_POINT('',#201636);
#39983=VERTEX_POINT('',#201640);
#39984=VERTEX_POINT('',#201641);
#39985=VERTEX_POINT('',#201646);
#39986=VERTEX_POINT('',#201647);
#39987=VERTEX_POINT('',#201655);
#39988=VERTEX_POINT('',#201656);
#39989=VERTEX_POINT('',#201658);
#39990=VERTEX_POINT('',#201660);
#39991=VERTEX_POINT('',#201664);
#39992=VERTEX_POINT('',#201665);
#39993=VERTEX_POINT('',#201670);
#39994=VERTEX_POINT('',#201671);
#39995=VERTEX_POINT('',#201679);
#39996=VERTEX_POINT('',#201680);
#39997=VERTEX_POINT('',#201682);
#39998=VERTEX_POINT('',#201684);
#39999=VERTEX_POINT('',#201688);
#40000=VERTEX_POINT('',#201689);
#40001=VERTEX_POINT('',#201694);
#40002=VERTEX_POINT('',#201695);
#40003=VERTEX_POINT('',#201703);
#40004=VERTEX_POINT('',#201704);
#40005=VERTEX_POINT('',#201706);
#40006=VERTEX_POINT('',#201708);
#40007=VERTEX_POINT('',#201712);
#40008=VERTEX_POINT('',#201713);
#40009=VERTEX_POINT('',#201718);
#40010=VERTEX_POINT('',#201719);
#40011=VERTEX_POINT('',#201727);
#40012=VERTEX_POINT('',#201728);
#40013=VERTEX_POINT('',#201730);
#40014=VERTEX_POINT('',#201732);
#40015=VERTEX_POINT('',#201736);
#40016=VERTEX_POINT('',#201737);
#40017=VERTEX_POINT('',#201742);
#40018=VERTEX_POINT('',#201743);
#40019=VERTEX_POINT('',#201751);
#40020=VERTEX_POINT('',#201752);
#40021=VERTEX_POINT('',#201754);
#40022=VERTEX_POINT('',#201756);
#40023=VERTEX_POINT('',#201760);
#40024=VERTEX_POINT('',#201761);
#40025=VERTEX_POINT('',#201766);
#40026=VERTEX_POINT('',#201767);
#40027=VERTEX_POINT('',#201775);
#40028=VERTEX_POINT('',#201776);
#40029=VERTEX_POINT('',#201778);
#40030=VERTEX_POINT('',#201780);
#40031=VERTEX_POINT('',#201784);
#40032=VERTEX_POINT('',#201785);
#40033=VERTEX_POINT('',#201790);
#40034=VERTEX_POINT('',#201791);
#40035=VERTEX_POINT('',#201799);
#40036=VERTEX_POINT('',#201800);
#40037=VERTEX_POINT('',#201802);
#40038=VERTEX_POINT('',#201804);
#40039=VERTEX_POINT('',#201808);
#40040=VERTEX_POINT('',#201809);
#40041=VERTEX_POINT('',#201814);
#40042=VERTEX_POINT('',#201815);
#40043=VERTEX_POINT('',#201823);
#40044=VERTEX_POINT('',#201824);
#40045=VERTEX_POINT('',#201826);
#40046=VERTEX_POINT('',#201828);
#40047=VERTEX_POINT('',#201832);
#40048=VERTEX_POINT('',#201833);
#40049=VERTEX_POINT('',#201838);
#40050=VERTEX_POINT('',#201839);
#40051=VERTEX_POINT('',#201847);
#40052=VERTEX_POINT('',#201848);
#40053=VERTEX_POINT('',#201850);
#40054=VERTEX_POINT('',#201852);
#40055=VERTEX_POINT('',#201856);
#40056=VERTEX_POINT('',#201857);
#40057=VERTEX_POINT('',#201862);
#40058=VERTEX_POINT('',#201863);
#40059=VERTEX_POINT('',#201871);
#40060=VERTEX_POINT('',#201872);
#40061=VERTEX_POINT('',#201874);
#40062=VERTEX_POINT('',#201876);
#40063=VERTEX_POINT('',#201880);
#40064=VERTEX_POINT('',#201881);
#40065=VERTEX_POINT('',#201886);
#40066=VERTEX_POINT('',#201887);
#40067=VERTEX_POINT('',#201895);
#40068=VERTEX_POINT('',#201896);
#40069=VERTEX_POINT('',#201898);
#40070=VERTEX_POINT('',#201900);
#40071=VERTEX_POINT('',#201904);
#40072=VERTEX_POINT('',#201905);
#40073=VERTEX_POINT('',#201910);
#40074=VERTEX_POINT('',#201911);
#40075=VERTEX_POINT('',#201919);
#40076=VERTEX_POINT('',#201920);
#40077=VERTEX_POINT('',#201922);
#40078=VERTEX_POINT('',#201924);
#40079=VERTEX_POINT('',#201928);
#40080=VERTEX_POINT('',#201929);
#40081=VERTEX_POINT('',#201934);
#40082=VERTEX_POINT('',#201935);
#40083=VERTEX_POINT('',#201943);
#40084=VERTEX_POINT('',#201944);
#40085=VERTEX_POINT('',#201946);
#40086=VERTEX_POINT('',#201948);
#40087=VERTEX_POINT('',#201952);
#40088=VERTEX_POINT('',#201953);
#40089=VERTEX_POINT('',#201958);
#40090=VERTEX_POINT('',#201959);
#40091=VERTEX_POINT('',#201967);
#40092=VERTEX_POINT('',#201968);
#40093=VERTEX_POINT('',#201970);
#40094=VERTEX_POINT('',#201972);
#40095=VERTEX_POINT('',#201976);
#40096=VERTEX_POINT('',#201977);
#40097=VERTEX_POINT('',#201982);
#40098=VERTEX_POINT('',#201983);
#40099=VERTEX_POINT('',#201991);
#40100=VERTEX_POINT('',#201992);
#40101=VERTEX_POINT('',#201994);
#40102=VERTEX_POINT('',#201996);
#40103=VERTEX_POINT('',#202000);
#40104=VERTEX_POINT('',#202001);
#40105=VERTEX_POINT('',#202006);
#40106=VERTEX_POINT('',#202007);
#40107=VERTEX_POINT('',#202015);
#40108=VERTEX_POINT('',#202016);
#40109=VERTEX_POINT('',#202018);
#40110=VERTEX_POINT('',#202020);
#40111=VERTEX_POINT('',#202024);
#40112=VERTEX_POINT('',#202025);
#40113=VERTEX_POINT('',#202030);
#40114=VERTEX_POINT('',#202031);
#40115=VERTEX_POINT('',#202039);
#40116=VERTEX_POINT('',#202040);
#40117=VERTEX_POINT('',#202042);
#40118=VERTEX_POINT('',#202044);
#40119=VERTEX_POINT('',#202048);
#40120=VERTEX_POINT('',#202049);
#40121=VERTEX_POINT('',#202054);
#40122=VERTEX_POINT('',#202055);
#40123=VERTEX_POINT('',#202063);
#40124=VERTEX_POINT('',#202064);
#40125=VERTEX_POINT('',#202066);
#40126=VERTEX_POINT('',#202068);
#40127=VERTEX_POINT('',#202072);
#40128=VERTEX_POINT('',#202073);
#40129=VERTEX_POINT('',#202078);
#40130=VERTEX_POINT('',#202079);
#40131=VERTEX_POINT('',#202087);
#40132=VERTEX_POINT('',#202088);
#40133=VERTEX_POINT('',#202090);
#40134=VERTEX_POINT('',#202092);
#40135=VERTEX_POINT('',#202096);
#40136=VERTEX_POINT('',#202097);
#40137=VERTEX_POINT('',#202102);
#40138=VERTEX_POINT('',#202103);
#40139=VERTEX_POINT('',#202111);
#40140=VERTEX_POINT('',#202112);
#40141=VERTEX_POINT('',#202114);
#40142=VERTEX_POINT('',#202116);
#40143=VERTEX_POINT('',#202120);
#40144=VERTEX_POINT('',#202121);
#40145=VERTEX_POINT('',#202126);
#40146=VERTEX_POINT('',#202127);
#40147=VERTEX_POINT('',#202135);
#40148=VERTEX_POINT('',#202136);
#40149=VERTEX_POINT('',#202138);
#40150=VERTEX_POINT('',#202140);
#40151=VERTEX_POINT('',#202144);
#40152=VERTEX_POINT('',#202145);
#40153=VERTEX_POINT('',#202150);
#40154=VERTEX_POINT('',#202151);
#40155=VERTEX_POINT('',#202159);
#40156=VERTEX_POINT('',#202160);
#40157=VERTEX_POINT('',#202162);
#40158=VERTEX_POINT('',#202164);
#40159=VERTEX_POINT('',#202168);
#40160=VERTEX_POINT('',#202169);
#40161=VERTEX_POINT('',#202174);
#40162=VERTEX_POINT('',#202175);
#40163=VERTEX_POINT('',#202183);
#40164=VERTEX_POINT('',#202184);
#40165=VERTEX_POINT('',#202186);
#40166=VERTEX_POINT('',#202188);
#40167=VERTEX_POINT('',#202192);
#40168=VERTEX_POINT('',#202193);
#40169=VERTEX_POINT('',#202198);
#40170=VERTEX_POINT('',#202199);
#40171=VERTEX_POINT('',#202207);
#40172=VERTEX_POINT('',#202208);
#40173=VERTEX_POINT('',#202210);
#40174=VERTEX_POINT('',#202212);
#40175=VERTEX_POINT('',#202216);
#40176=VERTEX_POINT('',#202217);
#40177=VERTEX_POINT('',#202222);
#40178=VERTEX_POINT('',#202223);
#40179=VERTEX_POINT('',#202231);
#40180=VERTEX_POINT('',#202232);
#40181=VERTEX_POINT('',#202234);
#40182=VERTEX_POINT('',#202236);
#40183=VERTEX_POINT('',#202240);
#40184=VERTEX_POINT('',#202241);
#40185=VERTEX_POINT('',#202246);
#40186=VERTEX_POINT('',#202247);
#40187=VERTEX_POINT('',#202255);
#40188=VERTEX_POINT('',#202256);
#40189=VERTEX_POINT('',#202258);
#40190=VERTEX_POINT('',#202260);
#40191=VERTEX_POINT('',#202264);
#40192=VERTEX_POINT('',#202265);
#40193=VERTEX_POINT('',#202270);
#40194=VERTEX_POINT('',#202271);
#40195=VERTEX_POINT('',#202279);
#40196=VERTEX_POINT('',#202280);
#40197=VERTEX_POINT('',#202282);
#40198=VERTEX_POINT('',#202284);
#40199=VERTEX_POINT('',#202288);
#40200=VERTEX_POINT('',#202289);
#40201=VERTEX_POINT('',#202294);
#40202=VERTEX_POINT('',#202295);
#40203=VERTEX_POINT('',#202303);
#40204=VERTEX_POINT('',#202304);
#40205=VERTEX_POINT('',#202306);
#40206=VERTEX_POINT('',#202308);
#40207=VERTEX_POINT('',#202312);
#40208=VERTEX_POINT('',#202313);
#40209=VERTEX_POINT('',#202318);
#40210=VERTEX_POINT('',#202319);
#40211=VERTEX_POINT('',#202327);
#40212=VERTEX_POINT('',#202328);
#40213=VERTEX_POINT('',#202330);
#40214=VERTEX_POINT('',#202332);
#40215=VERTEX_POINT('',#202336);
#40216=VERTEX_POINT('',#202337);
#40217=VERTEX_POINT('',#202342);
#40218=VERTEX_POINT('',#202343);
#40219=VERTEX_POINT('',#202351);
#40220=VERTEX_POINT('',#202352);
#40221=VERTEX_POINT('',#202354);
#40222=VERTEX_POINT('',#202356);
#40223=VERTEX_POINT('',#202360);
#40224=VERTEX_POINT('',#202361);
#40225=VERTEX_POINT('',#202366);
#40226=VERTEX_POINT('',#202367);
#40227=VERTEX_POINT('',#202375);
#40228=VERTEX_POINT('',#202376);
#40229=VERTEX_POINT('',#202378);
#40230=VERTEX_POINT('',#202380);
#40231=VERTEX_POINT('',#202384);
#40232=VERTEX_POINT('',#202385);
#40233=VERTEX_POINT('',#202390);
#40234=VERTEX_POINT('',#202391);
#40235=VERTEX_POINT('',#202399);
#40236=VERTEX_POINT('',#202400);
#40237=VERTEX_POINT('',#202402);
#40238=VERTEX_POINT('',#202404);
#40239=VERTEX_POINT('',#202408);
#40240=VERTEX_POINT('',#202409);
#40241=VERTEX_POINT('',#202414);
#40242=VERTEX_POINT('',#202415);
#40243=VERTEX_POINT('',#202423);
#40244=VERTEX_POINT('',#202424);
#40245=VERTEX_POINT('',#202426);
#40246=VERTEX_POINT('',#202428);
#40247=VERTEX_POINT('',#202432);
#40248=VERTEX_POINT('',#202433);
#40249=VERTEX_POINT('',#202438);
#40250=VERTEX_POINT('',#202439);
#40251=VERTEX_POINT('',#202447);
#40252=VERTEX_POINT('',#202448);
#40253=VERTEX_POINT('',#202450);
#40254=VERTEX_POINT('',#202452);
#40255=VERTEX_POINT('',#202456);
#40256=VERTEX_POINT('',#202457);
#40257=VERTEX_POINT('',#202462);
#40258=VERTEX_POINT('',#202463);
#40259=VERTEX_POINT('',#202471);
#40260=VERTEX_POINT('',#202472);
#40261=VERTEX_POINT('',#202474);
#40262=VERTEX_POINT('',#202476);
#40263=VERTEX_POINT('',#202480);
#40264=VERTEX_POINT('',#202481);
#40265=VERTEX_POINT('',#202486);
#40266=VERTEX_POINT('',#202487);
#40267=VERTEX_POINT('',#202495);
#40268=VERTEX_POINT('',#202496);
#40269=VERTEX_POINT('',#202498);
#40270=VERTEX_POINT('',#202500);
#40271=VERTEX_POINT('',#202504);
#40272=VERTEX_POINT('',#202505);
#40273=VERTEX_POINT('',#202510);
#40274=VERTEX_POINT('',#202511);
#40275=VERTEX_POINT('',#202519);
#40276=VERTEX_POINT('',#202520);
#40277=VERTEX_POINT('',#202522);
#40278=VERTEX_POINT('',#202524);
#40279=VERTEX_POINT('',#202528);
#40280=VERTEX_POINT('',#202529);
#40281=VERTEX_POINT('',#202534);
#40282=VERTEX_POINT('',#202535);
#40283=VERTEX_POINT('',#202543);
#40284=VERTEX_POINT('',#202544);
#40285=VERTEX_POINT('',#202546);
#40286=VERTEX_POINT('',#202548);
#40287=VERTEX_POINT('',#202552);
#40288=VERTEX_POINT('',#202553);
#40289=VERTEX_POINT('',#202558);
#40290=VERTEX_POINT('',#202559);
#40291=VERTEX_POINT('',#202567);
#40292=VERTEX_POINT('',#202568);
#40293=VERTEX_POINT('',#202570);
#40294=VERTEX_POINT('',#202572);
#40295=VERTEX_POINT('',#202576);
#40296=VERTEX_POINT('',#202577);
#40297=VERTEX_POINT('',#202582);
#40298=VERTEX_POINT('',#202583);
#40299=VERTEX_POINT('',#202591);
#40300=VERTEX_POINT('',#202592);
#40301=VERTEX_POINT('',#202594);
#40302=VERTEX_POINT('',#202596);
#40303=VERTEX_POINT('',#202600);
#40304=VERTEX_POINT('',#202601);
#40305=VERTEX_POINT('',#202606);
#40306=VERTEX_POINT('',#202607);
#40307=VERTEX_POINT('',#202615);
#40308=VERTEX_POINT('',#202616);
#40309=VERTEX_POINT('',#202618);
#40310=VERTEX_POINT('',#202620);
#40311=VERTEX_POINT('',#202624);
#40312=VERTEX_POINT('',#202625);
#40313=VERTEX_POINT('',#202630);
#40314=VERTEX_POINT('',#202631);
#40315=VERTEX_POINT('',#202639);
#40316=VERTEX_POINT('',#202640);
#40317=VERTEX_POINT('',#202642);
#40318=VERTEX_POINT('',#202644);
#40319=VERTEX_POINT('',#202648);
#40320=VERTEX_POINT('',#202649);
#40321=VERTEX_POINT('',#202654);
#40322=VERTEX_POINT('',#202655);
#40323=VERTEX_POINT('',#202663);
#40324=VERTEX_POINT('',#202664);
#40325=VERTEX_POINT('',#202666);
#40326=VERTEX_POINT('',#202668);
#40327=VERTEX_POINT('',#202672);
#40328=VERTEX_POINT('',#202673);
#40329=VERTEX_POINT('',#202678);
#40330=VERTEX_POINT('',#202679);
#40331=VERTEX_POINT('',#202687);
#40332=VERTEX_POINT('',#202688);
#40333=VERTEX_POINT('',#202690);
#40334=VERTEX_POINT('',#202692);
#40335=VERTEX_POINT('',#202696);
#40336=VERTEX_POINT('',#202697);
#40337=VERTEX_POINT('',#202702);
#40338=VERTEX_POINT('',#202703);
#40339=VERTEX_POINT('',#202711);
#40340=VERTEX_POINT('',#202712);
#40341=VERTEX_POINT('',#202714);
#40342=VERTEX_POINT('',#202716);
#40343=VERTEX_POINT('',#202720);
#40344=VERTEX_POINT('',#202721);
#40345=VERTEX_POINT('',#202726);
#40346=VERTEX_POINT('',#202727);
#40347=VERTEX_POINT('',#202735);
#40348=VERTEX_POINT('',#202736);
#40349=VERTEX_POINT('',#202738);
#40350=VERTEX_POINT('',#202740);
#40351=VERTEX_POINT('',#202744);
#40352=VERTEX_POINT('',#202745);
#40353=VERTEX_POINT('',#202750);
#40354=VERTEX_POINT('',#202751);
#40355=VERTEX_POINT('',#202759);
#40356=VERTEX_POINT('',#202760);
#40357=VERTEX_POINT('',#202762);
#40358=VERTEX_POINT('',#202764);
#40359=VERTEX_POINT('',#202768);
#40360=VERTEX_POINT('',#202769);
#40361=VERTEX_POINT('',#202774);
#40362=VERTEX_POINT('',#202775);
#40363=VERTEX_POINT('',#202783);
#40364=VERTEX_POINT('',#202784);
#40365=VERTEX_POINT('',#202786);
#40366=VERTEX_POINT('',#202788);
#40367=VERTEX_POINT('',#202792);
#40368=VERTEX_POINT('',#202793);
#40369=VERTEX_POINT('',#202798);
#40370=VERTEX_POINT('',#202799);
#40371=VERTEX_POINT('',#202807);
#40372=VERTEX_POINT('',#202808);
#40373=VERTEX_POINT('',#202810);
#40374=VERTEX_POINT('',#202812);
#40375=VERTEX_POINT('',#202816);
#40376=VERTEX_POINT('',#202817);
#40377=VERTEX_POINT('',#202822);
#40378=VERTEX_POINT('',#202823);
#40379=VERTEX_POINT('',#202831);
#40380=VERTEX_POINT('',#202832);
#40381=VERTEX_POINT('',#202834);
#40382=VERTEX_POINT('',#202836);
#40383=VERTEX_POINT('',#202840);
#40384=VERTEX_POINT('',#202841);
#40385=VERTEX_POINT('',#202846);
#40386=VERTEX_POINT('',#202847);
#40387=VERTEX_POINT('',#202855);
#40388=VERTEX_POINT('',#202856);
#40389=VERTEX_POINT('',#202858);
#40390=VERTEX_POINT('',#202860);
#40391=VERTEX_POINT('',#202864);
#40392=VERTEX_POINT('',#202865);
#40393=VERTEX_POINT('',#202870);
#40394=VERTEX_POINT('',#202871);
#40395=VERTEX_POINT('',#202879);
#40396=VERTEX_POINT('',#202880);
#40397=VERTEX_POINT('',#202882);
#40398=VERTEX_POINT('',#202884);
#40399=VERTEX_POINT('',#202888);
#40400=VERTEX_POINT('',#202889);
#40401=VERTEX_POINT('',#202894);
#40402=VERTEX_POINT('',#202895);
#40403=VERTEX_POINT('',#202903);
#40404=VERTEX_POINT('',#202904);
#40405=VERTEX_POINT('',#202906);
#40406=VERTEX_POINT('',#202908);
#40407=VERTEX_POINT('',#202912);
#40408=VERTEX_POINT('',#202913);
#40409=VERTEX_POINT('',#202918);
#40410=VERTEX_POINT('',#202919);
#40411=VERTEX_POINT('',#202927);
#40412=VERTEX_POINT('',#202928);
#40413=VERTEX_POINT('',#202930);
#40414=VERTEX_POINT('',#202932);
#40415=VERTEX_POINT('',#202936);
#40416=VERTEX_POINT('',#202937);
#40417=VERTEX_POINT('',#202942);
#40418=VERTEX_POINT('',#202943);
#40419=VERTEX_POINT('',#202951);
#40420=VERTEX_POINT('',#202952);
#40421=VERTEX_POINT('',#202954);
#40422=VERTEX_POINT('',#202956);
#40423=VERTEX_POINT('',#202960);
#40424=VERTEX_POINT('',#202961);
#40425=VERTEX_POINT('',#202966);
#40426=VERTEX_POINT('',#202967);
#40427=VERTEX_POINT('',#202975);
#40428=VERTEX_POINT('',#202976);
#40429=VERTEX_POINT('',#202978);
#40430=VERTEX_POINT('',#202980);
#40431=VERTEX_POINT('',#202984);
#40432=VERTEX_POINT('',#202985);
#40433=VERTEX_POINT('',#202990);
#40434=VERTEX_POINT('',#202991);
#40435=VERTEX_POINT('',#202999);
#40436=VERTEX_POINT('',#203000);
#40437=VERTEX_POINT('',#203002);
#40438=VERTEX_POINT('',#203004);
#40439=VERTEX_POINT('',#203008);
#40440=VERTEX_POINT('',#203009);
#40441=VERTEX_POINT('',#203014);
#40442=VERTEX_POINT('',#203015);
#40443=VERTEX_POINT('',#203023);
#40444=VERTEX_POINT('',#203024);
#40445=VERTEX_POINT('',#203026);
#40446=VERTEX_POINT('',#203028);
#40447=VERTEX_POINT('',#203032);
#40448=VERTEX_POINT('',#203033);
#40449=VERTEX_POINT('',#203038);
#40450=VERTEX_POINT('',#203039);
#40451=VERTEX_POINT('',#203047);
#40452=VERTEX_POINT('',#203048);
#40453=VERTEX_POINT('',#203050);
#40454=VERTEX_POINT('',#203052);
#40455=VERTEX_POINT('',#203056);
#40456=VERTEX_POINT('',#203057);
#40457=VERTEX_POINT('',#203062);
#40458=VERTEX_POINT('',#203063);
#40459=VERTEX_POINT('',#203071);
#40460=VERTEX_POINT('',#203072);
#40461=VERTEX_POINT('',#203074);
#40462=VERTEX_POINT('',#203076);
#40463=VERTEX_POINT('',#203080);
#40464=VERTEX_POINT('',#203081);
#40465=VERTEX_POINT('',#203086);
#40466=VERTEX_POINT('',#203087);
#40467=VERTEX_POINT('',#203095);
#40468=VERTEX_POINT('',#203096);
#40469=VERTEX_POINT('',#203098);
#40470=VERTEX_POINT('',#203100);
#40471=VERTEX_POINT('',#203104);
#40472=VERTEX_POINT('',#203105);
#40473=VERTEX_POINT('',#203110);
#40474=VERTEX_POINT('',#203111);
#40475=VERTEX_POINT('',#203119);
#40476=VERTEX_POINT('',#203120);
#40477=VERTEX_POINT('',#203122);
#40478=VERTEX_POINT('',#203124);
#40479=VERTEX_POINT('',#203128);
#40480=VERTEX_POINT('',#203129);
#40481=VERTEX_POINT('',#203134);
#40482=VERTEX_POINT('',#203135);
#40483=VERTEX_POINT('',#203143);
#40484=VERTEX_POINT('',#203144);
#40485=VERTEX_POINT('',#203146);
#40486=VERTEX_POINT('',#203148);
#40487=VERTEX_POINT('',#203152);
#40488=VERTEX_POINT('',#203153);
#40489=VERTEX_POINT('',#203158);
#40490=VERTEX_POINT('',#203159);
#40491=VERTEX_POINT('',#203167);
#40492=VERTEX_POINT('',#203168);
#40493=VERTEX_POINT('',#203170);
#40494=VERTEX_POINT('',#203172);
#40495=VERTEX_POINT('',#203176);
#40496=VERTEX_POINT('',#203177);
#40497=VERTEX_POINT('',#203182);
#40498=VERTEX_POINT('',#203183);
#40499=VERTEX_POINT('',#203191);
#40500=VERTEX_POINT('',#203192);
#40501=VERTEX_POINT('',#203194);
#40502=VERTEX_POINT('',#203196);
#40503=VERTEX_POINT('',#203200);
#40504=VERTEX_POINT('',#203201);
#40505=VERTEX_POINT('',#203206);
#40506=VERTEX_POINT('',#203207);
#40507=VERTEX_POINT('',#203215);
#40508=VERTEX_POINT('',#203216);
#40509=VERTEX_POINT('',#203218);
#40510=VERTEX_POINT('',#203220);
#40511=VERTEX_POINT('',#203224);
#40512=VERTEX_POINT('',#203225);
#40513=VERTEX_POINT('',#203230);
#40514=VERTEX_POINT('',#203231);
#40515=VERTEX_POINT('',#203239);
#40516=VERTEX_POINT('',#203240);
#40517=VERTEX_POINT('',#203242);
#40518=VERTEX_POINT('',#203244);
#40519=VERTEX_POINT('',#203248);
#40520=VERTEX_POINT('',#203249);
#40521=VERTEX_POINT('',#203254);
#40522=VERTEX_POINT('',#203255);
#40523=VERTEX_POINT('',#203263);
#40524=VERTEX_POINT('',#203264);
#40525=VERTEX_POINT('',#203266);
#40526=VERTEX_POINT('',#203268);
#40527=VERTEX_POINT('',#203272);
#40528=VERTEX_POINT('',#203273);
#40529=VERTEX_POINT('',#203278);
#40530=VERTEX_POINT('',#203279);
#40531=VERTEX_POINT('',#203287);
#40532=VERTEX_POINT('',#203288);
#40533=VERTEX_POINT('',#203290);
#40534=VERTEX_POINT('',#203292);
#40535=VERTEX_POINT('',#203296);
#40536=VERTEX_POINT('',#203297);
#40537=VERTEX_POINT('',#203302);
#40538=VERTEX_POINT('',#203303);
#40539=VERTEX_POINT('',#203311);
#40540=VERTEX_POINT('',#203312);
#40541=VERTEX_POINT('',#203314);
#40542=VERTEX_POINT('',#203316);
#40543=VERTEX_POINT('',#203320);
#40544=VERTEX_POINT('',#203321);
#40545=VERTEX_POINT('',#203326);
#40546=VERTEX_POINT('',#203327);
#40547=VERTEX_POINT('',#203335);
#40548=VERTEX_POINT('',#203336);
#40549=VERTEX_POINT('',#203338);
#40550=VERTEX_POINT('',#203340);
#40551=VERTEX_POINT('',#203344);
#40552=VERTEX_POINT('',#203345);
#40553=VERTEX_POINT('',#203350);
#40554=VERTEX_POINT('',#203351);
#40555=VERTEX_POINT('',#203359);
#40556=VERTEX_POINT('',#203360);
#40557=VERTEX_POINT('',#203362);
#40558=VERTEX_POINT('',#203364);
#40559=VERTEX_POINT('',#203368);
#40560=VERTEX_POINT('',#203369);
#40561=VERTEX_POINT('',#203374);
#40562=VERTEX_POINT('',#203375);
#40563=VERTEX_POINT('',#203383);
#40564=VERTEX_POINT('',#203384);
#40565=VERTEX_POINT('',#203386);
#40566=VERTEX_POINT('',#203388);
#40567=VERTEX_POINT('',#203392);
#40568=VERTEX_POINT('',#203393);
#40569=VERTEX_POINT('',#203398);
#40570=VERTEX_POINT('',#203399);
#40571=VERTEX_POINT('',#203407);
#40572=VERTEX_POINT('',#203408);
#40573=VERTEX_POINT('',#203410);
#40574=VERTEX_POINT('',#203412);
#40575=VERTEX_POINT('',#203416);
#40576=VERTEX_POINT('',#203417);
#40577=VERTEX_POINT('',#203422);
#40578=VERTEX_POINT('',#203423);
#40579=VERTEX_POINT('',#203431);
#40580=VERTEX_POINT('',#203432);
#40581=VERTEX_POINT('',#203434);
#40582=VERTEX_POINT('',#203436);
#40583=VERTEX_POINT('',#203440);
#40584=VERTEX_POINT('',#203441);
#40585=VERTEX_POINT('',#203446);
#40586=VERTEX_POINT('',#203447);
#40587=VERTEX_POINT('',#203455);
#40588=VERTEX_POINT('',#203456);
#40589=VERTEX_POINT('',#203458);
#40590=VERTEX_POINT('',#203460);
#40591=VERTEX_POINT('',#203464);
#40592=VERTEX_POINT('',#203465);
#40593=VERTEX_POINT('',#203470);
#40594=VERTEX_POINT('',#203471);
#40595=VERTEX_POINT('',#203479);
#40596=VERTEX_POINT('',#203480);
#40597=VERTEX_POINT('',#203482);
#40598=VERTEX_POINT('',#203484);
#40599=VERTEX_POINT('',#203488);
#40600=VERTEX_POINT('',#203489);
#40601=VERTEX_POINT('',#203494);
#40602=VERTEX_POINT('',#203495);
#40603=VERTEX_POINT('',#203503);
#40604=VERTEX_POINT('',#203504);
#40605=VERTEX_POINT('',#203506);
#40606=VERTEX_POINT('',#203508);
#40607=VERTEX_POINT('',#203512);
#40608=VERTEX_POINT('',#203513);
#40609=VERTEX_POINT('',#203518);
#40610=VERTEX_POINT('',#203519);
#40611=VERTEX_POINT('',#203527);
#40612=VERTEX_POINT('',#203528);
#40613=VERTEX_POINT('',#203530);
#40614=VERTEX_POINT('',#203532);
#40615=VERTEX_POINT('',#203536);
#40616=VERTEX_POINT('',#203537);
#40617=VERTEX_POINT('',#203542);
#40618=VERTEX_POINT('',#203543);
#40619=VERTEX_POINT('',#203551);
#40620=VERTEX_POINT('',#203552);
#40621=VERTEX_POINT('',#203554);
#40622=VERTEX_POINT('',#203556);
#40623=VERTEX_POINT('',#203560);
#40624=VERTEX_POINT('',#203561);
#40625=VERTEX_POINT('',#203566);
#40626=VERTEX_POINT('',#203567);
#40627=VERTEX_POINT('',#203575);
#40628=VERTEX_POINT('',#203576);
#40629=VERTEX_POINT('',#203578);
#40630=VERTEX_POINT('',#203580);
#40631=VERTEX_POINT('',#203584);
#40632=VERTEX_POINT('',#203585);
#40633=VERTEX_POINT('',#203590);
#40634=VERTEX_POINT('',#203591);
#40635=VERTEX_POINT('',#203599);
#40636=VERTEX_POINT('',#203600);
#40637=VERTEX_POINT('',#203602);
#40638=VERTEX_POINT('',#203604);
#40639=VERTEX_POINT('',#203608);
#40640=VERTEX_POINT('',#203609);
#40641=VERTEX_POINT('',#203614);
#40642=VERTEX_POINT('',#203615);
#40643=VERTEX_POINT('',#203623);
#40644=VERTEX_POINT('',#203624);
#40645=VERTEX_POINT('',#203626);
#40646=VERTEX_POINT('',#203628);
#40647=VERTEX_POINT('',#203632);
#40648=VERTEX_POINT('',#203633);
#40649=VERTEX_POINT('',#203638);
#40650=VERTEX_POINT('',#203639);
#40651=VERTEX_POINT('',#203647);
#40652=VERTEX_POINT('',#203648);
#40653=VERTEX_POINT('',#203650);
#40654=VERTEX_POINT('',#203652);
#40655=VERTEX_POINT('',#203656);
#40656=VERTEX_POINT('',#203657);
#40657=VERTEX_POINT('',#203662);
#40658=VERTEX_POINT('',#203663);
#40659=VERTEX_POINT('',#203671);
#40660=VERTEX_POINT('',#203672);
#40661=VERTEX_POINT('',#203674);
#40662=VERTEX_POINT('',#203676);
#40663=VERTEX_POINT('',#203680);
#40664=VERTEX_POINT('',#203681);
#40665=VERTEX_POINT('',#203686);
#40666=VERTEX_POINT('',#203687);
#40667=VERTEX_POINT('',#203695);
#40668=VERTEX_POINT('',#203696);
#40669=VERTEX_POINT('',#203698);
#40670=VERTEX_POINT('',#203700);
#40671=VERTEX_POINT('',#203704);
#40672=VERTEX_POINT('',#203705);
#40673=VERTEX_POINT('',#203710);
#40674=VERTEX_POINT('',#203711);
#40675=VERTEX_POINT('',#203719);
#40676=VERTEX_POINT('',#203720);
#40677=VERTEX_POINT('',#203722);
#40678=VERTEX_POINT('',#203724);
#40679=VERTEX_POINT('',#203728);
#40680=VERTEX_POINT('',#203729);
#40681=VERTEX_POINT('',#203734);
#40682=VERTEX_POINT('',#203735);
#40683=VERTEX_POINT('',#203743);
#40684=VERTEX_POINT('',#203744);
#40685=VERTEX_POINT('',#203746);
#40686=VERTEX_POINT('',#203748);
#40687=VERTEX_POINT('',#203752);
#40688=VERTEX_POINT('',#203753);
#40689=VERTEX_POINT('',#203758);
#40690=VERTEX_POINT('',#203759);
#40691=VERTEX_POINT('',#203767);
#40692=VERTEX_POINT('',#203768);
#40693=VERTEX_POINT('',#203770);
#40694=VERTEX_POINT('',#203772);
#40695=VERTEX_POINT('',#203776);
#40696=VERTEX_POINT('',#203777);
#40697=VERTEX_POINT('',#203782);
#40698=VERTEX_POINT('',#203783);
#40699=VERTEX_POINT('',#203791);
#40700=VERTEX_POINT('',#203792);
#40701=VERTEX_POINT('',#203794);
#40702=VERTEX_POINT('',#203796);
#40703=VERTEX_POINT('',#203800);
#40704=VERTEX_POINT('',#203801);
#40705=VERTEX_POINT('',#203806);
#40706=VERTEX_POINT('',#203807);
#40707=VERTEX_POINT('',#203815);
#40708=VERTEX_POINT('',#203816);
#40709=VERTEX_POINT('',#203818);
#40710=VERTEX_POINT('',#203820);
#40711=VERTEX_POINT('',#203824);
#40712=VERTEX_POINT('',#203825);
#40713=VERTEX_POINT('',#203830);
#40714=VERTEX_POINT('',#203831);
#40715=VERTEX_POINT('',#203839);
#40716=VERTEX_POINT('',#203840);
#40717=VERTEX_POINT('',#203842);
#40718=VERTEX_POINT('',#203844);
#40719=VERTEX_POINT('',#203848);
#40720=VERTEX_POINT('',#203849);
#40721=VERTEX_POINT('',#203854);
#40722=VERTEX_POINT('',#203855);
#40723=VERTEX_POINT('',#203863);
#40724=VERTEX_POINT('',#203864);
#40725=VERTEX_POINT('',#203866);
#40726=VERTEX_POINT('',#203868);
#40727=VERTEX_POINT('',#203872);
#40728=VERTEX_POINT('',#203873);
#40729=VERTEX_POINT('',#203878);
#40730=VERTEX_POINT('',#203879);
#40731=VERTEX_POINT('',#203888);
#40732=VERTEX_POINT('',#203889);
#40733=VERTEX_POINT('',#203891);
#40734=VERTEX_POINT('',#203893);
#40735=VERTEX_POINT('',#203897);
#40736=VERTEX_POINT('',#203899);
#40737=VERTEX_POINT('',#203903);
#40738=VERTEX_POINT('',#203907);
#40739=VERTEX_POINT('',#203935);
#40740=VERTEX_POINT('',#203938);
#40741=VERTEX_POINT('',#203939);
#40742=VERTEX_POINT('',#203941);
#40743=VERTEX_POINT('',#203943);
#40744=VERTEX_POINT('',#203947);
#40745=VERTEX_POINT('',#203949);
#40746=VERTEX_POINT('',#203953);
#40747=VERTEX_POINT('',#203957);
#40748=VERTEX_POINT('',#203963);
#40749=VERTEX_POINT('',#203968);
#40750=VERTEX_POINT('',#203969);
#40751=VERTEX_POINT('',#203971);
#40752=VERTEX_POINT('',#204036);
#40753=VERTEX_POINT('',#204038);
#40754=VERTEX_POINT('',#204041);
#40755=VERTEX_POINT('',#204064);
#40756=VERTEX_POINT('',#204077);
#40757=VERTEX_POINT('',#204088);
#40758=VERTEX_POINT('',#204090);
#40759=VERTEX_POINT('',#204101);
#40760=VERTEX_POINT('',#204139);
#40761=VERTEX_POINT('',#204140);
#40762=VERTEX_POINT('',#204281);
#40763=VERTEX_POINT('',#204282);
#40764=VERTEX_POINT('',#204415);
#40765=VERTEX_POINT('',#204416);
#40766=VERTEX_POINT('',#204418);
#40767=VERTEX_POINT('',#204552);
#40768=VERTEX_POINT('',#204553);
#40769=VERTEX_POINT('',#204623);
#40770=VERTEX_POINT('',#204691);
#40771=VERTEX_POINT('',#204692);
#40772=VERTEX_POINT('',#204829);
#40773=VERTEX_POINT('',#204830);
#40774=VERTEX_POINT('',#204965);
#40775=VERTEX_POINT('',#204966);
#40776=VERTEX_POINT('',#204968);
#40777=VERTEX_POINT('',#205094);
#40778=VERTEX_POINT('',#205095);
#40779=VERTEX_POINT('',#205097);
#40780=VERTEX_POINT('',#205108);
#40781=VERTEX_POINT('',#205109);
#40782=VERTEX_POINT('',#205175);
#40783=VERTEX_POINT('',#205177);
#40784=VERTEX_POINT('',#205182);
#40785=VERTEX_POINT('',#205242);
#40786=VERTEX_POINT('',#205243);
#40787=VERTEX_POINT('',#205245);
#40788=VERTEX_POINT('',#205385);
#40789=VERTEX_POINT('',#205386);
#40790=VERTEX_POINT('',#205466);
#40791=VERTEX_POINT('',#205550);
#40792=VERTEX_POINT('',#205551);
#40793=VERTEX_POINT('',#205710);
#40794=VERTEX_POINT('',#205711);
#40795=VERTEX_POINT('',#205713);
#40796=VERTEX_POINT('',#205877);
#40797=VERTEX_POINT('',#205878);
#40798=VERTEX_POINT('',#205958);
#40799=VERTEX_POINT('',#206042);
#40800=VERTEX_POINT('',#206043);
#40801=VERTEX_POINT('',#206202);
#40802=VERTEX_POINT('',#206203);
#40803=VERTEX_POINT('',#206206);
#40804=VERTEX_POINT('',#206208);
#40805=VERTEX_POINT('',#206215);
#40806=VERTEX_POINT('',#206217);
#40807=VERTEX_POINT('',#206224);
#40808=VERTEX_POINT('',#206226);
#40809=VERTEX_POINT('',#206302);
#40810=VERTEX_POINT('',#206304);
#40811=VERTEX_POINT('',#206309);
#40812=VERTEX_POINT('',#206356);
#40813=VERTEX_POINT('',#206417);
#40814=VERTEX_POINT('',#206418);
#40815=VERTEX_POINT('',#206420);
#40816=VERTEX_POINT('',#206425);
#40817=VERTEX_POINT('',#206438);
#40818=VERTEX_POINT('',#206453);
#40819=VERTEX_POINT('',#206520);
#40820=VERTEX_POINT('',#206587);
#40821=VERTEX_POINT('',#206588);
#40822=VERTEX_POINT('',#206735);
#40823=VERTEX_POINT('',#206736);
#40824=VERTEX_POINT('',#206879);
#40825=VERTEX_POINT('',#206880);
#40826=VERTEX_POINT('',#206882);
#40827=VERTEX_POINT('',#206887);
#40828=VERTEX_POINT('',#206896);
#40829=VERTEX_POINT('',#206907);
#40830=VERTEX_POINT('',#206974);
#40831=VERTEX_POINT('',#207041);
#40832=VERTEX_POINT('',#207042);
#40833=VERTEX_POINT('',#207169);
#40834=VERTEX_POINT('',#207170);
#40835=VERTEX_POINT('',#207315);
#40836=VERTEX_POINT('',#207316);
#40837=VERTEX_POINT('',#207318);
#40838=VERTEX_POINT('',#207323);
#40839=VERTEX_POINT('',#207332);
#40840=VERTEX_POINT('',#207333);
#40841=VERTEX_POINT('',#207335);
#40842=VERTEX_POINT('',#207410);
#40843=VERTEX_POINT('',#207485);
#40844=VERTEX_POINT('',#207486);
#40845=VERTEX_POINT('',#207643);
#40846=VERTEX_POINT('',#207644);
#40847=VERTEX_POINT('',#207801);
#40848=VERTEX_POINT('',#207802);
#40849=VERTEX_POINT('',#207804);
#40850=VERTEX_POINT('',#207809);
#40851=VERTEX_POINT('',#207834);
#40852=VERTEX_POINT('',#207859);
#40853=VERTEX_POINT('',#207936);
#40854=VERTEX_POINT('',#208017);
#40855=VERTEX_POINT('',#208018);
#40856=VERTEX_POINT('',#208179);
#40857=VERTEX_POINT('',#208180);
#40858=VERTEX_POINT('',#208337);
#40859=VERTEX_POINT('',#208338);
#40860=VERTEX_POINT('',#208340);
#40861=VERTEX_POINT('',#208342);
#40862=VERTEX_POINT('',#208347);
#40863=VERTEX_POINT('',#208378);
#40864=VERTEX_POINT('',#208413);
#40865=VERTEX_POINT('',#208453);
#40866=VERTEX_POINT('',#208468);
#40867=VERTEX_POINT('',#208470);
#40868=VERTEX_POINT('',#208491);
#40869=VERTEX_POINT('',#208524);
#40870=VERTEX_POINT('',#208559);
#40871=VERTEX_POINT('',#208560);
#40872=VERTEX_POINT('',#208572);
#40873=VERTEX_POINT('',#208574);
#40874=VERTEX_POINT('',#208586);
#40875=VERTEX_POINT('',#208593);
#40876=VERTEX_POINT('',#208595);
#40877=VERTEX_POINT('',#208664);
#40878=VERTEX_POINT('',#208726);
#40879=VERTEX_POINT('',#208785);
#40880=VERTEX_POINT('',#208847);
#40881=VERTEX_POINT('',#208880);
#40882=VERTEX_POINT('',#208903);
#40883=VERTEX_POINT('',#208908);
#40884=VERTEX_POINT('',#208991);
#40885=VERTEX_POINT('',#209011);
#40886=VERTEX_POINT('',#209295);
#40887=VERTEX_POINT('',#210312);
#40888=VERTEX_POINT('',#210313);
#40889=VERTEX_POINT('',#210315);
#40890=VERTEX_POINT('',#210321);
#40891=VERTEX_POINT('',#210368);
#40892=VERTEX_POINT('',#210388);
#40893=VERTEX_POINT('',#210544);
#40894=VERTEX_POINT('',#210751);
#40895=VERTEX_POINT('',#210837);
#40896=VERTEX_POINT('',#211288);
#40897=VERTEX_POINT('',#212199);
#40898=VERTEX_POINT('',#212620);
#40899=VERTEX_POINT('',#212632);
#40900=VERTEX_POINT('',#212633);
#40901=VERTEX_POINT('',#212635);
#40902=VERTEX_POINT('',#212640);
#40903=VERTEX_POINT('',#212646);
#40904=VERTEX_POINT('',#212649);
#40905=VERTEX_POINT('',#212653);
#40906=VERTEX_POINT('',#212664);
#40907=VERTEX_POINT('',#212669);
#40908=VERTEX_POINT('',#212773);
#40909=VERTEX_POINT('',#212791);
#40910=VERTEX_POINT('',#212792);
#40911=VERTEX_POINT('',#212794);
#40912=VERTEX_POINT('',#212859);
#40913=VERTEX_POINT('',#212861);
#40914=VERTEX_POINT('',#212864);
#40915=VERTEX_POINT('',#212887);
#40916=VERTEX_POINT('',#212900);
#40917=VERTEX_POINT('',#212911);
#40918=VERTEX_POINT('',#212913);
#40919=VERTEX_POINT('',#212924);
#40920=VERTEX_POINT('',#212960);
#40921=VERTEX_POINT('',#212961);
#40922=VERTEX_POINT('',#213100);
#40923=VERTEX_POINT('',#213101);
#40924=VERTEX_POINT('',#213236);
#40925=VERTEX_POINT('',#213237);
#40926=VERTEX_POINT('',#213239);
#40927=VERTEX_POINT('',#213379);
#40928=VERTEX_POINT('',#213380);
#40929=VERTEX_POINT('',#213444);
#40930=VERTEX_POINT('',#213516);
#40931=VERTEX_POINT('',#213517);
#40932=VERTEX_POINT('',#213652);
#40933=VERTEX_POINT('',#213653);
#40934=VERTEX_POINT('',#213788);
#40935=VERTEX_POINT('',#213789);
#40936=VERTEX_POINT('',#213791);
#40937=VERTEX_POINT('',#213915);
#40938=VERTEX_POINT('',#213916);
#40939=VERTEX_POINT('',#213918);
#40940=VERTEX_POINT('',#213929);
#40941=VERTEX_POINT('',#213930);
#40942=VERTEX_POINT('',#213996);
#40943=VERTEX_POINT('',#213998);
#40944=VERTEX_POINT('',#214003);
#40945=VERTEX_POINT('',#214063);
#40946=VERTEX_POINT('',#214064);
#40947=VERTEX_POINT('',#214066);
#40948=VERTEX_POINT('',#214204);
#40949=VERTEX_POINT('',#214205);
#40950=VERTEX_POINT('',#214285);
#40951=VERTEX_POINT('',#214369);
#40952=VERTEX_POINT('',#214370);
#40953=VERTEX_POINT('',#214527);
#40954=VERTEX_POINT('',#214528);
#40955=VERTEX_POINT('',#214530);
#40956=VERTEX_POINT('',#214694);
#40957=VERTEX_POINT('',#214695);
#40958=VERTEX_POINT('',#214775);
#40959=VERTEX_POINT('',#214859);
#40960=VERTEX_POINT('',#214860);
#40961=VERTEX_POINT('',#215019);
#40962=VERTEX_POINT('',#215020);
#40963=VERTEX_POINT('',#215023);
#40964=VERTEX_POINT('',#215025);
#40965=VERTEX_POINT('',#215032);
#40966=VERTEX_POINT('',#215034);
#40967=VERTEX_POINT('',#215041);
#40968=VERTEX_POINT('',#215043);
#40969=VERTEX_POINT('',#215119);
#40970=VERTEX_POINT('',#215121);
#40971=VERTEX_POINT('',#215126);
#40972=VERTEX_POINT('',#215173);
#40973=VERTEX_POINT('',#215234);
#40974=VERTEX_POINT('',#215235);
#40975=VERTEX_POINT('',#215237);
#40976=VERTEX_POINT('',#215242);
#40977=VERTEX_POINT('',#215255);
#40978=VERTEX_POINT('',#215270);
#40979=VERTEX_POINT('',#215341);
#40980=VERTEX_POINT('',#215412);
#40981=VERTEX_POINT('',#215413);
#40982=VERTEX_POINT('',#215562);
#40983=VERTEX_POINT('',#215563);
#40984=VERTEX_POINT('',#215708);
#40985=VERTEX_POINT('',#215709);
#40986=VERTEX_POINT('',#215711);
#40987=VERTEX_POINT('',#215716);
#40988=VERTEX_POINT('',#215725);
#40989=VERTEX_POINT('',#215736);
#40990=VERTEX_POINT('',#215803);
#40991=VERTEX_POINT('',#215876);
#40992=VERTEX_POINT('',#215877);
#40993=VERTEX_POINT('',#216012);
#40994=VERTEX_POINT('',#216013);
#40995=VERTEX_POINT('',#216150);
#40996=VERTEX_POINT('',#216151);
#40997=VERTEX_POINT('',#216153);
#40998=VERTEX_POINT('',#216158);
#40999=VERTEX_POINT('',#216167);
#41000=VERTEX_POINT('',#216168);
#41001=VERTEX_POINT('',#216170);
#41002=VERTEX_POINT('',#216245);
#41003=VERTEX_POINT('',#216320);
#41004=VERTEX_POINT('',#216321);
#41005=VERTEX_POINT('',#216478);
#41006=VERTEX_POINT('',#216479);
#41007=VERTEX_POINT('',#216636);
#41008=VERTEX_POINT('',#216637);
#41009=VERTEX_POINT('',#216639);
#41010=VERTEX_POINT('',#216644);
#41011=VERTEX_POINT('',#216669);
#41012=VERTEX_POINT('',#216694);
#41013=VERTEX_POINT('',#216773);
#41014=VERTEX_POINT('',#216854);
#41015=VERTEX_POINT('',#216855);
#41016=VERTEX_POINT('',#217014);
#41017=VERTEX_POINT('',#217015);
#41018=VERTEX_POINT('',#217174);
#41019=VERTEX_POINT('',#217175);
#41020=VERTEX_POINT('',#217177);
#41021=VERTEX_POINT('',#217179);
#41022=VERTEX_POINT('',#217184);
#41023=VERTEX_POINT('',#217215);
#41024=VERTEX_POINT('',#217250);
#41025=VERTEX_POINT('',#217290);
#41026=VERTEX_POINT('',#217305);
#41027=VERTEX_POINT('',#217307);
#41028=VERTEX_POINT('',#217328);
#41029=VERTEX_POINT('',#217361);
#41030=VERTEX_POINT('',#217396);
#41031=VERTEX_POINT('',#217397);
#41032=VERTEX_POINT('',#217409);
#41033=VERTEX_POINT('',#217411);
#41034=VERTEX_POINT('',#217423);
#41035=VERTEX_POINT('',#217430);
#41036=VERTEX_POINT('',#217432);
#41037=VERTEX_POINT('',#217501);
#41038=VERTEX_POINT('',#217561);
#41039=VERTEX_POINT('',#217616);
#41040=VERTEX_POINT('',#217674);
#41041=VERTEX_POINT('',#217709);
#41042=VERTEX_POINT('',#217732);
#41043=VERTEX_POINT('',#217737);
#41044=VERTEX_POINT('',#217822);
#41045=VERTEX_POINT('',#217842);
#41046=VERTEX_POINT('',#218126);
#41047=VERTEX_POINT('',#219143);
#41048=VERTEX_POINT('',#219144);
#41049=VERTEX_POINT('',#219146);
#41050=VERTEX_POINT('',#219152);
#41051=VERTEX_POINT('',#219199);
#41052=VERTEX_POINT('',#219219);
#41053=VERTEX_POINT('',#219375);
#41054=VERTEX_POINT('',#219580);
#41055=VERTEX_POINT('',#219666);
#41056=VERTEX_POINT('',#220117);
#41057=VERTEX_POINT('',#221030);
#41058=VERTEX_POINT('',#221451);
#41059=VERTEX_POINT('',#221463);
#41060=VERTEX_POINT('',#221464);
#41061=VERTEX_POINT('',#221466);
#41062=VERTEX_POINT('',#221471);
#41063=VERTEX_POINT('',#221477);
#41064=VERTEX_POINT('',#221480);
#41065=VERTEX_POINT('',#221484);
#41066=VERTEX_POINT('',#221495);
#41067=VERTEX_POINT('',#221500);
#41068=VERTEX_POINT('',#221604);
#41069=EDGE_CURVE('',#33580,#33581,#30630,.T.);
#41070=EDGE_CURVE('',#33582,#33581,#30631,.T.);
#41071=EDGE_CURVE('',#33583,#33582,#30632,.T.);
#41072=EDGE_CURVE('',#33580,#33583,#29387,.T.);
#41073=EDGE_CURVE('',#33581,#33584,#2701,.T.);
#41074=EDGE_CURVE('',#33584,#33585,#2702,.T.);
#41075=EDGE_CURVE('',#33585,#33581,#2634,.T.);
#41076=EDGE_CURVE('',#33583,#33586,#29388,.T.);
#41077=EDGE_CURVE('',#33586,#33582,#29389,.T.);
#41078=EDGE_CURVE('',#33587,#33582,#29390,.T.);
#41079=EDGE_CURVE('',#33587,#33586,#29391,.T.);
#41080=EDGE_CURVE('',#33587,#33585,#29392,.T.);
#41081=EDGE_CURVE('',#33584,#33580,#29393,.T.);
#41082=EDGE_CURVE('',#33588,#33589,#30633,.T.);
#41083=EDGE_CURVE('',#33590,#33589,#30634,.T.);
#41084=EDGE_CURVE('',#33591,#33590,#30635,.T.);
#41085=EDGE_CURVE('',#33588,#33591,#29394,.T.);
#41086=EDGE_CURVE('',#33592,#33588,#29395,.T.);
#41087=EDGE_CURVE('',#33589,#33592,#29396,.T.);
#41088=EDGE_CURVE('',#33590,#33593,#2635,.T.);
#41089=EDGE_CURVE('',#33593,#33594,#2703,.T.);
#41090=EDGE_CURVE('',#33594,#33590,#2704,.T.);
#41091=EDGE_CURVE('',#33593,#33595,#29397,.T.);
#41092=EDGE_CURVE('',#33589,#33595,#29398,.T.);
#41093=EDGE_CURVE('',#33592,#33595,#29399,.T.);
#41094=EDGE_CURVE('',#33591,#33594,#29400,.T.);
#41095=EDGE_CURVE('',#33596,#33597,#29401,.T.);
#41096=EDGE_CURVE('',#33596,#33598,#29402,.T.);
#41097=EDGE_CURVE('',#33599,#33598,#30636,.T.);
#41098=EDGE_CURVE('',#33599,#33600,#29403,.T.);
#41099=EDGE_CURVE('',#33601,#33600,#2705,.T.);
#41100=EDGE_CURVE('',#33601,#33602,#29404,.T.);
#41101=EDGE_CURVE('',#33597,#33602,#29405,.T.);
#41102=EDGE_CURVE('',#33603,#33604,#29406,.T.);
#41103=EDGE_CURVE('',#33605,#33604,#29407,.T.);
#41104=EDGE_CURVE('',#33606,#33605,#29408,.T.);
#41105=EDGE_CURVE('',#33606,#33603,#29409,.T.);
#41106=EDGE_CURVE('',#33607,#33605,#29410,.T.);
#41107=EDGE_CURVE('',#33607,#33606,#29411,.T.);
#41108=EDGE_CURVE('',#33599,#33607,#2706,.T.);
#41109=EDGE_CURVE('',#33600,#33605,#2707,.T.);
#41110=EDGE_CURVE('',#33604,#33601,#29412,.T.);
#41111=EDGE_CURVE('',#33603,#33602,#29413,.T.);
#41112=EDGE_CURVE('',#33597,#33603,#30637,.T.);
#41113=EDGE_CURVE('',#33596,#33606,#29414,.T.);
#41114=EDGE_CURVE('',#33598,#33607,#29415,.T.);
#41115=EDGE_CURVE('',#33608,#33609,#30638,.T.);
#41116=EDGE_CURVE('',#33608,#33610,#29416,.T.);
#41117=EDGE_CURVE('',#33611,#33610,#29417,.T.);
#41118=EDGE_CURVE('',#33612,#33611,#29418,.T.);
#41119=EDGE_CURVE('',#33612,#33613,#29419,.T.);
#41120=EDGE_CURVE('',#33614,#33613,#2708,.T.);
#41121=EDGE_CURVE('',#33614,#33609,#29420,.T.);
#41122=EDGE_CURVE('',#33615,#33616,#30639,.T.);
#41123=EDGE_CURVE('',#33617,#33616,#29421,.T.);
#41124=EDGE_CURVE('',#33617,#33615,#29422,.T.);
#41125=EDGE_CURVE('',#33618,#33616,#29423,.T.);
#41126=EDGE_CURVE('',#33619,#33618,#29424,.T.);
#41127=EDGE_CURVE('',#33619,#33617,#29425,.T.);
#41128=EDGE_CURVE('',#33612,#33619,#29426,.T.);
#41129=EDGE_CURVE('',#33613,#33618,#29427,.T.);
#41130=EDGE_CURVE('',#33616,#33614,#2709,.T.);
#41131=EDGE_CURVE('',#33615,#33609,#2710,.T.);
#41132=EDGE_CURVE('',#33611,#33619,#30640,.T.);
#41133=EDGE_CURVE('',#33617,#33610,#29428,.T.);
#41134=EDGE_CURVE('',#33615,#33608,#29429,.T.);
#41135=EDGE_CURVE('',#33620,#33621,#2711,.T.);
#41136=EDGE_CURVE('',#33620,#33622,#29430,.T.);
#41137=EDGE_CURVE('',#33622,#33623,#30641,.T.);
#41138=EDGE_CURVE('',#33623,#33621,#29431,.T.);
#41139=EDGE_CURVE('',#33621,#33624,#29432,.T.);
#41140=EDGE_CURVE('',#33625,#33624,#2712,.T.);
#41141=EDGE_CURVE('',#33625,#33626,#29433,.T.);
#41142=EDGE_CURVE('',#33626,#33627,#29434,.T.);
#41143=EDGE_CURVE('',#33627,#33620,#29435,.T.);
#41144=EDGE_CURVE('',#33628,#33629,#2713,.T.);
#41145=EDGE_CURVE('',#33628,#33625,#29436,.T.);
#41146=EDGE_CURVE('',#33624,#33630,#29437,.T.);
#41147=EDGE_CURVE('',#33630,#33629,#29438,.T.);
#41148=EDGE_CURVE('',#33631,#33632,#2714,.T.);
#41149=EDGE_CURVE('',#33632,#33633,#29439,.T.);
#41150=EDGE_CURVE('',#33634,#33633,#30642,.T.);
#41151=EDGE_CURVE('',#33635,#33634,#29440,.T.);
#41152=EDGE_CURVE('',#33631,#33635,#29441,.F.);
#41153=EDGE_CURVE('',#33636,#33637,#2715,.T.);
#41154=EDGE_CURVE('',#33637,#33632,#29442,.T.);
#41155=EDGE_CURVE('',#33638,#33631,#29443,.F.);
#41156=EDGE_CURVE('',#33638,#33636,#29444,.T.);
#41157=EDGE_CURVE('',#33639,#33640,#2716,.T.);
#41158=EDGE_CURVE('',#33639,#33641,#29445,.T.);
#41159=EDGE_CURVE('',#33641,#33642,#30643,.T.);
#41160=EDGE_CURVE('',#33640,#33642,#29446,.F.);
#41161=EDGE_CURVE('',#33643,#33644,#2717,.T.);
#41162=EDGE_CURVE('',#33644,#33645,#29447,.T.);
#41163=EDGE_CURVE('',#33646,#33645,#2718,.T.);
#41164=EDGE_CURVE('',#33646,#33643,#29448,.T.);
#41165=EDGE_CURVE('',#33647,#33648,#2719,.T.);
#41166=EDGE_CURVE('',#33648,#33644,#29449,.T.);
#41167=EDGE_CURVE('',#33643,#33647,#29450,.T.);
#41168=EDGE_CURVE('',#33649,#33650,#2720,.T.);
#41169=EDGE_CURVE('',#33650,#33648,#29451,.T.);
#41170=EDGE_CURVE('',#33647,#33649,#29452,.T.);
#41171=EDGE_CURVE('',#33651,#33652,#2721,.T.);
#41172=EDGE_CURVE('',#33652,#33650,#29453,.T.);
#41173=EDGE_CURVE('',#33649,#33651,#29454,.T.);
#41174=EDGE_CURVE('',#33653,#33654,#2722,.T.);
#41175=EDGE_CURVE('',#33653,#33655,#30644,.T.);
#41176=EDGE_CURVE('',#33655,#33654,#29455,.T.);
#41177=EDGE_CURVE('',#33656,#33657,#2723,.T.);
#41178=EDGE_CURVE('',#33657,#33658,#29456,.T.);
#41179=EDGE_CURVE('',#33659,#33658,#2724,.T.);
#41180=EDGE_CURVE('',#33659,#33660,#29457,.T.);
#41181=EDGE_CURVE('',#33660,#33661,#2725,.T.);
#41182=EDGE_CURVE('',#33661,#33662,#30645,.T.);
#41183=EDGE_CURVE('',#33662,#33661,#30646,.T.);
#41184=EDGE_CURVE('',#33660,#33656,#29458,.T.);
#41185=EDGE_CURVE('',#33663,#33664,#2726,.T.);
#41186=EDGE_CURVE('',#33664,#33657,#29459,.T.);
#41187=EDGE_CURVE('',#33656,#33663,#29460,.T.);
#41188=EDGE_CURVE('',#33665,#33666,#2727,.T.);
#41189=EDGE_CURVE('',#33665,#33667,#29461,.T.);
#41190=EDGE_CURVE('',#33667,#33668,#30647,.T.);
#41191=EDGE_CURVE('',#33668,#33666,#29462,.T.);
#41192=EDGE_CURVE('',#33669,#33669,#30648,.T.);
#41193=EDGE_CURVE('',#33669,#33670,#30649,.T.);
#41194=EDGE_CURVE('',#33670,#33670,#30650,.T.);
#41195=EDGE_CURVE('',#33671,#33672,#30651,.T.);
#41196=EDGE_CURVE('',#33673,#33671,#29463,.T.);
#41197=EDGE_CURVE('',#33674,#33673,#29464,.T.);
#41198=EDGE_CURVE('',#33675,#33674,#29465,.T.);
#41199=EDGE_CURVE('',#33675,#33676,#29466,.T.);
#41200=EDGE_CURVE('',#33676,#33677,#29467,.T.);
#41201=EDGE_CURVE('',#33678,#33677,#29468,.T.);
#41202=EDGE_CURVE('',#33678,#33679,#29469,.T.);
#41203=EDGE_CURVE('',#33679,#33680,#29470,.T.);
#41204=EDGE_CURVE('',#33681,#33680,#30652,.T.);
#41205=EDGE_CURVE('',#33682,#33681,#29471,.F.);
#41206=EDGE_CURVE('',#33683,#33682,#30653,.T.);
#41207=EDGE_CURVE('',#33683,#33684,#29472,.T.);
#41208=EDGE_CURVE('',#33684,#33685,#29473,.T.);
#41209=EDGE_CURVE('',#33686,#33685,#29474,.T.);
#41210=EDGE_CURVE('',#33686,#33687,#29475,.T.);
#41211=EDGE_CURVE('',#33687,#33688,#29476,.T.);
#41212=EDGE_CURVE('',#33689,#33688,#29477,.T.);
#41213=EDGE_CURVE('',#33690,#33689,#29478,.T.);
#41214=EDGE_CURVE('',#33672,#33690,#29479,.T.);
#41215=EDGE_CURVE('',#33691,#33692,#30654,.T.);
#41216=EDGE_CURVE('',#33692,#33693,#30655,.T.);
#41217=EDGE_CURVE('',#33692,#33694,#30656,.T.);
#41218=EDGE_CURVE('',#33694,#33695,#30657,.T.);
#41219=EDGE_CURVE('',#33691,#33695,#30658,.T.);
#41220=EDGE_CURVE('',#33696,#33697,#30659,.T.);
#41221=EDGE_CURVE('',#33698,#33696,#2728,.T.);
#41222=EDGE_CURVE('',#33699,#33698,#29480,.T.);
#41223=EDGE_CURVE('',#33700,#33699,#29481,.T.);
#41224=EDGE_CURVE('',#33700,#33697,#2729,.T.);
#41225=EDGE_CURVE('',#33701,#33702,#30660,.T.);
#41226=EDGE_CURVE('',#33702,#33703,#29482,.T.);
#41227=EDGE_CURVE('',#33704,#33703,#29483,.T.);
#41228=EDGE_CURVE('',#33705,#33704,#30661,.T.);
#41229=EDGE_CURVE('',#33701,#33705,#30662,.T.);
#41230=EDGE_CURVE('',#33706,#33707,#30663,.T.);
#41231=EDGE_CURVE('',#33707,#33708,#2730,.T.);
#41232=EDGE_CURVE('',#33709,#33708,#30664,.T.);
#41233=EDGE_CURVE('',#33706,#33709,#2731,.T.);
#41234=EDGE_CURVE('',#33710,#33711,#30665,.T.);
#41235=EDGE_CURVE('',#33710,#33712,#2732,.T.);
#41236=EDGE_CURVE('',#33712,#33712,#30666,.T.);
#41237=EDGE_CURVE('',#33711,#33710,#30667,.T.);
#41238=EDGE_CURVE('',#33713,#33713,#30668,.T.);
#41239=EDGE_CURVE('',#33713,#33711,#30669,.T.);
#41240=EDGE_CURVE('',#33714,#33715,#30670,.T.);
#41241=EDGE_CURVE('',#33714,#33716,#2733,.T.);
#41242=EDGE_CURVE('',#33716,#33716,#30671,.T.);
#41243=EDGE_CURVE('',#33715,#33714,#30672,.T.);
#41244=EDGE_CURVE('',#33717,#33717,#30673,.T.);
#41245=EDGE_CURVE('',#33717,#33715,#30674,.T.);
#41246=EDGE_CURVE('',#33718,#33719,#30675,.T.);
#41247=EDGE_CURVE('',#33719,#33720,#30676,.T.);
#41248=EDGE_CURVE('',#33721,#33720,#30677,.T.);
#41249=EDGE_CURVE('',#33721,#33718,#30678,.T.);
#41250=EDGE_CURVE('',#33722,#33723,#29484,.T.);
#41251=EDGE_CURVE('',#33724,#33722,#29485,.T.);
#41252=EDGE_CURVE('',#33719,#33724,#2734,.T.);
#41253=EDGE_CURVE('',#33718,#33723,#2735,.T.);
#41254=EDGE_CURVE('',#33725,#33726,#29486,.T.);
#41255=EDGE_CURVE('',#33727,#33726,#29487,.T.);
#41256=EDGE_CURVE('',#33727,#33728,#29488,.T.);
#41257=EDGE_CURVE('',#33728,#33729,#29489,.T.);
#41258=EDGE_CURVE('',#33729,#33730,#29490,.T.);
#41259=EDGE_CURVE('',#33730,#33731,#29491,.T.);
#41260=EDGE_CURVE('',#33732,#33731,#29492,.T.);
#41261=EDGE_CURVE('',#33733,#33732,#29493,.T.);
#41262=EDGE_CURVE('',#33733,#33734,#2636,.T.);
#41263=EDGE_CURVE('',#33734,#33735,#2736,.T.);
#41264=EDGE_CURVE('',#33735,#33735,#30679,.T.);
#41265=EDGE_CURVE('',#33734,#33736,#2637,.T.);
#41266=EDGE_CURVE('',#33737,#33736,#29494,.T.);
#41267=EDGE_CURVE('',#33738,#33737,#29495,.T.);
#41268=EDGE_CURVE('',#33738,#33739,#29496,.T.);
#41269=EDGE_CURVE('',#33740,#33739,#29497,.T.);
#41270=EDGE_CURVE('',#33740,#33741,#29498,.T.);
#41271=EDGE_CURVE('',#33741,#33742,#29499,.T.);
#41272=EDGE_CURVE('',#33743,#33742,#29500,.T.);
#41273=EDGE_CURVE('',#33743,#33725,#29501,.T.);
#41274=EDGE_CURVE('',#33744,#33745,#30680,.T.);
#41275=EDGE_CURVE('',#33744,#33696,#30681,.T.);
#41276=EDGE_CURVE('',#33697,#33745,#30682,.T.);
#41277=EDGE_CURVE('',#33746,#33747,#29502,.T.);
#41278=EDGE_CURVE('',#33747,#33748,#29503,.T.);
#41279=EDGE_CURVE('',#33748,#33749,#29504,.T.);
#41280=EDGE_CURVE('',#33750,#33749,#2737,.T.);
#41281=EDGE_CURVE('',#33750,#33751,#29505,.T.);
#41282=EDGE_CURVE('',#33751,#33752,#29506,.T.);
#41283=EDGE_CURVE('',#33752,#33753,#29507,.T.);
#41284=EDGE_CURVE('',#33753,#33754,#29508,.T.);
#41285=EDGE_CURVE('',#33755,#33754,#2738,.T.);
#41286=EDGE_CURVE('',#33755,#33746,#29509,.T.);
#41287=EDGE_CURVE('',#33756,#33757,#30683,.T.);
#41288=EDGE_CURVE('',#33757,#33758,#30684,.T.);
#41289=EDGE_CURVE('',#33757,#33759,#30685,.T.);
#41290=EDGE_CURVE('',#33759,#33760,#30686,.T.);
#41291=EDGE_CURVE('',#33756,#33760,#30687,.T.);
#41292=EDGE_CURVE('',#33707,#33706,#30688,.T.);
#41293=EDGE_CURVE('',#33707,#33761,#2739,.T.);
#41294=EDGE_CURVE('',#33762,#33761,#29510,.F.);
#41295=EDGE_CURVE('',#33762,#33763,#30689,.T.);
#41296=EDGE_CURVE('',#33761,#33763,#29511,.F.);
#41297=EDGE_CURVE('',#33764,#33764,#30690,.T.);
#41298=EDGE_CURVE('',#33764,#33765,#30691,.T.);
#41299=EDGE_CURVE('',#33765,#33766,#30692,.T.);
#41300=EDGE_CURVE('',#33766,#33765,#30693,.T.);
#41301=EDGE_CURVE('',#33766,#33767,#2740,.T.);
#41302=EDGE_CURVE('',#33767,#33767,#30694,.T.);
#41303=EDGE_CURVE('',#33768,#33768,#30695,.T.);
#41304=EDGE_CURVE('',#33768,#33769,#2741,.T.);
#41305=EDGE_CURVE('',#33769,#33770,#30696,.T.);
#41306=EDGE_CURVE('',#33771,#33770,#29512,.T.);
#41307=EDGE_CURVE('',#33771,#33769,#30697,.T.);
#41308=EDGE_CURVE('',#33772,#33773,#30698,.T.);
#41309=EDGE_CURVE('',#33774,#33773,#29513,.T.);
#41310=EDGE_CURVE('',#33775,#33774,#30699,.T.);
#41311=EDGE_CURVE('',#33775,#33776,#2742,.T.);
#41312=EDGE_CURVE('',#33776,#33776,#30700,.T.);
#41313=EDGE_CURVE('',#33777,#33775,#30701,.T.);
#41314=EDGE_CURVE('',#33772,#33777,#29514,.T.);
#41315=EDGE_CURVE('',#33778,#33778,#30702,.T.);
#41316=EDGE_CURVE('',#33778,#33779,#2743,.T.);
#41317=EDGE_CURVE('',#33779,#33780,#30703,.T.);
#41318=EDGE_CURVE('',#33780,#33779,#30704,.T.);
#41319=EDGE_CURVE('',#33780,#33781,#2744,.T.);
#41320=EDGE_CURVE('',#33781,#33781,#30705,.T.);
#41321=EDGE_CURVE('',#33782,#33782,#30706,.T.);
#41322=EDGE_CURVE('',#33782,#33783,#2745,.T.);
#41323=EDGE_CURVE('',#33783,#33783,#30707,.T.);
#41324=EDGE_CURVE('',#33784,#33784,#30708,.T.);
#41325=EDGE_CURVE('',#33784,#33785,#2746,.T.);
#41326=EDGE_CURVE('',#33786,#33785,#2638,.T.);
#41327=EDGE_CURVE('',#33787,#33786,#1729,.T.);
#41328=EDGE_CURVE('',#33788,#33787,#2639,.T.);
#41329=EDGE_CURVE('',#33789,#33788,#2640,.T.);
#41330=EDGE_CURVE('',#33790,#33789,#1730,.T.);
#41331=EDGE_CURVE('',#33785,#33790,#2641,.T.);
#41332=EDGE_CURVE('',#33791,#33792,#30709,.T.);
#41333=EDGE_CURVE('',#33792,#33791,#30710,.T.);
#41334=EDGE_CURVE('',#33792,#33793,#30711,.T.);
#41335=EDGE_CURVE('',#33793,#33793,#30712,.T.);
#41336=EDGE_CURVE('',#33794,#33794,#30713,.T.);
#41337=EDGE_CURVE('',#33794,#33791,#2747,.T.);
#41338=EDGE_CURVE('',#33795,#33796,#30714,.T.);
#41339=EDGE_CURVE('',#33795,#33797,#2748,.T.);
#41340=EDGE_CURVE('',#33797,#33797,#30715,.T.);
#41341=EDGE_CURVE('',#33796,#33795,#30716,.T.);
#41342=EDGE_CURVE('',#33798,#33799,#30717,.T.);
#41343=EDGE_CURVE('',#33799,#33798,#30718,.T.);
#41344=EDGE_CURVE('',#33799,#33796,#2749,.T.);
#41345=EDGE_CURVE('',#33800,#33801,#2642,.T.);
#41346=EDGE_CURVE('',#33801,#33802,#29515,.T.);
#41347=EDGE_CURVE('',#33803,#33802,#30719,.T.);
#41348=EDGE_CURVE('',#33803,#33800,#29516,.T.);
#41349=EDGE_CURVE('',#33804,#33805,#30720,.T.);
#41350=EDGE_CURVE('',#33805,#33806,#2750,.T.);
#41351=EDGE_CURVE('',#33806,#33807,#30721,.T.);
#41352=EDGE_CURVE('',#33807,#33804,#2751,.T.);
#41353=EDGE_CURVE('',#33666,#33664,#29517,.T.);
#41354=EDGE_CURVE('',#33663,#33665,#29518,.T.);
#41355=EDGE_CURVE('',#33808,#33809,#30722,.T.);
#41356=EDGE_CURVE('',#33809,#33810,#2752,.T.);
#41357=EDGE_CURVE('',#33810,#33810,#30723,.T.);
#41358=EDGE_CURVE('',#33809,#33808,#30724,.T.);
#41359=EDGE_CURVE('',#33808,#33662,#2753,.T.);
#41360=EDGE_CURVE('',#33811,#33653,#30725,.T.);
#41361=EDGE_CURVE('',#33812,#33811,#29519,.F.);
#41362=EDGE_CURVE('',#33812,#33813,#2754,.T.);
#41363=EDGE_CURVE('',#33813,#33813,#30726,.T.);
#41364=EDGE_CURVE('',#33668,#33812,#29520,.F.);
#41365=EDGE_CURVE('',#33655,#33667,#29521,.T.);
#41366=EDGE_CURVE('',#33654,#33652,#29522,.T.);
#41367=EDGE_CURVE('',#33651,#33811,#29523,.T.);
#41368=EDGE_CURVE('',#33814,#33814,#30727,.T.);
#41369=EDGE_CURVE('',#33814,#33815,#30728,.T.);
#41370=EDGE_CURVE('',#33815,#33816,#30729,.T.);
#41371=EDGE_CURVE('',#33816,#33815,#30730,.T.);
#41372=EDGE_CURVE('',#33816,#33817,#2755,.T.);
#41373=EDGE_CURVE('',#33817,#33817,#30731,.T.);
#41374=EDGE_CURVE('',#33818,#33819,#29524,.T.);
#41375=EDGE_CURVE('',#33642,#33818,#29525,.T.);
#41376=EDGE_CURVE('',#33820,#33641,#29526,.T.);
#41377=EDGE_CURVE('',#33821,#33820,#29527,.T.);
#41378=EDGE_CURVE('',#33819,#33821,#30732,.T.);
#41379=EDGE_CURVE('',#33822,#33640,#29528,.F.);
#41380=EDGE_CURVE('',#33822,#33823,#29529,.T.);
#41381=EDGE_CURVE('',#33823,#33637,#29530,.T.);
#41382=EDGE_CURVE('',#33636,#33639,#29531,.T.);
#41383=EDGE_CURVE('',#33824,#33825,#29532,.T.);
#41384=EDGE_CURVE('',#33825,#33826,#29533,.T.);
#41385=EDGE_CURVE('',#33826,#33827,#29534,.T.);
#41386=EDGE_CURVE('',#33827,#33828,#29535,.T.);
#41387=EDGE_CURVE('',#33828,#33829,#29536,.T.);
#41388=EDGE_CURVE('',#33829,#33830,#29537,.T.);
#41389=EDGE_CURVE('',#33830,#33831,#2756,.T.);
#41390=EDGE_CURVE('',#33831,#33831,#30733,.T.);
#41391=EDGE_CURVE('',#33830,#33832,#29538,.T.);
#41392=EDGE_CURVE('',#33832,#33833,#29539,.T.);
#41393=EDGE_CURVE('',#33833,#33824,#29540,.T.);
#41394=EDGE_CURVE('',#33834,#33835,#30734,.T.);
#41395=EDGE_CURVE('',#33834,#33836,#2757,.T.);
#41396=EDGE_CURVE('',#33837,#33836,#30735,.T.);
#41397=EDGE_CURVE('',#33837,#33838,#2758,.T.);
#41398=EDGE_CURVE('',#33838,#33839,#29541,.T.);
#41399=EDGE_CURVE('',#33839,#33840,#29542,.T.);
#41400=EDGE_CURVE('',#33840,#33835,#2759,.T.);
#41401=EDGE_CURVE('',#33841,#33842,#30736,.T.);
#41402=EDGE_CURVE('',#33843,#33842,#2760,.T.);
#41403=EDGE_CURVE('',#33844,#33843,#29543,.T.);
#41404=EDGE_CURVE('',#33845,#33844,#29544,.T.);
#41405=EDGE_CURVE('',#33845,#33841,#2761,.T.);
#41406=EDGE_CURVE('',#33846,#33846,#30737,.T.);
#41407=EDGE_CURVE('',#33846,#33847,#2762,.T.);
#41408=EDGE_CURVE('',#33847,#33847,#30738,.T.);
#41409=EDGE_CURVE('',#33848,#33849,#30739,.T.);
#41410=EDGE_CURVE('',#33849,#33850,#2763,.T.);
#41411=EDGE_CURVE('',#33850,#33850,#30740,.T.);
#41412=EDGE_CURVE('',#33849,#33848,#30741,.T.);
#41413=EDGE_CURVE('',#33848,#33851,#2764,.T.);
#41414=EDGE_CURVE('',#33851,#33851,#30742,.T.);
#41415=EDGE_CURVE('',#33852,#33853,#30743,.T.);
#41416=EDGE_CURVE('',#33853,#33854,#2765,.T.);
#41417=EDGE_CURVE('',#33855,#33854,#30744,.T.);
#41418=EDGE_CURVE('',#33854,#33855,#30745,.T.);
#41419=EDGE_CURVE('',#33853,#33852,#30746,.T.);
#41420=EDGE_CURVE('',#33856,#33857,#1731,.T.);
#41421=EDGE_CURVE('',#33858,#33856,#1732,.T.);
#41422=EDGE_CURVE('',#33859,#33858,#1733,.T.);
#41423=EDGE_CURVE('',#33860,#33859,#1734,.F.);
#41424=EDGE_CURVE('',#33860,#33855,#2766,.T.);
#41425=EDGE_CURVE('',#33861,#33860,#1735,.F.);
#41426=EDGE_CURVE('',#33862,#33861,#1736,.T.);
#41427=EDGE_CURVE('',#33857,#33862,#1737,.T.);
#41428=EDGE_CURVE('',#33852,#33863,#2767,.T.);
#41429=EDGE_CURVE('',#33863,#33863,#30747,.T.);
#41430=EDGE_CURVE('',#33864,#33865,#30748,.T.);
#41431=EDGE_CURVE('',#33865,#33864,#30749,.T.);
#41432=EDGE_CURVE('',#33864,#33866,#30750,.T.);
#41433=EDGE_CURVE('',#33866,#33866,#30751,.T.);
#41434=EDGE_CURVE('',#33867,#33867,#30752,.T.);
#41435=EDGE_CURVE('',#33867,#33865,#2768,.T.);
#41436=EDGE_CURVE('',#33868,#33622,#29545,.T.);
#41437=EDGE_CURVE('',#33869,#33868,#29546,.T.);
#41438=EDGE_CURVE('',#33870,#33869,#30753,.T.);
#41439=EDGE_CURVE('',#33871,#33870,#29547,.T.);
#41440=EDGE_CURVE('',#33623,#33871,#29548,.T.);
#41441=EDGE_CURVE('',#33629,#33872,#29549,.T.);
#41442=EDGE_CURVE('',#33873,#33872,#29550,.T.);
#41443=EDGE_CURVE('',#33874,#33873,#30754,.T.);
#41444=EDGE_CURVE('',#33874,#33628,#29551,.T.);
#41445=EDGE_CURVE('',#33875,#33876,#29552,.T.);
#41446=EDGE_CURVE('',#33876,#33877,#29553,.T.);
#41447=EDGE_CURVE('',#33877,#33878,#29554,.T.);
#41448=EDGE_CURVE('',#33878,#33879,#29555,.T.);
#41449=EDGE_CURVE('',#33879,#33880,#2769,.T.);
#41450=EDGE_CURVE('',#33880,#33880,#30755,.T.);
#41451=EDGE_CURVE('',#33879,#33881,#29556,.T.);
#41452=EDGE_CURVE('',#33881,#33882,#29557,.T.);
#41453=EDGE_CURVE('',#33882,#33883,#29558,.T.);
#41454=EDGE_CURVE('',#33883,#33884,#29559,.T.);
#41455=EDGE_CURVE('',#33884,#33875,#29560,.T.);
#41456=EDGE_CURVE('',#33885,#33886,#29561,.T.);
#41457=EDGE_CURVE('',#33886,#33887,#29562,.T.);
#41458=EDGE_CURVE('',#33887,#33888,#2770,.T.);
#41459=EDGE_CURVE('',#33889,#33888,#30756,.T.);
#41460=EDGE_CURVE('',#33889,#33890,#2771,.T.);
#41461=EDGE_CURVE('',#33891,#33890,#30757,.T.);
#41462=EDGE_CURVE('',#33891,#33885,#2772,.T.);
#41463=EDGE_CURVE('',#33892,#33893,#1738,.T.);
#41464=EDGE_CURVE('',#33894,#33892,#29563,.T.);
#41465=EDGE_CURVE('',#33895,#33894,#2773,.T.);
#41466=EDGE_CURVE('',#33895,#33896,#30758,.T.);
#41467=EDGE_CURVE('',#33896,#33893,#2774,.T.);
#41468=EDGE_CURVE('',#33897,#33897,#30759,.T.);
#41469=EDGE_CURVE('',#33897,#33898,#2775,.T.);
#41470=EDGE_CURVE('',#33898,#33898,#30760,.T.);
#41471=EDGE_CURVE('',#33899,#33900,#30761,.T.);
#41472=EDGE_CURVE('',#33900,#33901,#2776,.T.);
#41473=EDGE_CURVE('',#33901,#33901,#30762,.T.);
#41474=EDGE_CURVE('',#33900,#33899,#30763,.T.);
#41475=EDGE_CURVE('',#33899,#33902,#2777,.T.);
#41476=EDGE_CURVE('',#33902,#33902,#30764,.T.);
#41477=EDGE_CURVE('',#33903,#33904,#30765,.T.);
#41478=EDGE_CURVE('',#33904,#33905,#2778,.T.);
#41479=EDGE_CURVE('',#33906,#33905,#30766,.T.);
#41480=EDGE_CURVE('',#33905,#33906,#30767,.T.);
#41481=EDGE_CURVE('',#33904,#33903,#30768,.T.);
#41482=EDGE_CURVE('',#33907,#33908,#1739,.T.);
#41483=EDGE_CURVE('',#33909,#33907,#1740,.T.);
#41484=EDGE_CURVE('',#33910,#33909,#1741,.T.);
#41485=EDGE_CURVE('',#33911,#33910,#1742,.F.);
#41486=EDGE_CURVE('',#33911,#33906,#2779,.T.);
#41487=EDGE_CURVE('',#33912,#33911,#1743,.F.);
#41488=EDGE_CURVE('',#33913,#33912,#1744,.T.);
#41489=EDGE_CURVE('',#33908,#33913,#1745,.T.);
#41490=EDGE_CURVE('',#33903,#33914,#2780,.T.);
#41491=EDGE_CURVE('',#33914,#33914,#30769,.T.);
#41492=EDGE_CURVE('',#33915,#33916,#2781,.T.);
#41493=EDGE_CURVE('',#33916,#33917,#2782,.T.);
#41494=EDGE_CURVE('',#33917,#33918,#2783,.T.);
#41495=EDGE_CURVE('',#33918,#33919,#2784,.T.);
#41496=EDGE_CURVE('',#33919,#33920,#2785,.T.);
#41497=EDGE_CURVE('',#33920,#33915,#2786,.T.);
#41498=EDGE_CURVE('',#33915,#33909,#2787,.T.);
#41499=EDGE_CURVE('',#33916,#33907,#2788,.T.);
#41500=EDGE_CURVE('',#33917,#33908,#2789,.T.);
#41501=EDGE_CURVE('',#33918,#33913,#2790,.T.);
#41502=EDGE_CURVE('',#33919,#33912,#2791,.T.);
#41503=EDGE_CURVE('',#33920,#33910,#2792,.T.);
#41504=EDGE_CURVE('',#33921,#33922,#2793,.T.);
#41505=EDGE_CURVE('',#33921,#33923,#30770,.T.);
#41506=EDGE_CURVE('',#33923,#33924,#2794,.T.);
#41507=EDGE_CURVE('',#33924,#33922,#30771,.T.);
#41508=EDGE_CURVE('',#33925,#33926,#29564,.T.);
#41509=EDGE_CURVE('',#33925,#33927,#29565,.T.);
#41510=EDGE_CURVE('',#33927,#33926,#29566,.T.);
#41511=EDGE_CURVE('',#33928,#33893,#30772,.T.);
#41512=EDGE_CURVE('',#33928,#33929,#29567,.T.);
#41513=EDGE_CURVE('',#33929,#33894,#30773,.T.);
#41514=EDGE_CURVE('',#33923,#33930,#30774,.T.);
#41515=EDGE_CURVE('',#33930,#33931,#29568,.T.);
#41516=EDGE_CURVE('',#33924,#33931,#29569,.T.);
#41517=EDGE_CURVE('',#33932,#33922,#30775,.T.);
#41518=EDGE_CURVE('',#33924,#33932,#30776,.T.);
#41519=EDGE_CURVE('',#33921,#33933,#2795,.T.);
#41520=EDGE_CURVE('',#33922,#33934,#2796,.T.);
#41521=EDGE_CURVE('',#33934,#33935,#2643,.T.);
#41522=EDGE_CURVE('',#33935,#33933,#2797,.T.);
#41523=EDGE_CURVE('',#33936,#33934,#29570,.T.);
#41524=EDGE_CURVE('',#33937,#33936,#29571,.T.);
#41525=EDGE_CURVE('',#33937,#33934,#30777,.T.);
#41526=EDGE_CURVE('',#33938,#33937,#29572,.T.);
#41527=EDGE_CURVE('',#33938,#33935,#29573,.T.);
#41528=EDGE_CURVE('',#33938,#33939,#2798,.T.);
#41529=EDGE_CURVE('',#33939,#33933,#30778,.T.);
#41530=EDGE_CURVE('',#33940,#33941,#30779,.T.);
#41531=EDGE_CURVE('',#33941,#33930,#29574,.T.);
#41532=EDGE_CURVE('',#33939,#33940,#2799,.T.);
#41533=EDGE_CURVE('',#33942,#33943,#30780,.T.);
#41534=EDGE_CURVE('',#33943,#33927,#1746,.T.);
#41535=EDGE_CURVE('',#33942,#33925,#29575,.T.);
#41536=EDGE_CURVE('',#33944,#33945,#29576,.T.);
#41537=EDGE_CURVE('',#33946,#33944,#2800,.T.);
#41538=EDGE_CURVE('',#33947,#33946,#30781,.T.);
#41539=EDGE_CURVE('',#33947,#33945,#2801,.T.);
#41540=EDGE_CURVE('',#33944,#33940,#2802,.T.);
#41541=EDGE_CURVE('',#33948,#33945,#30782,.T.);
#41542=EDGE_CURVE('',#33948,#33949,#29577,.T.);
#41543=EDGE_CURVE('',#33929,#33949,#29578,.T.);
#41544=EDGE_CURVE('',#33941,#33928,#29579,.T.);
#41545=EDGE_CURVE('',#33925,#33948,#29580,.T.);
#41546=EDGE_CURVE('',#33926,#33949,#1747,.T.);
#41547=EDGE_CURVE('',#33950,#33951,#30783,.T.);
#41548=EDGE_CURVE('',#33951,#33943,#2803,.T.);
#41549=EDGE_CURVE('',#33950,#33942,#2804,.T.);
#41550=EDGE_CURVE('',#33952,#33943,#29581,.T.);
#41551=EDGE_CURVE('',#33953,#33952,#30784,.T.);
#41552=EDGE_CURVE('',#33926,#33953,#29582,.T.);
#41553=EDGE_CURVE('',#33954,#33952,#29583,.T.);
#41554=EDGE_CURVE('',#33955,#33954,#30785,.T.);
#41555=EDGE_CURVE('',#33955,#33953,#29584,.T.);
#41556=EDGE_CURVE('',#33953,#33956,#30786,.T.);
#41557=EDGE_CURVE('',#33956,#33894,#29585,.T.);
#41558=EDGE_CURVE('',#33957,#33895,#30787,.T.);
#41559=EDGE_CURVE('',#33958,#33895,#30788,.T.);
#41560=EDGE_CURVE('',#33959,#33958,#30789,.T.);
#41561=EDGE_CURVE('',#33959,#33957,#30790,.T.);
#41562=EDGE_CURVE('',#33960,#33896,#30791,.T.);
#41563=EDGE_CURVE('',#33957,#33960,#30792,.T.);
#41564=EDGE_CURVE('',#33961,#33962,#30793,.T.);
#41565=EDGE_CURVE('',#33896,#33962,#30794,.T.);
#41566=EDGE_CURVE('',#33960,#33961,#30795,.T.);
#41567=EDGE_CURVE('',#33893,#33963,#29586,.T.);
#41568=EDGE_CURVE('',#33931,#33963,#30796,.T.);
#41569=EDGE_CURVE('',#33963,#33964,#29587,.T.);
#41570=EDGE_CURVE('',#33965,#33964,#1748,.T.);
#41571=EDGE_CURVE('',#33931,#33965,#29588,.T.);
#41572=EDGE_CURVE('',#33965,#33966,#29589,.T.);
#41573=EDGE_CURVE('',#33932,#33966,#29590,.T.);
#41574=EDGE_CURVE('',#33932,#33936,#2805,.T.);
#41575=EDGE_CURVE('',#33936,#33967,#30797,.T.);
#41576=EDGE_CURVE('',#33967,#33968,#30798,.T.);
#41577=EDGE_CURVE('',#33938,#33968,#30799,.T.);
#41578=EDGE_CURVE('',#33968,#33969,#30800,.T.);
#41579=EDGE_CURVE('',#33969,#33946,#30801,.T.);
#41580=EDGE_CURVE('',#33890,#33946,#30802,.T.);
#41581=EDGE_CURVE('',#33890,#33947,#30803,.T.);
#41582=EDGE_CURVE('',#33970,#33947,#2806,.T.);
#41583=EDGE_CURVE('',#33970,#33950,#29591,.T.);
#41584=EDGE_CURVE('',#33970,#33971,#30804,.T.);
#41585=EDGE_CURVE('',#33971,#33951,#30805,.T.);
#41586=EDGE_CURVE('',#33951,#33972,#30806,.T.);
#41587=EDGE_CURVE('',#33972,#33954,#30807,.T.);
#41588=EDGE_CURVE('',#33889,#33971,#29592,.T.);
#41589=EDGE_CURVE('',#33889,#33970,#29593,.T.);
#41590=EDGE_CURVE('',#33888,#33972,#30808,.T.);
#41591=EDGE_CURVE('',#33888,#33955,#30809,.T.);
#41592=EDGE_CURVE('',#33955,#33956,#29594,.T.);
#41593=EDGE_CURVE('',#33958,#33956,#2807,.T.);
#41594=EDGE_CURVE('',#33973,#33958,#30810,.T.);
#41595=EDGE_CURVE('',#33974,#33973,#30811,.T.);
#41596=EDGE_CURVE('',#33974,#33959,#30812,.T.);
#41597=EDGE_CURVE('',#33975,#33974,#30813,.T.);
#41598=EDGE_CURVE('',#33961,#33975,#30814,.T.);
#41599=EDGE_CURVE('',#33975,#33976,#30815,.T.);
#41600=EDGE_CURVE('',#33962,#33976,#30816,.T.);
#41601=EDGE_CURVE('',#33964,#33962,#2808,.T.);
#41602=EDGE_CURVE('',#33964,#33966,#29595,.T.);
#41603=EDGE_CURVE('',#33967,#33966,#2809,.T.);
#41604=EDGE_CURVE('',#33891,#33969,#30817,.T.);
#41605=EDGE_CURVE('',#33967,#33891,#30818,.T.);
#41606=EDGE_CURVE('',#33887,#33977,#29596,.T.);
#41607=EDGE_CURVE('',#33973,#33977,#2810,.T.);
#41608=EDGE_CURVE('',#33977,#33978,#29597,.T.);
#41609=EDGE_CURVE('',#33978,#33973,#30819,.T.);
#41610=EDGE_CURVE('',#33978,#33979,#29598,.T.);
#41611=EDGE_CURVE('',#33976,#33979,#30820,.T.);
#41612=EDGE_CURVE('',#33979,#33980,#29599,.T.);
#41613=EDGE_CURVE('',#33980,#33976,#2811,.T.);
#41614=EDGE_CURVE('',#33980,#33981,#29600,.T.);
#41615=EDGE_CURVE('',#33981,#33885,#29601,.T.);
#41616=EDGE_CURVE('',#33977,#33982,#30821,.T.);
#41617=EDGE_CURVE('',#33887,#33983,#29602,.T.);
#41618=EDGE_CURVE('',#33984,#33983,#29603,.T.);
#41619=EDGE_CURVE('',#33982,#33984,#29604,.T.);
#41620=EDGE_CURVE('',#33978,#33985,#30822,.T.);
#41621=EDGE_CURVE('',#33985,#33982,#29605,.T.);
#41622=EDGE_CURVE('',#33979,#33986,#30823,.T.);
#41623=EDGE_CURVE('',#33986,#33985,#29606,.T.);
#41624=EDGE_CURVE('',#33980,#33987,#1749,.T.);
#41625=EDGE_CURVE('',#33987,#33986,#29607,.T.);
#41626=EDGE_CURVE('',#33981,#33988,#30824,.T.);
#41627=EDGE_CURVE('',#33988,#33987,#29608,.T.);
#41628=EDGE_CURVE('',#33885,#33989,#30825,.T.);
#41629=EDGE_CURVE('',#33989,#33988,#29609,.T.);
#41630=EDGE_CURVE('',#33886,#33990,#30826,.T.);
#41631=EDGE_CURVE('',#33990,#33989,#29610,.T.);
#41632=EDGE_CURVE('',#33983,#33990,#29611,.T.);
#41633=EDGE_CURVE('',#33983,#33876,#30827,.T.);
#41634=EDGE_CURVE('',#33984,#33875,#29612,.T.);
#41635=EDGE_CURVE('',#33982,#33884,#30828,.T.);
#41636=EDGE_CURVE('',#33985,#33883,#30829,.T.);
#41637=EDGE_CURVE('',#33986,#33882,#30830,.T.);
#41638=EDGE_CURVE('',#33987,#33881,#30831,.T.);
#41639=EDGE_CURVE('',#33988,#33879,#29613,.T.);
#41640=EDGE_CURVE('',#33989,#33878,#30832,.T.);
#41641=EDGE_CURVE('',#33990,#33877,#29614,.T.);
#41642=EDGE_CURVE('',#33991,#33992,#29615,.T.);
#41643=EDGE_CURVE('',#33992,#33874,#29616,.T.);
#41644=EDGE_CURVE('',#33873,#33991,#29617,.T.);
#41645=EDGE_CURVE('',#33993,#33991,#29618,.T.);
#41646=EDGE_CURVE('',#33630,#33993,#2812,.T.);
#41647=EDGE_CURVE('',#33993,#33994,#2813,.T.);
#41648=EDGE_CURVE('',#33994,#33992,#29619,.T.);
#41649=EDGE_CURVE('',#33994,#33626,#2814,.T.);
#41650=EDGE_CURVE('',#33995,#33870,#29620,.T.);
#41651=EDGE_CURVE('',#33995,#33993,#29621,.T.);
#41652=EDGE_CURVE('',#33996,#33995,#29622,.T.);
#41653=EDGE_CURVE('',#33996,#33994,#29623,.T.);
#41654=EDGE_CURVE('',#33869,#33996,#29624,.T.);
#41655=EDGE_CURVE('',#33997,#33998,#2815,.T.);
#41656=EDGE_CURVE('',#33998,#33999,#2816,.T.);
#41657=EDGE_CURVE('',#33999,#34000,#2817,.T.);
#41658=EDGE_CURVE('',#34000,#34001,#2818,.T.);
#41659=EDGE_CURVE('',#34001,#34002,#2819,.T.);
#41660=EDGE_CURVE('',#34002,#33997,#2820,.T.);
#41661=EDGE_CURVE('',#33997,#33858,#2821,.T.);
#41662=EDGE_CURVE('',#33998,#33856,#2822,.T.);
#41663=EDGE_CURVE('',#33999,#33857,#2823,.T.);
#41664=EDGE_CURVE('',#34000,#33862,#2824,.T.);
#41665=EDGE_CURVE('',#34001,#33861,#2825,.T.);
#41666=EDGE_CURVE('',#34002,#33859,#2826,.T.);
#41667=EDGE_CURVE('',#34003,#34004,#29625,.T.);
#41668=EDGE_CURVE('',#34003,#34005,#29626,.T.);
#41669=EDGE_CURVE('',#34005,#34004,#29627,.T.);
#41670=EDGE_CURVE('',#34006,#34007,#2827,.T.);
#41671=EDGE_CURVE('',#34007,#34008,#30833,.T.);
#41672=EDGE_CURVE('',#34009,#34008,#2828,.T.);
#41673=EDGE_CURVE('',#34006,#34009,#30834,.T.);
#41674=EDGE_CURVE('',#34010,#34004,#29628,.T.);
#41675=EDGE_CURVE('',#34010,#34011,#30835,.T.);
#41676=EDGE_CURVE('',#34012,#34011,#29629,.T.);
#41677=EDGE_CURVE('',#34012,#34003,#29630,.T.);
#41678=EDGE_CURVE('',#34013,#34014,#30836,.T.);
#41679=EDGE_CURVE('',#34014,#34015,#2829,.T.);
#41680=EDGE_CURVE('',#34012,#34015,#30837,.T.);
#41681=EDGE_CURVE('',#34013,#34012,#2830,.T.);
#41682=EDGE_CURVE('',#34015,#34005,#29631,.T.);
#41683=EDGE_CURVE('',#34016,#34017,#29632,.T.);
#41684=EDGE_CURVE('',#34004,#34016,#29633,.T.);
#41685=EDGE_CURVE('',#34005,#34017,#29634,.T.);
#41686=EDGE_CURVE('',#34018,#34019,#2831,.T.);
#41687=EDGE_CURVE('',#34018,#34020,#30838,.T.);
#41688=EDGE_CURVE('',#34020,#34021,#29635,.T.);
#41689=EDGE_CURVE('',#34019,#34021,#29636,.T.);
#41690=EDGE_CURVE('',#34022,#34023,#29637,.T.);
#41691=EDGE_CURVE('',#34022,#34024,#2832,.T.);
#41692=EDGE_CURVE('',#34024,#34025,#30839,.T.);
#41693=EDGE_CURVE('',#34023,#34025,#2833,.T.);
#41694=EDGE_CURVE('',#34026,#34021,#29638,.T.);
#41695=EDGE_CURVE('',#34027,#34026,#30840,.T.);
#41696=EDGE_CURVE('',#34027,#34019,#2644,.T.);
#41697=EDGE_CURVE('',#34018,#34008,#2834,.T.);
#41698=EDGE_CURVE('',#34027,#34009,#2835,.T.);
#41699=EDGE_CURVE('',#34028,#34026,#29639,.T.);
#41700=EDGE_CURVE('',#34027,#34028,#29640,.T.);
#41701=EDGE_CURVE('',#34029,#34009,#30841,.T.);
#41702=EDGE_CURVE('',#34029,#34006,#30842,.T.);
#41703=EDGE_CURVE('',#34030,#34031,#29641,.T.);
#41704=EDGE_CURVE('',#34031,#34007,#30843,.T.);
#41705=EDGE_CURVE('',#34030,#34006,#29642,.T.);
#41706=EDGE_CURVE('',#34031,#34032,#29643,.T.);
#41707=EDGE_CURVE('',#34032,#34033,#30844,.T.);
#41708=EDGE_CURVE('',#34033,#34020,#2836,.T.);
#41709=EDGE_CURVE('',#34034,#34032,#29644,.T.);
#41710=EDGE_CURVE('',#34035,#34034,#29645,.T.);
#41711=EDGE_CURVE('',#34016,#34035,#29646,.T.);
#41712=EDGE_CURVE('',#34022,#34017,#30845,.T.);
#41713=EDGE_CURVE('',#34033,#34023,#2837,.T.);
#41714=EDGE_CURVE('',#34035,#33843,#30846,.T.);
#41715=EDGE_CURVE('',#34034,#33845,#30847,.T.);
#41716=EDGE_CURVE('',#33843,#34036,#29647,.T.);
#41717=EDGE_CURVE('',#34010,#34036,#30848,.T.);
#41718=EDGE_CURVE('',#34037,#34038,#30849,.T.);
#41719=EDGE_CURVE('',#34011,#34038,#29648,.T.);
#41720=EDGE_CURVE('',#34010,#34037,#29649,.T.);
#41721=EDGE_CURVE('',#34039,#34040,#30850,.T.);
#41722=EDGE_CURVE('',#34040,#34014,#30851,.T.);
#41723=EDGE_CURVE('',#34039,#34013,#30852,.T.);
#41724=EDGE_CURVE('',#34038,#34041,#30853,.T.);
#41725=EDGE_CURVE('',#34041,#34013,#30854,.T.);
#41726=EDGE_CURVE('',#33836,#34040,#29650,.T.);
#41727=EDGE_CURVE('',#33836,#34039,#29651,.T.);
#41728=EDGE_CURVE('',#34024,#34040,#2838,.T.);
#41729=EDGE_CURVE('',#33834,#34025,#30855,.T.);
#41730=EDGE_CURVE('',#34024,#33834,#30856,.T.);
#41731=EDGE_CURVE('',#34025,#34042,#30857,.T.);
#41732=EDGE_CURVE('',#34042,#34043,#30858,.T.);
#41733=EDGE_CURVE('',#34043,#34021,#30859,.T.);
#41734=EDGE_CURVE('',#34044,#34043,#30860,.T.);
#41735=EDGE_CURVE('',#34044,#34028,#30861,.T.);
#41736=EDGE_CURVE('',#34028,#34029,#2839,.T.);
#41737=EDGE_CURVE('',#34045,#34029,#29652,.T.);
#41738=EDGE_CURVE('',#34045,#34046,#29653,.T.);
#41739=EDGE_CURVE('',#34046,#34030,#29654,.T.);
#41740=EDGE_CURVE('',#34046,#34047,#1750,.T.);
#41741=EDGE_CURVE('',#34047,#34048,#29655,.T.);
#41742=EDGE_CURVE('',#34030,#34048,#30862,.T.);
#41743=EDGE_CURVE('',#34048,#33845,#1751,.T.);
#41744=EDGE_CURVE('',#34049,#33841,#30863,.T.);
#41745=EDGE_CURVE('',#34050,#33841,#30864,.T.);
#41746=EDGE_CURVE('',#34051,#34050,#30865,.T.);
#41747=EDGE_CURVE('',#34051,#34049,#30866,.T.);
#41748=EDGE_CURVE('',#34052,#33842,#30867,.T.);
#41749=EDGE_CURVE('',#34049,#34052,#30868,.T.);
#41750=EDGE_CURVE('',#34053,#34054,#30869,.T.);
#41751=EDGE_CURVE('',#33842,#34054,#30870,.T.);
#41752=EDGE_CURVE('',#34052,#34053,#30871,.T.);
#41753=EDGE_CURVE('',#34036,#34054,#2840,.T.);
#41754=EDGE_CURVE('',#34036,#34037,#29656,.T.);
#41755=EDGE_CURVE('',#33837,#34041,#30872,.T.);
#41756=EDGE_CURVE('',#34037,#33837,#30873,.T.);
#41757=EDGE_CURVE('',#33835,#34042,#30874,.T.);
#41758=EDGE_CURVE('',#33835,#34044,#30875,.T.);
#41759=EDGE_CURVE('',#34045,#34044,#2841,.T.);
#41760=EDGE_CURVE('',#34045,#34047,#29657,.T.);
#41761=EDGE_CURVE('',#34047,#34050,#2842,.T.);
#41762=EDGE_CURVE('',#34055,#34050,#30876,.T.);
#41763=EDGE_CURVE('',#34056,#34055,#30877,.T.);
#41764=EDGE_CURVE('',#34056,#34051,#30878,.T.);
#41765=EDGE_CURVE('',#34057,#34056,#30879,.T.);
#41766=EDGE_CURVE('',#34053,#34057,#30880,.T.);
#41767=EDGE_CURVE('',#34057,#34058,#30881,.T.);
#41768=EDGE_CURVE('',#34054,#34058,#30882,.T.);
#41769=EDGE_CURVE('',#34059,#34058,#2843,.T.);
#41770=EDGE_CURVE('',#34059,#33838,#29658,.T.);
#41771=EDGE_CURVE('',#33840,#34060,#29659,.T.);
#41772=EDGE_CURVE('',#34060,#34061,#29660,.T.);
#41773=EDGE_CURVE('',#34055,#34061,#2844,.T.);
#41774=EDGE_CURVE('',#34061,#34062,#29661,.T.);
#41775=EDGE_CURVE('',#34062,#34055,#30883,.T.);
#41776=EDGE_CURVE('',#34062,#34063,#29662,.T.);
#41777=EDGE_CURVE('',#34063,#34064,#29663,.T.);
#41778=EDGE_CURVE('',#34058,#34064,#30884,.T.);
#41779=EDGE_CURVE('',#34064,#34059,#29664,.T.);
#41780=EDGE_CURVE('',#33838,#34065,#30885,.T.);
#41781=EDGE_CURVE('',#34059,#34066,#1752,.T.);
#41782=EDGE_CURVE('',#34067,#34066,#29665,.T.);
#41783=EDGE_CURVE('',#34065,#34067,#29666,.T.);
#41784=EDGE_CURVE('',#33840,#34068,#1753,.T.);
#41785=EDGE_CURVE('',#34068,#34065,#29667,.T.);
#41786=EDGE_CURVE('',#34060,#34069,#30886,.T.);
#41787=EDGE_CURVE('',#34069,#34068,#29668,.T.);
#41788=EDGE_CURVE('',#34061,#34070,#30887,.T.);
#41789=EDGE_CURVE('',#34070,#34069,#29669,.T.);
#41790=EDGE_CURVE('',#34062,#34071,#30888,.T.);
#41791=EDGE_CURVE('',#34071,#34070,#29670,.T.);
#41792=EDGE_CURVE('',#34063,#34072,#30889,.T.);
#41793=EDGE_CURVE('',#34072,#34071,#29671,.T.);
#41794=EDGE_CURVE('',#34064,#34073,#30890,.T.);
#41795=EDGE_CURVE('',#34073,#34072,#29672,.T.);
#41796=EDGE_CURVE('',#34066,#34073,#29673,.T.);
#41797=EDGE_CURVE('',#34066,#33825,#30891,.T.);
#41798=EDGE_CURVE('',#34067,#33824,#29674,.T.);
#41799=EDGE_CURVE('',#34065,#33833,#30892,.T.);
#41800=EDGE_CURVE('',#34068,#33832,#30893,.T.);
#41801=EDGE_CURVE('',#34069,#33830,#29675,.T.);
#41802=EDGE_CURVE('',#34070,#33829,#30894,.T.);
#41803=EDGE_CURVE('',#34071,#33828,#30895,.T.);
#41804=EDGE_CURVE('',#34072,#33827,#29676,.T.);
#41805=EDGE_CURVE('',#34073,#33826,#29677,.T.);
#41806=EDGE_CURVE('',#33633,#34074,#29678,.T.);
#41807=EDGE_CURVE('',#34074,#34075,#29679,.T.);
#41808=EDGE_CURVE('',#34075,#33634,#29680,.T.);
#41809=EDGE_CURVE('',#34076,#34075,#29681,.T.);
#41810=EDGE_CURVE('',#33638,#34076,#2845,.T.);
#41811=EDGE_CURVE('',#34077,#33823,#2846,.T.);
#41812=EDGE_CURVE('',#34077,#34074,#29682,.T.);
#41813=EDGE_CURVE('',#34076,#34077,#2847,.T.);
#41814=EDGE_CURVE('',#34078,#34076,#29683,.T.);
#41815=EDGE_CURVE('',#33821,#34078,#29684,.T.);
#41816=EDGE_CURVE('',#34079,#34077,#29685,.T.);
#41817=EDGE_CURVE('',#34079,#33819,#29686,.T.);
#41818=EDGE_CURVE('',#34078,#34079,#29687,.T.);
#41819=EDGE_CURVE('',#33658,#33646,#2848,.T.);
#41820=EDGE_CURVE('',#33645,#33659,#2849,.T.);
#41821=EDGE_CURVE('',#34080,#34081,#2850,.T.);
#41822=EDGE_CURVE('',#34080,#34082,#2851,.T.);
#41823=EDGE_CURVE('',#34083,#34082,#2852,.T.);
#41824=EDGE_CURVE('',#34083,#34084,#2853,.T.);
#41825=EDGE_CURVE('',#34084,#34085,#30896,.T.);
#41826=EDGE_CURVE('',#34086,#34085,#30897,.T.);
#41827=EDGE_CURVE('',#34087,#34086,#30898,.T.);
#41828=EDGE_CURVE('',#34088,#34087,#30899,.T.);
#41829=EDGE_CURVE('',#34081,#34088,#30900,.T.);
#41830=EDGE_CURVE('',#34089,#34090,#2854,.T.);
#41831=EDGE_CURVE('',#34089,#34091,#2855,.T.);
#41832=EDGE_CURVE('',#34092,#34091,#2856,.T.);
#41833=EDGE_CURVE('',#34093,#34092,#30901,.T.);
#41834=EDGE_CURVE('',#34094,#34093,#30902,.T.);
#41835=EDGE_CURVE('',#34095,#34094,#30903,.T.);
#41836=EDGE_CURVE('',#34096,#34095,#30904,.T.);
#41837=EDGE_CURVE('',#34096,#34097,#30905,.T.);
#41838=EDGE_CURVE('',#34097,#34090,#2857,.T.);
#41839=EDGE_CURVE('',#33683,#34098,#2858,.T.);
#41840=EDGE_CURVE('',#34099,#33682,#2859,.T.);
#41841=EDGE_CURVE('',#34098,#34099,#2645,.T.);
#41842=EDGE_CURVE('',#33681,#34100,#2860,.T.);
#41843=EDGE_CURVE('',#34101,#33680,#2861,.T.);
#41844=EDGE_CURVE('',#34100,#34101,#2646,.T.);
#41845=EDGE_CURVE('',#34098,#34102,#30906,.T.);
#41846=EDGE_CURVE('',#34102,#34103,#30907,.T.);
#41847=EDGE_CURVE('',#34104,#34103,#2862,.T.);
#41848=EDGE_CURVE('',#33684,#34104,#30908,.T.);
#41849=EDGE_CURVE('',#33685,#34104,#29688,.T.);
#41850=EDGE_CURVE('',#34105,#34106,#2863,.T.);
#41851=EDGE_CURVE('',#34105,#34107,#29689,.T.);
#41852=EDGE_CURVE('',#34107,#33760,#2864,.T.);
#41853=EDGE_CURVE('',#33760,#34108,#2865,.T.);
#41854=EDGE_CURVE('',#34106,#34108,#2866,.T.);
#41855=EDGE_CURVE('',#34109,#33678,#29690,.T.);
#41856=EDGE_CURVE('',#33677,#34109,#29691,.T.);
#41857=EDGE_CURVE('',#34110,#33676,#29692,.T.);
#41858=EDGE_CURVE('',#34111,#34110,#29693,.T.);
#41859=EDGE_CURVE('',#34112,#34111,#30909,.T.);
#41860=EDGE_CURVE('',#34113,#34112,#2867,.T.);
#41861=EDGE_CURVE('',#34114,#34113,#29694,.T.);
#41862=EDGE_CURVE('',#34115,#34114,#30910,.T.);
#41863=EDGE_CURVE('',#34115,#34116,#29695,.T.);
#41864=EDGE_CURVE('',#34116,#34109,#2868,.T.);
#41865=EDGE_CURVE('',#34104,#33686,#29696,.T.);
#41866=EDGE_CURVE('',#34103,#34117,#29697,.T.);
#41867=EDGE_CURVE('',#34117,#34118,#29698,.T.);
#41868=EDGE_CURVE('',#34118,#34119,#29699,.T.);
#41869=EDGE_CURVE('',#34120,#34119,#30911,.T.);
#41870=EDGE_CURVE('',#34121,#34120,#29700,.T.);
#41871=EDGE_CURVE('',#34121,#34122,#2869,.T.);
#41872=EDGE_CURVE('',#34123,#34122,#30912,.T.);
#41873=EDGE_CURVE('',#34124,#34123,#29701,.T.);
#41874=EDGE_CURVE('',#33687,#34124,#29702,.T.);
#41875=EDGE_CURVE('',#34125,#34124,#29703,.T.);
#41876=EDGE_CURVE('',#34126,#34125,#2870,.T.);
#41877=EDGE_CURVE('',#34127,#34126,#30913,.T.);
#41878=EDGE_CURVE('',#34127,#34128,#29704,.T.);
#41879=EDGE_CURVE('',#34129,#34128,#2871,.T.);
#41880=EDGE_CURVE('',#34130,#34129,#29705,.T.);
#41881=EDGE_CURVE('',#33688,#34130,#29706,.T.);
#41882=EDGE_CURVE('',#34131,#33675,#29707,.T.);
#41883=EDGE_CURVE('',#34132,#34131,#29708,.T.);
#41884=EDGE_CURVE('',#34132,#34133,#2872,.T.);
#41885=EDGE_CURVE('',#34133,#34134,#29709,.T.);
#41886=EDGE_CURVE('',#34135,#34134,#30914,.T.);
#41887=EDGE_CURVE('',#34136,#34135,#2873,.T.);
#41888=EDGE_CURVE('',#34110,#34136,#29710,.T.);
#41889=EDGE_CURVE('',#33672,#34137,#29711,.T.);
#41890=EDGE_CURVE('',#33690,#34129,#1754,.T.);
#41891=EDGE_CURVE('',#34129,#34138,#29712,.T.);
#41892=EDGE_CURVE('',#34139,#34138,#30915,.T.);
#41893=EDGE_CURVE('',#34140,#34139,#29713,.T.);
#41894=EDGE_CURVE('',#34140,#34137,#1755,.T.);
#41895=EDGE_CURVE('',#33689,#34130,#29714,.T.);
#41896=EDGE_CURVE('',#34080,#34141,#29715,.T.);
#41897=EDGE_CURVE('',#34081,#34142,#30916,.T.);
#41898=EDGE_CURVE('',#34141,#34142,#2874,.T.);
#41899=EDGE_CURVE('',#34143,#34091,#29716,.T.);
#41900=EDGE_CURVE('',#34144,#34143,#2875,.T.);
#41901=EDGE_CURVE('',#34092,#34144,#30917,.T.);
#41902=EDGE_CURVE('',#33674,#34131,#30918,.T.);
#41903=EDGE_CURVE('',#33673,#34132,#29717,.T.);
#41904=EDGE_CURVE('',#34145,#33671,#29718,.T.);
#41905=EDGE_CURVE('',#34146,#34145,#29719,.T.);
#41906=EDGE_CURVE('',#34139,#34146,#29720,.T.);
#41907=EDGE_CURVE('',#34138,#34132,#29721,.T.);
#41908=EDGE_CURVE('',#33679,#34109,#30919,.T.);
#41909=EDGE_CURVE('',#34101,#34116,#29722,.T.);
#41910=EDGE_CURVE('',#34147,#34100,#30920,.T.);
#41911=EDGE_CURVE('',#34148,#34147,#2876,.T.);
#41912=EDGE_CURVE('',#34148,#34099,#29723,.T.);
#41913=EDGE_CURVE('',#34149,#34118,#30921,.T.);
#41914=EDGE_CURVE('',#34149,#34150,#29724,.T.);
#41915=EDGE_CURVE('',#34119,#34150,#29725,.T.);
#41916=EDGE_CURVE('',#34151,#34152,#2647,.T.);
#41917=EDGE_CURVE('',#34153,#34151,#30922,.T.);
#41918=EDGE_CURVE('',#34153,#34152,#29726,.T.);
#41919=EDGE_CURVE('',#34152,#34149,#29727,.T.);
#41920=EDGE_CURVE('',#34151,#34117,#30923,.T.);
#41921=EDGE_CURVE('',#34102,#34154,#29728,.T.);
#41922=EDGE_CURVE('',#34098,#34154,#29729,.T.);
#41923=EDGE_CURVE('',#34155,#34156,#2648,.T.);
#41924=EDGE_CURVE('',#34157,#34155,#29730,.T.);
#41925=EDGE_CURVE('',#34157,#34156,#29731,.T.);
#41926=EDGE_CURVE('',#34158,#34159,#2649,.T.);
#41927=EDGE_CURVE('',#34158,#34160,#29732,.T.);
#41928=EDGE_CURVE('',#34159,#34160,#2650,.T.);
#41929=EDGE_CURVE('',#34155,#34161,#29733,.T.);
#41930=EDGE_CURVE('',#34156,#34158,#29734,.T.);
#41931=EDGE_CURVE('',#34161,#34159,#30924,.T.);
#41932=EDGE_CURVE('',#34162,#34163,#29735,.T.);
#41933=EDGE_CURVE('',#34162,#34164,#29736,.T.);
#41934=EDGE_CURVE('',#34163,#34164,#29737,.T.);
#41935=EDGE_CURVE('',#34165,#34166,#2651,.T.);
#41936=EDGE_CURVE('',#34167,#34165,#29738,.T.);
#41937=EDGE_CURVE('',#34167,#34166,#29739,.T.);
#41938=EDGE_CURVE('',#34165,#34168,#29740,.T.);
#41939=EDGE_CURVE('',#34166,#34169,#2652,.T.);
#41940=EDGE_CURVE('',#34170,#34169,#30925,.T.);
#41941=EDGE_CURVE('',#34168,#34170,#2653,.T.);
#41942=EDGE_CURVE('',#34168,#34171,#29741,.T.);
#41943=EDGE_CURVE('',#34171,#34170,#2654,.T.);
#41944=EDGE_CURVE('',#34171,#34172,#29742,.T.);
#41945=EDGE_CURVE('',#34169,#34173,#29743,.T.);
#41946=EDGE_CURVE('',#34174,#34173,#30926,.T.);
#41947=EDGE_CURVE('',#34172,#34174,#29744,.T.);
#41948=EDGE_CURVE('',#34087,#33807,#30927,.T.);
#41949=EDGE_CURVE('',#34088,#33806,#30928,.T.);
#41950=EDGE_CURVE('',#34085,#34175,#29745,.T.);
#41951=EDGE_CURVE('',#34176,#34175,#30929,.T.);
#41952=EDGE_CURVE('',#34086,#34176,#30930,.T.);
#41953=EDGE_CURVE('',#33807,#34176,#30931,.T.);
#41954=EDGE_CURVE('',#34176,#34177,#2877,.T.);
#41955=EDGE_CURVE('',#34177,#33804,#30932,.T.);
#41956=EDGE_CURVE('',#34094,#33804,#30933,.T.);
#41957=EDGE_CURVE('',#34095,#34177,#30934,.T.);
#41958=EDGE_CURVE('',#34143,#34141,#30935,.T.);
#41959=EDGE_CURVE('',#34144,#34142,#2878,.T.);
#41960=EDGE_CURVE('',#34178,#34179,#2879,.T.);
#41961=EDGE_CURVE('',#34180,#34178,#2880,.T.);
#41962=EDGE_CURVE('',#34180,#33695,#2881,.T.);
#41963=EDGE_CURVE('',#33695,#34181,#2882,.T.);
#41964=EDGE_CURVE('',#34181,#34179,#29746,.T.);
#41965=EDGE_CURVE('',#34090,#34178,#30936,.T.);
#41966=EDGE_CURVE('',#34097,#34180,#30937,.T.);
#41967=EDGE_CURVE('',#34182,#34113,#30938,.T.);
#41968=EDGE_CURVE('',#34114,#34182,#29747,.T.);
#41969=EDGE_CURVE('',#34182,#34183,#29748,.T.);
#41970=EDGE_CURVE('',#34184,#34183,#29749,.T.);
#41971=EDGE_CURVE('',#34114,#34184,#29750,.T.);
#41972=EDGE_CURVE('',#34147,#34184,#30939,.T.);
#41973=EDGE_CURVE('',#34147,#34185,#29751,.T.);
#41974=EDGE_CURVE('',#34115,#34185,#29752,.T.);
#41975=EDGE_CURVE('',#34185,#34101,#29753,.T.);
#41976=EDGE_CURVE('',#34186,#34187,#29754,.T.);
#41977=EDGE_CURVE('',#34188,#34186,#30940,.T.);
#41978=EDGE_CURVE('',#34189,#34188,#29755,.T.);
#41979=EDGE_CURVE('',#34190,#34189,#2883,.T.);
#41980=EDGE_CURVE('',#34191,#34190,#29756,.T.);
#41981=EDGE_CURVE('',#34192,#34191,#30941,.T.);
#41982=EDGE_CURVE('',#34193,#34192,#29757,.T.);
#41983=EDGE_CURVE('',#34194,#34193,#29758,.T.);
#41984=EDGE_CURVE('',#34195,#34194,#2884,.T.);
#41985=EDGE_CURVE('',#34195,#34196,#29759,.T.);
#41986=EDGE_CURVE('',#34187,#34196,#2885,.T.);
#41987=EDGE_CURVE('',#34111,#34197,#30942,.T.);
#41988=EDGE_CURVE('',#34198,#34197,#30943,.T.);
#41989=EDGE_CURVE('',#34112,#34198,#30944,.T.);
#41990=EDGE_CURVE('',#34199,#34198,#30945,.T.);
#41991=EDGE_CURVE('',#34122,#34199,#30946,.T.);
#41992=EDGE_CURVE('',#34122,#34112,#30947,.T.);
#41993=EDGE_CURVE('',#34200,#34194,#2655,.T.);
#41994=EDGE_CURVE('',#34201,#34200,#2656,.T.);
#41995=EDGE_CURVE('',#34202,#34201,#2886,.T.);
#41996=EDGE_CURVE('',#34195,#34202,#30948,.T.);
#41997=EDGE_CURVE('',#34203,#34121,#2657,.T.);
#41998=EDGE_CURVE('',#34113,#34203,#2658,.T.);
#41999=EDGE_CURVE('',#34202,#33801,#29760,.T.);
#42000=EDGE_CURVE('',#34195,#33800,#29761,.T.);
#42001=EDGE_CURVE('',#34204,#33803,#29762,.T.);
#42002=EDGE_CURVE('',#34196,#34204,#29763,.T.);
#42003=EDGE_CURVE('',#34205,#34202,#29764,.T.);
#42004=EDGE_CURVE('',#34206,#34205,#29765,.T.);
#42005=EDGE_CURVE('',#33802,#34206,#29766,.T.);
#42006=EDGE_CURVE('',#34207,#33802,#1756,.T.);
#42007=EDGE_CURVE('',#34208,#34206,#29767,.T.);
#42008=EDGE_CURVE('',#34207,#34208,#29768,.T.);
#42009=EDGE_CURVE('',#34209,#33798,#2887,.T.);
#42010=EDGE_CURVE('',#34209,#34210,#2888,.T.);
#42011=EDGE_CURVE('',#34210,#34211,#29769,.T.);
#42012=EDGE_CURVE('',#34211,#34207,#30949,.T.);
#42013=EDGE_CURVE('',#34208,#34212,#2889,.T.);
#42014=EDGE_CURVE('',#33798,#34212,#2890,.T.);
#42015=EDGE_CURVE('',#34213,#33786,#30950,.T.);
#42016=EDGE_CURVE('',#34214,#33785,#30951,.T.);
#42017=EDGE_CURVE('',#34213,#34214,#2659,.T.);
#42018=EDGE_CURVE('',#34214,#34215,#2660,.T.);
#42019=EDGE_CURVE('',#34215,#34216,#2891,.T.);
#42020=EDGE_CURVE('',#34216,#34217,#30952,.T.);
#42021=EDGE_CURVE('',#34217,#34218,#30953,.T.);
#42022=EDGE_CURVE('',#34213,#34218,#2892,.T.);
#42023=EDGE_CURVE('',#34219,#34220,#2661,.T.);
#42024=EDGE_CURVE('',#34221,#34220,#2893,.T.);
#42025=EDGE_CURVE('',#34221,#34222,#2662,.T.);
#42026=EDGE_CURVE('',#34222,#34223,#2894,.T.);
#42027=EDGE_CURVE('',#34223,#34219,#2663,.T.);
#42028=EDGE_CURVE('',#34218,#34224,#29770,.T.);
#42029=EDGE_CURVE('',#34224,#34225,#2895,.T.);
#42030=EDGE_CURVE('',#34221,#34225,#29771,.T.);
#42031=EDGE_CURVE('',#34220,#34213,#29772,.T.);
#42032=EDGE_CURVE('',#34220,#33787,#2664,.T.);
#42033=EDGE_CURVE('',#34219,#33788,#30954,.T.);
#42034=EDGE_CURVE('',#34223,#33789,#30955,.T.);
#42035=EDGE_CURVE('',#34215,#33790,#2665,.T.);
#42036=EDGE_CURVE('',#34215,#34223,#29773,.T.);
#42037=EDGE_CURVE('',#34226,#34222,#29774,.T.);
#42038=EDGE_CURVE('',#34226,#34227,#2896,.T.);
#42039=EDGE_CURVE('',#34227,#34216,#29775,.T.);
#42040=EDGE_CURVE('',#34228,#34227,#29776,.T.);
#42041=EDGE_CURVE('',#34229,#34228,#29777,.T.);
#42042=EDGE_CURVE('',#34217,#34229,#29778,.T.);
#42043=EDGE_CURVE('',#34230,#34229,#29779,.T.);
#42044=EDGE_CURVE('',#34230,#34224,#29780,.T.);
#42045=EDGE_CURVE('',#34231,#34230,#29781,.T.);
#42046=EDGE_CURVE('',#34232,#34231,#2897,.T.);
#42047=EDGE_CURVE('',#34232,#34233,#29782,.T.);
#42048=EDGE_CURVE('',#34234,#34233,#2666,.T.);
#42049=EDGE_CURVE('',#34224,#34234,#29783,.T.);
#42050=EDGE_CURVE('',#34235,#34234,#2898,.T.);
#42051=EDGE_CURVE('',#34235,#34236,#29784,.T.);
#42052=EDGE_CURVE('',#34237,#34236,#2899,.T.);
#42053=EDGE_CURVE('',#34225,#34237,#29785,.T.);
#42054=EDGE_CURVE('',#34237,#33738,#29786,.T.);
#42055=EDGE_CURVE('',#33737,#34225,#29787,.T.);
#42056=EDGE_CURVE('',#33736,#34221,#29788,.T.);
#42057=EDGE_CURVE('',#33733,#34222,#29789,.T.);
#42058=EDGE_CURVE('',#33732,#34226,#29790,.T.);
#42059=EDGE_CURVE('',#34238,#33731,#30956,.T.);
#42060=EDGE_CURVE('',#34238,#34226,#29791,.T.);
#42061=EDGE_CURVE('',#34238,#34239,#2900,.T.);
#42062=EDGE_CURVE('',#34239,#34240,#29792,.T.);
#42063=EDGE_CURVE('',#34240,#34241,#2901,.T.);
#42064=EDGE_CURVE('',#34241,#34227,#29793,.T.);
#42065=EDGE_CURVE('',#34242,#34241,#2667,.T.);
#42066=EDGE_CURVE('',#34232,#34242,#29794,.T.);
#42067=EDGE_CURVE('',#34228,#34231,#29795,.T.);
#42068=EDGE_CURVE('',#33774,#34243,#29796,.T.);
#42069=EDGE_CURVE('',#34243,#34244,#29797,.T.);
#42070=EDGE_CURVE('',#34245,#34244,#2902,.T.);
#42071=EDGE_CURVE('',#34245,#34246,#29798,.T.);
#42072=EDGE_CURVE('',#34246,#33777,#29799,.T.);
#42073=EDGE_CURVE('',#34247,#33772,#29800,.T.);
#42074=EDGE_CURVE('',#33773,#34247,#29801,.T.);
#42075=EDGE_CURVE('',#34248,#34247,#30957,.T.);
#42076=EDGE_CURVE('',#34248,#34249,#29802,.T.);
#42077=EDGE_CURVE('',#34249,#34243,#1757,.T.);
#42078=EDGE_CURVE('',#34249,#34250,#29803,.T.);
#42079=EDGE_CURVE('',#34250,#34244,#30958,.T.);
#42080=EDGE_CURVE('',#34244,#34251,#29804,.T.);
#42081=EDGE_CURVE('',#34250,#34252,#29805,.T.);
#42082=EDGE_CURVE('',#34252,#34251,#29806,.T.);
#42083=EDGE_CURVE('',#34253,#34254,#29807,.T.);
#42084=EDGE_CURVE('',#34251,#34254,#2668,.T.);
#42085=EDGE_CURVE('',#34252,#34253,#30959,.T.);
#42086=EDGE_CURVE('',#34252,#34193,#29808,.T.);
#42087=EDGE_CURVE('',#34193,#34255,#29809,.T.);
#42088=EDGE_CURVE('',#34256,#34255,#29810,.T.);
#42089=EDGE_CURVE('',#34253,#34256,#29811,.T.);
#42090=EDGE_CURVE('',#34256,#34257,#30960,.T.);
#42091=EDGE_CURVE('',#34254,#34257,#29812,.T.);
#42092=EDGE_CURVE('',#34257,#34258,#29813,.T.);
#42093=EDGE_CURVE('',#34258,#34259,#29814,.T.);
#42094=EDGE_CURVE('',#34259,#34260,#29815,.T.);
#42095=EDGE_CURVE('',#34260,#34261,#29816,.T.);
#42096=EDGE_CURVE('',#34261,#34262,#29817,.T.);
#42097=EDGE_CURVE('',#34262,#34263,#29818,.T.);
#42098=EDGE_CURVE('',#34263,#34264,#29819,.T.);
#42099=EDGE_CURVE('',#34264,#34254,#2903,.T.);
#42100=EDGE_CURVE('',#34264,#34265,#2669,.T.);
#42101=EDGE_CURVE('',#34265,#34245,#29820,.T.);
#42102=EDGE_CURVE('',#34266,#34245,#30961,.T.);
#42103=EDGE_CURVE('',#34267,#34265,#29821,.T.);
#42104=EDGE_CURVE('',#34267,#34266,#29822,.T.);
#42105=EDGE_CURVE('',#34267,#34268,#29823,.T.);
#42106=EDGE_CURVE('',#34268,#34201,#29824,.T.);
#42107=EDGE_CURVE('',#34200,#34269,#29825,.T.);
#42108=EDGE_CURVE('',#34270,#34269,#29826,.T.);
#42109=EDGE_CURVE('',#34266,#34270,#29827,.T.);
#42110=EDGE_CURVE('',#34270,#34246,#29828,.T.);
#42111=EDGE_CURVE('',#34270,#34248,#29829,.T.);
#42112=EDGE_CURVE('',#34269,#34248,#29830,.T.);
#42113=EDGE_CURVE('',#34269,#34249,#29831,.T.);
#42114=EDGE_CURVE('',#34271,#34268,#29832,.T.);
#42115=EDGE_CURVE('',#34272,#34271,#30962,.T.);
#42116=EDGE_CURVE('',#34273,#34272,#29833,.T.);
#42117=EDGE_CURVE('',#34274,#34273,#2904,.T.);
#42118=EDGE_CURVE('',#34275,#34274,#29834,.T.);
#42119=EDGE_CURVE('',#34276,#34275,#30963,.T.);
#42120=EDGE_CURVE('',#34277,#34276,#29835,.T.);
#42121=EDGE_CURVE('',#34205,#34277,#2905,.T.);
#42122=EDGE_CURVE('',#34123,#34278,#30964,.T.);
#42123=EDGE_CURVE('',#34279,#34278,#29836,.T.);
#42124=EDGE_CURVE('',#34124,#34279,#2670,.T.);
#42125=EDGE_CURVE('',#34280,#34279,#29837,.T.);
#42126=EDGE_CURVE('',#34125,#34280,#29838,.T.);
#42127=EDGE_CURVE('',#34281,#34268,#29839,.T.);
#42128=EDGE_CURVE('',#34282,#34281,#29840,.T.);
#42129=EDGE_CURVE('',#34283,#34282,#29841,.T.);
#42130=EDGE_CURVE('',#34271,#34283,#30965,.T.);
#42131=EDGE_CURVE('',#34283,#34284,#29842,.T.);
#42132=EDGE_CURVE('',#34285,#34284,#30966,.T.);
#42133=EDGE_CURVE('',#34271,#34285,#29843,.T.);
#42134=EDGE_CURVE('',#34286,#34285,#30967,.T.);
#42135=EDGE_CURVE('',#34272,#34286,#30968,.T.);
#42136=EDGE_CURVE('',#34287,#34286,#29844,.T.);
#42137=EDGE_CURVE('',#34273,#34287,#29845,.T.);
#42138=EDGE_CURVE('',#34288,#34287,#2906,.T.);
#42139=EDGE_CURVE('',#34274,#34288,#30969,.T.);
#42140=EDGE_CURVE('',#34289,#34288,#29846,.T.);
#42141=EDGE_CURVE('',#34275,#34289,#30970,.T.);
#42142=EDGE_CURVE('',#34290,#34289,#30971,.T.);
#42143=EDGE_CURVE('',#34276,#34290,#30972,.T.);
#42144=EDGE_CURVE('',#34212,#34290,#29847,.T.);
#42145=EDGE_CURVE('',#34277,#34212,#29848,.T.);
#42146=EDGE_CURVE('',#34208,#34205,#29849,.T.);
#42147=EDGE_CURVE('',#34291,#34290,#2907,.T.);
#42148=EDGE_CURVE('',#34291,#34209,#29850,.T.);
#42149=EDGE_CURVE('',#34187,#34209,#30973,.T.);
#42150=EDGE_CURVE('',#34186,#34291,#30974,.T.);
#42151=EDGE_CURVE('',#34292,#34291,#30975,.T.);
#42152=EDGE_CURVE('',#34188,#34292,#30976,.T.);
#42153=EDGE_CURVE('',#34293,#34292,#29851,.T.);
#42154=EDGE_CURVE('',#34189,#34293,#30977,.T.);
#42155=EDGE_CURVE('',#34294,#34293,#2908,.T.);
#42156=EDGE_CURVE('',#34190,#34294,#2671,.T.);
#42157=EDGE_CURVE('',#34295,#34294,#29852,.T.);
#42158=EDGE_CURVE('',#34191,#34295,#30978,.T.);
#42159=EDGE_CURVE('',#34296,#34295,#30979,.T.);
#42160=EDGE_CURVE('',#34192,#34296,#30980,.T.);
#42161=EDGE_CURVE('',#34297,#34296,#29853,.T.);
#42162=EDGE_CURVE('',#34298,#34297,#29854,.T.);
#42163=EDGE_CURVE('',#34298,#34192,#30981,.T.);
#42164=EDGE_CURVE('',#34255,#34299,#29855,.T.);
#42165=EDGE_CURVE('',#34298,#34299,#29856,.T.);
#42166=EDGE_CURVE('',#34300,#34301,#29857,.T.);
#42167=EDGE_CURVE('',#34302,#34300,#29858,.T.);
#42168=EDGE_CURVE('',#34299,#34302,#29859,.T.);
#42169=EDGE_CURVE('',#34303,#34298,#30982,.T.);
#42170=EDGE_CURVE('',#34303,#34301,#29860,.T.);
#42171=EDGE_CURVE('',#34304,#34303,#29861,.T.);
#42172=EDGE_CURVE('',#34304,#34301,#2672,.T.);
#42173=EDGE_CURVE('',#34301,#34305,#29862,.T.);
#42174=EDGE_CURVE('',#34306,#34304,#29863,.T.);
#42175=EDGE_CURVE('',#34306,#34305,#2673,.T.);
#42176=EDGE_CURVE('',#34305,#34307,#29864,.T.);
#42177=EDGE_CURVE('',#34308,#34306,#29865,.T.);
#42178=EDGE_CURVE('',#34308,#34307,#2674,.T.);
#42179=EDGE_CURVE('',#34309,#34308,#29866,.T.);
#42180=EDGE_CURVE('',#34307,#34309,#29867,.T.);
#42181=EDGE_CURVE('',#34283,#34309,#30983,.T.);
#42182=EDGE_CURVE('',#34310,#34282,#29868,.T.);
#42183=EDGE_CURVE('',#34311,#34310,#29869,.T.);
#42184=EDGE_CURVE('',#34307,#34311,#29870,.T.);
#42185=EDGE_CURVE('',#34305,#34312,#2909,.T.);
#42186=EDGE_CURVE('',#34311,#34313,#29871,.T.);
#42187=EDGE_CURVE('',#34312,#34313,#29872,.T.);
#42188=EDGE_CURVE('',#34313,#34261,#30984,.T.);
#42189=EDGE_CURVE('',#34312,#34260,#30985,.T.);
#42190=EDGE_CURVE('',#34314,#34259,#30986,.T.);
#42191=EDGE_CURVE('',#34314,#34312,#29873,.T.);
#42192=EDGE_CURVE('',#34314,#34300,#29874,.T.);
#42193=EDGE_CURVE('',#34315,#34302,#29875,.T.);
#42194=EDGE_CURVE('',#34315,#34314,#29876,.T.);
#42195=EDGE_CURVE('',#34315,#34258,#30987,.T.);
#42196=EDGE_CURVE('',#34256,#34315,#29877,.T.);
#42197=EDGE_CURVE('',#34313,#34316,#29878,.T.);
#42198=EDGE_CURVE('',#34316,#34262,#30988,.T.);
#42199=EDGE_CURVE('',#34317,#34263,#29879,.T.);
#42200=EDGE_CURVE('',#34316,#34317,#29880,.T.);
#42201=EDGE_CURVE('',#34310,#34316,#29881,.T.);
#42202=EDGE_CURVE('',#34281,#34317,#29882,.T.);
#42203=EDGE_CURVE('',#34318,#34267,#30989,.T.);
#42204=EDGE_CURVE('',#34317,#34318,#29883,.T.);
#42205=EDGE_CURVE('',#34318,#34264,#30990,.T.);
#42206=EDGE_CURVE('',#34309,#34319,#29884,.T.);
#42207=EDGE_CURVE('',#34284,#34319,#30991,.T.);
#42208=EDGE_CURVE('',#34319,#34320,#29885,.T.);
#42209=EDGE_CURVE('',#34320,#34321,#29886,.T.);
#42210=EDGE_CURVE('',#34321,#34322,#29887,.T.);
#42211=EDGE_CURVE('',#34322,#34323,#29888,.T.);
#42212=EDGE_CURVE('',#34323,#34297,#30992,.T.);
#42213=EDGE_CURVE('',#34286,#34295,#2910,.T.);
#42214=EDGE_CURVE('',#34287,#34294,#2911,.T.);
#42215=EDGE_CURVE('',#33771,#34288,#2912,.T.);
#42216=EDGE_CURVE('',#34293,#33770,#2913,.T.);
#42217=EDGE_CURVE('',#34292,#34289,#2914,.T.);
#42218=EDGE_CURVE('',#34324,#34325,#30993,.T.);
#42219=EDGE_CURVE('',#34325,#34324,#2915,.T.);
#42220=EDGE_CURVE('',#34326,#34327,#2916,.T.);
#42221=EDGE_CURVE('',#34328,#34326,#29889,.T.);
#42222=EDGE_CURVE('',#34328,#34329,#2917,.T.);
#42223=EDGE_CURVE('',#34329,#34330,#29890,.T.);
#42224=EDGE_CURVE('',#34331,#34330,#2918,.T.);
#42225=EDGE_CURVE('',#34331,#34324,#29891,.T.);
#42226=EDGE_CURVE('',#34325,#34327,#29892,.T.);
#42227=EDGE_CURVE('',#34332,#34331,#30994,.T.);
#42228=EDGE_CURVE('',#34327,#34332,#30995,.T.);
#42229=EDGE_CURVE('',#34333,#34332,#2919,.T.);
#42230=EDGE_CURVE('',#34334,#34333,#30996,.T.);
#42231=EDGE_CURVE('',#34335,#34334,#30997,.T.);
#42232=EDGE_CURVE('',#34336,#34335,#29893,.T.);
#42233=EDGE_CURVE('',#34326,#34336,#30998,.T.);
#42234=EDGE_CURVE('',#34330,#34337,#30999,.T.);
#42235=EDGE_CURVE('',#34337,#34338,#29894,.T.);
#42236=EDGE_CURVE('',#34338,#34339,#31000,.T.);
#42237=EDGE_CURVE('',#34339,#34340,#31001,.T.);
#42238=EDGE_CURVE('',#34332,#34340,#2920,.T.);
#42239=EDGE_CURVE('',#34341,#34336,#31002,.T.);
#42240=EDGE_CURVE('',#34342,#34341,#31003,.T.);
#42241=EDGE_CURVE('',#34342,#34326,#31004,.T.);
#42242=EDGE_CURVE('',#34343,#34328,#31005,.T.);
#42243=EDGE_CURVE('',#34343,#34342,#29895,.T.);
#42244=EDGE_CURVE('',#34341,#34344,#29896,.T.);
#42245=EDGE_CURVE('',#34344,#34343,#2921,.T.);
#42246=EDGE_CURVE('',#34164,#34345,#2922,.T.);
#42247=EDGE_CURVE('',#34164,#34346,#29897,.T.);
#42248=EDGE_CURVE('',#34347,#34346,#31006,.T.);
#42249=EDGE_CURVE('',#34345,#34347,#1758,.T.);
#42250=EDGE_CURVE('',#34344,#34174,#29898,.T.);
#42251=EDGE_CURVE('',#34173,#34328,#2923,.T.);
#42252=EDGE_CURVE('',#34278,#34167,#2924,.T.);
#42253=EDGE_CURVE('',#34278,#34199,#31007,.T.);
#42254=EDGE_CURVE('',#34157,#34197,#2925,.T.);
#42255=EDGE_CURVE('',#34161,#34348,#29899,.T.);
#42256=EDGE_CURVE('',#34348,#34329,#2926,.T.);
#42257=EDGE_CURVE('',#34348,#34163,#31008,.T.);
#42258=EDGE_CURVE('',#34329,#34345,#31009,.T.);
#42259=EDGE_CURVE('',#34330,#34347,#31010,.T.);
#42260=EDGE_CURVE('',#34337,#34346,#1759,.T.);
#42261=EDGE_CURVE('',#34346,#34349,#29900,.T.);
#42262=EDGE_CURVE('',#34338,#34349,#29901,.T.);
#42263=EDGE_CURVE('',#34349,#33705,#31011,.T.);
#42264=EDGE_CURVE('',#34339,#33705,#31012,.T.);
#42265=EDGE_CURVE('',#34340,#33704,#29902,.T.);
#42266=EDGE_CURVE('',#34340,#34350,#29903,.T.);
#42267=EDGE_CURVE('',#34350,#33703,#1760,.T.);
#42268=EDGE_CURVE('',#34350,#34351,#29904,.T.);
#42269=EDGE_CURVE('',#33703,#34351,#29905,.T.);
#42270=EDGE_CURVE('',#34351,#33702,#2927,.T.);
#42271=EDGE_CURVE('',#34352,#33702,#2928,.T.);
#42272=EDGE_CURVE('',#34352,#34353,#29906,.T.);
#42273=EDGE_CURVE('',#34353,#34354,#29907,.T.);
#42274=EDGE_CURVE('',#34354,#34355,#29908,.T.);
#42275=EDGE_CURVE('',#34355,#34356,#2929,.T.);
#42276=EDGE_CURVE('',#34356,#34357,#29909,.T.);
#42277=EDGE_CURVE('',#34357,#34358,#29910,.T.);
#42278=EDGE_CURVE('',#34358,#34359,#29911,.T.);
#42279=EDGE_CURVE('',#34360,#34359,#2930,.T.);
#42280=EDGE_CURVE('',#34360,#34361,#2931,.T.);
#42281=EDGE_CURVE('',#34361,#34351,#2932,.T.);
#42282=EDGE_CURVE('',#34362,#34361,#29912,.T.);
#42283=EDGE_CURVE('',#34333,#34362,#29913,.T.);
#42284=EDGE_CURVE('',#34363,#34333,#29914,.T.);
#42285=EDGE_CURVE('',#34364,#34362,#29915,.T.);
#42286=EDGE_CURVE('',#34363,#34364,#29916,.T.);
#42287=EDGE_CURVE('',#34360,#34364,#31013,.T.);
#42288=EDGE_CURVE('',#34360,#34365,#31014,.T.);
#42289=EDGE_CURVE('',#34365,#34366,#31015,.T.);
#42290=EDGE_CURVE('',#34366,#34363,#31016,.T.);
#42291=EDGE_CURVE('',#34366,#34334,#31017,.T.);
#42292=EDGE_CURVE('',#34367,#34335,#29917,.T.);
#42293=EDGE_CURVE('',#34367,#34366,#31018,.T.);
#42294=EDGE_CURVE('',#34365,#34368,#31019,.T.);
#42295=EDGE_CURVE('',#34368,#34367,#29918,.T.);
#42296=EDGE_CURVE('',#34341,#34367,#29919,.T.);
#42297=EDGE_CURVE('',#34368,#34167,#29920,.T.);
#42298=EDGE_CURVE('',#34172,#34344,#29921,.T.);
#42299=EDGE_CURVE('',#34280,#34368,#2933,.T.);
#42300=EDGE_CURVE('',#34365,#34369,#2934,.T.);
#42301=EDGE_CURVE('',#34369,#34280,#2935,.T.);
#42302=EDGE_CURVE('',#34370,#34371,#2936,.T.);
#42303=EDGE_CURVE('',#34371,#34372,#2937,.T.);
#42304=EDGE_CURVE('',#34372,#33701,#2938,.T.);
#42305=EDGE_CURVE('',#34370,#33701,#31020,.T.);
#42306=EDGE_CURVE('',#34126,#34369,#31021,.T.);
#42307=EDGE_CURVE('',#34359,#34369,#31022,.T.);
#42308=EDGE_CURVE('',#34126,#34359,#31023,.T.);
#42309=EDGE_CURVE('',#34127,#34358,#29922,.T.);
#42310=EDGE_CURVE('',#34373,#34357,#29923,.T.);
#42311=EDGE_CURVE('',#34373,#34127,#29924,.T.);
#42312=EDGE_CURVE('',#34128,#34374,#29925,.T.);
#42313=EDGE_CURVE('',#34373,#34375,#2675,.T.);
#42314=EDGE_CURVE('',#34374,#34375,#29926,.T.);
#42315=EDGE_CURVE('',#34375,#34376,#2676,.T.);
#42316=EDGE_CURVE('',#34377,#34376,#29927,.T.);
#42317=EDGE_CURVE('',#34374,#34377,#31024,.T.);
#42318=EDGE_CURVE('',#34378,#34377,#29928,.T.);
#42319=EDGE_CURVE('',#34379,#34378,#29929,.T.);
#42320=EDGE_CURVE('',#34379,#34374,#29930,.T.);
#42321=EDGE_CURVE('',#34380,#34379,#2677,.T.);
#42322=EDGE_CURVE('',#34128,#34380,#29931,.T.);
#42323=EDGE_CURVE('',#34380,#34381,#29932,.T.);
#42324=EDGE_CURVE('',#34381,#34133,#29933,.T.);
#42325=EDGE_CURVE('',#33756,#34382,#2939,.T.);
#42326=EDGE_CURVE('',#34382,#34140,#2678,.T.);
#42327=EDGE_CURVE('',#34139,#34383,#31025,.T.);
#42328=EDGE_CURVE('',#33759,#34383,#29934,.T.);
#42329=EDGE_CURVE('',#34384,#34107,#29935,.T.);
#42330=EDGE_CURVE('',#34384,#33756,#29936,.T.);
#42331=EDGE_CURVE('',#34384,#34382,#29937,.T.);
#42332=EDGE_CURVE('',#34385,#33694,#2940,.T.);
#42333=EDGE_CURVE('',#34385,#34386,#29938,.T.);
#42334=EDGE_CURVE('',#33694,#34386,#2941,.T.);
#42335=EDGE_CURVE('',#34387,#34388,#29939,.T.);
#42336=EDGE_CURVE('',#34382,#34387,#29940,.T.);
#42337=EDGE_CURVE('',#34388,#34384,#29941,.T.);
#42338=EDGE_CURVE('',#34105,#34388,#29942,.T.);
#42339=EDGE_CURVE('',#34137,#34387,#29943,.T.);
#42340=EDGE_CURVE('',#34389,#34121,#31026,.T.);
#42341=EDGE_CURVE('',#34389,#34120,#29944,.T.);
#42342=EDGE_CURVE('',#34120,#34390,#1761,.T.);
#42343=EDGE_CURVE('',#34391,#34390,#29945,.T.);
#42344=EDGE_CURVE('',#34389,#34391,#29946,.T.);
#42345=EDGE_CURVE('',#34392,#34391,#29947,.T.);
#42346=EDGE_CURVE('',#34393,#34392,#31027,.T.);
#42347=EDGE_CURVE('',#34393,#34389,#2679,.T.);
#42348=EDGE_CURVE('',#34393,#34203,#31028,.T.);
#42349=EDGE_CURVE('',#34394,#34395,#31029,.T.);
#42350=EDGE_CURVE('',#34395,#34396,#29948,.T.);
#42351=EDGE_CURVE('',#34396,#34397,#31030,.T.);
#42352=EDGE_CURVE('',#34397,#34398,#29949,.T.);
#42353=EDGE_CURVE('',#34398,#34399,#29950,.T.);
#42354=EDGE_CURVE('',#34399,#34394,#29951,.T.);
#42355=EDGE_CURVE('',#34399,#34400,#31031,.T.);
#42356=EDGE_CURVE('',#34401,#34400,#29952,.T.);
#42357=EDGE_CURVE('',#34394,#34401,#31032,.T.);
#42358=EDGE_CURVE('',#34394,#34402,#29953,.T.);
#42359=EDGE_CURVE('',#34403,#34401,#29954,.T.);
#42360=EDGE_CURVE('',#34403,#34402,#31033,.T.);
#42361=EDGE_CURVE('',#33754,#34403,#29955,.T.);
#42362=EDGE_CURVE('',#33754,#34404,#31034,.T.);
#42363=EDGE_CURVE('',#34404,#34402,#29956,.T.);
#42364=EDGE_CURVE('',#34404,#34395,#29957,.T.);
#42365=EDGE_CURVE('',#33753,#34395,#31035,.T.);
#42366=EDGE_CURVE('',#33751,#34396,#31036,.T.);
#42367=EDGE_CURVE('',#33750,#34405,#31037,.T.);
#42368=EDGE_CURVE('',#34396,#34405,#29958,.T.);
#42369=EDGE_CURVE('',#34406,#34397,#29959,.T.);
#42370=EDGE_CURVE('',#34406,#34405,#29960,.T.);
#42371=EDGE_CURVE('',#34407,#33750,#29961,.T.);
#42372=EDGE_CURVE('',#34406,#34407,#31038,.T.);
#42373=EDGE_CURVE('',#34408,#34407,#29962,.T.);
#42374=EDGE_CURVE('',#34397,#34408,#31039,.T.);
#42375=EDGE_CURVE('',#34409,#34408,#29963,.T.);
#42376=EDGE_CURVE('',#34398,#34409,#31040,.T.);
#42377=EDGE_CURVE('',#34410,#34409,#29964,.T.);
#42378=EDGE_CURVE('',#34400,#34410,#29965,.T.);
#42379=EDGE_CURVE('',#34409,#34411,#31041,.T.);
#42380=EDGE_CURVE('',#34412,#34411,#31042,.T.);
#42381=EDGE_CURVE('',#34413,#34412,#31043,.T.);
#42382=EDGE_CURVE('',#34414,#34413,#31044,.T.);
#42383=EDGE_CURVE('',#34414,#34400,#31045,.T.);
#42384=EDGE_CURVE('',#34403,#34414,#2942,.T.);
#42385=EDGE_CURVE('',#34415,#33755,#29966,.T.);
#42386=EDGE_CURVE('',#34416,#34414,#31046,.T.);
#42387=EDGE_CURVE('',#34417,#34416,#2943,.T.);
#42388=EDGE_CURVE('',#34417,#34418,#29967,.T.);
#42389=EDGE_CURVE('',#34419,#34418,#2944,.T.);
#42390=EDGE_CURVE('',#34420,#34419,#31047,.T.);
#42391=EDGE_CURVE('',#34420,#34415,#2945,.T.);
#42392=EDGE_CURVE('',#34421,#34422,#29968,.T.);
#42393=EDGE_CURVE('',#34422,#34415,#29969,.T.);
#42394=EDGE_CURVE('',#34421,#34420,#31048,.T.);
#42395=EDGE_CURVE('',#34423,#34424,#29970,.T.);
#42396=EDGE_CURVE('',#34424,#34421,#29971,.T.);
#42397=EDGE_CURVE('',#34425,#34420,#31049,.T.);
#42398=EDGE_CURVE('',#34426,#34425,#31050,.T.);
#42399=EDGE_CURVE('',#34427,#34426,#31051,.T.);
#42400=EDGE_CURVE('',#34427,#34423,#31052,.T.);
#42401=EDGE_CURVE('',#34428,#34429,#29972,.T.);
#42402=EDGE_CURVE('',#34429,#34423,#29973,.T.);
#42403=EDGE_CURVE('',#34428,#34427,#2946,.T.);
#42404=EDGE_CURVE('',#33749,#34428,#29974,.T.);
#42405=EDGE_CURVE('',#34430,#34427,#31053,.T.);
#42406=EDGE_CURVE('',#34430,#34431,#2947,.T.);
#42407=EDGE_CURVE('',#34431,#34432,#29975,.T.);
#42408=EDGE_CURVE('',#34433,#34432,#2948,.T.);
#42409=EDGE_CURVE('',#34433,#34434,#29976,.T.);
#42410=EDGE_CURVE('',#34434,#34435,#2949,.T.);
#42411=EDGE_CURVE('',#34411,#34435,#31054,.T.);
#42412=EDGE_CURVE('',#34411,#34407,#2950,.T.);
#42413=EDGE_CURVE('',#33748,#34436,#31055,.T.);
#42414=EDGE_CURVE('',#34437,#34436,#29977,.T.);
#42415=EDGE_CURVE('',#33749,#34437,#31056,.T.);
#42416=EDGE_CURVE('',#34437,#34438,#29978,.T.);
#42417=EDGE_CURVE('',#34428,#34438,#31057,.T.);
#42418=EDGE_CURVE('',#34439,#34438,#29979,.T.);
#42419=EDGE_CURVE('',#34439,#34429,#31058,.T.);
#42420=EDGE_CURVE('',#34440,#34439,#29980,.T.);
#42421=EDGE_CURVE('',#34440,#34423,#31059,.T.);
#42422=EDGE_CURVE('',#34441,#34440,#29981,.F.);
#42423=EDGE_CURVE('',#34441,#34421,#31060,.T.);
#42424=EDGE_CURVE('',#34442,#34441,#29982,.T.);
#42425=EDGE_CURVE('',#34442,#34422,#31061,.T.);
#42426=EDGE_CURVE('',#34443,#34442,#29983,.T.);
#42427=EDGE_CURVE('',#34443,#34415,#31062,.T.);
#42428=EDGE_CURVE('',#34443,#34444,#29984,.T.);
#42429=EDGE_CURVE('',#33755,#34444,#31063,.T.);
#42430=EDGE_CURVE('',#34445,#34444,#29985,.T.);
#42431=EDGE_CURVE('',#33746,#34445,#31064,.T.);
#42432=EDGE_CURVE('',#34436,#34445,#29986,.T.);
#42433=EDGE_CURVE('',#34439,#34436,#31065,.T.);
#42434=EDGE_CURVE('',#34445,#34442,#31066,.T.);
#42435=EDGE_CURVE('',#34412,#34446,#31067,.T.);
#42436=EDGE_CURVE('',#34446,#34435,#31068,.T.);
#42437=EDGE_CURVE('',#34446,#33744,#31069,.T.);
#42438=EDGE_CURVE('',#34435,#33696,#31070,.T.);
#42439=EDGE_CURVE('',#33697,#34416,#31071,.T.);
#42440=EDGE_CURVE('',#34416,#34447,#31072,.T.);
#42441=EDGE_CURVE('',#33745,#34447,#31073,.T.);
#42442=EDGE_CURVE('',#34447,#34413,#31074,.T.);
#42443=EDGE_CURVE('',#33700,#34417,#29987,.T.);
#42444=EDGE_CURVE('',#33726,#34417,#29988,.T.);
#42445=EDGE_CURVE('',#33727,#33700,#29989,.T.);
#42446=EDGE_CURVE('',#33728,#33698,#31075,.T.);
#42447=EDGE_CURVE('',#34448,#33698,#29990,.T.);
#42448=EDGE_CURVE('',#33729,#34448,#29991,.T.);
#42449=EDGE_CURVE('',#33729,#34449,#29992,.T.);
#42450=EDGE_CURVE('',#34434,#34448,#29993,.T.);
#42451=EDGE_CURVE('',#34449,#34434,#29994,.T.);
#42452=EDGE_CURVE('',#34433,#34449,#29995,.T.);
#42453=EDGE_CURVE('',#33739,#33730,#29996,.T.);
#42454=EDGE_CURVE('',#34433,#34450,#29997,.T.);
#42455=EDGE_CURVE('',#34450,#34432,#29998,.T.);
#42456=EDGE_CURVE('',#34451,#34432,#29999,.T.);
#42457=EDGE_CURVE('',#34451,#33740,#30000,.T.);
#42458=EDGE_CURVE('',#33743,#34418,#30001,.T.);
#42459=EDGE_CURVE('',#33742,#33723,#30002,.T.);
#42460=EDGE_CURVE('',#34418,#33723,#30003,.T.);
#42461=EDGE_CURVE('',#34419,#33718,#31076,.T.);
#42462=EDGE_CURVE('',#33719,#34430,#31077,.T.);
#42463=EDGE_CURVE('',#33724,#34452,#30004,.T.);
#42464=EDGE_CURVE('',#34431,#34452,#30005,.T.);
#42465=EDGE_CURVE('',#34451,#34431,#30006,.T.);
#42466=EDGE_CURVE('',#33740,#34452,#30007,.T.);
#42467=EDGE_CURVE('',#33741,#33724,#31078,.T.);
#42468=EDGE_CURVE('',#34430,#34453,#31079,.T.);
#42469=EDGE_CURVE('',#33720,#34453,#31080,.T.);
#42470=EDGE_CURVE('',#34454,#33721,#31081,.T.);
#42471=EDGE_CURVE('',#34454,#34419,#31082,.T.);
#42472=EDGE_CURVE('',#34425,#34454,#31083,.T.);
#42473=EDGE_CURVE('',#34453,#34426,#31084,.T.);
#42474=EDGE_CURVE('',#34238,#34455,#30008,.T.);
#42475=EDGE_CURVE('',#34455,#33730,#30009,.T.);
#42476=EDGE_CURVE('',#34455,#34456,#30010,.T.);
#42477=EDGE_CURVE('',#34456,#33739,#31085,.T.);
#42478=EDGE_CURVE('',#34456,#34237,#30011,.T.);
#42479=EDGE_CURVE('',#34236,#34457,#30012,.T.);
#42480=EDGE_CURVE('',#34457,#34458,#30013,.T.);
#42481=EDGE_CURVE('',#34458,#34239,#30014,.T.);
#42482=EDGE_CURVE('',#34458,#34459,#30015,.T.);
#42483=EDGE_CURVE('',#34460,#34459,#30016,.T.);
#42484=EDGE_CURVE('',#34239,#34460,#31086,.T.);
#42485=EDGE_CURVE('',#34461,#34460,#30017,.T.);
#42486=EDGE_CURVE('',#34240,#34461,#31087,.T.);
#42487=EDGE_CURVE('',#34462,#34461,#30018,.T.);
#42488=EDGE_CURVE('',#34462,#34463,#31088,.T.);
#42489=EDGE_CURVE('',#34240,#34463,#30019,.T.);
#42490=EDGE_CURVE('',#34463,#34242,#30020,.T.);
#42491=EDGE_CURVE('',#34464,#34462,#30021,.T.);
#42492=EDGE_CURVE('',#34464,#34242,#31089,.T.);
#42493=EDGE_CURVE('',#34465,#34464,#30022,.T.);
#42494=EDGE_CURVE('',#34465,#34232,#30023,.T.);
#42495=EDGE_CURVE('',#34466,#34465,#30024,.T.);
#42496=EDGE_CURVE('',#34466,#34233,#30025,.T.);
#42497=EDGE_CURVE('',#34467,#34466,#30026,.T.);
#42498=EDGE_CURVE('',#34467,#34468,#31090,.T.);
#42499=EDGE_CURVE('',#34233,#34468,#30027,.T.);
#42500=EDGE_CURVE('',#34468,#34235,#30028,.T.);
#42501=EDGE_CURVE('',#34469,#34467,#30029,.T.);
#42502=EDGE_CURVE('',#34469,#34235,#31091,.T.);
#42503=EDGE_CURVE('',#34470,#34469,#30030,.T.);
#42504=EDGE_CURVE('',#34236,#34470,#31092,.T.);
#42505=EDGE_CURVE('',#34471,#34470,#30031,.T.);
#42506=EDGE_CURVE('',#34457,#34471,#30032,.T.);
#42507=EDGE_CURVE('',#34459,#34471,#30033,.F.);
#42508=EDGE_CURVE('',#34462,#34459,#31093,.T.);
#42509=EDGE_CURVE('',#34471,#34467,#31094,.T.);
#42510=EDGE_CURVE('',#33708,#33709,#31095,.T.);
#42511=EDGE_CURVE('',#33763,#34472,#2951,.T.);
#42512=EDGE_CURVE('',#34472,#34356,#31096,.T.);
#42513=EDGE_CURVE('',#34355,#34473,#31097,.T.);
#42514=EDGE_CURVE('',#34473,#33762,#2952,.T.);
#42515=EDGE_CURVE('',#34473,#34474,#30034,.T.);
#42516=EDGE_CURVE('',#34474,#34475,#30035,.T.);
#42517=EDGE_CURVE('',#34475,#34476,#30036,.T.);
#42518=EDGE_CURVE('',#34476,#34477,#30037,.T.);
#42519=EDGE_CURVE('',#34478,#34477,#2953,.T.);
#42520=EDGE_CURVE('',#34478,#34378,#30038,.T.);
#42521=EDGE_CURVE('',#34376,#34472,#30039,.T.);
#42522=EDGE_CURVE('',#34479,#34472,#31098,.T.);
#42523=EDGE_CURVE('',#34375,#34479,#31099,.T.);
#42524=EDGE_CURVE('',#34479,#34373,#30040,.T.);
#42525=EDGE_CURVE('',#34479,#34356,#31100,.T.);
#42526=EDGE_CURVE('',#34480,#34478,#1762,.T.);
#42527=EDGE_CURVE('',#34480,#34379,#30041,.T.);
#42528=EDGE_CURVE('',#34381,#34481,#30042,.T.);
#42529=EDGE_CURVE('',#34482,#34480,#30043,.T.);
#42530=EDGE_CURVE('',#34481,#34482,#30044,.T.);
#42531=EDGE_CURVE('',#34482,#34477,#1763,.T.);
#42532=EDGE_CURVE('',#34481,#34476,#30045,.T.);
#42533=EDGE_CURVE('',#34483,#34475,#2680,.T.);
#42534=EDGE_CURVE('',#34483,#34481,#30046,.T.);
#42535=EDGE_CURVE('',#34133,#34483,#30047,.T.);
#42536=EDGE_CURVE('',#34484,#34483,#30048,.T.);
#42537=EDGE_CURVE('',#34484,#34485,#2681,.T.);
#42538=EDGE_CURVE('',#34134,#34485,#30049,.T.);
#42539=EDGE_CURVE('',#34485,#34354,#30050,.T.);
#42540=EDGE_CURVE('',#34134,#34353,#30051,.T.);
#42541=EDGE_CURVE('',#34135,#34352,#31101,.T.);
#42542=EDGE_CURVE('',#34372,#34352,#31102,.T.);
#42543=EDGE_CURVE('',#34135,#34372,#31103,.T.);
#42544=EDGE_CURVE('',#34136,#34371,#30052,.T.);
#42545=EDGE_CURVE('',#34486,#34371,#30053,.T.);
#42546=EDGE_CURVE('',#34110,#34486,#30054,.T.);
#42547=EDGE_CURVE('',#34197,#34486,#30055,.T.);
#42548=EDGE_CURVE('',#34157,#34370,#30056,.T.);
#42549=EDGE_CURVE('',#34370,#34349,#1764,.T.);
#42550=EDGE_CURVE('',#34160,#34162,#30057,.T.);
#42551=EDGE_CURVE('',#34487,#34355,#31104,.T.);
#42552=EDGE_CURVE('',#34485,#34487,#30058,.T.);
#42553=EDGE_CURVE('',#34487,#34484,#31105,.T.);
#42554=EDGE_CURVE('',#34484,#34474,#31106,.T.);
#42555=EDGE_CURVE('',#34487,#34473,#31107,.T.);
#42556=EDGE_CURVE('',#34477,#34478,#30059,.T.);
#42557=EDGE_CURVE('',#34383,#33691,#30060,.T.);
#42558=EDGE_CURVE('',#34146,#34385,#30061,.T.);
#42559=EDGE_CURVE('',#34488,#33691,#2954,.T.);
#42560=EDGE_CURVE('',#34488,#34180,#31108,.T.);
#42561=EDGE_CURVE('',#34488,#34096,#1765,.T.);
#42562=EDGE_CURVE('',#34096,#34489,#31109,.T.);
#42563=EDGE_CURVE('',#34488,#34489,#30062,.T.);
#42564=EDGE_CURVE('',#33759,#34490,#2955,.T.);
#42565=EDGE_CURVE('',#34489,#34177,#31110,.T.);
#42566=EDGE_CURVE('',#34175,#34490,#30063,.T.);
#42567=EDGE_CURVE('',#33805,#34144,#31111,.T.);
#42568=EDGE_CURVE('',#34142,#33806,#31112,.T.);
#42569=EDGE_CURVE('',#34106,#34083,#31113,.T.);
#42570=EDGE_CURVE('',#34084,#34108,#31114,.T.);
#42571=EDGE_CURVE('',#34108,#34490,#31115,.T.);
#42572=EDGE_CURVE('',#34085,#34490,#30064,.T.);
#42573=EDGE_CURVE('',#34093,#33805,#31116,.T.);
#42574=EDGE_CURVE('',#34386,#34181,#31117,.T.);
#42575=EDGE_CURVE('',#34386,#34491,#30065,.T.);
#42576=EDGE_CURVE('',#34491,#34179,#30066,.T.);
#42577=EDGE_CURVE('',#34491,#34492,#30067,.T.);
#42578=EDGE_CURVE('',#34385,#34492,#31118,.T.);
#42579=EDGE_CURVE('',#34492,#34145,#30068,.T.);
#42580=EDGE_CURVE('',#34182,#34393,#2682,.T.);
#42581=EDGE_CURVE('',#34183,#34392,#30069,.T.);
#42582=EDGE_CURVE('',#34390,#34148,#31119,.T.);
#42583=EDGE_CURVE('',#34150,#34148,#30070,.T.);
#42584=EDGE_CURVE('',#34154,#34153,#30071,.T.);
#42585=EDGE_CURVE('',#34364,#34361,#30072,.T.);
#42586=EDGE_CURVE('',#34303,#34323,#30073,.T.);
#42587=EDGE_CURVE('',#34304,#34322,#30074,.T.);
#42588=EDGE_CURVE('',#34306,#34321,#31120,.T.);
#42589=EDGE_CURVE('',#34308,#34320,#30075,.T.);
#42590=EDGE_CURVE('',#34196,#34210,#30076,.T.);
#42591=EDGE_CURVE('',#34210,#34204,#31121,.T.);
#42592=EDGE_CURVE('',#34211,#33803,#30077,.T.);
#42593=EDGE_CURVE('',#34082,#34089,#31122,.T.);
#42594=EDGE_CURVE('',#34493,#34494,#31123,.T.);
#42595=EDGE_CURVE('',#34495,#34493,#30078,.T.);
#42596=EDGE_CURVE('',#34496,#34495,#31124,.T.);
#42597=EDGE_CURVE('',#34497,#34496,#30079,.T.);
#42598=EDGE_CURVE('',#34494,#34497,#31125,.T.);
#42599=EDGE_CURVE('',#34498,#34499,#30080,.T.);
#42600=EDGE_CURVE('',#34500,#34498,#30081,.T.);
#42601=EDGE_CURVE('',#34493,#34500,#30082,.T.);
#42602=EDGE_CURVE('',#34494,#34501,#2956,.T.);
#42603=EDGE_CURVE('',#34501,#34502,#30083,.T.);
#42604=EDGE_CURVE('',#34502,#34503,#2957,.T.);
#42605=EDGE_CURVE('',#34503,#34504,#2683,.T.);
#42606=EDGE_CURVE('',#34504,#34505,#31126,.T.);
#42607=EDGE_CURVE('',#34505,#34503,#2684,.T.);
#42608=EDGE_CURVE('',#34502,#34501,#30084,.T.);
#42609=EDGE_CURVE('',#34506,#34497,#30085,.T.);
#42610=EDGE_CURVE('',#34507,#34506,#30086,.T.);
#42611=EDGE_CURVE('',#34499,#34507,#30087,.T.);
#42612=EDGE_CURVE('',#34508,#34509,#30088,.T.);
#42613=EDGE_CURVE('',#34509,#34510,#30089,.T.);
#42614=EDGE_CURVE('',#34510,#34511,#2958,.T.);
#42615=EDGE_CURVE('',#34511,#34512,#30090,.T.);
#42616=EDGE_CURVE('',#34512,#34513,#30091,.T.);
#42617=EDGE_CURVE('',#34508,#34513,#2959,.T.);
#42618=EDGE_CURVE('',#34514,#34515,#31127,.T.);
#42619=EDGE_CURVE('',#34516,#34514,#2685,.T.);
#42620=EDGE_CURVE('',#34516,#34517,#2960,.T.);
#42621=EDGE_CURVE('',#34517,#34518,#30092,.T.);
#42622=EDGE_CURVE('',#34518,#34519,#2961,.T.);
#42623=EDGE_CURVE('',#34520,#34519,#31128,.T.);
#42624=EDGE_CURVE('',#34519,#34520,#31129,.T.);
#42625=EDGE_CURVE('',#34518,#34517,#30093,.T.);
#42626=EDGE_CURVE('',#34515,#34516,#2686,.T.);
#42627=EDGE_CURVE('',#34501,#34518,#2962,.T.);
#42628=EDGE_CURVE('',#34515,#34521,#2687,.T.);
#42629=EDGE_CURVE('',#34522,#34521,#31130,.T.);
#42630=EDGE_CURVE('',#34522,#34514,#2688,.T.);
#42631=EDGE_CURVE('',#34520,#34523,#31131,.T.);
#42632=EDGE_CURVE('',#34523,#34523,#31132,.T.);
#42633=EDGE_CURVE('',#34524,#34525,#30094,.T.);
#42634=EDGE_CURVE('',#34525,#34526,#30095,.T.);
#42635=EDGE_CURVE('',#34526,#34527,#30096,.T.);
#42636=EDGE_CURVE('',#34528,#34527,#31133,.T.);
#42637=EDGE_CURVE('',#34524,#34528,#31134,.T.);
#42638=EDGE_CURVE('',#34529,#34530,#30097,.T.);
#42639=EDGE_CURVE('',#34530,#34531,#30098,.T.);
#42640=EDGE_CURVE('',#34531,#34532,#31135,.T.);
#42641=EDGE_CURVE('',#34533,#34532,#31136,.T.);
#42642=EDGE_CURVE('',#34533,#34529,#30099,.T.);
#42643=EDGE_CURVE('',#34534,#34535,#30100,.T.);
#42644=EDGE_CURVE('',#34534,#34536,#2963,.T.);
#42645=EDGE_CURVE('',#34536,#34536,#31137,.T.);
#42646=EDGE_CURVE('',#34535,#34534,#30101,.T.);
#42647=EDGE_CURVE('',#34537,#34538,#2964,.T.);
#42648=EDGE_CURVE('',#34539,#34538,#2965,.T.);
#42649=EDGE_CURVE('',#34540,#34539,#2966,.T.);
#42650=EDGE_CURVE('',#34540,#34537,#2967,.T.);
#42651=EDGE_CURVE('',#34541,#34537,#31138,.T.);
#42652=EDGE_CURVE('',#34542,#34540,#31139,.T.);
#42653=EDGE_CURVE('',#34542,#34541,#2968,.T.);
#42654=EDGE_CURVE('',#34538,#34543,#31140,.T.);
#42655=EDGE_CURVE('',#34543,#34541,#2969,.T.);
#42656=EDGE_CURVE('',#34544,#34539,#31141,.T.);
#42657=EDGE_CURVE('',#34544,#34543,#2970,.T.);
#42658=EDGE_CURVE('',#34544,#34542,#2971,.T.);
#42659=EDGE_CURVE('',#34545,#34546,#31142,.T.);
#42660=EDGE_CURVE('',#34546,#34547,#2972,.T.);
#42661=EDGE_CURVE('',#34547,#34548,#31143,.T.);
#42662=EDGE_CURVE('',#34548,#34545,#2973,.T.);
#42663=EDGE_CURVE('',#34549,#34546,#2974,.T.);
#42664=EDGE_CURVE('',#34550,#34545,#2975,.T.);
#42665=EDGE_CURVE('',#34550,#34549,#31144,.T.);
#42666=EDGE_CURVE('',#34551,#34547,#2976,.T.);
#42667=EDGE_CURVE('',#34549,#34551,#2977,.T.);
#42668=EDGE_CURVE('',#34552,#34548,#2978,.T.);
#42669=EDGE_CURVE('',#34552,#34551,#31145,.T.);
#42670=EDGE_CURVE('',#34552,#34550,#2979,.T.);
#42671=EDGE_CURVE('',#34553,#34554,#2980,.T.);
#42672=EDGE_CURVE('',#34553,#34555,#2981,.T.);
#42673=EDGE_CURVE('',#34555,#34556,#2982,.T.);
#42674=EDGE_CURVE('',#34556,#34554,#2983,.T.);
#42675=EDGE_CURVE('',#34555,#34557,#31146,.T.);
#42676=EDGE_CURVE('',#34557,#34558,#2984,.T.);
#42677=EDGE_CURVE('',#34558,#34556,#31147,.T.);
#42678=EDGE_CURVE('',#34557,#34559,#2985,.T.);
#42679=EDGE_CURVE('',#34559,#34560,#2986,.T.);
#42680=EDGE_CURVE('',#34560,#34558,#2987,.T.);
#42681=EDGE_CURVE('',#34559,#34561,#31148,.T.);
#42682=EDGE_CURVE('',#34561,#34562,#2988,.T.);
#42683=EDGE_CURVE('',#34562,#34560,#31149,.T.);
#42684=EDGE_CURVE('',#34561,#34563,#2989,.T.);
#42685=EDGE_CURVE('',#34563,#34564,#2990,.T.);
#42686=EDGE_CURVE('',#34564,#34562,#2991,.T.);
#42687=EDGE_CURVE('',#34565,#34562,#31150,.T.);
#42688=EDGE_CURVE('',#34566,#34564,#31151,.T.);
#42689=EDGE_CURVE('',#34566,#34565,#2992,.T.);
#42690=EDGE_CURVE('',#34567,#34560,#31152,.T.);
#42691=EDGE_CURVE('',#34565,#34567,#31153,.T.);
#42692=EDGE_CURVE('',#34568,#34558,#31154,.T.);
#42693=EDGE_CURVE('',#34567,#34568,#2993,.T.);
#42694=EDGE_CURVE('',#34569,#34556,#31155,.T.);
#42695=EDGE_CURVE('',#34568,#34569,#31156,.T.);
#42696=EDGE_CURVE('',#34570,#34554,#31157,.T.);
#42697=EDGE_CURVE('',#34569,#34570,#2994,.T.);
#42698=EDGE_CURVE('',#34571,#34572,#31158,.T.);
#42699=EDGE_CURVE('',#34554,#34572,#31159,.T.);
#42700=EDGE_CURVE('',#34570,#34571,#31160,.T.);
#42701=EDGE_CURVE('',#34573,#34572,#2995,.T.);
#42702=EDGE_CURVE('',#34573,#34553,#31161,.T.);
#42703=EDGE_CURVE('',#34572,#34574,#2996,.T.);
#42704=EDGE_CURVE('',#34574,#34575,#2997,.T.);
#42705=EDGE_CURVE('',#34575,#34573,#2998,.T.);
#42706=EDGE_CURVE('',#34571,#34529,#30102,.T.);
#42707=EDGE_CURVE('',#34529,#34574,#30103,.T.);
#42708=EDGE_CURVE('',#34533,#34574,#31162,.T.);
#42709=EDGE_CURVE('',#34533,#34576,#2999,.T.);
#42710=EDGE_CURVE('',#34576,#34575,#2689,.T.);
#42711=EDGE_CURVE('',#34534,#34577,#31163,.T.);
#42712=EDGE_CURVE('',#34535,#34578,#31164,.T.);
#42713=EDGE_CURVE('',#34577,#34578,#30104,.T.);
#42714=EDGE_CURVE('',#34578,#34577,#30105,.T.);
#42715=EDGE_CURVE('',#34579,#34528,#3000,.T.);
#42716=EDGE_CURVE('',#34527,#34580,#3001,.T.);
#42717=EDGE_CURVE('',#34580,#34579,#2690,.T.);
#42718=EDGE_CURVE('',#34581,#34532,#3002,.T.);
#42719=EDGE_CURVE('',#34532,#34528,#3003,.T.);
#42720=EDGE_CURVE('',#34579,#34581,#3004,.T.);
#42721=EDGE_CURVE('',#34581,#34576,#2691,.T.);
#42722=EDGE_CURVE('',#34531,#34524,#3005,.T.);
#42723=EDGE_CURVE('',#34582,#34526,#30106,.T.);
#42724=EDGE_CURVE('',#34582,#34527,#31165,.T.);
#42725=EDGE_CURVE('',#34526,#34583,#30107,.T.);
#42726=EDGE_CURVE('',#34583,#34584,#31166,.T.);
#42727=EDGE_CURVE('',#34582,#34584,#3006,.T.);
#42728=EDGE_CURVE('',#34584,#34564,#31167,.T.);
#42729=EDGE_CURVE('',#34583,#34566,#31168,.T.);
#42730=EDGE_CURVE('',#34563,#34585,#31169,.T.);
#42731=EDGE_CURVE('',#34585,#34584,#3007,.T.);
#42732=EDGE_CURVE('',#34582,#34586,#3008,.T.);
#42733=EDGE_CURVE('',#34585,#34586,#3009,.T.);
#42734=EDGE_CURVE('',#34586,#34580,#2692,.T.);
#42735=EDGE_CURVE('',#34586,#34575,#3010,.T.);
#42736=EDGE_CURVE('',#34587,#34588,#3011,.T.);
#42737=EDGE_CURVE('',#34589,#34587,#3012,.T.);
#42738=EDGE_CURVE('',#34590,#34589,#3013,.T.);
#42739=EDGE_CURVE('',#34591,#34590,#3014,.T.);
#42740=EDGE_CURVE('',#34592,#34591,#3015,.T.);
#42741=EDGE_CURVE('',#34593,#34592,#3016,.T.);
#42742=EDGE_CURVE('',#34594,#34593,#3017,.T.);
#42743=EDGE_CURVE('',#34588,#34594,#3018,.T.);
#42744=EDGE_CURVE('',#34587,#34595,#3019,.T.);
#42745=EDGE_CURVE('',#34588,#34596,#3020,.T.);
#42746=EDGE_CURVE('',#34596,#34595,#3021,.T.);
#42747=EDGE_CURVE('',#34589,#34597,#3022,.T.);
#42748=EDGE_CURVE('',#34595,#34597,#3023,.T.);
#42749=EDGE_CURVE('',#34590,#34598,#3024,.T.);
#42750=EDGE_CURVE('',#34597,#34598,#3025,.T.);
#42751=EDGE_CURVE('',#34591,#34599,#3026,.T.);
#42752=EDGE_CURVE('',#34598,#34599,#3027,.T.);
#42753=EDGE_CURVE('',#34592,#34600,#3028,.T.);
#42754=EDGE_CURVE('',#34599,#34600,#3029,.T.);
#42755=EDGE_CURVE('',#34593,#34601,#3030,.T.);
#42756=EDGE_CURVE('',#34600,#34601,#3031,.T.);
#42757=EDGE_CURVE('',#34594,#34602,#3032,.T.);
#42758=EDGE_CURVE('',#34601,#34602,#3033,.T.);
#42759=EDGE_CURVE('',#34602,#34596,#3034,.T.);
#42760=EDGE_CURVE('',#34522,#34504,#3035,.T.);
#42761=EDGE_CURVE('',#34505,#34521,#3036,.T.);
#42762=EDGE_CURVE('',#34511,#34603,#31170,.T.);
#42763=EDGE_CURVE('',#34603,#34604,#1766,.T.);
#42764=EDGE_CURVE('',#34513,#34604,#31171,.T.);
#42765=EDGE_CURVE('',#34604,#34605,#30108,.T.);
#42766=EDGE_CURVE('',#34606,#34603,#30109,.T.);
#42767=EDGE_CURVE('',#34607,#34606,#1767,.T.);
#42768=EDGE_CURVE('',#34608,#34607,#1768,.T.);
#42769=EDGE_CURVE('',#34605,#34608,#1769,.T.);
#42770=EDGE_CURVE('',#34609,#34605,#31172,.T.);
#42771=EDGE_CURVE('',#34513,#34609,#30110,.T.);
#42772=EDGE_CURVE('',#34498,#34508,#31173,.T.);
#42773=EDGE_CURVE('',#34610,#34508,#30111,.T.);
#42774=EDGE_CURVE('',#34500,#34610,#31174,.T.);
#42775=EDGE_CURVE('',#34610,#34609,#3037,.T.);
#42776=EDGE_CURVE('',#34506,#34611,#31175,.T.);
#42777=EDGE_CURVE('',#34510,#34611,#30112,.T.);
#42778=EDGE_CURVE('',#34507,#34510,#31176,.T.);
#42779=EDGE_CURVE('',#34611,#34612,#3038,.T.);
#42780=EDGE_CURVE('',#34612,#34511,#30113,.T.);
#42781=EDGE_CURVE('',#34612,#34606,#31177,.T.);
#42782=EDGE_CURVE('',#34613,#34607,#31178,.T.);
#42783=EDGE_CURVE('',#34613,#34612,#30114,.T.);
#42784=EDGE_CURVE('',#34614,#34608,#31179,.T.);
#42785=EDGE_CURVE('',#34614,#34613,#30115,.T.);
#42786=EDGE_CURVE('',#34609,#34614,#30116,.T.);
#42787=EDGE_CURVE('',#34615,#34610,#30117,.T.);
#42788=EDGE_CURVE('',#34616,#34614,#3039,.T.);
#42789=EDGE_CURVE('',#34616,#34617,#2693,.T.);
#42790=EDGE_CURVE('',#34617,#34615,#30118,.T.);
#42791=EDGE_CURVE('',#34493,#34615,#31180,.T.);
#42792=EDGE_CURVE('',#34499,#34509,#31181,.T.);
#42793=EDGE_CURVE('',#34497,#34618,#31182,.T.);
#42794=EDGE_CURVE('',#34611,#34618,#30119,.T.);
#42795=EDGE_CURVE('',#34618,#34619,#30120,.T.);
#42796=EDGE_CURVE('',#34619,#34620,#2694,.T.);
#42797=EDGE_CURVE('',#34620,#34613,#3040,.T.);
#42798=EDGE_CURVE('',#34620,#34616,#30121,.T.);
#42799=EDGE_CURVE('',#34621,#34616,#31183,.T.);
#42800=EDGE_CURVE('',#34622,#34620,#31184,.T.);
#42801=EDGE_CURVE('',#34622,#34621,#30122,.T.);
#42802=EDGE_CURVE('',#34495,#34617,#31185,.T.);
#42803=EDGE_CURVE('',#34621,#34495,#2695,.T.);
#42804=EDGE_CURVE('',#34496,#34619,#31186,.T.);
#42805=EDGE_CURVE('',#34496,#34622,#2696,.T.);
#42806=EDGE_CURVE('',#34623,#34624,#3041,.T.);
#42807=EDGE_CURVE('',#34625,#34623,#30123,.F.);
#42808=EDGE_CURVE('',#34626,#34625,#31187,.T.);
#42809=EDGE_CURVE('',#34624,#34626,#30124,.F.);
#42810=EDGE_CURVE('',#34627,#34628,#3042,.T.);
#42811=EDGE_CURVE('',#34623,#34627,#30125,.F.);
#42812=EDGE_CURVE('',#34628,#34624,#30126,.F.);
#42813=EDGE_CURVE('',#34629,#34628,#30127,.F.);
#42814=EDGE_CURVE('',#34630,#34629,#3043,.T.);
#42815=EDGE_CURVE('',#34627,#34630,#30128,.F.);
#42816=EDGE_CURVE('',#34631,#34632,#3044,.T.);
#42817=EDGE_CURVE('',#34630,#34631,#30129,.F.);
#42818=EDGE_CURVE('',#34632,#34629,#30130,.F.);
#42819=EDGE_CURVE('',#34633,#34634,#3045,.T.);
#42820=EDGE_CURVE('',#34631,#34633,#30131,.F.);
#42821=EDGE_CURVE('',#34635,#34632,#30132,.F.);
#42822=EDGE_CURVE('',#34634,#34635,#30133,.F.);
#42823=EDGE_CURVE('',#34636,#34637,#3046,.T.);
#42824=EDGE_CURVE('',#34633,#34636,#30134,.F.);
#42825=EDGE_CURVE('',#34637,#34634,#30135,.F.);
#42826=EDGE_CURVE('',#34638,#34639,#3047,.T.);
#42827=EDGE_CURVE('',#34640,#34638,#31188,.T.);
#42828=EDGE_CURVE('',#34636,#34640,#30136,.F.);
#42829=EDGE_CURVE('',#34639,#34637,#30137,.F.);
#42830=EDGE_CURVE('',#34641,#34642,#3048,.T.);
#42831=EDGE_CURVE('',#34643,#34641,#30138,.F.);
#42832=EDGE_CURVE('',#34644,#34643,#31189,.T.);
#42833=EDGE_CURVE('',#34642,#34644,#30139,.F.);
#42834=EDGE_CURVE('',#34645,#34646,#3049,.T.);
#42835=EDGE_CURVE('',#34641,#34645,#30140,.F.);
#42836=EDGE_CURVE('',#34646,#34642,#30141,.F.);
#42837=EDGE_CURVE('',#34647,#34648,#3050,.T.);
#42838=EDGE_CURVE('',#34645,#34647,#30142,.F.);
#42839=EDGE_CURVE('',#34648,#34646,#30143,.F.);
#42840=EDGE_CURVE('',#34649,#34650,#3051,.T.);
#42841=EDGE_CURVE('',#34651,#34649,#30144,.F.);
#42842=EDGE_CURVE('',#34647,#34651,#30145,.F.);
#42843=EDGE_CURVE('',#34652,#34648,#30146,.F.);
#42844=EDGE_CURVE('',#34650,#34652,#30147,.F.);
#42845=EDGE_CURVE('',#34653,#34654,#3052,.T.);
#42846=EDGE_CURVE('',#34649,#34653,#30148,.F.);
#42847=EDGE_CURVE('',#34654,#34650,#30149,.F.);
#42848=EDGE_CURVE('',#34655,#34656,#3053,.T.);
#42849=EDGE_CURVE('',#34653,#34655,#30150,.F.);
#42850=EDGE_CURVE('',#34656,#34654,#30151,.F.);
#42851=EDGE_CURVE('',#34657,#34658,#3054,.T.);
#42852=EDGE_CURVE('',#34655,#34657,#30152,.F.);
#42853=EDGE_CURVE('',#34658,#34656,#30153,.F.);
#42854=EDGE_CURVE('',#34659,#34660,#3055,.T.);
#42855=EDGE_CURVE('',#34644,#34659,#30154,.F.);
#42856=EDGE_CURVE('',#34660,#34644,#31190,.T.);
#42857=EDGE_CURVE('',#34661,#34662,#3056,.T.);
#42858=EDGE_CURVE('',#34663,#34661,#30155,.F.);
#42859=EDGE_CURVE('',#34663,#34664,#31191,.T.);
#42860=EDGE_CURVE('',#34662,#34664,#30156,.F.);
#42861=EDGE_CURVE('',#34665,#34666,#3057,.T.);
#42862=EDGE_CURVE('',#34661,#34665,#30157,.F.);
#42863=EDGE_CURVE('',#34666,#34662,#30158,.F.);
#42864=EDGE_CURVE('',#34667,#34668,#3058,.T.);
#42865=EDGE_CURVE('',#34665,#34667,#30159,.F.);
#42866=EDGE_CURVE('',#34668,#34666,#30160,.F.);
#42867=EDGE_CURVE('',#34669,#34670,#3059,.T.);
#42868=EDGE_CURVE('',#34667,#34669,#30161,.F.);
#42869=EDGE_CURVE('',#34670,#34668,#30162,.F.);
#42870=EDGE_CURVE('',#34671,#34672,#3060,.T.);
#42871=EDGE_CURVE('',#34669,#34671,#30163,.F.);
#42872=EDGE_CURVE('',#34672,#34670,#30164,.F.);
#42873=EDGE_CURVE('',#34673,#34674,#3061,.T.);
#42874=EDGE_CURVE('',#34675,#34673,#30165,.F.);
#42875=EDGE_CURVE('',#34675,#34676,#31192,.T.);
#42876=EDGE_CURVE('',#34674,#34676,#30166,.F.);
#42877=EDGE_CURVE('',#34677,#34678,#3062,.T.);
#42878=EDGE_CURVE('',#34673,#34677,#30167,.F.);
#42879=EDGE_CURVE('',#34678,#34674,#30168,.F.);
#42880=EDGE_CURVE('',#34679,#34680,#3063,.T.);
#42881=EDGE_CURVE('',#34677,#34679,#30169,.F.);
#42882=EDGE_CURVE('',#34680,#34678,#30170,.F.);
#42883=EDGE_CURVE('',#34681,#34682,#3064,.T.);
#42884=EDGE_CURVE('',#34679,#34681,#30171,.F.);
#42885=EDGE_CURVE('',#34682,#34680,#30172,.F.);
#42886=EDGE_CURVE('',#34683,#34682,#30173,.F.);
#42887=EDGE_CURVE('',#34684,#34683,#3065,.T.);
#42888=EDGE_CURVE('',#34681,#34684,#30174,.F.);
#42889=EDGE_CURVE('',#34685,#34686,#3066,.T.);
#42890=EDGE_CURVE('',#34684,#34685,#30175,.F.);
#42891=EDGE_CURVE('',#34686,#34683,#30176,.F.);
#42892=EDGE_CURVE('',#34687,#34688,#1770,.T.);
#42893=EDGE_CURVE('',#34688,#34689,#1771,.T.);
#42894=EDGE_CURVE('',#34689,#34690,#1772,.T.);
#42895=EDGE_CURVE('',#34690,#34691,#3067,.T.);
#42896=EDGE_CURVE('',#34691,#34691,#31193,.T.);
#42897=EDGE_CURVE('',#34690,#34692,#1773,.T.);
#42898=EDGE_CURVE('',#34692,#34693,#1774,.T.);
#42899=EDGE_CURVE('',#34693,#34687,#1775,.T.);
#42900=EDGE_CURVE('',#34694,#34686,#30177,.F.);
#42901=EDGE_CURVE('',#34694,#34695,#31194,.T.);
#42902=EDGE_CURVE('',#34685,#34695,#30178,.F.);
#42903=EDGE_CURVE('',#34696,#34696,#31195,.T.);
#42904=EDGE_CURVE('',#34696,#34697,#3068,.T.);
#42905=EDGE_CURVE('',#34697,#34698,#31196,.T.);
#42906=EDGE_CURVE('',#34698,#34697,#31197,.T.);
#42907=EDGE_CURVE('',#34699,#34699,#31198,.T.);
#42908=EDGE_CURVE('',#34699,#34700,#3069,.T.);
#42909=EDGE_CURVE('',#34700,#34700,#31199,.T.);
#42910=EDGE_CURVE('',#34701,#34701,#31200,.T.);
#42911=EDGE_CURVE('',#34701,#34702,#3070,.T.);
#42912=EDGE_CURVE('',#34702,#34702,#31201,.T.);
#42913=EDGE_CURVE('',#34703,#34672,#30179,.F.);
#42914=EDGE_CURVE('',#34703,#34704,#31202,.T.);
#42915=EDGE_CURVE('',#34671,#34704,#30180,.F.);
#42916=EDGE_CURVE('',#34638,#34705,#31203,.T.);
#42917=EDGE_CURVE('',#34695,#34705,#30181,.T.);
#42918=EDGE_CURVE('',#34706,#34694,#30182,.F.);
#42919=EDGE_CURVE('',#34706,#34698,#3071,.T.);
#42920=EDGE_CURVE('',#34640,#34706,#30183,.F.);
#42921=EDGE_CURVE('',#34707,#34708,#30184,.F.);
#42922=EDGE_CURVE('',#34707,#34709,#31204,.T.);
#42923=EDGE_CURVE('',#34664,#34709,#31205,.T.);
#42924=EDGE_CURVE('',#34708,#34663,#30185,.F.);
#42925=EDGE_CURVE('',#34708,#34701,#3072,.T.);
#42926=EDGE_CURVE('',#34710,#34711,#31206,.T.);
#42927=EDGE_CURVE('',#34711,#34712,#3073,.T.);
#42928=EDGE_CURVE('',#34712,#34712,#31207,.T.);
#42929=EDGE_CURVE('',#34711,#34710,#31208,.T.);
#42930=EDGE_CURVE('',#34713,#34713,#31209,.T.);
#42931=EDGE_CURVE('',#34713,#34714,#3074,.T.);
#42932=EDGE_CURVE('',#34714,#34714,#31210,.T.);
#42933=EDGE_CURVE('',#34715,#34715,#31211,.T.);
#42934=EDGE_CURVE('',#34715,#34713,#31212,.T.);
#42935=EDGE_CURVE('',#34710,#34716,#31213,.T.);
#42936=EDGE_CURVE('',#34716,#34716,#31214,.T.);
#42937=EDGE_CURVE('',#34717,#34718,#31215,.T.);
#42938=EDGE_CURVE('',#34717,#34719,#3075,.T.);
#42939=EDGE_CURVE('',#34720,#34719,#31216,.T.);
#42940=EDGE_CURVE('',#34718,#34720,#3076,.T.);
#42941=EDGE_CURVE('',#34643,#34660,#31217,.T.);
#42942=EDGE_CURVE('',#34704,#34643,#30186,.F.);
#42943=EDGE_CURVE('',#34659,#34703,#30187,.F.);
#42944=EDGE_CURVE('',#34626,#34721,#30188,.F.);
#42945=EDGE_CURVE('',#34676,#34625,#30189,.T.);
#42946=EDGE_CURVE('',#34721,#34675,#30190,.F.);
#42947=EDGE_CURVE('',#34721,#34722,#3077,.T.);
#42948=EDGE_CURVE('',#34722,#34722,#31218,.T.);
#42949=EDGE_CURVE('',#34709,#34658,#30191,.F.);
#42950=EDGE_CURVE('',#34657,#34707,#30192,.F.);
#42951=EDGE_CURVE('',#34705,#34639,#30193,.F.);
#42952=EDGE_CURVE('',#34723,#34717,#3078,.T.);
#42953=EDGE_CURVE('',#34723,#34724,#3079,.T.);
#42954=EDGE_CURVE('',#34719,#34724,#3080,.T.);
#42955=EDGE_CURVE('',#34725,#34723,#3081,.T.);
#42956=EDGE_CURVE('',#34725,#34726,#3082,.T.);
#42957=EDGE_CURVE('',#34724,#34726,#3083,.T.);
#42958=EDGE_CURVE('',#34727,#34725,#3084,.T.);
#42959=EDGE_CURVE('',#34727,#34728,#3085,.T.);
#42960=EDGE_CURVE('',#34726,#34728,#3086,.T.);
#42961=EDGE_CURVE('',#34729,#34727,#31219,.T.);
#42962=EDGE_CURVE('',#34729,#34730,#3087,.T.);
#42963=EDGE_CURVE('',#34728,#34730,#31220,.T.);
#42964=EDGE_CURVE('',#34731,#34729,#3088,.T.);
#42965=EDGE_CURVE('',#34731,#34732,#3089,.T.);
#42966=EDGE_CURVE('',#34730,#34732,#3090,.T.);
#42967=EDGE_CURVE('',#34733,#34731,#3091,.T.);
#42968=EDGE_CURVE('',#34733,#34734,#3092,.T.);
#42969=EDGE_CURVE('',#34732,#34734,#3093,.T.);
#42970=EDGE_CURVE('',#34718,#34733,#3094,.T.);
#42971=EDGE_CURVE('',#34734,#34720,#3095,.T.);
#42972=EDGE_CURVE('',#34735,#34736,#3096,.T.);
#42973=EDGE_CURVE('',#34737,#34735,#3097,.T.);
#42974=EDGE_CURVE('',#34738,#34737,#3098,.T.);
#42975=EDGE_CURVE('',#34739,#34738,#3099,.T.);
#42976=EDGE_CURVE('',#34740,#34739,#3100,.T.);
#42977=EDGE_CURVE('',#34736,#34740,#3101,.T.);
#42978=EDGE_CURVE('',#34738,#34690,#3102,.T.);
#42979=EDGE_CURVE('',#34739,#34689,#3103,.T.);
#42980=EDGE_CURVE('',#34740,#34688,#3104,.T.);
#42981=EDGE_CURVE('',#34736,#34687,#3105,.T.);
#42982=EDGE_CURVE('',#34735,#34693,#3106,.T.);
#42983=EDGE_CURVE('',#34737,#34692,#3107,.T.);
#42984=EDGE_CURVE('',#34741,#34741,#31221,.T.);
#42985=EDGE_CURVE('',#34741,#34742,#31222,.T.);
#42986=EDGE_CURVE('',#34742,#34742,#31223,.T.);
#42987=EDGE_CURVE('',#34743,#34743,#31224,.T.);
#42988=EDGE_CURVE('',#34743,#34744,#31225,.T.);
#42989=EDGE_CURVE('',#34744,#34744,#31226,.T.);
#42990=EDGE_CURVE('',#34745,#34745,#31227,.T.);
#42991=EDGE_CURVE('',#34745,#34746,#3108,.T.);
#42992=EDGE_CURVE('',#34746,#34747,#31228,.T.);
#42993=EDGE_CURVE('',#34748,#34747,#3109,.T.);
#42994=EDGE_CURVE('',#34748,#34749,#31229,.T.);
#42995=EDGE_CURVE('',#34750,#34749,#3110,.T.);
#42996=EDGE_CURVE('',#34750,#34751,#31230,.T.);
#42997=EDGE_CURVE('',#34752,#34751,#3111,.T.);
#42998=EDGE_CURVE('',#34752,#34753,#31231,.T.);
#42999=EDGE_CURVE('',#34754,#34753,#3112,.T.);
#43000=EDGE_CURVE('',#34754,#34755,#31232,.T.);
#43001=EDGE_CURVE('',#34756,#34755,#3113,.T.);
#43002=EDGE_CURVE('',#34756,#34757,#31233,.T.);
#43003=EDGE_CURVE('',#34758,#34757,#3114,.T.);
#43004=EDGE_CURVE('',#34758,#34746,#31234,.T.);
#43005=EDGE_CURVE('',#34759,#34759,#31235,.T.);
#43006=EDGE_CURVE('',#34759,#34760,#31236,.T.);
#43007=EDGE_CURVE('',#34760,#34760,#31237,.T.);
#43008=EDGE_CURVE('',#34761,#34761,#31238,.T.);
#43009=EDGE_CURVE('',#34761,#34762,#31239,.T.);
#43010=EDGE_CURVE('',#34762,#34762,#31240,.T.);
#43011=EDGE_CURVE('',#34763,#34763,#31241,.T.);
#43012=EDGE_CURVE('',#34763,#34764,#3115,.T.);
#43013=EDGE_CURVE('',#34764,#34764,#31242,.T.);
#43014=EDGE_CURVE('',#34757,#34756,#31243,.T.);
#43015=EDGE_CURVE('',#34758,#34755,#31244,.T.);
#43016=EDGE_CURVE('',#34749,#34748,#31245,.T.);
#43017=EDGE_CURVE('',#34750,#34747,#31246,.T.);
#43018=EDGE_CURVE('',#34753,#34752,#31247,.T.);
#43019=EDGE_CURVE('',#34754,#34751,#31248,.T.);
#43020=EDGE_CURVE('',#34765,#34766,#3116,.T.);
#43021=EDGE_CURVE('',#34767,#34766,#30194,.F.);
#43022=EDGE_CURVE('',#34768,#34767,#30195,.T.);
#43023=EDGE_CURVE('',#34769,#34768,#3117,.T.);
#43024=EDGE_CURVE('',#34769,#34765,#30196,.T.);
#43025=EDGE_CURVE('',#34770,#34771,#3118,.T.);
#43026=EDGE_CURVE('',#34766,#34771,#30197,.F.);
#43027=EDGE_CURVE('',#34765,#34770,#30198,.T.);
#43028=EDGE_CURVE('',#34772,#34773,#3119,.T.);
#43029=EDGE_CURVE('',#34772,#34774,#30199,.T.);
#43030=EDGE_CURVE('',#34774,#34775,#30200,.T.);
#43031=EDGE_CURVE('',#34773,#34775,#30201,.T.);
#43032=EDGE_CURVE('',#34776,#34777,#3120,.T.);
#43033=EDGE_CURVE('',#34777,#34778,#30202,.T.);
#43034=EDGE_CURVE('',#34778,#34779,#30203,.T.);
#43035=EDGE_CURVE('',#34779,#34780,#30204,.T.);
#43036=EDGE_CURVE('',#34780,#34781,#3121,.T.);
#43037=EDGE_CURVE('',#34781,#34782,#30205,.T.);
#43038=EDGE_CURVE('',#34782,#34783,#30206,.T.);
#43039=EDGE_CURVE('',#34783,#34784,#30207,.T.);
#43040=EDGE_CURVE('',#34784,#34785,#3122,.T.);
#43041=EDGE_CURVE('',#34785,#34785,#31249,.T.);
#43042=EDGE_CURVE('',#34784,#34776,#30208,.T.);
#43043=EDGE_CURVE('',#34786,#34787,#3123,.T.);
#43044=EDGE_CURVE('',#34787,#34777,#30209,.T.);
#43045=EDGE_CURVE('',#34776,#34786,#30210,.T.);
#43046=EDGE_CURVE('',#34788,#34789,#3124,.T.);
#43047=EDGE_CURVE('',#34789,#34787,#30211,.T.);
#43048=EDGE_CURVE('',#34786,#34790,#30212,.T.);
#43049=EDGE_CURVE('',#34790,#34788,#30213,.T.);
#43050=EDGE_CURVE('',#34791,#34792,#3125,.T.);
#43051=EDGE_CURVE('',#34793,#34792,#30214,.F.);
#43052=EDGE_CURVE('',#34793,#34789,#30215,.T.);
#43053=EDGE_CURVE('',#34788,#34791,#30216,.T.);
#43054=EDGE_CURVE('',#34794,#34795,#3126,.T.);
#43055=EDGE_CURVE('',#34794,#34796,#31250,.T.);
#43056=EDGE_CURVE('',#34795,#34796,#30217,.F.);
#43057=EDGE_CURVE('',#34797,#34797,#31251,.T.);
#43058=EDGE_CURVE('',#34797,#34798,#3127,.T.);
#43059=EDGE_CURVE('',#34798,#34798,#31252,.T.);
#43060=EDGE_CURVE('',#34792,#34795,#30218,.F.);
#43061=EDGE_CURVE('',#34791,#34799,#30219,.T.);
#43062=EDGE_CURVE('',#34799,#34800,#30220,.T.);
#43063=EDGE_CURVE('',#34800,#34794,#31253,.T.);
#43064=EDGE_CURVE('',#34771,#34773,#30221,.F.);
#43065=EDGE_CURVE('',#34770,#34772,#30222,.T.);
#43066=EDGE_CURVE('',#34801,#34802,#30223,.T.);
#43067=EDGE_CURVE('',#34802,#34803,#3128,.T.);
#43068=EDGE_CURVE('',#34803,#34803,#31254,.T.);
#43069=EDGE_CURVE('',#34802,#34796,#30224,.T.);
#43070=EDGE_CURVE('',#34804,#34800,#30225,.T.);
#43071=EDGE_CURVE('',#34804,#34805,#30226,.T.);
#43072=EDGE_CURVE('',#34805,#34801,#30227,.T.);
#43073=EDGE_CURVE('',#34806,#34807,#1776,.T.);
#43074=EDGE_CURVE('',#34806,#34808,#31255,.T.);
#43075=EDGE_CURVE('',#34809,#34808,#1777,.T.);
#43076=EDGE_CURVE('',#34809,#34810,#31256,.T.);
#43077=EDGE_CURVE('',#34811,#34810,#1778,.T.);
#43078=EDGE_CURVE('',#34811,#34812,#31257,.T.);
#43079=EDGE_CURVE('',#34813,#34812,#1779,.F.);
#43080=EDGE_CURVE('',#34814,#34813,#31258,.T.);
#43081=EDGE_CURVE('',#34815,#34814,#1780,.T.);
#43082=EDGE_CURVE('',#34816,#34815,#31259,.T.);
#43083=EDGE_CURVE('',#34816,#34817,#3129,.T.);
#43084=EDGE_CURVE('',#34817,#34817,#31260,.T.);
#43085=EDGE_CURVE('',#34818,#34816,#31261,.T.);
#43086=EDGE_CURVE('',#34819,#34818,#1781,.T.);
#43087=EDGE_CURVE('',#34807,#34819,#31262,.T.);
#43088=EDGE_CURVE('',#34820,#34821,#1782,.F.);
#43089=EDGE_CURVE('',#34821,#34822,#31263,.T.);
#43090=EDGE_CURVE('',#34822,#34823,#1783,.T.);
#43091=EDGE_CURVE('',#34823,#34824,#31264,.T.);
#43092=EDGE_CURVE('',#34824,#34825,#1784,.T.);
#43093=EDGE_CURVE('',#34825,#34826,#31265,.T.);
#43094=EDGE_CURVE('',#34826,#34827,#1785,.T.);
#43095=EDGE_CURVE('',#34828,#34827,#31266,.T.);
#43096=EDGE_CURVE('',#34828,#34829,#1786,.T.);
#43097=EDGE_CURVE('',#34830,#34829,#31267,.T.);
#43098=EDGE_CURVE('',#34830,#34831,#3130,.T.);
#43099=EDGE_CURVE('',#34831,#34831,#31268,.T.);
#43100=EDGE_CURVE('',#34832,#34830,#31269,.T.);
#43101=EDGE_CURVE('',#34832,#34833,#1787,.T.);
#43102=EDGE_CURVE('',#34820,#34833,#31270,.T.);
#43103=EDGE_CURVE('',#34809,#34832,#3131,.T.);
#43104=EDGE_CURVE('',#34810,#34829,#3132,.T.);
#43105=EDGE_CURVE('',#34818,#34823,#3133,.T.);
#43106=EDGE_CURVE('',#34819,#34822,#3134,.T.);
#43107=EDGE_CURVE('',#34811,#34828,#3135,.T.);
#43108=EDGE_CURVE('',#34808,#34833,#3136,.T.);
#43109=EDGE_CURVE('',#34812,#34827,#3137,.T.);
#43110=EDGE_CURVE('',#34806,#34820,#3138,.T.);
#43111=EDGE_CURVE('',#34807,#34821,#3139,.T.);
#43112=EDGE_CURVE('',#34814,#34825,#3140,.T.);
#43113=EDGE_CURVE('',#34815,#34824,#3141,.T.);
#43114=EDGE_CURVE('',#34813,#34826,#3142,.T.);
#43115=EDGE_CURVE('',#34801,#34768,#30228,.T.);
#43116=EDGE_CURVE('',#34768,#34793,#3143,.T.);
#43117=EDGE_CURVE('',#34804,#34769,#30229,.T.);
#43118=EDGE_CURVE('',#34782,#34774,#30230,.T.);
#43119=EDGE_CURVE('',#34790,#34769,#3144,.T.);
#43120=EDGE_CURVE('',#34774,#34781,#30231,.T.);
#43121=EDGE_CURVE('',#34775,#34780,#30232,.T.);
#43122=EDGE_CURVE('',#34775,#34779,#30233,.T.);
#43123=EDGE_CURVE('',#34834,#34834,#31271,.T.);
#43124=EDGE_CURVE('',#34834,#34835,#31272,.T.);
#43125=EDGE_CURVE('',#34835,#34835,#31273,.T.);
#43126=EDGE_CURVE('',#34836,#34836,#31274,.T.);
#43127=EDGE_CURVE('',#34836,#34837,#31275,.T.);
#43128=EDGE_CURVE('',#34837,#34837,#31276,.T.);
#43129=EDGE_CURVE('',#34838,#34838,#31277,.T.);
#43130=EDGE_CURVE('',#34838,#34839,#3145,.T.);
#43131=EDGE_CURVE('',#34839,#34840,#31278,.T.);
#43132=EDGE_CURVE('',#34841,#34840,#3146,.T.);
#43133=EDGE_CURVE('',#34841,#34842,#31279,.T.);
#43134=EDGE_CURVE('',#34843,#34842,#3147,.T.);
#43135=EDGE_CURVE('',#34843,#34844,#31280,.T.);
#43136=EDGE_CURVE('',#34845,#34844,#3148,.T.);
#43137=EDGE_CURVE('',#34845,#34846,#31281,.T.);
#43138=EDGE_CURVE('',#34847,#34846,#3149,.T.);
#43139=EDGE_CURVE('',#34847,#34848,#31282,.T.);
#43140=EDGE_CURVE('',#34849,#34848,#3150,.T.);
#43141=EDGE_CURVE('',#34849,#34850,#31283,.T.);
#43142=EDGE_CURVE('',#34851,#34850,#3151,.T.);
#43143=EDGE_CURVE('',#34851,#34839,#31284,.T.);
#43144=EDGE_CURVE('',#34852,#34852,#31285,.T.);
#43145=EDGE_CURVE('',#34852,#34853,#31286,.T.);
#43146=EDGE_CURVE('',#34853,#34853,#31287,.T.);
#43147=EDGE_CURVE('',#34854,#34854,#31288,.T.);
#43148=EDGE_CURVE('',#34854,#34855,#31289,.T.);
#43149=EDGE_CURVE('',#34855,#34855,#31290,.T.);
#43150=EDGE_CURVE('',#34856,#34856,#31291,.T.);
#43151=EDGE_CURVE('',#34856,#34857,#3152,.T.);
#43152=EDGE_CURVE('',#34857,#34857,#31292,.T.);
#43153=EDGE_CURVE('',#34850,#34849,#31293,.T.);
#43154=EDGE_CURVE('',#34851,#34848,#31294,.T.);
#43155=EDGE_CURVE('',#34842,#34841,#31295,.T.);
#43156=EDGE_CURVE('',#34843,#34840,#31296,.T.);
#43157=EDGE_CURVE('',#34846,#34845,#31297,.T.);
#43158=EDGE_CURVE('',#34847,#34844,#31298,.T.);
#43159=EDGE_CURVE('',#34858,#34858,#31299,.T.);
#43160=EDGE_CURVE('',#34858,#34859,#31300,.T.);
#43161=EDGE_CURVE('',#34859,#34859,#31301,.T.);
#43162=EDGE_CURVE('',#34859,#34860,#3153,.T.);
#43163=EDGE_CURVE('',#34860,#34860,#31302,.T.);
#43164=EDGE_CURVE('',#34861,#34862,#31303,.T.);
#43165=EDGE_CURVE('',#34863,#34861,#3154,.T.);
#43166=EDGE_CURVE('',#34863,#34864,#31304,.T.);
#43167=EDGE_CURVE('',#34864,#34862,#3155,.T.);
#43168=EDGE_CURVE('',#34862,#34861,#31305,.T.);
#43169=EDGE_CURVE('',#34864,#34863,#31306,.T.);
#43170=EDGE_CURVE('',#34865,#34865,#31307,.T.);
#43171=EDGE_CURVE('',#34865,#34866,#31308,.T.);
#43172=EDGE_CURVE('',#34866,#34866,#31309,.T.);
#43173=EDGE_CURVE('',#34867,#34867,#31310,.T.);
#43174=EDGE_CURVE('',#34867,#34865,#3156,.T.);
#43175=EDGE_CURVE('',#34868,#34868,#31311,.T.);
#43176=EDGE_CURVE('',#34868,#34869,#3157,.T.);
#43177=EDGE_CURVE('',#34869,#34869,#31312,.T.);
#43178=EDGE_CURVE('',#34870,#34870,#31313,.T.);
#43179=EDGE_CURVE('',#34870,#34871,#3158,.T.);
#43180=EDGE_CURVE('',#34871,#34871,#31314,.T.);
#43181=EDGE_CURVE('',#34872,#34873,#3159,.T.);
#43182=EDGE_CURVE('',#34874,#34873,#30234,.F.);
#43183=EDGE_CURVE('',#34875,#34874,#30235,.T.);
#43184=EDGE_CURVE('',#34876,#34875,#3160,.T.);
#43185=EDGE_CURVE('',#34876,#34872,#30236,.T.);
#43186=EDGE_CURVE('',#34877,#34878,#3161,.T.);
#43187=EDGE_CURVE('',#34873,#34878,#30237,.F.);
#43188=EDGE_CURVE('',#34872,#34877,#30238,.T.);
#43189=EDGE_CURVE('',#34879,#34880,#3162,.T.);
#43190=EDGE_CURVE('',#34879,#34881,#30239,.T.);
#43191=EDGE_CURVE('',#34881,#34882,#30240,.T.);
#43192=EDGE_CURVE('',#34880,#34882,#30241,.T.);
#43193=EDGE_CURVE('',#34883,#34884,#3163,.T.);
#43194=EDGE_CURVE('',#34884,#34885,#30242,.T.);
#43195=EDGE_CURVE('',#34885,#34886,#30243,.T.);
#43196=EDGE_CURVE('',#34886,#34887,#30244,.T.);
#43197=EDGE_CURVE('',#34887,#34888,#3164,.T.);
#43198=EDGE_CURVE('',#34888,#34889,#30245,.T.);
#43199=EDGE_CURVE('',#34889,#34890,#30246,.T.);
#43200=EDGE_CURVE('',#34890,#34891,#30247,.T.);
#43201=EDGE_CURVE('',#34891,#34892,#3165,.T.);
#43202=EDGE_CURVE('',#34892,#34892,#31315,.T.);
#43203=EDGE_CURVE('',#34891,#34883,#30248,.T.);
#43204=EDGE_CURVE('',#34893,#34894,#3166,.T.);
#43205=EDGE_CURVE('',#34894,#34884,#30249,.T.);
#43206=EDGE_CURVE('',#34883,#34893,#30250,.T.);
#43207=EDGE_CURVE('',#34895,#34896,#3167,.T.);
#43208=EDGE_CURVE('',#34896,#34894,#30251,.T.);
#43209=EDGE_CURVE('',#34893,#34897,#30252,.T.);
#43210=EDGE_CURVE('',#34897,#34895,#30253,.T.);
#43211=EDGE_CURVE('',#34898,#34899,#3168,.T.);
#43212=EDGE_CURVE('',#34900,#34899,#30254,.F.);
#43213=EDGE_CURVE('',#34900,#34896,#30255,.T.);
#43214=EDGE_CURVE('',#34895,#34898,#30256,.T.);
#43215=EDGE_CURVE('',#34901,#34902,#3169,.T.);
#43216=EDGE_CURVE('',#34901,#34903,#31316,.T.);
#43217=EDGE_CURVE('',#34902,#34903,#30257,.F.);
#43218=EDGE_CURVE('',#34904,#34904,#31317,.T.);
#43219=EDGE_CURVE('',#34904,#34905,#3170,.T.);
#43220=EDGE_CURVE('',#34905,#34905,#31318,.T.);
#43221=EDGE_CURVE('',#34899,#34902,#30258,.F.);
#43222=EDGE_CURVE('',#34898,#34906,#30259,.T.);
#43223=EDGE_CURVE('',#34906,#34907,#30260,.T.);
#43224=EDGE_CURVE('',#34907,#34901,#31319,.T.);
#43225=EDGE_CURVE('',#34878,#34880,#30261,.F.);
#43226=EDGE_CURVE('',#34877,#34879,#30262,.T.);
#43227=EDGE_CURVE('',#34908,#34909,#30263,.T.);
#43228=EDGE_CURVE('',#34909,#34910,#3171,.T.);
#43229=EDGE_CURVE('',#34910,#34910,#31320,.T.);
#43230=EDGE_CURVE('',#34909,#34903,#30264,.T.);
#43231=EDGE_CURVE('',#34911,#34907,#30265,.T.);
#43232=EDGE_CURVE('',#34911,#34912,#30266,.T.);
#43233=EDGE_CURVE('',#34912,#34908,#30267,.T.);
#43234=EDGE_CURVE('',#34913,#34914,#1788,.T.);
#43235=EDGE_CURVE('',#34913,#34915,#31321,.T.);
#43236=EDGE_CURVE('',#34916,#34915,#1789,.T.);
#43237=EDGE_CURVE('',#34916,#34917,#31322,.T.);
#43238=EDGE_CURVE('',#34918,#34917,#1790,.T.);
#43239=EDGE_CURVE('',#34918,#34919,#31323,.T.);
#43240=EDGE_CURVE('',#34920,#34919,#1791,.F.);
#43241=EDGE_CURVE('',#34921,#34920,#31324,.T.);
#43242=EDGE_CURVE('',#34922,#34921,#1792,.T.);
#43243=EDGE_CURVE('',#34923,#34922,#31325,.T.);
#43244=EDGE_CURVE('',#34923,#34924,#3172,.T.);
#43245=EDGE_CURVE('',#34924,#34924,#31326,.T.);
#43246=EDGE_CURVE('',#34925,#34923,#31327,.T.);
#43247=EDGE_CURVE('',#34926,#34925,#1793,.T.);
#43248=EDGE_CURVE('',#34914,#34926,#31328,.T.);
#43249=EDGE_CURVE('',#34927,#34928,#1794,.F.);
#43250=EDGE_CURVE('',#34928,#34929,#31329,.T.);
#43251=EDGE_CURVE('',#34929,#34930,#1795,.T.);
#43252=EDGE_CURVE('',#34930,#34931,#31330,.T.);
#43253=EDGE_CURVE('',#34931,#34932,#1796,.T.);
#43254=EDGE_CURVE('',#34932,#34933,#31331,.T.);
#43255=EDGE_CURVE('',#34933,#34934,#1797,.T.);
#43256=EDGE_CURVE('',#34935,#34934,#31332,.T.);
#43257=EDGE_CURVE('',#34935,#34936,#1798,.T.);
#43258=EDGE_CURVE('',#34937,#34936,#31333,.T.);
#43259=EDGE_CURVE('',#34937,#34938,#3173,.T.);
#43260=EDGE_CURVE('',#34938,#34938,#31334,.T.);
#43261=EDGE_CURVE('',#34939,#34937,#31335,.T.);
#43262=EDGE_CURVE('',#34939,#34940,#1799,.T.);
#43263=EDGE_CURVE('',#34927,#34940,#31336,.T.);
#43264=EDGE_CURVE('',#34916,#34939,#3174,.T.);
#43265=EDGE_CURVE('',#34917,#34936,#3175,.T.);
#43266=EDGE_CURVE('',#34925,#34930,#3176,.T.);
#43267=EDGE_CURVE('',#34926,#34929,#3177,.T.);
#43268=EDGE_CURVE('',#34918,#34935,#3178,.T.);
#43269=EDGE_CURVE('',#34915,#34940,#3179,.T.);
#43270=EDGE_CURVE('',#34919,#34934,#3180,.T.);
#43271=EDGE_CURVE('',#34913,#34927,#3181,.T.);
#43272=EDGE_CURVE('',#34914,#34928,#3182,.T.);
#43273=EDGE_CURVE('',#34921,#34932,#3183,.T.);
#43274=EDGE_CURVE('',#34922,#34931,#3184,.T.);
#43275=EDGE_CURVE('',#34920,#34933,#3185,.T.);
#43276=EDGE_CURVE('',#34908,#34875,#30268,.T.);
#43277=EDGE_CURVE('',#34875,#34900,#3186,.T.);
#43278=EDGE_CURVE('',#34911,#34876,#30269,.T.);
#43279=EDGE_CURVE('',#34889,#34881,#30270,.T.);
#43280=EDGE_CURVE('',#34897,#34876,#3187,.T.);
#43281=EDGE_CURVE('',#34881,#34888,#30271,.T.);
#43282=EDGE_CURVE('',#34882,#34887,#30272,.T.);
#43283=EDGE_CURVE('',#34882,#34886,#30273,.T.);
#43284=EDGE_CURVE('',#34941,#34941,#31337,.T.);
#43285=EDGE_CURVE('',#34941,#34942,#3188,.T.);
#43286=EDGE_CURVE('',#34942,#34943,#31338,.T.);
#43287=EDGE_CURVE('',#34943,#34942,#31339,.T.);
#43288=EDGE_CURVE('',#34944,#34943,#3189,.T.);
#43289=EDGE_CURVE('',#34945,#34946,#3190,.T.);
#43290=EDGE_CURVE('',#34947,#34945,#30274,.F.);
#43291=EDGE_CURVE('',#34948,#34947,#31340,.T.);
#43292=EDGE_CURVE('',#34946,#34948,#30275,.F.);
#43293=EDGE_CURVE('',#34949,#34950,#3191,.T.);
#43294=EDGE_CURVE('',#34945,#34949,#30276,.F.);
#43295=EDGE_CURVE('',#34950,#34946,#30277,.F.);
#43296=EDGE_CURVE('',#34951,#34952,#3192,.T.);
#43297=EDGE_CURVE('',#34949,#34951,#30278,.F.);
#43298=EDGE_CURVE('',#34952,#34950,#30279,.F.);
#43299=EDGE_CURVE('',#34953,#34954,#3193,.T.);
#43300=EDGE_CURVE('',#34948,#34953,#30280,.F.);
#43301=EDGE_CURVE('',#34954,#34948,#31341,.T.);
#43302=EDGE_CURVE('',#34955,#34956,#3194,.T.);
#43303=EDGE_CURVE('',#34957,#34955,#30281,.F.);
#43304=EDGE_CURVE('',#34957,#34958,#31342,.T.);
#43305=EDGE_CURVE('',#34956,#34958,#30282,.F.);
#43306=EDGE_CURVE('',#34959,#34960,#3195,.T.);
#43307=EDGE_CURVE('',#34955,#34959,#30283,.F.);
#43308=EDGE_CURVE('',#34960,#34956,#30284,.F.);
#43309=EDGE_CURVE('',#34961,#34961,#31343,.T.);
#43310=EDGE_CURVE('',#34961,#34962,#3196,.T.);
#43311=EDGE_CURVE('',#34962,#34963,#31344,.T.);
#43312=EDGE_CURVE('',#34963,#34964,#3197,.T.);
#43313=EDGE_CURVE('',#34965,#34964,#31345,.T.);
#43314=EDGE_CURVE('',#34965,#34966,#3198,.T.);
#43315=EDGE_CURVE('',#34966,#34967,#31346,.T.);
#43316=EDGE_CURVE('',#34967,#34968,#3199,.T.);
#43317=EDGE_CURVE('',#34969,#34968,#31347,.T.);
#43318=EDGE_CURVE('',#34969,#34970,#3200,.T.);
#43319=EDGE_CURVE('',#34970,#34962,#31348,.T.);
#43320=EDGE_CURVE('',#34971,#34972,#31349,.T.);
#43321=EDGE_CURVE('',#34971,#34967,#30285,.T.);
#43322=EDGE_CURVE('',#34966,#34972,#1800,.T.);
#43323=EDGE_CURVE('',#34973,#34973,#31350,.T.);
#43324=EDGE_CURVE('',#34973,#34974,#3201,.T.);
#43325=EDGE_CURVE('',#34974,#34974,#31351,.T.);
#43326=EDGE_CURVE('',#34975,#34960,#30286,.F.);
#43327=EDGE_CURVE('',#34975,#34976,#31352,.T.);
#43328=EDGE_CURVE('',#34959,#34976,#30287,.F.);
#43329=EDGE_CURVE('',#34977,#34978,#30288,.F.);
#43330=EDGE_CURVE('',#34977,#34979,#31353,.T.);
#43331=EDGE_CURVE('',#34958,#34979,#31354,.T.);
#43332=EDGE_CURVE('',#34978,#34957,#30289,.F.);
#43333=EDGE_CURVE('',#34978,#34973,#3202,.T.);
#43334=EDGE_CURVE('',#34980,#34981,#31355,.T.);
#43335=EDGE_CURVE('',#34981,#34982,#3203,.T.);
#43336=EDGE_CURVE('',#34982,#34982,#31356,.T.);
#43337=EDGE_CURVE('',#34981,#34980,#31357,.T.);
#43338=EDGE_CURVE('',#34983,#34984,#31358,.T.);
#43339=EDGE_CURVE('',#34984,#34985,#31359,.T.);
#43340=EDGE_CURVE('',#34986,#34985,#3204,.T.);
#43341=EDGE_CURVE('',#34986,#34987,#31360,.T.);
#43342=EDGE_CURVE('',#34987,#34988,#31361,.T.);
#43343=EDGE_CURVE('',#34983,#34988,#3205,.T.);
#43344=EDGE_CURVE('',#34988,#34986,#30290,.F.);
#43345=EDGE_CURVE('',#34987,#34989,#3206,.T.);
#43346=EDGE_CURVE('',#34989,#34989,#31362,.T.);
#43347=EDGE_CURVE('',#34985,#34983,#30291,.F.);
#43348=EDGE_CURVE('',#34984,#34990,#3207,.T.);
#43349=EDGE_CURVE('',#34990,#34990,#31363,.T.);
#43350=EDGE_CURVE('',#34947,#34954,#31364,.T.);
#43351=EDGE_CURVE('',#34991,#34947,#30292,.T.);
#43352=EDGE_CURVE('',#34976,#34991,#30293,.T.);
#43353=EDGE_CURVE('',#34953,#34975,#30294,.F.);
#43354=EDGE_CURVE('',#34980,#34992,#3208,.T.);
#43355=EDGE_CURVE('',#34992,#34992,#31365,.T.);
#43356=EDGE_CURVE('',#34979,#34952,#30295,.F.);
#43357=EDGE_CURVE('',#34951,#34977,#30296,.F.);
#43358=EDGE_CURVE('',#34993,#34993,#31366,.T.);
#43359=EDGE_CURVE('',#34993,#34994,#3209,.T.);
#43360=EDGE_CURVE('',#34994,#34994,#31367,.T.);
#43361=EDGE_CURVE('',#34994,#34995,#31368,.T.);
#43362=EDGE_CURVE('',#34995,#34995,#31369,.T.);
#43363=EDGE_CURVE('',#34995,#34996,#3210,.T.);
#43364=EDGE_CURVE('',#34996,#34996,#31370,.T.);
#43365=EDGE_CURVE('',#34997,#34998,#31371,.T.);
#43366=EDGE_CURVE('',#34998,#34999,#3211,.T.);
#43367=EDGE_CURVE('',#34999,#34999,#31372,.T.);
#43368=EDGE_CURVE('',#34998,#34997,#31373,.T.);
#43369=EDGE_CURVE('',#35000,#35000,#31374,.T.);
#43370=EDGE_CURVE('',#35000,#35001,#3212,.T.);
#43371=EDGE_CURVE('',#35001,#35002,#31375,.T.);
#43372=EDGE_CURVE('',#35002,#35001,#31376,.T.);
#43373=EDGE_CURVE('',#35003,#35003,#31377,.T.);
#43374=EDGE_CURVE('',#35003,#35000,#31378,.T.);
#43375=EDGE_CURVE('',#35004,#35004,#31379,.T.);
#43376=EDGE_CURVE('',#35004,#35002,#31380,.T.);
#43377=EDGE_CURVE('',#34997,#35004,#31381,.T.);
#43378=EDGE_CURVE('',#35005,#35005,#31382,.T.);
#43379=EDGE_CURVE('',#35005,#35006,#3213,.T.);
#43380=EDGE_CURVE('',#35006,#35006,#31383,.T.);
#43381=EDGE_CURVE('',#35006,#35007,#31384,.T.);
#43382=EDGE_CURVE('',#35007,#35007,#31385,.T.);
#43383=EDGE_CURVE('',#35008,#35008,#31386,.T.);
#43384=EDGE_CURVE('',#35008,#35009,#3214,.T.);
#43385=EDGE_CURVE('',#35009,#35009,#31387,.T.);
#43386=EDGE_CURVE('',#35010,#35010,#31388,.T.);
#43387=EDGE_CURVE('',#35010,#35011,#3215,.T.);
#43388=EDGE_CURVE('',#35011,#35011,#31389,.T.);
#43389=EDGE_CURVE('',#34965,#34964,#3216,.T.);
#43390=EDGE_CURVE('',#35012,#34963,#30297,.T.);
#43391=EDGE_CURVE('',#34972,#35012,#3217,.T.);
#43392=EDGE_CURVE('',#34969,#34968,#3218,.T.);
#43393=EDGE_CURVE('',#35013,#34971,#3219,.T.);
#43394=EDGE_CURVE('',#34970,#35013,#1801,.T.);
#43395=EDGE_CURVE('',#35012,#35013,#31390,.T.);
#43396=EDGE_CURVE('',#35014,#35014,#31391,.T.);
#43397=EDGE_CURVE('',#35014,#35015,#31392,.T.);
#43398=EDGE_CURVE('',#35015,#35015,#31393,.T.);
#43399=EDGE_CURVE('',#35015,#35016,#3220,.T.);
#43400=EDGE_CURVE('',#35016,#35016,#31394,.T.);
#43401=EDGE_CURVE('',#35017,#35018,#31395,.T.);
#43402=EDGE_CURVE('',#35019,#35017,#3221,.T.);
#43403=EDGE_CURVE('',#35019,#35020,#31396,.T.);
#43404=EDGE_CURVE('',#35020,#35018,#3222,.T.);
#43405=EDGE_CURVE('',#35018,#35017,#31397,.T.);
#43406=EDGE_CURVE('',#35020,#35019,#31398,.T.);
#43407=EDGE_CURVE('',#35021,#35021,#31399,.T.);
#43408=EDGE_CURVE('',#35021,#35022,#31400,.T.);
#43409=EDGE_CURVE('',#35022,#35022,#31401,.T.);
#43410=EDGE_CURVE('',#35023,#35023,#31402,.T.);
#43411=EDGE_CURVE('',#35023,#35021,#3223,.T.);
#43412=EDGE_CURVE('',#35024,#35024,#31403,.T.);
#43413=EDGE_CURVE('',#35024,#35025,#3224,.T.);
#43414=EDGE_CURVE('',#35025,#35025,#31404,.T.);
#43415=EDGE_CURVE('',#35026,#35026,#31405,.T.);
#43416=EDGE_CURVE('',#35026,#35027,#3225,.T.);
#43417=EDGE_CURVE('',#35027,#35027,#31406,.T.);
#43418=EDGE_CURVE('',#35028,#35029,#3226,.T.);
#43419=EDGE_CURVE('',#35028,#35030,#30298,.T.);
#43420=EDGE_CURVE('',#35030,#35029,#31407,.T.);
#43421=EDGE_CURVE('',#35031,#35032,#3227,.T.);
#43422=EDGE_CURVE('',#35028,#35031,#30299,.T.);
#43423=EDGE_CURVE('',#35029,#35033,#31408,.T.);
#43424=EDGE_CURVE('',#35032,#35033,#30300,.F.);
#43425=EDGE_CURVE('',#35034,#35035,#3228,.T.);
#43426=EDGE_CURVE('',#35031,#35034,#30301,.T.);
#43427=EDGE_CURVE('',#35032,#35035,#30302,.F.);
#43428=EDGE_CURVE('',#35036,#35037,#3229,.T.);
#43429=EDGE_CURVE('',#35038,#35036,#31409,.T.);
#43430=EDGE_CURVE('',#35034,#35038,#30303,.T.);
#43431=EDGE_CURVE('',#35035,#35037,#30304,.F.);
#43432=EDGE_CURVE('',#35039,#35040,#31410,.T.);
#43433=EDGE_CURVE('',#35040,#35041,#3230,.T.);
#43434=EDGE_CURVE('',#35041,#35041,#31411,.T.);
#43435=EDGE_CURVE('',#35040,#35039,#31412,.T.);
#43436=EDGE_CURVE('',#35039,#35042,#31413,.T.);
#43437=EDGE_CURVE('',#35042,#35042,#31414,.T.);
#43438=EDGE_CURVE('',#35042,#35043,#31415,.T.);
#43439=EDGE_CURVE('',#35043,#35043,#31416,.T.);
#43440=EDGE_CURVE('',#35044,#35045,#30305,.F.);
#43441=EDGE_CURVE('',#35044,#35046,#3231,.T.);
#43442=EDGE_CURVE('',#35047,#35046,#30306,.F.);
#43443=EDGE_CURVE('',#35045,#35047,#3232,.T.);
#43444=EDGE_CURVE('',#35048,#35049,#30307,.F.);
#43445=EDGE_CURVE('',#35048,#35050,#3233,.T.);
#43446=EDGE_CURVE('',#35051,#35050,#30308,.F.);
#43447=EDGE_CURVE('',#35049,#35051,#3234,.T.);
#43448=EDGE_CURVE('',#35043,#35052,#3235,.T.);
#43449=EDGE_CURVE('',#35052,#35053,#31417,.T.);
#43450=EDGE_CURVE('',#35053,#35054,#30309,.T.);
#43451=EDGE_CURVE('',#35055,#35054,#31418,.T.);
#43452=EDGE_CURVE('',#35055,#35056,#3236,.T.);
#43453=EDGE_CURVE('',#35056,#35056,#31419,.T.);
#43454=EDGE_CURVE('',#35044,#35055,#31420,.T.);
#43455=EDGE_CURVE('',#35045,#35052,#31421,.T.);
#43456=EDGE_CURVE('',#35057,#35058,#31422,.T.);
#43457=EDGE_CURVE('',#35057,#35059,#30310,.T.);
#43458=EDGE_CURVE('',#35059,#35060,#31423,.T.);
#43459=EDGE_CURVE('',#35060,#35058,#30311,.T.);
#43460=EDGE_CURVE('',#35061,#35062,#31424,.T.);
#43461=EDGE_CURVE('',#35062,#35063,#30312,.T.);
#43462=EDGE_CURVE('',#35064,#35063,#31425,.T.);
#43463=EDGE_CURVE('',#35064,#35061,#30313,.T.);
#43464=EDGE_CURVE('',#35065,#35050,#31426,.T.);
#43465=EDGE_CURVE('',#35065,#35066,#30314,.T.);
#43466=EDGE_CURVE('',#35066,#35051,#31427,.T.);
#43467=EDGE_CURVE('',#35067,#35068,#30315,.F.);
#43468=EDGE_CURVE('',#35067,#35063,#3237,.T.);
#43469=EDGE_CURVE('',#35068,#35062,#3238,.T.);
#43470=EDGE_CURVE('',#35057,#35069,#3239,.T.);
#43471=EDGE_CURVE('',#35070,#35069,#30316,.F.);
#43472=EDGE_CURVE('',#35059,#35070,#3240,.T.);
#43473=EDGE_CURVE('',#35071,#35071,#31428,.T.);
#43474=EDGE_CURVE('',#35071,#35072,#3241,.T.);
#43475=EDGE_CURVE('',#35072,#35073,#31429,.T.);
#43476=EDGE_CURVE('',#35073,#35074,#30317,.T.);
#43477=EDGE_CURVE('',#35075,#35074,#31430,.T.);
#43478=EDGE_CURVE('',#35075,#35076,#3242,.T.);
#43479=EDGE_CURVE('',#35076,#35076,#31431,.T.);
#43480=EDGE_CURVE('',#35047,#35075,#31432,.T.);
#43481=EDGE_CURVE('',#35046,#35072,#31433,.T.);
#43482=EDGE_CURVE('',#35077,#35067,#31434,.T.);
#43483=EDGE_CURVE('',#35078,#35068,#31435,.T.);
#43484=EDGE_CURVE('',#35078,#35077,#30318,.T.);
#43485=EDGE_CURVE('',#35070,#35079,#31436,.T.);
#43486=EDGE_CURVE('',#35069,#35080,#31437,.T.);
#43487=EDGE_CURVE('',#35080,#35079,#30319,.T.);
#43488=EDGE_CURVE('',#35081,#35048,#31438,.T.);
#43489=EDGE_CURVE('',#35082,#35049,#31439,.T.);
#43490=EDGE_CURVE('',#35082,#35081,#30320,.T.);
#43491=EDGE_CURVE('',#35083,#35083,#31440,.T.);
#43492=EDGE_CURVE('',#35083,#35071,#31441,.T.);
#43493=EDGE_CURVE('',#35084,#35084,#31442,.T.);
#43494=EDGE_CURVE('',#35084,#35085,#3243,.T.);
#43495=EDGE_CURVE('',#35085,#35085,#31443,.T.);
#43496=EDGE_CURVE('',#35086,#35086,#31444,.T.);
#43497=EDGE_CURVE('',#35086,#35087,#3244,.T.);
#43498=EDGE_CURVE('',#35087,#35087,#31445,.T.);
#43499=EDGE_CURVE('',#35076,#35088,#31446,.T.);
#43500=EDGE_CURVE('',#35088,#35088,#31447,.T.);
#43501=EDGE_CURVE('',#35088,#35089,#31448,.T.);
#43502=EDGE_CURVE('',#35090,#35089,#31449,.T.);
#43503=EDGE_CURVE('',#35089,#35090,#31450,.T.);
#43504=EDGE_CURVE('',#35091,#35091,#31451,.T.);
#43505=EDGE_CURVE('',#35091,#35090,#3245,.T.);
#43506=EDGE_CURVE('',#35092,#35092,#31452,.T.);
#43507=EDGE_CURVE('',#35092,#35093,#3246,.T.);
#43508=EDGE_CURVE('',#35093,#35093,#31453,.T.);
#43509=EDGE_CURVE('',#35094,#35094,#31454,.T.);
#43510=EDGE_CURVE('',#35094,#35095,#3247,.T.);
#43511=EDGE_CURVE('',#35095,#35095,#31455,.T.);
#43512=EDGE_CURVE('',#35096,#35096,#31456,.T.);
#43513=EDGE_CURVE('',#35096,#35097,#3248,.T.);
#43514=EDGE_CURVE('',#35097,#35097,#31457,.T.);
#43515=EDGE_CURVE('',#35098,#35099,#31458,.T.);
#43516=EDGE_CURVE('',#35100,#35099,#3249,.T.);
#43517=EDGE_CURVE('',#35101,#35100,#31459,.T.);
#43518=EDGE_CURVE('',#35101,#35102,#3250,.T.);
#43519=EDGE_CURVE('',#35102,#35103,#31460,.T.);
#43520=EDGE_CURVE('',#35103,#35104,#3251,.T.);
#43521=EDGE_CURVE('',#35105,#35104,#31461,.T.);
#43522=EDGE_CURVE('',#35105,#35106,#3252,.T.);
#43523=EDGE_CURVE('',#35106,#35106,#31462,.T.);
#43524=EDGE_CURVE('',#35107,#35105,#31463,.T.);
#43525=EDGE_CURVE('',#35098,#35107,#3253,.T.);
#43526=EDGE_CURVE('',#35108,#35030,#30321,.F.);
#43527=EDGE_CURVE('',#35109,#35108,#31464,.T.);
#43528=EDGE_CURVE('',#35109,#35110,#30322,.T.);
#43529=EDGE_CURVE('',#35110,#35033,#30323,.T.);
#43530=EDGE_CURVE('',#35111,#35111,#31465,.T.);
#43531=EDGE_CURVE('',#35111,#35112,#3254,.T.);
#43532=EDGE_CURVE('',#35112,#35112,#31466,.T.);
#43533=EDGE_CURVE('',#35113,#35114,#30324,.T.);
#43534=EDGE_CURVE('',#35115,#35114,#30325,.T.);
#43535=EDGE_CURVE('',#35116,#35115,#30326,.T.);
#43536=EDGE_CURVE('',#35037,#35116,#30327,.F.);
#43537=EDGE_CURVE('',#35113,#35032,#3255,.T.);
#43538=EDGE_CURVE('',#35117,#35113,#3256,.T.);
#43539=EDGE_CURVE('',#35118,#35113,#30328,.T.);
#43540=EDGE_CURVE('',#35119,#35118,#30329,.T.);
#43541=EDGE_CURVE('',#35119,#35120,#30330,.T.);
#43542=EDGE_CURVE('',#35120,#35117,#30331,.T.);
#43543=EDGE_CURVE('',#35117,#35121,#30332,.T.);
#43544=EDGE_CURVE('',#35122,#35121,#30333,.T.);
#43545=EDGE_CURVE('',#35114,#35122,#30334,.T.);
#43546=EDGE_CURVE('',#35102,#35123,#1802,.T.);
#43547=EDGE_CURVE('',#35100,#35101,#3257,.T.);
#43548=EDGE_CURVE('',#35124,#35099,#1803,.T.);
#43549=EDGE_CURVE('',#35124,#35123,#3258,.T.);
#43550=EDGE_CURVE('',#35125,#35103,#1804,.T.);
#43551=EDGE_CURVE('',#35125,#35123,#31467,.T.);
#43552=EDGE_CURVE('',#35098,#35126,#1805,.T.);
#43553=EDGE_CURVE('',#35124,#35126,#31468,.T.);
#43554=EDGE_CURVE('',#35104,#35107,#3259,.T.);
#43555=EDGE_CURVE('',#35125,#35126,#3260,.T.);
#43556=EDGE_CURVE('',#35121,#35127,#30335,.T.);
#43557=EDGE_CURVE('',#35127,#35038,#30336,.T.);
#43558=EDGE_CURVE('',#35036,#35116,#31469,.T.);
#43559=EDGE_CURVE('',#35028,#35117,#3261,.T.);
#43560=EDGE_CURVE('',#35118,#35109,#30337,.T.);
#43561=EDGE_CURVE('',#35128,#35120,#30338,.T.);
#43562=EDGE_CURVE('',#35128,#35108,#30339,.T.);
#43563=EDGE_CURVE('',#35129,#35130,#31470,.T.);
#43564=EDGE_CURVE('',#35131,#35129,#3262,.T.);
#43565=EDGE_CURVE('',#35132,#35131,#3263,.T.);
#43566=EDGE_CURVE('',#35132,#35130,#3264,.T.);
#43567=EDGE_CURVE('',#35133,#35132,#3265,.T.);
#43568=EDGE_CURVE('',#35133,#35134,#31471,.T.);
#43569=EDGE_CURVE('',#35134,#35135,#3266,.T.);
#43570=EDGE_CURVE('',#35130,#35135,#31472,.T.);
#43571=EDGE_CURVE('',#35135,#35136,#31473,.T.);
#43572=EDGE_CURVE('',#35134,#35137,#31474,.T.);
#43573=EDGE_CURVE('',#35137,#35136,#3267,.T.);
#43574=EDGE_CURVE('',#35136,#35129,#31475,.T.);
#43575=EDGE_CURVE('',#35137,#35138,#31476,.T.);
#43576=EDGE_CURVE('',#35131,#35138,#3268,.T.);
#43577=EDGE_CURVE('',#35138,#35133,#31477,.T.);
#43578=EDGE_CURVE('',#35139,#35140,#31478,.T.);
#43579=EDGE_CURVE('',#35141,#35139,#3269,.T.);
#43580=EDGE_CURVE('',#35142,#35141,#3270,.T.);
#43581=EDGE_CURVE('',#35142,#35140,#3271,.T.);
#43582=EDGE_CURVE('',#35143,#35144,#31479,.T.);
#43583=EDGE_CURVE('',#35144,#35145,#3272,.T.);
#43584=EDGE_CURVE('',#35140,#35145,#31480,.T.);
#43585=EDGE_CURVE('',#35143,#35142,#3273,.T.);
#43586=EDGE_CURVE('',#35145,#35146,#31481,.T.);
#43587=EDGE_CURVE('',#35144,#35147,#31482,.T.);
#43588=EDGE_CURVE('',#35147,#35146,#3274,.T.);
#43589=EDGE_CURVE('',#35146,#35139,#31483,.T.);
#43590=EDGE_CURVE('',#35147,#35148,#31484,.T.);
#43591=EDGE_CURVE('',#35141,#35148,#3275,.T.);
#43592=EDGE_CURVE('',#35148,#35143,#31485,.T.);
#43593=EDGE_CURVE('',#35149,#35150,#3276,.T.);
#43594=EDGE_CURVE('',#35149,#35151,#31486,.T.);
#43595=EDGE_CURVE('',#35151,#35152,#3277,.T.);
#43596=EDGE_CURVE('',#35150,#35152,#31487,.T.);
#43597=EDGE_CURVE('',#35153,#35154,#3278,.T.);
#43598=EDGE_CURVE('',#35149,#35153,#3279,.T.);
#43599=EDGE_CURVE('',#35154,#35150,#31488,.T.);
#43600=EDGE_CURVE('',#35155,#35156,#3280,.T.);
#43601=EDGE_CURVE('',#35153,#35155,#3281,.T.);
#43602=EDGE_CURVE('',#35156,#35154,#31489,.T.);
#43603=EDGE_CURVE('',#35151,#35157,#31490,.T.);
#43604=EDGE_CURVE('',#35155,#35157,#3282,.T.);
#43605=EDGE_CURVE('',#35152,#35156,#31491,.T.);
#43606=EDGE_CURVE('',#35157,#35149,#31492,.T.);
#43607=EDGE_CURVE('',#35158,#35159,#3283,.T.);
#43608=EDGE_CURVE('',#35158,#35160,#31493,.T.);
#43609=EDGE_CURVE('',#35160,#35161,#3284,.T.);
#43610=EDGE_CURVE('',#35159,#35161,#31494,.T.);
#43611=EDGE_CURVE('',#35162,#35163,#3285,.T.);
#43612=EDGE_CURVE('',#35162,#35158,#31495,.T.);
#43613=EDGE_CURVE('',#35163,#35159,#31496,.T.);
#43614=EDGE_CURVE('',#35164,#35165,#3286,.T.);
#43615=EDGE_CURVE('',#35164,#35162,#31497,.T.);
#43616=EDGE_CURVE('',#35165,#35163,#31498,.T.);
#43617=EDGE_CURVE('',#35160,#35164,#31499,.T.);
#43618=EDGE_CURVE('',#35161,#35165,#31500,.T.);
#43619=EDGE_CURVE('',#35166,#35167,#3287,.T.);
#43620=EDGE_CURVE('',#35166,#35168,#31501,.T.);
#43621=EDGE_CURVE('',#35168,#35169,#3288,.T.);
#43622=EDGE_CURVE('',#35167,#35169,#31502,.T.);
#43623=EDGE_CURVE('',#35170,#35171,#3289,.T.);
#43624=EDGE_CURVE('',#35170,#35166,#31503,.T.);
#43625=EDGE_CURVE('',#35171,#35167,#31504,.T.);
#43626=EDGE_CURVE('',#35172,#35173,#3290,.T.);
#43627=EDGE_CURVE('',#35172,#35170,#31505,.T.);
#43628=EDGE_CURVE('',#35173,#35171,#31506,.T.);
#43629=EDGE_CURVE('',#35168,#35172,#31507,.T.);
#43630=EDGE_CURVE('',#35169,#35173,#31508,.T.);
#43631=EDGE_CURVE('',#35174,#35175,#3291,.T.);
#43632=EDGE_CURVE('',#35174,#35176,#31509,.T.);
#43633=EDGE_CURVE('',#35176,#35177,#3292,.T.);
#43634=EDGE_CURVE('',#35175,#35177,#31510,.T.);
#43635=EDGE_CURVE('',#35178,#35179,#3293,.T.);
#43636=EDGE_CURVE('',#35178,#35174,#31511,.T.);
#43637=EDGE_CURVE('',#35179,#35175,#31512,.T.);
#43638=EDGE_CURVE('',#35180,#35181,#3294,.T.);
#43639=EDGE_CURVE('',#35180,#35178,#31513,.T.);
#43640=EDGE_CURVE('',#35181,#35179,#31514,.T.);
#43641=EDGE_CURVE('',#35176,#35180,#31515,.T.);
#43642=EDGE_CURVE('',#35177,#35181,#31516,.T.);
#43643=EDGE_CURVE('',#35182,#35183,#3295,.T.);
#43644=EDGE_CURVE('',#35182,#35184,#31517,.T.);
#43645=EDGE_CURVE('',#35184,#35185,#3296,.T.);
#43646=EDGE_CURVE('',#35183,#35185,#31518,.T.);
#43647=EDGE_CURVE('',#35186,#35187,#3297,.T.);
#43648=EDGE_CURVE('',#35186,#35182,#31519,.T.);
#43649=EDGE_CURVE('',#35187,#35183,#31520,.T.);
#43650=EDGE_CURVE('',#35188,#35189,#3298,.T.);
#43651=EDGE_CURVE('',#35188,#35186,#31521,.T.);
#43652=EDGE_CURVE('',#35189,#35187,#31522,.T.);
#43653=EDGE_CURVE('',#35184,#35188,#31523,.T.);
#43654=EDGE_CURVE('',#35185,#35189,#31524,.T.);
#43655=EDGE_CURVE('',#35190,#35191,#31525,.T.);
#43656=EDGE_CURVE('',#35192,#35190,#3299,.T.);
#43657=EDGE_CURVE('',#35193,#35192,#3300,.T.);
#43658=EDGE_CURVE('',#35193,#35191,#3301,.T.);
#43659=EDGE_CURVE('',#35194,#35195,#31526,.T.);
#43660=EDGE_CURVE('',#35195,#35196,#3302,.T.);
#43661=EDGE_CURVE('',#35191,#35196,#31527,.T.);
#43662=EDGE_CURVE('',#35194,#35193,#3303,.T.);
#43663=EDGE_CURVE('',#35196,#35197,#31528,.T.);
#43664=EDGE_CURVE('',#35195,#35198,#31529,.T.);
#43665=EDGE_CURVE('',#35198,#35197,#3304,.T.);
#43666=EDGE_CURVE('',#35197,#35190,#31530,.T.);
#43667=EDGE_CURVE('',#35198,#35199,#31531,.T.);
#43668=EDGE_CURVE('',#35192,#35199,#3305,.T.);
#43669=EDGE_CURVE('',#35199,#35194,#31532,.T.);
#43670=EDGE_CURVE('',#35200,#35201,#3306,.T.);
#43671=EDGE_CURVE('',#35200,#35202,#31533,.T.);
#43672=EDGE_CURVE('',#35202,#35203,#3307,.T.);
#43673=EDGE_CURVE('',#35201,#35203,#31534,.T.);
#43674=EDGE_CURVE('',#35204,#35205,#3308,.T.);
#43675=EDGE_CURVE('',#35206,#35204,#3309,.T.);
#43676=EDGE_CURVE('',#35206,#35200,#31535,.T.);
#43677=EDGE_CURVE('',#35205,#35201,#31536,.T.);
#43678=EDGE_CURVE('',#35207,#35208,#3310,.T.);
#43679=EDGE_CURVE('',#35204,#35207,#3311,.T.);
#43680=EDGE_CURVE('',#35208,#35205,#31537,.T.);
#43681=EDGE_CURVE('',#35202,#35209,#31538,.T.);
#43682=EDGE_CURVE('',#35207,#35209,#3312,.T.);
#43683=EDGE_CURVE('',#35203,#35208,#31539,.T.);
#43684=EDGE_CURVE('',#35209,#35206,#31540,.T.);
#43685=EDGE_CURVE('',#35210,#35211,#3313,.T.);
#43686=EDGE_CURVE('',#35210,#35212,#31541,.T.);
#43687=EDGE_CURVE('',#35212,#35213,#3314,.T.);
#43688=EDGE_CURVE('',#35211,#35213,#31542,.T.);
#43689=EDGE_CURVE('',#35214,#35215,#3315,.T.);
#43690=EDGE_CURVE('',#35216,#35214,#3316,.T.);
#43691=EDGE_CURVE('',#35216,#35210,#31543,.T.);
#43692=EDGE_CURVE('',#35215,#35211,#31544,.T.);
#43693=EDGE_CURVE('',#35217,#35218,#3317,.T.);
#43694=EDGE_CURVE('',#35214,#35217,#3318,.T.);
#43695=EDGE_CURVE('',#35218,#35215,#31545,.T.);
#43696=EDGE_CURVE('',#35212,#35219,#31546,.T.);
#43697=EDGE_CURVE('',#35217,#35219,#3319,.T.);
#43698=EDGE_CURVE('',#35213,#35218,#31547,.T.);
#43699=EDGE_CURVE('',#35219,#35216,#31548,.T.);
#43700=EDGE_CURVE('',#35220,#35221,#3320,.T.);
#43701=EDGE_CURVE('',#35220,#35222,#31549,.T.);
#43702=EDGE_CURVE('',#35222,#35223,#3321,.T.);
#43703=EDGE_CURVE('',#35221,#35223,#31550,.T.);
#43704=EDGE_CURVE('',#35224,#35225,#3322,.T.);
#43705=EDGE_CURVE('',#35224,#35220,#31551,.T.);
#43706=EDGE_CURVE('',#35225,#35221,#31552,.T.);
#43707=EDGE_CURVE('',#35226,#35227,#3323,.T.);
#43708=EDGE_CURVE('',#35228,#35226,#3324,.T.);
#43709=EDGE_CURVE('',#35228,#35224,#31553,.T.);
#43710=EDGE_CURVE('',#35227,#35225,#31554,.T.);
#43711=EDGE_CURVE('',#35222,#35229,#31555,.T.);
#43712=EDGE_CURVE('',#35226,#35229,#3325,.T.);
#43713=EDGE_CURVE('',#35223,#35227,#31556,.T.);
#43714=EDGE_CURVE('',#35229,#35228,#31557,.T.);
#43715=EDGE_CURVE('',#35230,#35231,#3326,.T.);
#43716=EDGE_CURVE('',#35230,#35232,#31558,.T.);
#43717=EDGE_CURVE('',#35232,#35233,#3327,.T.);
#43718=EDGE_CURVE('',#35231,#35233,#31559,.T.);
#43719=EDGE_CURVE('',#35234,#35235,#3328,.T.);
#43720=EDGE_CURVE('',#35234,#35230,#31560,.T.);
#43721=EDGE_CURVE('',#35235,#35231,#31561,.T.);
#43722=EDGE_CURVE('',#35236,#35237,#3329,.T.);
#43723=EDGE_CURVE('',#35236,#35234,#31562,.T.);
#43724=EDGE_CURVE('',#35237,#35235,#31563,.T.);
#43725=EDGE_CURVE('',#35232,#35236,#31564,.T.);
#43726=EDGE_CURVE('',#35233,#35237,#31565,.T.);
#43727=EDGE_CURVE('',#35238,#35239,#3330,.T.);
#43728=EDGE_CURVE('',#35238,#35240,#31566,.T.);
#43729=EDGE_CURVE('',#35240,#35241,#3331,.T.);
#43730=EDGE_CURVE('',#35239,#35241,#31567,.T.);
#43731=EDGE_CURVE('',#35242,#35243,#3332,.T.);
#43732=EDGE_CURVE('',#35244,#35242,#3333,.T.);
#43733=EDGE_CURVE('',#35244,#35238,#31568,.T.);
#43734=EDGE_CURVE('',#35243,#35239,#31569,.T.);
#43735=EDGE_CURVE('',#35245,#35246,#3334,.T.);
#43736=EDGE_CURVE('',#35242,#35245,#3335,.T.);
#43737=EDGE_CURVE('',#35246,#35243,#31570,.T.);
#43738=EDGE_CURVE('',#35240,#35247,#31571,.T.);
#43739=EDGE_CURVE('',#35245,#35247,#3336,.T.);
#43740=EDGE_CURVE('',#35241,#35246,#31572,.T.);
#43741=EDGE_CURVE('',#35247,#35244,#31573,.T.);
#43742=EDGE_CURVE('',#35248,#35249,#3337,.T.);
#43743=EDGE_CURVE('',#35248,#35250,#31574,.T.);
#43744=EDGE_CURVE('',#35250,#35251,#3338,.T.);
#43745=EDGE_CURVE('',#35249,#35251,#31575,.T.);
#43746=EDGE_CURVE('',#35252,#35253,#3339,.T.);
#43747=EDGE_CURVE('',#35254,#35252,#3340,.T.);
#43748=EDGE_CURVE('',#35254,#35248,#31576,.T.);
#43749=EDGE_CURVE('',#35253,#35249,#31577,.T.);
#43750=EDGE_CURVE('',#35255,#35256,#3341,.T.);
#43751=EDGE_CURVE('',#35252,#35255,#3342,.T.);
#43752=EDGE_CURVE('',#35256,#35253,#31578,.T.);
#43753=EDGE_CURVE('',#35250,#35257,#31579,.T.);
#43754=EDGE_CURVE('',#35255,#35257,#3343,.T.);
#43755=EDGE_CURVE('',#35251,#35256,#31580,.T.);
#43756=EDGE_CURVE('',#35257,#35254,#31581,.T.);
#43757=EDGE_CURVE('',#35258,#35259,#3344,.T.);
#43758=EDGE_CURVE('',#35258,#35260,#31582,.T.);
#43759=EDGE_CURVE('',#35260,#35261,#3345,.T.);
#43760=EDGE_CURVE('',#35259,#35261,#31583,.T.);
#43761=EDGE_CURVE('',#35262,#35263,#3346,.T.);
#43762=EDGE_CURVE('',#35264,#35262,#3347,.T.);
#43763=EDGE_CURVE('',#35264,#35258,#31584,.T.);
#43764=EDGE_CURVE('',#35263,#35259,#31585,.T.);
#43765=EDGE_CURVE('',#35265,#35266,#3348,.T.);
#43766=EDGE_CURVE('',#35262,#35265,#3349,.T.);
#43767=EDGE_CURVE('',#35266,#35263,#31586,.T.);
#43768=EDGE_CURVE('',#35260,#35267,#31587,.T.);
#43769=EDGE_CURVE('',#35265,#35267,#3350,.T.);
#43770=EDGE_CURVE('',#35261,#35266,#31588,.T.);
#43771=EDGE_CURVE('',#35267,#35264,#31589,.T.);
#43772=EDGE_CURVE('',#35268,#35269,#3351,.T.);
#43773=EDGE_CURVE('',#35268,#35270,#31590,.T.);
#43774=EDGE_CURVE('',#35270,#35271,#3352,.T.);
#43775=EDGE_CURVE('',#35269,#35271,#31591,.T.);
#43776=EDGE_CURVE('',#35272,#35273,#3353,.T.);
#43777=EDGE_CURVE('',#35274,#35272,#3354,.T.);
#43778=EDGE_CURVE('',#35274,#35268,#31592,.T.);
#43779=EDGE_CURVE('',#35273,#35269,#31593,.T.);
#43780=EDGE_CURVE('',#35275,#35276,#3355,.T.);
#43781=EDGE_CURVE('',#35272,#35275,#3356,.T.);
#43782=EDGE_CURVE('',#35276,#35273,#31594,.T.);
#43783=EDGE_CURVE('',#35270,#35277,#31595,.T.);
#43784=EDGE_CURVE('',#35275,#35277,#3357,.T.);
#43785=EDGE_CURVE('',#35271,#35276,#31596,.T.);
#43786=EDGE_CURVE('',#35277,#35274,#31597,.T.);
#43787=EDGE_CURVE('',#35278,#35279,#3358,.T.);
#43788=EDGE_CURVE('',#35278,#35280,#31598,.T.);
#43789=EDGE_CURVE('',#35280,#35281,#3359,.T.);
#43790=EDGE_CURVE('',#35279,#35281,#31599,.T.);
#43791=EDGE_CURVE('',#35282,#35283,#3360,.T.);
#43792=EDGE_CURVE('',#35282,#35278,#31600,.T.);
#43793=EDGE_CURVE('',#35283,#35279,#31601,.T.);
#43794=EDGE_CURVE('',#35284,#35285,#3361,.T.);
#43795=EDGE_CURVE('',#35284,#35282,#31602,.T.);
#43796=EDGE_CURVE('',#35285,#35283,#31603,.T.);
#43797=EDGE_CURVE('',#35280,#35284,#31604,.T.);
#43798=EDGE_CURVE('',#35281,#35285,#31605,.T.);
#43799=EDGE_CURVE('',#35286,#35287,#3362,.T.);
#43800=EDGE_CURVE('',#35286,#35288,#31606,.T.);
#43801=EDGE_CURVE('',#35288,#35289,#3363,.T.);
#43802=EDGE_CURVE('',#35287,#35289,#31607,.T.);
#43803=EDGE_CURVE('',#35290,#35291,#3364,.T.);
#43804=EDGE_CURVE('',#35290,#35286,#31608,.T.);
#43805=EDGE_CURVE('',#35291,#35287,#31609,.T.);
#43806=EDGE_CURVE('',#35292,#35293,#3365,.T.);
#43807=EDGE_CURVE('',#35292,#35290,#31610,.T.);
#43808=EDGE_CURVE('',#35293,#35291,#31611,.T.);
#43809=EDGE_CURVE('',#35288,#35292,#31612,.T.);
#43810=EDGE_CURVE('',#35289,#35293,#31613,.T.);
#43811=EDGE_CURVE('',#35294,#35295,#3366,.T.);
#43812=EDGE_CURVE('',#35294,#35296,#31614,.T.);
#43813=EDGE_CURVE('',#35296,#35297,#3367,.T.);
#43814=EDGE_CURVE('',#35295,#35297,#31615,.T.);
#43815=EDGE_CURVE('',#35298,#35299,#3368,.T.);
#43816=EDGE_CURVE('',#35298,#35294,#31616,.T.);
#43817=EDGE_CURVE('',#35299,#35295,#31617,.T.);
#43818=EDGE_CURVE('',#35300,#35301,#3369,.T.);
#43819=EDGE_CURVE('',#35300,#35298,#31618,.T.);
#43820=EDGE_CURVE('',#35301,#35299,#31619,.T.);
#43821=EDGE_CURVE('',#35296,#35300,#31620,.T.);
#43822=EDGE_CURVE('',#35297,#35301,#31621,.T.);
#43823=EDGE_CURVE('',#35302,#35303,#3370,.T.);
#43824=EDGE_CURVE('',#35302,#35304,#31622,.T.);
#43825=EDGE_CURVE('',#35304,#35305,#3371,.T.);
#43826=EDGE_CURVE('',#35303,#35305,#31623,.T.);
#43827=EDGE_CURVE('',#35306,#35307,#3372,.T.);
#43828=EDGE_CURVE('',#35306,#35302,#31624,.T.);
#43829=EDGE_CURVE('',#35307,#35303,#31625,.T.);
#43830=EDGE_CURVE('',#35308,#35309,#3373,.T.);
#43831=EDGE_CURVE('',#35308,#35306,#31626,.T.);
#43832=EDGE_CURVE('',#35309,#35307,#31627,.T.);
#43833=EDGE_CURVE('',#35304,#35308,#31628,.T.);
#43834=EDGE_CURVE('',#35305,#35309,#31629,.T.);
#43835=EDGE_CURVE('',#35310,#35311,#3374,.T.);
#43836=EDGE_CURVE('',#35310,#35312,#31630,.T.);
#43837=EDGE_CURVE('',#35312,#35313,#3375,.T.);
#43838=EDGE_CURVE('',#35311,#35313,#31631,.T.);
#43839=EDGE_CURVE('',#35314,#35315,#3376,.T.);
#43840=EDGE_CURVE('',#35314,#35310,#31632,.T.);
#43841=EDGE_CURVE('',#35315,#35311,#31633,.T.);
#43842=EDGE_CURVE('',#35316,#35317,#3377,.T.);
#43843=EDGE_CURVE('',#35316,#35314,#31634,.T.);
#43844=EDGE_CURVE('',#35317,#35315,#31635,.T.);
#43845=EDGE_CURVE('',#35312,#35316,#31636,.T.);
#43846=EDGE_CURVE('',#35313,#35317,#31637,.T.);
#43847=EDGE_CURVE('',#35318,#35319,#3378,.T.);
#43848=EDGE_CURVE('',#35318,#35320,#31638,.T.);
#43849=EDGE_CURVE('',#35320,#35321,#3379,.T.);
#43850=EDGE_CURVE('',#35319,#35321,#31639,.T.);
#43851=EDGE_CURVE('',#35322,#35323,#3380,.T.);
#43852=EDGE_CURVE('',#35322,#35318,#31640,.T.);
#43853=EDGE_CURVE('',#35323,#35319,#31641,.T.);
#43854=EDGE_CURVE('',#35324,#35325,#3381,.T.);
#43855=EDGE_CURVE('',#35324,#35322,#31642,.T.);
#43856=EDGE_CURVE('',#35325,#35323,#31643,.T.);
#43857=EDGE_CURVE('',#35320,#35324,#31644,.T.);
#43858=EDGE_CURVE('',#35321,#35325,#31645,.T.);
#43859=EDGE_CURVE('',#35326,#35327,#31646,.T.);
#43860=EDGE_CURVE('',#35328,#35326,#3382,.T.);
#43861=EDGE_CURVE('',#35328,#35329,#31647,.T.);
#43862=EDGE_CURVE('',#35329,#35327,#3383,.T.);
#43863=EDGE_CURVE('',#35330,#35326,#31648,.T.);
#43864=EDGE_CURVE('',#35331,#35330,#3384,.T.);
#43865=EDGE_CURVE('',#35331,#35328,#31649,.T.);
#43866=EDGE_CURVE('',#35332,#35333,#3385,.T.);
#43867=EDGE_CURVE('',#35332,#35331,#31650,.T.);
#43868=EDGE_CURVE('',#35334,#35330,#31651,.T.);
#43869=EDGE_CURVE('',#35333,#35334,#3386,.T.);
#43870=EDGE_CURVE('',#35327,#35334,#31652,.T.);
#43871=EDGE_CURVE('',#35329,#35335,#31653,.T.);
#43872=EDGE_CURVE('',#35333,#35335,#3387,.T.);
#43873=EDGE_CURVE('',#35335,#35332,#31654,.T.);
#43874=EDGE_CURVE('',#35336,#35337,#3388,.T.);
#43875=EDGE_CURVE('',#35336,#35338,#31655,.T.);
#43876=EDGE_CURVE('',#35338,#35339,#3389,.T.);
#43877=EDGE_CURVE('',#35337,#35339,#31656,.T.);
#43878=EDGE_CURVE('',#35340,#35341,#3390,.T.);
#43879=EDGE_CURVE('',#35342,#35340,#3391,.T.);
#43880=EDGE_CURVE('',#35342,#35336,#31657,.T.);
#43881=EDGE_CURVE('',#35341,#35337,#31658,.T.);
#43882=EDGE_CURVE('',#35343,#35344,#3392,.T.);
#43883=EDGE_CURVE('',#35340,#35343,#3393,.T.);
#43884=EDGE_CURVE('',#35344,#35341,#31659,.T.);
#43885=EDGE_CURVE('',#35338,#35345,#31660,.T.);
#43886=EDGE_CURVE('',#35343,#35345,#3394,.T.);
#43887=EDGE_CURVE('',#35339,#35344,#31661,.T.);
#43888=EDGE_CURVE('',#35345,#35342,#31662,.T.);
#43889=EDGE_CURVE('',#35346,#35347,#3395,.T.);
#43890=EDGE_CURVE('',#35346,#35348,#31663,.T.);
#43891=EDGE_CURVE('',#35348,#35349,#3396,.T.);
#43892=EDGE_CURVE('',#35347,#35349,#31664,.T.);
#43893=EDGE_CURVE('',#35350,#35351,#3397,.T.);
#43894=EDGE_CURVE('',#35350,#35346,#31665,.T.);
#43895=EDGE_CURVE('',#35351,#35347,#31666,.T.);
#43896=EDGE_CURVE('',#35352,#35353,#3398,.T.);
#43897=EDGE_CURVE('',#35352,#35350,#31667,.T.);
#43898=EDGE_CURVE('',#35353,#35351,#31668,.T.);
#43899=EDGE_CURVE('',#35348,#35352,#31669,.T.);
#43900=EDGE_CURVE('',#35349,#35353,#31670,.T.);
#43901=EDGE_CURVE('',#35354,#35355,#3399,.T.);
#43902=EDGE_CURVE('',#35354,#35356,#31671,.T.);
#43903=EDGE_CURVE('',#35356,#35357,#3400,.T.);
#43904=EDGE_CURVE('',#35355,#35357,#31672,.T.);
#43905=EDGE_CURVE('',#35358,#35359,#3401,.T.);
#43906=EDGE_CURVE('',#35358,#35354,#31673,.T.);
#43907=EDGE_CURVE('',#35359,#35355,#31674,.T.);
#43908=EDGE_CURVE('',#35360,#35361,#3402,.T.);
#43909=EDGE_CURVE('',#35360,#35358,#31675,.T.);
#43910=EDGE_CURVE('',#35361,#35359,#31676,.T.);
#43911=EDGE_CURVE('',#35356,#35360,#31677,.T.);
#43912=EDGE_CURVE('',#35357,#35361,#31678,.T.);
#43913=EDGE_CURVE('',#35362,#35363,#3403,.T.);
#43914=EDGE_CURVE('',#35362,#35364,#31679,.T.);
#43915=EDGE_CURVE('',#35364,#35365,#3404,.T.);
#43916=EDGE_CURVE('',#35363,#35365,#31680,.T.);
#43917=EDGE_CURVE('',#35366,#35367,#3405,.T.);
#43918=EDGE_CURVE('',#35366,#35362,#31681,.T.);
#43919=EDGE_CURVE('',#35367,#35363,#31682,.T.);
#43920=EDGE_CURVE('',#35368,#35369,#3406,.T.);
#43921=EDGE_CURVE('',#35368,#35366,#31683,.T.);
#43922=EDGE_CURVE('',#35369,#35367,#31684,.T.);
#43923=EDGE_CURVE('',#35364,#35368,#31685,.T.);
#43924=EDGE_CURVE('',#35365,#35369,#31686,.T.);
#43925=EDGE_CURVE('',#35370,#35371,#3407,.T.);
#43926=EDGE_CURVE('',#35370,#35372,#31687,.T.);
#43927=EDGE_CURVE('',#35372,#35373,#3408,.T.);
#43928=EDGE_CURVE('',#35371,#35373,#31688,.T.);
#43929=EDGE_CURVE('',#35374,#35375,#3409,.T.);
#43930=EDGE_CURVE('',#35374,#35370,#31689,.T.);
#43931=EDGE_CURVE('',#35375,#35371,#31690,.T.);
#43932=EDGE_CURVE('',#35376,#35377,#3410,.T.);
#43933=EDGE_CURVE('',#35376,#35374,#31691,.T.);
#43934=EDGE_CURVE('',#35377,#35375,#31692,.T.);
#43935=EDGE_CURVE('',#35372,#35376,#31693,.T.);
#43936=EDGE_CURVE('',#35373,#35377,#31694,.T.);
#43937=EDGE_CURVE('',#35378,#35379,#3411,.T.);
#43938=EDGE_CURVE('',#35378,#35380,#31695,.T.);
#43939=EDGE_CURVE('',#35380,#35381,#3412,.T.);
#43940=EDGE_CURVE('',#35379,#35381,#31696,.T.);
#43941=EDGE_CURVE('',#35382,#35383,#3413,.T.);
#43942=EDGE_CURVE('',#35382,#35378,#31697,.T.);
#43943=EDGE_CURVE('',#35383,#35379,#31698,.T.);
#43944=EDGE_CURVE('',#35384,#35385,#3414,.T.);
#43945=EDGE_CURVE('',#35384,#35382,#31699,.T.);
#43946=EDGE_CURVE('',#35385,#35383,#31700,.T.);
#43947=EDGE_CURVE('',#35380,#35384,#31701,.T.);
#43948=EDGE_CURVE('',#35381,#35385,#31702,.T.);
#43949=EDGE_CURVE('',#35386,#35387,#3415,.T.);
#43950=EDGE_CURVE('',#35386,#35388,#31703,.T.);
#43951=EDGE_CURVE('',#35388,#35389,#3416,.T.);
#43952=EDGE_CURVE('',#35387,#35389,#31704,.T.);
#43953=EDGE_CURVE('',#35390,#35391,#3417,.T.);
#43954=EDGE_CURVE('',#35390,#35386,#31705,.T.);
#43955=EDGE_CURVE('',#35391,#35387,#31706,.T.);
#43956=EDGE_CURVE('',#35392,#35393,#3418,.T.);
#43957=EDGE_CURVE('',#35392,#35390,#31707,.T.);
#43958=EDGE_CURVE('',#35393,#35391,#31708,.T.);
#43959=EDGE_CURVE('',#35388,#35392,#31709,.T.);
#43960=EDGE_CURVE('',#35389,#35393,#31710,.T.);
#43961=EDGE_CURVE('',#35394,#35395,#3419,.T.);
#43962=EDGE_CURVE('',#35394,#35396,#31711,.T.);
#43963=EDGE_CURVE('',#35396,#35397,#3420,.T.);
#43964=EDGE_CURVE('',#35395,#35397,#31712,.T.);
#43965=EDGE_CURVE('',#35398,#35399,#3421,.T.);
#43966=EDGE_CURVE('',#35398,#35394,#31713,.T.);
#43967=EDGE_CURVE('',#35399,#35395,#31714,.T.);
#43968=EDGE_CURVE('',#35400,#35401,#3422,.T.);
#43969=EDGE_CURVE('',#35400,#35398,#31715,.T.);
#43970=EDGE_CURVE('',#35401,#35399,#31716,.T.);
#43971=EDGE_CURVE('',#35396,#35400,#31717,.T.);
#43972=EDGE_CURVE('',#35397,#35401,#31718,.T.);
#43973=EDGE_CURVE('',#35402,#35403,#3423,.T.);
#43974=EDGE_CURVE('',#35402,#35404,#31719,.T.);
#43975=EDGE_CURVE('',#35404,#35405,#3424,.T.);
#43976=EDGE_CURVE('',#35403,#35405,#31720,.T.);
#43977=EDGE_CURVE('',#35406,#35407,#3425,.T.);
#43978=EDGE_CURVE('',#35406,#35402,#31721,.T.);
#43979=EDGE_CURVE('',#35407,#35403,#31722,.T.);
#43980=EDGE_CURVE('',#35408,#35409,#3426,.T.);
#43981=EDGE_CURVE('',#35408,#35406,#31723,.T.);
#43982=EDGE_CURVE('',#35409,#35407,#31724,.T.);
#43983=EDGE_CURVE('',#35404,#35408,#31725,.T.);
#43984=EDGE_CURVE('',#35405,#35409,#31726,.T.);
#43985=EDGE_CURVE('',#35410,#35411,#3427,.T.);
#43986=EDGE_CURVE('',#35410,#35412,#31727,.T.);
#43987=EDGE_CURVE('',#35412,#35413,#3428,.T.);
#43988=EDGE_CURVE('',#35411,#35413,#31728,.T.);
#43989=EDGE_CURVE('',#35414,#35415,#3429,.T.);
#43990=EDGE_CURVE('',#35416,#35414,#3430,.T.);
#43991=EDGE_CURVE('',#35416,#35410,#31729,.T.);
#43992=EDGE_CURVE('',#35415,#35411,#31730,.T.);
#43993=EDGE_CURVE('',#35417,#35418,#3431,.T.);
#43994=EDGE_CURVE('',#35414,#35417,#3432,.T.);
#43995=EDGE_CURVE('',#35418,#35415,#31731,.T.);
#43996=EDGE_CURVE('',#35412,#35419,#31732,.T.);
#43997=EDGE_CURVE('',#35417,#35419,#3433,.T.);
#43998=EDGE_CURVE('',#35413,#35418,#31733,.T.);
#43999=EDGE_CURVE('',#35419,#35416,#31734,.T.);
#44000=EDGE_CURVE('',#35420,#35421,#3434,.T.);
#44001=EDGE_CURVE('',#35420,#35422,#31735,.T.);
#44002=EDGE_CURVE('',#35422,#35423,#3435,.T.);
#44003=EDGE_CURVE('',#35421,#35423,#31736,.T.);
#44004=EDGE_CURVE('',#35424,#35425,#3436,.T.);
#44005=EDGE_CURVE('',#35426,#35424,#3437,.T.);
#44006=EDGE_CURVE('',#35426,#35420,#31737,.T.);
#44007=EDGE_CURVE('',#35425,#35421,#31738,.T.);
#44008=EDGE_CURVE('',#35427,#35428,#3438,.T.);
#44009=EDGE_CURVE('',#35424,#35427,#3439,.T.);
#44010=EDGE_CURVE('',#35428,#35425,#31739,.T.);
#44011=EDGE_CURVE('',#35422,#35429,#31740,.T.);
#44012=EDGE_CURVE('',#35427,#35429,#3440,.T.);
#44013=EDGE_CURVE('',#35423,#35428,#31741,.T.);
#44014=EDGE_CURVE('',#35429,#35426,#31742,.T.);
#44015=EDGE_CURVE('',#35430,#35431,#3441,.T.);
#44016=EDGE_CURVE('',#35430,#35432,#31743,.T.);
#44017=EDGE_CURVE('',#35432,#35433,#3442,.T.);
#44018=EDGE_CURVE('',#35431,#35433,#31744,.T.);
#44019=EDGE_CURVE('',#35434,#35435,#3443,.T.);
#44020=EDGE_CURVE('',#35434,#35430,#31745,.T.);
#44021=EDGE_CURVE('',#35435,#35431,#31746,.T.);
#44022=EDGE_CURVE('',#35436,#35437,#3444,.T.);
#44023=EDGE_CURVE('',#35436,#35434,#31747,.T.);
#44024=EDGE_CURVE('',#35437,#35435,#31748,.T.);
#44025=EDGE_CURVE('',#35432,#35436,#31749,.T.);
#44026=EDGE_CURVE('',#35433,#35437,#31750,.T.);
#44027=EDGE_CURVE('',#35438,#35439,#3445,.T.);
#44028=EDGE_CURVE('',#35438,#35440,#31751,.T.);
#44029=EDGE_CURVE('',#35440,#35441,#3446,.T.);
#44030=EDGE_CURVE('',#35439,#35441,#31752,.T.);
#44031=EDGE_CURVE('',#35442,#35443,#3447,.T.);
#44032=EDGE_CURVE('',#35442,#35438,#31753,.T.);
#44033=EDGE_CURVE('',#35443,#35439,#31754,.T.);
#44034=EDGE_CURVE('',#35444,#35445,#3448,.T.);
#44035=EDGE_CURVE('',#35444,#35442,#31755,.T.);
#44036=EDGE_CURVE('',#35445,#35443,#31756,.T.);
#44037=EDGE_CURVE('',#35440,#35444,#31757,.T.);
#44038=EDGE_CURVE('',#35441,#35445,#31758,.T.);
#44039=EDGE_CURVE('',#35446,#35447,#3449,.T.);
#44040=EDGE_CURVE('',#35446,#35448,#31759,.T.);
#44041=EDGE_CURVE('',#35448,#35449,#3450,.T.);
#44042=EDGE_CURVE('',#35447,#35449,#31760,.T.);
#44043=EDGE_CURVE('',#35450,#35451,#3451,.T.);
#44044=EDGE_CURVE('',#35450,#35446,#31761,.T.);
#44045=EDGE_CURVE('',#35451,#35447,#31762,.T.);
#44046=EDGE_CURVE('',#35452,#35453,#3452,.T.);
#44047=EDGE_CURVE('',#35452,#35450,#31763,.T.);
#44048=EDGE_CURVE('',#35453,#35451,#31764,.T.);
#44049=EDGE_CURVE('',#35448,#35452,#31765,.T.);
#44050=EDGE_CURVE('',#35449,#35453,#31766,.T.);
#44051=EDGE_CURVE('',#35454,#35455,#3453,.T.);
#44052=EDGE_CURVE('',#35454,#35456,#31767,.T.);
#44053=EDGE_CURVE('',#35456,#35457,#3454,.T.);
#44054=EDGE_CURVE('',#35455,#35457,#31768,.T.);
#44055=EDGE_CURVE('',#35458,#35459,#3455,.T.);
#44056=EDGE_CURVE('',#35458,#35454,#31769,.T.);
#44057=EDGE_CURVE('',#35459,#35455,#31770,.T.);
#44058=EDGE_CURVE('',#35460,#35461,#3456,.T.);
#44059=EDGE_CURVE('',#35460,#35458,#31771,.T.);
#44060=EDGE_CURVE('',#35461,#35459,#31772,.T.);
#44061=EDGE_CURVE('',#35456,#35460,#31773,.T.);
#44062=EDGE_CURVE('',#35457,#35461,#31774,.T.);
#44063=EDGE_CURVE('',#35462,#35463,#3457,.T.);
#44064=EDGE_CURVE('',#35462,#35464,#31775,.T.);
#44065=EDGE_CURVE('',#35464,#35465,#3458,.T.);
#44066=EDGE_CURVE('',#35463,#35465,#31776,.T.);
#44067=EDGE_CURVE('',#35466,#35467,#3459,.T.);
#44068=EDGE_CURVE('',#35466,#35462,#31777,.T.);
#44069=EDGE_CURVE('',#35467,#35463,#31778,.T.);
#44070=EDGE_CURVE('',#35468,#35469,#3460,.T.);
#44071=EDGE_CURVE('',#35468,#35466,#31779,.T.);
#44072=EDGE_CURVE('',#35469,#35467,#31780,.T.);
#44073=EDGE_CURVE('',#35464,#35468,#31781,.T.);
#44074=EDGE_CURVE('',#35465,#35469,#31782,.T.);
#44075=EDGE_CURVE('',#35470,#35471,#3461,.T.);
#44076=EDGE_CURVE('',#35470,#35472,#31783,.T.);
#44077=EDGE_CURVE('',#35472,#35473,#3462,.T.);
#44078=EDGE_CURVE('',#35471,#35473,#31784,.T.);
#44079=EDGE_CURVE('',#35474,#35475,#3463,.T.);
#44080=EDGE_CURVE('',#35474,#35470,#31785,.T.);
#44081=EDGE_CURVE('',#35475,#35471,#31786,.T.);
#44082=EDGE_CURVE('',#35476,#35477,#3464,.T.);
#44083=EDGE_CURVE('',#35476,#35474,#31787,.T.);
#44084=EDGE_CURVE('',#35477,#35475,#31788,.T.);
#44085=EDGE_CURVE('',#35472,#35476,#31789,.T.);
#44086=EDGE_CURVE('',#35473,#35477,#31790,.T.);
#44087=EDGE_CURVE('',#35478,#35479,#3465,.T.);
#44088=EDGE_CURVE('',#35478,#35480,#31791,.T.);
#44089=EDGE_CURVE('',#35480,#35481,#3466,.T.);
#44090=EDGE_CURVE('',#35479,#35481,#31792,.T.);
#44091=EDGE_CURVE('',#35482,#35483,#3467,.T.);
#44092=EDGE_CURVE('',#35482,#35478,#31793,.T.);
#44093=EDGE_CURVE('',#35483,#35479,#31794,.T.);
#44094=EDGE_CURVE('',#35484,#35485,#3468,.T.);
#44095=EDGE_CURVE('',#35484,#35482,#31795,.T.);
#44096=EDGE_CURVE('',#35485,#35483,#31796,.T.);
#44097=EDGE_CURVE('',#35480,#35484,#31797,.T.);
#44098=EDGE_CURVE('',#35481,#35485,#31798,.T.);
#44099=EDGE_CURVE('',#35486,#35487,#3469,.T.);
#44100=EDGE_CURVE('',#35486,#35488,#31799,.T.);
#44101=EDGE_CURVE('',#35488,#35489,#3470,.T.);
#44102=EDGE_CURVE('',#35487,#35489,#31800,.T.);
#44103=EDGE_CURVE('',#35490,#35491,#3471,.T.);
#44104=EDGE_CURVE('',#35490,#35486,#31801,.T.);
#44105=EDGE_CURVE('',#35491,#35487,#31802,.T.);
#44106=EDGE_CURVE('',#35492,#35493,#3472,.T.);
#44107=EDGE_CURVE('',#35492,#35490,#31803,.T.);
#44108=EDGE_CURVE('',#35493,#35491,#31804,.T.);
#44109=EDGE_CURVE('',#35488,#35492,#31805,.T.);
#44110=EDGE_CURVE('',#35489,#35493,#31806,.T.);
#44111=EDGE_CURVE('',#35494,#35495,#3473,.T.);
#44112=EDGE_CURVE('',#35494,#35496,#31807,.T.);
#44113=EDGE_CURVE('',#35496,#35497,#3474,.T.);
#44114=EDGE_CURVE('',#35495,#35497,#31808,.T.);
#44115=EDGE_CURVE('',#35498,#35499,#3475,.T.);
#44116=EDGE_CURVE('',#35498,#35494,#31809,.T.);
#44117=EDGE_CURVE('',#35499,#35495,#31810,.T.);
#44118=EDGE_CURVE('',#35500,#35501,#3476,.T.);
#44119=EDGE_CURVE('',#35500,#35498,#31811,.T.);
#44120=EDGE_CURVE('',#35501,#35499,#31812,.T.);
#44121=EDGE_CURVE('',#35496,#35500,#31813,.T.);
#44122=EDGE_CURVE('',#35497,#35501,#31814,.T.);
#44123=EDGE_CURVE('',#35502,#35503,#3477,.T.);
#44124=EDGE_CURVE('',#35502,#35504,#31815,.T.);
#44125=EDGE_CURVE('',#35504,#35505,#3478,.T.);
#44126=EDGE_CURVE('',#35503,#35505,#31816,.T.);
#44127=EDGE_CURVE('',#35506,#35507,#3479,.T.);
#44128=EDGE_CURVE('',#35506,#35502,#31817,.T.);
#44129=EDGE_CURVE('',#35507,#35503,#31818,.T.);
#44130=EDGE_CURVE('',#35508,#35509,#3480,.T.);
#44131=EDGE_CURVE('',#35508,#35506,#31819,.T.);
#44132=EDGE_CURVE('',#35509,#35507,#31820,.T.);
#44133=EDGE_CURVE('',#35504,#35508,#31821,.T.);
#44134=EDGE_CURVE('',#35505,#35509,#31822,.T.);
#44135=EDGE_CURVE('',#35510,#35511,#3481,.T.);
#44136=EDGE_CURVE('',#35511,#35512,#3482,.T.);
#44137=EDGE_CURVE('',#35512,#35510,#31823,.T.);
#44138=EDGE_CURVE('',#35513,#35514,#3483,.T.);
#44139=EDGE_CURVE('',#35513,#35515,#31824,.T.);
#44140=EDGE_CURVE('',#35515,#35516,#3484,.T.);
#44141=EDGE_CURVE('',#35514,#35516,#31825,.T.);
#44142=EDGE_CURVE('',#35517,#35518,#3485,.T.);
#44143=EDGE_CURVE('',#35517,#35513,#31826,.T.);
#44144=EDGE_CURVE('',#35518,#35514,#31827,.T.);
#44145=EDGE_CURVE('',#35511,#35519,#3486,.T.);
#44146=EDGE_CURVE('',#35510,#35517,#31828,.T.);
#44147=EDGE_CURVE('',#35519,#35518,#31829,.T.);
#44148=EDGE_CURVE('',#35515,#35512,#31830,.T.);
#44149=EDGE_CURVE('',#35516,#35519,#31831,.T.);
#44150=EDGE_CURVE('',#35520,#35521,#3487,.T.);
#44151=EDGE_CURVE('',#35520,#35522,#31832,.T.);
#44152=EDGE_CURVE('',#35522,#35523,#3488,.T.);
#44153=EDGE_CURVE('',#35521,#35523,#31833,.T.);
#44154=EDGE_CURVE('',#35524,#35525,#3489,.T.);
#44155=EDGE_CURVE('',#35524,#35520,#31834,.T.);
#44156=EDGE_CURVE('',#35525,#35521,#31835,.T.);
#44157=EDGE_CURVE('',#35526,#35527,#3490,.T.);
#44158=EDGE_CURVE('',#35526,#35524,#31836,.T.);
#44159=EDGE_CURVE('',#35527,#35525,#31837,.T.);
#44160=EDGE_CURVE('',#35522,#35526,#31838,.T.);
#44161=EDGE_CURVE('',#35523,#35527,#31839,.T.);
#44162=EDGE_CURVE('',#35528,#35529,#3491,.T.);
#44163=EDGE_CURVE('',#35528,#35530,#31840,.T.);
#44164=EDGE_CURVE('',#35530,#35531,#3492,.T.);
#44165=EDGE_CURVE('',#35529,#35531,#31841,.T.);
#44166=EDGE_CURVE('',#35532,#35533,#3493,.T.);
#44167=EDGE_CURVE('',#35532,#35528,#31842,.T.);
#44168=EDGE_CURVE('',#35533,#35529,#31843,.T.);
#44169=EDGE_CURVE('',#35534,#35535,#3494,.T.);
#44170=EDGE_CURVE('',#35534,#35532,#31844,.T.);
#44171=EDGE_CURVE('',#35535,#35533,#31845,.T.);
#44172=EDGE_CURVE('',#35530,#35534,#31846,.T.);
#44173=EDGE_CURVE('',#35531,#35535,#31847,.T.);
#44174=EDGE_CURVE('',#35536,#35537,#3495,.T.);
#44175=EDGE_CURVE('',#35536,#35538,#31848,.T.);
#44176=EDGE_CURVE('',#35538,#35539,#3496,.T.);
#44177=EDGE_CURVE('',#35537,#35539,#31849,.T.);
#44178=EDGE_CURVE('',#35540,#35541,#3497,.T.);
#44179=EDGE_CURVE('',#35540,#35536,#31850,.T.);
#44180=EDGE_CURVE('',#35541,#35537,#31851,.T.);
#44181=EDGE_CURVE('',#35542,#35543,#3498,.T.);
#44182=EDGE_CURVE('',#35542,#35540,#31852,.T.);
#44183=EDGE_CURVE('',#35543,#35541,#31853,.T.);
#44184=EDGE_CURVE('',#35538,#35542,#31854,.T.);
#44185=EDGE_CURVE('',#35539,#35543,#31855,.T.);
#44186=EDGE_CURVE('',#35544,#35545,#3499,.T.);
#44187=EDGE_CURVE('',#35544,#35546,#31856,.T.);
#44188=EDGE_CURVE('',#35546,#35547,#3500,.T.);
#44189=EDGE_CURVE('',#35545,#35547,#31857,.T.);
#44190=EDGE_CURVE('',#35548,#35549,#3501,.T.);
#44191=EDGE_CURVE('',#35548,#35544,#31858,.T.);
#44192=EDGE_CURVE('',#35549,#35545,#31859,.T.);
#44193=EDGE_CURVE('',#35550,#35551,#3502,.T.);
#44194=EDGE_CURVE('',#35550,#35548,#31860,.T.);
#44195=EDGE_CURVE('',#35551,#35549,#31861,.T.);
#44196=EDGE_CURVE('',#35546,#35550,#31862,.T.);
#44197=EDGE_CURVE('',#35547,#35551,#31863,.T.);
#44198=EDGE_CURVE('',#35552,#35553,#3503,.T.);
#44199=EDGE_CURVE('',#35552,#35554,#31864,.T.);
#44200=EDGE_CURVE('',#35554,#35555,#3504,.T.);
#44201=EDGE_CURVE('',#35553,#35555,#31865,.T.);
#44202=EDGE_CURVE('',#35556,#35557,#3505,.T.);
#44203=EDGE_CURVE('',#35556,#35552,#31866,.T.);
#44204=EDGE_CURVE('',#35557,#35553,#31867,.T.);
#44205=EDGE_CURVE('',#35558,#35559,#3506,.T.);
#44206=EDGE_CURVE('',#35558,#35556,#31868,.T.);
#44207=EDGE_CURVE('',#35559,#35557,#31869,.T.);
#44208=EDGE_CURVE('',#35554,#35558,#31870,.T.);
#44209=EDGE_CURVE('',#35555,#35559,#31871,.T.);
#44210=EDGE_CURVE('',#35560,#35561,#3507,.T.);
#44211=EDGE_CURVE('',#35560,#35562,#31872,.T.);
#44212=EDGE_CURVE('',#35562,#35563,#3508,.T.);
#44213=EDGE_CURVE('',#35561,#35563,#31873,.T.);
#44214=EDGE_CURVE('',#35564,#35565,#3509,.T.);
#44215=EDGE_CURVE('',#35564,#35560,#31874,.T.);
#44216=EDGE_CURVE('',#35565,#35561,#31875,.T.);
#44217=EDGE_CURVE('',#35566,#35567,#3510,.T.);
#44218=EDGE_CURVE('',#35566,#35564,#31876,.T.);
#44219=EDGE_CURVE('',#35567,#35565,#31877,.T.);
#44220=EDGE_CURVE('',#35562,#35566,#31878,.T.);
#44221=EDGE_CURVE('',#35563,#35567,#31879,.T.);
#44222=EDGE_CURVE('',#35568,#35569,#3511,.T.);
#44223=EDGE_CURVE('',#35568,#35570,#31880,.T.);
#44224=EDGE_CURVE('',#35570,#35571,#3512,.T.);
#44225=EDGE_CURVE('',#35569,#35571,#31881,.T.);
#44226=EDGE_CURVE('',#35572,#35573,#3513,.T.);
#44227=EDGE_CURVE('',#35572,#35568,#31882,.T.);
#44228=EDGE_CURVE('',#35573,#35569,#31883,.T.);
#44229=EDGE_CURVE('',#35574,#35575,#3514,.T.);
#44230=EDGE_CURVE('',#35574,#35572,#31884,.T.);
#44231=EDGE_CURVE('',#35575,#35573,#31885,.T.);
#44232=EDGE_CURVE('',#35570,#35574,#31886,.T.);
#44233=EDGE_CURVE('',#35571,#35575,#31887,.T.);
#44234=EDGE_CURVE('',#35576,#35577,#3515,.T.);
#44235=EDGE_CURVE('',#35576,#35578,#31888,.T.);
#44236=EDGE_CURVE('',#35578,#35579,#3516,.T.);
#44237=EDGE_CURVE('',#35577,#35579,#31889,.T.);
#44238=EDGE_CURVE('',#35580,#35581,#3517,.T.);
#44239=EDGE_CURVE('',#35580,#35576,#31890,.T.);
#44240=EDGE_CURVE('',#35581,#35577,#31891,.T.);
#44241=EDGE_CURVE('',#35582,#35583,#3518,.T.);
#44242=EDGE_CURVE('',#35582,#35580,#31892,.T.);
#44243=EDGE_CURVE('',#35583,#35581,#31893,.T.);
#44244=EDGE_CURVE('',#35578,#35582,#31894,.T.);
#44245=EDGE_CURVE('',#35579,#35583,#31895,.T.);
#44246=EDGE_CURVE('',#35584,#35585,#3519,.T.);
#44247=EDGE_CURVE('',#35584,#35586,#31896,.T.);
#44248=EDGE_CURVE('',#35586,#35587,#3520,.T.);
#44249=EDGE_CURVE('',#35585,#35587,#31897,.T.);
#44250=EDGE_CURVE('',#35588,#35589,#3521,.T.);
#44251=EDGE_CURVE('',#35588,#35584,#31898,.T.);
#44252=EDGE_CURVE('',#35589,#35585,#31899,.T.);
#44253=EDGE_CURVE('',#35590,#35591,#3522,.T.);
#44254=EDGE_CURVE('',#35590,#35588,#31900,.T.);
#44255=EDGE_CURVE('',#35591,#35589,#31901,.T.);
#44256=EDGE_CURVE('',#35586,#35590,#31902,.T.);
#44257=EDGE_CURVE('',#35587,#35591,#31903,.T.);
#44258=EDGE_CURVE('',#35592,#35593,#3523,.T.);
#44259=EDGE_CURVE('',#35592,#35594,#31904,.T.);
#44260=EDGE_CURVE('',#35594,#35595,#3524,.T.);
#44261=EDGE_CURVE('',#35593,#35595,#31905,.T.);
#44262=EDGE_CURVE('',#35596,#35597,#3525,.T.);
#44263=EDGE_CURVE('',#35596,#35592,#31906,.T.);
#44264=EDGE_CURVE('',#35597,#35593,#31907,.T.);
#44265=EDGE_CURVE('',#35598,#35599,#3526,.T.);
#44266=EDGE_CURVE('',#35598,#35596,#31908,.T.);
#44267=EDGE_CURVE('',#35599,#35597,#31909,.T.);
#44268=EDGE_CURVE('',#35594,#35598,#31910,.T.);
#44269=EDGE_CURVE('',#35595,#35599,#31911,.T.);
#44270=EDGE_CURVE('',#35600,#35601,#3527,.T.);
#44271=EDGE_CURVE('',#35600,#35602,#31912,.T.);
#44272=EDGE_CURVE('',#35602,#35603,#3528,.T.);
#44273=EDGE_CURVE('',#35601,#35603,#31913,.T.);
#44274=EDGE_CURVE('',#35604,#35605,#3529,.T.);
#44275=EDGE_CURVE('',#35604,#35600,#31914,.T.);
#44276=EDGE_CURVE('',#35605,#35601,#31915,.T.);
#44277=EDGE_CURVE('',#35606,#35607,#3530,.T.);
#44278=EDGE_CURVE('',#35608,#35606,#3531,.T.);
#44279=EDGE_CURVE('',#35608,#35604,#31916,.T.);
#44280=EDGE_CURVE('',#35607,#35605,#31917,.T.);
#44281=EDGE_CURVE('',#35602,#35609,#31918,.T.);
#44282=EDGE_CURVE('',#35606,#35609,#3532,.T.);
#44283=EDGE_CURVE('',#35603,#35607,#31919,.T.);
#44284=EDGE_CURVE('',#35609,#35608,#31920,.T.);
#44285=EDGE_CURVE('',#35610,#35611,#3533,.T.);
#44286=EDGE_CURVE('',#35610,#35612,#31921,.T.);
#44287=EDGE_CURVE('',#35612,#35613,#3534,.T.);
#44288=EDGE_CURVE('',#35611,#35613,#31922,.T.);
#44289=EDGE_CURVE('',#35614,#35615,#3535,.T.);
#44290=EDGE_CURVE('',#35614,#35610,#31923,.T.);
#44291=EDGE_CURVE('',#35615,#35611,#31924,.T.);
#44292=EDGE_CURVE('',#35616,#35617,#3536,.T.);
#44293=EDGE_CURVE('',#35618,#35616,#3537,.T.);
#44294=EDGE_CURVE('',#35618,#35614,#31925,.T.);
#44295=EDGE_CURVE('',#35617,#35615,#31926,.T.);
#44296=EDGE_CURVE('',#35612,#35619,#31927,.T.);
#44297=EDGE_CURVE('',#35616,#35619,#3538,.T.);
#44298=EDGE_CURVE('',#35613,#35617,#31928,.T.);
#44299=EDGE_CURVE('',#35619,#35618,#31929,.T.);
#44300=EDGE_CURVE('',#35620,#35621,#3539,.T.);
#44301=EDGE_CURVE('',#35620,#35622,#31930,.T.);
#44302=EDGE_CURVE('',#35622,#35623,#3540,.T.);
#44303=EDGE_CURVE('',#35621,#35623,#31931,.T.);
#44304=EDGE_CURVE('',#35624,#35625,#3541,.T.);
#44305=EDGE_CURVE('',#35624,#35620,#31932,.T.);
#44306=EDGE_CURVE('',#35625,#35621,#31933,.T.);
#44307=EDGE_CURVE('',#35626,#35627,#3542,.T.);
#44308=EDGE_CURVE('',#35626,#35624,#31934,.T.);
#44309=EDGE_CURVE('',#35627,#35625,#31935,.T.);
#44310=EDGE_CURVE('',#35622,#35626,#31936,.T.);
#44311=EDGE_CURVE('',#35623,#35627,#31937,.T.);
#44312=EDGE_CURVE('',#35628,#35629,#3543,.T.);
#44313=EDGE_CURVE('',#35628,#35630,#31938,.T.);
#44314=EDGE_CURVE('',#35630,#35631,#3544,.T.);
#44315=EDGE_CURVE('',#35629,#35631,#31939,.T.);
#44316=EDGE_CURVE('',#35632,#35633,#3545,.T.);
#44317=EDGE_CURVE('',#35632,#35628,#31940,.T.);
#44318=EDGE_CURVE('',#35633,#35629,#31941,.T.);
#44319=EDGE_CURVE('',#35634,#35635,#3546,.T.);
#44320=EDGE_CURVE('',#35634,#35632,#31942,.T.);
#44321=EDGE_CURVE('',#35635,#35633,#31943,.T.);
#44322=EDGE_CURVE('',#35630,#35634,#31944,.T.);
#44323=EDGE_CURVE('',#35631,#35635,#31945,.T.);
#44324=EDGE_CURVE('',#35636,#35637,#3547,.T.);
#44325=EDGE_CURVE('',#35636,#35638,#31946,.T.);
#44326=EDGE_CURVE('',#35638,#35639,#3548,.T.);
#44327=EDGE_CURVE('',#35637,#35639,#31947,.T.);
#44328=EDGE_CURVE('',#35640,#35641,#3549,.T.);
#44329=EDGE_CURVE('',#35640,#35636,#31948,.T.);
#44330=EDGE_CURVE('',#35641,#35637,#31949,.T.);
#44331=EDGE_CURVE('',#35642,#35643,#3550,.T.);
#44332=EDGE_CURVE('',#35642,#35640,#31950,.T.);
#44333=EDGE_CURVE('',#35643,#35641,#31951,.T.);
#44334=EDGE_CURVE('',#35638,#35642,#31952,.T.);
#44335=EDGE_CURVE('',#35639,#35643,#31953,.T.);
#44336=EDGE_CURVE('',#35644,#35645,#3551,.T.);
#44337=EDGE_CURVE('',#35644,#35646,#31954,.T.);
#44338=EDGE_CURVE('',#35646,#35647,#3552,.T.);
#44339=EDGE_CURVE('',#35645,#35647,#31955,.T.);
#44340=EDGE_CURVE('',#35648,#35649,#3553,.T.);
#44341=EDGE_CURVE('',#35648,#35644,#31956,.T.);
#44342=EDGE_CURVE('',#35649,#35645,#31957,.T.);
#44343=EDGE_CURVE('',#35650,#35651,#3554,.T.);
#44344=EDGE_CURVE('',#35650,#35648,#31958,.T.);
#44345=EDGE_CURVE('',#35651,#35649,#31959,.T.);
#44346=EDGE_CURVE('',#35646,#35650,#31960,.T.);
#44347=EDGE_CURVE('',#35647,#35651,#31961,.T.);
#44348=EDGE_CURVE('',#35652,#35653,#3555,.T.);
#44349=EDGE_CURVE('',#35652,#35654,#31962,.T.);
#44350=EDGE_CURVE('',#35654,#35655,#3556,.T.);
#44351=EDGE_CURVE('',#35653,#35655,#31963,.T.);
#44352=EDGE_CURVE('',#35656,#35657,#3557,.T.);
#44353=EDGE_CURVE('',#35656,#35652,#31964,.T.);
#44354=EDGE_CURVE('',#35657,#35653,#31965,.T.);
#44355=EDGE_CURVE('',#35658,#35659,#3558,.T.);
#44356=EDGE_CURVE('',#35658,#35656,#31966,.T.);
#44357=EDGE_CURVE('',#35659,#35657,#31967,.T.);
#44358=EDGE_CURVE('',#35654,#35658,#31968,.T.);
#44359=EDGE_CURVE('',#35655,#35659,#31969,.T.);
#44360=EDGE_CURVE('',#35660,#35661,#3559,.T.);
#44361=EDGE_CURVE('',#35660,#35662,#31970,.T.);
#44362=EDGE_CURVE('',#35662,#35663,#3560,.T.);
#44363=EDGE_CURVE('',#35661,#35663,#31971,.T.);
#44364=EDGE_CURVE('',#35664,#35665,#3561,.T.);
#44365=EDGE_CURVE('',#35664,#35660,#31972,.T.);
#44366=EDGE_CURVE('',#35665,#35661,#31973,.T.);
#44367=EDGE_CURVE('',#35666,#35667,#3562,.T.);
#44368=EDGE_CURVE('',#35666,#35664,#31974,.T.);
#44369=EDGE_CURVE('',#35667,#35665,#31975,.T.);
#44370=EDGE_CURVE('',#35662,#35666,#31976,.T.);
#44371=EDGE_CURVE('',#35663,#35667,#31977,.T.);
#44372=EDGE_CURVE('',#35668,#35669,#3563,.T.);
#44373=EDGE_CURVE('',#35668,#35670,#31978,.T.);
#44374=EDGE_CURVE('',#35670,#35671,#3564,.T.);
#44375=EDGE_CURVE('',#35669,#35671,#31979,.T.);
#44376=EDGE_CURVE('',#35672,#35673,#3565,.T.);
#44377=EDGE_CURVE('',#35672,#35668,#31980,.T.);
#44378=EDGE_CURVE('',#35673,#35669,#31981,.T.);
#44379=EDGE_CURVE('',#35674,#35675,#3566,.T.);
#44380=EDGE_CURVE('',#35674,#35672,#31982,.T.);
#44381=EDGE_CURVE('',#35675,#35673,#31983,.T.);
#44382=EDGE_CURVE('',#35670,#35674,#31984,.T.);
#44383=EDGE_CURVE('',#35671,#35675,#31985,.T.);
#44384=EDGE_CURVE('',#35676,#35677,#3567,.T.);
#44385=EDGE_CURVE('',#35676,#35678,#31986,.T.);
#44386=EDGE_CURVE('',#35678,#35679,#3568,.T.);
#44387=EDGE_CURVE('',#35677,#35679,#31987,.T.);
#44388=EDGE_CURVE('',#35680,#35681,#3569,.T.);
#44389=EDGE_CURVE('',#35680,#35676,#31988,.T.);
#44390=EDGE_CURVE('',#35681,#35677,#31989,.T.);
#44391=EDGE_CURVE('',#35682,#35683,#3570,.T.);
#44392=EDGE_CURVE('',#35682,#35680,#31990,.T.);
#44393=EDGE_CURVE('',#35683,#35681,#31991,.T.);
#44394=EDGE_CURVE('',#35678,#35682,#31992,.T.);
#44395=EDGE_CURVE('',#35679,#35683,#31993,.T.);
#44396=EDGE_CURVE('',#35684,#35685,#3571,.T.);
#44397=EDGE_CURVE('',#35684,#35686,#31994,.T.);
#44398=EDGE_CURVE('',#35686,#35687,#3572,.T.);
#44399=EDGE_CURVE('',#35685,#35687,#31995,.T.);
#44400=EDGE_CURVE('',#35688,#35689,#3573,.T.);
#44401=EDGE_CURVE('',#35688,#35684,#31996,.T.);
#44402=EDGE_CURVE('',#35689,#35685,#31997,.T.);
#44403=EDGE_CURVE('',#35690,#35691,#3574,.T.);
#44404=EDGE_CURVE('',#35690,#35688,#31998,.T.);
#44405=EDGE_CURVE('',#35691,#35689,#31999,.T.);
#44406=EDGE_CURVE('',#35686,#35690,#32000,.T.);
#44407=EDGE_CURVE('',#35687,#35691,#32001,.T.);
#44408=EDGE_CURVE('',#35692,#35693,#3575,.T.);
#44409=EDGE_CURVE('',#35692,#35694,#32002,.T.);
#44410=EDGE_CURVE('',#35694,#35695,#3576,.T.);
#44411=EDGE_CURVE('',#35693,#35695,#32003,.T.);
#44412=EDGE_CURVE('',#35696,#35697,#3577,.T.);
#44413=EDGE_CURVE('',#35696,#35692,#32004,.T.);
#44414=EDGE_CURVE('',#35697,#35693,#32005,.T.);
#44415=EDGE_CURVE('',#35698,#35699,#3578,.T.);
#44416=EDGE_CURVE('',#35698,#35696,#32006,.T.);
#44417=EDGE_CURVE('',#35699,#35697,#32007,.T.);
#44418=EDGE_CURVE('',#35694,#35698,#32008,.T.);
#44419=EDGE_CURVE('',#35695,#35699,#32009,.T.);
#44420=EDGE_CURVE('',#35700,#35701,#3579,.T.);
#44421=EDGE_CURVE('',#35700,#35702,#32010,.T.);
#44422=EDGE_CURVE('',#35702,#35703,#3580,.T.);
#44423=EDGE_CURVE('',#35701,#35703,#32011,.T.);
#44424=EDGE_CURVE('',#35704,#35705,#3581,.T.);
#44425=EDGE_CURVE('',#35704,#35700,#32012,.T.);
#44426=EDGE_CURVE('',#35705,#35701,#32013,.T.);
#44427=EDGE_CURVE('',#35706,#35707,#3582,.T.);
#44428=EDGE_CURVE('',#35706,#35704,#32014,.T.);
#44429=EDGE_CURVE('',#35707,#35705,#32015,.T.);
#44430=EDGE_CURVE('',#35702,#35706,#32016,.T.);
#44431=EDGE_CURVE('',#35703,#35707,#32017,.T.);
#44432=EDGE_CURVE('',#35708,#35709,#3583,.T.);
#44433=EDGE_CURVE('',#35708,#35710,#32018,.T.);
#44434=EDGE_CURVE('',#35710,#35711,#3584,.T.);
#44435=EDGE_CURVE('',#35709,#35711,#32019,.T.);
#44436=EDGE_CURVE('',#35712,#35713,#3585,.T.);
#44437=EDGE_CURVE('',#35712,#35708,#32020,.T.);
#44438=EDGE_CURVE('',#35713,#35709,#32021,.T.);
#44439=EDGE_CURVE('',#35714,#35715,#3586,.T.);
#44440=EDGE_CURVE('',#35714,#35712,#32022,.T.);
#44441=EDGE_CURVE('',#35715,#35713,#32023,.T.);
#44442=EDGE_CURVE('',#35710,#35714,#32024,.T.);
#44443=EDGE_CURVE('',#35711,#35715,#32025,.T.);
#44444=EDGE_CURVE('',#35716,#35717,#3587,.T.);
#44445=EDGE_CURVE('',#35716,#35718,#32026,.T.);
#44446=EDGE_CURVE('',#35718,#35719,#3588,.T.);
#44447=EDGE_CURVE('',#35717,#35719,#32027,.T.);
#44448=EDGE_CURVE('',#35720,#35721,#3589,.T.);
#44449=EDGE_CURVE('',#35720,#35716,#32028,.T.);
#44450=EDGE_CURVE('',#35721,#35717,#32029,.T.);
#44451=EDGE_CURVE('',#35722,#35723,#3590,.T.);
#44452=EDGE_CURVE('',#35722,#35720,#32030,.T.);
#44453=EDGE_CURVE('',#35723,#35721,#32031,.T.);
#44454=EDGE_CURVE('',#35718,#35722,#32032,.T.);
#44455=EDGE_CURVE('',#35719,#35723,#32033,.T.);
#44456=EDGE_CURVE('',#35724,#35725,#3591,.T.);
#44457=EDGE_CURVE('',#35724,#35726,#32034,.T.);
#44458=EDGE_CURVE('',#35726,#35727,#3592,.T.);
#44459=EDGE_CURVE('',#35725,#35727,#32035,.T.);
#44460=EDGE_CURVE('',#35728,#35729,#3593,.T.);
#44461=EDGE_CURVE('',#35728,#35724,#32036,.T.);
#44462=EDGE_CURVE('',#35729,#35725,#32037,.T.);
#44463=EDGE_CURVE('',#35730,#35731,#3594,.T.);
#44464=EDGE_CURVE('',#35730,#35728,#32038,.T.);
#44465=EDGE_CURVE('',#35731,#35729,#32039,.T.);
#44466=EDGE_CURVE('',#35726,#35730,#32040,.T.);
#44467=EDGE_CURVE('',#35727,#35731,#32041,.T.);
#44468=EDGE_CURVE('',#35732,#35733,#3595,.T.);
#44469=EDGE_CURVE('',#35732,#35734,#32042,.T.);
#44470=EDGE_CURVE('',#35734,#35735,#3596,.T.);
#44471=EDGE_CURVE('',#35733,#35735,#32043,.T.);
#44472=EDGE_CURVE('',#35736,#35737,#3597,.T.);
#44473=EDGE_CURVE('',#35736,#35732,#32044,.T.);
#44474=EDGE_CURVE('',#35737,#35733,#32045,.T.);
#44475=EDGE_CURVE('',#35738,#35739,#3598,.T.);
#44476=EDGE_CURVE('',#35738,#35736,#32046,.T.);
#44477=EDGE_CURVE('',#35739,#35737,#32047,.T.);
#44478=EDGE_CURVE('',#35734,#35738,#32048,.T.);
#44479=EDGE_CURVE('',#35735,#35739,#32049,.T.);
#44480=EDGE_CURVE('',#35740,#35741,#3599,.T.);
#44481=EDGE_CURVE('',#35740,#35742,#32050,.T.);
#44482=EDGE_CURVE('',#35742,#35743,#3600,.T.);
#44483=EDGE_CURVE('',#35741,#35743,#32051,.T.);
#44484=EDGE_CURVE('',#35744,#35745,#3601,.T.);
#44485=EDGE_CURVE('',#35744,#35740,#32052,.T.);
#44486=EDGE_CURVE('',#35745,#35741,#32053,.T.);
#44487=EDGE_CURVE('',#35746,#35747,#3602,.T.);
#44488=EDGE_CURVE('',#35746,#35744,#32054,.T.);
#44489=EDGE_CURVE('',#35747,#35745,#32055,.T.);
#44490=EDGE_CURVE('',#35742,#35746,#32056,.T.);
#44491=EDGE_CURVE('',#35743,#35747,#32057,.T.);
#44492=EDGE_CURVE('',#35748,#35749,#3603,.T.);
#44493=EDGE_CURVE('',#35748,#35750,#32058,.T.);
#44494=EDGE_CURVE('',#35750,#35751,#3604,.T.);
#44495=EDGE_CURVE('',#35749,#35751,#32059,.T.);
#44496=EDGE_CURVE('',#35752,#35753,#3605,.T.);
#44497=EDGE_CURVE('',#35752,#35748,#32060,.T.);
#44498=EDGE_CURVE('',#35753,#35749,#32061,.T.);
#44499=EDGE_CURVE('',#35754,#35755,#3606,.T.);
#44500=EDGE_CURVE('',#35754,#35752,#32062,.T.);
#44501=EDGE_CURVE('',#35755,#35753,#32063,.T.);
#44502=EDGE_CURVE('',#35750,#35754,#32064,.T.);
#44503=EDGE_CURVE('',#35751,#35755,#32065,.T.);
#44504=EDGE_CURVE('',#35756,#35757,#3607,.T.);
#44505=EDGE_CURVE('',#35756,#35758,#32066,.T.);
#44506=EDGE_CURVE('',#35758,#35759,#3608,.T.);
#44507=EDGE_CURVE('',#35757,#35759,#32067,.T.);
#44508=EDGE_CURVE('',#35760,#35761,#3609,.T.);
#44509=EDGE_CURVE('',#35760,#35756,#32068,.T.);
#44510=EDGE_CURVE('',#35761,#35757,#32069,.T.);
#44511=EDGE_CURVE('',#35762,#35763,#3610,.T.);
#44512=EDGE_CURVE('',#35762,#35760,#32070,.T.);
#44513=EDGE_CURVE('',#35763,#35761,#32071,.T.);
#44514=EDGE_CURVE('',#35758,#35762,#32072,.T.);
#44515=EDGE_CURVE('',#35759,#35763,#32073,.T.);
#44516=EDGE_CURVE('',#35764,#35765,#3611,.T.);
#44517=EDGE_CURVE('',#35764,#35766,#32074,.T.);
#44518=EDGE_CURVE('',#35766,#35767,#3612,.T.);
#44519=EDGE_CURVE('',#35765,#35767,#32075,.T.);
#44520=EDGE_CURVE('',#35768,#35769,#3613,.T.);
#44521=EDGE_CURVE('',#35768,#35764,#32076,.T.);
#44522=EDGE_CURVE('',#35769,#35765,#32077,.T.);
#44523=EDGE_CURVE('',#35770,#35771,#3614,.T.);
#44524=EDGE_CURVE('',#35770,#35768,#32078,.T.);
#44525=EDGE_CURVE('',#35771,#35769,#32079,.T.);
#44526=EDGE_CURVE('',#35766,#35770,#32080,.T.);
#44527=EDGE_CURVE('',#35767,#35771,#32081,.T.);
#44528=EDGE_CURVE('',#35772,#35773,#3615,.T.);
#44529=EDGE_CURVE('',#35772,#35774,#32082,.T.);
#44530=EDGE_CURVE('',#35774,#35775,#3616,.T.);
#44531=EDGE_CURVE('',#35773,#35775,#32083,.T.);
#44532=EDGE_CURVE('',#35776,#35777,#3617,.T.);
#44533=EDGE_CURVE('',#35776,#35772,#32084,.T.);
#44534=EDGE_CURVE('',#35777,#35773,#32085,.T.);
#44535=EDGE_CURVE('',#35778,#35779,#3618,.T.);
#44536=EDGE_CURVE('',#35778,#35776,#32086,.T.);
#44537=EDGE_CURVE('',#35779,#35777,#32087,.T.);
#44538=EDGE_CURVE('',#35774,#35778,#32088,.T.);
#44539=EDGE_CURVE('',#35775,#35779,#32089,.T.);
#44540=EDGE_CURVE('',#35780,#35781,#3619,.T.);
#44541=EDGE_CURVE('',#35780,#35782,#32090,.T.);
#44542=EDGE_CURVE('',#35782,#35783,#3620,.T.);
#44543=EDGE_CURVE('',#35781,#35783,#32091,.T.);
#44544=EDGE_CURVE('',#35784,#35785,#3621,.T.);
#44545=EDGE_CURVE('',#35784,#35780,#32092,.T.);
#44546=EDGE_CURVE('',#35785,#35781,#32093,.T.);
#44547=EDGE_CURVE('',#35786,#35787,#3622,.T.);
#44548=EDGE_CURVE('',#35786,#35784,#32094,.T.);
#44549=EDGE_CURVE('',#35787,#35785,#32095,.T.);
#44550=EDGE_CURVE('',#35782,#35786,#32096,.T.);
#44551=EDGE_CURVE('',#35783,#35787,#32097,.T.);
#44552=EDGE_CURVE('',#35788,#35789,#3623,.T.);
#44553=EDGE_CURVE('',#35788,#35790,#32098,.T.);
#44554=EDGE_CURVE('',#35790,#35791,#3624,.T.);
#44555=EDGE_CURVE('',#35789,#35791,#32099,.T.);
#44556=EDGE_CURVE('',#35792,#35793,#3625,.T.);
#44557=EDGE_CURVE('',#35792,#35788,#32100,.T.);
#44558=EDGE_CURVE('',#35793,#35789,#32101,.T.);
#44559=EDGE_CURVE('',#35794,#35795,#3626,.T.);
#44560=EDGE_CURVE('',#35794,#35792,#32102,.T.);
#44561=EDGE_CURVE('',#35795,#35793,#32103,.T.);
#44562=EDGE_CURVE('',#35790,#35794,#32104,.T.);
#44563=EDGE_CURVE('',#35791,#35795,#32105,.T.);
#44564=EDGE_CURVE('',#35796,#35797,#3627,.T.);
#44565=EDGE_CURVE('',#35796,#35798,#32106,.T.);
#44566=EDGE_CURVE('',#35798,#35799,#3628,.T.);
#44567=EDGE_CURVE('',#35797,#35799,#32107,.T.);
#44568=EDGE_CURVE('',#35800,#35801,#3629,.T.);
#44569=EDGE_CURVE('',#35800,#35796,#32108,.T.);
#44570=EDGE_CURVE('',#35801,#35797,#32109,.T.);
#44571=EDGE_CURVE('',#35802,#35803,#3630,.T.);
#44572=EDGE_CURVE('',#35802,#35800,#32110,.T.);
#44573=EDGE_CURVE('',#35803,#35801,#32111,.T.);
#44574=EDGE_CURVE('',#35798,#35802,#32112,.T.);
#44575=EDGE_CURVE('',#35799,#35803,#32113,.T.);
#44576=EDGE_CURVE('',#35804,#35805,#3631,.T.);
#44577=EDGE_CURVE('',#35804,#35806,#32114,.T.);
#44578=EDGE_CURVE('',#35806,#35807,#3632,.T.);
#44579=EDGE_CURVE('',#35805,#35807,#32115,.T.);
#44580=EDGE_CURVE('',#35808,#35809,#3633,.T.);
#44581=EDGE_CURVE('',#35808,#35804,#32116,.T.);
#44582=EDGE_CURVE('',#35809,#35805,#32117,.T.);
#44583=EDGE_CURVE('',#35810,#35811,#3634,.T.);
#44584=EDGE_CURVE('',#35810,#35808,#32118,.T.);
#44585=EDGE_CURVE('',#35811,#35809,#32119,.T.);
#44586=EDGE_CURVE('',#35806,#35810,#32120,.T.);
#44587=EDGE_CURVE('',#35807,#35811,#32121,.T.);
#44588=EDGE_CURVE('',#35812,#35813,#3635,.T.);
#44589=EDGE_CURVE('',#35812,#35814,#32122,.T.);
#44590=EDGE_CURVE('',#35814,#35815,#3636,.T.);
#44591=EDGE_CURVE('',#35813,#35815,#32123,.T.);
#44592=EDGE_CURVE('',#35816,#35817,#3637,.T.);
#44593=EDGE_CURVE('',#35816,#35812,#32124,.T.);
#44594=EDGE_CURVE('',#35817,#35813,#32125,.T.);
#44595=EDGE_CURVE('',#35818,#35819,#3638,.T.);
#44596=EDGE_CURVE('',#35818,#35816,#32126,.T.);
#44597=EDGE_CURVE('',#35819,#35817,#32127,.T.);
#44598=EDGE_CURVE('',#35814,#35818,#32128,.T.);
#44599=EDGE_CURVE('',#35815,#35819,#32129,.T.);
#44600=EDGE_CURVE('',#35820,#35821,#3639,.T.);
#44601=EDGE_CURVE('',#35820,#35822,#32130,.T.);
#44602=EDGE_CURVE('',#35822,#35823,#3640,.T.);
#44603=EDGE_CURVE('',#35821,#35823,#32131,.T.);
#44604=EDGE_CURVE('',#35824,#35825,#3641,.T.);
#44605=EDGE_CURVE('',#35824,#35820,#32132,.T.);
#44606=EDGE_CURVE('',#35825,#35821,#32133,.T.);
#44607=EDGE_CURVE('',#35826,#35827,#3642,.T.);
#44608=EDGE_CURVE('',#35826,#35824,#32134,.T.);
#44609=EDGE_CURVE('',#35827,#35825,#32135,.T.);
#44610=EDGE_CURVE('',#35822,#35826,#32136,.T.);
#44611=EDGE_CURVE('',#35823,#35827,#32137,.T.);
#44612=EDGE_CURVE('',#35828,#35829,#3643,.T.);
#44613=EDGE_CURVE('',#35828,#35830,#32138,.T.);
#44614=EDGE_CURVE('',#35830,#35831,#3644,.T.);
#44615=EDGE_CURVE('',#35829,#35831,#32139,.T.);
#44616=EDGE_CURVE('',#35832,#35833,#3645,.T.);
#44617=EDGE_CURVE('',#35832,#35828,#32140,.T.);
#44618=EDGE_CURVE('',#35833,#35829,#32141,.T.);
#44619=EDGE_CURVE('',#35834,#35835,#3646,.T.);
#44620=EDGE_CURVE('',#35834,#35832,#32142,.T.);
#44621=EDGE_CURVE('',#35835,#35833,#32143,.T.);
#44622=EDGE_CURVE('',#35830,#35834,#32144,.T.);
#44623=EDGE_CURVE('',#35831,#35835,#32145,.T.);
#44624=EDGE_CURVE('',#35836,#35837,#3647,.T.);
#44625=EDGE_CURVE('',#35836,#35838,#32146,.T.);
#44626=EDGE_CURVE('',#35838,#35839,#3648,.T.);
#44627=EDGE_CURVE('',#35837,#35839,#32147,.T.);
#44628=EDGE_CURVE('',#35840,#35841,#3649,.T.);
#44629=EDGE_CURVE('',#35840,#35836,#32148,.T.);
#44630=EDGE_CURVE('',#35841,#35837,#32149,.T.);
#44631=EDGE_CURVE('',#35842,#35843,#3650,.T.);
#44632=EDGE_CURVE('',#35842,#35840,#32150,.T.);
#44633=EDGE_CURVE('',#35843,#35841,#32151,.T.);
#44634=EDGE_CURVE('',#35838,#35842,#32152,.T.);
#44635=EDGE_CURVE('',#35839,#35843,#32153,.T.);
#44636=EDGE_CURVE('',#35844,#35845,#3651,.T.);
#44637=EDGE_CURVE('',#35844,#35846,#32154,.T.);
#44638=EDGE_CURVE('',#35846,#35847,#3652,.T.);
#44639=EDGE_CURVE('',#35845,#35847,#32155,.T.);
#44640=EDGE_CURVE('',#35848,#35849,#3653,.T.);
#44641=EDGE_CURVE('',#35848,#35844,#32156,.T.);
#44642=EDGE_CURVE('',#35849,#35845,#32157,.T.);
#44643=EDGE_CURVE('',#35850,#35851,#3654,.T.);
#44644=EDGE_CURVE('',#35850,#35848,#32158,.T.);
#44645=EDGE_CURVE('',#35851,#35849,#32159,.T.);
#44646=EDGE_CURVE('',#35846,#35850,#32160,.T.);
#44647=EDGE_CURVE('',#35847,#35851,#32161,.T.);
#44648=EDGE_CURVE('',#35852,#35853,#3655,.T.);
#44649=EDGE_CURVE('',#35852,#35854,#32162,.T.);
#44650=EDGE_CURVE('',#35854,#35855,#3656,.T.);
#44651=EDGE_CURVE('',#35853,#35855,#32163,.T.);
#44652=EDGE_CURVE('',#35856,#35857,#3657,.T.);
#44653=EDGE_CURVE('',#35856,#35852,#32164,.T.);
#44654=EDGE_CURVE('',#35857,#35853,#32165,.T.);
#44655=EDGE_CURVE('',#35858,#35859,#3658,.T.);
#44656=EDGE_CURVE('',#35858,#35856,#32166,.T.);
#44657=EDGE_CURVE('',#35859,#35857,#32167,.T.);
#44658=EDGE_CURVE('',#35854,#35858,#32168,.T.);
#44659=EDGE_CURVE('',#35855,#35859,#32169,.T.);
#44660=EDGE_CURVE('',#35860,#35861,#3659,.T.);
#44661=EDGE_CURVE('',#35860,#35862,#32170,.T.);
#44662=EDGE_CURVE('',#35862,#35863,#3660,.T.);
#44663=EDGE_CURVE('',#35861,#35863,#32171,.T.);
#44664=EDGE_CURVE('',#35864,#35865,#3661,.T.);
#44665=EDGE_CURVE('',#35864,#35860,#32172,.T.);
#44666=EDGE_CURVE('',#35865,#35861,#32173,.T.);
#44667=EDGE_CURVE('',#35866,#35867,#3662,.T.);
#44668=EDGE_CURVE('',#35866,#35864,#32174,.T.);
#44669=EDGE_CURVE('',#35867,#35865,#32175,.T.);
#44670=EDGE_CURVE('',#35862,#35866,#32176,.T.);
#44671=EDGE_CURVE('',#35863,#35867,#32177,.T.);
#44672=EDGE_CURVE('',#35868,#35869,#3663,.T.);
#44673=EDGE_CURVE('',#35868,#35870,#32178,.T.);
#44674=EDGE_CURVE('',#35870,#35871,#3664,.T.);
#44675=EDGE_CURVE('',#35869,#35871,#32179,.T.);
#44676=EDGE_CURVE('',#35872,#35873,#3665,.T.);
#44677=EDGE_CURVE('',#35872,#35868,#32180,.T.);
#44678=EDGE_CURVE('',#35873,#35869,#32181,.T.);
#44679=EDGE_CURVE('',#35874,#35875,#3666,.T.);
#44680=EDGE_CURVE('',#35874,#35872,#32182,.T.);
#44681=EDGE_CURVE('',#35875,#35873,#32183,.T.);
#44682=EDGE_CURVE('',#35870,#35874,#32184,.T.);
#44683=EDGE_CURVE('',#35871,#35875,#32185,.T.);
#44684=EDGE_CURVE('',#35876,#35877,#3667,.T.);
#44685=EDGE_CURVE('',#35876,#35878,#32186,.T.);
#44686=EDGE_CURVE('',#35878,#35879,#3668,.T.);
#44687=EDGE_CURVE('',#35877,#35879,#32187,.T.);
#44688=EDGE_CURVE('',#35880,#35881,#3669,.T.);
#44689=EDGE_CURVE('',#35880,#35876,#32188,.T.);
#44690=EDGE_CURVE('',#35881,#35877,#32189,.T.);
#44691=EDGE_CURVE('',#35882,#35883,#3670,.T.);
#44692=EDGE_CURVE('',#35882,#35880,#32190,.T.);
#44693=EDGE_CURVE('',#35883,#35881,#32191,.T.);
#44694=EDGE_CURVE('',#35878,#35882,#32192,.T.);
#44695=EDGE_CURVE('',#35879,#35883,#32193,.T.);
#44696=EDGE_CURVE('',#35884,#35885,#3671,.T.);
#44697=EDGE_CURVE('',#35884,#35886,#32194,.T.);
#44698=EDGE_CURVE('',#35886,#35887,#3672,.T.);
#44699=EDGE_CURVE('',#35885,#35887,#32195,.T.);
#44700=EDGE_CURVE('',#35888,#35889,#3673,.T.);
#44701=EDGE_CURVE('',#35888,#35884,#32196,.T.);
#44702=EDGE_CURVE('',#35889,#35885,#32197,.T.);
#44703=EDGE_CURVE('',#35890,#35891,#3674,.T.);
#44704=EDGE_CURVE('',#35890,#35888,#32198,.T.);
#44705=EDGE_CURVE('',#35891,#35889,#32199,.T.);
#44706=EDGE_CURVE('',#35886,#35890,#32200,.T.);
#44707=EDGE_CURVE('',#35887,#35891,#32201,.T.);
#44708=EDGE_CURVE('',#35892,#35893,#3675,.T.);
#44709=EDGE_CURVE('',#35892,#35894,#32202,.T.);
#44710=EDGE_CURVE('',#35894,#35895,#3676,.T.);
#44711=EDGE_CURVE('',#35893,#35895,#32203,.T.);
#44712=EDGE_CURVE('',#35896,#35897,#3677,.T.);
#44713=EDGE_CURVE('',#35896,#35892,#32204,.T.);
#44714=EDGE_CURVE('',#35897,#35893,#32205,.T.);
#44715=EDGE_CURVE('',#35898,#35899,#3678,.T.);
#44716=EDGE_CURVE('',#35898,#35896,#32206,.T.);
#44717=EDGE_CURVE('',#35899,#35897,#32207,.T.);
#44718=EDGE_CURVE('',#35894,#35898,#32208,.T.);
#44719=EDGE_CURVE('',#35895,#35899,#32209,.T.);
#44720=EDGE_CURVE('',#35900,#35901,#3679,.T.);
#44721=EDGE_CURVE('',#35900,#35902,#32210,.T.);
#44722=EDGE_CURVE('',#35902,#35903,#3680,.T.);
#44723=EDGE_CURVE('',#35901,#35903,#32211,.T.);
#44724=EDGE_CURVE('',#35904,#35905,#3681,.T.);
#44725=EDGE_CURVE('',#35904,#35900,#32212,.T.);
#44726=EDGE_CURVE('',#35905,#35901,#32213,.T.);
#44727=EDGE_CURVE('',#35906,#35907,#3682,.T.);
#44728=EDGE_CURVE('',#35906,#35904,#32214,.T.);
#44729=EDGE_CURVE('',#35907,#35905,#32215,.T.);
#44730=EDGE_CURVE('',#35902,#35906,#32216,.T.);
#44731=EDGE_CURVE('',#35903,#35907,#32217,.T.);
#44732=EDGE_CURVE('',#35908,#35909,#3683,.T.);
#44733=EDGE_CURVE('',#35908,#35910,#32218,.T.);
#44734=EDGE_CURVE('',#35910,#35911,#3684,.T.);
#44735=EDGE_CURVE('',#35909,#35911,#32219,.T.);
#44736=EDGE_CURVE('',#35912,#35913,#3685,.T.);
#44737=EDGE_CURVE('',#35912,#35908,#32220,.T.);
#44738=EDGE_CURVE('',#35913,#35909,#32221,.T.);
#44739=EDGE_CURVE('',#35914,#35915,#3686,.T.);
#44740=EDGE_CURVE('',#35914,#35912,#32222,.T.);
#44741=EDGE_CURVE('',#35915,#35913,#32223,.T.);
#44742=EDGE_CURVE('',#35910,#35914,#32224,.T.);
#44743=EDGE_CURVE('',#35911,#35915,#32225,.T.);
#44744=EDGE_CURVE('',#35916,#35917,#3687,.T.);
#44745=EDGE_CURVE('',#35916,#35918,#32226,.T.);
#44746=EDGE_CURVE('',#35918,#35919,#3688,.T.);
#44747=EDGE_CURVE('',#35917,#35919,#32227,.T.);
#44748=EDGE_CURVE('',#35920,#35921,#3689,.T.);
#44749=EDGE_CURVE('',#35920,#35916,#32228,.T.);
#44750=EDGE_CURVE('',#35921,#35917,#32229,.T.);
#44751=EDGE_CURVE('',#35922,#35923,#3690,.T.);
#44752=EDGE_CURVE('',#35922,#35920,#32230,.T.);
#44753=EDGE_CURVE('',#35923,#35921,#32231,.T.);
#44754=EDGE_CURVE('',#35918,#35922,#32232,.T.);
#44755=EDGE_CURVE('',#35919,#35923,#32233,.T.);
#44756=EDGE_CURVE('',#35924,#35925,#3691,.T.);
#44757=EDGE_CURVE('',#35924,#35926,#32234,.T.);
#44758=EDGE_CURVE('',#35926,#35927,#3692,.T.);
#44759=EDGE_CURVE('',#35925,#35927,#32235,.T.);
#44760=EDGE_CURVE('',#35928,#35929,#3693,.T.);
#44761=EDGE_CURVE('',#35928,#35924,#32236,.T.);
#44762=EDGE_CURVE('',#35929,#35925,#32237,.T.);
#44763=EDGE_CURVE('',#35930,#35931,#3694,.T.);
#44764=EDGE_CURVE('',#35930,#35928,#32238,.T.);
#44765=EDGE_CURVE('',#35931,#35929,#32239,.T.);
#44766=EDGE_CURVE('',#35926,#35930,#32240,.T.);
#44767=EDGE_CURVE('',#35927,#35931,#32241,.T.);
#44768=EDGE_CURVE('',#35932,#35933,#3695,.T.);
#44769=EDGE_CURVE('',#35932,#35934,#32242,.T.);
#44770=EDGE_CURVE('',#35934,#35935,#3696,.T.);
#44771=EDGE_CURVE('',#35933,#35935,#32243,.T.);
#44772=EDGE_CURVE('',#35936,#35937,#3697,.T.);
#44773=EDGE_CURVE('',#35936,#35932,#32244,.T.);
#44774=EDGE_CURVE('',#35937,#35933,#32245,.T.);
#44775=EDGE_CURVE('',#35938,#35939,#3698,.T.);
#44776=EDGE_CURVE('',#35938,#35936,#32246,.T.);
#44777=EDGE_CURVE('',#35939,#35937,#32247,.T.);
#44778=EDGE_CURVE('',#35934,#35938,#32248,.T.);
#44779=EDGE_CURVE('',#35935,#35939,#32249,.T.);
#44780=EDGE_CURVE('',#35940,#35941,#3699,.T.);
#44781=EDGE_CURVE('',#35940,#35942,#32250,.T.);
#44782=EDGE_CURVE('',#35942,#35943,#3700,.T.);
#44783=EDGE_CURVE('',#35941,#35943,#32251,.T.);
#44784=EDGE_CURVE('',#35944,#35945,#3701,.T.);
#44785=EDGE_CURVE('',#35944,#35940,#32252,.T.);
#44786=EDGE_CURVE('',#35945,#35941,#32253,.T.);
#44787=EDGE_CURVE('',#35946,#35947,#3702,.T.);
#44788=EDGE_CURVE('',#35946,#35944,#32254,.T.);
#44789=EDGE_CURVE('',#35947,#35945,#32255,.T.);
#44790=EDGE_CURVE('',#35942,#35946,#32256,.T.);
#44791=EDGE_CURVE('',#35943,#35947,#32257,.T.);
#44792=EDGE_CURVE('',#35948,#35949,#3703,.T.);
#44793=EDGE_CURVE('',#35948,#35950,#32258,.T.);
#44794=EDGE_CURVE('',#35950,#35951,#3704,.T.);
#44795=EDGE_CURVE('',#35949,#35951,#32259,.T.);
#44796=EDGE_CURVE('',#35952,#35953,#3705,.T.);
#44797=EDGE_CURVE('',#35952,#35948,#32260,.T.);
#44798=EDGE_CURVE('',#35953,#35949,#32261,.T.);
#44799=EDGE_CURVE('',#35954,#35955,#3706,.T.);
#44800=EDGE_CURVE('',#35954,#35952,#32262,.T.);
#44801=EDGE_CURVE('',#35955,#35953,#32263,.T.);
#44802=EDGE_CURVE('',#35950,#35954,#32264,.T.);
#44803=EDGE_CURVE('',#35951,#35955,#32265,.T.);
#44804=EDGE_CURVE('',#35956,#35957,#3707,.T.);
#44805=EDGE_CURVE('',#35956,#35958,#32266,.T.);
#44806=EDGE_CURVE('',#35958,#35959,#3708,.T.);
#44807=EDGE_CURVE('',#35957,#35959,#32267,.T.);
#44808=EDGE_CURVE('',#35960,#35961,#3709,.T.);
#44809=EDGE_CURVE('',#35960,#35956,#32268,.T.);
#44810=EDGE_CURVE('',#35961,#35957,#32269,.T.);
#44811=EDGE_CURVE('',#35962,#35963,#3710,.T.);
#44812=EDGE_CURVE('',#35962,#35960,#32270,.T.);
#44813=EDGE_CURVE('',#35963,#35961,#32271,.T.);
#44814=EDGE_CURVE('',#35958,#35962,#32272,.T.);
#44815=EDGE_CURVE('',#35959,#35963,#32273,.T.);
#44816=EDGE_CURVE('',#35964,#35965,#3711,.T.);
#44817=EDGE_CURVE('',#35964,#35966,#32274,.T.);
#44818=EDGE_CURVE('',#35966,#35967,#3712,.T.);
#44819=EDGE_CURVE('',#35965,#35967,#32275,.T.);
#44820=EDGE_CURVE('',#35968,#35969,#3713,.T.);
#44821=EDGE_CURVE('',#35968,#35964,#32276,.T.);
#44822=EDGE_CURVE('',#35969,#35965,#32277,.T.);
#44823=EDGE_CURVE('',#35970,#35971,#3714,.T.);
#44824=EDGE_CURVE('',#35970,#35968,#32278,.T.);
#44825=EDGE_CURVE('',#35971,#35969,#32279,.T.);
#44826=EDGE_CURVE('',#35966,#35970,#32280,.T.);
#44827=EDGE_CURVE('',#35967,#35971,#32281,.T.);
#44828=EDGE_CURVE('',#35972,#35973,#3715,.T.);
#44829=EDGE_CURVE('',#35972,#35974,#32282,.T.);
#44830=EDGE_CURVE('',#35974,#35975,#3716,.T.);
#44831=EDGE_CURVE('',#35973,#35975,#32283,.T.);
#44832=EDGE_CURVE('',#35976,#35977,#3717,.T.);
#44833=EDGE_CURVE('',#35976,#35972,#32284,.T.);
#44834=EDGE_CURVE('',#35977,#35973,#32285,.T.);
#44835=EDGE_CURVE('',#35978,#35979,#3718,.T.);
#44836=EDGE_CURVE('',#35978,#35976,#32286,.T.);
#44837=EDGE_CURVE('',#35979,#35977,#32287,.T.);
#44838=EDGE_CURVE('',#35974,#35978,#32288,.T.);
#44839=EDGE_CURVE('',#35975,#35979,#32289,.T.);
#44840=EDGE_CURVE('',#35980,#35981,#3719,.T.);
#44841=EDGE_CURVE('',#35980,#35982,#32290,.T.);
#44842=EDGE_CURVE('',#35982,#35983,#3720,.T.);
#44843=EDGE_CURVE('',#35981,#35983,#32291,.T.);
#44844=EDGE_CURVE('',#35984,#35985,#3721,.T.);
#44845=EDGE_CURVE('',#35984,#35980,#32292,.T.);
#44846=EDGE_CURVE('',#35985,#35981,#32293,.T.);
#44847=EDGE_CURVE('',#35986,#35987,#3722,.T.);
#44848=EDGE_CURVE('',#35986,#35984,#32294,.T.);
#44849=EDGE_CURVE('',#35987,#35985,#32295,.T.);
#44850=EDGE_CURVE('',#35982,#35986,#32296,.T.);
#44851=EDGE_CURVE('',#35983,#35987,#32297,.T.);
#44852=EDGE_CURVE('',#35988,#35989,#3723,.T.);
#44853=EDGE_CURVE('',#35988,#35990,#32298,.T.);
#44854=EDGE_CURVE('',#35990,#35991,#3724,.T.);
#44855=EDGE_CURVE('',#35989,#35991,#32299,.T.);
#44856=EDGE_CURVE('',#35992,#35993,#3725,.T.);
#44857=EDGE_CURVE('',#35992,#35988,#32300,.T.);
#44858=EDGE_CURVE('',#35993,#35989,#32301,.T.);
#44859=EDGE_CURVE('',#35994,#35995,#3726,.T.);
#44860=EDGE_CURVE('',#35994,#35992,#32302,.T.);
#44861=EDGE_CURVE('',#35995,#35993,#32303,.T.);
#44862=EDGE_CURVE('',#35990,#35994,#32304,.T.);
#44863=EDGE_CURVE('',#35991,#35995,#32305,.T.);
#44864=EDGE_CURVE('',#35996,#35997,#3727,.T.);
#44865=EDGE_CURVE('',#35996,#35998,#32306,.T.);
#44866=EDGE_CURVE('',#35998,#35999,#3728,.T.);
#44867=EDGE_CURVE('',#35997,#35999,#32307,.T.);
#44868=EDGE_CURVE('',#36000,#36001,#3729,.T.);
#44869=EDGE_CURVE('',#36000,#35996,#32308,.T.);
#44870=EDGE_CURVE('',#36001,#35997,#32309,.T.);
#44871=EDGE_CURVE('',#36002,#36003,#3730,.T.);
#44872=EDGE_CURVE('',#36002,#36000,#32310,.T.);
#44873=EDGE_CURVE('',#36003,#36001,#32311,.T.);
#44874=EDGE_CURVE('',#35998,#36002,#32312,.T.);
#44875=EDGE_CURVE('',#35999,#36003,#32313,.T.);
#44876=EDGE_CURVE('',#36004,#36005,#3731,.T.);
#44877=EDGE_CURVE('',#36004,#36006,#32314,.T.);
#44878=EDGE_CURVE('',#36006,#36007,#3732,.T.);
#44879=EDGE_CURVE('',#36005,#36007,#32315,.T.);
#44880=EDGE_CURVE('',#36008,#36009,#3733,.T.);
#44881=EDGE_CURVE('',#36008,#36004,#32316,.T.);
#44882=EDGE_CURVE('',#36009,#36005,#32317,.T.);
#44883=EDGE_CURVE('',#36010,#36011,#3734,.T.);
#44884=EDGE_CURVE('',#36010,#36008,#32318,.T.);
#44885=EDGE_CURVE('',#36011,#36009,#32319,.T.);
#44886=EDGE_CURVE('',#36006,#36010,#32320,.T.);
#44887=EDGE_CURVE('',#36007,#36011,#32321,.T.);
#44888=EDGE_CURVE('',#36012,#36013,#3735,.T.);
#44889=EDGE_CURVE('',#36012,#36014,#32322,.T.);
#44890=EDGE_CURVE('',#36014,#36015,#3736,.T.);
#44891=EDGE_CURVE('',#36013,#36015,#32323,.T.);
#44892=EDGE_CURVE('',#36016,#36017,#3737,.T.);
#44893=EDGE_CURVE('',#36016,#36012,#32324,.T.);
#44894=EDGE_CURVE('',#36017,#36013,#32325,.T.);
#44895=EDGE_CURVE('',#36018,#36019,#3738,.T.);
#44896=EDGE_CURVE('',#36018,#36016,#32326,.T.);
#44897=EDGE_CURVE('',#36019,#36017,#32327,.T.);
#44898=EDGE_CURVE('',#36014,#36018,#32328,.T.);
#44899=EDGE_CURVE('',#36015,#36019,#32329,.T.);
#44900=EDGE_CURVE('',#36020,#36021,#3739,.T.);
#44901=EDGE_CURVE('',#36020,#36022,#32330,.T.);
#44902=EDGE_CURVE('',#36022,#36023,#3740,.T.);
#44903=EDGE_CURVE('',#36021,#36023,#32331,.T.);
#44904=EDGE_CURVE('',#36024,#36025,#3741,.T.);
#44905=EDGE_CURVE('',#36024,#36020,#32332,.T.);
#44906=EDGE_CURVE('',#36025,#36021,#32333,.T.);
#44907=EDGE_CURVE('',#36026,#36027,#3742,.T.);
#44908=EDGE_CURVE('',#36026,#36024,#32334,.T.);
#44909=EDGE_CURVE('',#36027,#36025,#32335,.T.);
#44910=EDGE_CURVE('',#36022,#36026,#32336,.T.);
#44911=EDGE_CURVE('',#36023,#36027,#32337,.T.);
#44912=EDGE_CURVE('',#36028,#36029,#3743,.T.);
#44913=EDGE_CURVE('',#36028,#36030,#32338,.T.);
#44914=EDGE_CURVE('',#36030,#36031,#3744,.T.);
#44915=EDGE_CURVE('',#36029,#36031,#32339,.T.);
#44916=EDGE_CURVE('',#36032,#36033,#3745,.T.);
#44917=EDGE_CURVE('',#36032,#36028,#32340,.T.);
#44918=EDGE_CURVE('',#36033,#36029,#32341,.T.);
#44919=EDGE_CURVE('',#36034,#36035,#3746,.T.);
#44920=EDGE_CURVE('',#36034,#36032,#32342,.T.);
#44921=EDGE_CURVE('',#36035,#36033,#32343,.T.);
#44922=EDGE_CURVE('',#36030,#36034,#32344,.T.);
#44923=EDGE_CURVE('',#36031,#36035,#32345,.T.);
#44924=EDGE_CURVE('',#36036,#36037,#3747,.T.);
#44925=EDGE_CURVE('',#36036,#36038,#32346,.T.);
#44926=EDGE_CURVE('',#36038,#36039,#3748,.T.);
#44927=EDGE_CURVE('',#36037,#36039,#32347,.T.);
#44928=EDGE_CURVE('',#36040,#36041,#3749,.T.);
#44929=EDGE_CURVE('',#36040,#36036,#32348,.T.);
#44930=EDGE_CURVE('',#36041,#36037,#32349,.T.);
#44931=EDGE_CURVE('',#36042,#36043,#3750,.T.);
#44932=EDGE_CURVE('',#36042,#36040,#32350,.T.);
#44933=EDGE_CURVE('',#36043,#36041,#32351,.T.);
#44934=EDGE_CURVE('',#36038,#36042,#32352,.T.);
#44935=EDGE_CURVE('',#36039,#36043,#32353,.T.);
#44936=EDGE_CURVE('',#36044,#36045,#3751,.T.);
#44937=EDGE_CURVE('',#36044,#36046,#32354,.T.);
#44938=EDGE_CURVE('',#36046,#36047,#3752,.T.);
#44939=EDGE_CURVE('',#36045,#36047,#32355,.T.);
#44940=EDGE_CURVE('',#36048,#36049,#3753,.T.);
#44941=EDGE_CURVE('',#36048,#36044,#32356,.T.);
#44942=EDGE_CURVE('',#36049,#36045,#32357,.T.);
#44943=EDGE_CURVE('',#36050,#36051,#3754,.T.);
#44944=EDGE_CURVE('',#36050,#36048,#32358,.T.);
#44945=EDGE_CURVE('',#36051,#36049,#32359,.T.);
#44946=EDGE_CURVE('',#36046,#36050,#32360,.T.);
#44947=EDGE_CURVE('',#36047,#36051,#32361,.T.);
#44948=EDGE_CURVE('',#36052,#36053,#3755,.T.);
#44949=EDGE_CURVE('',#36052,#36054,#32362,.T.);
#44950=EDGE_CURVE('',#36054,#36055,#3756,.T.);
#44951=EDGE_CURVE('',#36053,#36055,#32363,.T.);
#44952=EDGE_CURVE('',#36056,#36057,#3757,.T.);
#44953=EDGE_CURVE('',#36056,#36052,#32364,.T.);
#44954=EDGE_CURVE('',#36057,#36053,#32365,.T.);
#44955=EDGE_CURVE('',#36058,#36059,#3758,.T.);
#44956=EDGE_CURVE('',#36058,#36056,#32366,.T.);
#44957=EDGE_CURVE('',#36059,#36057,#32367,.T.);
#44958=EDGE_CURVE('',#36054,#36058,#32368,.T.);
#44959=EDGE_CURVE('',#36055,#36059,#32369,.T.);
#44960=EDGE_CURVE('',#36060,#36061,#3759,.T.);
#44961=EDGE_CURVE('',#36060,#36062,#32370,.T.);
#44962=EDGE_CURVE('',#36062,#36063,#3760,.T.);
#44963=EDGE_CURVE('',#36061,#36063,#32371,.T.);
#44964=EDGE_CURVE('',#36064,#36065,#3761,.T.);
#44965=EDGE_CURVE('',#36064,#36060,#32372,.T.);
#44966=EDGE_CURVE('',#36065,#36061,#32373,.T.);
#44967=EDGE_CURVE('',#36066,#36067,#3762,.T.);
#44968=EDGE_CURVE('',#36066,#36064,#32374,.T.);
#44969=EDGE_CURVE('',#36067,#36065,#32375,.T.);
#44970=EDGE_CURVE('',#36062,#36066,#32376,.T.);
#44971=EDGE_CURVE('',#36063,#36067,#32377,.T.);
#44972=EDGE_CURVE('',#36068,#36069,#3763,.T.);
#44973=EDGE_CURVE('',#36068,#36070,#32378,.T.);
#44974=EDGE_CURVE('',#36070,#36071,#3764,.T.);
#44975=EDGE_CURVE('',#36069,#36071,#32379,.T.);
#44976=EDGE_CURVE('',#36072,#36073,#3765,.T.);
#44977=EDGE_CURVE('',#36072,#36068,#32380,.T.);
#44978=EDGE_CURVE('',#36073,#36069,#32381,.T.);
#44979=EDGE_CURVE('',#36074,#36075,#3766,.T.);
#44980=EDGE_CURVE('',#36074,#36072,#32382,.T.);
#44981=EDGE_CURVE('',#36075,#36073,#32383,.T.);
#44982=EDGE_CURVE('',#36070,#36074,#32384,.T.);
#44983=EDGE_CURVE('',#36071,#36075,#32385,.T.);
#44984=EDGE_CURVE('',#36076,#36077,#3767,.T.);
#44985=EDGE_CURVE('',#36076,#36078,#32386,.T.);
#44986=EDGE_CURVE('',#36078,#36079,#3768,.T.);
#44987=EDGE_CURVE('',#36077,#36079,#32387,.T.);
#44988=EDGE_CURVE('',#36080,#36081,#3769,.T.);
#44989=EDGE_CURVE('',#36080,#36076,#32388,.T.);
#44990=EDGE_CURVE('',#36081,#36077,#32389,.T.);
#44991=EDGE_CURVE('',#36082,#36083,#3770,.T.);
#44992=EDGE_CURVE('',#36082,#36080,#32390,.T.);
#44993=EDGE_CURVE('',#36083,#36081,#32391,.T.);
#44994=EDGE_CURVE('',#36078,#36082,#32392,.T.);
#44995=EDGE_CURVE('',#36079,#36083,#32393,.T.);
#44996=EDGE_CURVE('',#36084,#36085,#3771,.T.);
#44997=EDGE_CURVE('',#36084,#36086,#32394,.T.);
#44998=EDGE_CURVE('',#36086,#36087,#3772,.T.);
#44999=EDGE_CURVE('',#36085,#36087,#32395,.T.);
#45000=EDGE_CURVE('',#36088,#36089,#3773,.T.);
#45001=EDGE_CURVE('',#36088,#36084,#32396,.T.);
#45002=EDGE_CURVE('',#36089,#36085,#32397,.T.);
#45003=EDGE_CURVE('',#36090,#36091,#3774,.T.);
#45004=EDGE_CURVE('',#36090,#36088,#32398,.T.);
#45005=EDGE_CURVE('',#36091,#36089,#32399,.T.);
#45006=EDGE_CURVE('',#36086,#36090,#32400,.T.);
#45007=EDGE_CURVE('',#36087,#36091,#32401,.T.);
#45008=EDGE_CURVE('',#36092,#36093,#3775,.T.);
#45009=EDGE_CURVE('',#36092,#36094,#32402,.T.);
#45010=EDGE_CURVE('',#36094,#36095,#3776,.T.);
#45011=EDGE_CURVE('',#36093,#36095,#32403,.T.);
#45012=EDGE_CURVE('',#36096,#36097,#3777,.T.);
#45013=EDGE_CURVE('',#36096,#36092,#32404,.T.);
#45014=EDGE_CURVE('',#36097,#36093,#32405,.T.);
#45015=EDGE_CURVE('',#36098,#36099,#3778,.T.);
#45016=EDGE_CURVE('',#36098,#36096,#32406,.T.);
#45017=EDGE_CURVE('',#36099,#36097,#32407,.T.);
#45018=EDGE_CURVE('',#36094,#36098,#32408,.T.);
#45019=EDGE_CURVE('',#36095,#36099,#32409,.T.);
#45020=EDGE_CURVE('',#36100,#36101,#3779,.T.);
#45021=EDGE_CURVE('',#36100,#36102,#32410,.T.);
#45022=EDGE_CURVE('',#36102,#36103,#3780,.T.);
#45023=EDGE_CURVE('',#36101,#36103,#32411,.T.);
#45024=EDGE_CURVE('',#36104,#36105,#3781,.T.);
#45025=EDGE_CURVE('',#36104,#36100,#32412,.T.);
#45026=EDGE_CURVE('',#36105,#36101,#32413,.T.);
#45027=EDGE_CURVE('',#36106,#36107,#3782,.T.);
#45028=EDGE_CURVE('',#36106,#36104,#32414,.T.);
#45029=EDGE_CURVE('',#36107,#36105,#32415,.T.);
#45030=EDGE_CURVE('',#36102,#36106,#32416,.T.);
#45031=EDGE_CURVE('',#36103,#36107,#32417,.T.);
#45032=EDGE_CURVE('',#36108,#36109,#3783,.T.);
#45033=EDGE_CURVE('',#36108,#36110,#32418,.T.);
#45034=EDGE_CURVE('',#36110,#36111,#3784,.T.);
#45035=EDGE_CURVE('',#36109,#36111,#32419,.T.);
#45036=EDGE_CURVE('',#36112,#36113,#3785,.T.);
#45037=EDGE_CURVE('',#36112,#36108,#32420,.T.);
#45038=EDGE_CURVE('',#36113,#36109,#32421,.T.);
#45039=EDGE_CURVE('',#36114,#36115,#3786,.T.);
#45040=EDGE_CURVE('',#36114,#36112,#32422,.T.);
#45041=EDGE_CURVE('',#36115,#36113,#32423,.T.);
#45042=EDGE_CURVE('',#36110,#36114,#32424,.T.);
#45043=EDGE_CURVE('',#36111,#36115,#32425,.T.);
#45044=EDGE_CURVE('',#36116,#36117,#3787,.T.);
#45045=EDGE_CURVE('',#36116,#36118,#32426,.T.);
#45046=EDGE_CURVE('',#36118,#36119,#3788,.T.);
#45047=EDGE_CURVE('',#36117,#36119,#32427,.T.);
#45048=EDGE_CURVE('',#36120,#36121,#3789,.T.);
#45049=EDGE_CURVE('',#36120,#36116,#32428,.T.);
#45050=EDGE_CURVE('',#36121,#36117,#32429,.T.);
#45051=EDGE_CURVE('',#36122,#36123,#3790,.T.);
#45052=EDGE_CURVE('',#36122,#36120,#32430,.T.);
#45053=EDGE_CURVE('',#36123,#36121,#32431,.T.);
#45054=EDGE_CURVE('',#36118,#36122,#32432,.T.);
#45055=EDGE_CURVE('',#36119,#36123,#32433,.T.);
#45056=EDGE_CURVE('',#36124,#36125,#3791,.T.);
#45057=EDGE_CURVE('',#36124,#36126,#32434,.T.);
#45058=EDGE_CURVE('',#36126,#36127,#3792,.T.);
#45059=EDGE_CURVE('',#36125,#36127,#32435,.T.);
#45060=EDGE_CURVE('',#36128,#36129,#3793,.T.);
#45061=EDGE_CURVE('',#36128,#36124,#32436,.T.);
#45062=EDGE_CURVE('',#36129,#36125,#32437,.T.);
#45063=EDGE_CURVE('',#36130,#36131,#3794,.T.);
#45064=EDGE_CURVE('',#36130,#36128,#32438,.T.);
#45065=EDGE_CURVE('',#36131,#36129,#32439,.T.);
#45066=EDGE_CURVE('',#36126,#36130,#32440,.T.);
#45067=EDGE_CURVE('',#36127,#36131,#32441,.T.);
#45068=EDGE_CURVE('',#36132,#36133,#3795,.T.);
#45069=EDGE_CURVE('',#36132,#36134,#32442,.T.);
#45070=EDGE_CURVE('',#36134,#36135,#3796,.T.);
#45071=EDGE_CURVE('',#36133,#36135,#32443,.T.);
#45072=EDGE_CURVE('',#36136,#36137,#3797,.T.);
#45073=EDGE_CURVE('',#36136,#36132,#32444,.T.);
#45074=EDGE_CURVE('',#36137,#36133,#32445,.T.);
#45075=EDGE_CURVE('',#36138,#36139,#3798,.T.);
#45076=EDGE_CURVE('',#36138,#36136,#32446,.T.);
#45077=EDGE_CURVE('',#36139,#36137,#32447,.T.);
#45078=EDGE_CURVE('',#36134,#36138,#32448,.T.);
#45079=EDGE_CURVE('',#36135,#36139,#32449,.T.);
#45080=EDGE_CURVE('',#36140,#36141,#3799,.T.);
#45081=EDGE_CURVE('',#36140,#36142,#32450,.T.);
#45082=EDGE_CURVE('',#36142,#36143,#3800,.T.);
#45083=EDGE_CURVE('',#36141,#36143,#32451,.T.);
#45084=EDGE_CURVE('',#36144,#36145,#3801,.T.);
#45085=EDGE_CURVE('',#36144,#36140,#32452,.T.);
#45086=EDGE_CURVE('',#36145,#36141,#32453,.T.);
#45087=EDGE_CURVE('',#36146,#36147,#3802,.T.);
#45088=EDGE_CURVE('',#36146,#36144,#32454,.T.);
#45089=EDGE_CURVE('',#36147,#36145,#32455,.T.);
#45090=EDGE_CURVE('',#36142,#36146,#32456,.T.);
#45091=EDGE_CURVE('',#36143,#36147,#32457,.T.);
#45092=EDGE_CURVE('',#36148,#36149,#3803,.T.);
#45093=EDGE_CURVE('',#36148,#36150,#32458,.T.);
#45094=EDGE_CURVE('',#36150,#36151,#3804,.T.);
#45095=EDGE_CURVE('',#36149,#36151,#32459,.T.);
#45096=EDGE_CURVE('',#36152,#36153,#3805,.T.);
#45097=EDGE_CURVE('',#36152,#36148,#32460,.T.);
#45098=EDGE_CURVE('',#36153,#36149,#32461,.T.);
#45099=EDGE_CURVE('',#36154,#36155,#3806,.T.);
#45100=EDGE_CURVE('',#36154,#36152,#32462,.T.);
#45101=EDGE_CURVE('',#36155,#36153,#32463,.T.);
#45102=EDGE_CURVE('',#36150,#36154,#32464,.T.);
#45103=EDGE_CURVE('',#36151,#36155,#32465,.T.);
#45104=EDGE_CURVE('',#36156,#36157,#3807,.T.);
#45105=EDGE_CURVE('',#36156,#36158,#32466,.T.);
#45106=EDGE_CURVE('',#36158,#36159,#3808,.T.);
#45107=EDGE_CURVE('',#36157,#36159,#32467,.T.);
#45108=EDGE_CURVE('',#36160,#36161,#3809,.T.);
#45109=EDGE_CURVE('',#36160,#36156,#32468,.T.);
#45110=EDGE_CURVE('',#36161,#36157,#32469,.T.);
#45111=EDGE_CURVE('',#36162,#36163,#3810,.T.);
#45112=EDGE_CURVE('',#36162,#36160,#32470,.T.);
#45113=EDGE_CURVE('',#36163,#36161,#32471,.T.);
#45114=EDGE_CURVE('',#36158,#36162,#32472,.T.);
#45115=EDGE_CURVE('',#36159,#36163,#32473,.T.);
#45116=EDGE_CURVE('',#36164,#36165,#3811,.T.);
#45117=EDGE_CURVE('',#36164,#36166,#32474,.T.);
#45118=EDGE_CURVE('',#36166,#36167,#3812,.T.);
#45119=EDGE_CURVE('',#36165,#36167,#32475,.T.);
#45120=EDGE_CURVE('',#36168,#36169,#3813,.T.);
#45121=EDGE_CURVE('',#36168,#36164,#32476,.T.);
#45122=EDGE_CURVE('',#36169,#36165,#32477,.T.);
#45123=EDGE_CURVE('',#36170,#36171,#3814,.T.);
#45124=EDGE_CURVE('',#36170,#36168,#32478,.T.);
#45125=EDGE_CURVE('',#36171,#36169,#32479,.T.);
#45126=EDGE_CURVE('',#36166,#36170,#32480,.T.);
#45127=EDGE_CURVE('',#36167,#36171,#32481,.T.);
#45128=EDGE_CURVE('',#36172,#36173,#3815,.T.);
#45129=EDGE_CURVE('',#36172,#36174,#32482,.T.);
#45130=EDGE_CURVE('',#36174,#36175,#3816,.T.);
#45131=EDGE_CURVE('',#36173,#36175,#32483,.T.);
#45132=EDGE_CURVE('',#36176,#36177,#3817,.T.);
#45133=EDGE_CURVE('',#36176,#36172,#32484,.T.);
#45134=EDGE_CURVE('',#36177,#36173,#32485,.T.);
#45135=EDGE_CURVE('',#36178,#36179,#3818,.T.);
#45136=EDGE_CURVE('',#36178,#36176,#32486,.T.);
#45137=EDGE_CURVE('',#36179,#36177,#32487,.T.);
#45138=EDGE_CURVE('',#36174,#36178,#32488,.T.);
#45139=EDGE_CURVE('',#36175,#36179,#32489,.T.);
#45140=EDGE_CURVE('',#36180,#36181,#3819,.T.);
#45141=EDGE_CURVE('',#36180,#36182,#32490,.T.);
#45142=EDGE_CURVE('',#36182,#36183,#3820,.T.);
#45143=EDGE_CURVE('',#36181,#36183,#32491,.T.);
#45144=EDGE_CURVE('',#36184,#36185,#3821,.T.);
#45145=EDGE_CURVE('',#36186,#36184,#3822,.T.);
#45146=EDGE_CURVE('',#36186,#36180,#32492,.T.);
#45147=EDGE_CURVE('',#36185,#36181,#32493,.T.);
#45148=EDGE_CURVE('',#36187,#36188,#3823,.T.);
#45149=EDGE_CURVE('',#36184,#36187,#3824,.T.);
#45150=EDGE_CURVE('',#36188,#36185,#32494,.T.);
#45151=EDGE_CURVE('',#36187,#36182,#3825,.T.);
#45152=EDGE_CURVE('',#36183,#36188,#32495,.T.);
#45153=EDGE_CURVE('',#36182,#36186,#32496,.T.);
#45154=EDGE_CURVE('',#36189,#36190,#3826,.T.);
#45155=EDGE_CURVE('',#36189,#36191,#32497,.T.);
#45156=EDGE_CURVE('',#36191,#36192,#3827,.T.);
#45157=EDGE_CURVE('',#36190,#36192,#32498,.T.);
#45158=EDGE_CURVE('',#36193,#36194,#3828,.T.);
#45159=EDGE_CURVE('',#36195,#36193,#3829,.T.);
#45160=EDGE_CURVE('',#36195,#36189,#32499,.T.);
#45161=EDGE_CURVE('',#36194,#36190,#32500,.T.);
#45162=EDGE_CURVE('',#36196,#36197,#3830,.T.);
#45163=EDGE_CURVE('',#36193,#36196,#3831,.T.);
#45164=EDGE_CURVE('',#36197,#36194,#32501,.T.);
#45165=EDGE_CURVE('',#36191,#36198,#32502,.T.);
#45166=EDGE_CURVE('',#36196,#36198,#3832,.T.);
#45167=EDGE_CURVE('',#36192,#36197,#32503,.T.);
#45168=EDGE_CURVE('',#36198,#36195,#32504,.T.);
#45169=EDGE_CURVE('',#36199,#36200,#3833,.T.);
#45170=EDGE_CURVE('',#36199,#36201,#32505,.T.);
#45171=EDGE_CURVE('',#36201,#36202,#3834,.T.);
#45172=EDGE_CURVE('',#36200,#36202,#32506,.T.);
#45173=EDGE_CURVE('',#36203,#36204,#3835,.T.);
#45174=EDGE_CURVE('',#36205,#36203,#3836,.T.);
#45175=EDGE_CURVE('',#36205,#36199,#32507,.T.);
#45176=EDGE_CURVE('',#36204,#36200,#32508,.T.);
#45177=EDGE_CURVE('',#36206,#36207,#3837,.T.);
#45178=EDGE_CURVE('',#36203,#36206,#3838,.T.);
#45179=EDGE_CURVE('',#36207,#36204,#32509,.T.);
#45180=EDGE_CURVE('',#36201,#36208,#32510,.T.);
#45181=EDGE_CURVE('',#36206,#36208,#3839,.T.);
#45182=EDGE_CURVE('',#36202,#36207,#32511,.T.);
#45183=EDGE_CURVE('',#36208,#36205,#32512,.T.);
#45184=EDGE_CURVE('',#36209,#36210,#3840,.T.);
#45185=EDGE_CURVE('',#36209,#36211,#32513,.T.);
#45186=EDGE_CURVE('',#36211,#36212,#3841,.T.);
#45187=EDGE_CURVE('',#36210,#36212,#32514,.T.);
#45188=EDGE_CURVE('',#36213,#36214,#3842,.T.);
#45189=EDGE_CURVE('',#36215,#36213,#3843,.T.);
#45190=EDGE_CURVE('',#36215,#36209,#32515,.T.);
#45191=EDGE_CURVE('',#36214,#36210,#32516,.T.);
#45192=EDGE_CURVE('',#36216,#36217,#3844,.T.);
#45193=EDGE_CURVE('',#36213,#36216,#3845,.T.);
#45194=EDGE_CURVE('',#36217,#36214,#32517,.T.);
#45195=EDGE_CURVE('',#36211,#36218,#32518,.T.);
#45196=EDGE_CURVE('',#36216,#36218,#3846,.T.);
#45197=EDGE_CURVE('',#36212,#36217,#32519,.T.);
#45198=EDGE_CURVE('',#36218,#36215,#32520,.T.);
#45199=EDGE_CURVE('',#36219,#36220,#3847,.T.);
#45200=EDGE_CURVE('',#36219,#36221,#32521,.T.);
#45201=EDGE_CURVE('',#36221,#36222,#3848,.T.);
#45202=EDGE_CURVE('',#36220,#36222,#32522,.T.);
#45203=EDGE_CURVE('',#36223,#36224,#3849,.T.);
#45204=EDGE_CURVE('',#36225,#36223,#3850,.T.);
#45205=EDGE_CURVE('',#36225,#36219,#32523,.T.);
#45206=EDGE_CURVE('',#36224,#36220,#32524,.T.);
#45207=EDGE_CURVE('',#36226,#36227,#3851,.T.);
#45208=EDGE_CURVE('',#36223,#36226,#3852,.T.);
#45209=EDGE_CURVE('',#36227,#36224,#32525,.T.);
#45210=EDGE_CURVE('',#36221,#36228,#32526,.T.);
#45211=EDGE_CURVE('',#36226,#36228,#3853,.T.);
#45212=EDGE_CURVE('',#36222,#36227,#32527,.T.);
#45213=EDGE_CURVE('',#36228,#36225,#32528,.T.);
#45214=EDGE_CURVE('',#36229,#36230,#3854,.T.);
#45215=EDGE_CURVE('',#36231,#36229,#3855,.T.);
#45216=EDGE_CURVE('',#36231,#36232,#32529,.T.);
#45217=EDGE_CURVE('',#36232,#36233,#3856,.T.);
#45218=EDGE_CURVE('',#36230,#36233,#32530,.T.);
#45219=EDGE_CURVE('',#36234,#36235,#3857,.T.);
#45220=EDGE_CURVE('',#36229,#36234,#3858,.T.);
#45221=EDGE_CURVE('',#36235,#36230,#32531,.T.);
#45222=EDGE_CURVE('',#36236,#36237,#3859,.T.);
#45223=EDGE_CURVE('',#36234,#36236,#3860,.T.);
#45224=EDGE_CURVE('',#36237,#36235,#32532,.T.);
#45225=EDGE_CURVE('',#36232,#36238,#32533,.T.);
#45226=EDGE_CURVE('',#36236,#36238,#3861,.T.);
#45227=EDGE_CURVE('',#36233,#36237,#32534,.T.);
#45228=EDGE_CURVE('',#36238,#36231,#32535,.T.);
#45229=EDGE_CURVE('',#36239,#36240,#3862,.T.);
#45230=EDGE_CURVE('',#36241,#36239,#3863,.T.);
#45231=EDGE_CURVE('',#36241,#36242,#32536,.T.);
#45232=EDGE_CURVE('',#36242,#36243,#3864,.T.);
#45233=EDGE_CURVE('',#36240,#36243,#32537,.T.);
#45234=EDGE_CURVE('',#36244,#36245,#3865,.T.);
#45235=EDGE_CURVE('',#36239,#36244,#3866,.T.);
#45236=EDGE_CURVE('',#36245,#36240,#32538,.T.);
#45237=EDGE_CURVE('',#36246,#36247,#3867,.T.);
#45238=EDGE_CURVE('',#36244,#36246,#3868,.T.);
#45239=EDGE_CURVE('',#36247,#36245,#32539,.T.);
#45240=EDGE_CURVE('',#36242,#36248,#32540,.T.);
#45241=EDGE_CURVE('',#36246,#36248,#3869,.T.);
#45242=EDGE_CURVE('',#36243,#36247,#32541,.T.);
#45243=EDGE_CURVE('',#36248,#36241,#32542,.T.);
#45244=EDGE_CURVE('',#36249,#36250,#3870,.T.);
#45245=EDGE_CURVE('',#36249,#36251,#32543,.T.);
#45246=EDGE_CURVE('',#36251,#36252,#3871,.T.);
#45247=EDGE_CURVE('',#36250,#36252,#32544,.T.);
#45248=EDGE_CURVE('',#36253,#36254,#3872,.T.);
#45249=EDGE_CURVE('',#36255,#36253,#3873,.T.);
#45250=EDGE_CURVE('',#36255,#36249,#32545,.T.);
#45251=EDGE_CURVE('',#36254,#36250,#32546,.T.);
#45252=EDGE_CURVE('',#36256,#36257,#3874,.T.);
#45253=EDGE_CURVE('',#36253,#36256,#3875,.T.);
#45254=EDGE_CURVE('',#36257,#36254,#32547,.T.);
#45255=EDGE_CURVE('',#36251,#36258,#32548,.T.);
#45256=EDGE_CURVE('',#36256,#36258,#3876,.T.);
#45257=EDGE_CURVE('',#36252,#36257,#32549,.T.);
#45258=EDGE_CURVE('',#36258,#36255,#32550,.T.);
#45259=EDGE_CURVE('',#36259,#36260,#3877,.T.);
#45260=EDGE_CURVE('',#36259,#36261,#32551,.T.);
#45261=EDGE_CURVE('',#36261,#36262,#3878,.T.);
#45262=EDGE_CURVE('',#36260,#36262,#32552,.T.);
#45263=EDGE_CURVE('',#36263,#36264,#3879,.T.);
#45264=EDGE_CURVE('',#36265,#36263,#3880,.T.);
#45265=EDGE_CURVE('',#36265,#36259,#32553,.T.);
#45266=EDGE_CURVE('',#36264,#36260,#32554,.T.);
#45267=EDGE_CURVE('',#36266,#36267,#3881,.T.);
#45268=EDGE_CURVE('',#36263,#36266,#3882,.T.);
#45269=EDGE_CURVE('',#36267,#36264,#32555,.T.);
#45270=EDGE_CURVE('',#36261,#36268,#32556,.T.);
#45271=EDGE_CURVE('',#36266,#36268,#3883,.T.);
#45272=EDGE_CURVE('',#36262,#36267,#32557,.T.);
#45273=EDGE_CURVE('',#36268,#36265,#32558,.T.);
#45274=EDGE_CURVE('',#36269,#36270,#3884,.T.);
#45275=EDGE_CURVE('',#36269,#36271,#32559,.T.);
#45276=EDGE_CURVE('',#36271,#36272,#3885,.T.);
#45277=EDGE_CURVE('',#36270,#36272,#32560,.T.);
#45278=EDGE_CURVE('',#36273,#36274,#3886,.T.);
#45279=EDGE_CURVE('',#36275,#36273,#3887,.T.);
#45280=EDGE_CURVE('',#36275,#36269,#32561,.T.);
#45281=EDGE_CURVE('',#36274,#36270,#32562,.T.);
#45282=EDGE_CURVE('',#36276,#36277,#3888,.T.);
#45283=EDGE_CURVE('',#36273,#36276,#3889,.T.);
#45284=EDGE_CURVE('',#36277,#36274,#32563,.T.);
#45285=EDGE_CURVE('',#36271,#36278,#32564,.T.);
#45286=EDGE_CURVE('',#36276,#36278,#3890,.T.);
#45287=EDGE_CURVE('',#36272,#36277,#32565,.T.);
#45288=EDGE_CURVE('',#36278,#36275,#32566,.T.);
#45289=EDGE_CURVE('',#36279,#36280,#3891,.T.);
#45290=EDGE_CURVE('',#36279,#36281,#32567,.T.);
#45291=EDGE_CURVE('',#36281,#36282,#3892,.T.);
#45292=EDGE_CURVE('',#36280,#36282,#32568,.T.);
#45293=EDGE_CURVE('',#36283,#36284,#3893,.T.);
#45294=EDGE_CURVE('',#36283,#36279,#32569,.T.);
#45295=EDGE_CURVE('',#36284,#36280,#32570,.T.);
#45296=EDGE_CURVE('',#36285,#36286,#3894,.T.);
#45297=EDGE_CURVE('',#36285,#36283,#32571,.T.);
#45298=EDGE_CURVE('',#36286,#36284,#32572,.T.);
#45299=EDGE_CURVE('',#36281,#36285,#32573,.T.);
#45300=EDGE_CURVE('',#36282,#36286,#32574,.T.);
#45301=EDGE_CURVE('',#36287,#36288,#3895,.T.);
#45302=EDGE_CURVE('',#36287,#36289,#32575,.T.);
#45303=EDGE_CURVE('',#36289,#36290,#3896,.T.);
#45304=EDGE_CURVE('',#36288,#36290,#32576,.T.);
#45305=EDGE_CURVE('',#36291,#36292,#3897,.T.);
#45306=EDGE_CURVE('',#36291,#36287,#32577,.T.);
#45307=EDGE_CURVE('',#36292,#36288,#32578,.T.);
#45308=EDGE_CURVE('',#36293,#36294,#3898,.T.);
#45309=EDGE_CURVE('',#36293,#36291,#32579,.T.);
#45310=EDGE_CURVE('',#36294,#36292,#32580,.T.);
#45311=EDGE_CURVE('',#36289,#36293,#32581,.T.);
#45312=EDGE_CURVE('',#36290,#36294,#32582,.T.);
#45313=EDGE_CURVE('',#36295,#36296,#3899,.T.);
#45314=EDGE_CURVE('',#36295,#36297,#32583,.T.);
#45315=EDGE_CURVE('',#36297,#36298,#3900,.T.);
#45316=EDGE_CURVE('',#36296,#36298,#32584,.T.);
#45317=EDGE_CURVE('',#36299,#36300,#3901,.T.);
#45318=EDGE_CURVE('',#36299,#36295,#32585,.T.);
#45319=EDGE_CURVE('',#36300,#36296,#32586,.T.);
#45320=EDGE_CURVE('',#36301,#36302,#3902,.T.);
#45321=EDGE_CURVE('',#36301,#36299,#32587,.T.);
#45322=EDGE_CURVE('',#36302,#36300,#32588,.T.);
#45323=EDGE_CURVE('',#36297,#36301,#32589,.T.);
#45324=EDGE_CURVE('',#36298,#36302,#32590,.T.);
#45325=EDGE_CURVE('',#36303,#36304,#3903,.T.);
#45326=EDGE_CURVE('',#36303,#36305,#32591,.T.);
#45327=EDGE_CURVE('',#36305,#36306,#3904,.T.);
#45328=EDGE_CURVE('',#36304,#36306,#32592,.T.);
#45329=EDGE_CURVE('',#36307,#36308,#3905,.T.);
#45330=EDGE_CURVE('',#36307,#36303,#32593,.T.);
#45331=EDGE_CURVE('',#36308,#36304,#32594,.T.);
#45332=EDGE_CURVE('',#36309,#36310,#3906,.T.);
#45333=EDGE_CURVE('',#36309,#36307,#32595,.T.);
#45334=EDGE_CURVE('',#36310,#36308,#32596,.T.);
#45335=EDGE_CURVE('',#36305,#36309,#32597,.T.);
#45336=EDGE_CURVE('',#36306,#36310,#32598,.T.);
#45337=EDGE_CURVE('',#36311,#36312,#3907,.T.);
#45338=EDGE_CURVE('',#36311,#36313,#32599,.T.);
#45339=EDGE_CURVE('',#36313,#36314,#3908,.T.);
#45340=EDGE_CURVE('',#36312,#36314,#32600,.T.);
#45341=EDGE_CURVE('',#36315,#36316,#3909,.T.);
#45342=EDGE_CURVE('',#36315,#36311,#32601,.T.);
#45343=EDGE_CURVE('',#36316,#36312,#32602,.T.);
#45344=EDGE_CURVE('',#36317,#36318,#3910,.T.);
#45345=EDGE_CURVE('',#36317,#36315,#32603,.T.);
#45346=EDGE_CURVE('',#36318,#36316,#32604,.T.);
#45347=EDGE_CURVE('',#36313,#36317,#32605,.T.);
#45348=EDGE_CURVE('',#36314,#36318,#32606,.T.);
#45349=EDGE_CURVE('',#36319,#36320,#3911,.T.);
#45350=EDGE_CURVE('',#36319,#36321,#32607,.T.);
#45351=EDGE_CURVE('',#36321,#36322,#3912,.T.);
#45352=EDGE_CURVE('',#36320,#36322,#32608,.T.);
#45353=EDGE_CURVE('',#36323,#36324,#3913,.T.);
#45354=EDGE_CURVE('',#36323,#36319,#32609,.T.);
#45355=EDGE_CURVE('',#36324,#36320,#32610,.T.);
#45356=EDGE_CURVE('',#36325,#36326,#3914,.T.);
#45357=EDGE_CURVE('',#36325,#36323,#32611,.T.);
#45358=EDGE_CURVE('',#36326,#36324,#32612,.T.);
#45359=EDGE_CURVE('',#36321,#36325,#32613,.T.);
#45360=EDGE_CURVE('',#36322,#36326,#32614,.T.);
#45361=EDGE_CURVE('',#36327,#36328,#3915,.T.);
#45362=EDGE_CURVE('',#36327,#36329,#32615,.T.);
#45363=EDGE_CURVE('',#36329,#36330,#3916,.T.);
#45364=EDGE_CURVE('',#36328,#36330,#32616,.T.);
#45365=EDGE_CURVE('',#36331,#36332,#3917,.T.);
#45366=EDGE_CURVE('',#36331,#36327,#32617,.T.);
#45367=EDGE_CURVE('',#36332,#36328,#32618,.T.);
#45368=EDGE_CURVE('',#36333,#36334,#3918,.T.);
#45369=EDGE_CURVE('',#36333,#36331,#32619,.T.);
#45370=EDGE_CURVE('',#36334,#36332,#32620,.T.);
#45371=EDGE_CURVE('',#36329,#36333,#32621,.T.);
#45372=EDGE_CURVE('',#36330,#36334,#32622,.T.);
#45373=EDGE_CURVE('',#36335,#36336,#3919,.T.);
#45374=EDGE_CURVE('',#36335,#36337,#32623,.T.);
#45375=EDGE_CURVE('',#36337,#36338,#3920,.T.);
#45376=EDGE_CURVE('',#36336,#36338,#32624,.T.);
#45377=EDGE_CURVE('',#36339,#36340,#3921,.T.);
#45378=EDGE_CURVE('',#36339,#36335,#32625,.T.);
#45379=EDGE_CURVE('',#36340,#36336,#32626,.T.);
#45380=EDGE_CURVE('',#36341,#36342,#3922,.T.);
#45381=EDGE_CURVE('',#36341,#36339,#32627,.T.);
#45382=EDGE_CURVE('',#36342,#36340,#32628,.T.);
#45383=EDGE_CURVE('',#36337,#36341,#32629,.T.);
#45384=EDGE_CURVE('',#36338,#36342,#32630,.T.);
#45385=EDGE_CURVE('',#36343,#36344,#3923,.T.);
#45386=EDGE_CURVE('',#36345,#36343,#3924,.T.);
#45387=EDGE_CURVE('',#36345,#36346,#32631,.T.);
#45388=EDGE_CURVE('',#36346,#36347,#3925,.T.);
#45389=EDGE_CURVE('',#36344,#36347,#32632,.T.);
#45390=EDGE_CURVE('',#36348,#36349,#3926,.T.);
#45391=EDGE_CURVE('',#36343,#36348,#3927,.T.);
#45392=EDGE_CURVE('',#36349,#36344,#32633,.T.);
#45393=EDGE_CURVE('',#36350,#36351,#3928,.T.);
#45394=EDGE_CURVE('',#36348,#36350,#3929,.T.);
#45395=EDGE_CURVE('',#36351,#36349,#32634,.T.);
#45396=EDGE_CURVE('',#36346,#36352,#32635,.T.);
#45397=EDGE_CURVE('',#36350,#36352,#3930,.T.);
#45398=EDGE_CURVE('',#36347,#36351,#32636,.T.);
#45399=EDGE_CURVE('',#36352,#36345,#32637,.T.);
#45400=EDGE_CURVE('',#36353,#36354,#3931,.T.);
#45401=EDGE_CURVE('',#36355,#36353,#3932,.T.);
#45402=EDGE_CURVE('',#36355,#36356,#32638,.T.);
#45403=EDGE_CURVE('',#36356,#36357,#3933,.T.);
#45404=EDGE_CURVE('',#36354,#36357,#32639,.T.);
#45405=EDGE_CURVE('',#36358,#36359,#3934,.T.);
#45406=EDGE_CURVE('',#36353,#36358,#3935,.T.);
#45407=EDGE_CURVE('',#36359,#36354,#32640,.T.);
#45408=EDGE_CURVE('',#36360,#36361,#3936,.T.);
#45409=EDGE_CURVE('',#36358,#36360,#3937,.T.);
#45410=EDGE_CURVE('',#36361,#36359,#32641,.T.);
#45411=EDGE_CURVE('',#36356,#36362,#32642,.T.);
#45412=EDGE_CURVE('',#36360,#36362,#3938,.T.);
#45413=EDGE_CURVE('',#36357,#36361,#32643,.T.);
#45414=EDGE_CURVE('',#36362,#36355,#32644,.T.);
#45415=EDGE_CURVE('',#36363,#36364,#3939,.T.);
#45416=EDGE_CURVE('',#36363,#36365,#32645,.T.);
#45417=EDGE_CURVE('',#36365,#36366,#3940,.T.);
#45418=EDGE_CURVE('',#36364,#36366,#32646,.T.);
#45419=EDGE_CURVE('',#36367,#36368,#3941,.T.);
#45420=EDGE_CURVE('',#36367,#36363,#32647,.T.);
#45421=EDGE_CURVE('',#36368,#36364,#32648,.T.);
#45422=EDGE_CURVE('',#36369,#36370,#3942,.T.);
#45423=EDGE_CURVE('',#36369,#36367,#32649,.T.);
#45424=EDGE_CURVE('',#36370,#36368,#32650,.T.);
#45425=EDGE_CURVE('',#36365,#36369,#32651,.T.);
#45426=EDGE_CURVE('',#36366,#36370,#32652,.T.);
#45427=EDGE_CURVE('',#36371,#36372,#3943,.T.);
#45428=EDGE_CURVE('',#36371,#36373,#32653,.T.);
#45429=EDGE_CURVE('',#36373,#36374,#3944,.T.);
#45430=EDGE_CURVE('',#36372,#36374,#32654,.T.);
#45431=EDGE_CURVE('',#36375,#36376,#3945,.T.);
#45432=EDGE_CURVE('',#36375,#36371,#32655,.T.);
#45433=EDGE_CURVE('',#36376,#36372,#32656,.T.);
#45434=EDGE_CURVE('',#36377,#36378,#3946,.T.);
#45435=EDGE_CURVE('',#36377,#36375,#32657,.T.);
#45436=EDGE_CURVE('',#36378,#36376,#32658,.T.);
#45437=EDGE_CURVE('',#36373,#36377,#32659,.T.);
#45438=EDGE_CURVE('',#36374,#36378,#32660,.T.);
#45439=EDGE_CURVE('',#36379,#36380,#3947,.T.);
#45440=EDGE_CURVE('',#36379,#36381,#32661,.T.);
#45441=EDGE_CURVE('',#36381,#36382,#3948,.T.);
#45442=EDGE_CURVE('',#36380,#36382,#32662,.T.);
#45443=EDGE_CURVE('',#36383,#36384,#3949,.T.);
#45444=EDGE_CURVE('',#36383,#36379,#32663,.T.);
#45445=EDGE_CURVE('',#36384,#36380,#32664,.T.);
#45446=EDGE_CURVE('',#36385,#36386,#3950,.T.);
#45447=EDGE_CURVE('',#36385,#36383,#32665,.T.);
#45448=EDGE_CURVE('',#36386,#36384,#32666,.T.);
#45449=EDGE_CURVE('',#36381,#36385,#32667,.T.);
#45450=EDGE_CURVE('',#36382,#36386,#32668,.T.);
#45451=EDGE_CURVE('',#36387,#36388,#3951,.T.);
#45452=EDGE_CURVE('',#36387,#36389,#32669,.T.);
#45453=EDGE_CURVE('',#36389,#36390,#3952,.T.);
#45454=EDGE_CURVE('',#36388,#36390,#32670,.T.);
#45455=EDGE_CURVE('',#36391,#36392,#3953,.T.);
#45456=EDGE_CURVE('',#36391,#36387,#32671,.T.);
#45457=EDGE_CURVE('',#36392,#36388,#32672,.T.);
#45458=EDGE_CURVE('',#36393,#36394,#3954,.T.);
#45459=EDGE_CURVE('',#36393,#36391,#32673,.T.);
#45460=EDGE_CURVE('',#36394,#36392,#32674,.T.);
#45461=EDGE_CURVE('',#36389,#36393,#32675,.T.);
#45462=EDGE_CURVE('',#36390,#36394,#32676,.T.);
#45463=EDGE_CURVE('',#36395,#36396,#3955,.T.);
#45464=EDGE_CURVE('',#36395,#36397,#32677,.T.);
#45465=EDGE_CURVE('',#36397,#36398,#3956,.T.);
#45466=EDGE_CURVE('',#36396,#36398,#32678,.T.);
#45467=EDGE_CURVE('',#36399,#36400,#3957,.T.);
#45468=EDGE_CURVE('',#36399,#36395,#32679,.T.);
#45469=EDGE_CURVE('',#36400,#36396,#32680,.T.);
#45470=EDGE_CURVE('',#36401,#36402,#3958,.T.);
#45471=EDGE_CURVE('',#36403,#36401,#3959,.T.);
#45472=EDGE_CURVE('',#36403,#36399,#32681,.T.);
#45473=EDGE_CURVE('',#36402,#36400,#32682,.T.);
#45474=EDGE_CURVE('',#36397,#36404,#32683,.T.);
#45475=EDGE_CURVE('',#36401,#36404,#3960,.T.);
#45476=EDGE_CURVE('',#36398,#36402,#32684,.T.);
#45477=EDGE_CURVE('',#36404,#36403,#32685,.T.);
#45478=EDGE_CURVE('',#36405,#36406,#3961,.T.);
#45479=EDGE_CURVE('',#36405,#36407,#32686,.T.);
#45480=EDGE_CURVE('',#36407,#36408,#3962,.T.);
#45481=EDGE_CURVE('',#36406,#36408,#32687,.T.);
#45482=EDGE_CURVE('',#36409,#36410,#3963,.T.);
#45483=EDGE_CURVE('',#36411,#36409,#3964,.T.);
#45484=EDGE_CURVE('',#36411,#36405,#32688,.T.);
#45485=EDGE_CURVE('',#36410,#36406,#32689,.T.);
#45486=EDGE_CURVE('',#36412,#36413,#3965,.T.);
#45487=EDGE_CURVE('',#36409,#36412,#3966,.T.);
#45488=EDGE_CURVE('',#36413,#36410,#32690,.T.);
#45489=EDGE_CURVE('',#36407,#36414,#32691,.T.);
#45490=EDGE_CURVE('',#36412,#36414,#3967,.T.);
#45491=EDGE_CURVE('',#36408,#36413,#32692,.T.);
#45492=EDGE_CURVE('',#36414,#36411,#32693,.T.);
#45493=EDGE_CURVE('',#36415,#36416,#3968,.T.);
#45494=EDGE_CURVE('',#36415,#36417,#32694,.T.);
#45495=EDGE_CURVE('',#36417,#36418,#3969,.T.);
#45496=EDGE_CURVE('',#36416,#36418,#32695,.T.);
#45497=EDGE_CURVE('',#36419,#36420,#3970,.T.);
#45498=EDGE_CURVE('',#36421,#36419,#3971,.T.);
#45499=EDGE_CURVE('',#36421,#36415,#32696,.T.);
#45500=EDGE_CURVE('',#36420,#36416,#32697,.T.);
#45501=EDGE_CURVE('',#36422,#36423,#3972,.T.);
#45502=EDGE_CURVE('',#36419,#36422,#3973,.T.);
#45503=EDGE_CURVE('',#36423,#36420,#32698,.T.);
#45504=EDGE_CURVE('',#36417,#36424,#32699,.T.);
#45505=EDGE_CURVE('',#36422,#36424,#3974,.T.);
#45506=EDGE_CURVE('',#36418,#36423,#32700,.T.);
#45507=EDGE_CURVE('',#36424,#36421,#32701,.T.);
#45508=EDGE_CURVE('',#36425,#36426,#3975,.T.);
#45509=EDGE_CURVE('',#36425,#36427,#32702,.T.);
#45510=EDGE_CURVE('',#36427,#36428,#3976,.T.);
#45511=EDGE_CURVE('',#36426,#36428,#32703,.T.);
#45512=EDGE_CURVE('',#36429,#36430,#3977,.T.);
#45513=EDGE_CURVE('',#36429,#36425,#32704,.T.);
#45514=EDGE_CURVE('',#36430,#36426,#32705,.T.);
#45515=EDGE_CURVE('',#36431,#36432,#3978,.T.);
#45516=EDGE_CURVE('',#36433,#36431,#3979,.T.);
#45517=EDGE_CURVE('',#36433,#36429,#32706,.T.);
#45518=EDGE_CURVE('',#36432,#36430,#32707,.T.);
#45519=EDGE_CURVE('',#36427,#36434,#32708,.T.);
#45520=EDGE_CURVE('',#36431,#36434,#3980,.T.);
#45521=EDGE_CURVE('',#36428,#36432,#32709,.T.);
#45522=EDGE_CURVE('',#36434,#36433,#32710,.T.);
#45523=EDGE_CURVE('',#36435,#36436,#3981,.T.);
#45524=EDGE_CURVE('',#36435,#36437,#32711,.T.);
#45525=EDGE_CURVE('',#36437,#36438,#3982,.T.);
#45526=EDGE_CURVE('',#36436,#36438,#32712,.T.);
#45527=EDGE_CURVE('',#36439,#36440,#3983,.T.);
#45528=EDGE_CURVE('',#36439,#36435,#32713,.T.);
#45529=EDGE_CURVE('',#36440,#36436,#32714,.T.);
#45530=EDGE_CURVE('',#36441,#36442,#3984,.T.);
#45531=EDGE_CURVE('',#36441,#36439,#32715,.T.);
#45532=EDGE_CURVE('',#36442,#36440,#32716,.T.);
#45533=EDGE_CURVE('',#36437,#36441,#32717,.T.);
#45534=EDGE_CURVE('',#36438,#36442,#32718,.T.);
#45535=EDGE_CURVE('',#36443,#36444,#3985,.T.);
#45536=EDGE_CURVE('',#36443,#36445,#32719,.T.);
#45537=EDGE_CURVE('',#36445,#36446,#3986,.T.);
#45538=EDGE_CURVE('',#36444,#36446,#32720,.T.);
#45539=EDGE_CURVE('',#36447,#36448,#3987,.T.);
#45540=EDGE_CURVE('',#36447,#36443,#32721,.T.);
#45541=EDGE_CURVE('',#36448,#36444,#32722,.T.);
#45542=EDGE_CURVE('',#36449,#36450,#3988,.T.);
#45543=EDGE_CURVE('',#36449,#36447,#32723,.T.);
#45544=EDGE_CURVE('',#36450,#36448,#32724,.T.);
#45545=EDGE_CURVE('',#36445,#36449,#32725,.T.);
#45546=EDGE_CURVE('',#36446,#36450,#32726,.T.);
#45547=EDGE_CURVE('',#36451,#36452,#3989,.T.);
#45548=EDGE_CURVE('',#36451,#36453,#32727,.T.);
#45549=EDGE_CURVE('',#36453,#36454,#3990,.T.);
#45550=EDGE_CURVE('',#36452,#36454,#32728,.T.);
#45551=EDGE_CURVE('',#36455,#36456,#3991,.T.);
#45552=EDGE_CURVE('',#36455,#36451,#32729,.T.);
#45553=EDGE_CURVE('',#36456,#36452,#32730,.T.);
#45554=EDGE_CURVE('',#36457,#36458,#3992,.T.);
#45555=EDGE_CURVE('',#36457,#36455,#32731,.T.);
#45556=EDGE_CURVE('',#36458,#36456,#32732,.T.);
#45557=EDGE_CURVE('',#36453,#36457,#32733,.T.);
#45558=EDGE_CURVE('',#36454,#36458,#32734,.T.);
#45559=EDGE_CURVE('',#36459,#36460,#3993,.T.);
#45560=EDGE_CURVE('',#36459,#36461,#32735,.T.);
#45561=EDGE_CURVE('',#36461,#36462,#3994,.T.);
#45562=EDGE_CURVE('',#36460,#36462,#32736,.T.);
#45563=EDGE_CURVE('',#36463,#36464,#3995,.T.);
#45564=EDGE_CURVE('',#36463,#36459,#32737,.T.);
#45565=EDGE_CURVE('',#36464,#36460,#32738,.T.);
#45566=EDGE_CURVE('',#36465,#36466,#3996,.T.);
#45567=EDGE_CURVE('',#36465,#36463,#32739,.T.);
#45568=EDGE_CURVE('',#36466,#36464,#32740,.T.);
#45569=EDGE_CURVE('',#36461,#36465,#32741,.T.);
#45570=EDGE_CURVE('',#36462,#36466,#32742,.T.);
#45571=EDGE_CURVE('',#36467,#36468,#3997,.T.);
#45572=EDGE_CURVE('',#36467,#36469,#32743,.T.);
#45573=EDGE_CURVE('',#36469,#36470,#3998,.T.);
#45574=EDGE_CURVE('',#36468,#36470,#32744,.T.);
#45575=EDGE_CURVE('',#36471,#36472,#3999,.T.);
#45576=EDGE_CURVE('',#36471,#36467,#32745,.T.);
#45577=EDGE_CURVE('',#36472,#36468,#32746,.T.);
#45578=EDGE_CURVE('',#36473,#36474,#4000,.T.);
#45579=EDGE_CURVE('',#36473,#36471,#32747,.T.);
#45580=EDGE_CURVE('',#36474,#36472,#32748,.T.);
#45581=EDGE_CURVE('',#36469,#36473,#32749,.T.);
#45582=EDGE_CURVE('',#36470,#36474,#32750,.T.);
#45583=EDGE_CURVE('',#36475,#36476,#4001,.T.);
#45584=EDGE_CURVE('',#36475,#36477,#32751,.T.);
#45585=EDGE_CURVE('',#36477,#36478,#4002,.T.);
#45586=EDGE_CURVE('',#36476,#36478,#32752,.T.);
#45587=EDGE_CURVE('',#36479,#36480,#4003,.T.);
#45588=EDGE_CURVE('',#36479,#36475,#32753,.T.);
#45589=EDGE_CURVE('',#36480,#36476,#32754,.T.);
#45590=EDGE_CURVE('',#36481,#36482,#4004,.T.);
#45591=EDGE_CURVE('',#36481,#36479,#32755,.T.);
#45592=EDGE_CURVE('',#36482,#36480,#32756,.T.);
#45593=EDGE_CURVE('',#36477,#36481,#32757,.T.);
#45594=EDGE_CURVE('',#36478,#36482,#32758,.T.);
#45595=EDGE_CURVE('',#36483,#36484,#4005,.T.);
#45596=EDGE_CURVE('',#36483,#36485,#32759,.T.);
#45597=EDGE_CURVE('',#36485,#36486,#4006,.T.);
#45598=EDGE_CURVE('',#36484,#36486,#32760,.T.);
#45599=EDGE_CURVE('',#36487,#36488,#4007,.T.);
#45600=EDGE_CURVE('',#36487,#36483,#32761,.T.);
#45601=EDGE_CURVE('',#36488,#36484,#32762,.T.);
#45602=EDGE_CURVE('',#36489,#36490,#4008,.T.);
#45603=EDGE_CURVE('',#36489,#36487,#32763,.T.);
#45604=EDGE_CURVE('',#36490,#36488,#32764,.T.);
#45605=EDGE_CURVE('',#36485,#36489,#32765,.T.);
#45606=EDGE_CURVE('',#36486,#36490,#32766,.T.);
#45607=EDGE_CURVE('',#36491,#36492,#4009,.T.);
#45608=EDGE_CURVE('',#36491,#36493,#32767,.T.);
#45609=EDGE_CURVE('',#36493,#36494,#4010,.T.);
#45610=EDGE_CURVE('',#36492,#36494,#32768,.T.);
#45611=EDGE_CURVE('',#36495,#36496,#4011,.T.);
#45612=EDGE_CURVE('',#36495,#36491,#32769,.T.);
#45613=EDGE_CURVE('',#36496,#36492,#32770,.T.);
#45614=EDGE_CURVE('',#36497,#36498,#4012,.T.);
#45615=EDGE_CURVE('',#36497,#36495,#32771,.T.);
#45616=EDGE_CURVE('',#36498,#36496,#32772,.T.);
#45617=EDGE_CURVE('',#36493,#36497,#32773,.T.);
#45618=EDGE_CURVE('',#36494,#36498,#32774,.T.);
#45619=EDGE_CURVE('',#36499,#36500,#4013,.T.);
#45620=EDGE_CURVE('',#36499,#36501,#32775,.T.);
#45621=EDGE_CURVE('',#36501,#36502,#4014,.T.);
#45622=EDGE_CURVE('',#36500,#36502,#32776,.T.);
#45623=EDGE_CURVE('',#36503,#36504,#4015,.T.);
#45624=EDGE_CURVE('',#36503,#36499,#32777,.T.);
#45625=EDGE_CURVE('',#36504,#36500,#32778,.T.);
#45626=EDGE_CURVE('',#36505,#36506,#4016,.T.);
#45627=EDGE_CURVE('',#36505,#36503,#32779,.T.);
#45628=EDGE_CURVE('',#36506,#36504,#32780,.T.);
#45629=EDGE_CURVE('',#36501,#36505,#32781,.T.);
#45630=EDGE_CURVE('',#36502,#36506,#32782,.T.);
#45631=EDGE_CURVE('',#36507,#36508,#4017,.T.);
#45632=EDGE_CURVE('',#36507,#36509,#32783,.T.);
#45633=EDGE_CURVE('',#36509,#36510,#4018,.T.);
#45634=EDGE_CURVE('',#36508,#36510,#32784,.T.);
#45635=EDGE_CURVE('',#36511,#36512,#4019,.T.);
#45636=EDGE_CURVE('',#36511,#36507,#32785,.T.);
#45637=EDGE_CURVE('',#36512,#36508,#32786,.T.);
#45638=EDGE_CURVE('',#36513,#36514,#4020,.T.);
#45639=EDGE_CURVE('',#36513,#36511,#32787,.T.);
#45640=EDGE_CURVE('',#36514,#36512,#32788,.T.);
#45641=EDGE_CURVE('',#36509,#36513,#32789,.T.);
#45642=EDGE_CURVE('',#36510,#36514,#32790,.T.);
#45643=EDGE_CURVE('',#36515,#36516,#4021,.T.);
#45644=EDGE_CURVE('',#36515,#36517,#32791,.T.);
#45645=EDGE_CURVE('',#36517,#36518,#4022,.T.);
#45646=EDGE_CURVE('',#36516,#36518,#32792,.T.);
#45647=EDGE_CURVE('',#36519,#36520,#4023,.T.);
#45648=EDGE_CURVE('',#36519,#36515,#32793,.T.);
#45649=EDGE_CURVE('',#36520,#36516,#32794,.T.);
#45650=EDGE_CURVE('',#36521,#36522,#4024,.T.);
#45651=EDGE_CURVE('',#36523,#36521,#4025,.T.);
#45652=EDGE_CURVE('',#36523,#36519,#32795,.T.);
#45653=EDGE_CURVE('',#36522,#36520,#32796,.T.);
#45654=EDGE_CURVE('',#36517,#36524,#32797,.T.);
#45655=EDGE_CURVE('',#36521,#36524,#4026,.T.);
#45656=EDGE_CURVE('',#36518,#36522,#32798,.T.);
#45657=EDGE_CURVE('',#36524,#36523,#32799,.T.);
#45658=EDGE_CURVE('',#36525,#36526,#4027,.T.);
#45659=EDGE_CURVE('',#36525,#36527,#32800,.T.);
#45660=EDGE_CURVE('',#36527,#36528,#4028,.T.);
#45661=EDGE_CURVE('',#36526,#36528,#32801,.T.);
#45662=EDGE_CURVE('',#36529,#36530,#4029,.T.);
#45663=EDGE_CURVE('',#36529,#36525,#32802,.T.);
#45664=EDGE_CURVE('',#36530,#36526,#32803,.T.);
#45665=EDGE_CURVE('',#36531,#36532,#4030,.T.);
#45666=EDGE_CURVE('',#36533,#36531,#4031,.T.);
#45667=EDGE_CURVE('',#36533,#36529,#32804,.T.);
#45668=EDGE_CURVE('',#36532,#36530,#32805,.T.);
#45669=EDGE_CURVE('',#36527,#36534,#32806,.T.);
#45670=EDGE_CURVE('',#36531,#36534,#4032,.T.);
#45671=EDGE_CURVE('',#36528,#36532,#32807,.T.);
#45672=EDGE_CURVE('',#36534,#36533,#32808,.T.);
#45673=EDGE_CURVE('',#36535,#36536,#4033,.T.);
#45674=EDGE_CURVE('',#36535,#36537,#32809,.T.);
#45675=EDGE_CURVE('',#36537,#36538,#4034,.T.);
#45676=EDGE_CURVE('',#36536,#36538,#32810,.T.);
#45677=EDGE_CURVE('',#36539,#36540,#4035,.T.);
#45678=EDGE_CURVE('',#36539,#36535,#32811,.T.);
#45679=EDGE_CURVE('',#36540,#36536,#32812,.T.);
#45680=EDGE_CURVE('',#36541,#36542,#4036,.T.);
#45681=EDGE_CURVE('',#36541,#36539,#32813,.T.);
#45682=EDGE_CURVE('',#36542,#36540,#32814,.T.);
#45683=EDGE_CURVE('',#36537,#36541,#32815,.T.);
#45684=EDGE_CURVE('',#36538,#36542,#32816,.T.);
#45685=EDGE_CURVE('',#36543,#36544,#4037,.T.);
#45686=EDGE_CURVE('',#36543,#36545,#32817,.T.);
#45687=EDGE_CURVE('',#36545,#36546,#4038,.T.);
#45688=EDGE_CURVE('',#36544,#36546,#32818,.T.);
#45689=EDGE_CURVE('',#36547,#36548,#4039,.T.);
#45690=EDGE_CURVE('',#36547,#36543,#32819,.T.);
#45691=EDGE_CURVE('',#36548,#36544,#32820,.T.);
#45692=EDGE_CURVE('',#36549,#36550,#4040,.T.);
#45693=EDGE_CURVE('',#36549,#36547,#32821,.T.);
#45694=EDGE_CURVE('',#36550,#36548,#32822,.T.);
#45695=EDGE_CURVE('',#36545,#36549,#32823,.T.);
#45696=EDGE_CURVE('',#36546,#36550,#32824,.T.);
#45697=EDGE_CURVE('',#36551,#36552,#4041,.T.);
#45698=EDGE_CURVE('',#36551,#36553,#32825,.T.);
#45699=EDGE_CURVE('',#36553,#36554,#4042,.T.);
#45700=EDGE_CURVE('',#36552,#36554,#32826,.T.);
#45701=EDGE_CURVE('',#36555,#36556,#4043,.T.);
#45702=EDGE_CURVE('',#36555,#36551,#32827,.T.);
#45703=EDGE_CURVE('',#36556,#36552,#32828,.T.);
#45704=EDGE_CURVE('',#36557,#36558,#4044,.T.);
#45705=EDGE_CURVE('',#36557,#36555,#32829,.T.);
#45706=EDGE_CURVE('',#36558,#36556,#32830,.T.);
#45707=EDGE_CURVE('',#36553,#36557,#32831,.T.);
#45708=EDGE_CURVE('',#36554,#36558,#32832,.T.);
#45709=EDGE_CURVE('',#36559,#36560,#4045,.T.);
#45710=EDGE_CURVE('',#36559,#36561,#32833,.T.);
#45711=EDGE_CURVE('',#36561,#36562,#4046,.T.);
#45712=EDGE_CURVE('',#36560,#36562,#32834,.T.);
#45713=EDGE_CURVE('',#36563,#36564,#4047,.T.);
#45714=EDGE_CURVE('',#36563,#36559,#32835,.T.);
#45715=EDGE_CURVE('',#36564,#36560,#32836,.T.);
#45716=EDGE_CURVE('',#36565,#36566,#4048,.T.);
#45717=EDGE_CURVE('',#36565,#36563,#32837,.T.);
#45718=EDGE_CURVE('',#36566,#36564,#32838,.T.);
#45719=EDGE_CURVE('',#36561,#36565,#32839,.T.);
#45720=EDGE_CURVE('',#36562,#36566,#32840,.T.);
#45721=EDGE_CURVE('',#36567,#36568,#4049,.T.);
#45722=EDGE_CURVE('',#36567,#36569,#32841,.T.);
#45723=EDGE_CURVE('',#36569,#36570,#4050,.T.);
#45724=EDGE_CURVE('',#36568,#36570,#32842,.T.);
#45725=EDGE_CURVE('',#36571,#36572,#4051,.T.);
#45726=EDGE_CURVE('',#36571,#36567,#32843,.T.);
#45727=EDGE_CURVE('',#36572,#36568,#32844,.T.);
#45728=EDGE_CURVE('',#36573,#36574,#4052,.T.);
#45729=EDGE_CURVE('',#36573,#36571,#32845,.T.);
#45730=EDGE_CURVE('',#36574,#36572,#32846,.T.);
#45731=EDGE_CURVE('',#36569,#36573,#32847,.T.);
#45732=EDGE_CURVE('',#36570,#36574,#32848,.T.);
#45733=EDGE_CURVE('',#36575,#36576,#4053,.T.);
#45734=EDGE_CURVE('',#36575,#36577,#32849,.T.);
#45735=EDGE_CURVE('',#36577,#36578,#4054,.T.);
#45736=EDGE_CURVE('',#36576,#36578,#32850,.T.);
#45737=EDGE_CURVE('',#36579,#36580,#4055,.T.);
#45738=EDGE_CURVE('',#36579,#36575,#32851,.T.);
#45739=EDGE_CURVE('',#36580,#36576,#32852,.T.);
#45740=EDGE_CURVE('',#36581,#36582,#4056,.T.);
#45741=EDGE_CURVE('',#36581,#36579,#32853,.T.);
#45742=EDGE_CURVE('',#36582,#36580,#32854,.T.);
#45743=EDGE_CURVE('',#36577,#36581,#32855,.T.);
#45744=EDGE_CURVE('',#36578,#36582,#32856,.T.);
#45745=EDGE_CURVE('',#36583,#36584,#4057,.T.);
#45746=EDGE_CURVE('',#36583,#36585,#32857,.T.);
#45747=EDGE_CURVE('',#36585,#36586,#4058,.T.);
#45748=EDGE_CURVE('',#36584,#36586,#32858,.T.);
#45749=EDGE_CURVE('',#36587,#36588,#4059,.T.);
#45750=EDGE_CURVE('',#36587,#36583,#32859,.T.);
#45751=EDGE_CURVE('',#36588,#36584,#32860,.T.);
#45752=EDGE_CURVE('',#36589,#36590,#4060,.T.);
#45753=EDGE_CURVE('',#36589,#36587,#32861,.T.);
#45754=EDGE_CURVE('',#36590,#36588,#32862,.T.);
#45755=EDGE_CURVE('',#36585,#36589,#32863,.T.);
#45756=EDGE_CURVE('',#36586,#36590,#32864,.T.);
#45757=EDGE_CURVE('',#36591,#36592,#4061,.T.);
#45758=EDGE_CURVE('',#36591,#36593,#32865,.T.);
#45759=EDGE_CURVE('',#36593,#36594,#4062,.T.);
#45760=EDGE_CURVE('',#36592,#36594,#32866,.T.);
#45761=EDGE_CURVE('',#36595,#36596,#4063,.T.);
#45762=EDGE_CURVE('',#36595,#36591,#32867,.T.);
#45763=EDGE_CURVE('',#36596,#36592,#32868,.T.);
#45764=EDGE_CURVE('',#36597,#36598,#4064,.T.);
#45765=EDGE_CURVE('',#36597,#36595,#32869,.T.);
#45766=EDGE_CURVE('',#36598,#36596,#32870,.T.);
#45767=EDGE_CURVE('',#36593,#36597,#32871,.T.);
#45768=EDGE_CURVE('',#36594,#36598,#32872,.T.);
#45769=EDGE_CURVE('',#36599,#36600,#4065,.T.);
#45770=EDGE_CURVE('',#36599,#36601,#32873,.T.);
#45771=EDGE_CURVE('',#36601,#36602,#4066,.T.);
#45772=EDGE_CURVE('',#36600,#36602,#32874,.T.);
#45773=EDGE_CURVE('',#36603,#36604,#4067,.T.);
#45774=EDGE_CURVE('',#36603,#36599,#32875,.T.);
#45775=EDGE_CURVE('',#36604,#36600,#32876,.T.);
#45776=EDGE_CURVE('',#36605,#36606,#4068,.T.);
#45777=EDGE_CURVE('',#36605,#36603,#32877,.T.);
#45778=EDGE_CURVE('',#36606,#36604,#32878,.T.);
#45779=EDGE_CURVE('',#36601,#36605,#32879,.T.);
#45780=EDGE_CURVE('',#36602,#36606,#32880,.T.);
#45781=EDGE_CURVE('',#36607,#36608,#4069,.T.);
#45782=EDGE_CURVE('',#36607,#36609,#32881,.T.);
#45783=EDGE_CURVE('',#36609,#36610,#4070,.T.);
#45784=EDGE_CURVE('',#36608,#36610,#32882,.T.);
#45785=EDGE_CURVE('',#36611,#36612,#4071,.T.);
#45786=EDGE_CURVE('',#36613,#36611,#4072,.T.);
#45787=EDGE_CURVE('',#36613,#36607,#32883,.T.);
#45788=EDGE_CURVE('',#36612,#36608,#32884,.T.);
#45789=EDGE_CURVE('',#36614,#36615,#4073,.T.);
#45790=EDGE_CURVE('',#36611,#36614,#4074,.T.);
#45791=EDGE_CURVE('',#36615,#36612,#32885,.T.);
#45792=EDGE_CURVE('',#36609,#36616,#32886,.T.);
#45793=EDGE_CURVE('',#36614,#36616,#4075,.T.);
#45794=EDGE_CURVE('',#36610,#36615,#32887,.T.);
#45795=EDGE_CURVE('',#36616,#36613,#32888,.T.);
#45796=EDGE_CURVE('',#36617,#36618,#4076,.T.);
#45797=EDGE_CURVE('',#36617,#36619,#32889,.T.);
#45798=EDGE_CURVE('',#36619,#36620,#4077,.T.);
#45799=EDGE_CURVE('',#36618,#36620,#32890,.T.);
#45800=EDGE_CURVE('',#36621,#36622,#4078,.T.);
#45801=EDGE_CURVE('',#36621,#36617,#32891,.T.);
#45802=EDGE_CURVE('',#36622,#36618,#32892,.T.);
#45803=EDGE_CURVE('',#36623,#36624,#4079,.T.);
#45804=EDGE_CURVE('',#36625,#36623,#4080,.T.);
#45805=EDGE_CURVE('',#36625,#36621,#32893,.T.);
#45806=EDGE_CURVE('',#36624,#36622,#32894,.T.);
#45807=EDGE_CURVE('',#36619,#36626,#32895,.T.);
#45808=EDGE_CURVE('',#36623,#36626,#4081,.T.);
#45809=EDGE_CURVE('',#36620,#36624,#32896,.T.);
#45810=EDGE_CURVE('',#36626,#36625,#32897,.T.);
#45811=EDGE_CURVE('',#36627,#36628,#4082,.T.);
#45812=EDGE_CURVE('',#36627,#36629,#32898,.T.);
#45813=EDGE_CURVE('',#36629,#36630,#4083,.T.);
#45814=EDGE_CURVE('',#36628,#36630,#32899,.T.);
#45815=EDGE_CURVE('',#36631,#36632,#4084,.T.);
#45816=EDGE_CURVE('',#36631,#36627,#32900,.T.);
#45817=EDGE_CURVE('',#36632,#36628,#32901,.T.);
#45818=EDGE_CURVE('',#36633,#36634,#4085,.T.);
#45819=EDGE_CURVE('',#36633,#36631,#32902,.T.);
#45820=EDGE_CURVE('',#36634,#36632,#32903,.T.);
#45821=EDGE_CURVE('',#36629,#36633,#32904,.T.);
#45822=EDGE_CURVE('',#36630,#36634,#32905,.T.);
#45823=EDGE_CURVE('',#36635,#36636,#4086,.T.);
#45824=EDGE_CURVE('',#36635,#36637,#32906,.T.);
#45825=EDGE_CURVE('',#36637,#36638,#4087,.T.);
#45826=EDGE_CURVE('',#36636,#36638,#32907,.T.);
#45827=EDGE_CURVE('',#36639,#36640,#4088,.T.);
#45828=EDGE_CURVE('',#36639,#36635,#32908,.T.);
#45829=EDGE_CURVE('',#36640,#36636,#32909,.T.);
#45830=EDGE_CURVE('',#36641,#36642,#4089,.T.);
#45831=EDGE_CURVE('',#36641,#36639,#32910,.T.);
#45832=EDGE_CURVE('',#36642,#36640,#32911,.T.);
#45833=EDGE_CURVE('',#36637,#36641,#32912,.T.);
#45834=EDGE_CURVE('',#36638,#36642,#32913,.T.);
#45835=EDGE_CURVE('',#36643,#36644,#4090,.T.);
#45836=EDGE_CURVE('',#36643,#36645,#32914,.T.);
#45837=EDGE_CURVE('',#36645,#36646,#4091,.T.);
#45838=EDGE_CURVE('',#36644,#36646,#32915,.T.);
#45839=EDGE_CURVE('',#36647,#36648,#4092,.T.);
#45840=EDGE_CURVE('',#36647,#36643,#32916,.T.);
#45841=EDGE_CURVE('',#36648,#36644,#32917,.T.);
#45842=EDGE_CURVE('',#36649,#36650,#4093,.T.);
#45843=EDGE_CURVE('',#36649,#36647,#32918,.T.);
#45844=EDGE_CURVE('',#36650,#36648,#32919,.T.);
#45845=EDGE_CURVE('',#36645,#36649,#32920,.T.);
#45846=EDGE_CURVE('',#36646,#36650,#32921,.T.);
#45847=EDGE_CURVE('',#36651,#36652,#4094,.T.);
#45848=EDGE_CURVE('',#36651,#36653,#32922,.T.);
#45849=EDGE_CURVE('',#36653,#36654,#4095,.T.);
#45850=EDGE_CURVE('',#36652,#36654,#32923,.T.);
#45851=EDGE_CURVE('',#36655,#36656,#4096,.T.);
#45852=EDGE_CURVE('',#36655,#36651,#32924,.T.);
#45853=EDGE_CURVE('',#36656,#36652,#32925,.T.);
#45854=EDGE_CURVE('',#36657,#36658,#4097,.T.);
#45855=EDGE_CURVE('',#36657,#36655,#32926,.T.);
#45856=EDGE_CURVE('',#36658,#36656,#32927,.T.);
#45857=EDGE_CURVE('',#36653,#36657,#32928,.T.);
#45858=EDGE_CURVE('',#36654,#36658,#32929,.T.);
#45859=EDGE_CURVE('',#36659,#36660,#4098,.T.);
#45860=EDGE_CURVE('',#36659,#36661,#32930,.T.);
#45861=EDGE_CURVE('',#36661,#36662,#4099,.T.);
#45862=EDGE_CURVE('',#36660,#36662,#32931,.T.);
#45863=EDGE_CURVE('',#36663,#36664,#4100,.T.);
#45864=EDGE_CURVE('',#36663,#36659,#32932,.T.);
#45865=EDGE_CURVE('',#36664,#36660,#32933,.T.);
#45866=EDGE_CURVE('',#36665,#36666,#4101,.T.);
#45867=EDGE_CURVE('',#36665,#36663,#32934,.T.);
#45868=EDGE_CURVE('',#36666,#36664,#32935,.T.);
#45869=EDGE_CURVE('',#36661,#36665,#32936,.T.);
#45870=EDGE_CURVE('',#36662,#36666,#32937,.T.);
#45871=EDGE_CURVE('',#36667,#36668,#4102,.T.);
#45872=EDGE_CURVE('',#36667,#36669,#32938,.T.);
#45873=EDGE_CURVE('',#36669,#36670,#4103,.T.);
#45874=EDGE_CURVE('',#36668,#36670,#32939,.T.);
#45875=EDGE_CURVE('',#36671,#36672,#4104,.T.);
#45876=EDGE_CURVE('',#36671,#36667,#32940,.T.);
#45877=EDGE_CURVE('',#36672,#36668,#32941,.T.);
#45878=EDGE_CURVE('',#36673,#36674,#4105,.T.);
#45879=EDGE_CURVE('',#36673,#36671,#32942,.T.);
#45880=EDGE_CURVE('',#36674,#36672,#32943,.T.);
#45881=EDGE_CURVE('',#36669,#36673,#32944,.T.);
#45882=EDGE_CURVE('',#36670,#36674,#32945,.T.);
#45883=EDGE_CURVE('',#36675,#36676,#4106,.T.);
#45884=EDGE_CURVE('',#36675,#36677,#32946,.T.);
#45885=EDGE_CURVE('',#36677,#36678,#4107,.T.);
#45886=EDGE_CURVE('',#36676,#36678,#32947,.T.);
#45887=EDGE_CURVE('',#36679,#36680,#4108,.T.);
#45888=EDGE_CURVE('',#36679,#36675,#32948,.T.);
#45889=EDGE_CURVE('',#36680,#36676,#32949,.T.);
#45890=EDGE_CURVE('',#36681,#36682,#4109,.T.);
#45891=EDGE_CURVE('',#36681,#36679,#32950,.T.);
#45892=EDGE_CURVE('',#36682,#36680,#32951,.T.);
#45893=EDGE_CURVE('',#36677,#36681,#32952,.T.);
#45894=EDGE_CURVE('',#36678,#36682,#32953,.T.);
#45895=EDGE_CURVE('',#36683,#36684,#4110,.T.);
#45896=EDGE_CURVE('',#36683,#36685,#32954,.T.);
#45897=EDGE_CURVE('',#36685,#36686,#4111,.T.);
#45898=EDGE_CURVE('',#36684,#36686,#32955,.T.);
#45899=EDGE_CURVE('',#36687,#36688,#4112,.T.);
#45900=EDGE_CURVE('',#36687,#36683,#32956,.T.);
#45901=EDGE_CURVE('',#36688,#36684,#32957,.T.);
#45902=EDGE_CURVE('',#36689,#36690,#4113,.T.);
#45903=EDGE_CURVE('',#36689,#36687,#32958,.T.);
#45904=EDGE_CURVE('',#36690,#36688,#32959,.T.);
#45905=EDGE_CURVE('',#36685,#36689,#32960,.T.);
#45906=EDGE_CURVE('',#36686,#36690,#32961,.T.);
#45907=EDGE_CURVE('',#36691,#36692,#4114,.T.);
#45908=EDGE_CURVE('',#36691,#36693,#32962,.T.);
#45909=EDGE_CURVE('',#36693,#36694,#4115,.T.);
#45910=EDGE_CURVE('',#36692,#36694,#32963,.T.);
#45911=EDGE_CURVE('',#36695,#36696,#4116,.T.);
#45912=EDGE_CURVE('',#36695,#36691,#32964,.T.);
#45913=EDGE_CURVE('',#36696,#36692,#32965,.T.);
#45914=EDGE_CURVE('',#36697,#36698,#4117,.T.);
#45915=EDGE_CURVE('',#36697,#36695,#32966,.T.);
#45916=EDGE_CURVE('',#36698,#36696,#32967,.T.);
#45917=EDGE_CURVE('',#36693,#36697,#32968,.T.);
#45918=EDGE_CURVE('',#36694,#36698,#32969,.T.);
#45919=EDGE_CURVE('',#36699,#36700,#4118,.T.);
#45920=EDGE_CURVE('',#36699,#36701,#32970,.T.);
#45921=EDGE_CURVE('',#36701,#36702,#4119,.T.);
#45922=EDGE_CURVE('',#36700,#36702,#32971,.T.);
#45923=EDGE_CURVE('',#36703,#36704,#4120,.T.);
#45924=EDGE_CURVE('',#36703,#36699,#32972,.T.);
#45925=EDGE_CURVE('',#36704,#36700,#32973,.T.);
#45926=EDGE_CURVE('',#36705,#36706,#4121,.T.);
#45927=EDGE_CURVE('',#36705,#36703,#32974,.T.);
#45928=EDGE_CURVE('',#36706,#36704,#32975,.T.);
#45929=EDGE_CURVE('',#36701,#36705,#32976,.T.);
#45930=EDGE_CURVE('',#36702,#36706,#32977,.T.);
#45931=EDGE_CURVE('',#36707,#36708,#4122,.T.);
#45932=EDGE_CURVE('',#36707,#36709,#32978,.T.);
#45933=EDGE_CURVE('',#36709,#36710,#4123,.T.);
#45934=EDGE_CURVE('',#36708,#36710,#32979,.T.);
#45935=EDGE_CURVE('',#36711,#36712,#4124,.T.);
#45936=EDGE_CURVE('',#36711,#36707,#32980,.T.);
#45937=EDGE_CURVE('',#36712,#36708,#32981,.T.);
#45938=EDGE_CURVE('',#36713,#36714,#4125,.T.);
#45939=EDGE_CURVE('',#36713,#36711,#32982,.T.);
#45940=EDGE_CURVE('',#36714,#36712,#32983,.T.);
#45941=EDGE_CURVE('',#36709,#36713,#32984,.T.);
#45942=EDGE_CURVE('',#36710,#36714,#32985,.T.);
#45943=EDGE_CURVE('',#36715,#36716,#4126,.T.);
#45944=EDGE_CURVE('',#36715,#36717,#32986,.T.);
#45945=EDGE_CURVE('',#36717,#36718,#4127,.T.);
#45946=EDGE_CURVE('',#36716,#36718,#32987,.T.);
#45947=EDGE_CURVE('',#36719,#36720,#4128,.T.);
#45948=EDGE_CURVE('',#36719,#36715,#32988,.T.);
#45949=EDGE_CURVE('',#36720,#36716,#32989,.T.);
#45950=EDGE_CURVE('',#36721,#36722,#4129,.T.);
#45951=EDGE_CURVE('',#36721,#36719,#32990,.T.);
#45952=EDGE_CURVE('',#36722,#36720,#32991,.T.);
#45953=EDGE_CURVE('',#36717,#36721,#32992,.T.);
#45954=EDGE_CURVE('',#36718,#36722,#32993,.T.);
#45955=EDGE_CURVE('',#36723,#36724,#4130,.T.);
#45956=EDGE_CURVE('',#36723,#36725,#32994,.T.);
#45957=EDGE_CURVE('',#36725,#36726,#4131,.T.);
#45958=EDGE_CURVE('',#36724,#36726,#32995,.T.);
#45959=EDGE_CURVE('',#36727,#36728,#4132,.T.);
#45960=EDGE_CURVE('',#36727,#36723,#32996,.T.);
#45961=EDGE_CURVE('',#36728,#36724,#32997,.T.);
#45962=EDGE_CURVE('',#36729,#36730,#4133,.T.);
#45963=EDGE_CURVE('',#36729,#36727,#32998,.T.);
#45964=EDGE_CURVE('',#36730,#36728,#32999,.T.);
#45965=EDGE_CURVE('',#36725,#36729,#33000,.T.);
#45966=EDGE_CURVE('',#36726,#36730,#33001,.T.);
#45967=EDGE_CURVE('',#36731,#36732,#4134,.T.);
#45968=EDGE_CURVE('',#36731,#36733,#33002,.T.);
#45969=EDGE_CURVE('',#36733,#36734,#4135,.T.);
#45970=EDGE_CURVE('',#36732,#36734,#33003,.T.);
#45971=EDGE_CURVE('',#36735,#36736,#4136,.T.);
#45972=EDGE_CURVE('',#36735,#36731,#33004,.T.);
#45973=EDGE_CURVE('',#36736,#36732,#33005,.T.);
#45974=EDGE_CURVE('',#36737,#36738,#4137,.T.);
#45975=EDGE_CURVE('',#36737,#36735,#33006,.T.);
#45976=EDGE_CURVE('',#36738,#36736,#33007,.T.);
#45977=EDGE_CURVE('',#36733,#36737,#33008,.T.);
#45978=EDGE_CURVE('',#36734,#36738,#33009,.T.);
#45979=EDGE_CURVE('',#36739,#36740,#4138,.T.);
#45980=EDGE_CURVE('',#36739,#36741,#33010,.T.);
#45981=EDGE_CURVE('',#36741,#36742,#4139,.T.);
#45982=EDGE_CURVE('',#36740,#36742,#33011,.T.);
#45983=EDGE_CURVE('',#36743,#36744,#4140,.T.);
#45984=EDGE_CURVE('',#36743,#36739,#33012,.T.);
#45985=EDGE_CURVE('',#36744,#36740,#33013,.T.);
#45986=EDGE_CURVE('',#36745,#36746,#4141,.T.);
#45987=EDGE_CURVE('',#36745,#36743,#33014,.T.);
#45988=EDGE_CURVE('',#36746,#36744,#33015,.T.);
#45989=EDGE_CURVE('',#36741,#36745,#33016,.T.);
#45990=EDGE_CURVE('',#36742,#36746,#33017,.T.);
#45991=EDGE_CURVE('',#36747,#36748,#4142,.T.);
#45992=EDGE_CURVE('',#36747,#36749,#33018,.T.);
#45993=EDGE_CURVE('',#36749,#36750,#4143,.T.);
#45994=EDGE_CURVE('',#36748,#36750,#33019,.T.);
#45995=EDGE_CURVE('',#36751,#36752,#4144,.T.);
#45996=EDGE_CURVE('',#36751,#36747,#33020,.T.);
#45997=EDGE_CURVE('',#36752,#36748,#33021,.T.);
#45998=EDGE_CURVE('',#36753,#36754,#4145,.T.);
#45999=EDGE_CURVE('',#36753,#36751,#33022,.T.);
#46000=EDGE_CURVE('',#36754,#36752,#33023,.T.);
#46001=EDGE_CURVE('',#36749,#36753,#33024,.T.);
#46002=EDGE_CURVE('',#36750,#36754,#33025,.T.);
#46003=EDGE_CURVE('',#36755,#36756,#4146,.T.);
#46004=EDGE_CURVE('',#36755,#36757,#33026,.T.);
#46005=EDGE_CURVE('',#36757,#36758,#4147,.T.);
#46006=EDGE_CURVE('',#36756,#36758,#33027,.T.);
#46007=EDGE_CURVE('',#36759,#36760,#4148,.T.);
#46008=EDGE_CURVE('',#36759,#36755,#33028,.T.);
#46009=EDGE_CURVE('',#36760,#36756,#33029,.T.);
#46010=EDGE_CURVE('',#36761,#36762,#4149,.T.);
#46011=EDGE_CURVE('',#36761,#36759,#33030,.T.);
#46012=EDGE_CURVE('',#36762,#36760,#33031,.T.);
#46013=EDGE_CURVE('',#36757,#36761,#33032,.T.);
#46014=EDGE_CURVE('',#36758,#36762,#33033,.T.);
#46015=EDGE_CURVE('',#36763,#36764,#4150,.T.);
#46016=EDGE_CURVE('',#36763,#36765,#33034,.T.);
#46017=EDGE_CURVE('',#36765,#36766,#4151,.T.);
#46018=EDGE_CURVE('',#36764,#36766,#33035,.T.);
#46019=EDGE_CURVE('',#36767,#36768,#4152,.T.);
#46020=EDGE_CURVE('',#36767,#36763,#33036,.T.);
#46021=EDGE_CURVE('',#36768,#36764,#33037,.T.);
#46022=EDGE_CURVE('',#36769,#36770,#4153,.T.);
#46023=EDGE_CURVE('',#36769,#36767,#33038,.T.);
#46024=EDGE_CURVE('',#36770,#36768,#33039,.T.);
#46025=EDGE_CURVE('',#36765,#36769,#33040,.T.);
#46026=EDGE_CURVE('',#36766,#36770,#33041,.T.);
#46027=EDGE_CURVE('',#36771,#36772,#4154,.T.);
#46028=EDGE_CURVE('',#36771,#36773,#33042,.T.);
#46029=EDGE_CURVE('',#36773,#36774,#4155,.T.);
#46030=EDGE_CURVE('',#36772,#36774,#33043,.T.);
#46031=EDGE_CURVE('',#36775,#36776,#4156,.T.);
#46032=EDGE_CURVE('',#36775,#36771,#33044,.T.);
#46033=EDGE_CURVE('',#36776,#36772,#33045,.T.);
#46034=EDGE_CURVE('',#36777,#36778,#4157,.T.);
#46035=EDGE_CURVE('',#36777,#36775,#33046,.T.);
#46036=EDGE_CURVE('',#36778,#36776,#33047,.T.);
#46037=EDGE_CURVE('',#36773,#36777,#33048,.T.);
#46038=EDGE_CURVE('',#36774,#36778,#33049,.T.);
#46039=EDGE_CURVE('',#36779,#36780,#4158,.T.);
#46040=EDGE_CURVE('',#36779,#36781,#33050,.T.);
#46041=EDGE_CURVE('',#36781,#36782,#4159,.T.);
#46042=EDGE_CURVE('',#36780,#36782,#33051,.T.);
#46043=EDGE_CURVE('',#36783,#36784,#4160,.T.);
#46044=EDGE_CURVE('',#36783,#36779,#33052,.T.);
#46045=EDGE_CURVE('',#36784,#36780,#33053,.T.);
#46046=EDGE_CURVE('',#36785,#36786,#4161,.T.);
#46047=EDGE_CURVE('',#36785,#36783,#33054,.T.);
#46048=EDGE_CURVE('',#36786,#36784,#33055,.T.);
#46049=EDGE_CURVE('',#36781,#36785,#33056,.T.);
#46050=EDGE_CURVE('',#36782,#36786,#33057,.T.);
#46051=EDGE_CURVE('',#36787,#36788,#4162,.T.);
#46052=EDGE_CURVE('',#36787,#36789,#33058,.T.);
#46053=EDGE_CURVE('',#36789,#36790,#4163,.T.);
#46054=EDGE_CURVE('',#36788,#36790,#33059,.T.);
#46055=EDGE_CURVE('',#36791,#36792,#4164,.T.);
#46056=EDGE_CURVE('',#36791,#36787,#33060,.T.);
#46057=EDGE_CURVE('',#36792,#36788,#33061,.T.);
#46058=EDGE_CURVE('',#36793,#36794,#4165,.T.);
#46059=EDGE_CURVE('',#36793,#36791,#33062,.T.);
#46060=EDGE_CURVE('',#36794,#36792,#33063,.T.);
#46061=EDGE_CURVE('',#36789,#36793,#33064,.T.);
#46062=EDGE_CURVE('',#36790,#36794,#33065,.T.);
#46063=EDGE_CURVE('',#36795,#36796,#4166,.T.);
#46064=EDGE_CURVE('',#36795,#36797,#33066,.T.);
#46065=EDGE_CURVE('',#36797,#36798,#4167,.T.);
#46066=EDGE_CURVE('',#36796,#36798,#33067,.T.);
#46067=EDGE_CURVE('',#36799,#36800,#4168,.T.);
#46068=EDGE_CURVE('',#36799,#36795,#33068,.T.);
#46069=EDGE_CURVE('',#36800,#36796,#33069,.T.);
#46070=EDGE_CURVE('',#36801,#36802,#4169,.T.);
#46071=EDGE_CURVE('',#36801,#36799,#33070,.T.);
#46072=EDGE_CURVE('',#36802,#36800,#33071,.T.);
#46073=EDGE_CURVE('',#36797,#36801,#33072,.T.);
#46074=EDGE_CURVE('',#36798,#36802,#33073,.T.);
#46075=EDGE_CURVE('',#36803,#36804,#4170,.T.);
#46076=EDGE_CURVE('',#36803,#36805,#33074,.T.);
#46077=EDGE_CURVE('',#36805,#36806,#4171,.T.);
#46078=EDGE_CURVE('',#36804,#36806,#33075,.T.);
#46079=EDGE_CURVE('',#36807,#36808,#4172,.T.);
#46080=EDGE_CURVE('',#36807,#36803,#33076,.T.);
#46081=EDGE_CURVE('',#36808,#36804,#33077,.T.);
#46082=EDGE_CURVE('',#36809,#36810,#4173,.T.);
#46083=EDGE_CURVE('',#36809,#36807,#33078,.T.);
#46084=EDGE_CURVE('',#36810,#36808,#33079,.T.);
#46085=EDGE_CURVE('',#36805,#36809,#33080,.T.);
#46086=EDGE_CURVE('',#36806,#36810,#33081,.T.);
#46087=EDGE_CURVE('',#36811,#36812,#4174,.T.);
#46088=EDGE_CURVE('',#36811,#36813,#33082,.T.);
#46089=EDGE_CURVE('',#36813,#36814,#4175,.T.);
#46090=EDGE_CURVE('',#36812,#36814,#33083,.T.);
#46091=EDGE_CURVE('',#36815,#36816,#4176,.T.);
#46092=EDGE_CURVE('',#36815,#36811,#33084,.T.);
#46093=EDGE_CURVE('',#36816,#36812,#33085,.T.);
#46094=EDGE_CURVE('',#36817,#36818,#4177,.T.);
#46095=EDGE_CURVE('',#36817,#36815,#33086,.T.);
#46096=EDGE_CURVE('',#36818,#36816,#33087,.T.);
#46097=EDGE_CURVE('',#36813,#36817,#33088,.T.);
#46098=EDGE_CURVE('',#36814,#36818,#33089,.T.);
#46099=EDGE_CURVE('',#36819,#36820,#4178,.T.);
#46100=EDGE_CURVE('',#36819,#36821,#33090,.T.);
#46101=EDGE_CURVE('',#36821,#36822,#4179,.T.);
#46102=EDGE_CURVE('',#36820,#36822,#33091,.T.);
#46103=EDGE_CURVE('',#36823,#36824,#4180,.T.);
#46104=EDGE_CURVE('',#36823,#36819,#33092,.T.);
#46105=EDGE_CURVE('',#36824,#36820,#33093,.T.);
#46106=EDGE_CURVE('',#36825,#36826,#4181,.T.);
#46107=EDGE_CURVE('',#36825,#36823,#33094,.T.);
#46108=EDGE_CURVE('',#36826,#36824,#33095,.T.);
#46109=EDGE_CURVE('',#36821,#36825,#33096,.T.);
#46110=EDGE_CURVE('',#36822,#36826,#33097,.T.);
#46111=EDGE_CURVE('',#36827,#36828,#4182,.T.);
#46112=EDGE_CURVE('',#36827,#36829,#33098,.T.);
#46113=EDGE_CURVE('',#36829,#36830,#4183,.T.);
#46114=EDGE_CURVE('',#36828,#36830,#33099,.T.);
#46115=EDGE_CURVE('',#36831,#36832,#4184,.T.);
#46116=EDGE_CURVE('',#36831,#36827,#33100,.T.);
#46117=EDGE_CURVE('',#36832,#36828,#33101,.T.);
#46118=EDGE_CURVE('',#36833,#36834,#4185,.T.);
#46119=EDGE_CURVE('',#36833,#36831,#33102,.T.);
#46120=EDGE_CURVE('',#36834,#36832,#33103,.T.);
#46121=EDGE_CURVE('',#36829,#36833,#33104,.T.);
#46122=EDGE_CURVE('',#36830,#36834,#33105,.T.);
#46123=EDGE_CURVE('',#36835,#36836,#4186,.T.);
#46124=EDGE_CURVE('',#36835,#36837,#33106,.T.);
#46125=EDGE_CURVE('',#36837,#36838,#4187,.T.);
#46126=EDGE_CURVE('',#36836,#36838,#33107,.T.);
#46127=EDGE_CURVE('',#36839,#36840,#4188,.T.);
#46128=EDGE_CURVE('',#36839,#36835,#33108,.T.);
#46129=EDGE_CURVE('',#36840,#36836,#33109,.T.);
#46130=EDGE_CURVE('',#36841,#36842,#4189,.T.);
#46131=EDGE_CURVE('',#36841,#36839,#33110,.T.);
#46132=EDGE_CURVE('',#36842,#36840,#33111,.T.);
#46133=EDGE_CURVE('',#36837,#36841,#33112,.T.);
#46134=EDGE_CURVE('',#36838,#36842,#33113,.T.);
#46135=EDGE_CURVE('',#36843,#36844,#4190,.T.);
#46136=EDGE_CURVE('',#36843,#36845,#33114,.T.);
#46137=EDGE_CURVE('',#36845,#36846,#4191,.T.);
#46138=EDGE_CURVE('',#36844,#36846,#33115,.T.);
#46139=EDGE_CURVE('',#36847,#36848,#4192,.T.);
#46140=EDGE_CURVE('',#36847,#36843,#33116,.T.);
#46141=EDGE_CURVE('',#36848,#36844,#33117,.T.);
#46142=EDGE_CURVE('',#36849,#36850,#4193,.T.);
#46143=EDGE_CURVE('',#36849,#36847,#33118,.T.);
#46144=EDGE_CURVE('',#36850,#36848,#33119,.T.);
#46145=EDGE_CURVE('',#36845,#36849,#33120,.T.);
#46146=EDGE_CURVE('',#36846,#36850,#33121,.T.);
#46147=EDGE_CURVE('',#36851,#36852,#4194,.T.);
#46148=EDGE_CURVE('',#36851,#36853,#33122,.T.);
#46149=EDGE_CURVE('',#36853,#36854,#4195,.T.);
#46150=EDGE_CURVE('',#36852,#36854,#33123,.T.);
#46151=EDGE_CURVE('',#36855,#36856,#4196,.T.);
#46152=EDGE_CURVE('',#36855,#36851,#33124,.T.);
#46153=EDGE_CURVE('',#36856,#36852,#33125,.T.);
#46154=EDGE_CURVE('',#36857,#36858,#4197,.T.);
#46155=EDGE_CURVE('',#36857,#36855,#33126,.T.);
#46156=EDGE_CURVE('',#36858,#36856,#33127,.T.);
#46157=EDGE_CURVE('',#36853,#36857,#33128,.T.);
#46158=EDGE_CURVE('',#36854,#36858,#33129,.T.);
#46159=EDGE_CURVE('',#36859,#36860,#4198,.T.);
#46160=EDGE_CURVE('',#36859,#36861,#33130,.T.);
#46161=EDGE_CURVE('',#36861,#36862,#4199,.T.);
#46162=EDGE_CURVE('',#36860,#36862,#33131,.T.);
#46163=EDGE_CURVE('',#36863,#36864,#4200,.T.);
#46164=EDGE_CURVE('',#36863,#36859,#33132,.T.);
#46165=EDGE_CURVE('',#36864,#36860,#33133,.T.);
#46166=EDGE_CURVE('',#36865,#36866,#4201,.T.);
#46167=EDGE_CURVE('',#36865,#36863,#33134,.T.);
#46168=EDGE_CURVE('',#36866,#36864,#33135,.T.);
#46169=EDGE_CURVE('',#36861,#36865,#33136,.T.);
#46170=EDGE_CURVE('',#36862,#36866,#33137,.T.);
#46171=EDGE_CURVE('',#36867,#36868,#4202,.T.);
#46172=EDGE_CURVE('',#36867,#36869,#33138,.T.);
#46173=EDGE_CURVE('',#36869,#36870,#4203,.T.);
#46174=EDGE_CURVE('',#36868,#36870,#33139,.T.);
#46175=EDGE_CURVE('',#36871,#36872,#4204,.T.);
#46176=EDGE_CURVE('',#36871,#36867,#33140,.T.);
#46177=EDGE_CURVE('',#36872,#36868,#33141,.T.);
#46178=EDGE_CURVE('',#36873,#36874,#4205,.T.);
#46179=EDGE_CURVE('',#36873,#36871,#33142,.T.);
#46180=EDGE_CURVE('',#36874,#36872,#33143,.T.);
#46181=EDGE_CURVE('',#36869,#36873,#33144,.T.);
#46182=EDGE_CURVE('',#36870,#36874,#33145,.T.);
#46183=EDGE_CURVE('',#36875,#36876,#4206,.T.);
#46184=EDGE_CURVE('',#36875,#36877,#33146,.T.);
#46185=EDGE_CURVE('',#36877,#36878,#4207,.T.);
#46186=EDGE_CURVE('',#36876,#36878,#33147,.T.);
#46187=EDGE_CURVE('',#36879,#36880,#4208,.T.);
#46188=EDGE_CURVE('',#36879,#36875,#33148,.T.);
#46189=EDGE_CURVE('',#36880,#36876,#33149,.T.);
#46190=EDGE_CURVE('',#36881,#36882,#4209,.T.);
#46191=EDGE_CURVE('',#36881,#36879,#33150,.T.);
#46192=EDGE_CURVE('',#36882,#36880,#33151,.T.);
#46193=EDGE_CURVE('',#36877,#36881,#33152,.T.);
#46194=EDGE_CURVE('',#36878,#36882,#33153,.T.);
#46195=EDGE_CURVE('',#36883,#36884,#4210,.T.);
#46196=EDGE_CURVE('',#36883,#36885,#33154,.T.);
#46197=EDGE_CURVE('',#36885,#36886,#4211,.T.);
#46198=EDGE_CURVE('',#36884,#36886,#33155,.T.);
#46199=EDGE_CURVE('',#36887,#36888,#4212,.T.);
#46200=EDGE_CURVE('',#36887,#36883,#33156,.T.);
#46201=EDGE_CURVE('',#36888,#36884,#33157,.T.);
#46202=EDGE_CURVE('',#36889,#36890,#4213,.T.);
#46203=EDGE_CURVE('',#36889,#36887,#33158,.T.);
#46204=EDGE_CURVE('',#36890,#36888,#33159,.T.);
#46205=EDGE_CURVE('',#36885,#36889,#33160,.T.);
#46206=EDGE_CURVE('',#36886,#36890,#33161,.T.);
#46207=EDGE_CURVE('',#36891,#36892,#4214,.T.);
#46208=EDGE_CURVE('',#36891,#36893,#33162,.T.);
#46209=EDGE_CURVE('',#36893,#36894,#4215,.T.);
#46210=EDGE_CURVE('',#36892,#36894,#33163,.T.);
#46211=EDGE_CURVE('',#36895,#36896,#4216,.T.);
#46212=EDGE_CURVE('',#36895,#36891,#33164,.T.);
#46213=EDGE_CURVE('',#36896,#36892,#33165,.T.);
#46214=EDGE_CURVE('',#36897,#36898,#4217,.T.);
#46215=EDGE_CURVE('',#36897,#36895,#33166,.T.);
#46216=EDGE_CURVE('',#36898,#36896,#33167,.T.);
#46217=EDGE_CURVE('',#36893,#36897,#33168,.T.);
#46218=EDGE_CURVE('',#36894,#36898,#33169,.T.);
#46219=EDGE_CURVE('',#36899,#36900,#4218,.T.);
#46220=EDGE_CURVE('',#36899,#36901,#33170,.T.);
#46221=EDGE_CURVE('',#36901,#36902,#4219,.T.);
#46222=EDGE_CURVE('',#36900,#36902,#33171,.T.);
#46223=EDGE_CURVE('',#36903,#36904,#4220,.T.);
#46224=EDGE_CURVE('',#36903,#36899,#33172,.T.);
#46225=EDGE_CURVE('',#36904,#36900,#33173,.T.);
#46226=EDGE_CURVE('',#36905,#36906,#4221,.T.);
#46227=EDGE_CURVE('',#36905,#36903,#33174,.T.);
#46228=EDGE_CURVE('',#36906,#36904,#33175,.T.);
#46229=EDGE_CURVE('',#36901,#36905,#33176,.T.);
#46230=EDGE_CURVE('',#36902,#36906,#33177,.T.);
#46231=EDGE_CURVE('',#36907,#36908,#4222,.T.);
#46232=EDGE_CURVE('',#36907,#36909,#33178,.T.);
#46233=EDGE_CURVE('',#36909,#36910,#4223,.T.);
#46234=EDGE_CURVE('',#36908,#36910,#33179,.T.);
#46235=EDGE_CURVE('',#36911,#36912,#4224,.T.);
#46236=EDGE_CURVE('',#36911,#36907,#33180,.T.);
#46237=EDGE_CURVE('',#36912,#36908,#33181,.T.);
#46238=EDGE_CURVE('',#36913,#36914,#4225,.T.);
#46239=EDGE_CURVE('',#36913,#36911,#33182,.T.);
#46240=EDGE_CURVE('',#36914,#36912,#33183,.T.);
#46241=EDGE_CURVE('',#36909,#36913,#33184,.T.);
#46242=EDGE_CURVE('',#36910,#36914,#33185,.T.);
#46243=EDGE_CURVE('',#36915,#36916,#4226,.T.);
#46244=EDGE_CURVE('',#36915,#36917,#33186,.T.);
#46245=EDGE_CURVE('',#36917,#36918,#4227,.T.);
#46246=EDGE_CURVE('',#36916,#36918,#33187,.T.);
#46247=EDGE_CURVE('',#36919,#36920,#4228,.T.);
#46248=EDGE_CURVE('',#36919,#36915,#33188,.T.);
#46249=EDGE_CURVE('',#36920,#36916,#33189,.T.);
#46250=EDGE_CURVE('',#36921,#36922,#4229,.T.);
#46251=EDGE_CURVE('',#36921,#36919,#33190,.T.);
#46252=EDGE_CURVE('',#36922,#36920,#33191,.T.);
#46253=EDGE_CURVE('',#36917,#36921,#33192,.T.);
#46254=EDGE_CURVE('',#36918,#36922,#33193,.T.);
#46255=EDGE_CURVE('',#36923,#36924,#4230,.T.);
#46256=EDGE_CURVE('',#36923,#36925,#33194,.T.);
#46257=EDGE_CURVE('',#36925,#36926,#4231,.T.);
#46258=EDGE_CURVE('',#36924,#36926,#33195,.T.);
#46259=EDGE_CURVE('',#36927,#36928,#4232,.T.);
#46260=EDGE_CURVE('',#36927,#36923,#33196,.T.);
#46261=EDGE_CURVE('',#36928,#36924,#33197,.T.);
#46262=EDGE_CURVE('',#36929,#36930,#4233,.T.);
#46263=EDGE_CURVE('',#36929,#36927,#33198,.T.);
#46264=EDGE_CURVE('',#36930,#36928,#33199,.T.);
#46265=EDGE_CURVE('',#36925,#36929,#33200,.T.);
#46266=EDGE_CURVE('',#36926,#36930,#33201,.T.);
#46267=EDGE_CURVE('',#36931,#36932,#4234,.T.);
#46268=EDGE_CURVE('',#36931,#36933,#33202,.T.);
#46269=EDGE_CURVE('',#36933,#36934,#4235,.T.);
#46270=EDGE_CURVE('',#36932,#36934,#33203,.T.);
#46271=EDGE_CURVE('',#36935,#36936,#4236,.T.);
#46272=EDGE_CURVE('',#36935,#36931,#33204,.T.);
#46273=EDGE_CURVE('',#36936,#36932,#33205,.T.);
#46274=EDGE_CURVE('',#36937,#36938,#4237,.T.);
#46275=EDGE_CURVE('',#36937,#36935,#33206,.T.);
#46276=EDGE_CURVE('',#36938,#36936,#33207,.T.);
#46277=EDGE_CURVE('',#36933,#36937,#33208,.T.);
#46278=EDGE_CURVE('',#36934,#36938,#33209,.T.);
#46279=EDGE_CURVE('',#36939,#36940,#4238,.T.);
#46280=EDGE_CURVE('',#36939,#36941,#33210,.T.);
#46281=EDGE_CURVE('',#36941,#36942,#4239,.T.);
#46282=EDGE_CURVE('',#36940,#36942,#33211,.T.);
#46283=EDGE_CURVE('',#36943,#36944,#4240,.T.);
#46284=EDGE_CURVE('',#36943,#36939,#33212,.T.);
#46285=EDGE_CURVE('',#36944,#36940,#33213,.T.);
#46286=EDGE_CURVE('',#36945,#36946,#4241,.T.);
#46287=EDGE_CURVE('',#36945,#36943,#33214,.T.);
#46288=EDGE_CURVE('',#36946,#36944,#33215,.T.);
#46289=EDGE_CURVE('',#36941,#36945,#33216,.T.);
#46290=EDGE_CURVE('',#36942,#36946,#33217,.T.);
#46291=EDGE_CURVE('',#36947,#36948,#4242,.T.);
#46292=EDGE_CURVE('',#36947,#36949,#33218,.T.);
#46293=EDGE_CURVE('',#36949,#36950,#4243,.T.);
#46294=EDGE_CURVE('',#36948,#36950,#33219,.T.);
#46295=EDGE_CURVE('',#36951,#36952,#4244,.T.);
#46296=EDGE_CURVE('',#36951,#36947,#33220,.T.);
#46297=EDGE_CURVE('',#36952,#36948,#33221,.T.);
#46298=EDGE_CURVE('',#36953,#36954,#4245,.T.);
#46299=EDGE_CURVE('',#36953,#36951,#33222,.T.);
#46300=EDGE_CURVE('',#36954,#36952,#33223,.T.);
#46301=EDGE_CURVE('',#36949,#36953,#33224,.T.);
#46302=EDGE_CURVE('',#36950,#36954,#33225,.T.);
#46303=EDGE_CURVE('',#36955,#36956,#4246,.T.);
#46304=EDGE_CURVE('',#36955,#36957,#33226,.T.);
#46305=EDGE_CURVE('',#36957,#36958,#4247,.T.);
#46306=EDGE_CURVE('',#36956,#36958,#33227,.T.);
#46307=EDGE_CURVE('',#36959,#36960,#4248,.T.);
#46308=EDGE_CURVE('',#36959,#36955,#33228,.T.);
#46309=EDGE_CURVE('',#36960,#36956,#33229,.T.);
#46310=EDGE_CURVE('',#36961,#36962,#4249,.T.);
#46311=EDGE_CURVE('',#36961,#36959,#33230,.T.);
#46312=EDGE_CURVE('',#36962,#36960,#33231,.T.);
#46313=EDGE_CURVE('',#36957,#36961,#33232,.T.);
#46314=EDGE_CURVE('',#36958,#36962,#33233,.T.);
#46315=EDGE_CURVE('',#36963,#36964,#4250,.T.);
#46316=EDGE_CURVE('',#36963,#36965,#33234,.T.);
#46317=EDGE_CURVE('',#36965,#36966,#4251,.T.);
#46318=EDGE_CURVE('',#36964,#36966,#33235,.T.);
#46319=EDGE_CURVE('',#36967,#36968,#4252,.T.);
#46320=EDGE_CURVE('',#36967,#36963,#33236,.T.);
#46321=EDGE_CURVE('',#36968,#36964,#33237,.T.);
#46322=EDGE_CURVE('',#36969,#36970,#4253,.T.);
#46323=EDGE_CURVE('',#36969,#36967,#33238,.T.);
#46324=EDGE_CURVE('',#36970,#36968,#33239,.T.);
#46325=EDGE_CURVE('',#36965,#36969,#33240,.T.);
#46326=EDGE_CURVE('',#36966,#36970,#33241,.T.);
#46327=EDGE_CURVE('',#36971,#36972,#4254,.T.);
#46328=EDGE_CURVE('',#36971,#36973,#33242,.T.);
#46329=EDGE_CURVE('',#36973,#36974,#4255,.T.);
#46330=EDGE_CURVE('',#36972,#36974,#33243,.T.);
#46331=EDGE_CURVE('',#36975,#36976,#4256,.T.);
#46332=EDGE_CURVE('',#36975,#36971,#33244,.T.);
#46333=EDGE_CURVE('',#36976,#36972,#33245,.T.);
#46334=EDGE_CURVE('',#36977,#36978,#4257,.T.);
#46335=EDGE_CURVE('',#36977,#36975,#33246,.T.);
#46336=EDGE_CURVE('',#36978,#36976,#33247,.T.);
#46337=EDGE_CURVE('',#36973,#36977,#33248,.T.);
#46338=EDGE_CURVE('',#36974,#36978,#33249,.T.);
#46339=EDGE_CURVE('',#36979,#36980,#4258,.T.);
#46340=EDGE_CURVE('',#36979,#36981,#33250,.T.);
#46341=EDGE_CURVE('',#36981,#36982,#4259,.T.);
#46342=EDGE_CURVE('',#36980,#36982,#33251,.T.);
#46343=EDGE_CURVE('',#36983,#36984,#4260,.T.);
#46344=EDGE_CURVE('',#36983,#36979,#33252,.T.);
#46345=EDGE_CURVE('',#36984,#36980,#33253,.T.);
#46346=EDGE_CURVE('',#36985,#36986,#4261,.T.);
#46347=EDGE_CURVE('',#36985,#36983,#33254,.T.);
#46348=EDGE_CURVE('',#36986,#36984,#33255,.T.);
#46349=EDGE_CURVE('',#36981,#36985,#33256,.T.);
#46350=EDGE_CURVE('',#36982,#36986,#33257,.T.);
#46351=EDGE_CURVE('',#36987,#36988,#4262,.T.);
#46352=EDGE_CURVE('',#36987,#36989,#33258,.T.);
#46353=EDGE_CURVE('',#36989,#36990,#4263,.T.);
#46354=EDGE_CURVE('',#36988,#36990,#33259,.T.);
#46355=EDGE_CURVE('',#36991,#36992,#4264,.T.);
#46356=EDGE_CURVE('',#36991,#36987,#33260,.T.);
#46357=EDGE_CURVE('',#36992,#36988,#33261,.T.);
#46358=EDGE_CURVE('',#36993,#36994,#4265,.T.);
#46359=EDGE_CURVE('',#36993,#36991,#33262,.T.);
#46360=EDGE_CURVE('',#36994,#36992,#33263,.T.);
#46361=EDGE_CURVE('',#36989,#36993,#33264,.T.);
#46362=EDGE_CURVE('',#36990,#36994,#33265,.T.);
#46363=EDGE_CURVE('',#36995,#36996,#4266,.T.);
#46364=EDGE_CURVE('',#36995,#36997,#33266,.T.);
#46365=EDGE_CURVE('',#36997,#36998,#4267,.T.);
#46366=EDGE_CURVE('',#36996,#36998,#33267,.T.);
#46367=EDGE_CURVE('',#36999,#37000,#4268,.T.);
#46368=EDGE_CURVE('',#36999,#36995,#33268,.T.);
#46369=EDGE_CURVE('',#37000,#36996,#33269,.T.);
#46370=EDGE_CURVE('',#37001,#37002,#4269,.T.);
#46371=EDGE_CURVE('',#37001,#36999,#33270,.T.);
#46372=EDGE_CURVE('',#37002,#37000,#33271,.T.);
#46373=EDGE_CURVE('',#36997,#37001,#33272,.T.);
#46374=EDGE_CURVE('',#36998,#37002,#33273,.T.);
#46375=EDGE_CURVE('',#37003,#37004,#4270,.T.);
#46376=EDGE_CURVE('',#37003,#37005,#33274,.T.);
#46377=EDGE_CURVE('',#37005,#37006,#4271,.T.);
#46378=EDGE_CURVE('',#37004,#37006,#33275,.T.);
#46379=EDGE_CURVE('',#37007,#37008,#4272,.T.);
#46380=EDGE_CURVE('',#37007,#37003,#33276,.T.);
#46381=EDGE_CURVE('',#37008,#37004,#33277,.T.);
#46382=EDGE_CURVE('',#37009,#37010,#4273,.T.);
#46383=EDGE_CURVE('',#37009,#37007,#33278,.T.);
#46384=EDGE_CURVE('',#37010,#37008,#33279,.T.);
#46385=EDGE_CURVE('',#37005,#37009,#33280,.T.);
#46386=EDGE_CURVE('',#37006,#37010,#33281,.T.);
#46387=EDGE_CURVE('',#37011,#37012,#4274,.T.);
#46388=EDGE_CURVE('',#37011,#37013,#33282,.T.);
#46389=EDGE_CURVE('',#37013,#37014,#4275,.T.);
#46390=EDGE_CURVE('',#37012,#37014,#33283,.T.);
#46391=EDGE_CURVE('',#37015,#37016,#4276,.T.);
#46392=EDGE_CURVE('',#37015,#37011,#33284,.T.);
#46393=EDGE_CURVE('',#37016,#37012,#33285,.T.);
#46394=EDGE_CURVE('',#37017,#37018,#4277,.T.);
#46395=EDGE_CURVE('',#37017,#37015,#33286,.T.);
#46396=EDGE_CURVE('',#37018,#37016,#33287,.T.);
#46397=EDGE_CURVE('',#37013,#37017,#33288,.T.);
#46398=EDGE_CURVE('',#37014,#37018,#33289,.T.);
#46399=EDGE_CURVE('',#37019,#37020,#4278,.T.);
#46400=EDGE_CURVE('',#37019,#37021,#33290,.T.);
#46401=EDGE_CURVE('',#37021,#37022,#4279,.T.);
#46402=EDGE_CURVE('',#37020,#37022,#33291,.T.);
#46403=EDGE_CURVE('',#37023,#37024,#4280,.T.);
#46404=EDGE_CURVE('',#37023,#37019,#33292,.T.);
#46405=EDGE_CURVE('',#37024,#37020,#33293,.T.);
#46406=EDGE_CURVE('',#37025,#37026,#4281,.T.);
#46407=EDGE_CURVE('',#37025,#37023,#33294,.T.);
#46408=EDGE_CURVE('',#37026,#37024,#33295,.T.);
#46409=EDGE_CURVE('',#37021,#37025,#33296,.T.);
#46410=EDGE_CURVE('',#37022,#37026,#33297,.T.);
#46411=EDGE_CURVE('',#37027,#37028,#4282,.T.);
#46412=EDGE_CURVE('',#37027,#37029,#33298,.T.);
#46413=EDGE_CURVE('',#37029,#37030,#4283,.T.);
#46414=EDGE_CURVE('',#37028,#37030,#33299,.T.);
#46415=EDGE_CURVE('',#37031,#37032,#4284,.T.);
#46416=EDGE_CURVE('',#37031,#37027,#33300,.T.);
#46417=EDGE_CURVE('',#37032,#37028,#33301,.T.);
#46418=EDGE_CURVE('',#37033,#37034,#4285,.T.);
#46419=EDGE_CURVE('',#37033,#37031,#33302,.T.);
#46420=EDGE_CURVE('',#37034,#37032,#33303,.T.);
#46421=EDGE_CURVE('',#37029,#37033,#33304,.T.);
#46422=EDGE_CURVE('',#37030,#37034,#33305,.T.);
#46423=EDGE_CURVE('',#37035,#37036,#4286,.T.);
#46424=EDGE_CURVE('',#37035,#37037,#33306,.T.);
#46425=EDGE_CURVE('',#37037,#37038,#4287,.T.);
#46426=EDGE_CURVE('',#37036,#37038,#33307,.T.);
#46427=EDGE_CURVE('',#37039,#37040,#4288,.T.);
#46428=EDGE_CURVE('',#37039,#37035,#33308,.T.);
#46429=EDGE_CURVE('',#37040,#37036,#33309,.T.);
#46430=EDGE_CURVE('',#37041,#37042,#4289,.T.);
#46431=EDGE_CURVE('',#37041,#37039,#33310,.T.);
#46432=EDGE_CURVE('',#37042,#37040,#33311,.T.);
#46433=EDGE_CURVE('',#37037,#37041,#33312,.T.);
#46434=EDGE_CURVE('',#37038,#37042,#33313,.T.);
#46435=EDGE_CURVE('',#37043,#37044,#4290,.T.);
#46436=EDGE_CURVE('',#37043,#37045,#33314,.T.);
#46437=EDGE_CURVE('',#37045,#37046,#4291,.T.);
#46438=EDGE_CURVE('',#37044,#37046,#33315,.T.);
#46439=EDGE_CURVE('',#37047,#37048,#4292,.T.);
#46440=EDGE_CURVE('',#37047,#37043,#33316,.T.);
#46441=EDGE_CURVE('',#37048,#37044,#33317,.T.);
#46442=EDGE_CURVE('',#37049,#37050,#4293,.T.);
#46443=EDGE_CURVE('',#37049,#37047,#33318,.T.);
#46444=EDGE_CURVE('',#37050,#37048,#33319,.T.);
#46445=EDGE_CURVE('',#37045,#37049,#33320,.T.);
#46446=EDGE_CURVE('',#37046,#37050,#33321,.T.);
#46447=EDGE_CURVE('',#37051,#37052,#4294,.T.);
#46448=EDGE_CURVE('',#37051,#37053,#33322,.T.);
#46449=EDGE_CURVE('',#37053,#37054,#4295,.T.);
#46450=EDGE_CURVE('',#37052,#37054,#33323,.T.);
#46451=EDGE_CURVE('',#37055,#37056,#4296,.T.);
#46452=EDGE_CURVE('',#37055,#37051,#33324,.T.);
#46453=EDGE_CURVE('',#37056,#37052,#33325,.T.);
#46454=EDGE_CURVE('',#37057,#37058,#4297,.T.);
#46455=EDGE_CURVE('',#37057,#37055,#33326,.T.);
#46456=EDGE_CURVE('',#37058,#37056,#33327,.T.);
#46457=EDGE_CURVE('',#37053,#37057,#33328,.T.);
#46458=EDGE_CURVE('',#37054,#37058,#33329,.T.);
#46459=EDGE_CURVE('',#37059,#37060,#4298,.T.);
#46460=EDGE_CURVE('',#37059,#37061,#33330,.T.);
#46461=EDGE_CURVE('',#37061,#37062,#4299,.T.);
#46462=EDGE_CURVE('',#37060,#37062,#33331,.T.);
#46463=EDGE_CURVE('',#37063,#37064,#4300,.T.);
#46464=EDGE_CURVE('',#37063,#37059,#33332,.T.);
#46465=EDGE_CURVE('',#37064,#37060,#33333,.T.);
#46466=EDGE_CURVE('',#37065,#37066,#4301,.T.);
#46467=EDGE_CURVE('',#37065,#37063,#33334,.T.);
#46468=EDGE_CURVE('',#37066,#37064,#33335,.T.);
#46469=EDGE_CURVE('',#37061,#37065,#33336,.T.);
#46470=EDGE_CURVE('',#37062,#37066,#33337,.T.);
#46471=EDGE_CURVE('',#37067,#37068,#4302,.T.);
#46472=EDGE_CURVE('',#37067,#37069,#33338,.T.);
#46473=EDGE_CURVE('',#37069,#37070,#4303,.T.);
#46474=EDGE_CURVE('',#37068,#37070,#33339,.T.);
#46475=EDGE_CURVE('',#37071,#37072,#4304,.T.);
#46476=EDGE_CURVE('',#37071,#37067,#33340,.T.);
#46477=EDGE_CURVE('',#37072,#37068,#33341,.T.);
#46478=EDGE_CURVE('',#37073,#37074,#4305,.T.);
#46479=EDGE_CURVE('',#37073,#37071,#33342,.T.);
#46480=EDGE_CURVE('',#37074,#37072,#33343,.T.);
#46481=EDGE_CURVE('',#37069,#37073,#33344,.T.);
#46482=EDGE_CURVE('',#37070,#37074,#33345,.T.);
#46483=EDGE_CURVE('',#37075,#37076,#4306,.T.);
#46484=EDGE_CURVE('',#37075,#37077,#33346,.T.);
#46485=EDGE_CURVE('',#37077,#37078,#4307,.T.);
#46486=EDGE_CURVE('',#37076,#37078,#33347,.T.);
#46487=EDGE_CURVE('',#37079,#37080,#4308,.T.);
#46488=EDGE_CURVE('',#37079,#37075,#33348,.T.);
#46489=EDGE_CURVE('',#37080,#37076,#33349,.T.);
#46490=EDGE_CURVE('',#37081,#37082,#4309,.T.);
#46491=EDGE_CURVE('',#37081,#37079,#33350,.T.);
#46492=EDGE_CURVE('',#37082,#37080,#33351,.T.);
#46493=EDGE_CURVE('',#37077,#37081,#33352,.T.);
#46494=EDGE_CURVE('',#37078,#37082,#33353,.T.);
#46495=EDGE_CURVE('',#37083,#37084,#4310,.T.);
#46496=EDGE_CURVE('',#37083,#37085,#33354,.T.);
#46497=EDGE_CURVE('',#37085,#37086,#4311,.T.);
#46498=EDGE_CURVE('',#37084,#37086,#33355,.T.);
#46499=EDGE_CURVE('',#37087,#37088,#4312,.T.);
#46500=EDGE_CURVE('',#37087,#37083,#33356,.T.);
#46501=EDGE_CURVE('',#37088,#37084,#33357,.T.);
#46502=EDGE_CURVE('',#37089,#37090,#4313,.T.);
#46503=EDGE_CURVE('',#37089,#37087,#33358,.T.);
#46504=EDGE_CURVE('',#37090,#37088,#33359,.T.);
#46505=EDGE_CURVE('',#37085,#37089,#33360,.T.);
#46506=EDGE_CURVE('',#37086,#37090,#33361,.T.);
#46507=EDGE_CURVE('',#37091,#37092,#4314,.T.);
#46508=EDGE_CURVE('',#37091,#37093,#33362,.T.);
#46509=EDGE_CURVE('',#37093,#37094,#4315,.T.);
#46510=EDGE_CURVE('',#37092,#37094,#33363,.T.);
#46511=EDGE_CURVE('',#37095,#37096,#4316,.T.);
#46512=EDGE_CURVE('',#37095,#37091,#33364,.T.);
#46513=EDGE_CURVE('',#37096,#37092,#33365,.T.);
#46514=EDGE_CURVE('',#37097,#37098,#4317,.T.);
#46515=EDGE_CURVE('',#37097,#37095,#33366,.T.);
#46516=EDGE_CURVE('',#37098,#37096,#33367,.T.);
#46517=EDGE_CURVE('',#37093,#37097,#33368,.T.);
#46518=EDGE_CURVE('',#37094,#37098,#33369,.T.);
#46519=EDGE_CURVE('',#37099,#37100,#4318,.T.);
#46520=EDGE_CURVE('',#37099,#37101,#33370,.T.);
#46521=EDGE_CURVE('',#37101,#37102,#4319,.T.);
#46522=EDGE_CURVE('',#37100,#37102,#33371,.T.);
#46523=EDGE_CURVE('',#37103,#37104,#4320,.T.);
#46524=EDGE_CURVE('',#37103,#37099,#33372,.T.);
#46525=EDGE_CURVE('',#37104,#37100,#33373,.T.);
#46526=EDGE_CURVE('',#37105,#37106,#4321,.T.);
#46527=EDGE_CURVE('',#37105,#37103,#33374,.T.);
#46528=EDGE_CURVE('',#37106,#37104,#33375,.T.);
#46529=EDGE_CURVE('',#37101,#37105,#33376,.T.);
#46530=EDGE_CURVE('',#37102,#37106,#33377,.T.);
#46531=EDGE_CURVE('',#37107,#37108,#4322,.T.);
#46532=EDGE_CURVE('',#37107,#37109,#33378,.T.);
#46533=EDGE_CURVE('',#37109,#37110,#4323,.T.);
#46534=EDGE_CURVE('',#37108,#37110,#33379,.T.);
#46535=EDGE_CURVE('',#37111,#37112,#4324,.T.);
#46536=EDGE_CURVE('',#37111,#37107,#33380,.T.);
#46537=EDGE_CURVE('',#37112,#37108,#33381,.T.);
#46538=EDGE_CURVE('',#37113,#37114,#4325,.T.);
#46539=EDGE_CURVE('',#37113,#37111,#33382,.T.);
#46540=EDGE_CURVE('',#37114,#37112,#33383,.T.);
#46541=EDGE_CURVE('',#37109,#37113,#33384,.T.);
#46542=EDGE_CURVE('',#37110,#37114,#33385,.T.);
#46543=EDGE_CURVE('',#37115,#37116,#4326,.T.);
#46544=EDGE_CURVE('',#37115,#37117,#33386,.T.);
#46545=EDGE_CURVE('',#37117,#37118,#4327,.T.);
#46546=EDGE_CURVE('',#37116,#37118,#33387,.T.);
#46547=EDGE_CURVE('',#37119,#37120,#4328,.T.);
#46548=EDGE_CURVE('',#37119,#37115,#33388,.T.);
#46549=EDGE_CURVE('',#37120,#37116,#33389,.T.);
#46550=EDGE_CURVE('',#37121,#37122,#4329,.T.);
#46551=EDGE_CURVE('',#37121,#37119,#33390,.T.);
#46552=EDGE_CURVE('',#37122,#37120,#33391,.T.);
#46553=EDGE_CURVE('',#37117,#37121,#33392,.T.);
#46554=EDGE_CURVE('',#37118,#37122,#33393,.T.);
#46555=EDGE_CURVE('',#37123,#37124,#4330,.T.);
#46556=EDGE_CURVE('',#37123,#37125,#33394,.T.);
#46557=EDGE_CURVE('',#37125,#37126,#4331,.T.);
#46558=EDGE_CURVE('',#37124,#37126,#33395,.T.);
#46559=EDGE_CURVE('',#37127,#37128,#4332,.T.);
#46560=EDGE_CURVE('',#37127,#37123,#33396,.T.);
#46561=EDGE_CURVE('',#37128,#37124,#33397,.T.);
#46562=EDGE_CURVE('',#37129,#37130,#4333,.T.);
#46563=EDGE_CURVE('',#37129,#37127,#33398,.T.);
#46564=EDGE_CURVE('',#37130,#37128,#33399,.T.);
#46565=EDGE_CURVE('',#37125,#37129,#33400,.T.);
#46566=EDGE_CURVE('',#37126,#37130,#33401,.T.);
#46567=EDGE_CURVE('',#37131,#37132,#4334,.T.);
#46568=EDGE_CURVE('',#37131,#37133,#33402,.T.);
#46569=EDGE_CURVE('',#37133,#37134,#4335,.T.);
#46570=EDGE_CURVE('',#37132,#37134,#33403,.T.);
#46571=EDGE_CURVE('',#37135,#37136,#4336,.T.);
#46572=EDGE_CURVE('',#37135,#37131,#33404,.T.);
#46573=EDGE_CURVE('',#37136,#37132,#33405,.T.);
#46574=EDGE_CURVE('',#37137,#37138,#4337,.T.);
#46575=EDGE_CURVE('',#37137,#37135,#33406,.T.);
#46576=EDGE_CURVE('',#37138,#37136,#33407,.T.);
#46577=EDGE_CURVE('',#37133,#37137,#33408,.T.);
#46578=EDGE_CURVE('',#37134,#37138,#33409,.T.);
#46579=EDGE_CURVE('',#37139,#37140,#4338,.T.);
#46580=EDGE_CURVE('',#37139,#37141,#33410,.T.);
#46581=EDGE_CURVE('',#37141,#37142,#4339,.T.);
#46582=EDGE_CURVE('',#37140,#37142,#33411,.T.);
#46583=EDGE_CURVE('',#37143,#37144,#4340,.T.);
#46584=EDGE_CURVE('',#37143,#37139,#33412,.T.);
#46585=EDGE_CURVE('',#37144,#37140,#33413,.T.);
#46586=EDGE_CURVE('',#37145,#37146,#4341,.T.);
#46587=EDGE_CURVE('',#37145,#37143,#33414,.T.);
#46588=EDGE_CURVE('',#37146,#37144,#33415,.T.);
#46589=EDGE_CURVE('',#37141,#37145,#33416,.T.);
#46590=EDGE_CURVE('',#37142,#37146,#33417,.T.);
#46591=EDGE_CURVE('',#37147,#37148,#4342,.T.);
#46592=EDGE_CURVE('',#37147,#37149,#33418,.T.);
#46593=EDGE_CURVE('',#37149,#37150,#4343,.T.);
#46594=EDGE_CURVE('',#37148,#37150,#33419,.T.);
#46595=EDGE_CURVE('',#37151,#37152,#4344,.T.);
#46596=EDGE_CURVE('',#37151,#37147,#33420,.T.);
#46597=EDGE_CURVE('',#37152,#37148,#33421,.T.);
#46598=EDGE_CURVE('',#37153,#37154,#4345,.T.);
#46599=EDGE_CURVE('',#37153,#37151,#33422,.T.);
#46600=EDGE_CURVE('',#37154,#37152,#33423,.T.);
#46601=EDGE_CURVE('',#37149,#37153,#33424,.T.);
#46602=EDGE_CURVE('',#37150,#37154,#33425,.T.);
#46603=EDGE_CURVE('',#37155,#37156,#4346,.T.);
#46604=EDGE_CURVE('',#37155,#37157,#33426,.T.);
#46605=EDGE_CURVE('',#37157,#37158,#4347,.T.);
#46606=EDGE_CURVE('',#37156,#37158,#33427,.T.);
#46607=EDGE_CURVE('',#37159,#37160,#4348,.T.);
#46608=EDGE_CURVE('',#37159,#37155,#33428,.T.);
#46609=EDGE_CURVE('',#37160,#37156,#33429,.T.);
#46610=EDGE_CURVE('',#37161,#37162,#4349,.T.);
#46611=EDGE_CURVE('',#37161,#37159,#33430,.T.);
#46612=EDGE_CURVE('',#37162,#37160,#33431,.T.);
#46613=EDGE_CURVE('',#37157,#37161,#33432,.T.);
#46614=EDGE_CURVE('',#37158,#37162,#33433,.T.);
#46615=EDGE_CURVE('',#37163,#37164,#4350,.T.);
#46616=EDGE_CURVE('',#37163,#37165,#33434,.T.);
#46617=EDGE_CURVE('',#37165,#37166,#4351,.T.);
#46618=EDGE_CURVE('',#37164,#37166,#33435,.T.);
#46619=EDGE_CURVE('',#37167,#37168,#4352,.T.);
#46620=EDGE_CURVE('',#37167,#37163,#33436,.T.);
#46621=EDGE_CURVE('',#37168,#37164,#33437,.T.);
#46622=EDGE_CURVE('',#37169,#37170,#4353,.T.);
#46623=EDGE_CURVE('',#37169,#37167,#33438,.T.);
#46624=EDGE_CURVE('',#37170,#37168,#33439,.T.);
#46625=EDGE_CURVE('',#37165,#37169,#33440,.T.);
#46626=EDGE_CURVE('',#37166,#37170,#33441,.T.);
#46627=EDGE_CURVE('',#37171,#37172,#4354,.T.);
#46628=EDGE_CURVE('',#37171,#37173,#33442,.T.);
#46629=EDGE_CURVE('',#37173,#37174,#4355,.T.);
#46630=EDGE_CURVE('',#37172,#37174,#33443,.T.);
#46631=EDGE_CURVE('',#37175,#37176,#4356,.T.);
#46632=EDGE_CURVE('',#37175,#37171,#33444,.T.);
#46633=EDGE_CURVE('',#37176,#37172,#33445,.T.);
#46634=EDGE_CURVE('',#37177,#37178,#4357,.T.);
#46635=EDGE_CURVE('',#37177,#37175,#33446,.T.);
#46636=EDGE_CURVE('',#37178,#37176,#33447,.T.);
#46637=EDGE_CURVE('',#37173,#37177,#33448,.T.);
#46638=EDGE_CURVE('',#37174,#37178,#33449,.T.);
#46639=EDGE_CURVE('',#37179,#37180,#4358,.T.);
#46640=EDGE_CURVE('',#37179,#37181,#33450,.T.);
#46641=EDGE_CURVE('',#37181,#37182,#4359,.T.);
#46642=EDGE_CURVE('',#37180,#37182,#33451,.T.);
#46643=EDGE_CURVE('',#37183,#37184,#4360,.T.);
#46644=EDGE_CURVE('',#37183,#37179,#33452,.T.);
#46645=EDGE_CURVE('',#37184,#37180,#33453,.T.);
#46646=EDGE_CURVE('',#37185,#37186,#4361,.T.);
#46647=EDGE_CURVE('',#37185,#37183,#33454,.T.);
#46648=EDGE_CURVE('',#37186,#37184,#33455,.T.);
#46649=EDGE_CURVE('',#37181,#37185,#33456,.T.);
#46650=EDGE_CURVE('',#37182,#37186,#33457,.T.);
#46651=EDGE_CURVE('',#37187,#37188,#4362,.T.);
#46652=EDGE_CURVE('',#37187,#37189,#33458,.T.);
#46653=EDGE_CURVE('',#37189,#37190,#4363,.T.);
#46654=EDGE_CURVE('',#37188,#37190,#33459,.T.);
#46655=EDGE_CURVE('',#37191,#37192,#4364,.T.);
#46656=EDGE_CURVE('',#37191,#37187,#33460,.T.);
#46657=EDGE_CURVE('',#37192,#37188,#33461,.T.);
#46658=EDGE_CURVE('',#37193,#37194,#4365,.T.);
#46659=EDGE_CURVE('',#37193,#37191,#33462,.T.);
#46660=EDGE_CURVE('',#37194,#37192,#33463,.T.);
#46661=EDGE_CURVE('',#37189,#37193,#33464,.T.);
#46662=EDGE_CURVE('',#37190,#37194,#33465,.T.);
#46663=EDGE_CURVE('',#37195,#37196,#4366,.T.);
#46664=EDGE_CURVE('',#37195,#37197,#33466,.T.);
#46665=EDGE_CURVE('',#37197,#37198,#4367,.T.);
#46666=EDGE_CURVE('',#37196,#37198,#33467,.T.);
#46667=EDGE_CURVE('',#37199,#37200,#4368,.T.);
#46668=EDGE_CURVE('',#37199,#37195,#33468,.T.);
#46669=EDGE_CURVE('',#37200,#37196,#33469,.T.);
#46670=EDGE_CURVE('',#37201,#37202,#4369,.T.);
#46671=EDGE_CURVE('',#37201,#37199,#33470,.T.);
#46672=EDGE_CURVE('',#37202,#37200,#33471,.T.);
#46673=EDGE_CURVE('',#37197,#37201,#33472,.T.);
#46674=EDGE_CURVE('',#37198,#37202,#33473,.T.);
#46675=EDGE_CURVE('',#37203,#37204,#4370,.T.);
#46676=EDGE_CURVE('',#37203,#37205,#33474,.T.);
#46677=EDGE_CURVE('',#37205,#37206,#4371,.T.);
#46678=EDGE_CURVE('',#37204,#37206,#33475,.T.);
#46679=EDGE_CURVE('',#37207,#37208,#4372,.T.);
#46680=EDGE_CURVE('',#37207,#37203,#33476,.T.);
#46681=EDGE_CURVE('',#37208,#37204,#33477,.T.);
#46682=EDGE_CURVE('',#37209,#37210,#4373,.T.);
#46683=EDGE_CURVE('',#37209,#37207,#33478,.T.);
#46684=EDGE_CURVE('',#37210,#37208,#33479,.T.);
#46685=EDGE_CURVE('',#37205,#37209,#33480,.T.);
#46686=EDGE_CURVE('',#37206,#37210,#33481,.T.);
#46687=EDGE_CURVE('',#37211,#37212,#4374,.T.);
#46688=EDGE_CURVE('',#37211,#37213,#33482,.T.);
#46689=EDGE_CURVE('',#37213,#37214,#4375,.T.);
#46690=EDGE_CURVE('',#37212,#37214,#33483,.T.);
#46691=EDGE_CURVE('',#37215,#37216,#4376,.T.);
#46692=EDGE_CURVE('',#37215,#37211,#33484,.T.);
#46693=EDGE_CURVE('',#37216,#37212,#33485,.T.);
#46694=EDGE_CURVE('',#37217,#37218,#4377,.T.);
#46695=EDGE_CURVE('',#37217,#37215,#33486,.T.);
#46696=EDGE_CURVE('',#37218,#37216,#33487,.T.);
#46697=EDGE_CURVE('',#37213,#37217,#33488,.T.);
#46698=EDGE_CURVE('',#37214,#37218,#33489,.T.);
#46699=EDGE_CURVE('',#37219,#37220,#4378,.T.);
#46700=EDGE_CURVE('',#37219,#37221,#33490,.T.);
#46701=EDGE_CURVE('',#37221,#37222,#4379,.T.);
#46702=EDGE_CURVE('',#37220,#37222,#33491,.T.);
#46703=EDGE_CURVE('',#37223,#37224,#4380,.T.);
#46704=EDGE_CURVE('',#37223,#37219,#33492,.T.);
#46705=EDGE_CURVE('',#37224,#37220,#33493,.T.);
#46706=EDGE_CURVE('',#37225,#37226,#4381,.T.);
#46707=EDGE_CURVE('',#37225,#37223,#33494,.T.);
#46708=EDGE_CURVE('',#37226,#37224,#33495,.T.);
#46709=EDGE_CURVE('',#37221,#37225,#33496,.T.);
#46710=EDGE_CURVE('',#37222,#37226,#33497,.T.);
#46711=EDGE_CURVE('',#37227,#37228,#4382,.T.);
#46712=EDGE_CURVE('',#37227,#37229,#33498,.T.);
#46713=EDGE_CURVE('',#37229,#37230,#4383,.T.);
#46714=EDGE_CURVE('',#37228,#37230,#33499,.T.);
#46715=EDGE_CURVE('',#37231,#37232,#4384,.T.);
#46716=EDGE_CURVE('',#37231,#37227,#33500,.T.);
#46717=EDGE_CURVE('',#37232,#37228,#33501,.T.);
#46718=EDGE_CURVE('',#37233,#37234,#4385,.T.);
#46719=EDGE_CURVE('',#37233,#37231,#33502,.T.);
#46720=EDGE_CURVE('',#37234,#37232,#33503,.T.);
#46721=EDGE_CURVE('',#37229,#37233,#33504,.T.);
#46722=EDGE_CURVE('',#37230,#37234,#33505,.T.);
#46723=EDGE_CURVE('',#37235,#37236,#4386,.T.);
#46724=EDGE_CURVE('',#37235,#37237,#33506,.T.);
#46725=EDGE_CURVE('',#37237,#37238,#4387,.T.);
#46726=EDGE_CURVE('',#37236,#37238,#33507,.T.);
#46727=EDGE_CURVE('',#37239,#37240,#4388,.T.);
#46728=EDGE_CURVE('',#37239,#37235,#33508,.T.);
#46729=EDGE_CURVE('',#37240,#37236,#33509,.T.);
#46730=EDGE_CURVE('',#37241,#37242,#4389,.T.);
#46731=EDGE_CURVE('',#37241,#37239,#33510,.T.);
#46732=EDGE_CURVE('',#37242,#37240,#33511,.T.);
#46733=EDGE_CURVE('',#37237,#37241,#33512,.T.);
#46734=EDGE_CURVE('',#37238,#37242,#33513,.T.);
#46735=EDGE_CURVE('',#37243,#37244,#4390,.T.);
#46736=EDGE_CURVE('',#37245,#37244,#4391,.T.);
#46737=EDGE_CURVE('',#37246,#37245,#4392,.T.);
#46738=EDGE_CURVE('',#37246,#37243,#4393,.T.);
#46739=EDGE_CURVE('',#37247,#37248,#4394,.T.);
#46740=EDGE_CURVE('',#37244,#37248,#4395,.T.);
#46741=EDGE_CURVE('',#37243,#37247,#4396,.T.);
#46742=EDGE_CURVE('',#37249,#37250,#4397,.T.);
#46743=EDGE_CURVE('',#37248,#37250,#4398,.T.);
#46744=EDGE_CURVE('',#37247,#37249,#4399,.T.);
#46745=EDGE_CURVE('',#37250,#37245,#4400,.T.);
#46746=EDGE_CURVE('',#37249,#37246,#4401,.T.);
#46747=EDGE_CURVE('',#37251,#37252,#4402,.T.);
#46748=EDGE_CURVE('',#37253,#37252,#4403,.T.);
#46749=EDGE_CURVE('',#37254,#37253,#4404,.T.);
#46750=EDGE_CURVE('',#37254,#37251,#4405,.T.);
#46751=EDGE_CURVE('',#37255,#37256,#4406,.T.);
#46752=EDGE_CURVE('',#37252,#37256,#4407,.T.);
#46753=EDGE_CURVE('',#37251,#37255,#4408,.T.);
#46754=EDGE_CURVE('',#37257,#37258,#4409,.T.);
#46755=EDGE_CURVE('',#37256,#37258,#4410,.T.);
#46756=EDGE_CURVE('',#37255,#37257,#4411,.T.);
#46757=EDGE_CURVE('',#37258,#37253,#4412,.T.);
#46758=EDGE_CURVE('',#37257,#37254,#4413,.T.);
#46759=EDGE_CURVE('',#37259,#37260,#4414,.T.);
#46760=EDGE_CURVE('',#37261,#37260,#4415,.T.);
#46761=EDGE_CURVE('',#37262,#37261,#4416,.T.);
#46762=EDGE_CURVE('',#37262,#37259,#4417,.T.);
#46763=EDGE_CURVE('',#37263,#37264,#4418,.T.);
#46764=EDGE_CURVE('',#37260,#37264,#4419,.T.);
#46765=EDGE_CURVE('',#37259,#37263,#4420,.T.);
#46766=EDGE_CURVE('',#37265,#37266,#4421,.T.);
#46767=EDGE_CURVE('',#37264,#37266,#4422,.T.);
#46768=EDGE_CURVE('',#37263,#37265,#4423,.T.);
#46769=EDGE_CURVE('',#37266,#37261,#4424,.T.);
#46770=EDGE_CURVE('',#37265,#37262,#4425,.T.);
#46771=EDGE_CURVE('',#37267,#37268,#4426,.T.);
#46772=EDGE_CURVE('',#37269,#37268,#4427,.T.);
#46773=EDGE_CURVE('',#37270,#37269,#4428,.T.);
#46774=EDGE_CURVE('',#37270,#37267,#4429,.T.);
#46775=EDGE_CURVE('',#37271,#37272,#4430,.T.);
#46776=EDGE_CURVE('',#37268,#37272,#4431,.T.);
#46777=EDGE_CURVE('',#37267,#37271,#4432,.T.);
#46778=EDGE_CURVE('',#37273,#37274,#4433,.T.);
#46779=EDGE_CURVE('',#37272,#37274,#4434,.T.);
#46780=EDGE_CURVE('',#37271,#37273,#4435,.T.);
#46781=EDGE_CURVE('',#37274,#37269,#4436,.T.);
#46782=EDGE_CURVE('',#37273,#37270,#4437,.T.);
#46783=EDGE_CURVE('',#37275,#37276,#4438,.T.);
#46784=EDGE_CURVE('',#37277,#37276,#4439,.T.);
#46785=EDGE_CURVE('',#37278,#37277,#4440,.T.);
#46786=EDGE_CURVE('',#37278,#37275,#4441,.T.);
#46787=EDGE_CURVE('',#37279,#37280,#4442,.T.);
#46788=EDGE_CURVE('',#37276,#37280,#4443,.T.);
#46789=EDGE_CURVE('',#37275,#37279,#4444,.T.);
#46790=EDGE_CURVE('',#37281,#37282,#4445,.T.);
#46791=EDGE_CURVE('',#37280,#37282,#4446,.T.);
#46792=EDGE_CURVE('',#37279,#37281,#4447,.T.);
#46793=EDGE_CURVE('',#37282,#37277,#4448,.T.);
#46794=EDGE_CURVE('',#37281,#37278,#4449,.T.);
#46795=EDGE_CURVE('',#37283,#37284,#4450,.T.);
#46796=EDGE_CURVE('',#37285,#37284,#4451,.T.);
#46797=EDGE_CURVE('',#37286,#37285,#4452,.T.);
#46798=EDGE_CURVE('',#37286,#37283,#4453,.T.);
#46799=EDGE_CURVE('',#37287,#37288,#4454,.T.);
#46800=EDGE_CURVE('',#37284,#37288,#4455,.T.);
#46801=EDGE_CURVE('',#37283,#37287,#4456,.T.);
#46802=EDGE_CURVE('',#37289,#37290,#4457,.T.);
#46803=EDGE_CURVE('',#37288,#37290,#4458,.T.);
#46804=EDGE_CURVE('',#37287,#37289,#4459,.T.);
#46805=EDGE_CURVE('',#37290,#37285,#4460,.T.);
#46806=EDGE_CURVE('',#37289,#37286,#4461,.T.);
#46807=EDGE_CURVE('',#37291,#37292,#4462,.T.);
#46808=EDGE_CURVE('',#37293,#37292,#4463,.T.);
#46809=EDGE_CURVE('',#37294,#37293,#4464,.T.);
#46810=EDGE_CURVE('',#37294,#37291,#4465,.T.);
#46811=EDGE_CURVE('',#37295,#37296,#4466,.T.);
#46812=EDGE_CURVE('',#37292,#37296,#4467,.T.);
#46813=EDGE_CURVE('',#37291,#37295,#4468,.T.);
#46814=EDGE_CURVE('',#37297,#37298,#4469,.T.);
#46815=EDGE_CURVE('',#37296,#37298,#4470,.T.);
#46816=EDGE_CURVE('',#37295,#37297,#4471,.T.);
#46817=EDGE_CURVE('',#37298,#37293,#4472,.T.);
#46818=EDGE_CURVE('',#37297,#37294,#4473,.T.);
#46819=EDGE_CURVE('',#37299,#37300,#4474,.T.);
#46820=EDGE_CURVE('',#37301,#37300,#4475,.T.);
#46821=EDGE_CURVE('',#37302,#37301,#4476,.T.);
#46822=EDGE_CURVE('',#37302,#37299,#4477,.T.);
#46823=EDGE_CURVE('',#37303,#37304,#4478,.T.);
#46824=EDGE_CURVE('',#37300,#37304,#4479,.T.);
#46825=EDGE_CURVE('',#37299,#37303,#4480,.T.);
#46826=EDGE_CURVE('',#37305,#37306,#4481,.T.);
#46827=EDGE_CURVE('',#37304,#37306,#4482,.T.);
#46828=EDGE_CURVE('',#37303,#37305,#4483,.T.);
#46829=EDGE_CURVE('',#37306,#37301,#4484,.T.);
#46830=EDGE_CURVE('',#37305,#37302,#4485,.T.);
#46831=EDGE_CURVE('',#37307,#37308,#4486,.T.);
#46832=EDGE_CURVE('',#37309,#37308,#4487,.T.);
#46833=EDGE_CURVE('',#37310,#37309,#4488,.T.);
#46834=EDGE_CURVE('',#37310,#37307,#4489,.T.);
#46835=EDGE_CURVE('',#37311,#37312,#4490,.T.);
#46836=EDGE_CURVE('',#37308,#37312,#4491,.T.);
#46837=EDGE_CURVE('',#37307,#37311,#4492,.T.);
#46838=EDGE_CURVE('',#37313,#37314,#4493,.T.);
#46839=EDGE_CURVE('',#37312,#37314,#4494,.T.);
#46840=EDGE_CURVE('',#37311,#37313,#4495,.T.);
#46841=EDGE_CURVE('',#37314,#37309,#4496,.T.);
#46842=EDGE_CURVE('',#37313,#37310,#4497,.T.);
#46843=EDGE_CURVE('',#37315,#37316,#4498,.T.);
#46844=EDGE_CURVE('',#37317,#37316,#4499,.T.);
#46845=EDGE_CURVE('',#37318,#37317,#4500,.T.);
#46846=EDGE_CURVE('',#37318,#37315,#4501,.T.);
#46847=EDGE_CURVE('',#37319,#37320,#4502,.T.);
#46848=EDGE_CURVE('',#37316,#37320,#4503,.T.);
#46849=EDGE_CURVE('',#37315,#37319,#4504,.T.);
#46850=EDGE_CURVE('',#37321,#37322,#4505,.T.);
#46851=EDGE_CURVE('',#37320,#37322,#4506,.T.);
#46852=EDGE_CURVE('',#37319,#37321,#4507,.T.);
#46853=EDGE_CURVE('',#37322,#37317,#4508,.T.);
#46854=EDGE_CURVE('',#37321,#37318,#4509,.T.);
#46855=EDGE_CURVE('',#37323,#37324,#4510,.T.);
#46856=EDGE_CURVE('',#37325,#37324,#4511,.T.);
#46857=EDGE_CURVE('',#37326,#37325,#4512,.T.);
#46858=EDGE_CURVE('',#37326,#37323,#4513,.T.);
#46859=EDGE_CURVE('',#37327,#37328,#4514,.T.);
#46860=EDGE_CURVE('',#37324,#37328,#4515,.T.);
#46861=EDGE_CURVE('',#37323,#37327,#4516,.T.);
#46862=EDGE_CURVE('',#37329,#37330,#4517,.T.);
#46863=EDGE_CURVE('',#37328,#37330,#4518,.T.);
#46864=EDGE_CURVE('',#37327,#37329,#4519,.T.);
#46865=EDGE_CURVE('',#37330,#37325,#4520,.T.);
#46866=EDGE_CURVE('',#37329,#37326,#4521,.T.);
#46867=EDGE_CURVE('',#37331,#37332,#4522,.T.);
#46868=EDGE_CURVE('',#37333,#37332,#4523,.T.);
#46869=EDGE_CURVE('',#37334,#37333,#4524,.T.);
#46870=EDGE_CURVE('',#37334,#37331,#4525,.T.);
#46871=EDGE_CURVE('',#37335,#37336,#4526,.T.);
#46872=EDGE_CURVE('',#37332,#37336,#4527,.T.);
#46873=EDGE_CURVE('',#37331,#37335,#4528,.T.);
#46874=EDGE_CURVE('',#37337,#37338,#4529,.T.);
#46875=EDGE_CURVE('',#37336,#37338,#4530,.T.);
#46876=EDGE_CURVE('',#37335,#37337,#4531,.T.);
#46877=EDGE_CURVE('',#37338,#37333,#4532,.T.);
#46878=EDGE_CURVE('',#37337,#37334,#4533,.T.);
#46879=EDGE_CURVE('',#37339,#37340,#4534,.T.);
#46880=EDGE_CURVE('',#37341,#37340,#4535,.T.);
#46881=EDGE_CURVE('',#37342,#37341,#4536,.T.);
#46882=EDGE_CURVE('',#37342,#37339,#4537,.T.);
#46883=EDGE_CURVE('',#37343,#37344,#4538,.T.);
#46884=EDGE_CURVE('',#37340,#37344,#4539,.T.);
#46885=EDGE_CURVE('',#37339,#37343,#4540,.T.);
#46886=EDGE_CURVE('',#37345,#37346,#4541,.T.);
#46887=EDGE_CURVE('',#37344,#37346,#4542,.T.);
#46888=EDGE_CURVE('',#37343,#37345,#4543,.T.);
#46889=EDGE_CURVE('',#37346,#37341,#4544,.T.);
#46890=EDGE_CURVE('',#37345,#37342,#4545,.T.);
#46891=EDGE_CURVE('',#37347,#37348,#4546,.T.);
#46892=EDGE_CURVE('',#37349,#37348,#4547,.T.);
#46893=EDGE_CURVE('',#37350,#37349,#4548,.T.);
#46894=EDGE_CURVE('',#37350,#37347,#4549,.T.);
#46895=EDGE_CURVE('',#37351,#37352,#4550,.T.);
#46896=EDGE_CURVE('',#37348,#37352,#4551,.T.);
#46897=EDGE_CURVE('',#37347,#37351,#4552,.T.);
#46898=EDGE_CURVE('',#37353,#37354,#4553,.T.);
#46899=EDGE_CURVE('',#37352,#37354,#4554,.T.);
#46900=EDGE_CURVE('',#37351,#37353,#4555,.T.);
#46901=EDGE_CURVE('',#37354,#37349,#4556,.T.);
#46902=EDGE_CURVE('',#37353,#37350,#4557,.T.);
#46903=EDGE_CURVE('',#37355,#37356,#4558,.T.);
#46904=EDGE_CURVE('',#37357,#37356,#4559,.T.);
#46905=EDGE_CURVE('',#37358,#37357,#4560,.T.);
#46906=EDGE_CURVE('',#37358,#37355,#4561,.T.);
#46907=EDGE_CURVE('',#37359,#37360,#4562,.T.);
#46908=EDGE_CURVE('',#37356,#37360,#4563,.T.);
#46909=EDGE_CURVE('',#37355,#37359,#4564,.T.);
#46910=EDGE_CURVE('',#37361,#37362,#4565,.T.);
#46911=EDGE_CURVE('',#37360,#37362,#4566,.T.);
#46912=EDGE_CURVE('',#37359,#37361,#4567,.T.);
#46913=EDGE_CURVE('',#37362,#37357,#4568,.T.);
#46914=EDGE_CURVE('',#37361,#37358,#4569,.T.);
#46915=EDGE_CURVE('',#37363,#37364,#4570,.T.);
#46916=EDGE_CURVE('',#37365,#37364,#4571,.T.);
#46917=EDGE_CURVE('',#37366,#37365,#4572,.T.);
#46918=EDGE_CURVE('',#37366,#37363,#4573,.T.);
#46919=EDGE_CURVE('',#37367,#37368,#4574,.T.);
#46920=EDGE_CURVE('',#37364,#37368,#4575,.T.);
#46921=EDGE_CURVE('',#37363,#37367,#4576,.T.);
#46922=EDGE_CURVE('',#37369,#37370,#4577,.T.);
#46923=EDGE_CURVE('',#37368,#37370,#4578,.T.);
#46924=EDGE_CURVE('',#37367,#37369,#4579,.T.);
#46925=EDGE_CURVE('',#37370,#37365,#4580,.T.);
#46926=EDGE_CURVE('',#37369,#37366,#4581,.T.);
#46927=EDGE_CURVE('',#37371,#37372,#4582,.T.);
#46928=EDGE_CURVE('',#37373,#37372,#4583,.T.);
#46929=EDGE_CURVE('',#37374,#37373,#4584,.T.);
#46930=EDGE_CURVE('',#37374,#37371,#4585,.T.);
#46931=EDGE_CURVE('',#37375,#37376,#4586,.T.);
#46932=EDGE_CURVE('',#37372,#37376,#4587,.T.);
#46933=EDGE_CURVE('',#37371,#37375,#4588,.T.);
#46934=EDGE_CURVE('',#37377,#37378,#4589,.T.);
#46935=EDGE_CURVE('',#37376,#37378,#4590,.T.);
#46936=EDGE_CURVE('',#37375,#37377,#4591,.T.);
#46937=EDGE_CURVE('',#37378,#37373,#4592,.T.);
#46938=EDGE_CURVE('',#37377,#37374,#4593,.T.);
#46939=EDGE_CURVE('',#37379,#37380,#4594,.T.);
#46940=EDGE_CURVE('',#37381,#37380,#4595,.T.);
#46941=EDGE_CURVE('',#37382,#37381,#4596,.T.);
#46942=EDGE_CURVE('',#37382,#37379,#4597,.T.);
#46943=EDGE_CURVE('',#37383,#37384,#4598,.T.);
#46944=EDGE_CURVE('',#37380,#37384,#4599,.T.);
#46945=EDGE_CURVE('',#37379,#37383,#4600,.T.);
#46946=EDGE_CURVE('',#37385,#37386,#4601,.T.);
#46947=EDGE_CURVE('',#37384,#37386,#4602,.T.);
#46948=EDGE_CURVE('',#37383,#37385,#4603,.T.);
#46949=EDGE_CURVE('',#37386,#37381,#4604,.T.);
#46950=EDGE_CURVE('',#37385,#37382,#4605,.T.);
#46951=EDGE_CURVE('',#37387,#37388,#4606,.T.);
#46952=EDGE_CURVE('',#37389,#37388,#4607,.T.);
#46953=EDGE_CURVE('',#37390,#37389,#4608,.T.);
#46954=EDGE_CURVE('',#37390,#37387,#4609,.T.);
#46955=EDGE_CURVE('',#37391,#37392,#4610,.T.);
#46956=EDGE_CURVE('',#37388,#37392,#4611,.T.);
#46957=EDGE_CURVE('',#37387,#37391,#4612,.T.);
#46958=EDGE_CURVE('',#37393,#37394,#4613,.T.);
#46959=EDGE_CURVE('',#37392,#37394,#4614,.T.);
#46960=EDGE_CURVE('',#37391,#37393,#4615,.T.);
#46961=EDGE_CURVE('',#37394,#37389,#4616,.T.);
#46962=EDGE_CURVE('',#37393,#37390,#4617,.T.);
#46963=EDGE_CURVE('',#37395,#37396,#4618,.T.);
#46964=EDGE_CURVE('',#37397,#37396,#4619,.T.);
#46965=EDGE_CURVE('',#37398,#37397,#4620,.T.);
#46966=EDGE_CURVE('',#37398,#37395,#4621,.T.);
#46967=EDGE_CURVE('',#37399,#37400,#4622,.T.);
#46968=EDGE_CURVE('',#37396,#37400,#4623,.T.);
#46969=EDGE_CURVE('',#37395,#37399,#4624,.T.);
#46970=EDGE_CURVE('',#37401,#37402,#4625,.T.);
#46971=EDGE_CURVE('',#37400,#37402,#4626,.T.);
#46972=EDGE_CURVE('',#37399,#37401,#4627,.T.);
#46973=EDGE_CURVE('',#37402,#37397,#4628,.T.);
#46974=EDGE_CURVE('',#37401,#37398,#4629,.T.);
#46975=EDGE_CURVE('',#37403,#37404,#4630,.T.);
#46976=EDGE_CURVE('',#37405,#37404,#4631,.T.);
#46977=EDGE_CURVE('',#37406,#37405,#4632,.T.);
#46978=EDGE_CURVE('',#37406,#37403,#4633,.T.);
#46979=EDGE_CURVE('',#37407,#37408,#4634,.T.);
#46980=EDGE_CURVE('',#37404,#37408,#4635,.T.);
#46981=EDGE_CURVE('',#37403,#37407,#4636,.T.);
#46982=EDGE_CURVE('',#37409,#37410,#4637,.T.);
#46983=EDGE_CURVE('',#37408,#37410,#4638,.T.);
#46984=EDGE_CURVE('',#37407,#37409,#4639,.T.);
#46985=EDGE_CURVE('',#37410,#37405,#4640,.T.);
#46986=EDGE_CURVE('',#37409,#37406,#4641,.T.);
#46987=EDGE_CURVE('',#37411,#37412,#4642,.T.);
#46988=EDGE_CURVE('',#37413,#37412,#4643,.T.);
#46989=EDGE_CURVE('',#37414,#37413,#4644,.T.);
#46990=EDGE_CURVE('',#37414,#37411,#4645,.T.);
#46991=EDGE_CURVE('',#37415,#37416,#4646,.T.);
#46992=EDGE_CURVE('',#37412,#37416,#4647,.T.);
#46993=EDGE_CURVE('',#37411,#37415,#4648,.T.);
#46994=EDGE_CURVE('',#37417,#37418,#4649,.T.);
#46995=EDGE_CURVE('',#37416,#37418,#4650,.T.);
#46996=EDGE_CURVE('',#37415,#37417,#4651,.T.);
#46997=EDGE_CURVE('',#37418,#37413,#4652,.T.);
#46998=EDGE_CURVE('',#37417,#37414,#4653,.T.);
#46999=EDGE_CURVE('',#37419,#37420,#4654,.T.);
#47000=EDGE_CURVE('',#37421,#37420,#4655,.T.);
#47001=EDGE_CURVE('',#37422,#37421,#4656,.T.);
#47002=EDGE_CURVE('',#37422,#37419,#4657,.T.);
#47003=EDGE_CURVE('',#37423,#37424,#4658,.T.);
#47004=EDGE_CURVE('',#37420,#37424,#4659,.T.);
#47005=EDGE_CURVE('',#37419,#37423,#4660,.T.);
#47006=EDGE_CURVE('',#37425,#37426,#4661,.T.);
#47007=EDGE_CURVE('',#37424,#37426,#4662,.T.);
#47008=EDGE_CURVE('',#37423,#37425,#4663,.T.);
#47009=EDGE_CURVE('',#37426,#37421,#4664,.T.);
#47010=EDGE_CURVE('',#37425,#37422,#4665,.T.);
#47011=EDGE_CURVE('',#37427,#37428,#4666,.T.);
#47012=EDGE_CURVE('',#37429,#37428,#4667,.T.);
#47013=EDGE_CURVE('',#37430,#37429,#4668,.T.);
#47014=EDGE_CURVE('',#37430,#37427,#4669,.T.);
#47015=EDGE_CURVE('',#37431,#37432,#4670,.T.);
#47016=EDGE_CURVE('',#37428,#37432,#4671,.T.);
#47017=EDGE_CURVE('',#37427,#37431,#4672,.T.);
#47018=EDGE_CURVE('',#37433,#37434,#4673,.T.);
#47019=EDGE_CURVE('',#37432,#37434,#4674,.T.);
#47020=EDGE_CURVE('',#37431,#37433,#4675,.T.);
#47021=EDGE_CURVE('',#37434,#37429,#4676,.T.);
#47022=EDGE_CURVE('',#37433,#37430,#4677,.T.);
#47023=EDGE_CURVE('',#37435,#37436,#4678,.T.);
#47024=EDGE_CURVE('',#37437,#37436,#4679,.T.);
#47025=EDGE_CURVE('',#37438,#37437,#4680,.T.);
#47026=EDGE_CURVE('',#37438,#37435,#4681,.T.);
#47027=EDGE_CURVE('',#37439,#37440,#4682,.T.);
#47028=EDGE_CURVE('',#37436,#37440,#4683,.T.);
#47029=EDGE_CURVE('',#37435,#37439,#4684,.T.);
#47030=EDGE_CURVE('',#37441,#37442,#4685,.T.);
#47031=EDGE_CURVE('',#37440,#37442,#4686,.T.);
#47032=EDGE_CURVE('',#37439,#37441,#4687,.T.);
#47033=EDGE_CURVE('',#37442,#37437,#4688,.T.);
#47034=EDGE_CURVE('',#37441,#37438,#4689,.T.);
#47035=EDGE_CURVE('',#37443,#37444,#4690,.T.);
#47036=EDGE_CURVE('',#37445,#37444,#4691,.T.);
#47037=EDGE_CURVE('',#37446,#37445,#4692,.T.);
#47038=EDGE_CURVE('',#37446,#37443,#4693,.T.);
#47039=EDGE_CURVE('',#37447,#37448,#4694,.T.);
#47040=EDGE_CURVE('',#37444,#37448,#4695,.T.);
#47041=EDGE_CURVE('',#37443,#37447,#4696,.T.);
#47042=EDGE_CURVE('',#37449,#37450,#4697,.T.);
#47043=EDGE_CURVE('',#37448,#37450,#4698,.T.);
#47044=EDGE_CURVE('',#37447,#37449,#4699,.T.);
#47045=EDGE_CURVE('',#37450,#37445,#4700,.T.);
#47046=EDGE_CURVE('',#37449,#37446,#4701,.T.);
#47047=EDGE_CURVE('',#37451,#37452,#4702,.T.);
#47048=EDGE_CURVE('',#37453,#37452,#4703,.T.);
#47049=EDGE_CURVE('',#37454,#37453,#4704,.T.);
#47050=EDGE_CURVE('',#37454,#37451,#4705,.T.);
#47051=EDGE_CURVE('',#37455,#37456,#4706,.T.);
#47052=EDGE_CURVE('',#37452,#37456,#4707,.T.);
#47053=EDGE_CURVE('',#37451,#37455,#4708,.T.);
#47054=EDGE_CURVE('',#37457,#37458,#4709,.T.);
#47055=EDGE_CURVE('',#37456,#37458,#4710,.T.);
#47056=EDGE_CURVE('',#37455,#37457,#4711,.T.);
#47057=EDGE_CURVE('',#37458,#37453,#4712,.T.);
#47058=EDGE_CURVE('',#37457,#37454,#4713,.T.);
#47059=EDGE_CURVE('',#37459,#37460,#4714,.T.);
#47060=EDGE_CURVE('',#37461,#37460,#4715,.T.);
#47061=EDGE_CURVE('',#37462,#37461,#4716,.T.);
#47062=EDGE_CURVE('',#37462,#37459,#4717,.T.);
#47063=EDGE_CURVE('',#37463,#37464,#4718,.T.);
#47064=EDGE_CURVE('',#37460,#37464,#4719,.T.);
#47065=EDGE_CURVE('',#37459,#37463,#4720,.T.);
#47066=EDGE_CURVE('',#37465,#37466,#4721,.T.);
#47067=EDGE_CURVE('',#37464,#37466,#4722,.T.);
#47068=EDGE_CURVE('',#37463,#37465,#4723,.T.);
#47069=EDGE_CURVE('',#37466,#37461,#4724,.T.);
#47070=EDGE_CURVE('',#37465,#37462,#4725,.T.);
#47071=EDGE_CURVE('',#37467,#37468,#4726,.T.);
#47072=EDGE_CURVE('',#37469,#37468,#4727,.T.);
#47073=EDGE_CURVE('',#37470,#37469,#4728,.T.);
#47074=EDGE_CURVE('',#37470,#37467,#4729,.T.);
#47075=EDGE_CURVE('',#37471,#37472,#4730,.T.);
#47076=EDGE_CURVE('',#37468,#37472,#4731,.T.);
#47077=EDGE_CURVE('',#37467,#37471,#4732,.T.);
#47078=EDGE_CURVE('',#37473,#37474,#4733,.T.);
#47079=EDGE_CURVE('',#37472,#37474,#4734,.T.);
#47080=EDGE_CURVE('',#37471,#37473,#4735,.T.);
#47081=EDGE_CURVE('',#37474,#37469,#4736,.T.);
#47082=EDGE_CURVE('',#37473,#37470,#4737,.T.);
#47083=EDGE_CURVE('',#37475,#37476,#4738,.T.);
#47084=EDGE_CURVE('',#37477,#37476,#4739,.T.);
#47085=EDGE_CURVE('',#37478,#37477,#4740,.T.);
#47086=EDGE_CURVE('',#37478,#37475,#4741,.T.);
#47087=EDGE_CURVE('',#37479,#37480,#4742,.T.);
#47088=EDGE_CURVE('',#37476,#37480,#4743,.T.);
#47089=EDGE_CURVE('',#37475,#37479,#4744,.T.);
#47090=EDGE_CURVE('',#37481,#37482,#4745,.T.);
#47091=EDGE_CURVE('',#37480,#37482,#4746,.T.);
#47092=EDGE_CURVE('',#37479,#37481,#4747,.T.);
#47093=EDGE_CURVE('',#37482,#37477,#4748,.T.);
#47094=EDGE_CURVE('',#37481,#37478,#4749,.T.);
#47095=EDGE_CURVE('',#37483,#37484,#4750,.T.);
#47096=EDGE_CURVE('',#37485,#37484,#4751,.T.);
#47097=EDGE_CURVE('',#37486,#37485,#4752,.T.);
#47098=EDGE_CURVE('',#37486,#37483,#4753,.T.);
#47099=EDGE_CURVE('',#37487,#37488,#4754,.T.);
#47100=EDGE_CURVE('',#37484,#37488,#4755,.T.);
#47101=EDGE_CURVE('',#37483,#37487,#4756,.T.);
#47102=EDGE_CURVE('',#37489,#37490,#4757,.T.);
#47103=EDGE_CURVE('',#37488,#37490,#4758,.T.);
#47104=EDGE_CURVE('',#37487,#37489,#4759,.T.);
#47105=EDGE_CURVE('',#37490,#37485,#4760,.T.);
#47106=EDGE_CURVE('',#37489,#37486,#4761,.T.);
#47107=EDGE_CURVE('',#37491,#37492,#4762,.T.);
#47108=EDGE_CURVE('',#37493,#37492,#4763,.T.);
#47109=EDGE_CURVE('',#37494,#37493,#4764,.T.);
#47110=EDGE_CURVE('',#37494,#37491,#4765,.T.);
#47111=EDGE_CURVE('',#37495,#37496,#4766,.T.);
#47112=EDGE_CURVE('',#37492,#37496,#4767,.T.);
#47113=EDGE_CURVE('',#37491,#37495,#4768,.T.);
#47114=EDGE_CURVE('',#37497,#37498,#4769,.T.);
#47115=EDGE_CURVE('',#37496,#37498,#4770,.T.);
#47116=EDGE_CURVE('',#37495,#37497,#4771,.T.);
#47117=EDGE_CURVE('',#37498,#37493,#4772,.T.);
#47118=EDGE_CURVE('',#37497,#37494,#4773,.T.);
#47119=EDGE_CURVE('',#37499,#37500,#4774,.T.);
#47120=EDGE_CURVE('',#37501,#37500,#4775,.T.);
#47121=EDGE_CURVE('',#37502,#37501,#4776,.T.);
#47122=EDGE_CURVE('',#37502,#37499,#4777,.T.);
#47123=EDGE_CURVE('',#37503,#37504,#4778,.T.);
#47124=EDGE_CURVE('',#37500,#37504,#4779,.T.);
#47125=EDGE_CURVE('',#37499,#37503,#4780,.T.);
#47126=EDGE_CURVE('',#37505,#37506,#4781,.T.);
#47127=EDGE_CURVE('',#37504,#37506,#4782,.T.);
#47128=EDGE_CURVE('',#37503,#37505,#4783,.T.);
#47129=EDGE_CURVE('',#37506,#37501,#4784,.T.);
#47130=EDGE_CURVE('',#37505,#37502,#4785,.T.);
#47131=EDGE_CURVE('',#37507,#37508,#4786,.T.);
#47132=EDGE_CURVE('',#37509,#37508,#4787,.T.);
#47133=EDGE_CURVE('',#37510,#37509,#4788,.T.);
#47134=EDGE_CURVE('',#37510,#37507,#4789,.T.);
#47135=EDGE_CURVE('',#37511,#37512,#4790,.T.);
#47136=EDGE_CURVE('',#37508,#37512,#4791,.T.);
#47137=EDGE_CURVE('',#37507,#37511,#4792,.T.);
#47138=EDGE_CURVE('',#37513,#37514,#4793,.T.);
#47139=EDGE_CURVE('',#37512,#37514,#4794,.T.);
#47140=EDGE_CURVE('',#37511,#37513,#4795,.T.);
#47141=EDGE_CURVE('',#37514,#37509,#4796,.T.);
#47142=EDGE_CURVE('',#37513,#37510,#4797,.T.);
#47143=EDGE_CURVE('',#37515,#37516,#4798,.T.);
#47144=EDGE_CURVE('',#37517,#37516,#4799,.T.);
#47145=EDGE_CURVE('',#37518,#37517,#4800,.T.);
#47146=EDGE_CURVE('',#37518,#37515,#4801,.T.);
#47147=EDGE_CURVE('',#37519,#37520,#4802,.T.);
#47148=EDGE_CURVE('',#37516,#37520,#4803,.T.);
#47149=EDGE_CURVE('',#37515,#37519,#4804,.T.);
#47150=EDGE_CURVE('',#37521,#37522,#4805,.T.);
#47151=EDGE_CURVE('',#37520,#37522,#4806,.T.);
#47152=EDGE_CURVE('',#37519,#37521,#4807,.T.);
#47153=EDGE_CURVE('',#37522,#37517,#4808,.T.);
#47154=EDGE_CURVE('',#37521,#37518,#4809,.T.);
#47155=EDGE_CURVE('',#37523,#37524,#4810,.T.);
#47156=EDGE_CURVE('',#37525,#37524,#4811,.T.);
#47157=EDGE_CURVE('',#37526,#37525,#4812,.T.);
#47158=EDGE_CURVE('',#37526,#37523,#4813,.T.);
#47159=EDGE_CURVE('',#37527,#37528,#4814,.T.);
#47160=EDGE_CURVE('',#37524,#37528,#4815,.T.);
#47161=EDGE_CURVE('',#37523,#37527,#4816,.T.);
#47162=EDGE_CURVE('',#37529,#37530,#4817,.T.);
#47163=EDGE_CURVE('',#37528,#37530,#4818,.T.);
#47164=EDGE_CURVE('',#37527,#37529,#4819,.T.);
#47165=EDGE_CURVE('',#37530,#37525,#4820,.T.);
#47166=EDGE_CURVE('',#37529,#37526,#4821,.T.);
#47167=EDGE_CURVE('',#37531,#37532,#4822,.T.);
#47168=EDGE_CURVE('',#37533,#37532,#4823,.T.);
#47169=EDGE_CURVE('',#37534,#37533,#4824,.T.);
#47170=EDGE_CURVE('',#37534,#37531,#4825,.T.);
#47171=EDGE_CURVE('',#37535,#37536,#4826,.T.);
#47172=EDGE_CURVE('',#37532,#37536,#4827,.T.);
#47173=EDGE_CURVE('',#37531,#37535,#4828,.T.);
#47174=EDGE_CURVE('',#37537,#37538,#4829,.T.);
#47175=EDGE_CURVE('',#37536,#37538,#4830,.T.);
#47176=EDGE_CURVE('',#37535,#37537,#4831,.T.);
#47177=EDGE_CURVE('',#37538,#37533,#4832,.T.);
#47178=EDGE_CURVE('',#37537,#37534,#4833,.T.);
#47179=EDGE_CURVE('',#37539,#37540,#4834,.T.);
#47180=EDGE_CURVE('',#37541,#37540,#4835,.T.);
#47181=EDGE_CURVE('',#37542,#37541,#4836,.T.);
#47182=EDGE_CURVE('',#37542,#37539,#4837,.T.);
#47183=EDGE_CURVE('',#37543,#37544,#4838,.T.);
#47184=EDGE_CURVE('',#37540,#37544,#4839,.T.);
#47185=EDGE_CURVE('',#37539,#37543,#4840,.T.);
#47186=EDGE_CURVE('',#37545,#37546,#4841,.T.);
#47187=EDGE_CURVE('',#37544,#37546,#4842,.T.);
#47188=EDGE_CURVE('',#37543,#37545,#4843,.T.);
#47189=EDGE_CURVE('',#37546,#37541,#4844,.T.);
#47190=EDGE_CURVE('',#37545,#37542,#4845,.T.);
#47191=EDGE_CURVE('',#37547,#37548,#4846,.T.);
#47192=EDGE_CURVE('',#37549,#37548,#4847,.T.);
#47193=EDGE_CURVE('',#37550,#37549,#4848,.T.);
#47194=EDGE_CURVE('',#37550,#37547,#4849,.T.);
#47195=EDGE_CURVE('',#37551,#37552,#4850,.T.);
#47196=EDGE_CURVE('',#37548,#37552,#4851,.T.);
#47197=EDGE_CURVE('',#37547,#37551,#4852,.T.);
#47198=EDGE_CURVE('',#37553,#37554,#4853,.T.);
#47199=EDGE_CURVE('',#37552,#37554,#4854,.T.);
#47200=EDGE_CURVE('',#37551,#37553,#4855,.T.);
#47201=EDGE_CURVE('',#37554,#37549,#4856,.T.);
#47202=EDGE_CURVE('',#37553,#37550,#4857,.T.);
#47203=EDGE_CURVE('',#37555,#37556,#4858,.T.);
#47204=EDGE_CURVE('',#37557,#37556,#4859,.T.);
#47205=EDGE_CURVE('',#37558,#37557,#4860,.T.);
#47206=EDGE_CURVE('',#37558,#37555,#4861,.T.);
#47207=EDGE_CURVE('',#37559,#37560,#4862,.T.);
#47208=EDGE_CURVE('',#37556,#37560,#4863,.T.);
#47209=EDGE_CURVE('',#37555,#37559,#4864,.T.);
#47210=EDGE_CURVE('',#37561,#37562,#4865,.T.);
#47211=EDGE_CURVE('',#37560,#37562,#4866,.T.);
#47212=EDGE_CURVE('',#37559,#37561,#4867,.T.);
#47213=EDGE_CURVE('',#37562,#37557,#4868,.T.);
#47214=EDGE_CURVE('',#37561,#37558,#4869,.T.);
#47215=EDGE_CURVE('',#37563,#37564,#4870,.T.);
#47216=EDGE_CURVE('',#37565,#37564,#4871,.T.);
#47217=EDGE_CURVE('',#37566,#37565,#4872,.T.);
#47218=EDGE_CURVE('',#37566,#37563,#4873,.T.);
#47219=EDGE_CURVE('',#37567,#37568,#4874,.T.);
#47220=EDGE_CURVE('',#37564,#37568,#4875,.T.);
#47221=EDGE_CURVE('',#37563,#37567,#4876,.T.);
#47222=EDGE_CURVE('',#37569,#37570,#4877,.T.);
#47223=EDGE_CURVE('',#37568,#37570,#4878,.T.);
#47224=EDGE_CURVE('',#37567,#37569,#4879,.T.);
#47225=EDGE_CURVE('',#37570,#37565,#4880,.T.);
#47226=EDGE_CURVE('',#37569,#37566,#4881,.T.);
#47227=EDGE_CURVE('',#37571,#37572,#4882,.T.);
#47228=EDGE_CURVE('',#37573,#37572,#4883,.T.);
#47229=EDGE_CURVE('',#37574,#37573,#4884,.T.);
#47230=EDGE_CURVE('',#37574,#37571,#4885,.T.);
#47231=EDGE_CURVE('',#37575,#37576,#4886,.T.);
#47232=EDGE_CURVE('',#37572,#37576,#4887,.T.);
#47233=EDGE_CURVE('',#37571,#37575,#4888,.T.);
#47234=EDGE_CURVE('',#37577,#37578,#4889,.T.);
#47235=EDGE_CURVE('',#37576,#37578,#4890,.T.);
#47236=EDGE_CURVE('',#37575,#37577,#4891,.T.);
#47237=EDGE_CURVE('',#37578,#37573,#4892,.T.);
#47238=EDGE_CURVE('',#37577,#37574,#4893,.T.);
#47239=EDGE_CURVE('',#37579,#37580,#4894,.T.);
#47240=EDGE_CURVE('',#37581,#37580,#4895,.T.);
#47241=EDGE_CURVE('',#37582,#37581,#4896,.T.);
#47242=EDGE_CURVE('',#37582,#37579,#4897,.T.);
#47243=EDGE_CURVE('',#37583,#37584,#4898,.T.);
#47244=EDGE_CURVE('',#37580,#37584,#4899,.T.);
#47245=EDGE_CURVE('',#37579,#37583,#4900,.T.);
#47246=EDGE_CURVE('',#37585,#37586,#4901,.T.);
#47247=EDGE_CURVE('',#37584,#37586,#4902,.T.);
#47248=EDGE_CURVE('',#37583,#37585,#4903,.T.);
#47249=EDGE_CURVE('',#37586,#37581,#4904,.T.);
#47250=EDGE_CURVE('',#37585,#37582,#4905,.T.);
#47251=EDGE_CURVE('',#37587,#37588,#4906,.T.);
#47252=EDGE_CURVE('',#37589,#37588,#4907,.T.);
#47253=EDGE_CURVE('',#37590,#37589,#4908,.T.);
#47254=EDGE_CURVE('',#37590,#37587,#4909,.T.);
#47255=EDGE_CURVE('',#37591,#37592,#4910,.T.);
#47256=EDGE_CURVE('',#37588,#37592,#4911,.T.);
#47257=EDGE_CURVE('',#37587,#37591,#4912,.T.);
#47258=EDGE_CURVE('',#37593,#37594,#4913,.T.);
#47259=EDGE_CURVE('',#37592,#37594,#4914,.T.);
#47260=EDGE_CURVE('',#37591,#37593,#4915,.T.);
#47261=EDGE_CURVE('',#37594,#37589,#4916,.T.);
#47262=EDGE_CURVE('',#37593,#37590,#4917,.T.);
#47263=EDGE_CURVE('',#37595,#37596,#4918,.T.);
#47264=EDGE_CURVE('',#37597,#37596,#4919,.T.);
#47265=EDGE_CURVE('',#37598,#37597,#4920,.T.);
#47266=EDGE_CURVE('',#37598,#37595,#4921,.T.);
#47267=EDGE_CURVE('',#37599,#37600,#4922,.T.);
#47268=EDGE_CURVE('',#37596,#37600,#4923,.T.);
#47269=EDGE_CURVE('',#37595,#37599,#4924,.T.);
#47270=EDGE_CURVE('',#37601,#37602,#4925,.T.);
#47271=EDGE_CURVE('',#37600,#37602,#4926,.T.);
#47272=EDGE_CURVE('',#37599,#37601,#4927,.T.);
#47273=EDGE_CURVE('',#37602,#37597,#4928,.T.);
#47274=EDGE_CURVE('',#37601,#37598,#4929,.T.);
#47275=EDGE_CURVE('',#37603,#37604,#4930,.T.);
#47276=EDGE_CURVE('',#37605,#37604,#4931,.T.);
#47277=EDGE_CURVE('',#37606,#37605,#4932,.T.);
#47278=EDGE_CURVE('',#37606,#37603,#4933,.T.);
#47279=EDGE_CURVE('',#37607,#37608,#4934,.T.);
#47280=EDGE_CURVE('',#37604,#37608,#4935,.T.);
#47281=EDGE_CURVE('',#37603,#37607,#4936,.T.);
#47282=EDGE_CURVE('',#37609,#37610,#4937,.T.);
#47283=EDGE_CURVE('',#37608,#37610,#4938,.T.);
#47284=EDGE_CURVE('',#37607,#37609,#4939,.T.);
#47285=EDGE_CURVE('',#37610,#37605,#4940,.T.);
#47286=EDGE_CURVE('',#37609,#37606,#4941,.T.);
#47287=EDGE_CURVE('',#37611,#37612,#4942,.T.);
#47288=EDGE_CURVE('',#37613,#37612,#4943,.T.);
#47289=EDGE_CURVE('',#37614,#37613,#4944,.T.);
#47290=EDGE_CURVE('',#37614,#37611,#4945,.T.);
#47291=EDGE_CURVE('',#37615,#37616,#4946,.T.);
#47292=EDGE_CURVE('',#37612,#37616,#4947,.T.);
#47293=EDGE_CURVE('',#37611,#37615,#4948,.T.);
#47294=EDGE_CURVE('',#37617,#37618,#4949,.T.);
#47295=EDGE_CURVE('',#37616,#37618,#4950,.T.);
#47296=EDGE_CURVE('',#37615,#37617,#4951,.T.);
#47297=EDGE_CURVE('',#37618,#37613,#4952,.T.);
#47298=EDGE_CURVE('',#37617,#37614,#4953,.T.);
#47299=EDGE_CURVE('',#37619,#37620,#4954,.T.);
#47300=EDGE_CURVE('',#37621,#37620,#4955,.T.);
#47301=EDGE_CURVE('',#37622,#37621,#4956,.T.);
#47302=EDGE_CURVE('',#37622,#37619,#4957,.T.);
#47303=EDGE_CURVE('',#37623,#37624,#4958,.T.);
#47304=EDGE_CURVE('',#37620,#37624,#4959,.T.);
#47305=EDGE_CURVE('',#37619,#37623,#4960,.T.);
#47306=EDGE_CURVE('',#37625,#37626,#4961,.T.);
#47307=EDGE_CURVE('',#37624,#37626,#4962,.T.);
#47308=EDGE_CURVE('',#37623,#37625,#4963,.T.);
#47309=EDGE_CURVE('',#37626,#37621,#4964,.T.);
#47310=EDGE_CURVE('',#37625,#37622,#4965,.T.);
#47311=EDGE_CURVE('',#37627,#37628,#4966,.T.);
#47312=EDGE_CURVE('',#37629,#37628,#4967,.T.);
#47313=EDGE_CURVE('',#37630,#37629,#4968,.T.);
#47314=EDGE_CURVE('',#37630,#37627,#4969,.T.);
#47315=EDGE_CURVE('',#37631,#37632,#4970,.T.);
#47316=EDGE_CURVE('',#37628,#37632,#4971,.T.);
#47317=EDGE_CURVE('',#37627,#37631,#4972,.T.);
#47318=EDGE_CURVE('',#37633,#37634,#4973,.T.);
#47319=EDGE_CURVE('',#37632,#37634,#4974,.T.);
#47320=EDGE_CURVE('',#37631,#37633,#4975,.T.);
#47321=EDGE_CURVE('',#37634,#37629,#4976,.T.);
#47322=EDGE_CURVE('',#37633,#37630,#4977,.T.);
#47323=EDGE_CURVE('',#37635,#37636,#4978,.T.);
#47324=EDGE_CURVE('',#37637,#37636,#4979,.T.);
#47325=EDGE_CURVE('',#37638,#37637,#4980,.T.);
#47326=EDGE_CURVE('',#37638,#37635,#4981,.T.);
#47327=EDGE_CURVE('',#37639,#37640,#4982,.T.);
#47328=EDGE_CURVE('',#37636,#37640,#4983,.T.);
#47329=EDGE_CURVE('',#37635,#37639,#4984,.T.);
#47330=EDGE_CURVE('',#37641,#37642,#4985,.T.);
#47331=EDGE_CURVE('',#37640,#37642,#4986,.T.);
#47332=EDGE_CURVE('',#37639,#37641,#4987,.T.);
#47333=EDGE_CURVE('',#37642,#37637,#4988,.T.);
#47334=EDGE_CURVE('',#37641,#37638,#4989,.T.);
#47335=EDGE_CURVE('',#37643,#37644,#4990,.T.);
#47336=EDGE_CURVE('',#37645,#37644,#4991,.T.);
#47337=EDGE_CURVE('',#37646,#37645,#4992,.T.);
#47338=EDGE_CURVE('',#37646,#37643,#4993,.T.);
#47339=EDGE_CURVE('',#37647,#37648,#4994,.T.);
#47340=EDGE_CURVE('',#37644,#37648,#4995,.T.);
#47341=EDGE_CURVE('',#37643,#37647,#4996,.T.);
#47342=EDGE_CURVE('',#37649,#37650,#4997,.T.);
#47343=EDGE_CURVE('',#37648,#37650,#4998,.T.);
#47344=EDGE_CURVE('',#37647,#37649,#4999,.T.);
#47345=EDGE_CURVE('',#37650,#37645,#5000,.T.);
#47346=EDGE_CURVE('',#37649,#37646,#5001,.T.);
#47347=EDGE_CURVE('',#37651,#37652,#5002,.T.);
#47348=EDGE_CURVE('',#37653,#37652,#5003,.T.);
#47349=EDGE_CURVE('',#37654,#37653,#5004,.T.);
#47350=EDGE_CURVE('',#37654,#37651,#5005,.T.);
#47351=EDGE_CURVE('',#37655,#37656,#5006,.T.);
#47352=EDGE_CURVE('',#37652,#37656,#5007,.T.);
#47353=EDGE_CURVE('',#37651,#37655,#5008,.T.);
#47354=EDGE_CURVE('',#37657,#37658,#5009,.T.);
#47355=EDGE_CURVE('',#37656,#37658,#5010,.T.);
#47356=EDGE_CURVE('',#37655,#37657,#5011,.T.);
#47357=EDGE_CURVE('',#37658,#37653,#5012,.T.);
#47358=EDGE_CURVE('',#37657,#37654,#5013,.T.);
#47359=EDGE_CURVE('',#37659,#37660,#5014,.T.);
#47360=EDGE_CURVE('',#37661,#37660,#5015,.T.);
#47361=EDGE_CURVE('',#37662,#37661,#5016,.T.);
#47362=EDGE_CURVE('',#37662,#37659,#5017,.T.);
#47363=EDGE_CURVE('',#37663,#37664,#5018,.T.);
#47364=EDGE_CURVE('',#37660,#37664,#5019,.T.);
#47365=EDGE_CURVE('',#37659,#37663,#5020,.T.);
#47366=EDGE_CURVE('',#37665,#37666,#5021,.T.);
#47367=EDGE_CURVE('',#37664,#37666,#5022,.T.);
#47368=EDGE_CURVE('',#37663,#37665,#5023,.T.);
#47369=EDGE_CURVE('',#37666,#37661,#5024,.T.);
#47370=EDGE_CURVE('',#37665,#37662,#5025,.T.);
#47371=EDGE_CURVE('',#37667,#37668,#5026,.T.);
#47372=EDGE_CURVE('',#37669,#37668,#5027,.T.);
#47373=EDGE_CURVE('',#37670,#37669,#5028,.T.);
#47374=EDGE_CURVE('',#37670,#37667,#5029,.T.);
#47375=EDGE_CURVE('',#37671,#37672,#5030,.T.);
#47376=EDGE_CURVE('',#37668,#37672,#5031,.T.);
#47377=EDGE_CURVE('',#37667,#37671,#5032,.T.);
#47378=EDGE_CURVE('',#37673,#37674,#5033,.T.);
#47379=EDGE_CURVE('',#37672,#37674,#5034,.T.);
#47380=EDGE_CURVE('',#37671,#37673,#5035,.T.);
#47381=EDGE_CURVE('',#37674,#37669,#5036,.T.);
#47382=EDGE_CURVE('',#37673,#37670,#5037,.T.);
#47383=EDGE_CURVE('',#37675,#37676,#5038,.T.);
#47384=EDGE_CURVE('',#37677,#37676,#5039,.T.);
#47385=EDGE_CURVE('',#37678,#37677,#5040,.T.);
#47386=EDGE_CURVE('',#37678,#37675,#5041,.T.);
#47387=EDGE_CURVE('',#37679,#37680,#5042,.T.);
#47388=EDGE_CURVE('',#37676,#37680,#5043,.T.);
#47389=EDGE_CURVE('',#37675,#37679,#5044,.T.);
#47390=EDGE_CURVE('',#37681,#37682,#5045,.T.);
#47391=EDGE_CURVE('',#37680,#37682,#5046,.T.);
#47392=EDGE_CURVE('',#37679,#37681,#5047,.T.);
#47393=EDGE_CURVE('',#37682,#37677,#5048,.T.);
#47394=EDGE_CURVE('',#37681,#37678,#5049,.T.);
#47395=EDGE_CURVE('',#37683,#37684,#5050,.T.);
#47396=EDGE_CURVE('',#37685,#37684,#5051,.T.);
#47397=EDGE_CURVE('',#37686,#37685,#5052,.T.);
#47398=EDGE_CURVE('',#37686,#37683,#5053,.T.);
#47399=EDGE_CURVE('',#37687,#37688,#5054,.T.);
#47400=EDGE_CURVE('',#37684,#37688,#5055,.T.);
#47401=EDGE_CURVE('',#37683,#37687,#5056,.T.);
#47402=EDGE_CURVE('',#37689,#37690,#5057,.T.);
#47403=EDGE_CURVE('',#37688,#37690,#5058,.T.);
#47404=EDGE_CURVE('',#37687,#37689,#5059,.T.);
#47405=EDGE_CURVE('',#37690,#37685,#5060,.T.);
#47406=EDGE_CURVE('',#37689,#37686,#5061,.T.);
#47407=EDGE_CURVE('',#37691,#37692,#5062,.T.);
#47408=EDGE_CURVE('',#37693,#37692,#5063,.T.);
#47409=EDGE_CURVE('',#37694,#37693,#5064,.T.);
#47410=EDGE_CURVE('',#37694,#37691,#5065,.T.);
#47411=EDGE_CURVE('',#37695,#37696,#5066,.T.);
#47412=EDGE_CURVE('',#37692,#37696,#5067,.T.);
#47413=EDGE_CURVE('',#37691,#37695,#5068,.T.);
#47414=EDGE_CURVE('',#37697,#37698,#5069,.T.);
#47415=EDGE_CURVE('',#37696,#37698,#5070,.T.);
#47416=EDGE_CURVE('',#37695,#37697,#5071,.T.);
#47417=EDGE_CURVE('',#37698,#37693,#5072,.T.);
#47418=EDGE_CURVE('',#37697,#37694,#5073,.T.);
#47419=EDGE_CURVE('',#37699,#37700,#5074,.T.);
#47420=EDGE_CURVE('',#37701,#37700,#5075,.T.);
#47421=EDGE_CURVE('',#37702,#37701,#5076,.T.);
#47422=EDGE_CURVE('',#37702,#37699,#5077,.T.);
#47423=EDGE_CURVE('',#37703,#37704,#5078,.T.);
#47424=EDGE_CURVE('',#37700,#37704,#5079,.T.);
#47425=EDGE_CURVE('',#37699,#37703,#5080,.T.);
#47426=EDGE_CURVE('',#37705,#37706,#5081,.T.);
#47427=EDGE_CURVE('',#37704,#37706,#5082,.T.);
#47428=EDGE_CURVE('',#37703,#37705,#5083,.T.);
#47429=EDGE_CURVE('',#37706,#37701,#5084,.T.);
#47430=EDGE_CURVE('',#37705,#37702,#5085,.T.);
#47431=EDGE_CURVE('',#37707,#37708,#5086,.T.);
#47432=EDGE_CURVE('',#37709,#37708,#5087,.T.);
#47433=EDGE_CURVE('',#37710,#37709,#5088,.T.);
#47434=EDGE_CURVE('',#37710,#37707,#5089,.T.);
#47435=EDGE_CURVE('',#37711,#37712,#5090,.T.);
#47436=EDGE_CURVE('',#37708,#37712,#5091,.T.);
#47437=EDGE_CURVE('',#37707,#37711,#5092,.T.);
#47438=EDGE_CURVE('',#37713,#37714,#5093,.T.);
#47439=EDGE_CURVE('',#37712,#37714,#5094,.T.);
#47440=EDGE_CURVE('',#37711,#37713,#5095,.T.);
#47441=EDGE_CURVE('',#37714,#37709,#5096,.T.);
#47442=EDGE_CURVE('',#37713,#37710,#5097,.T.);
#47443=EDGE_CURVE('',#37715,#37716,#5098,.T.);
#47444=EDGE_CURVE('',#37717,#37716,#5099,.T.);
#47445=EDGE_CURVE('',#37718,#37717,#5100,.T.);
#47446=EDGE_CURVE('',#37718,#37715,#5101,.T.);
#47447=EDGE_CURVE('',#37719,#37720,#5102,.T.);
#47448=EDGE_CURVE('',#37716,#37720,#5103,.T.);
#47449=EDGE_CURVE('',#37715,#37719,#5104,.T.);
#47450=EDGE_CURVE('',#37721,#37722,#5105,.T.);
#47451=EDGE_CURVE('',#37720,#37722,#5106,.T.);
#47452=EDGE_CURVE('',#37719,#37721,#5107,.T.);
#47453=EDGE_CURVE('',#37722,#37717,#5108,.T.);
#47454=EDGE_CURVE('',#37721,#37718,#5109,.T.);
#47455=EDGE_CURVE('',#37723,#37724,#5110,.T.);
#47456=EDGE_CURVE('',#37725,#37724,#5111,.T.);
#47457=EDGE_CURVE('',#37726,#37725,#5112,.T.);
#47458=EDGE_CURVE('',#37726,#37723,#5113,.T.);
#47459=EDGE_CURVE('',#37727,#37728,#5114,.T.);
#47460=EDGE_CURVE('',#37724,#37728,#5115,.T.);
#47461=EDGE_CURVE('',#37723,#37727,#5116,.T.);
#47462=EDGE_CURVE('',#37729,#37730,#5117,.T.);
#47463=EDGE_CURVE('',#37728,#37730,#5118,.T.);
#47464=EDGE_CURVE('',#37727,#37729,#5119,.T.);
#47465=EDGE_CURVE('',#37730,#37725,#5120,.T.);
#47466=EDGE_CURVE('',#37729,#37726,#5121,.T.);
#47467=EDGE_CURVE('',#37731,#37732,#5122,.T.);
#47468=EDGE_CURVE('',#37733,#37732,#5123,.T.);
#47469=EDGE_CURVE('',#37734,#37733,#5124,.T.);
#47470=EDGE_CURVE('',#37734,#37731,#5125,.T.);
#47471=EDGE_CURVE('',#37735,#37736,#5126,.T.);
#47472=EDGE_CURVE('',#37732,#37736,#5127,.T.);
#47473=EDGE_CURVE('',#37731,#37735,#5128,.T.);
#47474=EDGE_CURVE('',#37737,#37738,#5129,.T.);
#47475=EDGE_CURVE('',#37736,#37738,#5130,.T.);
#47476=EDGE_CURVE('',#37735,#37737,#5131,.T.);
#47477=EDGE_CURVE('',#37738,#37733,#5132,.T.);
#47478=EDGE_CURVE('',#37737,#37734,#5133,.T.);
#47479=EDGE_CURVE('',#37739,#37740,#5134,.T.);
#47480=EDGE_CURVE('',#37741,#37740,#5135,.T.);
#47481=EDGE_CURVE('',#37742,#37741,#5136,.T.);
#47482=EDGE_CURVE('',#37742,#37739,#5137,.T.);
#47483=EDGE_CURVE('',#37743,#37744,#5138,.T.);
#47484=EDGE_CURVE('',#37740,#37744,#5139,.T.);
#47485=EDGE_CURVE('',#37739,#37743,#5140,.T.);
#47486=EDGE_CURVE('',#37745,#37746,#5141,.T.);
#47487=EDGE_CURVE('',#37744,#37746,#5142,.T.);
#47488=EDGE_CURVE('',#37743,#37745,#5143,.T.);
#47489=EDGE_CURVE('',#37746,#37741,#5144,.T.);
#47490=EDGE_CURVE('',#37745,#37742,#5145,.T.);
#47491=EDGE_CURVE('',#37747,#37748,#5146,.T.);
#47492=EDGE_CURVE('',#37749,#37748,#5147,.T.);
#47493=EDGE_CURVE('',#37750,#37749,#5148,.T.);
#47494=EDGE_CURVE('',#37750,#37747,#5149,.T.);
#47495=EDGE_CURVE('',#37751,#37752,#5150,.T.);
#47496=EDGE_CURVE('',#37748,#37752,#5151,.T.);
#47497=EDGE_CURVE('',#37747,#37751,#5152,.T.);
#47498=EDGE_CURVE('',#37753,#37754,#5153,.T.);
#47499=EDGE_CURVE('',#37752,#37754,#5154,.T.);
#47500=EDGE_CURVE('',#37751,#37753,#5155,.T.);
#47501=EDGE_CURVE('',#37754,#37749,#5156,.T.);
#47502=EDGE_CURVE('',#37753,#37750,#5157,.T.);
#47503=EDGE_CURVE('',#37755,#37756,#5158,.T.);
#47504=EDGE_CURVE('',#37757,#37756,#5159,.T.);
#47505=EDGE_CURVE('',#37758,#37757,#5160,.T.);
#47506=EDGE_CURVE('',#37758,#37755,#5161,.T.);
#47507=EDGE_CURVE('',#37759,#37760,#5162,.T.);
#47508=EDGE_CURVE('',#37756,#37760,#5163,.T.);
#47509=EDGE_CURVE('',#37755,#37759,#5164,.T.);
#47510=EDGE_CURVE('',#37761,#37762,#5165,.T.);
#47511=EDGE_CURVE('',#37760,#37762,#5166,.T.);
#47512=EDGE_CURVE('',#37759,#37761,#5167,.T.);
#47513=EDGE_CURVE('',#37762,#37757,#5168,.T.);
#47514=EDGE_CURVE('',#37761,#37758,#5169,.T.);
#47515=EDGE_CURVE('',#37763,#37764,#5170,.T.);
#47516=EDGE_CURVE('',#37765,#37764,#5171,.T.);
#47517=EDGE_CURVE('',#37766,#37765,#5172,.T.);
#47518=EDGE_CURVE('',#37766,#37763,#5173,.T.);
#47519=EDGE_CURVE('',#37767,#37768,#5174,.T.);
#47520=EDGE_CURVE('',#37764,#37768,#5175,.T.);
#47521=EDGE_CURVE('',#37763,#37767,#5176,.T.);
#47522=EDGE_CURVE('',#37769,#37770,#5177,.T.);
#47523=EDGE_CURVE('',#37768,#37770,#5178,.T.);
#47524=EDGE_CURVE('',#37767,#37769,#5179,.T.);
#47525=EDGE_CURVE('',#37770,#37765,#5180,.T.);
#47526=EDGE_CURVE('',#37769,#37766,#5181,.T.);
#47527=EDGE_CURVE('',#37771,#37772,#5182,.T.);
#47528=EDGE_CURVE('',#37773,#37772,#5183,.T.);
#47529=EDGE_CURVE('',#37774,#37773,#5184,.T.);
#47530=EDGE_CURVE('',#37774,#37771,#5185,.T.);
#47531=EDGE_CURVE('',#37775,#37776,#5186,.T.);
#47532=EDGE_CURVE('',#37772,#37776,#5187,.T.);
#47533=EDGE_CURVE('',#37771,#37775,#5188,.T.);
#47534=EDGE_CURVE('',#37777,#37778,#5189,.T.);
#47535=EDGE_CURVE('',#37776,#37778,#5190,.T.);
#47536=EDGE_CURVE('',#37775,#37777,#5191,.T.);
#47537=EDGE_CURVE('',#37778,#37773,#5192,.T.);
#47538=EDGE_CURVE('',#37777,#37774,#5193,.T.);
#47539=EDGE_CURVE('',#37779,#37780,#5194,.T.);
#47540=EDGE_CURVE('',#37781,#37780,#5195,.T.);
#47541=EDGE_CURVE('',#37782,#37781,#5196,.T.);
#47542=EDGE_CURVE('',#37782,#37779,#5197,.T.);
#47543=EDGE_CURVE('',#37783,#37784,#5198,.T.);
#47544=EDGE_CURVE('',#37780,#37784,#5199,.T.);
#47545=EDGE_CURVE('',#37779,#37783,#5200,.T.);
#47546=EDGE_CURVE('',#37785,#37786,#5201,.T.);
#47547=EDGE_CURVE('',#37784,#37786,#5202,.T.);
#47548=EDGE_CURVE('',#37783,#37785,#5203,.T.);
#47549=EDGE_CURVE('',#37786,#37781,#5204,.T.);
#47550=EDGE_CURVE('',#37785,#37782,#5205,.T.);
#47551=EDGE_CURVE('',#37787,#37788,#5206,.T.);
#47552=EDGE_CURVE('',#37789,#37788,#5207,.T.);
#47553=EDGE_CURVE('',#37790,#37789,#5208,.T.);
#47554=EDGE_CURVE('',#37790,#37787,#5209,.T.);
#47555=EDGE_CURVE('',#37791,#37792,#5210,.T.);
#47556=EDGE_CURVE('',#37788,#37792,#5211,.T.);
#47557=EDGE_CURVE('',#37787,#37791,#5212,.T.);
#47558=EDGE_CURVE('',#37793,#37794,#5213,.T.);
#47559=EDGE_CURVE('',#37792,#37794,#5214,.T.);
#47560=EDGE_CURVE('',#37791,#37793,#5215,.T.);
#47561=EDGE_CURVE('',#37794,#37789,#5216,.T.);
#47562=EDGE_CURVE('',#37793,#37790,#5217,.T.);
#47563=EDGE_CURVE('',#37795,#37796,#5218,.T.);
#47564=EDGE_CURVE('',#37797,#37796,#5219,.T.);
#47565=EDGE_CURVE('',#37798,#37797,#5220,.T.);
#47566=EDGE_CURVE('',#37798,#37795,#5221,.T.);
#47567=EDGE_CURVE('',#37799,#37800,#5222,.T.);
#47568=EDGE_CURVE('',#37796,#37800,#5223,.T.);
#47569=EDGE_CURVE('',#37795,#37799,#5224,.T.);
#47570=EDGE_CURVE('',#37801,#37802,#5225,.T.);
#47571=EDGE_CURVE('',#37800,#37802,#5226,.T.);
#47572=EDGE_CURVE('',#37799,#37801,#5227,.T.);
#47573=EDGE_CURVE('',#37802,#37797,#5228,.T.);
#47574=EDGE_CURVE('',#37801,#37798,#5229,.T.);
#47575=EDGE_CURVE('',#37803,#37804,#5230,.T.);
#47576=EDGE_CURVE('',#37805,#37804,#5231,.T.);
#47577=EDGE_CURVE('',#37806,#37805,#5232,.T.);
#47578=EDGE_CURVE('',#37806,#37803,#5233,.T.);
#47579=EDGE_CURVE('',#37807,#37808,#5234,.T.);
#47580=EDGE_CURVE('',#37804,#37808,#5235,.T.);
#47581=EDGE_CURVE('',#37803,#37807,#5236,.T.);
#47582=EDGE_CURVE('',#37809,#37810,#5237,.T.);
#47583=EDGE_CURVE('',#37808,#37810,#5238,.T.);
#47584=EDGE_CURVE('',#37807,#37809,#5239,.T.);
#47585=EDGE_CURVE('',#37810,#37805,#5240,.T.);
#47586=EDGE_CURVE('',#37809,#37806,#5241,.T.);
#47587=EDGE_CURVE('',#37811,#37812,#5242,.T.);
#47588=EDGE_CURVE('',#37813,#37812,#5243,.T.);
#47589=EDGE_CURVE('',#37814,#37813,#5244,.T.);
#47590=EDGE_CURVE('',#37814,#37811,#5245,.T.);
#47591=EDGE_CURVE('',#37815,#37816,#5246,.T.);
#47592=EDGE_CURVE('',#37812,#37816,#5247,.T.);
#47593=EDGE_CURVE('',#37811,#37815,#5248,.T.);
#47594=EDGE_CURVE('',#37817,#37818,#5249,.T.);
#47595=EDGE_CURVE('',#37816,#37818,#5250,.T.);
#47596=EDGE_CURVE('',#37815,#37817,#5251,.T.);
#47597=EDGE_CURVE('',#37818,#37813,#5252,.T.);
#47598=EDGE_CURVE('',#37817,#37814,#5253,.T.);
#47599=EDGE_CURVE('',#37819,#37820,#5254,.T.);
#47600=EDGE_CURVE('',#37821,#37820,#5255,.T.);
#47601=EDGE_CURVE('',#37822,#37821,#5256,.T.);
#47602=EDGE_CURVE('',#37822,#37819,#5257,.T.);
#47603=EDGE_CURVE('',#37823,#37824,#5258,.T.);
#47604=EDGE_CURVE('',#37820,#37824,#5259,.T.);
#47605=EDGE_CURVE('',#37819,#37823,#5260,.T.);
#47606=EDGE_CURVE('',#37825,#37826,#5261,.T.);
#47607=EDGE_CURVE('',#37824,#37826,#5262,.T.);
#47608=EDGE_CURVE('',#37823,#37825,#5263,.T.);
#47609=EDGE_CURVE('',#37826,#37821,#5264,.T.);
#47610=EDGE_CURVE('',#37825,#37822,#5265,.T.);
#47611=EDGE_CURVE('',#37827,#37828,#5266,.T.);
#47612=EDGE_CURVE('',#37829,#37828,#5267,.T.);
#47613=EDGE_CURVE('',#37830,#37829,#5268,.T.);
#47614=EDGE_CURVE('',#37830,#37827,#5269,.T.);
#47615=EDGE_CURVE('',#37831,#37832,#5270,.T.);
#47616=EDGE_CURVE('',#37828,#37832,#5271,.T.);
#47617=EDGE_CURVE('',#37827,#37831,#5272,.T.);
#47618=EDGE_CURVE('',#37833,#37834,#5273,.T.);
#47619=EDGE_CURVE('',#37832,#37834,#5274,.T.);
#47620=EDGE_CURVE('',#37831,#37833,#5275,.T.);
#47621=EDGE_CURVE('',#37834,#37829,#5276,.T.);
#47622=EDGE_CURVE('',#37833,#37830,#5277,.T.);
#47623=EDGE_CURVE('',#37835,#37836,#5278,.T.);
#47624=EDGE_CURVE('',#37837,#37836,#5279,.T.);
#47625=EDGE_CURVE('',#37838,#37837,#5280,.T.);
#47626=EDGE_CURVE('',#37838,#37835,#5281,.T.);
#47627=EDGE_CURVE('',#37839,#37840,#5282,.T.);
#47628=EDGE_CURVE('',#37836,#37840,#5283,.T.);
#47629=EDGE_CURVE('',#37835,#37839,#5284,.T.);
#47630=EDGE_CURVE('',#37841,#37842,#5285,.T.);
#47631=EDGE_CURVE('',#37840,#37842,#5286,.T.);
#47632=EDGE_CURVE('',#37839,#37841,#5287,.T.);
#47633=EDGE_CURVE('',#37842,#37837,#5288,.T.);
#47634=EDGE_CURVE('',#37841,#37838,#5289,.T.);
#47635=EDGE_CURVE('',#37843,#37844,#5290,.T.);
#47636=EDGE_CURVE('',#37845,#37844,#5291,.T.);
#47637=EDGE_CURVE('',#37846,#37845,#5292,.T.);
#47638=EDGE_CURVE('',#37846,#37843,#5293,.T.);
#47639=EDGE_CURVE('',#37847,#37848,#5294,.T.);
#47640=EDGE_CURVE('',#37844,#37848,#5295,.T.);
#47641=EDGE_CURVE('',#37843,#37847,#5296,.T.);
#47642=EDGE_CURVE('',#37849,#37850,#5297,.T.);
#47643=EDGE_CURVE('',#37848,#37850,#5298,.T.);
#47644=EDGE_CURVE('',#37847,#37849,#5299,.T.);
#47645=EDGE_CURVE('',#37850,#37845,#5300,.T.);
#47646=EDGE_CURVE('',#37849,#37846,#5301,.T.);
#47647=EDGE_CURVE('',#37851,#37852,#5302,.T.);
#47648=EDGE_CURVE('',#37853,#37852,#5303,.T.);
#47649=EDGE_CURVE('',#37854,#37853,#5304,.T.);
#47650=EDGE_CURVE('',#37854,#37851,#5305,.T.);
#47651=EDGE_CURVE('',#37855,#37856,#5306,.T.);
#47652=EDGE_CURVE('',#37852,#37856,#5307,.T.);
#47653=EDGE_CURVE('',#37851,#37855,#5308,.T.);
#47654=EDGE_CURVE('',#37857,#37858,#5309,.T.);
#47655=EDGE_CURVE('',#37856,#37858,#5310,.T.);
#47656=EDGE_CURVE('',#37855,#37857,#5311,.T.);
#47657=EDGE_CURVE('',#37858,#37853,#5312,.T.);
#47658=EDGE_CURVE('',#37857,#37854,#5313,.T.);
#47659=EDGE_CURVE('',#37859,#37860,#5314,.T.);
#47660=EDGE_CURVE('',#37861,#37860,#5315,.T.);
#47661=EDGE_CURVE('',#37862,#37861,#5316,.T.);
#47662=EDGE_CURVE('',#37862,#37859,#5317,.T.);
#47663=EDGE_CURVE('',#37863,#37864,#5318,.T.);
#47664=EDGE_CURVE('',#37860,#37864,#5319,.T.);
#47665=EDGE_CURVE('',#37859,#37863,#5320,.T.);
#47666=EDGE_CURVE('',#37865,#37866,#5321,.T.);
#47667=EDGE_CURVE('',#37864,#37866,#5322,.T.);
#47668=EDGE_CURVE('',#37863,#37865,#5323,.T.);
#47669=EDGE_CURVE('',#37866,#37861,#5324,.T.);
#47670=EDGE_CURVE('',#37865,#37862,#5325,.T.);
#47671=EDGE_CURVE('',#37867,#37868,#5326,.T.);
#47672=EDGE_CURVE('',#37869,#37868,#5327,.T.);
#47673=EDGE_CURVE('',#37870,#37869,#5328,.T.);
#47674=EDGE_CURVE('',#37870,#37867,#5329,.T.);
#47675=EDGE_CURVE('',#37871,#37872,#5330,.T.);
#47676=EDGE_CURVE('',#37868,#37872,#5331,.T.);
#47677=EDGE_CURVE('',#37867,#37871,#5332,.T.);
#47678=EDGE_CURVE('',#37873,#37874,#5333,.T.);
#47679=EDGE_CURVE('',#37872,#37874,#5334,.T.);
#47680=EDGE_CURVE('',#37871,#37873,#5335,.T.);
#47681=EDGE_CURVE('',#37874,#37869,#5336,.T.);
#47682=EDGE_CURVE('',#37873,#37870,#5337,.T.);
#47683=EDGE_CURVE('',#37875,#37876,#5338,.T.);
#47684=EDGE_CURVE('',#37877,#37876,#5339,.T.);
#47685=EDGE_CURVE('',#37878,#37877,#5340,.T.);
#47686=EDGE_CURVE('',#37878,#37875,#5341,.T.);
#47687=EDGE_CURVE('',#37879,#37880,#5342,.T.);
#47688=EDGE_CURVE('',#37876,#37880,#5343,.T.);
#47689=EDGE_CURVE('',#37875,#37879,#5344,.T.);
#47690=EDGE_CURVE('',#37881,#37882,#5345,.T.);
#47691=EDGE_CURVE('',#37880,#37882,#5346,.T.);
#47692=EDGE_CURVE('',#37879,#37881,#5347,.T.);
#47693=EDGE_CURVE('',#37882,#37877,#5348,.T.);
#47694=EDGE_CURVE('',#37881,#37878,#5349,.T.);
#47695=EDGE_CURVE('',#37883,#37884,#5350,.T.);
#47696=EDGE_CURVE('',#37885,#37884,#5351,.T.);
#47697=EDGE_CURVE('',#37886,#37885,#5352,.T.);
#47698=EDGE_CURVE('',#37886,#37883,#5353,.T.);
#47699=EDGE_CURVE('',#37887,#37888,#5354,.T.);
#47700=EDGE_CURVE('',#37884,#37888,#5355,.T.);
#47701=EDGE_CURVE('',#37883,#37887,#5356,.T.);
#47702=EDGE_CURVE('',#37889,#37890,#5357,.T.);
#47703=EDGE_CURVE('',#37888,#37890,#5358,.T.);
#47704=EDGE_CURVE('',#37887,#37889,#5359,.T.);
#47705=EDGE_CURVE('',#37890,#37885,#5360,.T.);
#47706=EDGE_CURVE('',#37889,#37886,#5361,.T.);
#47707=EDGE_CURVE('',#37891,#37892,#5362,.T.);
#47708=EDGE_CURVE('',#37893,#37892,#5363,.T.);
#47709=EDGE_CURVE('',#37894,#37893,#5364,.T.);
#47710=EDGE_CURVE('',#37894,#37891,#5365,.T.);
#47711=EDGE_CURVE('',#37895,#37896,#5366,.T.);
#47712=EDGE_CURVE('',#37892,#37896,#5367,.T.);
#47713=EDGE_CURVE('',#37891,#37895,#5368,.T.);
#47714=EDGE_CURVE('',#37897,#37898,#5369,.T.);
#47715=EDGE_CURVE('',#37896,#37898,#5370,.T.);
#47716=EDGE_CURVE('',#37895,#37897,#5371,.T.);
#47717=EDGE_CURVE('',#37898,#37893,#5372,.T.);
#47718=EDGE_CURVE('',#37897,#37894,#5373,.T.);
#47719=EDGE_CURVE('',#37899,#37900,#5374,.T.);
#47720=EDGE_CURVE('',#37901,#37900,#5375,.T.);
#47721=EDGE_CURVE('',#37902,#37901,#5376,.T.);
#47722=EDGE_CURVE('',#37902,#37899,#5377,.T.);
#47723=EDGE_CURVE('',#37903,#37904,#5378,.T.);
#47724=EDGE_CURVE('',#37900,#37904,#5379,.T.);
#47725=EDGE_CURVE('',#37899,#37903,#5380,.T.);
#47726=EDGE_CURVE('',#37905,#37906,#5381,.T.);
#47727=EDGE_CURVE('',#37904,#37906,#5382,.T.);
#47728=EDGE_CURVE('',#37903,#37905,#5383,.T.);
#47729=EDGE_CURVE('',#37906,#37901,#5384,.T.);
#47730=EDGE_CURVE('',#37905,#37902,#5385,.T.);
#47731=EDGE_CURVE('',#37907,#37908,#5386,.T.);
#47732=EDGE_CURVE('',#37909,#37908,#5387,.T.);
#47733=EDGE_CURVE('',#37910,#37909,#5388,.T.);
#47734=EDGE_CURVE('',#37910,#37907,#5389,.T.);
#47735=EDGE_CURVE('',#37911,#37912,#5390,.T.);
#47736=EDGE_CURVE('',#37908,#37912,#5391,.T.);
#47737=EDGE_CURVE('',#37907,#37911,#5392,.T.);
#47738=EDGE_CURVE('',#37913,#37914,#5393,.T.);
#47739=EDGE_CURVE('',#37912,#37914,#5394,.T.);
#47740=EDGE_CURVE('',#37911,#37913,#5395,.T.);
#47741=EDGE_CURVE('',#37914,#37909,#5396,.T.);
#47742=EDGE_CURVE('',#37913,#37910,#5397,.T.);
#47743=EDGE_CURVE('',#37915,#37916,#5398,.T.);
#47744=EDGE_CURVE('',#37917,#37916,#5399,.T.);
#47745=EDGE_CURVE('',#37918,#37917,#5400,.T.);
#47746=EDGE_CURVE('',#37918,#37915,#5401,.T.);
#47747=EDGE_CURVE('',#37919,#37920,#5402,.T.);
#47748=EDGE_CURVE('',#37916,#37920,#5403,.T.);
#47749=EDGE_CURVE('',#37915,#37919,#5404,.T.);
#47750=EDGE_CURVE('',#37921,#37922,#5405,.T.);
#47751=EDGE_CURVE('',#37920,#37922,#5406,.T.);
#47752=EDGE_CURVE('',#37919,#37921,#5407,.T.);
#47753=EDGE_CURVE('',#37922,#37917,#5408,.T.);
#47754=EDGE_CURVE('',#37921,#37918,#5409,.T.);
#47755=EDGE_CURVE('',#37923,#37924,#5410,.T.);
#47756=EDGE_CURVE('',#37925,#37924,#5411,.T.);
#47757=EDGE_CURVE('',#37926,#37925,#5412,.T.);
#47758=EDGE_CURVE('',#37926,#37923,#5413,.T.);
#47759=EDGE_CURVE('',#37927,#37928,#5414,.T.);
#47760=EDGE_CURVE('',#37924,#37928,#5415,.T.);
#47761=EDGE_CURVE('',#37923,#37927,#5416,.T.);
#47762=EDGE_CURVE('',#37929,#37930,#5417,.T.);
#47763=EDGE_CURVE('',#37928,#37930,#5418,.T.);
#47764=EDGE_CURVE('',#37927,#37929,#5419,.T.);
#47765=EDGE_CURVE('',#37930,#37925,#5420,.T.);
#47766=EDGE_CURVE('',#37929,#37926,#5421,.T.);
#47767=EDGE_CURVE('',#37931,#37932,#5422,.T.);
#47768=EDGE_CURVE('',#37933,#37932,#5423,.T.);
#47769=EDGE_CURVE('',#37934,#37933,#5424,.T.);
#47770=EDGE_CURVE('',#37934,#37931,#5425,.T.);
#47771=EDGE_CURVE('',#37935,#37936,#5426,.T.);
#47772=EDGE_CURVE('',#37932,#37936,#5427,.T.);
#47773=EDGE_CURVE('',#37931,#37935,#5428,.T.);
#47774=EDGE_CURVE('',#37937,#37938,#5429,.T.);
#47775=EDGE_CURVE('',#37936,#37938,#5430,.T.);
#47776=EDGE_CURVE('',#37935,#37937,#5431,.T.);
#47777=EDGE_CURVE('',#37938,#37933,#5432,.T.);
#47778=EDGE_CURVE('',#37937,#37934,#5433,.T.);
#47779=EDGE_CURVE('',#37939,#37940,#5434,.T.);
#47780=EDGE_CURVE('',#37941,#37940,#5435,.T.);
#47781=EDGE_CURVE('',#37942,#37941,#5436,.T.);
#47782=EDGE_CURVE('',#37942,#37939,#5437,.T.);
#47783=EDGE_CURVE('',#37943,#37944,#5438,.T.);
#47784=EDGE_CURVE('',#37940,#37944,#5439,.T.);
#47785=EDGE_CURVE('',#37939,#37943,#5440,.T.);
#47786=EDGE_CURVE('',#37945,#37946,#5441,.T.);
#47787=EDGE_CURVE('',#37944,#37946,#5442,.T.);
#47788=EDGE_CURVE('',#37943,#37945,#5443,.T.);
#47789=EDGE_CURVE('',#37946,#37941,#5444,.T.);
#47790=EDGE_CURVE('',#37945,#37942,#5445,.T.);
#47791=EDGE_CURVE('',#37947,#37948,#5446,.T.);
#47792=EDGE_CURVE('',#37949,#37948,#5447,.T.);
#47793=EDGE_CURVE('',#37950,#37949,#5448,.T.);
#47794=EDGE_CURVE('',#37950,#37947,#5449,.T.);
#47795=EDGE_CURVE('',#37951,#37952,#5450,.T.);
#47796=EDGE_CURVE('',#37948,#37952,#5451,.T.);
#47797=EDGE_CURVE('',#37947,#37951,#5452,.T.);
#47798=EDGE_CURVE('',#37953,#37954,#5453,.T.);
#47799=EDGE_CURVE('',#37952,#37954,#5454,.T.);
#47800=EDGE_CURVE('',#37951,#37953,#5455,.T.);
#47801=EDGE_CURVE('',#37954,#37949,#5456,.T.);
#47802=EDGE_CURVE('',#37953,#37950,#5457,.T.);
#47803=EDGE_CURVE('',#37955,#37956,#5458,.T.);
#47804=EDGE_CURVE('',#37957,#37956,#5459,.T.);
#47805=EDGE_CURVE('',#37958,#37957,#5460,.T.);
#47806=EDGE_CURVE('',#37958,#37955,#5461,.T.);
#47807=EDGE_CURVE('',#37959,#37960,#5462,.T.);
#47808=EDGE_CURVE('',#37956,#37960,#5463,.T.);
#47809=EDGE_CURVE('',#37955,#37959,#5464,.T.);
#47810=EDGE_CURVE('',#37961,#37962,#5465,.T.);
#47811=EDGE_CURVE('',#37960,#37962,#5466,.T.);
#47812=EDGE_CURVE('',#37959,#37961,#5467,.T.);
#47813=EDGE_CURVE('',#37962,#37957,#5468,.T.);
#47814=EDGE_CURVE('',#37961,#37958,#5469,.T.);
#47815=EDGE_CURVE('',#37963,#37964,#5470,.T.);
#47816=EDGE_CURVE('',#37965,#37964,#5471,.T.);
#47817=EDGE_CURVE('',#37966,#37965,#5472,.T.);
#47818=EDGE_CURVE('',#37966,#37963,#5473,.T.);
#47819=EDGE_CURVE('',#37967,#37968,#5474,.T.);
#47820=EDGE_CURVE('',#37964,#37968,#5475,.T.);
#47821=EDGE_CURVE('',#37963,#37967,#5476,.T.);
#47822=EDGE_CURVE('',#37969,#37970,#5477,.T.);
#47823=EDGE_CURVE('',#37968,#37970,#5478,.T.);
#47824=EDGE_CURVE('',#37967,#37969,#5479,.T.);
#47825=EDGE_CURVE('',#37970,#37965,#5480,.T.);
#47826=EDGE_CURVE('',#37969,#37966,#5481,.T.);
#47827=EDGE_CURVE('',#37971,#37972,#5482,.T.);
#47828=EDGE_CURVE('',#37973,#37972,#5483,.T.);
#47829=EDGE_CURVE('',#37974,#37973,#5484,.T.);
#47830=EDGE_CURVE('',#37974,#37971,#5485,.T.);
#47831=EDGE_CURVE('',#37975,#37976,#5486,.T.);
#47832=EDGE_CURVE('',#37972,#37976,#5487,.T.);
#47833=EDGE_CURVE('',#37971,#37975,#5488,.T.);
#47834=EDGE_CURVE('',#37977,#37978,#5489,.T.);
#47835=EDGE_CURVE('',#37976,#37978,#5490,.T.);
#47836=EDGE_CURVE('',#37975,#37977,#5491,.T.);
#47837=EDGE_CURVE('',#37978,#37973,#5492,.T.);
#47838=EDGE_CURVE('',#37977,#37974,#5493,.T.);
#47839=EDGE_CURVE('',#37979,#37980,#5494,.T.);
#47840=EDGE_CURVE('',#37981,#37980,#5495,.T.);
#47841=EDGE_CURVE('',#37982,#37981,#5496,.T.);
#47842=EDGE_CURVE('',#37982,#37979,#5497,.T.);
#47843=EDGE_CURVE('',#37983,#37984,#5498,.T.);
#47844=EDGE_CURVE('',#37980,#37984,#5499,.T.);
#47845=EDGE_CURVE('',#37979,#37983,#5500,.T.);
#47846=EDGE_CURVE('',#37985,#37986,#5501,.T.);
#47847=EDGE_CURVE('',#37984,#37986,#5502,.T.);
#47848=EDGE_CURVE('',#37983,#37985,#5503,.T.);
#47849=EDGE_CURVE('',#37986,#37981,#5504,.T.);
#47850=EDGE_CURVE('',#37985,#37982,#5505,.T.);
#47851=EDGE_CURVE('',#37987,#37988,#5506,.T.);
#47852=EDGE_CURVE('',#37989,#37988,#5507,.T.);
#47853=EDGE_CURVE('',#37990,#37989,#5508,.T.);
#47854=EDGE_CURVE('',#37990,#37987,#5509,.T.);
#47855=EDGE_CURVE('',#37991,#37992,#5510,.T.);
#47856=EDGE_CURVE('',#37988,#37992,#5511,.T.);
#47857=EDGE_CURVE('',#37987,#37991,#5512,.T.);
#47858=EDGE_CURVE('',#37993,#37994,#5513,.T.);
#47859=EDGE_CURVE('',#37992,#37994,#5514,.T.);
#47860=EDGE_CURVE('',#37991,#37993,#5515,.T.);
#47861=EDGE_CURVE('',#37994,#37989,#5516,.T.);
#47862=EDGE_CURVE('',#37993,#37990,#5517,.T.);
#47863=EDGE_CURVE('',#37995,#37996,#5518,.T.);
#47864=EDGE_CURVE('',#37997,#37996,#5519,.T.);
#47865=EDGE_CURVE('',#37998,#37997,#5520,.T.);
#47866=EDGE_CURVE('',#37998,#37995,#5521,.T.);
#47867=EDGE_CURVE('',#37999,#38000,#5522,.T.);
#47868=EDGE_CURVE('',#37996,#38000,#5523,.T.);
#47869=EDGE_CURVE('',#37995,#37999,#5524,.T.);
#47870=EDGE_CURVE('',#38001,#38002,#5525,.T.);
#47871=EDGE_CURVE('',#38000,#38002,#5526,.T.);
#47872=EDGE_CURVE('',#37999,#38001,#5527,.T.);
#47873=EDGE_CURVE('',#38002,#37997,#5528,.T.);
#47874=EDGE_CURVE('',#38001,#37998,#5529,.T.);
#47875=EDGE_CURVE('',#38003,#38004,#5530,.T.);
#47876=EDGE_CURVE('',#38005,#38004,#5531,.T.);
#47877=EDGE_CURVE('',#38006,#38005,#5532,.T.);
#47878=EDGE_CURVE('',#38006,#38003,#5533,.T.);
#47879=EDGE_CURVE('',#38007,#38008,#5534,.T.);
#47880=EDGE_CURVE('',#38004,#38008,#5535,.T.);
#47881=EDGE_CURVE('',#38003,#38007,#5536,.T.);
#47882=EDGE_CURVE('',#38009,#38010,#5537,.T.);
#47883=EDGE_CURVE('',#38008,#38010,#5538,.T.);
#47884=EDGE_CURVE('',#38007,#38009,#5539,.T.);
#47885=EDGE_CURVE('',#38010,#38005,#5540,.T.);
#47886=EDGE_CURVE('',#38009,#38006,#5541,.T.);
#47887=EDGE_CURVE('',#38011,#38012,#5542,.T.);
#47888=EDGE_CURVE('',#38013,#38012,#5543,.T.);
#47889=EDGE_CURVE('',#38014,#38013,#5544,.T.);
#47890=EDGE_CURVE('',#38014,#38011,#5545,.T.);
#47891=EDGE_CURVE('',#38015,#38016,#5546,.T.);
#47892=EDGE_CURVE('',#38012,#38016,#5547,.T.);
#47893=EDGE_CURVE('',#38011,#38015,#5548,.T.);
#47894=EDGE_CURVE('',#38017,#38018,#5549,.T.);
#47895=EDGE_CURVE('',#38016,#38018,#5550,.T.);
#47896=EDGE_CURVE('',#38015,#38017,#5551,.T.);
#47897=EDGE_CURVE('',#38018,#38013,#5552,.T.);
#47898=EDGE_CURVE('',#38017,#38014,#5553,.T.);
#47899=EDGE_CURVE('',#38019,#38020,#5554,.T.);
#47900=EDGE_CURVE('',#38021,#38020,#5555,.T.);
#47901=EDGE_CURVE('',#38022,#38021,#5556,.T.);
#47902=EDGE_CURVE('',#38022,#38019,#5557,.T.);
#47903=EDGE_CURVE('',#38023,#38024,#5558,.T.);
#47904=EDGE_CURVE('',#38020,#38024,#5559,.T.);
#47905=EDGE_CURVE('',#38019,#38023,#5560,.T.);
#47906=EDGE_CURVE('',#38025,#38026,#5561,.T.);
#47907=EDGE_CURVE('',#38024,#38026,#5562,.T.);
#47908=EDGE_CURVE('',#38023,#38025,#5563,.T.);
#47909=EDGE_CURVE('',#38026,#38021,#5564,.T.);
#47910=EDGE_CURVE('',#38025,#38022,#5565,.T.);
#47911=EDGE_CURVE('',#38027,#38028,#5566,.T.);
#47912=EDGE_CURVE('',#38029,#38028,#5567,.T.);
#47913=EDGE_CURVE('',#38030,#38029,#5568,.T.);
#47914=EDGE_CURVE('',#38030,#38027,#5569,.T.);
#47915=EDGE_CURVE('',#38031,#38032,#5570,.T.);
#47916=EDGE_CURVE('',#38028,#38032,#5571,.T.);
#47917=EDGE_CURVE('',#38027,#38031,#5572,.T.);
#47918=EDGE_CURVE('',#38033,#38034,#5573,.T.);
#47919=EDGE_CURVE('',#38032,#38034,#5574,.T.);
#47920=EDGE_CURVE('',#38031,#38033,#5575,.T.);
#47921=EDGE_CURVE('',#38034,#38029,#5576,.T.);
#47922=EDGE_CURVE('',#38033,#38030,#5577,.T.);
#47923=EDGE_CURVE('',#38035,#38036,#5578,.T.);
#47924=EDGE_CURVE('',#38037,#38036,#5579,.T.);
#47925=EDGE_CURVE('',#38038,#38037,#5580,.T.);
#47926=EDGE_CURVE('',#38038,#38035,#5581,.T.);
#47927=EDGE_CURVE('',#38039,#38040,#5582,.T.);
#47928=EDGE_CURVE('',#38036,#38040,#5583,.T.);
#47929=EDGE_CURVE('',#38035,#38039,#5584,.T.);
#47930=EDGE_CURVE('',#38041,#38042,#5585,.T.);
#47931=EDGE_CURVE('',#38040,#38042,#5586,.T.);
#47932=EDGE_CURVE('',#38039,#38041,#5587,.T.);
#47933=EDGE_CURVE('',#38042,#38037,#5588,.T.);
#47934=EDGE_CURVE('',#38041,#38038,#5589,.T.);
#47935=EDGE_CURVE('',#38043,#38044,#5590,.T.);
#47936=EDGE_CURVE('',#38045,#38044,#5591,.T.);
#47937=EDGE_CURVE('',#38046,#38045,#5592,.T.);
#47938=EDGE_CURVE('',#38046,#38043,#5593,.T.);
#47939=EDGE_CURVE('',#38047,#38048,#5594,.T.);
#47940=EDGE_CURVE('',#38044,#38048,#5595,.T.);
#47941=EDGE_CURVE('',#38043,#38047,#5596,.T.);
#47942=EDGE_CURVE('',#38049,#38050,#5597,.T.);
#47943=EDGE_CURVE('',#38048,#38050,#5598,.T.);
#47944=EDGE_CURVE('',#38047,#38049,#5599,.T.);
#47945=EDGE_CURVE('',#38050,#38045,#5600,.T.);
#47946=EDGE_CURVE('',#38049,#38046,#5601,.T.);
#47947=EDGE_CURVE('',#38051,#38052,#5602,.T.);
#47948=EDGE_CURVE('',#38053,#38052,#5603,.T.);
#47949=EDGE_CURVE('',#38054,#38053,#5604,.T.);
#47950=EDGE_CURVE('',#38054,#38051,#5605,.T.);
#47951=EDGE_CURVE('',#38055,#38056,#5606,.T.);
#47952=EDGE_CURVE('',#38052,#38056,#5607,.T.);
#47953=EDGE_CURVE('',#38051,#38055,#5608,.T.);
#47954=EDGE_CURVE('',#38057,#38058,#5609,.T.);
#47955=EDGE_CURVE('',#38056,#38058,#5610,.T.);
#47956=EDGE_CURVE('',#38055,#38057,#5611,.T.);
#47957=EDGE_CURVE('',#38058,#38053,#5612,.T.);
#47958=EDGE_CURVE('',#38057,#38054,#5613,.T.);
#47959=EDGE_CURVE('',#38059,#38060,#5614,.T.);
#47960=EDGE_CURVE('',#38061,#38060,#5615,.T.);
#47961=EDGE_CURVE('',#38062,#38061,#5616,.T.);
#47962=EDGE_CURVE('',#38062,#38059,#5617,.T.);
#47963=EDGE_CURVE('',#38063,#38064,#5618,.T.);
#47964=EDGE_CURVE('',#38060,#38064,#5619,.T.);
#47965=EDGE_CURVE('',#38059,#38063,#5620,.T.);
#47966=EDGE_CURVE('',#38065,#38066,#5621,.T.);
#47967=EDGE_CURVE('',#38064,#38066,#5622,.T.);
#47968=EDGE_CURVE('',#38063,#38065,#5623,.T.);
#47969=EDGE_CURVE('',#38066,#38061,#5624,.T.);
#47970=EDGE_CURVE('',#38065,#38062,#5625,.T.);
#47971=EDGE_CURVE('',#38067,#38068,#5626,.T.);
#47972=EDGE_CURVE('',#38069,#38068,#5627,.T.);
#47973=EDGE_CURVE('',#38070,#38069,#5628,.T.);
#47974=EDGE_CURVE('',#38070,#38067,#5629,.T.);
#47975=EDGE_CURVE('',#38071,#38072,#5630,.T.);
#47976=EDGE_CURVE('',#38068,#38072,#5631,.T.);
#47977=EDGE_CURVE('',#38067,#38071,#5632,.T.);
#47978=EDGE_CURVE('',#38073,#38074,#5633,.T.);
#47979=EDGE_CURVE('',#38072,#38074,#5634,.T.);
#47980=EDGE_CURVE('',#38071,#38073,#5635,.T.);
#47981=EDGE_CURVE('',#38074,#38069,#5636,.T.);
#47982=EDGE_CURVE('',#38073,#38070,#5637,.T.);
#47983=EDGE_CURVE('',#38075,#38076,#5638,.T.);
#47984=EDGE_CURVE('',#38077,#38076,#5639,.T.);
#47985=EDGE_CURVE('',#38078,#38077,#5640,.T.);
#47986=EDGE_CURVE('',#38078,#38075,#5641,.T.);
#47987=EDGE_CURVE('',#38079,#38080,#5642,.T.);
#47988=EDGE_CURVE('',#38076,#38080,#5643,.T.);
#47989=EDGE_CURVE('',#38075,#38079,#5644,.T.);
#47990=EDGE_CURVE('',#38081,#38082,#5645,.T.);
#47991=EDGE_CURVE('',#38080,#38082,#5646,.T.);
#47992=EDGE_CURVE('',#38079,#38081,#5647,.T.);
#47993=EDGE_CURVE('',#38082,#38077,#5648,.T.);
#47994=EDGE_CURVE('',#38081,#38078,#5649,.T.);
#47995=EDGE_CURVE('',#38083,#38084,#5650,.T.);
#47996=EDGE_CURVE('',#38085,#38084,#5651,.T.);
#47997=EDGE_CURVE('',#38086,#38085,#5652,.T.);
#47998=EDGE_CURVE('',#38086,#38083,#5653,.T.);
#47999=EDGE_CURVE('',#38087,#38088,#5654,.T.);
#48000=EDGE_CURVE('',#38084,#38088,#5655,.T.);
#48001=EDGE_CURVE('',#38083,#38087,#5656,.T.);
#48002=EDGE_CURVE('',#38089,#38090,#5657,.T.);
#48003=EDGE_CURVE('',#38088,#38090,#5658,.T.);
#48004=EDGE_CURVE('',#38087,#38089,#5659,.T.);
#48005=EDGE_CURVE('',#38090,#38085,#5660,.T.);
#48006=EDGE_CURVE('',#38089,#38086,#5661,.T.);
#48007=EDGE_CURVE('',#38091,#38092,#5662,.T.);
#48008=EDGE_CURVE('',#38093,#38092,#5663,.T.);
#48009=EDGE_CURVE('',#38094,#38093,#5664,.T.);
#48010=EDGE_CURVE('',#38094,#38091,#5665,.T.);
#48011=EDGE_CURVE('',#38095,#38096,#5666,.T.);
#48012=EDGE_CURVE('',#38092,#38096,#5667,.T.);
#48013=EDGE_CURVE('',#38091,#38095,#5668,.T.);
#48014=EDGE_CURVE('',#38097,#38098,#5669,.T.);
#48015=EDGE_CURVE('',#38096,#38098,#5670,.T.);
#48016=EDGE_CURVE('',#38095,#38097,#5671,.T.);
#48017=EDGE_CURVE('',#38098,#38093,#5672,.T.);
#48018=EDGE_CURVE('',#38097,#38094,#5673,.T.);
#48019=EDGE_CURVE('',#38099,#38100,#5674,.T.);
#48020=EDGE_CURVE('',#38101,#38100,#5675,.T.);
#48021=EDGE_CURVE('',#38102,#38101,#5676,.T.);
#48022=EDGE_CURVE('',#38102,#38099,#5677,.T.);
#48023=EDGE_CURVE('',#38103,#38104,#5678,.T.);
#48024=EDGE_CURVE('',#38100,#38104,#5679,.T.);
#48025=EDGE_CURVE('',#38099,#38103,#5680,.T.);
#48026=EDGE_CURVE('',#38105,#38106,#5681,.T.);
#48027=EDGE_CURVE('',#38104,#38106,#5682,.T.);
#48028=EDGE_CURVE('',#38103,#38105,#5683,.T.);
#48029=EDGE_CURVE('',#38106,#38101,#5684,.T.);
#48030=EDGE_CURVE('',#38105,#38102,#5685,.T.);
#48031=EDGE_CURVE('',#38107,#38108,#5686,.T.);
#48032=EDGE_CURVE('',#38109,#38108,#5687,.T.);
#48033=EDGE_CURVE('',#38110,#38109,#5688,.T.);
#48034=EDGE_CURVE('',#38110,#38107,#5689,.T.);
#48035=EDGE_CURVE('',#38111,#38112,#5690,.T.);
#48036=EDGE_CURVE('',#38108,#38112,#5691,.T.);
#48037=EDGE_CURVE('',#38107,#38111,#5692,.T.);
#48038=EDGE_CURVE('',#38113,#38114,#5693,.T.);
#48039=EDGE_CURVE('',#38112,#38114,#5694,.T.);
#48040=EDGE_CURVE('',#38111,#38113,#5695,.T.);
#48041=EDGE_CURVE('',#38114,#38109,#5696,.T.);
#48042=EDGE_CURVE('',#38113,#38110,#5697,.T.);
#48043=EDGE_CURVE('',#38115,#38116,#5698,.T.);
#48044=EDGE_CURVE('',#38117,#38116,#5699,.T.);
#48045=EDGE_CURVE('',#38118,#38117,#5700,.T.);
#48046=EDGE_CURVE('',#38118,#38115,#5701,.T.);
#48047=EDGE_CURVE('',#38119,#38120,#5702,.T.);
#48048=EDGE_CURVE('',#38116,#38120,#5703,.T.);
#48049=EDGE_CURVE('',#38115,#38119,#5704,.T.);
#48050=EDGE_CURVE('',#38121,#38122,#5705,.T.);
#48051=EDGE_CURVE('',#38120,#38122,#5706,.T.);
#48052=EDGE_CURVE('',#38119,#38121,#5707,.T.);
#48053=EDGE_CURVE('',#38122,#38117,#5708,.T.);
#48054=EDGE_CURVE('',#38121,#38118,#5709,.T.);
#48055=EDGE_CURVE('',#38123,#38124,#5710,.T.);
#48056=EDGE_CURVE('',#38125,#38124,#5711,.T.);
#48057=EDGE_CURVE('',#38126,#38125,#5712,.T.);
#48058=EDGE_CURVE('',#38126,#38123,#5713,.T.);
#48059=EDGE_CURVE('',#38127,#38128,#5714,.T.);
#48060=EDGE_CURVE('',#38124,#38128,#5715,.T.);
#48061=EDGE_CURVE('',#38123,#38127,#5716,.T.);
#48062=EDGE_CURVE('',#38129,#38130,#5717,.T.);
#48063=EDGE_CURVE('',#38128,#38130,#5718,.T.);
#48064=EDGE_CURVE('',#38127,#38129,#5719,.T.);
#48065=EDGE_CURVE('',#38130,#38125,#5720,.T.);
#48066=EDGE_CURVE('',#38129,#38126,#5721,.T.);
#48067=EDGE_CURVE('',#38131,#38132,#5722,.T.);
#48068=EDGE_CURVE('',#38133,#38132,#5723,.T.);
#48069=EDGE_CURVE('',#38134,#38133,#5724,.T.);
#48070=EDGE_CURVE('',#38134,#38131,#5725,.T.);
#48071=EDGE_CURVE('',#38135,#38136,#5726,.T.);
#48072=EDGE_CURVE('',#38132,#38136,#5727,.T.);
#48073=EDGE_CURVE('',#38131,#38135,#5728,.T.);
#48074=EDGE_CURVE('',#38137,#38138,#5729,.T.);
#48075=EDGE_CURVE('',#38136,#38138,#5730,.T.);
#48076=EDGE_CURVE('',#38135,#38137,#5731,.T.);
#48077=EDGE_CURVE('',#38138,#38133,#5732,.T.);
#48078=EDGE_CURVE('',#38137,#38134,#5733,.T.);
#48079=EDGE_CURVE('',#38139,#38140,#5734,.T.);
#48080=EDGE_CURVE('',#38141,#38140,#5735,.T.);
#48081=EDGE_CURVE('',#38142,#38141,#5736,.T.);
#48082=EDGE_CURVE('',#38142,#38139,#5737,.T.);
#48083=EDGE_CURVE('',#38143,#38144,#5738,.T.);
#48084=EDGE_CURVE('',#38140,#38144,#5739,.T.);
#48085=EDGE_CURVE('',#38139,#38143,#5740,.T.);
#48086=EDGE_CURVE('',#38145,#38146,#5741,.T.);
#48087=EDGE_CURVE('',#38144,#38146,#5742,.T.);
#48088=EDGE_CURVE('',#38143,#38145,#5743,.T.);
#48089=EDGE_CURVE('',#38146,#38141,#5744,.T.);
#48090=EDGE_CURVE('',#38145,#38142,#5745,.T.);
#48091=EDGE_CURVE('',#38147,#38148,#5746,.T.);
#48092=EDGE_CURVE('',#38149,#38148,#5747,.T.);
#48093=EDGE_CURVE('',#38150,#38149,#5748,.T.);
#48094=EDGE_CURVE('',#38150,#38147,#5749,.T.);
#48095=EDGE_CURVE('',#38151,#38152,#5750,.T.);
#48096=EDGE_CURVE('',#38148,#38152,#5751,.T.);
#48097=EDGE_CURVE('',#38147,#38151,#5752,.T.);
#48098=EDGE_CURVE('',#38153,#38154,#5753,.T.);
#48099=EDGE_CURVE('',#38152,#38154,#5754,.T.);
#48100=EDGE_CURVE('',#38151,#38153,#5755,.T.);
#48101=EDGE_CURVE('',#38154,#38149,#5756,.T.);
#48102=EDGE_CURVE('',#38153,#38150,#5757,.T.);
#48103=EDGE_CURVE('',#38155,#38156,#5758,.T.);
#48104=EDGE_CURVE('',#38157,#38156,#5759,.T.);
#48105=EDGE_CURVE('',#38158,#38157,#5760,.T.);
#48106=EDGE_CURVE('',#38158,#38155,#5761,.T.);
#48107=EDGE_CURVE('',#38159,#38160,#5762,.T.);
#48108=EDGE_CURVE('',#38156,#38160,#5763,.T.);
#48109=EDGE_CURVE('',#38155,#38159,#5764,.T.);
#48110=EDGE_CURVE('',#38161,#38162,#5765,.T.);
#48111=EDGE_CURVE('',#38160,#38162,#5766,.T.);
#48112=EDGE_CURVE('',#38159,#38161,#5767,.T.);
#48113=EDGE_CURVE('',#38162,#38157,#5768,.T.);
#48114=EDGE_CURVE('',#38161,#38158,#5769,.T.);
#48115=EDGE_CURVE('',#38163,#38164,#5770,.T.);
#48116=EDGE_CURVE('',#38165,#38164,#5771,.T.);
#48117=EDGE_CURVE('',#38166,#38165,#5772,.T.);
#48118=EDGE_CURVE('',#38166,#38163,#5773,.T.);
#48119=EDGE_CURVE('',#38167,#38168,#5774,.T.);
#48120=EDGE_CURVE('',#38164,#38168,#5775,.T.);
#48121=EDGE_CURVE('',#38163,#38167,#5776,.T.);
#48122=EDGE_CURVE('',#38169,#38170,#5777,.T.);
#48123=EDGE_CURVE('',#38168,#38170,#5778,.T.);
#48124=EDGE_CURVE('',#38167,#38169,#5779,.T.);
#48125=EDGE_CURVE('',#38170,#38165,#5780,.T.);
#48126=EDGE_CURVE('',#38169,#38166,#5781,.T.);
#48127=EDGE_CURVE('',#38171,#38172,#5782,.T.);
#48128=EDGE_CURVE('',#38173,#38172,#5783,.T.);
#48129=EDGE_CURVE('',#38174,#38173,#5784,.T.);
#48130=EDGE_CURVE('',#38174,#38171,#5785,.T.);
#48131=EDGE_CURVE('',#38175,#38176,#5786,.T.);
#48132=EDGE_CURVE('',#38172,#38176,#5787,.T.);
#48133=EDGE_CURVE('',#38171,#38175,#5788,.T.);
#48134=EDGE_CURVE('',#38177,#38178,#5789,.T.);
#48135=EDGE_CURVE('',#38176,#38178,#5790,.T.);
#48136=EDGE_CURVE('',#38175,#38177,#5791,.T.);
#48137=EDGE_CURVE('',#38178,#38173,#5792,.T.);
#48138=EDGE_CURVE('',#38177,#38174,#5793,.T.);
#48139=EDGE_CURVE('',#38179,#38180,#5794,.T.);
#48140=EDGE_CURVE('',#38181,#38180,#5795,.T.);
#48141=EDGE_CURVE('',#38182,#38181,#5796,.T.);
#48142=EDGE_CURVE('',#38182,#38179,#5797,.T.);
#48143=EDGE_CURVE('',#38183,#38184,#5798,.T.);
#48144=EDGE_CURVE('',#38180,#38184,#5799,.T.);
#48145=EDGE_CURVE('',#38179,#38183,#5800,.T.);
#48146=EDGE_CURVE('',#38185,#38186,#5801,.T.);
#48147=EDGE_CURVE('',#38184,#38186,#5802,.T.);
#48148=EDGE_CURVE('',#38183,#38185,#5803,.T.);
#48149=EDGE_CURVE('',#38186,#38181,#5804,.T.);
#48150=EDGE_CURVE('',#38185,#38182,#5805,.T.);
#48151=EDGE_CURVE('',#38187,#38188,#5806,.T.);
#48152=EDGE_CURVE('',#38189,#38188,#5807,.T.);
#48153=EDGE_CURVE('',#38190,#38189,#5808,.T.);
#48154=EDGE_CURVE('',#38190,#38187,#5809,.T.);
#48155=EDGE_CURVE('',#38191,#38192,#5810,.T.);
#48156=EDGE_CURVE('',#38188,#38192,#5811,.T.);
#48157=EDGE_CURVE('',#38187,#38191,#5812,.T.);
#48158=EDGE_CURVE('',#38193,#38194,#5813,.T.);
#48159=EDGE_CURVE('',#38192,#38194,#5814,.T.);
#48160=EDGE_CURVE('',#38191,#38193,#5815,.T.);
#48161=EDGE_CURVE('',#38194,#38189,#5816,.T.);
#48162=EDGE_CURVE('',#38193,#38190,#5817,.T.);
#48163=EDGE_CURVE('',#38195,#38196,#5818,.T.);
#48164=EDGE_CURVE('',#38197,#38196,#5819,.T.);
#48165=EDGE_CURVE('',#38198,#38197,#5820,.T.);
#48166=EDGE_CURVE('',#38198,#38195,#5821,.T.);
#48167=EDGE_CURVE('',#38199,#38200,#5822,.T.);
#48168=EDGE_CURVE('',#38196,#38200,#5823,.T.);
#48169=EDGE_CURVE('',#38195,#38199,#5824,.T.);
#48170=EDGE_CURVE('',#38201,#38202,#5825,.T.);
#48171=EDGE_CURVE('',#38200,#38202,#5826,.T.);
#48172=EDGE_CURVE('',#38199,#38201,#5827,.T.);
#48173=EDGE_CURVE('',#38202,#38197,#5828,.T.);
#48174=EDGE_CURVE('',#38201,#38198,#5829,.T.);
#48175=EDGE_CURVE('',#38203,#38204,#5830,.T.);
#48176=EDGE_CURVE('',#38205,#38204,#5831,.T.);
#48177=EDGE_CURVE('',#38206,#38205,#5832,.T.);
#48178=EDGE_CURVE('',#38206,#38203,#5833,.T.);
#48179=EDGE_CURVE('',#38207,#38208,#5834,.T.);
#48180=EDGE_CURVE('',#38204,#38208,#5835,.T.);
#48181=EDGE_CURVE('',#38203,#38207,#5836,.T.);
#48182=EDGE_CURVE('',#38209,#38210,#5837,.T.);
#48183=EDGE_CURVE('',#38208,#38210,#5838,.T.);
#48184=EDGE_CURVE('',#38207,#38209,#5839,.T.);
#48185=EDGE_CURVE('',#38210,#38205,#5840,.T.);
#48186=EDGE_CURVE('',#38209,#38206,#5841,.T.);
#48187=EDGE_CURVE('',#38211,#38212,#5842,.T.);
#48188=EDGE_CURVE('',#38213,#38212,#5843,.T.);
#48189=EDGE_CURVE('',#38214,#38213,#5844,.T.);
#48190=EDGE_CURVE('',#38214,#38211,#5845,.T.);
#48191=EDGE_CURVE('',#38215,#38216,#5846,.T.);
#48192=EDGE_CURVE('',#38212,#38216,#5847,.T.);
#48193=EDGE_CURVE('',#38211,#38215,#5848,.T.);
#48194=EDGE_CURVE('',#38217,#38218,#5849,.T.);
#48195=EDGE_CURVE('',#38216,#38218,#5850,.T.);
#48196=EDGE_CURVE('',#38215,#38217,#5851,.T.);
#48197=EDGE_CURVE('',#38218,#38213,#5852,.T.);
#48198=EDGE_CURVE('',#38217,#38214,#5853,.T.);
#48199=EDGE_CURVE('',#38219,#38220,#5854,.T.);
#48200=EDGE_CURVE('',#38221,#38220,#5855,.T.);
#48201=EDGE_CURVE('',#38222,#38221,#5856,.T.);
#48202=EDGE_CURVE('',#38222,#38219,#5857,.T.);
#48203=EDGE_CURVE('',#38223,#38224,#5858,.T.);
#48204=EDGE_CURVE('',#38220,#38224,#5859,.T.);
#48205=EDGE_CURVE('',#38219,#38223,#5860,.T.);
#48206=EDGE_CURVE('',#38225,#38226,#5861,.T.);
#48207=EDGE_CURVE('',#38224,#38226,#5862,.T.);
#48208=EDGE_CURVE('',#38223,#38225,#5863,.T.);
#48209=EDGE_CURVE('',#38226,#38221,#5864,.T.);
#48210=EDGE_CURVE('',#38225,#38222,#5865,.T.);
#48211=EDGE_CURVE('',#38227,#38228,#5866,.T.);
#48212=EDGE_CURVE('',#38229,#38228,#5867,.T.);
#48213=EDGE_CURVE('',#38230,#38229,#5868,.T.);
#48214=EDGE_CURVE('',#38230,#38227,#5869,.T.);
#48215=EDGE_CURVE('',#38231,#38232,#5870,.T.);
#48216=EDGE_CURVE('',#38228,#38232,#5871,.T.);
#48217=EDGE_CURVE('',#38227,#38231,#5872,.T.);
#48218=EDGE_CURVE('',#38233,#38234,#5873,.T.);
#48219=EDGE_CURVE('',#38232,#38234,#5874,.T.);
#48220=EDGE_CURVE('',#38231,#38233,#5875,.T.);
#48221=EDGE_CURVE('',#38234,#38229,#5876,.T.);
#48222=EDGE_CURVE('',#38233,#38230,#5877,.T.);
#48223=EDGE_CURVE('',#38235,#38236,#5878,.T.);
#48224=EDGE_CURVE('',#38237,#38236,#5879,.T.);
#48225=EDGE_CURVE('',#38238,#38237,#5880,.T.);
#48226=EDGE_CURVE('',#38238,#38235,#5881,.T.);
#48227=EDGE_CURVE('',#38239,#38240,#5882,.T.);
#48228=EDGE_CURVE('',#38236,#38240,#5883,.T.);
#48229=EDGE_CURVE('',#38235,#38239,#5884,.T.);
#48230=EDGE_CURVE('',#38241,#38242,#5885,.T.);
#48231=EDGE_CURVE('',#38240,#38242,#5886,.T.);
#48232=EDGE_CURVE('',#38239,#38241,#5887,.T.);
#48233=EDGE_CURVE('',#38242,#38237,#5888,.T.);
#48234=EDGE_CURVE('',#38241,#38238,#5889,.T.);
#48235=EDGE_CURVE('',#38243,#38244,#5890,.T.);
#48236=EDGE_CURVE('',#38245,#38244,#5891,.T.);
#48237=EDGE_CURVE('',#38246,#38245,#5892,.T.);
#48238=EDGE_CURVE('',#38246,#38243,#5893,.T.);
#48239=EDGE_CURVE('',#38247,#38248,#5894,.T.);
#48240=EDGE_CURVE('',#38244,#38248,#5895,.T.);
#48241=EDGE_CURVE('',#38243,#38247,#5896,.T.);
#48242=EDGE_CURVE('',#38249,#38250,#5897,.T.);
#48243=EDGE_CURVE('',#38248,#38250,#5898,.T.);
#48244=EDGE_CURVE('',#38247,#38249,#5899,.T.);
#48245=EDGE_CURVE('',#38250,#38245,#5900,.T.);
#48246=EDGE_CURVE('',#38249,#38246,#5901,.T.);
#48247=EDGE_CURVE('',#38251,#38252,#5902,.T.);
#48248=EDGE_CURVE('',#38253,#38252,#5903,.T.);
#48249=EDGE_CURVE('',#38254,#38253,#5904,.T.);
#48250=EDGE_CURVE('',#38254,#38251,#5905,.T.);
#48251=EDGE_CURVE('',#38255,#38256,#5906,.T.);
#48252=EDGE_CURVE('',#38252,#38256,#5907,.T.);
#48253=EDGE_CURVE('',#38251,#38255,#5908,.T.);
#48254=EDGE_CURVE('',#38257,#38258,#5909,.T.);
#48255=EDGE_CURVE('',#38256,#38258,#5910,.T.);
#48256=EDGE_CURVE('',#38255,#38257,#5911,.T.);
#48257=EDGE_CURVE('',#38258,#38253,#5912,.T.);
#48258=EDGE_CURVE('',#38257,#38254,#5913,.T.);
#48259=EDGE_CURVE('',#38259,#38260,#5914,.T.);
#48260=EDGE_CURVE('',#38261,#38260,#5915,.T.);
#48261=EDGE_CURVE('',#38262,#38261,#5916,.T.);
#48262=EDGE_CURVE('',#38262,#38259,#5917,.T.);
#48263=EDGE_CURVE('',#38263,#38264,#5918,.T.);
#48264=EDGE_CURVE('',#38260,#38264,#5919,.T.);
#48265=EDGE_CURVE('',#38259,#38263,#5920,.T.);
#48266=EDGE_CURVE('',#38265,#38266,#5921,.T.);
#48267=EDGE_CURVE('',#38264,#38266,#5922,.T.);
#48268=EDGE_CURVE('',#38263,#38265,#5923,.T.);
#48269=EDGE_CURVE('',#38266,#38261,#5924,.T.);
#48270=EDGE_CURVE('',#38265,#38262,#5925,.T.);
#48271=EDGE_CURVE('',#38267,#38268,#5926,.T.);
#48272=EDGE_CURVE('',#38269,#38268,#5927,.T.);
#48273=EDGE_CURVE('',#38270,#38269,#5928,.T.);
#48274=EDGE_CURVE('',#38270,#38267,#5929,.T.);
#48275=EDGE_CURVE('',#38271,#38272,#5930,.T.);
#48276=EDGE_CURVE('',#38268,#38272,#5931,.T.);
#48277=EDGE_CURVE('',#38267,#38271,#5932,.T.);
#48278=EDGE_CURVE('',#38273,#38274,#5933,.T.);
#48279=EDGE_CURVE('',#38272,#38274,#5934,.T.);
#48280=EDGE_CURVE('',#38271,#38273,#5935,.T.);
#48281=EDGE_CURVE('',#38274,#38269,#5936,.T.);
#48282=EDGE_CURVE('',#38273,#38270,#5937,.T.);
#48283=EDGE_CURVE('',#38275,#38276,#5938,.T.);
#48284=EDGE_CURVE('',#38277,#38276,#5939,.T.);
#48285=EDGE_CURVE('',#38278,#38277,#5940,.T.);
#48286=EDGE_CURVE('',#38278,#38275,#5941,.T.);
#48287=EDGE_CURVE('',#38279,#38280,#5942,.T.);
#48288=EDGE_CURVE('',#38276,#38280,#5943,.T.);
#48289=EDGE_CURVE('',#38275,#38279,#5944,.T.);
#48290=EDGE_CURVE('',#38281,#38282,#5945,.T.);
#48291=EDGE_CURVE('',#38280,#38282,#5946,.T.);
#48292=EDGE_CURVE('',#38279,#38281,#5947,.T.);
#48293=EDGE_CURVE('',#38282,#38277,#5948,.T.);
#48294=EDGE_CURVE('',#38281,#38278,#5949,.T.);
#48295=EDGE_CURVE('',#38283,#38284,#5950,.T.);
#48296=EDGE_CURVE('',#38285,#38284,#5951,.T.);
#48297=EDGE_CURVE('',#38286,#38285,#5952,.T.);
#48298=EDGE_CURVE('',#38286,#38283,#5953,.T.);
#48299=EDGE_CURVE('',#38287,#38288,#5954,.T.);
#48300=EDGE_CURVE('',#38284,#38288,#5955,.T.);
#48301=EDGE_CURVE('',#38283,#38287,#5956,.T.);
#48302=EDGE_CURVE('',#38289,#38290,#5957,.T.);
#48303=EDGE_CURVE('',#38288,#38290,#5958,.T.);
#48304=EDGE_CURVE('',#38287,#38289,#5959,.T.);
#48305=EDGE_CURVE('',#38290,#38285,#5960,.T.);
#48306=EDGE_CURVE('',#38289,#38286,#5961,.T.);
#48307=EDGE_CURVE('',#38291,#38292,#5962,.T.);
#48308=EDGE_CURVE('',#38293,#38292,#5963,.T.);
#48309=EDGE_CURVE('',#38294,#38293,#5964,.T.);
#48310=EDGE_CURVE('',#38294,#38291,#5965,.T.);
#48311=EDGE_CURVE('',#38295,#38296,#5966,.T.);
#48312=EDGE_CURVE('',#38292,#38296,#5967,.T.);
#48313=EDGE_CURVE('',#38291,#38295,#5968,.T.);
#48314=EDGE_CURVE('',#38297,#38298,#5969,.T.);
#48315=EDGE_CURVE('',#38296,#38298,#5970,.T.);
#48316=EDGE_CURVE('',#38295,#38297,#5971,.T.);
#48317=EDGE_CURVE('',#38298,#38293,#5972,.T.);
#48318=EDGE_CURVE('',#38297,#38294,#5973,.T.);
#48319=EDGE_CURVE('',#38299,#38300,#5974,.T.);
#48320=EDGE_CURVE('',#38301,#38300,#5975,.T.);
#48321=EDGE_CURVE('',#38302,#38301,#5976,.T.);
#48322=EDGE_CURVE('',#38302,#38299,#5977,.T.);
#48323=EDGE_CURVE('',#38303,#38304,#5978,.T.);
#48324=EDGE_CURVE('',#38300,#38304,#5979,.T.);
#48325=EDGE_CURVE('',#38299,#38303,#5980,.T.);
#48326=EDGE_CURVE('',#38305,#38306,#5981,.T.);
#48327=EDGE_CURVE('',#38304,#38306,#5982,.T.);
#48328=EDGE_CURVE('',#38303,#38305,#5983,.T.);
#48329=EDGE_CURVE('',#38306,#38301,#5984,.T.);
#48330=EDGE_CURVE('',#38305,#38302,#5985,.T.);
#48331=EDGE_CURVE('',#38307,#38308,#5986,.T.);
#48332=EDGE_CURVE('',#38309,#38308,#5987,.T.);
#48333=EDGE_CURVE('',#38310,#38309,#5988,.T.);
#48334=EDGE_CURVE('',#38310,#38307,#5989,.T.);
#48335=EDGE_CURVE('',#38311,#38312,#5990,.T.);
#48336=EDGE_CURVE('',#38308,#38312,#5991,.T.);
#48337=EDGE_CURVE('',#38307,#38311,#5992,.T.);
#48338=EDGE_CURVE('',#38313,#38314,#5993,.T.);
#48339=EDGE_CURVE('',#38312,#38314,#5994,.T.);
#48340=EDGE_CURVE('',#38311,#38313,#5995,.T.);
#48341=EDGE_CURVE('',#38314,#38309,#5996,.T.);
#48342=EDGE_CURVE('',#38313,#38310,#5997,.T.);
#48343=EDGE_CURVE('',#38315,#38316,#5998,.T.);
#48344=EDGE_CURVE('',#38317,#38316,#5999,.T.);
#48345=EDGE_CURVE('',#38318,#38317,#6000,.T.);
#48346=EDGE_CURVE('',#38318,#38315,#6001,.T.);
#48347=EDGE_CURVE('',#38319,#38320,#6002,.T.);
#48348=EDGE_CURVE('',#38316,#38320,#6003,.T.);
#48349=EDGE_CURVE('',#38315,#38319,#6004,.T.);
#48350=EDGE_CURVE('',#38321,#38322,#6005,.T.);
#48351=EDGE_CURVE('',#38320,#38322,#6006,.T.);
#48352=EDGE_CURVE('',#38319,#38321,#6007,.T.);
#48353=EDGE_CURVE('',#38322,#38317,#6008,.T.);
#48354=EDGE_CURVE('',#38321,#38318,#6009,.T.);
#48355=EDGE_CURVE('',#38323,#38324,#6010,.T.);
#48356=EDGE_CURVE('',#38325,#38324,#6011,.T.);
#48357=EDGE_CURVE('',#38326,#38325,#6012,.T.);
#48358=EDGE_CURVE('',#38326,#38323,#6013,.T.);
#48359=EDGE_CURVE('',#38327,#38328,#6014,.T.);
#48360=EDGE_CURVE('',#38324,#38328,#6015,.T.);
#48361=EDGE_CURVE('',#38323,#38327,#6016,.T.);
#48362=EDGE_CURVE('',#38329,#38330,#6017,.T.);
#48363=EDGE_CURVE('',#38328,#38330,#6018,.T.);
#48364=EDGE_CURVE('',#38327,#38329,#6019,.T.);
#48365=EDGE_CURVE('',#38330,#38325,#6020,.T.);
#48366=EDGE_CURVE('',#38329,#38326,#6021,.T.);
#48367=EDGE_CURVE('',#38331,#38332,#6022,.T.);
#48368=EDGE_CURVE('',#38333,#38332,#6023,.T.);
#48369=EDGE_CURVE('',#38334,#38333,#6024,.T.);
#48370=EDGE_CURVE('',#38334,#38331,#6025,.T.);
#48371=EDGE_CURVE('',#38335,#38336,#6026,.T.);
#48372=EDGE_CURVE('',#38332,#38336,#6027,.T.);
#48373=EDGE_CURVE('',#38331,#38335,#6028,.T.);
#48374=EDGE_CURVE('',#38337,#38338,#6029,.T.);
#48375=EDGE_CURVE('',#38336,#38338,#6030,.T.);
#48376=EDGE_CURVE('',#38335,#38337,#6031,.T.);
#48377=EDGE_CURVE('',#38338,#38333,#6032,.T.);
#48378=EDGE_CURVE('',#38337,#38334,#6033,.T.);
#48379=EDGE_CURVE('',#38339,#38340,#6034,.T.);
#48380=EDGE_CURVE('',#38341,#38340,#6035,.T.);
#48381=EDGE_CURVE('',#38342,#38341,#6036,.T.);
#48382=EDGE_CURVE('',#38342,#38339,#6037,.T.);
#48383=EDGE_CURVE('',#38343,#38344,#6038,.T.);
#48384=EDGE_CURVE('',#38340,#38344,#6039,.T.);
#48385=EDGE_CURVE('',#38339,#38343,#6040,.T.);
#48386=EDGE_CURVE('',#38345,#38346,#6041,.T.);
#48387=EDGE_CURVE('',#38344,#38346,#6042,.T.);
#48388=EDGE_CURVE('',#38343,#38345,#6043,.T.);
#48389=EDGE_CURVE('',#38346,#38341,#6044,.T.);
#48390=EDGE_CURVE('',#38345,#38342,#6045,.T.);
#48391=EDGE_CURVE('',#38347,#38348,#6046,.T.);
#48392=EDGE_CURVE('',#38349,#38348,#6047,.T.);
#48393=EDGE_CURVE('',#38350,#38349,#6048,.T.);
#48394=EDGE_CURVE('',#38350,#38347,#6049,.T.);
#48395=EDGE_CURVE('',#38351,#38352,#6050,.T.);
#48396=EDGE_CURVE('',#38348,#38352,#6051,.T.);
#48397=EDGE_CURVE('',#38347,#38351,#6052,.T.);
#48398=EDGE_CURVE('',#38353,#38354,#6053,.T.);
#48399=EDGE_CURVE('',#38352,#38354,#6054,.T.);
#48400=EDGE_CURVE('',#38351,#38353,#6055,.T.);
#48401=EDGE_CURVE('',#38354,#38349,#6056,.T.);
#48402=EDGE_CURVE('',#38353,#38350,#6057,.T.);
#48403=EDGE_CURVE('',#38355,#38356,#6058,.T.);
#48404=EDGE_CURVE('',#38357,#38356,#6059,.T.);
#48405=EDGE_CURVE('',#38358,#38357,#6060,.T.);
#48406=EDGE_CURVE('',#38358,#38355,#6061,.T.);
#48407=EDGE_CURVE('',#38359,#38360,#6062,.T.);
#48408=EDGE_CURVE('',#38356,#38360,#6063,.T.);
#48409=EDGE_CURVE('',#38355,#38359,#6064,.T.);
#48410=EDGE_CURVE('',#38361,#38362,#6065,.T.);
#48411=EDGE_CURVE('',#38360,#38362,#6066,.T.);
#48412=EDGE_CURVE('',#38359,#38361,#6067,.T.);
#48413=EDGE_CURVE('',#38362,#38357,#6068,.T.);
#48414=EDGE_CURVE('',#38361,#38358,#6069,.T.);
#48415=EDGE_CURVE('',#38363,#38364,#6070,.T.);
#48416=EDGE_CURVE('',#38365,#38364,#6071,.T.);
#48417=EDGE_CURVE('',#38366,#38365,#6072,.T.);
#48418=EDGE_CURVE('',#38366,#38363,#6073,.T.);
#48419=EDGE_CURVE('',#38367,#38368,#6074,.T.);
#48420=EDGE_CURVE('',#38364,#38368,#6075,.T.);
#48421=EDGE_CURVE('',#38363,#38367,#6076,.T.);
#48422=EDGE_CURVE('',#38369,#38370,#6077,.T.);
#48423=EDGE_CURVE('',#38368,#38370,#6078,.T.);
#48424=EDGE_CURVE('',#38367,#38369,#6079,.T.);
#48425=EDGE_CURVE('',#38370,#38365,#6080,.T.);
#48426=EDGE_CURVE('',#38369,#38366,#6081,.T.);
#48427=EDGE_CURVE('',#38371,#38372,#6082,.T.);
#48428=EDGE_CURVE('',#38373,#38372,#6083,.T.);
#48429=EDGE_CURVE('',#38374,#38373,#6084,.T.);
#48430=EDGE_CURVE('',#38374,#38371,#6085,.T.);
#48431=EDGE_CURVE('',#38375,#38376,#6086,.T.);
#48432=EDGE_CURVE('',#38372,#38376,#6087,.T.);
#48433=EDGE_CURVE('',#38371,#38375,#6088,.T.);
#48434=EDGE_CURVE('',#38377,#38378,#6089,.T.);
#48435=EDGE_CURVE('',#38376,#38378,#6090,.T.);
#48436=EDGE_CURVE('',#38375,#38377,#6091,.T.);
#48437=EDGE_CURVE('',#38378,#38373,#6092,.T.);
#48438=EDGE_CURVE('',#38377,#38374,#6093,.T.);
#48439=EDGE_CURVE('',#38379,#38380,#6094,.T.);
#48440=EDGE_CURVE('',#38381,#38380,#6095,.T.);
#48441=EDGE_CURVE('',#38382,#38381,#6096,.T.);
#48442=EDGE_CURVE('',#38382,#38379,#6097,.T.);
#48443=EDGE_CURVE('',#38383,#38384,#6098,.T.);
#48444=EDGE_CURVE('',#38380,#38384,#6099,.T.);
#48445=EDGE_CURVE('',#38379,#38383,#6100,.T.);
#48446=EDGE_CURVE('',#38385,#38386,#6101,.T.);
#48447=EDGE_CURVE('',#38384,#38386,#6102,.T.);
#48448=EDGE_CURVE('',#38383,#38385,#6103,.T.);
#48449=EDGE_CURVE('',#38386,#38381,#6104,.T.);
#48450=EDGE_CURVE('',#38385,#38382,#6105,.T.);
#48451=EDGE_CURVE('',#38387,#38388,#6106,.T.);
#48452=EDGE_CURVE('',#38389,#38388,#6107,.T.);
#48453=EDGE_CURVE('',#38390,#38389,#6108,.T.);
#48454=EDGE_CURVE('',#38390,#38387,#6109,.T.);
#48455=EDGE_CURVE('',#38391,#38392,#6110,.T.);
#48456=EDGE_CURVE('',#38388,#38392,#6111,.T.);
#48457=EDGE_CURVE('',#38387,#38391,#6112,.T.);
#48458=EDGE_CURVE('',#38393,#38394,#6113,.T.);
#48459=EDGE_CURVE('',#38392,#38394,#6114,.T.);
#48460=EDGE_CURVE('',#38391,#38393,#6115,.T.);
#48461=EDGE_CURVE('',#38394,#38389,#6116,.T.);
#48462=EDGE_CURVE('',#38393,#38390,#6117,.T.);
#48463=EDGE_CURVE('',#38395,#38396,#6118,.T.);
#48464=EDGE_CURVE('',#38397,#38396,#6119,.T.);
#48465=EDGE_CURVE('',#38398,#38397,#6120,.T.);
#48466=EDGE_CURVE('',#38398,#38395,#6121,.T.);
#48467=EDGE_CURVE('',#38399,#38400,#6122,.T.);
#48468=EDGE_CURVE('',#38396,#38400,#6123,.T.);
#48469=EDGE_CURVE('',#38395,#38399,#6124,.T.);
#48470=EDGE_CURVE('',#38401,#38402,#6125,.T.);
#48471=EDGE_CURVE('',#38400,#38402,#6126,.T.);
#48472=EDGE_CURVE('',#38399,#38401,#6127,.T.);
#48473=EDGE_CURVE('',#38402,#38397,#6128,.T.);
#48474=EDGE_CURVE('',#38401,#38398,#6129,.T.);
#48475=EDGE_CURVE('',#38403,#38404,#6130,.T.);
#48476=EDGE_CURVE('',#38405,#38404,#6131,.T.);
#48477=EDGE_CURVE('',#38406,#38405,#6132,.T.);
#48478=EDGE_CURVE('',#38406,#38403,#6133,.T.);
#48479=EDGE_CURVE('',#38407,#38408,#6134,.T.);
#48480=EDGE_CURVE('',#38404,#38408,#6135,.T.);
#48481=EDGE_CURVE('',#38403,#38407,#6136,.T.);
#48482=EDGE_CURVE('',#38409,#38410,#6137,.T.);
#48483=EDGE_CURVE('',#38408,#38410,#6138,.T.);
#48484=EDGE_CURVE('',#38407,#38409,#6139,.T.);
#48485=EDGE_CURVE('',#38410,#38405,#6140,.T.);
#48486=EDGE_CURVE('',#38409,#38406,#6141,.T.);
#48487=EDGE_CURVE('',#38411,#38412,#6142,.T.);
#48488=EDGE_CURVE('',#38413,#38412,#6143,.T.);
#48489=EDGE_CURVE('',#38414,#38413,#6144,.T.);
#48490=EDGE_CURVE('',#38414,#38411,#6145,.T.);
#48491=EDGE_CURVE('',#38415,#38416,#6146,.T.);
#48492=EDGE_CURVE('',#38412,#38416,#6147,.T.);
#48493=EDGE_CURVE('',#38411,#38415,#6148,.T.);
#48494=EDGE_CURVE('',#38417,#38418,#6149,.T.);
#48495=EDGE_CURVE('',#38416,#38418,#6150,.T.);
#48496=EDGE_CURVE('',#38415,#38417,#6151,.T.);
#48497=EDGE_CURVE('',#38418,#38413,#6152,.T.);
#48498=EDGE_CURVE('',#38417,#38414,#6153,.T.);
#48499=EDGE_CURVE('',#38419,#38420,#6154,.T.);
#48500=EDGE_CURVE('',#38421,#38420,#6155,.T.);
#48501=EDGE_CURVE('',#38422,#38421,#6156,.T.);
#48502=EDGE_CURVE('',#38422,#38419,#6157,.T.);
#48503=EDGE_CURVE('',#38423,#38424,#6158,.T.);
#48504=EDGE_CURVE('',#38420,#38424,#6159,.T.);
#48505=EDGE_CURVE('',#38419,#38423,#6160,.T.);
#48506=EDGE_CURVE('',#38425,#38426,#6161,.T.);
#48507=EDGE_CURVE('',#38424,#38426,#6162,.T.);
#48508=EDGE_CURVE('',#38423,#38425,#6163,.T.);
#48509=EDGE_CURVE('',#38426,#38421,#6164,.T.);
#48510=EDGE_CURVE('',#38425,#38422,#6165,.T.);
#48511=EDGE_CURVE('',#38427,#38428,#6166,.T.);
#48512=EDGE_CURVE('',#38429,#38428,#6167,.T.);
#48513=EDGE_CURVE('',#38430,#38429,#6168,.T.);
#48514=EDGE_CURVE('',#38430,#38427,#6169,.T.);
#48515=EDGE_CURVE('',#38431,#38432,#6170,.T.);
#48516=EDGE_CURVE('',#38428,#38432,#6171,.T.);
#48517=EDGE_CURVE('',#38427,#38431,#6172,.T.);
#48518=EDGE_CURVE('',#38433,#38434,#6173,.T.);
#48519=EDGE_CURVE('',#38432,#38434,#6174,.T.);
#48520=EDGE_CURVE('',#38431,#38433,#6175,.T.);
#48521=EDGE_CURVE('',#38434,#38429,#6176,.T.);
#48522=EDGE_CURVE('',#38433,#38430,#6177,.T.);
#48523=EDGE_CURVE('',#38435,#38436,#6178,.T.);
#48524=EDGE_CURVE('',#38437,#38436,#6179,.T.);
#48525=EDGE_CURVE('',#38438,#38437,#6180,.T.);
#48526=EDGE_CURVE('',#38438,#38435,#6181,.T.);
#48527=EDGE_CURVE('',#38439,#38440,#6182,.T.);
#48528=EDGE_CURVE('',#38436,#38440,#6183,.T.);
#48529=EDGE_CURVE('',#38435,#38439,#6184,.T.);
#48530=EDGE_CURVE('',#38441,#38442,#6185,.T.);
#48531=EDGE_CURVE('',#38440,#38442,#6186,.T.);
#48532=EDGE_CURVE('',#38439,#38441,#6187,.T.);
#48533=EDGE_CURVE('',#38442,#38437,#6188,.T.);
#48534=EDGE_CURVE('',#38441,#38438,#6189,.T.);
#48535=EDGE_CURVE('',#38443,#38444,#6190,.T.);
#48536=EDGE_CURVE('',#38445,#38444,#6191,.T.);
#48537=EDGE_CURVE('',#38446,#38445,#6192,.T.);
#48538=EDGE_CURVE('',#38446,#38443,#6193,.T.);
#48539=EDGE_CURVE('',#38447,#38448,#6194,.T.);
#48540=EDGE_CURVE('',#38444,#38448,#6195,.T.);
#48541=EDGE_CURVE('',#38443,#38447,#6196,.T.);
#48542=EDGE_CURVE('',#38449,#38450,#6197,.T.);
#48543=EDGE_CURVE('',#38448,#38450,#6198,.T.);
#48544=EDGE_CURVE('',#38447,#38449,#6199,.T.);
#48545=EDGE_CURVE('',#38450,#38445,#6200,.T.);
#48546=EDGE_CURVE('',#38449,#38446,#6201,.T.);
#48547=EDGE_CURVE('',#38451,#38452,#6202,.T.);
#48548=EDGE_CURVE('',#38453,#38452,#6203,.T.);
#48549=EDGE_CURVE('',#38454,#38453,#6204,.T.);
#48550=EDGE_CURVE('',#38454,#38451,#6205,.T.);
#48551=EDGE_CURVE('',#38455,#38456,#6206,.T.);
#48552=EDGE_CURVE('',#38452,#38456,#6207,.T.);
#48553=EDGE_CURVE('',#38451,#38455,#6208,.T.);
#48554=EDGE_CURVE('',#38457,#38458,#6209,.T.);
#48555=EDGE_CURVE('',#38456,#38458,#6210,.T.);
#48556=EDGE_CURVE('',#38455,#38457,#6211,.T.);
#48557=EDGE_CURVE('',#38458,#38453,#6212,.T.);
#48558=EDGE_CURVE('',#38457,#38454,#6213,.T.);
#48559=EDGE_CURVE('',#38459,#38460,#6214,.T.);
#48560=EDGE_CURVE('',#38461,#38460,#6215,.T.);
#48561=EDGE_CURVE('',#38462,#38461,#6216,.T.);
#48562=EDGE_CURVE('',#38462,#38459,#6217,.T.);
#48563=EDGE_CURVE('',#38463,#38464,#6218,.T.);
#48564=EDGE_CURVE('',#38460,#38464,#6219,.T.);
#48565=EDGE_CURVE('',#38459,#38463,#6220,.T.);
#48566=EDGE_CURVE('',#38465,#38466,#6221,.T.);
#48567=EDGE_CURVE('',#38464,#38466,#6222,.T.);
#48568=EDGE_CURVE('',#38463,#38465,#6223,.T.);
#48569=EDGE_CURVE('',#38466,#38461,#6224,.T.);
#48570=EDGE_CURVE('',#38465,#38462,#6225,.T.);
#48571=EDGE_CURVE('',#38467,#38468,#6226,.T.);
#48572=EDGE_CURVE('',#38469,#38468,#6227,.T.);
#48573=EDGE_CURVE('',#38470,#38469,#6228,.T.);
#48574=EDGE_CURVE('',#38470,#38467,#6229,.T.);
#48575=EDGE_CURVE('',#38471,#38472,#6230,.T.);
#48576=EDGE_CURVE('',#38468,#38472,#6231,.T.);
#48577=EDGE_CURVE('',#38467,#38471,#6232,.T.);
#48578=EDGE_CURVE('',#38473,#38474,#6233,.T.);
#48579=EDGE_CURVE('',#38472,#38474,#6234,.T.);
#48580=EDGE_CURVE('',#38471,#38473,#6235,.T.);
#48581=EDGE_CURVE('',#38474,#38469,#6236,.T.);
#48582=EDGE_CURVE('',#38473,#38470,#6237,.T.);
#48583=EDGE_CURVE('',#38475,#38476,#6238,.T.);
#48584=EDGE_CURVE('',#38477,#38476,#6239,.T.);
#48585=EDGE_CURVE('',#38478,#38477,#6240,.T.);
#48586=EDGE_CURVE('',#38478,#38475,#6241,.T.);
#48587=EDGE_CURVE('',#38479,#38480,#6242,.T.);
#48588=EDGE_CURVE('',#38476,#38480,#6243,.T.);
#48589=EDGE_CURVE('',#38475,#38479,#6244,.T.);
#48590=EDGE_CURVE('',#38481,#38482,#6245,.T.);
#48591=EDGE_CURVE('',#38480,#38482,#6246,.T.);
#48592=EDGE_CURVE('',#38479,#38481,#6247,.T.);
#48593=EDGE_CURVE('',#38482,#38477,#6248,.T.);
#48594=EDGE_CURVE('',#38481,#38478,#6249,.T.);
#48595=EDGE_CURVE('',#38483,#38484,#6250,.T.);
#48596=EDGE_CURVE('',#38485,#38484,#6251,.T.);
#48597=EDGE_CURVE('',#38486,#38485,#6252,.T.);
#48598=EDGE_CURVE('',#38486,#38483,#6253,.T.);
#48599=EDGE_CURVE('',#38487,#38488,#6254,.T.);
#48600=EDGE_CURVE('',#38484,#38488,#6255,.T.);
#48601=EDGE_CURVE('',#38483,#38487,#6256,.T.);
#48602=EDGE_CURVE('',#38489,#38490,#6257,.T.);
#48603=EDGE_CURVE('',#38488,#38490,#6258,.T.);
#48604=EDGE_CURVE('',#38487,#38489,#6259,.T.);
#48605=EDGE_CURVE('',#38490,#38485,#6260,.T.);
#48606=EDGE_CURVE('',#38489,#38486,#6261,.T.);
#48607=EDGE_CURVE('',#38491,#38492,#6262,.T.);
#48608=EDGE_CURVE('',#38493,#38492,#6263,.T.);
#48609=EDGE_CURVE('',#38494,#38493,#6264,.T.);
#48610=EDGE_CURVE('',#38494,#38491,#6265,.T.);
#48611=EDGE_CURVE('',#38495,#38496,#6266,.T.);
#48612=EDGE_CURVE('',#38492,#38496,#6267,.T.);
#48613=EDGE_CURVE('',#38491,#38495,#6268,.T.);
#48614=EDGE_CURVE('',#38497,#38498,#6269,.T.);
#48615=EDGE_CURVE('',#38496,#38498,#6270,.T.);
#48616=EDGE_CURVE('',#38495,#38497,#6271,.T.);
#48617=EDGE_CURVE('',#38498,#38493,#6272,.T.);
#48618=EDGE_CURVE('',#38497,#38494,#6273,.T.);
#48619=EDGE_CURVE('',#38499,#38500,#6274,.T.);
#48620=EDGE_CURVE('',#38501,#38500,#6275,.T.);
#48621=EDGE_CURVE('',#38502,#38501,#6276,.T.);
#48622=EDGE_CURVE('',#38502,#38499,#6277,.T.);
#48623=EDGE_CURVE('',#38503,#38504,#6278,.T.);
#48624=EDGE_CURVE('',#38500,#38504,#6279,.T.);
#48625=EDGE_CURVE('',#38499,#38503,#6280,.T.);
#48626=EDGE_CURVE('',#38505,#38506,#6281,.T.);
#48627=EDGE_CURVE('',#38504,#38506,#6282,.T.);
#48628=EDGE_CURVE('',#38503,#38505,#6283,.T.);
#48629=EDGE_CURVE('',#38506,#38501,#6284,.T.);
#48630=EDGE_CURVE('',#38505,#38502,#6285,.T.);
#48631=EDGE_CURVE('',#38507,#38508,#6286,.T.);
#48632=EDGE_CURVE('',#38509,#38508,#6287,.T.);
#48633=EDGE_CURVE('',#38510,#38509,#6288,.T.);
#48634=EDGE_CURVE('',#38510,#38507,#6289,.T.);
#48635=EDGE_CURVE('',#38511,#38512,#6290,.T.);
#48636=EDGE_CURVE('',#38508,#38512,#6291,.T.);
#48637=EDGE_CURVE('',#38507,#38511,#6292,.T.);
#48638=EDGE_CURVE('',#38513,#38514,#6293,.T.);
#48639=EDGE_CURVE('',#38512,#38514,#6294,.T.);
#48640=EDGE_CURVE('',#38511,#38513,#6295,.T.);
#48641=EDGE_CURVE('',#38514,#38509,#6296,.T.);
#48642=EDGE_CURVE('',#38513,#38510,#6297,.T.);
#48643=EDGE_CURVE('',#38515,#38516,#6298,.T.);
#48644=EDGE_CURVE('',#38517,#38516,#6299,.T.);
#48645=EDGE_CURVE('',#38518,#38517,#6300,.T.);
#48646=EDGE_CURVE('',#38518,#38515,#6301,.T.);
#48647=EDGE_CURVE('',#38519,#38520,#6302,.T.);
#48648=EDGE_CURVE('',#38516,#38520,#6303,.T.);
#48649=EDGE_CURVE('',#38515,#38519,#6304,.T.);
#48650=EDGE_CURVE('',#38521,#38522,#6305,.T.);
#48651=EDGE_CURVE('',#38520,#38522,#6306,.T.);
#48652=EDGE_CURVE('',#38519,#38521,#6307,.T.);
#48653=EDGE_CURVE('',#38522,#38517,#6308,.T.);
#48654=EDGE_CURVE('',#38521,#38518,#6309,.T.);
#48655=EDGE_CURVE('',#38523,#38524,#6310,.T.);
#48656=EDGE_CURVE('',#38525,#38524,#6311,.T.);
#48657=EDGE_CURVE('',#38526,#38525,#6312,.T.);
#48658=EDGE_CURVE('',#38526,#38523,#6313,.T.);
#48659=EDGE_CURVE('',#38527,#38528,#6314,.T.);
#48660=EDGE_CURVE('',#38524,#38528,#6315,.T.);
#48661=EDGE_CURVE('',#38523,#38527,#6316,.T.);
#48662=EDGE_CURVE('',#38529,#38530,#6317,.T.);
#48663=EDGE_CURVE('',#38528,#38530,#6318,.T.);
#48664=EDGE_CURVE('',#38527,#38529,#6319,.T.);
#48665=EDGE_CURVE('',#38530,#38525,#6320,.T.);
#48666=EDGE_CURVE('',#38529,#38526,#6321,.T.);
#48667=EDGE_CURVE('',#38531,#38532,#6322,.T.);
#48668=EDGE_CURVE('',#38533,#38532,#6323,.T.);
#48669=EDGE_CURVE('',#38534,#38533,#6324,.T.);
#48670=EDGE_CURVE('',#38534,#38531,#6325,.T.);
#48671=EDGE_CURVE('',#38535,#38536,#6326,.T.);
#48672=EDGE_CURVE('',#38532,#38536,#6327,.T.);
#48673=EDGE_CURVE('',#38531,#38535,#6328,.T.);
#48674=EDGE_CURVE('',#38537,#38538,#6329,.T.);
#48675=EDGE_CURVE('',#38536,#38538,#6330,.T.);
#48676=EDGE_CURVE('',#38535,#38537,#6331,.T.);
#48677=EDGE_CURVE('',#38538,#38533,#6332,.T.);
#48678=EDGE_CURVE('',#38537,#38534,#6333,.T.);
#48679=EDGE_CURVE('',#38539,#38540,#6334,.T.);
#48680=EDGE_CURVE('',#38541,#38540,#6335,.T.);
#48681=EDGE_CURVE('',#38542,#38541,#6336,.T.);
#48682=EDGE_CURVE('',#38542,#38539,#6337,.T.);
#48683=EDGE_CURVE('',#38543,#38544,#6338,.T.);
#48684=EDGE_CURVE('',#38540,#38544,#6339,.T.);
#48685=EDGE_CURVE('',#38539,#38543,#6340,.T.);
#48686=EDGE_CURVE('',#38545,#38546,#6341,.T.);
#48687=EDGE_CURVE('',#38544,#38546,#6342,.T.);
#48688=EDGE_CURVE('',#38543,#38545,#6343,.T.);
#48689=EDGE_CURVE('',#38546,#38541,#6344,.T.);
#48690=EDGE_CURVE('',#38545,#38542,#6345,.T.);
#48691=EDGE_CURVE('',#38547,#38548,#6346,.T.);
#48692=EDGE_CURVE('',#38549,#38548,#6347,.T.);
#48693=EDGE_CURVE('',#38550,#38549,#6348,.T.);
#48694=EDGE_CURVE('',#38550,#38547,#6349,.T.);
#48695=EDGE_CURVE('',#38551,#38552,#6350,.T.);
#48696=EDGE_CURVE('',#38548,#38552,#6351,.T.);
#48697=EDGE_CURVE('',#38547,#38551,#6352,.T.);
#48698=EDGE_CURVE('',#38553,#38554,#6353,.T.);
#48699=EDGE_CURVE('',#38552,#38554,#6354,.T.);
#48700=EDGE_CURVE('',#38551,#38553,#6355,.T.);
#48701=EDGE_CURVE('',#38554,#38549,#6356,.T.);
#48702=EDGE_CURVE('',#38553,#38550,#6357,.T.);
#48703=EDGE_CURVE('',#38555,#38556,#6358,.T.);
#48704=EDGE_CURVE('',#38557,#38556,#6359,.T.);
#48705=EDGE_CURVE('',#38558,#38557,#6360,.T.);
#48706=EDGE_CURVE('',#38558,#38555,#6361,.T.);
#48707=EDGE_CURVE('',#38559,#38560,#6362,.T.);
#48708=EDGE_CURVE('',#38556,#38560,#6363,.T.);
#48709=EDGE_CURVE('',#38555,#38559,#6364,.T.);
#48710=EDGE_CURVE('',#38561,#38562,#6365,.T.);
#48711=EDGE_CURVE('',#38560,#38562,#6366,.T.);
#48712=EDGE_CURVE('',#38559,#38561,#6367,.T.);
#48713=EDGE_CURVE('',#38562,#38557,#6368,.T.);
#48714=EDGE_CURVE('',#38561,#38558,#6369,.T.);
#48715=EDGE_CURVE('',#38563,#38564,#6370,.T.);
#48716=EDGE_CURVE('',#38565,#38564,#6371,.T.);
#48717=EDGE_CURVE('',#38566,#38565,#6372,.T.);
#48718=EDGE_CURVE('',#38566,#38563,#6373,.T.);
#48719=EDGE_CURVE('',#38567,#38568,#6374,.T.);
#48720=EDGE_CURVE('',#38564,#38568,#6375,.T.);
#48721=EDGE_CURVE('',#38563,#38567,#6376,.T.);
#48722=EDGE_CURVE('',#38569,#38570,#6377,.T.);
#48723=EDGE_CURVE('',#38568,#38570,#6378,.T.);
#48724=EDGE_CURVE('',#38567,#38569,#6379,.T.);
#48725=EDGE_CURVE('',#38570,#38565,#6380,.T.);
#48726=EDGE_CURVE('',#38569,#38566,#6381,.T.);
#48727=EDGE_CURVE('',#38571,#38572,#6382,.T.);
#48728=EDGE_CURVE('',#38573,#38572,#6383,.T.);
#48729=EDGE_CURVE('',#38574,#38573,#6384,.T.);
#48730=EDGE_CURVE('',#38574,#38571,#6385,.T.);
#48731=EDGE_CURVE('',#38575,#38576,#6386,.T.);
#48732=EDGE_CURVE('',#38572,#38576,#6387,.T.);
#48733=EDGE_CURVE('',#38571,#38575,#6388,.T.);
#48734=EDGE_CURVE('',#38577,#38578,#6389,.T.);
#48735=EDGE_CURVE('',#38576,#38578,#6390,.T.);
#48736=EDGE_CURVE('',#38575,#38577,#6391,.T.);
#48737=EDGE_CURVE('',#38578,#38573,#6392,.T.);
#48738=EDGE_CURVE('',#38577,#38574,#6393,.T.);
#48739=EDGE_CURVE('',#38579,#38580,#6394,.T.);
#48740=EDGE_CURVE('',#38581,#38580,#6395,.T.);
#48741=EDGE_CURVE('',#38582,#38581,#6396,.T.);
#48742=EDGE_CURVE('',#38582,#38579,#6397,.T.);
#48743=EDGE_CURVE('',#38583,#38584,#6398,.T.);
#48744=EDGE_CURVE('',#38580,#38584,#6399,.T.);
#48745=EDGE_CURVE('',#38579,#38583,#6400,.T.);
#48746=EDGE_CURVE('',#38585,#38586,#6401,.T.);
#48747=EDGE_CURVE('',#38584,#38586,#6402,.T.);
#48748=EDGE_CURVE('',#38583,#38585,#6403,.T.);
#48749=EDGE_CURVE('',#38586,#38581,#6404,.T.);
#48750=EDGE_CURVE('',#38585,#38582,#6405,.T.);
#48751=EDGE_CURVE('',#38587,#38588,#6406,.T.);
#48752=EDGE_CURVE('',#38589,#38588,#6407,.T.);
#48753=EDGE_CURVE('',#38590,#38589,#6408,.T.);
#48754=EDGE_CURVE('',#38590,#38587,#6409,.T.);
#48755=EDGE_CURVE('',#38591,#38592,#6410,.T.);
#48756=EDGE_CURVE('',#38588,#38592,#6411,.T.);
#48757=EDGE_CURVE('',#38587,#38591,#6412,.T.);
#48758=EDGE_CURVE('',#38593,#38594,#6413,.T.);
#48759=EDGE_CURVE('',#38592,#38594,#6414,.T.);
#48760=EDGE_CURVE('',#38591,#38593,#6415,.T.);
#48761=EDGE_CURVE('',#38594,#38589,#6416,.T.);
#48762=EDGE_CURVE('',#38593,#38590,#6417,.T.);
#48763=EDGE_CURVE('',#38595,#38596,#6418,.T.);
#48764=EDGE_CURVE('',#38597,#38596,#6419,.T.);
#48765=EDGE_CURVE('',#38598,#38597,#6420,.T.);
#48766=EDGE_CURVE('',#38598,#38595,#6421,.T.);
#48767=EDGE_CURVE('',#38599,#38600,#6422,.T.);
#48768=EDGE_CURVE('',#38596,#38600,#6423,.T.);
#48769=EDGE_CURVE('',#38595,#38599,#6424,.T.);
#48770=EDGE_CURVE('',#38601,#38602,#6425,.T.);
#48771=EDGE_CURVE('',#38600,#38602,#6426,.T.);
#48772=EDGE_CURVE('',#38599,#38601,#6427,.T.);
#48773=EDGE_CURVE('',#38602,#38597,#6428,.T.);
#48774=EDGE_CURVE('',#38601,#38598,#6429,.T.);
#48775=EDGE_CURVE('',#38603,#38604,#6430,.T.);
#48776=EDGE_CURVE('',#38605,#38604,#6431,.T.);
#48777=EDGE_CURVE('',#38606,#38605,#6432,.T.);
#48778=EDGE_CURVE('',#38606,#38603,#6433,.T.);
#48779=EDGE_CURVE('',#38607,#38608,#6434,.T.);
#48780=EDGE_CURVE('',#38604,#38608,#6435,.T.);
#48781=EDGE_CURVE('',#38603,#38607,#6436,.T.);
#48782=EDGE_CURVE('',#38609,#38610,#6437,.T.);
#48783=EDGE_CURVE('',#38608,#38610,#6438,.T.);
#48784=EDGE_CURVE('',#38607,#38609,#6439,.T.);
#48785=EDGE_CURVE('',#38610,#38605,#6440,.T.);
#48786=EDGE_CURVE('',#38609,#38606,#6441,.T.);
#48787=EDGE_CURVE('',#38611,#38612,#6442,.T.);
#48788=EDGE_CURVE('',#38613,#38612,#6443,.T.);
#48789=EDGE_CURVE('',#38614,#38613,#6444,.T.);
#48790=EDGE_CURVE('',#38614,#38611,#6445,.T.);
#48791=EDGE_CURVE('',#38615,#38616,#6446,.T.);
#48792=EDGE_CURVE('',#38612,#38616,#6447,.T.);
#48793=EDGE_CURVE('',#38611,#38615,#6448,.T.);
#48794=EDGE_CURVE('',#38617,#38618,#6449,.T.);
#48795=EDGE_CURVE('',#38616,#38618,#6450,.T.);
#48796=EDGE_CURVE('',#38615,#38617,#6451,.T.);
#48797=EDGE_CURVE('',#38618,#38613,#6452,.T.);
#48798=EDGE_CURVE('',#38617,#38614,#6453,.T.);
#48799=EDGE_CURVE('',#38619,#38620,#6454,.T.);
#48800=EDGE_CURVE('',#38621,#38620,#6455,.T.);
#48801=EDGE_CURVE('',#38622,#38621,#6456,.T.);
#48802=EDGE_CURVE('',#38622,#38619,#6457,.T.);
#48803=EDGE_CURVE('',#38623,#38624,#6458,.T.);
#48804=EDGE_CURVE('',#38620,#38624,#6459,.T.);
#48805=EDGE_CURVE('',#38619,#38623,#6460,.T.);
#48806=EDGE_CURVE('',#38625,#38626,#6461,.T.);
#48807=EDGE_CURVE('',#38624,#38626,#6462,.T.);
#48808=EDGE_CURVE('',#38623,#38625,#6463,.T.);
#48809=EDGE_CURVE('',#38626,#38621,#6464,.T.);
#48810=EDGE_CURVE('',#38625,#38622,#6465,.T.);
#48811=EDGE_CURVE('',#38627,#38628,#6466,.T.);
#48812=EDGE_CURVE('',#38629,#38628,#6467,.T.);
#48813=EDGE_CURVE('',#38630,#38629,#6468,.T.);
#48814=EDGE_CURVE('',#38630,#38627,#6469,.T.);
#48815=EDGE_CURVE('',#38631,#38632,#6470,.T.);
#48816=EDGE_CURVE('',#38628,#38632,#6471,.T.);
#48817=EDGE_CURVE('',#38627,#38631,#6472,.T.);
#48818=EDGE_CURVE('',#38633,#38634,#6473,.T.);
#48819=EDGE_CURVE('',#38632,#38634,#6474,.T.);
#48820=EDGE_CURVE('',#38631,#38633,#6475,.T.);
#48821=EDGE_CURVE('',#38634,#38629,#6476,.T.);
#48822=EDGE_CURVE('',#38633,#38630,#6477,.T.);
#48823=EDGE_CURVE('',#38635,#38636,#6478,.T.);
#48824=EDGE_CURVE('',#38637,#38636,#6479,.T.);
#48825=EDGE_CURVE('',#38638,#38637,#6480,.T.);
#48826=EDGE_CURVE('',#38638,#38635,#6481,.T.);
#48827=EDGE_CURVE('',#38639,#38640,#6482,.T.);
#48828=EDGE_CURVE('',#38636,#38640,#6483,.T.);
#48829=EDGE_CURVE('',#38635,#38639,#6484,.T.);
#48830=EDGE_CURVE('',#38641,#38642,#6485,.T.);
#48831=EDGE_CURVE('',#38640,#38642,#6486,.T.);
#48832=EDGE_CURVE('',#38639,#38641,#6487,.T.);
#48833=EDGE_CURVE('',#38642,#38637,#6488,.T.);
#48834=EDGE_CURVE('',#38641,#38638,#6489,.T.);
#48835=EDGE_CURVE('',#38643,#38644,#6490,.T.);
#48836=EDGE_CURVE('',#38645,#38644,#6491,.T.);
#48837=EDGE_CURVE('',#38646,#38645,#6492,.T.);
#48838=EDGE_CURVE('',#38646,#38643,#6493,.T.);
#48839=EDGE_CURVE('',#38647,#38648,#6494,.T.);
#48840=EDGE_CURVE('',#38644,#38648,#6495,.T.);
#48841=EDGE_CURVE('',#38643,#38647,#6496,.T.);
#48842=EDGE_CURVE('',#38649,#38650,#6497,.T.);
#48843=EDGE_CURVE('',#38648,#38650,#6498,.T.);
#48844=EDGE_CURVE('',#38647,#38649,#6499,.T.);
#48845=EDGE_CURVE('',#38650,#38645,#6500,.T.);
#48846=EDGE_CURVE('',#38649,#38646,#6501,.T.);
#48847=EDGE_CURVE('',#38651,#38652,#6502,.T.);
#48848=EDGE_CURVE('',#38653,#38652,#6503,.T.);
#48849=EDGE_CURVE('',#38654,#38653,#6504,.T.);
#48850=EDGE_CURVE('',#38654,#38651,#6505,.T.);
#48851=EDGE_CURVE('',#38655,#38656,#6506,.T.);
#48852=EDGE_CURVE('',#38652,#38656,#6507,.T.);
#48853=EDGE_CURVE('',#38651,#38655,#6508,.T.);
#48854=EDGE_CURVE('',#38657,#38658,#6509,.T.);
#48855=EDGE_CURVE('',#38656,#38658,#6510,.T.);
#48856=EDGE_CURVE('',#38655,#38657,#6511,.T.);
#48857=EDGE_CURVE('',#38658,#38653,#6512,.T.);
#48858=EDGE_CURVE('',#38657,#38654,#6513,.T.);
#48859=EDGE_CURVE('',#38659,#38660,#6514,.T.);
#48860=EDGE_CURVE('',#38661,#38660,#6515,.T.);
#48861=EDGE_CURVE('',#38662,#38661,#6516,.T.);
#48862=EDGE_CURVE('',#38662,#38659,#6517,.T.);
#48863=EDGE_CURVE('',#38663,#38664,#6518,.T.);
#48864=EDGE_CURVE('',#38660,#38664,#6519,.T.);
#48865=EDGE_CURVE('',#38659,#38663,#6520,.T.);
#48866=EDGE_CURVE('',#38665,#38666,#6521,.T.);
#48867=EDGE_CURVE('',#38664,#38666,#6522,.T.);
#48868=EDGE_CURVE('',#38663,#38665,#6523,.T.);
#48869=EDGE_CURVE('',#38666,#38661,#6524,.T.);
#48870=EDGE_CURVE('',#38665,#38662,#6525,.T.);
#48871=EDGE_CURVE('',#38667,#38668,#6526,.T.);
#48872=EDGE_CURVE('',#38669,#38668,#6527,.T.);
#48873=EDGE_CURVE('',#38670,#38669,#6528,.T.);
#48874=EDGE_CURVE('',#38670,#38667,#6529,.T.);
#48875=EDGE_CURVE('',#38671,#38672,#6530,.T.);
#48876=EDGE_CURVE('',#38668,#38672,#6531,.T.);
#48877=EDGE_CURVE('',#38667,#38671,#6532,.T.);
#48878=EDGE_CURVE('',#38673,#38674,#6533,.T.);
#48879=EDGE_CURVE('',#38672,#38674,#6534,.T.);
#48880=EDGE_CURVE('',#38671,#38673,#6535,.T.);
#48881=EDGE_CURVE('',#38674,#38669,#6536,.T.);
#48882=EDGE_CURVE('',#38673,#38670,#6537,.T.);
#48883=EDGE_CURVE('',#38675,#38676,#6538,.T.);
#48884=EDGE_CURVE('',#38677,#38676,#6539,.T.);
#48885=EDGE_CURVE('',#38678,#38677,#6540,.T.);
#48886=EDGE_CURVE('',#38678,#38675,#6541,.T.);
#48887=EDGE_CURVE('',#38679,#38680,#6542,.T.);
#48888=EDGE_CURVE('',#38676,#38680,#6543,.T.);
#48889=EDGE_CURVE('',#38675,#38679,#6544,.T.);
#48890=EDGE_CURVE('',#38681,#38682,#6545,.T.);
#48891=EDGE_CURVE('',#38680,#38682,#6546,.T.);
#48892=EDGE_CURVE('',#38679,#38681,#6547,.T.);
#48893=EDGE_CURVE('',#38682,#38677,#6548,.T.);
#48894=EDGE_CURVE('',#38681,#38678,#6549,.T.);
#48895=EDGE_CURVE('',#38683,#38684,#6550,.T.);
#48896=EDGE_CURVE('',#38685,#38684,#6551,.T.);
#48897=EDGE_CURVE('',#38686,#38685,#6552,.T.);
#48898=EDGE_CURVE('',#38686,#38683,#6553,.T.);
#48899=EDGE_CURVE('',#38687,#38688,#6554,.T.);
#48900=EDGE_CURVE('',#38684,#38688,#6555,.T.);
#48901=EDGE_CURVE('',#38683,#38687,#6556,.T.);
#48902=EDGE_CURVE('',#38689,#38690,#6557,.T.);
#48903=EDGE_CURVE('',#38688,#38690,#6558,.T.);
#48904=EDGE_CURVE('',#38687,#38689,#6559,.T.);
#48905=EDGE_CURVE('',#38690,#38685,#6560,.T.);
#48906=EDGE_CURVE('',#38689,#38686,#6561,.T.);
#48907=EDGE_CURVE('',#38691,#38692,#6562,.T.);
#48908=EDGE_CURVE('',#38693,#38692,#6563,.T.);
#48909=EDGE_CURVE('',#38694,#38693,#6564,.T.);
#48910=EDGE_CURVE('',#38694,#38691,#6565,.T.);
#48911=EDGE_CURVE('',#38695,#38696,#6566,.T.);
#48912=EDGE_CURVE('',#38692,#38696,#6567,.T.);
#48913=EDGE_CURVE('',#38691,#38695,#6568,.T.);
#48914=EDGE_CURVE('',#38697,#38698,#6569,.T.);
#48915=EDGE_CURVE('',#38696,#38698,#6570,.T.);
#48916=EDGE_CURVE('',#38695,#38697,#6571,.T.);
#48917=EDGE_CURVE('',#38698,#38693,#6572,.T.);
#48918=EDGE_CURVE('',#38697,#38694,#6573,.T.);
#48919=EDGE_CURVE('',#38699,#38700,#6574,.T.);
#48920=EDGE_CURVE('',#38701,#38700,#6575,.T.);
#48921=EDGE_CURVE('',#38702,#38701,#6576,.T.);
#48922=EDGE_CURVE('',#38702,#38699,#6577,.T.);
#48923=EDGE_CURVE('',#38703,#38704,#6578,.T.);
#48924=EDGE_CURVE('',#38700,#38704,#6579,.T.);
#48925=EDGE_CURVE('',#38699,#38703,#6580,.T.);
#48926=EDGE_CURVE('',#38705,#38706,#6581,.T.);
#48927=EDGE_CURVE('',#38704,#38706,#6582,.T.);
#48928=EDGE_CURVE('',#38703,#38705,#6583,.T.);
#48929=EDGE_CURVE('',#38706,#38701,#6584,.T.);
#48930=EDGE_CURVE('',#38705,#38702,#6585,.T.);
#48931=EDGE_CURVE('',#38707,#38708,#6586,.T.);
#48932=EDGE_CURVE('',#38709,#38708,#6587,.T.);
#48933=EDGE_CURVE('',#38710,#38709,#6588,.T.);
#48934=EDGE_CURVE('',#38710,#38707,#6589,.T.);
#48935=EDGE_CURVE('',#38711,#38712,#6590,.T.);
#48936=EDGE_CURVE('',#38708,#38712,#6591,.T.);
#48937=EDGE_CURVE('',#38707,#38711,#6592,.T.);
#48938=EDGE_CURVE('',#38713,#38714,#6593,.T.);
#48939=EDGE_CURVE('',#38712,#38714,#6594,.T.);
#48940=EDGE_CURVE('',#38711,#38713,#6595,.T.);
#48941=EDGE_CURVE('',#38714,#38709,#6596,.T.);
#48942=EDGE_CURVE('',#38713,#38710,#6597,.T.);
#48943=EDGE_CURVE('',#38715,#38716,#6598,.T.);
#48944=EDGE_CURVE('',#38717,#38716,#6599,.T.);
#48945=EDGE_CURVE('',#38718,#38717,#6600,.T.);
#48946=EDGE_CURVE('',#38718,#38715,#6601,.T.);
#48947=EDGE_CURVE('',#38719,#38720,#6602,.T.);
#48948=EDGE_CURVE('',#38716,#38720,#6603,.T.);
#48949=EDGE_CURVE('',#38715,#38719,#6604,.T.);
#48950=EDGE_CURVE('',#38721,#38722,#6605,.T.);
#48951=EDGE_CURVE('',#38720,#38722,#6606,.T.);
#48952=EDGE_CURVE('',#38719,#38721,#6607,.T.);
#48953=EDGE_CURVE('',#38722,#38717,#6608,.T.);
#48954=EDGE_CURVE('',#38721,#38718,#6609,.T.);
#48955=EDGE_CURVE('',#38723,#38724,#6610,.T.);
#48956=EDGE_CURVE('',#38725,#38724,#6611,.T.);
#48957=EDGE_CURVE('',#38726,#38725,#6612,.T.);
#48958=EDGE_CURVE('',#38726,#38723,#6613,.T.);
#48959=EDGE_CURVE('',#38727,#38728,#6614,.T.);
#48960=EDGE_CURVE('',#38724,#38728,#6615,.T.);
#48961=EDGE_CURVE('',#38723,#38727,#6616,.T.);
#48962=EDGE_CURVE('',#38729,#38730,#6617,.T.);
#48963=EDGE_CURVE('',#38728,#38730,#6618,.T.);
#48964=EDGE_CURVE('',#38727,#38729,#6619,.T.);
#48965=EDGE_CURVE('',#38730,#38725,#6620,.T.);
#48966=EDGE_CURVE('',#38729,#38726,#6621,.T.);
#48967=EDGE_CURVE('',#38731,#38732,#6622,.T.);
#48968=EDGE_CURVE('',#38733,#38732,#6623,.T.);
#48969=EDGE_CURVE('',#38734,#38733,#6624,.T.);
#48970=EDGE_CURVE('',#38734,#38731,#6625,.T.);
#48971=EDGE_CURVE('',#38735,#38736,#6626,.T.);
#48972=EDGE_CURVE('',#38732,#38736,#6627,.T.);
#48973=EDGE_CURVE('',#38731,#38735,#6628,.T.);
#48974=EDGE_CURVE('',#38737,#38738,#6629,.T.);
#48975=EDGE_CURVE('',#38736,#38738,#6630,.T.);
#48976=EDGE_CURVE('',#38735,#38737,#6631,.T.);
#48977=EDGE_CURVE('',#38738,#38733,#6632,.T.);
#48978=EDGE_CURVE('',#38737,#38734,#6633,.T.);
#48979=EDGE_CURVE('',#38739,#38740,#6634,.T.);
#48980=EDGE_CURVE('',#38741,#38740,#6635,.T.);
#48981=EDGE_CURVE('',#38742,#38741,#6636,.T.);
#48982=EDGE_CURVE('',#38742,#38739,#6637,.T.);
#48983=EDGE_CURVE('',#38743,#38744,#6638,.T.);
#48984=EDGE_CURVE('',#38740,#38744,#6639,.T.);
#48985=EDGE_CURVE('',#38739,#38743,#6640,.T.);
#48986=EDGE_CURVE('',#38745,#38746,#6641,.T.);
#48987=EDGE_CURVE('',#38744,#38746,#6642,.T.);
#48988=EDGE_CURVE('',#38743,#38745,#6643,.T.);
#48989=EDGE_CURVE('',#38746,#38741,#6644,.T.);
#48990=EDGE_CURVE('',#38745,#38742,#6645,.T.);
#48991=EDGE_CURVE('',#38747,#38748,#6646,.T.);
#48992=EDGE_CURVE('',#38749,#38748,#6647,.T.);
#48993=EDGE_CURVE('',#38750,#38749,#6648,.T.);
#48994=EDGE_CURVE('',#38750,#38747,#6649,.T.);
#48995=EDGE_CURVE('',#38751,#38752,#6650,.T.);
#48996=EDGE_CURVE('',#38748,#38752,#6651,.T.);
#48997=EDGE_CURVE('',#38747,#38751,#6652,.T.);
#48998=EDGE_CURVE('',#38753,#38754,#6653,.T.);
#48999=EDGE_CURVE('',#38752,#38754,#6654,.T.);
#49000=EDGE_CURVE('',#38751,#38753,#6655,.T.);
#49001=EDGE_CURVE('',#38754,#38749,#6656,.T.);
#49002=EDGE_CURVE('',#38753,#38750,#6657,.T.);
#49003=EDGE_CURVE('',#38755,#38756,#6658,.T.);
#49004=EDGE_CURVE('',#38757,#38756,#6659,.T.);
#49005=EDGE_CURVE('',#38758,#38757,#6660,.T.);
#49006=EDGE_CURVE('',#38758,#38755,#6661,.T.);
#49007=EDGE_CURVE('',#38759,#38760,#6662,.T.);
#49008=EDGE_CURVE('',#38756,#38760,#6663,.T.);
#49009=EDGE_CURVE('',#38755,#38759,#6664,.T.);
#49010=EDGE_CURVE('',#38761,#38762,#6665,.T.);
#49011=EDGE_CURVE('',#38760,#38762,#6666,.T.);
#49012=EDGE_CURVE('',#38759,#38761,#6667,.T.);
#49013=EDGE_CURVE('',#38762,#38757,#6668,.T.);
#49014=EDGE_CURVE('',#38761,#38758,#6669,.T.);
#49015=EDGE_CURVE('',#38763,#38764,#6670,.T.);
#49016=EDGE_CURVE('',#38765,#38764,#6671,.T.);
#49017=EDGE_CURVE('',#38766,#38765,#6672,.T.);
#49018=EDGE_CURVE('',#38766,#38763,#6673,.T.);
#49019=EDGE_CURVE('',#38767,#38768,#6674,.T.);
#49020=EDGE_CURVE('',#38764,#38768,#6675,.T.);
#49021=EDGE_CURVE('',#38763,#38767,#6676,.T.);
#49022=EDGE_CURVE('',#38769,#38770,#6677,.T.);
#49023=EDGE_CURVE('',#38768,#38770,#6678,.T.);
#49024=EDGE_CURVE('',#38767,#38769,#6679,.T.);
#49025=EDGE_CURVE('',#38770,#38765,#6680,.T.);
#49026=EDGE_CURVE('',#38769,#38766,#6681,.T.);
#49027=EDGE_CURVE('',#38771,#38772,#6682,.T.);
#49028=EDGE_CURVE('',#38773,#38772,#6683,.T.);
#49029=EDGE_CURVE('',#38774,#38773,#6684,.T.);
#49030=EDGE_CURVE('',#38774,#38771,#6685,.T.);
#49031=EDGE_CURVE('',#38775,#38776,#6686,.T.);
#49032=EDGE_CURVE('',#38772,#38776,#6687,.T.);
#49033=EDGE_CURVE('',#38771,#38775,#6688,.T.);
#49034=EDGE_CURVE('',#38777,#38778,#6689,.T.);
#49035=EDGE_CURVE('',#38776,#38778,#6690,.T.);
#49036=EDGE_CURVE('',#38775,#38777,#6691,.T.);
#49037=EDGE_CURVE('',#38778,#38773,#6692,.T.);
#49038=EDGE_CURVE('',#38777,#38774,#6693,.T.);
#49039=EDGE_CURVE('',#38779,#38780,#6694,.T.);
#49040=EDGE_CURVE('',#38781,#38780,#6695,.T.);
#49041=EDGE_CURVE('',#38782,#38781,#6696,.T.);
#49042=EDGE_CURVE('',#38782,#38779,#6697,.T.);
#49043=EDGE_CURVE('',#38783,#38784,#6698,.T.);
#49044=EDGE_CURVE('',#38780,#38784,#6699,.T.);
#49045=EDGE_CURVE('',#38779,#38783,#6700,.T.);
#49046=EDGE_CURVE('',#38785,#38786,#6701,.T.);
#49047=EDGE_CURVE('',#38784,#38786,#6702,.T.);
#49048=EDGE_CURVE('',#38783,#38785,#6703,.T.);
#49049=EDGE_CURVE('',#38786,#38781,#6704,.T.);
#49050=EDGE_CURVE('',#38785,#38782,#6705,.T.);
#49051=EDGE_CURVE('',#38787,#38788,#6706,.T.);
#49052=EDGE_CURVE('',#38789,#38788,#6707,.T.);
#49053=EDGE_CURVE('',#38790,#38789,#6708,.T.);
#49054=EDGE_CURVE('',#38790,#38787,#6709,.T.);
#49055=EDGE_CURVE('',#38791,#38792,#6710,.T.);
#49056=EDGE_CURVE('',#38788,#38792,#6711,.T.);
#49057=EDGE_CURVE('',#38787,#38791,#6712,.T.);
#49058=EDGE_CURVE('',#38793,#38794,#6713,.T.);
#49059=EDGE_CURVE('',#38792,#38794,#6714,.T.);
#49060=EDGE_CURVE('',#38791,#38793,#6715,.T.);
#49061=EDGE_CURVE('',#38794,#38789,#6716,.T.);
#49062=EDGE_CURVE('',#38793,#38790,#6717,.T.);
#49063=EDGE_CURVE('',#38795,#38796,#6718,.T.);
#49064=EDGE_CURVE('',#38797,#38796,#6719,.T.);
#49065=EDGE_CURVE('',#38798,#38797,#6720,.T.);
#49066=EDGE_CURVE('',#38798,#38795,#6721,.T.);
#49067=EDGE_CURVE('',#38799,#38800,#6722,.T.);
#49068=EDGE_CURVE('',#38796,#38800,#6723,.T.);
#49069=EDGE_CURVE('',#38795,#38799,#6724,.T.);
#49070=EDGE_CURVE('',#38801,#38802,#6725,.T.);
#49071=EDGE_CURVE('',#38800,#38802,#6726,.T.);
#49072=EDGE_CURVE('',#38799,#38801,#6727,.T.);
#49073=EDGE_CURVE('',#38802,#38797,#6728,.T.);
#49074=EDGE_CURVE('',#38801,#38798,#6729,.T.);
#49075=EDGE_CURVE('',#38803,#38804,#6730,.T.);
#49076=EDGE_CURVE('',#38805,#38804,#6731,.T.);
#49077=EDGE_CURVE('',#38806,#38805,#6732,.T.);
#49078=EDGE_CURVE('',#38806,#38803,#6733,.T.);
#49079=EDGE_CURVE('',#38807,#38808,#6734,.T.);
#49080=EDGE_CURVE('',#38804,#38808,#6735,.T.);
#49081=EDGE_CURVE('',#38803,#38807,#6736,.T.);
#49082=EDGE_CURVE('',#38809,#38810,#6737,.T.);
#49083=EDGE_CURVE('',#38808,#38810,#6738,.T.);
#49084=EDGE_CURVE('',#38807,#38809,#6739,.T.);
#49085=EDGE_CURVE('',#38810,#38805,#6740,.T.);
#49086=EDGE_CURVE('',#38809,#38806,#6741,.T.);
#49087=EDGE_CURVE('',#38811,#38812,#6742,.T.);
#49088=EDGE_CURVE('',#38813,#38812,#6743,.T.);
#49089=EDGE_CURVE('',#38814,#38813,#6744,.T.);
#49090=EDGE_CURVE('',#38814,#38811,#6745,.T.);
#49091=EDGE_CURVE('',#38815,#38816,#6746,.T.);
#49092=EDGE_CURVE('',#38812,#38816,#6747,.T.);
#49093=EDGE_CURVE('',#38811,#38815,#6748,.T.);
#49094=EDGE_CURVE('',#38817,#38818,#6749,.T.);
#49095=EDGE_CURVE('',#38816,#38818,#6750,.T.);
#49096=EDGE_CURVE('',#38815,#38817,#6751,.T.);
#49097=EDGE_CURVE('',#38818,#38813,#6752,.T.);
#49098=EDGE_CURVE('',#38817,#38814,#6753,.T.);
#49099=EDGE_CURVE('',#38819,#38820,#6754,.T.);
#49100=EDGE_CURVE('',#38821,#38820,#6755,.T.);
#49101=EDGE_CURVE('',#38822,#38821,#6756,.T.);
#49102=EDGE_CURVE('',#38822,#38819,#6757,.T.);
#49103=EDGE_CURVE('',#38823,#38824,#6758,.T.);
#49104=EDGE_CURVE('',#38820,#38824,#6759,.T.);
#49105=EDGE_CURVE('',#38819,#38823,#6760,.T.);
#49106=EDGE_CURVE('',#38825,#38826,#6761,.T.);
#49107=EDGE_CURVE('',#38824,#38826,#6762,.T.);
#49108=EDGE_CURVE('',#38823,#38825,#6763,.T.);
#49109=EDGE_CURVE('',#38826,#38821,#6764,.T.);
#49110=EDGE_CURVE('',#38825,#38822,#6765,.T.);
#49111=EDGE_CURVE('',#38827,#38828,#6766,.T.);
#49112=EDGE_CURVE('',#38829,#38828,#6767,.T.);
#49113=EDGE_CURVE('',#38830,#38829,#6768,.T.);
#49114=EDGE_CURVE('',#38830,#38827,#6769,.T.);
#49115=EDGE_CURVE('',#38831,#38832,#6770,.T.);
#49116=EDGE_CURVE('',#38828,#38832,#6771,.T.);
#49117=EDGE_CURVE('',#38827,#38831,#6772,.T.);
#49118=EDGE_CURVE('',#38833,#38834,#6773,.T.);
#49119=EDGE_CURVE('',#38832,#38834,#6774,.T.);
#49120=EDGE_CURVE('',#38831,#38833,#6775,.T.);
#49121=EDGE_CURVE('',#38834,#38829,#6776,.T.);
#49122=EDGE_CURVE('',#38833,#38830,#6777,.T.);
#49123=EDGE_CURVE('',#38835,#38836,#6778,.T.);
#49124=EDGE_CURVE('',#38837,#38836,#6779,.T.);
#49125=EDGE_CURVE('',#38838,#38837,#6780,.T.);
#49126=EDGE_CURVE('',#38838,#38835,#6781,.T.);
#49127=EDGE_CURVE('',#38839,#38840,#6782,.T.);
#49128=EDGE_CURVE('',#38836,#38840,#6783,.T.);
#49129=EDGE_CURVE('',#38835,#38839,#6784,.T.);
#49130=EDGE_CURVE('',#38841,#38842,#6785,.T.);
#49131=EDGE_CURVE('',#38840,#38842,#6786,.T.);
#49132=EDGE_CURVE('',#38839,#38841,#6787,.T.);
#49133=EDGE_CURVE('',#38842,#38837,#6788,.T.);
#49134=EDGE_CURVE('',#38841,#38838,#6789,.T.);
#49135=EDGE_CURVE('',#38843,#38844,#6790,.T.);
#49136=EDGE_CURVE('',#38845,#38844,#6791,.T.);
#49137=EDGE_CURVE('',#38846,#38845,#6792,.T.);
#49138=EDGE_CURVE('',#38846,#38843,#6793,.T.);
#49139=EDGE_CURVE('',#38847,#38848,#6794,.T.);
#49140=EDGE_CURVE('',#38844,#38848,#6795,.T.);
#49141=EDGE_CURVE('',#38843,#38847,#6796,.T.);
#49142=EDGE_CURVE('',#38849,#38850,#6797,.T.);
#49143=EDGE_CURVE('',#38848,#38850,#6798,.T.);
#49144=EDGE_CURVE('',#38847,#38849,#6799,.T.);
#49145=EDGE_CURVE('',#38850,#38845,#6800,.T.);
#49146=EDGE_CURVE('',#38849,#38846,#6801,.T.);
#49147=EDGE_CURVE('',#38851,#38852,#6802,.T.);
#49148=EDGE_CURVE('',#38853,#38852,#6803,.T.);
#49149=EDGE_CURVE('',#38854,#38853,#6804,.T.);
#49150=EDGE_CURVE('',#38854,#38851,#6805,.T.);
#49151=EDGE_CURVE('',#38855,#38856,#6806,.T.);
#49152=EDGE_CURVE('',#38852,#38856,#6807,.T.);
#49153=EDGE_CURVE('',#38851,#38855,#6808,.T.);
#49154=EDGE_CURVE('',#38857,#38858,#6809,.T.);
#49155=EDGE_CURVE('',#38856,#38858,#6810,.T.);
#49156=EDGE_CURVE('',#38855,#38857,#6811,.T.);
#49157=EDGE_CURVE('',#38858,#38853,#6812,.T.);
#49158=EDGE_CURVE('',#38857,#38854,#6813,.T.);
#49159=EDGE_CURVE('',#38859,#38860,#6814,.T.);
#49160=EDGE_CURVE('',#38861,#38860,#6815,.T.);
#49161=EDGE_CURVE('',#38862,#38861,#6816,.T.);
#49162=EDGE_CURVE('',#38862,#38859,#6817,.T.);
#49163=EDGE_CURVE('',#38863,#38864,#6818,.T.);
#49164=EDGE_CURVE('',#38860,#38864,#6819,.T.);
#49165=EDGE_CURVE('',#38859,#38863,#6820,.T.);
#49166=EDGE_CURVE('',#38865,#38866,#6821,.T.);
#49167=EDGE_CURVE('',#38864,#38866,#6822,.T.);
#49168=EDGE_CURVE('',#38863,#38865,#6823,.T.);
#49169=EDGE_CURVE('',#38866,#38861,#6824,.T.);
#49170=EDGE_CURVE('',#38865,#38862,#6825,.T.);
#49171=EDGE_CURVE('',#38867,#38868,#6826,.T.);
#49172=EDGE_CURVE('',#38869,#38868,#6827,.T.);
#49173=EDGE_CURVE('',#38870,#38869,#6828,.T.);
#49174=EDGE_CURVE('',#38870,#38867,#6829,.T.);
#49175=EDGE_CURVE('',#38871,#38872,#6830,.T.);
#49176=EDGE_CURVE('',#38868,#38872,#6831,.T.);
#49177=EDGE_CURVE('',#38867,#38871,#6832,.T.);
#49178=EDGE_CURVE('',#38873,#38874,#6833,.T.);
#49179=EDGE_CURVE('',#38872,#38874,#6834,.T.);
#49180=EDGE_CURVE('',#38871,#38873,#6835,.T.);
#49181=EDGE_CURVE('',#38874,#38869,#6836,.T.);
#49182=EDGE_CURVE('',#38873,#38870,#6837,.T.);
#49183=EDGE_CURVE('',#38875,#38876,#6838,.T.);
#49184=EDGE_CURVE('',#38877,#38876,#6839,.T.);
#49185=EDGE_CURVE('',#38878,#38877,#6840,.T.);
#49186=EDGE_CURVE('',#38878,#38875,#6841,.T.);
#49187=EDGE_CURVE('',#38879,#38880,#6842,.T.);
#49188=EDGE_CURVE('',#38876,#38880,#6843,.T.);
#49189=EDGE_CURVE('',#38875,#38879,#6844,.T.);
#49190=EDGE_CURVE('',#38881,#38882,#6845,.T.);
#49191=EDGE_CURVE('',#38880,#38882,#6846,.T.);
#49192=EDGE_CURVE('',#38879,#38881,#6847,.T.);
#49193=EDGE_CURVE('',#38882,#38877,#6848,.T.);
#49194=EDGE_CURVE('',#38881,#38878,#6849,.T.);
#49195=EDGE_CURVE('',#38883,#38884,#6850,.T.);
#49196=EDGE_CURVE('',#38885,#38884,#6851,.T.);
#49197=EDGE_CURVE('',#38886,#38885,#6852,.T.);
#49198=EDGE_CURVE('',#38886,#38883,#6853,.T.);
#49199=EDGE_CURVE('',#38887,#38888,#6854,.T.);
#49200=EDGE_CURVE('',#38884,#38888,#6855,.T.);
#49201=EDGE_CURVE('',#38883,#38887,#6856,.T.);
#49202=EDGE_CURVE('',#38889,#38890,#6857,.T.);
#49203=EDGE_CURVE('',#38888,#38890,#6858,.T.);
#49204=EDGE_CURVE('',#38887,#38889,#6859,.T.);
#49205=EDGE_CURVE('',#38890,#38885,#6860,.T.);
#49206=EDGE_CURVE('',#38889,#38886,#6861,.T.);
#49207=EDGE_CURVE('',#38891,#38892,#6862,.T.);
#49208=EDGE_CURVE('',#38893,#38892,#6863,.T.);
#49209=EDGE_CURVE('',#38894,#38893,#6864,.T.);
#49210=EDGE_CURVE('',#38894,#38891,#6865,.T.);
#49211=EDGE_CURVE('',#38895,#38896,#6866,.T.);
#49212=EDGE_CURVE('',#38892,#38896,#6867,.T.);
#49213=EDGE_CURVE('',#38891,#38895,#6868,.T.);
#49214=EDGE_CURVE('',#38897,#38898,#6869,.T.);
#49215=EDGE_CURVE('',#38896,#38898,#6870,.T.);
#49216=EDGE_CURVE('',#38895,#38897,#6871,.T.);
#49217=EDGE_CURVE('',#38898,#38893,#6872,.T.);
#49218=EDGE_CURVE('',#38897,#38894,#6873,.T.);
#49219=EDGE_CURVE('',#38899,#38900,#6874,.T.);
#49220=EDGE_CURVE('',#38901,#38900,#6875,.T.);
#49221=EDGE_CURVE('',#38902,#38901,#6876,.T.);
#49222=EDGE_CURVE('',#38902,#38899,#6877,.T.);
#49223=EDGE_CURVE('',#38903,#38904,#6878,.T.);
#49224=EDGE_CURVE('',#38900,#38904,#6879,.T.);
#49225=EDGE_CURVE('',#38899,#38903,#6880,.T.);
#49226=EDGE_CURVE('',#38905,#38906,#6881,.T.);
#49227=EDGE_CURVE('',#38904,#38906,#6882,.T.);
#49228=EDGE_CURVE('',#38903,#38905,#6883,.T.);
#49229=EDGE_CURVE('',#38906,#38901,#6884,.T.);
#49230=EDGE_CURVE('',#38905,#38902,#6885,.T.);
#49231=EDGE_CURVE('',#38907,#38908,#6886,.T.);
#49232=EDGE_CURVE('',#38909,#38908,#6887,.T.);
#49233=EDGE_CURVE('',#38910,#38909,#6888,.T.);
#49234=EDGE_CURVE('',#38910,#38907,#6889,.T.);
#49235=EDGE_CURVE('',#38911,#38912,#6890,.T.);
#49236=EDGE_CURVE('',#38908,#38912,#6891,.T.);
#49237=EDGE_CURVE('',#38907,#38911,#6892,.T.);
#49238=EDGE_CURVE('',#38913,#38914,#6893,.T.);
#49239=EDGE_CURVE('',#38912,#38914,#6894,.T.);
#49240=EDGE_CURVE('',#38911,#38913,#6895,.T.);
#49241=EDGE_CURVE('',#38914,#38909,#6896,.T.);
#49242=EDGE_CURVE('',#38913,#38910,#6897,.T.);
#49243=EDGE_CURVE('',#38915,#38916,#6898,.T.);
#49244=EDGE_CURVE('',#38917,#38916,#6899,.T.);
#49245=EDGE_CURVE('',#38918,#38917,#6900,.T.);
#49246=EDGE_CURVE('',#38918,#38915,#6901,.T.);
#49247=EDGE_CURVE('',#38919,#38920,#6902,.T.);
#49248=EDGE_CURVE('',#38916,#38920,#6903,.T.);
#49249=EDGE_CURVE('',#38915,#38919,#6904,.T.);
#49250=EDGE_CURVE('',#38921,#38922,#6905,.T.);
#49251=EDGE_CURVE('',#38920,#38922,#6906,.T.);
#49252=EDGE_CURVE('',#38919,#38921,#6907,.T.);
#49253=EDGE_CURVE('',#38922,#38917,#6908,.T.);
#49254=EDGE_CURVE('',#38921,#38918,#6909,.T.);
#49255=EDGE_CURVE('',#38923,#38924,#6910,.T.);
#49256=EDGE_CURVE('',#38925,#38924,#6911,.T.);
#49257=EDGE_CURVE('',#38926,#38925,#6912,.T.);
#49258=EDGE_CURVE('',#38926,#38923,#6913,.T.);
#49259=EDGE_CURVE('',#38927,#38928,#6914,.T.);
#49260=EDGE_CURVE('',#38924,#38928,#6915,.T.);
#49261=EDGE_CURVE('',#38923,#38927,#6916,.T.);
#49262=EDGE_CURVE('',#38929,#38930,#6917,.T.);
#49263=EDGE_CURVE('',#38928,#38930,#6918,.T.);
#49264=EDGE_CURVE('',#38927,#38929,#6919,.T.);
#49265=EDGE_CURVE('',#38930,#38925,#6920,.T.);
#49266=EDGE_CURVE('',#38929,#38926,#6921,.T.);
#49267=EDGE_CURVE('',#38931,#38932,#6922,.T.);
#49268=EDGE_CURVE('',#38933,#38932,#6923,.T.);
#49269=EDGE_CURVE('',#38934,#38933,#6924,.T.);
#49270=EDGE_CURVE('',#38934,#38931,#6925,.T.);
#49271=EDGE_CURVE('',#38935,#38936,#6926,.T.);
#49272=EDGE_CURVE('',#38932,#38936,#6927,.T.);
#49273=EDGE_CURVE('',#38931,#38935,#6928,.T.);
#49274=EDGE_CURVE('',#38937,#38938,#6929,.T.);
#49275=EDGE_CURVE('',#38936,#38938,#6930,.T.);
#49276=EDGE_CURVE('',#38935,#38937,#6931,.T.);
#49277=EDGE_CURVE('',#38938,#38933,#6932,.T.);
#49278=EDGE_CURVE('',#38937,#38934,#6933,.T.);
#49279=EDGE_CURVE('',#38939,#38940,#6934,.T.);
#49280=EDGE_CURVE('',#38941,#38940,#6935,.T.);
#49281=EDGE_CURVE('',#38942,#38941,#6936,.T.);
#49282=EDGE_CURVE('',#38942,#38939,#6937,.T.);
#49283=EDGE_CURVE('',#38943,#38944,#6938,.T.);
#49284=EDGE_CURVE('',#38940,#38944,#6939,.T.);
#49285=EDGE_CURVE('',#38939,#38943,#6940,.T.);
#49286=EDGE_CURVE('',#38945,#38946,#6941,.T.);
#49287=EDGE_CURVE('',#38944,#38946,#6942,.T.);
#49288=EDGE_CURVE('',#38943,#38945,#6943,.T.);
#49289=EDGE_CURVE('',#38946,#38941,#6944,.T.);
#49290=EDGE_CURVE('',#38945,#38942,#6945,.T.);
#49291=EDGE_CURVE('',#38947,#38948,#6946,.T.);
#49292=EDGE_CURVE('',#38949,#38948,#6947,.T.);
#49293=EDGE_CURVE('',#38950,#38949,#6948,.T.);
#49294=EDGE_CURVE('',#38950,#38947,#6949,.T.);
#49295=EDGE_CURVE('',#38951,#38952,#6950,.T.);
#49296=EDGE_CURVE('',#38948,#38952,#6951,.T.);
#49297=EDGE_CURVE('',#38947,#38951,#6952,.T.);
#49298=EDGE_CURVE('',#38953,#38954,#6953,.T.);
#49299=EDGE_CURVE('',#38952,#38954,#6954,.T.);
#49300=EDGE_CURVE('',#38951,#38953,#6955,.T.);
#49301=EDGE_CURVE('',#38954,#38949,#6956,.T.);
#49302=EDGE_CURVE('',#38953,#38950,#6957,.T.);
#49303=EDGE_CURVE('',#38955,#38956,#6958,.T.);
#49304=EDGE_CURVE('',#38957,#38956,#6959,.T.);
#49305=EDGE_CURVE('',#38958,#38957,#6960,.T.);
#49306=EDGE_CURVE('',#38958,#38955,#6961,.T.);
#49307=EDGE_CURVE('',#38959,#38960,#6962,.T.);
#49308=EDGE_CURVE('',#38956,#38960,#6963,.T.);
#49309=EDGE_CURVE('',#38955,#38959,#6964,.T.);
#49310=EDGE_CURVE('',#38961,#38962,#6965,.T.);
#49311=EDGE_CURVE('',#38960,#38962,#6966,.T.);
#49312=EDGE_CURVE('',#38959,#38961,#6967,.T.);
#49313=EDGE_CURVE('',#38962,#38957,#6968,.T.);
#49314=EDGE_CURVE('',#38961,#38958,#6969,.T.);
#49315=EDGE_CURVE('',#38963,#38964,#6970,.T.);
#49316=EDGE_CURVE('',#38965,#38964,#6971,.T.);
#49317=EDGE_CURVE('',#38966,#38965,#6972,.T.);
#49318=EDGE_CURVE('',#38966,#38963,#6973,.T.);
#49319=EDGE_CURVE('',#38967,#38968,#6974,.T.);
#49320=EDGE_CURVE('',#38964,#38968,#6975,.T.);
#49321=EDGE_CURVE('',#38963,#38967,#6976,.T.);
#49322=EDGE_CURVE('',#38969,#38970,#6977,.T.);
#49323=EDGE_CURVE('',#38968,#38970,#6978,.T.);
#49324=EDGE_CURVE('',#38967,#38969,#6979,.T.);
#49325=EDGE_CURVE('',#38970,#38965,#6980,.T.);
#49326=EDGE_CURVE('',#38969,#38966,#6981,.T.);
#49327=EDGE_CURVE('',#38971,#38972,#6982,.T.);
#49328=EDGE_CURVE('',#38973,#38972,#6983,.T.);
#49329=EDGE_CURVE('',#38974,#38973,#6984,.T.);
#49330=EDGE_CURVE('',#38974,#38971,#6985,.T.);
#49331=EDGE_CURVE('',#38975,#38976,#6986,.T.);
#49332=EDGE_CURVE('',#38972,#38976,#6987,.T.);
#49333=EDGE_CURVE('',#38971,#38975,#6988,.T.);
#49334=EDGE_CURVE('',#38977,#38978,#6989,.T.);
#49335=EDGE_CURVE('',#38976,#38978,#6990,.T.);
#49336=EDGE_CURVE('',#38975,#38977,#6991,.T.);
#49337=EDGE_CURVE('',#38978,#38973,#6992,.T.);
#49338=EDGE_CURVE('',#38977,#38974,#6993,.T.);
#49339=EDGE_CURVE('',#38979,#38980,#6994,.T.);
#49340=EDGE_CURVE('',#38981,#38980,#6995,.T.);
#49341=EDGE_CURVE('',#38982,#38981,#6996,.T.);
#49342=EDGE_CURVE('',#38982,#38979,#6997,.T.);
#49343=EDGE_CURVE('',#38983,#38984,#6998,.T.);
#49344=EDGE_CURVE('',#38980,#38984,#6999,.T.);
#49345=EDGE_CURVE('',#38979,#38983,#7000,.T.);
#49346=EDGE_CURVE('',#38985,#38986,#7001,.T.);
#49347=EDGE_CURVE('',#38984,#38986,#7002,.T.);
#49348=EDGE_CURVE('',#38983,#38985,#7003,.T.);
#49349=EDGE_CURVE('',#38986,#38981,#7004,.T.);
#49350=EDGE_CURVE('',#38985,#38982,#7005,.T.);
#49351=EDGE_CURVE('',#38987,#38988,#7006,.T.);
#49352=EDGE_CURVE('',#38989,#38988,#7007,.T.);
#49353=EDGE_CURVE('',#38990,#38989,#7008,.T.);
#49354=EDGE_CURVE('',#38990,#38987,#7009,.T.);
#49355=EDGE_CURVE('',#38991,#38992,#7010,.T.);
#49356=EDGE_CURVE('',#38988,#38992,#7011,.T.);
#49357=EDGE_CURVE('',#38987,#38991,#7012,.T.);
#49358=EDGE_CURVE('',#38993,#38994,#7013,.T.);
#49359=EDGE_CURVE('',#38992,#38994,#7014,.T.);
#49360=EDGE_CURVE('',#38991,#38993,#7015,.T.);
#49361=EDGE_CURVE('',#38994,#38989,#7016,.T.);
#49362=EDGE_CURVE('',#38993,#38990,#7017,.T.);
#49363=EDGE_CURVE('',#38995,#38996,#7018,.T.);
#49364=EDGE_CURVE('',#38997,#38996,#7019,.T.);
#49365=EDGE_CURVE('',#38998,#38997,#7020,.T.);
#49366=EDGE_CURVE('',#38998,#38995,#7021,.T.);
#49367=EDGE_CURVE('',#38999,#39000,#7022,.T.);
#49368=EDGE_CURVE('',#38996,#39000,#7023,.T.);
#49369=EDGE_CURVE('',#38995,#38999,#7024,.T.);
#49370=EDGE_CURVE('',#39001,#39002,#7025,.T.);
#49371=EDGE_CURVE('',#39000,#39002,#7026,.T.);
#49372=EDGE_CURVE('',#38999,#39001,#7027,.T.);
#49373=EDGE_CURVE('',#39002,#38997,#7028,.T.);
#49374=EDGE_CURVE('',#39001,#38998,#7029,.T.);
#49375=EDGE_CURVE('',#39003,#39004,#7030,.T.);
#49376=EDGE_CURVE('',#39005,#39004,#7031,.T.);
#49377=EDGE_CURVE('',#39006,#39005,#7032,.T.);
#49378=EDGE_CURVE('',#39006,#39003,#7033,.T.);
#49379=EDGE_CURVE('',#39007,#39008,#7034,.T.);
#49380=EDGE_CURVE('',#39004,#39008,#7035,.T.);
#49381=EDGE_CURVE('',#39003,#39007,#7036,.T.);
#49382=EDGE_CURVE('',#39009,#39010,#7037,.T.);
#49383=EDGE_CURVE('',#39008,#39010,#7038,.T.);
#49384=EDGE_CURVE('',#39007,#39009,#7039,.T.);
#49385=EDGE_CURVE('',#39010,#39005,#7040,.T.);
#49386=EDGE_CURVE('',#39009,#39006,#7041,.T.);
#49387=EDGE_CURVE('',#39011,#39012,#7042,.T.);
#49388=EDGE_CURVE('',#39013,#39012,#7043,.T.);
#49389=EDGE_CURVE('',#39014,#39013,#7044,.T.);
#49390=EDGE_CURVE('',#39014,#39011,#7045,.T.);
#49391=EDGE_CURVE('',#39015,#39016,#7046,.T.);
#49392=EDGE_CURVE('',#39012,#39016,#7047,.T.);
#49393=EDGE_CURVE('',#39011,#39015,#7048,.T.);
#49394=EDGE_CURVE('',#39017,#39018,#7049,.T.);
#49395=EDGE_CURVE('',#39016,#39018,#7050,.T.);
#49396=EDGE_CURVE('',#39015,#39017,#7051,.T.);
#49397=EDGE_CURVE('',#39018,#39013,#7052,.T.);
#49398=EDGE_CURVE('',#39017,#39014,#7053,.T.);
#49399=EDGE_CURVE('',#39019,#39020,#7054,.T.);
#49400=EDGE_CURVE('',#39021,#39020,#7055,.T.);
#49401=EDGE_CURVE('',#39022,#39021,#7056,.T.);
#49402=EDGE_CURVE('',#39022,#39019,#7057,.T.);
#49403=EDGE_CURVE('',#39023,#39024,#7058,.T.);
#49404=EDGE_CURVE('',#39020,#39024,#7059,.T.);
#49405=EDGE_CURVE('',#39019,#39023,#7060,.T.);
#49406=EDGE_CURVE('',#39025,#39026,#7061,.T.);
#49407=EDGE_CURVE('',#39024,#39026,#7062,.T.);
#49408=EDGE_CURVE('',#39023,#39025,#7063,.T.);
#49409=EDGE_CURVE('',#39026,#39021,#7064,.T.);
#49410=EDGE_CURVE('',#39025,#39022,#7065,.T.);
#49411=EDGE_CURVE('',#39027,#39028,#7066,.T.);
#49412=EDGE_CURVE('',#39029,#39028,#7067,.T.);
#49413=EDGE_CURVE('',#39030,#39029,#7068,.T.);
#49414=EDGE_CURVE('',#39030,#39027,#7069,.T.);
#49415=EDGE_CURVE('',#39031,#39032,#7070,.T.);
#49416=EDGE_CURVE('',#39028,#39032,#7071,.T.);
#49417=EDGE_CURVE('',#39027,#39031,#7072,.T.);
#49418=EDGE_CURVE('',#39033,#39034,#7073,.T.);
#49419=EDGE_CURVE('',#39032,#39034,#7074,.T.);
#49420=EDGE_CURVE('',#39031,#39033,#7075,.T.);
#49421=EDGE_CURVE('',#39034,#39029,#7076,.T.);
#49422=EDGE_CURVE('',#39033,#39030,#7077,.T.);
#49423=EDGE_CURVE('',#39035,#39036,#7078,.T.);
#49424=EDGE_CURVE('',#39037,#39036,#7079,.T.);
#49425=EDGE_CURVE('',#39038,#39037,#7080,.T.);
#49426=EDGE_CURVE('',#39038,#39035,#7081,.T.);
#49427=EDGE_CURVE('',#39039,#39040,#7082,.T.);
#49428=EDGE_CURVE('',#39036,#39040,#7083,.T.);
#49429=EDGE_CURVE('',#39035,#39039,#7084,.T.);
#49430=EDGE_CURVE('',#39041,#39042,#7085,.T.);
#49431=EDGE_CURVE('',#39040,#39042,#7086,.T.);
#49432=EDGE_CURVE('',#39039,#39041,#7087,.T.);
#49433=EDGE_CURVE('',#39042,#39037,#7088,.T.);
#49434=EDGE_CURVE('',#39041,#39038,#7089,.T.);
#49435=EDGE_CURVE('',#39043,#39044,#7090,.T.);
#49436=EDGE_CURVE('',#39045,#39044,#7091,.T.);
#49437=EDGE_CURVE('',#39046,#39045,#7092,.T.);
#49438=EDGE_CURVE('',#39046,#39043,#7093,.T.);
#49439=EDGE_CURVE('',#39047,#39048,#7094,.T.);
#49440=EDGE_CURVE('',#39044,#39048,#7095,.T.);
#49441=EDGE_CURVE('',#39043,#39047,#7096,.T.);
#49442=EDGE_CURVE('',#39049,#39050,#7097,.T.);
#49443=EDGE_CURVE('',#39048,#39050,#7098,.T.);
#49444=EDGE_CURVE('',#39047,#39049,#7099,.T.);
#49445=EDGE_CURVE('',#39050,#39045,#7100,.T.);
#49446=EDGE_CURVE('',#39049,#39046,#7101,.T.);
#49447=EDGE_CURVE('',#39051,#39052,#7102,.T.);
#49448=EDGE_CURVE('',#39053,#39052,#7103,.T.);
#49449=EDGE_CURVE('',#39054,#39053,#7104,.T.);
#49450=EDGE_CURVE('',#39054,#39051,#7105,.T.);
#49451=EDGE_CURVE('',#39055,#39056,#7106,.T.);
#49452=EDGE_CURVE('',#39052,#39056,#7107,.T.);
#49453=EDGE_CURVE('',#39051,#39055,#7108,.T.);
#49454=EDGE_CURVE('',#39057,#39058,#7109,.T.);
#49455=EDGE_CURVE('',#39056,#39058,#7110,.T.);
#49456=EDGE_CURVE('',#39055,#39057,#7111,.T.);
#49457=EDGE_CURVE('',#39058,#39053,#7112,.T.);
#49458=EDGE_CURVE('',#39057,#39054,#7113,.T.);
#49459=EDGE_CURVE('',#39059,#39060,#7114,.T.);
#49460=EDGE_CURVE('',#39061,#39060,#7115,.T.);
#49461=EDGE_CURVE('',#39062,#39061,#7116,.T.);
#49462=EDGE_CURVE('',#39062,#39059,#7117,.T.);
#49463=EDGE_CURVE('',#39063,#39064,#7118,.T.);
#49464=EDGE_CURVE('',#39060,#39064,#7119,.T.);
#49465=EDGE_CURVE('',#39059,#39063,#7120,.T.);
#49466=EDGE_CURVE('',#39065,#39066,#7121,.T.);
#49467=EDGE_CURVE('',#39064,#39066,#7122,.T.);
#49468=EDGE_CURVE('',#39063,#39065,#7123,.T.);
#49469=EDGE_CURVE('',#39066,#39061,#7124,.T.);
#49470=EDGE_CURVE('',#39065,#39062,#7125,.T.);
#49471=EDGE_CURVE('',#39067,#39068,#7126,.T.);
#49472=EDGE_CURVE('',#39069,#39068,#7127,.T.);
#49473=EDGE_CURVE('',#39070,#39069,#7128,.T.);
#49474=EDGE_CURVE('',#39070,#39067,#7129,.T.);
#49475=EDGE_CURVE('',#39071,#39072,#7130,.T.);
#49476=EDGE_CURVE('',#39068,#39072,#7131,.T.);
#49477=EDGE_CURVE('',#39067,#39071,#7132,.T.);
#49478=EDGE_CURVE('',#39073,#39074,#7133,.T.);
#49479=EDGE_CURVE('',#39072,#39074,#7134,.T.);
#49480=EDGE_CURVE('',#39071,#39073,#7135,.T.);
#49481=EDGE_CURVE('',#39074,#39069,#7136,.T.);
#49482=EDGE_CURVE('',#39073,#39070,#7137,.T.);
#49483=EDGE_CURVE('',#39075,#39076,#7138,.T.);
#49484=EDGE_CURVE('',#39077,#39076,#7139,.T.);
#49485=EDGE_CURVE('',#39078,#39077,#7140,.T.);
#49486=EDGE_CURVE('',#39078,#39075,#7141,.T.);
#49487=EDGE_CURVE('',#39079,#39080,#7142,.T.);
#49488=EDGE_CURVE('',#39076,#39080,#7143,.T.);
#49489=EDGE_CURVE('',#39075,#39079,#7144,.T.);
#49490=EDGE_CURVE('',#39081,#39082,#7145,.T.);
#49491=EDGE_CURVE('',#39080,#39082,#7146,.T.);
#49492=EDGE_CURVE('',#39079,#39081,#7147,.T.);
#49493=EDGE_CURVE('',#39082,#39077,#7148,.T.);
#49494=EDGE_CURVE('',#39081,#39078,#7149,.T.);
#49495=EDGE_CURVE('',#39083,#39084,#7150,.T.);
#49496=EDGE_CURVE('',#39085,#39084,#7151,.T.);
#49497=EDGE_CURVE('',#39086,#39085,#7152,.T.);
#49498=EDGE_CURVE('',#39086,#39083,#7153,.T.);
#49499=EDGE_CURVE('',#39087,#39088,#7154,.T.);
#49500=EDGE_CURVE('',#39084,#39088,#7155,.T.);
#49501=EDGE_CURVE('',#39083,#39087,#7156,.T.);
#49502=EDGE_CURVE('',#39089,#39090,#7157,.T.);
#49503=EDGE_CURVE('',#39088,#39090,#7158,.T.);
#49504=EDGE_CURVE('',#39087,#39089,#7159,.T.);
#49505=EDGE_CURVE('',#39090,#39085,#7160,.T.);
#49506=EDGE_CURVE('',#39089,#39086,#7161,.T.);
#49507=EDGE_CURVE('',#39091,#39092,#7162,.T.);
#49508=EDGE_CURVE('',#39093,#39092,#7163,.T.);
#49509=EDGE_CURVE('',#39094,#39093,#7164,.T.);
#49510=EDGE_CURVE('',#39094,#39091,#7165,.T.);
#49511=EDGE_CURVE('',#39095,#39096,#7166,.T.);
#49512=EDGE_CURVE('',#39092,#39096,#7167,.T.);
#49513=EDGE_CURVE('',#39091,#39095,#7168,.T.);
#49514=EDGE_CURVE('',#39097,#39098,#7169,.T.);
#49515=EDGE_CURVE('',#39096,#39098,#7170,.T.);
#49516=EDGE_CURVE('',#39095,#39097,#7171,.T.);
#49517=EDGE_CURVE('',#39098,#39093,#7172,.T.);
#49518=EDGE_CURVE('',#39097,#39094,#7173,.T.);
#49519=EDGE_CURVE('',#39099,#39100,#7174,.T.);
#49520=EDGE_CURVE('',#39101,#39100,#7175,.T.);
#49521=EDGE_CURVE('',#39102,#39101,#7176,.T.);
#49522=EDGE_CURVE('',#39102,#39099,#7177,.T.);
#49523=EDGE_CURVE('',#39103,#39104,#7178,.T.);
#49524=EDGE_CURVE('',#39100,#39104,#7179,.T.);
#49525=EDGE_CURVE('',#39099,#39103,#7180,.T.);
#49526=EDGE_CURVE('',#39105,#39106,#7181,.T.);
#49527=EDGE_CURVE('',#39104,#39106,#7182,.T.);
#49528=EDGE_CURVE('',#39103,#39105,#7183,.T.);
#49529=EDGE_CURVE('',#39106,#39101,#7184,.T.);
#49530=EDGE_CURVE('',#39105,#39102,#7185,.T.);
#49531=EDGE_CURVE('',#39107,#39108,#7186,.T.);
#49532=EDGE_CURVE('',#39109,#39108,#7187,.T.);
#49533=EDGE_CURVE('',#39110,#39109,#7188,.T.);
#49534=EDGE_CURVE('',#39110,#39107,#7189,.T.);
#49535=EDGE_CURVE('',#39111,#39112,#7190,.T.);
#49536=EDGE_CURVE('',#39108,#39112,#7191,.T.);
#49537=EDGE_CURVE('',#39107,#39111,#7192,.T.);
#49538=EDGE_CURVE('',#39113,#39114,#7193,.T.);
#49539=EDGE_CURVE('',#39112,#39114,#7194,.T.);
#49540=EDGE_CURVE('',#39111,#39113,#7195,.T.);
#49541=EDGE_CURVE('',#39114,#39109,#7196,.T.);
#49542=EDGE_CURVE('',#39113,#39110,#7197,.T.);
#49543=EDGE_CURVE('',#39115,#39116,#7198,.T.);
#49544=EDGE_CURVE('',#39117,#39116,#7199,.T.);
#49545=EDGE_CURVE('',#39118,#39117,#7200,.T.);
#49546=EDGE_CURVE('',#39118,#39115,#7201,.T.);
#49547=EDGE_CURVE('',#39119,#39120,#7202,.T.);
#49548=EDGE_CURVE('',#39116,#39120,#7203,.T.);
#49549=EDGE_CURVE('',#39115,#39119,#7204,.T.);
#49550=EDGE_CURVE('',#39121,#39122,#7205,.T.);
#49551=EDGE_CURVE('',#39120,#39122,#7206,.T.);
#49552=EDGE_CURVE('',#39119,#39121,#7207,.T.);
#49553=EDGE_CURVE('',#39122,#39117,#7208,.T.);
#49554=EDGE_CURVE('',#39121,#39118,#7209,.T.);
#49555=EDGE_CURVE('',#39123,#39124,#7210,.T.);
#49556=EDGE_CURVE('',#39125,#39124,#7211,.T.);
#49557=EDGE_CURVE('',#39126,#39125,#7212,.T.);
#49558=EDGE_CURVE('',#39126,#39123,#7213,.T.);
#49559=EDGE_CURVE('',#39127,#39128,#7214,.T.);
#49560=EDGE_CURVE('',#39124,#39128,#7215,.T.);
#49561=EDGE_CURVE('',#39123,#39127,#7216,.T.);
#49562=EDGE_CURVE('',#39129,#39130,#7217,.T.);
#49563=EDGE_CURVE('',#39128,#39130,#7218,.T.);
#49564=EDGE_CURVE('',#39127,#39129,#7219,.T.);
#49565=EDGE_CURVE('',#39130,#39125,#7220,.T.);
#49566=EDGE_CURVE('',#39129,#39126,#7221,.T.);
#49567=EDGE_CURVE('',#39131,#39132,#7222,.T.);
#49568=EDGE_CURVE('',#39133,#39132,#7223,.T.);
#49569=EDGE_CURVE('',#39134,#39133,#7224,.T.);
#49570=EDGE_CURVE('',#39134,#39131,#7225,.T.);
#49571=EDGE_CURVE('',#39135,#39136,#7226,.T.);
#49572=EDGE_CURVE('',#39132,#39136,#7227,.T.);
#49573=EDGE_CURVE('',#39131,#39135,#7228,.T.);
#49574=EDGE_CURVE('',#39137,#39138,#7229,.T.);
#49575=EDGE_CURVE('',#39136,#39138,#7230,.T.);
#49576=EDGE_CURVE('',#39135,#39137,#7231,.T.);
#49577=EDGE_CURVE('',#39138,#39133,#7232,.T.);
#49578=EDGE_CURVE('',#39137,#39134,#7233,.T.);
#49579=EDGE_CURVE('',#39139,#39140,#7234,.T.);
#49580=EDGE_CURVE('',#39141,#39140,#7235,.T.);
#49581=EDGE_CURVE('',#39142,#39141,#7236,.T.);
#49582=EDGE_CURVE('',#39142,#39139,#7237,.T.);
#49583=EDGE_CURVE('',#39143,#39144,#7238,.T.);
#49584=EDGE_CURVE('',#39140,#39144,#7239,.T.);
#49585=EDGE_CURVE('',#39139,#39143,#7240,.T.);
#49586=EDGE_CURVE('',#39145,#39146,#7241,.T.);
#49587=EDGE_CURVE('',#39144,#39146,#7242,.T.);
#49588=EDGE_CURVE('',#39143,#39145,#7243,.T.);
#49589=EDGE_CURVE('',#39146,#39141,#7244,.T.);
#49590=EDGE_CURVE('',#39145,#39142,#7245,.T.);
#49591=EDGE_CURVE('',#39147,#39148,#7246,.T.);
#49592=EDGE_CURVE('',#39149,#39148,#7247,.T.);
#49593=EDGE_CURVE('',#39150,#39149,#7248,.T.);
#49594=EDGE_CURVE('',#39150,#39147,#7249,.T.);
#49595=EDGE_CURVE('',#39151,#39152,#7250,.T.);
#49596=EDGE_CURVE('',#39148,#39152,#7251,.T.);
#49597=EDGE_CURVE('',#39147,#39151,#7252,.T.);
#49598=EDGE_CURVE('',#39153,#39154,#7253,.T.);
#49599=EDGE_CURVE('',#39152,#39154,#7254,.T.);
#49600=EDGE_CURVE('',#39151,#39153,#7255,.T.);
#49601=EDGE_CURVE('',#39154,#39149,#7256,.T.);
#49602=EDGE_CURVE('',#39153,#39150,#7257,.T.);
#49603=EDGE_CURVE('',#39155,#39156,#7258,.T.);
#49604=EDGE_CURVE('',#39157,#39156,#7259,.T.);
#49605=EDGE_CURVE('',#39158,#39157,#7260,.T.);
#49606=EDGE_CURVE('',#39158,#39155,#7261,.T.);
#49607=EDGE_CURVE('',#39159,#39160,#7262,.T.);
#49608=EDGE_CURVE('',#39156,#39160,#7263,.T.);
#49609=EDGE_CURVE('',#39155,#39159,#7264,.T.);
#49610=EDGE_CURVE('',#39161,#39162,#7265,.T.);
#49611=EDGE_CURVE('',#39160,#39162,#7266,.T.);
#49612=EDGE_CURVE('',#39159,#39161,#7267,.T.);
#49613=EDGE_CURVE('',#39162,#39157,#7268,.T.);
#49614=EDGE_CURVE('',#39161,#39158,#7269,.T.);
#49615=EDGE_CURVE('',#39163,#39164,#7270,.T.);
#49616=EDGE_CURVE('',#39165,#39164,#7271,.T.);
#49617=EDGE_CURVE('',#39166,#39165,#7272,.T.);
#49618=EDGE_CURVE('',#39166,#39163,#7273,.T.);
#49619=EDGE_CURVE('',#39167,#39168,#7274,.T.);
#49620=EDGE_CURVE('',#39164,#39168,#7275,.T.);
#49621=EDGE_CURVE('',#39163,#39167,#7276,.T.);
#49622=EDGE_CURVE('',#39169,#39170,#7277,.T.);
#49623=EDGE_CURVE('',#39168,#39170,#7278,.T.);
#49624=EDGE_CURVE('',#39167,#39169,#7279,.T.);
#49625=EDGE_CURVE('',#39170,#39165,#7280,.T.);
#49626=EDGE_CURVE('',#39169,#39166,#7281,.T.);
#49627=EDGE_CURVE('',#39171,#39172,#7282,.T.);
#49628=EDGE_CURVE('',#39173,#39172,#7283,.T.);
#49629=EDGE_CURVE('',#39174,#39173,#7284,.T.);
#49630=EDGE_CURVE('',#39174,#39171,#7285,.T.);
#49631=EDGE_CURVE('',#39175,#39176,#7286,.T.);
#49632=EDGE_CURVE('',#39172,#39176,#7287,.T.);
#49633=EDGE_CURVE('',#39171,#39175,#7288,.T.);
#49634=EDGE_CURVE('',#39177,#39178,#7289,.T.);
#49635=EDGE_CURVE('',#39176,#39178,#7290,.T.);
#49636=EDGE_CURVE('',#39175,#39177,#7291,.T.);
#49637=EDGE_CURVE('',#39178,#39173,#7292,.T.);
#49638=EDGE_CURVE('',#39177,#39174,#7293,.T.);
#49639=EDGE_CURVE('',#39179,#39180,#7294,.T.);
#49640=EDGE_CURVE('',#39181,#39180,#7295,.T.);
#49641=EDGE_CURVE('',#39182,#39181,#7296,.T.);
#49642=EDGE_CURVE('',#39182,#39179,#7297,.T.);
#49643=EDGE_CURVE('',#39183,#39184,#7298,.T.);
#49644=EDGE_CURVE('',#39180,#39184,#7299,.T.);
#49645=EDGE_CURVE('',#39179,#39183,#7300,.T.);
#49646=EDGE_CURVE('',#39185,#39186,#7301,.T.);
#49647=EDGE_CURVE('',#39184,#39186,#7302,.T.);
#49648=EDGE_CURVE('',#39183,#39185,#7303,.T.);
#49649=EDGE_CURVE('',#39186,#39181,#7304,.T.);
#49650=EDGE_CURVE('',#39185,#39182,#7305,.T.);
#49651=EDGE_CURVE('',#39187,#39188,#7306,.T.);
#49652=EDGE_CURVE('',#39189,#39188,#7307,.T.);
#49653=EDGE_CURVE('',#39190,#39189,#7308,.T.);
#49654=EDGE_CURVE('',#39190,#39187,#7309,.T.);
#49655=EDGE_CURVE('',#39191,#39192,#7310,.T.);
#49656=EDGE_CURVE('',#39188,#39192,#7311,.T.);
#49657=EDGE_CURVE('',#39187,#39191,#7312,.T.);
#49658=EDGE_CURVE('',#39193,#39194,#7313,.T.);
#49659=EDGE_CURVE('',#39192,#39194,#7314,.T.);
#49660=EDGE_CURVE('',#39191,#39193,#7315,.T.);
#49661=EDGE_CURVE('',#39194,#39189,#7316,.T.);
#49662=EDGE_CURVE('',#39193,#39190,#7317,.T.);
#49663=EDGE_CURVE('',#39195,#39196,#7318,.T.);
#49664=EDGE_CURVE('',#39197,#39196,#7319,.T.);
#49665=EDGE_CURVE('',#39198,#39197,#7320,.T.);
#49666=EDGE_CURVE('',#39198,#39195,#7321,.T.);
#49667=EDGE_CURVE('',#39199,#39200,#7322,.T.);
#49668=EDGE_CURVE('',#39196,#39200,#7323,.T.);
#49669=EDGE_CURVE('',#39195,#39199,#7324,.T.);
#49670=EDGE_CURVE('',#39201,#39202,#7325,.T.);
#49671=EDGE_CURVE('',#39200,#39202,#7326,.T.);
#49672=EDGE_CURVE('',#39199,#39201,#7327,.T.);
#49673=EDGE_CURVE('',#39202,#39197,#7328,.T.);
#49674=EDGE_CURVE('',#39201,#39198,#7329,.T.);
#49675=EDGE_CURVE('',#39203,#39204,#7330,.T.);
#49676=EDGE_CURVE('',#39205,#39204,#7331,.T.);
#49677=EDGE_CURVE('',#39206,#39205,#7332,.T.);
#49678=EDGE_CURVE('',#39206,#39203,#7333,.T.);
#49679=EDGE_CURVE('',#39207,#39208,#7334,.T.);
#49680=EDGE_CURVE('',#39204,#39208,#7335,.T.);
#49681=EDGE_CURVE('',#39203,#39207,#7336,.T.);
#49682=EDGE_CURVE('',#39209,#39210,#7337,.T.);
#49683=EDGE_CURVE('',#39208,#39210,#7338,.T.);
#49684=EDGE_CURVE('',#39207,#39209,#7339,.T.);
#49685=EDGE_CURVE('',#39210,#39205,#7340,.T.);
#49686=EDGE_CURVE('',#39209,#39206,#7341,.T.);
#49687=EDGE_CURVE('',#39211,#39212,#7342,.T.);
#49688=EDGE_CURVE('',#39213,#39212,#7343,.T.);
#49689=EDGE_CURVE('',#39214,#39213,#7344,.T.);
#49690=EDGE_CURVE('',#39214,#39211,#7345,.T.);
#49691=EDGE_CURVE('',#39215,#39216,#7346,.T.);
#49692=EDGE_CURVE('',#39212,#39216,#7347,.T.);
#49693=EDGE_CURVE('',#39211,#39215,#7348,.T.);
#49694=EDGE_CURVE('',#39217,#39218,#7349,.T.);
#49695=EDGE_CURVE('',#39216,#39218,#7350,.T.);
#49696=EDGE_CURVE('',#39215,#39217,#7351,.T.);
#49697=EDGE_CURVE('',#39218,#39213,#7352,.T.);
#49698=EDGE_CURVE('',#39217,#39214,#7353,.T.);
#49699=EDGE_CURVE('',#39219,#39220,#7354,.T.);
#49700=EDGE_CURVE('',#39221,#39220,#7355,.T.);
#49701=EDGE_CURVE('',#39222,#39221,#7356,.T.);
#49702=EDGE_CURVE('',#39222,#39219,#7357,.T.);
#49703=EDGE_CURVE('',#39223,#39224,#7358,.T.);
#49704=EDGE_CURVE('',#39220,#39224,#7359,.T.);
#49705=EDGE_CURVE('',#39219,#39223,#7360,.T.);
#49706=EDGE_CURVE('',#39225,#39226,#7361,.T.);
#49707=EDGE_CURVE('',#39224,#39226,#7362,.T.);
#49708=EDGE_CURVE('',#39223,#39225,#7363,.T.);
#49709=EDGE_CURVE('',#39226,#39221,#7364,.T.);
#49710=EDGE_CURVE('',#39225,#39222,#7365,.T.);
#49711=EDGE_CURVE('',#39227,#39228,#7366,.T.);
#49712=EDGE_CURVE('',#39229,#39228,#7367,.T.);
#49713=EDGE_CURVE('',#39230,#39229,#7368,.T.);
#49714=EDGE_CURVE('',#39230,#39227,#7369,.T.);
#49715=EDGE_CURVE('',#39231,#39232,#7370,.T.);
#49716=EDGE_CURVE('',#39228,#39232,#7371,.T.);
#49717=EDGE_CURVE('',#39227,#39231,#7372,.T.);
#49718=EDGE_CURVE('',#39233,#39234,#7373,.T.);
#49719=EDGE_CURVE('',#39232,#39234,#7374,.T.);
#49720=EDGE_CURVE('',#39231,#39233,#7375,.T.);
#49721=EDGE_CURVE('',#39234,#39229,#7376,.T.);
#49722=EDGE_CURVE('',#39233,#39230,#7377,.T.);
#49723=EDGE_CURVE('',#39235,#39236,#7378,.T.);
#49724=EDGE_CURVE('',#39237,#39236,#7379,.T.);
#49725=EDGE_CURVE('',#39238,#39237,#7380,.T.);
#49726=EDGE_CURVE('',#39238,#39235,#7381,.T.);
#49727=EDGE_CURVE('',#39239,#39240,#7382,.T.);
#49728=EDGE_CURVE('',#39236,#39240,#7383,.T.);
#49729=EDGE_CURVE('',#39235,#39239,#7384,.T.);
#49730=EDGE_CURVE('',#39241,#39242,#7385,.T.);
#49731=EDGE_CURVE('',#39240,#39242,#7386,.T.);
#49732=EDGE_CURVE('',#39239,#39241,#7387,.T.);
#49733=EDGE_CURVE('',#39242,#39237,#7388,.T.);
#49734=EDGE_CURVE('',#39241,#39238,#7389,.T.);
#49735=EDGE_CURVE('',#39243,#39244,#7390,.T.);
#49736=EDGE_CURVE('',#39245,#39244,#7391,.T.);
#49737=EDGE_CURVE('',#39246,#39245,#7392,.T.);
#49738=EDGE_CURVE('',#39246,#39243,#7393,.T.);
#49739=EDGE_CURVE('',#39247,#39248,#7394,.T.);
#49740=EDGE_CURVE('',#39244,#39248,#7395,.T.);
#49741=EDGE_CURVE('',#39243,#39247,#7396,.T.);
#49742=EDGE_CURVE('',#39249,#39250,#7397,.T.);
#49743=EDGE_CURVE('',#39248,#39250,#7398,.T.);
#49744=EDGE_CURVE('',#39247,#39249,#7399,.T.);
#49745=EDGE_CURVE('',#39250,#39245,#7400,.T.);
#49746=EDGE_CURVE('',#39249,#39246,#7401,.T.);
#49747=EDGE_CURVE('',#39251,#39252,#7402,.T.);
#49748=EDGE_CURVE('',#39253,#39252,#7403,.T.);
#49749=EDGE_CURVE('',#39254,#39253,#7404,.T.);
#49750=EDGE_CURVE('',#39254,#39251,#7405,.T.);
#49751=EDGE_CURVE('',#39255,#39256,#7406,.T.);
#49752=EDGE_CURVE('',#39252,#39256,#7407,.T.);
#49753=EDGE_CURVE('',#39251,#39255,#7408,.T.);
#49754=EDGE_CURVE('',#39257,#39258,#7409,.T.);
#49755=EDGE_CURVE('',#39256,#39258,#7410,.T.);
#49756=EDGE_CURVE('',#39255,#39257,#7411,.T.);
#49757=EDGE_CURVE('',#39258,#39253,#7412,.T.);
#49758=EDGE_CURVE('',#39257,#39254,#7413,.T.);
#49759=EDGE_CURVE('',#39259,#39260,#7414,.T.);
#49760=EDGE_CURVE('',#39261,#39260,#7415,.T.);
#49761=EDGE_CURVE('',#39262,#39261,#7416,.T.);
#49762=EDGE_CURVE('',#39262,#39259,#7417,.T.);
#49763=EDGE_CURVE('',#39263,#39264,#7418,.T.);
#49764=EDGE_CURVE('',#39260,#39264,#7419,.T.);
#49765=EDGE_CURVE('',#39259,#39263,#7420,.T.);
#49766=EDGE_CURVE('',#39265,#39266,#7421,.T.);
#49767=EDGE_CURVE('',#39264,#39266,#7422,.T.);
#49768=EDGE_CURVE('',#39263,#39265,#7423,.T.);
#49769=EDGE_CURVE('',#39266,#39261,#7424,.T.);
#49770=EDGE_CURVE('',#39265,#39262,#7425,.T.);
#49771=EDGE_CURVE('',#39267,#39268,#7426,.T.);
#49772=EDGE_CURVE('',#39269,#39268,#7427,.T.);
#49773=EDGE_CURVE('',#39270,#39269,#7428,.T.);
#49774=EDGE_CURVE('',#39270,#39267,#7429,.T.);
#49775=EDGE_CURVE('',#39271,#39272,#7430,.T.);
#49776=EDGE_CURVE('',#39268,#39272,#7431,.T.);
#49777=EDGE_CURVE('',#39267,#39271,#7432,.T.);
#49778=EDGE_CURVE('',#39273,#39274,#7433,.T.);
#49779=EDGE_CURVE('',#39272,#39274,#7434,.T.);
#49780=EDGE_CURVE('',#39271,#39273,#7435,.T.);
#49781=EDGE_CURVE('',#39274,#39269,#7436,.T.);
#49782=EDGE_CURVE('',#39273,#39270,#7437,.T.);
#49783=EDGE_CURVE('',#39275,#39276,#7438,.T.);
#49784=EDGE_CURVE('',#39277,#39276,#7439,.T.);
#49785=EDGE_CURVE('',#39278,#39277,#7440,.T.);
#49786=EDGE_CURVE('',#39278,#39275,#7441,.T.);
#49787=EDGE_CURVE('',#39279,#39280,#7442,.T.);
#49788=EDGE_CURVE('',#39276,#39280,#7443,.T.);
#49789=EDGE_CURVE('',#39275,#39279,#7444,.T.);
#49790=EDGE_CURVE('',#39281,#39282,#7445,.T.);
#49791=EDGE_CURVE('',#39280,#39282,#7446,.T.);
#49792=EDGE_CURVE('',#39279,#39281,#7447,.T.);
#49793=EDGE_CURVE('',#39282,#39277,#7448,.T.);
#49794=EDGE_CURVE('',#39281,#39278,#7449,.T.);
#49795=EDGE_CURVE('',#39283,#39284,#7450,.T.);
#49796=EDGE_CURVE('',#39285,#39284,#7451,.T.);
#49797=EDGE_CURVE('',#39286,#39285,#7452,.T.);
#49798=EDGE_CURVE('',#39286,#39283,#7453,.T.);
#49799=EDGE_CURVE('',#39287,#39288,#7454,.T.);
#49800=EDGE_CURVE('',#39284,#39288,#7455,.T.);
#49801=EDGE_CURVE('',#39283,#39287,#7456,.T.);
#49802=EDGE_CURVE('',#39289,#39290,#7457,.T.);
#49803=EDGE_CURVE('',#39288,#39290,#7458,.T.);
#49804=EDGE_CURVE('',#39287,#39289,#7459,.T.);
#49805=EDGE_CURVE('',#39290,#39285,#7460,.T.);
#49806=EDGE_CURVE('',#39289,#39286,#7461,.T.);
#49807=EDGE_CURVE('',#39291,#39292,#7462,.T.);
#49808=EDGE_CURVE('',#39293,#39292,#7463,.T.);
#49809=EDGE_CURVE('',#39294,#39293,#7464,.T.);
#49810=EDGE_CURVE('',#39294,#39291,#7465,.T.);
#49811=EDGE_CURVE('',#39295,#39296,#7466,.T.);
#49812=EDGE_CURVE('',#39292,#39296,#7467,.T.);
#49813=EDGE_CURVE('',#39291,#39295,#7468,.T.);
#49814=EDGE_CURVE('',#39297,#39298,#7469,.T.);
#49815=EDGE_CURVE('',#39296,#39298,#7470,.T.);
#49816=EDGE_CURVE('',#39295,#39297,#7471,.T.);
#49817=EDGE_CURVE('',#39298,#39293,#7472,.T.);
#49818=EDGE_CURVE('',#39297,#39294,#7473,.T.);
#49819=EDGE_CURVE('',#39299,#39300,#7474,.T.);
#49820=EDGE_CURVE('',#39301,#39300,#7475,.T.);
#49821=EDGE_CURVE('',#39302,#39301,#7476,.T.);
#49822=EDGE_CURVE('',#39302,#39299,#7477,.T.);
#49823=EDGE_CURVE('',#39303,#39304,#7478,.T.);
#49824=EDGE_CURVE('',#39300,#39304,#7479,.T.);
#49825=EDGE_CURVE('',#39299,#39303,#7480,.T.);
#49826=EDGE_CURVE('',#39305,#39306,#7481,.T.);
#49827=EDGE_CURVE('',#39304,#39306,#7482,.T.);
#49828=EDGE_CURVE('',#39303,#39305,#7483,.T.);
#49829=EDGE_CURVE('',#39306,#39301,#7484,.T.);
#49830=EDGE_CURVE('',#39305,#39302,#7485,.T.);
#49831=EDGE_CURVE('',#39307,#39308,#7486,.T.);
#49832=EDGE_CURVE('',#39309,#39308,#7487,.T.);
#49833=EDGE_CURVE('',#39310,#39309,#7488,.T.);
#49834=EDGE_CURVE('',#39310,#39307,#7489,.T.);
#49835=EDGE_CURVE('',#39311,#39312,#7490,.T.);
#49836=EDGE_CURVE('',#39308,#39312,#7491,.T.);
#49837=EDGE_CURVE('',#39307,#39311,#7492,.T.);
#49838=EDGE_CURVE('',#39313,#39314,#7493,.T.);
#49839=EDGE_CURVE('',#39312,#39314,#7494,.T.);
#49840=EDGE_CURVE('',#39311,#39313,#7495,.T.);
#49841=EDGE_CURVE('',#39314,#39309,#7496,.T.);
#49842=EDGE_CURVE('',#39313,#39310,#7497,.T.);
#49843=EDGE_CURVE('',#39315,#39316,#7498,.T.);
#49844=EDGE_CURVE('',#39317,#39316,#7499,.T.);
#49845=EDGE_CURVE('',#39318,#39317,#7500,.T.);
#49846=EDGE_CURVE('',#39318,#39315,#7501,.T.);
#49847=EDGE_CURVE('',#39319,#39320,#7502,.T.);
#49848=EDGE_CURVE('',#39316,#39320,#7503,.T.);
#49849=EDGE_CURVE('',#39315,#39319,#7504,.T.);
#49850=EDGE_CURVE('',#39321,#39322,#7505,.T.);
#49851=EDGE_CURVE('',#39320,#39322,#7506,.T.);
#49852=EDGE_CURVE('',#39319,#39321,#7507,.T.);
#49853=EDGE_CURVE('',#39322,#39317,#7508,.T.);
#49854=EDGE_CURVE('',#39321,#39318,#7509,.T.);
#49855=EDGE_CURVE('',#39323,#39324,#7510,.T.);
#49856=EDGE_CURVE('',#39325,#39324,#7511,.T.);
#49857=EDGE_CURVE('',#39326,#39325,#7512,.T.);
#49858=EDGE_CURVE('',#39326,#39323,#7513,.T.);
#49859=EDGE_CURVE('',#39327,#39328,#7514,.T.);
#49860=EDGE_CURVE('',#39324,#39328,#7515,.T.);
#49861=EDGE_CURVE('',#39323,#39327,#7516,.T.);
#49862=EDGE_CURVE('',#39329,#39330,#7517,.T.);
#49863=EDGE_CURVE('',#39328,#39330,#7518,.T.);
#49864=EDGE_CURVE('',#39327,#39329,#7519,.T.);
#49865=EDGE_CURVE('',#39330,#39325,#7520,.T.);
#49866=EDGE_CURVE('',#39329,#39326,#7521,.T.);
#49867=EDGE_CURVE('',#39331,#39332,#7522,.T.);
#49868=EDGE_CURVE('',#39333,#39332,#7523,.T.);
#49869=EDGE_CURVE('',#39334,#39333,#7524,.T.);
#49870=EDGE_CURVE('',#39334,#39331,#7525,.T.);
#49871=EDGE_CURVE('',#39335,#39336,#7526,.T.);
#49872=EDGE_CURVE('',#39332,#39336,#7527,.T.);
#49873=EDGE_CURVE('',#39331,#39335,#7528,.T.);
#49874=EDGE_CURVE('',#39337,#39338,#7529,.T.);
#49875=EDGE_CURVE('',#39336,#39338,#7530,.T.);
#49876=EDGE_CURVE('',#39335,#39337,#7531,.T.);
#49877=EDGE_CURVE('',#39338,#39333,#7532,.T.);
#49878=EDGE_CURVE('',#39337,#39334,#7533,.T.);
#49879=EDGE_CURVE('',#39339,#39340,#7534,.T.);
#49880=EDGE_CURVE('',#39341,#39340,#7535,.T.);
#49881=EDGE_CURVE('',#39342,#39341,#7536,.T.);
#49882=EDGE_CURVE('',#39342,#39339,#7537,.T.);
#49883=EDGE_CURVE('',#39343,#39344,#7538,.T.);
#49884=EDGE_CURVE('',#39340,#39344,#7539,.T.);
#49885=EDGE_CURVE('',#39339,#39343,#7540,.T.);
#49886=EDGE_CURVE('',#39345,#39346,#7541,.T.);
#49887=EDGE_CURVE('',#39344,#39346,#7542,.T.);
#49888=EDGE_CURVE('',#39343,#39345,#7543,.T.);
#49889=EDGE_CURVE('',#39346,#39341,#7544,.T.);
#49890=EDGE_CURVE('',#39345,#39342,#7545,.T.);
#49891=EDGE_CURVE('',#39347,#39348,#7546,.T.);
#49892=EDGE_CURVE('',#39349,#39348,#7547,.T.);
#49893=EDGE_CURVE('',#39350,#39349,#7548,.T.);
#49894=EDGE_CURVE('',#39350,#39347,#7549,.T.);
#49895=EDGE_CURVE('',#39351,#39352,#7550,.T.);
#49896=EDGE_CURVE('',#39348,#39352,#7551,.T.);
#49897=EDGE_CURVE('',#39347,#39351,#7552,.T.);
#49898=EDGE_CURVE('',#39353,#39354,#7553,.T.);
#49899=EDGE_CURVE('',#39352,#39354,#7554,.T.);
#49900=EDGE_CURVE('',#39351,#39353,#7555,.T.);
#49901=EDGE_CURVE('',#39354,#39349,#7556,.T.);
#49902=EDGE_CURVE('',#39353,#39350,#7557,.T.);
#49903=EDGE_CURVE('',#39355,#39356,#7558,.T.);
#49904=EDGE_CURVE('',#39357,#39356,#7559,.T.);
#49905=EDGE_CURVE('',#39358,#39357,#7560,.T.);
#49906=EDGE_CURVE('',#39358,#39355,#7561,.T.);
#49907=EDGE_CURVE('',#39359,#39360,#7562,.T.);
#49908=EDGE_CURVE('',#39356,#39360,#7563,.T.);
#49909=EDGE_CURVE('',#39355,#39359,#7564,.T.);
#49910=EDGE_CURVE('',#39361,#39362,#7565,.T.);
#49911=EDGE_CURVE('',#39360,#39362,#7566,.T.);
#49912=EDGE_CURVE('',#39359,#39361,#7567,.T.);
#49913=EDGE_CURVE('',#39362,#39357,#7568,.T.);
#49914=EDGE_CURVE('',#39361,#39358,#7569,.T.);
#49915=EDGE_CURVE('',#39363,#39364,#7570,.T.);
#49916=EDGE_CURVE('',#39365,#39364,#7571,.T.);
#49917=EDGE_CURVE('',#39366,#39365,#7572,.T.);
#49918=EDGE_CURVE('',#39366,#39363,#7573,.T.);
#49919=EDGE_CURVE('',#39367,#39368,#7574,.T.);
#49920=EDGE_CURVE('',#39364,#39368,#7575,.T.);
#49921=EDGE_CURVE('',#39363,#39367,#7576,.T.);
#49922=EDGE_CURVE('',#39369,#39370,#7577,.T.);
#49923=EDGE_CURVE('',#39368,#39370,#7578,.T.);
#49924=EDGE_CURVE('',#39367,#39369,#7579,.T.);
#49925=EDGE_CURVE('',#39370,#39365,#7580,.T.);
#49926=EDGE_CURVE('',#39369,#39366,#7581,.T.);
#49927=EDGE_CURVE('',#39371,#39372,#7582,.T.);
#49928=EDGE_CURVE('',#39373,#39372,#7583,.T.);
#49929=EDGE_CURVE('',#39374,#39373,#7584,.T.);
#49930=EDGE_CURVE('',#39374,#39371,#7585,.T.);
#49931=EDGE_CURVE('',#39375,#39376,#7586,.T.);
#49932=EDGE_CURVE('',#39372,#39376,#7587,.T.);
#49933=EDGE_CURVE('',#39371,#39375,#7588,.T.);
#49934=EDGE_CURVE('',#39377,#39378,#7589,.T.);
#49935=EDGE_CURVE('',#39376,#39378,#7590,.T.);
#49936=EDGE_CURVE('',#39375,#39377,#7591,.T.);
#49937=EDGE_CURVE('',#39378,#39373,#7592,.T.);
#49938=EDGE_CURVE('',#39377,#39374,#7593,.T.);
#49939=EDGE_CURVE('',#39379,#39380,#7594,.T.);
#49940=EDGE_CURVE('',#39381,#39380,#7595,.T.);
#49941=EDGE_CURVE('',#39382,#39381,#7596,.T.);
#49942=EDGE_CURVE('',#39382,#39379,#7597,.T.);
#49943=EDGE_CURVE('',#39383,#39384,#7598,.T.);
#49944=EDGE_CURVE('',#39380,#39384,#7599,.T.);
#49945=EDGE_CURVE('',#39379,#39383,#7600,.T.);
#49946=EDGE_CURVE('',#39385,#39386,#7601,.T.);
#49947=EDGE_CURVE('',#39384,#39386,#7602,.T.);
#49948=EDGE_CURVE('',#39383,#39385,#7603,.T.);
#49949=EDGE_CURVE('',#39386,#39381,#7604,.T.);
#49950=EDGE_CURVE('',#39385,#39382,#7605,.T.);
#49951=EDGE_CURVE('',#39387,#39388,#7606,.T.);
#49952=EDGE_CURVE('',#39389,#39388,#7607,.T.);
#49953=EDGE_CURVE('',#39390,#39389,#7608,.T.);
#49954=EDGE_CURVE('',#39390,#39387,#7609,.T.);
#49955=EDGE_CURVE('',#39391,#39392,#7610,.T.);
#49956=EDGE_CURVE('',#39388,#39392,#7611,.T.);
#49957=EDGE_CURVE('',#39387,#39391,#7612,.T.);
#49958=EDGE_CURVE('',#39393,#39394,#7613,.T.);
#49959=EDGE_CURVE('',#39392,#39394,#7614,.T.);
#49960=EDGE_CURVE('',#39391,#39393,#7615,.T.);
#49961=EDGE_CURVE('',#39394,#39389,#7616,.T.);
#49962=EDGE_CURVE('',#39393,#39390,#7617,.T.);
#49963=EDGE_CURVE('',#39395,#39396,#7618,.T.);
#49964=EDGE_CURVE('',#39397,#39396,#7619,.T.);
#49965=EDGE_CURVE('',#39398,#39397,#7620,.T.);
#49966=EDGE_CURVE('',#39398,#39395,#7621,.T.);
#49967=EDGE_CURVE('',#39399,#39400,#7622,.T.);
#49968=EDGE_CURVE('',#39396,#39400,#7623,.T.);
#49969=EDGE_CURVE('',#39395,#39399,#7624,.T.);
#49970=EDGE_CURVE('',#39401,#39402,#7625,.T.);
#49971=EDGE_CURVE('',#39400,#39402,#7626,.T.);
#49972=EDGE_CURVE('',#39399,#39401,#7627,.T.);
#49973=EDGE_CURVE('',#39402,#39397,#7628,.T.);
#49974=EDGE_CURVE('',#39401,#39398,#7629,.T.);
#49975=EDGE_CURVE('',#39403,#39404,#7630,.T.);
#49976=EDGE_CURVE('',#39405,#39404,#7631,.T.);
#49977=EDGE_CURVE('',#39406,#39405,#7632,.T.);
#49978=EDGE_CURVE('',#39406,#39403,#7633,.T.);
#49979=EDGE_CURVE('',#39407,#39408,#7634,.T.);
#49980=EDGE_CURVE('',#39404,#39408,#7635,.T.);
#49981=EDGE_CURVE('',#39403,#39407,#7636,.T.);
#49982=EDGE_CURVE('',#39409,#39410,#7637,.T.);
#49983=EDGE_CURVE('',#39408,#39410,#7638,.T.);
#49984=EDGE_CURVE('',#39407,#39409,#7639,.T.);
#49985=EDGE_CURVE('',#39410,#39405,#7640,.T.);
#49986=EDGE_CURVE('',#39409,#39406,#7641,.T.);
#49987=EDGE_CURVE('',#39411,#39412,#7642,.T.);
#49988=EDGE_CURVE('',#39413,#39412,#7643,.T.);
#49989=EDGE_CURVE('',#39414,#39413,#7644,.T.);
#49990=EDGE_CURVE('',#39414,#39411,#7645,.T.);
#49991=EDGE_CURVE('',#39415,#39416,#7646,.T.);
#49992=EDGE_CURVE('',#39412,#39416,#7647,.T.);
#49993=EDGE_CURVE('',#39411,#39415,#7648,.T.);
#49994=EDGE_CURVE('',#39417,#39418,#7649,.T.);
#49995=EDGE_CURVE('',#39416,#39418,#7650,.T.);
#49996=EDGE_CURVE('',#39415,#39417,#7651,.T.);
#49997=EDGE_CURVE('',#39418,#39413,#7652,.T.);
#49998=EDGE_CURVE('',#39417,#39414,#7653,.T.);
#49999=EDGE_CURVE('',#39419,#39420,#7654,.T.);
#50000=EDGE_CURVE('',#39421,#39420,#7655,.T.);
#50001=EDGE_CURVE('',#39422,#39421,#7656,.T.);
#50002=EDGE_CURVE('',#39422,#39419,#7657,.T.);
#50003=EDGE_CURVE('',#39423,#39424,#7658,.T.);
#50004=EDGE_CURVE('',#39420,#39424,#7659,.T.);
#50005=EDGE_CURVE('',#39419,#39423,#7660,.T.);
#50006=EDGE_CURVE('',#39425,#39426,#7661,.T.);
#50007=EDGE_CURVE('',#39424,#39426,#7662,.T.);
#50008=EDGE_CURVE('',#39423,#39425,#7663,.T.);
#50009=EDGE_CURVE('',#39426,#39421,#7664,.T.);
#50010=EDGE_CURVE('',#39425,#39422,#7665,.T.);
#50011=EDGE_CURVE('',#39427,#39428,#7666,.T.);
#50012=EDGE_CURVE('',#39429,#39428,#7667,.T.);
#50013=EDGE_CURVE('',#39430,#39429,#7668,.T.);
#50014=EDGE_CURVE('',#39430,#39427,#7669,.T.);
#50015=EDGE_CURVE('',#39431,#39432,#7670,.T.);
#50016=EDGE_CURVE('',#39428,#39432,#7671,.T.);
#50017=EDGE_CURVE('',#39427,#39431,#7672,.T.);
#50018=EDGE_CURVE('',#39433,#39434,#7673,.T.);
#50019=EDGE_CURVE('',#39432,#39434,#7674,.T.);
#50020=EDGE_CURVE('',#39431,#39433,#7675,.T.);
#50021=EDGE_CURVE('',#39434,#39429,#7676,.T.);
#50022=EDGE_CURVE('',#39433,#39430,#7677,.T.);
#50023=EDGE_CURVE('',#39435,#39436,#7678,.T.);
#50024=EDGE_CURVE('',#39437,#39436,#7679,.T.);
#50025=EDGE_CURVE('',#39438,#39437,#7680,.T.);
#50026=EDGE_CURVE('',#39438,#39435,#7681,.T.);
#50027=EDGE_CURVE('',#39439,#39440,#7682,.T.);
#50028=EDGE_CURVE('',#39436,#39440,#7683,.T.);
#50029=EDGE_CURVE('',#39435,#39439,#7684,.T.);
#50030=EDGE_CURVE('',#39441,#39442,#7685,.T.);
#50031=EDGE_CURVE('',#39440,#39442,#7686,.T.);
#50032=EDGE_CURVE('',#39439,#39441,#7687,.T.);
#50033=EDGE_CURVE('',#39442,#39437,#7688,.T.);
#50034=EDGE_CURVE('',#39441,#39438,#7689,.T.);
#50035=EDGE_CURVE('',#39443,#39444,#7690,.T.);
#50036=EDGE_CURVE('',#39445,#39444,#7691,.T.);
#50037=EDGE_CURVE('',#39446,#39445,#7692,.T.);
#50038=EDGE_CURVE('',#39446,#39443,#7693,.T.);
#50039=EDGE_CURVE('',#39447,#39448,#7694,.T.);
#50040=EDGE_CURVE('',#39444,#39448,#7695,.T.);
#50041=EDGE_CURVE('',#39443,#39447,#7696,.T.);
#50042=EDGE_CURVE('',#39449,#39450,#7697,.T.);
#50043=EDGE_CURVE('',#39448,#39450,#7698,.T.);
#50044=EDGE_CURVE('',#39447,#39449,#7699,.T.);
#50045=EDGE_CURVE('',#39450,#39445,#7700,.T.);
#50046=EDGE_CURVE('',#39449,#39446,#7701,.T.);
#50047=EDGE_CURVE('',#39451,#39452,#7702,.T.);
#50048=EDGE_CURVE('',#39453,#39452,#7703,.T.);
#50049=EDGE_CURVE('',#39454,#39453,#7704,.T.);
#50050=EDGE_CURVE('',#39454,#39451,#7705,.T.);
#50051=EDGE_CURVE('',#39455,#39456,#7706,.T.);
#50052=EDGE_CURVE('',#39452,#39456,#7707,.T.);
#50053=EDGE_CURVE('',#39451,#39455,#7708,.T.);
#50054=EDGE_CURVE('',#39457,#39458,#7709,.T.);
#50055=EDGE_CURVE('',#39456,#39458,#7710,.T.);
#50056=EDGE_CURVE('',#39455,#39457,#7711,.T.);
#50057=EDGE_CURVE('',#39458,#39453,#7712,.T.);
#50058=EDGE_CURVE('',#39457,#39454,#7713,.T.);
#50059=EDGE_CURVE('',#39459,#39460,#7714,.T.);
#50060=EDGE_CURVE('',#39461,#39460,#7715,.T.);
#50061=EDGE_CURVE('',#39462,#39461,#7716,.T.);
#50062=EDGE_CURVE('',#39462,#39459,#7717,.T.);
#50063=EDGE_CURVE('',#39463,#39464,#7718,.T.);
#50064=EDGE_CURVE('',#39460,#39464,#7719,.T.);
#50065=EDGE_CURVE('',#39459,#39463,#7720,.T.);
#50066=EDGE_CURVE('',#39465,#39466,#7721,.T.);
#50067=EDGE_CURVE('',#39464,#39466,#7722,.T.);
#50068=EDGE_CURVE('',#39463,#39465,#7723,.T.);
#50069=EDGE_CURVE('',#39466,#39461,#7724,.T.);
#50070=EDGE_CURVE('',#39465,#39462,#7725,.T.);
#50071=EDGE_CURVE('',#39467,#39468,#7726,.T.);
#50072=EDGE_CURVE('',#39469,#39468,#7727,.T.);
#50073=EDGE_CURVE('',#39470,#39469,#7728,.T.);
#50074=EDGE_CURVE('',#39470,#39467,#7729,.T.);
#50075=EDGE_CURVE('',#39471,#39472,#7730,.T.);
#50076=EDGE_CURVE('',#39468,#39472,#7731,.T.);
#50077=EDGE_CURVE('',#39467,#39471,#7732,.T.);
#50078=EDGE_CURVE('',#39473,#39474,#7733,.T.);
#50079=EDGE_CURVE('',#39472,#39474,#7734,.T.);
#50080=EDGE_CURVE('',#39471,#39473,#7735,.T.);
#50081=EDGE_CURVE('',#39474,#39469,#7736,.T.);
#50082=EDGE_CURVE('',#39473,#39470,#7737,.T.);
#50083=EDGE_CURVE('',#39475,#39476,#7738,.T.);
#50084=EDGE_CURVE('',#39477,#39476,#7739,.T.);
#50085=EDGE_CURVE('',#39478,#39477,#7740,.T.);
#50086=EDGE_CURVE('',#39478,#39475,#7741,.T.);
#50087=EDGE_CURVE('',#39479,#39480,#7742,.T.);
#50088=EDGE_CURVE('',#39476,#39480,#7743,.T.);
#50089=EDGE_CURVE('',#39475,#39479,#7744,.T.);
#50090=EDGE_CURVE('',#39481,#39482,#7745,.T.);
#50091=EDGE_CURVE('',#39480,#39482,#7746,.T.);
#50092=EDGE_CURVE('',#39479,#39481,#7747,.T.);
#50093=EDGE_CURVE('',#39482,#39477,#7748,.T.);
#50094=EDGE_CURVE('',#39481,#39478,#7749,.T.);
#50095=EDGE_CURVE('',#39483,#39484,#7750,.T.);
#50096=EDGE_CURVE('',#39485,#39484,#7751,.T.);
#50097=EDGE_CURVE('',#39486,#39485,#7752,.T.);
#50098=EDGE_CURVE('',#39486,#39483,#7753,.T.);
#50099=EDGE_CURVE('',#39487,#39488,#7754,.T.);
#50100=EDGE_CURVE('',#39484,#39488,#7755,.T.);
#50101=EDGE_CURVE('',#39483,#39487,#7756,.T.);
#50102=EDGE_CURVE('',#39489,#39490,#7757,.T.);
#50103=EDGE_CURVE('',#39488,#39490,#7758,.T.);
#50104=EDGE_CURVE('',#39487,#39489,#7759,.T.);
#50105=EDGE_CURVE('',#39490,#39485,#7760,.T.);
#50106=EDGE_CURVE('',#39489,#39486,#7761,.T.);
#50107=EDGE_CURVE('',#39491,#39492,#7762,.T.);
#50108=EDGE_CURVE('',#39493,#39492,#7763,.T.);
#50109=EDGE_CURVE('',#39494,#39493,#7764,.T.);
#50110=EDGE_CURVE('',#39494,#39491,#7765,.T.);
#50111=EDGE_CURVE('',#39495,#39496,#7766,.T.);
#50112=EDGE_CURVE('',#39492,#39496,#7767,.T.);
#50113=EDGE_CURVE('',#39491,#39495,#7768,.T.);
#50114=EDGE_CURVE('',#39497,#39498,#7769,.T.);
#50115=EDGE_CURVE('',#39496,#39498,#7770,.T.);
#50116=EDGE_CURVE('',#39495,#39497,#7771,.T.);
#50117=EDGE_CURVE('',#39498,#39493,#7772,.T.);
#50118=EDGE_CURVE('',#39497,#39494,#7773,.T.);
#50119=EDGE_CURVE('',#39499,#39500,#7774,.T.);
#50120=EDGE_CURVE('',#39501,#39500,#7775,.T.);
#50121=EDGE_CURVE('',#39502,#39501,#7776,.T.);
#50122=EDGE_CURVE('',#39502,#39499,#7777,.T.);
#50123=EDGE_CURVE('',#39503,#39504,#7778,.T.);
#50124=EDGE_CURVE('',#39500,#39504,#7779,.T.);
#50125=EDGE_CURVE('',#39499,#39503,#7780,.T.);
#50126=EDGE_CURVE('',#39505,#39506,#7781,.T.);
#50127=EDGE_CURVE('',#39504,#39506,#7782,.T.);
#50128=EDGE_CURVE('',#39503,#39505,#7783,.T.);
#50129=EDGE_CURVE('',#39506,#39501,#7784,.T.);
#50130=EDGE_CURVE('',#39505,#39502,#7785,.T.);
#50131=EDGE_CURVE('',#39507,#39508,#7786,.T.);
#50132=EDGE_CURVE('',#39509,#39508,#7787,.T.);
#50133=EDGE_CURVE('',#39510,#39509,#7788,.T.);
#50134=EDGE_CURVE('',#39510,#39507,#7789,.T.);
#50135=EDGE_CURVE('',#39511,#39512,#7790,.T.);
#50136=EDGE_CURVE('',#39508,#39512,#7791,.T.);
#50137=EDGE_CURVE('',#39507,#39511,#7792,.T.);
#50138=EDGE_CURVE('',#39513,#39514,#7793,.T.);
#50139=EDGE_CURVE('',#39512,#39514,#7794,.T.);
#50140=EDGE_CURVE('',#39511,#39513,#7795,.T.);
#50141=EDGE_CURVE('',#39514,#39509,#7796,.T.);
#50142=EDGE_CURVE('',#39513,#39510,#7797,.T.);
#50143=EDGE_CURVE('',#39515,#39516,#7798,.T.);
#50144=EDGE_CURVE('',#39517,#39516,#7799,.T.);
#50145=EDGE_CURVE('',#39518,#39517,#7800,.T.);
#50146=EDGE_CURVE('',#39518,#39515,#7801,.T.);
#50147=EDGE_CURVE('',#39519,#39520,#7802,.T.);
#50148=EDGE_CURVE('',#39516,#39520,#7803,.T.);
#50149=EDGE_CURVE('',#39515,#39519,#7804,.T.);
#50150=EDGE_CURVE('',#39521,#39522,#7805,.T.);
#50151=EDGE_CURVE('',#39520,#39522,#7806,.T.);
#50152=EDGE_CURVE('',#39519,#39521,#7807,.T.);
#50153=EDGE_CURVE('',#39522,#39517,#7808,.T.);
#50154=EDGE_CURVE('',#39521,#39518,#7809,.T.);
#50155=EDGE_CURVE('',#39523,#39524,#7810,.T.);
#50156=EDGE_CURVE('',#39525,#39524,#7811,.T.);
#50157=EDGE_CURVE('',#39526,#39525,#7812,.T.);
#50158=EDGE_CURVE('',#39526,#39523,#7813,.T.);
#50159=EDGE_CURVE('',#39527,#39528,#7814,.T.);
#50160=EDGE_CURVE('',#39524,#39528,#7815,.T.);
#50161=EDGE_CURVE('',#39523,#39527,#7816,.T.);
#50162=EDGE_CURVE('',#39529,#39530,#7817,.T.);
#50163=EDGE_CURVE('',#39528,#39530,#7818,.T.);
#50164=EDGE_CURVE('',#39527,#39529,#7819,.T.);
#50165=EDGE_CURVE('',#39530,#39525,#7820,.T.);
#50166=EDGE_CURVE('',#39529,#39526,#7821,.T.);
#50167=EDGE_CURVE('',#39531,#39532,#7822,.T.);
#50168=EDGE_CURVE('',#39533,#39532,#7823,.T.);
#50169=EDGE_CURVE('',#39534,#39533,#7824,.T.);
#50170=EDGE_CURVE('',#39534,#39531,#7825,.T.);
#50171=EDGE_CURVE('',#39535,#39536,#7826,.T.);
#50172=EDGE_CURVE('',#39532,#39536,#7827,.T.);
#50173=EDGE_CURVE('',#39531,#39535,#7828,.T.);
#50174=EDGE_CURVE('',#39537,#39538,#7829,.T.);
#50175=EDGE_CURVE('',#39536,#39538,#7830,.T.);
#50176=EDGE_CURVE('',#39535,#39537,#7831,.T.);
#50177=EDGE_CURVE('',#39538,#39533,#7832,.T.);
#50178=EDGE_CURVE('',#39537,#39534,#7833,.T.);
#50179=EDGE_CURVE('',#39539,#39540,#7834,.T.);
#50180=EDGE_CURVE('',#39541,#39540,#7835,.T.);
#50181=EDGE_CURVE('',#39542,#39541,#7836,.T.);
#50182=EDGE_CURVE('',#39542,#39539,#7837,.T.);
#50183=EDGE_CURVE('',#39543,#39544,#7838,.T.);
#50184=EDGE_CURVE('',#39540,#39544,#7839,.T.);
#50185=EDGE_CURVE('',#39539,#39543,#7840,.T.);
#50186=EDGE_CURVE('',#39545,#39546,#7841,.T.);
#50187=EDGE_CURVE('',#39544,#39546,#7842,.T.);
#50188=EDGE_CURVE('',#39543,#39545,#7843,.T.);
#50189=EDGE_CURVE('',#39546,#39541,#7844,.T.);
#50190=EDGE_CURVE('',#39545,#39542,#7845,.T.);
#50191=EDGE_CURVE('',#39547,#39548,#7846,.T.);
#50192=EDGE_CURVE('',#39549,#39548,#7847,.T.);
#50193=EDGE_CURVE('',#39550,#39549,#7848,.T.);
#50194=EDGE_CURVE('',#39550,#39547,#7849,.T.);
#50195=EDGE_CURVE('',#39551,#39552,#7850,.T.);
#50196=EDGE_CURVE('',#39548,#39552,#7851,.T.);
#50197=EDGE_CURVE('',#39547,#39551,#7852,.T.);
#50198=EDGE_CURVE('',#39553,#39554,#7853,.T.);
#50199=EDGE_CURVE('',#39552,#39554,#7854,.T.);
#50200=EDGE_CURVE('',#39551,#39553,#7855,.T.);
#50201=EDGE_CURVE('',#39554,#39549,#7856,.T.);
#50202=EDGE_CURVE('',#39553,#39550,#7857,.T.);
#50203=EDGE_CURVE('',#39555,#39556,#7858,.T.);
#50204=EDGE_CURVE('',#39557,#39556,#7859,.T.);
#50205=EDGE_CURVE('',#39558,#39557,#7860,.T.);
#50206=EDGE_CURVE('',#39558,#39555,#7861,.T.);
#50207=EDGE_CURVE('',#39559,#39560,#7862,.T.);
#50208=EDGE_CURVE('',#39556,#39560,#7863,.T.);
#50209=EDGE_CURVE('',#39555,#39559,#7864,.T.);
#50210=EDGE_CURVE('',#39561,#39562,#7865,.T.);
#50211=EDGE_CURVE('',#39560,#39562,#7866,.T.);
#50212=EDGE_CURVE('',#39559,#39561,#7867,.T.);
#50213=EDGE_CURVE('',#39562,#39557,#7868,.T.);
#50214=EDGE_CURVE('',#39561,#39558,#7869,.T.);
#50215=EDGE_CURVE('',#39563,#39564,#7870,.T.);
#50216=EDGE_CURVE('',#39565,#39564,#7871,.T.);
#50217=EDGE_CURVE('',#39566,#39565,#7872,.T.);
#50218=EDGE_CURVE('',#39566,#39563,#7873,.T.);
#50219=EDGE_CURVE('',#39567,#39568,#7874,.T.);
#50220=EDGE_CURVE('',#39564,#39568,#7875,.T.);
#50221=EDGE_CURVE('',#39563,#39567,#7876,.T.);
#50222=EDGE_CURVE('',#39569,#39570,#7877,.T.);
#50223=EDGE_CURVE('',#39568,#39570,#7878,.T.);
#50224=EDGE_CURVE('',#39567,#39569,#7879,.T.);
#50225=EDGE_CURVE('',#39570,#39565,#7880,.T.);
#50226=EDGE_CURVE('',#39569,#39566,#7881,.T.);
#50227=EDGE_CURVE('',#39571,#39572,#7882,.T.);
#50228=EDGE_CURVE('',#39573,#39572,#7883,.T.);
#50229=EDGE_CURVE('',#39574,#39573,#7884,.T.);
#50230=EDGE_CURVE('',#39574,#39571,#7885,.T.);
#50231=EDGE_CURVE('',#39575,#39576,#7886,.T.);
#50232=EDGE_CURVE('',#39572,#39576,#7887,.T.);
#50233=EDGE_CURVE('',#39571,#39575,#7888,.T.);
#50234=EDGE_CURVE('',#39577,#39578,#7889,.T.);
#50235=EDGE_CURVE('',#39576,#39578,#7890,.T.);
#50236=EDGE_CURVE('',#39575,#39577,#7891,.T.);
#50237=EDGE_CURVE('',#39578,#39573,#7892,.T.);
#50238=EDGE_CURVE('',#39577,#39574,#7893,.T.);
#50239=EDGE_CURVE('',#39579,#39580,#7894,.T.);
#50240=EDGE_CURVE('',#39581,#39580,#7895,.T.);
#50241=EDGE_CURVE('',#39582,#39581,#7896,.T.);
#50242=EDGE_CURVE('',#39582,#39579,#7897,.T.);
#50243=EDGE_CURVE('',#39583,#39584,#7898,.T.);
#50244=EDGE_CURVE('',#39580,#39584,#7899,.T.);
#50245=EDGE_CURVE('',#39579,#39583,#7900,.T.);
#50246=EDGE_CURVE('',#39585,#39586,#7901,.T.);
#50247=EDGE_CURVE('',#39584,#39586,#7902,.T.);
#50248=EDGE_CURVE('',#39583,#39585,#7903,.T.);
#50249=EDGE_CURVE('',#39586,#39581,#7904,.T.);
#50250=EDGE_CURVE('',#39585,#39582,#7905,.T.);
#50251=EDGE_CURVE('',#39587,#39588,#7906,.T.);
#50252=EDGE_CURVE('',#39589,#39588,#7907,.T.);
#50253=EDGE_CURVE('',#39590,#39589,#7908,.T.);
#50254=EDGE_CURVE('',#39590,#39587,#7909,.T.);
#50255=EDGE_CURVE('',#39591,#39592,#7910,.T.);
#50256=EDGE_CURVE('',#39588,#39592,#7911,.T.);
#50257=EDGE_CURVE('',#39587,#39591,#7912,.T.);
#50258=EDGE_CURVE('',#39593,#39594,#7913,.T.);
#50259=EDGE_CURVE('',#39592,#39594,#7914,.T.);
#50260=EDGE_CURVE('',#39591,#39593,#7915,.T.);
#50261=EDGE_CURVE('',#39594,#39589,#7916,.T.);
#50262=EDGE_CURVE('',#39593,#39590,#7917,.T.);
#50263=EDGE_CURVE('',#39595,#39596,#7918,.T.);
#50264=EDGE_CURVE('',#39597,#39596,#7919,.T.);
#50265=EDGE_CURVE('',#39598,#39597,#7920,.T.);
#50266=EDGE_CURVE('',#39598,#39595,#7921,.T.);
#50267=EDGE_CURVE('',#39599,#39600,#7922,.T.);
#50268=EDGE_CURVE('',#39596,#39600,#7923,.T.);
#50269=EDGE_CURVE('',#39595,#39599,#7924,.T.);
#50270=EDGE_CURVE('',#39601,#39602,#7925,.T.);
#50271=EDGE_CURVE('',#39600,#39602,#7926,.T.);
#50272=EDGE_CURVE('',#39599,#39601,#7927,.T.);
#50273=EDGE_CURVE('',#39602,#39597,#7928,.T.);
#50274=EDGE_CURVE('',#39601,#39598,#7929,.T.);
#50275=EDGE_CURVE('',#39603,#39604,#7930,.T.);
#50276=EDGE_CURVE('',#39605,#39604,#7931,.T.);
#50277=EDGE_CURVE('',#39606,#39605,#7932,.T.);
#50278=EDGE_CURVE('',#39606,#39603,#7933,.T.);
#50279=EDGE_CURVE('',#39607,#39608,#7934,.T.);
#50280=EDGE_CURVE('',#39604,#39608,#7935,.T.);
#50281=EDGE_CURVE('',#39603,#39607,#7936,.T.);
#50282=EDGE_CURVE('',#39609,#39610,#7937,.T.);
#50283=EDGE_CURVE('',#39608,#39610,#7938,.T.);
#50284=EDGE_CURVE('',#39607,#39609,#7939,.T.);
#50285=EDGE_CURVE('',#39610,#39605,#7940,.T.);
#50286=EDGE_CURVE('',#39609,#39606,#7941,.T.);
#50287=EDGE_CURVE('',#39611,#39612,#7942,.T.);
#50288=EDGE_CURVE('',#39613,#39612,#7943,.T.);
#50289=EDGE_CURVE('',#39614,#39613,#7944,.T.);
#50290=EDGE_CURVE('',#39614,#39611,#7945,.T.);
#50291=EDGE_CURVE('',#39615,#39616,#7946,.T.);
#50292=EDGE_CURVE('',#39612,#39616,#7947,.T.);
#50293=EDGE_CURVE('',#39611,#39615,#7948,.T.);
#50294=EDGE_CURVE('',#39617,#39618,#7949,.T.);
#50295=EDGE_CURVE('',#39616,#39618,#7950,.T.);
#50296=EDGE_CURVE('',#39615,#39617,#7951,.T.);
#50297=EDGE_CURVE('',#39618,#39613,#7952,.T.);
#50298=EDGE_CURVE('',#39617,#39614,#7953,.T.);
#50299=EDGE_CURVE('',#39619,#39620,#7954,.T.);
#50300=EDGE_CURVE('',#39621,#39620,#7955,.T.);
#50301=EDGE_CURVE('',#39622,#39621,#7956,.T.);
#50302=EDGE_CURVE('',#39622,#39619,#7957,.T.);
#50303=EDGE_CURVE('',#39623,#39624,#7958,.T.);
#50304=EDGE_CURVE('',#39620,#39624,#7959,.T.);
#50305=EDGE_CURVE('',#39619,#39623,#7960,.T.);
#50306=EDGE_CURVE('',#39625,#39626,#7961,.T.);
#50307=EDGE_CURVE('',#39624,#39626,#7962,.T.);
#50308=EDGE_CURVE('',#39623,#39625,#7963,.T.);
#50309=EDGE_CURVE('',#39626,#39621,#7964,.T.);
#50310=EDGE_CURVE('',#39625,#39622,#7965,.T.);
#50311=EDGE_CURVE('',#39627,#39628,#7966,.T.);
#50312=EDGE_CURVE('',#39629,#39628,#7967,.T.);
#50313=EDGE_CURVE('',#39630,#39629,#7968,.T.);
#50314=EDGE_CURVE('',#39630,#39627,#7969,.T.);
#50315=EDGE_CURVE('',#39631,#39632,#7970,.T.);
#50316=EDGE_CURVE('',#39628,#39632,#7971,.T.);
#50317=EDGE_CURVE('',#39627,#39631,#7972,.T.);
#50318=EDGE_CURVE('',#39633,#39634,#7973,.T.);
#50319=EDGE_CURVE('',#39632,#39634,#7974,.T.);
#50320=EDGE_CURVE('',#39631,#39633,#7975,.T.);
#50321=EDGE_CURVE('',#39634,#39629,#7976,.T.);
#50322=EDGE_CURVE('',#39633,#39630,#7977,.T.);
#50323=EDGE_CURVE('',#39635,#39636,#7978,.T.);
#50324=EDGE_CURVE('',#39637,#39636,#7979,.T.);
#50325=EDGE_CURVE('',#39638,#39637,#7980,.T.);
#50326=EDGE_CURVE('',#39638,#39635,#7981,.T.);
#50327=EDGE_CURVE('',#39639,#39640,#7982,.T.);
#50328=EDGE_CURVE('',#39636,#39640,#7983,.T.);
#50329=EDGE_CURVE('',#39635,#39639,#7984,.T.);
#50330=EDGE_CURVE('',#39641,#39642,#7985,.T.);
#50331=EDGE_CURVE('',#39640,#39642,#7986,.T.);
#50332=EDGE_CURVE('',#39639,#39641,#7987,.T.);
#50333=EDGE_CURVE('',#39642,#39637,#7988,.T.);
#50334=EDGE_CURVE('',#39641,#39638,#7989,.T.);
#50335=EDGE_CURVE('',#39643,#39644,#7990,.T.);
#50336=EDGE_CURVE('',#39645,#39644,#7991,.T.);
#50337=EDGE_CURVE('',#39646,#39645,#7992,.T.);
#50338=EDGE_CURVE('',#39646,#39643,#7993,.T.);
#50339=EDGE_CURVE('',#39647,#39648,#7994,.T.);
#50340=EDGE_CURVE('',#39644,#39648,#7995,.T.);
#50341=EDGE_CURVE('',#39643,#39647,#7996,.T.);
#50342=EDGE_CURVE('',#39649,#39650,#7997,.T.);
#50343=EDGE_CURVE('',#39648,#39650,#7998,.T.);
#50344=EDGE_CURVE('',#39647,#39649,#7999,.T.);
#50345=EDGE_CURVE('',#39650,#39645,#8000,.T.);
#50346=EDGE_CURVE('',#39649,#39646,#8001,.T.);
#50347=EDGE_CURVE('',#39651,#39652,#8002,.T.);
#50348=EDGE_CURVE('',#39653,#39652,#8003,.T.);
#50349=EDGE_CURVE('',#39654,#39653,#8004,.T.);
#50350=EDGE_CURVE('',#39654,#39651,#8005,.T.);
#50351=EDGE_CURVE('',#39655,#39656,#8006,.T.);
#50352=EDGE_CURVE('',#39652,#39656,#8007,.T.);
#50353=EDGE_CURVE('',#39651,#39655,#8008,.T.);
#50354=EDGE_CURVE('',#39657,#39658,#8009,.T.);
#50355=EDGE_CURVE('',#39656,#39658,#8010,.T.);
#50356=EDGE_CURVE('',#39655,#39657,#8011,.T.);
#50357=EDGE_CURVE('',#39658,#39653,#8012,.T.);
#50358=EDGE_CURVE('',#39657,#39654,#8013,.T.);
#50359=EDGE_CURVE('',#39659,#39660,#8014,.T.);
#50360=EDGE_CURVE('',#39661,#39660,#8015,.T.);
#50361=EDGE_CURVE('',#39662,#39661,#8016,.T.);
#50362=EDGE_CURVE('',#39662,#39659,#8017,.T.);
#50363=EDGE_CURVE('',#39663,#39664,#8018,.T.);
#50364=EDGE_CURVE('',#39660,#39664,#8019,.T.);
#50365=EDGE_CURVE('',#39659,#39663,#8020,.T.);
#50366=EDGE_CURVE('',#39665,#39666,#8021,.T.);
#50367=EDGE_CURVE('',#39664,#39666,#8022,.T.);
#50368=EDGE_CURVE('',#39663,#39665,#8023,.T.);
#50369=EDGE_CURVE('',#39666,#39661,#8024,.T.);
#50370=EDGE_CURVE('',#39665,#39662,#8025,.T.);
#50371=EDGE_CURVE('',#39667,#39668,#8026,.T.);
#50372=EDGE_CURVE('',#39669,#39668,#8027,.T.);
#50373=EDGE_CURVE('',#39670,#39669,#8028,.T.);
#50374=EDGE_CURVE('',#39670,#39667,#8029,.T.);
#50375=EDGE_CURVE('',#39671,#39672,#8030,.T.);
#50376=EDGE_CURVE('',#39668,#39672,#8031,.T.);
#50377=EDGE_CURVE('',#39667,#39671,#8032,.T.);
#50378=EDGE_CURVE('',#39673,#39674,#8033,.T.);
#50379=EDGE_CURVE('',#39672,#39674,#8034,.T.);
#50380=EDGE_CURVE('',#39671,#39673,#8035,.T.);
#50381=EDGE_CURVE('',#39674,#39669,#8036,.T.);
#50382=EDGE_CURVE('',#39673,#39670,#8037,.T.);
#50383=EDGE_CURVE('',#39675,#39676,#8038,.T.);
#50384=EDGE_CURVE('',#39677,#39676,#8039,.T.);
#50385=EDGE_CURVE('',#39678,#39677,#8040,.T.);
#50386=EDGE_CURVE('',#39678,#39675,#8041,.T.);
#50387=EDGE_CURVE('',#39679,#39680,#8042,.T.);
#50388=EDGE_CURVE('',#39676,#39680,#8043,.T.);
#50389=EDGE_CURVE('',#39675,#39679,#8044,.T.);
#50390=EDGE_CURVE('',#39681,#39682,#8045,.T.);
#50391=EDGE_CURVE('',#39680,#39682,#8046,.T.);
#50392=EDGE_CURVE('',#39679,#39681,#8047,.T.);
#50393=EDGE_CURVE('',#39682,#39677,#8048,.T.);
#50394=EDGE_CURVE('',#39681,#39678,#8049,.T.);
#50395=EDGE_CURVE('',#39683,#39684,#8050,.T.);
#50396=EDGE_CURVE('',#39685,#39684,#8051,.T.);
#50397=EDGE_CURVE('',#39686,#39685,#8052,.T.);
#50398=EDGE_CURVE('',#39686,#39683,#8053,.T.);
#50399=EDGE_CURVE('',#39687,#39688,#8054,.T.);
#50400=EDGE_CURVE('',#39684,#39688,#8055,.T.);
#50401=EDGE_CURVE('',#39683,#39687,#8056,.T.);
#50402=EDGE_CURVE('',#39689,#39690,#8057,.T.);
#50403=EDGE_CURVE('',#39688,#39690,#8058,.T.);
#50404=EDGE_CURVE('',#39687,#39689,#8059,.T.);
#50405=EDGE_CURVE('',#39690,#39685,#8060,.T.);
#50406=EDGE_CURVE('',#39689,#39686,#8061,.T.);
#50407=EDGE_CURVE('',#39691,#39692,#8062,.T.);
#50408=EDGE_CURVE('',#39693,#39692,#8063,.T.);
#50409=EDGE_CURVE('',#39694,#39693,#8064,.T.);
#50410=EDGE_CURVE('',#39694,#39691,#8065,.T.);
#50411=EDGE_CURVE('',#39695,#39696,#8066,.T.);
#50412=EDGE_CURVE('',#39692,#39696,#8067,.T.);
#50413=EDGE_CURVE('',#39691,#39695,#8068,.T.);
#50414=EDGE_CURVE('',#39697,#39698,#8069,.T.);
#50415=EDGE_CURVE('',#39696,#39698,#8070,.T.);
#50416=EDGE_CURVE('',#39695,#39697,#8071,.T.);
#50417=EDGE_CURVE('',#39698,#39693,#8072,.T.);
#50418=EDGE_CURVE('',#39697,#39694,#8073,.T.);
#50419=EDGE_CURVE('',#39699,#39700,#8074,.T.);
#50420=EDGE_CURVE('',#39701,#39700,#8075,.T.);
#50421=EDGE_CURVE('',#39702,#39701,#8076,.T.);
#50422=EDGE_CURVE('',#39702,#39699,#8077,.T.);
#50423=EDGE_CURVE('',#39703,#39704,#8078,.T.);
#50424=EDGE_CURVE('',#39700,#39704,#8079,.T.);
#50425=EDGE_CURVE('',#39699,#39703,#8080,.T.);
#50426=EDGE_CURVE('',#39705,#39706,#8081,.T.);
#50427=EDGE_CURVE('',#39704,#39706,#8082,.T.);
#50428=EDGE_CURVE('',#39703,#39705,#8083,.T.);
#50429=EDGE_CURVE('',#39706,#39701,#8084,.T.);
#50430=EDGE_CURVE('',#39705,#39702,#8085,.T.);
#50431=EDGE_CURVE('',#39707,#39708,#8086,.T.);
#50432=EDGE_CURVE('',#39709,#39708,#8087,.T.);
#50433=EDGE_CURVE('',#39710,#39709,#8088,.T.);
#50434=EDGE_CURVE('',#39710,#39707,#8089,.T.);
#50435=EDGE_CURVE('',#39711,#39712,#8090,.T.);
#50436=EDGE_CURVE('',#39708,#39712,#8091,.T.);
#50437=EDGE_CURVE('',#39707,#39711,#8092,.T.);
#50438=EDGE_CURVE('',#39713,#39714,#8093,.T.);
#50439=EDGE_CURVE('',#39712,#39714,#8094,.T.);
#50440=EDGE_CURVE('',#39711,#39713,#8095,.T.);
#50441=EDGE_CURVE('',#39714,#39709,#8096,.T.);
#50442=EDGE_CURVE('',#39713,#39710,#8097,.T.);
#50443=EDGE_CURVE('',#39715,#39716,#8098,.T.);
#50444=EDGE_CURVE('',#39717,#39716,#8099,.T.);
#50445=EDGE_CURVE('',#39718,#39717,#8100,.T.);
#50446=EDGE_CURVE('',#39718,#39715,#8101,.T.);
#50447=EDGE_CURVE('',#39719,#39720,#8102,.T.);
#50448=EDGE_CURVE('',#39716,#39720,#8103,.T.);
#50449=EDGE_CURVE('',#39715,#39719,#8104,.T.);
#50450=EDGE_CURVE('',#39721,#39722,#8105,.T.);
#50451=EDGE_CURVE('',#39720,#39722,#8106,.T.);
#50452=EDGE_CURVE('',#39719,#39721,#8107,.T.);
#50453=EDGE_CURVE('',#39722,#39717,#8108,.T.);
#50454=EDGE_CURVE('',#39721,#39718,#8109,.T.);
#50455=EDGE_CURVE('',#39723,#39724,#8110,.T.);
#50456=EDGE_CURVE('',#39725,#39724,#8111,.T.);
#50457=EDGE_CURVE('',#39726,#39725,#8112,.T.);
#50458=EDGE_CURVE('',#39726,#39723,#8113,.T.);
#50459=EDGE_CURVE('',#39727,#39728,#8114,.T.);
#50460=EDGE_CURVE('',#39724,#39728,#8115,.T.);
#50461=EDGE_CURVE('',#39723,#39727,#8116,.T.);
#50462=EDGE_CURVE('',#39729,#39730,#8117,.T.);
#50463=EDGE_CURVE('',#39728,#39730,#8118,.T.);
#50464=EDGE_CURVE('',#39727,#39729,#8119,.T.);
#50465=EDGE_CURVE('',#39730,#39725,#8120,.T.);
#50466=EDGE_CURVE('',#39729,#39726,#8121,.T.);
#50467=EDGE_CURVE('',#39731,#39732,#8122,.T.);
#50468=EDGE_CURVE('',#39733,#39732,#8123,.T.);
#50469=EDGE_CURVE('',#39734,#39733,#8124,.T.);
#50470=EDGE_CURVE('',#39734,#39731,#8125,.T.);
#50471=EDGE_CURVE('',#39735,#39736,#8126,.T.);
#50472=EDGE_CURVE('',#39732,#39736,#8127,.T.);
#50473=EDGE_CURVE('',#39731,#39735,#8128,.T.);
#50474=EDGE_CURVE('',#39737,#39738,#8129,.T.);
#50475=EDGE_CURVE('',#39736,#39738,#8130,.T.);
#50476=EDGE_CURVE('',#39735,#39737,#8131,.T.);
#50477=EDGE_CURVE('',#39738,#39733,#8132,.T.);
#50478=EDGE_CURVE('',#39737,#39734,#8133,.T.);
#50479=EDGE_CURVE('',#39739,#39740,#8134,.T.);
#50480=EDGE_CURVE('',#39741,#39740,#8135,.T.);
#50481=EDGE_CURVE('',#39742,#39741,#8136,.T.);
#50482=EDGE_CURVE('',#39742,#39739,#8137,.T.);
#50483=EDGE_CURVE('',#39743,#39744,#8138,.T.);
#50484=EDGE_CURVE('',#39740,#39744,#8139,.T.);
#50485=EDGE_CURVE('',#39739,#39743,#8140,.T.);
#50486=EDGE_CURVE('',#39745,#39746,#8141,.T.);
#50487=EDGE_CURVE('',#39744,#39746,#8142,.T.);
#50488=EDGE_CURVE('',#39743,#39745,#8143,.T.);
#50489=EDGE_CURVE('',#39746,#39741,#8144,.T.);
#50490=EDGE_CURVE('',#39745,#39742,#8145,.T.);
#50491=EDGE_CURVE('',#39747,#39748,#8146,.T.);
#50492=EDGE_CURVE('',#39749,#39748,#8147,.T.);
#50493=EDGE_CURVE('',#39750,#39749,#8148,.T.);
#50494=EDGE_CURVE('',#39750,#39747,#8149,.T.);
#50495=EDGE_CURVE('',#39751,#39752,#8150,.T.);
#50496=EDGE_CURVE('',#39748,#39752,#8151,.T.);
#50497=EDGE_CURVE('',#39747,#39751,#8152,.T.);
#50498=EDGE_CURVE('',#39753,#39754,#8153,.T.);
#50499=EDGE_CURVE('',#39752,#39754,#8154,.T.);
#50500=EDGE_CURVE('',#39751,#39753,#8155,.T.);
#50501=EDGE_CURVE('',#39754,#39749,#8156,.T.);
#50502=EDGE_CURVE('',#39753,#39750,#8157,.T.);
#50503=EDGE_CURVE('',#39755,#39756,#8158,.T.);
#50504=EDGE_CURVE('',#39757,#39756,#8159,.T.);
#50505=EDGE_CURVE('',#39758,#39757,#8160,.T.);
#50506=EDGE_CURVE('',#39758,#39755,#8161,.T.);
#50507=EDGE_CURVE('',#39759,#39760,#8162,.T.);
#50508=EDGE_CURVE('',#39756,#39760,#8163,.T.);
#50509=EDGE_CURVE('',#39755,#39759,#8164,.T.);
#50510=EDGE_CURVE('',#39761,#39762,#8165,.T.);
#50511=EDGE_CURVE('',#39760,#39762,#8166,.T.);
#50512=EDGE_CURVE('',#39759,#39761,#8167,.T.);
#50513=EDGE_CURVE('',#39762,#39757,#8168,.T.);
#50514=EDGE_CURVE('',#39761,#39758,#8169,.T.);
#50515=EDGE_CURVE('',#39763,#39764,#8170,.T.);
#50516=EDGE_CURVE('',#39765,#39764,#8171,.T.);
#50517=EDGE_CURVE('',#39766,#39765,#8172,.T.);
#50518=EDGE_CURVE('',#39766,#39763,#8173,.T.);
#50519=EDGE_CURVE('',#39767,#39768,#8174,.T.);
#50520=EDGE_CURVE('',#39764,#39768,#8175,.T.);
#50521=EDGE_CURVE('',#39763,#39767,#8176,.T.);
#50522=EDGE_CURVE('',#39769,#39770,#8177,.T.);
#50523=EDGE_CURVE('',#39768,#39770,#8178,.T.);
#50524=EDGE_CURVE('',#39767,#39769,#8179,.T.);
#50525=EDGE_CURVE('',#39770,#39765,#8180,.T.);
#50526=EDGE_CURVE('',#39769,#39766,#8181,.T.);
#50527=EDGE_CURVE('',#39771,#39772,#8182,.T.);
#50528=EDGE_CURVE('',#39773,#39772,#8183,.T.);
#50529=EDGE_CURVE('',#39774,#39773,#8184,.T.);
#50530=EDGE_CURVE('',#39774,#39771,#8185,.T.);
#50531=EDGE_CURVE('',#39775,#39776,#8186,.T.);
#50532=EDGE_CURVE('',#39772,#39776,#8187,.T.);
#50533=EDGE_CURVE('',#39771,#39775,#8188,.T.);
#50534=EDGE_CURVE('',#39777,#39778,#8189,.T.);
#50535=EDGE_CURVE('',#39776,#39778,#8190,.T.);
#50536=EDGE_CURVE('',#39775,#39777,#8191,.T.);
#50537=EDGE_CURVE('',#39778,#39773,#8192,.T.);
#50538=EDGE_CURVE('',#39777,#39774,#8193,.T.);
#50539=EDGE_CURVE('',#39779,#39780,#8194,.T.);
#50540=EDGE_CURVE('',#39781,#39780,#8195,.T.);
#50541=EDGE_CURVE('',#39782,#39781,#8196,.T.);
#50542=EDGE_CURVE('',#39782,#39779,#8197,.T.);
#50543=EDGE_CURVE('',#39783,#39784,#8198,.T.);
#50544=EDGE_CURVE('',#39780,#39784,#8199,.T.);
#50545=EDGE_CURVE('',#39779,#39783,#8200,.T.);
#50546=EDGE_CURVE('',#39785,#39786,#8201,.T.);
#50547=EDGE_CURVE('',#39784,#39786,#8202,.T.);
#50548=EDGE_CURVE('',#39783,#39785,#8203,.T.);
#50549=EDGE_CURVE('',#39786,#39781,#8204,.T.);
#50550=EDGE_CURVE('',#39785,#39782,#8205,.T.);
#50551=EDGE_CURVE('',#39787,#39788,#8206,.T.);
#50552=EDGE_CURVE('',#39789,#39788,#8207,.T.);
#50553=EDGE_CURVE('',#39790,#39789,#8208,.T.);
#50554=EDGE_CURVE('',#39790,#39787,#8209,.T.);
#50555=EDGE_CURVE('',#39791,#39792,#8210,.T.);
#50556=EDGE_CURVE('',#39788,#39792,#8211,.T.);
#50557=EDGE_CURVE('',#39787,#39791,#8212,.T.);
#50558=EDGE_CURVE('',#39793,#39794,#8213,.T.);
#50559=EDGE_CURVE('',#39792,#39794,#8214,.T.);
#50560=EDGE_CURVE('',#39791,#39793,#8215,.T.);
#50561=EDGE_CURVE('',#39794,#39789,#8216,.T.);
#50562=EDGE_CURVE('',#39793,#39790,#8217,.T.);
#50563=EDGE_CURVE('',#39795,#39796,#8218,.T.);
#50564=EDGE_CURVE('',#39797,#39796,#8219,.T.);
#50565=EDGE_CURVE('',#39798,#39797,#8220,.T.);
#50566=EDGE_CURVE('',#39798,#39795,#8221,.T.);
#50567=EDGE_CURVE('',#39799,#39800,#8222,.T.);
#50568=EDGE_CURVE('',#39796,#39800,#8223,.T.);
#50569=EDGE_CURVE('',#39795,#39799,#8224,.T.);
#50570=EDGE_CURVE('',#39801,#39802,#8225,.T.);
#50571=EDGE_CURVE('',#39800,#39802,#8226,.T.);
#50572=EDGE_CURVE('',#39799,#39801,#8227,.T.);
#50573=EDGE_CURVE('',#39802,#39797,#8228,.T.);
#50574=EDGE_CURVE('',#39801,#39798,#8229,.T.);
#50575=EDGE_CURVE('',#39803,#39804,#8230,.T.);
#50576=EDGE_CURVE('',#39805,#39804,#8231,.T.);
#50577=EDGE_CURVE('',#39806,#39805,#8232,.T.);
#50578=EDGE_CURVE('',#39806,#39803,#8233,.T.);
#50579=EDGE_CURVE('',#39807,#39808,#8234,.T.);
#50580=EDGE_CURVE('',#39804,#39808,#8235,.T.);
#50581=EDGE_CURVE('',#39803,#39807,#8236,.T.);
#50582=EDGE_CURVE('',#39809,#39810,#8237,.T.);
#50583=EDGE_CURVE('',#39808,#39810,#8238,.T.);
#50584=EDGE_CURVE('',#39807,#39809,#8239,.T.);
#50585=EDGE_CURVE('',#39810,#39805,#8240,.T.);
#50586=EDGE_CURVE('',#39809,#39806,#8241,.T.);
#50587=EDGE_CURVE('',#39811,#39812,#8242,.T.);
#50588=EDGE_CURVE('',#39813,#39812,#8243,.T.);
#50589=EDGE_CURVE('',#39814,#39813,#8244,.T.);
#50590=EDGE_CURVE('',#39814,#39811,#8245,.T.);
#50591=EDGE_CURVE('',#39815,#39816,#8246,.T.);
#50592=EDGE_CURVE('',#39812,#39816,#8247,.T.);
#50593=EDGE_CURVE('',#39811,#39815,#8248,.T.);
#50594=EDGE_CURVE('',#39817,#39818,#8249,.T.);
#50595=EDGE_CURVE('',#39816,#39818,#8250,.T.);
#50596=EDGE_CURVE('',#39815,#39817,#8251,.T.);
#50597=EDGE_CURVE('',#39818,#39813,#8252,.T.);
#50598=EDGE_CURVE('',#39817,#39814,#8253,.T.);
#50599=EDGE_CURVE('',#39819,#39820,#8254,.T.);
#50600=EDGE_CURVE('',#39821,#39820,#8255,.T.);
#50601=EDGE_CURVE('',#39822,#39821,#8256,.T.);
#50602=EDGE_CURVE('',#39822,#39819,#8257,.T.);
#50603=EDGE_CURVE('',#39823,#39824,#8258,.T.);
#50604=EDGE_CURVE('',#39820,#39824,#8259,.T.);
#50605=EDGE_CURVE('',#39819,#39823,#8260,.T.);
#50606=EDGE_CURVE('',#39825,#39826,#8261,.T.);
#50607=EDGE_CURVE('',#39824,#39826,#8262,.T.);
#50608=EDGE_CURVE('',#39823,#39825,#8263,.T.);
#50609=EDGE_CURVE('',#39826,#39821,#8264,.T.);
#50610=EDGE_CURVE('',#39825,#39822,#8265,.T.);
#50611=EDGE_CURVE('',#39827,#39828,#8266,.T.);
#50612=EDGE_CURVE('',#39829,#39828,#8267,.T.);
#50613=EDGE_CURVE('',#39830,#39829,#8268,.T.);
#50614=EDGE_CURVE('',#39830,#39827,#8269,.T.);
#50615=EDGE_CURVE('',#39831,#39832,#8270,.T.);
#50616=EDGE_CURVE('',#39828,#39832,#8271,.T.);
#50617=EDGE_CURVE('',#39827,#39831,#8272,.T.);
#50618=EDGE_CURVE('',#39833,#39834,#8273,.T.);
#50619=EDGE_CURVE('',#39832,#39834,#8274,.T.);
#50620=EDGE_CURVE('',#39831,#39833,#8275,.T.);
#50621=EDGE_CURVE('',#39834,#39829,#8276,.T.);
#50622=EDGE_CURVE('',#39833,#39830,#8277,.T.);
#50623=EDGE_CURVE('',#39835,#39836,#8278,.T.);
#50624=EDGE_CURVE('',#39837,#39836,#8279,.T.);
#50625=EDGE_CURVE('',#39838,#39837,#8280,.T.);
#50626=EDGE_CURVE('',#39838,#39835,#8281,.T.);
#50627=EDGE_CURVE('',#39839,#39840,#8282,.T.);
#50628=EDGE_CURVE('',#39836,#39840,#8283,.T.);
#50629=EDGE_CURVE('',#39835,#39839,#8284,.T.);
#50630=EDGE_CURVE('',#39841,#39842,#8285,.T.);
#50631=EDGE_CURVE('',#39840,#39842,#8286,.T.);
#50632=EDGE_CURVE('',#39839,#39841,#8287,.T.);
#50633=EDGE_CURVE('',#39842,#39837,#8288,.T.);
#50634=EDGE_CURVE('',#39841,#39838,#8289,.T.);
#50635=EDGE_CURVE('',#39843,#39844,#8290,.T.);
#50636=EDGE_CURVE('',#39845,#39844,#8291,.T.);
#50637=EDGE_CURVE('',#39846,#39845,#8292,.T.);
#50638=EDGE_CURVE('',#39846,#39843,#8293,.T.);
#50639=EDGE_CURVE('',#39847,#39848,#8294,.T.);
#50640=EDGE_CURVE('',#39844,#39848,#8295,.T.);
#50641=EDGE_CURVE('',#39843,#39847,#8296,.T.);
#50642=EDGE_CURVE('',#39849,#39850,#8297,.T.);
#50643=EDGE_CURVE('',#39848,#39850,#8298,.T.);
#50644=EDGE_CURVE('',#39847,#39849,#8299,.T.);
#50645=EDGE_CURVE('',#39850,#39845,#8300,.T.);
#50646=EDGE_CURVE('',#39849,#39846,#8301,.T.);
#50647=EDGE_CURVE('',#39851,#39852,#8302,.T.);
#50648=EDGE_CURVE('',#39853,#39852,#8303,.T.);
#50649=EDGE_CURVE('',#39854,#39853,#8304,.T.);
#50650=EDGE_CURVE('',#39854,#39851,#8305,.T.);
#50651=EDGE_CURVE('',#39855,#39856,#8306,.T.);
#50652=EDGE_CURVE('',#39852,#39856,#8307,.T.);
#50653=EDGE_CURVE('',#39851,#39855,#8308,.T.);
#50654=EDGE_CURVE('',#39857,#39858,#8309,.T.);
#50655=EDGE_CURVE('',#39856,#39858,#8310,.T.);
#50656=EDGE_CURVE('',#39855,#39857,#8311,.T.);
#50657=EDGE_CURVE('',#39858,#39853,#8312,.T.);
#50658=EDGE_CURVE('',#39857,#39854,#8313,.T.);
#50659=EDGE_CURVE('',#39859,#39860,#8314,.T.);
#50660=EDGE_CURVE('',#39861,#39860,#8315,.T.);
#50661=EDGE_CURVE('',#39862,#39861,#8316,.T.);
#50662=EDGE_CURVE('',#39862,#39859,#8317,.T.);
#50663=EDGE_CURVE('',#39863,#39864,#8318,.T.);
#50664=EDGE_CURVE('',#39860,#39864,#8319,.T.);
#50665=EDGE_CURVE('',#39859,#39863,#8320,.T.);
#50666=EDGE_CURVE('',#39865,#39866,#8321,.T.);
#50667=EDGE_CURVE('',#39864,#39866,#8322,.T.);
#50668=EDGE_CURVE('',#39863,#39865,#8323,.T.);
#50669=EDGE_CURVE('',#39866,#39861,#8324,.T.);
#50670=EDGE_CURVE('',#39865,#39862,#8325,.T.);
#50671=EDGE_CURVE('',#39867,#39868,#8326,.T.);
#50672=EDGE_CURVE('',#39869,#39868,#8327,.T.);
#50673=EDGE_CURVE('',#39870,#39869,#8328,.T.);
#50674=EDGE_CURVE('',#39870,#39867,#8329,.T.);
#50675=EDGE_CURVE('',#39871,#39872,#8330,.T.);
#50676=EDGE_CURVE('',#39868,#39872,#8331,.T.);
#50677=EDGE_CURVE('',#39867,#39871,#8332,.T.);
#50678=EDGE_CURVE('',#39873,#39874,#8333,.T.);
#50679=EDGE_CURVE('',#39872,#39874,#8334,.T.);
#50680=EDGE_CURVE('',#39871,#39873,#8335,.T.);
#50681=EDGE_CURVE('',#39874,#39869,#8336,.T.);
#50682=EDGE_CURVE('',#39873,#39870,#8337,.T.);
#50683=EDGE_CURVE('',#39875,#39876,#8338,.T.);
#50684=EDGE_CURVE('',#39877,#39876,#8339,.T.);
#50685=EDGE_CURVE('',#39878,#39877,#8340,.T.);
#50686=EDGE_CURVE('',#39878,#39875,#8341,.T.);
#50687=EDGE_CURVE('',#39879,#39880,#8342,.T.);
#50688=EDGE_CURVE('',#39876,#39880,#8343,.T.);
#50689=EDGE_CURVE('',#39875,#39879,#8344,.T.);
#50690=EDGE_CURVE('',#39881,#39882,#8345,.T.);
#50691=EDGE_CURVE('',#39880,#39882,#8346,.T.);
#50692=EDGE_CURVE('',#39879,#39881,#8347,.T.);
#50693=EDGE_CURVE('',#39882,#39877,#8348,.T.);
#50694=EDGE_CURVE('',#39881,#39878,#8349,.T.);
#50695=EDGE_CURVE('',#39883,#39884,#8350,.T.);
#50696=EDGE_CURVE('',#39885,#39884,#8351,.T.);
#50697=EDGE_CURVE('',#39886,#39885,#8352,.T.);
#50698=EDGE_CURVE('',#39886,#39883,#8353,.T.);
#50699=EDGE_CURVE('',#39887,#39888,#8354,.T.);
#50700=EDGE_CURVE('',#39884,#39888,#8355,.T.);
#50701=EDGE_CURVE('',#39883,#39887,#8356,.T.);
#50702=EDGE_CURVE('',#39889,#39890,#8357,.T.);
#50703=EDGE_CURVE('',#39888,#39890,#8358,.T.);
#50704=EDGE_CURVE('',#39887,#39889,#8359,.T.);
#50705=EDGE_CURVE('',#39890,#39885,#8360,.T.);
#50706=EDGE_CURVE('',#39889,#39886,#8361,.T.);
#50707=EDGE_CURVE('',#39891,#39892,#8362,.T.);
#50708=EDGE_CURVE('',#39893,#39892,#8363,.T.);
#50709=EDGE_CURVE('',#39894,#39893,#8364,.T.);
#50710=EDGE_CURVE('',#39894,#39891,#8365,.T.);
#50711=EDGE_CURVE('',#39895,#39896,#8366,.T.);
#50712=EDGE_CURVE('',#39892,#39896,#8367,.T.);
#50713=EDGE_CURVE('',#39891,#39895,#8368,.T.);
#50714=EDGE_CURVE('',#39897,#39898,#8369,.T.);
#50715=EDGE_CURVE('',#39896,#39898,#8370,.T.);
#50716=EDGE_CURVE('',#39895,#39897,#8371,.T.);
#50717=EDGE_CURVE('',#39898,#39893,#8372,.T.);
#50718=EDGE_CURVE('',#39897,#39894,#8373,.T.);
#50719=EDGE_CURVE('',#39899,#39900,#8374,.T.);
#50720=EDGE_CURVE('',#39901,#39900,#8375,.T.);
#50721=EDGE_CURVE('',#39902,#39901,#8376,.T.);
#50722=EDGE_CURVE('',#39902,#39899,#8377,.T.);
#50723=EDGE_CURVE('',#39903,#39904,#8378,.T.);
#50724=EDGE_CURVE('',#39900,#39904,#8379,.T.);
#50725=EDGE_CURVE('',#39899,#39903,#8380,.T.);
#50726=EDGE_CURVE('',#39905,#39906,#8381,.T.);
#50727=EDGE_CURVE('',#39904,#39906,#8382,.T.);
#50728=EDGE_CURVE('',#39903,#39905,#8383,.T.);
#50729=EDGE_CURVE('',#39906,#39901,#8384,.T.);
#50730=EDGE_CURVE('',#39905,#39902,#8385,.T.);
#50731=EDGE_CURVE('',#39907,#39908,#8386,.T.);
#50732=EDGE_CURVE('',#39909,#39908,#8387,.T.);
#50733=EDGE_CURVE('',#39910,#39909,#8388,.T.);
#50734=EDGE_CURVE('',#39910,#39907,#8389,.T.);
#50735=EDGE_CURVE('',#39911,#39912,#8390,.T.);
#50736=EDGE_CURVE('',#39908,#39912,#8391,.T.);
#50737=EDGE_CURVE('',#39907,#39911,#8392,.T.);
#50738=EDGE_CURVE('',#39913,#39914,#8393,.T.);
#50739=EDGE_CURVE('',#39912,#39914,#8394,.T.);
#50740=EDGE_CURVE('',#39911,#39913,#8395,.T.);
#50741=EDGE_CURVE('',#39914,#39909,#8396,.T.);
#50742=EDGE_CURVE('',#39913,#39910,#8397,.T.);
#50743=EDGE_CURVE('',#39915,#39916,#8398,.T.);
#50744=EDGE_CURVE('',#39917,#39916,#8399,.T.);
#50745=EDGE_CURVE('',#39918,#39917,#8400,.T.);
#50746=EDGE_CURVE('',#39918,#39915,#8401,.T.);
#50747=EDGE_CURVE('',#39919,#39920,#8402,.T.);
#50748=EDGE_CURVE('',#39916,#39920,#8403,.T.);
#50749=EDGE_CURVE('',#39915,#39919,#8404,.T.);
#50750=EDGE_CURVE('',#39921,#39922,#8405,.T.);
#50751=EDGE_CURVE('',#39920,#39922,#8406,.T.);
#50752=EDGE_CURVE('',#39919,#39921,#8407,.T.);
#50753=EDGE_CURVE('',#39922,#39917,#8408,.T.);
#50754=EDGE_CURVE('',#39921,#39918,#8409,.T.);
#50755=EDGE_CURVE('',#39923,#39924,#8410,.T.);
#50756=EDGE_CURVE('',#39925,#39924,#8411,.T.);
#50757=EDGE_CURVE('',#39926,#39925,#8412,.T.);
#50758=EDGE_CURVE('',#39926,#39923,#8413,.T.);
#50759=EDGE_CURVE('',#39927,#39928,#8414,.T.);
#50760=EDGE_CURVE('',#39924,#39928,#8415,.T.);
#50761=EDGE_CURVE('',#39923,#39927,#8416,.T.);
#50762=EDGE_CURVE('',#39929,#39930,#8417,.T.);
#50763=EDGE_CURVE('',#39928,#39930,#8418,.T.);
#50764=EDGE_CURVE('',#39927,#39929,#8419,.T.);
#50765=EDGE_CURVE('',#39930,#39925,#8420,.T.);
#50766=EDGE_CURVE('',#39929,#39926,#8421,.T.);
#50767=EDGE_CURVE('',#39931,#39932,#8422,.T.);
#50768=EDGE_CURVE('',#39933,#39932,#8423,.T.);
#50769=EDGE_CURVE('',#39934,#39933,#8424,.T.);
#50770=EDGE_CURVE('',#39934,#39931,#8425,.T.);
#50771=EDGE_CURVE('',#39935,#39936,#8426,.T.);
#50772=EDGE_CURVE('',#39932,#39936,#8427,.T.);
#50773=EDGE_CURVE('',#39931,#39935,#8428,.T.);
#50774=EDGE_CURVE('',#39937,#39938,#8429,.T.);
#50775=EDGE_CURVE('',#39936,#39938,#8430,.T.);
#50776=EDGE_CURVE('',#39935,#39937,#8431,.T.);
#50777=EDGE_CURVE('',#39938,#39933,#8432,.T.);
#50778=EDGE_CURVE('',#39937,#39934,#8433,.T.);
#50779=EDGE_CURVE('',#39939,#39940,#8434,.T.);
#50780=EDGE_CURVE('',#39941,#39940,#8435,.T.);
#50781=EDGE_CURVE('',#39942,#39941,#8436,.T.);
#50782=EDGE_CURVE('',#39942,#39939,#8437,.T.);
#50783=EDGE_CURVE('',#39943,#39944,#8438,.T.);
#50784=EDGE_CURVE('',#39940,#39944,#8439,.T.);
#50785=EDGE_CURVE('',#39939,#39943,#8440,.T.);
#50786=EDGE_CURVE('',#39945,#39946,#8441,.T.);
#50787=EDGE_CURVE('',#39944,#39946,#8442,.T.);
#50788=EDGE_CURVE('',#39943,#39945,#8443,.T.);
#50789=EDGE_CURVE('',#39946,#39941,#8444,.T.);
#50790=EDGE_CURVE('',#39945,#39942,#8445,.T.);
#50791=EDGE_CURVE('',#39947,#39948,#8446,.T.);
#50792=EDGE_CURVE('',#39949,#39948,#8447,.T.);
#50793=EDGE_CURVE('',#39950,#39949,#8448,.T.);
#50794=EDGE_CURVE('',#39950,#39947,#8449,.T.);
#50795=EDGE_CURVE('',#39951,#39952,#8450,.T.);
#50796=EDGE_CURVE('',#39948,#39952,#8451,.T.);
#50797=EDGE_CURVE('',#39947,#39951,#8452,.T.);
#50798=EDGE_CURVE('',#39953,#39954,#8453,.T.);
#50799=EDGE_CURVE('',#39952,#39954,#8454,.T.);
#50800=EDGE_CURVE('',#39951,#39953,#8455,.T.);
#50801=EDGE_CURVE('',#39954,#39949,#8456,.T.);
#50802=EDGE_CURVE('',#39953,#39950,#8457,.T.);
#50803=EDGE_CURVE('',#39955,#39956,#8458,.T.);
#50804=EDGE_CURVE('',#39957,#39956,#8459,.T.);
#50805=EDGE_CURVE('',#39958,#39957,#8460,.T.);
#50806=EDGE_CURVE('',#39958,#39955,#8461,.T.);
#50807=EDGE_CURVE('',#39959,#39960,#8462,.T.);
#50808=EDGE_CURVE('',#39956,#39960,#8463,.T.);
#50809=EDGE_CURVE('',#39955,#39959,#8464,.T.);
#50810=EDGE_CURVE('',#39961,#39962,#8465,.T.);
#50811=EDGE_CURVE('',#39960,#39962,#8466,.T.);
#50812=EDGE_CURVE('',#39959,#39961,#8467,.T.);
#50813=EDGE_CURVE('',#39962,#39957,#8468,.T.);
#50814=EDGE_CURVE('',#39961,#39958,#8469,.T.);
#50815=EDGE_CURVE('',#39963,#39964,#8470,.T.);
#50816=EDGE_CURVE('',#39965,#39964,#8471,.T.);
#50817=EDGE_CURVE('',#39966,#39965,#8472,.T.);
#50818=EDGE_CURVE('',#39966,#39963,#8473,.T.);
#50819=EDGE_CURVE('',#39967,#39968,#8474,.T.);
#50820=EDGE_CURVE('',#39964,#39968,#8475,.T.);
#50821=EDGE_CURVE('',#39963,#39967,#8476,.T.);
#50822=EDGE_CURVE('',#39969,#39970,#8477,.T.);
#50823=EDGE_CURVE('',#39968,#39970,#8478,.T.);
#50824=EDGE_CURVE('',#39967,#39969,#8479,.T.);
#50825=EDGE_CURVE('',#39970,#39965,#8480,.T.);
#50826=EDGE_CURVE('',#39969,#39966,#8481,.T.);
#50827=EDGE_CURVE('',#39971,#39972,#8482,.T.);
#50828=EDGE_CURVE('',#39973,#39972,#8483,.T.);
#50829=EDGE_CURVE('',#39974,#39973,#8484,.T.);
#50830=EDGE_CURVE('',#39974,#39971,#8485,.T.);
#50831=EDGE_CURVE('',#39975,#39976,#8486,.T.);
#50832=EDGE_CURVE('',#39972,#39976,#8487,.T.);
#50833=EDGE_CURVE('',#39971,#39975,#8488,.T.);
#50834=EDGE_CURVE('',#39977,#39978,#8489,.T.);
#50835=EDGE_CURVE('',#39976,#39978,#8490,.T.);
#50836=EDGE_CURVE('',#39975,#39977,#8491,.T.);
#50837=EDGE_CURVE('',#39978,#39973,#8492,.T.);
#50838=EDGE_CURVE('',#39977,#39974,#8493,.T.);
#50839=EDGE_CURVE('',#39979,#39980,#8494,.T.);
#50840=EDGE_CURVE('',#39981,#39980,#8495,.T.);
#50841=EDGE_CURVE('',#39982,#39981,#8496,.T.);
#50842=EDGE_CURVE('',#39982,#39979,#8497,.T.);
#50843=EDGE_CURVE('',#39983,#39984,#8498,.T.);
#50844=EDGE_CURVE('',#39980,#39984,#8499,.T.);
#50845=EDGE_CURVE('',#39979,#39983,#8500,.T.);
#50846=EDGE_CURVE('',#39985,#39986,#8501,.T.);
#50847=EDGE_CURVE('',#39984,#39986,#8502,.T.);
#50848=EDGE_CURVE('',#39983,#39985,#8503,.T.);
#50849=EDGE_CURVE('',#39986,#39981,#8504,.T.);
#50850=EDGE_CURVE('',#39985,#39982,#8505,.T.);
#50851=EDGE_CURVE('',#39987,#39988,#8506,.T.);
#50852=EDGE_CURVE('',#39989,#39988,#8507,.T.);
#50853=EDGE_CURVE('',#39990,#39989,#8508,.T.);
#50854=EDGE_CURVE('',#39990,#39987,#8509,.T.);
#50855=EDGE_CURVE('',#39991,#39992,#8510,.T.);
#50856=EDGE_CURVE('',#39988,#39992,#8511,.T.);
#50857=EDGE_CURVE('',#39987,#39991,#8512,.T.);
#50858=EDGE_CURVE('',#39993,#39994,#8513,.T.);
#50859=EDGE_CURVE('',#39992,#39994,#8514,.T.);
#50860=EDGE_CURVE('',#39991,#39993,#8515,.T.);
#50861=EDGE_CURVE('',#39994,#39989,#8516,.T.);
#50862=EDGE_CURVE('',#39993,#39990,#8517,.T.);
#50863=EDGE_CURVE('',#39995,#39996,#8518,.T.);
#50864=EDGE_CURVE('',#39997,#39996,#8519,.T.);
#50865=EDGE_CURVE('',#39998,#39997,#8520,.T.);
#50866=EDGE_CURVE('',#39998,#39995,#8521,.T.);
#50867=EDGE_CURVE('',#39999,#40000,#8522,.T.);
#50868=EDGE_CURVE('',#39996,#40000,#8523,.T.);
#50869=EDGE_CURVE('',#39995,#39999,#8524,.T.);
#50870=EDGE_CURVE('',#40001,#40002,#8525,.T.);
#50871=EDGE_CURVE('',#40000,#40002,#8526,.T.);
#50872=EDGE_CURVE('',#39999,#40001,#8527,.T.);
#50873=EDGE_CURVE('',#40002,#39997,#8528,.T.);
#50874=EDGE_CURVE('',#40001,#39998,#8529,.T.);
#50875=EDGE_CURVE('',#40003,#40004,#8530,.T.);
#50876=EDGE_CURVE('',#40005,#40004,#8531,.T.);
#50877=EDGE_CURVE('',#40006,#40005,#8532,.T.);
#50878=EDGE_CURVE('',#40006,#40003,#8533,.T.);
#50879=EDGE_CURVE('',#40007,#40008,#8534,.T.);
#50880=EDGE_CURVE('',#40004,#40008,#8535,.T.);
#50881=EDGE_CURVE('',#40003,#40007,#8536,.T.);
#50882=EDGE_CURVE('',#40009,#40010,#8537,.T.);
#50883=EDGE_CURVE('',#40008,#40010,#8538,.T.);
#50884=EDGE_CURVE('',#40007,#40009,#8539,.T.);
#50885=EDGE_CURVE('',#40010,#40005,#8540,.T.);
#50886=EDGE_CURVE('',#40009,#40006,#8541,.T.);
#50887=EDGE_CURVE('',#40011,#40012,#8542,.T.);
#50888=EDGE_CURVE('',#40013,#40012,#8543,.T.);
#50889=EDGE_CURVE('',#40014,#40013,#8544,.T.);
#50890=EDGE_CURVE('',#40014,#40011,#8545,.T.);
#50891=EDGE_CURVE('',#40015,#40016,#8546,.T.);
#50892=EDGE_CURVE('',#40012,#40016,#8547,.T.);
#50893=EDGE_CURVE('',#40011,#40015,#8548,.T.);
#50894=EDGE_CURVE('',#40017,#40018,#8549,.T.);
#50895=EDGE_CURVE('',#40016,#40018,#8550,.T.);
#50896=EDGE_CURVE('',#40015,#40017,#8551,.T.);
#50897=EDGE_CURVE('',#40018,#40013,#8552,.T.);
#50898=EDGE_CURVE('',#40017,#40014,#8553,.T.);
#50899=EDGE_CURVE('',#40019,#40020,#8554,.T.);
#50900=EDGE_CURVE('',#40021,#40020,#8555,.T.);
#50901=EDGE_CURVE('',#40022,#40021,#8556,.T.);
#50902=EDGE_CURVE('',#40022,#40019,#8557,.T.);
#50903=EDGE_CURVE('',#40023,#40024,#8558,.T.);
#50904=EDGE_CURVE('',#40020,#40024,#8559,.T.);
#50905=EDGE_CURVE('',#40019,#40023,#8560,.T.);
#50906=EDGE_CURVE('',#40025,#40026,#8561,.T.);
#50907=EDGE_CURVE('',#40024,#40026,#8562,.T.);
#50908=EDGE_CURVE('',#40023,#40025,#8563,.T.);
#50909=EDGE_CURVE('',#40026,#40021,#8564,.T.);
#50910=EDGE_CURVE('',#40025,#40022,#8565,.T.);
#50911=EDGE_CURVE('',#40027,#40028,#8566,.T.);
#50912=EDGE_CURVE('',#40029,#40028,#8567,.T.);
#50913=EDGE_CURVE('',#40030,#40029,#8568,.T.);
#50914=EDGE_CURVE('',#40030,#40027,#8569,.T.);
#50915=EDGE_CURVE('',#40031,#40032,#8570,.T.);
#50916=EDGE_CURVE('',#40028,#40032,#8571,.T.);
#50917=EDGE_CURVE('',#40027,#40031,#8572,.T.);
#50918=EDGE_CURVE('',#40033,#40034,#8573,.T.);
#50919=EDGE_CURVE('',#40032,#40034,#8574,.T.);
#50920=EDGE_CURVE('',#40031,#40033,#8575,.T.);
#50921=EDGE_CURVE('',#40034,#40029,#8576,.T.);
#50922=EDGE_CURVE('',#40033,#40030,#8577,.T.);
#50923=EDGE_CURVE('',#40035,#40036,#8578,.T.);
#50924=EDGE_CURVE('',#40037,#40036,#8579,.T.);
#50925=EDGE_CURVE('',#40038,#40037,#8580,.T.);
#50926=EDGE_CURVE('',#40038,#40035,#8581,.T.);
#50927=EDGE_CURVE('',#40039,#40040,#8582,.T.);
#50928=EDGE_CURVE('',#40036,#40040,#8583,.T.);
#50929=EDGE_CURVE('',#40035,#40039,#8584,.T.);
#50930=EDGE_CURVE('',#40041,#40042,#8585,.T.);
#50931=EDGE_CURVE('',#40040,#40042,#8586,.T.);
#50932=EDGE_CURVE('',#40039,#40041,#8587,.T.);
#50933=EDGE_CURVE('',#40042,#40037,#8588,.T.);
#50934=EDGE_CURVE('',#40041,#40038,#8589,.T.);
#50935=EDGE_CURVE('',#40043,#40044,#8590,.T.);
#50936=EDGE_CURVE('',#40045,#40044,#8591,.T.);
#50937=EDGE_CURVE('',#40046,#40045,#8592,.T.);
#50938=EDGE_CURVE('',#40046,#40043,#8593,.T.);
#50939=EDGE_CURVE('',#40047,#40048,#8594,.T.);
#50940=EDGE_CURVE('',#40044,#40048,#8595,.T.);
#50941=EDGE_CURVE('',#40043,#40047,#8596,.T.);
#50942=EDGE_CURVE('',#40049,#40050,#8597,.T.);
#50943=EDGE_CURVE('',#40048,#40050,#8598,.T.);
#50944=EDGE_CURVE('',#40047,#40049,#8599,.T.);
#50945=EDGE_CURVE('',#40050,#40045,#8600,.T.);
#50946=EDGE_CURVE('',#40049,#40046,#8601,.T.);
#50947=EDGE_CURVE('',#40051,#40052,#8602,.T.);
#50948=EDGE_CURVE('',#40053,#40052,#8603,.T.);
#50949=EDGE_CURVE('',#40054,#40053,#8604,.T.);
#50950=EDGE_CURVE('',#40054,#40051,#8605,.T.);
#50951=EDGE_CURVE('',#40055,#40056,#8606,.T.);
#50952=EDGE_CURVE('',#40052,#40056,#8607,.T.);
#50953=EDGE_CURVE('',#40051,#40055,#8608,.T.);
#50954=EDGE_CURVE('',#40057,#40058,#8609,.T.);
#50955=EDGE_CURVE('',#40056,#40058,#8610,.T.);
#50956=EDGE_CURVE('',#40055,#40057,#8611,.T.);
#50957=EDGE_CURVE('',#40058,#40053,#8612,.T.);
#50958=EDGE_CURVE('',#40057,#40054,#8613,.T.);
#50959=EDGE_CURVE('',#40059,#40060,#8614,.T.);
#50960=EDGE_CURVE('',#40061,#40060,#8615,.T.);
#50961=EDGE_CURVE('',#40062,#40061,#8616,.T.);
#50962=EDGE_CURVE('',#40062,#40059,#8617,.T.);
#50963=EDGE_CURVE('',#40063,#40064,#8618,.T.);
#50964=EDGE_CURVE('',#40060,#40064,#8619,.T.);
#50965=EDGE_CURVE('',#40059,#40063,#8620,.T.);
#50966=EDGE_CURVE('',#40065,#40066,#8621,.T.);
#50967=EDGE_CURVE('',#40064,#40066,#8622,.T.);
#50968=EDGE_CURVE('',#40063,#40065,#8623,.T.);
#50969=EDGE_CURVE('',#40066,#40061,#8624,.T.);
#50970=EDGE_CURVE('',#40065,#40062,#8625,.T.);
#50971=EDGE_CURVE('',#40067,#40068,#8626,.T.);
#50972=EDGE_CURVE('',#40069,#40068,#8627,.T.);
#50973=EDGE_CURVE('',#40070,#40069,#8628,.T.);
#50974=EDGE_CURVE('',#40070,#40067,#8629,.T.);
#50975=EDGE_CURVE('',#40071,#40072,#8630,.T.);
#50976=EDGE_CURVE('',#40068,#40072,#8631,.T.);
#50977=EDGE_CURVE('',#40067,#40071,#8632,.T.);
#50978=EDGE_CURVE('',#40073,#40074,#8633,.T.);
#50979=EDGE_CURVE('',#40072,#40074,#8634,.T.);
#50980=EDGE_CURVE('',#40071,#40073,#8635,.T.);
#50981=EDGE_CURVE('',#40074,#40069,#8636,.T.);
#50982=EDGE_CURVE('',#40073,#40070,#8637,.T.);
#50983=EDGE_CURVE('',#40075,#40076,#8638,.T.);
#50984=EDGE_CURVE('',#40077,#40076,#8639,.T.);
#50985=EDGE_CURVE('',#40078,#40077,#8640,.T.);
#50986=EDGE_CURVE('',#40078,#40075,#8641,.T.);
#50987=EDGE_CURVE('',#40079,#40080,#8642,.T.);
#50988=EDGE_CURVE('',#40076,#40080,#8643,.T.);
#50989=EDGE_CURVE('',#40075,#40079,#8644,.T.);
#50990=EDGE_CURVE('',#40081,#40082,#8645,.T.);
#50991=EDGE_CURVE('',#40080,#40082,#8646,.T.);
#50992=EDGE_CURVE('',#40079,#40081,#8647,.T.);
#50993=EDGE_CURVE('',#40082,#40077,#8648,.T.);
#50994=EDGE_CURVE('',#40081,#40078,#8649,.T.);
#50995=EDGE_CURVE('',#40083,#40084,#8650,.T.);
#50996=EDGE_CURVE('',#40085,#40084,#8651,.T.);
#50997=EDGE_CURVE('',#40086,#40085,#8652,.T.);
#50998=EDGE_CURVE('',#40086,#40083,#8653,.T.);
#50999=EDGE_CURVE('',#40087,#40088,#8654,.T.);
#51000=EDGE_CURVE('',#40084,#40088,#8655,.T.);
#51001=EDGE_CURVE('',#40083,#40087,#8656,.T.);
#51002=EDGE_CURVE('',#40089,#40090,#8657,.T.);
#51003=EDGE_CURVE('',#40088,#40090,#8658,.T.);
#51004=EDGE_CURVE('',#40087,#40089,#8659,.T.);
#51005=EDGE_CURVE('',#40090,#40085,#8660,.T.);
#51006=EDGE_CURVE('',#40089,#40086,#8661,.T.);
#51007=EDGE_CURVE('',#40091,#40092,#8662,.T.);
#51008=EDGE_CURVE('',#40093,#40092,#8663,.T.);
#51009=EDGE_CURVE('',#40094,#40093,#8664,.T.);
#51010=EDGE_CURVE('',#40094,#40091,#8665,.T.);
#51011=EDGE_CURVE('',#40095,#40096,#8666,.T.);
#51012=EDGE_CURVE('',#40092,#40096,#8667,.T.);
#51013=EDGE_CURVE('',#40091,#40095,#8668,.T.);
#51014=EDGE_CURVE('',#40097,#40098,#8669,.T.);
#51015=EDGE_CURVE('',#40096,#40098,#8670,.T.);
#51016=EDGE_CURVE('',#40095,#40097,#8671,.T.);
#51017=EDGE_CURVE('',#40098,#40093,#8672,.T.);
#51018=EDGE_CURVE('',#40097,#40094,#8673,.T.);
#51019=EDGE_CURVE('',#40099,#40100,#8674,.T.);
#51020=EDGE_CURVE('',#40101,#40100,#8675,.T.);
#51021=EDGE_CURVE('',#40102,#40101,#8676,.T.);
#51022=EDGE_CURVE('',#40102,#40099,#8677,.T.);
#51023=EDGE_CURVE('',#40103,#40104,#8678,.T.);
#51024=EDGE_CURVE('',#40100,#40104,#8679,.T.);
#51025=EDGE_CURVE('',#40099,#40103,#8680,.T.);
#51026=EDGE_CURVE('',#40105,#40106,#8681,.T.);
#51027=EDGE_CURVE('',#40104,#40106,#8682,.T.);
#51028=EDGE_CURVE('',#40103,#40105,#8683,.T.);
#51029=EDGE_CURVE('',#40106,#40101,#8684,.T.);
#51030=EDGE_CURVE('',#40105,#40102,#8685,.T.);
#51031=EDGE_CURVE('',#40107,#40108,#8686,.T.);
#51032=EDGE_CURVE('',#40109,#40108,#8687,.T.);
#51033=EDGE_CURVE('',#40110,#40109,#8688,.T.);
#51034=EDGE_CURVE('',#40110,#40107,#8689,.T.);
#51035=EDGE_CURVE('',#40111,#40112,#8690,.T.);
#51036=EDGE_CURVE('',#40108,#40112,#8691,.T.);
#51037=EDGE_CURVE('',#40107,#40111,#8692,.T.);
#51038=EDGE_CURVE('',#40113,#40114,#8693,.T.);
#51039=EDGE_CURVE('',#40112,#40114,#8694,.T.);
#51040=EDGE_CURVE('',#40111,#40113,#8695,.T.);
#51041=EDGE_CURVE('',#40114,#40109,#8696,.T.);
#51042=EDGE_CURVE('',#40113,#40110,#8697,.T.);
#51043=EDGE_CURVE('',#40115,#40116,#8698,.T.);
#51044=EDGE_CURVE('',#40117,#40116,#8699,.T.);
#51045=EDGE_CURVE('',#40118,#40117,#8700,.T.);
#51046=EDGE_CURVE('',#40118,#40115,#8701,.T.);
#51047=EDGE_CURVE('',#40119,#40120,#8702,.T.);
#51048=EDGE_CURVE('',#40116,#40120,#8703,.T.);
#51049=EDGE_CURVE('',#40115,#40119,#8704,.T.);
#51050=EDGE_CURVE('',#40121,#40122,#8705,.T.);
#51051=EDGE_CURVE('',#40120,#40122,#8706,.T.);
#51052=EDGE_CURVE('',#40119,#40121,#8707,.T.);
#51053=EDGE_CURVE('',#40122,#40117,#8708,.T.);
#51054=EDGE_CURVE('',#40121,#40118,#8709,.T.);
#51055=EDGE_CURVE('',#40123,#40124,#8710,.T.);
#51056=EDGE_CURVE('',#40125,#40124,#8711,.T.);
#51057=EDGE_CURVE('',#40126,#40125,#8712,.T.);
#51058=EDGE_CURVE('',#40126,#40123,#8713,.T.);
#51059=EDGE_CURVE('',#40127,#40128,#8714,.T.);
#51060=EDGE_CURVE('',#40124,#40128,#8715,.T.);
#51061=EDGE_CURVE('',#40123,#40127,#8716,.T.);
#51062=EDGE_CURVE('',#40129,#40130,#8717,.T.);
#51063=EDGE_CURVE('',#40128,#40130,#8718,.T.);
#51064=EDGE_CURVE('',#40127,#40129,#8719,.T.);
#51065=EDGE_CURVE('',#40130,#40125,#8720,.T.);
#51066=EDGE_CURVE('',#40129,#40126,#8721,.T.);
#51067=EDGE_CURVE('',#40131,#40132,#8722,.T.);
#51068=EDGE_CURVE('',#40133,#40132,#8723,.T.);
#51069=EDGE_CURVE('',#40134,#40133,#8724,.T.);
#51070=EDGE_CURVE('',#40134,#40131,#8725,.T.);
#51071=EDGE_CURVE('',#40135,#40136,#8726,.T.);
#51072=EDGE_CURVE('',#40132,#40136,#8727,.T.);
#51073=EDGE_CURVE('',#40131,#40135,#8728,.T.);
#51074=EDGE_CURVE('',#40137,#40138,#8729,.T.);
#51075=EDGE_CURVE('',#40136,#40138,#8730,.T.);
#51076=EDGE_CURVE('',#40135,#40137,#8731,.T.);
#51077=EDGE_CURVE('',#40138,#40133,#8732,.T.);
#51078=EDGE_CURVE('',#40137,#40134,#8733,.T.);
#51079=EDGE_CURVE('',#40139,#40140,#8734,.T.);
#51080=EDGE_CURVE('',#40141,#40140,#8735,.T.);
#51081=EDGE_CURVE('',#40142,#40141,#8736,.T.);
#51082=EDGE_CURVE('',#40142,#40139,#8737,.T.);
#51083=EDGE_CURVE('',#40143,#40144,#8738,.T.);
#51084=EDGE_CURVE('',#40140,#40144,#8739,.T.);
#51085=EDGE_CURVE('',#40139,#40143,#8740,.T.);
#51086=EDGE_CURVE('',#40145,#40146,#8741,.T.);
#51087=EDGE_CURVE('',#40144,#40146,#8742,.T.);
#51088=EDGE_CURVE('',#40143,#40145,#8743,.T.);
#51089=EDGE_CURVE('',#40146,#40141,#8744,.T.);
#51090=EDGE_CURVE('',#40145,#40142,#8745,.T.);
#51091=EDGE_CURVE('',#40147,#40148,#8746,.T.);
#51092=EDGE_CURVE('',#40149,#40148,#8747,.T.);
#51093=EDGE_CURVE('',#40150,#40149,#8748,.T.);
#51094=EDGE_CURVE('',#40150,#40147,#8749,.T.);
#51095=EDGE_CURVE('',#40151,#40152,#8750,.T.);
#51096=EDGE_CURVE('',#40148,#40152,#8751,.T.);
#51097=EDGE_CURVE('',#40147,#40151,#8752,.T.);
#51098=EDGE_CURVE('',#40153,#40154,#8753,.T.);
#51099=EDGE_CURVE('',#40152,#40154,#8754,.T.);
#51100=EDGE_CURVE('',#40151,#40153,#8755,.T.);
#51101=EDGE_CURVE('',#40154,#40149,#8756,.T.);
#51102=EDGE_CURVE('',#40153,#40150,#8757,.T.);
#51103=EDGE_CURVE('',#40155,#40156,#8758,.T.);
#51104=EDGE_CURVE('',#40157,#40156,#8759,.T.);
#51105=EDGE_CURVE('',#40158,#40157,#8760,.T.);
#51106=EDGE_CURVE('',#40158,#40155,#8761,.T.);
#51107=EDGE_CURVE('',#40159,#40160,#8762,.T.);
#51108=EDGE_CURVE('',#40156,#40160,#8763,.T.);
#51109=EDGE_CURVE('',#40155,#40159,#8764,.T.);
#51110=EDGE_CURVE('',#40161,#40162,#8765,.T.);
#51111=EDGE_CURVE('',#40160,#40162,#8766,.T.);
#51112=EDGE_CURVE('',#40159,#40161,#8767,.T.);
#51113=EDGE_CURVE('',#40162,#40157,#8768,.T.);
#51114=EDGE_CURVE('',#40161,#40158,#8769,.T.);
#51115=EDGE_CURVE('',#40163,#40164,#8770,.T.);
#51116=EDGE_CURVE('',#40165,#40164,#8771,.T.);
#51117=EDGE_CURVE('',#40166,#40165,#8772,.T.);
#51118=EDGE_CURVE('',#40166,#40163,#8773,.T.);
#51119=EDGE_CURVE('',#40167,#40168,#8774,.T.);
#51120=EDGE_CURVE('',#40164,#40168,#8775,.T.);
#51121=EDGE_CURVE('',#40163,#40167,#8776,.T.);
#51122=EDGE_CURVE('',#40169,#40170,#8777,.T.);
#51123=EDGE_CURVE('',#40168,#40170,#8778,.T.);
#51124=EDGE_CURVE('',#40167,#40169,#8779,.T.);
#51125=EDGE_CURVE('',#40170,#40165,#8780,.T.);
#51126=EDGE_CURVE('',#40169,#40166,#8781,.T.);
#51127=EDGE_CURVE('',#40171,#40172,#8782,.T.);
#51128=EDGE_CURVE('',#40173,#40172,#8783,.T.);
#51129=EDGE_CURVE('',#40174,#40173,#8784,.T.);
#51130=EDGE_CURVE('',#40174,#40171,#8785,.T.);
#51131=EDGE_CURVE('',#40175,#40176,#8786,.T.);
#51132=EDGE_CURVE('',#40172,#40176,#8787,.T.);
#51133=EDGE_CURVE('',#40171,#40175,#8788,.T.);
#51134=EDGE_CURVE('',#40177,#40178,#8789,.T.);
#51135=EDGE_CURVE('',#40176,#40178,#8790,.T.);
#51136=EDGE_CURVE('',#40175,#40177,#8791,.T.);
#51137=EDGE_CURVE('',#40178,#40173,#8792,.T.);
#51138=EDGE_CURVE('',#40177,#40174,#8793,.T.);
#51139=EDGE_CURVE('',#40179,#40180,#8794,.T.);
#51140=EDGE_CURVE('',#40181,#40180,#8795,.T.);
#51141=EDGE_CURVE('',#40182,#40181,#8796,.T.);
#51142=EDGE_CURVE('',#40182,#40179,#8797,.T.);
#51143=EDGE_CURVE('',#40183,#40184,#8798,.T.);
#51144=EDGE_CURVE('',#40180,#40184,#8799,.T.);
#51145=EDGE_CURVE('',#40179,#40183,#8800,.T.);
#51146=EDGE_CURVE('',#40185,#40186,#8801,.T.);
#51147=EDGE_CURVE('',#40184,#40186,#8802,.T.);
#51148=EDGE_CURVE('',#40183,#40185,#8803,.T.);
#51149=EDGE_CURVE('',#40186,#40181,#8804,.T.);
#51150=EDGE_CURVE('',#40185,#40182,#8805,.T.);
#51151=EDGE_CURVE('',#40187,#40188,#8806,.T.);
#51152=EDGE_CURVE('',#40189,#40188,#8807,.T.);
#51153=EDGE_CURVE('',#40190,#40189,#8808,.T.);
#51154=EDGE_CURVE('',#40190,#40187,#8809,.T.);
#51155=EDGE_CURVE('',#40191,#40192,#8810,.T.);
#51156=EDGE_CURVE('',#40188,#40192,#8811,.T.);
#51157=EDGE_CURVE('',#40187,#40191,#8812,.T.);
#51158=EDGE_CURVE('',#40193,#40194,#8813,.T.);
#51159=EDGE_CURVE('',#40192,#40194,#8814,.T.);
#51160=EDGE_CURVE('',#40191,#40193,#8815,.T.);
#51161=EDGE_CURVE('',#40194,#40189,#8816,.T.);
#51162=EDGE_CURVE('',#40193,#40190,#8817,.T.);
#51163=EDGE_CURVE('',#40195,#40196,#8818,.T.);
#51164=EDGE_CURVE('',#40197,#40196,#8819,.T.);
#51165=EDGE_CURVE('',#40198,#40197,#8820,.T.);
#51166=EDGE_CURVE('',#40198,#40195,#8821,.T.);
#51167=EDGE_CURVE('',#40199,#40200,#8822,.T.);
#51168=EDGE_CURVE('',#40196,#40200,#8823,.T.);
#51169=EDGE_CURVE('',#40195,#40199,#8824,.T.);
#51170=EDGE_CURVE('',#40201,#40202,#8825,.T.);
#51171=EDGE_CURVE('',#40200,#40202,#8826,.T.);
#51172=EDGE_CURVE('',#40199,#40201,#8827,.T.);
#51173=EDGE_CURVE('',#40202,#40197,#8828,.T.);
#51174=EDGE_CURVE('',#40201,#40198,#8829,.T.);
#51175=EDGE_CURVE('',#40203,#40204,#8830,.T.);
#51176=EDGE_CURVE('',#40205,#40204,#8831,.T.);
#51177=EDGE_CURVE('',#40206,#40205,#8832,.T.);
#51178=EDGE_CURVE('',#40206,#40203,#8833,.T.);
#51179=EDGE_CURVE('',#40207,#40208,#8834,.T.);
#51180=EDGE_CURVE('',#40204,#40208,#8835,.T.);
#51181=EDGE_CURVE('',#40203,#40207,#8836,.T.);
#51182=EDGE_CURVE('',#40209,#40210,#8837,.T.);
#51183=EDGE_CURVE('',#40208,#40210,#8838,.T.);
#51184=EDGE_CURVE('',#40207,#40209,#8839,.T.);
#51185=EDGE_CURVE('',#40210,#40205,#8840,.T.);
#51186=EDGE_CURVE('',#40209,#40206,#8841,.T.);
#51187=EDGE_CURVE('',#40211,#40212,#8842,.T.);
#51188=EDGE_CURVE('',#40213,#40212,#8843,.T.);
#51189=EDGE_CURVE('',#40214,#40213,#8844,.T.);
#51190=EDGE_CURVE('',#40214,#40211,#8845,.T.);
#51191=EDGE_CURVE('',#40215,#40216,#8846,.T.);
#51192=EDGE_CURVE('',#40212,#40216,#8847,.T.);
#51193=EDGE_CURVE('',#40211,#40215,#8848,.T.);
#51194=EDGE_CURVE('',#40217,#40218,#8849,.T.);
#51195=EDGE_CURVE('',#40216,#40218,#8850,.T.);
#51196=EDGE_CURVE('',#40215,#40217,#8851,.T.);
#51197=EDGE_CURVE('',#40218,#40213,#8852,.T.);
#51198=EDGE_CURVE('',#40217,#40214,#8853,.T.);
#51199=EDGE_CURVE('',#40219,#40220,#8854,.T.);
#51200=EDGE_CURVE('',#40221,#40220,#8855,.T.);
#51201=EDGE_CURVE('',#40222,#40221,#8856,.T.);
#51202=EDGE_CURVE('',#40222,#40219,#8857,.T.);
#51203=EDGE_CURVE('',#40223,#40224,#8858,.T.);
#51204=EDGE_CURVE('',#40220,#40224,#8859,.T.);
#51205=EDGE_CURVE('',#40219,#40223,#8860,.T.);
#51206=EDGE_CURVE('',#40225,#40226,#8861,.T.);
#51207=EDGE_CURVE('',#40224,#40226,#8862,.T.);
#51208=EDGE_CURVE('',#40223,#40225,#8863,.T.);
#51209=EDGE_CURVE('',#40226,#40221,#8864,.T.);
#51210=EDGE_CURVE('',#40225,#40222,#8865,.T.);
#51211=EDGE_CURVE('',#40227,#40228,#8866,.T.);
#51212=EDGE_CURVE('',#40229,#40228,#8867,.T.);
#51213=EDGE_CURVE('',#40230,#40229,#8868,.T.);
#51214=EDGE_CURVE('',#40230,#40227,#8869,.T.);
#51215=EDGE_CURVE('',#40231,#40232,#8870,.T.);
#51216=EDGE_CURVE('',#40228,#40232,#8871,.T.);
#51217=EDGE_CURVE('',#40227,#40231,#8872,.T.);
#51218=EDGE_CURVE('',#40233,#40234,#8873,.T.);
#51219=EDGE_CURVE('',#40232,#40234,#8874,.T.);
#51220=EDGE_CURVE('',#40231,#40233,#8875,.T.);
#51221=EDGE_CURVE('',#40234,#40229,#8876,.T.);
#51222=EDGE_CURVE('',#40233,#40230,#8877,.T.);
#51223=EDGE_CURVE('',#40235,#40236,#8878,.T.);
#51224=EDGE_CURVE('',#40237,#40236,#8879,.T.);
#51225=EDGE_CURVE('',#40238,#40237,#8880,.T.);
#51226=EDGE_CURVE('',#40238,#40235,#8881,.T.);
#51227=EDGE_CURVE('',#40239,#40240,#8882,.T.);
#51228=EDGE_CURVE('',#40236,#40240,#8883,.T.);
#51229=EDGE_CURVE('',#40235,#40239,#8884,.T.);
#51230=EDGE_CURVE('',#40241,#40242,#8885,.T.);
#51231=EDGE_CURVE('',#40240,#40242,#8886,.T.);
#51232=EDGE_CURVE('',#40239,#40241,#8887,.T.);
#51233=EDGE_CURVE('',#40242,#40237,#8888,.T.);
#51234=EDGE_CURVE('',#40241,#40238,#8889,.T.);
#51235=EDGE_CURVE('',#40243,#40244,#8890,.T.);
#51236=EDGE_CURVE('',#40245,#40244,#8891,.T.);
#51237=EDGE_CURVE('',#40246,#40245,#8892,.T.);
#51238=EDGE_CURVE('',#40246,#40243,#8893,.T.);
#51239=EDGE_CURVE('',#40247,#40248,#8894,.T.);
#51240=EDGE_CURVE('',#40244,#40248,#8895,.T.);
#51241=EDGE_CURVE('',#40243,#40247,#8896,.T.);
#51242=EDGE_CURVE('',#40249,#40250,#8897,.T.);
#51243=EDGE_CURVE('',#40248,#40250,#8898,.T.);
#51244=EDGE_CURVE('',#40247,#40249,#8899,.T.);
#51245=EDGE_CURVE('',#40250,#40245,#8900,.T.);
#51246=EDGE_CURVE('',#40249,#40246,#8901,.T.);
#51247=EDGE_CURVE('',#40251,#40252,#8902,.T.);
#51248=EDGE_CURVE('',#40253,#40252,#8903,.T.);
#51249=EDGE_CURVE('',#40254,#40253,#8904,.T.);
#51250=EDGE_CURVE('',#40254,#40251,#8905,.T.);
#51251=EDGE_CURVE('',#40255,#40256,#8906,.T.);
#51252=EDGE_CURVE('',#40252,#40256,#8907,.T.);
#51253=EDGE_CURVE('',#40251,#40255,#8908,.T.);
#51254=EDGE_CURVE('',#40257,#40258,#8909,.T.);
#51255=EDGE_CURVE('',#40256,#40258,#8910,.T.);
#51256=EDGE_CURVE('',#40255,#40257,#8911,.T.);
#51257=EDGE_CURVE('',#40258,#40253,#8912,.T.);
#51258=EDGE_CURVE('',#40257,#40254,#8913,.T.);
#51259=EDGE_CURVE('',#40259,#40260,#8914,.T.);
#51260=EDGE_CURVE('',#40261,#40260,#8915,.T.);
#51261=EDGE_CURVE('',#40262,#40261,#8916,.T.);
#51262=EDGE_CURVE('',#40262,#40259,#8917,.T.);
#51263=EDGE_CURVE('',#40263,#40264,#8918,.T.);
#51264=EDGE_CURVE('',#40260,#40264,#8919,.T.);
#51265=EDGE_CURVE('',#40259,#40263,#8920,.T.);
#51266=EDGE_CURVE('',#40265,#40266,#8921,.T.);
#51267=EDGE_CURVE('',#40264,#40266,#8922,.T.);
#51268=EDGE_CURVE('',#40263,#40265,#8923,.T.);
#51269=EDGE_CURVE('',#40266,#40261,#8924,.T.);
#51270=EDGE_CURVE('',#40265,#40262,#8925,.T.);
#51271=EDGE_CURVE('',#40267,#40268,#8926,.T.);
#51272=EDGE_CURVE('',#40269,#40268,#8927,.T.);
#51273=EDGE_CURVE('',#40270,#40269,#8928,.T.);
#51274=EDGE_CURVE('',#40270,#40267,#8929,.T.);
#51275=EDGE_CURVE('',#40271,#40272,#8930,.T.);
#51276=EDGE_CURVE('',#40268,#40272,#8931,.T.);
#51277=EDGE_CURVE('',#40267,#40271,#8932,.T.);
#51278=EDGE_CURVE('',#40273,#40274,#8933,.T.);
#51279=EDGE_CURVE('',#40272,#40274,#8934,.T.);
#51280=EDGE_CURVE('',#40271,#40273,#8935,.T.);
#51281=EDGE_CURVE('',#40274,#40269,#8936,.T.);
#51282=EDGE_CURVE('',#40273,#40270,#8937,.T.);
#51283=EDGE_CURVE('',#40275,#40276,#8938,.T.);
#51284=EDGE_CURVE('',#40277,#40276,#8939,.T.);
#51285=EDGE_CURVE('',#40278,#40277,#8940,.T.);
#51286=EDGE_CURVE('',#40278,#40275,#8941,.T.);
#51287=EDGE_CURVE('',#40279,#40280,#8942,.T.);
#51288=EDGE_CURVE('',#40276,#40280,#8943,.T.);
#51289=EDGE_CURVE('',#40275,#40279,#8944,.T.);
#51290=EDGE_CURVE('',#40281,#40282,#8945,.T.);
#51291=EDGE_CURVE('',#40280,#40282,#8946,.T.);
#51292=EDGE_CURVE('',#40279,#40281,#8947,.T.);
#51293=EDGE_CURVE('',#40282,#40277,#8948,.T.);
#51294=EDGE_CURVE('',#40281,#40278,#8949,.T.);
#51295=EDGE_CURVE('',#40283,#40284,#8950,.T.);
#51296=EDGE_CURVE('',#40285,#40284,#8951,.T.);
#51297=EDGE_CURVE('',#40286,#40285,#8952,.T.);
#51298=EDGE_CURVE('',#40286,#40283,#8953,.T.);
#51299=EDGE_CURVE('',#40287,#40288,#8954,.T.);
#51300=EDGE_CURVE('',#40284,#40288,#8955,.T.);
#51301=EDGE_CURVE('',#40283,#40287,#8956,.T.);
#51302=EDGE_CURVE('',#40289,#40290,#8957,.T.);
#51303=EDGE_CURVE('',#40288,#40290,#8958,.T.);
#51304=EDGE_CURVE('',#40287,#40289,#8959,.T.);
#51305=EDGE_CURVE('',#40290,#40285,#8960,.T.);
#51306=EDGE_CURVE('',#40289,#40286,#8961,.T.);
#51307=EDGE_CURVE('',#40291,#40292,#8962,.T.);
#51308=EDGE_CURVE('',#40293,#40292,#8963,.T.);
#51309=EDGE_CURVE('',#40294,#40293,#8964,.T.);
#51310=EDGE_CURVE('',#40294,#40291,#8965,.T.);
#51311=EDGE_CURVE('',#40295,#40296,#8966,.T.);
#51312=EDGE_CURVE('',#40292,#40296,#8967,.T.);
#51313=EDGE_CURVE('',#40291,#40295,#8968,.T.);
#51314=EDGE_CURVE('',#40297,#40298,#8969,.T.);
#51315=EDGE_CURVE('',#40296,#40298,#8970,.T.);
#51316=EDGE_CURVE('',#40295,#40297,#8971,.T.);
#51317=EDGE_CURVE('',#40298,#40293,#8972,.T.);
#51318=EDGE_CURVE('',#40297,#40294,#8973,.T.);
#51319=EDGE_CURVE('',#40299,#40300,#8974,.T.);
#51320=EDGE_CURVE('',#40301,#40300,#8975,.T.);
#51321=EDGE_CURVE('',#40302,#40301,#8976,.T.);
#51322=EDGE_CURVE('',#40302,#40299,#8977,.T.);
#51323=EDGE_CURVE('',#40303,#40304,#8978,.T.);
#51324=EDGE_CURVE('',#40300,#40304,#8979,.T.);
#51325=EDGE_CURVE('',#40299,#40303,#8980,.T.);
#51326=EDGE_CURVE('',#40305,#40306,#8981,.T.);
#51327=EDGE_CURVE('',#40304,#40306,#8982,.T.);
#51328=EDGE_CURVE('',#40303,#40305,#8983,.T.);
#51329=EDGE_CURVE('',#40306,#40301,#8984,.T.);
#51330=EDGE_CURVE('',#40305,#40302,#8985,.T.);
#51331=EDGE_CURVE('',#40307,#40308,#8986,.T.);
#51332=EDGE_CURVE('',#40309,#40308,#8987,.T.);
#51333=EDGE_CURVE('',#40310,#40309,#8988,.T.);
#51334=EDGE_CURVE('',#40310,#40307,#8989,.T.);
#51335=EDGE_CURVE('',#40311,#40312,#8990,.T.);
#51336=EDGE_CURVE('',#40308,#40312,#8991,.T.);
#51337=EDGE_CURVE('',#40307,#40311,#8992,.T.);
#51338=EDGE_CURVE('',#40313,#40314,#8993,.T.);
#51339=EDGE_CURVE('',#40312,#40314,#8994,.T.);
#51340=EDGE_CURVE('',#40311,#40313,#8995,.T.);
#51341=EDGE_CURVE('',#40314,#40309,#8996,.T.);
#51342=EDGE_CURVE('',#40313,#40310,#8997,.T.);
#51343=EDGE_CURVE('',#40315,#40316,#8998,.T.);
#51344=EDGE_CURVE('',#40317,#40316,#8999,.T.);
#51345=EDGE_CURVE('',#40318,#40317,#9000,.T.);
#51346=EDGE_CURVE('',#40318,#40315,#9001,.T.);
#51347=EDGE_CURVE('',#40319,#40320,#9002,.T.);
#51348=EDGE_CURVE('',#40316,#40320,#9003,.T.);
#51349=EDGE_CURVE('',#40315,#40319,#9004,.T.);
#51350=EDGE_CURVE('',#40321,#40322,#9005,.T.);
#51351=EDGE_CURVE('',#40320,#40322,#9006,.T.);
#51352=EDGE_CURVE('',#40319,#40321,#9007,.T.);
#51353=EDGE_CURVE('',#40322,#40317,#9008,.T.);
#51354=EDGE_CURVE('',#40321,#40318,#9009,.T.);
#51355=EDGE_CURVE('',#40323,#40324,#9010,.T.);
#51356=EDGE_CURVE('',#40325,#40324,#9011,.T.);
#51357=EDGE_CURVE('',#40326,#40325,#9012,.T.);
#51358=EDGE_CURVE('',#40326,#40323,#9013,.T.);
#51359=EDGE_CURVE('',#40327,#40328,#9014,.T.);
#51360=EDGE_CURVE('',#40324,#40328,#9015,.T.);
#51361=EDGE_CURVE('',#40323,#40327,#9016,.T.);
#51362=EDGE_CURVE('',#40329,#40330,#9017,.T.);
#51363=EDGE_CURVE('',#40328,#40330,#9018,.T.);
#51364=EDGE_CURVE('',#40327,#40329,#9019,.T.);
#51365=EDGE_CURVE('',#40330,#40325,#9020,.T.);
#51366=EDGE_CURVE('',#40329,#40326,#9021,.T.);
#51367=EDGE_CURVE('',#40331,#40332,#9022,.T.);
#51368=EDGE_CURVE('',#40333,#40332,#9023,.T.);
#51369=EDGE_CURVE('',#40334,#40333,#9024,.T.);
#51370=EDGE_CURVE('',#40334,#40331,#9025,.T.);
#51371=EDGE_CURVE('',#40335,#40336,#9026,.T.);
#51372=EDGE_CURVE('',#40332,#40336,#9027,.T.);
#51373=EDGE_CURVE('',#40331,#40335,#9028,.T.);
#51374=EDGE_CURVE('',#40337,#40338,#9029,.T.);
#51375=EDGE_CURVE('',#40336,#40338,#9030,.T.);
#51376=EDGE_CURVE('',#40335,#40337,#9031,.T.);
#51377=EDGE_CURVE('',#40338,#40333,#9032,.T.);
#51378=EDGE_CURVE('',#40337,#40334,#9033,.T.);
#51379=EDGE_CURVE('',#40339,#40340,#9034,.T.);
#51380=EDGE_CURVE('',#40341,#40340,#9035,.T.);
#51381=EDGE_CURVE('',#40342,#40341,#9036,.T.);
#51382=EDGE_CURVE('',#40342,#40339,#9037,.T.);
#51383=EDGE_CURVE('',#40343,#40344,#9038,.T.);
#51384=EDGE_CURVE('',#40340,#40344,#9039,.T.);
#51385=EDGE_CURVE('',#40339,#40343,#9040,.T.);
#51386=EDGE_CURVE('',#40345,#40346,#9041,.T.);
#51387=EDGE_CURVE('',#40344,#40346,#9042,.T.);
#51388=EDGE_CURVE('',#40343,#40345,#9043,.T.);
#51389=EDGE_CURVE('',#40346,#40341,#9044,.T.);
#51390=EDGE_CURVE('',#40345,#40342,#9045,.T.);
#51391=EDGE_CURVE('',#40347,#40348,#9046,.T.);
#51392=EDGE_CURVE('',#40349,#40348,#9047,.T.);
#51393=EDGE_CURVE('',#40350,#40349,#9048,.T.);
#51394=EDGE_CURVE('',#40350,#40347,#9049,.T.);
#51395=EDGE_CURVE('',#40351,#40352,#9050,.T.);
#51396=EDGE_CURVE('',#40348,#40352,#9051,.T.);
#51397=EDGE_CURVE('',#40347,#40351,#9052,.T.);
#51398=EDGE_CURVE('',#40353,#40354,#9053,.T.);
#51399=EDGE_CURVE('',#40352,#40354,#9054,.T.);
#51400=EDGE_CURVE('',#40351,#40353,#9055,.T.);
#51401=EDGE_CURVE('',#40354,#40349,#9056,.T.);
#51402=EDGE_CURVE('',#40353,#40350,#9057,.T.);
#51403=EDGE_CURVE('',#40355,#40356,#9058,.T.);
#51404=EDGE_CURVE('',#40357,#40356,#9059,.T.);
#51405=EDGE_CURVE('',#40358,#40357,#9060,.T.);
#51406=EDGE_CURVE('',#40358,#40355,#9061,.T.);
#51407=EDGE_CURVE('',#40359,#40360,#9062,.T.);
#51408=EDGE_CURVE('',#40356,#40360,#9063,.T.);
#51409=EDGE_CURVE('',#40355,#40359,#9064,.T.);
#51410=EDGE_CURVE('',#40361,#40362,#9065,.T.);
#51411=EDGE_CURVE('',#40360,#40362,#9066,.T.);
#51412=EDGE_CURVE('',#40359,#40361,#9067,.T.);
#51413=EDGE_CURVE('',#40362,#40357,#9068,.T.);
#51414=EDGE_CURVE('',#40361,#40358,#9069,.T.);
#51415=EDGE_CURVE('',#40363,#40364,#9070,.T.);
#51416=EDGE_CURVE('',#40365,#40364,#9071,.T.);
#51417=EDGE_CURVE('',#40366,#40365,#9072,.T.);
#51418=EDGE_CURVE('',#40366,#40363,#9073,.T.);
#51419=EDGE_CURVE('',#40367,#40368,#9074,.T.);
#51420=EDGE_CURVE('',#40364,#40368,#9075,.T.);
#51421=EDGE_CURVE('',#40363,#40367,#9076,.T.);
#51422=EDGE_CURVE('',#40369,#40370,#9077,.T.);
#51423=EDGE_CURVE('',#40368,#40370,#9078,.T.);
#51424=EDGE_CURVE('',#40367,#40369,#9079,.T.);
#51425=EDGE_CURVE('',#40370,#40365,#9080,.T.);
#51426=EDGE_CURVE('',#40369,#40366,#9081,.T.);
#51427=EDGE_CURVE('',#40371,#40372,#9082,.T.);
#51428=EDGE_CURVE('',#40373,#40372,#9083,.T.);
#51429=EDGE_CURVE('',#40374,#40373,#9084,.T.);
#51430=EDGE_CURVE('',#40374,#40371,#9085,.T.);
#51431=EDGE_CURVE('',#40375,#40376,#9086,.T.);
#51432=EDGE_CURVE('',#40372,#40376,#9087,.T.);
#51433=EDGE_CURVE('',#40371,#40375,#9088,.T.);
#51434=EDGE_CURVE('',#40377,#40378,#9089,.T.);
#51435=EDGE_CURVE('',#40376,#40378,#9090,.T.);
#51436=EDGE_CURVE('',#40375,#40377,#9091,.T.);
#51437=EDGE_CURVE('',#40378,#40373,#9092,.T.);
#51438=EDGE_CURVE('',#40377,#40374,#9093,.T.);
#51439=EDGE_CURVE('',#40379,#40380,#9094,.T.);
#51440=EDGE_CURVE('',#40381,#40380,#9095,.T.);
#51441=EDGE_CURVE('',#40382,#40381,#9096,.T.);
#51442=EDGE_CURVE('',#40382,#40379,#9097,.T.);
#51443=EDGE_CURVE('',#40383,#40384,#9098,.T.);
#51444=EDGE_CURVE('',#40380,#40384,#9099,.T.);
#51445=EDGE_CURVE('',#40379,#40383,#9100,.T.);
#51446=EDGE_CURVE('',#40385,#40386,#9101,.T.);
#51447=EDGE_CURVE('',#40384,#40386,#9102,.T.);
#51448=EDGE_CURVE('',#40383,#40385,#9103,.T.);
#51449=EDGE_CURVE('',#40386,#40381,#9104,.T.);
#51450=EDGE_CURVE('',#40385,#40382,#9105,.T.);
#51451=EDGE_CURVE('',#40387,#40388,#9106,.T.);
#51452=EDGE_CURVE('',#40389,#40388,#9107,.T.);
#51453=EDGE_CURVE('',#40390,#40389,#9108,.T.);
#51454=EDGE_CURVE('',#40390,#40387,#9109,.T.);
#51455=EDGE_CURVE('',#40391,#40392,#9110,.T.);
#51456=EDGE_CURVE('',#40388,#40392,#9111,.T.);
#51457=EDGE_CURVE('',#40387,#40391,#9112,.T.);
#51458=EDGE_CURVE('',#40393,#40394,#9113,.T.);
#51459=EDGE_CURVE('',#40392,#40394,#9114,.T.);
#51460=EDGE_CURVE('',#40391,#40393,#9115,.T.);
#51461=EDGE_CURVE('',#40394,#40389,#9116,.T.);
#51462=EDGE_CURVE('',#40393,#40390,#9117,.T.);
#51463=EDGE_CURVE('',#40395,#40396,#9118,.T.);
#51464=EDGE_CURVE('',#40397,#40396,#9119,.T.);
#51465=EDGE_CURVE('',#40398,#40397,#9120,.T.);
#51466=EDGE_CURVE('',#40398,#40395,#9121,.T.);
#51467=EDGE_CURVE('',#40399,#40400,#9122,.T.);
#51468=EDGE_CURVE('',#40396,#40400,#9123,.T.);
#51469=EDGE_CURVE('',#40395,#40399,#9124,.T.);
#51470=EDGE_CURVE('',#40401,#40402,#9125,.T.);
#51471=EDGE_CURVE('',#40400,#40402,#9126,.T.);
#51472=EDGE_CURVE('',#40399,#40401,#9127,.T.);
#51473=EDGE_CURVE('',#40402,#40397,#9128,.T.);
#51474=EDGE_CURVE('',#40401,#40398,#9129,.T.);
#51475=EDGE_CURVE('',#40403,#40404,#9130,.T.);
#51476=EDGE_CURVE('',#40405,#40404,#9131,.T.);
#51477=EDGE_CURVE('',#40406,#40405,#9132,.T.);
#51478=EDGE_CURVE('',#40406,#40403,#9133,.T.);
#51479=EDGE_CURVE('',#40407,#40408,#9134,.T.);
#51480=EDGE_CURVE('',#40404,#40408,#9135,.T.);
#51481=EDGE_CURVE('',#40403,#40407,#9136,.T.);
#51482=EDGE_CURVE('',#40409,#40410,#9137,.T.);
#51483=EDGE_CURVE('',#40408,#40410,#9138,.T.);
#51484=EDGE_CURVE('',#40407,#40409,#9139,.T.);
#51485=EDGE_CURVE('',#40410,#40405,#9140,.T.);
#51486=EDGE_CURVE('',#40409,#40406,#9141,.T.);
#51487=EDGE_CURVE('',#40411,#40412,#9142,.T.);
#51488=EDGE_CURVE('',#40413,#40412,#9143,.T.);
#51489=EDGE_CURVE('',#40414,#40413,#9144,.T.);
#51490=EDGE_CURVE('',#40414,#40411,#9145,.T.);
#51491=EDGE_CURVE('',#40415,#40416,#9146,.T.);
#51492=EDGE_CURVE('',#40412,#40416,#9147,.T.);
#51493=EDGE_CURVE('',#40411,#40415,#9148,.T.);
#51494=EDGE_CURVE('',#40417,#40418,#9149,.T.);
#51495=EDGE_CURVE('',#40416,#40418,#9150,.T.);
#51496=EDGE_CURVE('',#40415,#40417,#9151,.T.);
#51497=EDGE_CURVE('',#40418,#40413,#9152,.T.);
#51498=EDGE_CURVE('',#40417,#40414,#9153,.T.);
#51499=EDGE_CURVE('',#40419,#40420,#9154,.T.);
#51500=EDGE_CURVE('',#40421,#40420,#9155,.T.);
#51501=EDGE_CURVE('',#40422,#40421,#9156,.T.);
#51502=EDGE_CURVE('',#40422,#40419,#9157,.T.);
#51503=EDGE_CURVE('',#40423,#40424,#9158,.T.);
#51504=EDGE_CURVE('',#40420,#40424,#9159,.T.);
#51505=EDGE_CURVE('',#40419,#40423,#9160,.T.);
#51506=EDGE_CURVE('',#40425,#40426,#9161,.T.);
#51507=EDGE_CURVE('',#40424,#40426,#9162,.T.);
#51508=EDGE_CURVE('',#40423,#40425,#9163,.T.);
#51509=EDGE_CURVE('',#40426,#40421,#9164,.T.);
#51510=EDGE_CURVE('',#40425,#40422,#9165,.T.);
#51511=EDGE_CURVE('',#40427,#40428,#9166,.T.);
#51512=EDGE_CURVE('',#40429,#40428,#9167,.T.);
#51513=EDGE_CURVE('',#40430,#40429,#9168,.T.);
#51514=EDGE_CURVE('',#40430,#40427,#9169,.T.);
#51515=EDGE_CURVE('',#40431,#40432,#9170,.T.);
#51516=EDGE_CURVE('',#40428,#40432,#9171,.T.);
#51517=EDGE_CURVE('',#40427,#40431,#9172,.T.);
#51518=EDGE_CURVE('',#40433,#40434,#9173,.T.);
#51519=EDGE_CURVE('',#40432,#40434,#9174,.T.);
#51520=EDGE_CURVE('',#40431,#40433,#9175,.T.);
#51521=EDGE_CURVE('',#40434,#40429,#9176,.T.);
#51522=EDGE_CURVE('',#40433,#40430,#9177,.T.);
#51523=EDGE_CURVE('',#40435,#40436,#9178,.T.);
#51524=EDGE_CURVE('',#40437,#40436,#9179,.T.);
#51525=EDGE_CURVE('',#40438,#40437,#9180,.T.);
#51526=EDGE_CURVE('',#40438,#40435,#9181,.T.);
#51527=EDGE_CURVE('',#40439,#40440,#9182,.T.);
#51528=EDGE_CURVE('',#40436,#40440,#9183,.T.);
#51529=EDGE_CURVE('',#40435,#40439,#9184,.T.);
#51530=EDGE_CURVE('',#40441,#40442,#9185,.T.);
#51531=EDGE_CURVE('',#40440,#40442,#9186,.T.);
#51532=EDGE_CURVE('',#40439,#40441,#9187,.T.);
#51533=EDGE_CURVE('',#40442,#40437,#9188,.T.);
#51534=EDGE_CURVE('',#40441,#40438,#9189,.T.);
#51535=EDGE_CURVE('',#40443,#40444,#9190,.T.);
#51536=EDGE_CURVE('',#40445,#40444,#9191,.T.);
#51537=EDGE_CURVE('',#40446,#40445,#9192,.T.);
#51538=EDGE_CURVE('',#40446,#40443,#9193,.T.);
#51539=EDGE_CURVE('',#40447,#40448,#9194,.T.);
#51540=EDGE_CURVE('',#40444,#40448,#9195,.T.);
#51541=EDGE_CURVE('',#40443,#40447,#9196,.T.);
#51542=EDGE_CURVE('',#40449,#40450,#9197,.T.);
#51543=EDGE_CURVE('',#40448,#40450,#9198,.T.);
#51544=EDGE_CURVE('',#40447,#40449,#9199,.T.);
#51545=EDGE_CURVE('',#40450,#40445,#9200,.T.);
#51546=EDGE_CURVE('',#40449,#40446,#9201,.T.);
#51547=EDGE_CURVE('',#40451,#40452,#9202,.T.);
#51548=EDGE_CURVE('',#40453,#40452,#9203,.T.);
#51549=EDGE_CURVE('',#40454,#40453,#9204,.T.);
#51550=EDGE_CURVE('',#40454,#40451,#9205,.T.);
#51551=EDGE_CURVE('',#40455,#40456,#9206,.T.);
#51552=EDGE_CURVE('',#40452,#40456,#9207,.T.);
#51553=EDGE_CURVE('',#40451,#40455,#9208,.T.);
#51554=EDGE_CURVE('',#40457,#40458,#9209,.T.);
#51555=EDGE_CURVE('',#40456,#40458,#9210,.T.);
#51556=EDGE_CURVE('',#40455,#40457,#9211,.T.);
#51557=EDGE_CURVE('',#40458,#40453,#9212,.T.);
#51558=EDGE_CURVE('',#40457,#40454,#9213,.T.);
#51559=EDGE_CURVE('',#40459,#40460,#9214,.T.);
#51560=EDGE_CURVE('',#40461,#40460,#9215,.T.);
#51561=EDGE_CURVE('',#40462,#40461,#9216,.T.);
#51562=EDGE_CURVE('',#40462,#40459,#9217,.T.);
#51563=EDGE_CURVE('',#40463,#40464,#9218,.T.);
#51564=EDGE_CURVE('',#40460,#40464,#9219,.T.);
#51565=EDGE_CURVE('',#40459,#40463,#9220,.T.);
#51566=EDGE_CURVE('',#40465,#40466,#9221,.T.);
#51567=EDGE_CURVE('',#40464,#40466,#9222,.T.);
#51568=EDGE_CURVE('',#40463,#40465,#9223,.T.);
#51569=EDGE_CURVE('',#40466,#40461,#9224,.T.);
#51570=EDGE_CURVE('',#40465,#40462,#9225,.T.);
#51571=EDGE_CURVE('',#40467,#40468,#9226,.T.);
#51572=EDGE_CURVE('',#40469,#40468,#9227,.T.);
#51573=EDGE_CURVE('',#40470,#40469,#9228,.T.);
#51574=EDGE_CURVE('',#40470,#40467,#9229,.T.);
#51575=EDGE_CURVE('',#40471,#40472,#9230,.T.);
#51576=EDGE_CURVE('',#40468,#40472,#9231,.T.);
#51577=EDGE_CURVE('',#40467,#40471,#9232,.T.);
#51578=EDGE_CURVE('',#40473,#40474,#9233,.T.);
#51579=EDGE_CURVE('',#40472,#40474,#9234,.T.);
#51580=EDGE_CURVE('',#40471,#40473,#9235,.T.);
#51581=EDGE_CURVE('',#40474,#40469,#9236,.T.);
#51582=EDGE_CURVE('',#40473,#40470,#9237,.T.);
#51583=EDGE_CURVE('',#40475,#40476,#9238,.T.);
#51584=EDGE_CURVE('',#40477,#40476,#9239,.T.);
#51585=EDGE_CURVE('',#40478,#40477,#9240,.T.);
#51586=EDGE_CURVE('',#40478,#40475,#9241,.T.);
#51587=EDGE_CURVE('',#40479,#40480,#9242,.T.);
#51588=EDGE_CURVE('',#40476,#40480,#9243,.T.);
#51589=EDGE_CURVE('',#40475,#40479,#9244,.T.);
#51590=EDGE_CURVE('',#40481,#40482,#9245,.T.);
#51591=EDGE_CURVE('',#40480,#40482,#9246,.T.);
#51592=EDGE_CURVE('',#40479,#40481,#9247,.T.);
#51593=EDGE_CURVE('',#40482,#40477,#9248,.T.);
#51594=EDGE_CURVE('',#40481,#40478,#9249,.T.);
#51595=EDGE_CURVE('',#40483,#40484,#9250,.T.);
#51596=EDGE_CURVE('',#40485,#40484,#9251,.T.);
#51597=EDGE_CURVE('',#40486,#40485,#9252,.T.);
#51598=EDGE_CURVE('',#40486,#40483,#9253,.T.);
#51599=EDGE_CURVE('',#40487,#40488,#9254,.T.);
#51600=EDGE_CURVE('',#40484,#40488,#9255,.T.);
#51601=EDGE_CURVE('',#40483,#40487,#9256,.T.);
#51602=EDGE_CURVE('',#40489,#40490,#9257,.T.);
#51603=EDGE_CURVE('',#40488,#40490,#9258,.T.);
#51604=EDGE_CURVE('',#40487,#40489,#9259,.T.);
#51605=EDGE_CURVE('',#40490,#40485,#9260,.T.);
#51606=EDGE_CURVE('',#40489,#40486,#9261,.T.);
#51607=EDGE_CURVE('',#40491,#40492,#9262,.T.);
#51608=EDGE_CURVE('',#40493,#40492,#9263,.T.);
#51609=EDGE_CURVE('',#40494,#40493,#9264,.T.);
#51610=EDGE_CURVE('',#40494,#40491,#9265,.T.);
#51611=EDGE_CURVE('',#40495,#40496,#9266,.T.);
#51612=EDGE_CURVE('',#40492,#40496,#9267,.T.);
#51613=EDGE_CURVE('',#40491,#40495,#9268,.T.);
#51614=EDGE_CURVE('',#40497,#40498,#9269,.T.);
#51615=EDGE_CURVE('',#40496,#40498,#9270,.T.);
#51616=EDGE_CURVE('',#40495,#40497,#9271,.T.);
#51617=EDGE_CURVE('',#40498,#40493,#9272,.T.);
#51618=EDGE_CURVE('',#40497,#40494,#9273,.T.);
#51619=EDGE_CURVE('',#40499,#40500,#9274,.T.);
#51620=EDGE_CURVE('',#40501,#40500,#9275,.T.);
#51621=EDGE_CURVE('',#40502,#40501,#9276,.T.);
#51622=EDGE_CURVE('',#40502,#40499,#9277,.T.);
#51623=EDGE_CURVE('',#40503,#40504,#9278,.T.);
#51624=EDGE_CURVE('',#40500,#40504,#9279,.T.);
#51625=EDGE_CURVE('',#40499,#40503,#9280,.T.);
#51626=EDGE_CURVE('',#40505,#40506,#9281,.T.);
#51627=EDGE_CURVE('',#40504,#40506,#9282,.T.);
#51628=EDGE_CURVE('',#40503,#40505,#9283,.T.);
#51629=EDGE_CURVE('',#40506,#40501,#9284,.T.);
#51630=EDGE_CURVE('',#40505,#40502,#9285,.T.);
#51631=EDGE_CURVE('',#40507,#40508,#9286,.T.);
#51632=EDGE_CURVE('',#40509,#40508,#9287,.T.);
#51633=EDGE_CURVE('',#40510,#40509,#9288,.T.);
#51634=EDGE_CURVE('',#40510,#40507,#9289,.T.);
#51635=EDGE_CURVE('',#40511,#40512,#9290,.T.);
#51636=EDGE_CURVE('',#40508,#40512,#9291,.T.);
#51637=EDGE_CURVE('',#40507,#40511,#9292,.T.);
#51638=EDGE_CURVE('',#40513,#40514,#9293,.T.);
#51639=EDGE_CURVE('',#40512,#40514,#9294,.T.);
#51640=EDGE_CURVE('',#40511,#40513,#9295,.T.);
#51641=EDGE_CURVE('',#40514,#40509,#9296,.T.);
#51642=EDGE_CURVE('',#40513,#40510,#9297,.T.);
#51643=EDGE_CURVE('',#40515,#40516,#9298,.T.);
#51644=EDGE_CURVE('',#40517,#40516,#9299,.T.);
#51645=EDGE_CURVE('',#40518,#40517,#9300,.T.);
#51646=EDGE_CURVE('',#40518,#40515,#9301,.T.);
#51647=EDGE_CURVE('',#40519,#40520,#9302,.T.);
#51648=EDGE_CURVE('',#40516,#40520,#9303,.T.);
#51649=EDGE_CURVE('',#40515,#40519,#9304,.T.);
#51650=EDGE_CURVE('',#40521,#40522,#9305,.T.);
#51651=EDGE_CURVE('',#40520,#40522,#9306,.T.);
#51652=EDGE_CURVE('',#40519,#40521,#9307,.T.);
#51653=EDGE_CURVE('',#40522,#40517,#9308,.T.);
#51654=EDGE_CURVE('',#40521,#40518,#9309,.T.);
#51655=EDGE_CURVE('',#40523,#40524,#9310,.T.);
#51656=EDGE_CURVE('',#40525,#40524,#9311,.T.);
#51657=EDGE_CURVE('',#40526,#40525,#9312,.T.);
#51658=EDGE_CURVE('',#40526,#40523,#9313,.T.);
#51659=EDGE_CURVE('',#40527,#40528,#9314,.T.);
#51660=EDGE_CURVE('',#40524,#40528,#9315,.T.);
#51661=EDGE_CURVE('',#40523,#40527,#9316,.T.);
#51662=EDGE_CURVE('',#40529,#40530,#9317,.T.);
#51663=EDGE_CURVE('',#40528,#40530,#9318,.T.);
#51664=EDGE_CURVE('',#40527,#40529,#9319,.T.);
#51665=EDGE_CURVE('',#40530,#40525,#9320,.T.);
#51666=EDGE_CURVE('',#40529,#40526,#9321,.T.);
#51667=EDGE_CURVE('',#40531,#40532,#9322,.T.);
#51668=EDGE_CURVE('',#40533,#40532,#9323,.T.);
#51669=EDGE_CURVE('',#40534,#40533,#9324,.T.);
#51670=EDGE_CURVE('',#40534,#40531,#9325,.T.);
#51671=EDGE_CURVE('',#40535,#40536,#9326,.T.);
#51672=EDGE_CURVE('',#40532,#40536,#9327,.T.);
#51673=EDGE_CURVE('',#40531,#40535,#9328,.T.);
#51674=EDGE_CURVE('',#40537,#40538,#9329,.T.);
#51675=EDGE_CURVE('',#40536,#40538,#9330,.T.);
#51676=EDGE_CURVE('',#40535,#40537,#9331,.T.);
#51677=EDGE_CURVE('',#40538,#40533,#9332,.T.);
#51678=EDGE_CURVE('',#40537,#40534,#9333,.T.);
#51679=EDGE_CURVE('',#40539,#40540,#9334,.T.);
#51680=EDGE_CURVE('',#40541,#40540,#9335,.T.);
#51681=EDGE_CURVE('',#40542,#40541,#9336,.T.);
#51682=EDGE_CURVE('',#40542,#40539,#9337,.T.);
#51683=EDGE_CURVE('',#40543,#40544,#9338,.T.);
#51684=EDGE_CURVE('',#40540,#40544,#9339,.T.);
#51685=EDGE_CURVE('',#40539,#40543,#9340,.T.);
#51686=EDGE_CURVE('',#40545,#40546,#9341,.T.);
#51687=EDGE_CURVE('',#40544,#40546,#9342,.T.);
#51688=EDGE_CURVE('',#40543,#40545,#9343,.T.);
#51689=EDGE_CURVE('',#40546,#40541,#9344,.T.);
#51690=EDGE_CURVE('',#40545,#40542,#9345,.T.);
#51691=EDGE_CURVE('',#40547,#40548,#9346,.T.);
#51692=EDGE_CURVE('',#40549,#40548,#9347,.T.);
#51693=EDGE_CURVE('',#40550,#40549,#9348,.T.);
#51694=EDGE_CURVE('',#40550,#40547,#9349,.T.);
#51695=EDGE_CURVE('',#40551,#40552,#9350,.T.);
#51696=EDGE_CURVE('',#40548,#40552,#9351,.T.);
#51697=EDGE_CURVE('',#40547,#40551,#9352,.T.);
#51698=EDGE_CURVE('',#40553,#40554,#9353,.T.);
#51699=EDGE_CURVE('',#40552,#40554,#9354,.T.);
#51700=EDGE_CURVE('',#40551,#40553,#9355,.T.);
#51701=EDGE_CURVE('',#40554,#40549,#9356,.T.);
#51702=EDGE_CURVE('',#40553,#40550,#9357,.T.);
#51703=EDGE_CURVE('',#40555,#40556,#9358,.T.);
#51704=EDGE_CURVE('',#40557,#40556,#9359,.T.);
#51705=EDGE_CURVE('',#40558,#40557,#9360,.T.);
#51706=EDGE_CURVE('',#40558,#40555,#9361,.T.);
#51707=EDGE_CURVE('',#40559,#40560,#9362,.T.);
#51708=EDGE_CURVE('',#40556,#40560,#9363,.T.);
#51709=EDGE_CURVE('',#40555,#40559,#9364,.T.);
#51710=EDGE_CURVE('',#40561,#40562,#9365,.T.);
#51711=EDGE_CURVE('',#40560,#40562,#9366,.T.);
#51712=EDGE_CURVE('',#40559,#40561,#9367,.T.);
#51713=EDGE_CURVE('',#40562,#40557,#9368,.T.);
#51714=EDGE_CURVE('',#40561,#40558,#9369,.T.);
#51715=EDGE_CURVE('',#40563,#40564,#9370,.T.);
#51716=EDGE_CURVE('',#40565,#40564,#9371,.T.);
#51717=EDGE_CURVE('',#40566,#40565,#9372,.T.);
#51718=EDGE_CURVE('',#40566,#40563,#9373,.T.);
#51719=EDGE_CURVE('',#40567,#40568,#9374,.T.);
#51720=EDGE_CURVE('',#40564,#40568,#9375,.T.);
#51721=EDGE_CURVE('',#40563,#40567,#9376,.T.);
#51722=EDGE_CURVE('',#40569,#40570,#9377,.T.);
#51723=EDGE_CURVE('',#40568,#40570,#9378,.T.);
#51724=EDGE_CURVE('',#40567,#40569,#9379,.T.);
#51725=EDGE_CURVE('',#40570,#40565,#9380,.T.);
#51726=EDGE_CURVE('',#40569,#40566,#9381,.T.);
#51727=EDGE_CURVE('',#40571,#40572,#9382,.T.);
#51728=EDGE_CURVE('',#40573,#40572,#9383,.T.);
#51729=EDGE_CURVE('',#40574,#40573,#9384,.T.);
#51730=EDGE_CURVE('',#40574,#40571,#9385,.T.);
#51731=EDGE_CURVE('',#40575,#40576,#9386,.T.);
#51732=EDGE_CURVE('',#40572,#40576,#9387,.T.);
#51733=EDGE_CURVE('',#40571,#40575,#9388,.T.);
#51734=EDGE_CURVE('',#40577,#40578,#9389,.T.);
#51735=EDGE_CURVE('',#40576,#40578,#9390,.T.);
#51736=EDGE_CURVE('',#40575,#40577,#9391,.T.);
#51737=EDGE_CURVE('',#40578,#40573,#9392,.T.);
#51738=EDGE_CURVE('',#40577,#40574,#9393,.T.);
#51739=EDGE_CURVE('',#40579,#40580,#9394,.T.);
#51740=EDGE_CURVE('',#40581,#40580,#9395,.T.);
#51741=EDGE_CURVE('',#40582,#40581,#9396,.T.);
#51742=EDGE_CURVE('',#40582,#40579,#9397,.T.);
#51743=EDGE_CURVE('',#40583,#40584,#9398,.T.);
#51744=EDGE_CURVE('',#40580,#40584,#9399,.T.);
#51745=EDGE_CURVE('',#40579,#40583,#9400,.T.);
#51746=EDGE_CURVE('',#40585,#40586,#9401,.T.);
#51747=EDGE_CURVE('',#40584,#40586,#9402,.T.);
#51748=EDGE_CURVE('',#40583,#40585,#9403,.T.);
#51749=EDGE_CURVE('',#40586,#40581,#9404,.T.);
#51750=EDGE_CURVE('',#40585,#40582,#9405,.T.);
#51751=EDGE_CURVE('',#40587,#40588,#9406,.T.);
#51752=EDGE_CURVE('',#40589,#40588,#9407,.T.);
#51753=EDGE_CURVE('',#40590,#40589,#9408,.T.);
#51754=EDGE_CURVE('',#40590,#40587,#9409,.T.);
#51755=EDGE_CURVE('',#40591,#40592,#9410,.T.);
#51756=EDGE_CURVE('',#40588,#40592,#9411,.T.);
#51757=EDGE_CURVE('',#40587,#40591,#9412,.T.);
#51758=EDGE_CURVE('',#40593,#40594,#9413,.T.);
#51759=EDGE_CURVE('',#40592,#40594,#9414,.T.);
#51760=EDGE_CURVE('',#40591,#40593,#9415,.T.);
#51761=EDGE_CURVE('',#40594,#40589,#9416,.T.);
#51762=EDGE_CURVE('',#40593,#40590,#9417,.T.);
#51763=EDGE_CURVE('',#40595,#40596,#9418,.T.);
#51764=EDGE_CURVE('',#40597,#40596,#9419,.T.);
#51765=EDGE_CURVE('',#40598,#40597,#9420,.T.);
#51766=EDGE_CURVE('',#40598,#40595,#9421,.T.);
#51767=EDGE_CURVE('',#40599,#40600,#9422,.T.);
#51768=EDGE_CURVE('',#40596,#40600,#9423,.T.);
#51769=EDGE_CURVE('',#40595,#40599,#9424,.T.);
#51770=EDGE_CURVE('',#40601,#40602,#9425,.T.);
#51771=EDGE_CURVE('',#40600,#40602,#9426,.T.);
#51772=EDGE_CURVE('',#40599,#40601,#9427,.T.);
#51773=EDGE_CURVE('',#40602,#40597,#9428,.T.);
#51774=EDGE_CURVE('',#40601,#40598,#9429,.T.);
#51775=EDGE_CURVE('',#40603,#40604,#9430,.T.);
#51776=EDGE_CURVE('',#40605,#40604,#9431,.T.);
#51777=EDGE_CURVE('',#40606,#40605,#9432,.T.);
#51778=EDGE_CURVE('',#40606,#40603,#9433,.T.);
#51779=EDGE_CURVE('',#40607,#40608,#9434,.T.);
#51780=EDGE_CURVE('',#40604,#40608,#9435,.T.);
#51781=EDGE_CURVE('',#40603,#40607,#9436,.T.);
#51782=EDGE_CURVE('',#40609,#40610,#9437,.T.);
#51783=EDGE_CURVE('',#40608,#40610,#9438,.T.);
#51784=EDGE_CURVE('',#40607,#40609,#9439,.T.);
#51785=EDGE_CURVE('',#40610,#40605,#9440,.T.);
#51786=EDGE_CURVE('',#40609,#40606,#9441,.T.);
#51787=EDGE_CURVE('',#40611,#40612,#9442,.T.);
#51788=EDGE_CURVE('',#40613,#40612,#9443,.T.);
#51789=EDGE_CURVE('',#40614,#40613,#9444,.T.);
#51790=EDGE_CURVE('',#40614,#40611,#9445,.T.);
#51791=EDGE_CURVE('',#40615,#40616,#9446,.T.);
#51792=EDGE_CURVE('',#40612,#40616,#9447,.T.);
#51793=EDGE_CURVE('',#40611,#40615,#9448,.T.);
#51794=EDGE_CURVE('',#40617,#40618,#9449,.T.);
#51795=EDGE_CURVE('',#40616,#40618,#9450,.T.);
#51796=EDGE_CURVE('',#40615,#40617,#9451,.T.);
#51797=EDGE_CURVE('',#40618,#40613,#9452,.T.);
#51798=EDGE_CURVE('',#40617,#40614,#9453,.T.);
#51799=EDGE_CURVE('',#40619,#40620,#9454,.T.);
#51800=EDGE_CURVE('',#40621,#40620,#9455,.T.);
#51801=EDGE_CURVE('',#40622,#40621,#9456,.T.);
#51802=EDGE_CURVE('',#40622,#40619,#9457,.T.);
#51803=EDGE_CURVE('',#40623,#40624,#9458,.T.);
#51804=EDGE_CURVE('',#40620,#40624,#9459,.T.);
#51805=EDGE_CURVE('',#40619,#40623,#9460,.T.);
#51806=EDGE_CURVE('',#40625,#40626,#9461,.T.);
#51807=EDGE_CURVE('',#40624,#40626,#9462,.T.);
#51808=EDGE_CURVE('',#40623,#40625,#9463,.T.);
#51809=EDGE_CURVE('',#40626,#40621,#9464,.T.);
#51810=EDGE_CURVE('',#40625,#40622,#9465,.T.);
#51811=EDGE_CURVE('',#40627,#40628,#9466,.T.);
#51812=EDGE_CURVE('',#40629,#40628,#9467,.T.);
#51813=EDGE_CURVE('',#40630,#40629,#9468,.T.);
#51814=EDGE_CURVE('',#40630,#40627,#9469,.T.);
#51815=EDGE_CURVE('',#40631,#40632,#9470,.T.);
#51816=EDGE_CURVE('',#40628,#40632,#9471,.T.);
#51817=EDGE_CURVE('',#40627,#40631,#9472,.T.);
#51818=EDGE_CURVE('',#40633,#40634,#9473,.T.);
#51819=EDGE_CURVE('',#40632,#40634,#9474,.T.);
#51820=EDGE_CURVE('',#40631,#40633,#9475,.T.);
#51821=EDGE_CURVE('',#40634,#40629,#9476,.T.);
#51822=EDGE_CURVE('',#40633,#40630,#9477,.T.);
#51823=EDGE_CURVE('',#40635,#40636,#9478,.T.);
#51824=EDGE_CURVE('',#40637,#40636,#9479,.T.);
#51825=EDGE_CURVE('',#40638,#40637,#9480,.T.);
#51826=EDGE_CURVE('',#40638,#40635,#9481,.T.);
#51827=EDGE_CURVE('',#40639,#40640,#9482,.T.);
#51828=EDGE_CURVE('',#40636,#40640,#9483,.T.);
#51829=EDGE_CURVE('',#40635,#40639,#9484,.T.);
#51830=EDGE_CURVE('',#40641,#40642,#9485,.T.);
#51831=EDGE_CURVE('',#40640,#40642,#9486,.T.);
#51832=EDGE_CURVE('',#40639,#40641,#9487,.T.);
#51833=EDGE_CURVE('',#40642,#40637,#9488,.T.);
#51834=EDGE_CURVE('',#40641,#40638,#9489,.T.);
#51835=EDGE_CURVE('',#40643,#40644,#9490,.T.);
#51836=EDGE_CURVE('',#40645,#40644,#9491,.T.);
#51837=EDGE_CURVE('',#40646,#40645,#9492,.T.);
#51838=EDGE_CURVE('',#40646,#40643,#9493,.T.);
#51839=EDGE_CURVE('',#40647,#40648,#9494,.T.);
#51840=EDGE_CURVE('',#40644,#40648,#9495,.T.);
#51841=EDGE_CURVE('',#40643,#40647,#9496,.T.);
#51842=EDGE_CURVE('',#40649,#40650,#9497,.T.);
#51843=EDGE_CURVE('',#40648,#40650,#9498,.T.);
#51844=EDGE_CURVE('',#40647,#40649,#9499,.T.);
#51845=EDGE_CURVE('',#40650,#40645,#9500,.T.);
#51846=EDGE_CURVE('',#40649,#40646,#9501,.T.);
#51847=EDGE_CURVE('',#40651,#40652,#9502,.T.);
#51848=EDGE_CURVE('',#40653,#40652,#9503,.T.);
#51849=EDGE_CURVE('',#40654,#40653,#9504,.T.);
#51850=EDGE_CURVE('',#40654,#40651,#9505,.T.);
#51851=EDGE_CURVE('',#40655,#40656,#9506,.T.);
#51852=EDGE_CURVE('',#40652,#40656,#9507,.T.);
#51853=EDGE_CURVE('',#40651,#40655,#9508,.T.);
#51854=EDGE_CURVE('',#40657,#40658,#9509,.T.);
#51855=EDGE_CURVE('',#40656,#40658,#9510,.T.);
#51856=EDGE_CURVE('',#40655,#40657,#9511,.T.);
#51857=EDGE_CURVE('',#40658,#40653,#9512,.T.);
#51858=EDGE_CURVE('',#40657,#40654,#9513,.T.);
#51859=EDGE_CURVE('',#40659,#40660,#9514,.T.);
#51860=EDGE_CURVE('',#40661,#40660,#9515,.T.);
#51861=EDGE_CURVE('',#40662,#40661,#9516,.T.);
#51862=EDGE_CURVE('',#40662,#40659,#9517,.T.);
#51863=EDGE_CURVE('',#40663,#40664,#9518,.T.);
#51864=EDGE_CURVE('',#40660,#40664,#9519,.T.);
#51865=EDGE_CURVE('',#40659,#40663,#9520,.T.);
#51866=EDGE_CURVE('',#40665,#40666,#9521,.T.);
#51867=EDGE_CURVE('',#40664,#40666,#9522,.T.);
#51868=EDGE_CURVE('',#40663,#40665,#9523,.T.);
#51869=EDGE_CURVE('',#40666,#40661,#9524,.T.);
#51870=EDGE_CURVE('',#40665,#40662,#9525,.T.);
#51871=EDGE_CURVE('',#40667,#40668,#9526,.T.);
#51872=EDGE_CURVE('',#40669,#40668,#9527,.T.);
#51873=EDGE_CURVE('',#40670,#40669,#9528,.T.);
#51874=EDGE_CURVE('',#40670,#40667,#9529,.T.);
#51875=EDGE_CURVE('',#40671,#40672,#9530,.T.);
#51876=EDGE_CURVE('',#40668,#40672,#9531,.T.);
#51877=EDGE_CURVE('',#40667,#40671,#9532,.T.);
#51878=EDGE_CURVE('',#40673,#40674,#9533,.T.);
#51879=EDGE_CURVE('',#40672,#40674,#9534,.T.);
#51880=EDGE_CURVE('',#40671,#40673,#9535,.T.);
#51881=EDGE_CURVE('',#40674,#40669,#9536,.T.);
#51882=EDGE_CURVE('',#40673,#40670,#9537,.T.);
#51883=EDGE_CURVE('',#40675,#40676,#9538,.T.);
#51884=EDGE_CURVE('',#40677,#40676,#9539,.T.);
#51885=EDGE_CURVE('',#40678,#40677,#9540,.T.);
#51886=EDGE_CURVE('',#40678,#40675,#9541,.T.);
#51887=EDGE_CURVE('',#40679,#40680,#9542,.T.);
#51888=EDGE_CURVE('',#40676,#40680,#9543,.T.);
#51889=EDGE_CURVE('',#40675,#40679,#9544,.T.);
#51890=EDGE_CURVE('',#40681,#40682,#9545,.T.);
#51891=EDGE_CURVE('',#40680,#40682,#9546,.T.);
#51892=EDGE_CURVE('',#40679,#40681,#9547,.T.);
#51893=EDGE_CURVE('',#40682,#40677,#9548,.T.);
#51894=EDGE_CURVE('',#40681,#40678,#9549,.T.);
#51895=EDGE_CURVE('',#40683,#40684,#9550,.T.);
#51896=EDGE_CURVE('',#40685,#40684,#9551,.T.);
#51897=EDGE_CURVE('',#40686,#40685,#9552,.T.);
#51898=EDGE_CURVE('',#40686,#40683,#9553,.T.);
#51899=EDGE_CURVE('',#40687,#40688,#9554,.T.);
#51900=EDGE_CURVE('',#40684,#40688,#9555,.T.);
#51901=EDGE_CURVE('',#40683,#40687,#9556,.T.);
#51902=EDGE_CURVE('',#40689,#40690,#9557,.T.);
#51903=EDGE_CURVE('',#40688,#40690,#9558,.T.);
#51904=EDGE_CURVE('',#40687,#40689,#9559,.T.);
#51905=EDGE_CURVE('',#40690,#40685,#9560,.T.);
#51906=EDGE_CURVE('',#40689,#40686,#9561,.T.);
#51907=EDGE_CURVE('',#40691,#40692,#9562,.T.);
#51908=EDGE_CURVE('',#40693,#40692,#9563,.T.);
#51909=EDGE_CURVE('',#40694,#40693,#9564,.T.);
#51910=EDGE_CURVE('',#40694,#40691,#9565,.T.);
#51911=EDGE_CURVE('',#40695,#40696,#9566,.T.);
#51912=EDGE_CURVE('',#40692,#40696,#9567,.T.);
#51913=EDGE_CURVE('',#40691,#40695,#9568,.T.);
#51914=EDGE_CURVE('',#40697,#40698,#9569,.T.);
#51915=EDGE_CURVE('',#40696,#40698,#9570,.T.);
#51916=EDGE_CURVE('',#40695,#40697,#9571,.T.);
#51917=EDGE_CURVE('',#40698,#40693,#9572,.T.);
#51918=EDGE_CURVE('',#40697,#40694,#9573,.T.);
#51919=EDGE_CURVE('',#40699,#40700,#9574,.T.);
#51920=EDGE_CURVE('',#40701,#40700,#9575,.T.);
#51921=EDGE_CURVE('',#40702,#40701,#9576,.T.);
#51922=EDGE_CURVE('',#40702,#40699,#9577,.T.);
#51923=EDGE_CURVE('',#40703,#40704,#9578,.T.);
#51924=EDGE_CURVE('',#40700,#40704,#9579,.T.);
#51925=EDGE_CURVE('',#40699,#40703,#9580,.T.);
#51926=EDGE_CURVE('',#40705,#40706,#9581,.T.);
#51927=EDGE_CURVE('',#40704,#40706,#9582,.T.);
#51928=EDGE_CURVE('',#40703,#40705,#9583,.T.);
#51929=EDGE_CURVE('',#40706,#40701,#9584,.T.);
#51930=EDGE_CURVE('',#40705,#40702,#9585,.T.);
#51931=EDGE_CURVE('',#40707,#40708,#9586,.T.);
#51932=EDGE_CURVE('',#40709,#40708,#9587,.T.);
#51933=EDGE_CURVE('',#40710,#40709,#9588,.T.);
#51934=EDGE_CURVE('',#40710,#40707,#9589,.T.);
#51935=EDGE_CURVE('',#40711,#40712,#9590,.T.);
#51936=EDGE_CURVE('',#40708,#40712,#9591,.T.);
#51937=EDGE_CURVE('',#40707,#40711,#9592,.T.);
#51938=EDGE_CURVE('',#40713,#40714,#9593,.T.);
#51939=EDGE_CURVE('',#40712,#40714,#9594,.T.);
#51940=EDGE_CURVE('',#40711,#40713,#9595,.T.);
#51941=EDGE_CURVE('',#40714,#40709,#9596,.T.);
#51942=EDGE_CURVE('',#40713,#40710,#9597,.T.);
#51943=EDGE_CURVE('',#40715,#40716,#9598,.T.);
#51944=EDGE_CURVE('',#40717,#40716,#9599,.T.);
#51945=EDGE_CURVE('',#40718,#40717,#9600,.T.);
#51946=EDGE_CURVE('',#40718,#40715,#9601,.T.);
#51947=EDGE_CURVE('',#40719,#40720,#9602,.T.);
#51948=EDGE_CURVE('',#40716,#40720,#9603,.T.);
#51949=EDGE_CURVE('',#40715,#40719,#9604,.T.);
#51950=EDGE_CURVE('',#40721,#40722,#9605,.T.);
#51951=EDGE_CURVE('',#40720,#40722,#9606,.T.);
#51952=EDGE_CURVE('',#40719,#40721,#9607,.T.);
#51953=EDGE_CURVE('',#40722,#40717,#9608,.T.);
#51954=EDGE_CURVE('',#40721,#40718,#9609,.T.);
#51955=EDGE_CURVE('',#40723,#40724,#9610,.T.);
#51956=EDGE_CURVE('',#40725,#40724,#9611,.T.);
#51957=EDGE_CURVE('',#40726,#40725,#9612,.T.);
#51958=EDGE_CURVE('',#40726,#40723,#9613,.T.);
#51959=EDGE_CURVE('',#40727,#40728,#9614,.T.);
#51960=EDGE_CURVE('',#40724,#40728,#9615,.T.);
#51961=EDGE_CURVE('',#40723,#40727,#9616,.T.);
#51962=EDGE_CURVE('',#40729,#40730,#9617,.T.);
#51963=EDGE_CURVE('',#40728,#40730,#9618,.T.);
#51964=EDGE_CURVE('',#40727,#40729,#9619,.T.);
#51965=EDGE_CURVE('',#40730,#40725,#9620,.T.);
#51966=EDGE_CURVE('',#40729,#40726,#9621,.T.);
#51967=EDGE_CURVE('',#40731,#40732,#9622,.T.);
#51968=EDGE_CURVE('',#40732,#40733,#9623,.T.);
#51969=EDGE_CURVE('',#40733,#40734,#9624,.T.);
#51970=EDGE_CURVE('',#40734,#40731,#9625,.T.);
#51971=EDGE_CURVE('',#40735,#40732,#9626,.T.);
#51972=EDGE_CURVE('',#40736,#40731,#9627,.T.);
#51973=EDGE_CURVE('',#40736,#40735,#9628,.T.);
#51974=EDGE_CURVE('',#40737,#40733,#9629,.T.);
#51975=EDGE_CURVE('',#40735,#40737,#9630,.T.);
#51976=EDGE_CURVE('',#40738,#40734,#9631,.T.);
#51977=EDGE_CURVE('',#40737,#40738,#9632,.T.);
#51978=EDGE_CURVE('',#40738,#40736,#9633,.T.);
#51979=EDGE_CURVE('',#35058,#35080,#9634,.T.);
#51980=EDGE_CURVE('',#35077,#35064,#9635,.T.);
#51981=EDGE_CURVE('',#35060,#35079,#9636,.T.);
#51982=EDGE_CURVE('',#35078,#35061,#9637,.T.);
#51983=EDGE_CURVE('',#35082,#35066,#9638,.T.);
#51984=EDGE_CURVE('',#35053,#35074,#9639,.T.);
#51985=EDGE_CURVE('',#35081,#35065,#9640,.T.);
#51986=EDGE_CURVE('',#35054,#35073,#9641,.T.);
#51987=EDGE_CURVE('',#40739,#40739,#33514,.T.);
#51988=EDGE_CURVE('',#40740,#40741,#33515,.T.);
#51989=EDGE_CURVE('',#40742,#40740,#33516,.T.);
#51990=EDGE_CURVE('',#40743,#40742,#33517,.T.);
#51991=EDGE_CURVE('',#40741,#40743,#33518,.T.);
#51992=EDGE_CURVE('',#40740,#40744,#9642,.T.);
#51993=EDGE_CURVE('',#40741,#40745,#9643,.T.);
#51994=EDGE_CURVE('',#40744,#40745,#33519,.T.);
#51995=EDGE_CURVE('',#40742,#40746,#9644,.T.);
#51996=EDGE_CURVE('',#40746,#40744,#33520,.T.);
#51997=EDGE_CURVE('',#40743,#40747,#9645,.T.);
#51998=EDGE_CURVE('',#40747,#40746,#33521,.T.);
#51999=EDGE_CURVE('',#40745,#40747,#33522,.T.);
#52000=EDGE_CURVE('',#40748,#40748,#33523,.T.);
#52001=EDGE_CURVE('',#40749,#40750,#9646,.T.);
#52002=EDGE_CURVE('',#40749,#40751,#30340,.F.);
#52003=EDGE_CURVE('',#40751,#40752,#9647,.T.);
#52004=EDGE_CURVE('',#40752,#40753,#33524,.T.);
#52005=EDGE_CURVE('',#40753,#40752,#33525,.T.);
#52006=EDGE_CURVE('',#40751,#40754,#30341,.F.);
#52007=EDGE_CURVE('',#40754,#40755,#30342,.T.);
#52008=EDGE_CURVE('',#40755,#40756,#30343,.T.);
#52009=EDGE_CURVE('',#40756,#40757,#9648,.T.);
#52010=EDGE_CURVE('',#40757,#40758,#30344,.T.);
#52011=EDGE_CURVE('',#40758,#40759,#30345,.T.);
#52012=EDGE_CURVE('',#40759,#40750,#30346,.F.);
#52013=EDGE_CURVE('',#40760,#40761,#9649,.T.);
#52014=EDGE_CURVE('',#40760,#40749,#30347,.F.);
#52015=EDGE_CURVE('',#40750,#40761,#30348,.F.);
#52016=EDGE_CURVE('',#40762,#40763,#9650,.T.);
#52017=EDGE_CURVE('',#40762,#40760,#30349,.F.);
#52018=EDGE_CURVE('',#40761,#40763,#30350,.F.);
#52019=EDGE_CURVE('',#40764,#40765,#9651,.T.);
#52020=EDGE_CURVE('',#40764,#40766,#30351,.F.);
#52021=EDGE_CURVE('',#40766,#40762,#30352,.F.);
#52022=EDGE_CURVE('',#40763,#40765,#30353,.F.);
#52023=EDGE_CURVE('',#40767,#40768,#9652,.T.);
#52024=EDGE_CURVE('',#40767,#40764,#30354,.F.);
#52025=EDGE_CURVE('',#40765,#40769,#30355,.F.);
#52026=EDGE_CURVE('',#40769,#40768,#30356,.F.);
#52027=EDGE_CURVE('',#40770,#40771,#9653,.T.);
#52028=EDGE_CURVE('',#40770,#40767,#30357,.F.);
#52029=EDGE_CURVE('',#40768,#40771,#30358,.F.);
#52030=EDGE_CURVE('',#40772,#40773,#9654,.T.);
#52031=EDGE_CURVE('',#40772,#40770,#30359,.F.);
#52032=EDGE_CURVE('',#40771,#40773,#30360,.F.);
#52033=EDGE_CURVE('',#40774,#40775,#9655,.T.);
#52034=EDGE_CURVE('',#40774,#40776,#30361,.T.);
#52035=EDGE_CURVE('',#40776,#40772,#30362,.F.);
#52036=EDGE_CURVE('',#40773,#40775,#30363,.F.);
#52037=EDGE_CURVE('',#40777,#40778,#9656,.T.);
#52038=EDGE_CURVE('',#40777,#40779,#30364,.T.);
#52039=EDGE_CURVE('',#40778,#40779,#33526,.T.);
#52040=EDGE_CURVE('',#40780,#40781,#9657,.T.);
#52041=EDGE_CURVE('',#40780,#40777,#30365,.T.);
#52042=EDGE_CURVE('',#40782,#40778,#33527,.T.);
#52043=EDGE_CURVE('',#40782,#40783,#30366,.T.);
#52044=EDGE_CURVE('',#40783,#40784,#30367,.T.);
#52045=EDGE_CURVE('',#40784,#40781,#30368,.F.);
#52046=EDGE_CURVE('',#40785,#40786,#9658,.T.);
#52047=EDGE_CURVE('',#40785,#40787,#30369,.T.);
#52048=EDGE_CURVE('',#40787,#40780,#30370,.T.);
#52049=EDGE_CURVE('',#40781,#40786,#30371,.F.);
#52050=EDGE_CURVE('',#40788,#40789,#9659,.T.);
#52051=EDGE_CURVE('',#40788,#40785,#30372,.T.);
#52052=EDGE_CURVE('',#40786,#40790,#30373,.F.);
#52053=EDGE_CURVE('',#40790,#40789,#30374,.F.);
#52054=EDGE_CURVE('',#40791,#40792,#9660,.T.);
#52055=EDGE_CURVE('',#40791,#40788,#30375,.T.);
#52056=EDGE_CURVE('',#40789,#40792,#30376,.F.);
#52057=EDGE_CURVE('',#40793,#40794,#9661,.T.);
#52058=EDGE_CURVE('',#40793,#40795,#30377,.F.);
#52059=EDGE_CURVE('',#40795,#40791,#30378,.T.);
#52060=EDGE_CURVE('',#40792,#40794,#30379,.F.);
#52061=EDGE_CURVE('',#40796,#40797,#9662,.T.);
#52062=EDGE_CURVE('',#40796,#40793,#30380,.F.);
#52063=EDGE_CURVE('',#40794,#40798,#30381,.F.);
#52064=EDGE_CURVE('',#40798,#40797,#30382,.F.);
#52065=EDGE_CURVE('',#40799,#40800,#9663,.T.);
#52066=EDGE_CURVE('',#40799,#40796,#30383,.F.);
#52067=EDGE_CURVE('',#40797,#40800,#30384,.F.);
#52068=EDGE_CURVE('',#40801,#40802,#33528,.T.);
#52069=EDGE_CURVE('',#40802,#40801,#33529,.T.);
#52070=EDGE_CURVE('',#40801,#40803,#9664,.T.);
#52071=EDGE_CURVE('',#40803,#40804,#30385,.T.);
#52072=EDGE_CURVE('',#40805,#40804,#9665,.T.);
#52073=EDGE_CURVE('',#40805,#40806,#30386,.T.);
#52074=EDGE_CURVE('',#40806,#40807,#9666,.T.);
#52075=EDGE_CURVE('',#40807,#40808,#30387,.F.);
#52076=EDGE_CURVE('',#40808,#40803,#30388,.T.);
#52077=EDGE_CURVE('',#40778,#40809,#9667,.T.);
#52078=EDGE_CURVE('',#40810,#40779,#30389,.T.);
#52079=EDGE_CURVE('',#40811,#40810,#30390,.F.);
#52080=EDGE_CURVE('',#40812,#40811,#33530,.T.);
#52081=EDGE_CURVE('',#40812,#40809,#30391,.T.);
#52082=EDGE_CURVE('',#40813,#40814,#9668,.T.);
#52083=EDGE_CURVE('',#40815,#40813,#30392,.F.);
#52084=EDGE_CURVE('',#40816,#40815,#30393,.T.);
#52085=EDGE_CURVE('',#40817,#40816,#9669,.T.);
#52086=EDGE_CURVE('',#40817,#40814,#30394,.T.);
#52087=EDGE_CURVE('',#40814,#40818,#30395,.T.);
#52088=EDGE_CURVE('',#40819,#40818,#9670,.T.);
#52089=EDGE_CURVE('',#40813,#40819,#30396,.F.);
#52090=EDGE_CURVE('',#40820,#40821,#9671,.T.);
#52091=EDGE_CURVE('',#40819,#40820,#30397,.F.);
#52092=EDGE_CURVE('',#40818,#40821,#30398,.T.);
#52093=EDGE_CURVE('',#40822,#40823,#9672,.T.);
#52094=EDGE_CURVE('',#40820,#40822,#30399,.F.);
#52095=EDGE_CURVE('',#40821,#40823,#30400,.T.);
#52096=EDGE_CURVE('',#40824,#40825,#9673,.T.);
#52097=EDGE_CURVE('',#40826,#40824,#30401,.F.);
#52098=EDGE_CURVE('',#40827,#40826,#30402,.T.);
#52099=EDGE_CURVE('',#40828,#40827,#9674,.T.);
#52100=EDGE_CURVE('',#40828,#40825,#30403,.T.);
#52101=EDGE_CURVE('',#40825,#40829,#30404,.T.);
#52102=EDGE_CURVE('',#40830,#40829,#9675,.T.);
#52103=EDGE_CURVE('',#40824,#40830,#30405,.F.);
#52104=EDGE_CURVE('',#40831,#40832,#9676,.T.);
#52105=EDGE_CURVE('',#40830,#40831,#30406,.F.);
#52106=EDGE_CURVE('',#40829,#40832,#30407,.T.);
#52107=EDGE_CURVE('',#40833,#40834,#9677,.T.);
#52108=EDGE_CURVE('',#40831,#40833,#30408,.F.);
#52109=EDGE_CURVE('',#40832,#40834,#30409,.T.);
#52110=EDGE_CURVE('',#40835,#40836,#9678,.T.);
#52111=EDGE_CURVE('',#40837,#40835,#30410,.T.);
#52112=EDGE_CURVE('',#40838,#40837,#30411,.T.);
#52113=EDGE_CURVE('',#40836,#40838,#33531,.T.);
#52114=EDGE_CURVE('',#40839,#40840,#9679,.T.);
#52115=EDGE_CURVE('',#40839,#40841,#30412,.T.);
#52116=EDGE_CURVE('',#40841,#40842,#33532,.T.);
#52117=EDGE_CURVE('',#40840,#40842,#30413,.F.);
#52118=EDGE_CURVE('',#40843,#40844,#9680,.T.);
#52119=EDGE_CURVE('',#40843,#40839,#30414,.T.);
#52120=EDGE_CURVE('',#40844,#40840,#30415,.F.);
#52121=EDGE_CURVE('',#40845,#40846,#9681,.T.);
#52122=EDGE_CURVE('',#40845,#40843,#30416,.T.);
#52123=EDGE_CURVE('',#40846,#40844,#30417,.F.);
#52124=EDGE_CURVE('',#40847,#40848,#9682,.T.);
#52125=EDGE_CURVE('',#40847,#40849,#30418,.T.);
#52126=EDGE_CURVE('',#40849,#40850,#30419,.T.);
#52127=EDGE_CURVE('',#40850,#40851,#9683,.T.);
#52128=EDGE_CURVE('',#40848,#40851,#30420,.T.);
#52129=EDGE_CURVE('',#40852,#40848,#30421,.F.);
#52130=EDGE_CURVE('',#40853,#40852,#9684,.T.);
#52131=EDGE_CURVE('',#40853,#40847,#30422,.T.);
#52132=EDGE_CURVE('',#40854,#40855,#9685,.T.);
#52133=EDGE_CURVE('',#40854,#40853,#30423,.T.);
#52134=EDGE_CURVE('',#40855,#40852,#30424,.F.);
#52135=EDGE_CURVE('',#40856,#40857,#9686,.T.);
#52136=EDGE_CURVE('',#40856,#40854,#30425,.T.);
#52137=EDGE_CURVE('',#40857,#40855,#30426,.F.);
#52138=EDGE_CURVE('',#40858,#40859,#9687,.T.);
#52139=EDGE_CURVE('',#40858,#40860,#33533,.T.);
#52140=EDGE_CURVE('',#40860,#40861,#30427,.T.);
#52141=EDGE_CURVE('',#40862,#40861,#30428,.T.);
#52142=EDGE_CURVE('',#40863,#40862,#30429,.T.);
#52143=EDGE_CURVE('',#40864,#40863,#33534,.T.);
#52144=EDGE_CURVE('',#40864,#40859,#30430,.T.);
#52145=EDGE_CURVE('',#40859,#40865,#30431,.T.);
#52146=EDGE_CURVE('',#40865,#40858,#33535,.T.);
#52147=EDGE_CURVE('',#40866,#40866,#2697,.T.);
#52148=EDGE_CURVE('',#40866,#40867,#9688,.T.);
#52149=EDGE_CURVE('',#40867,#40867,#2698,.T.);
#52150=EDGE_CURVE('',#40842,#40857,#30432,.F.);
#52151=EDGE_CURVE('',#40841,#40856,#30433,.T.);
#52152=EDGE_CURVE('',#40868,#40846,#30434,.F.);
#52153=EDGE_CURVE('',#40869,#40868,#33536,.T.);
#52154=EDGE_CURVE('',#40869,#40845,#30435,.T.);
#52155=EDGE_CURVE('',#40870,#40871,#30436,.T.);
#52156=EDGE_CURVE('',#40871,#40872,#9689,.T.);
#52157=EDGE_CURVE('',#40872,#40873,#30437,.T.);
#52158=EDGE_CURVE('',#40873,#40874,#30438,.T.);
#52159=EDGE_CURVE('',#40870,#40874,#9690,.T.);
#52160=EDGE_CURVE('',#40875,#40836,#33537,.T.);
#52161=EDGE_CURVE('',#40875,#40876,#30439,.T.);
#52162=EDGE_CURVE('',#40876,#40828,#30440,.T.);
#52163=EDGE_CURVE('',#40877,#40827,#30441,.T.);
#52164=EDGE_CURVE('',#40835,#40877,#30442,.T.);
#52165=EDGE_CURVE('',#40834,#40878,#30443,.T.);
#52166=EDGE_CURVE('',#40878,#40817,#30444,.T.);
#52167=EDGE_CURVE('',#40879,#40816,#30445,.T.);
#52168=EDGE_CURVE('',#40833,#40879,#30446,.F.);
#52169=EDGE_CURVE('',#40823,#40880,#30447,.T.);
#52170=EDGE_CURVE('',#40880,#40881,#30448,.T.);
#52171=EDGE_CURVE('',#40881,#40882,#30449,.T.);
#52172=EDGE_CURVE('',#40883,#40882,#30450,.T.);
#52173=EDGE_CURVE('',#40822,#40883,#30451,.F.);
#52174=EDGE_CURVE('',#40881,#40884,#30452,.T.);
#52175=EDGE_CURVE('',#40884,#40885,#9691,.T.);
#52176=EDGE_CURVE('',#40882,#40885,#30453,.T.);
#52177=EDGE_CURVE('',#40886,#40828,#9692,.T.);
#52178=EDGE_CURVE('',#40775,#40886,#30454,.F.);
#52179=EDGE_CURVE('',#40769,#40817,#9693,.T.);
#52180=EDGE_CURVE('',#40759,#40881,#30455,.T.);
#52181=EDGE_CURVE('',#40757,#40884,#30456,.T.);
#52182=EDGE_CURVE('',#40885,#40756,#30457,.T.);
#52183=EDGE_CURVE('',#40882,#40754,#30458,.T.);
#52184=EDGE_CURVE('',#40816,#40766,#9694,.T.);
#52185=EDGE_CURVE('',#40827,#40776,#9695,.T.);
#52186=EDGE_CURVE('',#40863,#40875,#30459,.T.);
#52187=EDGE_CURVE('',#40886,#40860,#30460,.T.);
#52188=EDGE_CURVE('',#40887,#40888,#9696,.T.);
#52189=EDGE_CURVE('',#40889,#40887,#33538,.T.);
#52190=EDGE_CURVE('',#40870,#40889,#33539,.T.);
#52191=EDGE_CURVE('',#40888,#40874,#33540,.T.);
#52192=EDGE_CURVE('',#40802,#40873,#33541,.T.);
#52193=EDGE_CURVE('',#40872,#40890,#33542,.T.);
#52194=EDGE_CURVE('',#40888,#40890,#30461,.T.);
#52195=EDGE_CURVE('',#40809,#40782,#30462,.T.);
#52196=EDGE_CURVE('',#40850,#40891,#30463,.T.);
#52197=EDGE_CURVE('',#40891,#40892,#9697,.T.);
#52198=EDGE_CURVE('',#40851,#40892,#30464,.T.);
#52199=EDGE_CURVE('',#40893,#40868,#30465,.T.);
#52200=EDGE_CURVE('',#40894,#40893,#30466,.T.);
#52201=EDGE_CURVE('',#40894,#40895,#30467,.T.);
#52202=EDGE_CURVE('',#40895,#40869,#30468,.T.);
#52203=EDGE_CURVE('',#40896,#40850,#30469,.T.);
#52204=EDGE_CURVE('',#40795,#40841,#9698,.T.);
#52205=EDGE_CURVE('',#40896,#40799,#30470,.F.);
#52206=EDGE_CURVE('',#40805,#40891,#30471,.T.);
#52207=EDGE_CURVE('',#40806,#40896,#30472,.T.);
#52208=EDGE_CURVE('',#40892,#40804,#30473,.T.);
#52209=EDGE_CURVE('',#40851,#40808,#30474,.T.);
#52210=EDGE_CURVE('',#40800,#40807,#30475,.F.);
#52211=EDGE_CURVE('',#40842,#40798,#9699,.T.);
#52212=EDGE_CURVE('',#40868,#40790,#9700,.T.);
#52213=EDGE_CURVE('',#40897,#40812,#30476,.T.);
#52214=EDGE_CURVE('',#40897,#40893,#30477,.T.);
#52215=EDGE_CURVE('',#40787,#40869,#9701,.T.);
#52216=EDGE_CURVE('',#40898,#40895,#30478,.T.);
#52217=EDGE_CURVE('',#40898,#40811,#30479,.T.);
#52218=EDGE_CURVE('',#40899,#40900,#33543,.T.);
#52219=EDGE_CURVE('',#40899,#40901,#9702,.T.);
#52220=EDGE_CURVE('',#40901,#40901,#33544,.T.);
#52221=EDGE_CURVE('',#40900,#40899,#33545,.T.);
#52222=EDGE_CURVE('',#40900,#40902,#9703,.T.);
#52223=EDGE_CURVE('',#40902,#40902,#33546,.T.);
#52224=EDGE_CURVE('',#40903,#40903,#33547,.T.);
#52225=EDGE_CURVE('',#40903,#40904,#9704,.T.);
#52226=EDGE_CURVE('',#40904,#40904,#33548,.T.);
#52227=EDGE_CURVE('',#40904,#40905,#9705,.T.);
#52228=EDGE_CURVE('',#40905,#40905,#33549,.T.);
#52229=EDGE_CURVE('',#40838,#40864,#30480,.T.);
#52230=EDGE_CURVE('',#40865,#40906,#30481,.T.);
#52231=EDGE_CURVE('',#40906,#40907,#30482,.T.);
#52232=EDGE_CURVE('',#40907,#40774,#30483,.T.);
#52233=EDGE_CURVE('',#40908,#40887,#30484,.T.);
#52234=EDGE_CURVE('',#40908,#40871,#33550,.T.);
#52235=EDGE_CURVE('',#40889,#40753,#33551,.T.);
#52236=EDGE_CURVE('',#40908,#40890,#9706,.T.);
#52237=EDGE_CURVE('',#40909,#40910,#9707,.T.);
#52238=EDGE_CURVE('',#40909,#40911,#30485,.F.);
#52239=EDGE_CURVE('',#40911,#40912,#9708,.T.);
#52240=EDGE_CURVE('',#40912,#40913,#33552,.T.);
#52241=EDGE_CURVE('',#40913,#40912,#33553,.T.);
#52242=EDGE_CURVE('',#40911,#40914,#30486,.F.);
#52243=EDGE_CURVE('',#40914,#40915,#30487,.T.);
#52244=EDGE_CURVE('',#40915,#40916,#30488,.T.);
#52245=EDGE_CURVE('',#40916,#40917,#9709,.T.);
#52246=EDGE_CURVE('',#40917,#40918,#30489,.T.);
#52247=EDGE_CURVE('',#40918,#40919,#30490,.T.);
#52248=EDGE_CURVE('',#40919,#40910,#30491,.F.);
#52249=EDGE_CURVE('',#40920,#40921,#9710,.T.);
#52250=EDGE_CURVE('',#40920,#40909,#30492,.F.);
#52251=EDGE_CURVE('',#40910,#40921,#30493,.F.);
#52252=EDGE_CURVE('',#40922,#40923,#9711,.T.);
#52253=EDGE_CURVE('',#40922,#40920,#30494,.F.);
#52254=EDGE_CURVE('',#40921,#40923,#30495,.F.);
#52255=EDGE_CURVE('',#40924,#40925,#9712,.T.);
#52256=EDGE_CURVE('',#40924,#40926,#30496,.F.);
#52257=EDGE_CURVE('',#40926,#40922,#30497,.F.);
#52258=EDGE_CURVE('',#40923,#40925,#30498,.F.);
#52259=EDGE_CURVE('',#40927,#40928,#9713,.T.);
#52260=EDGE_CURVE('',#40927,#40924,#30499,.F.);
#52261=EDGE_CURVE('',#40925,#40929,#30500,.F.);
#52262=EDGE_CURVE('',#40929,#40928,#30501,.F.);
#52263=EDGE_CURVE('',#40930,#40931,#9714,.T.);
#52264=EDGE_CURVE('',#40930,#40927,#30502,.F.);
#52265=EDGE_CURVE('',#40928,#40931,#30503,.F.);
#52266=EDGE_CURVE('',#40932,#40933,#9715,.T.);
#52267=EDGE_CURVE('',#40932,#40930,#30504,.F.);
#52268=EDGE_CURVE('',#40931,#40933,#30505,.F.);
#52269=EDGE_CURVE('',#40934,#40935,#9716,.T.);
#52270=EDGE_CURVE('',#40934,#40936,#30506,.T.);
#52271=EDGE_CURVE('',#40936,#40932,#30507,.F.);
#52272=EDGE_CURVE('',#40933,#40935,#30508,.F.);
#52273=EDGE_CURVE('',#40937,#40938,#9717,.T.);
#52274=EDGE_CURVE('',#40937,#40939,#30509,.T.);
#52275=EDGE_CURVE('',#40938,#40939,#33554,.T.);
#52276=EDGE_CURVE('',#40940,#40941,#9718,.T.);
#52277=EDGE_CURVE('',#40940,#40937,#30510,.T.);
#52278=EDGE_CURVE('',#40942,#40938,#33555,.T.);
#52279=EDGE_CURVE('',#40942,#40943,#30511,.T.);
#52280=EDGE_CURVE('',#40943,#40944,#30512,.T.);
#52281=EDGE_CURVE('',#40944,#40941,#30513,.F.);
#52282=EDGE_CURVE('',#40945,#40946,#9719,.T.);
#52283=EDGE_CURVE('',#40945,#40947,#30514,.T.);
#52284=EDGE_CURVE('',#40947,#40940,#30515,.T.);
#52285=EDGE_CURVE('',#40941,#40946,#30516,.F.);
#52286=EDGE_CURVE('',#40948,#40949,#9720,.T.);
#52287=EDGE_CURVE('',#40948,#40945,#30517,.T.);
#52288=EDGE_CURVE('',#40946,#40950,#30518,.F.);
#52289=EDGE_CURVE('',#40950,#40949,#30519,.F.);
#52290=EDGE_CURVE('',#40951,#40952,#9721,.T.);
#52291=EDGE_CURVE('',#40951,#40948,#30520,.T.);
#52292=EDGE_CURVE('',#40949,#40952,#30521,.F.);
#52293=EDGE_CURVE('',#40953,#40954,#9722,.T.);
#52294=EDGE_CURVE('',#40953,#40955,#30522,.F.);
#52295=EDGE_CURVE('',#40955,#40951,#30523,.T.);
#52296=EDGE_CURVE('',#40952,#40954,#30524,.F.);
#52297=EDGE_CURVE('',#40956,#40957,#9723,.T.);
#52298=EDGE_CURVE('',#40956,#40953,#30525,.F.);
#52299=EDGE_CURVE('',#40954,#40958,#30526,.F.);
#52300=EDGE_CURVE('',#40958,#40957,#30527,.F.);
#52301=EDGE_CURVE('',#40959,#40960,#9724,.T.);
#52302=EDGE_CURVE('',#40959,#40956,#30528,.F.);
#52303=EDGE_CURVE('',#40957,#40960,#30529,.F.);
#52304=EDGE_CURVE('',#40961,#40962,#33556,.T.);
#52305=EDGE_CURVE('',#40962,#40961,#33557,.T.);
#52306=EDGE_CURVE('',#40961,#40963,#9725,.T.);
#52307=EDGE_CURVE('',#40963,#40964,#30530,.T.);
#52308=EDGE_CURVE('',#40965,#40964,#9726,.T.);
#52309=EDGE_CURVE('',#40965,#40966,#30531,.T.);
#52310=EDGE_CURVE('',#40966,#40967,#9727,.T.);
#52311=EDGE_CURVE('',#40967,#40968,#30532,.F.);
#52312=EDGE_CURVE('',#40968,#40963,#30533,.T.);
#52313=EDGE_CURVE('',#40938,#40969,#9728,.T.);
#52314=EDGE_CURVE('',#40970,#40939,#30534,.T.);
#52315=EDGE_CURVE('',#40971,#40970,#30535,.F.);
#52316=EDGE_CURVE('',#40972,#40971,#33558,.T.);
#52317=EDGE_CURVE('',#40972,#40969,#30536,.T.);
#52318=EDGE_CURVE('',#40973,#40974,#9729,.T.);
#52319=EDGE_CURVE('',#40975,#40973,#30537,.F.);
#52320=EDGE_CURVE('',#40976,#40975,#30538,.T.);
#52321=EDGE_CURVE('',#40977,#40976,#9730,.T.);
#52322=EDGE_CURVE('',#40977,#40974,#30539,.T.);
#52323=EDGE_CURVE('',#40974,#40978,#30540,.T.);
#52324=EDGE_CURVE('',#40979,#40978,#9731,.T.);
#52325=EDGE_CURVE('',#40973,#40979,#30541,.F.);
#52326=EDGE_CURVE('',#40980,#40981,#9732,.T.);
#52327=EDGE_CURVE('',#40979,#40980,#30542,.F.);
#52328=EDGE_CURVE('',#40978,#40981,#30543,.T.);
#52329=EDGE_CURVE('',#40982,#40983,#9733,.T.);
#52330=EDGE_CURVE('',#40980,#40982,#30544,.F.);
#52331=EDGE_CURVE('',#40981,#40983,#30545,.T.);
#52332=EDGE_CURVE('',#40984,#40985,#9734,.T.);
#52333=EDGE_CURVE('',#40986,#40984,#30546,.F.);
#52334=EDGE_CURVE('',#40987,#40986,#30547,.T.);
#52335=EDGE_CURVE('',#40988,#40987,#9735,.T.);
#52336=EDGE_CURVE('',#40988,#40985,#30548,.T.);
#52337=EDGE_CURVE('',#40985,#40989,#30549,.T.);
#52338=EDGE_CURVE('',#40990,#40989,#9736,.T.);
#52339=EDGE_CURVE('',#40984,#40990,#30550,.F.);
#52340=EDGE_CURVE('',#40991,#40992,#9737,.T.);
#52341=EDGE_CURVE('',#40990,#40991,#30551,.F.);
#52342=EDGE_CURVE('',#40989,#40992,#30552,.T.);
#52343=EDGE_CURVE('',#40993,#40994,#9738,.T.);
#52344=EDGE_CURVE('',#40991,#40993,#30553,.F.);
#52345=EDGE_CURVE('',#40992,#40994,#30554,.T.);
#52346=EDGE_CURVE('',#40995,#40996,#9739,.T.);
#52347=EDGE_CURVE('',#40997,#40995,#30555,.T.);
#52348=EDGE_CURVE('',#40998,#40997,#30556,.T.);
#52349=EDGE_CURVE('',#40996,#40998,#33559,.T.);
#52350=EDGE_CURVE('',#40999,#41000,#9740,.T.);
#52351=EDGE_CURVE('',#40999,#41001,#30557,.T.);
#52352=EDGE_CURVE('',#41001,#41002,#33560,.T.);
#52353=EDGE_CURVE('',#41000,#41002,#30558,.F.);
#52354=EDGE_CURVE('',#41003,#41004,#9741,.T.);
#52355=EDGE_CURVE('',#41003,#40999,#30559,.T.);
#52356=EDGE_CURVE('',#41004,#41000,#30560,.F.);
#52357=EDGE_CURVE('',#41005,#41006,#9742,.T.);
#52358=EDGE_CURVE('',#41005,#41003,#30561,.T.);
#52359=EDGE_CURVE('',#41006,#41004,#30562,.F.);
#52360=EDGE_CURVE('',#41007,#41008,#9743,.T.);
#52361=EDGE_CURVE('',#41007,#41009,#30563,.T.);
#52362=EDGE_CURVE('',#41009,#41010,#30564,.T.);
#52363=EDGE_CURVE('',#41010,#41011,#9744,.T.);
#52364=EDGE_CURVE('',#41008,#41011,#30565,.T.);
#52365=EDGE_CURVE('',#41012,#41008,#30566,.F.);
#52366=EDGE_CURVE('',#41013,#41012,#9745,.T.);
#52367=EDGE_CURVE('',#41013,#41007,#30567,.T.);
#52368=EDGE_CURVE('',#41014,#41015,#9746,.T.);
#52369=EDGE_CURVE('',#41014,#41013,#30568,.T.);
#52370=EDGE_CURVE('',#41015,#41012,#30569,.F.);
#52371=EDGE_CURVE('',#41016,#41017,#9747,.T.);
#52372=EDGE_CURVE('',#41016,#41014,#30570,.T.);
#52373=EDGE_CURVE('',#41017,#41015,#30571,.F.);
#52374=EDGE_CURVE('',#41018,#41019,#9748,.T.);
#52375=EDGE_CURVE('',#41018,#41020,#33561,.T.);
#52376=EDGE_CURVE('',#41020,#41021,#30572,.T.);
#52377=EDGE_CURVE('',#41022,#41021,#30573,.T.);
#52378=EDGE_CURVE('',#41023,#41022,#30574,.T.);
#52379=EDGE_CURVE('',#41024,#41023,#33562,.T.);
#52380=EDGE_CURVE('',#41024,#41019,#30575,.T.);
#52381=EDGE_CURVE('',#41019,#41025,#30576,.T.);
#52382=EDGE_CURVE('',#41025,#41018,#33563,.T.);
#52383=EDGE_CURVE('',#41026,#41026,#2699,.T.);
#52384=EDGE_CURVE('',#41026,#41027,#9749,.T.);
#52385=EDGE_CURVE('',#41027,#41027,#2700,.T.);
#52386=EDGE_CURVE('',#41002,#41017,#30577,.F.);
#52387=EDGE_CURVE('',#41001,#41016,#30578,.T.);
#52388=EDGE_CURVE('',#41028,#41006,#30579,.F.);
#52389=EDGE_CURVE('',#41029,#41028,#33564,.T.);
#52390=EDGE_CURVE('',#41029,#41005,#30580,.T.);
#52391=EDGE_CURVE('',#41030,#41031,#30581,.T.);
#52392=EDGE_CURVE('',#41031,#41032,#9750,.T.);
#52393=EDGE_CURVE('',#41032,#41033,#30582,.T.);
#52394=EDGE_CURVE('',#41033,#41034,#30583,.T.);
#52395=EDGE_CURVE('',#41030,#41034,#9751,.T.);
#52396=EDGE_CURVE('',#41035,#40996,#33565,.T.);
#52397=EDGE_CURVE('',#41035,#41036,#30584,.T.);
#52398=EDGE_CURVE('',#41036,#40988,#30585,.T.);
#52399=EDGE_CURVE('',#41037,#40987,#30586,.T.);
#52400=EDGE_CURVE('',#40995,#41037,#30587,.T.);
#52401=EDGE_CURVE('',#40994,#41038,#30588,.T.);
#52402=EDGE_CURVE('',#41038,#40977,#30589,.T.);
#52403=EDGE_CURVE('',#41039,#40976,#30590,.T.);
#52404=EDGE_CURVE('',#40993,#41039,#30591,.F.);
#52405=EDGE_CURVE('',#40983,#41040,#30592,.T.);
#52406=EDGE_CURVE('',#41040,#41041,#30593,.T.);
#52407=EDGE_CURVE('',#41041,#41042,#30594,.T.);
#52408=EDGE_CURVE('',#41043,#41042,#30595,.T.);
#52409=EDGE_CURVE('',#40982,#41043,#30596,.F.);
#52410=EDGE_CURVE('',#41041,#41044,#30597,.T.);
#52411=EDGE_CURVE('',#41044,#41045,#9752,.T.);
#52412=EDGE_CURVE('',#41042,#41045,#30598,.T.);
#52413=EDGE_CURVE('',#41046,#40988,#9753,.T.);
#52414=EDGE_CURVE('',#40935,#41046,#30599,.F.);
#52415=EDGE_CURVE('',#40929,#40977,#9754,.T.);
#52416=EDGE_CURVE('',#40919,#41041,#30600,.T.);
#52417=EDGE_CURVE('',#40917,#41044,#30601,.T.);
#52418=EDGE_CURVE('',#41045,#40916,#30602,.T.);
#52419=EDGE_CURVE('',#41042,#40914,#30603,.T.);
#52420=EDGE_CURVE('',#40976,#40926,#9755,.T.);
#52421=EDGE_CURVE('',#40987,#40936,#9756,.T.);
#52422=EDGE_CURVE('',#41023,#41035,#30604,.T.);
#52423=EDGE_CURVE('',#41046,#41020,#30605,.T.);
#52424=EDGE_CURVE('',#41047,#41048,#9757,.T.);
#52425=EDGE_CURVE('',#41049,#41047,#33566,.T.);
#52426=EDGE_CURVE('',#41030,#41049,#33567,.T.);
#52427=EDGE_CURVE('',#41048,#41034,#33568,.T.);
#52428=EDGE_CURVE('',#40962,#41033,#33569,.T.);
#52429=EDGE_CURVE('',#41032,#41050,#33570,.T.);
#52430=EDGE_CURVE('',#41048,#41050,#30606,.T.);
#52431=EDGE_CURVE('',#40969,#40942,#30607,.T.);
#52432=EDGE_CURVE('',#41010,#41051,#30608,.T.);
#52433=EDGE_CURVE('',#41051,#41052,#9758,.T.);
#52434=EDGE_CURVE('',#41011,#41052,#30609,.T.);
#52435=EDGE_CURVE('',#41053,#41028,#30610,.T.);
#52436=EDGE_CURVE('',#41054,#41053,#30611,.T.);
#52437=EDGE_CURVE('',#41054,#41055,#30612,.T.);
#52438=EDGE_CURVE('',#41055,#41029,#30613,.T.);
#52439=EDGE_CURVE('',#41056,#41010,#30614,.T.);
#52440=EDGE_CURVE('',#40955,#41001,#9759,.T.);
#52441=EDGE_CURVE('',#41056,#40959,#30615,.F.);
#52442=EDGE_CURVE('',#40965,#41051,#30616,.T.);
#52443=EDGE_CURVE('',#40966,#41056,#30617,.T.);
#52444=EDGE_CURVE('',#41052,#40964,#30618,.T.);
#52445=EDGE_CURVE('',#41011,#40968,#30619,.T.);
#52446=EDGE_CURVE('',#40960,#40967,#30620,.F.);
#52447=EDGE_CURVE('',#41002,#40958,#9760,.T.);
#52448=EDGE_CURVE('',#41028,#40950,#9761,.T.);
#52449=EDGE_CURVE('',#41057,#40972,#30621,.T.);
#52450=EDGE_CURVE('',#41057,#41053,#30622,.T.);
#52451=EDGE_CURVE('',#40947,#41029,#9762,.T.);
#52452=EDGE_CURVE('',#41058,#41055,#30623,.T.);
#52453=EDGE_CURVE('',#41058,#40971,#30624,.T.);
#52454=EDGE_CURVE('',#41059,#41060,#33571,.T.);
#52455=EDGE_CURVE('',#41059,#41061,#9763,.T.);
#52456=EDGE_CURVE('',#41061,#41061,#33572,.T.);
#52457=EDGE_CURVE('',#41060,#41059,#33573,.T.);
#52458=EDGE_CURVE('',#41060,#41062,#9764,.T.);
#52459=EDGE_CURVE('',#41062,#41062,#33574,.T.);
#52460=EDGE_CURVE('',#41063,#41063,#33575,.T.);
#52461=EDGE_CURVE('',#41063,#41064,#9765,.T.);
#52462=EDGE_CURVE('',#41064,#41064,#33576,.T.);
#52463=EDGE_CURVE('',#41064,#41065,#9766,.T.);
#52464=EDGE_CURVE('',#41065,#41065,#33577,.T.);
#52465=EDGE_CURVE('',#40998,#41024,#30625,.T.);
#52466=EDGE_CURVE('',#41025,#41066,#30626,.T.);
#52467=EDGE_CURVE('',#41066,#41067,#30627,.T.);
#52468=EDGE_CURVE('',#41067,#40934,#30628,.T.);
#52469=EDGE_CURVE('',#41068,#41047,#30629,.T.);
#52470=EDGE_CURVE('',#41068,#41031,#33578,.T.);
#52471=EDGE_CURVE('',#41049,#40913,#33579,.T.);
#52472=EDGE_CURVE('',#41068,#41050,#9767,.T.);
#52473=ORIENTED_EDGE('',*,*,#41069,.T.);
#52474=ORIENTED_EDGE('',*,*,#41070,.F.);
#52475=ORIENTED_EDGE('',*,*,#41071,.F.);
#52476=ORIENTED_EDGE('',*,*,#41072,.F.);
#52477=ORIENTED_EDGE('',*,*,#41073,.T.);
#52478=ORIENTED_EDGE('',*,*,#41074,.T.);
#52479=ORIENTED_EDGE('',*,*,#41075,.T.);
#52480=ORIENTED_EDGE('',*,*,#41076,.F.);
#52481=ORIENTED_EDGE('',*,*,#41071,.T.);
#52482=ORIENTED_EDGE('',*,*,#41077,.F.);
#52483=ORIENTED_EDGE('',*,*,#41078,.F.);
#52484=ORIENTED_EDGE('',*,*,#41079,.T.);
#52485=ORIENTED_EDGE('',*,*,#41077,.T.);
#52486=ORIENTED_EDGE('',*,*,#41080,.F.);
#52487=ORIENTED_EDGE('',*,*,#41078,.T.);
#52488=ORIENTED_EDGE('',*,*,#41070,.T.);
#52489=ORIENTED_EDGE('',*,*,#41075,.F.);
#52490=ORIENTED_EDGE('',*,*,#41081,.F.);
#52491=ORIENTED_EDGE('',*,*,#41073,.F.);
#52492=ORIENTED_EDGE('',*,*,#41069,.F.);
#52493=ORIENTED_EDGE('',*,*,#41072,.T.);
#52494=ORIENTED_EDGE('',*,*,#41076,.T.);
#52495=ORIENTED_EDGE('',*,*,#41079,.F.);
#52496=ORIENTED_EDGE('',*,*,#41080,.T.);
#52497=ORIENTED_EDGE('',*,*,#41074,.F.);
#52498=ORIENTED_EDGE('',*,*,#41081,.T.);
#52499=ORIENTED_EDGE('',*,*,#41082,.T.);
#52500=ORIENTED_EDGE('',*,*,#41083,.F.);
#52501=ORIENTED_EDGE('',*,*,#41084,.F.);
#52502=ORIENTED_EDGE('',*,*,#41085,.F.);
#52503=ORIENTED_EDGE('',*,*,#41086,.F.);
#52504=ORIENTED_EDGE('',*,*,#41087,.F.);
#52505=ORIENTED_EDGE('',*,*,#41082,.F.);
#52506=ORIENTED_EDGE('',*,*,#41088,.T.);
#52507=ORIENTED_EDGE('',*,*,#41089,.T.);
#52508=ORIENTED_EDGE('',*,*,#41090,.T.);
#52509=ORIENTED_EDGE('',*,*,#41091,.F.);
#52510=ORIENTED_EDGE('',*,*,#41088,.F.);
#52511=ORIENTED_EDGE('',*,*,#41083,.T.);
#52512=ORIENTED_EDGE('',*,*,#41092,.T.);
#52513=ORIENTED_EDGE('',*,*,#41087,.T.);
#52514=ORIENTED_EDGE('',*,*,#41093,.T.);
#52515=ORIENTED_EDGE('',*,*,#41092,.F.);
#52516=ORIENTED_EDGE('',*,*,#41094,.F.);
#52517=ORIENTED_EDGE('',*,*,#41084,.T.);
#52518=ORIENTED_EDGE('',*,*,#41090,.F.);
#52519=ORIENTED_EDGE('',*,*,#41086,.T.);
#52520=ORIENTED_EDGE('',*,*,#41085,.T.);
#52521=ORIENTED_EDGE('',*,*,#41094,.T.);
#52522=ORIENTED_EDGE('',*,*,#41089,.F.);
#52523=ORIENTED_EDGE('',*,*,#41091,.T.);
#52524=ORIENTED_EDGE('',*,*,#41093,.F.);
#52525=ORIENTED_EDGE('',*,*,#41095,.F.);
#52526=ORIENTED_EDGE('',*,*,#41096,.T.);
#52527=ORIENTED_EDGE('',*,*,#41097,.F.);
#52528=ORIENTED_EDGE('',*,*,#41098,.T.);
#52529=ORIENTED_EDGE('',*,*,#41099,.F.);
#52530=ORIENTED_EDGE('',*,*,#41100,.T.);
#52531=ORIENTED_EDGE('',*,*,#41101,.F.);
#52532=ORIENTED_EDGE('',*,*,#41102,.T.);
#52533=ORIENTED_EDGE('',*,*,#41103,.F.);
#52534=ORIENTED_EDGE('',*,*,#41104,.F.);
#52535=ORIENTED_EDGE('',*,*,#41105,.T.);
#52536=ORIENTED_EDGE('',*,*,#41104,.T.);
#52537=ORIENTED_EDGE('',*,*,#41106,.F.);
#52538=ORIENTED_EDGE('',*,*,#41107,.T.);
#52539=ORIENTED_EDGE('',*,*,#41098,.F.);
#52540=ORIENTED_EDGE('',*,*,#41108,.T.);
#52541=ORIENTED_EDGE('',*,*,#41106,.T.);
#52542=ORIENTED_EDGE('',*,*,#41109,.F.);
#52543=ORIENTED_EDGE('',*,*,#41110,.T.);
#52544=ORIENTED_EDGE('',*,*,#41099,.T.);
#52545=ORIENTED_EDGE('',*,*,#41109,.T.);
#52546=ORIENTED_EDGE('',*,*,#41103,.T.);
#52547=ORIENTED_EDGE('',*,*,#41100,.F.);
#52548=ORIENTED_EDGE('',*,*,#41110,.F.);
#52549=ORIENTED_EDGE('',*,*,#41102,.F.);
#52550=ORIENTED_EDGE('',*,*,#41111,.T.);
#52551=ORIENTED_EDGE('',*,*,#41112,.F.);
#52552=ORIENTED_EDGE('',*,*,#41101,.T.);
#52553=ORIENTED_EDGE('',*,*,#41111,.F.);
#52554=ORIENTED_EDGE('',*,*,#41096,.F.);
#52555=ORIENTED_EDGE('',*,*,#41113,.T.);
#52556=ORIENTED_EDGE('',*,*,#41107,.F.);
#52557=ORIENTED_EDGE('',*,*,#41114,.F.);
#52558=ORIENTED_EDGE('',*,*,#41113,.F.);
#52559=ORIENTED_EDGE('',*,*,#41095,.T.);
#52560=ORIENTED_EDGE('',*,*,#41112,.T.);
#52561=ORIENTED_EDGE('',*,*,#41105,.F.);
#52562=ORIENTED_EDGE('',*,*,#41108,.F.);
#52563=ORIENTED_EDGE('',*,*,#41097,.T.);
#52564=ORIENTED_EDGE('',*,*,#41114,.T.);
#52565=ORIENTED_EDGE('',*,*,#41115,.F.);
#52566=ORIENTED_EDGE('',*,*,#41116,.T.);
#52567=ORIENTED_EDGE('',*,*,#41117,.F.);
#52568=ORIENTED_EDGE('',*,*,#41118,.F.);
#52569=ORIENTED_EDGE('',*,*,#41119,.T.);
#52570=ORIENTED_EDGE('',*,*,#41120,.F.);
#52571=ORIENTED_EDGE('',*,*,#41121,.T.);
#52572=ORIENTED_EDGE('',*,*,#41122,.T.);
#52573=ORIENTED_EDGE('',*,*,#41123,.F.);
#52574=ORIENTED_EDGE('',*,*,#41124,.T.);
#52575=ORIENTED_EDGE('',*,*,#41123,.T.);
#52576=ORIENTED_EDGE('',*,*,#41125,.F.);
#52577=ORIENTED_EDGE('',*,*,#41126,.F.);
#52578=ORIENTED_EDGE('',*,*,#41127,.T.);
#52579=ORIENTED_EDGE('',*,*,#41119,.F.);
#52580=ORIENTED_EDGE('',*,*,#41128,.T.);
#52581=ORIENTED_EDGE('',*,*,#41126,.T.);
#52582=ORIENTED_EDGE('',*,*,#41129,.F.);
#52583=ORIENTED_EDGE('',*,*,#41130,.T.);
#52584=ORIENTED_EDGE('',*,*,#41120,.T.);
#52585=ORIENTED_EDGE('',*,*,#41129,.T.);
#52586=ORIENTED_EDGE('',*,*,#41125,.T.);
#52587=ORIENTED_EDGE('',*,*,#41121,.F.);
#52588=ORIENTED_EDGE('',*,*,#41130,.F.);
#52589=ORIENTED_EDGE('',*,*,#41122,.F.);
#52590=ORIENTED_EDGE('',*,*,#41131,.T.);
#52591=ORIENTED_EDGE('',*,*,#41128,.F.);
#52592=ORIENTED_EDGE('',*,*,#41118,.T.);
#52593=ORIENTED_EDGE('',*,*,#41132,.T.);
#52594=ORIENTED_EDGE('',*,*,#41132,.F.);
#52595=ORIENTED_EDGE('',*,*,#41117,.T.);
#52596=ORIENTED_EDGE('',*,*,#41133,.F.);
#52597=ORIENTED_EDGE('',*,*,#41127,.F.);
#52598=ORIENTED_EDGE('',*,*,#41116,.F.);
#52599=ORIENTED_EDGE('',*,*,#41134,.F.);
#52600=ORIENTED_EDGE('',*,*,#41124,.F.);
#52601=ORIENTED_EDGE('',*,*,#41133,.T.);
#52602=ORIENTED_EDGE('',*,*,#41134,.T.);
#52603=ORIENTED_EDGE('',*,*,#41115,.T.);
#52604=ORIENTED_EDGE('',*,*,#41131,.F.);
#52605=ORIENTED_EDGE('',*,*,#41135,.F.);
#52606=ORIENTED_EDGE('',*,*,#41136,.T.);
#52607=ORIENTED_EDGE('',*,*,#41137,.T.);
#52608=ORIENTED_EDGE('',*,*,#41138,.T.);
#52609=ORIENTED_EDGE('',*,*,#41139,.T.);
#52610=ORIENTED_EDGE('',*,*,#41140,.F.);
#52611=ORIENTED_EDGE('',*,*,#41141,.T.);
#52612=ORIENTED_EDGE('',*,*,#41142,.T.);
#52613=ORIENTED_EDGE('',*,*,#41143,.T.);
#52614=ORIENTED_EDGE('',*,*,#41135,.T.);
#52615=ORIENTED_EDGE('',*,*,#41144,.F.);
#52616=ORIENTED_EDGE('',*,*,#41145,.T.);
#52617=ORIENTED_EDGE('',*,*,#41140,.T.);
#52618=ORIENTED_EDGE('',*,*,#41146,.T.);
#52619=ORIENTED_EDGE('',*,*,#41147,.T.);
#52620=ORIENTED_EDGE('',*,*,#41148,.T.);
#52621=ORIENTED_EDGE('',*,*,#41149,.T.);
#52622=ORIENTED_EDGE('',*,*,#41150,.F.);
#52623=ORIENTED_EDGE('',*,*,#41151,.F.);
#52624=ORIENTED_EDGE('',*,*,#41152,.F.);
#52625=ORIENTED_EDGE('',*,*,#41153,.T.);
#52626=ORIENTED_EDGE('',*,*,#41154,.T.);
#52627=ORIENTED_EDGE('',*,*,#41148,.F.);
#52628=ORIENTED_EDGE('',*,*,#41155,.F.);
#52629=ORIENTED_EDGE('',*,*,#41156,.T.);
#52630=ORIENTED_EDGE('',*,*,#41157,.F.);
#52631=ORIENTED_EDGE('',*,*,#41158,.T.);
#52632=ORIENTED_EDGE('',*,*,#41159,.T.);
#52633=ORIENTED_EDGE('',*,*,#41160,.F.);
#52634=ORIENTED_EDGE('',*,*,#41161,.T.);
#52635=ORIENTED_EDGE('',*,*,#41162,.T.);
#52636=ORIENTED_EDGE('',*,*,#41163,.F.);
#52637=ORIENTED_EDGE('',*,*,#41164,.T.);
#52638=ORIENTED_EDGE('',*,*,#41165,.T.);
#52639=ORIENTED_EDGE('',*,*,#41166,.T.);
#52640=ORIENTED_EDGE('',*,*,#41161,.F.);
#52641=ORIENTED_EDGE('',*,*,#41167,.T.);
#52642=ORIENTED_EDGE('',*,*,#41168,.T.);
#52643=ORIENTED_EDGE('',*,*,#41169,.T.);
#52644=ORIENTED_EDGE('',*,*,#41165,.F.);
#52645=ORIENTED_EDGE('',*,*,#41170,.T.);
#52646=ORIENTED_EDGE('',*,*,#41171,.T.);
#52647=ORIENTED_EDGE('',*,*,#41172,.T.);
#52648=ORIENTED_EDGE('',*,*,#41168,.F.);
#52649=ORIENTED_EDGE('',*,*,#41173,.T.);
#52650=ORIENTED_EDGE('',*,*,#41174,.F.);
#52651=ORIENTED_EDGE('',*,*,#41175,.T.);
#52652=ORIENTED_EDGE('',*,*,#41176,.T.);
#52653=ORIENTED_EDGE('',*,*,#41177,.T.);
#52654=ORIENTED_EDGE('',*,*,#41178,.T.);
#52655=ORIENTED_EDGE('',*,*,#41179,.F.);
#52656=ORIENTED_EDGE('',*,*,#41180,.T.);
#52657=ORIENTED_EDGE('',*,*,#41181,.T.);
#52658=ORIENTED_EDGE('',*,*,#41182,.T.);
#52659=ORIENTED_EDGE('',*,*,#41183,.T.);
#52660=ORIENTED_EDGE('',*,*,#41181,.F.);
#52661=ORIENTED_EDGE('',*,*,#41184,.T.);
#52662=ORIENTED_EDGE('',*,*,#41185,.T.);
#52663=ORIENTED_EDGE('',*,*,#41186,.T.);
#52664=ORIENTED_EDGE('',*,*,#41177,.F.);
#52665=ORIENTED_EDGE('',*,*,#41187,.T.);
#52666=ORIENTED_EDGE('',*,*,#41188,.F.);
#52667=ORIENTED_EDGE('',*,*,#41189,.T.);
#52668=ORIENTED_EDGE('',*,*,#41190,.T.);
#52669=ORIENTED_EDGE('',*,*,#41191,.T.);
#52670=ORIENTED_EDGE('',*,*,#41192,.F.);
#52671=ORIENTED_EDGE('',*,*,#41193,.T.);
#52672=ORIENTED_EDGE('',*,*,#41194,.T.);
#52673=ORIENTED_EDGE('',*,*,#41193,.F.);
#52674=ORIENTED_EDGE('',*,*,#41195,.F.);
#52675=ORIENTED_EDGE('',*,*,#41196,.F.);
#52676=ORIENTED_EDGE('',*,*,#41197,.F.);
#52677=ORIENTED_EDGE('',*,*,#41198,.F.);
#52678=ORIENTED_EDGE('',*,*,#41199,.T.);
#52679=ORIENTED_EDGE('',*,*,#41200,.T.);
#52680=ORIENTED_EDGE('',*,*,#41201,.F.);
#52681=ORIENTED_EDGE('',*,*,#41202,.T.);
#52682=ORIENTED_EDGE('',*,*,#41203,.T.);
#52683=ORIENTED_EDGE('',*,*,#41204,.F.);
#52684=ORIENTED_EDGE('',*,*,#41205,.F.);
#52685=ORIENTED_EDGE('',*,*,#41206,.F.);
#52686=ORIENTED_EDGE('',*,*,#41207,.T.);
#52687=ORIENTED_EDGE('',*,*,#41208,.T.);
#52688=ORIENTED_EDGE('',*,*,#41209,.F.);
#52689=ORIENTED_EDGE('',*,*,#41210,.T.);
#52690=ORIENTED_EDGE('',*,*,#41211,.T.);
#52691=ORIENTED_EDGE('',*,*,#41212,.F.);
#52692=ORIENTED_EDGE('',*,*,#41213,.F.);
#52693=ORIENTED_EDGE('',*,*,#41214,.F.);
#52694=ORIENTED_EDGE('',*,*,#41215,.T.);
#52695=ORIENTED_EDGE('',*,*,#41216,.T.);
#52696=ORIENTED_EDGE('',*,*,#41216,.F.);
#52697=ORIENTED_EDGE('',*,*,#41217,.T.);
#52698=ORIENTED_EDGE('',*,*,#41218,.T.);
#52699=ORIENTED_EDGE('',*,*,#41219,.F.);
#52700=ORIENTED_EDGE('',*,*,#41220,.F.);
#52701=ORIENTED_EDGE('',*,*,#41221,.F.);
#52702=ORIENTED_EDGE('',*,*,#41222,.F.);
#52703=ORIENTED_EDGE('',*,*,#41223,.F.);
#52704=ORIENTED_EDGE('',*,*,#41224,.T.);
#52705=ORIENTED_EDGE('',*,*,#41225,.T.);
#52706=ORIENTED_EDGE('',*,*,#41226,.T.);
#52707=ORIENTED_EDGE('',*,*,#41227,.F.);
#52708=ORIENTED_EDGE('',*,*,#41228,.F.);
#52709=ORIENTED_EDGE('',*,*,#41229,.F.);
#52710=ORIENTED_EDGE('',*,*,#41230,.T.);
#52711=ORIENTED_EDGE('',*,*,#41231,.T.);
#52712=ORIENTED_EDGE('',*,*,#41232,.F.);
#52713=ORIENTED_EDGE('',*,*,#41233,.F.);
#52714=ORIENTED_EDGE('',*,*,#41234,.F.);
#52715=ORIENTED_EDGE('',*,*,#41235,.T.);
#52716=ORIENTED_EDGE('',*,*,#41236,.T.);
#52717=ORIENTED_EDGE('',*,*,#41235,.F.);
#52718=ORIENTED_EDGE('',*,*,#41237,.F.);
#52719=ORIENTED_EDGE('',*,*,#41238,.F.);
#52720=ORIENTED_EDGE('',*,*,#41239,.T.);
#52721=ORIENTED_EDGE('',*,*,#41237,.T.);
#52722=ORIENTED_EDGE('',*,*,#41234,.T.);
#52723=ORIENTED_EDGE('',*,*,#41239,.F.);
#52724=ORIENTED_EDGE('',*,*,#41240,.F.);
#52725=ORIENTED_EDGE('',*,*,#41241,.T.);
#52726=ORIENTED_EDGE('',*,*,#41242,.T.);
#52727=ORIENTED_EDGE('',*,*,#41241,.F.);
#52728=ORIENTED_EDGE('',*,*,#41243,.F.);
#52729=ORIENTED_EDGE('',*,*,#41244,.F.);
#52730=ORIENTED_EDGE('',*,*,#41245,.T.);
#52731=ORIENTED_EDGE('',*,*,#41243,.T.);
#52732=ORIENTED_EDGE('',*,*,#41240,.T.);
#52733=ORIENTED_EDGE('',*,*,#41245,.F.);
#52734=ORIENTED_EDGE('',*,*,#41246,.T.);
#52735=ORIENTED_EDGE('',*,*,#41247,.T.);
#52736=ORIENTED_EDGE('',*,*,#41248,.F.);
#52737=ORIENTED_EDGE('',*,*,#41249,.T.);
#52738=ORIENTED_EDGE('',*,*,#41250,.F.);
#52739=ORIENTED_EDGE('',*,*,#41251,.F.);
#52740=ORIENTED_EDGE('',*,*,#41252,.F.);
#52741=ORIENTED_EDGE('',*,*,#41246,.F.);
#52742=ORIENTED_EDGE('',*,*,#41253,.T.);
#52743=ORIENTED_EDGE('',*,*,#41254,.T.);
#52744=ORIENTED_EDGE('',*,*,#41255,.F.);
#52745=ORIENTED_EDGE('',*,*,#41256,.T.);
#52746=ORIENTED_EDGE('',*,*,#41257,.T.);
#52747=ORIENTED_EDGE('',*,*,#41258,.T.);
#52748=ORIENTED_EDGE('',*,*,#41259,.T.);
#52749=ORIENTED_EDGE('',*,*,#41260,.F.);
#52750=ORIENTED_EDGE('',*,*,#41261,.F.);
#52751=ORIENTED_EDGE('',*,*,#41262,.T.);
#52752=ORIENTED_EDGE('',*,*,#41263,.T.);
#52753=ORIENTED_EDGE('',*,*,#41264,.F.);
#52754=ORIENTED_EDGE('',*,*,#41263,.F.);
#52755=ORIENTED_EDGE('',*,*,#41265,.T.);
#52756=ORIENTED_EDGE('',*,*,#41266,.F.);
#52757=ORIENTED_EDGE('',*,*,#41267,.F.);
#52758=ORIENTED_EDGE('',*,*,#41268,.T.);
#52759=ORIENTED_EDGE('',*,*,#41269,.F.);
#52760=ORIENTED_EDGE('',*,*,#41270,.T.);
#52761=ORIENTED_EDGE('',*,*,#41271,.T.);
#52762=ORIENTED_EDGE('',*,*,#41272,.F.);
#52763=ORIENTED_EDGE('',*,*,#41273,.T.);
#52764=ORIENTED_EDGE('',*,*,#41274,.F.);
#52765=ORIENTED_EDGE('',*,*,#41275,.T.);
#52766=ORIENTED_EDGE('',*,*,#41220,.T.);
#52767=ORIENTED_EDGE('',*,*,#41276,.T.);
#52768=ORIENTED_EDGE('',*,*,#41277,.T.);
#52769=ORIENTED_EDGE('',*,*,#41278,.T.);
#52770=ORIENTED_EDGE('',*,*,#41279,.T.);
#52771=ORIENTED_EDGE('',*,*,#41280,.F.);
#52772=ORIENTED_EDGE('',*,*,#41281,.T.);
#52773=ORIENTED_EDGE('',*,*,#41282,.T.);
#52774=ORIENTED_EDGE('',*,*,#41283,.T.);
#52775=ORIENTED_EDGE('',*,*,#41284,.T.);
#52776=ORIENTED_EDGE('',*,*,#41285,.F.);
#52777=ORIENTED_EDGE('',*,*,#41286,.T.);
#52778=ORIENTED_EDGE('',*,*,#41287,.T.);
#52779=ORIENTED_EDGE('',*,*,#41288,.T.);
#52780=ORIENTED_EDGE('',*,*,#41288,.F.);
#52781=ORIENTED_EDGE('',*,*,#41289,.T.);
#52782=ORIENTED_EDGE('',*,*,#41290,.T.);
#52783=ORIENTED_EDGE('',*,*,#41291,.F.);
#52784=ORIENTED_EDGE('',*,*,#41292,.F.);
#52785=ORIENTED_EDGE('',*,*,#41293,.T.);
#52786=ORIENTED_EDGE('',*,*,#41294,.F.);
#52787=ORIENTED_EDGE('',*,*,#41295,.T.);
#52788=ORIENTED_EDGE('',*,*,#41296,.F.);
#52789=ORIENTED_EDGE('',*,*,#41293,.F.);
#52790=ORIENTED_EDGE('',*,*,#41230,.F.);
#52791=ORIENTED_EDGE('',*,*,#41297,.F.);
#52792=ORIENTED_EDGE('',*,*,#41298,.T.);
#52793=ORIENTED_EDGE('',*,*,#41299,.T.);
#52794=ORIENTED_EDGE('',*,*,#41300,.T.);
#52795=ORIENTED_EDGE('',*,*,#41298,.F.);
#52796=ORIENTED_EDGE('',*,*,#41300,.F.);
#52797=ORIENTED_EDGE('',*,*,#41301,.T.);
#52798=ORIENTED_EDGE('',*,*,#41302,.T.);
#52799=ORIENTED_EDGE('',*,*,#41301,.F.);
#52800=ORIENTED_EDGE('',*,*,#41299,.F.);
#52801=ORIENTED_EDGE('',*,*,#41303,.F.);
#52802=ORIENTED_EDGE('',*,*,#41304,.T.);
#52803=ORIENTED_EDGE('',*,*,#41305,.T.);
#52804=ORIENTED_EDGE('',*,*,#41306,.F.);
#52805=ORIENTED_EDGE('',*,*,#41307,.T.);
#52806=ORIENTED_EDGE('',*,*,#41304,.F.);
#52807=ORIENTED_EDGE('',*,*,#41308,.T.);
#52808=ORIENTED_EDGE('',*,*,#41309,.F.);
#52809=ORIENTED_EDGE('',*,*,#41310,.F.);
#52810=ORIENTED_EDGE('',*,*,#41311,.T.);
#52811=ORIENTED_EDGE('',*,*,#41312,.T.);
#52812=ORIENTED_EDGE('',*,*,#41311,.F.);
#52813=ORIENTED_EDGE('',*,*,#41313,.F.);
#52814=ORIENTED_EDGE('',*,*,#41314,.F.);
#52815=ORIENTED_EDGE('',*,*,#41315,.F.);
#52816=ORIENTED_EDGE('',*,*,#41316,.T.);
#52817=ORIENTED_EDGE('',*,*,#41317,.T.);
#52818=ORIENTED_EDGE('',*,*,#41318,.T.);
#52819=ORIENTED_EDGE('',*,*,#41316,.F.);
#52820=ORIENTED_EDGE('',*,*,#41318,.F.);
#52821=ORIENTED_EDGE('',*,*,#41319,.T.);
#52822=ORIENTED_EDGE('',*,*,#41320,.T.);
#52823=ORIENTED_EDGE('',*,*,#41319,.F.);
#52824=ORIENTED_EDGE('',*,*,#41317,.F.);
#52825=ORIENTED_EDGE('',*,*,#41321,.F.);
#52826=ORIENTED_EDGE('',*,*,#41322,.T.);
#52827=ORIENTED_EDGE('',*,*,#41323,.T.);
#52828=ORIENTED_EDGE('',*,*,#41322,.F.);
#52829=ORIENTED_EDGE('',*,*,#41324,.F.);
#52830=ORIENTED_EDGE('',*,*,#41325,.T.);
#52831=ORIENTED_EDGE('',*,*,#41326,.F.);
#52832=ORIENTED_EDGE('',*,*,#41327,.F.);
#52833=ORIENTED_EDGE('',*,*,#41328,.F.);
#52834=ORIENTED_EDGE('',*,*,#41329,.F.);
#52835=ORIENTED_EDGE('',*,*,#41330,.F.);
#52836=ORIENTED_EDGE('',*,*,#41331,.F.);
#52837=ORIENTED_EDGE('',*,*,#41325,.F.);
#52838=ORIENTED_EDGE('',*,*,#41332,.F.);
#52839=ORIENTED_EDGE('',*,*,#41333,.F.);
#52840=ORIENTED_EDGE('',*,*,#41334,.T.);
#52841=ORIENTED_EDGE('',*,*,#41335,.T.);
#52842=ORIENTED_EDGE('',*,*,#41334,.F.);
#52843=ORIENTED_EDGE('',*,*,#41336,.F.);
#52844=ORIENTED_EDGE('',*,*,#41337,.T.);
#52845=ORIENTED_EDGE('',*,*,#41332,.T.);
#52846=ORIENTED_EDGE('',*,*,#41333,.T.);
#52847=ORIENTED_EDGE('',*,*,#41337,.F.);
#52848=ORIENTED_EDGE('',*,*,#41338,.F.);
#52849=ORIENTED_EDGE('',*,*,#41339,.T.);
#52850=ORIENTED_EDGE('',*,*,#41340,.T.);
#52851=ORIENTED_EDGE('',*,*,#41339,.F.);
#52852=ORIENTED_EDGE('',*,*,#41341,.F.);
#52853=ORIENTED_EDGE('',*,*,#41342,.F.);
#52854=ORIENTED_EDGE('',*,*,#41343,.F.);
#52855=ORIENTED_EDGE('',*,*,#41344,.T.);
#52856=ORIENTED_EDGE('',*,*,#41341,.T.);
#52857=ORIENTED_EDGE('',*,*,#41338,.T.);
#52858=ORIENTED_EDGE('',*,*,#41344,.F.);
#52859=ORIENTED_EDGE('',*,*,#41345,.T.);
#52860=ORIENTED_EDGE('',*,*,#41346,.T.);
#52861=ORIENTED_EDGE('',*,*,#41347,.F.);
#52862=ORIENTED_EDGE('',*,*,#41348,.T.);
#52863=ORIENTED_EDGE('',*,*,#41349,.T.);
#52864=ORIENTED_EDGE('',*,*,#41350,.T.);
#52865=ORIENTED_EDGE('',*,*,#41351,.T.);
#52866=ORIENTED_EDGE('',*,*,#41352,.T.);
#52867=ORIENTED_EDGE('',*,*,#41188,.T.);
#52868=ORIENTED_EDGE('',*,*,#41353,.T.);
#52869=ORIENTED_EDGE('',*,*,#41185,.F.);
#52870=ORIENTED_EDGE('',*,*,#41354,.T.);
#52871=ORIENTED_EDGE('',*,*,#41355,.T.);
#52872=ORIENTED_EDGE('',*,*,#41356,.T.);
#52873=ORIENTED_EDGE('',*,*,#41357,.T.);
#52874=ORIENTED_EDGE('',*,*,#41356,.F.);
#52875=ORIENTED_EDGE('',*,*,#41358,.T.);
#52876=ORIENTED_EDGE('',*,*,#41355,.F.);
#52877=ORIENTED_EDGE('',*,*,#41359,.T.);
#52878=ORIENTED_EDGE('',*,*,#41182,.F.);
#52879=ORIENTED_EDGE('',*,*,#41183,.F.);
#52880=ORIENTED_EDGE('',*,*,#41359,.F.);
#52881=ORIENTED_EDGE('',*,*,#41358,.F.);
#52882=ORIENTED_EDGE('',*,*,#41360,.F.);
#52883=ORIENTED_EDGE('',*,*,#41361,.F.);
#52884=ORIENTED_EDGE('',*,*,#41362,.T.);
#52885=ORIENTED_EDGE('',*,*,#41363,.F.);
#52886=ORIENTED_EDGE('',*,*,#41362,.F.);
#52887=ORIENTED_EDGE('',*,*,#41364,.F.);
#52888=ORIENTED_EDGE('',*,*,#41190,.F.);
#52889=ORIENTED_EDGE('',*,*,#41365,.F.);
#52890=ORIENTED_EDGE('',*,*,#41175,.F.);
#52891=ORIENTED_EDGE('',*,*,#41174,.T.);
#52892=ORIENTED_EDGE('',*,*,#41366,.T.);
#52893=ORIENTED_EDGE('',*,*,#41171,.F.);
#52894=ORIENTED_EDGE('',*,*,#41367,.T.);
#52895=ORIENTED_EDGE('',*,*,#41360,.T.);
#52896=ORIENTED_EDGE('',*,*,#41368,.F.);
#52897=ORIENTED_EDGE('',*,*,#41369,.T.);
#52898=ORIENTED_EDGE('',*,*,#41370,.T.);
#52899=ORIENTED_EDGE('',*,*,#41371,.T.);
#52900=ORIENTED_EDGE('',*,*,#41369,.F.);
#52901=ORIENTED_EDGE('',*,*,#41370,.F.);
#52902=ORIENTED_EDGE('',*,*,#41371,.F.);
#52903=ORIENTED_EDGE('',*,*,#41372,.T.);
#52904=ORIENTED_EDGE('',*,*,#41373,.F.);
#52905=ORIENTED_EDGE('',*,*,#41372,.F.);
#52906=ORIENTED_EDGE('',*,*,#41374,.F.);
#52907=ORIENTED_EDGE('',*,*,#41375,.F.);
#52908=ORIENTED_EDGE('',*,*,#41159,.F.);
#52909=ORIENTED_EDGE('',*,*,#41376,.F.);
#52910=ORIENTED_EDGE('',*,*,#41377,.F.);
#52911=ORIENTED_EDGE('',*,*,#41378,.F.);
#52912=ORIENTED_EDGE('',*,*,#41157,.T.);
#52913=ORIENTED_EDGE('',*,*,#41379,.F.);
#52914=ORIENTED_EDGE('',*,*,#41380,.T.);
#52915=ORIENTED_EDGE('',*,*,#41381,.T.);
#52916=ORIENTED_EDGE('',*,*,#41153,.F.);
#52917=ORIENTED_EDGE('',*,*,#41382,.T.);
#52918=ORIENTED_EDGE('',*,*,#41383,.T.);
#52919=ORIENTED_EDGE('',*,*,#41384,.T.);
#52920=ORIENTED_EDGE('',*,*,#41385,.T.);
#52921=ORIENTED_EDGE('',*,*,#41386,.T.);
#52922=ORIENTED_EDGE('',*,*,#41387,.T.);
#52923=ORIENTED_EDGE('',*,*,#41388,.T.);
#52924=ORIENTED_EDGE('',*,*,#41389,.T.);
#52925=ORIENTED_EDGE('',*,*,#41390,.T.);
#52926=ORIENTED_EDGE('',*,*,#41389,.F.);
#52927=ORIENTED_EDGE('',*,*,#41391,.T.);
#52928=ORIENTED_EDGE('',*,*,#41392,.T.);
#52929=ORIENTED_EDGE('',*,*,#41393,.T.);
#52930=ORIENTED_EDGE('',*,*,#41394,.F.);
#52931=ORIENTED_EDGE('',*,*,#41395,.T.);
#52932=ORIENTED_EDGE('',*,*,#41396,.F.);
#52933=ORIENTED_EDGE('',*,*,#41397,.T.);
#52934=ORIENTED_EDGE('',*,*,#41398,.T.);
#52935=ORIENTED_EDGE('',*,*,#41399,.T.);
#52936=ORIENTED_EDGE('',*,*,#41400,.T.);
#52937=ORIENTED_EDGE('',*,*,#41401,.T.);
#52938=ORIENTED_EDGE('',*,*,#41402,.F.);
#52939=ORIENTED_EDGE('',*,*,#41403,.F.);
#52940=ORIENTED_EDGE('',*,*,#41404,.F.);
#52941=ORIENTED_EDGE('',*,*,#41405,.T.);
#52942=ORIENTED_EDGE('',*,*,#41406,.F.);
#52943=ORIENTED_EDGE('',*,*,#41407,.T.);
#52944=ORIENTED_EDGE('',*,*,#41408,.F.);
#52945=ORIENTED_EDGE('',*,*,#41407,.F.);
#52946=ORIENTED_EDGE('',*,*,#41409,.T.);
#52947=ORIENTED_EDGE('',*,*,#41410,.T.);
#52948=ORIENTED_EDGE('',*,*,#41411,.T.);
#52949=ORIENTED_EDGE('',*,*,#41410,.F.);
#52950=ORIENTED_EDGE('',*,*,#41412,.T.);
#52951=ORIENTED_EDGE('',*,*,#41409,.F.);
#52952=ORIENTED_EDGE('',*,*,#41413,.T.);
#52953=ORIENTED_EDGE('',*,*,#41414,.F.);
#52954=ORIENTED_EDGE('',*,*,#41413,.F.);
#52955=ORIENTED_EDGE('',*,*,#41412,.F.);
#52956=ORIENTED_EDGE('',*,*,#41415,.T.);
#52957=ORIENTED_EDGE('',*,*,#41416,.T.);
#52958=ORIENTED_EDGE('',*,*,#41417,.F.);
#52959=ORIENTED_EDGE('',*,*,#41418,.F.);
#52960=ORIENTED_EDGE('',*,*,#41416,.F.);
#52961=ORIENTED_EDGE('',*,*,#41419,.T.);
#52962=ORIENTED_EDGE('',*,*,#41420,.F.);
#52963=ORIENTED_EDGE('',*,*,#41421,.F.);
#52964=ORIENTED_EDGE('',*,*,#41422,.F.);
#52965=ORIENTED_EDGE('',*,*,#41423,.F.);
#52966=ORIENTED_EDGE('',*,*,#41424,.T.);
#52967=ORIENTED_EDGE('',*,*,#41417,.T.);
#52968=ORIENTED_EDGE('',*,*,#41418,.T.);
#52969=ORIENTED_EDGE('',*,*,#41424,.F.);
#52970=ORIENTED_EDGE('',*,*,#41425,.F.);
#52971=ORIENTED_EDGE('',*,*,#41426,.F.);
#52972=ORIENTED_EDGE('',*,*,#41427,.F.);
#52973=ORIENTED_EDGE('',*,*,#41415,.F.);
#52974=ORIENTED_EDGE('',*,*,#41428,.T.);
#52975=ORIENTED_EDGE('',*,*,#41429,.F.);
#52976=ORIENTED_EDGE('',*,*,#41428,.F.);
#52977=ORIENTED_EDGE('',*,*,#41419,.F.);
#52978=ORIENTED_EDGE('',*,*,#41430,.T.);
#52979=ORIENTED_EDGE('',*,*,#41431,.T.);
#52980=ORIENTED_EDGE('',*,*,#41432,.T.);
#52981=ORIENTED_EDGE('',*,*,#41433,.T.);
#52982=ORIENTED_EDGE('',*,*,#41432,.F.);
#52983=ORIENTED_EDGE('',*,*,#41434,.F.);
#52984=ORIENTED_EDGE('',*,*,#41435,.T.);
#52985=ORIENTED_EDGE('',*,*,#41430,.F.);
#52986=ORIENTED_EDGE('',*,*,#41431,.F.);
#52987=ORIENTED_EDGE('',*,*,#41435,.F.);
#52988=ORIENTED_EDGE('',*,*,#41137,.F.);
#52989=ORIENTED_EDGE('',*,*,#41436,.F.);
#52990=ORIENTED_EDGE('',*,*,#41437,.F.);
#52991=ORIENTED_EDGE('',*,*,#41438,.F.);
#52992=ORIENTED_EDGE('',*,*,#41439,.F.);
#52993=ORIENTED_EDGE('',*,*,#41440,.F.);
#52994=ORIENTED_EDGE('',*,*,#41144,.T.);
#52995=ORIENTED_EDGE('',*,*,#41441,.T.);
#52996=ORIENTED_EDGE('',*,*,#41442,.F.);
#52997=ORIENTED_EDGE('',*,*,#41443,.F.);
#52998=ORIENTED_EDGE('',*,*,#41444,.T.);
#52999=ORIENTED_EDGE('',*,*,#41445,.T.);
#53000=ORIENTED_EDGE('',*,*,#41446,.T.);
#53001=ORIENTED_EDGE('',*,*,#41447,.T.);
#53002=ORIENTED_EDGE('',*,*,#41448,.T.);
#53003=ORIENTED_EDGE('',*,*,#41449,.T.);
#53004=ORIENTED_EDGE('',*,*,#41450,.T.);
#53005=ORIENTED_EDGE('',*,*,#41449,.F.);
#53006=ORIENTED_EDGE('',*,*,#41451,.T.);
#53007=ORIENTED_EDGE('',*,*,#41452,.T.);
#53008=ORIENTED_EDGE('',*,*,#41453,.T.);
#53009=ORIENTED_EDGE('',*,*,#41454,.T.);
#53010=ORIENTED_EDGE('',*,*,#41455,.T.);
#53011=ORIENTED_EDGE('',*,*,#41456,.T.);
#53012=ORIENTED_EDGE('',*,*,#41457,.T.);
#53013=ORIENTED_EDGE('',*,*,#41458,.T.);
#53014=ORIENTED_EDGE('',*,*,#41459,.F.);
#53015=ORIENTED_EDGE('',*,*,#41460,.T.);
#53016=ORIENTED_EDGE('',*,*,#41461,.F.);
#53017=ORIENTED_EDGE('',*,*,#41462,.T.);
#53018=ORIENTED_EDGE('',*,*,#41463,.F.);
#53019=ORIENTED_EDGE('',*,*,#41464,.F.);
#53020=ORIENTED_EDGE('',*,*,#41465,.F.);
#53021=ORIENTED_EDGE('',*,*,#41466,.T.);
#53022=ORIENTED_EDGE('',*,*,#41467,.T.);
#53023=ORIENTED_EDGE('',*,*,#41468,.F.);
#53024=ORIENTED_EDGE('',*,*,#41469,.T.);
#53025=ORIENTED_EDGE('',*,*,#41470,.F.);
#53026=ORIENTED_EDGE('',*,*,#41469,.F.);
#53027=ORIENTED_EDGE('',*,*,#41471,.T.);
#53028=ORIENTED_EDGE('',*,*,#41472,.T.);
#53029=ORIENTED_EDGE('',*,*,#41473,.T.);
#53030=ORIENTED_EDGE('',*,*,#41472,.F.);
#53031=ORIENTED_EDGE('',*,*,#41474,.T.);
#53032=ORIENTED_EDGE('',*,*,#41471,.F.);
#53033=ORIENTED_EDGE('',*,*,#41475,.T.);
#53034=ORIENTED_EDGE('',*,*,#41476,.F.);
#53035=ORIENTED_EDGE('',*,*,#41475,.F.);
#53036=ORIENTED_EDGE('',*,*,#41474,.F.);
#53037=ORIENTED_EDGE('',*,*,#41477,.T.);
#53038=ORIENTED_EDGE('',*,*,#41478,.T.);
#53039=ORIENTED_EDGE('',*,*,#41479,.F.);
#53040=ORIENTED_EDGE('',*,*,#41480,.F.);
#53041=ORIENTED_EDGE('',*,*,#41478,.F.);
#53042=ORIENTED_EDGE('',*,*,#41481,.T.);
#53043=ORIENTED_EDGE('',*,*,#41482,.F.);
#53044=ORIENTED_EDGE('',*,*,#41483,.F.);
#53045=ORIENTED_EDGE('',*,*,#41484,.F.);
#53046=ORIENTED_EDGE('',*,*,#41485,.F.);
#53047=ORIENTED_EDGE('',*,*,#41486,.T.);
#53048=ORIENTED_EDGE('',*,*,#41479,.T.);
#53049=ORIENTED_EDGE('',*,*,#41480,.T.);
#53050=ORIENTED_EDGE('',*,*,#41486,.F.);
#53051=ORIENTED_EDGE('',*,*,#41487,.F.);
#53052=ORIENTED_EDGE('',*,*,#41488,.F.);
#53053=ORIENTED_EDGE('',*,*,#41489,.F.);
#53054=ORIENTED_EDGE('',*,*,#41477,.F.);
#53055=ORIENTED_EDGE('',*,*,#41490,.T.);
#53056=ORIENTED_EDGE('',*,*,#41491,.F.);
#53057=ORIENTED_EDGE('',*,*,#41490,.F.);
#53058=ORIENTED_EDGE('',*,*,#41481,.F.);
#53059=ORIENTED_EDGE('',*,*,#41433,.F.);
#53060=ORIENTED_EDGE('',*,*,#41492,.T.);
#53061=ORIENTED_EDGE('',*,*,#41493,.T.);
#53062=ORIENTED_EDGE('',*,*,#41494,.T.);
#53063=ORIENTED_EDGE('',*,*,#41495,.T.);
#53064=ORIENTED_EDGE('',*,*,#41496,.T.);
#53065=ORIENTED_EDGE('',*,*,#41497,.T.);
#53066=ORIENTED_EDGE('',*,*,#41492,.F.);
#53067=ORIENTED_EDGE('',*,*,#41498,.T.);
#53068=ORIENTED_EDGE('',*,*,#41483,.T.);
#53069=ORIENTED_EDGE('',*,*,#41499,.F.);
#53070=ORIENTED_EDGE('',*,*,#41493,.F.);
#53071=ORIENTED_EDGE('',*,*,#41499,.T.);
#53072=ORIENTED_EDGE('',*,*,#41482,.T.);
#53073=ORIENTED_EDGE('',*,*,#41500,.F.);
#53074=ORIENTED_EDGE('',*,*,#41494,.F.);
#53075=ORIENTED_EDGE('',*,*,#41500,.T.);
#53076=ORIENTED_EDGE('',*,*,#41489,.T.);
#53077=ORIENTED_EDGE('',*,*,#41501,.F.);
#53078=ORIENTED_EDGE('',*,*,#41495,.F.);
#53079=ORIENTED_EDGE('',*,*,#41501,.T.);
#53080=ORIENTED_EDGE('',*,*,#41488,.T.);
#53081=ORIENTED_EDGE('',*,*,#41502,.F.);
#53082=ORIENTED_EDGE('',*,*,#41496,.F.);
#53083=ORIENTED_EDGE('',*,*,#41502,.T.);
#53084=ORIENTED_EDGE('',*,*,#41487,.T.);
#53085=ORIENTED_EDGE('',*,*,#41485,.T.);
#53086=ORIENTED_EDGE('',*,*,#41503,.F.);
#53087=ORIENTED_EDGE('',*,*,#41497,.F.);
#53088=ORIENTED_EDGE('',*,*,#41503,.T.);
#53089=ORIENTED_EDGE('',*,*,#41484,.T.);
#53090=ORIENTED_EDGE('',*,*,#41498,.F.);
#53091=ORIENTED_EDGE('',*,*,#41473,.F.);
#53092=ORIENTED_EDGE('',*,*,#41468,.T.);
#53093=ORIENTED_EDGE('',*,*,#41476,.T.);
#53094=ORIENTED_EDGE('',*,*,#41491,.T.);
#53095=ORIENTED_EDGE('',*,*,#41504,.F.);
#53096=ORIENTED_EDGE('',*,*,#41505,.T.);
#53097=ORIENTED_EDGE('',*,*,#41506,.T.);
#53098=ORIENTED_EDGE('',*,*,#41507,.T.);
#53099=ORIENTED_EDGE('',*,*,#41508,.F.);
#53100=ORIENTED_EDGE('',*,*,#41509,.T.);
#53101=ORIENTED_EDGE('',*,*,#41510,.T.);
#53102=ORIENTED_EDGE('',*,*,#41511,.F.);
#53103=ORIENTED_EDGE('',*,*,#41512,.T.);
#53104=ORIENTED_EDGE('',*,*,#41513,.T.);
#53105=ORIENTED_EDGE('',*,*,#41464,.T.);
#53106=ORIENTED_EDGE('',*,*,#41463,.T.);
#53107=ORIENTED_EDGE('',*,*,#41506,.F.);
#53108=ORIENTED_EDGE('',*,*,#41514,.T.);
#53109=ORIENTED_EDGE('',*,*,#41515,.T.);
#53110=ORIENTED_EDGE('',*,*,#41516,.F.);
#53111=ORIENTED_EDGE('',*,*,#41517,.T.);
#53112=ORIENTED_EDGE('',*,*,#41507,.F.);
#53113=ORIENTED_EDGE('',*,*,#41518,.T.);
#53114=ORIENTED_EDGE('',*,*,#41519,.F.);
#53115=ORIENTED_EDGE('',*,*,#41504,.T.);
#53116=ORIENTED_EDGE('',*,*,#41520,.T.);
#53117=ORIENTED_EDGE('',*,*,#41521,.T.);
#53118=ORIENTED_EDGE('',*,*,#41522,.T.);
#53119=ORIENTED_EDGE('',*,*,#41523,.F.);
#53120=ORIENTED_EDGE('',*,*,#41524,.F.);
#53121=ORIENTED_EDGE('',*,*,#41525,.T.);
#53122=ORIENTED_EDGE('',*,*,#41525,.F.);
#53123=ORIENTED_EDGE('',*,*,#41526,.F.);
#53124=ORIENTED_EDGE('',*,*,#41527,.T.);
#53125=ORIENTED_EDGE('',*,*,#41521,.F.);
#53126=ORIENTED_EDGE('',*,*,#41528,.T.);
#53127=ORIENTED_EDGE('',*,*,#41529,.T.);
#53128=ORIENTED_EDGE('',*,*,#41522,.F.);
#53129=ORIENTED_EDGE('',*,*,#41527,.F.);
#53130=ORIENTED_EDGE('',*,*,#41530,.T.);
#53131=ORIENTED_EDGE('',*,*,#41531,.T.);
#53132=ORIENTED_EDGE('',*,*,#41514,.F.);
#53133=ORIENTED_EDGE('',*,*,#41505,.F.);
#53134=ORIENTED_EDGE('',*,*,#41519,.T.);
#53135=ORIENTED_EDGE('',*,*,#41529,.F.);
#53136=ORIENTED_EDGE('',*,*,#41532,.T.);
#53137=ORIENTED_EDGE('',*,*,#41533,.T.);
#53138=ORIENTED_EDGE('',*,*,#41534,.T.);
#53139=ORIENTED_EDGE('',*,*,#41509,.F.);
#53140=ORIENTED_EDGE('',*,*,#41535,.F.);
#53141=ORIENTED_EDGE('',*,*,#41536,.F.);
#53142=ORIENTED_EDGE('',*,*,#41537,.F.);
#53143=ORIENTED_EDGE('',*,*,#41538,.F.);
#53144=ORIENTED_EDGE('',*,*,#41539,.T.);
#53145=ORIENTED_EDGE('',*,*,#41540,.F.);
#53146=ORIENTED_EDGE('',*,*,#41536,.T.);
#53147=ORIENTED_EDGE('',*,*,#41541,.F.);
#53148=ORIENTED_EDGE('',*,*,#41542,.T.);
#53149=ORIENTED_EDGE('',*,*,#41543,.F.);
#53150=ORIENTED_EDGE('',*,*,#41512,.F.);
#53151=ORIENTED_EDGE('',*,*,#41544,.F.);
#53152=ORIENTED_EDGE('',*,*,#41530,.F.);
#53153=ORIENTED_EDGE('',*,*,#41542,.F.);
#53154=ORIENTED_EDGE('',*,*,#41545,.F.);
#53155=ORIENTED_EDGE('',*,*,#41508,.T.);
#53156=ORIENTED_EDGE('',*,*,#41546,.T.);
#53157=ORIENTED_EDGE('',*,*,#41547,.T.);
#53158=ORIENTED_EDGE('',*,*,#41548,.T.);
#53159=ORIENTED_EDGE('',*,*,#41533,.F.);
#53160=ORIENTED_EDGE('',*,*,#41549,.F.);
#53161=ORIENTED_EDGE('',*,*,#41534,.F.);
#53162=ORIENTED_EDGE('',*,*,#41550,.F.);
#53163=ORIENTED_EDGE('',*,*,#41551,.F.);
#53164=ORIENTED_EDGE('',*,*,#41552,.F.);
#53165=ORIENTED_EDGE('',*,*,#41510,.F.);
#53166=ORIENTED_EDGE('',*,*,#41551,.T.);
#53167=ORIENTED_EDGE('',*,*,#41553,.F.);
#53168=ORIENTED_EDGE('',*,*,#41554,.F.);
#53169=ORIENTED_EDGE('',*,*,#41555,.T.);
#53170=ORIENTED_EDGE('',*,*,#41513,.F.);
#53171=ORIENTED_EDGE('',*,*,#41543,.T.);
#53172=ORIENTED_EDGE('',*,*,#41546,.F.);
#53173=ORIENTED_EDGE('',*,*,#41552,.T.);
#53174=ORIENTED_EDGE('',*,*,#41556,.T.);
#53175=ORIENTED_EDGE('',*,*,#41557,.T.);
#53176=ORIENTED_EDGE('',*,*,#41558,.T.);
#53177=ORIENTED_EDGE('',*,*,#41559,.F.);
#53178=ORIENTED_EDGE('',*,*,#41560,.F.);
#53179=ORIENTED_EDGE('',*,*,#41561,.T.);
#53180=ORIENTED_EDGE('',*,*,#41562,.T.);
#53181=ORIENTED_EDGE('',*,*,#41466,.F.);
#53182=ORIENTED_EDGE('',*,*,#41558,.F.);
#53183=ORIENTED_EDGE('',*,*,#41563,.T.);
#53184=ORIENTED_EDGE('',*,*,#41564,.T.);
#53185=ORIENTED_EDGE('',*,*,#41565,.F.);
#53186=ORIENTED_EDGE('',*,*,#41562,.F.);
#53187=ORIENTED_EDGE('',*,*,#41566,.T.);
#53188=ORIENTED_EDGE('',*,*,#41531,.F.);
#53189=ORIENTED_EDGE('',*,*,#41544,.T.);
#53190=ORIENTED_EDGE('',*,*,#41511,.T.);
#53191=ORIENTED_EDGE('',*,*,#41567,.T.);
#53192=ORIENTED_EDGE('',*,*,#41568,.F.);
#53193=ORIENTED_EDGE('',*,*,#41515,.F.);
#53194=ORIENTED_EDGE('',*,*,#41568,.T.);
#53195=ORIENTED_EDGE('',*,*,#41569,.T.);
#53196=ORIENTED_EDGE('',*,*,#41570,.F.);
#53197=ORIENTED_EDGE('',*,*,#41571,.F.);
#53198=ORIENTED_EDGE('',*,*,#41516,.T.);
#53199=ORIENTED_EDGE('',*,*,#41571,.T.);
#53200=ORIENTED_EDGE('',*,*,#41572,.T.);
#53201=ORIENTED_EDGE('',*,*,#41573,.F.);
#53202=ORIENTED_EDGE('',*,*,#41518,.F.);
#53203=ORIENTED_EDGE('',*,*,#41523,.T.);
#53204=ORIENTED_EDGE('',*,*,#41520,.F.);
#53205=ORIENTED_EDGE('',*,*,#41517,.F.);
#53206=ORIENTED_EDGE('',*,*,#41574,.T.);
#53207=ORIENTED_EDGE('',*,*,#41526,.T.);
#53208=ORIENTED_EDGE('',*,*,#41524,.T.);
#53209=ORIENTED_EDGE('',*,*,#41575,.T.);
#53210=ORIENTED_EDGE('',*,*,#41576,.T.);
#53211=ORIENTED_EDGE('',*,*,#41577,.F.);
#53212=ORIENTED_EDGE('',*,*,#41537,.T.);
#53213=ORIENTED_EDGE('',*,*,#41540,.T.);
#53214=ORIENTED_EDGE('',*,*,#41532,.F.);
#53215=ORIENTED_EDGE('',*,*,#41528,.F.);
#53216=ORIENTED_EDGE('',*,*,#41577,.T.);
#53217=ORIENTED_EDGE('',*,*,#41578,.T.);
#53218=ORIENTED_EDGE('',*,*,#41579,.T.);
#53219=ORIENTED_EDGE('',*,*,#41538,.T.);
#53220=ORIENTED_EDGE('',*,*,#41580,.F.);
#53221=ORIENTED_EDGE('',*,*,#41581,.T.);
#53222=ORIENTED_EDGE('',*,*,#41545,.T.);
#53223=ORIENTED_EDGE('',*,*,#41541,.T.);
#53224=ORIENTED_EDGE('',*,*,#41539,.F.);
#53225=ORIENTED_EDGE('',*,*,#41582,.F.);
#53226=ORIENTED_EDGE('',*,*,#41583,.T.);
#53227=ORIENTED_EDGE('',*,*,#41549,.T.);
#53228=ORIENTED_EDGE('',*,*,#41535,.T.);
#53229=ORIENTED_EDGE('',*,*,#41584,.T.);
#53230=ORIENTED_EDGE('',*,*,#41585,.T.);
#53231=ORIENTED_EDGE('',*,*,#41547,.F.);
#53232=ORIENTED_EDGE('',*,*,#41583,.F.);
#53233=ORIENTED_EDGE('',*,*,#41586,.T.);
#53234=ORIENTED_EDGE('',*,*,#41587,.T.);
#53235=ORIENTED_EDGE('',*,*,#41553,.T.);
#53236=ORIENTED_EDGE('',*,*,#41550,.T.);
#53237=ORIENTED_EDGE('',*,*,#41548,.F.);
#53238=ORIENTED_EDGE('',*,*,#41588,.T.);
#53239=ORIENTED_EDGE('',*,*,#41584,.F.);
#53240=ORIENTED_EDGE('',*,*,#41589,.F.);
#53241=ORIENTED_EDGE('',*,*,#41554,.T.);
#53242=ORIENTED_EDGE('',*,*,#41587,.F.);
#53243=ORIENTED_EDGE('',*,*,#41590,.F.);
#53244=ORIENTED_EDGE('',*,*,#41591,.T.);
#53245=ORIENTED_EDGE('',*,*,#41592,.T.);
#53246=ORIENTED_EDGE('',*,*,#41556,.F.);
#53247=ORIENTED_EDGE('',*,*,#41555,.F.);
#53248=ORIENTED_EDGE('',*,*,#41465,.T.);
#53249=ORIENTED_EDGE('',*,*,#41557,.F.);
#53250=ORIENTED_EDGE('',*,*,#41593,.F.);
#53251=ORIENTED_EDGE('',*,*,#41559,.T.);
#53252=ORIENTED_EDGE('',*,*,#41560,.T.);
#53253=ORIENTED_EDGE('',*,*,#41594,.F.);
#53254=ORIENTED_EDGE('',*,*,#41595,.F.);
#53255=ORIENTED_EDGE('',*,*,#41596,.T.);
#53256=ORIENTED_EDGE('',*,*,#41596,.F.);
#53257=ORIENTED_EDGE('',*,*,#41597,.F.);
#53258=ORIENTED_EDGE('',*,*,#41598,.F.);
#53259=ORIENTED_EDGE('',*,*,#41566,.F.);
#53260=ORIENTED_EDGE('',*,*,#41563,.F.);
#53261=ORIENTED_EDGE('',*,*,#41561,.F.);
#53262=ORIENTED_EDGE('',*,*,#41599,.T.);
#53263=ORIENTED_EDGE('',*,*,#41600,.F.);
#53264=ORIENTED_EDGE('',*,*,#41564,.F.);
#53265=ORIENTED_EDGE('',*,*,#41598,.T.);
#53266=ORIENTED_EDGE('',*,*,#41601,.F.);
#53267=ORIENTED_EDGE('',*,*,#41569,.F.);
#53268=ORIENTED_EDGE('',*,*,#41567,.F.);
#53269=ORIENTED_EDGE('',*,*,#41467,.F.);
#53270=ORIENTED_EDGE('',*,*,#41565,.T.);
#53271=ORIENTED_EDGE('',*,*,#41572,.F.);
#53272=ORIENTED_EDGE('',*,*,#41570,.T.);
#53273=ORIENTED_EDGE('',*,*,#41602,.T.);
#53274=ORIENTED_EDGE('',*,*,#41574,.F.);
#53275=ORIENTED_EDGE('',*,*,#41573,.T.);
#53276=ORIENTED_EDGE('',*,*,#41603,.F.);
#53277=ORIENTED_EDGE('',*,*,#41575,.F.);
#53278=ORIENTED_EDGE('',*,*,#41604,.T.);
#53279=ORIENTED_EDGE('',*,*,#41578,.F.);
#53280=ORIENTED_EDGE('',*,*,#41576,.F.);
#53281=ORIENTED_EDGE('',*,*,#41605,.T.);
#53282=ORIENTED_EDGE('',*,*,#41580,.T.);
#53283=ORIENTED_EDGE('',*,*,#41579,.F.);
#53284=ORIENTED_EDGE('',*,*,#41604,.F.);
#53285=ORIENTED_EDGE('',*,*,#41461,.T.);
#53286=ORIENTED_EDGE('',*,*,#41582,.T.);
#53287=ORIENTED_EDGE('',*,*,#41581,.F.);
#53288=ORIENTED_EDGE('',*,*,#41460,.F.);
#53289=ORIENTED_EDGE('',*,*,#41589,.T.);
#53290=ORIENTED_EDGE('',*,*,#41588,.F.);
#53291=ORIENTED_EDGE('',*,*,#41459,.T.);
#53292=ORIENTED_EDGE('',*,*,#41590,.T.);
#53293=ORIENTED_EDGE('',*,*,#41586,.F.);
#53294=ORIENTED_EDGE('',*,*,#41585,.F.);
#53295=ORIENTED_EDGE('',*,*,#41594,.T.);
#53296=ORIENTED_EDGE('',*,*,#41593,.T.);
#53297=ORIENTED_EDGE('',*,*,#41592,.F.);
#53298=ORIENTED_EDGE('',*,*,#41591,.F.);
#53299=ORIENTED_EDGE('',*,*,#41458,.F.);
#53300=ORIENTED_EDGE('',*,*,#41606,.T.);
#53301=ORIENTED_EDGE('',*,*,#41607,.F.);
#53302=ORIENTED_EDGE('',*,*,#41607,.T.);
#53303=ORIENTED_EDGE('',*,*,#41608,.T.);
#53304=ORIENTED_EDGE('',*,*,#41609,.T.);
#53305=ORIENTED_EDGE('',*,*,#41599,.F.);
#53306=ORIENTED_EDGE('',*,*,#41597,.T.);
#53307=ORIENTED_EDGE('',*,*,#41595,.T.);
#53308=ORIENTED_EDGE('',*,*,#41609,.F.);
#53309=ORIENTED_EDGE('',*,*,#41610,.T.);
#53310=ORIENTED_EDGE('',*,*,#41611,.F.);
#53311=ORIENTED_EDGE('',*,*,#41612,.T.);
#53312=ORIENTED_EDGE('',*,*,#41613,.T.);
#53313=ORIENTED_EDGE('',*,*,#41611,.T.);
#53314=ORIENTED_EDGE('',*,*,#41605,.F.);
#53315=ORIENTED_EDGE('',*,*,#41603,.T.);
#53316=ORIENTED_EDGE('',*,*,#41602,.F.);
#53317=ORIENTED_EDGE('',*,*,#41601,.T.);
#53318=ORIENTED_EDGE('',*,*,#41600,.T.);
#53319=ORIENTED_EDGE('',*,*,#41613,.F.);
#53320=ORIENTED_EDGE('',*,*,#41614,.T.);
#53321=ORIENTED_EDGE('',*,*,#41615,.T.);
#53322=ORIENTED_EDGE('',*,*,#41462,.F.);
#53323=ORIENTED_EDGE('',*,*,#41616,.F.);
#53324=ORIENTED_EDGE('',*,*,#41606,.F.);
#53325=ORIENTED_EDGE('',*,*,#41617,.T.);
#53326=ORIENTED_EDGE('',*,*,#41618,.F.);
#53327=ORIENTED_EDGE('',*,*,#41619,.F.);
#53328=ORIENTED_EDGE('',*,*,#41620,.F.);
#53329=ORIENTED_EDGE('',*,*,#41608,.F.);
#53330=ORIENTED_EDGE('',*,*,#41616,.T.);
#53331=ORIENTED_EDGE('',*,*,#41621,.F.);
#53332=ORIENTED_EDGE('',*,*,#41622,.F.);
#53333=ORIENTED_EDGE('',*,*,#41610,.F.);
#53334=ORIENTED_EDGE('',*,*,#41620,.T.);
#53335=ORIENTED_EDGE('',*,*,#41623,.F.);
#53336=ORIENTED_EDGE('',*,*,#41624,.F.);
#53337=ORIENTED_EDGE('',*,*,#41612,.F.);
#53338=ORIENTED_EDGE('',*,*,#41622,.T.);
#53339=ORIENTED_EDGE('',*,*,#41625,.F.);
#53340=ORIENTED_EDGE('',*,*,#41626,.F.);
#53341=ORIENTED_EDGE('',*,*,#41614,.F.);
#53342=ORIENTED_EDGE('',*,*,#41624,.T.);
#53343=ORIENTED_EDGE('',*,*,#41627,.F.);
#53344=ORIENTED_EDGE('',*,*,#41628,.F.);
#53345=ORIENTED_EDGE('',*,*,#41615,.F.);
#53346=ORIENTED_EDGE('',*,*,#41626,.T.);
#53347=ORIENTED_EDGE('',*,*,#41629,.F.);
#53348=ORIENTED_EDGE('',*,*,#41630,.F.);
#53349=ORIENTED_EDGE('',*,*,#41456,.F.);
#53350=ORIENTED_EDGE('',*,*,#41628,.T.);
#53351=ORIENTED_EDGE('',*,*,#41631,.F.);
#53352=ORIENTED_EDGE('',*,*,#41617,.F.);
#53353=ORIENTED_EDGE('',*,*,#41457,.F.);
#53354=ORIENTED_EDGE('',*,*,#41630,.T.);
#53355=ORIENTED_EDGE('',*,*,#41632,.F.);
#53356=ORIENTED_EDGE('',*,*,#41633,.T.);
#53357=ORIENTED_EDGE('',*,*,#41445,.F.);
#53358=ORIENTED_EDGE('',*,*,#41634,.F.);
#53359=ORIENTED_EDGE('',*,*,#41618,.T.);
#53360=ORIENTED_EDGE('',*,*,#41634,.T.);
#53361=ORIENTED_EDGE('',*,*,#41455,.F.);
#53362=ORIENTED_EDGE('',*,*,#41635,.F.);
#53363=ORIENTED_EDGE('',*,*,#41619,.T.);
#53364=ORIENTED_EDGE('',*,*,#41635,.T.);
#53365=ORIENTED_EDGE('',*,*,#41454,.F.);
#53366=ORIENTED_EDGE('',*,*,#41636,.F.);
#53367=ORIENTED_EDGE('',*,*,#41621,.T.);
#53368=ORIENTED_EDGE('',*,*,#41636,.T.);
#53369=ORIENTED_EDGE('',*,*,#41453,.F.);
#53370=ORIENTED_EDGE('',*,*,#41637,.F.);
#53371=ORIENTED_EDGE('',*,*,#41623,.T.);
#53372=ORIENTED_EDGE('',*,*,#41637,.T.);
#53373=ORIENTED_EDGE('',*,*,#41452,.F.);
#53374=ORIENTED_EDGE('',*,*,#41638,.F.);
#53375=ORIENTED_EDGE('',*,*,#41625,.T.);
#53376=ORIENTED_EDGE('',*,*,#41638,.T.);
#53377=ORIENTED_EDGE('',*,*,#41451,.F.);
#53378=ORIENTED_EDGE('',*,*,#41639,.F.);
#53379=ORIENTED_EDGE('',*,*,#41627,.T.);
#53380=ORIENTED_EDGE('',*,*,#41639,.T.);
#53381=ORIENTED_EDGE('',*,*,#41448,.F.);
#53382=ORIENTED_EDGE('',*,*,#41640,.F.);
#53383=ORIENTED_EDGE('',*,*,#41629,.T.);
#53384=ORIENTED_EDGE('',*,*,#41640,.T.);
#53385=ORIENTED_EDGE('',*,*,#41447,.F.);
#53386=ORIENTED_EDGE('',*,*,#41641,.F.);
#53387=ORIENTED_EDGE('',*,*,#41631,.T.);
#53388=ORIENTED_EDGE('',*,*,#41641,.T.);
#53389=ORIENTED_EDGE('',*,*,#41446,.F.);
#53390=ORIENTED_EDGE('',*,*,#41633,.F.);
#53391=ORIENTED_EDGE('',*,*,#41632,.T.);
#53392=ORIENTED_EDGE('',*,*,#41450,.F.);
#53393=ORIENTED_EDGE('',*,*,#41642,.T.);
#53394=ORIENTED_EDGE('',*,*,#41643,.T.);
#53395=ORIENTED_EDGE('',*,*,#41443,.T.);
#53396=ORIENTED_EDGE('',*,*,#41644,.T.);
#53397=ORIENTED_EDGE('',*,*,#41645,.T.);
#53398=ORIENTED_EDGE('',*,*,#41644,.F.);
#53399=ORIENTED_EDGE('',*,*,#41442,.T.);
#53400=ORIENTED_EDGE('',*,*,#41441,.F.);
#53401=ORIENTED_EDGE('',*,*,#41147,.F.);
#53402=ORIENTED_EDGE('',*,*,#41646,.T.);
#53403=ORIENTED_EDGE('',*,*,#41647,.T.);
#53404=ORIENTED_EDGE('',*,*,#41648,.T.);
#53405=ORIENTED_EDGE('',*,*,#41642,.F.);
#53406=ORIENTED_EDGE('',*,*,#41645,.F.);
#53407=ORIENTED_EDGE('',*,*,#41145,.F.);
#53408=ORIENTED_EDGE('',*,*,#41444,.F.);
#53409=ORIENTED_EDGE('',*,*,#41643,.F.);
#53410=ORIENTED_EDGE('',*,*,#41648,.F.);
#53411=ORIENTED_EDGE('',*,*,#41649,.T.);
#53412=ORIENTED_EDGE('',*,*,#41141,.F.);
#53413=ORIENTED_EDGE('',*,*,#41138,.F.);
#53414=ORIENTED_EDGE('',*,*,#41440,.T.);
#53415=ORIENTED_EDGE('',*,*,#41439,.T.);
#53416=ORIENTED_EDGE('',*,*,#41650,.F.);
#53417=ORIENTED_EDGE('',*,*,#41651,.T.);
#53418=ORIENTED_EDGE('',*,*,#41646,.F.);
#53419=ORIENTED_EDGE('',*,*,#41146,.F.);
#53420=ORIENTED_EDGE('',*,*,#41139,.F.);
#53421=ORIENTED_EDGE('',*,*,#41652,.F.);
#53422=ORIENTED_EDGE('',*,*,#41653,.T.);
#53423=ORIENTED_EDGE('',*,*,#41647,.F.);
#53424=ORIENTED_EDGE('',*,*,#41651,.F.);
#53425=ORIENTED_EDGE('',*,*,#41653,.F.);
#53426=ORIENTED_EDGE('',*,*,#41654,.F.);
#53427=ORIENTED_EDGE('',*,*,#41437,.T.);
#53428=ORIENTED_EDGE('',*,*,#41436,.T.);
#53429=ORIENTED_EDGE('',*,*,#41136,.F.);
#53430=ORIENTED_EDGE('',*,*,#41143,.F.);
#53431=ORIENTED_EDGE('',*,*,#41142,.F.);
#53432=ORIENTED_EDGE('',*,*,#41649,.F.);
#53433=ORIENTED_EDGE('',*,*,#41434,.T.);
#53434=ORIENTED_EDGE('',*,*,#41438,.T.);
#53435=ORIENTED_EDGE('',*,*,#41654,.T.);
#53436=ORIENTED_EDGE('',*,*,#41652,.T.);
#53437=ORIENTED_EDGE('',*,*,#41650,.T.);
#53438=ORIENTED_EDGE('',*,*,#41368,.T.);
#53439=ORIENTED_EDGE('',*,*,#41655,.T.);
#53440=ORIENTED_EDGE('',*,*,#41656,.T.);
#53441=ORIENTED_EDGE('',*,*,#41657,.T.);
#53442=ORIENTED_EDGE('',*,*,#41658,.T.);
#53443=ORIENTED_EDGE('',*,*,#41659,.T.);
#53444=ORIENTED_EDGE('',*,*,#41660,.T.);
#53445=ORIENTED_EDGE('',*,*,#41655,.F.);
#53446=ORIENTED_EDGE('',*,*,#41661,.T.);
#53447=ORIENTED_EDGE('',*,*,#41421,.T.);
#53448=ORIENTED_EDGE('',*,*,#41662,.F.);
#53449=ORIENTED_EDGE('',*,*,#41656,.F.);
#53450=ORIENTED_EDGE('',*,*,#41662,.T.);
#53451=ORIENTED_EDGE('',*,*,#41420,.T.);
#53452=ORIENTED_EDGE('',*,*,#41663,.F.);
#53453=ORIENTED_EDGE('',*,*,#41657,.F.);
#53454=ORIENTED_EDGE('',*,*,#41663,.T.);
#53455=ORIENTED_EDGE('',*,*,#41427,.T.);
#53456=ORIENTED_EDGE('',*,*,#41664,.F.);
#53457=ORIENTED_EDGE('',*,*,#41658,.F.);
#53458=ORIENTED_EDGE('',*,*,#41664,.T.);
#53459=ORIENTED_EDGE('',*,*,#41426,.T.);
#53460=ORIENTED_EDGE('',*,*,#41665,.F.);
#53461=ORIENTED_EDGE('',*,*,#41659,.F.);
#53462=ORIENTED_EDGE('',*,*,#41665,.T.);
#53463=ORIENTED_EDGE('',*,*,#41425,.T.);
#53464=ORIENTED_EDGE('',*,*,#41423,.T.);
#53465=ORIENTED_EDGE('',*,*,#41666,.F.);
#53466=ORIENTED_EDGE('',*,*,#41660,.F.);
#53467=ORIENTED_EDGE('',*,*,#41666,.T.);
#53468=ORIENTED_EDGE('',*,*,#41422,.T.);
#53469=ORIENTED_EDGE('',*,*,#41661,.F.);
#53470=ORIENTED_EDGE('',*,*,#41411,.F.);
#53471=ORIENTED_EDGE('',*,*,#41406,.T.);
#53472=ORIENTED_EDGE('',*,*,#41414,.T.);
#53473=ORIENTED_EDGE('',*,*,#41429,.T.);
#53474=ORIENTED_EDGE('',*,*,#41667,.F.);
#53475=ORIENTED_EDGE('',*,*,#41668,.T.);
#53476=ORIENTED_EDGE('',*,*,#41669,.T.);
#53477=ORIENTED_EDGE('',*,*,#41670,.T.);
#53478=ORIENTED_EDGE('',*,*,#41671,.T.);
#53479=ORIENTED_EDGE('',*,*,#41672,.F.);
#53480=ORIENTED_EDGE('',*,*,#41673,.F.);
#53481=ORIENTED_EDGE('',*,*,#41674,.F.);
#53482=ORIENTED_EDGE('',*,*,#41675,.T.);
#53483=ORIENTED_EDGE('',*,*,#41676,.F.);
#53484=ORIENTED_EDGE('',*,*,#41677,.T.);
#53485=ORIENTED_EDGE('',*,*,#41667,.T.);
#53486=ORIENTED_EDGE('',*,*,#41678,.T.);
#53487=ORIENTED_EDGE('',*,*,#41679,.T.);
#53488=ORIENTED_EDGE('',*,*,#41680,.F.);
#53489=ORIENTED_EDGE('',*,*,#41681,.F.);
#53490=ORIENTED_EDGE('',*,*,#41680,.T.);
#53491=ORIENTED_EDGE('',*,*,#41682,.T.);
#53492=ORIENTED_EDGE('',*,*,#41668,.F.);
#53493=ORIENTED_EDGE('',*,*,#41677,.F.);
#53494=ORIENTED_EDGE('',*,*,#41683,.F.);
#53495=ORIENTED_EDGE('',*,*,#41684,.F.);
#53496=ORIENTED_EDGE('',*,*,#41669,.F.);
#53497=ORIENTED_EDGE('',*,*,#41685,.T.);
#53498=ORIENTED_EDGE('',*,*,#41686,.F.);
#53499=ORIENTED_EDGE('',*,*,#41687,.T.);
#53500=ORIENTED_EDGE('',*,*,#41688,.T.);
#53501=ORIENTED_EDGE('',*,*,#41689,.F.);
#53502=ORIENTED_EDGE('',*,*,#41690,.F.);
#53503=ORIENTED_EDGE('',*,*,#41691,.T.);
#53504=ORIENTED_EDGE('',*,*,#41692,.T.);
#53505=ORIENTED_EDGE('',*,*,#41693,.F.);
#53506=ORIENTED_EDGE('',*,*,#41689,.T.);
#53507=ORIENTED_EDGE('',*,*,#41694,.F.);
#53508=ORIENTED_EDGE('',*,*,#41695,.F.);
#53509=ORIENTED_EDGE('',*,*,#41696,.T.);
#53510=ORIENTED_EDGE('',*,*,#41697,.F.);
#53511=ORIENTED_EDGE('',*,*,#41686,.T.);
#53512=ORIENTED_EDGE('',*,*,#41696,.F.);
#53513=ORIENTED_EDGE('',*,*,#41698,.T.);
#53514=ORIENTED_EDGE('',*,*,#41672,.T.);
#53515=ORIENTED_EDGE('',*,*,#41699,.F.);
#53516=ORIENTED_EDGE('',*,*,#41700,.F.);
#53517=ORIENTED_EDGE('',*,*,#41695,.T.);
#53518=ORIENTED_EDGE('',*,*,#41673,.T.);
#53519=ORIENTED_EDGE('',*,*,#41701,.F.);
#53520=ORIENTED_EDGE('',*,*,#41702,.T.);
#53521=ORIENTED_EDGE('',*,*,#41703,.T.);
#53522=ORIENTED_EDGE('',*,*,#41704,.T.);
#53523=ORIENTED_EDGE('',*,*,#41670,.F.);
#53524=ORIENTED_EDGE('',*,*,#41705,.F.);
#53525=ORIENTED_EDGE('',*,*,#41704,.F.);
#53526=ORIENTED_EDGE('',*,*,#41706,.T.);
#53527=ORIENTED_EDGE('',*,*,#41707,.T.);
#53528=ORIENTED_EDGE('',*,*,#41708,.T.);
#53529=ORIENTED_EDGE('',*,*,#41687,.F.);
#53530=ORIENTED_EDGE('',*,*,#41697,.T.);
#53531=ORIENTED_EDGE('',*,*,#41671,.F.);
#53532=ORIENTED_EDGE('',*,*,#41709,.F.);
#53533=ORIENTED_EDGE('',*,*,#41710,.F.);
#53534=ORIENTED_EDGE('',*,*,#41711,.F.);
#53535=ORIENTED_EDGE('',*,*,#41683,.T.);
#53536=ORIENTED_EDGE('',*,*,#41712,.F.);
#53537=ORIENTED_EDGE('',*,*,#41690,.T.);
#53538=ORIENTED_EDGE('',*,*,#41713,.F.);
#53539=ORIENTED_EDGE('',*,*,#41707,.F.);
#53540=ORIENTED_EDGE('',*,*,#41714,.F.);
#53541=ORIENTED_EDGE('',*,*,#41710,.T.);
#53542=ORIENTED_EDGE('',*,*,#41715,.T.);
#53543=ORIENTED_EDGE('',*,*,#41404,.T.);
#53544=ORIENTED_EDGE('',*,*,#41403,.T.);
#53545=ORIENTED_EDGE('',*,*,#41684,.T.);
#53546=ORIENTED_EDGE('',*,*,#41711,.T.);
#53547=ORIENTED_EDGE('',*,*,#41714,.T.);
#53548=ORIENTED_EDGE('',*,*,#41716,.T.);
#53549=ORIENTED_EDGE('',*,*,#41717,.F.);
#53550=ORIENTED_EDGE('',*,*,#41674,.T.);
#53551=ORIENTED_EDGE('',*,*,#41718,.T.);
#53552=ORIENTED_EDGE('',*,*,#41719,.F.);
#53553=ORIENTED_EDGE('',*,*,#41675,.F.);
#53554=ORIENTED_EDGE('',*,*,#41720,.T.);
#53555=ORIENTED_EDGE('',*,*,#41721,.T.);
#53556=ORIENTED_EDGE('',*,*,#41722,.T.);
#53557=ORIENTED_EDGE('',*,*,#41678,.F.);
#53558=ORIENTED_EDGE('',*,*,#41723,.F.);
#53559=ORIENTED_EDGE('',*,*,#41676,.T.);
#53560=ORIENTED_EDGE('',*,*,#41719,.T.);
#53561=ORIENTED_EDGE('',*,*,#41724,.T.);
#53562=ORIENTED_EDGE('',*,*,#41725,.T.);
#53563=ORIENTED_EDGE('',*,*,#41681,.T.);
#53564=ORIENTED_EDGE('',*,*,#41726,.T.);
#53565=ORIENTED_EDGE('',*,*,#41721,.F.);
#53566=ORIENTED_EDGE('',*,*,#41727,.F.);
#53567=ORIENTED_EDGE('',*,*,#41691,.F.);
#53568=ORIENTED_EDGE('',*,*,#41712,.T.);
#53569=ORIENTED_EDGE('',*,*,#41685,.F.);
#53570=ORIENTED_EDGE('',*,*,#41682,.F.);
#53571=ORIENTED_EDGE('',*,*,#41679,.F.);
#53572=ORIENTED_EDGE('',*,*,#41722,.F.);
#53573=ORIENTED_EDGE('',*,*,#41728,.F.);
#53574=ORIENTED_EDGE('',*,*,#41729,.T.);
#53575=ORIENTED_EDGE('',*,*,#41692,.F.);
#53576=ORIENTED_EDGE('',*,*,#41730,.T.);
#53577=ORIENTED_EDGE('',*,*,#41708,.F.);
#53578=ORIENTED_EDGE('',*,*,#41713,.T.);
#53579=ORIENTED_EDGE('',*,*,#41693,.T.);
#53580=ORIENTED_EDGE('',*,*,#41731,.T.);
#53581=ORIENTED_EDGE('',*,*,#41732,.T.);
#53582=ORIENTED_EDGE('',*,*,#41733,.T.);
#53583=ORIENTED_EDGE('',*,*,#41688,.F.);
#53584=ORIENTED_EDGE('',*,*,#41699,.T.);
#53585=ORIENTED_EDGE('',*,*,#41694,.T.);
#53586=ORIENTED_EDGE('',*,*,#41733,.F.);
#53587=ORIENTED_EDGE('',*,*,#41734,.F.);
#53588=ORIENTED_EDGE('',*,*,#41735,.T.);
#53589=ORIENTED_EDGE('',*,*,#41700,.T.);
#53590=ORIENTED_EDGE('',*,*,#41736,.T.);
#53591=ORIENTED_EDGE('',*,*,#41701,.T.);
#53592=ORIENTED_EDGE('',*,*,#41698,.F.);
#53593=ORIENTED_EDGE('',*,*,#41737,.F.);
#53594=ORIENTED_EDGE('',*,*,#41738,.T.);
#53595=ORIENTED_EDGE('',*,*,#41739,.T.);
#53596=ORIENTED_EDGE('',*,*,#41705,.T.);
#53597=ORIENTED_EDGE('',*,*,#41702,.F.);
#53598=ORIENTED_EDGE('',*,*,#41740,.T.);
#53599=ORIENTED_EDGE('',*,*,#41741,.T.);
#53600=ORIENTED_EDGE('',*,*,#41742,.F.);
#53601=ORIENTED_EDGE('',*,*,#41739,.F.);
#53602=ORIENTED_EDGE('',*,*,#41715,.F.);
#53603=ORIENTED_EDGE('',*,*,#41709,.T.);
#53604=ORIENTED_EDGE('',*,*,#41706,.F.);
#53605=ORIENTED_EDGE('',*,*,#41703,.F.);
#53606=ORIENTED_EDGE('',*,*,#41742,.T.);
#53607=ORIENTED_EDGE('',*,*,#41743,.T.);
#53608=ORIENTED_EDGE('',*,*,#41744,.T.);
#53609=ORIENTED_EDGE('',*,*,#41745,.F.);
#53610=ORIENTED_EDGE('',*,*,#41746,.F.);
#53611=ORIENTED_EDGE('',*,*,#41747,.T.);
#53612=ORIENTED_EDGE('',*,*,#41748,.T.);
#53613=ORIENTED_EDGE('',*,*,#41401,.F.);
#53614=ORIENTED_EDGE('',*,*,#41744,.F.);
#53615=ORIENTED_EDGE('',*,*,#41749,.T.);
#53616=ORIENTED_EDGE('',*,*,#41750,.T.);
#53617=ORIENTED_EDGE('',*,*,#41751,.F.);
#53618=ORIENTED_EDGE('',*,*,#41748,.F.);
#53619=ORIENTED_EDGE('',*,*,#41752,.T.);
#53620=ORIENTED_EDGE('',*,*,#41753,.F.);
#53621=ORIENTED_EDGE('',*,*,#41716,.F.);
#53622=ORIENTED_EDGE('',*,*,#41402,.T.);
#53623=ORIENTED_EDGE('',*,*,#41751,.T.);
#53624=ORIENTED_EDGE('',*,*,#41717,.T.);
#53625=ORIENTED_EDGE('',*,*,#41754,.T.);
#53626=ORIENTED_EDGE('',*,*,#41720,.F.);
#53627=ORIENTED_EDGE('',*,*,#41755,.T.);
#53628=ORIENTED_EDGE('',*,*,#41724,.F.);
#53629=ORIENTED_EDGE('',*,*,#41718,.F.);
#53630=ORIENTED_EDGE('',*,*,#41756,.T.);
#53631=ORIENTED_EDGE('',*,*,#41725,.F.);
#53632=ORIENTED_EDGE('',*,*,#41755,.F.);
#53633=ORIENTED_EDGE('',*,*,#41396,.T.);
#53634=ORIENTED_EDGE('',*,*,#41727,.T.);
#53635=ORIENTED_EDGE('',*,*,#41723,.T.);
#53636=ORIENTED_EDGE('',*,*,#41395,.F.);
#53637=ORIENTED_EDGE('',*,*,#41730,.F.);
#53638=ORIENTED_EDGE('',*,*,#41728,.T.);
#53639=ORIENTED_EDGE('',*,*,#41726,.F.);
#53640=ORIENTED_EDGE('',*,*,#41757,.T.);
#53641=ORIENTED_EDGE('',*,*,#41731,.F.);
#53642=ORIENTED_EDGE('',*,*,#41729,.F.);
#53643=ORIENTED_EDGE('',*,*,#41394,.T.);
#53644=ORIENTED_EDGE('',*,*,#41734,.T.);
#53645=ORIENTED_EDGE('',*,*,#41732,.F.);
#53646=ORIENTED_EDGE('',*,*,#41757,.F.);
#53647=ORIENTED_EDGE('',*,*,#41758,.T.);
#53648=ORIENTED_EDGE('',*,*,#41759,.F.);
#53649=ORIENTED_EDGE('',*,*,#41737,.T.);
#53650=ORIENTED_EDGE('',*,*,#41736,.F.);
#53651=ORIENTED_EDGE('',*,*,#41735,.F.);
#53652=ORIENTED_EDGE('',*,*,#41760,.T.);
#53653=ORIENTED_EDGE('',*,*,#41740,.F.);
#53654=ORIENTED_EDGE('',*,*,#41738,.F.);
#53655=ORIENTED_EDGE('',*,*,#41405,.F.);
#53656=ORIENTED_EDGE('',*,*,#41743,.F.);
#53657=ORIENTED_EDGE('',*,*,#41741,.F.);
#53658=ORIENTED_EDGE('',*,*,#41761,.T.);
#53659=ORIENTED_EDGE('',*,*,#41745,.T.);
#53660=ORIENTED_EDGE('',*,*,#41746,.T.);
#53661=ORIENTED_EDGE('',*,*,#41762,.F.);
#53662=ORIENTED_EDGE('',*,*,#41763,.F.);
#53663=ORIENTED_EDGE('',*,*,#41764,.T.);
#53664=ORIENTED_EDGE('',*,*,#41752,.F.);
#53665=ORIENTED_EDGE('',*,*,#41749,.F.);
#53666=ORIENTED_EDGE('',*,*,#41747,.F.);
#53667=ORIENTED_EDGE('',*,*,#41764,.F.);
#53668=ORIENTED_EDGE('',*,*,#41765,.F.);
#53669=ORIENTED_EDGE('',*,*,#41766,.F.);
#53670=ORIENTED_EDGE('',*,*,#41767,.T.);
#53671=ORIENTED_EDGE('',*,*,#41768,.F.);
#53672=ORIENTED_EDGE('',*,*,#41750,.F.);
#53673=ORIENTED_EDGE('',*,*,#41766,.T.);
#53674=ORIENTED_EDGE('',*,*,#41756,.F.);
#53675=ORIENTED_EDGE('',*,*,#41754,.F.);
#53676=ORIENTED_EDGE('',*,*,#41753,.T.);
#53677=ORIENTED_EDGE('',*,*,#41768,.T.);
#53678=ORIENTED_EDGE('',*,*,#41769,.F.);
#53679=ORIENTED_EDGE('',*,*,#41770,.T.);
#53680=ORIENTED_EDGE('',*,*,#41397,.F.);
#53681=ORIENTED_EDGE('',*,*,#41762,.T.);
#53682=ORIENTED_EDGE('',*,*,#41761,.F.);
#53683=ORIENTED_EDGE('',*,*,#41760,.F.);
#53684=ORIENTED_EDGE('',*,*,#41759,.T.);
#53685=ORIENTED_EDGE('',*,*,#41758,.F.);
#53686=ORIENTED_EDGE('',*,*,#41400,.F.);
#53687=ORIENTED_EDGE('',*,*,#41771,.T.);
#53688=ORIENTED_EDGE('',*,*,#41772,.T.);
#53689=ORIENTED_EDGE('',*,*,#41773,.F.);
#53690=ORIENTED_EDGE('',*,*,#41773,.T.);
#53691=ORIENTED_EDGE('',*,*,#41774,.T.);
#53692=ORIENTED_EDGE('',*,*,#41775,.T.);
#53693=ORIENTED_EDGE('',*,*,#41767,.F.);
#53694=ORIENTED_EDGE('',*,*,#41765,.T.);
#53695=ORIENTED_EDGE('',*,*,#41763,.T.);
#53696=ORIENTED_EDGE('',*,*,#41775,.F.);
#53697=ORIENTED_EDGE('',*,*,#41776,.T.);
#53698=ORIENTED_EDGE('',*,*,#41777,.T.);
#53699=ORIENTED_EDGE('',*,*,#41778,.F.);
#53700=ORIENTED_EDGE('',*,*,#41779,.T.);
#53701=ORIENTED_EDGE('',*,*,#41769,.T.);
#53702=ORIENTED_EDGE('',*,*,#41778,.T.);
#53703=ORIENTED_EDGE('',*,*,#41780,.F.);
#53704=ORIENTED_EDGE('',*,*,#41770,.F.);
#53705=ORIENTED_EDGE('',*,*,#41781,.T.);
#53706=ORIENTED_EDGE('',*,*,#41782,.F.);
#53707=ORIENTED_EDGE('',*,*,#41783,.F.);
#53708=ORIENTED_EDGE('',*,*,#41784,.F.);
#53709=ORIENTED_EDGE('',*,*,#41399,.F.);
#53710=ORIENTED_EDGE('',*,*,#41398,.F.);
#53711=ORIENTED_EDGE('',*,*,#41780,.T.);
#53712=ORIENTED_EDGE('',*,*,#41785,.F.);
#53713=ORIENTED_EDGE('',*,*,#41786,.F.);
#53714=ORIENTED_EDGE('',*,*,#41771,.F.);
#53715=ORIENTED_EDGE('',*,*,#41784,.T.);
#53716=ORIENTED_EDGE('',*,*,#41787,.F.);
#53717=ORIENTED_EDGE('',*,*,#41788,.F.);
#53718=ORIENTED_EDGE('',*,*,#41772,.F.);
#53719=ORIENTED_EDGE('',*,*,#41786,.T.);
#53720=ORIENTED_EDGE('',*,*,#41789,.F.);
#53721=ORIENTED_EDGE('',*,*,#41790,.F.);
#53722=ORIENTED_EDGE('',*,*,#41774,.F.);
#53723=ORIENTED_EDGE('',*,*,#41788,.T.);
#53724=ORIENTED_EDGE('',*,*,#41791,.F.);
#53725=ORIENTED_EDGE('',*,*,#41792,.F.);
#53726=ORIENTED_EDGE('',*,*,#41776,.F.);
#53727=ORIENTED_EDGE('',*,*,#41790,.T.);
#53728=ORIENTED_EDGE('',*,*,#41793,.F.);
#53729=ORIENTED_EDGE('',*,*,#41794,.F.);
#53730=ORIENTED_EDGE('',*,*,#41777,.F.);
#53731=ORIENTED_EDGE('',*,*,#41792,.T.);
#53732=ORIENTED_EDGE('',*,*,#41795,.F.);
#53733=ORIENTED_EDGE('',*,*,#41781,.F.);
#53734=ORIENTED_EDGE('',*,*,#41779,.F.);
#53735=ORIENTED_EDGE('',*,*,#41794,.T.);
#53736=ORIENTED_EDGE('',*,*,#41796,.F.);
#53737=ORIENTED_EDGE('',*,*,#41797,.T.);
#53738=ORIENTED_EDGE('',*,*,#41383,.F.);
#53739=ORIENTED_EDGE('',*,*,#41798,.F.);
#53740=ORIENTED_EDGE('',*,*,#41782,.T.);
#53741=ORIENTED_EDGE('',*,*,#41798,.T.);
#53742=ORIENTED_EDGE('',*,*,#41393,.F.);
#53743=ORIENTED_EDGE('',*,*,#41799,.F.);
#53744=ORIENTED_EDGE('',*,*,#41783,.T.);
#53745=ORIENTED_EDGE('',*,*,#41799,.T.);
#53746=ORIENTED_EDGE('',*,*,#41392,.F.);
#53747=ORIENTED_EDGE('',*,*,#41800,.F.);
#53748=ORIENTED_EDGE('',*,*,#41785,.T.);
#53749=ORIENTED_EDGE('',*,*,#41800,.T.);
#53750=ORIENTED_EDGE('',*,*,#41391,.F.);
#53751=ORIENTED_EDGE('',*,*,#41801,.F.);
#53752=ORIENTED_EDGE('',*,*,#41787,.T.);
#53753=ORIENTED_EDGE('',*,*,#41801,.T.);
#53754=ORIENTED_EDGE('',*,*,#41388,.F.);
#53755=ORIENTED_EDGE('',*,*,#41802,.F.);
#53756=ORIENTED_EDGE('',*,*,#41789,.T.);
#53757=ORIENTED_EDGE('',*,*,#41802,.T.);
#53758=ORIENTED_EDGE('',*,*,#41387,.F.);
#53759=ORIENTED_EDGE('',*,*,#41803,.F.);
#53760=ORIENTED_EDGE('',*,*,#41791,.T.);
#53761=ORIENTED_EDGE('',*,*,#41803,.T.);
#53762=ORIENTED_EDGE('',*,*,#41386,.F.);
#53763=ORIENTED_EDGE('',*,*,#41804,.F.);
#53764=ORIENTED_EDGE('',*,*,#41793,.T.);
#53765=ORIENTED_EDGE('',*,*,#41804,.T.);
#53766=ORIENTED_EDGE('',*,*,#41385,.F.);
#53767=ORIENTED_EDGE('',*,*,#41805,.F.);
#53768=ORIENTED_EDGE('',*,*,#41795,.T.);
#53769=ORIENTED_EDGE('',*,*,#41805,.T.);
#53770=ORIENTED_EDGE('',*,*,#41384,.F.);
#53771=ORIENTED_EDGE('',*,*,#41797,.F.);
#53772=ORIENTED_EDGE('',*,*,#41796,.T.);
#53773=ORIENTED_EDGE('',*,*,#41390,.F.);
#53774=ORIENTED_EDGE('',*,*,#41150,.T.);
#53775=ORIENTED_EDGE('',*,*,#41806,.T.);
#53776=ORIENTED_EDGE('',*,*,#41807,.T.);
#53777=ORIENTED_EDGE('',*,*,#41808,.T.);
#53778=ORIENTED_EDGE('',*,*,#41809,.F.);
#53779=ORIENTED_EDGE('',*,*,#41810,.F.);
#53780=ORIENTED_EDGE('',*,*,#41155,.T.);
#53781=ORIENTED_EDGE('',*,*,#41152,.T.);
#53782=ORIENTED_EDGE('',*,*,#41151,.T.);
#53783=ORIENTED_EDGE('',*,*,#41808,.F.);
#53784=ORIENTED_EDGE('',*,*,#41381,.F.);
#53785=ORIENTED_EDGE('',*,*,#41811,.F.);
#53786=ORIENTED_EDGE('',*,*,#41812,.T.);
#53787=ORIENTED_EDGE('',*,*,#41806,.F.);
#53788=ORIENTED_EDGE('',*,*,#41149,.F.);
#53789=ORIENTED_EDGE('',*,*,#41154,.F.);
#53790=ORIENTED_EDGE('',*,*,#41812,.F.);
#53791=ORIENTED_EDGE('',*,*,#41813,.F.);
#53792=ORIENTED_EDGE('',*,*,#41809,.T.);
#53793=ORIENTED_EDGE('',*,*,#41807,.F.);
#53794=ORIENTED_EDGE('',*,*,#41382,.F.);
#53795=ORIENTED_EDGE('',*,*,#41156,.F.);
#53796=ORIENTED_EDGE('',*,*,#41810,.T.);
#53797=ORIENTED_EDGE('',*,*,#41814,.F.);
#53798=ORIENTED_EDGE('',*,*,#41815,.F.);
#53799=ORIENTED_EDGE('',*,*,#41377,.T.);
#53800=ORIENTED_EDGE('',*,*,#41376,.T.);
#53801=ORIENTED_EDGE('',*,*,#41158,.F.);
#53802=ORIENTED_EDGE('',*,*,#41816,.T.);
#53803=ORIENTED_EDGE('',*,*,#41811,.T.);
#53804=ORIENTED_EDGE('',*,*,#41380,.F.);
#53805=ORIENTED_EDGE('',*,*,#41379,.T.);
#53806=ORIENTED_EDGE('',*,*,#41160,.T.);
#53807=ORIENTED_EDGE('',*,*,#41375,.T.);
#53808=ORIENTED_EDGE('',*,*,#41374,.T.);
#53809=ORIENTED_EDGE('',*,*,#41817,.F.);
#53810=ORIENTED_EDGE('',*,*,#41814,.T.);
#53811=ORIENTED_EDGE('',*,*,#41813,.T.);
#53812=ORIENTED_EDGE('',*,*,#41816,.F.);
#53813=ORIENTED_EDGE('',*,*,#41818,.F.);
#53814=ORIENTED_EDGE('',*,*,#41373,.T.);
#53815=ORIENTED_EDGE('',*,*,#41818,.T.);
#53816=ORIENTED_EDGE('',*,*,#41817,.T.);
#53817=ORIENTED_EDGE('',*,*,#41378,.T.);
#53818=ORIENTED_EDGE('',*,*,#41815,.T.);
#53819=ORIENTED_EDGE('',*,*,#41364,.T.);
#53820=ORIENTED_EDGE('',*,*,#41361,.T.);
#53821=ORIENTED_EDGE('',*,*,#41367,.F.);
#53822=ORIENTED_EDGE('',*,*,#41173,.F.);
#53823=ORIENTED_EDGE('',*,*,#41170,.F.);
#53824=ORIENTED_EDGE('',*,*,#41167,.F.);
#53825=ORIENTED_EDGE('',*,*,#41164,.F.);
#53826=ORIENTED_EDGE('',*,*,#41819,.F.);
#53827=ORIENTED_EDGE('',*,*,#41178,.F.);
#53828=ORIENTED_EDGE('',*,*,#41186,.F.);
#53829=ORIENTED_EDGE('',*,*,#41353,.F.);
#53830=ORIENTED_EDGE('',*,*,#41191,.F.);
#53831=ORIENTED_EDGE('',*,*,#41820,.F.);
#53832=ORIENTED_EDGE('',*,*,#41162,.F.);
#53833=ORIENTED_EDGE('',*,*,#41166,.F.);
#53834=ORIENTED_EDGE('',*,*,#41169,.F.);
#53835=ORIENTED_EDGE('',*,*,#41172,.F.);
#53836=ORIENTED_EDGE('',*,*,#41366,.F.);
#53837=ORIENTED_EDGE('',*,*,#41176,.F.);
#53838=ORIENTED_EDGE('',*,*,#41365,.T.);
#53839=ORIENTED_EDGE('',*,*,#41189,.F.);
#53840=ORIENTED_EDGE('',*,*,#41354,.F.);
#53841=ORIENTED_EDGE('',*,*,#41187,.F.);
#53842=ORIENTED_EDGE('',*,*,#41184,.F.);
#53843=ORIENTED_EDGE('',*,*,#41180,.F.);
#53844=ORIENTED_EDGE('',*,*,#41179,.T.);
#53845=ORIENTED_EDGE('',*,*,#41819,.T.);
#53846=ORIENTED_EDGE('',*,*,#41163,.T.);
#53847=ORIENTED_EDGE('',*,*,#41820,.T.);
#53848=ORIENTED_EDGE('',*,*,#41192,.T.);
#53849=ORIENTED_EDGE('',*,*,#41357,.F.);
#53850=ORIENTED_EDGE('',*,*,#41363,.T.);
#53851=ORIENTED_EDGE('',*,*,#41821,.F.);
#53852=ORIENTED_EDGE('',*,*,#41822,.T.);
#53853=ORIENTED_EDGE('',*,*,#41823,.F.);
#53854=ORIENTED_EDGE('',*,*,#41824,.T.);
#53855=ORIENTED_EDGE('',*,*,#41825,.T.);
#53856=ORIENTED_EDGE('',*,*,#41826,.F.);
#53857=ORIENTED_EDGE('',*,*,#41827,.F.);
#53858=ORIENTED_EDGE('',*,*,#41828,.F.);
#53859=ORIENTED_EDGE('',*,*,#41829,.F.);
#53860=ORIENTED_EDGE('',*,*,#41830,.F.);
#53861=ORIENTED_EDGE('',*,*,#41831,.T.);
#53862=ORIENTED_EDGE('',*,*,#41832,.F.);
#53863=ORIENTED_EDGE('',*,*,#41833,.F.);
#53864=ORIENTED_EDGE('',*,*,#41834,.F.);
#53865=ORIENTED_EDGE('',*,*,#41835,.F.);
#53866=ORIENTED_EDGE('',*,*,#41836,.F.);
#53867=ORIENTED_EDGE('',*,*,#41837,.T.);
#53868=ORIENTED_EDGE('',*,*,#41838,.T.);
#53869=ORIENTED_EDGE('',*,*,#41839,.F.);
#53870=ORIENTED_EDGE('',*,*,#41206,.T.);
#53871=ORIENTED_EDGE('',*,*,#41840,.F.);
#53872=ORIENTED_EDGE('',*,*,#41841,.F.);
#53873=ORIENTED_EDGE('',*,*,#41842,.F.);
#53874=ORIENTED_EDGE('',*,*,#41204,.T.);
#53875=ORIENTED_EDGE('',*,*,#41843,.F.);
#53876=ORIENTED_EDGE('',*,*,#41844,.F.);
#53877=ORIENTED_EDGE('',*,*,#41207,.F.);
#53878=ORIENTED_EDGE('',*,*,#41839,.T.);
#53879=ORIENTED_EDGE('',*,*,#41845,.T.);
#53880=ORIENTED_EDGE('',*,*,#41846,.T.);
#53881=ORIENTED_EDGE('',*,*,#41847,.F.);
#53882=ORIENTED_EDGE('',*,*,#41848,.F.);
#53883=ORIENTED_EDGE('',*,*,#41208,.F.);
#53884=ORIENTED_EDGE('',*,*,#41848,.T.);
#53885=ORIENTED_EDGE('',*,*,#41849,.F.);
#53886=ORIENTED_EDGE('',*,*,#41850,.F.);
#53887=ORIENTED_EDGE('',*,*,#41851,.T.);
#53888=ORIENTED_EDGE('',*,*,#41852,.T.);
#53889=ORIENTED_EDGE('',*,*,#41853,.T.);
#53890=ORIENTED_EDGE('',*,*,#41854,.F.);
#53891=ORIENTED_EDGE('',*,*,#41855,.T.);
#53892=ORIENTED_EDGE('',*,*,#41201,.T.);
#53893=ORIENTED_EDGE('',*,*,#41856,.T.);
#53894=ORIENTED_EDGE('',*,*,#41200,.F.);
#53895=ORIENTED_EDGE('',*,*,#41857,.F.);
#53896=ORIENTED_EDGE('',*,*,#41858,.F.);
#53897=ORIENTED_EDGE('',*,*,#41859,.F.);
#53898=ORIENTED_EDGE('',*,*,#41860,.F.);
#53899=ORIENTED_EDGE('',*,*,#41861,.F.);
#53900=ORIENTED_EDGE('',*,*,#41862,.F.);
#53901=ORIENTED_EDGE('',*,*,#41863,.T.);
#53902=ORIENTED_EDGE('',*,*,#41864,.T.);
#53903=ORIENTED_EDGE('',*,*,#41856,.F.);
#53904=ORIENTED_EDGE('',*,*,#41210,.F.);
#53905=ORIENTED_EDGE('',*,*,#41865,.F.);
#53906=ORIENTED_EDGE('',*,*,#41847,.T.);
#53907=ORIENTED_EDGE('',*,*,#41866,.T.);
#53908=ORIENTED_EDGE('',*,*,#41867,.T.);
#53909=ORIENTED_EDGE('',*,*,#41868,.T.);
#53910=ORIENTED_EDGE('',*,*,#41869,.F.);
#53911=ORIENTED_EDGE('',*,*,#41870,.F.);
#53912=ORIENTED_EDGE('',*,*,#41871,.T.);
#53913=ORIENTED_EDGE('',*,*,#41872,.F.);
#53914=ORIENTED_EDGE('',*,*,#41873,.F.);
#53915=ORIENTED_EDGE('',*,*,#41874,.F.);
#53916=ORIENTED_EDGE('',*,*,#41211,.F.);
#53917=ORIENTED_EDGE('',*,*,#41874,.T.);
#53918=ORIENTED_EDGE('',*,*,#41875,.F.);
#53919=ORIENTED_EDGE('',*,*,#41876,.F.);
#53920=ORIENTED_EDGE('',*,*,#41877,.F.);
#53921=ORIENTED_EDGE('',*,*,#41878,.T.);
#53922=ORIENTED_EDGE('',*,*,#41879,.F.);
#53923=ORIENTED_EDGE('',*,*,#41880,.F.);
#53924=ORIENTED_EDGE('',*,*,#41881,.F.);
#53925=ORIENTED_EDGE('',*,*,#41199,.F.);
#53926=ORIENTED_EDGE('',*,*,#41882,.F.);
#53927=ORIENTED_EDGE('',*,*,#41883,.F.);
#53928=ORIENTED_EDGE('',*,*,#41884,.T.);
#53929=ORIENTED_EDGE('',*,*,#41885,.T.);
#53930=ORIENTED_EDGE('',*,*,#41886,.F.);
#53931=ORIENTED_EDGE('',*,*,#41887,.F.);
#53932=ORIENTED_EDGE('',*,*,#41888,.F.);
#53933=ORIENTED_EDGE('',*,*,#41857,.T.);
#53934=ORIENTED_EDGE('',*,*,#41889,.F.);
#53935=ORIENTED_EDGE('',*,*,#41214,.T.);
#53936=ORIENTED_EDGE('',*,*,#41890,.T.);
#53937=ORIENTED_EDGE('',*,*,#41891,.T.);
#53938=ORIENTED_EDGE('',*,*,#41892,.F.);
#53939=ORIENTED_EDGE('',*,*,#41893,.F.);
#53940=ORIENTED_EDGE('',*,*,#41894,.T.);
#53941=ORIENTED_EDGE('',*,*,#41895,.F.);
#53942=ORIENTED_EDGE('',*,*,#41212,.T.);
#53943=ORIENTED_EDGE('',*,*,#41881,.T.);
#53944=ORIENTED_EDGE('',*,*,#41890,.F.);
#53945=ORIENTED_EDGE('',*,*,#41213,.T.);
#53946=ORIENTED_EDGE('',*,*,#41895,.T.);
#53947=ORIENTED_EDGE('',*,*,#41880,.T.);
#53948=ORIENTED_EDGE('',*,*,#41865,.T.);
#53949=ORIENTED_EDGE('',*,*,#41209,.T.);
#53950=ORIENTED_EDGE('',*,*,#41849,.T.);
#53951=ORIENTED_EDGE('',*,*,#41896,.F.);
#53952=ORIENTED_EDGE('',*,*,#41821,.T.);
#53953=ORIENTED_EDGE('',*,*,#41897,.T.);
#53954=ORIENTED_EDGE('',*,*,#41898,.F.);
#53955=ORIENTED_EDGE('',*,*,#41899,.F.);
#53956=ORIENTED_EDGE('',*,*,#41900,.F.);
#53957=ORIENTED_EDGE('',*,*,#41901,.F.);
#53958=ORIENTED_EDGE('',*,*,#41832,.T.);
#53959=ORIENTED_EDGE('',*,*,#41882,.T.);
#53960=ORIENTED_EDGE('',*,*,#41198,.T.);
#53961=ORIENTED_EDGE('',*,*,#41902,.T.);
#53962=ORIENTED_EDGE('',*,*,#41902,.F.);
#53963=ORIENTED_EDGE('',*,*,#41197,.T.);
#53964=ORIENTED_EDGE('',*,*,#41903,.T.);
#53965=ORIENTED_EDGE('',*,*,#41883,.T.);
#53966=ORIENTED_EDGE('',*,*,#41903,.F.);
#53967=ORIENTED_EDGE('',*,*,#41196,.T.);
#53968=ORIENTED_EDGE('',*,*,#41904,.F.);
#53969=ORIENTED_EDGE('',*,*,#41905,.F.);
#53970=ORIENTED_EDGE('',*,*,#41906,.F.);
#53971=ORIENTED_EDGE('',*,*,#41892,.T.);
#53972=ORIENTED_EDGE('',*,*,#41907,.T.);
#53973=ORIENTED_EDGE('',*,*,#41202,.F.);
#53974=ORIENTED_EDGE('',*,*,#41855,.F.);
#53975=ORIENTED_EDGE('',*,*,#41908,.F.);
#53976=ORIENTED_EDGE('',*,*,#41203,.F.);
#53977=ORIENTED_EDGE('',*,*,#41908,.T.);
#53978=ORIENTED_EDGE('',*,*,#41864,.F.);
#53979=ORIENTED_EDGE('',*,*,#41909,.F.);
#53980=ORIENTED_EDGE('',*,*,#41843,.T.);
#53981=ORIENTED_EDGE('',*,*,#41840,.T.);
#53982=ORIENTED_EDGE('',*,*,#41205,.T.);
#53983=ORIENTED_EDGE('',*,*,#41842,.T.);
#53984=ORIENTED_EDGE('',*,*,#41910,.F.);
#53985=ORIENTED_EDGE('',*,*,#41911,.F.);
#53986=ORIENTED_EDGE('',*,*,#41912,.T.);
#53987=ORIENTED_EDGE('',*,*,#41913,.F.);
#53988=ORIENTED_EDGE('',*,*,#41914,.T.);
#53989=ORIENTED_EDGE('',*,*,#41915,.F.);
#53990=ORIENTED_EDGE('',*,*,#41868,.F.);
#53991=ORIENTED_EDGE('',*,*,#41916,.F.);
#53992=ORIENTED_EDGE('',*,*,#41917,.F.);
#53993=ORIENTED_EDGE('',*,*,#41918,.T.);
#53994=ORIENTED_EDGE('',*,*,#41919,.T.);
#53995=ORIENTED_EDGE('',*,*,#41913,.T.);
#53996=ORIENTED_EDGE('',*,*,#41867,.F.);
#53997=ORIENTED_EDGE('',*,*,#41920,.F.);
#53998=ORIENTED_EDGE('',*,*,#41916,.T.);
#53999=ORIENTED_EDGE('',*,*,#41921,.F.);
#54000=ORIENTED_EDGE('',*,*,#41845,.F.);
#54001=ORIENTED_EDGE('',*,*,#41922,.T.);
#54002=ORIENTED_EDGE('',*,*,#41923,.F.);
#54003=ORIENTED_EDGE('',*,*,#41924,.F.);
#54004=ORIENTED_EDGE('',*,*,#41925,.T.);
#54005=ORIENTED_EDGE('',*,*,#41926,.F.);
#54006=ORIENTED_EDGE('',*,*,#41927,.T.);
#54007=ORIENTED_EDGE('',*,*,#41928,.F.);
#54008=ORIENTED_EDGE('',*,*,#41929,.F.);
#54009=ORIENTED_EDGE('',*,*,#41923,.T.);
#54010=ORIENTED_EDGE('',*,*,#41930,.T.);
#54011=ORIENTED_EDGE('',*,*,#41926,.T.);
#54012=ORIENTED_EDGE('',*,*,#41931,.F.);
#54013=ORIENTED_EDGE('',*,*,#41932,.F.);
#54014=ORIENTED_EDGE('',*,*,#41933,.T.);
#54015=ORIENTED_EDGE('',*,*,#41934,.F.);
#54016=ORIENTED_EDGE('',*,*,#41935,.F.);
#54017=ORIENTED_EDGE('',*,*,#41936,.F.);
#54018=ORIENTED_EDGE('',*,*,#41937,.T.);
#54019=ORIENTED_EDGE('',*,*,#41938,.F.);
#54020=ORIENTED_EDGE('',*,*,#41935,.T.);
#54021=ORIENTED_EDGE('',*,*,#41939,.T.);
#54022=ORIENTED_EDGE('',*,*,#41940,.F.);
#54023=ORIENTED_EDGE('',*,*,#41941,.F.);
#54024=ORIENTED_EDGE('',*,*,#41942,.F.);
#54025=ORIENTED_EDGE('',*,*,#41941,.T.);
#54026=ORIENTED_EDGE('',*,*,#41943,.F.);
#54027=ORIENTED_EDGE('',*,*,#41944,.F.);
#54028=ORIENTED_EDGE('',*,*,#41943,.T.);
#54029=ORIENTED_EDGE('',*,*,#41940,.T.);
#54030=ORIENTED_EDGE('',*,*,#41945,.T.);
#54031=ORIENTED_EDGE('',*,*,#41946,.F.);
#54032=ORIENTED_EDGE('',*,*,#41947,.F.);
#54033=ORIENTED_EDGE('',*,*,#41948,.T.);
#54034=ORIENTED_EDGE('',*,*,#41351,.F.);
#54035=ORIENTED_EDGE('',*,*,#41949,.F.);
#54036=ORIENTED_EDGE('',*,*,#41828,.T.);
#54037=ORIENTED_EDGE('',*,*,#41950,.T.);
#54038=ORIENTED_EDGE('',*,*,#41951,.F.);
#54039=ORIENTED_EDGE('',*,*,#41952,.F.);
#54040=ORIENTED_EDGE('',*,*,#41826,.T.);
#54041=ORIENTED_EDGE('',*,*,#41952,.T.);
#54042=ORIENTED_EDGE('',*,*,#41953,.F.);
#54043=ORIENTED_EDGE('',*,*,#41948,.F.);
#54044=ORIENTED_EDGE('',*,*,#41827,.T.);
#54045=ORIENTED_EDGE('',*,*,#41954,.T.);
#54046=ORIENTED_EDGE('',*,*,#41955,.T.);
#54047=ORIENTED_EDGE('',*,*,#41352,.F.);
#54048=ORIENTED_EDGE('',*,*,#41953,.T.);
#54049=ORIENTED_EDGE('',*,*,#41956,.T.);
#54050=ORIENTED_EDGE('',*,*,#41955,.F.);
#54051=ORIENTED_EDGE('',*,*,#41957,.F.);
#54052=ORIENTED_EDGE('',*,*,#41835,.T.);
#54053=ORIENTED_EDGE('',*,*,#41900,.T.);
#54054=ORIENTED_EDGE('',*,*,#41958,.T.);
#54055=ORIENTED_EDGE('',*,*,#41898,.T.);
#54056=ORIENTED_EDGE('',*,*,#41959,.F.);
#54057=ORIENTED_EDGE('',*,*,#41960,.F.);
#54058=ORIENTED_EDGE('',*,*,#41961,.F.);
#54059=ORIENTED_EDGE('',*,*,#41962,.T.);
#54060=ORIENTED_EDGE('',*,*,#41963,.T.);
#54061=ORIENTED_EDGE('',*,*,#41964,.T.);
#54062=ORIENTED_EDGE('',*,*,#41965,.F.);
#54063=ORIENTED_EDGE('',*,*,#41838,.F.);
#54064=ORIENTED_EDGE('',*,*,#41966,.T.);
#54065=ORIENTED_EDGE('',*,*,#41961,.T.);
#54066=ORIENTED_EDGE('',*,*,#41861,.T.);
#54067=ORIENTED_EDGE('',*,*,#41967,.F.);
#54068=ORIENTED_EDGE('',*,*,#41968,.F.);
#54069=ORIENTED_EDGE('',*,*,#41969,.T.);
#54070=ORIENTED_EDGE('',*,*,#41970,.F.);
#54071=ORIENTED_EDGE('',*,*,#41971,.F.);
#54072=ORIENTED_EDGE('',*,*,#41968,.T.);
#54073=ORIENTED_EDGE('',*,*,#41862,.T.);
#54074=ORIENTED_EDGE('',*,*,#41971,.T.);
#54075=ORIENTED_EDGE('',*,*,#41972,.F.);
#54076=ORIENTED_EDGE('',*,*,#41973,.T.);
#54077=ORIENTED_EDGE('',*,*,#41974,.F.);
#54078=ORIENTED_EDGE('',*,*,#41975,.F.);
#54079=ORIENTED_EDGE('',*,*,#41973,.F.);
#54080=ORIENTED_EDGE('',*,*,#41910,.T.);
#54081=ORIENTED_EDGE('',*,*,#41844,.T.);
#54082=ORIENTED_EDGE('',*,*,#41975,.T.);
#54083=ORIENTED_EDGE('',*,*,#41909,.T.);
#54084=ORIENTED_EDGE('',*,*,#41863,.F.);
#54085=ORIENTED_EDGE('',*,*,#41974,.T.);
#54086=ORIENTED_EDGE('',*,*,#41976,.F.);
#54087=ORIENTED_EDGE('',*,*,#41977,.F.);
#54088=ORIENTED_EDGE('',*,*,#41978,.F.);
#54089=ORIENTED_EDGE('',*,*,#41979,.F.);
#54090=ORIENTED_EDGE('',*,*,#41980,.F.);
#54091=ORIENTED_EDGE('',*,*,#41981,.F.);
#54092=ORIENTED_EDGE('',*,*,#41982,.F.);
#54093=ORIENTED_EDGE('',*,*,#41983,.F.);
#54094=ORIENTED_EDGE('',*,*,#41984,.F.);
#54095=ORIENTED_EDGE('',*,*,#41985,.T.);
#54096=ORIENTED_EDGE('',*,*,#41986,.F.);
#54097=ORIENTED_EDGE('',*,*,#41987,.T.);
#54098=ORIENTED_EDGE('',*,*,#41988,.F.);
#54099=ORIENTED_EDGE('',*,*,#41989,.F.);
#54100=ORIENTED_EDGE('',*,*,#41859,.T.);
#54101=ORIENTED_EDGE('',*,*,#41989,.T.);
#54102=ORIENTED_EDGE('',*,*,#41990,.F.);
#54103=ORIENTED_EDGE('',*,*,#41991,.F.);
#54104=ORIENTED_EDGE('',*,*,#41992,.T.);
#54105=ORIENTED_EDGE('',*,*,#41984,.T.);
#54106=ORIENTED_EDGE('',*,*,#41993,.F.);
#54107=ORIENTED_EDGE('',*,*,#41994,.F.);
#54108=ORIENTED_EDGE('',*,*,#41995,.F.);
#54109=ORIENTED_EDGE('',*,*,#41996,.F.);
#54110=ORIENTED_EDGE('',*,*,#41871,.F.);
#54111=ORIENTED_EDGE('',*,*,#41997,.F.);
#54112=ORIENTED_EDGE('',*,*,#41998,.F.);
#54113=ORIENTED_EDGE('',*,*,#41860,.T.);
#54114=ORIENTED_EDGE('',*,*,#41992,.F.);
#54115=ORIENTED_EDGE('',*,*,#41999,.T.);
#54116=ORIENTED_EDGE('',*,*,#41345,.F.);
#54117=ORIENTED_EDGE('',*,*,#42000,.F.);
#54118=ORIENTED_EDGE('',*,*,#41996,.T.);
#54119=ORIENTED_EDGE('',*,*,#42001,.F.);
#54120=ORIENTED_EDGE('',*,*,#42002,.F.);
#54121=ORIENTED_EDGE('',*,*,#41985,.F.);
#54122=ORIENTED_EDGE('',*,*,#42000,.T.);
#54123=ORIENTED_EDGE('',*,*,#41348,.F.);
#54124=ORIENTED_EDGE('',*,*,#41999,.F.);
#54125=ORIENTED_EDGE('',*,*,#42003,.F.);
#54126=ORIENTED_EDGE('',*,*,#42004,.F.);
#54127=ORIENTED_EDGE('',*,*,#42005,.F.);
#54128=ORIENTED_EDGE('',*,*,#41346,.F.);
#54129=ORIENTED_EDGE('',*,*,#42006,.T.);
#54130=ORIENTED_EDGE('',*,*,#42005,.T.);
#54131=ORIENTED_EDGE('',*,*,#42007,.F.);
#54132=ORIENTED_EDGE('',*,*,#42008,.F.);
#54133=ORIENTED_EDGE('',*,*,#41342,.T.);
#54134=ORIENTED_EDGE('',*,*,#41343,.T.);
#54135=ORIENTED_EDGE('',*,*,#42009,.F.);
#54136=ORIENTED_EDGE('',*,*,#42010,.T.);
#54137=ORIENTED_EDGE('',*,*,#42011,.T.);
#54138=ORIENTED_EDGE('',*,*,#42012,.T.);
#54139=ORIENTED_EDGE('',*,*,#42008,.T.);
#54140=ORIENTED_EDGE('',*,*,#42013,.T.);
#54141=ORIENTED_EDGE('',*,*,#42014,.F.);
#54142=ORIENTED_EDGE('',*,*,#41336,.T.);
#54143=ORIENTED_EDGE('',*,*,#41340,.F.);
#54144=ORIENTED_EDGE('',*,*,#41324,.T.);
#54145=ORIENTED_EDGE('',*,*,#41335,.F.);
#54146=ORIENTED_EDGE('',*,*,#42015,.T.);
#54147=ORIENTED_EDGE('',*,*,#41326,.T.);
#54148=ORIENTED_EDGE('',*,*,#42016,.F.);
#54149=ORIENTED_EDGE('',*,*,#42017,.F.);
#54150=ORIENTED_EDGE('',*,*,#42018,.T.);
#54151=ORIENTED_EDGE('',*,*,#42019,.T.);
#54152=ORIENTED_EDGE('',*,*,#42020,.T.);
#54153=ORIENTED_EDGE('',*,*,#42021,.T.);
#54154=ORIENTED_EDGE('',*,*,#42022,.F.);
#54155=ORIENTED_EDGE('',*,*,#42017,.T.);
#54156=ORIENTED_EDGE('',*,*,#42023,.T.);
#54157=ORIENTED_EDGE('',*,*,#42024,.F.);
#54158=ORIENTED_EDGE('',*,*,#42025,.T.);
#54159=ORIENTED_EDGE('',*,*,#42026,.T.);
#54160=ORIENTED_EDGE('',*,*,#42027,.T.);
#54161=ORIENTED_EDGE('',*,*,#42022,.T.);
#54162=ORIENTED_EDGE('',*,*,#42028,.T.);
#54163=ORIENTED_EDGE('',*,*,#42029,.T.);
#54164=ORIENTED_EDGE('',*,*,#42030,.F.);
#54165=ORIENTED_EDGE('',*,*,#42024,.T.);
#54166=ORIENTED_EDGE('',*,*,#42031,.T.);
#54167=ORIENTED_EDGE('',*,*,#42032,.T.);
#54168=ORIENTED_EDGE('',*,*,#41327,.T.);
#54169=ORIENTED_EDGE('',*,*,#42015,.F.);
#54170=ORIENTED_EDGE('',*,*,#42031,.F.);
#54171=ORIENTED_EDGE('',*,*,#42033,.T.);
#54172=ORIENTED_EDGE('',*,*,#41328,.T.);
#54173=ORIENTED_EDGE('',*,*,#42032,.F.);
#54174=ORIENTED_EDGE('',*,*,#42023,.F.);
#54175=ORIENTED_EDGE('',*,*,#42034,.T.);
#54176=ORIENTED_EDGE('',*,*,#41329,.T.);
#54177=ORIENTED_EDGE('',*,*,#42033,.F.);
#54178=ORIENTED_EDGE('',*,*,#42027,.F.);
#54179=ORIENTED_EDGE('',*,*,#42016,.T.);
#54180=ORIENTED_EDGE('',*,*,#41331,.T.);
#54181=ORIENTED_EDGE('',*,*,#42035,.F.);
#54182=ORIENTED_EDGE('',*,*,#42018,.F.);
#54183=ORIENTED_EDGE('',*,*,#42035,.T.);
#54184=ORIENTED_EDGE('',*,*,#41330,.T.);
#54185=ORIENTED_EDGE('',*,*,#42034,.F.);
#54186=ORIENTED_EDGE('',*,*,#42036,.F.);
#54187=ORIENTED_EDGE('',*,*,#42026,.F.);
#54188=ORIENTED_EDGE('',*,*,#42037,.F.);
#54189=ORIENTED_EDGE('',*,*,#42038,.T.);
#54190=ORIENTED_EDGE('',*,*,#42039,.T.);
#54191=ORIENTED_EDGE('',*,*,#42019,.F.);
#54192=ORIENTED_EDGE('',*,*,#42036,.T.);
#54193=ORIENTED_EDGE('',*,*,#42040,.F.);
#54194=ORIENTED_EDGE('',*,*,#42041,.F.);
#54195=ORIENTED_EDGE('',*,*,#42042,.F.);
#54196=ORIENTED_EDGE('',*,*,#42020,.F.);
#54197=ORIENTED_EDGE('',*,*,#42039,.F.);
#54198=ORIENTED_EDGE('',*,*,#42042,.T.);
#54199=ORIENTED_EDGE('',*,*,#42043,.F.);
#54200=ORIENTED_EDGE('',*,*,#42044,.T.);
#54201=ORIENTED_EDGE('',*,*,#42028,.F.);
#54202=ORIENTED_EDGE('',*,*,#42021,.F.);
#54203=ORIENTED_EDGE('',*,*,#42044,.F.);
#54204=ORIENTED_EDGE('',*,*,#42045,.F.);
#54205=ORIENTED_EDGE('',*,*,#42046,.F.);
#54206=ORIENTED_EDGE('',*,*,#42047,.T.);
#54207=ORIENTED_EDGE('',*,*,#42048,.F.);
#54208=ORIENTED_EDGE('',*,*,#42049,.F.);
#54209=ORIENTED_EDGE('',*,*,#42049,.T.);
#54210=ORIENTED_EDGE('',*,*,#42050,.F.);
#54211=ORIENTED_EDGE('',*,*,#42051,.T.);
#54212=ORIENTED_EDGE('',*,*,#42052,.F.);
#54213=ORIENTED_EDGE('',*,*,#42053,.F.);
#54214=ORIENTED_EDGE('',*,*,#42029,.F.);
#54215=ORIENTED_EDGE('',*,*,#42054,.T.);
#54216=ORIENTED_EDGE('',*,*,#41267,.T.);
#54217=ORIENTED_EDGE('',*,*,#42055,.T.);
#54218=ORIENTED_EDGE('',*,*,#42053,.T.);
#54219=ORIENTED_EDGE('',*,*,#42055,.F.);
#54220=ORIENTED_EDGE('',*,*,#41266,.T.);
#54221=ORIENTED_EDGE('',*,*,#42056,.T.);
#54222=ORIENTED_EDGE('',*,*,#42030,.T.);
#54223=ORIENTED_EDGE('',*,*,#42056,.F.);
#54224=ORIENTED_EDGE('',*,*,#41265,.F.);
#54225=ORIENTED_EDGE('',*,*,#41262,.F.);
#54226=ORIENTED_EDGE('',*,*,#42057,.T.);
#54227=ORIENTED_EDGE('',*,*,#42025,.F.);
#54228=ORIENTED_EDGE('',*,*,#42057,.F.);
#54229=ORIENTED_EDGE('',*,*,#41261,.T.);
#54230=ORIENTED_EDGE('',*,*,#42058,.T.);
#54231=ORIENTED_EDGE('',*,*,#42037,.T.);
#54232=ORIENTED_EDGE('',*,*,#42058,.F.);
#54233=ORIENTED_EDGE('',*,*,#41260,.T.);
#54234=ORIENTED_EDGE('',*,*,#42059,.F.);
#54235=ORIENTED_EDGE('',*,*,#42060,.T.);
#54236=ORIENTED_EDGE('',*,*,#42060,.F.);
#54237=ORIENTED_EDGE('',*,*,#42061,.T.);
#54238=ORIENTED_EDGE('',*,*,#42062,.T.);
#54239=ORIENTED_EDGE('',*,*,#42063,.T.);
#54240=ORIENTED_EDGE('',*,*,#42064,.T.);
#54241=ORIENTED_EDGE('',*,*,#42038,.F.);
#54242=ORIENTED_EDGE('',*,*,#42065,.F.);
#54243=ORIENTED_EDGE('',*,*,#42066,.F.);
#54244=ORIENTED_EDGE('',*,*,#42046,.T.);
#54245=ORIENTED_EDGE('',*,*,#42067,.F.);
#54246=ORIENTED_EDGE('',*,*,#42040,.T.);
#54247=ORIENTED_EDGE('',*,*,#42064,.F.);
#54248=ORIENTED_EDGE('',*,*,#42043,.T.);
#54249=ORIENTED_EDGE('',*,*,#42041,.T.);
#54250=ORIENTED_EDGE('',*,*,#42067,.T.);
#54251=ORIENTED_EDGE('',*,*,#42045,.T.);
#54252=ORIENTED_EDGE('',*,*,#41323,.F.);
#54253=ORIENTED_EDGE('',*,*,#41321,.T.);
#54254=ORIENTED_EDGE('',*,*,#41320,.F.);
#54255=ORIENTED_EDGE('',*,*,#41315,.T.);
#54256=ORIENTED_EDGE('',*,*,#41312,.F.);
#54257=ORIENTED_EDGE('',*,*,#41313,.T.);
#54258=ORIENTED_EDGE('',*,*,#41310,.T.);
#54259=ORIENTED_EDGE('',*,*,#42068,.T.);
#54260=ORIENTED_EDGE('',*,*,#42069,.T.);
#54261=ORIENTED_EDGE('',*,*,#42070,.F.);
#54262=ORIENTED_EDGE('',*,*,#42071,.T.);
#54263=ORIENTED_EDGE('',*,*,#42072,.T.);
#54264=ORIENTED_EDGE('',*,*,#42073,.F.);
#54265=ORIENTED_EDGE('',*,*,#42074,.F.);
#54266=ORIENTED_EDGE('',*,*,#41308,.F.);
#54267=ORIENTED_EDGE('',*,*,#42074,.T.);
#54268=ORIENTED_EDGE('',*,*,#42075,.F.);
#54269=ORIENTED_EDGE('',*,*,#42076,.T.);
#54270=ORIENTED_EDGE('',*,*,#42077,.T.);
#54271=ORIENTED_EDGE('',*,*,#42068,.F.);
#54272=ORIENTED_EDGE('',*,*,#41309,.T.);
#54273=ORIENTED_EDGE('',*,*,#42078,.T.);
#54274=ORIENTED_EDGE('',*,*,#42079,.T.);
#54275=ORIENTED_EDGE('',*,*,#42069,.F.);
#54276=ORIENTED_EDGE('',*,*,#42077,.F.);
#54277=ORIENTED_EDGE('',*,*,#42080,.F.);
#54278=ORIENTED_EDGE('',*,*,#42079,.F.);
#54279=ORIENTED_EDGE('',*,*,#42081,.T.);
#54280=ORIENTED_EDGE('',*,*,#42082,.T.);
#54281=ORIENTED_EDGE('',*,*,#42083,.T.);
#54282=ORIENTED_EDGE('',*,*,#42084,.F.);
#54283=ORIENTED_EDGE('',*,*,#42082,.F.);
#54284=ORIENTED_EDGE('',*,*,#42085,.T.);
#54285=ORIENTED_EDGE('',*,*,#42086,.T.);
#54286=ORIENTED_EDGE('',*,*,#42087,.T.);
#54287=ORIENTED_EDGE('',*,*,#42088,.F.);
#54288=ORIENTED_EDGE('',*,*,#42089,.F.);
#54289=ORIENTED_EDGE('',*,*,#42085,.F.);
#54290=ORIENTED_EDGE('',*,*,#42090,.T.);
#54291=ORIENTED_EDGE('',*,*,#42091,.F.);
#54292=ORIENTED_EDGE('',*,*,#42083,.F.);
#54293=ORIENTED_EDGE('',*,*,#42089,.T.);
#54294=ORIENTED_EDGE('',*,*,#42092,.T.);
#54295=ORIENTED_EDGE('',*,*,#42093,.T.);
#54296=ORIENTED_EDGE('',*,*,#42094,.T.);
#54297=ORIENTED_EDGE('',*,*,#42095,.T.);
#54298=ORIENTED_EDGE('',*,*,#42096,.T.);
#54299=ORIENTED_EDGE('',*,*,#42097,.T.);
#54300=ORIENTED_EDGE('',*,*,#42098,.T.);
#54301=ORIENTED_EDGE('',*,*,#42099,.T.);
#54302=ORIENTED_EDGE('',*,*,#42091,.T.);
#54303=ORIENTED_EDGE('',*,*,#42099,.F.);
#54304=ORIENTED_EDGE('',*,*,#42100,.T.);
#54305=ORIENTED_EDGE('',*,*,#42101,.T.);
#54306=ORIENTED_EDGE('',*,*,#42070,.T.);
#54307=ORIENTED_EDGE('',*,*,#42080,.T.);
#54308=ORIENTED_EDGE('',*,*,#42084,.T.);
#54309=ORIENTED_EDGE('',*,*,#42102,.T.);
#54310=ORIENTED_EDGE('',*,*,#42101,.F.);
#54311=ORIENTED_EDGE('',*,*,#42103,.F.);
#54312=ORIENTED_EDGE('',*,*,#42104,.T.);
#54313=ORIENTED_EDGE('',*,*,#42105,.T.);
#54314=ORIENTED_EDGE('',*,*,#42106,.T.);
#54315=ORIENTED_EDGE('',*,*,#41994,.T.);
#54316=ORIENTED_EDGE('',*,*,#42107,.T.);
#54317=ORIENTED_EDGE('',*,*,#42108,.F.);
#54318=ORIENTED_EDGE('',*,*,#42109,.F.);
#54319=ORIENTED_EDGE('',*,*,#42104,.F.);
#54320=ORIENTED_EDGE('',*,*,#42071,.F.);
#54321=ORIENTED_EDGE('',*,*,#42102,.F.);
#54322=ORIENTED_EDGE('',*,*,#42109,.T.);
#54323=ORIENTED_EDGE('',*,*,#42110,.T.);
#54324=ORIENTED_EDGE('',*,*,#42072,.F.);
#54325=ORIENTED_EDGE('',*,*,#42110,.F.);
#54326=ORIENTED_EDGE('',*,*,#42111,.T.);
#54327=ORIENTED_EDGE('',*,*,#42075,.T.);
#54328=ORIENTED_EDGE('',*,*,#42073,.T.);
#54329=ORIENTED_EDGE('',*,*,#41314,.T.);
#54330=ORIENTED_EDGE('',*,*,#42108,.T.);
#54331=ORIENTED_EDGE('',*,*,#42112,.T.);
#54332=ORIENTED_EDGE('',*,*,#42111,.F.);
#54333=ORIENTED_EDGE('',*,*,#42112,.F.);
#54334=ORIENTED_EDGE('',*,*,#42113,.T.);
#54335=ORIENTED_EDGE('',*,*,#42076,.F.);
#54336=ORIENTED_EDGE('',*,*,#42113,.F.);
#54337=ORIENTED_EDGE('',*,*,#42107,.F.);
#54338=ORIENTED_EDGE('',*,*,#41993,.T.);
#54339=ORIENTED_EDGE('',*,*,#41983,.T.);
#54340=ORIENTED_EDGE('',*,*,#42086,.F.);
#54341=ORIENTED_EDGE('',*,*,#42081,.F.);
#54342=ORIENTED_EDGE('',*,*,#42078,.F.);
#54343=ORIENTED_EDGE('',*,*,#42003,.T.);
#54344=ORIENTED_EDGE('',*,*,#41995,.T.);
#54345=ORIENTED_EDGE('',*,*,#42106,.F.);
#54346=ORIENTED_EDGE('',*,*,#42114,.F.);
#54347=ORIENTED_EDGE('',*,*,#42115,.F.);
#54348=ORIENTED_EDGE('',*,*,#42116,.F.);
#54349=ORIENTED_EDGE('',*,*,#42117,.F.);
#54350=ORIENTED_EDGE('',*,*,#42118,.F.);
#54351=ORIENTED_EDGE('',*,*,#42119,.F.);
#54352=ORIENTED_EDGE('',*,*,#42120,.F.);
#54353=ORIENTED_EDGE('',*,*,#42121,.F.);
#54354=ORIENTED_EDGE('',*,*,#42122,.T.);
#54355=ORIENTED_EDGE('',*,*,#42123,.F.);
#54356=ORIENTED_EDGE('',*,*,#42124,.F.);
#54357=ORIENTED_EDGE('',*,*,#41873,.T.);
#54358=ORIENTED_EDGE('',*,*,#42124,.T.);
#54359=ORIENTED_EDGE('',*,*,#42125,.F.);
#54360=ORIENTED_EDGE('',*,*,#42126,.F.);
#54361=ORIENTED_EDGE('',*,*,#41875,.T.);
#54362=ORIENTED_EDGE('',*,*,#42127,.F.);
#54363=ORIENTED_EDGE('',*,*,#42128,.F.);
#54364=ORIENTED_EDGE('',*,*,#42129,.F.);
#54365=ORIENTED_EDGE('',*,*,#42130,.F.);
#54366=ORIENTED_EDGE('',*,*,#42114,.T.);
#54367=ORIENTED_EDGE('',*,*,#42131,.T.);
#54368=ORIENTED_EDGE('',*,*,#42132,.F.);
#54369=ORIENTED_EDGE('',*,*,#42133,.F.);
#54370=ORIENTED_EDGE('',*,*,#42130,.T.);
#54371=ORIENTED_EDGE('',*,*,#42133,.T.);
#54372=ORIENTED_EDGE('',*,*,#42134,.F.);
#54373=ORIENTED_EDGE('',*,*,#42135,.F.);
#54374=ORIENTED_EDGE('',*,*,#42115,.T.);
#54375=ORIENTED_EDGE('',*,*,#42135,.T.);
#54376=ORIENTED_EDGE('',*,*,#42136,.F.);
#54377=ORIENTED_EDGE('',*,*,#42137,.F.);
#54378=ORIENTED_EDGE('',*,*,#42116,.T.);
#54379=ORIENTED_EDGE('',*,*,#42137,.T.);
#54380=ORIENTED_EDGE('',*,*,#42138,.F.);
#54381=ORIENTED_EDGE('',*,*,#42139,.F.);
#54382=ORIENTED_EDGE('',*,*,#42117,.T.);
#54383=ORIENTED_EDGE('',*,*,#42139,.T.);
#54384=ORIENTED_EDGE('',*,*,#42140,.F.);
#54385=ORIENTED_EDGE('',*,*,#42141,.F.);
#54386=ORIENTED_EDGE('',*,*,#42118,.T.);
#54387=ORIENTED_EDGE('',*,*,#42141,.T.);
#54388=ORIENTED_EDGE('',*,*,#42142,.F.);
#54389=ORIENTED_EDGE('',*,*,#42143,.F.);
#54390=ORIENTED_EDGE('',*,*,#42119,.T.);
#54391=ORIENTED_EDGE('',*,*,#42143,.T.);
#54392=ORIENTED_EDGE('',*,*,#42144,.F.);
#54393=ORIENTED_EDGE('',*,*,#42145,.F.);
#54394=ORIENTED_EDGE('',*,*,#42120,.T.);
#54395=ORIENTED_EDGE('',*,*,#42121,.T.);
#54396=ORIENTED_EDGE('',*,*,#42145,.T.);
#54397=ORIENTED_EDGE('',*,*,#42013,.F.);
#54398=ORIENTED_EDGE('',*,*,#42146,.T.);
#54399=ORIENTED_EDGE('',*,*,#42146,.F.);
#54400=ORIENTED_EDGE('',*,*,#42007,.T.);
#54401=ORIENTED_EDGE('',*,*,#42004,.T.);
#54402=ORIENTED_EDGE('',*,*,#42014,.T.);
#54403=ORIENTED_EDGE('',*,*,#42144,.T.);
#54404=ORIENTED_EDGE('',*,*,#42147,.F.);
#54405=ORIENTED_EDGE('',*,*,#42148,.T.);
#54406=ORIENTED_EDGE('',*,*,#42009,.T.);
#54407=ORIENTED_EDGE('',*,*,#42149,.T.);
#54408=ORIENTED_EDGE('',*,*,#42148,.F.);
#54409=ORIENTED_EDGE('',*,*,#42150,.F.);
#54410=ORIENTED_EDGE('',*,*,#41976,.T.);
#54411=ORIENTED_EDGE('',*,*,#42150,.T.);
#54412=ORIENTED_EDGE('',*,*,#42151,.F.);
#54413=ORIENTED_EDGE('',*,*,#42152,.F.);
#54414=ORIENTED_EDGE('',*,*,#41977,.T.);
#54415=ORIENTED_EDGE('',*,*,#42152,.T.);
#54416=ORIENTED_EDGE('',*,*,#42153,.F.);
#54417=ORIENTED_EDGE('',*,*,#42154,.F.);
#54418=ORIENTED_EDGE('',*,*,#41978,.T.);
#54419=ORIENTED_EDGE('',*,*,#42154,.T.);
#54420=ORIENTED_EDGE('',*,*,#42155,.F.);
#54421=ORIENTED_EDGE('',*,*,#42156,.F.);
#54422=ORIENTED_EDGE('',*,*,#41979,.T.);
#54423=ORIENTED_EDGE('',*,*,#42156,.T.);
#54424=ORIENTED_EDGE('',*,*,#42157,.F.);
#54425=ORIENTED_EDGE('',*,*,#42158,.F.);
#54426=ORIENTED_EDGE('',*,*,#41980,.T.);
#54427=ORIENTED_EDGE('',*,*,#42158,.T.);
#54428=ORIENTED_EDGE('',*,*,#42159,.F.);
#54429=ORIENTED_EDGE('',*,*,#42160,.F.);
#54430=ORIENTED_EDGE('',*,*,#41981,.T.);
#54431=ORIENTED_EDGE('',*,*,#42160,.T.);
#54432=ORIENTED_EDGE('',*,*,#42161,.F.);
#54433=ORIENTED_EDGE('',*,*,#42162,.F.);
#54434=ORIENTED_EDGE('',*,*,#42163,.T.);
#54435=ORIENTED_EDGE('',*,*,#42164,.F.);
#54436=ORIENTED_EDGE('',*,*,#42087,.F.);
#54437=ORIENTED_EDGE('',*,*,#41982,.T.);
#54438=ORIENTED_EDGE('',*,*,#42163,.F.);
#54439=ORIENTED_EDGE('',*,*,#42165,.T.);
#54440=ORIENTED_EDGE('',*,*,#42166,.F.);
#54441=ORIENTED_EDGE('',*,*,#42167,.F.);
#54442=ORIENTED_EDGE('',*,*,#42168,.F.);
#54443=ORIENTED_EDGE('',*,*,#42165,.F.);
#54444=ORIENTED_EDGE('',*,*,#42169,.F.);
#54445=ORIENTED_EDGE('',*,*,#42170,.T.);
#54446=ORIENTED_EDGE('',*,*,#42171,.F.);
#54447=ORIENTED_EDGE('',*,*,#42172,.T.);
#54448=ORIENTED_EDGE('',*,*,#42170,.F.);
#54449=ORIENTED_EDGE('',*,*,#42173,.F.);
#54450=ORIENTED_EDGE('',*,*,#42172,.F.);
#54451=ORIENTED_EDGE('',*,*,#42174,.F.);
#54452=ORIENTED_EDGE('',*,*,#42175,.T.);
#54453=ORIENTED_EDGE('',*,*,#42176,.F.);
#54454=ORIENTED_EDGE('',*,*,#42175,.F.);
#54455=ORIENTED_EDGE('',*,*,#42177,.F.);
#54456=ORIENTED_EDGE('',*,*,#42178,.T.);
#54457=ORIENTED_EDGE('',*,*,#42178,.F.);
#54458=ORIENTED_EDGE('',*,*,#42179,.F.);
#54459=ORIENTED_EDGE('',*,*,#42180,.F.);
#54460=ORIENTED_EDGE('',*,*,#42181,.F.);
#54461=ORIENTED_EDGE('',*,*,#42129,.T.);
#54462=ORIENTED_EDGE('',*,*,#42182,.F.);
#54463=ORIENTED_EDGE('',*,*,#42183,.F.);
#54464=ORIENTED_EDGE('',*,*,#42184,.F.);
#54465=ORIENTED_EDGE('',*,*,#42180,.T.);
#54466=ORIENTED_EDGE('',*,*,#42185,.F.);
#54467=ORIENTED_EDGE('',*,*,#42176,.T.);
#54468=ORIENTED_EDGE('',*,*,#42184,.T.);
#54469=ORIENTED_EDGE('',*,*,#42186,.T.);
#54470=ORIENTED_EDGE('',*,*,#42187,.F.);
#54471=ORIENTED_EDGE('',*,*,#42188,.T.);
#54472=ORIENTED_EDGE('',*,*,#42095,.F.);
#54473=ORIENTED_EDGE('',*,*,#42189,.F.);
#54474=ORIENTED_EDGE('',*,*,#42187,.T.);
#54475=ORIENTED_EDGE('',*,*,#42189,.T.);
#54476=ORIENTED_EDGE('',*,*,#42094,.F.);
#54477=ORIENTED_EDGE('',*,*,#42190,.F.);
#54478=ORIENTED_EDGE('',*,*,#42191,.T.);
#54479=ORIENTED_EDGE('',*,*,#42192,.T.);
#54480=ORIENTED_EDGE('',*,*,#42166,.T.);
#54481=ORIENTED_EDGE('',*,*,#42173,.T.);
#54482=ORIENTED_EDGE('',*,*,#42185,.T.);
#54483=ORIENTED_EDGE('',*,*,#42191,.F.);
#54484=ORIENTED_EDGE('',*,*,#42193,.T.);
#54485=ORIENTED_EDGE('',*,*,#42167,.T.);
#54486=ORIENTED_EDGE('',*,*,#42192,.F.);
#54487=ORIENTED_EDGE('',*,*,#42194,.F.);
#54488=ORIENTED_EDGE('',*,*,#42190,.T.);
#54489=ORIENTED_EDGE('',*,*,#42093,.F.);
#54490=ORIENTED_EDGE('',*,*,#42195,.F.);
#54491=ORIENTED_EDGE('',*,*,#42194,.T.);
#54492=ORIENTED_EDGE('',*,*,#42195,.T.);
#54493=ORIENTED_EDGE('',*,*,#42092,.F.);
#54494=ORIENTED_EDGE('',*,*,#42090,.F.);
#54495=ORIENTED_EDGE('',*,*,#42196,.T.);
#54496=ORIENTED_EDGE('',*,*,#42088,.T.);
#54497=ORIENTED_EDGE('',*,*,#42164,.T.);
#54498=ORIENTED_EDGE('',*,*,#42168,.T.);
#54499=ORIENTED_EDGE('',*,*,#42193,.F.);
#54500=ORIENTED_EDGE('',*,*,#42196,.F.);
#54501=ORIENTED_EDGE('',*,*,#42096,.F.);
#54502=ORIENTED_EDGE('',*,*,#42188,.F.);
#54503=ORIENTED_EDGE('',*,*,#42197,.T.);
#54504=ORIENTED_EDGE('',*,*,#42198,.T.);
#54505=ORIENTED_EDGE('',*,*,#42199,.T.);
#54506=ORIENTED_EDGE('',*,*,#42097,.F.);
#54507=ORIENTED_EDGE('',*,*,#42198,.F.);
#54508=ORIENTED_EDGE('',*,*,#42200,.T.);
#54509=ORIENTED_EDGE('',*,*,#42201,.F.);
#54510=ORIENTED_EDGE('',*,*,#42182,.T.);
#54511=ORIENTED_EDGE('',*,*,#42128,.T.);
#54512=ORIENTED_EDGE('',*,*,#42202,.T.);
#54513=ORIENTED_EDGE('',*,*,#42200,.F.);
#54514=ORIENTED_EDGE('',*,*,#42202,.F.);
#54515=ORIENTED_EDGE('',*,*,#42127,.T.);
#54516=ORIENTED_EDGE('',*,*,#42105,.F.);
#54517=ORIENTED_EDGE('',*,*,#42203,.F.);
#54518=ORIENTED_EDGE('',*,*,#42204,.F.);
#54519=ORIENTED_EDGE('',*,*,#42205,.T.);
#54520=ORIENTED_EDGE('',*,*,#42098,.F.);
#54521=ORIENTED_EDGE('',*,*,#42199,.F.);
#54522=ORIENTED_EDGE('',*,*,#42204,.T.);
#54523=ORIENTED_EDGE('',*,*,#42103,.T.);
#54524=ORIENTED_EDGE('',*,*,#42100,.F.);
#54525=ORIENTED_EDGE('',*,*,#42205,.F.);
#54526=ORIENTED_EDGE('',*,*,#42203,.T.);
#54527=ORIENTED_EDGE('',*,*,#42186,.F.);
#54528=ORIENTED_EDGE('',*,*,#42183,.T.);
#54529=ORIENTED_EDGE('',*,*,#42201,.T.);
#54530=ORIENTED_EDGE('',*,*,#42197,.F.);
#54531=ORIENTED_EDGE('',*,*,#42206,.T.);
#54532=ORIENTED_EDGE('',*,*,#42207,.F.);
#54533=ORIENTED_EDGE('',*,*,#42131,.F.);
#54534=ORIENTED_EDGE('',*,*,#42181,.T.);
#54535=ORIENTED_EDGE('',*,*,#42134,.T.);
#54536=ORIENTED_EDGE('',*,*,#42132,.T.);
#54537=ORIENTED_EDGE('',*,*,#42207,.T.);
#54538=ORIENTED_EDGE('',*,*,#42208,.T.);
#54539=ORIENTED_EDGE('',*,*,#42209,.T.);
#54540=ORIENTED_EDGE('',*,*,#42210,.T.);
#54541=ORIENTED_EDGE('',*,*,#42211,.T.);
#54542=ORIENTED_EDGE('',*,*,#42212,.T.);
#54543=ORIENTED_EDGE('',*,*,#42161,.T.);
#54544=ORIENTED_EDGE('',*,*,#42159,.T.);
#54545=ORIENTED_EDGE('',*,*,#42213,.F.);
#54546=ORIENTED_EDGE('',*,*,#42157,.T.);
#54547=ORIENTED_EDGE('',*,*,#42214,.F.);
#54548=ORIENTED_EDGE('',*,*,#42136,.T.);
#54549=ORIENTED_EDGE('',*,*,#42213,.T.);
#54550=ORIENTED_EDGE('',*,*,#42215,.T.);
#54551=ORIENTED_EDGE('',*,*,#42138,.T.);
#54552=ORIENTED_EDGE('',*,*,#42214,.T.);
#54553=ORIENTED_EDGE('',*,*,#42155,.T.);
#54554=ORIENTED_EDGE('',*,*,#42216,.T.);
#54555=ORIENTED_EDGE('',*,*,#41305,.F.);
#54556=ORIENTED_EDGE('',*,*,#41307,.F.);
#54557=ORIENTED_EDGE('',*,*,#41306,.T.);
#54558=ORIENTED_EDGE('',*,*,#42216,.F.);
#54559=ORIENTED_EDGE('',*,*,#42153,.T.);
#54560=ORIENTED_EDGE('',*,*,#42217,.T.);
#54561=ORIENTED_EDGE('',*,*,#42140,.T.);
#54562=ORIENTED_EDGE('',*,*,#42215,.F.);
#54563=ORIENTED_EDGE('',*,*,#42142,.T.);
#54564=ORIENTED_EDGE('',*,*,#42217,.F.);
#54565=ORIENTED_EDGE('',*,*,#42151,.T.);
#54566=ORIENTED_EDGE('',*,*,#42147,.T.);
#54567=ORIENTED_EDGE('',*,*,#41302,.F.);
#54568=ORIENTED_EDGE('',*,*,#41303,.T.);
#54569=ORIENTED_EDGE('',*,*,#42218,.T.);
#54570=ORIENTED_EDGE('',*,*,#42219,.T.);
#54571=ORIENTED_EDGE('',*,*,#41297,.T.);
#54572=ORIENTED_EDGE('',*,*,#42220,.F.);
#54573=ORIENTED_EDGE('',*,*,#42221,.F.);
#54574=ORIENTED_EDGE('',*,*,#42222,.T.);
#54575=ORIENTED_EDGE('',*,*,#42223,.T.);
#54576=ORIENTED_EDGE('',*,*,#42224,.F.);
#54577=ORIENTED_EDGE('',*,*,#42225,.T.);
#54578=ORIENTED_EDGE('',*,*,#42219,.F.);
#54579=ORIENTED_EDGE('',*,*,#42226,.T.);
#54580=ORIENTED_EDGE('',*,*,#42226,.F.);
#54581=ORIENTED_EDGE('',*,*,#42218,.F.);
#54582=ORIENTED_EDGE('',*,*,#42225,.F.);
#54583=ORIENTED_EDGE('',*,*,#42227,.F.);
#54584=ORIENTED_EDGE('',*,*,#42228,.F.);
#54585=ORIENTED_EDGE('',*,*,#42229,.F.);
#54586=ORIENTED_EDGE('',*,*,#42230,.F.);
#54587=ORIENTED_EDGE('',*,*,#42231,.F.);
#54588=ORIENTED_EDGE('',*,*,#42232,.F.);
#54589=ORIENTED_EDGE('',*,*,#42233,.F.);
#54590=ORIENTED_EDGE('',*,*,#42220,.T.);
#54591=ORIENTED_EDGE('',*,*,#42228,.T.);
#54592=ORIENTED_EDGE('',*,*,#42224,.T.);
#54593=ORIENTED_EDGE('',*,*,#42234,.T.);
#54594=ORIENTED_EDGE('',*,*,#42235,.T.);
#54595=ORIENTED_EDGE('',*,*,#42236,.T.);
#54596=ORIENTED_EDGE('',*,*,#42237,.T.);
#54597=ORIENTED_EDGE('',*,*,#42238,.F.);
#54598=ORIENTED_EDGE('',*,*,#42227,.T.);
#54599=ORIENTED_EDGE('',*,*,#42239,.F.);
#54600=ORIENTED_EDGE('',*,*,#42240,.F.);
#54601=ORIENTED_EDGE('',*,*,#42241,.T.);
#54602=ORIENTED_EDGE('',*,*,#42233,.T.);
#54603=ORIENTED_EDGE('',*,*,#42242,.T.);
#54604=ORIENTED_EDGE('',*,*,#42221,.T.);
#54605=ORIENTED_EDGE('',*,*,#42241,.F.);
#54606=ORIENTED_EDGE('',*,*,#42243,.F.);
#54607=ORIENTED_EDGE('',*,*,#42244,.T.);
#54608=ORIENTED_EDGE('',*,*,#42245,.T.);
#54609=ORIENTED_EDGE('',*,*,#42243,.T.);
#54610=ORIENTED_EDGE('',*,*,#42240,.T.);
#54611=ORIENTED_EDGE('',*,*,#42246,.F.);
#54612=ORIENTED_EDGE('',*,*,#42247,.T.);
#54613=ORIENTED_EDGE('',*,*,#42248,.F.);
#54614=ORIENTED_EDGE('',*,*,#42249,.F.);
#54615=ORIENTED_EDGE('',*,*,#42250,.T.);
#54616=ORIENTED_EDGE('',*,*,#41946,.T.);
#54617=ORIENTED_EDGE('',*,*,#42251,.T.);
#54618=ORIENTED_EDGE('',*,*,#42242,.F.);
#54619=ORIENTED_EDGE('',*,*,#42245,.F.);
#54620=ORIENTED_EDGE('',*,*,#41937,.F.);
#54621=ORIENTED_EDGE('',*,*,#42252,.F.);
#54622=ORIENTED_EDGE('',*,*,#42253,.T.);
#54623=ORIENTED_EDGE('',*,*,#41990,.T.);
#54624=ORIENTED_EDGE('',*,*,#41988,.T.);
#54625=ORIENTED_EDGE('',*,*,#42254,.F.);
#54626=ORIENTED_EDGE('',*,*,#41924,.T.);
#54627=ORIENTED_EDGE('',*,*,#41929,.T.);
#54628=ORIENTED_EDGE('',*,*,#42255,.T.);
#54629=ORIENTED_EDGE('',*,*,#42256,.T.);
#54630=ORIENTED_EDGE('',*,*,#42222,.F.);
#54631=ORIENTED_EDGE('',*,*,#42251,.F.);
#54632=ORIENTED_EDGE('',*,*,#41945,.F.);
#54633=ORIENTED_EDGE('',*,*,#41939,.F.);
#54634=ORIENTED_EDGE('',*,*,#42257,.T.);
#54635=ORIENTED_EDGE('',*,*,#41934,.T.);
#54636=ORIENTED_EDGE('',*,*,#42246,.T.);
#54637=ORIENTED_EDGE('',*,*,#42258,.F.);
#54638=ORIENTED_EDGE('',*,*,#42256,.F.);
#54639=ORIENTED_EDGE('',*,*,#42258,.T.);
#54640=ORIENTED_EDGE('',*,*,#42249,.T.);
#54641=ORIENTED_EDGE('',*,*,#42259,.F.);
#54642=ORIENTED_EDGE('',*,*,#42223,.F.);
#54643=ORIENTED_EDGE('',*,*,#42259,.T.);
#54644=ORIENTED_EDGE('',*,*,#42248,.T.);
#54645=ORIENTED_EDGE('',*,*,#42260,.F.);
#54646=ORIENTED_EDGE('',*,*,#42234,.F.);
#54647=ORIENTED_EDGE('',*,*,#42260,.T.);
#54648=ORIENTED_EDGE('',*,*,#42261,.T.);
#54649=ORIENTED_EDGE('',*,*,#42262,.F.);
#54650=ORIENTED_EDGE('',*,*,#42235,.F.);
#54651=ORIENTED_EDGE('',*,*,#42262,.T.);
#54652=ORIENTED_EDGE('',*,*,#42263,.T.);
#54653=ORIENTED_EDGE('',*,*,#42264,.F.);
#54654=ORIENTED_EDGE('',*,*,#42236,.F.);
#54655=ORIENTED_EDGE('',*,*,#42264,.T.);
#54656=ORIENTED_EDGE('',*,*,#41228,.T.);
#54657=ORIENTED_EDGE('',*,*,#42265,.F.);
#54658=ORIENTED_EDGE('',*,*,#42237,.F.);
#54659=ORIENTED_EDGE('',*,*,#42266,.F.);
#54660=ORIENTED_EDGE('',*,*,#42265,.T.);
#54661=ORIENTED_EDGE('',*,*,#41227,.T.);
#54662=ORIENTED_EDGE('',*,*,#42267,.F.);
#54663=ORIENTED_EDGE('',*,*,#42268,.F.);
#54664=ORIENTED_EDGE('',*,*,#42267,.T.);
#54665=ORIENTED_EDGE('',*,*,#42269,.T.);
#54666=ORIENTED_EDGE('',*,*,#41226,.F.);
#54667=ORIENTED_EDGE('',*,*,#42270,.F.);
#54668=ORIENTED_EDGE('',*,*,#42269,.F.);
#54669=ORIENTED_EDGE('',*,*,#42270,.T.);
#54670=ORIENTED_EDGE('',*,*,#42271,.F.);
#54671=ORIENTED_EDGE('',*,*,#42272,.T.);
#54672=ORIENTED_EDGE('',*,*,#42273,.T.);
#54673=ORIENTED_EDGE('',*,*,#42274,.T.);
#54674=ORIENTED_EDGE('',*,*,#42275,.T.);
#54675=ORIENTED_EDGE('',*,*,#42276,.T.);
#54676=ORIENTED_EDGE('',*,*,#42277,.T.);
#54677=ORIENTED_EDGE('',*,*,#42278,.T.);
#54678=ORIENTED_EDGE('',*,*,#42279,.F.);
#54679=ORIENTED_EDGE('',*,*,#42280,.T.);
#54680=ORIENTED_EDGE('',*,*,#42281,.T.);
#54681=ORIENTED_EDGE('',*,*,#42238,.T.);
#54682=ORIENTED_EDGE('',*,*,#42266,.T.);
#54683=ORIENTED_EDGE('',*,*,#42268,.T.);
#54684=ORIENTED_EDGE('',*,*,#42281,.F.);
#54685=ORIENTED_EDGE('',*,*,#42282,.F.);
#54686=ORIENTED_EDGE('',*,*,#42283,.F.);
#54687=ORIENTED_EDGE('',*,*,#42229,.T.);
#54688=ORIENTED_EDGE('',*,*,#42284,.T.);
#54689=ORIENTED_EDGE('',*,*,#42283,.T.);
#54690=ORIENTED_EDGE('',*,*,#42285,.F.);
#54691=ORIENTED_EDGE('',*,*,#42286,.F.);
#54692=ORIENTED_EDGE('',*,*,#42287,.F.);
#54693=ORIENTED_EDGE('',*,*,#42288,.T.);
#54694=ORIENTED_EDGE('',*,*,#42289,.T.);
#54695=ORIENTED_EDGE('',*,*,#42290,.T.);
#54696=ORIENTED_EDGE('',*,*,#42286,.T.);
#54697=ORIENTED_EDGE('',*,*,#42291,.T.);
#54698=ORIENTED_EDGE('',*,*,#42230,.T.);
#54699=ORIENTED_EDGE('',*,*,#42284,.F.);
#54700=ORIENTED_EDGE('',*,*,#42290,.F.);
#54701=ORIENTED_EDGE('',*,*,#42292,.T.);
#54702=ORIENTED_EDGE('',*,*,#42231,.T.);
#54703=ORIENTED_EDGE('',*,*,#42291,.F.);
#54704=ORIENTED_EDGE('',*,*,#42293,.F.);
#54705=ORIENTED_EDGE('',*,*,#42289,.F.);
#54706=ORIENTED_EDGE('',*,*,#42294,.T.);
#54707=ORIENTED_EDGE('',*,*,#42295,.T.);
#54708=ORIENTED_EDGE('',*,*,#42293,.T.);
#54709=ORIENTED_EDGE('',*,*,#42244,.F.);
#54710=ORIENTED_EDGE('',*,*,#42296,.T.);
#54711=ORIENTED_EDGE('',*,*,#42295,.F.);
#54712=ORIENTED_EDGE('',*,*,#42297,.T.);
#54713=ORIENTED_EDGE('',*,*,#41936,.T.);
#54714=ORIENTED_EDGE('',*,*,#41938,.T.);
#54715=ORIENTED_EDGE('',*,*,#41942,.T.);
#54716=ORIENTED_EDGE('',*,*,#41944,.T.);
#54717=ORIENTED_EDGE('',*,*,#42298,.T.);
#54718=ORIENTED_EDGE('',*,*,#42298,.F.);
#54719=ORIENTED_EDGE('',*,*,#41947,.T.);
#54720=ORIENTED_EDGE('',*,*,#42250,.F.);
#54721=ORIENTED_EDGE('',*,*,#42299,.F.);
#54722=ORIENTED_EDGE('',*,*,#42125,.T.);
#54723=ORIENTED_EDGE('',*,*,#42123,.T.);
#54724=ORIENTED_EDGE('',*,*,#42252,.T.);
#54725=ORIENTED_EDGE('',*,*,#42297,.F.);
#54726=ORIENTED_EDGE('',*,*,#42300,.T.);
#54727=ORIENTED_EDGE('',*,*,#42301,.T.);
#54728=ORIENTED_EDGE('',*,*,#42299,.T.);
#54729=ORIENTED_EDGE('',*,*,#42294,.F.);
#54730=ORIENTED_EDGE('',*,*,#42302,.T.);
#54731=ORIENTED_EDGE('',*,*,#42303,.T.);
#54732=ORIENTED_EDGE('',*,*,#42304,.T.);
#54733=ORIENTED_EDGE('',*,*,#42305,.F.);
#54734=ORIENTED_EDGE('',*,*,#42126,.T.);
#54735=ORIENTED_EDGE('',*,*,#42301,.F.);
#54736=ORIENTED_EDGE('',*,*,#42306,.F.);
#54737=ORIENTED_EDGE('',*,*,#41876,.T.);
#54738=ORIENTED_EDGE('',*,*,#42307,.F.);
#54739=ORIENTED_EDGE('',*,*,#42308,.F.);
#54740=ORIENTED_EDGE('',*,*,#42306,.T.);
#54741=ORIENTED_EDGE('',*,*,#42308,.T.);
#54742=ORIENTED_EDGE('',*,*,#42278,.F.);
#54743=ORIENTED_EDGE('',*,*,#42309,.F.);
#54744=ORIENTED_EDGE('',*,*,#41877,.T.);
#54745=ORIENTED_EDGE('',*,*,#42309,.T.);
#54746=ORIENTED_EDGE('',*,*,#42277,.F.);
#54747=ORIENTED_EDGE('',*,*,#42310,.F.);
#54748=ORIENTED_EDGE('',*,*,#42311,.T.);
#54749=ORIENTED_EDGE('',*,*,#42312,.F.);
#54750=ORIENTED_EDGE('',*,*,#41878,.F.);
#54751=ORIENTED_EDGE('',*,*,#42311,.F.);
#54752=ORIENTED_EDGE('',*,*,#42313,.T.);
#54753=ORIENTED_EDGE('',*,*,#42314,.F.);
#54754=ORIENTED_EDGE('',*,*,#42315,.T.);
#54755=ORIENTED_EDGE('',*,*,#42316,.F.);
#54756=ORIENTED_EDGE('',*,*,#42317,.F.);
#54757=ORIENTED_EDGE('',*,*,#42314,.T.);
#54758=ORIENTED_EDGE('',*,*,#42317,.T.);
#54759=ORIENTED_EDGE('',*,*,#42318,.F.);
#54760=ORIENTED_EDGE('',*,*,#42319,.F.);
#54761=ORIENTED_EDGE('',*,*,#42320,.T.);
#54762=ORIENTED_EDGE('',*,*,#42321,.F.);
#54763=ORIENTED_EDGE('',*,*,#42322,.F.);
#54764=ORIENTED_EDGE('',*,*,#42312,.T.);
#54765=ORIENTED_EDGE('',*,*,#42320,.F.);
#54766=ORIENTED_EDGE('',*,*,#42322,.T.);
#54767=ORIENTED_EDGE('',*,*,#42323,.T.);
#54768=ORIENTED_EDGE('',*,*,#42324,.T.);
#54769=ORIENTED_EDGE('',*,*,#41884,.F.);
#54770=ORIENTED_EDGE('',*,*,#41907,.F.);
#54771=ORIENTED_EDGE('',*,*,#41891,.F.);
#54772=ORIENTED_EDGE('',*,*,#41879,.T.);
#54773=ORIENTED_EDGE('',*,*,#42325,.T.);
#54774=ORIENTED_EDGE('',*,*,#42326,.T.);
#54775=ORIENTED_EDGE('',*,*,#41893,.T.);
#54776=ORIENTED_EDGE('',*,*,#42327,.T.);
#54777=ORIENTED_EDGE('',*,*,#42328,.F.);
#54778=ORIENTED_EDGE('',*,*,#41289,.F.);
#54779=ORIENTED_EDGE('',*,*,#41287,.F.);
#54780=ORIENTED_EDGE('',*,*,#41291,.T.);
#54781=ORIENTED_EDGE('',*,*,#41852,.F.);
#54782=ORIENTED_EDGE('',*,*,#42329,.F.);
#54783=ORIENTED_EDGE('',*,*,#42330,.T.);
#54784=ORIENTED_EDGE('',*,*,#42331,.T.);
#54785=ORIENTED_EDGE('',*,*,#42325,.F.);
#54786=ORIENTED_EDGE('',*,*,#42330,.F.);
#54787=ORIENTED_EDGE('',*,*,#42332,.F.);
#54788=ORIENTED_EDGE('',*,*,#42333,.T.);
#54789=ORIENTED_EDGE('',*,*,#42334,.F.);
#54790=ORIENTED_EDGE('',*,*,#42335,.F.);
#54791=ORIENTED_EDGE('',*,*,#42336,.F.);
#54792=ORIENTED_EDGE('',*,*,#42331,.F.);
#54793=ORIENTED_EDGE('',*,*,#42337,.F.);
#54794=ORIENTED_EDGE('',*,*,#41851,.F.);
#54795=ORIENTED_EDGE('',*,*,#42338,.T.);
#54796=ORIENTED_EDGE('',*,*,#42337,.T.);
#54797=ORIENTED_EDGE('',*,*,#42329,.T.);
#54798=ORIENTED_EDGE('',*,*,#42339,.F.);
#54799=ORIENTED_EDGE('',*,*,#41894,.F.);
#54800=ORIENTED_EDGE('',*,*,#42326,.F.);
#54801=ORIENTED_EDGE('',*,*,#42336,.T.);
#54802=ORIENTED_EDGE('',*,*,#42340,.T.);
#54803=ORIENTED_EDGE('',*,*,#41870,.T.);
#54804=ORIENTED_EDGE('',*,*,#42341,.F.);
#54805=ORIENTED_EDGE('',*,*,#42342,.T.);
#54806=ORIENTED_EDGE('',*,*,#42343,.F.);
#54807=ORIENTED_EDGE('',*,*,#42344,.F.);
#54808=ORIENTED_EDGE('',*,*,#42341,.T.);
#54809=ORIENTED_EDGE('',*,*,#42344,.T.);
#54810=ORIENTED_EDGE('',*,*,#42345,.F.);
#54811=ORIENTED_EDGE('',*,*,#42346,.F.);
#54812=ORIENTED_EDGE('',*,*,#42347,.T.);
#54813=ORIENTED_EDGE('',*,*,#42348,.T.);
#54814=ORIENTED_EDGE('',*,*,#41997,.T.);
#54815=ORIENTED_EDGE('',*,*,#42340,.F.);
#54816=ORIENTED_EDGE('',*,*,#42347,.F.);
#54817=ORIENTED_EDGE('',*,*,#42349,.T.);
#54818=ORIENTED_EDGE('',*,*,#42350,.T.);
#54819=ORIENTED_EDGE('',*,*,#42351,.T.);
#54820=ORIENTED_EDGE('',*,*,#42352,.T.);
#54821=ORIENTED_EDGE('',*,*,#42353,.T.);
#54822=ORIENTED_EDGE('',*,*,#42354,.T.);
#54823=ORIENTED_EDGE('',*,*,#41408,.T.);
#54824=ORIENTED_EDGE('',*,*,#42354,.F.);
#54825=ORIENTED_EDGE('',*,*,#42355,.T.);
#54826=ORIENTED_EDGE('',*,*,#42356,.F.);
#54827=ORIENTED_EDGE('',*,*,#42357,.F.);
#54828=ORIENTED_EDGE('',*,*,#42358,.F.);
#54829=ORIENTED_EDGE('',*,*,#42357,.T.);
#54830=ORIENTED_EDGE('',*,*,#42359,.F.);
#54831=ORIENTED_EDGE('',*,*,#42360,.T.);
#54832=ORIENTED_EDGE('',*,*,#42361,.F.);
#54833=ORIENTED_EDGE('',*,*,#42362,.T.);
#54834=ORIENTED_EDGE('',*,*,#42363,.T.);
#54835=ORIENTED_EDGE('',*,*,#42360,.F.);
#54836=ORIENTED_EDGE('',*,*,#42358,.T.);
#54837=ORIENTED_EDGE('',*,*,#42363,.F.);
#54838=ORIENTED_EDGE('',*,*,#42364,.T.);
#54839=ORIENTED_EDGE('',*,*,#42349,.F.);
#54840=ORIENTED_EDGE('',*,*,#41284,.F.);
#54841=ORIENTED_EDGE('',*,*,#42365,.T.);
#54842=ORIENTED_EDGE('',*,*,#42364,.F.);
#54843=ORIENTED_EDGE('',*,*,#42362,.F.);
#54844=ORIENTED_EDGE('',*,*,#41283,.F.);
#54845=ORIENTED_EDGE('',*,*,#41282,.F.);
#54846=ORIENTED_EDGE('',*,*,#42366,.T.);
#54847=ORIENTED_EDGE('',*,*,#42350,.F.);
#54848=ORIENTED_EDGE('',*,*,#42365,.F.);
#54849=ORIENTED_EDGE('',*,*,#41281,.F.);
#54850=ORIENTED_EDGE('',*,*,#42367,.T.);
#54851=ORIENTED_EDGE('',*,*,#42368,.F.);
#54852=ORIENTED_EDGE('',*,*,#42366,.F.);
#54853=ORIENTED_EDGE('',*,*,#42369,.T.);
#54854=ORIENTED_EDGE('',*,*,#42351,.F.);
#54855=ORIENTED_EDGE('',*,*,#42368,.T.);
#54856=ORIENTED_EDGE('',*,*,#42370,.F.);
#54857=ORIENTED_EDGE('',*,*,#42370,.T.);
#54858=ORIENTED_EDGE('',*,*,#42367,.F.);
#54859=ORIENTED_EDGE('',*,*,#42371,.F.);
#54860=ORIENTED_EDGE('',*,*,#42372,.F.);
#54861=ORIENTED_EDGE('',*,*,#42369,.F.);
#54862=ORIENTED_EDGE('',*,*,#42372,.T.);
#54863=ORIENTED_EDGE('',*,*,#42373,.F.);
#54864=ORIENTED_EDGE('',*,*,#42374,.F.);
#54865=ORIENTED_EDGE('',*,*,#42352,.F.);
#54866=ORIENTED_EDGE('',*,*,#42374,.T.);
#54867=ORIENTED_EDGE('',*,*,#42375,.F.);
#54868=ORIENTED_EDGE('',*,*,#42376,.F.);
#54869=ORIENTED_EDGE('',*,*,#42353,.F.);
#54870=ORIENTED_EDGE('',*,*,#42376,.T.);
#54871=ORIENTED_EDGE('',*,*,#42377,.F.);
#54872=ORIENTED_EDGE('',*,*,#42378,.F.);
#54873=ORIENTED_EDGE('',*,*,#42355,.F.);
#54874=ORIENTED_EDGE('',*,*,#42378,.T.);
#54875=ORIENTED_EDGE('',*,*,#42377,.T.);
#54876=ORIENTED_EDGE('',*,*,#42379,.T.);
#54877=ORIENTED_EDGE('',*,*,#42380,.F.);
#54878=ORIENTED_EDGE('',*,*,#42381,.F.);
#54879=ORIENTED_EDGE('',*,*,#42382,.F.);
#54880=ORIENTED_EDGE('',*,*,#42383,.T.);
#54881=ORIENTED_EDGE('',*,*,#42359,.T.);
#54882=ORIENTED_EDGE('',*,*,#42356,.T.);
#54883=ORIENTED_EDGE('',*,*,#42383,.F.);
#54884=ORIENTED_EDGE('',*,*,#42384,.F.);
#54885=ORIENTED_EDGE('',*,*,#42385,.T.);
#54886=ORIENTED_EDGE('',*,*,#41285,.T.);
#54887=ORIENTED_EDGE('',*,*,#42361,.T.);
#54888=ORIENTED_EDGE('',*,*,#42384,.T.);
#54889=ORIENTED_EDGE('',*,*,#42386,.F.);
#54890=ORIENTED_EDGE('',*,*,#42387,.F.);
#54891=ORIENTED_EDGE('',*,*,#42388,.T.);
#54892=ORIENTED_EDGE('',*,*,#42389,.F.);
#54893=ORIENTED_EDGE('',*,*,#42390,.F.);
#54894=ORIENTED_EDGE('',*,*,#42391,.T.);
#54895=ORIENTED_EDGE('',*,*,#42392,.T.);
#54896=ORIENTED_EDGE('',*,*,#42393,.T.);
#54897=ORIENTED_EDGE('',*,*,#42391,.F.);
#54898=ORIENTED_EDGE('',*,*,#42394,.F.);
#54899=ORIENTED_EDGE('',*,*,#42395,.T.);
#54900=ORIENTED_EDGE('',*,*,#42396,.T.);
#54901=ORIENTED_EDGE('',*,*,#42394,.T.);
#54902=ORIENTED_EDGE('',*,*,#42397,.F.);
#54903=ORIENTED_EDGE('',*,*,#42398,.F.);
#54904=ORIENTED_EDGE('',*,*,#42399,.F.);
#54905=ORIENTED_EDGE('',*,*,#42400,.T.);
#54906=ORIENTED_EDGE('',*,*,#42401,.T.);
#54907=ORIENTED_EDGE('',*,*,#42402,.T.);
#54908=ORIENTED_EDGE('',*,*,#42400,.F.);
#54909=ORIENTED_EDGE('',*,*,#42403,.F.);
#54910=ORIENTED_EDGE('',*,*,#42404,.T.);
#54911=ORIENTED_EDGE('',*,*,#42403,.T.);
#54912=ORIENTED_EDGE('',*,*,#42405,.F.);
#54913=ORIENTED_EDGE('',*,*,#42406,.T.);
#54914=ORIENTED_EDGE('',*,*,#42407,.T.);
#54915=ORIENTED_EDGE('',*,*,#42408,.F.);
#54916=ORIENTED_EDGE('',*,*,#42409,.T.);
#54917=ORIENTED_EDGE('',*,*,#42410,.T.);
#54918=ORIENTED_EDGE('',*,*,#42411,.F.);
#54919=ORIENTED_EDGE('',*,*,#42412,.T.);
#54920=ORIENTED_EDGE('',*,*,#42371,.T.);
#54921=ORIENTED_EDGE('',*,*,#41280,.T.);
#54922=ORIENTED_EDGE('',*,*,#41279,.F.);
#54923=ORIENTED_EDGE('',*,*,#42413,.T.);
#54924=ORIENTED_EDGE('',*,*,#42414,.F.);
#54925=ORIENTED_EDGE('',*,*,#42415,.F.);
#54926=ORIENTED_EDGE('',*,*,#42404,.F.);
#54927=ORIENTED_EDGE('',*,*,#42415,.T.);
#54928=ORIENTED_EDGE('',*,*,#42416,.T.);
#54929=ORIENTED_EDGE('',*,*,#42417,.F.);
#54930=ORIENTED_EDGE('',*,*,#42418,.F.);
#54931=ORIENTED_EDGE('',*,*,#42419,.T.);
#54932=ORIENTED_EDGE('',*,*,#42401,.F.);
#54933=ORIENTED_EDGE('',*,*,#42417,.T.);
#54934=ORIENTED_EDGE('',*,*,#42420,.F.);
#54935=ORIENTED_EDGE('',*,*,#42421,.T.);
#54936=ORIENTED_EDGE('',*,*,#42402,.F.);
#54937=ORIENTED_EDGE('',*,*,#42419,.F.);
#54938=ORIENTED_EDGE('',*,*,#42422,.F.);
#54939=ORIENTED_EDGE('',*,*,#42423,.T.);
#54940=ORIENTED_EDGE('',*,*,#42396,.F.);
#54941=ORIENTED_EDGE('',*,*,#42395,.F.);
#54942=ORIENTED_EDGE('',*,*,#42421,.F.);
#54943=ORIENTED_EDGE('',*,*,#42424,.F.);
#54944=ORIENTED_EDGE('',*,*,#42425,.T.);
#54945=ORIENTED_EDGE('',*,*,#42392,.F.);
#54946=ORIENTED_EDGE('',*,*,#42423,.F.);
#54947=ORIENTED_EDGE('',*,*,#42426,.F.);
#54948=ORIENTED_EDGE('',*,*,#42427,.T.);
#54949=ORIENTED_EDGE('',*,*,#42393,.F.);
#54950=ORIENTED_EDGE('',*,*,#42425,.F.);
#54951=ORIENTED_EDGE('',*,*,#42428,.T.);
#54952=ORIENTED_EDGE('',*,*,#42429,.F.);
#54953=ORIENTED_EDGE('',*,*,#42385,.F.);
#54954=ORIENTED_EDGE('',*,*,#42427,.F.);
#54955=ORIENTED_EDGE('',*,*,#41286,.F.);
#54956=ORIENTED_EDGE('',*,*,#42429,.T.);
#54957=ORIENTED_EDGE('',*,*,#42430,.F.);
#54958=ORIENTED_EDGE('',*,*,#42431,.F.);
#54959=ORIENTED_EDGE('',*,*,#41278,.F.);
#54960=ORIENTED_EDGE('',*,*,#41277,.F.);
#54961=ORIENTED_EDGE('',*,*,#42431,.T.);
#54962=ORIENTED_EDGE('',*,*,#42432,.F.);
#54963=ORIENTED_EDGE('',*,*,#42413,.F.);
#54964=ORIENTED_EDGE('',*,*,#42424,.T.);
#54965=ORIENTED_EDGE('',*,*,#42422,.T.);
#54966=ORIENTED_EDGE('',*,*,#42420,.T.);
#54967=ORIENTED_EDGE('',*,*,#42433,.T.);
#54968=ORIENTED_EDGE('',*,*,#42432,.T.);
#54969=ORIENTED_EDGE('',*,*,#42434,.T.);
#54970=ORIENTED_EDGE('',*,*,#41470,.T.);
#54971=ORIENTED_EDGE('',*,*,#42426,.T.);
#54972=ORIENTED_EDGE('',*,*,#42434,.F.);
#54973=ORIENTED_EDGE('',*,*,#42430,.T.);
#54974=ORIENTED_EDGE('',*,*,#42428,.F.);
#54975=ORIENTED_EDGE('',*,*,#42418,.T.);
#54976=ORIENTED_EDGE('',*,*,#42416,.F.);
#54977=ORIENTED_EDGE('',*,*,#42414,.T.);
#54978=ORIENTED_EDGE('',*,*,#42433,.F.);
#54979=ORIENTED_EDGE('',*,*,#42375,.T.);
#54980=ORIENTED_EDGE('',*,*,#42373,.T.);
#54981=ORIENTED_EDGE('',*,*,#42412,.F.);
#54982=ORIENTED_EDGE('',*,*,#42379,.F.);
#54983=ORIENTED_EDGE('',*,*,#42435,.F.);
#54984=ORIENTED_EDGE('',*,*,#42380,.T.);
#54985=ORIENTED_EDGE('',*,*,#42411,.T.);
#54986=ORIENTED_EDGE('',*,*,#42436,.F.);
#54987=ORIENTED_EDGE('',*,*,#42437,.F.);
#54988=ORIENTED_EDGE('',*,*,#42436,.T.);
#54989=ORIENTED_EDGE('',*,*,#42438,.T.);
#54990=ORIENTED_EDGE('',*,*,#41275,.F.);
#54991=ORIENTED_EDGE('',*,*,#42439,.T.);
#54992=ORIENTED_EDGE('',*,*,#42440,.T.);
#54993=ORIENTED_EDGE('',*,*,#42441,.F.);
#54994=ORIENTED_EDGE('',*,*,#41276,.F.);
#54995=ORIENTED_EDGE('',*,*,#42381,.T.);
#54996=ORIENTED_EDGE('',*,*,#42435,.T.);
#54997=ORIENTED_EDGE('',*,*,#42437,.T.);
#54998=ORIENTED_EDGE('',*,*,#41274,.T.);
#54999=ORIENTED_EDGE('',*,*,#42441,.T.);
#55000=ORIENTED_EDGE('',*,*,#42442,.T.);
#55001=ORIENTED_EDGE('',*,*,#42386,.T.);
#55002=ORIENTED_EDGE('',*,*,#42382,.T.);
#55003=ORIENTED_EDGE('',*,*,#42442,.F.);
#55004=ORIENTED_EDGE('',*,*,#42440,.F.);
#55005=ORIENTED_EDGE('',*,*,#42439,.F.);
#55006=ORIENTED_EDGE('',*,*,#41224,.F.);
#55007=ORIENTED_EDGE('',*,*,#42443,.T.);
#55008=ORIENTED_EDGE('',*,*,#42387,.T.);
#55009=ORIENTED_EDGE('',*,*,#41255,.T.);
#55010=ORIENTED_EDGE('',*,*,#42444,.T.);
#55011=ORIENTED_EDGE('',*,*,#42443,.F.);
#55012=ORIENTED_EDGE('',*,*,#42445,.F.);
#55013=ORIENTED_EDGE('',*,*,#41256,.F.);
#55014=ORIENTED_EDGE('',*,*,#42445,.T.);
#55015=ORIENTED_EDGE('',*,*,#41223,.T.);
#55016=ORIENTED_EDGE('',*,*,#41222,.T.);
#55017=ORIENTED_EDGE('',*,*,#42446,.F.);
#55018=ORIENTED_EDGE('',*,*,#41257,.F.);
#55019=ORIENTED_EDGE('',*,*,#42446,.T.);
#55020=ORIENTED_EDGE('',*,*,#42447,.F.);
#55021=ORIENTED_EDGE('',*,*,#42448,.F.);
#55022=ORIENTED_EDGE('',*,*,#42449,.F.);
#55023=ORIENTED_EDGE('',*,*,#42448,.T.);
#55024=ORIENTED_EDGE('',*,*,#42450,.F.);
#55025=ORIENTED_EDGE('',*,*,#42451,.F.);
#55026=ORIENTED_EDGE('',*,*,#42452,.T.);
#55027=ORIENTED_EDGE('',*,*,#42451,.T.);
#55028=ORIENTED_EDGE('',*,*,#42409,.F.);
#55029=ORIENTED_EDGE('',*,*,#42453,.T.);
#55030=ORIENTED_EDGE('',*,*,#41258,.F.);
#55031=ORIENTED_EDGE('',*,*,#42449,.T.);
#55032=ORIENTED_EDGE('',*,*,#42452,.F.);
#55033=ORIENTED_EDGE('',*,*,#42454,.T.);
#55034=ORIENTED_EDGE('',*,*,#42455,.T.);
#55035=ORIENTED_EDGE('',*,*,#42456,.F.);
#55036=ORIENTED_EDGE('',*,*,#42457,.T.);
#55037=ORIENTED_EDGE('',*,*,#41269,.T.);
#55038=ORIENTED_EDGE('',*,*,#41254,.F.);
#55039=ORIENTED_EDGE('',*,*,#41273,.F.);
#55040=ORIENTED_EDGE('',*,*,#42458,.T.);
#55041=ORIENTED_EDGE('',*,*,#42388,.F.);
#55042=ORIENTED_EDGE('',*,*,#42444,.F.);
#55043=ORIENTED_EDGE('',*,*,#41272,.T.);
#55044=ORIENTED_EDGE('',*,*,#42459,.T.);
#55045=ORIENTED_EDGE('',*,*,#42460,.F.);
#55046=ORIENTED_EDGE('',*,*,#42458,.F.);
#55047=ORIENTED_EDGE('',*,*,#42461,.F.);
#55048=ORIENTED_EDGE('',*,*,#42389,.T.);
#55049=ORIENTED_EDGE('',*,*,#42460,.T.);
#55050=ORIENTED_EDGE('',*,*,#41253,.F.);
#55051=ORIENTED_EDGE('',*,*,#42462,.F.);
#55052=ORIENTED_EDGE('',*,*,#41252,.T.);
#55053=ORIENTED_EDGE('',*,*,#42463,.T.);
#55054=ORIENTED_EDGE('',*,*,#42464,.F.);
#55055=ORIENTED_EDGE('',*,*,#42406,.F.);
#55056=ORIENTED_EDGE('',*,*,#42457,.F.);
#55057=ORIENTED_EDGE('',*,*,#42465,.T.);
#55058=ORIENTED_EDGE('',*,*,#42464,.T.);
#55059=ORIENTED_EDGE('',*,*,#42466,.F.);
#55060=ORIENTED_EDGE('',*,*,#41270,.F.);
#55061=ORIENTED_EDGE('',*,*,#42466,.T.);
#55062=ORIENTED_EDGE('',*,*,#42463,.F.);
#55063=ORIENTED_EDGE('',*,*,#42467,.F.);
#55064=ORIENTED_EDGE('',*,*,#41271,.F.);
#55065=ORIENTED_EDGE('',*,*,#42467,.T.);
#55066=ORIENTED_EDGE('',*,*,#41251,.T.);
#55067=ORIENTED_EDGE('',*,*,#41250,.T.);
#55068=ORIENTED_EDGE('',*,*,#42459,.F.);
#55069=ORIENTED_EDGE('',*,*,#42456,.T.);
#55070=ORIENTED_EDGE('',*,*,#42407,.F.);
#55071=ORIENTED_EDGE('',*,*,#42465,.F.);
#55072=ORIENTED_EDGE('',*,*,#42462,.T.);
#55073=ORIENTED_EDGE('',*,*,#42468,.T.);
#55074=ORIENTED_EDGE('',*,*,#42469,.F.);
#55075=ORIENTED_EDGE('',*,*,#41247,.F.);
#55076=ORIENTED_EDGE('',*,*,#42470,.F.);
#55077=ORIENTED_EDGE('',*,*,#42471,.T.);
#55078=ORIENTED_EDGE('',*,*,#42461,.T.);
#55079=ORIENTED_EDGE('',*,*,#41249,.F.);
#55080=ORIENTED_EDGE('',*,*,#42472,.F.);
#55081=ORIENTED_EDGE('',*,*,#42397,.T.);
#55082=ORIENTED_EDGE('',*,*,#42390,.T.);
#55083=ORIENTED_EDGE('',*,*,#42471,.F.);
#55084=ORIENTED_EDGE('',*,*,#42398,.T.);
#55085=ORIENTED_EDGE('',*,*,#42472,.T.);
#55086=ORIENTED_EDGE('',*,*,#42470,.T.);
#55087=ORIENTED_EDGE('',*,*,#41248,.T.);
#55088=ORIENTED_EDGE('',*,*,#42469,.T.);
#55089=ORIENTED_EDGE('',*,*,#42473,.T.);
#55090=ORIENTED_EDGE('',*,*,#42405,.T.);
#55091=ORIENTED_EDGE('',*,*,#42399,.T.);
#55092=ORIENTED_EDGE('',*,*,#42473,.F.);
#55093=ORIENTED_EDGE('',*,*,#42468,.F.);
#55094=ORIENTED_EDGE('',*,*,#41264,.T.);
#55095=ORIENTED_EDGE('',*,*,#41194,.F.);
#55096=ORIENTED_EDGE('',*,*,#42474,.F.);
#55097=ORIENTED_EDGE('',*,*,#42059,.T.);
#55098=ORIENTED_EDGE('',*,*,#41259,.F.);
#55099=ORIENTED_EDGE('',*,*,#42475,.F.);
#55100=ORIENTED_EDGE('',*,*,#42476,.F.);
#55101=ORIENTED_EDGE('',*,*,#42475,.T.);
#55102=ORIENTED_EDGE('',*,*,#42453,.F.);
#55103=ORIENTED_EDGE('',*,*,#42477,.F.);
#55104=ORIENTED_EDGE('',*,*,#42478,.F.);
#55105=ORIENTED_EDGE('',*,*,#42477,.T.);
#55106=ORIENTED_EDGE('',*,*,#41268,.F.);
#55107=ORIENTED_EDGE('',*,*,#42054,.F.);
#55108=ORIENTED_EDGE('',*,*,#42474,.T.);
#55109=ORIENTED_EDGE('',*,*,#42476,.T.);
#55110=ORIENTED_EDGE('',*,*,#42478,.T.);
#55111=ORIENTED_EDGE('',*,*,#42052,.T.);
#55112=ORIENTED_EDGE('',*,*,#42479,.T.);
#55113=ORIENTED_EDGE('',*,*,#42480,.T.);
#55114=ORIENTED_EDGE('',*,*,#42481,.T.);
#55115=ORIENTED_EDGE('',*,*,#42061,.F.);
#55116=ORIENTED_EDGE('',*,*,#42481,.F.);
#55117=ORIENTED_EDGE('',*,*,#42482,.T.);
#55118=ORIENTED_EDGE('',*,*,#42483,.F.);
#55119=ORIENTED_EDGE('',*,*,#42484,.F.);
#55120=ORIENTED_EDGE('',*,*,#42062,.F.);
#55121=ORIENTED_EDGE('',*,*,#42484,.T.);
#55122=ORIENTED_EDGE('',*,*,#42485,.F.);
#55123=ORIENTED_EDGE('',*,*,#42486,.F.);
#55124=ORIENTED_EDGE('',*,*,#42487,.F.);
#55125=ORIENTED_EDGE('',*,*,#42488,.T.);
#55126=ORIENTED_EDGE('',*,*,#42489,.F.);
#55127=ORIENTED_EDGE('',*,*,#42486,.T.);
#55128=ORIENTED_EDGE('',*,*,#42489,.T.);
#55129=ORIENTED_EDGE('',*,*,#42490,.T.);
#55130=ORIENTED_EDGE('',*,*,#42065,.T.);
#55131=ORIENTED_EDGE('',*,*,#42063,.F.);
#55132=ORIENTED_EDGE('',*,*,#42491,.F.);
#55133=ORIENTED_EDGE('',*,*,#42492,.T.);
#55134=ORIENTED_EDGE('',*,*,#42490,.F.);
#55135=ORIENTED_EDGE('',*,*,#42488,.F.);
#55136=ORIENTED_EDGE('',*,*,#42493,.F.);
#55137=ORIENTED_EDGE('',*,*,#42494,.T.);
#55138=ORIENTED_EDGE('',*,*,#42066,.T.);
#55139=ORIENTED_EDGE('',*,*,#42492,.F.);
#55140=ORIENTED_EDGE('',*,*,#42495,.F.);
#55141=ORIENTED_EDGE('',*,*,#42496,.T.);
#55142=ORIENTED_EDGE('',*,*,#42047,.F.);
#55143=ORIENTED_EDGE('',*,*,#42494,.F.);
#55144=ORIENTED_EDGE('',*,*,#42497,.F.);
#55145=ORIENTED_EDGE('',*,*,#42498,.T.);
#55146=ORIENTED_EDGE('',*,*,#42499,.F.);
#55147=ORIENTED_EDGE('',*,*,#42496,.F.);
#55148=ORIENTED_EDGE('',*,*,#42499,.T.);
#55149=ORIENTED_EDGE('',*,*,#42500,.T.);
#55150=ORIENTED_EDGE('',*,*,#42050,.T.);
#55151=ORIENTED_EDGE('',*,*,#42048,.T.);
#55152=ORIENTED_EDGE('',*,*,#42501,.F.);
#55153=ORIENTED_EDGE('',*,*,#42502,.T.);
#55154=ORIENTED_EDGE('',*,*,#42500,.F.);
#55155=ORIENTED_EDGE('',*,*,#42498,.F.);
#55156=ORIENTED_EDGE('',*,*,#42051,.F.);
#55157=ORIENTED_EDGE('',*,*,#42502,.F.);
#55158=ORIENTED_EDGE('',*,*,#42503,.F.);
#55159=ORIENTED_EDGE('',*,*,#42504,.F.);
#55160=ORIENTED_EDGE('',*,*,#42479,.F.);
#55161=ORIENTED_EDGE('',*,*,#42504,.T.);
#55162=ORIENTED_EDGE('',*,*,#42505,.F.);
#55163=ORIENTED_EDGE('',*,*,#42506,.F.);
#55164=ORIENTED_EDGE('',*,*,#42480,.F.);
#55165=ORIENTED_EDGE('',*,*,#42506,.T.);
#55166=ORIENTED_EDGE('',*,*,#42507,.F.);
#55167=ORIENTED_EDGE('',*,*,#42482,.F.);
#55168=ORIENTED_EDGE('',*,*,#42491,.T.);
#55169=ORIENTED_EDGE('',*,*,#42508,.T.);
#55170=ORIENTED_EDGE('',*,*,#42507,.T.);
#55171=ORIENTED_EDGE('',*,*,#42509,.T.);
#55172=ORIENTED_EDGE('',*,*,#42497,.T.);
#55173=ORIENTED_EDGE('',*,*,#42495,.T.);
#55174=ORIENTED_EDGE('',*,*,#42493,.T.);
#55175=ORIENTED_EDGE('',*,*,#41244,.T.);
#55176=ORIENTED_EDGE('',*,*,#42505,.T.);
#55177=ORIENTED_EDGE('',*,*,#42503,.T.);
#55178=ORIENTED_EDGE('',*,*,#42501,.T.);
#55179=ORIENTED_EDGE('',*,*,#42509,.F.);
#55180=ORIENTED_EDGE('',*,*,#42483,.T.);
#55181=ORIENTED_EDGE('',*,*,#42508,.F.);
#55182=ORIENTED_EDGE('',*,*,#42487,.T.);
#55183=ORIENTED_EDGE('',*,*,#42485,.T.);
#55184=ORIENTED_EDGE('',*,*,#41242,.F.);
#55185=ORIENTED_EDGE('',*,*,#41238,.T.);
#55186=ORIENTED_EDGE('',*,*,#41236,.F.);
#55187=ORIENTED_EDGE('',*,*,#41232,.T.);
#55188=ORIENTED_EDGE('',*,*,#42510,.T.);
#55189=ORIENTED_EDGE('',*,*,#41231,.F.);
#55190=ORIENTED_EDGE('',*,*,#41292,.T.);
#55191=ORIENTED_EDGE('',*,*,#41233,.T.);
#55192=ORIENTED_EDGE('',*,*,#42510,.F.);
#55193=ORIENTED_EDGE('',*,*,#42511,.T.);
#55194=ORIENTED_EDGE('',*,*,#42512,.T.);
#55195=ORIENTED_EDGE('',*,*,#42275,.F.);
#55196=ORIENTED_EDGE('',*,*,#42513,.T.);
#55197=ORIENTED_EDGE('',*,*,#42514,.T.);
#55198=ORIENTED_EDGE('',*,*,#41294,.T.);
#55199=ORIENTED_EDGE('',*,*,#41296,.T.);
#55200=ORIENTED_EDGE('',*,*,#41295,.F.);
#55201=ORIENTED_EDGE('',*,*,#42514,.F.);
#55202=ORIENTED_EDGE('',*,*,#42515,.T.);
#55203=ORIENTED_EDGE('',*,*,#42516,.T.);
#55204=ORIENTED_EDGE('',*,*,#42517,.T.);
#55205=ORIENTED_EDGE('',*,*,#42518,.T.);
#55206=ORIENTED_EDGE('',*,*,#42519,.F.);
#55207=ORIENTED_EDGE('',*,*,#42520,.T.);
#55208=ORIENTED_EDGE('',*,*,#42318,.T.);
#55209=ORIENTED_EDGE('',*,*,#42316,.T.);
#55210=ORIENTED_EDGE('',*,*,#42521,.T.);
#55211=ORIENTED_EDGE('',*,*,#42511,.F.);
#55212=ORIENTED_EDGE('',*,*,#42522,.T.);
#55213=ORIENTED_EDGE('',*,*,#42521,.F.);
#55214=ORIENTED_EDGE('',*,*,#42315,.F.);
#55215=ORIENTED_EDGE('',*,*,#42523,.T.);
#55216=ORIENTED_EDGE('',*,*,#42313,.F.);
#55217=ORIENTED_EDGE('',*,*,#42524,.F.);
#55218=ORIENTED_EDGE('',*,*,#42523,.F.);
#55219=ORIENTED_EDGE('',*,*,#42310,.T.);
#55220=ORIENTED_EDGE('',*,*,#42276,.F.);
#55221=ORIENTED_EDGE('',*,*,#42525,.F.);
#55222=ORIENTED_EDGE('',*,*,#42524,.T.);
#55223=ORIENTED_EDGE('',*,*,#42522,.F.);
#55224=ORIENTED_EDGE('',*,*,#42525,.T.);
#55225=ORIENTED_EDGE('',*,*,#42512,.F.);
#55226=ORIENTED_EDGE('',*,*,#42319,.T.);
#55227=ORIENTED_EDGE('',*,*,#42520,.F.);
#55228=ORIENTED_EDGE('',*,*,#42526,.F.);
#55229=ORIENTED_EDGE('',*,*,#42527,.T.);
#55230=ORIENTED_EDGE('',*,*,#42528,.F.);
#55231=ORIENTED_EDGE('',*,*,#42323,.F.);
#55232=ORIENTED_EDGE('',*,*,#42321,.T.);
#55233=ORIENTED_EDGE('',*,*,#42527,.F.);
#55234=ORIENTED_EDGE('',*,*,#42529,.F.);
#55235=ORIENTED_EDGE('',*,*,#42530,.F.);
#55236=ORIENTED_EDGE('',*,*,#42531,.T.);
#55237=ORIENTED_EDGE('',*,*,#42518,.F.);
#55238=ORIENTED_EDGE('',*,*,#42532,.F.);
#55239=ORIENTED_EDGE('',*,*,#42530,.T.);
#55240=ORIENTED_EDGE('',*,*,#42532,.T.);
#55241=ORIENTED_EDGE('',*,*,#42517,.F.);
#55242=ORIENTED_EDGE('',*,*,#42533,.F.);
#55243=ORIENTED_EDGE('',*,*,#42534,.T.);
#55244=ORIENTED_EDGE('',*,*,#42535,.F.);
#55245=ORIENTED_EDGE('',*,*,#42324,.F.);
#55246=ORIENTED_EDGE('',*,*,#42528,.T.);
#55247=ORIENTED_EDGE('',*,*,#42534,.F.);
#55248=ORIENTED_EDGE('',*,*,#41885,.F.);
#55249=ORIENTED_EDGE('',*,*,#42535,.T.);
#55250=ORIENTED_EDGE('',*,*,#42536,.F.);
#55251=ORIENTED_EDGE('',*,*,#42537,.T.);
#55252=ORIENTED_EDGE('',*,*,#42538,.F.);
#55253=ORIENTED_EDGE('',*,*,#42539,.T.);
#55254=ORIENTED_EDGE('',*,*,#42273,.F.);
#55255=ORIENTED_EDGE('',*,*,#42540,.F.);
#55256=ORIENTED_EDGE('',*,*,#42538,.T.);
#55257=ORIENTED_EDGE('',*,*,#42540,.T.);
#55258=ORIENTED_EDGE('',*,*,#42272,.F.);
#55259=ORIENTED_EDGE('',*,*,#42541,.F.);
#55260=ORIENTED_EDGE('',*,*,#41886,.T.);
#55261=ORIENTED_EDGE('',*,*,#42542,.F.);
#55262=ORIENTED_EDGE('',*,*,#42543,.F.);
#55263=ORIENTED_EDGE('',*,*,#42541,.T.);
#55264=ORIENTED_EDGE('',*,*,#42543,.T.);
#55265=ORIENTED_EDGE('',*,*,#42303,.F.);
#55266=ORIENTED_EDGE('',*,*,#42544,.F.);
#55267=ORIENTED_EDGE('',*,*,#41887,.T.);
#55268=ORIENTED_EDGE('',*,*,#42544,.T.);
#55269=ORIENTED_EDGE('',*,*,#42545,.F.);
#55270=ORIENTED_EDGE('',*,*,#42546,.F.);
#55271=ORIENTED_EDGE('',*,*,#41888,.T.);
#55272=ORIENTED_EDGE('',*,*,#42546,.T.);
#55273=ORIENTED_EDGE('',*,*,#42547,.F.);
#55274=ORIENTED_EDGE('',*,*,#41987,.F.);
#55275=ORIENTED_EDGE('',*,*,#41858,.T.);
#55276=ORIENTED_EDGE('',*,*,#42254,.T.);
#55277=ORIENTED_EDGE('',*,*,#42547,.T.);
#55278=ORIENTED_EDGE('',*,*,#42545,.T.);
#55279=ORIENTED_EDGE('',*,*,#42302,.F.);
#55280=ORIENTED_EDGE('',*,*,#42548,.F.);
#55281=ORIENTED_EDGE('',*,*,#42548,.T.);
#55282=ORIENTED_EDGE('',*,*,#42549,.T.);
#55283=ORIENTED_EDGE('',*,*,#42261,.F.);
#55284=ORIENTED_EDGE('',*,*,#42247,.F.);
#55285=ORIENTED_EDGE('',*,*,#41933,.F.);
#55286=ORIENTED_EDGE('',*,*,#42550,.F.);
#55287=ORIENTED_EDGE('',*,*,#41927,.F.);
#55288=ORIENTED_EDGE('',*,*,#41930,.F.);
#55289=ORIENTED_EDGE('',*,*,#41925,.F.);
#55290=ORIENTED_EDGE('',*,*,#42255,.F.);
#55291=ORIENTED_EDGE('',*,*,#41931,.T.);
#55292=ORIENTED_EDGE('',*,*,#41928,.T.);
#55293=ORIENTED_EDGE('',*,*,#42550,.T.);
#55294=ORIENTED_EDGE('',*,*,#41932,.T.);
#55295=ORIENTED_EDGE('',*,*,#42257,.F.);
#55296=ORIENTED_EDGE('',*,*,#42263,.F.);
#55297=ORIENTED_EDGE('',*,*,#42549,.F.);
#55298=ORIENTED_EDGE('',*,*,#42305,.T.);
#55299=ORIENTED_EDGE('',*,*,#41229,.T.);
#55300=ORIENTED_EDGE('',*,*,#42304,.F.);
#55301=ORIENTED_EDGE('',*,*,#42542,.T.);
#55302=ORIENTED_EDGE('',*,*,#42271,.T.);
#55303=ORIENTED_EDGE('',*,*,#41225,.F.);
#55304=ORIENTED_EDGE('',*,*,#42551,.T.);
#55305=ORIENTED_EDGE('',*,*,#42274,.F.);
#55306=ORIENTED_EDGE('',*,*,#42539,.F.);
#55307=ORIENTED_EDGE('',*,*,#42552,.T.);
#55308=ORIENTED_EDGE('',*,*,#42537,.F.);
#55309=ORIENTED_EDGE('',*,*,#42553,.F.);
#55310=ORIENTED_EDGE('',*,*,#42552,.F.);
#55311=ORIENTED_EDGE('',*,*,#42554,.T.);
#55312=ORIENTED_EDGE('',*,*,#42515,.F.);
#55313=ORIENTED_EDGE('',*,*,#42555,.F.);
#55314=ORIENTED_EDGE('',*,*,#42553,.T.);
#55315=ORIENTED_EDGE('',*,*,#42551,.F.);
#55316=ORIENTED_EDGE('',*,*,#42555,.T.);
#55317=ORIENTED_EDGE('',*,*,#42513,.F.);
#55318=ORIENTED_EDGE('',*,*,#42533,.T.);
#55319=ORIENTED_EDGE('',*,*,#42516,.F.);
#55320=ORIENTED_EDGE('',*,*,#42554,.F.);
#55321=ORIENTED_EDGE('',*,*,#42536,.T.);
#55322=ORIENTED_EDGE('',*,*,#42526,.T.);
#55323=ORIENTED_EDGE('',*,*,#42556,.F.);
#55324=ORIENTED_EDGE('',*,*,#42531,.F.);
#55325=ORIENTED_EDGE('',*,*,#42529,.T.);
#55326=ORIENTED_EDGE('',*,*,#42519,.T.);
#55327=ORIENTED_EDGE('',*,*,#42556,.T.);
#55328=ORIENTED_EDGE('',*,*,#42454,.F.);
#55329=ORIENTED_EDGE('',*,*,#42408,.T.);
#55330=ORIENTED_EDGE('',*,*,#42455,.F.);
#55331=ORIENTED_EDGE('',*,*,#42438,.F.);
#55332=ORIENTED_EDGE('',*,*,#42410,.F.);
#55333=ORIENTED_EDGE('',*,*,#42450,.T.);
#55334=ORIENTED_EDGE('',*,*,#42447,.T.);
#55335=ORIENTED_EDGE('',*,*,#41221,.T.);
#55336=ORIENTED_EDGE('',*,*,#42557,.F.);
#55337=ORIENTED_EDGE('',*,*,#42327,.F.);
#55338=ORIENTED_EDGE('',*,*,#41906,.T.);
#55339=ORIENTED_EDGE('',*,*,#42558,.T.);
#55340=ORIENTED_EDGE('',*,*,#42332,.T.);
#55341=ORIENTED_EDGE('',*,*,#41217,.F.);
#55342=ORIENTED_EDGE('',*,*,#41215,.F.);
#55343=ORIENTED_EDGE('',*,*,#42559,.T.);
#55344=ORIENTED_EDGE('',*,*,#41219,.T.);
#55345=ORIENTED_EDGE('',*,*,#41962,.F.);
#55346=ORIENTED_EDGE('',*,*,#42560,.F.);
#55347=ORIENTED_EDGE('',*,*,#42560,.T.);
#55348=ORIENTED_EDGE('',*,*,#41966,.F.);
#55349=ORIENTED_EDGE('',*,*,#41837,.F.);
#55350=ORIENTED_EDGE('',*,*,#42561,.F.);
#55351=ORIENTED_EDGE('',*,*,#42561,.T.);
#55352=ORIENTED_EDGE('',*,*,#42562,.T.);
#55353=ORIENTED_EDGE('',*,*,#42563,.F.);
#55354=ORIENTED_EDGE('',*,*,#42564,.F.);
#55355=ORIENTED_EDGE('',*,*,#42328,.T.);
#55356=ORIENTED_EDGE('',*,*,#42557,.T.);
#55357=ORIENTED_EDGE('',*,*,#42559,.F.);
#55358=ORIENTED_EDGE('',*,*,#42563,.T.);
#55359=ORIENTED_EDGE('',*,*,#42565,.T.);
#55360=ORIENTED_EDGE('',*,*,#41954,.F.);
#55361=ORIENTED_EDGE('',*,*,#41951,.T.);
#55362=ORIENTED_EDGE('',*,*,#42566,.T.);
#55363=ORIENTED_EDGE('',*,*,#41350,.F.);
#55364=ORIENTED_EDGE('',*,*,#42567,.T.);
#55365=ORIENTED_EDGE('',*,*,#41959,.T.);
#55366=ORIENTED_EDGE('',*,*,#42568,.T.);
#55367=ORIENTED_EDGE('',*,*,#41949,.T.);
#55368=ORIENTED_EDGE('',*,*,#42568,.F.);
#55369=ORIENTED_EDGE('',*,*,#41897,.F.);
#55370=ORIENTED_EDGE('',*,*,#41829,.T.);
#55371=ORIENTED_EDGE('',*,*,#42569,.F.);
#55372=ORIENTED_EDGE('',*,*,#41854,.T.);
#55373=ORIENTED_EDGE('',*,*,#42570,.F.);
#55374=ORIENTED_EDGE('',*,*,#41824,.F.);
#55375=ORIENTED_EDGE('',*,*,#41825,.F.);
#55376=ORIENTED_EDGE('',*,*,#42570,.T.);
#55377=ORIENTED_EDGE('',*,*,#42571,.T.);
#55378=ORIENTED_EDGE('',*,*,#42572,.F.);
#55379=ORIENTED_EDGE('',*,*,#42566,.F.);
#55380=ORIENTED_EDGE('',*,*,#41950,.F.);
#55381=ORIENTED_EDGE('',*,*,#42572,.T.);
#55382=ORIENTED_EDGE('',*,*,#41853,.F.);
#55383=ORIENTED_EDGE('',*,*,#41290,.F.);
#55384=ORIENTED_EDGE('',*,*,#42564,.T.);
#55385=ORIENTED_EDGE('',*,*,#42571,.F.);
#55386=ORIENTED_EDGE('',*,*,#41901,.T.);
#55387=ORIENTED_EDGE('',*,*,#42567,.F.);
#55388=ORIENTED_EDGE('',*,*,#42573,.F.);
#55389=ORIENTED_EDGE('',*,*,#41833,.T.);
#55390=ORIENTED_EDGE('',*,*,#42573,.T.);
#55391=ORIENTED_EDGE('',*,*,#41349,.F.);
#55392=ORIENTED_EDGE('',*,*,#41956,.F.);
#55393=ORIENTED_EDGE('',*,*,#41834,.T.);
#55394=ORIENTED_EDGE('',*,*,#41957,.T.);
#55395=ORIENTED_EDGE('',*,*,#42565,.F.);
#55396=ORIENTED_EDGE('',*,*,#42562,.F.);
#55397=ORIENTED_EDGE('',*,*,#41836,.T.);
#55398=ORIENTED_EDGE('',*,*,#42574,.T.);
#55399=ORIENTED_EDGE('',*,*,#41963,.F.);
#55400=ORIENTED_EDGE('',*,*,#41218,.F.);
#55401=ORIENTED_EDGE('',*,*,#42334,.T.);
#55402=ORIENTED_EDGE('',*,*,#42575,.T.);
#55403=ORIENTED_EDGE('',*,*,#42576,.T.);
#55404=ORIENTED_EDGE('',*,*,#41964,.F.);
#55405=ORIENTED_EDGE('',*,*,#42574,.F.);
#55406=ORIENTED_EDGE('',*,*,#42577,.F.);
#55407=ORIENTED_EDGE('',*,*,#42575,.F.);
#55408=ORIENTED_EDGE('',*,*,#42333,.F.);
#55409=ORIENTED_EDGE('',*,*,#42578,.T.);
#55410=ORIENTED_EDGE('',*,*,#42579,.F.);
#55411=ORIENTED_EDGE('',*,*,#42578,.F.);
#55412=ORIENTED_EDGE('',*,*,#42558,.F.);
#55413=ORIENTED_EDGE('',*,*,#41905,.T.);
#55414=ORIENTED_EDGE('',*,*,#41967,.T.);
#55415=ORIENTED_EDGE('',*,*,#41998,.T.);
#55416=ORIENTED_EDGE('',*,*,#42348,.F.);
#55417=ORIENTED_EDGE('',*,*,#42580,.F.);
#55418=ORIENTED_EDGE('',*,*,#42346,.T.);
#55419=ORIENTED_EDGE('',*,*,#42581,.F.);
#55420=ORIENTED_EDGE('',*,*,#41969,.F.);
#55421=ORIENTED_EDGE('',*,*,#42580,.T.);
#55422=ORIENTED_EDGE('',*,*,#41972,.T.);
#55423=ORIENTED_EDGE('',*,*,#41970,.T.);
#55424=ORIENTED_EDGE('',*,*,#42581,.T.);
#55425=ORIENTED_EDGE('',*,*,#42345,.T.);
#55426=ORIENTED_EDGE('',*,*,#42343,.T.);
#55427=ORIENTED_EDGE('',*,*,#42582,.T.);
#55428=ORIENTED_EDGE('',*,*,#41911,.T.);
#55429=ORIENTED_EDGE('',*,*,#42583,.F.);
#55430=ORIENTED_EDGE('',*,*,#41914,.F.);
#55431=ORIENTED_EDGE('',*,*,#41919,.F.);
#55432=ORIENTED_EDGE('',*,*,#41918,.F.);
#55433=ORIENTED_EDGE('',*,*,#42584,.F.);
#55434=ORIENTED_EDGE('',*,*,#41922,.F.);
#55435=ORIENTED_EDGE('',*,*,#41841,.T.);
#55436=ORIENTED_EDGE('',*,*,#41912,.F.);
#55437=ORIENTED_EDGE('',*,*,#42584,.T.);
#55438=ORIENTED_EDGE('',*,*,#41917,.T.);
#55439=ORIENTED_EDGE('',*,*,#41920,.T.);
#55440=ORIENTED_EDGE('',*,*,#41866,.F.);
#55441=ORIENTED_EDGE('',*,*,#41846,.F.);
#55442=ORIENTED_EDGE('',*,*,#41921,.T.);
#55443=ORIENTED_EDGE('',*,*,#42582,.F.);
#55444=ORIENTED_EDGE('',*,*,#42342,.F.);
#55445=ORIENTED_EDGE('',*,*,#41869,.T.);
#55446=ORIENTED_EDGE('',*,*,#41915,.T.);
#55447=ORIENTED_EDGE('',*,*,#42583,.T.);
#55448=ORIENTED_EDGE('',*,*,#42279,.T.);
#55449=ORIENTED_EDGE('',*,*,#42307,.T.);
#55450=ORIENTED_EDGE('',*,*,#42300,.F.);
#55451=ORIENTED_EDGE('',*,*,#42288,.F.);
#55452=ORIENTED_EDGE('',*,*,#42239,.T.);
#55453=ORIENTED_EDGE('',*,*,#42232,.T.);
#55454=ORIENTED_EDGE('',*,*,#42292,.F.);
#55455=ORIENTED_EDGE('',*,*,#42296,.F.);
#55456=ORIENTED_EDGE('',*,*,#42280,.F.);
#55457=ORIENTED_EDGE('',*,*,#42287,.T.);
#55458=ORIENTED_EDGE('',*,*,#42585,.T.);
#55459=ORIENTED_EDGE('',*,*,#42585,.F.);
#55460=ORIENTED_EDGE('',*,*,#42285,.T.);
#55461=ORIENTED_EDGE('',*,*,#42282,.T.);
#55462=ORIENTED_EDGE('',*,*,#41991,.T.);
#55463=ORIENTED_EDGE('',*,*,#42253,.F.);
#55464=ORIENTED_EDGE('',*,*,#42122,.F.);
#55465=ORIENTED_EDGE('',*,*,#41872,.T.);
#55466=ORIENTED_EDGE('',*,*,#42162,.T.);
#55467=ORIENTED_EDGE('',*,*,#42212,.F.);
#55468=ORIENTED_EDGE('',*,*,#42586,.F.);
#55469=ORIENTED_EDGE('',*,*,#42169,.T.);
#55470=ORIENTED_EDGE('',*,*,#42586,.T.);
#55471=ORIENTED_EDGE('',*,*,#42211,.F.);
#55472=ORIENTED_EDGE('',*,*,#42587,.F.);
#55473=ORIENTED_EDGE('',*,*,#42171,.T.);
#55474=ORIENTED_EDGE('',*,*,#42587,.T.);
#55475=ORIENTED_EDGE('',*,*,#42210,.F.);
#55476=ORIENTED_EDGE('',*,*,#42588,.F.);
#55477=ORIENTED_EDGE('',*,*,#42174,.T.);
#55478=ORIENTED_EDGE('',*,*,#42588,.T.);
#55479=ORIENTED_EDGE('',*,*,#42209,.F.);
#55480=ORIENTED_EDGE('',*,*,#42589,.F.);
#55481=ORIENTED_EDGE('',*,*,#42177,.T.);
#55482=ORIENTED_EDGE('',*,*,#42589,.T.);
#55483=ORIENTED_EDGE('',*,*,#42208,.F.);
#55484=ORIENTED_EDGE('',*,*,#42206,.F.);
#55485=ORIENTED_EDGE('',*,*,#42179,.T.);
#55486=ORIENTED_EDGE('',*,*,#42010,.F.);
#55487=ORIENTED_EDGE('',*,*,#42149,.F.);
#55488=ORIENTED_EDGE('',*,*,#41986,.T.);
#55489=ORIENTED_EDGE('',*,*,#42590,.T.);
#55490=ORIENTED_EDGE('',*,*,#42002,.T.);
#55491=ORIENTED_EDGE('',*,*,#42591,.F.);
#55492=ORIENTED_EDGE('',*,*,#42590,.F.);
#55493=ORIENTED_EDGE('',*,*,#42591,.T.);
#55494=ORIENTED_EDGE('',*,*,#42001,.T.);
#55495=ORIENTED_EDGE('',*,*,#42592,.F.);
#55496=ORIENTED_EDGE('',*,*,#42011,.F.);
#55497=ORIENTED_EDGE('',*,*,#42592,.T.);
#55498=ORIENTED_EDGE('',*,*,#41347,.T.);
#55499=ORIENTED_EDGE('',*,*,#42006,.F.);
#55500=ORIENTED_EDGE('',*,*,#42012,.F.);
#55501=ORIENTED_EDGE('',*,*,#41195,.T.);
#55502=ORIENTED_EDGE('',*,*,#41889,.T.);
#55503=ORIENTED_EDGE('',*,*,#42339,.T.);
#55504=ORIENTED_EDGE('',*,*,#42335,.T.);
#55505=ORIENTED_EDGE('',*,*,#42338,.F.);
#55506=ORIENTED_EDGE('',*,*,#41850,.T.);
#55507=ORIENTED_EDGE('',*,*,#42569,.T.);
#55508=ORIENTED_EDGE('',*,*,#41823,.T.);
#55509=ORIENTED_EDGE('',*,*,#42593,.T.);
#55510=ORIENTED_EDGE('',*,*,#41830,.T.);
#55511=ORIENTED_EDGE('',*,*,#41965,.T.);
#55512=ORIENTED_EDGE('',*,*,#41960,.T.);
#55513=ORIENTED_EDGE('',*,*,#42576,.F.);
#55514=ORIENTED_EDGE('',*,*,#42577,.T.);
#55515=ORIENTED_EDGE('',*,*,#42579,.T.);
#55516=ORIENTED_EDGE('',*,*,#41904,.T.);
#55517=ORIENTED_EDGE('',*,*,#41822,.F.);
#55518=ORIENTED_EDGE('',*,*,#41896,.T.);
#55519=ORIENTED_EDGE('',*,*,#41958,.F.);
#55520=ORIENTED_EDGE('',*,*,#41899,.T.);
#55521=ORIENTED_EDGE('',*,*,#41831,.F.);
#55522=ORIENTED_EDGE('',*,*,#42593,.F.);
#55523=ORIENTED_EDGE('',*,*,#42594,.F.);
#55524=ORIENTED_EDGE('',*,*,#42595,.F.);
#55525=ORIENTED_EDGE('',*,*,#42596,.F.);
#55526=ORIENTED_EDGE('',*,*,#42597,.F.);
#55527=ORIENTED_EDGE('',*,*,#42598,.F.);
#55528=ORIENTED_EDGE('',*,*,#42599,.F.);
#55529=ORIENTED_EDGE('',*,*,#42600,.F.);
#55530=ORIENTED_EDGE('',*,*,#42601,.F.);
#55531=ORIENTED_EDGE('',*,*,#42594,.T.);
#55532=ORIENTED_EDGE('',*,*,#42602,.T.);
#55533=ORIENTED_EDGE('',*,*,#42603,.T.);
#55534=ORIENTED_EDGE('',*,*,#42604,.T.);
#55535=ORIENTED_EDGE('',*,*,#42605,.T.);
#55536=ORIENTED_EDGE('',*,*,#42606,.T.);
#55537=ORIENTED_EDGE('',*,*,#42607,.T.);
#55538=ORIENTED_EDGE('',*,*,#42604,.F.);
#55539=ORIENTED_EDGE('',*,*,#42608,.T.);
#55540=ORIENTED_EDGE('',*,*,#42602,.F.);
#55541=ORIENTED_EDGE('',*,*,#42598,.T.);
#55542=ORIENTED_EDGE('',*,*,#42609,.F.);
#55543=ORIENTED_EDGE('',*,*,#42610,.F.);
#55544=ORIENTED_EDGE('',*,*,#42611,.F.);
#55545=ORIENTED_EDGE('',*,*,#42612,.T.);
#55546=ORIENTED_EDGE('',*,*,#42613,.T.);
#55547=ORIENTED_EDGE('',*,*,#42614,.T.);
#55548=ORIENTED_EDGE('',*,*,#42615,.T.);
#55549=ORIENTED_EDGE('',*,*,#42616,.T.);
#55550=ORIENTED_EDGE('',*,*,#42617,.F.);
#55551=ORIENTED_EDGE('',*,*,#42618,.F.);
#55552=ORIENTED_EDGE('',*,*,#42619,.F.);
#55553=ORIENTED_EDGE('',*,*,#42620,.T.);
#55554=ORIENTED_EDGE('',*,*,#42621,.T.);
#55555=ORIENTED_EDGE('',*,*,#42622,.T.);
#55556=ORIENTED_EDGE('',*,*,#42623,.F.);
#55557=ORIENTED_EDGE('',*,*,#42624,.F.);
#55558=ORIENTED_EDGE('',*,*,#42622,.F.);
#55559=ORIENTED_EDGE('',*,*,#42625,.T.);
#55560=ORIENTED_EDGE('',*,*,#42620,.F.);
#55561=ORIENTED_EDGE('',*,*,#42626,.F.);
#55562=ORIENTED_EDGE('',*,*,#42603,.F.);
#55563=ORIENTED_EDGE('',*,*,#42627,.T.);
#55564=ORIENTED_EDGE('',*,*,#42621,.F.);
#55565=ORIENTED_EDGE('',*,*,#42625,.F.);
#55566=ORIENTED_EDGE('',*,*,#42627,.F.);
#55567=ORIENTED_EDGE('',*,*,#42608,.F.);
#55568=ORIENTED_EDGE('',*,*,#42618,.T.);
#55569=ORIENTED_EDGE('',*,*,#42628,.T.);
#55570=ORIENTED_EDGE('',*,*,#42629,.F.);
#55571=ORIENTED_EDGE('',*,*,#42630,.T.);
#55572=ORIENTED_EDGE('',*,*,#42623,.T.);
#55573=ORIENTED_EDGE('',*,*,#42624,.T.);
#55574=ORIENTED_EDGE('',*,*,#42631,.T.);
#55575=ORIENTED_EDGE('',*,*,#42632,.F.);
#55576=ORIENTED_EDGE('',*,*,#42631,.F.);
#55577=ORIENTED_EDGE('',*,*,#42633,.T.);
#55578=ORIENTED_EDGE('',*,*,#42634,.T.);
#55579=ORIENTED_EDGE('',*,*,#42635,.T.);
#55580=ORIENTED_EDGE('',*,*,#42636,.F.);
#55581=ORIENTED_EDGE('',*,*,#42637,.F.);
#55582=ORIENTED_EDGE('',*,*,#42638,.T.);
#55583=ORIENTED_EDGE('',*,*,#42639,.T.);
#55584=ORIENTED_EDGE('',*,*,#42640,.T.);
#55585=ORIENTED_EDGE('',*,*,#42641,.F.);
#55586=ORIENTED_EDGE('',*,*,#42642,.T.);
#55587=ORIENTED_EDGE('',*,*,#42643,.F.);
#55588=ORIENTED_EDGE('',*,*,#42644,.T.);
#55589=ORIENTED_EDGE('',*,*,#42645,.T.);
#55590=ORIENTED_EDGE('',*,*,#42644,.F.);
#55591=ORIENTED_EDGE('',*,*,#42646,.F.);
#55592=ORIENTED_EDGE('',*,*,#42647,.T.);
#55593=ORIENTED_EDGE('',*,*,#42648,.F.);
#55594=ORIENTED_EDGE('',*,*,#42649,.F.);
#55595=ORIENTED_EDGE('',*,*,#42650,.T.);
#55596=ORIENTED_EDGE('',*,*,#42651,.T.);
#55597=ORIENTED_EDGE('',*,*,#42650,.F.);
#55598=ORIENTED_EDGE('',*,*,#42652,.F.);
#55599=ORIENTED_EDGE('',*,*,#42653,.T.);
#55600=ORIENTED_EDGE('',*,*,#42654,.F.);
#55601=ORIENTED_EDGE('',*,*,#42647,.F.);
#55602=ORIENTED_EDGE('',*,*,#42651,.F.);
#55603=ORIENTED_EDGE('',*,*,#42655,.F.);
#55604=ORIENTED_EDGE('',*,*,#42656,.T.);
#55605=ORIENTED_EDGE('',*,*,#42648,.T.);
#55606=ORIENTED_EDGE('',*,*,#42654,.T.);
#55607=ORIENTED_EDGE('',*,*,#42657,.F.);
#55608=ORIENTED_EDGE('',*,*,#42655,.T.);
#55609=ORIENTED_EDGE('',*,*,#42653,.F.);
#55610=ORIENTED_EDGE('',*,*,#42658,.F.);
#55611=ORIENTED_EDGE('',*,*,#42657,.T.);
#55612=ORIENTED_EDGE('',*,*,#42659,.T.);
#55613=ORIENTED_EDGE('',*,*,#42660,.T.);
#55614=ORIENTED_EDGE('',*,*,#42661,.T.);
#55615=ORIENTED_EDGE('',*,*,#42662,.T.);
#55616=ORIENTED_EDGE('',*,*,#42663,.T.);
#55617=ORIENTED_EDGE('',*,*,#42659,.F.);
#55618=ORIENTED_EDGE('',*,*,#42664,.F.);
#55619=ORIENTED_EDGE('',*,*,#42665,.T.);
#55620=ORIENTED_EDGE('',*,*,#42666,.T.);
#55621=ORIENTED_EDGE('',*,*,#42660,.F.);
#55622=ORIENTED_EDGE('',*,*,#42663,.F.);
#55623=ORIENTED_EDGE('',*,*,#42667,.T.);
#55624=ORIENTED_EDGE('',*,*,#42668,.T.);
#55625=ORIENTED_EDGE('',*,*,#42661,.F.);
#55626=ORIENTED_EDGE('',*,*,#42666,.F.);
#55627=ORIENTED_EDGE('',*,*,#42669,.F.);
#55628=ORIENTED_EDGE('',*,*,#42664,.T.);
#55629=ORIENTED_EDGE('',*,*,#42662,.F.);
#55630=ORIENTED_EDGE('',*,*,#42668,.F.);
#55631=ORIENTED_EDGE('',*,*,#42670,.T.);
#55632=ORIENTED_EDGE('',*,*,#42671,.F.);
#55633=ORIENTED_EDGE('',*,*,#42672,.T.);
#55634=ORIENTED_EDGE('',*,*,#42673,.T.);
#55635=ORIENTED_EDGE('',*,*,#42674,.T.);
#55636=ORIENTED_EDGE('',*,*,#42673,.F.);
#55637=ORIENTED_EDGE('',*,*,#42675,.T.);
#55638=ORIENTED_EDGE('',*,*,#42676,.T.);
#55639=ORIENTED_EDGE('',*,*,#42677,.T.);
#55640=ORIENTED_EDGE('',*,*,#42676,.F.);
#55641=ORIENTED_EDGE('',*,*,#42678,.T.);
#55642=ORIENTED_EDGE('',*,*,#42679,.T.);
#55643=ORIENTED_EDGE('',*,*,#42680,.T.);
#55644=ORIENTED_EDGE('',*,*,#42679,.F.);
#55645=ORIENTED_EDGE('',*,*,#42681,.T.);
#55646=ORIENTED_EDGE('',*,*,#42682,.T.);
#55647=ORIENTED_EDGE('',*,*,#42683,.T.);
#55648=ORIENTED_EDGE('',*,*,#42682,.F.);
#55649=ORIENTED_EDGE('',*,*,#42684,.T.);
#55650=ORIENTED_EDGE('',*,*,#42685,.T.);
#55651=ORIENTED_EDGE('',*,*,#42686,.T.);
#55652=ORIENTED_EDGE('',*,*,#42687,.T.);
#55653=ORIENTED_EDGE('',*,*,#42686,.F.);
#55654=ORIENTED_EDGE('',*,*,#42688,.F.);
#55655=ORIENTED_EDGE('',*,*,#42689,.T.);
#55656=ORIENTED_EDGE('',*,*,#42690,.T.);
#55657=ORIENTED_EDGE('',*,*,#42683,.F.);
#55658=ORIENTED_EDGE('',*,*,#42687,.F.);
#55659=ORIENTED_EDGE('',*,*,#42691,.T.);
#55660=ORIENTED_EDGE('',*,*,#42692,.T.);
#55661=ORIENTED_EDGE('',*,*,#42680,.F.);
#55662=ORIENTED_EDGE('',*,*,#42690,.F.);
#55663=ORIENTED_EDGE('',*,*,#42693,.T.);
#55664=ORIENTED_EDGE('',*,*,#42694,.T.);
#55665=ORIENTED_EDGE('',*,*,#42677,.F.);
#55666=ORIENTED_EDGE('',*,*,#42692,.F.);
#55667=ORIENTED_EDGE('',*,*,#42695,.T.);
#55668=ORIENTED_EDGE('',*,*,#42696,.T.);
#55669=ORIENTED_EDGE('',*,*,#42674,.F.);
#55670=ORIENTED_EDGE('',*,*,#42694,.F.);
#55671=ORIENTED_EDGE('',*,*,#42697,.T.);
#55672=ORIENTED_EDGE('',*,*,#42698,.T.);
#55673=ORIENTED_EDGE('',*,*,#42699,.F.);
#55674=ORIENTED_EDGE('',*,*,#42696,.F.);
#55675=ORIENTED_EDGE('',*,*,#42700,.T.);
#55676=ORIENTED_EDGE('',*,*,#42701,.F.);
#55677=ORIENTED_EDGE('',*,*,#42702,.T.);
#55678=ORIENTED_EDGE('',*,*,#42671,.T.);
#55679=ORIENTED_EDGE('',*,*,#42699,.T.);
#55680=ORIENTED_EDGE('',*,*,#42701,.T.);
#55681=ORIENTED_EDGE('',*,*,#42703,.T.);
#55682=ORIENTED_EDGE('',*,*,#42704,.T.);
#55683=ORIENTED_EDGE('',*,*,#42705,.T.);
#55684=ORIENTED_EDGE('',*,*,#42698,.F.);
#55685=ORIENTED_EDGE('',*,*,#42706,.T.);
#55686=ORIENTED_EDGE('',*,*,#42707,.T.);
#55687=ORIENTED_EDGE('',*,*,#42703,.F.);
#55688=ORIENTED_EDGE('',*,*,#42707,.F.);
#55689=ORIENTED_EDGE('',*,*,#42642,.F.);
#55690=ORIENTED_EDGE('',*,*,#42708,.T.);
#55691=ORIENTED_EDGE('',*,*,#42704,.F.);
#55692=ORIENTED_EDGE('',*,*,#42708,.F.);
#55693=ORIENTED_EDGE('',*,*,#42709,.T.);
#55694=ORIENTED_EDGE('',*,*,#42710,.T.);
#55695=ORIENTED_EDGE('',*,*,#42711,.F.);
#55696=ORIENTED_EDGE('',*,*,#42643,.T.);
#55697=ORIENTED_EDGE('',*,*,#42712,.T.);
#55698=ORIENTED_EDGE('',*,*,#42713,.F.);
#55699=ORIENTED_EDGE('',*,*,#42712,.F.);
#55700=ORIENTED_EDGE('',*,*,#42646,.T.);
#55701=ORIENTED_EDGE('',*,*,#42711,.T.);
#55702=ORIENTED_EDGE('',*,*,#42714,.F.);
#55703=ORIENTED_EDGE('',*,*,#42715,.T.);
#55704=ORIENTED_EDGE('',*,*,#42636,.T.);
#55705=ORIENTED_EDGE('',*,*,#42716,.T.);
#55706=ORIENTED_EDGE('',*,*,#42717,.T.);
#55707=ORIENTED_EDGE('',*,*,#42718,.T.);
#55708=ORIENTED_EDGE('',*,*,#42719,.T.);
#55709=ORIENTED_EDGE('',*,*,#42715,.F.);
#55710=ORIENTED_EDGE('',*,*,#42720,.T.);
#55711=ORIENTED_EDGE('',*,*,#42713,.T.);
#55712=ORIENTED_EDGE('',*,*,#42714,.T.);
#55713=ORIENTED_EDGE('',*,*,#42709,.F.);
#55714=ORIENTED_EDGE('',*,*,#42641,.T.);
#55715=ORIENTED_EDGE('',*,*,#42718,.F.);
#55716=ORIENTED_EDGE('',*,*,#42721,.T.);
#55717=ORIENTED_EDGE('',*,*,#42637,.T.);
#55718=ORIENTED_EDGE('',*,*,#42719,.F.);
#55719=ORIENTED_EDGE('',*,*,#42640,.F.);
#55720=ORIENTED_EDGE('',*,*,#42722,.T.);
#55721=ORIENTED_EDGE('',*,*,#42635,.F.);
#55722=ORIENTED_EDGE('',*,*,#42723,.F.);
#55723=ORIENTED_EDGE('',*,*,#42724,.T.);
#55724=ORIENTED_EDGE('',*,*,#42723,.T.);
#55725=ORIENTED_EDGE('',*,*,#42725,.T.);
#55726=ORIENTED_EDGE('',*,*,#42726,.T.);
#55727=ORIENTED_EDGE('',*,*,#42727,.F.);
#55728=ORIENTED_EDGE('',*,*,#42688,.T.);
#55729=ORIENTED_EDGE('',*,*,#42728,.F.);
#55730=ORIENTED_EDGE('',*,*,#42726,.F.);
#55731=ORIENTED_EDGE('',*,*,#42729,.T.);
#55732=ORIENTED_EDGE('',*,*,#42685,.F.);
#55733=ORIENTED_EDGE('',*,*,#42730,.T.);
#55734=ORIENTED_EDGE('',*,*,#42731,.T.);
#55735=ORIENTED_EDGE('',*,*,#42728,.T.);
#55736=ORIENTED_EDGE('',*,*,#42732,.F.);
#55737=ORIENTED_EDGE('',*,*,#42727,.T.);
#55738=ORIENTED_EDGE('',*,*,#42731,.F.);
#55739=ORIENTED_EDGE('',*,*,#42733,.T.);
#55740=ORIENTED_EDGE('',*,*,#42716,.F.);
#55741=ORIENTED_EDGE('',*,*,#42724,.F.);
#55742=ORIENTED_EDGE('',*,*,#42732,.T.);
#55743=ORIENTED_EDGE('',*,*,#42734,.T.);
#55744=ORIENTED_EDGE('',*,*,#42735,.T.);
#55745=ORIENTED_EDGE('',*,*,#42710,.F.);
#55746=ORIENTED_EDGE('',*,*,#42721,.F.);
#55747=ORIENTED_EDGE('',*,*,#42720,.F.);
#55748=ORIENTED_EDGE('',*,*,#42717,.F.);
#55749=ORIENTED_EDGE('',*,*,#42734,.F.);
#55750=ORIENTED_EDGE('',*,*,#42733,.F.);
#55751=ORIENTED_EDGE('',*,*,#42730,.F.);
#55752=ORIENTED_EDGE('',*,*,#42684,.F.);
#55753=ORIENTED_EDGE('',*,*,#42681,.F.);
#55754=ORIENTED_EDGE('',*,*,#42678,.F.);
#55755=ORIENTED_EDGE('',*,*,#42675,.F.);
#55756=ORIENTED_EDGE('',*,*,#42672,.F.);
#55757=ORIENTED_EDGE('',*,*,#42702,.F.);
#55758=ORIENTED_EDGE('',*,*,#42705,.F.);
#55759=ORIENTED_EDGE('',*,*,#42735,.F.);
#55760=ORIENTED_EDGE('',*,*,#42736,.F.);
#55761=ORIENTED_EDGE('',*,*,#42737,.F.);
#55762=ORIENTED_EDGE('',*,*,#42738,.F.);
#55763=ORIENTED_EDGE('',*,*,#42739,.F.);
#55764=ORIENTED_EDGE('',*,*,#42740,.F.);
#55765=ORIENTED_EDGE('',*,*,#42741,.F.);
#55766=ORIENTED_EDGE('',*,*,#42742,.F.);
#55767=ORIENTED_EDGE('',*,*,#42743,.F.);
#55768=ORIENTED_EDGE('',*,*,#42744,.F.);
#55769=ORIENTED_EDGE('',*,*,#42736,.T.);
#55770=ORIENTED_EDGE('',*,*,#42745,.T.);
#55771=ORIENTED_EDGE('',*,*,#42746,.T.);
#55772=ORIENTED_EDGE('',*,*,#42747,.F.);
#55773=ORIENTED_EDGE('',*,*,#42737,.T.);
#55774=ORIENTED_EDGE('',*,*,#42744,.T.);
#55775=ORIENTED_EDGE('',*,*,#42748,.T.);
#55776=ORIENTED_EDGE('',*,*,#42749,.F.);
#55777=ORIENTED_EDGE('',*,*,#42738,.T.);
#55778=ORIENTED_EDGE('',*,*,#42747,.T.);
#55779=ORIENTED_EDGE('',*,*,#42750,.T.);
#55780=ORIENTED_EDGE('',*,*,#42751,.F.);
#55781=ORIENTED_EDGE('',*,*,#42739,.T.);
#55782=ORIENTED_EDGE('',*,*,#42749,.T.);
#55783=ORIENTED_EDGE('',*,*,#42752,.T.);
#55784=ORIENTED_EDGE('',*,*,#42753,.F.);
#55785=ORIENTED_EDGE('',*,*,#42740,.T.);
#55786=ORIENTED_EDGE('',*,*,#42751,.T.);
#55787=ORIENTED_EDGE('',*,*,#42754,.T.);
#55788=ORIENTED_EDGE('',*,*,#42645,.F.);
#55789=ORIENTED_EDGE('',*,*,#42755,.F.);
#55790=ORIENTED_EDGE('',*,*,#42741,.T.);
#55791=ORIENTED_EDGE('',*,*,#42753,.T.);
#55792=ORIENTED_EDGE('',*,*,#42756,.T.);
#55793=ORIENTED_EDGE('',*,*,#42757,.F.);
#55794=ORIENTED_EDGE('',*,*,#42742,.T.);
#55795=ORIENTED_EDGE('',*,*,#42755,.T.);
#55796=ORIENTED_EDGE('',*,*,#42758,.T.);
#55797=ORIENTED_EDGE('',*,*,#42745,.F.);
#55798=ORIENTED_EDGE('',*,*,#42743,.T.);
#55799=ORIENTED_EDGE('',*,*,#42757,.T.);
#55800=ORIENTED_EDGE('',*,*,#42759,.T.);
#55801=ORIENTED_EDGE('',*,*,#42632,.T.);
#55802=ORIENTED_EDGE('',*,*,#42697,.F.);
#55803=ORIENTED_EDGE('',*,*,#42695,.F.);
#55804=ORIENTED_EDGE('',*,*,#42693,.F.);
#55805=ORIENTED_EDGE('',*,*,#42691,.F.);
#55806=ORIENTED_EDGE('',*,*,#42689,.F.);
#55807=ORIENTED_EDGE('',*,*,#42729,.F.);
#55808=ORIENTED_EDGE('',*,*,#42725,.F.);
#55809=ORIENTED_EDGE('',*,*,#42634,.F.);
#55810=ORIENTED_EDGE('',*,*,#42633,.F.);
#55811=ORIENTED_EDGE('',*,*,#42722,.F.);
#55812=ORIENTED_EDGE('',*,*,#42639,.F.);
#55813=ORIENTED_EDGE('',*,*,#42638,.F.);
#55814=ORIENTED_EDGE('',*,*,#42706,.F.);
#55815=ORIENTED_EDGE('',*,*,#42700,.F.);
#55816=ORIENTED_EDGE('',*,*,#42758,.F.);
#55817=ORIENTED_EDGE('',*,*,#42756,.F.);
#55818=ORIENTED_EDGE('',*,*,#42754,.F.);
#55819=ORIENTED_EDGE('',*,*,#42752,.F.);
#55820=ORIENTED_EDGE('',*,*,#42750,.F.);
#55821=ORIENTED_EDGE('',*,*,#42748,.F.);
#55822=ORIENTED_EDGE('',*,*,#42746,.F.);
#55823=ORIENTED_EDGE('',*,*,#42759,.F.);
#55824=ORIENTED_EDGE('',*,*,#42626,.T.);
#55825=ORIENTED_EDGE('',*,*,#42619,.T.);
#55826=ORIENTED_EDGE('',*,*,#42630,.F.);
#55827=ORIENTED_EDGE('',*,*,#42760,.T.);
#55828=ORIENTED_EDGE('',*,*,#42605,.F.);
#55829=ORIENTED_EDGE('',*,*,#42607,.F.);
#55830=ORIENTED_EDGE('',*,*,#42761,.T.);
#55831=ORIENTED_EDGE('',*,*,#42628,.F.);
#55832=ORIENTED_EDGE('',*,*,#42606,.F.);
#55833=ORIENTED_EDGE('',*,*,#42760,.F.);
#55834=ORIENTED_EDGE('',*,*,#42629,.T.);
#55835=ORIENTED_EDGE('',*,*,#42761,.F.);
#55836=ORIENTED_EDGE('',*,*,#42762,.T.);
#55837=ORIENTED_EDGE('',*,*,#42763,.T.);
#55838=ORIENTED_EDGE('',*,*,#42764,.F.);
#55839=ORIENTED_EDGE('',*,*,#42616,.F.);
#55840=ORIENTED_EDGE('',*,*,#42615,.F.);
#55841=ORIENTED_EDGE('',*,*,#42765,.F.);
#55842=ORIENTED_EDGE('',*,*,#42763,.F.);
#55843=ORIENTED_EDGE('',*,*,#42766,.F.);
#55844=ORIENTED_EDGE('',*,*,#42767,.F.);
#55845=ORIENTED_EDGE('',*,*,#42768,.F.);
#55846=ORIENTED_EDGE('',*,*,#42769,.F.);
#55847=ORIENTED_EDGE('',*,*,#42764,.T.);
#55848=ORIENTED_EDGE('',*,*,#42765,.T.);
#55849=ORIENTED_EDGE('',*,*,#42770,.F.);
#55850=ORIENTED_EDGE('',*,*,#42771,.F.);
#55851=ORIENTED_EDGE('',*,*,#42772,.T.);
#55852=ORIENTED_EDGE('',*,*,#42773,.F.);
#55853=ORIENTED_EDGE('',*,*,#42774,.F.);
#55854=ORIENTED_EDGE('',*,*,#42600,.T.);
#55855=ORIENTED_EDGE('',*,*,#42617,.T.);
#55856=ORIENTED_EDGE('',*,*,#42771,.T.);
#55857=ORIENTED_EDGE('',*,*,#42775,.F.);
#55858=ORIENTED_EDGE('',*,*,#42773,.T.);
#55859=ORIENTED_EDGE('',*,*,#42776,.T.);
#55860=ORIENTED_EDGE('',*,*,#42777,.F.);
#55861=ORIENTED_EDGE('',*,*,#42778,.F.);
#55862=ORIENTED_EDGE('',*,*,#42610,.T.);
#55863=ORIENTED_EDGE('',*,*,#42779,.T.);
#55864=ORIENTED_EDGE('',*,*,#42780,.T.);
#55865=ORIENTED_EDGE('',*,*,#42614,.F.);
#55866=ORIENTED_EDGE('',*,*,#42777,.T.);
#55867=ORIENTED_EDGE('',*,*,#42781,.T.);
#55868=ORIENTED_EDGE('',*,*,#42766,.T.);
#55869=ORIENTED_EDGE('',*,*,#42762,.F.);
#55870=ORIENTED_EDGE('',*,*,#42780,.F.);
#55871=ORIENTED_EDGE('',*,*,#42782,.T.);
#55872=ORIENTED_EDGE('',*,*,#42767,.T.);
#55873=ORIENTED_EDGE('',*,*,#42781,.F.);
#55874=ORIENTED_EDGE('',*,*,#42783,.F.);
#55875=ORIENTED_EDGE('',*,*,#42784,.T.);
#55876=ORIENTED_EDGE('',*,*,#42768,.T.);
#55877=ORIENTED_EDGE('',*,*,#42782,.F.);
#55878=ORIENTED_EDGE('',*,*,#42785,.F.);
#55879=ORIENTED_EDGE('',*,*,#42770,.T.);
#55880=ORIENTED_EDGE('',*,*,#42769,.T.);
#55881=ORIENTED_EDGE('',*,*,#42784,.F.);
#55882=ORIENTED_EDGE('',*,*,#42786,.F.);
#55883=ORIENTED_EDGE('',*,*,#42787,.T.);
#55884=ORIENTED_EDGE('',*,*,#42775,.T.);
#55885=ORIENTED_EDGE('',*,*,#42786,.T.);
#55886=ORIENTED_EDGE('',*,*,#42788,.F.);
#55887=ORIENTED_EDGE('',*,*,#42789,.T.);
#55888=ORIENTED_EDGE('',*,*,#42790,.T.);
#55889=ORIENTED_EDGE('',*,*,#42774,.T.);
#55890=ORIENTED_EDGE('',*,*,#42787,.F.);
#55891=ORIENTED_EDGE('',*,*,#42791,.F.);
#55892=ORIENTED_EDGE('',*,*,#42601,.T.);
#55893=ORIENTED_EDGE('',*,*,#42792,.T.);
#55894=ORIENTED_EDGE('',*,*,#42612,.F.);
#55895=ORIENTED_EDGE('',*,*,#42772,.F.);
#55896=ORIENTED_EDGE('',*,*,#42599,.T.);
#55897=ORIENTED_EDGE('',*,*,#42778,.T.);
#55898=ORIENTED_EDGE('',*,*,#42613,.F.);
#55899=ORIENTED_EDGE('',*,*,#42792,.F.);
#55900=ORIENTED_EDGE('',*,*,#42611,.T.);
#55901=ORIENTED_EDGE('',*,*,#42793,.T.);
#55902=ORIENTED_EDGE('',*,*,#42794,.F.);
#55903=ORIENTED_EDGE('',*,*,#42776,.F.);
#55904=ORIENTED_EDGE('',*,*,#42609,.T.);
#55905=ORIENTED_EDGE('',*,*,#42795,.T.);
#55906=ORIENTED_EDGE('',*,*,#42796,.T.);
#55907=ORIENTED_EDGE('',*,*,#42797,.T.);
#55908=ORIENTED_EDGE('',*,*,#42783,.T.);
#55909=ORIENTED_EDGE('',*,*,#42779,.F.);
#55910=ORIENTED_EDGE('',*,*,#42794,.T.);
#55911=ORIENTED_EDGE('',*,*,#42788,.T.);
#55912=ORIENTED_EDGE('',*,*,#42785,.T.);
#55913=ORIENTED_EDGE('',*,*,#42797,.F.);
#55914=ORIENTED_EDGE('',*,*,#42798,.T.);
#55915=ORIENTED_EDGE('',*,*,#42799,.T.);
#55916=ORIENTED_EDGE('',*,*,#42798,.F.);
#55917=ORIENTED_EDGE('',*,*,#42800,.F.);
#55918=ORIENTED_EDGE('',*,*,#42801,.T.);
#55919=ORIENTED_EDGE('',*,*,#42802,.T.);
#55920=ORIENTED_EDGE('',*,*,#42789,.F.);
#55921=ORIENTED_EDGE('',*,*,#42799,.F.);
#55922=ORIENTED_EDGE('',*,*,#42803,.T.);
#55923=ORIENTED_EDGE('',*,*,#42791,.T.);
#55924=ORIENTED_EDGE('',*,*,#42790,.F.);
#55925=ORIENTED_EDGE('',*,*,#42802,.F.);
#55926=ORIENTED_EDGE('',*,*,#42595,.T.);
#55927=ORIENTED_EDGE('',*,*,#42804,.T.);
#55928=ORIENTED_EDGE('',*,*,#42795,.F.);
#55929=ORIENTED_EDGE('',*,*,#42793,.F.);
#55930=ORIENTED_EDGE('',*,*,#42597,.T.);
#55931=ORIENTED_EDGE('',*,*,#42800,.T.);
#55932=ORIENTED_EDGE('',*,*,#42796,.F.);
#55933=ORIENTED_EDGE('',*,*,#42804,.F.);
#55934=ORIENTED_EDGE('',*,*,#42805,.T.);
#55935=ORIENTED_EDGE('',*,*,#42596,.T.);
#55936=ORIENTED_EDGE('',*,*,#42803,.F.);
#55937=ORIENTED_EDGE('',*,*,#42801,.F.);
#55938=ORIENTED_EDGE('',*,*,#42805,.F.);
#55939=ORIENTED_EDGE('',*,*,#42652,.T.);
#55940=ORIENTED_EDGE('',*,*,#42649,.T.);
#55941=ORIENTED_EDGE('',*,*,#42656,.F.);
#55942=ORIENTED_EDGE('',*,*,#42658,.T.);
#55943=ORIENTED_EDGE('',*,*,#42669,.T.);
#55944=ORIENTED_EDGE('',*,*,#42667,.F.);
#55945=ORIENTED_EDGE('',*,*,#42665,.F.);
#55946=ORIENTED_EDGE('',*,*,#42670,.F.);
#55947=ORIENTED_EDGE('',*,*,#42806,.F.);
#55948=ORIENTED_EDGE('',*,*,#42807,.F.);
#55949=ORIENTED_EDGE('',*,*,#42808,.F.);
#55950=ORIENTED_EDGE('',*,*,#42809,.F.);
#55951=ORIENTED_EDGE('',*,*,#42810,.F.);
#55952=ORIENTED_EDGE('',*,*,#42811,.F.);
#55953=ORIENTED_EDGE('',*,*,#42806,.T.);
#55954=ORIENTED_EDGE('',*,*,#42812,.F.);
#55955=ORIENTED_EDGE('',*,*,#42810,.T.);
#55956=ORIENTED_EDGE('',*,*,#42813,.F.);
#55957=ORIENTED_EDGE('',*,*,#42814,.F.);
#55958=ORIENTED_EDGE('',*,*,#42815,.F.);
#55959=ORIENTED_EDGE('',*,*,#42816,.F.);
#55960=ORIENTED_EDGE('',*,*,#42817,.F.);
#55961=ORIENTED_EDGE('',*,*,#42814,.T.);
#55962=ORIENTED_EDGE('',*,*,#42818,.F.);
#55963=ORIENTED_EDGE('',*,*,#42819,.F.);
#55964=ORIENTED_EDGE('',*,*,#42820,.F.);
#55965=ORIENTED_EDGE('',*,*,#42816,.T.);
#55966=ORIENTED_EDGE('',*,*,#42821,.F.);
#55967=ORIENTED_EDGE('',*,*,#42822,.F.);
#55968=ORIENTED_EDGE('',*,*,#42823,.F.);
#55969=ORIENTED_EDGE('',*,*,#42824,.F.);
#55970=ORIENTED_EDGE('',*,*,#42819,.T.);
#55971=ORIENTED_EDGE('',*,*,#42825,.F.);
#55972=ORIENTED_EDGE('',*,*,#42826,.F.);
#55973=ORIENTED_EDGE('',*,*,#42827,.F.);
#55974=ORIENTED_EDGE('',*,*,#42828,.F.);
#55975=ORIENTED_EDGE('',*,*,#42823,.T.);
#55976=ORIENTED_EDGE('',*,*,#42829,.F.);
#55977=ORIENTED_EDGE('',*,*,#42830,.F.);
#55978=ORIENTED_EDGE('',*,*,#42831,.F.);
#55979=ORIENTED_EDGE('',*,*,#42832,.F.);
#55980=ORIENTED_EDGE('',*,*,#42833,.F.);
#55981=ORIENTED_EDGE('',*,*,#42834,.F.);
#55982=ORIENTED_EDGE('',*,*,#42835,.F.);
#55983=ORIENTED_EDGE('',*,*,#42830,.T.);
#55984=ORIENTED_EDGE('',*,*,#42836,.F.);
#55985=ORIENTED_EDGE('',*,*,#42837,.F.);
#55986=ORIENTED_EDGE('',*,*,#42838,.F.);
#55987=ORIENTED_EDGE('',*,*,#42834,.T.);
#55988=ORIENTED_EDGE('',*,*,#42839,.F.);
#55989=ORIENTED_EDGE('',*,*,#42840,.F.);
#55990=ORIENTED_EDGE('',*,*,#42841,.F.);
#55991=ORIENTED_EDGE('',*,*,#42842,.F.);
#55992=ORIENTED_EDGE('',*,*,#42837,.T.);
#55993=ORIENTED_EDGE('',*,*,#42843,.F.);
#55994=ORIENTED_EDGE('',*,*,#42844,.F.);
#55995=ORIENTED_EDGE('',*,*,#42845,.F.);
#55996=ORIENTED_EDGE('',*,*,#42846,.F.);
#55997=ORIENTED_EDGE('',*,*,#42840,.T.);
#55998=ORIENTED_EDGE('',*,*,#42847,.F.);
#55999=ORIENTED_EDGE('',*,*,#42848,.F.);
#56000=ORIENTED_EDGE('',*,*,#42849,.F.);
#56001=ORIENTED_EDGE('',*,*,#42845,.T.);
#56002=ORIENTED_EDGE('',*,*,#42850,.F.);
#56003=ORIENTED_EDGE('',*,*,#42851,.F.);
#56004=ORIENTED_EDGE('',*,*,#42852,.F.);
#56005=ORIENTED_EDGE('',*,*,#42848,.T.);
#56006=ORIENTED_EDGE('',*,*,#42853,.F.);
#56007=ORIENTED_EDGE('',*,*,#42854,.F.);
#56008=ORIENTED_EDGE('',*,*,#42855,.F.);
#56009=ORIENTED_EDGE('',*,*,#42856,.F.);
#56010=ORIENTED_EDGE('',*,*,#42857,.F.);
#56011=ORIENTED_EDGE('',*,*,#42858,.F.);
#56012=ORIENTED_EDGE('',*,*,#42859,.T.);
#56013=ORIENTED_EDGE('',*,*,#42860,.F.);
#56014=ORIENTED_EDGE('',*,*,#42861,.F.);
#56015=ORIENTED_EDGE('',*,*,#42862,.F.);
#56016=ORIENTED_EDGE('',*,*,#42857,.T.);
#56017=ORIENTED_EDGE('',*,*,#42863,.F.);
#56018=ORIENTED_EDGE('',*,*,#42864,.F.);
#56019=ORIENTED_EDGE('',*,*,#42865,.F.);
#56020=ORIENTED_EDGE('',*,*,#42861,.T.);
#56021=ORIENTED_EDGE('',*,*,#42866,.F.);
#56022=ORIENTED_EDGE('',*,*,#42867,.F.);
#56023=ORIENTED_EDGE('',*,*,#42868,.F.);
#56024=ORIENTED_EDGE('',*,*,#42864,.T.);
#56025=ORIENTED_EDGE('',*,*,#42869,.F.);
#56026=ORIENTED_EDGE('',*,*,#42870,.F.);
#56027=ORIENTED_EDGE('',*,*,#42871,.F.);
#56028=ORIENTED_EDGE('',*,*,#42867,.T.);
#56029=ORIENTED_EDGE('',*,*,#42872,.F.);
#56030=ORIENTED_EDGE('',*,*,#42873,.F.);
#56031=ORIENTED_EDGE('',*,*,#42874,.F.);
#56032=ORIENTED_EDGE('',*,*,#42875,.T.);
#56033=ORIENTED_EDGE('',*,*,#42876,.F.);
#56034=ORIENTED_EDGE('',*,*,#42877,.F.);
#56035=ORIENTED_EDGE('',*,*,#42878,.F.);
#56036=ORIENTED_EDGE('',*,*,#42873,.T.);
#56037=ORIENTED_EDGE('',*,*,#42879,.F.);
#56038=ORIENTED_EDGE('',*,*,#42880,.F.);
#56039=ORIENTED_EDGE('',*,*,#42881,.F.);
#56040=ORIENTED_EDGE('',*,*,#42877,.T.);
#56041=ORIENTED_EDGE('',*,*,#42882,.F.);
#56042=ORIENTED_EDGE('',*,*,#42883,.F.);
#56043=ORIENTED_EDGE('',*,*,#42884,.F.);
#56044=ORIENTED_EDGE('',*,*,#42880,.T.);
#56045=ORIENTED_EDGE('',*,*,#42885,.F.);
#56046=ORIENTED_EDGE('',*,*,#42886,.F.);
#56047=ORIENTED_EDGE('',*,*,#42887,.F.);
#56048=ORIENTED_EDGE('',*,*,#42888,.F.);
#56049=ORIENTED_EDGE('',*,*,#42883,.T.);
#56050=ORIENTED_EDGE('',*,*,#42889,.F.);
#56051=ORIENTED_EDGE('',*,*,#42890,.F.);
#56052=ORIENTED_EDGE('',*,*,#42887,.T.);
#56053=ORIENTED_EDGE('',*,*,#42891,.F.);
#56054=ORIENTED_EDGE('',*,*,#42892,.T.);
#56055=ORIENTED_EDGE('',*,*,#42893,.T.);
#56056=ORIENTED_EDGE('',*,*,#42894,.T.);
#56057=ORIENTED_EDGE('',*,*,#42895,.T.);
#56058=ORIENTED_EDGE('',*,*,#42896,.F.);
#56059=ORIENTED_EDGE('',*,*,#42895,.F.);
#56060=ORIENTED_EDGE('',*,*,#42897,.T.);
#56061=ORIENTED_EDGE('',*,*,#42898,.T.);
#56062=ORIENTED_EDGE('',*,*,#42899,.T.);
#56063=ORIENTED_EDGE('',*,*,#42889,.T.);
#56064=ORIENTED_EDGE('',*,*,#42900,.F.);
#56065=ORIENTED_EDGE('',*,*,#42901,.T.);
#56066=ORIENTED_EDGE('',*,*,#42902,.F.);
#56067=ORIENTED_EDGE('',*,*,#42903,.F.);
#56068=ORIENTED_EDGE('',*,*,#42904,.T.);
#56069=ORIENTED_EDGE('',*,*,#42905,.T.);
#56070=ORIENTED_EDGE('',*,*,#42906,.T.);
#56071=ORIENTED_EDGE('',*,*,#42904,.F.);
#56072=ORIENTED_EDGE('',*,*,#42907,.F.);
#56073=ORIENTED_EDGE('',*,*,#42908,.T.);
#56074=ORIENTED_EDGE('',*,*,#42909,.T.);
#56075=ORIENTED_EDGE('',*,*,#42908,.F.);
#56076=ORIENTED_EDGE('',*,*,#42910,.F.);
#56077=ORIENTED_EDGE('',*,*,#42911,.T.);
#56078=ORIENTED_EDGE('',*,*,#42912,.T.);
#56079=ORIENTED_EDGE('',*,*,#42911,.F.);
#56080=ORIENTED_EDGE('',*,*,#42870,.T.);
#56081=ORIENTED_EDGE('',*,*,#42913,.F.);
#56082=ORIENTED_EDGE('',*,*,#42914,.T.);
#56083=ORIENTED_EDGE('',*,*,#42915,.F.);
#56084=ORIENTED_EDGE('',*,*,#42827,.T.);
#56085=ORIENTED_EDGE('',*,*,#42916,.T.);
#56086=ORIENTED_EDGE('',*,*,#42917,.F.);
#56087=ORIENTED_EDGE('',*,*,#42901,.F.);
#56088=ORIENTED_EDGE('',*,*,#42918,.F.);
#56089=ORIENTED_EDGE('',*,*,#42919,.T.);
#56090=ORIENTED_EDGE('',*,*,#42905,.F.);
#56091=ORIENTED_EDGE('',*,*,#42906,.F.);
#56092=ORIENTED_EDGE('',*,*,#42919,.F.);
#56093=ORIENTED_EDGE('',*,*,#42920,.F.);
#56094=ORIENTED_EDGE('',*,*,#42921,.F.);
#56095=ORIENTED_EDGE('',*,*,#42922,.T.);
#56096=ORIENTED_EDGE('',*,*,#42923,.F.);
#56097=ORIENTED_EDGE('',*,*,#42859,.F.);
#56098=ORIENTED_EDGE('',*,*,#42924,.F.);
#56099=ORIENTED_EDGE('',*,*,#42925,.T.);
#56100=ORIENTED_EDGE('',*,*,#42910,.T.);
#56101=ORIENTED_EDGE('',*,*,#42925,.F.);
#56102=ORIENTED_EDGE('',*,*,#42926,.T.);
#56103=ORIENTED_EDGE('',*,*,#42927,.T.);
#56104=ORIENTED_EDGE('',*,*,#42928,.T.);
#56105=ORIENTED_EDGE('',*,*,#42927,.F.);
#56106=ORIENTED_EDGE('',*,*,#42929,.T.);
#56107=ORIENTED_EDGE('',*,*,#42930,.T.);
#56108=ORIENTED_EDGE('',*,*,#42931,.T.);
#56109=ORIENTED_EDGE('',*,*,#42932,.T.);
#56110=ORIENTED_EDGE('',*,*,#42931,.F.);
#56111=ORIENTED_EDGE('',*,*,#42933,.F.);
#56112=ORIENTED_EDGE('',*,*,#42934,.T.);
#56113=ORIENTED_EDGE('',*,*,#42930,.F.);
#56114=ORIENTED_EDGE('',*,*,#42934,.F.);
#56115=ORIENTED_EDGE('',*,*,#42926,.F.);
#56116=ORIENTED_EDGE('',*,*,#42935,.T.);
#56117=ORIENTED_EDGE('',*,*,#42936,.F.);
#56118=ORIENTED_EDGE('',*,*,#42935,.F.);
#56119=ORIENTED_EDGE('',*,*,#42929,.F.);
#56120=ORIENTED_EDGE('',*,*,#42937,.F.);
#56121=ORIENTED_EDGE('',*,*,#42938,.T.);
#56122=ORIENTED_EDGE('',*,*,#42939,.F.);
#56123=ORIENTED_EDGE('',*,*,#42940,.F.);
#56124=ORIENTED_EDGE('',*,*,#42854,.T.);
#56125=ORIENTED_EDGE('',*,*,#42941,.F.);
#56126=ORIENTED_EDGE('',*,*,#42942,.F.);
#56127=ORIENTED_EDGE('',*,*,#42914,.F.);
#56128=ORIENTED_EDGE('',*,*,#42943,.F.);
#56129=ORIENTED_EDGE('',*,*,#42944,.F.);
#56130=ORIENTED_EDGE('',*,*,#42808,.T.);
#56131=ORIENTED_EDGE('',*,*,#42945,.F.);
#56132=ORIENTED_EDGE('',*,*,#42875,.F.);
#56133=ORIENTED_EDGE('',*,*,#42946,.F.);
#56134=ORIENTED_EDGE('',*,*,#42947,.T.);
#56135=ORIENTED_EDGE('',*,*,#42948,.F.);
#56136=ORIENTED_EDGE('',*,*,#42947,.F.);
#56137=ORIENTED_EDGE('',*,*,#42851,.T.);
#56138=ORIENTED_EDGE('',*,*,#42949,.F.);
#56139=ORIENTED_EDGE('',*,*,#42922,.F.);
#56140=ORIENTED_EDGE('',*,*,#42950,.F.);
#56141=ORIENTED_EDGE('',*,*,#42826,.T.);
#56142=ORIENTED_EDGE('',*,*,#42951,.F.);
#56143=ORIENTED_EDGE('',*,*,#42916,.F.);
#56144=ORIENTED_EDGE('',*,*,#42885,.T.);
#56145=ORIENTED_EDGE('',*,*,#42882,.T.);
#56146=ORIENTED_EDGE('',*,*,#42879,.T.);
#56147=ORIENTED_EDGE('',*,*,#42876,.T.);
#56148=ORIENTED_EDGE('',*,*,#42945,.T.);
#56149=ORIENTED_EDGE('',*,*,#42807,.T.);
#56150=ORIENTED_EDGE('',*,*,#42811,.T.);
#56151=ORIENTED_EDGE('',*,*,#42815,.T.);
#56152=ORIENTED_EDGE('',*,*,#42817,.T.);
#56153=ORIENTED_EDGE('',*,*,#42820,.T.);
#56154=ORIENTED_EDGE('',*,*,#42824,.T.);
#56155=ORIENTED_EDGE('',*,*,#42828,.T.);
#56156=ORIENTED_EDGE('',*,*,#42920,.T.);
#56157=ORIENTED_EDGE('',*,*,#42918,.T.);
#56158=ORIENTED_EDGE('',*,*,#42900,.T.);
#56159=ORIENTED_EDGE('',*,*,#42891,.T.);
#56160=ORIENTED_EDGE('',*,*,#42886,.T.);
#56161=ORIENTED_EDGE('',*,*,#42917,.T.);
#56162=ORIENTED_EDGE('',*,*,#42951,.T.);
#56163=ORIENTED_EDGE('',*,*,#42829,.T.);
#56164=ORIENTED_EDGE('',*,*,#42825,.T.);
#56165=ORIENTED_EDGE('',*,*,#42822,.T.);
#56166=ORIENTED_EDGE('',*,*,#42821,.T.);
#56167=ORIENTED_EDGE('',*,*,#42818,.T.);
#56168=ORIENTED_EDGE('',*,*,#42813,.T.);
#56169=ORIENTED_EDGE('',*,*,#42812,.T.);
#56170=ORIENTED_EDGE('',*,*,#42809,.T.);
#56171=ORIENTED_EDGE('',*,*,#42944,.T.);
#56172=ORIENTED_EDGE('',*,*,#42946,.T.);
#56173=ORIENTED_EDGE('',*,*,#42874,.T.);
#56174=ORIENTED_EDGE('',*,*,#42878,.T.);
#56175=ORIENTED_EDGE('',*,*,#42881,.T.);
#56176=ORIENTED_EDGE('',*,*,#42884,.T.);
#56177=ORIENTED_EDGE('',*,*,#42888,.T.);
#56178=ORIENTED_EDGE('',*,*,#42890,.T.);
#56179=ORIENTED_EDGE('',*,*,#42902,.T.);
#56180=ORIENTED_EDGE('',*,*,#42921,.T.);
#56181=ORIENTED_EDGE('',*,*,#42924,.T.);
#56182=ORIENTED_EDGE('',*,*,#42858,.T.);
#56183=ORIENTED_EDGE('',*,*,#42862,.T.);
#56184=ORIENTED_EDGE('',*,*,#42865,.T.);
#56185=ORIENTED_EDGE('',*,*,#42868,.T.);
#56186=ORIENTED_EDGE('',*,*,#42871,.T.);
#56187=ORIENTED_EDGE('',*,*,#42915,.T.);
#56188=ORIENTED_EDGE('',*,*,#42942,.T.);
#56189=ORIENTED_EDGE('',*,*,#42831,.T.);
#56190=ORIENTED_EDGE('',*,*,#42835,.T.);
#56191=ORIENTED_EDGE('',*,*,#42838,.T.);
#56192=ORIENTED_EDGE('',*,*,#42842,.T.);
#56193=ORIENTED_EDGE('',*,*,#42841,.T.);
#56194=ORIENTED_EDGE('',*,*,#42846,.T.);
#56195=ORIENTED_EDGE('',*,*,#42849,.T.);
#56196=ORIENTED_EDGE('',*,*,#42852,.T.);
#56197=ORIENTED_EDGE('',*,*,#42950,.T.);
#56198=ORIENTED_EDGE('',*,*,#42923,.T.);
#56199=ORIENTED_EDGE('',*,*,#42949,.T.);
#56200=ORIENTED_EDGE('',*,*,#42853,.T.);
#56201=ORIENTED_EDGE('',*,*,#42850,.T.);
#56202=ORIENTED_EDGE('',*,*,#42847,.T.);
#56203=ORIENTED_EDGE('',*,*,#42844,.T.);
#56204=ORIENTED_EDGE('',*,*,#42843,.T.);
#56205=ORIENTED_EDGE('',*,*,#42839,.T.);
#56206=ORIENTED_EDGE('',*,*,#42836,.T.);
#56207=ORIENTED_EDGE('',*,*,#42833,.T.);
#56208=ORIENTED_EDGE('',*,*,#42855,.T.);
#56209=ORIENTED_EDGE('',*,*,#42943,.T.);
#56210=ORIENTED_EDGE('',*,*,#42913,.T.);
#56211=ORIENTED_EDGE('',*,*,#42872,.T.);
#56212=ORIENTED_EDGE('',*,*,#42869,.T.);
#56213=ORIENTED_EDGE('',*,*,#42866,.T.);
#56214=ORIENTED_EDGE('',*,*,#42863,.T.);
#56215=ORIENTED_EDGE('',*,*,#42860,.T.);
#56216=ORIENTED_EDGE('',*,*,#42938,.F.);
#56217=ORIENTED_EDGE('',*,*,#42952,.F.);
#56218=ORIENTED_EDGE('',*,*,#42953,.T.);
#56219=ORIENTED_EDGE('',*,*,#42954,.F.);
#56220=ORIENTED_EDGE('',*,*,#42953,.F.);
#56221=ORIENTED_EDGE('',*,*,#42955,.F.);
#56222=ORIENTED_EDGE('',*,*,#42956,.T.);
#56223=ORIENTED_EDGE('',*,*,#42957,.F.);
#56224=ORIENTED_EDGE('',*,*,#42956,.F.);
#56225=ORIENTED_EDGE('',*,*,#42958,.F.);
#56226=ORIENTED_EDGE('',*,*,#42959,.T.);
#56227=ORIENTED_EDGE('',*,*,#42960,.F.);
#56228=ORIENTED_EDGE('',*,*,#42959,.F.);
#56229=ORIENTED_EDGE('',*,*,#42961,.F.);
#56230=ORIENTED_EDGE('',*,*,#42962,.T.);
#56231=ORIENTED_EDGE('',*,*,#42963,.F.);
#56232=ORIENTED_EDGE('',*,*,#42962,.F.);
#56233=ORIENTED_EDGE('',*,*,#42964,.F.);
#56234=ORIENTED_EDGE('',*,*,#42965,.T.);
#56235=ORIENTED_EDGE('',*,*,#42966,.F.);
#56236=ORIENTED_EDGE('',*,*,#42965,.F.);
#56237=ORIENTED_EDGE('',*,*,#42967,.F.);
#56238=ORIENTED_EDGE('',*,*,#42968,.T.);
#56239=ORIENTED_EDGE('',*,*,#42969,.F.);
#56240=ORIENTED_EDGE('',*,*,#42968,.F.);
#56241=ORIENTED_EDGE('',*,*,#42970,.F.);
#56242=ORIENTED_EDGE('',*,*,#42940,.T.);
#56243=ORIENTED_EDGE('',*,*,#42971,.F.);
#56244=ORIENTED_EDGE('',*,*,#42932,.F.);
#56245=ORIENTED_EDGE('',*,*,#42937,.T.);
#56246=ORIENTED_EDGE('',*,*,#42970,.T.);
#56247=ORIENTED_EDGE('',*,*,#42967,.T.);
#56248=ORIENTED_EDGE('',*,*,#42964,.T.);
#56249=ORIENTED_EDGE('',*,*,#42961,.T.);
#56250=ORIENTED_EDGE('',*,*,#42958,.T.);
#56251=ORIENTED_EDGE('',*,*,#42955,.T.);
#56252=ORIENTED_EDGE('',*,*,#42952,.T.);
#56253=ORIENTED_EDGE('',*,*,#42928,.F.);
#56254=ORIENTED_EDGE('',*,*,#42933,.T.);
#56255=ORIENTED_EDGE('',*,*,#42972,.F.);
#56256=ORIENTED_EDGE('',*,*,#42973,.F.);
#56257=ORIENTED_EDGE('',*,*,#42974,.F.);
#56258=ORIENTED_EDGE('',*,*,#42975,.F.);
#56259=ORIENTED_EDGE('',*,*,#42976,.F.);
#56260=ORIENTED_EDGE('',*,*,#42977,.F.);
#56261=ORIENTED_EDGE('',*,*,#42969,.T.);
#56262=ORIENTED_EDGE('',*,*,#42971,.T.);
#56263=ORIENTED_EDGE('',*,*,#42939,.T.);
#56264=ORIENTED_EDGE('',*,*,#42954,.T.);
#56265=ORIENTED_EDGE('',*,*,#42957,.T.);
#56266=ORIENTED_EDGE('',*,*,#42960,.T.);
#56267=ORIENTED_EDGE('',*,*,#42963,.T.);
#56268=ORIENTED_EDGE('',*,*,#42966,.T.);
#56269=ORIENTED_EDGE('',*,*,#42975,.T.);
#56270=ORIENTED_EDGE('',*,*,#42978,.T.);
#56271=ORIENTED_EDGE('',*,*,#42894,.F.);
#56272=ORIENTED_EDGE('',*,*,#42979,.F.);
#56273=ORIENTED_EDGE('',*,*,#42976,.T.);
#56274=ORIENTED_EDGE('',*,*,#42979,.T.);
#56275=ORIENTED_EDGE('',*,*,#42893,.F.);
#56276=ORIENTED_EDGE('',*,*,#42980,.F.);
#56277=ORIENTED_EDGE('',*,*,#42977,.T.);
#56278=ORIENTED_EDGE('',*,*,#42980,.T.);
#56279=ORIENTED_EDGE('',*,*,#42892,.F.);
#56280=ORIENTED_EDGE('',*,*,#42981,.F.);
#56281=ORIENTED_EDGE('',*,*,#42972,.T.);
#56282=ORIENTED_EDGE('',*,*,#42981,.T.);
#56283=ORIENTED_EDGE('',*,*,#42899,.F.);
#56284=ORIENTED_EDGE('',*,*,#42982,.F.);
#56285=ORIENTED_EDGE('',*,*,#42973,.T.);
#56286=ORIENTED_EDGE('',*,*,#42982,.T.);
#56287=ORIENTED_EDGE('',*,*,#42898,.F.);
#56288=ORIENTED_EDGE('',*,*,#42983,.F.);
#56289=ORIENTED_EDGE('',*,*,#42978,.F.);
#56290=ORIENTED_EDGE('',*,*,#42974,.T.);
#56291=ORIENTED_EDGE('',*,*,#42983,.T.);
#56292=ORIENTED_EDGE('',*,*,#42897,.F.);
#56293=ORIENTED_EDGE('',*,*,#42832,.T.);
#56294=ORIENTED_EDGE('',*,*,#42941,.T.);
#56295=ORIENTED_EDGE('',*,*,#42856,.T.);
#56296=ORIENTED_EDGE('',*,*,#42936,.T.);
#56297=ORIENTED_EDGE('',*,*,#42909,.F.);
#56298=ORIENTED_EDGE('',*,*,#42903,.T.);
#56299=ORIENTED_EDGE('',*,*,#42907,.T.);
#56300=ORIENTED_EDGE('',*,*,#42912,.F.);
#56301=ORIENTED_EDGE('',*,*,#42948,.T.);
#56302=ORIENTED_EDGE('',*,*,#42896,.T.);
#56303=ORIENTED_EDGE('',*,*,#42984,.F.);
#56304=ORIENTED_EDGE('',*,*,#42985,.T.);
#56305=ORIENTED_EDGE('',*,*,#42986,.T.);
#56306=ORIENTED_EDGE('',*,*,#42985,.F.);
#56307=ORIENTED_EDGE('',*,*,#42987,.F.);
#56308=ORIENTED_EDGE('',*,*,#42988,.T.);
#56309=ORIENTED_EDGE('',*,*,#42989,.T.);
#56310=ORIENTED_EDGE('',*,*,#42988,.F.);
#56311=ORIENTED_EDGE('',*,*,#42990,.F.);
#56312=ORIENTED_EDGE('',*,*,#42991,.T.);
#56313=ORIENTED_EDGE('',*,*,#42992,.T.);
#56314=ORIENTED_EDGE('',*,*,#42993,.F.);
#56315=ORIENTED_EDGE('',*,*,#42994,.T.);
#56316=ORIENTED_EDGE('',*,*,#42995,.F.);
#56317=ORIENTED_EDGE('',*,*,#42996,.T.);
#56318=ORIENTED_EDGE('',*,*,#42997,.F.);
#56319=ORIENTED_EDGE('',*,*,#42998,.T.);
#56320=ORIENTED_EDGE('',*,*,#42999,.F.);
#56321=ORIENTED_EDGE('',*,*,#43000,.T.);
#56322=ORIENTED_EDGE('',*,*,#43001,.F.);
#56323=ORIENTED_EDGE('',*,*,#43002,.T.);
#56324=ORIENTED_EDGE('',*,*,#43003,.F.);
#56325=ORIENTED_EDGE('',*,*,#43004,.T.);
#56326=ORIENTED_EDGE('',*,*,#42991,.F.);
#56327=ORIENTED_EDGE('',*,*,#43005,.F.);
#56328=ORIENTED_EDGE('',*,*,#43006,.T.);
#56329=ORIENTED_EDGE('',*,*,#43007,.T.);
#56330=ORIENTED_EDGE('',*,*,#43006,.F.);
#56331=ORIENTED_EDGE('',*,*,#43008,.F.);
#56332=ORIENTED_EDGE('',*,*,#43009,.T.);
#56333=ORIENTED_EDGE('',*,*,#43010,.T.);
#56334=ORIENTED_EDGE('',*,*,#43009,.F.);
#56335=ORIENTED_EDGE('',*,*,#43011,.F.);
#56336=ORIENTED_EDGE('',*,*,#43012,.T.);
#56337=ORIENTED_EDGE('',*,*,#43013,.T.);
#56338=ORIENTED_EDGE('',*,*,#43012,.F.);
#56339=ORIENTED_EDGE('',*,*,#43014,.T.);
#56340=ORIENTED_EDGE('',*,*,#43001,.T.);
#56341=ORIENTED_EDGE('',*,*,#43015,.F.);
#56342=ORIENTED_EDGE('',*,*,#43003,.T.);
#56343=ORIENTED_EDGE('',*,*,#43016,.T.);
#56344=ORIENTED_EDGE('',*,*,#42993,.T.);
#56345=ORIENTED_EDGE('',*,*,#43017,.F.);
#56346=ORIENTED_EDGE('',*,*,#42995,.T.);
#56347=ORIENTED_EDGE('',*,*,#42994,.F.);
#56348=ORIENTED_EDGE('',*,*,#43016,.F.);
#56349=ORIENTED_EDGE('',*,*,#42998,.F.);
#56350=ORIENTED_EDGE('',*,*,#43018,.F.);
#56351=ORIENTED_EDGE('',*,*,#43019,.F.);
#56352=ORIENTED_EDGE('',*,*,#42999,.T.);
#56353=ORIENTED_EDGE('',*,*,#43018,.T.);
#56354=ORIENTED_EDGE('',*,*,#42997,.T.);
#56355=ORIENTED_EDGE('',*,*,#43002,.F.);
#56356=ORIENTED_EDGE('',*,*,#43014,.F.);
#56357=ORIENTED_EDGE('',*,*,#42984,.T.);
#56358=ORIENTED_EDGE('',*,*,#43013,.F.);
#56359=ORIENTED_EDGE('',*,*,#43010,.F.);
#56360=ORIENTED_EDGE('',*,*,#43011,.T.);
#56361=ORIENTED_EDGE('',*,*,#43007,.F.);
#56362=ORIENTED_EDGE('',*,*,#43008,.T.);
#56363=ORIENTED_EDGE('',*,*,#42996,.F.);
#56364=ORIENTED_EDGE('',*,*,#43017,.T.);
#56365=ORIENTED_EDGE('',*,*,#42992,.F.);
#56366=ORIENTED_EDGE('',*,*,#43004,.F.);
#56367=ORIENTED_EDGE('',*,*,#43015,.T.);
#56368=ORIENTED_EDGE('',*,*,#43000,.F.);
#56369=ORIENTED_EDGE('',*,*,#43019,.T.);
#56370=ORIENTED_EDGE('',*,*,#43005,.T.);
#56371=ORIENTED_EDGE('',*,*,#42990,.T.);
#56372=ORIENTED_EDGE('',*,*,#42989,.F.);
#56373=ORIENTED_EDGE('',*,*,#42987,.T.);
#56374=ORIENTED_EDGE('',*,*,#42986,.F.);
#56375=ORIENTED_EDGE('',*,*,#43020,.T.);
#56376=ORIENTED_EDGE('',*,*,#43021,.F.);
#56377=ORIENTED_EDGE('',*,*,#43022,.F.);
#56378=ORIENTED_EDGE('',*,*,#43023,.F.);
#56379=ORIENTED_EDGE('',*,*,#43024,.T.);
#56380=ORIENTED_EDGE('',*,*,#43025,.T.);
#56381=ORIENTED_EDGE('',*,*,#43026,.F.);
#56382=ORIENTED_EDGE('',*,*,#43020,.F.);
#56383=ORIENTED_EDGE('',*,*,#43027,.T.);
#56384=ORIENTED_EDGE('',*,*,#43028,.F.);
#56385=ORIENTED_EDGE('',*,*,#43029,.T.);
#56386=ORIENTED_EDGE('',*,*,#43030,.T.);
#56387=ORIENTED_EDGE('',*,*,#43031,.F.);
#56388=ORIENTED_EDGE('',*,*,#43032,.T.);
#56389=ORIENTED_EDGE('',*,*,#43033,.T.);
#56390=ORIENTED_EDGE('',*,*,#43034,.T.);
#56391=ORIENTED_EDGE('',*,*,#43035,.T.);
#56392=ORIENTED_EDGE('',*,*,#43036,.T.);
#56393=ORIENTED_EDGE('',*,*,#43037,.T.);
#56394=ORIENTED_EDGE('',*,*,#43038,.T.);
#56395=ORIENTED_EDGE('',*,*,#43039,.T.);
#56396=ORIENTED_EDGE('',*,*,#43040,.T.);
#56397=ORIENTED_EDGE('',*,*,#43041,.F.);
#56398=ORIENTED_EDGE('',*,*,#43040,.F.);
#56399=ORIENTED_EDGE('',*,*,#43042,.T.);
#56400=ORIENTED_EDGE('',*,*,#43043,.T.);
#56401=ORIENTED_EDGE('',*,*,#43044,.T.);
#56402=ORIENTED_EDGE('',*,*,#43032,.F.);
#56403=ORIENTED_EDGE('',*,*,#43045,.T.);
#56404=ORIENTED_EDGE('',*,*,#43046,.T.);
#56405=ORIENTED_EDGE('',*,*,#43047,.T.);
#56406=ORIENTED_EDGE('',*,*,#43043,.F.);
#56407=ORIENTED_EDGE('',*,*,#43048,.T.);
#56408=ORIENTED_EDGE('',*,*,#43049,.T.);
#56409=ORIENTED_EDGE('',*,*,#43050,.T.);
#56410=ORIENTED_EDGE('',*,*,#43051,.F.);
#56411=ORIENTED_EDGE('',*,*,#43052,.T.);
#56412=ORIENTED_EDGE('',*,*,#43046,.F.);
#56413=ORIENTED_EDGE('',*,*,#43053,.T.);
#56414=ORIENTED_EDGE('',*,*,#43054,.F.);
#56415=ORIENTED_EDGE('',*,*,#43055,.T.);
#56416=ORIENTED_EDGE('',*,*,#43056,.F.);
#56417=ORIENTED_EDGE('',*,*,#43057,.T.);
#56418=ORIENTED_EDGE('',*,*,#43058,.T.);
#56419=ORIENTED_EDGE('',*,*,#43059,.T.);
#56420=ORIENTED_EDGE('',*,*,#43058,.F.);
#56421=ORIENTED_EDGE('',*,*,#43054,.T.);
#56422=ORIENTED_EDGE('',*,*,#43060,.F.);
#56423=ORIENTED_EDGE('',*,*,#43050,.F.);
#56424=ORIENTED_EDGE('',*,*,#43061,.T.);
#56425=ORIENTED_EDGE('',*,*,#43062,.T.);
#56426=ORIENTED_EDGE('',*,*,#43063,.T.);
#56427=ORIENTED_EDGE('',*,*,#43028,.T.);
#56428=ORIENTED_EDGE('',*,*,#43064,.F.);
#56429=ORIENTED_EDGE('',*,*,#43025,.F.);
#56430=ORIENTED_EDGE('',*,*,#43065,.T.);
#56431=ORIENTED_EDGE('',*,*,#43066,.T.);
#56432=ORIENTED_EDGE('',*,*,#43067,.T.);
#56433=ORIENTED_EDGE('',*,*,#43068,.F.);
#56434=ORIENTED_EDGE('',*,*,#43067,.F.);
#56435=ORIENTED_EDGE('',*,*,#43069,.T.);
#56436=ORIENTED_EDGE('',*,*,#43055,.F.);
#56437=ORIENTED_EDGE('',*,*,#43063,.F.);
#56438=ORIENTED_EDGE('',*,*,#43070,.F.);
#56439=ORIENTED_EDGE('',*,*,#43071,.T.);
#56440=ORIENTED_EDGE('',*,*,#43072,.T.);
#56441=ORIENTED_EDGE('',*,*,#43073,.F.);
#56442=ORIENTED_EDGE('',*,*,#43074,.T.);
#56443=ORIENTED_EDGE('',*,*,#43075,.F.);
#56444=ORIENTED_EDGE('',*,*,#43076,.T.);
#56445=ORIENTED_EDGE('',*,*,#43077,.F.);
#56446=ORIENTED_EDGE('',*,*,#43078,.T.);
#56447=ORIENTED_EDGE('',*,*,#43079,.F.);
#56448=ORIENTED_EDGE('',*,*,#43080,.F.);
#56449=ORIENTED_EDGE('',*,*,#43081,.F.);
#56450=ORIENTED_EDGE('',*,*,#43082,.F.);
#56451=ORIENTED_EDGE('',*,*,#43083,.T.);
#56452=ORIENTED_EDGE('',*,*,#43084,.T.);
#56453=ORIENTED_EDGE('',*,*,#43083,.F.);
#56454=ORIENTED_EDGE('',*,*,#43085,.F.);
#56455=ORIENTED_EDGE('',*,*,#43086,.F.);
#56456=ORIENTED_EDGE('',*,*,#43087,.F.);
#56457=ORIENTED_EDGE('',*,*,#43088,.T.);
#56458=ORIENTED_EDGE('',*,*,#43089,.T.);
#56459=ORIENTED_EDGE('',*,*,#43090,.T.);
#56460=ORIENTED_EDGE('',*,*,#43091,.T.);
#56461=ORIENTED_EDGE('',*,*,#43092,.T.);
#56462=ORIENTED_EDGE('',*,*,#43093,.T.);
#56463=ORIENTED_EDGE('',*,*,#43094,.T.);
#56464=ORIENTED_EDGE('',*,*,#43095,.F.);
#56465=ORIENTED_EDGE('',*,*,#43096,.T.);
#56466=ORIENTED_EDGE('',*,*,#43097,.F.);
#56467=ORIENTED_EDGE('',*,*,#43098,.T.);
#56468=ORIENTED_EDGE('',*,*,#43099,.F.);
#56469=ORIENTED_EDGE('',*,*,#43098,.F.);
#56470=ORIENTED_EDGE('',*,*,#43100,.F.);
#56471=ORIENTED_EDGE('',*,*,#43101,.T.);
#56472=ORIENTED_EDGE('',*,*,#43102,.F.);
#56473=ORIENTED_EDGE('',*,*,#43076,.F.);
#56474=ORIENTED_EDGE('',*,*,#43103,.T.);
#56475=ORIENTED_EDGE('',*,*,#43100,.T.);
#56476=ORIENTED_EDGE('',*,*,#43097,.T.);
#56477=ORIENTED_EDGE('',*,*,#43104,.F.);
#56478=ORIENTED_EDGE('',*,*,#43086,.T.);
#56479=ORIENTED_EDGE('',*,*,#43105,.T.);
#56480=ORIENTED_EDGE('',*,*,#43090,.F.);
#56481=ORIENTED_EDGE('',*,*,#43106,.F.);
#56482=ORIENTED_EDGE('',*,*,#43077,.T.);
#56483=ORIENTED_EDGE('',*,*,#43104,.T.);
#56484=ORIENTED_EDGE('',*,*,#43096,.F.);
#56485=ORIENTED_EDGE('',*,*,#43107,.F.);
#56486=ORIENTED_EDGE('',*,*,#43075,.T.);
#56487=ORIENTED_EDGE('',*,*,#43108,.T.);
#56488=ORIENTED_EDGE('',*,*,#43101,.F.);
#56489=ORIENTED_EDGE('',*,*,#43103,.F.);
#56490=ORIENTED_EDGE('',*,*,#43095,.T.);
#56491=ORIENTED_EDGE('',*,*,#43109,.F.);
#56492=ORIENTED_EDGE('',*,*,#43078,.F.);
#56493=ORIENTED_EDGE('',*,*,#43107,.T.);
#56494=ORIENTED_EDGE('',*,*,#43102,.T.);
#56495=ORIENTED_EDGE('',*,*,#43108,.F.);
#56496=ORIENTED_EDGE('',*,*,#43074,.F.);
#56497=ORIENTED_EDGE('',*,*,#43110,.T.);
#56498=ORIENTED_EDGE('',*,*,#43088,.F.);
#56499=ORIENTED_EDGE('',*,*,#43110,.F.);
#56500=ORIENTED_EDGE('',*,*,#43073,.T.);
#56501=ORIENTED_EDGE('',*,*,#43111,.T.);
#56502=ORIENTED_EDGE('',*,*,#43081,.T.);
#56503=ORIENTED_EDGE('',*,*,#43112,.T.);
#56504=ORIENTED_EDGE('',*,*,#43092,.F.);
#56505=ORIENTED_EDGE('',*,*,#43113,.F.);
#56506=ORIENTED_EDGE('',*,*,#43089,.F.);
#56507=ORIENTED_EDGE('',*,*,#43111,.F.);
#56508=ORIENTED_EDGE('',*,*,#43087,.T.);
#56509=ORIENTED_EDGE('',*,*,#43106,.T.);
#56510=ORIENTED_EDGE('',*,*,#43080,.T.);
#56511=ORIENTED_EDGE('',*,*,#43114,.T.);
#56512=ORIENTED_EDGE('',*,*,#43093,.F.);
#56513=ORIENTED_EDGE('',*,*,#43112,.F.);
#56514=ORIENTED_EDGE('',*,*,#43091,.F.);
#56515=ORIENTED_EDGE('',*,*,#43105,.F.);
#56516=ORIENTED_EDGE('',*,*,#43085,.T.);
#56517=ORIENTED_EDGE('',*,*,#43082,.T.);
#56518=ORIENTED_EDGE('',*,*,#43113,.T.);
#56519=ORIENTED_EDGE('',*,*,#43079,.T.);
#56520=ORIENTED_EDGE('',*,*,#43109,.T.);
#56521=ORIENTED_EDGE('',*,*,#43094,.F.);
#56522=ORIENTED_EDGE('',*,*,#43114,.F.);
#56523=ORIENTED_EDGE('',*,*,#43084,.F.);
#56524=ORIENTED_EDGE('',*,*,#43068,.T.);
#56525=ORIENTED_EDGE('',*,*,#43066,.F.);
#56526=ORIENTED_EDGE('',*,*,#43115,.T.);
#56527=ORIENTED_EDGE('',*,*,#43116,.T.);
#56528=ORIENTED_EDGE('',*,*,#43051,.T.);
#56529=ORIENTED_EDGE('',*,*,#43060,.T.);
#56530=ORIENTED_EDGE('',*,*,#43056,.T.);
#56531=ORIENTED_EDGE('',*,*,#43069,.F.);
#56532=ORIENTED_EDGE('',*,*,#43117,.T.);
#56533=ORIENTED_EDGE('',*,*,#43023,.T.);
#56534=ORIENTED_EDGE('',*,*,#43115,.F.);
#56535=ORIENTED_EDGE('',*,*,#43072,.F.);
#56536=ORIENTED_EDGE('',*,*,#43071,.F.);
#56537=ORIENTED_EDGE('',*,*,#43039,.F.);
#56538=ORIENTED_EDGE('',*,*,#43038,.F.);
#56539=ORIENTED_EDGE('',*,*,#43118,.T.);
#56540=ORIENTED_EDGE('',*,*,#43029,.F.);
#56541=ORIENTED_EDGE('',*,*,#43065,.F.);
#56542=ORIENTED_EDGE('',*,*,#43027,.F.);
#56543=ORIENTED_EDGE('',*,*,#43024,.F.);
#56544=ORIENTED_EDGE('',*,*,#43119,.F.);
#56545=ORIENTED_EDGE('',*,*,#43048,.F.);
#56546=ORIENTED_EDGE('',*,*,#43045,.F.);
#56547=ORIENTED_EDGE('',*,*,#43042,.F.);
#56548=ORIENTED_EDGE('',*,*,#43120,.F.);
#56549=ORIENTED_EDGE('',*,*,#43118,.F.);
#56550=ORIENTED_EDGE('',*,*,#43037,.F.);
#56551=ORIENTED_EDGE('',*,*,#43121,.F.);
#56552=ORIENTED_EDGE('',*,*,#43030,.F.);
#56553=ORIENTED_EDGE('',*,*,#43120,.T.);
#56554=ORIENTED_EDGE('',*,*,#43036,.F.);
#56555=ORIENTED_EDGE('',*,*,#43035,.F.);
#56556=ORIENTED_EDGE('',*,*,#43122,.F.);
#56557=ORIENTED_EDGE('',*,*,#43121,.T.);
#56558=ORIENTED_EDGE('',*,*,#43052,.F.);
#56559=ORIENTED_EDGE('',*,*,#43116,.F.);
#56560=ORIENTED_EDGE('',*,*,#43022,.T.);
#56561=ORIENTED_EDGE('',*,*,#43021,.T.);
#56562=ORIENTED_EDGE('',*,*,#43026,.T.);
#56563=ORIENTED_EDGE('',*,*,#43064,.T.);
#56564=ORIENTED_EDGE('',*,*,#43031,.T.);
#56565=ORIENTED_EDGE('',*,*,#43122,.T.);
#56566=ORIENTED_EDGE('',*,*,#43034,.F.);
#56567=ORIENTED_EDGE('',*,*,#43033,.F.);
#56568=ORIENTED_EDGE('',*,*,#43044,.F.);
#56569=ORIENTED_EDGE('',*,*,#43047,.F.);
#56570=ORIENTED_EDGE('',*,*,#43049,.F.);
#56571=ORIENTED_EDGE('',*,*,#43119,.T.);
#56572=ORIENTED_EDGE('',*,*,#43117,.F.);
#56573=ORIENTED_EDGE('',*,*,#43070,.T.);
#56574=ORIENTED_EDGE('',*,*,#43062,.F.);
#56575=ORIENTED_EDGE('',*,*,#43061,.F.);
#56576=ORIENTED_EDGE('',*,*,#43053,.F.);
#56577=ORIENTED_EDGE('',*,*,#43041,.T.);
#56578=ORIENTED_EDGE('',*,*,#43057,.F.);
#56579=ORIENTED_EDGE('',*,*,#43099,.T.);
#56580=ORIENTED_EDGE('',*,*,#43059,.F.);
#56581=ORIENTED_EDGE('',*,*,#43123,.F.);
#56582=ORIENTED_EDGE('',*,*,#43124,.T.);
#56583=ORIENTED_EDGE('',*,*,#43125,.T.);
#56584=ORIENTED_EDGE('',*,*,#43124,.F.);
#56585=ORIENTED_EDGE('',*,*,#43126,.F.);
#56586=ORIENTED_EDGE('',*,*,#43127,.T.);
#56587=ORIENTED_EDGE('',*,*,#43128,.T.);
#56588=ORIENTED_EDGE('',*,*,#43127,.F.);
#56589=ORIENTED_EDGE('',*,*,#43129,.F.);
#56590=ORIENTED_EDGE('',*,*,#43130,.T.);
#56591=ORIENTED_EDGE('',*,*,#43131,.T.);
#56592=ORIENTED_EDGE('',*,*,#43132,.F.);
#56593=ORIENTED_EDGE('',*,*,#43133,.T.);
#56594=ORIENTED_EDGE('',*,*,#43134,.F.);
#56595=ORIENTED_EDGE('',*,*,#43135,.T.);
#56596=ORIENTED_EDGE('',*,*,#43136,.F.);
#56597=ORIENTED_EDGE('',*,*,#43137,.T.);
#56598=ORIENTED_EDGE('',*,*,#43138,.F.);
#56599=ORIENTED_EDGE('',*,*,#43139,.T.);
#56600=ORIENTED_EDGE('',*,*,#43140,.F.);
#56601=ORIENTED_EDGE('',*,*,#43141,.T.);
#56602=ORIENTED_EDGE('',*,*,#43142,.F.);
#56603=ORIENTED_EDGE('',*,*,#43143,.T.);
#56604=ORIENTED_EDGE('',*,*,#43130,.F.);
#56605=ORIENTED_EDGE('',*,*,#43144,.F.);
#56606=ORIENTED_EDGE('',*,*,#43145,.T.);
#56607=ORIENTED_EDGE('',*,*,#43146,.T.);
#56608=ORIENTED_EDGE('',*,*,#43145,.F.);
#56609=ORIENTED_EDGE('',*,*,#43147,.F.);
#56610=ORIENTED_EDGE('',*,*,#43148,.T.);
#56611=ORIENTED_EDGE('',*,*,#43149,.T.);
#56612=ORIENTED_EDGE('',*,*,#43148,.F.);
#56613=ORIENTED_EDGE('',*,*,#43150,.F.);
#56614=ORIENTED_EDGE('',*,*,#43151,.T.);
#56615=ORIENTED_EDGE('',*,*,#43152,.T.);
#56616=ORIENTED_EDGE('',*,*,#43151,.F.);
#56617=ORIENTED_EDGE('',*,*,#43153,.T.);
#56618=ORIENTED_EDGE('',*,*,#43140,.T.);
#56619=ORIENTED_EDGE('',*,*,#43154,.F.);
#56620=ORIENTED_EDGE('',*,*,#43142,.T.);
#56621=ORIENTED_EDGE('',*,*,#43155,.T.);
#56622=ORIENTED_EDGE('',*,*,#43132,.T.);
#56623=ORIENTED_EDGE('',*,*,#43156,.F.);
#56624=ORIENTED_EDGE('',*,*,#43134,.T.);
#56625=ORIENTED_EDGE('',*,*,#43133,.F.);
#56626=ORIENTED_EDGE('',*,*,#43155,.F.);
#56627=ORIENTED_EDGE('',*,*,#43137,.F.);
#56628=ORIENTED_EDGE('',*,*,#43157,.F.);
#56629=ORIENTED_EDGE('',*,*,#43158,.F.);
#56630=ORIENTED_EDGE('',*,*,#43138,.T.);
#56631=ORIENTED_EDGE('',*,*,#43157,.T.);
#56632=ORIENTED_EDGE('',*,*,#43136,.T.);
#56633=ORIENTED_EDGE('',*,*,#43141,.F.);
#56634=ORIENTED_EDGE('',*,*,#43153,.F.);
#56635=ORIENTED_EDGE('',*,*,#43123,.T.);
#56636=ORIENTED_EDGE('',*,*,#43152,.F.);
#56637=ORIENTED_EDGE('',*,*,#43149,.F.);
#56638=ORIENTED_EDGE('',*,*,#43150,.T.);
#56639=ORIENTED_EDGE('',*,*,#43146,.F.);
#56640=ORIENTED_EDGE('',*,*,#43147,.T.);
#56641=ORIENTED_EDGE('',*,*,#43135,.F.);
#56642=ORIENTED_EDGE('',*,*,#43156,.T.);
#56643=ORIENTED_EDGE('',*,*,#43131,.F.);
#56644=ORIENTED_EDGE('',*,*,#43143,.F.);
#56645=ORIENTED_EDGE('',*,*,#43154,.T.);
#56646=ORIENTED_EDGE('',*,*,#43139,.F.);
#56647=ORIENTED_EDGE('',*,*,#43158,.T.);
#56648=ORIENTED_EDGE('',*,*,#43144,.T.);
#56649=ORIENTED_EDGE('',*,*,#43129,.T.);
#56650=ORIENTED_EDGE('',*,*,#43128,.F.);
#56651=ORIENTED_EDGE('',*,*,#43126,.T.);
#56652=ORIENTED_EDGE('',*,*,#43125,.F.);
#56653=ORIENTED_EDGE('',*,*,#43159,.F.);
#56654=ORIENTED_EDGE('',*,*,#43160,.T.);
#56655=ORIENTED_EDGE('',*,*,#43161,.T.);
#56656=ORIENTED_EDGE('',*,*,#43160,.F.);
#56657=ORIENTED_EDGE('',*,*,#43161,.F.);
#56658=ORIENTED_EDGE('',*,*,#43162,.T.);
#56659=ORIENTED_EDGE('',*,*,#43163,.T.);
#56660=ORIENTED_EDGE('',*,*,#43162,.F.);
#56661=ORIENTED_EDGE('',*,*,#43164,.F.);
#56662=ORIENTED_EDGE('',*,*,#43165,.F.);
#56663=ORIENTED_EDGE('',*,*,#43166,.T.);
#56664=ORIENTED_EDGE('',*,*,#43167,.T.);
#56665=ORIENTED_EDGE('',*,*,#43168,.F.);
#56666=ORIENTED_EDGE('',*,*,#43167,.F.);
#56667=ORIENTED_EDGE('',*,*,#43169,.T.);
#56668=ORIENTED_EDGE('',*,*,#43165,.T.);
#56669=ORIENTED_EDGE('',*,*,#43170,.F.);
#56670=ORIENTED_EDGE('',*,*,#43171,.T.);
#56671=ORIENTED_EDGE('',*,*,#43172,.T.);
#56672=ORIENTED_EDGE('',*,*,#43171,.F.);
#56673=ORIENTED_EDGE('',*,*,#43173,.F.);
#56674=ORIENTED_EDGE('',*,*,#43174,.T.);
#56675=ORIENTED_EDGE('',*,*,#43170,.T.);
#56676=ORIENTED_EDGE('',*,*,#43174,.F.);
#56677=ORIENTED_EDGE('',*,*,#43175,.F.);
#56678=ORIENTED_EDGE('',*,*,#43176,.T.);
#56679=ORIENTED_EDGE('',*,*,#43177,.T.);
#56680=ORIENTED_EDGE('',*,*,#43176,.F.);
#56681=ORIENTED_EDGE('',*,*,#43172,.F.);
#56682=ORIENTED_EDGE('',*,*,#43175,.T.);
#56683=ORIENTED_EDGE('',*,*,#43177,.F.);
#56684=ORIENTED_EDGE('',*,*,#43169,.F.);
#56685=ORIENTED_EDGE('',*,*,#43166,.F.);
#56686=ORIENTED_EDGE('',*,*,#43178,.T.);
#56687=ORIENTED_EDGE('',*,*,#43168,.T.);
#56688=ORIENTED_EDGE('',*,*,#43164,.T.);
#56689=ORIENTED_EDGE('',*,*,#43178,.F.);
#56690=ORIENTED_EDGE('',*,*,#43179,.T.);
#56691=ORIENTED_EDGE('',*,*,#43180,.T.);
#56692=ORIENTED_EDGE('',*,*,#43179,.F.);
#56693=ORIENTED_EDGE('',*,*,#43159,.T.);
#56694=ORIENTED_EDGE('',*,*,#43180,.F.);
#56695=ORIENTED_EDGE('',*,*,#43163,.F.);
#56696=ORIENTED_EDGE('',*,*,#43173,.T.);
#56697=ORIENTED_EDGE('',*,*,#43181,.T.);
#56698=ORIENTED_EDGE('',*,*,#43182,.F.);
#56699=ORIENTED_EDGE('',*,*,#43183,.F.);
#56700=ORIENTED_EDGE('',*,*,#43184,.F.);
#56701=ORIENTED_EDGE('',*,*,#43185,.T.);
#56702=ORIENTED_EDGE('',*,*,#43186,.T.);
#56703=ORIENTED_EDGE('',*,*,#43187,.F.);
#56704=ORIENTED_EDGE('',*,*,#43181,.F.);
#56705=ORIENTED_EDGE('',*,*,#43188,.T.);
#56706=ORIENTED_EDGE('',*,*,#43189,.F.);
#56707=ORIENTED_EDGE('',*,*,#43190,.T.);
#56708=ORIENTED_EDGE('',*,*,#43191,.T.);
#56709=ORIENTED_EDGE('',*,*,#43192,.F.);
#56710=ORIENTED_EDGE('',*,*,#43193,.T.);
#56711=ORIENTED_EDGE('',*,*,#43194,.T.);
#56712=ORIENTED_EDGE('',*,*,#43195,.T.);
#56713=ORIENTED_EDGE('',*,*,#43196,.T.);
#56714=ORIENTED_EDGE('',*,*,#43197,.T.);
#56715=ORIENTED_EDGE('',*,*,#43198,.T.);
#56716=ORIENTED_EDGE('',*,*,#43199,.T.);
#56717=ORIENTED_EDGE('',*,*,#43200,.T.);
#56718=ORIENTED_EDGE('',*,*,#43201,.T.);
#56719=ORIENTED_EDGE('',*,*,#43202,.F.);
#56720=ORIENTED_EDGE('',*,*,#43201,.F.);
#56721=ORIENTED_EDGE('',*,*,#43203,.T.);
#56722=ORIENTED_EDGE('',*,*,#43204,.T.);
#56723=ORIENTED_EDGE('',*,*,#43205,.T.);
#56724=ORIENTED_EDGE('',*,*,#43193,.F.);
#56725=ORIENTED_EDGE('',*,*,#43206,.T.);
#56726=ORIENTED_EDGE('',*,*,#43207,.T.);
#56727=ORIENTED_EDGE('',*,*,#43208,.T.);
#56728=ORIENTED_EDGE('',*,*,#43204,.F.);
#56729=ORIENTED_EDGE('',*,*,#43209,.T.);
#56730=ORIENTED_EDGE('',*,*,#43210,.T.);
#56731=ORIENTED_EDGE('',*,*,#43211,.T.);
#56732=ORIENTED_EDGE('',*,*,#43212,.F.);
#56733=ORIENTED_EDGE('',*,*,#43213,.T.);
#56734=ORIENTED_EDGE('',*,*,#43207,.F.);
#56735=ORIENTED_EDGE('',*,*,#43214,.T.);
#56736=ORIENTED_EDGE('',*,*,#43215,.F.);
#56737=ORIENTED_EDGE('',*,*,#43216,.T.);
#56738=ORIENTED_EDGE('',*,*,#43217,.F.);
#56739=ORIENTED_EDGE('',*,*,#43218,.T.);
#56740=ORIENTED_EDGE('',*,*,#43219,.T.);
#56741=ORIENTED_EDGE('',*,*,#43220,.T.);
#56742=ORIENTED_EDGE('',*,*,#43219,.F.);
#56743=ORIENTED_EDGE('',*,*,#43215,.T.);
#56744=ORIENTED_EDGE('',*,*,#43221,.F.);
#56745=ORIENTED_EDGE('',*,*,#43211,.F.);
#56746=ORIENTED_EDGE('',*,*,#43222,.T.);
#56747=ORIENTED_EDGE('',*,*,#43223,.T.);
#56748=ORIENTED_EDGE('',*,*,#43224,.T.);
#56749=ORIENTED_EDGE('',*,*,#43189,.T.);
#56750=ORIENTED_EDGE('',*,*,#43225,.F.);
#56751=ORIENTED_EDGE('',*,*,#43186,.F.);
#56752=ORIENTED_EDGE('',*,*,#43226,.T.);
#56753=ORIENTED_EDGE('',*,*,#43227,.T.);
#56754=ORIENTED_EDGE('',*,*,#43228,.T.);
#56755=ORIENTED_EDGE('',*,*,#43229,.F.);
#56756=ORIENTED_EDGE('',*,*,#43228,.F.);
#56757=ORIENTED_EDGE('',*,*,#43230,.T.);
#56758=ORIENTED_EDGE('',*,*,#43216,.F.);
#56759=ORIENTED_EDGE('',*,*,#43224,.F.);
#56760=ORIENTED_EDGE('',*,*,#43231,.F.);
#56761=ORIENTED_EDGE('',*,*,#43232,.T.);
#56762=ORIENTED_EDGE('',*,*,#43233,.T.);
#56763=ORIENTED_EDGE('',*,*,#43234,.F.);
#56764=ORIENTED_EDGE('',*,*,#43235,.T.);
#56765=ORIENTED_EDGE('',*,*,#43236,.F.);
#56766=ORIENTED_EDGE('',*,*,#43237,.T.);
#56767=ORIENTED_EDGE('',*,*,#43238,.F.);
#56768=ORIENTED_EDGE('',*,*,#43239,.T.);
#56769=ORIENTED_EDGE('',*,*,#43240,.F.);
#56770=ORIENTED_EDGE('',*,*,#43241,.F.);
#56771=ORIENTED_EDGE('',*,*,#43242,.F.);
#56772=ORIENTED_EDGE('',*,*,#43243,.F.);
#56773=ORIENTED_EDGE('',*,*,#43244,.T.);
#56774=ORIENTED_EDGE('',*,*,#43245,.T.);
#56775=ORIENTED_EDGE('',*,*,#43244,.F.);
#56776=ORIENTED_EDGE('',*,*,#43246,.F.);
#56777=ORIENTED_EDGE('',*,*,#43247,.F.);
#56778=ORIENTED_EDGE('',*,*,#43248,.F.);
#56779=ORIENTED_EDGE('',*,*,#43249,.T.);
#56780=ORIENTED_EDGE('',*,*,#43250,.T.);
#56781=ORIENTED_EDGE('',*,*,#43251,.T.);
#56782=ORIENTED_EDGE('',*,*,#43252,.T.);
#56783=ORIENTED_EDGE('',*,*,#43253,.T.);
#56784=ORIENTED_EDGE('',*,*,#43254,.T.);
#56785=ORIENTED_EDGE('',*,*,#43255,.T.);
#56786=ORIENTED_EDGE('',*,*,#43256,.F.);
#56787=ORIENTED_EDGE('',*,*,#43257,.T.);
#56788=ORIENTED_EDGE('',*,*,#43258,.F.);
#56789=ORIENTED_EDGE('',*,*,#43259,.T.);
#56790=ORIENTED_EDGE('',*,*,#43260,.F.);
#56791=ORIENTED_EDGE('',*,*,#43259,.F.);
#56792=ORIENTED_EDGE('',*,*,#43261,.F.);
#56793=ORIENTED_EDGE('',*,*,#43262,.T.);
#56794=ORIENTED_EDGE('',*,*,#43263,.F.);
#56795=ORIENTED_EDGE('',*,*,#43237,.F.);
#56796=ORIENTED_EDGE('',*,*,#43264,.T.);
#56797=ORIENTED_EDGE('',*,*,#43261,.T.);
#56798=ORIENTED_EDGE('',*,*,#43258,.T.);
#56799=ORIENTED_EDGE('',*,*,#43265,.F.);
#56800=ORIENTED_EDGE('',*,*,#43247,.T.);
#56801=ORIENTED_EDGE('',*,*,#43266,.T.);
#56802=ORIENTED_EDGE('',*,*,#43251,.F.);
#56803=ORIENTED_EDGE('',*,*,#43267,.F.);
#56804=ORIENTED_EDGE('',*,*,#43238,.T.);
#56805=ORIENTED_EDGE('',*,*,#43265,.T.);
#56806=ORIENTED_EDGE('',*,*,#43257,.F.);
#56807=ORIENTED_EDGE('',*,*,#43268,.F.);
#56808=ORIENTED_EDGE('',*,*,#43236,.T.);
#56809=ORIENTED_EDGE('',*,*,#43269,.T.);
#56810=ORIENTED_EDGE('',*,*,#43262,.F.);
#56811=ORIENTED_EDGE('',*,*,#43264,.F.);
#56812=ORIENTED_EDGE('',*,*,#43256,.T.);
#56813=ORIENTED_EDGE('',*,*,#43270,.F.);
#56814=ORIENTED_EDGE('',*,*,#43239,.F.);
#56815=ORIENTED_EDGE('',*,*,#43268,.T.);
#56816=ORIENTED_EDGE('',*,*,#43263,.T.);
#56817=ORIENTED_EDGE('',*,*,#43269,.F.);
#56818=ORIENTED_EDGE('',*,*,#43235,.F.);
#56819=ORIENTED_EDGE('',*,*,#43271,.T.);
#56820=ORIENTED_EDGE('',*,*,#43249,.F.);
#56821=ORIENTED_EDGE('',*,*,#43271,.F.);
#56822=ORIENTED_EDGE('',*,*,#43234,.T.);
#56823=ORIENTED_EDGE('',*,*,#43272,.T.);
#56824=ORIENTED_EDGE('',*,*,#43242,.T.);
#56825=ORIENTED_EDGE('',*,*,#43273,.T.);
#56826=ORIENTED_EDGE('',*,*,#43253,.F.);
#56827=ORIENTED_EDGE('',*,*,#43274,.F.);
#56828=ORIENTED_EDGE('',*,*,#43250,.F.);
#56829=ORIENTED_EDGE('',*,*,#43272,.F.);
#56830=ORIENTED_EDGE('',*,*,#43248,.T.);
#56831=ORIENTED_EDGE('',*,*,#43267,.T.);
#56832=ORIENTED_EDGE('',*,*,#43241,.T.);
#56833=ORIENTED_EDGE('',*,*,#43275,.T.);
#56834=ORIENTED_EDGE('',*,*,#43254,.F.);
#56835=ORIENTED_EDGE('',*,*,#43273,.F.);
#56836=ORIENTED_EDGE('',*,*,#43252,.F.);
#56837=ORIENTED_EDGE('',*,*,#43266,.F.);
#56838=ORIENTED_EDGE('',*,*,#43246,.T.);
#56839=ORIENTED_EDGE('',*,*,#43243,.T.);
#56840=ORIENTED_EDGE('',*,*,#43274,.T.);
#56841=ORIENTED_EDGE('',*,*,#43240,.T.);
#56842=ORIENTED_EDGE('',*,*,#43270,.T.);
#56843=ORIENTED_EDGE('',*,*,#43255,.F.);
#56844=ORIENTED_EDGE('',*,*,#43275,.F.);
#56845=ORIENTED_EDGE('',*,*,#43245,.F.);
#56846=ORIENTED_EDGE('',*,*,#43229,.T.);
#56847=ORIENTED_EDGE('',*,*,#43227,.F.);
#56848=ORIENTED_EDGE('',*,*,#43276,.T.);
#56849=ORIENTED_EDGE('',*,*,#43277,.T.);
#56850=ORIENTED_EDGE('',*,*,#43212,.T.);
#56851=ORIENTED_EDGE('',*,*,#43221,.T.);
#56852=ORIENTED_EDGE('',*,*,#43217,.T.);
#56853=ORIENTED_EDGE('',*,*,#43230,.F.);
#56854=ORIENTED_EDGE('',*,*,#43278,.T.);
#56855=ORIENTED_EDGE('',*,*,#43184,.T.);
#56856=ORIENTED_EDGE('',*,*,#43276,.F.);
#56857=ORIENTED_EDGE('',*,*,#43233,.F.);
#56858=ORIENTED_EDGE('',*,*,#43232,.F.);
#56859=ORIENTED_EDGE('',*,*,#43200,.F.);
#56860=ORIENTED_EDGE('',*,*,#43199,.F.);
#56861=ORIENTED_EDGE('',*,*,#43279,.T.);
#56862=ORIENTED_EDGE('',*,*,#43190,.F.);
#56863=ORIENTED_EDGE('',*,*,#43226,.F.);
#56864=ORIENTED_EDGE('',*,*,#43188,.F.);
#56865=ORIENTED_EDGE('',*,*,#43185,.F.);
#56866=ORIENTED_EDGE('',*,*,#43280,.F.);
#56867=ORIENTED_EDGE('',*,*,#43209,.F.);
#56868=ORIENTED_EDGE('',*,*,#43206,.F.);
#56869=ORIENTED_EDGE('',*,*,#43203,.F.);
#56870=ORIENTED_EDGE('',*,*,#43281,.F.);
#56871=ORIENTED_EDGE('',*,*,#43279,.F.);
#56872=ORIENTED_EDGE('',*,*,#43198,.F.);
#56873=ORIENTED_EDGE('',*,*,#43282,.F.);
#56874=ORIENTED_EDGE('',*,*,#43191,.F.);
#56875=ORIENTED_EDGE('',*,*,#43281,.T.);
#56876=ORIENTED_EDGE('',*,*,#43197,.F.);
#56877=ORIENTED_EDGE('',*,*,#43196,.F.);
#56878=ORIENTED_EDGE('',*,*,#43283,.F.);
#56879=ORIENTED_EDGE('',*,*,#43282,.T.);
#56880=ORIENTED_EDGE('',*,*,#43213,.F.);
#56881=ORIENTED_EDGE('',*,*,#43277,.F.);
#56882=ORIENTED_EDGE('',*,*,#43183,.T.);
#56883=ORIENTED_EDGE('',*,*,#43182,.T.);
#56884=ORIENTED_EDGE('',*,*,#43187,.T.);
#56885=ORIENTED_EDGE('',*,*,#43225,.T.);
#56886=ORIENTED_EDGE('',*,*,#43192,.T.);
#56887=ORIENTED_EDGE('',*,*,#43283,.T.);
#56888=ORIENTED_EDGE('',*,*,#43195,.F.);
#56889=ORIENTED_EDGE('',*,*,#43194,.F.);
#56890=ORIENTED_EDGE('',*,*,#43205,.F.);
#56891=ORIENTED_EDGE('',*,*,#43208,.F.);
#56892=ORIENTED_EDGE('',*,*,#43210,.F.);
#56893=ORIENTED_EDGE('',*,*,#43280,.T.);
#56894=ORIENTED_EDGE('',*,*,#43278,.F.);
#56895=ORIENTED_EDGE('',*,*,#43231,.T.);
#56896=ORIENTED_EDGE('',*,*,#43223,.F.);
#56897=ORIENTED_EDGE('',*,*,#43222,.F.);
#56898=ORIENTED_EDGE('',*,*,#43214,.F.);
#56899=ORIENTED_EDGE('',*,*,#43202,.T.);
#56900=ORIENTED_EDGE('',*,*,#43218,.F.);
#56901=ORIENTED_EDGE('',*,*,#43260,.T.);
#56902=ORIENTED_EDGE('',*,*,#43220,.F.);
#56903=ORIENTED_EDGE('',*,*,#43284,.T.);
#56904=ORIENTED_EDGE('',*,*,#43285,.T.);
#56905=ORIENTED_EDGE('',*,*,#43286,.T.);
#56906=ORIENTED_EDGE('',*,*,#43287,.T.);
#56907=ORIENTED_EDGE('',*,*,#43285,.F.);
#56908=ORIENTED_EDGE('',*,*,#43288,.T.);
#56909=ORIENTED_EDGE('',*,*,#43286,.F.);
#56910=ORIENTED_EDGE('',*,*,#43287,.F.);
#56911=ORIENTED_EDGE('',*,*,#43288,.F.);
#56912=ORIENTED_EDGE('',*,*,#43284,.F.);
#56913=ORIENTED_EDGE('',*,*,#43289,.F.);
#56914=ORIENTED_EDGE('',*,*,#43290,.F.);
#56915=ORIENTED_EDGE('',*,*,#43291,.F.);
#56916=ORIENTED_EDGE('',*,*,#43292,.F.);
#56917=ORIENTED_EDGE('',*,*,#43293,.F.);
#56918=ORIENTED_EDGE('',*,*,#43294,.F.);
#56919=ORIENTED_EDGE('',*,*,#43289,.T.);
#56920=ORIENTED_EDGE('',*,*,#43295,.F.);
#56921=ORIENTED_EDGE('',*,*,#43296,.F.);
#56922=ORIENTED_EDGE('',*,*,#43297,.F.);
#56923=ORIENTED_EDGE('',*,*,#43293,.T.);
#56924=ORIENTED_EDGE('',*,*,#43298,.F.);
#56925=ORIENTED_EDGE('',*,*,#43299,.F.);
#56926=ORIENTED_EDGE('',*,*,#43300,.F.);
#56927=ORIENTED_EDGE('',*,*,#43301,.F.);
#56928=ORIENTED_EDGE('',*,*,#43302,.F.);
#56929=ORIENTED_EDGE('',*,*,#43303,.F.);
#56930=ORIENTED_EDGE('',*,*,#43304,.T.);
#56931=ORIENTED_EDGE('',*,*,#43305,.F.);
#56932=ORIENTED_EDGE('',*,*,#43306,.F.);
#56933=ORIENTED_EDGE('',*,*,#43307,.F.);
#56934=ORIENTED_EDGE('',*,*,#43302,.T.);
#56935=ORIENTED_EDGE('',*,*,#43308,.F.);
#56936=ORIENTED_EDGE('',*,*,#43309,.T.);
#56937=ORIENTED_EDGE('',*,*,#43310,.T.);
#56938=ORIENTED_EDGE('',*,*,#43311,.T.);
#56939=ORIENTED_EDGE('',*,*,#43312,.T.);
#56940=ORIENTED_EDGE('',*,*,#43313,.F.);
#56941=ORIENTED_EDGE('',*,*,#43314,.T.);
#56942=ORIENTED_EDGE('',*,*,#43315,.T.);
#56943=ORIENTED_EDGE('',*,*,#43316,.T.);
#56944=ORIENTED_EDGE('',*,*,#43317,.F.);
#56945=ORIENTED_EDGE('',*,*,#43318,.T.);
#56946=ORIENTED_EDGE('',*,*,#43319,.T.);
#56947=ORIENTED_EDGE('',*,*,#43310,.F.);
#56948=ORIENTED_EDGE('',*,*,#43320,.F.);
#56949=ORIENTED_EDGE('',*,*,#43321,.T.);
#56950=ORIENTED_EDGE('',*,*,#43315,.F.);
#56951=ORIENTED_EDGE('',*,*,#43322,.T.);
#56952=ORIENTED_EDGE('',*,*,#43323,.F.);
#56953=ORIENTED_EDGE('',*,*,#43324,.T.);
#56954=ORIENTED_EDGE('',*,*,#43325,.T.);
#56955=ORIENTED_EDGE('',*,*,#43324,.F.);
#56956=ORIENTED_EDGE('',*,*,#43306,.T.);
#56957=ORIENTED_EDGE('',*,*,#43326,.F.);
#56958=ORIENTED_EDGE('',*,*,#43327,.T.);
#56959=ORIENTED_EDGE('',*,*,#43328,.F.);
#56960=ORIENTED_EDGE('',*,*,#43329,.F.);
#56961=ORIENTED_EDGE('',*,*,#43330,.T.);
#56962=ORIENTED_EDGE('',*,*,#43331,.F.);
#56963=ORIENTED_EDGE('',*,*,#43304,.F.);
#56964=ORIENTED_EDGE('',*,*,#43332,.F.);
#56965=ORIENTED_EDGE('',*,*,#43333,.T.);
#56966=ORIENTED_EDGE('',*,*,#43323,.T.);
#56967=ORIENTED_EDGE('',*,*,#43333,.F.);
#56968=ORIENTED_EDGE('',*,*,#43334,.T.);
#56969=ORIENTED_EDGE('',*,*,#43335,.T.);
#56970=ORIENTED_EDGE('',*,*,#43336,.T.);
#56971=ORIENTED_EDGE('',*,*,#43335,.F.);
#56972=ORIENTED_EDGE('',*,*,#43337,.T.);
#56973=ORIENTED_EDGE('',*,*,#43338,.T.);
#56974=ORIENTED_EDGE('',*,*,#43339,.T.);
#56975=ORIENTED_EDGE('',*,*,#43340,.F.);
#56976=ORIENTED_EDGE('',*,*,#43341,.T.);
#56977=ORIENTED_EDGE('',*,*,#43342,.T.);
#56978=ORIENTED_EDGE('',*,*,#43343,.F.);
#56979=ORIENTED_EDGE('',*,*,#43341,.F.);
#56980=ORIENTED_EDGE('',*,*,#43344,.F.);
#56981=ORIENTED_EDGE('',*,*,#43342,.F.);
#56982=ORIENTED_EDGE('',*,*,#43345,.T.);
#56983=ORIENTED_EDGE('',*,*,#43346,.F.);
#56984=ORIENTED_EDGE('',*,*,#43345,.F.);
#56985=ORIENTED_EDGE('',*,*,#43338,.F.);
#56986=ORIENTED_EDGE('',*,*,#43347,.F.);
#56987=ORIENTED_EDGE('',*,*,#43339,.F.);
#56988=ORIENTED_EDGE('',*,*,#43348,.T.);
#56989=ORIENTED_EDGE('',*,*,#43349,.F.);
#56990=ORIENTED_EDGE('',*,*,#43348,.F.);
#56991=ORIENTED_EDGE('',*,*,#43299,.T.);
#56992=ORIENTED_EDGE('',*,*,#43350,.F.);
#56993=ORIENTED_EDGE('',*,*,#43351,.F.);
#56994=ORIENTED_EDGE('',*,*,#43352,.F.);
#56995=ORIENTED_EDGE('',*,*,#43327,.F.);
#56996=ORIENTED_EDGE('',*,*,#43353,.F.);
#56997=ORIENTED_EDGE('',*,*,#43334,.F.);
#56998=ORIENTED_EDGE('',*,*,#43354,.T.);
#56999=ORIENTED_EDGE('',*,*,#43355,.F.);
#57000=ORIENTED_EDGE('',*,*,#43354,.F.);
#57001=ORIENTED_EDGE('',*,*,#43337,.F.);
#57002=ORIENTED_EDGE('',*,*,#43296,.T.);
#57003=ORIENTED_EDGE('',*,*,#43356,.F.);
#57004=ORIENTED_EDGE('',*,*,#43330,.F.);
#57005=ORIENTED_EDGE('',*,*,#43357,.F.);
#57006=ORIENTED_EDGE('',*,*,#43358,.F.);
#57007=ORIENTED_EDGE('',*,*,#43359,.T.);
#57008=ORIENTED_EDGE('',*,*,#43360,.T.);
#57009=ORIENTED_EDGE('',*,*,#43359,.F.);
#57010=ORIENTED_EDGE('',*,*,#43360,.F.);
#57011=ORIENTED_EDGE('',*,*,#43361,.T.);
#57012=ORIENTED_EDGE('',*,*,#43362,.T.);
#57013=ORIENTED_EDGE('',*,*,#43361,.F.);
#57014=ORIENTED_EDGE('',*,*,#43362,.F.);
#57015=ORIENTED_EDGE('',*,*,#43363,.T.);
#57016=ORIENTED_EDGE('',*,*,#43364,.T.);
#57017=ORIENTED_EDGE('',*,*,#43363,.F.);
#57018=ORIENTED_EDGE('',*,*,#43365,.T.);
#57019=ORIENTED_EDGE('',*,*,#43366,.T.);
#57020=ORIENTED_EDGE('',*,*,#43367,.T.);
#57021=ORIENTED_EDGE('',*,*,#43366,.F.);
#57022=ORIENTED_EDGE('',*,*,#43368,.T.);
#57023=ORIENTED_EDGE('',*,*,#43369,.T.);
#57024=ORIENTED_EDGE('',*,*,#43370,.T.);
#57025=ORIENTED_EDGE('',*,*,#43371,.T.);
#57026=ORIENTED_EDGE('',*,*,#43372,.T.);
#57027=ORIENTED_EDGE('',*,*,#43370,.F.);
#57028=ORIENTED_EDGE('',*,*,#43373,.F.);
#57029=ORIENTED_EDGE('',*,*,#43374,.T.);
#57030=ORIENTED_EDGE('',*,*,#43369,.F.);
#57031=ORIENTED_EDGE('',*,*,#43374,.F.);
#57032=ORIENTED_EDGE('',*,*,#43375,.F.);
#57033=ORIENTED_EDGE('',*,*,#43376,.T.);
#57034=ORIENTED_EDGE('',*,*,#43371,.F.);
#57035=ORIENTED_EDGE('',*,*,#43372,.F.);
#57036=ORIENTED_EDGE('',*,*,#43376,.F.);
#57037=ORIENTED_EDGE('',*,*,#43365,.F.);
#57038=ORIENTED_EDGE('',*,*,#43377,.T.);
#57039=ORIENTED_EDGE('',*,*,#43375,.T.);
#57040=ORIENTED_EDGE('',*,*,#43377,.F.);
#57041=ORIENTED_EDGE('',*,*,#43368,.F.);
#57042=ORIENTED_EDGE('',*,*,#43378,.F.);
#57043=ORIENTED_EDGE('',*,*,#43379,.T.);
#57044=ORIENTED_EDGE('',*,*,#43380,.T.);
#57045=ORIENTED_EDGE('',*,*,#43379,.F.);
#57046=ORIENTED_EDGE('',*,*,#43380,.F.);
#57047=ORIENTED_EDGE('',*,*,#43381,.T.);
#57048=ORIENTED_EDGE('',*,*,#43382,.F.);
#57049=ORIENTED_EDGE('',*,*,#43381,.F.);
#57050=ORIENTED_EDGE('',*,*,#43383,.F.);
#57051=ORIENTED_EDGE('',*,*,#43384,.T.);
#57052=ORIENTED_EDGE('',*,*,#43385,.T.);
#57053=ORIENTED_EDGE('',*,*,#43384,.F.);
#57054=ORIENTED_EDGE('',*,*,#43386,.T.);
#57055=ORIENTED_EDGE('',*,*,#43387,.T.);
#57056=ORIENTED_EDGE('',*,*,#43388,.T.);
#57057=ORIENTED_EDGE('',*,*,#43387,.F.);
#57058=ORIENTED_EDGE('',*,*,#43347,.T.);
#57059=ORIENTED_EDGE('',*,*,#43343,.T.);
#57060=ORIENTED_EDGE('',*,*,#43344,.T.);
#57061=ORIENTED_EDGE('',*,*,#43340,.T.);
#57062=ORIENTED_EDGE('',*,*,#43383,.T.);
#57063=ORIENTED_EDGE('',*,*,#43386,.F.);
#57064=ORIENTED_EDGE('',*,*,#43382,.T.);
#57065=ORIENTED_EDGE('',*,*,#43385,.F.);
#57066=ORIENTED_EDGE('',*,*,#43373,.T.);
#57067=ORIENTED_EDGE('',*,*,#43367,.F.);
#57068=ORIENTED_EDGE('',*,*,#43378,.T.);
#57069=ORIENTED_EDGE('',*,*,#43364,.F.);
#57070=ORIENTED_EDGE('',*,*,#43358,.T.);
#57071=ORIENTED_EDGE('',*,*,#43388,.F.);
#57072=ORIENTED_EDGE('',*,*,#43329,.T.);
#57073=ORIENTED_EDGE('',*,*,#43332,.T.);
#57074=ORIENTED_EDGE('',*,*,#43303,.T.);
#57075=ORIENTED_EDGE('',*,*,#43307,.T.);
#57076=ORIENTED_EDGE('',*,*,#43328,.T.);
#57077=ORIENTED_EDGE('',*,*,#43352,.T.);
#57078=ORIENTED_EDGE('',*,*,#43351,.T.);
#57079=ORIENTED_EDGE('',*,*,#43290,.T.);
#57080=ORIENTED_EDGE('',*,*,#43294,.T.);
#57081=ORIENTED_EDGE('',*,*,#43297,.T.);
#57082=ORIENTED_EDGE('',*,*,#43357,.T.);
#57083=ORIENTED_EDGE('',*,*,#43331,.T.);
#57084=ORIENTED_EDGE('',*,*,#43356,.T.);
#57085=ORIENTED_EDGE('',*,*,#43298,.T.);
#57086=ORIENTED_EDGE('',*,*,#43295,.T.);
#57087=ORIENTED_EDGE('',*,*,#43292,.T.);
#57088=ORIENTED_EDGE('',*,*,#43300,.T.);
#57089=ORIENTED_EDGE('',*,*,#43353,.T.);
#57090=ORIENTED_EDGE('',*,*,#43326,.T.);
#57091=ORIENTED_EDGE('',*,*,#43308,.T.);
#57092=ORIENTED_EDGE('',*,*,#43305,.T.);
#57093=ORIENTED_EDGE('',*,*,#43313,.T.);
#57094=ORIENTED_EDGE('',*,*,#43389,.F.);
#57095=ORIENTED_EDGE('',*,*,#43389,.T.);
#57096=ORIENTED_EDGE('',*,*,#43312,.F.);
#57097=ORIENTED_EDGE('',*,*,#43390,.F.);
#57098=ORIENTED_EDGE('',*,*,#43391,.F.);
#57099=ORIENTED_EDGE('',*,*,#43322,.F.);
#57100=ORIENTED_EDGE('',*,*,#43314,.F.);
#57101=ORIENTED_EDGE('',*,*,#43317,.T.);
#57102=ORIENTED_EDGE('',*,*,#43392,.F.);
#57103=ORIENTED_EDGE('',*,*,#43392,.T.);
#57104=ORIENTED_EDGE('',*,*,#43316,.F.);
#57105=ORIENTED_EDGE('',*,*,#43321,.F.);
#57106=ORIENTED_EDGE('',*,*,#43393,.F.);
#57107=ORIENTED_EDGE('',*,*,#43394,.F.);
#57108=ORIENTED_EDGE('',*,*,#43318,.F.);
#57109=ORIENTED_EDGE('',*,*,#43336,.F.);
#57110=ORIENTED_EDGE('',*,*,#43349,.T.);
#57111=ORIENTED_EDGE('',*,*,#43291,.T.);
#57112=ORIENTED_EDGE('',*,*,#43350,.T.);
#57113=ORIENTED_EDGE('',*,*,#43301,.T.);
#57114=ORIENTED_EDGE('',*,*,#43355,.T.);
#57115=ORIENTED_EDGE('',*,*,#43309,.F.);
#57116=ORIENTED_EDGE('',*,*,#43325,.F.);
#57117=ORIENTED_EDGE('',*,*,#43395,.F.);
#57118=ORIENTED_EDGE('',*,*,#43390,.T.);
#57119=ORIENTED_EDGE('',*,*,#43311,.F.);
#57120=ORIENTED_EDGE('',*,*,#43319,.F.);
#57121=ORIENTED_EDGE('',*,*,#43394,.T.);
#57122=ORIENTED_EDGE('',*,*,#43320,.T.);
#57123=ORIENTED_EDGE('',*,*,#43391,.T.);
#57124=ORIENTED_EDGE('',*,*,#43395,.T.);
#57125=ORIENTED_EDGE('',*,*,#43393,.T.);
#57126=ORIENTED_EDGE('',*,*,#43346,.T.);
#57127=ORIENTED_EDGE('',*,*,#43396,.F.);
#57128=ORIENTED_EDGE('',*,*,#43397,.T.);
#57129=ORIENTED_EDGE('',*,*,#43398,.T.);
#57130=ORIENTED_EDGE('',*,*,#43397,.F.);
#57131=ORIENTED_EDGE('',*,*,#43398,.F.);
#57132=ORIENTED_EDGE('',*,*,#43399,.T.);
#57133=ORIENTED_EDGE('',*,*,#43400,.T.);
#57134=ORIENTED_EDGE('',*,*,#43399,.F.);
#57135=ORIENTED_EDGE('',*,*,#43401,.F.);
#57136=ORIENTED_EDGE('',*,*,#43402,.F.);
#57137=ORIENTED_EDGE('',*,*,#43403,.T.);
#57138=ORIENTED_EDGE('',*,*,#43404,.T.);
#57139=ORIENTED_EDGE('',*,*,#43405,.F.);
#57140=ORIENTED_EDGE('',*,*,#43404,.F.);
#57141=ORIENTED_EDGE('',*,*,#43406,.T.);
#57142=ORIENTED_EDGE('',*,*,#43402,.T.);
#57143=ORIENTED_EDGE('',*,*,#43407,.F.);
#57144=ORIENTED_EDGE('',*,*,#43408,.T.);
#57145=ORIENTED_EDGE('',*,*,#43409,.T.);
#57146=ORIENTED_EDGE('',*,*,#43408,.F.);
#57147=ORIENTED_EDGE('',*,*,#43410,.F.);
#57148=ORIENTED_EDGE('',*,*,#43411,.T.);
#57149=ORIENTED_EDGE('',*,*,#43407,.T.);
#57150=ORIENTED_EDGE('',*,*,#43411,.F.);
#57151=ORIENTED_EDGE('',*,*,#43412,.F.);
#57152=ORIENTED_EDGE('',*,*,#43413,.T.);
#57153=ORIENTED_EDGE('',*,*,#43414,.T.);
#57154=ORIENTED_EDGE('',*,*,#43413,.F.);
#57155=ORIENTED_EDGE('',*,*,#43409,.F.);
#57156=ORIENTED_EDGE('',*,*,#43412,.T.);
#57157=ORIENTED_EDGE('',*,*,#43414,.F.);
#57158=ORIENTED_EDGE('',*,*,#43406,.F.);
#57159=ORIENTED_EDGE('',*,*,#43403,.F.);
#57160=ORIENTED_EDGE('',*,*,#43415,.T.);
#57161=ORIENTED_EDGE('',*,*,#43405,.T.);
#57162=ORIENTED_EDGE('',*,*,#43401,.T.);
#57163=ORIENTED_EDGE('',*,*,#43415,.F.);
#57164=ORIENTED_EDGE('',*,*,#43416,.T.);
#57165=ORIENTED_EDGE('',*,*,#43417,.T.);
#57166=ORIENTED_EDGE('',*,*,#43416,.F.);
#57167=ORIENTED_EDGE('',*,*,#43396,.T.);
#57168=ORIENTED_EDGE('',*,*,#43417,.F.);
#57169=ORIENTED_EDGE('',*,*,#43400,.F.);
#57170=ORIENTED_EDGE('',*,*,#43410,.T.);
#57171=ORIENTED_EDGE('',*,*,#43418,.F.);
#57172=ORIENTED_EDGE('',*,*,#43419,.T.);
#57173=ORIENTED_EDGE('',*,*,#43420,.T.);
#57174=ORIENTED_EDGE('',*,*,#43421,.F.);
#57175=ORIENTED_EDGE('',*,*,#43422,.F.);
#57176=ORIENTED_EDGE('',*,*,#43418,.T.);
#57177=ORIENTED_EDGE('',*,*,#43423,.T.);
#57178=ORIENTED_EDGE('',*,*,#43424,.F.);
#57179=ORIENTED_EDGE('',*,*,#43425,.F.);
#57180=ORIENTED_EDGE('',*,*,#43426,.F.);
#57181=ORIENTED_EDGE('',*,*,#43421,.T.);
#57182=ORIENTED_EDGE('',*,*,#43427,.T.);
#57183=ORIENTED_EDGE('',*,*,#43428,.F.);
#57184=ORIENTED_EDGE('',*,*,#43429,.F.);
#57185=ORIENTED_EDGE('',*,*,#43430,.F.);
#57186=ORIENTED_EDGE('',*,*,#43425,.T.);
#57187=ORIENTED_EDGE('',*,*,#43431,.T.);
#57188=ORIENTED_EDGE('',*,*,#43432,.T.);
#57189=ORIENTED_EDGE('',*,*,#43433,.T.);
#57190=ORIENTED_EDGE('',*,*,#43434,.T.);
#57191=ORIENTED_EDGE('',*,*,#43433,.F.);
#57192=ORIENTED_EDGE('',*,*,#43435,.T.);
#57193=ORIENTED_EDGE('',*,*,#43432,.F.);
#57194=ORIENTED_EDGE('',*,*,#43436,.T.);
#57195=ORIENTED_EDGE('',*,*,#43437,.F.);
#57196=ORIENTED_EDGE('',*,*,#43436,.F.);
#57197=ORIENTED_EDGE('',*,*,#43435,.F.);
#57198=ORIENTED_EDGE('',*,*,#43437,.T.);
#57199=ORIENTED_EDGE('',*,*,#43438,.T.);
#57200=ORIENTED_EDGE('',*,*,#43439,.F.);
#57201=ORIENTED_EDGE('',*,*,#43438,.F.);
#57202=ORIENTED_EDGE('',*,*,#43440,.F.);
#57203=ORIENTED_EDGE('',*,*,#43441,.T.);
#57204=ORIENTED_EDGE('',*,*,#43442,.F.);
#57205=ORIENTED_EDGE('',*,*,#43443,.F.);
#57206=ORIENTED_EDGE('',*,*,#43444,.F.);
#57207=ORIENTED_EDGE('',*,*,#43445,.T.);
#57208=ORIENTED_EDGE('',*,*,#43446,.F.);
#57209=ORIENTED_EDGE('',*,*,#43447,.F.);
#57210=ORIENTED_EDGE('',*,*,#43439,.T.);
#57211=ORIENTED_EDGE('',*,*,#43448,.T.);
#57212=ORIENTED_EDGE('',*,*,#43449,.T.);
#57213=ORIENTED_EDGE('',*,*,#43450,.T.);
#57214=ORIENTED_EDGE('',*,*,#43451,.F.);
#57215=ORIENTED_EDGE('',*,*,#43452,.T.);
#57216=ORIENTED_EDGE('',*,*,#43453,.F.);
#57217=ORIENTED_EDGE('',*,*,#43452,.F.);
#57218=ORIENTED_EDGE('',*,*,#43454,.F.);
#57219=ORIENTED_EDGE('',*,*,#43440,.T.);
#57220=ORIENTED_EDGE('',*,*,#43455,.T.);
#57221=ORIENTED_EDGE('',*,*,#43448,.F.);
#57222=ORIENTED_EDGE('',*,*,#43456,.F.);
#57223=ORIENTED_EDGE('',*,*,#43457,.T.);
#57224=ORIENTED_EDGE('',*,*,#43458,.T.);
#57225=ORIENTED_EDGE('',*,*,#43459,.T.);
#57226=ORIENTED_EDGE('',*,*,#43460,.T.);
#57227=ORIENTED_EDGE('',*,*,#43461,.T.);
#57228=ORIENTED_EDGE('',*,*,#43462,.F.);
#57229=ORIENTED_EDGE('',*,*,#43463,.T.);
#57230=ORIENTED_EDGE('',*,*,#43464,.F.);
#57231=ORIENTED_EDGE('',*,*,#43465,.T.);
#57232=ORIENTED_EDGE('',*,*,#43466,.T.);
#57233=ORIENTED_EDGE('',*,*,#43446,.T.);
#57234=ORIENTED_EDGE('',*,*,#43467,.F.);
#57235=ORIENTED_EDGE('',*,*,#43468,.T.);
#57236=ORIENTED_EDGE('',*,*,#43461,.F.);
#57237=ORIENTED_EDGE('',*,*,#43469,.F.);
#57238=ORIENTED_EDGE('',*,*,#43457,.F.);
#57239=ORIENTED_EDGE('',*,*,#43470,.T.);
#57240=ORIENTED_EDGE('',*,*,#43471,.F.);
#57241=ORIENTED_EDGE('',*,*,#43472,.F.);
#57242=ORIENTED_EDGE('',*,*,#43473,.T.);
#57243=ORIENTED_EDGE('',*,*,#43474,.T.);
#57244=ORIENTED_EDGE('',*,*,#43475,.T.);
#57245=ORIENTED_EDGE('',*,*,#43476,.T.);
#57246=ORIENTED_EDGE('',*,*,#43477,.F.);
#57247=ORIENTED_EDGE('',*,*,#43478,.T.);
#57248=ORIENTED_EDGE('',*,*,#43479,.F.);
#57249=ORIENTED_EDGE('',*,*,#43478,.F.);
#57250=ORIENTED_EDGE('',*,*,#43480,.F.);
#57251=ORIENTED_EDGE('',*,*,#43442,.T.);
#57252=ORIENTED_EDGE('',*,*,#43481,.T.);
#57253=ORIENTED_EDGE('',*,*,#43474,.F.);
#57254=ORIENTED_EDGE('',*,*,#43482,.T.);
#57255=ORIENTED_EDGE('',*,*,#43467,.T.);
#57256=ORIENTED_EDGE('',*,*,#43483,.F.);
#57257=ORIENTED_EDGE('',*,*,#43484,.T.);
#57258=ORIENTED_EDGE('',*,*,#43485,.F.);
#57259=ORIENTED_EDGE('',*,*,#43471,.T.);
#57260=ORIENTED_EDGE('',*,*,#43486,.T.);
#57261=ORIENTED_EDGE('',*,*,#43487,.T.);
#57262=ORIENTED_EDGE('',*,*,#43488,.T.);
#57263=ORIENTED_EDGE('',*,*,#43444,.T.);
#57264=ORIENTED_EDGE('',*,*,#43489,.F.);
#57265=ORIENTED_EDGE('',*,*,#43490,.T.);
#57266=ORIENTED_EDGE('',*,*,#43491,.T.);
#57267=ORIENTED_EDGE('',*,*,#43492,.T.);
#57268=ORIENTED_EDGE('',*,*,#43473,.F.);
#57269=ORIENTED_EDGE('',*,*,#43492,.F.);
#57270=ORIENTED_EDGE('',*,*,#43493,.T.);
#57271=ORIENTED_EDGE('',*,*,#43494,.T.);
#57272=ORIENTED_EDGE('',*,*,#43495,.F.);
#57273=ORIENTED_EDGE('',*,*,#43494,.F.);
#57274=ORIENTED_EDGE('',*,*,#43496,.T.);
#57275=ORIENTED_EDGE('',*,*,#43497,.T.);
#57276=ORIENTED_EDGE('',*,*,#43498,.F.);
#57277=ORIENTED_EDGE('',*,*,#43497,.F.);
#57278=ORIENTED_EDGE('',*,*,#43479,.T.);
#57279=ORIENTED_EDGE('',*,*,#43499,.T.);
#57280=ORIENTED_EDGE('',*,*,#43500,.F.);
#57281=ORIENTED_EDGE('',*,*,#43499,.F.);
#57282=ORIENTED_EDGE('',*,*,#43500,.T.);
#57283=ORIENTED_EDGE('',*,*,#43501,.T.);
#57284=ORIENTED_EDGE('',*,*,#43502,.F.);
#57285=ORIENTED_EDGE('',*,*,#43503,.F.);
#57286=ORIENTED_EDGE('',*,*,#43501,.F.);
#57287=ORIENTED_EDGE('',*,*,#43504,.T.);
#57288=ORIENTED_EDGE('',*,*,#43505,.T.);
#57289=ORIENTED_EDGE('',*,*,#43502,.T.);
#57290=ORIENTED_EDGE('',*,*,#43503,.T.);
#57291=ORIENTED_EDGE('',*,*,#43505,.F.);
#57292=ORIENTED_EDGE('',*,*,#43506,.T.);
#57293=ORIENTED_EDGE('',*,*,#43507,.T.);
#57294=ORIENTED_EDGE('',*,*,#43508,.F.);
#57295=ORIENTED_EDGE('',*,*,#43507,.F.);
#57296=ORIENTED_EDGE('',*,*,#43509,.T.);
#57297=ORIENTED_EDGE('',*,*,#43510,.T.);
#57298=ORIENTED_EDGE('',*,*,#43511,.F.);
#57299=ORIENTED_EDGE('',*,*,#43510,.F.);
#57300=ORIENTED_EDGE('',*,*,#43512,.T.);
#57301=ORIENTED_EDGE('',*,*,#43513,.T.);
#57302=ORIENTED_EDGE('',*,*,#43514,.F.);
#57303=ORIENTED_EDGE('',*,*,#43513,.F.);
#57304=ORIENTED_EDGE('',*,*,#43515,.T.);
#57305=ORIENTED_EDGE('',*,*,#43516,.F.);
#57306=ORIENTED_EDGE('',*,*,#43517,.F.);
#57307=ORIENTED_EDGE('',*,*,#43518,.T.);
#57308=ORIENTED_EDGE('',*,*,#43519,.T.);
#57309=ORIENTED_EDGE('',*,*,#43520,.T.);
#57310=ORIENTED_EDGE('',*,*,#43521,.F.);
#57311=ORIENTED_EDGE('',*,*,#43522,.T.);
#57312=ORIENTED_EDGE('',*,*,#43523,.F.);
#57313=ORIENTED_EDGE('',*,*,#43522,.F.);
#57314=ORIENTED_EDGE('',*,*,#43524,.F.);
#57315=ORIENTED_EDGE('',*,*,#43525,.F.);
#57316=ORIENTED_EDGE('',*,*,#43526,.F.);
#57317=ORIENTED_EDGE('',*,*,#43527,.F.);
#57318=ORIENTED_EDGE('',*,*,#43528,.T.);
#57319=ORIENTED_EDGE('',*,*,#43529,.T.);
#57320=ORIENTED_EDGE('',*,*,#43423,.F.);
#57321=ORIENTED_EDGE('',*,*,#43420,.F.);
#57322=ORIENTED_EDGE('',*,*,#43530,.T.);
#57323=ORIENTED_EDGE('',*,*,#43531,.T.);
#57324=ORIENTED_EDGE('',*,*,#43532,.F.);
#57325=ORIENTED_EDGE('',*,*,#43531,.F.);
#57326=ORIENTED_EDGE('',*,*,#43533,.T.);
#57327=ORIENTED_EDGE('',*,*,#43534,.F.);
#57328=ORIENTED_EDGE('',*,*,#43535,.F.);
#57329=ORIENTED_EDGE('',*,*,#43536,.F.);
#57330=ORIENTED_EDGE('',*,*,#43431,.F.);
#57331=ORIENTED_EDGE('',*,*,#43427,.F.);
#57332=ORIENTED_EDGE('',*,*,#43537,.F.);
#57333=ORIENTED_EDGE('',*,*,#43538,.T.);
#57334=ORIENTED_EDGE('',*,*,#43539,.F.);
#57335=ORIENTED_EDGE('',*,*,#43540,.F.);
#57336=ORIENTED_EDGE('',*,*,#43541,.T.);
#57337=ORIENTED_EDGE('',*,*,#43542,.T.);
#57338=ORIENTED_EDGE('',*,*,#43543,.T.);
#57339=ORIENTED_EDGE('',*,*,#43544,.F.);
#57340=ORIENTED_EDGE('',*,*,#43545,.F.);
#57341=ORIENTED_EDGE('',*,*,#43533,.F.);
#57342=ORIENTED_EDGE('',*,*,#43538,.F.);
#57343=ORIENTED_EDGE('',*,*,#43546,.F.);
#57344=ORIENTED_EDGE('',*,*,#43518,.F.);
#57345=ORIENTED_EDGE('',*,*,#43547,.F.);
#57346=ORIENTED_EDGE('',*,*,#43516,.T.);
#57347=ORIENTED_EDGE('',*,*,#43548,.F.);
#57348=ORIENTED_EDGE('',*,*,#43549,.T.);
#57349=ORIENTED_EDGE('',*,*,#43550,.T.);
#57350=ORIENTED_EDGE('',*,*,#43519,.F.);
#57351=ORIENTED_EDGE('',*,*,#43546,.T.);
#57352=ORIENTED_EDGE('',*,*,#43551,.F.);
#57353=ORIENTED_EDGE('',*,*,#43552,.T.);
#57354=ORIENTED_EDGE('',*,*,#43553,.F.);
#57355=ORIENTED_EDGE('',*,*,#43548,.T.);
#57356=ORIENTED_EDGE('',*,*,#43515,.F.);
#57357=ORIENTED_EDGE('',*,*,#43552,.F.);
#57358=ORIENTED_EDGE('',*,*,#43525,.T.);
#57359=ORIENTED_EDGE('',*,*,#43554,.F.);
#57360=ORIENTED_EDGE('',*,*,#43520,.F.);
#57361=ORIENTED_EDGE('',*,*,#43550,.F.);
#57362=ORIENTED_EDGE('',*,*,#43555,.T.);
#57363=ORIENTED_EDGE('',*,*,#43547,.T.);
#57364=ORIENTED_EDGE('',*,*,#43517,.T.);
#57365=ORIENTED_EDGE('',*,*,#43554,.T.);
#57366=ORIENTED_EDGE('',*,*,#43524,.T.);
#57367=ORIENTED_EDGE('',*,*,#43521,.T.);
#57368=ORIENTED_EDGE('',*,*,#43523,.T.);
#57369=ORIENTED_EDGE('',*,*,#43512,.F.);
#57370=ORIENTED_EDGE('',*,*,#43535,.T.);
#57371=ORIENTED_EDGE('',*,*,#43534,.T.);
#57372=ORIENTED_EDGE('',*,*,#43545,.T.);
#57373=ORIENTED_EDGE('',*,*,#43544,.T.);
#57374=ORIENTED_EDGE('',*,*,#43556,.T.);
#57375=ORIENTED_EDGE('',*,*,#43557,.T.);
#57376=ORIENTED_EDGE('',*,*,#43429,.T.);
#57377=ORIENTED_EDGE('',*,*,#43558,.T.);
#57378=ORIENTED_EDGE('',*,*,#43514,.T.);
#57379=ORIENTED_EDGE('',*,*,#43556,.F.);
#57380=ORIENTED_EDGE('',*,*,#43543,.F.);
#57381=ORIENTED_EDGE('',*,*,#43559,.F.);
#57382=ORIENTED_EDGE('',*,*,#43422,.T.);
#57383=ORIENTED_EDGE('',*,*,#43426,.T.);
#57384=ORIENTED_EDGE('',*,*,#43430,.T.);
#57385=ORIENTED_EDGE('',*,*,#43557,.F.);
#57386=ORIENTED_EDGE('',*,*,#43428,.T.);
#57387=ORIENTED_EDGE('',*,*,#43536,.T.);
#57388=ORIENTED_EDGE('',*,*,#43558,.F.);
#57389=ORIENTED_EDGE('',*,*,#43424,.T.);
#57390=ORIENTED_EDGE('',*,*,#43529,.F.);
#57391=ORIENTED_EDGE('',*,*,#43528,.F.);
#57392=ORIENTED_EDGE('',*,*,#43560,.F.);
#57393=ORIENTED_EDGE('',*,*,#43539,.T.);
#57394=ORIENTED_EDGE('',*,*,#43537,.T.);
#57395=ORIENTED_EDGE('',*,*,#43542,.F.);
#57396=ORIENTED_EDGE('',*,*,#43561,.F.);
#57397=ORIENTED_EDGE('',*,*,#43562,.T.);
#57398=ORIENTED_EDGE('',*,*,#43526,.T.);
#57399=ORIENTED_EDGE('',*,*,#43419,.F.);
#57400=ORIENTED_EDGE('',*,*,#43559,.T.);
#57401=ORIENTED_EDGE('',*,*,#43540,.T.);
#57402=ORIENTED_EDGE('',*,*,#43560,.T.);
#57403=ORIENTED_EDGE('',*,*,#43527,.T.);
#57404=ORIENTED_EDGE('',*,*,#43562,.F.);
#57405=ORIENTED_EDGE('',*,*,#43561,.T.);
#57406=ORIENTED_EDGE('',*,*,#43541,.F.);
#57407=ORIENTED_EDGE('',*,*,#43530,.F.);
#57408=ORIENTED_EDGE('',*,*,#43511,.T.);
#57409=ORIENTED_EDGE('',*,*,#43506,.F.);
#57410=ORIENTED_EDGE('',*,*,#43551,.T.);
#57411=ORIENTED_EDGE('',*,*,#43549,.F.);
#57412=ORIENTED_EDGE('',*,*,#43553,.T.);
#57413=ORIENTED_EDGE('',*,*,#43555,.F.);
#57414=ORIENTED_EDGE('',*,*,#43508,.T.);
#57415=ORIENTED_EDGE('',*,*,#43563,.F.);
#57416=ORIENTED_EDGE('',*,*,#43564,.F.);
#57417=ORIENTED_EDGE('',*,*,#43565,.F.);
#57418=ORIENTED_EDGE('',*,*,#43566,.T.);
#57419=ORIENTED_EDGE('',*,*,#43567,.F.);
#57420=ORIENTED_EDGE('',*,*,#43568,.T.);
#57421=ORIENTED_EDGE('',*,*,#43569,.T.);
#57422=ORIENTED_EDGE('',*,*,#43570,.F.);
#57423=ORIENTED_EDGE('',*,*,#43566,.F.);
#57424=ORIENTED_EDGE('',*,*,#43571,.F.);
#57425=ORIENTED_EDGE('',*,*,#43569,.F.);
#57426=ORIENTED_EDGE('',*,*,#43572,.T.);
#57427=ORIENTED_EDGE('',*,*,#43573,.T.);
#57428=ORIENTED_EDGE('',*,*,#43564,.T.);
#57429=ORIENTED_EDGE('',*,*,#43574,.F.);
#57430=ORIENTED_EDGE('',*,*,#43573,.F.);
#57431=ORIENTED_EDGE('',*,*,#43575,.T.);
#57432=ORIENTED_EDGE('',*,*,#43576,.F.);
#57433=ORIENTED_EDGE('',*,*,#43577,.T.);
#57434=ORIENTED_EDGE('',*,*,#43567,.T.);
#57435=ORIENTED_EDGE('',*,*,#43565,.T.);
#57436=ORIENTED_EDGE('',*,*,#43576,.T.);
#57437=ORIENTED_EDGE('',*,*,#43578,.F.);
#57438=ORIENTED_EDGE('',*,*,#43579,.F.);
#57439=ORIENTED_EDGE('',*,*,#43580,.F.);
#57440=ORIENTED_EDGE('',*,*,#43581,.T.);
#57441=ORIENTED_EDGE('',*,*,#43582,.T.);
#57442=ORIENTED_EDGE('',*,*,#43583,.T.);
#57443=ORIENTED_EDGE('',*,*,#43584,.F.);
#57444=ORIENTED_EDGE('',*,*,#43581,.F.);
#57445=ORIENTED_EDGE('',*,*,#43585,.F.);
#57446=ORIENTED_EDGE('',*,*,#43586,.F.);
#57447=ORIENTED_EDGE('',*,*,#43583,.F.);
#57448=ORIENTED_EDGE('',*,*,#43587,.T.);
#57449=ORIENTED_EDGE('',*,*,#43588,.T.);
#57450=ORIENTED_EDGE('',*,*,#43579,.T.);
#57451=ORIENTED_EDGE('',*,*,#43589,.F.);
#57452=ORIENTED_EDGE('',*,*,#43588,.F.);
#57453=ORIENTED_EDGE('',*,*,#43590,.T.);
#57454=ORIENTED_EDGE('',*,*,#43591,.F.);
#57455=ORIENTED_EDGE('',*,*,#43592,.T.);
#57456=ORIENTED_EDGE('',*,*,#43585,.T.);
#57457=ORIENTED_EDGE('',*,*,#43580,.T.);
#57458=ORIENTED_EDGE('',*,*,#43591,.T.);
#57459=ORIENTED_EDGE('',*,*,#43593,.F.);
#57460=ORIENTED_EDGE('',*,*,#43594,.T.);
#57461=ORIENTED_EDGE('',*,*,#43595,.T.);
#57462=ORIENTED_EDGE('',*,*,#43596,.F.);
#57463=ORIENTED_EDGE('',*,*,#43597,.F.);
#57464=ORIENTED_EDGE('',*,*,#43598,.F.);
#57465=ORIENTED_EDGE('',*,*,#43593,.T.);
#57466=ORIENTED_EDGE('',*,*,#43599,.F.);
#57467=ORIENTED_EDGE('',*,*,#43600,.F.);
#57468=ORIENTED_EDGE('',*,*,#43601,.F.);
#57469=ORIENTED_EDGE('',*,*,#43597,.T.);
#57470=ORIENTED_EDGE('',*,*,#43602,.F.);
#57471=ORIENTED_EDGE('',*,*,#43595,.F.);
#57472=ORIENTED_EDGE('',*,*,#43603,.T.);
#57473=ORIENTED_EDGE('',*,*,#43604,.F.);
#57474=ORIENTED_EDGE('',*,*,#43600,.T.);
#57475=ORIENTED_EDGE('',*,*,#43605,.F.);
#57476=ORIENTED_EDGE('',*,*,#43598,.T.);
#57477=ORIENTED_EDGE('',*,*,#43601,.T.);
#57478=ORIENTED_EDGE('',*,*,#43604,.T.);
#57479=ORIENTED_EDGE('',*,*,#43606,.T.);
#57480=ORIENTED_EDGE('',*,*,#43607,.F.);
#57481=ORIENTED_EDGE('',*,*,#43608,.T.);
#57482=ORIENTED_EDGE('',*,*,#43609,.T.);
#57483=ORIENTED_EDGE('',*,*,#43610,.F.);
#57484=ORIENTED_EDGE('',*,*,#43611,.F.);
#57485=ORIENTED_EDGE('',*,*,#43612,.T.);
#57486=ORIENTED_EDGE('',*,*,#43607,.T.);
#57487=ORIENTED_EDGE('',*,*,#43613,.F.);
#57488=ORIENTED_EDGE('',*,*,#43614,.F.);
#57489=ORIENTED_EDGE('',*,*,#43615,.T.);
#57490=ORIENTED_EDGE('',*,*,#43611,.T.);
#57491=ORIENTED_EDGE('',*,*,#43616,.F.);
#57492=ORIENTED_EDGE('',*,*,#43609,.F.);
#57493=ORIENTED_EDGE('',*,*,#43617,.T.);
#57494=ORIENTED_EDGE('',*,*,#43614,.T.);
#57495=ORIENTED_EDGE('',*,*,#43618,.F.);
#57496=ORIENTED_EDGE('',*,*,#43619,.F.);
#57497=ORIENTED_EDGE('',*,*,#43620,.T.);
#57498=ORIENTED_EDGE('',*,*,#43621,.T.);
#57499=ORIENTED_EDGE('',*,*,#43622,.F.);
#57500=ORIENTED_EDGE('',*,*,#43623,.F.);
#57501=ORIENTED_EDGE('',*,*,#43624,.T.);
#57502=ORIENTED_EDGE('',*,*,#43619,.T.);
#57503=ORIENTED_EDGE('',*,*,#43625,.F.);
#57504=ORIENTED_EDGE('',*,*,#43626,.F.);
#57505=ORIENTED_EDGE('',*,*,#43627,.T.);
#57506=ORIENTED_EDGE('',*,*,#43623,.T.);
#57507=ORIENTED_EDGE('',*,*,#43628,.F.);
#57508=ORIENTED_EDGE('',*,*,#43621,.F.);
#57509=ORIENTED_EDGE('',*,*,#43629,.T.);
#57510=ORIENTED_EDGE('',*,*,#43626,.T.);
#57511=ORIENTED_EDGE('',*,*,#43630,.F.);
#57512=ORIENTED_EDGE('',*,*,#43631,.F.);
#57513=ORIENTED_EDGE('',*,*,#43632,.T.);
#57514=ORIENTED_EDGE('',*,*,#43633,.T.);
#57515=ORIENTED_EDGE('',*,*,#43634,.F.);
#57516=ORIENTED_EDGE('',*,*,#43635,.F.);
#57517=ORIENTED_EDGE('',*,*,#43636,.T.);
#57518=ORIENTED_EDGE('',*,*,#43631,.T.);
#57519=ORIENTED_EDGE('',*,*,#43637,.F.);
#57520=ORIENTED_EDGE('',*,*,#43638,.F.);
#57521=ORIENTED_EDGE('',*,*,#43639,.T.);
#57522=ORIENTED_EDGE('',*,*,#43635,.T.);
#57523=ORIENTED_EDGE('',*,*,#43640,.F.);
#57524=ORIENTED_EDGE('',*,*,#43633,.F.);
#57525=ORIENTED_EDGE('',*,*,#43641,.T.);
#57526=ORIENTED_EDGE('',*,*,#43638,.T.);
#57527=ORIENTED_EDGE('',*,*,#43642,.F.);
#57528=ORIENTED_EDGE('',*,*,#43643,.F.);
#57529=ORIENTED_EDGE('',*,*,#43644,.T.);
#57530=ORIENTED_EDGE('',*,*,#43645,.T.);
#57531=ORIENTED_EDGE('',*,*,#43646,.F.);
#57532=ORIENTED_EDGE('',*,*,#43647,.F.);
#57533=ORIENTED_EDGE('',*,*,#43648,.T.);
#57534=ORIENTED_EDGE('',*,*,#43643,.T.);
#57535=ORIENTED_EDGE('',*,*,#43649,.F.);
#57536=ORIENTED_EDGE('',*,*,#43650,.F.);
#57537=ORIENTED_EDGE('',*,*,#43651,.T.);
#57538=ORIENTED_EDGE('',*,*,#43647,.T.);
#57539=ORIENTED_EDGE('',*,*,#43652,.F.);
#57540=ORIENTED_EDGE('',*,*,#43645,.F.);
#57541=ORIENTED_EDGE('',*,*,#43653,.T.);
#57542=ORIENTED_EDGE('',*,*,#43650,.T.);
#57543=ORIENTED_EDGE('',*,*,#43654,.F.);
#57544=ORIENTED_EDGE('',*,*,#43655,.F.);
#57545=ORIENTED_EDGE('',*,*,#43656,.F.);
#57546=ORIENTED_EDGE('',*,*,#43657,.F.);
#57547=ORIENTED_EDGE('',*,*,#43658,.T.);
#57548=ORIENTED_EDGE('',*,*,#43659,.T.);
#57549=ORIENTED_EDGE('',*,*,#43660,.T.);
#57550=ORIENTED_EDGE('',*,*,#43661,.F.);
#57551=ORIENTED_EDGE('',*,*,#43658,.F.);
#57552=ORIENTED_EDGE('',*,*,#43662,.F.);
#57553=ORIENTED_EDGE('',*,*,#43663,.F.);
#57554=ORIENTED_EDGE('',*,*,#43660,.F.);
#57555=ORIENTED_EDGE('',*,*,#43664,.T.);
#57556=ORIENTED_EDGE('',*,*,#43665,.T.);
#57557=ORIENTED_EDGE('',*,*,#43656,.T.);
#57558=ORIENTED_EDGE('',*,*,#43666,.F.);
#57559=ORIENTED_EDGE('',*,*,#43665,.F.);
#57560=ORIENTED_EDGE('',*,*,#43667,.T.);
#57561=ORIENTED_EDGE('',*,*,#43668,.F.);
#57562=ORIENTED_EDGE('',*,*,#43669,.T.);
#57563=ORIENTED_EDGE('',*,*,#43662,.T.);
#57564=ORIENTED_EDGE('',*,*,#43657,.T.);
#57565=ORIENTED_EDGE('',*,*,#43668,.T.);
#57566=ORIENTED_EDGE('',*,*,#43670,.F.);
#57567=ORIENTED_EDGE('',*,*,#43671,.T.);
#57568=ORIENTED_EDGE('',*,*,#43672,.T.);
#57569=ORIENTED_EDGE('',*,*,#43673,.F.);
#57570=ORIENTED_EDGE('',*,*,#43674,.F.);
#57571=ORIENTED_EDGE('',*,*,#43675,.F.);
#57572=ORIENTED_EDGE('',*,*,#43676,.T.);
#57573=ORIENTED_EDGE('',*,*,#43670,.T.);
#57574=ORIENTED_EDGE('',*,*,#43677,.F.);
#57575=ORIENTED_EDGE('',*,*,#43678,.F.);
#57576=ORIENTED_EDGE('',*,*,#43679,.F.);
#57577=ORIENTED_EDGE('',*,*,#43674,.T.);
#57578=ORIENTED_EDGE('',*,*,#43680,.F.);
#57579=ORIENTED_EDGE('',*,*,#43672,.F.);
#57580=ORIENTED_EDGE('',*,*,#43681,.T.);
#57581=ORIENTED_EDGE('',*,*,#43682,.F.);
#57582=ORIENTED_EDGE('',*,*,#43678,.T.);
#57583=ORIENTED_EDGE('',*,*,#43683,.F.);
#57584=ORIENTED_EDGE('',*,*,#43675,.T.);
#57585=ORIENTED_EDGE('',*,*,#43679,.T.);
#57586=ORIENTED_EDGE('',*,*,#43682,.T.);
#57587=ORIENTED_EDGE('',*,*,#43684,.T.);
#57588=ORIENTED_EDGE('',*,*,#43685,.F.);
#57589=ORIENTED_EDGE('',*,*,#43686,.T.);
#57590=ORIENTED_EDGE('',*,*,#43687,.T.);
#57591=ORIENTED_EDGE('',*,*,#43688,.F.);
#57592=ORIENTED_EDGE('',*,*,#43689,.F.);
#57593=ORIENTED_EDGE('',*,*,#43690,.F.);
#57594=ORIENTED_EDGE('',*,*,#43691,.T.);
#57595=ORIENTED_EDGE('',*,*,#43685,.T.);
#57596=ORIENTED_EDGE('',*,*,#43692,.F.);
#57597=ORIENTED_EDGE('',*,*,#43693,.F.);
#57598=ORIENTED_EDGE('',*,*,#43694,.F.);
#57599=ORIENTED_EDGE('',*,*,#43689,.T.);
#57600=ORIENTED_EDGE('',*,*,#43695,.F.);
#57601=ORIENTED_EDGE('',*,*,#43687,.F.);
#57602=ORIENTED_EDGE('',*,*,#43696,.T.);
#57603=ORIENTED_EDGE('',*,*,#43697,.F.);
#57604=ORIENTED_EDGE('',*,*,#43693,.T.);
#57605=ORIENTED_EDGE('',*,*,#43698,.F.);
#57606=ORIENTED_EDGE('',*,*,#43690,.T.);
#57607=ORIENTED_EDGE('',*,*,#43694,.T.);
#57608=ORIENTED_EDGE('',*,*,#43697,.T.);
#57609=ORIENTED_EDGE('',*,*,#43699,.T.);
#57610=ORIENTED_EDGE('',*,*,#43700,.F.);
#57611=ORIENTED_EDGE('',*,*,#43701,.T.);
#57612=ORIENTED_EDGE('',*,*,#43702,.T.);
#57613=ORIENTED_EDGE('',*,*,#43703,.F.);
#57614=ORIENTED_EDGE('',*,*,#43704,.F.);
#57615=ORIENTED_EDGE('',*,*,#43705,.T.);
#57616=ORIENTED_EDGE('',*,*,#43700,.T.);
#57617=ORIENTED_EDGE('',*,*,#43706,.F.);
#57618=ORIENTED_EDGE('',*,*,#43707,.F.);
#57619=ORIENTED_EDGE('',*,*,#43708,.F.);
#57620=ORIENTED_EDGE('',*,*,#43709,.T.);
#57621=ORIENTED_EDGE('',*,*,#43704,.T.);
#57622=ORIENTED_EDGE('',*,*,#43710,.F.);
#57623=ORIENTED_EDGE('',*,*,#43702,.F.);
#57624=ORIENTED_EDGE('',*,*,#43711,.T.);
#57625=ORIENTED_EDGE('',*,*,#43712,.F.);
#57626=ORIENTED_EDGE('',*,*,#43707,.T.);
#57627=ORIENTED_EDGE('',*,*,#43713,.F.);
#57628=ORIENTED_EDGE('',*,*,#43708,.T.);
#57629=ORIENTED_EDGE('',*,*,#43712,.T.);
#57630=ORIENTED_EDGE('',*,*,#43714,.T.);
#57631=ORIENTED_EDGE('',*,*,#43715,.F.);
#57632=ORIENTED_EDGE('',*,*,#43716,.T.);
#57633=ORIENTED_EDGE('',*,*,#43717,.T.);
#57634=ORIENTED_EDGE('',*,*,#43718,.F.);
#57635=ORIENTED_EDGE('',*,*,#43719,.F.);
#57636=ORIENTED_EDGE('',*,*,#43720,.T.);
#57637=ORIENTED_EDGE('',*,*,#43715,.T.);
#57638=ORIENTED_EDGE('',*,*,#43721,.F.);
#57639=ORIENTED_EDGE('',*,*,#43722,.F.);
#57640=ORIENTED_EDGE('',*,*,#43723,.T.);
#57641=ORIENTED_EDGE('',*,*,#43719,.T.);
#57642=ORIENTED_EDGE('',*,*,#43724,.F.);
#57643=ORIENTED_EDGE('',*,*,#43717,.F.);
#57644=ORIENTED_EDGE('',*,*,#43725,.T.);
#57645=ORIENTED_EDGE('',*,*,#43722,.T.);
#57646=ORIENTED_EDGE('',*,*,#43726,.F.);
#57647=ORIENTED_EDGE('',*,*,#43727,.F.);
#57648=ORIENTED_EDGE('',*,*,#43728,.T.);
#57649=ORIENTED_EDGE('',*,*,#43729,.T.);
#57650=ORIENTED_EDGE('',*,*,#43730,.F.);
#57651=ORIENTED_EDGE('',*,*,#43731,.F.);
#57652=ORIENTED_EDGE('',*,*,#43732,.F.);
#57653=ORIENTED_EDGE('',*,*,#43733,.T.);
#57654=ORIENTED_EDGE('',*,*,#43727,.T.);
#57655=ORIENTED_EDGE('',*,*,#43734,.F.);
#57656=ORIENTED_EDGE('',*,*,#43735,.F.);
#57657=ORIENTED_EDGE('',*,*,#43736,.F.);
#57658=ORIENTED_EDGE('',*,*,#43731,.T.);
#57659=ORIENTED_EDGE('',*,*,#43737,.F.);
#57660=ORIENTED_EDGE('',*,*,#43729,.F.);
#57661=ORIENTED_EDGE('',*,*,#43738,.T.);
#57662=ORIENTED_EDGE('',*,*,#43739,.F.);
#57663=ORIENTED_EDGE('',*,*,#43735,.T.);
#57664=ORIENTED_EDGE('',*,*,#43740,.F.);
#57665=ORIENTED_EDGE('',*,*,#43732,.T.);
#57666=ORIENTED_EDGE('',*,*,#43736,.T.);
#57667=ORIENTED_EDGE('',*,*,#43739,.T.);
#57668=ORIENTED_EDGE('',*,*,#43741,.T.);
#57669=ORIENTED_EDGE('',*,*,#43742,.F.);
#57670=ORIENTED_EDGE('',*,*,#43743,.T.);
#57671=ORIENTED_EDGE('',*,*,#43744,.T.);
#57672=ORIENTED_EDGE('',*,*,#43745,.F.);
#57673=ORIENTED_EDGE('',*,*,#43746,.F.);
#57674=ORIENTED_EDGE('',*,*,#43747,.F.);
#57675=ORIENTED_EDGE('',*,*,#43748,.T.);
#57676=ORIENTED_EDGE('',*,*,#43742,.T.);
#57677=ORIENTED_EDGE('',*,*,#43749,.F.);
#57678=ORIENTED_EDGE('',*,*,#43750,.F.);
#57679=ORIENTED_EDGE('',*,*,#43751,.F.);
#57680=ORIENTED_EDGE('',*,*,#43746,.T.);
#57681=ORIENTED_EDGE('',*,*,#43752,.F.);
#57682=ORIENTED_EDGE('',*,*,#43744,.F.);
#57683=ORIENTED_EDGE('',*,*,#43753,.T.);
#57684=ORIENTED_EDGE('',*,*,#43754,.F.);
#57685=ORIENTED_EDGE('',*,*,#43750,.T.);
#57686=ORIENTED_EDGE('',*,*,#43755,.F.);
#57687=ORIENTED_EDGE('',*,*,#43747,.T.);
#57688=ORIENTED_EDGE('',*,*,#43751,.T.);
#57689=ORIENTED_EDGE('',*,*,#43754,.T.);
#57690=ORIENTED_EDGE('',*,*,#43756,.T.);
#57691=ORIENTED_EDGE('',*,*,#43757,.F.);
#57692=ORIENTED_EDGE('',*,*,#43758,.T.);
#57693=ORIENTED_EDGE('',*,*,#43759,.T.);
#57694=ORIENTED_EDGE('',*,*,#43760,.F.);
#57695=ORIENTED_EDGE('',*,*,#43761,.F.);
#57696=ORIENTED_EDGE('',*,*,#43762,.F.);
#57697=ORIENTED_EDGE('',*,*,#43763,.T.);
#57698=ORIENTED_EDGE('',*,*,#43757,.T.);
#57699=ORIENTED_EDGE('',*,*,#43764,.F.);
#57700=ORIENTED_EDGE('',*,*,#43765,.F.);
#57701=ORIENTED_EDGE('',*,*,#43766,.F.);
#57702=ORIENTED_EDGE('',*,*,#43761,.T.);
#57703=ORIENTED_EDGE('',*,*,#43767,.F.);
#57704=ORIENTED_EDGE('',*,*,#43759,.F.);
#57705=ORIENTED_EDGE('',*,*,#43768,.T.);
#57706=ORIENTED_EDGE('',*,*,#43769,.F.);
#57707=ORIENTED_EDGE('',*,*,#43765,.T.);
#57708=ORIENTED_EDGE('',*,*,#43770,.F.);
#57709=ORIENTED_EDGE('',*,*,#43762,.T.);
#57710=ORIENTED_EDGE('',*,*,#43766,.T.);
#57711=ORIENTED_EDGE('',*,*,#43769,.T.);
#57712=ORIENTED_EDGE('',*,*,#43771,.T.);
#57713=ORIENTED_EDGE('',*,*,#43772,.F.);
#57714=ORIENTED_EDGE('',*,*,#43773,.T.);
#57715=ORIENTED_EDGE('',*,*,#43774,.T.);
#57716=ORIENTED_EDGE('',*,*,#43775,.F.);
#57717=ORIENTED_EDGE('',*,*,#43776,.F.);
#57718=ORIENTED_EDGE('',*,*,#43777,.F.);
#57719=ORIENTED_EDGE('',*,*,#43778,.T.);
#57720=ORIENTED_EDGE('',*,*,#43772,.T.);
#57721=ORIENTED_EDGE('',*,*,#43779,.F.);
#57722=ORIENTED_EDGE('',*,*,#43780,.F.);
#57723=ORIENTED_EDGE('',*,*,#43781,.F.);
#57724=ORIENTED_EDGE('',*,*,#43776,.T.);
#57725=ORIENTED_EDGE('',*,*,#43782,.F.);
#57726=ORIENTED_EDGE('',*,*,#43774,.F.);
#57727=ORIENTED_EDGE('',*,*,#43783,.T.);
#57728=ORIENTED_EDGE('',*,*,#43784,.F.);
#57729=ORIENTED_EDGE('',*,*,#43780,.T.);
#57730=ORIENTED_EDGE('',*,*,#43785,.F.);
#57731=ORIENTED_EDGE('',*,*,#43777,.T.);
#57732=ORIENTED_EDGE('',*,*,#43781,.T.);
#57733=ORIENTED_EDGE('',*,*,#43784,.T.);
#57734=ORIENTED_EDGE('',*,*,#43786,.T.);
#57735=ORIENTED_EDGE('',*,*,#43787,.F.);
#57736=ORIENTED_EDGE('',*,*,#43788,.T.);
#57737=ORIENTED_EDGE('',*,*,#43789,.T.);
#57738=ORIENTED_EDGE('',*,*,#43790,.F.);
#57739=ORIENTED_EDGE('',*,*,#43791,.F.);
#57740=ORIENTED_EDGE('',*,*,#43792,.T.);
#57741=ORIENTED_EDGE('',*,*,#43787,.T.);
#57742=ORIENTED_EDGE('',*,*,#43793,.F.);
#57743=ORIENTED_EDGE('',*,*,#43794,.F.);
#57744=ORIENTED_EDGE('',*,*,#43795,.T.);
#57745=ORIENTED_EDGE('',*,*,#43791,.T.);
#57746=ORIENTED_EDGE('',*,*,#43796,.F.);
#57747=ORIENTED_EDGE('',*,*,#43789,.F.);
#57748=ORIENTED_EDGE('',*,*,#43797,.T.);
#57749=ORIENTED_EDGE('',*,*,#43794,.T.);
#57750=ORIENTED_EDGE('',*,*,#43798,.F.);
#57751=ORIENTED_EDGE('',*,*,#43799,.F.);
#57752=ORIENTED_EDGE('',*,*,#43800,.T.);
#57753=ORIENTED_EDGE('',*,*,#43801,.T.);
#57754=ORIENTED_EDGE('',*,*,#43802,.F.);
#57755=ORIENTED_EDGE('',*,*,#43803,.F.);
#57756=ORIENTED_EDGE('',*,*,#43804,.T.);
#57757=ORIENTED_EDGE('',*,*,#43799,.T.);
#57758=ORIENTED_EDGE('',*,*,#43805,.F.);
#57759=ORIENTED_EDGE('',*,*,#43806,.F.);
#57760=ORIENTED_EDGE('',*,*,#43807,.T.);
#57761=ORIENTED_EDGE('',*,*,#43803,.T.);
#57762=ORIENTED_EDGE('',*,*,#43808,.F.);
#57763=ORIENTED_EDGE('',*,*,#43801,.F.);
#57764=ORIENTED_EDGE('',*,*,#43809,.T.);
#57765=ORIENTED_EDGE('',*,*,#43806,.T.);
#57766=ORIENTED_EDGE('',*,*,#43810,.F.);
#57767=ORIENTED_EDGE('',*,*,#43811,.F.);
#57768=ORIENTED_EDGE('',*,*,#43812,.T.);
#57769=ORIENTED_EDGE('',*,*,#43813,.T.);
#57770=ORIENTED_EDGE('',*,*,#43814,.F.);
#57771=ORIENTED_EDGE('',*,*,#43815,.F.);
#57772=ORIENTED_EDGE('',*,*,#43816,.T.);
#57773=ORIENTED_EDGE('',*,*,#43811,.T.);
#57774=ORIENTED_EDGE('',*,*,#43817,.F.);
#57775=ORIENTED_EDGE('',*,*,#43818,.F.);
#57776=ORIENTED_EDGE('',*,*,#43819,.T.);
#57777=ORIENTED_EDGE('',*,*,#43815,.T.);
#57778=ORIENTED_EDGE('',*,*,#43820,.F.);
#57779=ORIENTED_EDGE('',*,*,#43813,.F.);
#57780=ORIENTED_EDGE('',*,*,#43821,.T.);
#57781=ORIENTED_EDGE('',*,*,#43818,.T.);
#57782=ORIENTED_EDGE('',*,*,#43822,.F.);
#57783=ORIENTED_EDGE('',*,*,#43823,.F.);
#57784=ORIENTED_EDGE('',*,*,#43824,.T.);
#57785=ORIENTED_EDGE('',*,*,#43825,.T.);
#57786=ORIENTED_EDGE('',*,*,#43826,.F.);
#57787=ORIENTED_EDGE('',*,*,#43827,.F.);
#57788=ORIENTED_EDGE('',*,*,#43828,.T.);
#57789=ORIENTED_EDGE('',*,*,#43823,.T.);
#57790=ORIENTED_EDGE('',*,*,#43829,.F.);
#57791=ORIENTED_EDGE('',*,*,#43830,.F.);
#57792=ORIENTED_EDGE('',*,*,#43831,.T.);
#57793=ORIENTED_EDGE('',*,*,#43827,.T.);
#57794=ORIENTED_EDGE('',*,*,#43832,.F.);
#57795=ORIENTED_EDGE('',*,*,#43825,.F.);
#57796=ORIENTED_EDGE('',*,*,#43833,.T.);
#57797=ORIENTED_EDGE('',*,*,#43830,.T.);
#57798=ORIENTED_EDGE('',*,*,#43834,.F.);
#57799=ORIENTED_EDGE('',*,*,#43835,.F.);
#57800=ORIENTED_EDGE('',*,*,#43836,.T.);
#57801=ORIENTED_EDGE('',*,*,#43837,.T.);
#57802=ORIENTED_EDGE('',*,*,#43838,.F.);
#57803=ORIENTED_EDGE('',*,*,#43839,.F.);
#57804=ORIENTED_EDGE('',*,*,#43840,.T.);
#57805=ORIENTED_EDGE('',*,*,#43835,.T.);
#57806=ORIENTED_EDGE('',*,*,#43841,.F.);
#57807=ORIENTED_EDGE('',*,*,#43842,.F.);
#57808=ORIENTED_EDGE('',*,*,#43843,.T.);
#57809=ORIENTED_EDGE('',*,*,#43839,.T.);
#57810=ORIENTED_EDGE('',*,*,#43844,.F.);
#57811=ORIENTED_EDGE('',*,*,#43837,.F.);
#57812=ORIENTED_EDGE('',*,*,#43845,.T.);
#57813=ORIENTED_EDGE('',*,*,#43842,.T.);
#57814=ORIENTED_EDGE('',*,*,#43846,.F.);
#57815=ORIENTED_EDGE('',*,*,#43847,.F.);
#57816=ORIENTED_EDGE('',*,*,#43848,.T.);
#57817=ORIENTED_EDGE('',*,*,#43849,.T.);
#57818=ORIENTED_EDGE('',*,*,#43850,.F.);
#57819=ORIENTED_EDGE('',*,*,#43851,.F.);
#57820=ORIENTED_EDGE('',*,*,#43852,.T.);
#57821=ORIENTED_EDGE('',*,*,#43847,.T.);
#57822=ORIENTED_EDGE('',*,*,#43853,.F.);
#57823=ORIENTED_EDGE('',*,*,#43854,.F.);
#57824=ORIENTED_EDGE('',*,*,#43855,.T.);
#57825=ORIENTED_EDGE('',*,*,#43851,.T.);
#57826=ORIENTED_EDGE('',*,*,#43856,.F.);
#57827=ORIENTED_EDGE('',*,*,#43849,.F.);
#57828=ORIENTED_EDGE('',*,*,#43857,.T.);
#57829=ORIENTED_EDGE('',*,*,#43854,.T.);
#57830=ORIENTED_EDGE('',*,*,#43858,.F.);
#57831=ORIENTED_EDGE('',*,*,#43859,.F.);
#57832=ORIENTED_EDGE('',*,*,#43860,.F.);
#57833=ORIENTED_EDGE('',*,*,#43861,.T.);
#57834=ORIENTED_EDGE('',*,*,#43862,.T.);
#57835=ORIENTED_EDGE('',*,*,#43863,.F.);
#57836=ORIENTED_EDGE('',*,*,#43864,.F.);
#57837=ORIENTED_EDGE('',*,*,#43865,.T.);
#57838=ORIENTED_EDGE('',*,*,#43860,.T.);
#57839=ORIENTED_EDGE('',*,*,#43866,.F.);
#57840=ORIENTED_EDGE('',*,*,#43867,.T.);
#57841=ORIENTED_EDGE('',*,*,#43864,.T.);
#57842=ORIENTED_EDGE('',*,*,#43868,.F.);
#57843=ORIENTED_EDGE('',*,*,#43869,.F.);
#57844=ORIENTED_EDGE('',*,*,#43870,.F.);
#57845=ORIENTED_EDGE('',*,*,#43862,.F.);
#57846=ORIENTED_EDGE('',*,*,#43871,.T.);
#57847=ORIENTED_EDGE('',*,*,#43872,.F.);
#57848=ORIENTED_EDGE('',*,*,#43869,.T.);
#57849=ORIENTED_EDGE('',*,*,#43866,.T.);
#57850=ORIENTED_EDGE('',*,*,#43872,.T.);
#57851=ORIENTED_EDGE('',*,*,#43873,.T.);
#57852=ORIENTED_EDGE('',*,*,#43874,.F.);
#57853=ORIENTED_EDGE('',*,*,#43875,.T.);
#57854=ORIENTED_EDGE('',*,*,#43876,.T.);
#57855=ORIENTED_EDGE('',*,*,#43877,.F.);
#57856=ORIENTED_EDGE('',*,*,#43878,.F.);
#57857=ORIENTED_EDGE('',*,*,#43879,.F.);
#57858=ORIENTED_EDGE('',*,*,#43880,.T.);
#57859=ORIENTED_EDGE('',*,*,#43874,.T.);
#57860=ORIENTED_EDGE('',*,*,#43881,.F.);
#57861=ORIENTED_EDGE('',*,*,#43882,.F.);
#57862=ORIENTED_EDGE('',*,*,#43883,.F.);
#57863=ORIENTED_EDGE('',*,*,#43878,.T.);
#57864=ORIENTED_EDGE('',*,*,#43884,.F.);
#57865=ORIENTED_EDGE('',*,*,#43876,.F.);
#57866=ORIENTED_EDGE('',*,*,#43885,.T.);
#57867=ORIENTED_EDGE('',*,*,#43886,.F.);
#57868=ORIENTED_EDGE('',*,*,#43882,.T.);
#57869=ORIENTED_EDGE('',*,*,#43887,.F.);
#57870=ORIENTED_EDGE('',*,*,#43879,.T.);
#57871=ORIENTED_EDGE('',*,*,#43883,.T.);
#57872=ORIENTED_EDGE('',*,*,#43886,.T.);
#57873=ORIENTED_EDGE('',*,*,#43888,.T.);
#57874=ORIENTED_EDGE('',*,*,#43889,.F.);
#57875=ORIENTED_EDGE('',*,*,#43890,.T.);
#57876=ORIENTED_EDGE('',*,*,#43891,.T.);
#57877=ORIENTED_EDGE('',*,*,#43892,.F.);
#57878=ORIENTED_EDGE('',*,*,#43893,.F.);
#57879=ORIENTED_EDGE('',*,*,#43894,.T.);
#57880=ORIENTED_EDGE('',*,*,#43889,.T.);
#57881=ORIENTED_EDGE('',*,*,#43895,.F.);
#57882=ORIENTED_EDGE('',*,*,#43896,.F.);
#57883=ORIENTED_EDGE('',*,*,#43897,.T.);
#57884=ORIENTED_EDGE('',*,*,#43893,.T.);
#57885=ORIENTED_EDGE('',*,*,#43898,.F.);
#57886=ORIENTED_EDGE('',*,*,#43891,.F.);
#57887=ORIENTED_EDGE('',*,*,#43899,.T.);
#57888=ORIENTED_EDGE('',*,*,#43896,.T.);
#57889=ORIENTED_EDGE('',*,*,#43900,.F.);
#57890=ORIENTED_EDGE('',*,*,#43901,.F.);
#57891=ORIENTED_EDGE('',*,*,#43902,.T.);
#57892=ORIENTED_EDGE('',*,*,#43903,.T.);
#57893=ORIENTED_EDGE('',*,*,#43904,.F.);
#57894=ORIENTED_EDGE('',*,*,#43905,.F.);
#57895=ORIENTED_EDGE('',*,*,#43906,.T.);
#57896=ORIENTED_EDGE('',*,*,#43901,.T.);
#57897=ORIENTED_EDGE('',*,*,#43907,.F.);
#57898=ORIENTED_EDGE('',*,*,#43908,.F.);
#57899=ORIENTED_EDGE('',*,*,#43909,.T.);
#57900=ORIENTED_EDGE('',*,*,#43905,.T.);
#57901=ORIENTED_EDGE('',*,*,#43910,.F.);
#57902=ORIENTED_EDGE('',*,*,#43903,.F.);
#57903=ORIENTED_EDGE('',*,*,#43911,.T.);
#57904=ORIENTED_EDGE('',*,*,#43908,.T.);
#57905=ORIENTED_EDGE('',*,*,#43912,.F.);
#57906=ORIENTED_EDGE('',*,*,#43913,.F.);
#57907=ORIENTED_EDGE('',*,*,#43914,.T.);
#57908=ORIENTED_EDGE('',*,*,#43915,.T.);
#57909=ORIENTED_EDGE('',*,*,#43916,.F.);
#57910=ORIENTED_EDGE('',*,*,#43917,.F.);
#57911=ORIENTED_EDGE('',*,*,#43918,.T.);
#57912=ORIENTED_EDGE('',*,*,#43913,.T.);
#57913=ORIENTED_EDGE('',*,*,#43919,.F.);
#57914=ORIENTED_EDGE('',*,*,#43920,.F.);
#57915=ORIENTED_EDGE('',*,*,#43921,.T.);
#57916=ORIENTED_EDGE('',*,*,#43917,.T.);
#57917=ORIENTED_EDGE('',*,*,#43922,.F.);
#57918=ORIENTED_EDGE('',*,*,#43915,.F.);
#57919=ORIENTED_EDGE('',*,*,#43923,.T.);
#57920=ORIENTED_EDGE('',*,*,#43920,.T.);
#57921=ORIENTED_EDGE('',*,*,#43924,.F.);
#57922=ORIENTED_EDGE('',*,*,#43925,.F.);
#57923=ORIENTED_EDGE('',*,*,#43926,.T.);
#57924=ORIENTED_EDGE('',*,*,#43927,.T.);
#57925=ORIENTED_EDGE('',*,*,#43928,.F.);
#57926=ORIENTED_EDGE('',*,*,#43929,.F.);
#57927=ORIENTED_EDGE('',*,*,#43930,.T.);
#57928=ORIENTED_EDGE('',*,*,#43925,.T.);
#57929=ORIENTED_EDGE('',*,*,#43931,.F.);
#57930=ORIENTED_EDGE('',*,*,#43932,.F.);
#57931=ORIENTED_EDGE('',*,*,#43933,.T.);
#57932=ORIENTED_EDGE('',*,*,#43929,.T.);
#57933=ORIENTED_EDGE('',*,*,#43934,.F.);
#57934=ORIENTED_EDGE('',*,*,#43927,.F.);
#57935=ORIENTED_EDGE('',*,*,#43935,.T.);
#57936=ORIENTED_EDGE('',*,*,#43932,.T.);
#57937=ORIENTED_EDGE('',*,*,#43936,.F.);
#57938=ORIENTED_EDGE('',*,*,#43937,.F.);
#57939=ORIENTED_EDGE('',*,*,#43938,.T.);
#57940=ORIENTED_EDGE('',*,*,#43939,.T.);
#57941=ORIENTED_EDGE('',*,*,#43940,.F.);
#57942=ORIENTED_EDGE('',*,*,#43941,.F.);
#57943=ORIENTED_EDGE('',*,*,#43942,.T.);
#57944=ORIENTED_EDGE('',*,*,#43937,.T.);
#57945=ORIENTED_EDGE('',*,*,#43943,.F.);
#57946=ORIENTED_EDGE('',*,*,#43944,.F.);
#57947=ORIENTED_EDGE('',*,*,#43945,.T.);
#57948=ORIENTED_EDGE('',*,*,#43941,.T.);
#57949=ORIENTED_EDGE('',*,*,#43946,.F.);
#57950=ORIENTED_EDGE('',*,*,#43939,.F.);
#57951=ORIENTED_EDGE('',*,*,#43947,.T.);
#57952=ORIENTED_EDGE('',*,*,#43944,.T.);
#57953=ORIENTED_EDGE('',*,*,#43948,.F.);
#57954=ORIENTED_EDGE('',*,*,#43949,.F.);
#57955=ORIENTED_EDGE('',*,*,#43950,.T.);
#57956=ORIENTED_EDGE('',*,*,#43951,.T.);
#57957=ORIENTED_EDGE('',*,*,#43952,.F.);
#57958=ORIENTED_EDGE('',*,*,#43953,.F.);
#57959=ORIENTED_EDGE('',*,*,#43954,.T.);
#57960=ORIENTED_EDGE('',*,*,#43949,.T.);
#57961=ORIENTED_EDGE('',*,*,#43955,.F.);
#57962=ORIENTED_EDGE('',*,*,#43956,.F.);
#57963=ORIENTED_EDGE('',*,*,#43957,.T.);
#57964=ORIENTED_EDGE('',*,*,#43953,.T.);
#57965=ORIENTED_EDGE('',*,*,#43958,.F.);
#57966=ORIENTED_EDGE('',*,*,#43951,.F.);
#57967=ORIENTED_EDGE('',*,*,#43959,.T.);
#57968=ORIENTED_EDGE('',*,*,#43956,.T.);
#57969=ORIENTED_EDGE('',*,*,#43960,.F.);
#57970=ORIENTED_EDGE('',*,*,#43961,.F.);
#57971=ORIENTED_EDGE('',*,*,#43962,.T.);
#57972=ORIENTED_EDGE('',*,*,#43963,.T.);
#57973=ORIENTED_EDGE('',*,*,#43964,.F.);
#57974=ORIENTED_EDGE('',*,*,#43965,.F.);
#57975=ORIENTED_EDGE('',*,*,#43966,.T.);
#57976=ORIENTED_EDGE('',*,*,#43961,.T.);
#57977=ORIENTED_EDGE('',*,*,#43967,.F.);
#57978=ORIENTED_EDGE('',*,*,#43968,.F.);
#57979=ORIENTED_EDGE('',*,*,#43969,.T.);
#57980=ORIENTED_EDGE('',*,*,#43965,.T.);
#57981=ORIENTED_EDGE('',*,*,#43970,.F.);
#57982=ORIENTED_EDGE('',*,*,#43963,.F.);
#57983=ORIENTED_EDGE('',*,*,#43971,.T.);
#57984=ORIENTED_EDGE('',*,*,#43968,.T.);
#57985=ORIENTED_EDGE('',*,*,#43972,.F.);
#57986=ORIENTED_EDGE('',*,*,#43973,.F.);
#57987=ORIENTED_EDGE('',*,*,#43974,.T.);
#57988=ORIENTED_EDGE('',*,*,#43975,.T.);
#57989=ORIENTED_EDGE('',*,*,#43976,.F.);
#57990=ORIENTED_EDGE('',*,*,#43977,.F.);
#57991=ORIENTED_EDGE('',*,*,#43978,.T.);
#57992=ORIENTED_EDGE('',*,*,#43973,.T.);
#57993=ORIENTED_EDGE('',*,*,#43979,.F.);
#57994=ORIENTED_EDGE('',*,*,#43980,.F.);
#57995=ORIENTED_EDGE('',*,*,#43981,.T.);
#57996=ORIENTED_EDGE('',*,*,#43977,.T.);
#57997=ORIENTED_EDGE('',*,*,#43982,.F.);
#57998=ORIENTED_EDGE('',*,*,#43975,.F.);
#57999=ORIENTED_EDGE('',*,*,#43983,.T.);
#58000=ORIENTED_EDGE('',*,*,#43980,.T.);
#58001=ORIENTED_EDGE('',*,*,#43984,.F.);
#58002=ORIENTED_EDGE('',*,*,#43985,.F.);
#58003=ORIENTED_EDGE('',*,*,#43986,.T.);
#58004=ORIENTED_EDGE('',*,*,#43987,.T.);
#58005=ORIENTED_EDGE('',*,*,#43988,.F.);
#58006=ORIENTED_EDGE('',*,*,#43989,.F.);
#58007=ORIENTED_EDGE('',*,*,#43990,.F.);
#58008=ORIENTED_EDGE('',*,*,#43991,.T.);
#58009=ORIENTED_EDGE('',*,*,#43985,.T.);
#58010=ORIENTED_EDGE('',*,*,#43992,.F.);
#58011=ORIENTED_EDGE('',*,*,#43993,.F.);
#58012=ORIENTED_EDGE('',*,*,#43994,.F.);
#58013=ORIENTED_EDGE('',*,*,#43989,.T.);
#58014=ORIENTED_EDGE('',*,*,#43995,.F.);
#58015=ORIENTED_EDGE('',*,*,#43987,.F.);
#58016=ORIENTED_EDGE('',*,*,#43996,.T.);
#58017=ORIENTED_EDGE('',*,*,#43997,.F.);
#58018=ORIENTED_EDGE('',*,*,#43993,.T.);
#58019=ORIENTED_EDGE('',*,*,#43998,.F.);
#58020=ORIENTED_EDGE('',*,*,#43990,.T.);
#58021=ORIENTED_EDGE('',*,*,#43994,.T.);
#58022=ORIENTED_EDGE('',*,*,#43997,.T.);
#58023=ORIENTED_EDGE('',*,*,#43999,.T.);
#58024=ORIENTED_EDGE('',*,*,#44000,.F.);
#58025=ORIENTED_EDGE('',*,*,#44001,.T.);
#58026=ORIENTED_EDGE('',*,*,#44002,.T.);
#58027=ORIENTED_EDGE('',*,*,#44003,.F.);
#58028=ORIENTED_EDGE('',*,*,#44004,.F.);
#58029=ORIENTED_EDGE('',*,*,#44005,.F.);
#58030=ORIENTED_EDGE('',*,*,#44006,.T.);
#58031=ORIENTED_EDGE('',*,*,#44000,.T.);
#58032=ORIENTED_EDGE('',*,*,#44007,.F.);
#58033=ORIENTED_EDGE('',*,*,#44008,.F.);
#58034=ORIENTED_EDGE('',*,*,#44009,.F.);
#58035=ORIENTED_EDGE('',*,*,#44004,.T.);
#58036=ORIENTED_EDGE('',*,*,#44010,.F.);
#58037=ORIENTED_EDGE('',*,*,#44002,.F.);
#58038=ORIENTED_EDGE('',*,*,#44011,.T.);
#58039=ORIENTED_EDGE('',*,*,#44012,.F.);
#58040=ORIENTED_EDGE('',*,*,#44008,.T.);
#58041=ORIENTED_EDGE('',*,*,#44013,.F.);
#58042=ORIENTED_EDGE('',*,*,#44005,.T.);
#58043=ORIENTED_EDGE('',*,*,#44009,.T.);
#58044=ORIENTED_EDGE('',*,*,#44012,.T.);
#58045=ORIENTED_EDGE('',*,*,#44014,.T.);
#58046=ORIENTED_EDGE('',*,*,#44015,.F.);
#58047=ORIENTED_EDGE('',*,*,#44016,.T.);
#58048=ORIENTED_EDGE('',*,*,#44017,.T.);
#58049=ORIENTED_EDGE('',*,*,#44018,.F.);
#58050=ORIENTED_EDGE('',*,*,#44019,.F.);
#58051=ORIENTED_EDGE('',*,*,#44020,.T.);
#58052=ORIENTED_EDGE('',*,*,#44015,.T.);
#58053=ORIENTED_EDGE('',*,*,#44021,.F.);
#58054=ORIENTED_EDGE('',*,*,#44022,.F.);
#58055=ORIENTED_EDGE('',*,*,#44023,.T.);
#58056=ORIENTED_EDGE('',*,*,#44019,.T.);
#58057=ORIENTED_EDGE('',*,*,#44024,.F.);
#58058=ORIENTED_EDGE('',*,*,#44017,.F.);
#58059=ORIENTED_EDGE('',*,*,#44025,.T.);
#58060=ORIENTED_EDGE('',*,*,#44022,.T.);
#58061=ORIENTED_EDGE('',*,*,#44026,.F.);
#58062=ORIENTED_EDGE('',*,*,#44027,.F.);
#58063=ORIENTED_EDGE('',*,*,#44028,.T.);
#58064=ORIENTED_EDGE('',*,*,#44029,.T.);
#58065=ORIENTED_EDGE('',*,*,#44030,.F.);
#58066=ORIENTED_EDGE('',*,*,#44031,.F.);
#58067=ORIENTED_EDGE('',*,*,#44032,.T.);
#58068=ORIENTED_EDGE('',*,*,#44027,.T.);
#58069=ORIENTED_EDGE('',*,*,#44033,.F.);
#58070=ORIENTED_EDGE('',*,*,#44034,.F.);
#58071=ORIENTED_EDGE('',*,*,#44035,.T.);
#58072=ORIENTED_EDGE('',*,*,#44031,.T.);
#58073=ORIENTED_EDGE('',*,*,#44036,.F.);
#58074=ORIENTED_EDGE('',*,*,#44029,.F.);
#58075=ORIENTED_EDGE('',*,*,#44037,.T.);
#58076=ORIENTED_EDGE('',*,*,#44034,.T.);
#58077=ORIENTED_EDGE('',*,*,#44038,.F.);
#58078=ORIENTED_EDGE('',*,*,#44039,.F.);
#58079=ORIENTED_EDGE('',*,*,#44040,.T.);
#58080=ORIENTED_EDGE('',*,*,#44041,.T.);
#58081=ORIENTED_EDGE('',*,*,#44042,.F.);
#58082=ORIENTED_EDGE('',*,*,#44043,.F.);
#58083=ORIENTED_EDGE('',*,*,#44044,.T.);
#58084=ORIENTED_EDGE('',*,*,#44039,.T.);
#58085=ORIENTED_EDGE('',*,*,#44045,.F.);
#58086=ORIENTED_EDGE('',*,*,#44046,.F.);
#58087=ORIENTED_EDGE('',*,*,#44047,.T.);
#58088=ORIENTED_EDGE('',*,*,#44043,.T.);
#58089=ORIENTED_EDGE('',*,*,#44048,.F.);
#58090=ORIENTED_EDGE('',*,*,#44041,.F.);
#58091=ORIENTED_EDGE('',*,*,#44049,.T.);
#58092=ORIENTED_EDGE('',*,*,#44046,.T.);
#58093=ORIENTED_EDGE('',*,*,#44050,.F.);
#58094=ORIENTED_EDGE('',*,*,#44051,.F.);
#58095=ORIENTED_EDGE('',*,*,#44052,.T.);
#58096=ORIENTED_EDGE('',*,*,#44053,.T.);
#58097=ORIENTED_EDGE('',*,*,#44054,.F.);
#58098=ORIENTED_EDGE('',*,*,#44055,.F.);
#58099=ORIENTED_EDGE('',*,*,#44056,.T.);
#58100=ORIENTED_EDGE('',*,*,#44051,.T.);
#58101=ORIENTED_EDGE('',*,*,#44057,.F.);
#58102=ORIENTED_EDGE('',*,*,#44058,.F.);
#58103=ORIENTED_EDGE('',*,*,#44059,.T.);
#58104=ORIENTED_EDGE('',*,*,#44055,.T.);
#58105=ORIENTED_EDGE('',*,*,#44060,.F.);
#58106=ORIENTED_EDGE('',*,*,#44053,.F.);
#58107=ORIENTED_EDGE('',*,*,#44061,.T.);
#58108=ORIENTED_EDGE('',*,*,#44058,.T.);
#58109=ORIENTED_EDGE('',*,*,#44062,.F.);
#58110=ORIENTED_EDGE('',*,*,#44063,.F.);
#58111=ORIENTED_EDGE('',*,*,#44064,.T.);
#58112=ORIENTED_EDGE('',*,*,#44065,.T.);
#58113=ORIENTED_EDGE('',*,*,#44066,.F.);
#58114=ORIENTED_EDGE('',*,*,#44067,.F.);
#58115=ORIENTED_EDGE('',*,*,#44068,.T.);
#58116=ORIENTED_EDGE('',*,*,#44063,.T.);
#58117=ORIENTED_EDGE('',*,*,#44069,.F.);
#58118=ORIENTED_EDGE('',*,*,#44070,.F.);
#58119=ORIENTED_EDGE('',*,*,#44071,.T.);
#58120=ORIENTED_EDGE('',*,*,#44067,.T.);
#58121=ORIENTED_EDGE('',*,*,#44072,.F.);
#58122=ORIENTED_EDGE('',*,*,#44065,.F.);
#58123=ORIENTED_EDGE('',*,*,#44073,.T.);
#58124=ORIENTED_EDGE('',*,*,#44070,.T.);
#58125=ORIENTED_EDGE('',*,*,#44074,.F.);
#58126=ORIENTED_EDGE('',*,*,#44075,.F.);
#58127=ORIENTED_EDGE('',*,*,#44076,.T.);
#58128=ORIENTED_EDGE('',*,*,#44077,.T.);
#58129=ORIENTED_EDGE('',*,*,#44078,.F.);
#58130=ORIENTED_EDGE('',*,*,#44079,.F.);
#58131=ORIENTED_EDGE('',*,*,#44080,.T.);
#58132=ORIENTED_EDGE('',*,*,#44075,.T.);
#58133=ORIENTED_EDGE('',*,*,#44081,.F.);
#58134=ORIENTED_EDGE('',*,*,#44082,.F.);
#58135=ORIENTED_EDGE('',*,*,#44083,.T.);
#58136=ORIENTED_EDGE('',*,*,#44079,.T.);
#58137=ORIENTED_EDGE('',*,*,#44084,.F.);
#58138=ORIENTED_EDGE('',*,*,#44077,.F.);
#58139=ORIENTED_EDGE('',*,*,#44085,.T.);
#58140=ORIENTED_EDGE('',*,*,#44082,.T.);
#58141=ORIENTED_EDGE('',*,*,#44086,.F.);
#58142=ORIENTED_EDGE('',*,*,#44087,.F.);
#58143=ORIENTED_EDGE('',*,*,#44088,.T.);
#58144=ORIENTED_EDGE('',*,*,#44089,.T.);
#58145=ORIENTED_EDGE('',*,*,#44090,.F.);
#58146=ORIENTED_EDGE('',*,*,#44091,.F.);
#58147=ORIENTED_EDGE('',*,*,#44092,.T.);
#58148=ORIENTED_EDGE('',*,*,#44087,.T.);
#58149=ORIENTED_EDGE('',*,*,#44093,.F.);
#58150=ORIENTED_EDGE('',*,*,#44094,.F.);
#58151=ORIENTED_EDGE('',*,*,#44095,.T.);
#58152=ORIENTED_EDGE('',*,*,#44091,.T.);
#58153=ORIENTED_EDGE('',*,*,#44096,.F.);
#58154=ORIENTED_EDGE('',*,*,#44089,.F.);
#58155=ORIENTED_EDGE('',*,*,#44097,.T.);
#58156=ORIENTED_EDGE('',*,*,#44094,.T.);
#58157=ORIENTED_EDGE('',*,*,#44098,.F.);
#58158=ORIENTED_EDGE('',*,*,#44099,.F.);
#58159=ORIENTED_EDGE('',*,*,#44100,.T.);
#58160=ORIENTED_EDGE('',*,*,#44101,.T.);
#58161=ORIENTED_EDGE('',*,*,#44102,.F.);
#58162=ORIENTED_EDGE('',*,*,#44103,.F.);
#58163=ORIENTED_EDGE('',*,*,#44104,.T.);
#58164=ORIENTED_EDGE('',*,*,#44099,.T.);
#58165=ORIENTED_EDGE('',*,*,#44105,.F.);
#58166=ORIENTED_EDGE('',*,*,#44106,.F.);
#58167=ORIENTED_EDGE('',*,*,#44107,.T.);
#58168=ORIENTED_EDGE('',*,*,#44103,.T.);
#58169=ORIENTED_EDGE('',*,*,#44108,.F.);
#58170=ORIENTED_EDGE('',*,*,#44101,.F.);
#58171=ORIENTED_EDGE('',*,*,#44109,.T.);
#58172=ORIENTED_EDGE('',*,*,#44106,.T.);
#58173=ORIENTED_EDGE('',*,*,#44110,.F.);
#58174=ORIENTED_EDGE('',*,*,#44111,.F.);
#58175=ORIENTED_EDGE('',*,*,#44112,.T.);
#58176=ORIENTED_EDGE('',*,*,#44113,.T.);
#58177=ORIENTED_EDGE('',*,*,#44114,.F.);
#58178=ORIENTED_EDGE('',*,*,#44115,.F.);
#58179=ORIENTED_EDGE('',*,*,#44116,.T.);
#58180=ORIENTED_EDGE('',*,*,#44111,.T.);
#58181=ORIENTED_EDGE('',*,*,#44117,.F.);
#58182=ORIENTED_EDGE('',*,*,#44118,.F.);
#58183=ORIENTED_EDGE('',*,*,#44119,.T.);
#58184=ORIENTED_EDGE('',*,*,#44115,.T.);
#58185=ORIENTED_EDGE('',*,*,#44120,.F.);
#58186=ORIENTED_EDGE('',*,*,#44113,.F.);
#58187=ORIENTED_EDGE('',*,*,#44121,.T.);
#58188=ORIENTED_EDGE('',*,*,#44118,.T.);
#58189=ORIENTED_EDGE('',*,*,#44122,.F.);
#58190=ORIENTED_EDGE('',*,*,#44123,.F.);
#58191=ORIENTED_EDGE('',*,*,#44124,.T.);
#58192=ORIENTED_EDGE('',*,*,#44125,.T.);
#58193=ORIENTED_EDGE('',*,*,#44126,.F.);
#58194=ORIENTED_EDGE('',*,*,#44127,.F.);
#58195=ORIENTED_EDGE('',*,*,#44128,.T.);
#58196=ORIENTED_EDGE('',*,*,#44123,.T.);
#58197=ORIENTED_EDGE('',*,*,#44129,.F.);
#58198=ORIENTED_EDGE('',*,*,#44130,.F.);
#58199=ORIENTED_EDGE('',*,*,#44131,.T.);
#58200=ORIENTED_EDGE('',*,*,#44127,.T.);
#58201=ORIENTED_EDGE('',*,*,#44132,.F.);
#58202=ORIENTED_EDGE('',*,*,#44125,.F.);
#58203=ORIENTED_EDGE('',*,*,#44133,.T.);
#58204=ORIENTED_EDGE('',*,*,#44130,.T.);
#58205=ORIENTED_EDGE('',*,*,#44134,.F.);
#58206=ORIENTED_EDGE('',*,*,#44135,.T.);
#58207=ORIENTED_EDGE('',*,*,#44136,.T.);
#58208=ORIENTED_EDGE('',*,*,#44137,.T.);
#58209=ORIENTED_EDGE('',*,*,#44138,.F.);
#58210=ORIENTED_EDGE('',*,*,#44139,.T.);
#58211=ORIENTED_EDGE('',*,*,#44140,.T.);
#58212=ORIENTED_EDGE('',*,*,#44141,.F.);
#58213=ORIENTED_EDGE('',*,*,#44142,.F.);
#58214=ORIENTED_EDGE('',*,*,#44143,.T.);
#58215=ORIENTED_EDGE('',*,*,#44138,.T.);
#58216=ORIENTED_EDGE('',*,*,#44144,.F.);
#58217=ORIENTED_EDGE('',*,*,#44145,.F.);
#58218=ORIENTED_EDGE('',*,*,#44135,.F.);
#58219=ORIENTED_EDGE('',*,*,#44146,.T.);
#58220=ORIENTED_EDGE('',*,*,#44142,.T.);
#58221=ORIENTED_EDGE('',*,*,#44147,.F.);
#58222=ORIENTED_EDGE('',*,*,#44140,.F.);
#58223=ORIENTED_EDGE('',*,*,#44148,.T.);
#58224=ORIENTED_EDGE('',*,*,#44136,.F.);
#58225=ORIENTED_EDGE('',*,*,#44145,.T.);
#58226=ORIENTED_EDGE('',*,*,#44149,.F.);
#58227=ORIENTED_EDGE('',*,*,#44150,.F.);
#58228=ORIENTED_EDGE('',*,*,#44151,.T.);
#58229=ORIENTED_EDGE('',*,*,#44152,.T.);
#58230=ORIENTED_EDGE('',*,*,#44153,.F.);
#58231=ORIENTED_EDGE('',*,*,#44154,.F.);
#58232=ORIENTED_EDGE('',*,*,#44155,.T.);
#58233=ORIENTED_EDGE('',*,*,#44150,.T.);
#58234=ORIENTED_EDGE('',*,*,#44156,.F.);
#58235=ORIENTED_EDGE('',*,*,#44157,.F.);
#58236=ORIENTED_EDGE('',*,*,#44158,.T.);
#58237=ORIENTED_EDGE('',*,*,#44154,.T.);
#58238=ORIENTED_EDGE('',*,*,#44159,.F.);
#58239=ORIENTED_EDGE('',*,*,#44152,.F.);
#58240=ORIENTED_EDGE('',*,*,#44160,.T.);
#58241=ORIENTED_EDGE('',*,*,#44157,.T.);
#58242=ORIENTED_EDGE('',*,*,#44161,.F.);
#58243=ORIENTED_EDGE('',*,*,#44162,.F.);
#58244=ORIENTED_EDGE('',*,*,#44163,.T.);
#58245=ORIENTED_EDGE('',*,*,#44164,.T.);
#58246=ORIENTED_EDGE('',*,*,#44165,.F.);
#58247=ORIENTED_EDGE('',*,*,#44166,.F.);
#58248=ORIENTED_EDGE('',*,*,#44167,.T.);
#58249=ORIENTED_EDGE('',*,*,#44162,.T.);
#58250=ORIENTED_EDGE('',*,*,#44168,.F.);
#58251=ORIENTED_EDGE('',*,*,#44169,.F.);
#58252=ORIENTED_EDGE('',*,*,#44170,.T.);
#58253=ORIENTED_EDGE('',*,*,#44166,.T.);
#58254=ORIENTED_EDGE('',*,*,#44171,.F.);
#58255=ORIENTED_EDGE('',*,*,#44164,.F.);
#58256=ORIENTED_EDGE('',*,*,#44172,.T.);
#58257=ORIENTED_EDGE('',*,*,#44169,.T.);
#58258=ORIENTED_EDGE('',*,*,#44173,.F.);
#58259=ORIENTED_EDGE('',*,*,#44174,.F.);
#58260=ORIENTED_EDGE('',*,*,#44175,.T.);
#58261=ORIENTED_EDGE('',*,*,#44176,.T.);
#58262=ORIENTED_EDGE('',*,*,#44177,.F.);
#58263=ORIENTED_EDGE('',*,*,#44178,.F.);
#58264=ORIENTED_EDGE('',*,*,#44179,.T.);
#58265=ORIENTED_EDGE('',*,*,#44174,.T.);
#58266=ORIENTED_EDGE('',*,*,#44180,.F.);
#58267=ORIENTED_EDGE('',*,*,#44181,.F.);
#58268=ORIENTED_EDGE('',*,*,#44182,.T.);
#58269=ORIENTED_EDGE('',*,*,#44178,.T.);
#58270=ORIENTED_EDGE('',*,*,#44183,.F.);
#58271=ORIENTED_EDGE('',*,*,#44176,.F.);
#58272=ORIENTED_EDGE('',*,*,#44184,.T.);
#58273=ORIENTED_EDGE('',*,*,#44181,.T.);
#58274=ORIENTED_EDGE('',*,*,#44185,.F.);
#58275=ORIENTED_EDGE('',*,*,#44186,.F.);
#58276=ORIENTED_EDGE('',*,*,#44187,.T.);
#58277=ORIENTED_EDGE('',*,*,#44188,.T.);
#58278=ORIENTED_EDGE('',*,*,#44189,.F.);
#58279=ORIENTED_EDGE('',*,*,#44190,.F.);
#58280=ORIENTED_EDGE('',*,*,#44191,.T.);
#58281=ORIENTED_EDGE('',*,*,#44186,.T.);
#58282=ORIENTED_EDGE('',*,*,#44192,.F.);
#58283=ORIENTED_EDGE('',*,*,#44193,.F.);
#58284=ORIENTED_EDGE('',*,*,#44194,.T.);
#58285=ORIENTED_EDGE('',*,*,#44190,.T.);
#58286=ORIENTED_EDGE('',*,*,#44195,.F.);
#58287=ORIENTED_EDGE('',*,*,#44188,.F.);
#58288=ORIENTED_EDGE('',*,*,#44196,.T.);
#58289=ORIENTED_EDGE('',*,*,#44193,.T.);
#58290=ORIENTED_EDGE('',*,*,#44197,.F.);
#58291=ORIENTED_EDGE('',*,*,#44198,.F.);
#58292=ORIENTED_EDGE('',*,*,#44199,.T.);
#58293=ORIENTED_EDGE('',*,*,#44200,.T.);
#58294=ORIENTED_EDGE('',*,*,#44201,.F.);
#58295=ORIENTED_EDGE('',*,*,#44202,.F.);
#58296=ORIENTED_EDGE('',*,*,#44203,.T.);
#58297=ORIENTED_EDGE('',*,*,#44198,.T.);
#58298=ORIENTED_EDGE('',*,*,#44204,.F.);
#58299=ORIENTED_EDGE('',*,*,#44205,.F.);
#58300=ORIENTED_EDGE('',*,*,#44206,.T.);
#58301=ORIENTED_EDGE('',*,*,#44202,.T.);
#58302=ORIENTED_EDGE('',*,*,#44207,.F.);
#58303=ORIENTED_EDGE('',*,*,#44200,.F.);
#58304=ORIENTED_EDGE('',*,*,#44208,.T.);
#58305=ORIENTED_EDGE('',*,*,#44205,.T.);
#58306=ORIENTED_EDGE('',*,*,#44209,.F.);
#58307=ORIENTED_EDGE('',*,*,#44210,.F.);
#58308=ORIENTED_EDGE('',*,*,#44211,.T.);
#58309=ORIENTED_EDGE('',*,*,#44212,.T.);
#58310=ORIENTED_EDGE('',*,*,#44213,.F.);
#58311=ORIENTED_EDGE('',*,*,#44214,.F.);
#58312=ORIENTED_EDGE('',*,*,#44215,.T.);
#58313=ORIENTED_EDGE('',*,*,#44210,.T.);
#58314=ORIENTED_EDGE('',*,*,#44216,.F.);
#58315=ORIENTED_EDGE('',*,*,#44217,.F.);
#58316=ORIENTED_EDGE('',*,*,#44218,.T.);
#58317=ORIENTED_EDGE('',*,*,#44214,.T.);
#58318=ORIENTED_EDGE('',*,*,#44219,.F.);
#58319=ORIENTED_EDGE('',*,*,#44212,.F.);
#58320=ORIENTED_EDGE('',*,*,#44220,.T.);
#58321=ORIENTED_EDGE('',*,*,#44217,.T.);
#58322=ORIENTED_EDGE('',*,*,#44221,.F.);
#58323=ORIENTED_EDGE('',*,*,#44222,.F.);
#58324=ORIENTED_EDGE('',*,*,#44223,.T.);
#58325=ORIENTED_EDGE('',*,*,#44224,.T.);
#58326=ORIENTED_EDGE('',*,*,#44225,.F.);
#58327=ORIENTED_EDGE('',*,*,#44226,.F.);
#58328=ORIENTED_EDGE('',*,*,#44227,.T.);
#58329=ORIENTED_EDGE('',*,*,#44222,.T.);
#58330=ORIENTED_EDGE('',*,*,#44228,.F.);
#58331=ORIENTED_EDGE('',*,*,#44229,.F.);
#58332=ORIENTED_EDGE('',*,*,#44230,.T.);
#58333=ORIENTED_EDGE('',*,*,#44226,.T.);
#58334=ORIENTED_EDGE('',*,*,#44231,.F.);
#58335=ORIENTED_EDGE('',*,*,#44224,.F.);
#58336=ORIENTED_EDGE('',*,*,#44232,.T.);
#58337=ORIENTED_EDGE('',*,*,#44229,.T.);
#58338=ORIENTED_EDGE('',*,*,#44233,.F.);
#58339=ORIENTED_EDGE('',*,*,#44234,.F.);
#58340=ORIENTED_EDGE('',*,*,#44235,.T.);
#58341=ORIENTED_EDGE('',*,*,#44236,.T.);
#58342=ORIENTED_EDGE('',*,*,#44237,.F.);
#58343=ORIENTED_EDGE('',*,*,#44238,.F.);
#58344=ORIENTED_EDGE('',*,*,#44239,.T.);
#58345=ORIENTED_EDGE('',*,*,#44234,.T.);
#58346=ORIENTED_EDGE('',*,*,#44240,.F.);
#58347=ORIENTED_EDGE('',*,*,#44241,.F.);
#58348=ORIENTED_EDGE('',*,*,#44242,.T.);
#58349=ORIENTED_EDGE('',*,*,#44238,.T.);
#58350=ORIENTED_EDGE('',*,*,#44243,.F.);
#58351=ORIENTED_EDGE('',*,*,#44236,.F.);
#58352=ORIENTED_EDGE('',*,*,#44244,.T.);
#58353=ORIENTED_EDGE('',*,*,#44241,.T.);
#58354=ORIENTED_EDGE('',*,*,#44245,.F.);
#58355=ORIENTED_EDGE('',*,*,#44246,.F.);
#58356=ORIENTED_EDGE('',*,*,#44247,.T.);
#58357=ORIENTED_EDGE('',*,*,#44248,.T.);
#58358=ORIENTED_EDGE('',*,*,#44249,.F.);
#58359=ORIENTED_EDGE('',*,*,#44250,.F.);
#58360=ORIENTED_EDGE('',*,*,#44251,.T.);
#58361=ORIENTED_EDGE('',*,*,#44246,.T.);
#58362=ORIENTED_EDGE('',*,*,#44252,.F.);
#58363=ORIENTED_EDGE('',*,*,#44253,.F.);
#58364=ORIENTED_EDGE('',*,*,#44254,.T.);
#58365=ORIENTED_EDGE('',*,*,#44250,.T.);
#58366=ORIENTED_EDGE('',*,*,#44255,.F.);
#58367=ORIENTED_EDGE('',*,*,#44248,.F.);
#58368=ORIENTED_EDGE('',*,*,#44256,.T.);
#58369=ORIENTED_EDGE('',*,*,#44253,.T.);
#58370=ORIENTED_EDGE('',*,*,#44257,.F.);
#58371=ORIENTED_EDGE('',*,*,#44258,.F.);
#58372=ORIENTED_EDGE('',*,*,#44259,.T.);
#58373=ORIENTED_EDGE('',*,*,#44260,.T.);
#58374=ORIENTED_EDGE('',*,*,#44261,.F.);
#58375=ORIENTED_EDGE('',*,*,#44262,.F.);
#58376=ORIENTED_EDGE('',*,*,#44263,.T.);
#58377=ORIENTED_EDGE('',*,*,#44258,.T.);
#58378=ORIENTED_EDGE('',*,*,#44264,.F.);
#58379=ORIENTED_EDGE('',*,*,#44265,.F.);
#58380=ORIENTED_EDGE('',*,*,#44266,.T.);
#58381=ORIENTED_EDGE('',*,*,#44262,.T.);
#58382=ORIENTED_EDGE('',*,*,#44267,.F.);
#58383=ORIENTED_EDGE('',*,*,#44260,.F.);
#58384=ORIENTED_EDGE('',*,*,#44268,.T.);
#58385=ORIENTED_EDGE('',*,*,#44265,.T.);
#58386=ORIENTED_EDGE('',*,*,#44269,.F.);
#58387=ORIENTED_EDGE('',*,*,#44270,.F.);
#58388=ORIENTED_EDGE('',*,*,#44271,.T.);
#58389=ORIENTED_EDGE('',*,*,#44272,.T.);
#58390=ORIENTED_EDGE('',*,*,#44273,.F.);
#58391=ORIENTED_EDGE('',*,*,#44274,.F.);
#58392=ORIENTED_EDGE('',*,*,#44275,.T.);
#58393=ORIENTED_EDGE('',*,*,#44270,.T.);
#58394=ORIENTED_EDGE('',*,*,#44276,.F.);
#58395=ORIENTED_EDGE('',*,*,#44277,.F.);
#58396=ORIENTED_EDGE('',*,*,#44278,.F.);
#58397=ORIENTED_EDGE('',*,*,#44279,.T.);
#58398=ORIENTED_EDGE('',*,*,#44274,.T.);
#58399=ORIENTED_EDGE('',*,*,#44280,.F.);
#58400=ORIENTED_EDGE('',*,*,#44272,.F.);
#58401=ORIENTED_EDGE('',*,*,#44281,.T.);
#58402=ORIENTED_EDGE('',*,*,#44282,.F.);
#58403=ORIENTED_EDGE('',*,*,#44277,.T.);
#58404=ORIENTED_EDGE('',*,*,#44283,.F.);
#58405=ORIENTED_EDGE('',*,*,#44278,.T.);
#58406=ORIENTED_EDGE('',*,*,#44282,.T.);
#58407=ORIENTED_EDGE('',*,*,#44284,.T.);
#58408=ORIENTED_EDGE('',*,*,#44285,.F.);
#58409=ORIENTED_EDGE('',*,*,#44286,.T.);
#58410=ORIENTED_EDGE('',*,*,#44287,.T.);
#58411=ORIENTED_EDGE('',*,*,#44288,.F.);
#58412=ORIENTED_EDGE('',*,*,#44289,.F.);
#58413=ORIENTED_EDGE('',*,*,#44290,.T.);
#58414=ORIENTED_EDGE('',*,*,#44285,.T.);
#58415=ORIENTED_EDGE('',*,*,#44291,.F.);
#58416=ORIENTED_EDGE('',*,*,#44292,.F.);
#58417=ORIENTED_EDGE('',*,*,#44293,.F.);
#58418=ORIENTED_EDGE('',*,*,#44294,.T.);
#58419=ORIENTED_EDGE('',*,*,#44289,.T.);
#58420=ORIENTED_EDGE('',*,*,#44295,.F.);
#58421=ORIENTED_EDGE('',*,*,#44287,.F.);
#58422=ORIENTED_EDGE('',*,*,#44296,.T.);
#58423=ORIENTED_EDGE('',*,*,#44297,.F.);
#58424=ORIENTED_EDGE('',*,*,#44292,.T.);
#58425=ORIENTED_EDGE('',*,*,#44298,.F.);
#58426=ORIENTED_EDGE('',*,*,#44293,.T.);
#58427=ORIENTED_EDGE('',*,*,#44297,.T.);
#58428=ORIENTED_EDGE('',*,*,#44299,.T.);
#58429=ORIENTED_EDGE('',*,*,#44300,.F.);
#58430=ORIENTED_EDGE('',*,*,#44301,.T.);
#58431=ORIENTED_EDGE('',*,*,#44302,.T.);
#58432=ORIENTED_EDGE('',*,*,#44303,.F.);
#58433=ORIENTED_EDGE('',*,*,#44304,.F.);
#58434=ORIENTED_EDGE('',*,*,#44305,.T.);
#58435=ORIENTED_EDGE('',*,*,#44300,.T.);
#58436=ORIENTED_EDGE('',*,*,#44306,.F.);
#58437=ORIENTED_EDGE('',*,*,#44307,.F.);
#58438=ORIENTED_EDGE('',*,*,#44308,.T.);
#58439=ORIENTED_EDGE('',*,*,#44304,.T.);
#58440=ORIENTED_EDGE('',*,*,#44309,.F.);
#58441=ORIENTED_EDGE('',*,*,#44302,.F.);
#58442=ORIENTED_EDGE('',*,*,#44310,.T.);
#58443=ORIENTED_EDGE('',*,*,#44307,.T.);
#58444=ORIENTED_EDGE('',*,*,#44311,.F.);
#58445=ORIENTED_EDGE('',*,*,#44312,.F.);
#58446=ORIENTED_EDGE('',*,*,#44313,.T.);
#58447=ORIENTED_EDGE('',*,*,#44314,.T.);
#58448=ORIENTED_EDGE('',*,*,#44315,.F.);
#58449=ORIENTED_EDGE('',*,*,#44316,.F.);
#58450=ORIENTED_EDGE('',*,*,#44317,.T.);
#58451=ORIENTED_EDGE('',*,*,#44312,.T.);
#58452=ORIENTED_EDGE('',*,*,#44318,.F.);
#58453=ORIENTED_EDGE('',*,*,#44319,.F.);
#58454=ORIENTED_EDGE('',*,*,#44320,.T.);
#58455=ORIENTED_EDGE('',*,*,#44316,.T.);
#58456=ORIENTED_EDGE('',*,*,#44321,.F.);
#58457=ORIENTED_EDGE('',*,*,#44314,.F.);
#58458=ORIENTED_EDGE('',*,*,#44322,.T.);
#58459=ORIENTED_EDGE('',*,*,#44319,.T.);
#58460=ORIENTED_EDGE('',*,*,#44323,.F.);
#58461=ORIENTED_EDGE('',*,*,#44324,.F.);
#58462=ORIENTED_EDGE('',*,*,#44325,.T.);
#58463=ORIENTED_EDGE('',*,*,#44326,.T.);
#58464=ORIENTED_EDGE('',*,*,#44327,.F.);
#58465=ORIENTED_EDGE('',*,*,#44328,.F.);
#58466=ORIENTED_EDGE('',*,*,#44329,.T.);
#58467=ORIENTED_EDGE('',*,*,#44324,.T.);
#58468=ORIENTED_EDGE('',*,*,#44330,.F.);
#58469=ORIENTED_EDGE('',*,*,#44331,.F.);
#58470=ORIENTED_EDGE('',*,*,#44332,.T.);
#58471=ORIENTED_EDGE('',*,*,#44328,.T.);
#58472=ORIENTED_EDGE('',*,*,#44333,.F.);
#58473=ORIENTED_EDGE('',*,*,#44326,.F.);
#58474=ORIENTED_EDGE('',*,*,#44334,.T.);
#58475=ORIENTED_EDGE('',*,*,#44331,.T.);
#58476=ORIENTED_EDGE('',*,*,#44335,.F.);
#58477=ORIENTED_EDGE('',*,*,#44336,.F.);
#58478=ORIENTED_EDGE('',*,*,#44337,.T.);
#58479=ORIENTED_EDGE('',*,*,#44338,.T.);
#58480=ORIENTED_EDGE('',*,*,#44339,.F.);
#58481=ORIENTED_EDGE('',*,*,#44340,.F.);
#58482=ORIENTED_EDGE('',*,*,#44341,.T.);
#58483=ORIENTED_EDGE('',*,*,#44336,.T.);
#58484=ORIENTED_EDGE('',*,*,#44342,.F.);
#58485=ORIENTED_EDGE('',*,*,#44343,.F.);
#58486=ORIENTED_EDGE('',*,*,#44344,.T.);
#58487=ORIENTED_EDGE('',*,*,#44340,.T.);
#58488=ORIENTED_EDGE('',*,*,#44345,.F.);
#58489=ORIENTED_EDGE('',*,*,#44338,.F.);
#58490=ORIENTED_EDGE('',*,*,#44346,.T.);
#58491=ORIENTED_EDGE('',*,*,#44343,.T.);
#58492=ORIENTED_EDGE('',*,*,#44347,.F.);
#58493=ORIENTED_EDGE('',*,*,#44348,.F.);
#58494=ORIENTED_EDGE('',*,*,#44349,.T.);
#58495=ORIENTED_EDGE('',*,*,#44350,.T.);
#58496=ORIENTED_EDGE('',*,*,#44351,.F.);
#58497=ORIENTED_EDGE('',*,*,#44352,.F.);
#58498=ORIENTED_EDGE('',*,*,#44353,.T.);
#58499=ORIENTED_EDGE('',*,*,#44348,.T.);
#58500=ORIENTED_EDGE('',*,*,#44354,.F.);
#58501=ORIENTED_EDGE('',*,*,#44355,.F.);
#58502=ORIENTED_EDGE('',*,*,#44356,.T.);
#58503=ORIENTED_EDGE('',*,*,#44352,.T.);
#58504=ORIENTED_EDGE('',*,*,#44357,.F.);
#58505=ORIENTED_EDGE('',*,*,#44350,.F.);
#58506=ORIENTED_EDGE('',*,*,#44358,.T.);
#58507=ORIENTED_EDGE('',*,*,#44355,.T.);
#58508=ORIENTED_EDGE('',*,*,#44359,.F.);
#58509=ORIENTED_EDGE('',*,*,#44360,.F.);
#58510=ORIENTED_EDGE('',*,*,#44361,.T.);
#58511=ORIENTED_EDGE('',*,*,#44362,.T.);
#58512=ORIENTED_EDGE('',*,*,#44363,.F.);
#58513=ORIENTED_EDGE('',*,*,#44364,.F.);
#58514=ORIENTED_EDGE('',*,*,#44365,.T.);
#58515=ORIENTED_EDGE('',*,*,#44360,.T.);
#58516=ORIENTED_EDGE('',*,*,#44366,.F.);
#58517=ORIENTED_EDGE('',*,*,#44367,.F.);
#58518=ORIENTED_EDGE('',*,*,#44368,.T.);
#58519=ORIENTED_EDGE('',*,*,#44364,.T.);
#58520=ORIENTED_EDGE('',*,*,#44369,.F.);
#58521=ORIENTED_EDGE('',*,*,#44362,.F.);
#58522=ORIENTED_EDGE('',*,*,#44370,.T.);
#58523=ORIENTED_EDGE('',*,*,#44367,.T.);
#58524=ORIENTED_EDGE('',*,*,#44371,.F.);
#58525=ORIENTED_EDGE('',*,*,#44372,.F.);
#58526=ORIENTED_EDGE('',*,*,#44373,.T.);
#58527=ORIENTED_EDGE('',*,*,#44374,.T.);
#58528=ORIENTED_EDGE('',*,*,#44375,.F.);
#58529=ORIENTED_EDGE('',*,*,#44376,.F.);
#58530=ORIENTED_EDGE('',*,*,#44377,.T.);
#58531=ORIENTED_EDGE('',*,*,#44372,.T.);
#58532=ORIENTED_EDGE('',*,*,#44378,.F.);
#58533=ORIENTED_EDGE('',*,*,#44379,.F.);
#58534=ORIENTED_EDGE('',*,*,#44380,.T.);
#58535=ORIENTED_EDGE('',*,*,#44376,.T.);
#58536=ORIENTED_EDGE('',*,*,#44381,.F.);
#58537=ORIENTED_EDGE('',*,*,#44374,.F.);
#58538=ORIENTED_EDGE('',*,*,#44382,.T.);
#58539=ORIENTED_EDGE('',*,*,#44379,.T.);
#58540=ORIENTED_EDGE('',*,*,#44383,.F.);
#58541=ORIENTED_EDGE('',*,*,#44384,.F.);
#58542=ORIENTED_EDGE('',*,*,#44385,.T.);
#58543=ORIENTED_EDGE('',*,*,#44386,.T.);
#58544=ORIENTED_EDGE('',*,*,#44387,.F.);
#58545=ORIENTED_EDGE('',*,*,#44388,.F.);
#58546=ORIENTED_EDGE('',*,*,#44389,.T.);
#58547=ORIENTED_EDGE('',*,*,#44384,.T.);
#58548=ORIENTED_EDGE('',*,*,#44390,.F.);
#58549=ORIENTED_EDGE('',*,*,#44391,.F.);
#58550=ORIENTED_EDGE('',*,*,#44392,.T.);
#58551=ORIENTED_EDGE('',*,*,#44388,.T.);
#58552=ORIENTED_EDGE('',*,*,#44393,.F.);
#58553=ORIENTED_EDGE('',*,*,#44386,.F.);
#58554=ORIENTED_EDGE('',*,*,#44394,.T.);
#58555=ORIENTED_EDGE('',*,*,#44391,.T.);
#58556=ORIENTED_EDGE('',*,*,#44395,.F.);
#58557=ORIENTED_EDGE('',*,*,#44396,.F.);
#58558=ORIENTED_EDGE('',*,*,#44397,.T.);
#58559=ORIENTED_EDGE('',*,*,#44398,.T.);
#58560=ORIENTED_EDGE('',*,*,#44399,.F.);
#58561=ORIENTED_EDGE('',*,*,#44400,.F.);
#58562=ORIENTED_EDGE('',*,*,#44401,.T.);
#58563=ORIENTED_EDGE('',*,*,#44396,.T.);
#58564=ORIENTED_EDGE('',*,*,#44402,.F.);
#58565=ORIENTED_EDGE('',*,*,#44403,.F.);
#58566=ORIENTED_EDGE('',*,*,#44404,.T.);
#58567=ORIENTED_EDGE('',*,*,#44400,.T.);
#58568=ORIENTED_EDGE('',*,*,#44405,.F.);
#58569=ORIENTED_EDGE('',*,*,#44398,.F.);
#58570=ORIENTED_EDGE('',*,*,#44406,.T.);
#58571=ORIENTED_EDGE('',*,*,#44403,.T.);
#58572=ORIENTED_EDGE('',*,*,#44407,.F.);
#58573=ORIENTED_EDGE('',*,*,#44408,.F.);
#58574=ORIENTED_EDGE('',*,*,#44409,.T.);
#58575=ORIENTED_EDGE('',*,*,#44410,.T.);
#58576=ORIENTED_EDGE('',*,*,#44411,.F.);
#58577=ORIENTED_EDGE('',*,*,#44412,.F.);
#58578=ORIENTED_EDGE('',*,*,#44413,.T.);
#58579=ORIENTED_EDGE('',*,*,#44408,.T.);
#58580=ORIENTED_EDGE('',*,*,#44414,.F.);
#58581=ORIENTED_EDGE('',*,*,#44415,.F.);
#58582=ORIENTED_EDGE('',*,*,#44416,.T.);
#58583=ORIENTED_EDGE('',*,*,#44412,.T.);
#58584=ORIENTED_EDGE('',*,*,#44417,.F.);
#58585=ORIENTED_EDGE('',*,*,#44410,.F.);
#58586=ORIENTED_EDGE('',*,*,#44418,.T.);
#58587=ORIENTED_EDGE('',*,*,#44415,.T.);
#58588=ORIENTED_EDGE('',*,*,#44419,.F.);
#58589=ORIENTED_EDGE('',*,*,#44420,.F.);
#58590=ORIENTED_EDGE('',*,*,#44421,.T.);
#58591=ORIENTED_EDGE('',*,*,#44422,.T.);
#58592=ORIENTED_EDGE('',*,*,#44423,.F.);
#58593=ORIENTED_EDGE('',*,*,#44424,.F.);
#58594=ORIENTED_EDGE('',*,*,#44425,.T.);
#58595=ORIENTED_EDGE('',*,*,#44420,.T.);
#58596=ORIENTED_EDGE('',*,*,#44426,.F.);
#58597=ORIENTED_EDGE('',*,*,#44427,.F.);
#58598=ORIENTED_EDGE('',*,*,#44428,.T.);
#58599=ORIENTED_EDGE('',*,*,#44424,.T.);
#58600=ORIENTED_EDGE('',*,*,#44429,.F.);
#58601=ORIENTED_EDGE('',*,*,#44422,.F.);
#58602=ORIENTED_EDGE('',*,*,#44430,.T.);
#58603=ORIENTED_EDGE('',*,*,#44427,.T.);
#58604=ORIENTED_EDGE('',*,*,#44431,.F.);
#58605=ORIENTED_EDGE('',*,*,#44432,.F.);
#58606=ORIENTED_EDGE('',*,*,#44433,.T.);
#58607=ORIENTED_EDGE('',*,*,#44434,.T.);
#58608=ORIENTED_EDGE('',*,*,#44435,.F.);
#58609=ORIENTED_EDGE('',*,*,#44436,.F.);
#58610=ORIENTED_EDGE('',*,*,#44437,.T.);
#58611=ORIENTED_EDGE('',*,*,#44432,.T.);
#58612=ORIENTED_EDGE('',*,*,#44438,.F.);
#58613=ORIENTED_EDGE('',*,*,#44439,.F.);
#58614=ORIENTED_EDGE('',*,*,#44440,.T.);
#58615=ORIENTED_EDGE('',*,*,#44436,.T.);
#58616=ORIENTED_EDGE('',*,*,#44441,.F.);
#58617=ORIENTED_EDGE('',*,*,#44434,.F.);
#58618=ORIENTED_EDGE('',*,*,#44442,.T.);
#58619=ORIENTED_EDGE('',*,*,#44439,.T.);
#58620=ORIENTED_EDGE('',*,*,#44443,.F.);
#58621=ORIENTED_EDGE('',*,*,#44444,.F.);
#58622=ORIENTED_EDGE('',*,*,#44445,.T.);
#58623=ORIENTED_EDGE('',*,*,#44446,.T.);
#58624=ORIENTED_EDGE('',*,*,#44447,.F.);
#58625=ORIENTED_EDGE('',*,*,#44448,.F.);
#58626=ORIENTED_EDGE('',*,*,#44449,.T.);
#58627=ORIENTED_EDGE('',*,*,#44444,.T.);
#58628=ORIENTED_EDGE('',*,*,#44450,.F.);
#58629=ORIENTED_EDGE('',*,*,#44451,.F.);
#58630=ORIENTED_EDGE('',*,*,#44452,.T.);
#58631=ORIENTED_EDGE('',*,*,#44448,.T.);
#58632=ORIENTED_EDGE('',*,*,#44453,.F.);
#58633=ORIENTED_EDGE('',*,*,#44446,.F.);
#58634=ORIENTED_EDGE('',*,*,#44454,.T.);
#58635=ORIENTED_EDGE('',*,*,#44451,.T.);
#58636=ORIENTED_EDGE('',*,*,#44455,.F.);
#58637=ORIENTED_EDGE('',*,*,#44456,.F.);
#58638=ORIENTED_EDGE('',*,*,#44457,.T.);
#58639=ORIENTED_EDGE('',*,*,#44458,.T.);
#58640=ORIENTED_EDGE('',*,*,#44459,.F.);
#58641=ORIENTED_EDGE('',*,*,#44460,.F.);
#58642=ORIENTED_EDGE('',*,*,#44461,.T.);
#58643=ORIENTED_EDGE('',*,*,#44456,.T.);
#58644=ORIENTED_EDGE('',*,*,#44462,.F.);
#58645=ORIENTED_EDGE('',*,*,#44463,.F.);
#58646=ORIENTED_EDGE('',*,*,#44464,.T.);
#58647=ORIENTED_EDGE('',*,*,#44460,.T.);
#58648=ORIENTED_EDGE('',*,*,#44465,.F.);
#58649=ORIENTED_EDGE('',*,*,#44458,.F.);
#58650=ORIENTED_EDGE('',*,*,#44466,.T.);
#58651=ORIENTED_EDGE('',*,*,#44463,.T.);
#58652=ORIENTED_EDGE('',*,*,#44467,.F.);
#58653=ORIENTED_EDGE('',*,*,#44468,.F.);
#58654=ORIENTED_EDGE('',*,*,#44469,.T.);
#58655=ORIENTED_EDGE('',*,*,#44470,.T.);
#58656=ORIENTED_EDGE('',*,*,#44471,.F.);
#58657=ORIENTED_EDGE('',*,*,#44472,.F.);
#58658=ORIENTED_EDGE('',*,*,#44473,.T.);
#58659=ORIENTED_EDGE('',*,*,#44468,.T.);
#58660=ORIENTED_EDGE('',*,*,#44474,.F.);
#58661=ORIENTED_EDGE('',*,*,#44475,.F.);
#58662=ORIENTED_EDGE('',*,*,#44476,.T.);
#58663=ORIENTED_EDGE('',*,*,#44472,.T.);
#58664=ORIENTED_EDGE('',*,*,#44477,.F.);
#58665=ORIENTED_EDGE('',*,*,#44470,.F.);
#58666=ORIENTED_EDGE('',*,*,#44478,.T.);
#58667=ORIENTED_EDGE('',*,*,#44475,.T.);
#58668=ORIENTED_EDGE('',*,*,#44479,.F.);
#58669=ORIENTED_EDGE('',*,*,#44480,.F.);
#58670=ORIENTED_EDGE('',*,*,#44481,.T.);
#58671=ORIENTED_EDGE('',*,*,#44482,.T.);
#58672=ORIENTED_EDGE('',*,*,#44483,.F.);
#58673=ORIENTED_EDGE('',*,*,#44484,.F.);
#58674=ORIENTED_EDGE('',*,*,#44485,.T.);
#58675=ORIENTED_EDGE('',*,*,#44480,.T.);
#58676=ORIENTED_EDGE('',*,*,#44486,.F.);
#58677=ORIENTED_EDGE('',*,*,#44487,.F.);
#58678=ORIENTED_EDGE('',*,*,#44488,.T.);
#58679=ORIENTED_EDGE('',*,*,#44484,.T.);
#58680=ORIENTED_EDGE('',*,*,#44489,.F.);
#58681=ORIENTED_EDGE('',*,*,#44482,.F.);
#58682=ORIENTED_EDGE('',*,*,#44490,.T.);
#58683=ORIENTED_EDGE('',*,*,#44487,.T.);
#58684=ORIENTED_EDGE('',*,*,#44491,.F.);
#58685=ORIENTED_EDGE('',*,*,#44492,.F.);
#58686=ORIENTED_EDGE('',*,*,#44493,.T.);
#58687=ORIENTED_EDGE('',*,*,#44494,.T.);
#58688=ORIENTED_EDGE('',*,*,#44495,.F.);
#58689=ORIENTED_EDGE('',*,*,#44496,.F.);
#58690=ORIENTED_EDGE('',*,*,#44497,.T.);
#58691=ORIENTED_EDGE('',*,*,#44492,.T.);
#58692=ORIENTED_EDGE('',*,*,#44498,.F.);
#58693=ORIENTED_EDGE('',*,*,#44499,.F.);
#58694=ORIENTED_EDGE('',*,*,#44500,.T.);
#58695=ORIENTED_EDGE('',*,*,#44496,.T.);
#58696=ORIENTED_EDGE('',*,*,#44501,.F.);
#58697=ORIENTED_EDGE('',*,*,#44494,.F.);
#58698=ORIENTED_EDGE('',*,*,#44502,.T.);
#58699=ORIENTED_EDGE('',*,*,#44499,.T.);
#58700=ORIENTED_EDGE('',*,*,#44503,.F.);
#58701=ORIENTED_EDGE('',*,*,#44504,.F.);
#58702=ORIENTED_EDGE('',*,*,#44505,.T.);
#58703=ORIENTED_EDGE('',*,*,#44506,.T.);
#58704=ORIENTED_EDGE('',*,*,#44507,.F.);
#58705=ORIENTED_EDGE('',*,*,#44508,.F.);
#58706=ORIENTED_EDGE('',*,*,#44509,.T.);
#58707=ORIENTED_EDGE('',*,*,#44504,.T.);
#58708=ORIENTED_EDGE('',*,*,#44510,.F.);
#58709=ORIENTED_EDGE('',*,*,#44511,.F.);
#58710=ORIENTED_EDGE('',*,*,#44512,.T.);
#58711=ORIENTED_EDGE('',*,*,#44508,.T.);
#58712=ORIENTED_EDGE('',*,*,#44513,.F.);
#58713=ORIENTED_EDGE('',*,*,#44506,.F.);
#58714=ORIENTED_EDGE('',*,*,#44514,.T.);
#58715=ORIENTED_EDGE('',*,*,#44511,.T.);
#58716=ORIENTED_EDGE('',*,*,#44515,.F.);
#58717=ORIENTED_EDGE('',*,*,#44516,.F.);
#58718=ORIENTED_EDGE('',*,*,#44517,.T.);
#58719=ORIENTED_EDGE('',*,*,#44518,.T.);
#58720=ORIENTED_EDGE('',*,*,#44519,.F.);
#58721=ORIENTED_EDGE('',*,*,#44520,.F.);
#58722=ORIENTED_EDGE('',*,*,#44521,.T.);
#58723=ORIENTED_EDGE('',*,*,#44516,.T.);
#58724=ORIENTED_EDGE('',*,*,#44522,.F.);
#58725=ORIENTED_EDGE('',*,*,#44523,.F.);
#58726=ORIENTED_EDGE('',*,*,#44524,.T.);
#58727=ORIENTED_EDGE('',*,*,#44520,.T.);
#58728=ORIENTED_EDGE('',*,*,#44525,.F.);
#58729=ORIENTED_EDGE('',*,*,#44518,.F.);
#58730=ORIENTED_EDGE('',*,*,#44526,.T.);
#58731=ORIENTED_EDGE('',*,*,#44523,.T.);
#58732=ORIENTED_EDGE('',*,*,#44527,.F.);
#58733=ORIENTED_EDGE('',*,*,#44528,.F.);
#58734=ORIENTED_EDGE('',*,*,#44529,.T.);
#58735=ORIENTED_EDGE('',*,*,#44530,.T.);
#58736=ORIENTED_EDGE('',*,*,#44531,.F.);
#58737=ORIENTED_EDGE('',*,*,#44532,.F.);
#58738=ORIENTED_EDGE('',*,*,#44533,.T.);
#58739=ORIENTED_EDGE('',*,*,#44528,.T.);
#58740=ORIENTED_EDGE('',*,*,#44534,.F.);
#58741=ORIENTED_EDGE('',*,*,#44535,.F.);
#58742=ORIENTED_EDGE('',*,*,#44536,.T.);
#58743=ORIENTED_EDGE('',*,*,#44532,.T.);
#58744=ORIENTED_EDGE('',*,*,#44537,.F.);
#58745=ORIENTED_EDGE('',*,*,#44530,.F.);
#58746=ORIENTED_EDGE('',*,*,#44538,.T.);
#58747=ORIENTED_EDGE('',*,*,#44535,.T.);
#58748=ORIENTED_EDGE('',*,*,#44539,.F.);
#58749=ORIENTED_EDGE('',*,*,#44540,.F.);
#58750=ORIENTED_EDGE('',*,*,#44541,.T.);
#58751=ORIENTED_EDGE('',*,*,#44542,.T.);
#58752=ORIENTED_EDGE('',*,*,#44543,.F.);
#58753=ORIENTED_EDGE('',*,*,#44544,.F.);
#58754=ORIENTED_EDGE('',*,*,#44545,.T.);
#58755=ORIENTED_EDGE('',*,*,#44540,.T.);
#58756=ORIENTED_EDGE('',*,*,#44546,.F.);
#58757=ORIENTED_EDGE('',*,*,#44547,.F.);
#58758=ORIENTED_EDGE('',*,*,#44548,.T.);
#58759=ORIENTED_EDGE('',*,*,#44544,.T.);
#58760=ORIENTED_EDGE('',*,*,#44549,.F.);
#58761=ORIENTED_EDGE('',*,*,#44542,.F.);
#58762=ORIENTED_EDGE('',*,*,#44550,.T.);
#58763=ORIENTED_EDGE('',*,*,#44547,.T.);
#58764=ORIENTED_EDGE('',*,*,#44551,.F.);
#58765=ORIENTED_EDGE('',*,*,#44552,.F.);
#58766=ORIENTED_EDGE('',*,*,#44553,.T.);
#58767=ORIENTED_EDGE('',*,*,#44554,.T.);
#58768=ORIENTED_EDGE('',*,*,#44555,.F.);
#58769=ORIENTED_EDGE('',*,*,#44556,.F.);
#58770=ORIENTED_EDGE('',*,*,#44557,.T.);
#58771=ORIENTED_EDGE('',*,*,#44552,.T.);
#58772=ORIENTED_EDGE('',*,*,#44558,.F.);
#58773=ORIENTED_EDGE('',*,*,#44559,.F.);
#58774=ORIENTED_EDGE('',*,*,#44560,.T.);
#58775=ORIENTED_EDGE('',*,*,#44556,.T.);
#58776=ORIENTED_EDGE('',*,*,#44561,.F.);
#58777=ORIENTED_EDGE('',*,*,#44554,.F.);
#58778=ORIENTED_EDGE('',*,*,#44562,.T.);
#58779=ORIENTED_EDGE('',*,*,#44559,.T.);
#58780=ORIENTED_EDGE('',*,*,#44563,.F.);
#58781=ORIENTED_EDGE('',*,*,#44564,.F.);
#58782=ORIENTED_EDGE('',*,*,#44565,.T.);
#58783=ORIENTED_EDGE('',*,*,#44566,.T.);
#58784=ORIENTED_EDGE('',*,*,#44567,.F.);
#58785=ORIENTED_EDGE('',*,*,#44568,.F.);
#58786=ORIENTED_EDGE('',*,*,#44569,.T.);
#58787=ORIENTED_EDGE('',*,*,#44564,.T.);
#58788=ORIENTED_EDGE('',*,*,#44570,.F.);
#58789=ORIENTED_EDGE('',*,*,#44571,.F.);
#58790=ORIENTED_EDGE('',*,*,#44572,.T.);
#58791=ORIENTED_EDGE('',*,*,#44568,.T.);
#58792=ORIENTED_EDGE('',*,*,#44573,.F.);
#58793=ORIENTED_EDGE('',*,*,#44566,.F.);
#58794=ORIENTED_EDGE('',*,*,#44574,.T.);
#58795=ORIENTED_EDGE('',*,*,#44571,.T.);
#58796=ORIENTED_EDGE('',*,*,#44575,.F.);
#58797=ORIENTED_EDGE('',*,*,#44576,.F.);
#58798=ORIENTED_EDGE('',*,*,#44577,.T.);
#58799=ORIENTED_EDGE('',*,*,#44578,.T.);
#58800=ORIENTED_EDGE('',*,*,#44579,.F.);
#58801=ORIENTED_EDGE('',*,*,#44580,.F.);
#58802=ORIENTED_EDGE('',*,*,#44581,.T.);
#58803=ORIENTED_EDGE('',*,*,#44576,.T.);
#58804=ORIENTED_EDGE('',*,*,#44582,.F.);
#58805=ORIENTED_EDGE('',*,*,#44583,.F.);
#58806=ORIENTED_EDGE('',*,*,#44584,.T.);
#58807=ORIENTED_EDGE('',*,*,#44580,.T.);
#58808=ORIENTED_EDGE('',*,*,#44585,.F.);
#58809=ORIENTED_EDGE('',*,*,#44578,.F.);
#58810=ORIENTED_EDGE('',*,*,#44586,.T.);
#58811=ORIENTED_EDGE('',*,*,#44583,.T.);
#58812=ORIENTED_EDGE('',*,*,#44587,.F.);
#58813=ORIENTED_EDGE('',*,*,#44588,.F.);
#58814=ORIENTED_EDGE('',*,*,#44589,.T.);
#58815=ORIENTED_EDGE('',*,*,#44590,.T.);
#58816=ORIENTED_EDGE('',*,*,#44591,.F.);
#58817=ORIENTED_EDGE('',*,*,#44592,.F.);
#58818=ORIENTED_EDGE('',*,*,#44593,.T.);
#58819=ORIENTED_EDGE('',*,*,#44588,.T.);
#58820=ORIENTED_EDGE('',*,*,#44594,.F.);
#58821=ORIENTED_EDGE('',*,*,#44595,.F.);
#58822=ORIENTED_EDGE('',*,*,#44596,.T.);
#58823=ORIENTED_EDGE('',*,*,#44592,.T.);
#58824=ORIENTED_EDGE('',*,*,#44597,.F.);
#58825=ORIENTED_EDGE('',*,*,#44590,.F.);
#58826=ORIENTED_EDGE('',*,*,#44598,.T.);
#58827=ORIENTED_EDGE('',*,*,#44595,.T.);
#58828=ORIENTED_EDGE('',*,*,#44599,.F.);
#58829=ORIENTED_EDGE('',*,*,#44600,.F.);
#58830=ORIENTED_EDGE('',*,*,#44601,.T.);
#58831=ORIENTED_EDGE('',*,*,#44602,.T.);
#58832=ORIENTED_EDGE('',*,*,#44603,.F.);
#58833=ORIENTED_EDGE('',*,*,#44604,.F.);
#58834=ORIENTED_EDGE('',*,*,#44605,.T.);
#58835=ORIENTED_EDGE('',*,*,#44600,.T.);
#58836=ORIENTED_EDGE('',*,*,#44606,.F.);
#58837=ORIENTED_EDGE('',*,*,#44607,.F.);
#58838=ORIENTED_EDGE('',*,*,#44608,.T.);
#58839=ORIENTED_EDGE('',*,*,#44604,.T.);
#58840=ORIENTED_EDGE('',*,*,#44609,.F.);
#58841=ORIENTED_EDGE('',*,*,#44602,.F.);
#58842=ORIENTED_EDGE('',*,*,#44610,.T.);
#58843=ORIENTED_EDGE('',*,*,#44607,.T.);
#58844=ORIENTED_EDGE('',*,*,#44611,.F.);
#58845=ORIENTED_EDGE('',*,*,#44612,.F.);
#58846=ORIENTED_EDGE('',*,*,#44613,.T.);
#58847=ORIENTED_EDGE('',*,*,#44614,.T.);
#58848=ORIENTED_EDGE('',*,*,#44615,.F.);
#58849=ORIENTED_EDGE('',*,*,#44616,.F.);
#58850=ORIENTED_EDGE('',*,*,#44617,.T.);
#58851=ORIENTED_EDGE('',*,*,#44612,.T.);
#58852=ORIENTED_EDGE('',*,*,#44618,.F.);
#58853=ORIENTED_EDGE('',*,*,#44619,.F.);
#58854=ORIENTED_EDGE('',*,*,#44620,.T.);
#58855=ORIENTED_EDGE('',*,*,#44616,.T.);
#58856=ORIENTED_EDGE('',*,*,#44621,.F.);
#58857=ORIENTED_EDGE('',*,*,#44614,.F.);
#58858=ORIENTED_EDGE('',*,*,#44622,.T.);
#58859=ORIENTED_EDGE('',*,*,#44619,.T.);
#58860=ORIENTED_EDGE('',*,*,#44623,.F.);
#58861=ORIENTED_EDGE('',*,*,#44624,.F.);
#58862=ORIENTED_EDGE('',*,*,#44625,.T.);
#58863=ORIENTED_EDGE('',*,*,#44626,.T.);
#58864=ORIENTED_EDGE('',*,*,#44627,.F.);
#58865=ORIENTED_EDGE('',*,*,#44628,.F.);
#58866=ORIENTED_EDGE('',*,*,#44629,.T.);
#58867=ORIENTED_EDGE('',*,*,#44624,.T.);
#58868=ORIENTED_EDGE('',*,*,#44630,.F.);
#58869=ORIENTED_EDGE('',*,*,#44631,.F.);
#58870=ORIENTED_EDGE('',*,*,#44632,.T.);
#58871=ORIENTED_EDGE('',*,*,#44628,.T.);
#58872=ORIENTED_EDGE('',*,*,#44633,.F.);
#58873=ORIENTED_EDGE('',*,*,#44626,.F.);
#58874=ORIENTED_EDGE('',*,*,#44634,.T.);
#58875=ORIENTED_EDGE('',*,*,#44631,.T.);
#58876=ORIENTED_EDGE('',*,*,#44635,.F.);
#58877=ORIENTED_EDGE('',*,*,#44636,.F.);
#58878=ORIENTED_EDGE('',*,*,#44637,.T.);
#58879=ORIENTED_EDGE('',*,*,#44638,.T.);
#58880=ORIENTED_EDGE('',*,*,#44639,.F.);
#58881=ORIENTED_EDGE('',*,*,#44640,.F.);
#58882=ORIENTED_EDGE('',*,*,#44641,.T.);
#58883=ORIENTED_EDGE('',*,*,#44636,.T.);
#58884=ORIENTED_EDGE('',*,*,#44642,.F.);
#58885=ORIENTED_EDGE('',*,*,#44643,.F.);
#58886=ORIENTED_EDGE('',*,*,#44644,.T.);
#58887=ORIENTED_EDGE('',*,*,#44640,.T.);
#58888=ORIENTED_EDGE('',*,*,#44645,.F.);
#58889=ORIENTED_EDGE('',*,*,#44638,.F.);
#58890=ORIENTED_EDGE('',*,*,#44646,.T.);
#58891=ORIENTED_EDGE('',*,*,#44643,.T.);
#58892=ORIENTED_EDGE('',*,*,#44647,.F.);
#58893=ORIENTED_EDGE('',*,*,#44648,.F.);
#58894=ORIENTED_EDGE('',*,*,#44649,.T.);
#58895=ORIENTED_EDGE('',*,*,#44650,.T.);
#58896=ORIENTED_EDGE('',*,*,#44651,.F.);
#58897=ORIENTED_EDGE('',*,*,#44652,.F.);
#58898=ORIENTED_EDGE('',*,*,#44653,.T.);
#58899=ORIENTED_EDGE('',*,*,#44648,.T.);
#58900=ORIENTED_EDGE('',*,*,#44654,.F.);
#58901=ORIENTED_EDGE('',*,*,#44655,.F.);
#58902=ORIENTED_EDGE('',*,*,#44656,.T.);
#58903=ORIENTED_EDGE('',*,*,#44652,.T.);
#58904=ORIENTED_EDGE('',*,*,#44657,.F.);
#58905=ORIENTED_EDGE('',*,*,#44650,.F.);
#58906=ORIENTED_EDGE('',*,*,#44658,.T.);
#58907=ORIENTED_EDGE('',*,*,#44655,.T.);
#58908=ORIENTED_EDGE('',*,*,#44659,.F.);
#58909=ORIENTED_EDGE('',*,*,#44660,.F.);
#58910=ORIENTED_EDGE('',*,*,#44661,.T.);
#58911=ORIENTED_EDGE('',*,*,#44662,.T.);
#58912=ORIENTED_EDGE('',*,*,#44663,.F.);
#58913=ORIENTED_EDGE('',*,*,#44664,.F.);
#58914=ORIENTED_EDGE('',*,*,#44665,.T.);
#58915=ORIENTED_EDGE('',*,*,#44660,.T.);
#58916=ORIENTED_EDGE('',*,*,#44666,.F.);
#58917=ORIENTED_EDGE('',*,*,#44667,.F.);
#58918=ORIENTED_EDGE('',*,*,#44668,.T.);
#58919=ORIENTED_EDGE('',*,*,#44664,.T.);
#58920=ORIENTED_EDGE('',*,*,#44669,.F.);
#58921=ORIENTED_EDGE('',*,*,#44662,.F.);
#58922=ORIENTED_EDGE('',*,*,#44670,.T.);
#58923=ORIENTED_EDGE('',*,*,#44667,.T.);
#58924=ORIENTED_EDGE('',*,*,#44671,.F.);
#58925=ORIENTED_EDGE('',*,*,#44672,.F.);
#58926=ORIENTED_EDGE('',*,*,#44673,.T.);
#58927=ORIENTED_EDGE('',*,*,#44674,.T.);
#58928=ORIENTED_EDGE('',*,*,#44675,.F.);
#58929=ORIENTED_EDGE('',*,*,#44676,.F.);
#58930=ORIENTED_EDGE('',*,*,#44677,.T.);
#58931=ORIENTED_EDGE('',*,*,#44672,.T.);
#58932=ORIENTED_EDGE('',*,*,#44678,.F.);
#58933=ORIENTED_EDGE('',*,*,#44679,.F.);
#58934=ORIENTED_EDGE('',*,*,#44680,.T.);
#58935=ORIENTED_EDGE('',*,*,#44676,.T.);
#58936=ORIENTED_EDGE('',*,*,#44681,.F.);
#58937=ORIENTED_EDGE('',*,*,#44674,.F.);
#58938=ORIENTED_EDGE('',*,*,#44682,.T.);
#58939=ORIENTED_EDGE('',*,*,#44679,.T.);
#58940=ORIENTED_EDGE('',*,*,#44683,.F.);
#58941=ORIENTED_EDGE('',*,*,#44684,.F.);
#58942=ORIENTED_EDGE('',*,*,#44685,.T.);
#58943=ORIENTED_EDGE('',*,*,#44686,.T.);
#58944=ORIENTED_EDGE('',*,*,#44687,.F.);
#58945=ORIENTED_EDGE('',*,*,#44688,.F.);
#58946=ORIENTED_EDGE('',*,*,#44689,.T.);
#58947=ORIENTED_EDGE('',*,*,#44684,.T.);
#58948=ORIENTED_EDGE('',*,*,#44690,.F.);
#58949=ORIENTED_EDGE('',*,*,#44691,.F.);
#58950=ORIENTED_EDGE('',*,*,#44692,.T.);
#58951=ORIENTED_EDGE('',*,*,#44688,.T.);
#58952=ORIENTED_EDGE('',*,*,#44693,.F.);
#58953=ORIENTED_EDGE('',*,*,#44686,.F.);
#58954=ORIENTED_EDGE('',*,*,#44694,.T.);
#58955=ORIENTED_EDGE('',*,*,#44691,.T.);
#58956=ORIENTED_EDGE('',*,*,#44695,.F.);
#58957=ORIENTED_EDGE('',*,*,#44696,.F.);
#58958=ORIENTED_EDGE('',*,*,#44697,.T.);
#58959=ORIENTED_EDGE('',*,*,#44698,.T.);
#58960=ORIENTED_EDGE('',*,*,#44699,.F.);
#58961=ORIENTED_EDGE('',*,*,#44700,.F.);
#58962=ORIENTED_EDGE('',*,*,#44701,.T.);
#58963=ORIENTED_EDGE('',*,*,#44696,.T.);
#58964=ORIENTED_EDGE('',*,*,#44702,.F.);
#58965=ORIENTED_EDGE('',*,*,#44703,.F.);
#58966=ORIENTED_EDGE('',*,*,#44704,.T.);
#58967=ORIENTED_EDGE('',*,*,#44700,.T.);
#58968=ORIENTED_EDGE('',*,*,#44705,.F.);
#58969=ORIENTED_EDGE('',*,*,#44698,.F.);
#58970=ORIENTED_EDGE('',*,*,#44706,.T.);
#58971=ORIENTED_EDGE('',*,*,#44703,.T.);
#58972=ORIENTED_EDGE('',*,*,#44707,.F.);
#58973=ORIENTED_EDGE('',*,*,#44708,.F.);
#58974=ORIENTED_EDGE('',*,*,#44709,.T.);
#58975=ORIENTED_EDGE('',*,*,#44710,.T.);
#58976=ORIENTED_EDGE('',*,*,#44711,.F.);
#58977=ORIENTED_EDGE('',*,*,#44712,.F.);
#58978=ORIENTED_EDGE('',*,*,#44713,.T.);
#58979=ORIENTED_EDGE('',*,*,#44708,.T.);
#58980=ORIENTED_EDGE('',*,*,#44714,.F.);
#58981=ORIENTED_EDGE('',*,*,#44715,.F.);
#58982=ORIENTED_EDGE('',*,*,#44716,.T.);
#58983=ORIENTED_EDGE('',*,*,#44712,.T.);
#58984=ORIENTED_EDGE('',*,*,#44717,.F.);
#58985=ORIENTED_EDGE('',*,*,#44710,.F.);
#58986=ORIENTED_EDGE('',*,*,#44718,.T.);
#58987=ORIENTED_EDGE('',*,*,#44715,.T.);
#58988=ORIENTED_EDGE('',*,*,#44719,.F.);
#58989=ORIENTED_EDGE('',*,*,#44720,.F.);
#58990=ORIENTED_EDGE('',*,*,#44721,.T.);
#58991=ORIENTED_EDGE('',*,*,#44722,.T.);
#58992=ORIENTED_EDGE('',*,*,#44723,.F.);
#58993=ORIENTED_EDGE('',*,*,#44724,.F.);
#58994=ORIENTED_EDGE('',*,*,#44725,.T.);
#58995=ORIENTED_EDGE('',*,*,#44720,.T.);
#58996=ORIENTED_EDGE('',*,*,#44726,.F.);
#58997=ORIENTED_EDGE('',*,*,#44727,.F.);
#58998=ORIENTED_EDGE('',*,*,#44728,.T.);
#58999=ORIENTED_EDGE('',*,*,#44724,.T.);
#59000=ORIENTED_EDGE('',*,*,#44729,.F.);
#59001=ORIENTED_EDGE('',*,*,#44722,.F.);
#59002=ORIENTED_EDGE('',*,*,#44730,.T.);
#59003=ORIENTED_EDGE('',*,*,#44727,.T.);
#59004=ORIENTED_EDGE('',*,*,#44731,.F.);
#59005=ORIENTED_EDGE('',*,*,#44732,.F.);
#59006=ORIENTED_EDGE('',*,*,#44733,.T.);
#59007=ORIENTED_EDGE('',*,*,#44734,.T.);
#59008=ORIENTED_EDGE('',*,*,#44735,.F.);
#59009=ORIENTED_EDGE('',*,*,#44736,.F.);
#59010=ORIENTED_EDGE('',*,*,#44737,.T.);
#59011=ORIENTED_EDGE('',*,*,#44732,.T.);
#59012=ORIENTED_EDGE('',*,*,#44738,.F.);
#59013=ORIENTED_EDGE('',*,*,#44739,.F.);
#59014=ORIENTED_EDGE('',*,*,#44740,.T.);
#59015=ORIENTED_EDGE('',*,*,#44736,.T.);
#59016=ORIENTED_EDGE('',*,*,#44741,.F.);
#59017=ORIENTED_EDGE('',*,*,#44734,.F.);
#59018=ORIENTED_EDGE('',*,*,#44742,.T.);
#59019=ORIENTED_EDGE('',*,*,#44739,.T.);
#59020=ORIENTED_EDGE('',*,*,#44743,.F.);
#59021=ORIENTED_EDGE('',*,*,#44744,.F.);
#59022=ORIENTED_EDGE('',*,*,#44745,.T.);
#59023=ORIENTED_EDGE('',*,*,#44746,.T.);
#59024=ORIENTED_EDGE('',*,*,#44747,.F.);
#59025=ORIENTED_EDGE('',*,*,#44748,.F.);
#59026=ORIENTED_EDGE('',*,*,#44749,.T.);
#59027=ORIENTED_EDGE('',*,*,#44744,.T.);
#59028=ORIENTED_EDGE('',*,*,#44750,.F.);
#59029=ORIENTED_EDGE('',*,*,#44751,.F.);
#59030=ORIENTED_EDGE('',*,*,#44752,.T.);
#59031=ORIENTED_EDGE('',*,*,#44748,.T.);
#59032=ORIENTED_EDGE('',*,*,#44753,.F.);
#59033=ORIENTED_EDGE('',*,*,#44746,.F.);
#59034=ORIENTED_EDGE('',*,*,#44754,.T.);
#59035=ORIENTED_EDGE('',*,*,#44751,.T.);
#59036=ORIENTED_EDGE('',*,*,#44755,.F.);
#59037=ORIENTED_EDGE('',*,*,#44756,.F.);
#59038=ORIENTED_EDGE('',*,*,#44757,.T.);
#59039=ORIENTED_EDGE('',*,*,#44758,.T.);
#59040=ORIENTED_EDGE('',*,*,#44759,.F.);
#59041=ORIENTED_EDGE('',*,*,#44760,.F.);
#59042=ORIENTED_EDGE('',*,*,#44761,.T.);
#59043=ORIENTED_EDGE('',*,*,#44756,.T.);
#59044=ORIENTED_EDGE('',*,*,#44762,.F.);
#59045=ORIENTED_EDGE('',*,*,#44763,.F.);
#59046=ORIENTED_EDGE('',*,*,#44764,.T.);
#59047=ORIENTED_EDGE('',*,*,#44760,.T.);
#59048=ORIENTED_EDGE('',*,*,#44765,.F.);
#59049=ORIENTED_EDGE('',*,*,#44758,.F.);
#59050=ORIENTED_EDGE('',*,*,#44766,.T.);
#59051=ORIENTED_EDGE('',*,*,#44763,.T.);
#59052=ORIENTED_EDGE('',*,*,#44767,.F.);
#59053=ORIENTED_EDGE('',*,*,#44768,.F.);
#59054=ORIENTED_EDGE('',*,*,#44769,.T.);
#59055=ORIENTED_EDGE('',*,*,#44770,.T.);
#59056=ORIENTED_EDGE('',*,*,#44771,.F.);
#59057=ORIENTED_EDGE('',*,*,#44772,.F.);
#59058=ORIENTED_EDGE('',*,*,#44773,.T.);
#59059=ORIENTED_EDGE('',*,*,#44768,.T.);
#59060=ORIENTED_EDGE('',*,*,#44774,.F.);
#59061=ORIENTED_EDGE('',*,*,#44775,.F.);
#59062=ORIENTED_EDGE('',*,*,#44776,.T.);
#59063=ORIENTED_EDGE('',*,*,#44772,.T.);
#59064=ORIENTED_EDGE('',*,*,#44777,.F.);
#59065=ORIENTED_EDGE('',*,*,#44770,.F.);
#59066=ORIENTED_EDGE('',*,*,#44778,.T.);
#59067=ORIENTED_EDGE('',*,*,#44775,.T.);
#59068=ORIENTED_EDGE('',*,*,#44779,.F.);
#59069=ORIENTED_EDGE('',*,*,#44780,.F.);
#59070=ORIENTED_EDGE('',*,*,#44781,.T.);
#59071=ORIENTED_EDGE('',*,*,#44782,.T.);
#59072=ORIENTED_EDGE('',*,*,#44783,.F.);
#59073=ORIENTED_EDGE('',*,*,#44784,.F.);
#59074=ORIENTED_EDGE('',*,*,#44785,.T.);
#59075=ORIENTED_EDGE('',*,*,#44780,.T.);
#59076=ORIENTED_EDGE('',*,*,#44786,.F.);
#59077=ORIENTED_EDGE('',*,*,#44787,.F.);
#59078=ORIENTED_EDGE('',*,*,#44788,.T.);
#59079=ORIENTED_EDGE('',*,*,#44784,.T.);
#59080=ORIENTED_EDGE('',*,*,#44789,.F.);
#59081=ORIENTED_EDGE('',*,*,#44782,.F.);
#59082=ORIENTED_EDGE('',*,*,#44790,.T.);
#59083=ORIENTED_EDGE('',*,*,#44787,.T.);
#59084=ORIENTED_EDGE('',*,*,#44791,.F.);
#59085=ORIENTED_EDGE('',*,*,#44792,.F.);
#59086=ORIENTED_EDGE('',*,*,#44793,.T.);
#59087=ORIENTED_EDGE('',*,*,#44794,.T.);
#59088=ORIENTED_EDGE('',*,*,#44795,.F.);
#59089=ORIENTED_EDGE('',*,*,#44796,.F.);
#59090=ORIENTED_EDGE('',*,*,#44797,.T.);
#59091=ORIENTED_EDGE('',*,*,#44792,.T.);
#59092=ORIENTED_EDGE('',*,*,#44798,.F.);
#59093=ORIENTED_EDGE('',*,*,#44799,.F.);
#59094=ORIENTED_EDGE('',*,*,#44800,.T.);
#59095=ORIENTED_EDGE('',*,*,#44796,.T.);
#59096=ORIENTED_EDGE('',*,*,#44801,.F.);
#59097=ORIENTED_EDGE('',*,*,#44794,.F.);
#59098=ORIENTED_EDGE('',*,*,#44802,.T.);
#59099=ORIENTED_EDGE('',*,*,#44799,.T.);
#59100=ORIENTED_EDGE('',*,*,#44803,.F.);
#59101=ORIENTED_EDGE('',*,*,#44804,.F.);
#59102=ORIENTED_EDGE('',*,*,#44805,.T.);
#59103=ORIENTED_EDGE('',*,*,#44806,.T.);
#59104=ORIENTED_EDGE('',*,*,#44807,.F.);
#59105=ORIENTED_EDGE('',*,*,#44808,.F.);
#59106=ORIENTED_EDGE('',*,*,#44809,.T.);
#59107=ORIENTED_EDGE('',*,*,#44804,.T.);
#59108=ORIENTED_EDGE('',*,*,#44810,.F.);
#59109=ORIENTED_EDGE('',*,*,#44811,.F.);
#59110=ORIENTED_EDGE('',*,*,#44812,.T.);
#59111=ORIENTED_EDGE('',*,*,#44808,.T.);
#59112=ORIENTED_EDGE('',*,*,#44813,.F.);
#59113=ORIENTED_EDGE('',*,*,#44806,.F.);
#59114=ORIENTED_EDGE('',*,*,#44814,.T.);
#59115=ORIENTED_EDGE('',*,*,#44811,.T.);
#59116=ORIENTED_EDGE('',*,*,#44815,.F.);
#59117=ORIENTED_EDGE('',*,*,#44816,.F.);
#59118=ORIENTED_EDGE('',*,*,#44817,.T.);
#59119=ORIENTED_EDGE('',*,*,#44818,.T.);
#59120=ORIENTED_EDGE('',*,*,#44819,.F.);
#59121=ORIENTED_EDGE('',*,*,#44820,.F.);
#59122=ORIENTED_EDGE('',*,*,#44821,.T.);
#59123=ORIENTED_EDGE('',*,*,#44816,.T.);
#59124=ORIENTED_EDGE('',*,*,#44822,.F.);
#59125=ORIENTED_EDGE('',*,*,#44823,.F.);
#59126=ORIENTED_EDGE('',*,*,#44824,.T.);
#59127=ORIENTED_EDGE('',*,*,#44820,.T.);
#59128=ORIENTED_EDGE('',*,*,#44825,.F.);
#59129=ORIENTED_EDGE('',*,*,#44818,.F.);
#59130=ORIENTED_EDGE('',*,*,#44826,.T.);
#59131=ORIENTED_EDGE('',*,*,#44823,.T.);
#59132=ORIENTED_EDGE('',*,*,#44827,.F.);
#59133=ORIENTED_EDGE('',*,*,#44828,.F.);
#59134=ORIENTED_EDGE('',*,*,#44829,.T.);
#59135=ORIENTED_EDGE('',*,*,#44830,.T.);
#59136=ORIENTED_EDGE('',*,*,#44831,.F.);
#59137=ORIENTED_EDGE('',*,*,#44832,.F.);
#59138=ORIENTED_EDGE('',*,*,#44833,.T.);
#59139=ORIENTED_EDGE('',*,*,#44828,.T.);
#59140=ORIENTED_EDGE('',*,*,#44834,.F.);
#59141=ORIENTED_EDGE('',*,*,#44835,.F.);
#59142=ORIENTED_EDGE('',*,*,#44836,.T.);
#59143=ORIENTED_EDGE('',*,*,#44832,.T.);
#59144=ORIENTED_EDGE('',*,*,#44837,.F.);
#59145=ORIENTED_EDGE('',*,*,#44830,.F.);
#59146=ORIENTED_EDGE('',*,*,#44838,.T.);
#59147=ORIENTED_EDGE('',*,*,#44835,.T.);
#59148=ORIENTED_EDGE('',*,*,#44839,.F.);
#59149=ORIENTED_EDGE('',*,*,#44840,.F.);
#59150=ORIENTED_EDGE('',*,*,#44841,.T.);
#59151=ORIENTED_EDGE('',*,*,#44842,.T.);
#59152=ORIENTED_EDGE('',*,*,#44843,.F.);
#59153=ORIENTED_EDGE('',*,*,#44844,.F.);
#59154=ORIENTED_EDGE('',*,*,#44845,.T.);
#59155=ORIENTED_EDGE('',*,*,#44840,.T.);
#59156=ORIENTED_EDGE('',*,*,#44846,.F.);
#59157=ORIENTED_EDGE('',*,*,#44847,.F.);
#59158=ORIENTED_EDGE('',*,*,#44848,.T.);
#59159=ORIENTED_EDGE('',*,*,#44844,.T.);
#59160=ORIENTED_EDGE('',*,*,#44849,.F.);
#59161=ORIENTED_EDGE('',*,*,#44842,.F.);
#59162=ORIENTED_EDGE('',*,*,#44850,.T.);
#59163=ORIENTED_EDGE('',*,*,#44847,.T.);
#59164=ORIENTED_EDGE('',*,*,#44851,.F.);
#59165=ORIENTED_EDGE('',*,*,#44852,.F.);
#59166=ORIENTED_EDGE('',*,*,#44853,.T.);
#59167=ORIENTED_EDGE('',*,*,#44854,.T.);
#59168=ORIENTED_EDGE('',*,*,#44855,.F.);
#59169=ORIENTED_EDGE('',*,*,#44856,.F.);
#59170=ORIENTED_EDGE('',*,*,#44857,.T.);
#59171=ORIENTED_EDGE('',*,*,#44852,.T.);
#59172=ORIENTED_EDGE('',*,*,#44858,.F.);
#59173=ORIENTED_EDGE('',*,*,#44859,.F.);
#59174=ORIENTED_EDGE('',*,*,#44860,.T.);
#59175=ORIENTED_EDGE('',*,*,#44856,.T.);
#59176=ORIENTED_EDGE('',*,*,#44861,.F.);
#59177=ORIENTED_EDGE('',*,*,#44854,.F.);
#59178=ORIENTED_EDGE('',*,*,#44862,.T.);
#59179=ORIENTED_EDGE('',*,*,#44859,.T.);
#59180=ORIENTED_EDGE('',*,*,#44863,.F.);
#59181=ORIENTED_EDGE('',*,*,#44864,.F.);
#59182=ORIENTED_EDGE('',*,*,#44865,.T.);
#59183=ORIENTED_EDGE('',*,*,#44866,.T.);
#59184=ORIENTED_EDGE('',*,*,#44867,.F.);
#59185=ORIENTED_EDGE('',*,*,#44868,.F.);
#59186=ORIENTED_EDGE('',*,*,#44869,.T.);
#59187=ORIENTED_EDGE('',*,*,#44864,.T.);
#59188=ORIENTED_EDGE('',*,*,#44870,.F.);
#59189=ORIENTED_EDGE('',*,*,#44871,.F.);
#59190=ORIENTED_EDGE('',*,*,#44872,.T.);
#59191=ORIENTED_EDGE('',*,*,#44868,.T.);
#59192=ORIENTED_EDGE('',*,*,#44873,.F.);
#59193=ORIENTED_EDGE('',*,*,#44866,.F.);
#59194=ORIENTED_EDGE('',*,*,#44874,.T.);
#59195=ORIENTED_EDGE('',*,*,#44871,.T.);
#59196=ORIENTED_EDGE('',*,*,#44875,.F.);
#59197=ORIENTED_EDGE('',*,*,#44876,.F.);
#59198=ORIENTED_EDGE('',*,*,#44877,.T.);
#59199=ORIENTED_EDGE('',*,*,#44878,.T.);
#59200=ORIENTED_EDGE('',*,*,#44879,.F.);
#59201=ORIENTED_EDGE('',*,*,#44880,.F.);
#59202=ORIENTED_EDGE('',*,*,#44881,.T.);
#59203=ORIENTED_EDGE('',*,*,#44876,.T.);
#59204=ORIENTED_EDGE('',*,*,#44882,.F.);
#59205=ORIENTED_EDGE('',*,*,#44883,.F.);
#59206=ORIENTED_EDGE('',*,*,#44884,.T.);
#59207=ORIENTED_EDGE('',*,*,#44880,.T.);
#59208=ORIENTED_EDGE('',*,*,#44885,.F.);
#59209=ORIENTED_EDGE('',*,*,#44878,.F.);
#59210=ORIENTED_EDGE('',*,*,#44886,.T.);
#59211=ORIENTED_EDGE('',*,*,#44883,.T.);
#59212=ORIENTED_EDGE('',*,*,#44887,.F.);
#59213=ORIENTED_EDGE('',*,*,#44888,.F.);
#59214=ORIENTED_EDGE('',*,*,#44889,.T.);
#59215=ORIENTED_EDGE('',*,*,#44890,.T.);
#59216=ORIENTED_EDGE('',*,*,#44891,.F.);
#59217=ORIENTED_EDGE('',*,*,#44892,.F.);
#59218=ORIENTED_EDGE('',*,*,#44893,.T.);
#59219=ORIENTED_EDGE('',*,*,#44888,.T.);
#59220=ORIENTED_EDGE('',*,*,#44894,.F.);
#59221=ORIENTED_EDGE('',*,*,#44895,.F.);
#59222=ORIENTED_EDGE('',*,*,#44896,.T.);
#59223=ORIENTED_EDGE('',*,*,#44892,.T.);
#59224=ORIENTED_EDGE('',*,*,#44897,.F.);
#59225=ORIENTED_EDGE('',*,*,#44890,.F.);
#59226=ORIENTED_EDGE('',*,*,#44898,.T.);
#59227=ORIENTED_EDGE('',*,*,#44895,.T.);
#59228=ORIENTED_EDGE('',*,*,#44899,.F.);
#59229=ORIENTED_EDGE('',*,*,#44900,.F.);
#59230=ORIENTED_EDGE('',*,*,#44901,.T.);
#59231=ORIENTED_EDGE('',*,*,#44902,.T.);
#59232=ORIENTED_EDGE('',*,*,#44903,.F.);
#59233=ORIENTED_EDGE('',*,*,#44904,.F.);
#59234=ORIENTED_EDGE('',*,*,#44905,.T.);
#59235=ORIENTED_EDGE('',*,*,#44900,.T.);
#59236=ORIENTED_EDGE('',*,*,#44906,.F.);
#59237=ORIENTED_EDGE('',*,*,#44907,.F.);
#59238=ORIENTED_EDGE('',*,*,#44908,.T.);
#59239=ORIENTED_EDGE('',*,*,#44904,.T.);
#59240=ORIENTED_EDGE('',*,*,#44909,.F.);
#59241=ORIENTED_EDGE('',*,*,#44902,.F.);
#59242=ORIENTED_EDGE('',*,*,#44910,.T.);
#59243=ORIENTED_EDGE('',*,*,#44907,.T.);
#59244=ORIENTED_EDGE('',*,*,#44911,.F.);
#59245=ORIENTED_EDGE('',*,*,#44912,.F.);
#59246=ORIENTED_EDGE('',*,*,#44913,.T.);
#59247=ORIENTED_EDGE('',*,*,#44914,.T.);
#59248=ORIENTED_EDGE('',*,*,#44915,.F.);
#59249=ORIENTED_EDGE('',*,*,#44916,.F.);
#59250=ORIENTED_EDGE('',*,*,#44917,.T.);
#59251=ORIENTED_EDGE('',*,*,#44912,.T.);
#59252=ORIENTED_EDGE('',*,*,#44918,.F.);
#59253=ORIENTED_EDGE('',*,*,#44919,.F.);
#59254=ORIENTED_EDGE('',*,*,#44920,.T.);
#59255=ORIENTED_EDGE('',*,*,#44916,.T.);
#59256=ORIENTED_EDGE('',*,*,#44921,.F.);
#59257=ORIENTED_EDGE('',*,*,#44914,.F.);
#59258=ORIENTED_EDGE('',*,*,#44922,.T.);
#59259=ORIENTED_EDGE('',*,*,#44919,.T.);
#59260=ORIENTED_EDGE('',*,*,#44923,.F.);
#59261=ORIENTED_EDGE('',*,*,#44924,.F.);
#59262=ORIENTED_EDGE('',*,*,#44925,.T.);
#59263=ORIENTED_EDGE('',*,*,#44926,.T.);
#59264=ORIENTED_EDGE('',*,*,#44927,.F.);
#59265=ORIENTED_EDGE('',*,*,#44928,.F.);
#59266=ORIENTED_EDGE('',*,*,#44929,.T.);
#59267=ORIENTED_EDGE('',*,*,#44924,.T.);
#59268=ORIENTED_EDGE('',*,*,#44930,.F.);
#59269=ORIENTED_EDGE('',*,*,#44931,.F.);
#59270=ORIENTED_EDGE('',*,*,#44932,.T.);
#59271=ORIENTED_EDGE('',*,*,#44928,.T.);
#59272=ORIENTED_EDGE('',*,*,#44933,.F.);
#59273=ORIENTED_EDGE('',*,*,#44926,.F.);
#59274=ORIENTED_EDGE('',*,*,#44934,.T.);
#59275=ORIENTED_EDGE('',*,*,#44931,.T.);
#59276=ORIENTED_EDGE('',*,*,#44935,.F.);
#59277=ORIENTED_EDGE('',*,*,#44936,.F.);
#59278=ORIENTED_EDGE('',*,*,#44937,.T.);
#59279=ORIENTED_EDGE('',*,*,#44938,.T.);
#59280=ORIENTED_EDGE('',*,*,#44939,.F.);
#59281=ORIENTED_EDGE('',*,*,#44940,.F.);
#59282=ORIENTED_EDGE('',*,*,#44941,.T.);
#59283=ORIENTED_EDGE('',*,*,#44936,.T.);
#59284=ORIENTED_EDGE('',*,*,#44942,.F.);
#59285=ORIENTED_EDGE('',*,*,#44943,.F.);
#59286=ORIENTED_EDGE('',*,*,#44944,.T.);
#59287=ORIENTED_EDGE('',*,*,#44940,.T.);
#59288=ORIENTED_EDGE('',*,*,#44945,.F.);
#59289=ORIENTED_EDGE('',*,*,#44938,.F.);
#59290=ORIENTED_EDGE('',*,*,#44946,.T.);
#59291=ORIENTED_EDGE('',*,*,#44943,.T.);
#59292=ORIENTED_EDGE('',*,*,#44947,.F.);
#59293=ORIENTED_EDGE('',*,*,#44948,.F.);
#59294=ORIENTED_EDGE('',*,*,#44949,.T.);
#59295=ORIENTED_EDGE('',*,*,#44950,.T.);
#59296=ORIENTED_EDGE('',*,*,#44951,.F.);
#59297=ORIENTED_EDGE('',*,*,#44952,.F.);
#59298=ORIENTED_EDGE('',*,*,#44953,.T.);
#59299=ORIENTED_EDGE('',*,*,#44948,.T.);
#59300=ORIENTED_EDGE('',*,*,#44954,.F.);
#59301=ORIENTED_EDGE('',*,*,#44955,.F.);
#59302=ORIENTED_EDGE('',*,*,#44956,.T.);
#59303=ORIENTED_EDGE('',*,*,#44952,.T.);
#59304=ORIENTED_EDGE('',*,*,#44957,.F.);
#59305=ORIENTED_EDGE('',*,*,#44950,.F.);
#59306=ORIENTED_EDGE('',*,*,#44958,.T.);
#59307=ORIENTED_EDGE('',*,*,#44955,.T.);
#59308=ORIENTED_EDGE('',*,*,#44959,.F.);
#59309=ORIENTED_EDGE('',*,*,#44960,.F.);
#59310=ORIENTED_EDGE('',*,*,#44961,.T.);
#59311=ORIENTED_EDGE('',*,*,#44962,.T.);
#59312=ORIENTED_EDGE('',*,*,#44963,.F.);
#59313=ORIENTED_EDGE('',*,*,#44964,.F.);
#59314=ORIENTED_EDGE('',*,*,#44965,.T.);
#59315=ORIENTED_EDGE('',*,*,#44960,.T.);
#59316=ORIENTED_EDGE('',*,*,#44966,.F.);
#59317=ORIENTED_EDGE('',*,*,#44967,.F.);
#59318=ORIENTED_EDGE('',*,*,#44968,.T.);
#59319=ORIENTED_EDGE('',*,*,#44964,.T.);
#59320=ORIENTED_EDGE('',*,*,#44969,.F.);
#59321=ORIENTED_EDGE('',*,*,#44962,.F.);
#59322=ORIENTED_EDGE('',*,*,#44970,.T.);
#59323=ORIENTED_EDGE('',*,*,#44967,.T.);
#59324=ORIENTED_EDGE('',*,*,#44971,.F.);
#59325=ORIENTED_EDGE('',*,*,#44972,.F.);
#59326=ORIENTED_EDGE('',*,*,#44973,.T.);
#59327=ORIENTED_EDGE('',*,*,#44974,.T.);
#59328=ORIENTED_EDGE('',*,*,#44975,.F.);
#59329=ORIENTED_EDGE('',*,*,#44976,.F.);
#59330=ORIENTED_EDGE('',*,*,#44977,.T.);
#59331=ORIENTED_EDGE('',*,*,#44972,.T.);
#59332=ORIENTED_EDGE('',*,*,#44978,.F.);
#59333=ORIENTED_EDGE('',*,*,#44979,.F.);
#59334=ORIENTED_EDGE('',*,*,#44980,.T.);
#59335=ORIENTED_EDGE('',*,*,#44976,.T.);
#59336=ORIENTED_EDGE('',*,*,#44981,.F.);
#59337=ORIENTED_EDGE('',*,*,#44974,.F.);
#59338=ORIENTED_EDGE('',*,*,#44982,.T.);
#59339=ORIENTED_EDGE('',*,*,#44979,.T.);
#59340=ORIENTED_EDGE('',*,*,#44983,.F.);
#59341=ORIENTED_EDGE('',*,*,#44984,.F.);
#59342=ORIENTED_EDGE('',*,*,#44985,.T.);
#59343=ORIENTED_EDGE('',*,*,#44986,.T.);
#59344=ORIENTED_EDGE('',*,*,#44987,.F.);
#59345=ORIENTED_EDGE('',*,*,#44988,.F.);
#59346=ORIENTED_EDGE('',*,*,#44989,.T.);
#59347=ORIENTED_EDGE('',*,*,#44984,.T.);
#59348=ORIENTED_EDGE('',*,*,#44990,.F.);
#59349=ORIENTED_EDGE('',*,*,#44991,.F.);
#59350=ORIENTED_EDGE('',*,*,#44992,.T.);
#59351=ORIENTED_EDGE('',*,*,#44988,.T.);
#59352=ORIENTED_EDGE('',*,*,#44993,.F.);
#59353=ORIENTED_EDGE('',*,*,#44986,.F.);
#59354=ORIENTED_EDGE('',*,*,#44994,.T.);
#59355=ORIENTED_EDGE('',*,*,#44991,.T.);
#59356=ORIENTED_EDGE('',*,*,#44995,.F.);
#59357=ORIENTED_EDGE('',*,*,#44996,.F.);
#59358=ORIENTED_EDGE('',*,*,#44997,.T.);
#59359=ORIENTED_EDGE('',*,*,#44998,.T.);
#59360=ORIENTED_EDGE('',*,*,#44999,.F.);
#59361=ORIENTED_EDGE('',*,*,#45000,.F.);
#59362=ORIENTED_EDGE('',*,*,#45001,.T.);
#59363=ORIENTED_EDGE('',*,*,#44996,.T.);
#59364=ORIENTED_EDGE('',*,*,#45002,.F.);
#59365=ORIENTED_EDGE('',*,*,#45003,.F.);
#59366=ORIENTED_EDGE('',*,*,#45004,.T.);
#59367=ORIENTED_EDGE('',*,*,#45000,.T.);
#59368=ORIENTED_EDGE('',*,*,#45005,.F.);
#59369=ORIENTED_EDGE('',*,*,#44998,.F.);
#59370=ORIENTED_EDGE('',*,*,#45006,.T.);
#59371=ORIENTED_EDGE('',*,*,#45003,.T.);
#59372=ORIENTED_EDGE('',*,*,#45007,.F.);
#59373=ORIENTED_EDGE('',*,*,#45008,.F.);
#59374=ORIENTED_EDGE('',*,*,#45009,.T.);
#59375=ORIENTED_EDGE('',*,*,#45010,.T.);
#59376=ORIENTED_EDGE('',*,*,#45011,.F.);
#59377=ORIENTED_EDGE('',*,*,#45012,.F.);
#59378=ORIENTED_EDGE('',*,*,#45013,.T.);
#59379=ORIENTED_EDGE('',*,*,#45008,.T.);
#59380=ORIENTED_EDGE('',*,*,#45014,.F.);
#59381=ORIENTED_EDGE('',*,*,#45015,.F.);
#59382=ORIENTED_EDGE('',*,*,#45016,.T.);
#59383=ORIENTED_EDGE('',*,*,#45012,.T.);
#59384=ORIENTED_EDGE('',*,*,#45017,.F.);
#59385=ORIENTED_EDGE('',*,*,#45010,.F.);
#59386=ORIENTED_EDGE('',*,*,#45018,.T.);
#59387=ORIENTED_EDGE('',*,*,#45015,.T.);
#59388=ORIENTED_EDGE('',*,*,#45019,.F.);
#59389=ORIENTED_EDGE('',*,*,#45020,.F.);
#59390=ORIENTED_EDGE('',*,*,#45021,.T.);
#59391=ORIENTED_EDGE('',*,*,#45022,.T.);
#59392=ORIENTED_EDGE('',*,*,#45023,.F.);
#59393=ORIENTED_EDGE('',*,*,#45024,.F.);
#59394=ORIENTED_EDGE('',*,*,#45025,.T.);
#59395=ORIENTED_EDGE('',*,*,#45020,.T.);
#59396=ORIENTED_EDGE('',*,*,#45026,.F.);
#59397=ORIENTED_EDGE('',*,*,#45027,.F.);
#59398=ORIENTED_EDGE('',*,*,#45028,.T.);
#59399=ORIENTED_EDGE('',*,*,#45024,.T.);
#59400=ORIENTED_EDGE('',*,*,#45029,.F.);
#59401=ORIENTED_EDGE('',*,*,#45022,.F.);
#59402=ORIENTED_EDGE('',*,*,#45030,.T.);
#59403=ORIENTED_EDGE('',*,*,#45027,.T.);
#59404=ORIENTED_EDGE('',*,*,#45031,.F.);
#59405=ORIENTED_EDGE('',*,*,#45032,.F.);
#59406=ORIENTED_EDGE('',*,*,#45033,.T.);
#59407=ORIENTED_EDGE('',*,*,#45034,.T.);
#59408=ORIENTED_EDGE('',*,*,#45035,.F.);
#59409=ORIENTED_EDGE('',*,*,#45036,.F.);
#59410=ORIENTED_EDGE('',*,*,#45037,.T.);
#59411=ORIENTED_EDGE('',*,*,#45032,.T.);
#59412=ORIENTED_EDGE('',*,*,#45038,.F.);
#59413=ORIENTED_EDGE('',*,*,#45039,.F.);
#59414=ORIENTED_EDGE('',*,*,#45040,.T.);
#59415=ORIENTED_EDGE('',*,*,#45036,.T.);
#59416=ORIENTED_EDGE('',*,*,#45041,.F.);
#59417=ORIENTED_EDGE('',*,*,#45034,.F.);
#59418=ORIENTED_EDGE('',*,*,#45042,.T.);
#59419=ORIENTED_EDGE('',*,*,#45039,.T.);
#59420=ORIENTED_EDGE('',*,*,#45043,.F.);
#59421=ORIENTED_EDGE('',*,*,#45044,.F.);
#59422=ORIENTED_EDGE('',*,*,#45045,.T.);
#59423=ORIENTED_EDGE('',*,*,#45046,.T.);
#59424=ORIENTED_EDGE('',*,*,#45047,.F.);
#59425=ORIENTED_EDGE('',*,*,#45048,.F.);
#59426=ORIENTED_EDGE('',*,*,#45049,.T.);
#59427=ORIENTED_EDGE('',*,*,#45044,.T.);
#59428=ORIENTED_EDGE('',*,*,#45050,.F.);
#59429=ORIENTED_EDGE('',*,*,#45051,.F.);
#59430=ORIENTED_EDGE('',*,*,#45052,.T.);
#59431=ORIENTED_EDGE('',*,*,#45048,.T.);
#59432=ORIENTED_EDGE('',*,*,#45053,.F.);
#59433=ORIENTED_EDGE('',*,*,#45046,.F.);
#59434=ORIENTED_EDGE('',*,*,#45054,.T.);
#59435=ORIENTED_EDGE('',*,*,#45051,.T.);
#59436=ORIENTED_EDGE('',*,*,#45055,.F.);
#59437=ORIENTED_EDGE('',*,*,#45056,.F.);
#59438=ORIENTED_EDGE('',*,*,#45057,.T.);
#59439=ORIENTED_EDGE('',*,*,#45058,.T.);
#59440=ORIENTED_EDGE('',*,*,#45059,.F.);
#59441=ORIENTED_EDGE('',*,*,#45060,.F.);
#59442=ORIENTED_EDGE('',*,*,#45061,.T.);
#59443=ORIENTED_EDGE('',*,*,#45056,.T.);
#59444=ORIENTED_EDGE('',*,*,#45062,.F.);
#59445=ORIENTED_EDGE('',*,*,#45063,.F.);
#59446=ORIENTED_EDGE('',*,*,#45064,.T.);
#59447=ORIENTED_EDGE('',*,*,#45060,.T.);
#59448=ORIENTED_EDGE('',*,*,#45065,.F.);
#59449=ORIENTED_EDGE('',*,*,#45058,.F.);
#59450=ORIENTED_EDGE('',*,*,#45066,.T.);
#59451=ORIENTED_EDGE('',*,*,#45063,.T.);
#59452=ORIENTED_EDGE('',*,*,#45067,.F.);
#59453=ORIENTED_EDGE('',*,*,#45068,.F.);
#59454=ORIENTED_EDGE('',*,*,#45069,.T.);
#59455=ORIENTED_EDGE('',*,*,#45070,.T.);
#59456=ORIENTED_EDGE('',*,*,#45071,.F.);
#59457=ORIENTED_EDGE('',*,*,#45072,.F.);
#59458=ORIENTED_EDGE('',*,*,#45073,.T.);
#59459=ORIENTED_EDGE('',*,*,#45068,.T.);
#59460=ORIENTED_EDGE('',*,*,#45074,.F.);
#59461=ORIENTED_EDGE('',*,*,#45075,.F.);
#59462=ORIENTED_EDGE('',*,*,#45076,.T.);
#59463=ORIENTED_EDGE('',*,*,#45072,.T.);
#59464=ORIENTED_EDGE('',*,*,#45077,.F.);
#59465=ORIENTED_EDGE('',*,*,#45070,.F.);
#59466=ORIENTED_EDGE('',*,*,#45078,.T.);
#59467=ORIENTED_EDGE('',*,*,#45075,.T.);
#59468=ORIENTED_EDGE('',*,*,#45079,.F.);
#59469=ORIENTED_EDGE('',*,*,#45080,.F.);
#59470=ORIENTED_EDGE('',*,*,#45081,.T.);
#59471=ORIENTED_EDGE('',*,*,#45082,.T.);
#59472=ORIENTED_EDGE('',*,*,#45083,.F.);
#59473=ORIENTED_EDGE('',*,*,#45084,.F.);
#59474=ORIENTED_EDGE('',*,*,#45085,.T.);
#59475=ORIENTED_EDGE('',*,*,#45080,.T.);
#59476=ORIENTED_EDGE('',*,*,#45086,.F.);
#59477=ORIENTED_EDGE('',*,*,#45087,.F.);
#59478=ORIENTED_EDGE('',*,*,#45088,.T.);
#59479=ORIENTED_EDGE('',*,*,#45084,.T.);
#59480=ORIENTED_EDGE('',*,*,#45089,.F.);
#59481=ORIENTED_EDGE('',*,*,#45082,.F.);
#59482=ORIENTED_EDGE('',*,*,#45090,.T.);
#59483=ORIENTED_EDGE('',*,*,#45087,.T.);
#59484=ORIENTED_EDGE('',*,*,#45091,.F.);
#59485=ORIENTED_EDGE('',*,*,#45092,.F.);
#59486=ORIENTED_EDGE('',*,*,#45093,.T.);
#59487=ORIENTED_EDGE('',*,*,#45094,.T.);
#59488=ORIENTED_EDGE('',*,*,#45095,.F.);
#59489=ORIENTED_EDGE('',*,*,#45096,.F.);
#59490=ORIENTED_EDGE('',*,*,#45097,.T.);
#59491=ORIENTED_EDGE('',*,*,#45092,.T.);
#59492=ORIENTED_EDGE('',*,*,#45098,.F.);
#59493=ORIENTED_EDGE('',*,*,#45099,.F.);
#59494=ORIENTED_EDGE('',*,*,#45100,.T.);
#59495=ORIENTED_EDGE('',*,*,#45096,.T.);
#59496=ORIENTED_EDGE('',*,*,#45101,.F.);
#59497=ORIENTED_EDGE('',*,*,#45094,.F.);
#59498=ORIENTED_EDGE('',*,*,#45102,.T.);
#59499=ORIENTED_EDGE('',*,*,#45099,.T.);
#59500=ORIENTED_EDGE('',*,*,#45103,.F.);
#59501=ORIENTED_EDGE('',*,*,#45104,.F.);
#59502=ORIENTED_EDGE('',*,*,#45105,.T.);
#59503=ORIENTED_EDGE('',*,*,#45106,.T.);
#59504=ORIENTED_EDGE('',*,*,#45107,.F.);
#59505=ORIENTED_EDGE('',*,*,#45108,.F.);
#59506=ORIENTED_EDGE('',*,*,#45109,.T.);
#59507=ORIENTED_EDGE('',*,*,#45104,.T.);
#59508=ORIENTED_EDGE('',*,*,#45110,.F.);
#59509=ORIENTED_EDGE('',*,*,#45111,.F.);
#59510=ORIENTED_EDGE('',*,*,#45112,.T.);
#59511=ORIENTED_EDGE('',*,*,#45108,.T.);
#59512=ORIENTED_EDGE('',*,*,#45113,.F.);
#59513=ORIENTED_EDGE('',*,*,#45106,.F.);
#59514=ORIENTED_EDGE('',*,*,#45114,.T.);
#59515=ORIENTED_EDGE('',*,*,#45111,.T.);
#59516=ORIENTED_EDGE('',*,*,#45115,.F.);
#59517=ORIENTED_EDGE('',*,*,#45116,.F.);
#59518=ORIENTED_EDGE('',*,*,#45117,.T.);
#59519=ORIENTED_EDGE('',*,*,#45118,.T.);
#59520=ORIENTED_EDGE('',*,*,#45119,.F.);
#59521=ORIENTED_EDGE('',*,*,#45120,.F.);
#59522=ORIENTED_EDGE('',*,*,#45121,.T.);
#59523=ORIENTED_EDGE('',*,*,#45116,.T.);
#59524=ORIENTED_EDGE('',*,*,#45122,.F.);
#59525=ORIENTED_EDGE('',*,*,#45123,.F.);
#59526=ORIENTED_EDGE('',*,*,#45124,.T.);
#59527=ORIENTED_EDGE('',*,*,#45120,.T.);
#59528=ORIENTED_EDGE('',*,*,#45125,.F.);
#59529=ORIENTED_EDGE('',*,*,#45118,.F.);
#59530=ORIENTED_EDGE('',*,*,#45126,.T.);
#59531=ORIENTED_EDGE('',*,*,#45123,.T.);
#59532=ORIENTED_EDGE('',*,*,#45127,.F.);
#59533=ORIENTED_EDGE('',*,*,#45128,.F.);
#59534=ORIENTED_EDGE('',*,*,#45129,.T.);
#59535=ORIENTED_EDGE('',*,*,#45130,.T.);
#59536=ORIENTED_EDGE('',*,*,#45131,.F.);
#59537=ORIENTED_EDGE('',*,*,#45132,.F.);
#59538=ORIENTED_EDGE('',*,*,#45133,.T.);
#59539=ORIENTED_EDGE('',*,*,#45128,.T.);
#59540=ORIENTED_EDGE('',*,*,#45134,.F.);
#59541=ORIENTED_EDGE('',*,*,#45135,.F.);
#59542=ORIENTED_EDGE('',*,*,#45136,.T.);
#59543=ORIENTED_EDGE('',*,*,#45132,.T.);
#59544=ORIENTED_EDGE('',*,*,#45137,.F.);
#59545=ORIENTED_EDGE('',*,*,#45130,.F.);
#59546=ORIENTED_EDGE('',*,*,#45138,.T.);
#59547=ORIENTED_EDGE('',*,*,#45135,.T.);
#59548=ORIENTED_EDGE('',*,*,#45139,.F.);
#59549=ORIENTED_EDGE('',*,*,#45140,.F.);
#59550=ORIENTED_EDGE('',*,*,#45141,.T.);
#59551=ORIENTED_EDGE('',*,*,#45142,.T.);
#59552=ORIENTED_EDGE('',*,*,#45143,.F.);
#59553=ORIENTED_EDGE('',*,*,#45144,.F.);
#59554=ORIENTED_EDGE('',*,*,#45145,.F.);
#59555=ORIENTED_EDGE('',*,*,#45146,.T.);
#59556=ORIENTED_EDGE('',*,*,#45140,.T.);
#59557=ORIENTED_EDGE('',*,*,#45147,.F.);
#59558=ORIENTED_EDGE('',*,*,#45148,.F.);
#59559=ORIENTED_EDGE('',*,*,#45149,.F.);
#59560=ORIENTED_EDGE('',*,*,#45144,.T.);
#59561=ORIENTED_EDGE('',*,*,#45150,.F.);
#59562=ORIENTED_EDGE('',*,*,#45142,.F.);
#59563=ORIENTED_EDGE('',*,*,#45151,.F.);
#59564=ORIENTED_EDGE('',*,*,#45148,.T.);
#59565=ORIENTED_EDGE('',*,*,#45152,.F.);
#59566=ORIENTED_EDGE('',*,*,#45145,.T.);
#59567=ORIENTED_EDGE('',*,*,#45149,.T.);
#59568=ORIENTED_EDGE('',*,*,#45151,.T.);
#59569=ORIENTED_EDGE('',*,*,#45153,.T.);
#59570=ORIENTED_EDGE('',*,*,#45154,.F.);
#59571=ORIENTED_EDGE('',*,*,#45155,.T.);
#59572=ORIENTED_EDGE('',*,*,#45156,.T.);
#59573=ORIENTED_EDGE('',*,*,#45157,.F.);
#59574=ORIENTED_EDGE('',*,*,#45158,.F.);
#59575=ORIENTED_EDGE('',*,*,#45159,.F.);
#59576=ORIENTED_EDGE('',*,*,#45160,.T.);
#59577=ORIENTED_EDGE('',*,*,#45154,.T.);
#59578=ORIENTED_EDGE('',*,*,#45161,.F.);
#59579=ORIENTED_EDGE('',*,*,#45162,.F.);
#59580=ORIENTED_EDGE('',*,*,#45163,.F.);
#59581=ORIENTED_EDGE('',*,*,#45158,.T.);
#59582=ORIENTED_EDGE('',*,*,#45164,.F.);
#59583=ORIENTED_EDGE('',*,*,#45156,.F.);
#59584=ORIENTED_EDGE('',*,*,#45165,.T.);
#59585=ORIENTED_EDGE('',*,*,#45166,.F.);
#59586=ORIENTED_EDGE('',*,*,#45162,.T.);
#59587=ORIENTED_EDGE('',*,*,#45167,.F.);
#59588=ORIENTED_EDGE('',*,*,#45159,.T.);
#59589=ORIENTED_EDGE('',*,*,#45163,.T.);
#59590=ORIENTED_EDGE('',*,*,#45166,.T.);
#59591=ORIENTED_EDGE('',*,*,#45168,.T.);
#59592=ORIENTED_EDGE('',*,*,#45169,.F.);
#59593=ORIENTED_EDGE('',*,*,#45170,.T.);
#59594=ORIENTED_EDGE('',*,*,#45171,.T.);
#59595=ORIENTED_EDGE('',*,*,#45172,.F.);
#59596=ORIENTED_EDGE('',*,*,#45173,.F.);
#59597=ORIENTED_EDGE('',*,*,#45174,.F.);
#59598=ORIENTED_EDGE('',*,*,#45175,.T.);
#59599=ORIENTED_EDGE('',*,*,#45169,.T.);
#59600=ORIENTED_EDGE('',*,*,#45176,.F.);
#59601=ORIENTED_EDGE('',*,*,#45177,.F.);
#59602=ORIENTED_EDGE('',*,*,#45178,.F.);
#59603=ORIENTED_EDGE('',*,*,#45173,.T.);
#59604=ORIENTED_EDGE('',*,*,#45179,.F.);
#59605=ORIENTED_EDGE('',*,*,#45171,.F.);
#59606=ORIENTED_EDGE('',*,*,#45180,.T.);
#59607=ORIENTED_EDGE('',*,*,#45181,.F.);
#59608=ORIENTED_EDGE('',*,*,#45177,.T.);
#59609=ORIENTED_EDGE('',*,*,#45182,.F.);
#59610=ORIENTED_EDGE('',*,*,#45174,.T.);
#59611=ORIENTED_EDGE('',*,*,#45178,.T.);
#59612=ORIENTED_EDGE('',*,*,#45181,.T.);
#59613=ORIENTED_EDGE('',*,*,#45183,.T.);
#59614=ORIENTED_EDGE('',*,*,#45184,.F.);
#59615=ORIENTED_EDGE('',*,*,#45185,.T.);
#59616=ORIENTED_EDGE('',*,*,#45186,.T.);
#59617=ORIENTED_EDGE('',*,*,#45187,.F.);
#59618=ORIENTED_EDGE('',*,*,#45188,.F.);
#59619=ORIENTED_EDGE('',*,*,#45189,.F.);
#59620=ORIENTED_EDGE('',*,*,#45190,.T.);
#59621=ORIENTED_EDGE('',*,*,#45184,.T.);
#59622=ORIENTED_EDGE('',*,*,#45191,.F.);
#59623=ORIENTED_EDGE('',*,*,#45192,.F.);
#59624=ORIENTED_EDGE('',*,*,#45193,.F.);
#59625=ORIENTED_EDGE('',*,*,#45188,.T.);
#59626=ORIENTED_EDGE('',*,*,#45194,.F.);
#59627=ORIENTED_EDGE('',*,*,#45186,.F.);
#59628=ORIENTED_EDGE('',*,*,#45195,.T.);
#59629=ORIENTED_EDGE('',*,*,#45196,.F.);
#59630=ORIENTED_EDGE('',*,*,#45192,.T.);
#59631=ORIENTED_EDGE('',*,*,#45197,.F.);
#59632=ORIENTED_EDGE('',*,*,#45189,.T.);
#59633=ORIENTED_EDGE('',*,*,#45193,.T.);
#59634=ORIENTED_EDGE('',*,*,#45196,.T.);
#59635=ORIENTED_EDGE('',*,*,#45198,.T.);
#59636=ORIENTED_EDGE('',*,*,#45199,.F.);
#59637=ORIENTED_EDGE('',*,*,#45200,.T.);
#59638=ORIENTED_EDGE('',*,*,#45201,.T.);
#59639=ORIENTED_EDGE('',*,*,#45202,.F.);
#59640=ORIENTED_EDGE('',*,*,#45203,.F.);
#59641=ORIENTED_EDGE('',*,*,#45204,.F.);
#59642=ORIENTED_EDGE('',*,*,#45205,.T.);
#59643=ORIENTED_EDGE('',*,*,#45199,.T.);
#59644=ORIENTED_EDGE('',*,*,#45206,.F.);
#59645=ORIENTED_EDGE('',*,*,#45207,.F.);
#59646=ORIENTED_EDGE('',*,*,#45208,.F.);
#59647=ORIENTED_EDGE('',*,*,#45203,.T.);
#59648=ORIENTED_EDGE('',*,*,#45209,.F.);
#59649=ORIENTED_EDGE('',*,*,#45201,.F.);
#59650=ORIENTED_EDGE('',*,*,#45210,.T.);
#59651=ORIENTED_EDGE('',*,*,#45211,.F.);
#59652=ORIENTED_EDGE('',*,*,#45207,.T.);
#59653=ORIENTED_EDGE('',*,*,#45212,.F.);
#59654=ORIENTED_EDGE('',*,*,#45204,.T.);
#59655=ORIENTED_EDGE('',*,*,#45208,.T.);
#59656=ORIENTED_EDGE('',*,*,#45211,.T.);
#59657=ORIENTED_EDGE('',*,*,#45213,.T.);
#59658=ORIENTED_EDGE('',*,*,#45214,.F.);
#59659=ORIENTED_EDGE('',*,*,#45215,.F.);
#59660=ORIENTED_EDGE('',*,*,#45216,.T.);
#59661=ORIENTED_EDGE('',*,*,#45217,.T.);
#59662=ORIENTED_EDGE('',*,*,#45218,.F.);
#59663=ORIENTED_EDGE('',*,*,#45219,.F.);
#59664=ORIENTED_EDGE('',*,*,#45220,.F.);
#59665=ORIENTED_EDGE('',*,*,#45214,.T.);
#59666=ORIENTED_EDGE('',*,*,#45221,.F.);
#59667=ORIENTED_EDGE('',*,*,#45222,.F.);
#59668=ORIENTED_EDGE('',*,*,#45223,.F.);
#59669=ORIENTED_EDGE('',*,*,#45219,.T.);
#59670=ORIENTED_EDGE('',*,*,#45224,.F.);
#59671=ORIENTED_EDGE('',*,*,#45217,.F.);
#59672=ORIENTED_EDGE('',*,*,#45225,.T.);
#59673=ORIENTED_EDGE('',*,*,#45226,.F.);
#59674=ORIENTED_EDGE('',*,*,#45222,.T.);
#59675=ORIENTED_EDGE('',*,*,#45227,.F.);
#59676=ORIENTED_EDGE('',*,*,#45215,.T.);
#59677=ORIENTED_EDGE('',*,*,#45220,.T.);
#59678=ORIENTED_EDGE('',*,*,#45223,.T.);
#59679=ORIENTED_EDGE('',*,*,#45226,.T.);
#59680=ORIENTED_EDGE('',*,*,#45228,.T.);
#59681=ORIENTED_EDGE('',*,*,#45229,.F.);
#59682=ORIENTED_EDGE('',*,*,#45230,.F.);
#59683=ORIENTED_EDGE('',*,*,#45231,.T.);
#59684=ORIENTED_EDGE('',*,*,#45232,.T.);
#59685=ORIENTED_EDGE('',*,*,#45233,.F.);
#59686=ORIENTED_EDGE('',*,*,#45234,.F.);
#59687=ORIENTED_EDGE('',*,*,#45235,.F.);
#59688=ORIENTED_EDGE('',*,*,#45229,.T.);
#59689=ORIENTED_EDGE('',*,*,#45236,.F.);
#59690=ORIENTED_EDGE('',*,*,#45237,.F.);
#59691=ORIENTED_EDGE('',*,*,#45238,.F.);
#59692=ORIENTED_EDGE('',*,*,#45234,.T.);
#59693=ORIENTED_EDGE('',*,*,#45239,.F.);
#59694=ORIENTED_EDGE('',*,*,#45232,.F.);
#59695=ORIENTED_EDGE('',*,*,#45240,.T.);
#59696=ORIENTED_EDGE('',*,*,#45241,.F.);
#59697=ORIENTED_EDGE('',*,*,#45237,.T.);
#59698=ORIENTED_EDGE('',*,*,#45242,.F.);
#59699=ORIENTED_EDGE('',*,*,#45230,.T.);
#59700=ORIENTED_EDGE('',*,*,#45235,.T.);
#59701=ORIENTED_EDGE('',*,*,#45238,.T.);
#59702=ORIENTED_EDGE('',*,*,#45241,.T.);
#59703=ORIENTED_EDGE('',*,*,#45243,.T.);
#59704=ORIENTED_EDGE('',*,*,#45244,.F.);
#59705=ORIENTED_EDGE('',*,*,#45245,.T.);
#59706=ORIENTED_EDGE('',*,*,#45246,.T.);
#59707=ORIENTED_EDGE('',*,*,#45247,.F.);
#59708=ORIENTED_EDGE('',*,*,#45248,.F.);
#59709=ORIENTED_EDGE('',*,*,#45249,.F.);
#59710=ORIENTED_EDGE('',*,*,#45250,.T.);
#59711=ORIENTED_EDGE('',*,*,#45244,.T.);
#59712=ORIENTED_EDGE('',*,*,#45251,.F.);
#59713=ORIENTED_EDGE('',*,*,#45252,.F.);
#59714=ORIENTED_EDGE('',*,*,#45253,.F.);
#59715=ORIENTED_EDGE('',*,*,#45248,.T.);
#59716=ORIENTED_EDGE('',*,*,#45254,.F.);
#59717=ORIENTED_EDGE('',*,*,#45246,.F.);
#59718=ORIENTED_EDGE('',*,*,#45255,.T.);
#59719=ORIENTED_EDGE('',*,*,#45256,.F.);
#59720=ORIENTED_EDGE('',*,*,#45252,.T.);
#59721=ORIENTED_EDGE('',*,*,#45257,.F.);
#59722=ORIENTED_EDGE('',*,*,#45249,.T.);
#59723=ORIENTED_EDGE('',*,*,#45253,.T.);
#59724=ORIENTED_EDGE('',*,*,#45256,.T.);
#59725=ORIENTED_EDGE('',*,*,#45258,.T.);
#59726=ORIENTED_EDGE('',*,*,#45259,.F.);
#59727=ORIENTED_EDGE('',*,*,#45260,.T.);
#59728=ORIENTED_EDGE('',*,*,#45261,.T.);
#59729=ORIENTED_EDGE('',*,*,#45262,.F.);
#59730=ORIENTED_EDGE('',*,*,#45263,.F.);
#59731=ORIENTED_EDGE('',*,*,#45264,.F.);
#59732=ORIENTED_EDGE('',*,*,#45265,.T.);
#59733=ORIENTED_EDGE('',*,*,#45259,.T.);
#59734=ORIENTED_EDGE('',*,*,#45266,.F.);
#59735=ORIENTED_EDGE('',*,*,#45267,.F.);
#59736=ORIENTED_EDGE('',*,*,#45268,.F.);
#59737=ORIENTED_EDGE('',*,*,#45263,.T.);
#59738=ORIENTED_EDGE('',*,*,#45269,.F.);
#59739=ORIENTED_EDGE('',*,*,#45261,.F.);
#59740=ORIENTED_EDGE('',*,*,#45270,.T.);
#59741=ORIENTED_EDGE('',*,*,#45271,.F.);
#59742=ORIENTED_EDGE('',*,*,#45267,.T.);
#59743=ORIENTED_EDGE('',*,*,#45272,.F.);
#59744=ORIENTED_EDGE('',*,*,#45264,.T.);
#59745=ORIENTED_EDGE('',*,*,#45268,.T.);
#59746=ORIENTED_EDGE('',*,*,#45271,.T.);
#59747=ORIENTED_EDGE('',*,*,#45273,.T.);
#59748=ORIENTED_EDGE('',*,*,#45274,.F.);
#59749=ORIENTED_EDGE('',*,*,#45275,.T.);
#59750=ORIENTED_EDGE('',*,*,#45276,.T.);
#59751=ORIENTED_EDGE('',*,*,#45277,.F.);
#59752=ORIENTED_EDGE('',*,*,#45278,.F.);
#59753=ORIENTED_EDGE('',*,*,#45279,.F.);
#59754=ORIENTED_EDGE('',*,*,#45280,.T.);
#59755=ORIENTED_EDGE('',*,*,#45274,.T.);
#59756=ORIENTED_EDGE('',*,*,#45281,.F.);
#59757=ORIENTED_EDGE('',*,*,#45282,.F.);
#59758=ORIENTED_EDGE('',*,*,#45283,.F.);
#59759=ORIENTED_EDGE('',*,*,#45278,.T.);
#59760=ORIENTED_EDGE('',*,*,#45284,.F.);
#59761=ORIENTED_EDGE('',*,*,#45276,.F.);
#59762=ORIENTED_EDGE('',*,*,#45285,.T.);
#59763=ORIENTED_EDGE('',*,*,#45286,.F.);
#59764=ORIENTED_EDGE('',*,*,#45282,.T.);
#59765=ORIENTED_EDGE('',*,*,#45287,.F.);
#59766=ORIENTED_EDGE('',*,*,#45279,.T.);
#59767=ORIENTED_EDGE('',*,*,#45283,.T.);
#59768=ORIENTED_EDGE('',*,*,#45286,.T.);
#59769=ORIENTED_EDGE('',*,*,#45288,.T.);
#59770=ORIENTED_EDGE('',*,*,#45289,.F.);
#59771=ORIENTED_EDGE('',*,*,#45290,.T.);
#59772=ORIENTED_EDGE('',*,*,#45291,.T.);
#59773=ORIENTED_EDGE('',*,*,#45292,.F.);
#59774=ORIENTED_EDGE('',*,*,#45293,.F.);
#59775=ORIENTED_EDGE('',*,*,#45294,.T.);
#59776=ORIENTED_EDGE('',*,*,#45289,.T.);
#59777=ORIENTED_EDGE('',*,*,#45295,.F.);
#59778=ORIENTED_EDGE('',*,*,#45296,.F.);
#59779=ORIENTED_EDGE('',*,*,#45297,.T.);
#59780=ORIENTED_EDGE('',*,*,#45293,.T.);
#59781=ORIENTED_EDGE('',*,*,#45298,.F.);
#59782=ORIENTED_EDGE('',*,*,#45291,.F.);
#59783=ORIENTED_EDGE('',*,*,#45299,.T.);
#59784=ORIENTED_EDGE('',*,*,#45296,.T.);
#59785=ORIENTED_EDGE('',*,*,#45300,.F.);
#59786=ORIENTED_EDGE('',*,*,#45301,.F.);
#59787=ORIENTED_EDGE('',*,*,#45302,.T.);
#59788=ORIENTED_EDGE('',*,*,#45303,.T.);
#59789=ORIENTED_EDGE('',*,*,#45304,.F.);
#59790=ORIENTED_EDGE('',*,*,#45305,.F.);
#59791=ORIENTED_EDGE('',*,*,#45306,.T.);
#59792=ORIENTED_EDGE('',*,*,#45301,.T.);
#59793=ORIENTED_EDGE('',*,*,#45307,.F.);
#59794=ORIENTED_EDGE('',*,*,#45308,.F.);
#59795=ORIENTED_EDGE('',*,*,#45309,.T.);
#59796=ORIENTED_EDGE('',*,*,#45305,.T.);
#59797=ORIENTED_EDGE('',*,*,#45310,.F.);
#59798=ORIENTED_EDGE('',*,*,#45303,.F.);
#59799=ORIENTED_EDGE('',*,*,#45311,.T.);
#59800=ORIENTED_EDGE('',*,*,#45308,.T.);
#59801=ORIENTED_EDGE('',*,*,#45312,.F.);
#59802=ORIENTED_EDGE('',*,*,#45313,.F.);
#59803=ORIENTED_EDGE('',*,*,#45314,.T.);
#59804=ORIENTED_EDGE('',*,*,#45315,.T.);
#59805=ORIENTED_EDGE('',*,*,#45316,.F.);
#59806=ORIENTED_EDGE('',*,*,#45317,.F.);
#59807=ORIENTED_EDGE('',*,*,#45318,.T.);
#59808=ORIENTED_EDGE('',*,*,#45313,.T.);
#59809=ORIENTED_EDGE('',*,*,#45319,.F.);
#59810=ORIENTED_EDGE('',*,*,#45320,.F.);
#59811=ORIENTED_EDGE('',*,*,#45321,.T.);
#59812=ORIENTED_EDGE('',*,*,#45317,.T.);
#59813=ORIENTED_EDGE('',*,*,#45322,.F.);
#59814=ORIENTED_EDGE('',*,*,#45315,.F.);
#59815=ORIENTED_EDGE('',*,*,#45323,.T.);
#59816=ORIENTED_EDGE('',*,*,#45320,.T.);
#59817=ORIENTED_EDGE('',*,*,#45324,.F.);
#59818=ORIENTED_EDGE('',*,*,#45325,.F.);
#59819=ORIENTED_EDGE('',*,*,#45326,.T.);
#59820=ORIENTED_EDGE('',*,*,#45327,.T.);
#59821=ORIENTED_EDGE('',*,*,#45328,.F.);
#59822=ORIENTED_EDGE('',*,*,#45329,.F.);
#59823=ORIENTED_EDGE('',*,*,#45330,.T.);
#59824=ORIENTED_EDGE('',*,*,#45325,.T.);
#59825=ORIENTED_EDGE('',*,*,#45331,.F.);
#59826=ORIENTED_EDGE('',*,*,#45332,.F.);
#59827=ORIENTED_EDGE('',*,*,#45333,.T.);
#59828=ORIENTED_EDGE('',*,*,#45329,.T.);
#59829=ORIENTED_EDGE('',*,*,#45334,.F.);
#59830=ORIENTED_EDGE('',*,*,#45327,.F.);
#59831=ORIENTED_EDGE('',*,*,#45335,.T.);
#59832=ORIENTED_EDGE('',*,*,#45332,.T.);
#59833=ORIENTED_EDGE('',*,*,#45336,.F.);
#59834=ORIENTED_EDGE('',*,*,#45337,.F.);
#59835=ORIENTED_EDGE('',*,*,#45338,.T.);
#59836=ORIENTED_EDGE('',*,*,#45339,.T.);
#59837=ORIENTED_EDGE('',*,*,#45340,.F.);
#59838=ORIENTED_EDGE('',*,*,#45341,.F.);
#59839=ORIENTED_EDGE('',*,*,#45342,.T.);
#59840=ORIENTED_EDGE('',*,*,#45337,.T.);
#59841=ORIENTED_EDGE('',*,*,#45343,.F.);
#59842=ORIENTED_EDGE('',*,*,#45344,.F.);
#59843=ORIENTED_EDGE('',*,*,#45345,.T.);
#59844=ORIENTED_EDGE('',*,*,#45341,.T.);
#59845=ORIENTED_EDGE('',*,*,#45346,.F.);
#59846=ORIENTED_EDGE('',*,*,#45339,.F.);
#59847=ORIENTED_EDGE('',*,*,#45347,.T.);
#59848=ORIENTED_EDGE('',*,*,#45344,.T.);
#59849=ORIENTED_EDGE('',*,*,#45348,.F.);
#59850=ORIENTED_EDGE('',*,*,#45349,.F.);
#59851=ORIENTED_EDGE('',*,*,#45350,.T.);
#59852=ORIENTED_EDGE('',*,*,#45351,.T.);
#59853=ORIENTED_EDGE('',*,*,#45352,.F.);
#59854=ORIENTED_EDGE('',*,*,#45353,.F.);
#59855=ORIENTED_EDGE('',*,*,#45354,.T.);
#59856=ORIENTED_EDGE('',*,*,#45349,.T.);
#59857=ORIENTED_EDGE('',*,*,#45355,.F.);
#59858=ORIENTED_EDGE('',*,*,#45356,.F.);
#59859=ORIENTED_EDGE('',*,*,#45357,.T.);
#59860=ORIENTED_EDGE('',*,*,#45353,.T.);
#59861=ORIENTED_EDGE('',*,*,#45358,.F.);
#59862=ORIENTED_EDGE('',*,*,#45351,.F.);
#59863=ORIENTED_EDGE('',*,*,#45359,.T.);
#59864=ORIENTED_EDGE('',*,*,#45356,.T.);
#59865=ORIENTED_EDGE('',*,*,#45360,.F.);
#59866=ORIENTED_EDGE('',*,*,#45361,.F.);
#59867=ORIENTED_EDGE('',*,*,#45362,.T.);
#59868=ORIENTED_EDGE('',*,*,#45363,.T.);
#59869=ORIENTED_EDGE('',*,*,#45364,.F.);
#59870=ORIENTED_EDGE('',*,*,#45365,.F.);
#59871=ORIENTED_EDGE('',*,*,#45366,.T.);
#59872=ORIENTED_EDGE('',*,*,#45361,.T.);
#59873=ORIENTED_EDGE('',*,*,#45367,.F.);
#59874=ORIENTED_EDGE('',*,*,#45368,.F.);
#59875=ORIENTED_EDGE('',*,*,#45369,.T.);
#59876=ORIENTED_EDGE('',*,*,#45365,.T.);
#59877=ORIENTED_EDGE('',*,*,#45370,.F.);
#59878=ORIENTED_EDGE('',*,*,#45363,.F.);
#59879=ORIENTED_EDGE('',*,*,#45371,.T.);
#59880=ORIENTED_EDGE('',*,*,#45368,.T.);
#59881=ORIENTED_EDGE('',*,*,#45372,.F.);
#59882=ORIENTED_EDGE('',*,*,#45373,.F.);
#59883=ORIENTED_EDGE('',*,*,#45374,.T.);
#59884=ORIENTED_EDGE('',*,*,#45375,.T.);
#59885=ORIENTED_EDGE('',*,*,#45376,.F.);
#59886=ORIENTED_EDGE('',*,*,#45377,.F.);
#59887=ORIENTED_EDGE('',*,*,#45378,.T.);
#59888=ORIENTED_EDGE('',*,*,#45373,.T.);
#59889=ORIENTED_EDGE('',*,*,#45379,.F.);
#59890=ORIENTED_EDGE('',*,*,#45380,.F.);
#59891=ORIENTED_EDGE('',*,*,#45381,.T.);
#59892=ORIENTED_EDGE('',*,*,#45377,.T.);
#59893=ORIENTED_EDGE('',*,*,#45382,.F.);
#59894=ORIENTED_EDGE('',*,*,#45375,.F.);
#59895=ORIENTED_EDGE('',*,*,#45383,.T.);
#59896=ORIENTED_EDGE('',*,*,#45380,.T.);
#59897=ORIENTED_EDGE('',*,*,#45384,.F.);
#59898=ORIENTED_EDGE('',*,*,#45385,.F.);
#59899=ORIENTED_EDGE('',*,*,#45386,.F.);
#59900=ORIENTED_EDGE('',*,*,#45387,.T.);
#59901=ORIENTED_EDGE('',*,*,#45388,.T.);
#59902=ORIENTED_EDGE('',*,*,#45389,.F.);
#59903=ORIENTED_EDGE('',*,*,#45390,.F.);
#59904=ORIENTED_EDGE('',*,*,#45391,.F.);
#59905=ORIENTED_EDGE('',*,*,#45385,.T.);
#59906=ORIENTED_EDGE('',*,*,#45392,.F.);
#59907=ORIENTED_EDGE('',*,*,#45393,.F.);
#59908=ORIENTED_EDGE('',*,*,#45394,.F.);
#59909=ORIENTED_EDGE('',*,*,#45390,.T.);
#59910=ORIENTED_EDGE('',*,*,#45395,.F.);
#59911=ORIENTED_EDGE('',*,*,#45388,.F.);
#59912=ORIENTED_EDGE('',*,*,#45396,.T.);
#59913=ORIENTED_EDGE('',*,*,#45397,.F.);
#59914=ORIENTED_EDGE('',*,*,#45393,.T.);
#59915=ORIENTED_EDGE('',*,*,#45398,.F.);
#59916=ORIENTED_EDGE('',*,*,#45386,.T.);
#59917=ORIENTED_EDGE('',*,*,#45391,.T.);
#59918=ORIENTED_EDGE('',*,*,#45394,.T.);
#59919=ORIENTED_EDGE('',*,*,#45397,.T.);
#59920=ORIENTED_EDGE('',*,*,#45399,.T.);
#59921=ORIENTED_EDGE('',*,*,#45400,.F.);
#59922=ORIENTED_EDGE('',*,*,#45401,.F.);
#59923=ORIENTED_EDGE('',*,*,#45402,.T.);
#59924=ORIENTED_EDGE('',*,*,#45403,.T.);
#59925=ORIENTED_EDGE('',*,*,#45404,.F.);
#59926=ORIENTED_EDGE('',*,*,#45405,.F.);
#59927=ORIENTED_EDGE('',*,*,#45406,.F.);
#59928=ORIENTED_EDGE('',*,*,#45400,.T.);
#59929=ORIENTED_EDGE('',*,*,#45407,.F.);
#59930=ORIENTED_EDGE('',*,*,#45408,.F.);
#59931=ORIENTED_EDGE('',*,*,#45409,.F.);
#59932=ORIENTED_EDGE('',*,*,#45405,.T.);
#59933=ORIENTED_EDGE('',*,*,#45410,.F.);
#59934=ORIENTED_EDGE('',*,*,#45403,.F.);
#59935=ORIENTED_EDGE('',*,*,#45411,.T.);
#59936=ORIENTED_EDGE('',*,*,#45412,.F.);
#59937=ORIENTED_EDGE('',*,*,#45408,.T.);
#59938=ORIENTED_EDGE('',*,*,#45413,.F.);
#59939=ORIENTED_EDGE('',*,*,#45401,.T.);
#59940=ORIENTED_EDGE('',*,*,#45406,.T.);
#59941=ORIENTED_EDGE('',*,*,#45409,.T.);
#59942=ORIENTED_EDGE('',*,*,#45412,.T.);
#59943=ORIENTED_EDGE('',*,*,#45414,.T.);
#59944=ORIENTED_EDGE('',*,*,#45415,.F.);
#59945=ORIENTED_EDGE('',*,*,#45416,.T.);
#59946=ORIENTED_EDGE('',*,*,#45417,.T.);
#59947=ORIENTED_EDGE('',*,*,#45418,.F.);
#59948=ORIENTED_EDGE('',*,*,#45419,.F.);
#59949=ORIENTED_EDGE('',*,*,#45420,.T.);
#59950=ORIENTED_EDGE('',*,*,#45415,.T.);
#59951=ORIENTED_EDGE('',*,*,#45421,.F.);
#59952=ORIENTED_EDGE('',*,*,#45422,.F.);
#59953=ORIENTED_EDGE('',*,*,#45423,.T.);
#59954=ORIENTED_EDGE('',*,*,#45419,.T.);
#59955=ORIENTED_EDGE('',*,*,#45424,.F.);
#59956=ORIENTED_EDGE('',*,*,#45417,.F.);
#59957=ORIENTED_EDGE('',*,*,#45425,.T.);
#59958=ORIENTED_EDGE('',*,*,#45422,.T.);
#59959=ORIENTED_EDGE('',*,*,#45426,.F.);
#59960=ORIENTED_EDGE('',*,*,#45427,.F.);
#59961=ORIENTED_EDGE('',*,*,#45428,.T.);
#59962=ORIENTED_EDGE('',*,*,#45429,.T.);
#59963=ORIENTED_EDGE('',*,*,#45430,.F.);
#59964=ORIENTED_EDGE('',*,*,#45431,.F.);
#59965=ORIENTED_EDGE('',*,*,#45432,.T.);
#59966=ORIENTED_EDGE('',*,*,#45427,.T.);
#59967=ORIENTED_EDGE('',*,*,#45433,.F.);
#59968=ORIENTED_EDGE('',*,*,#45434,.F.);
#59969=ORIENTED_EDGE('',*,*,#45435,.T.);
#59970=ORIENTED_EDGE('',*,*,#45431,.T.);
#59971=ORIENTED_EDGE('',*,*,#45436,.F.);
#59972=ORIENTED_EDGE('',*,*,#45429,.F.);
#59973=ORIENTED_EDGE('',*,*,#45437,.T.);
#59974=ORIENTED_EDGE('',*,*,#45434,.T.);
#59975=ORIENTED_EDGE('',*,*,#45438,.F.);
#59976=ORIENTED_EDGE('',*,*,#45439,.F.);
#59977=ORIENTED_EDGE('',*,*,#45440,.T.);
#59978=ORIENTED_EDGE('',*,*,#45441,.T.);
#59979=ORIENTED_EDGE('',*,*,#45442,.F.);
#59980=ORIENTED_EDGE('',*,*,#45443,.F.);
#59981=ORIENTED_EDGE('',*,*,#45444,.T.);
#59982=ORIENTED_EDGE('',*,*,#45439,.T.);
#59983=ORIENTED_EDGE('',*,*,#45445,.F.);
#59984=ORIENTED_EDGE('',*,*,#45446,.F.);
#59985=ORIENTED_EDGE('',*,*,#45447,.T.);
#59986=ORIENTED_EDGE('',*,*,#45443,.T.);
#59987=ORIENTED_EDGE('',*,*,#45448,.F.);
#59988=ORIENTED_EDGE('',*,*,#45441,.F.);
#59989=ORIENTED_EDGE('',*,*,#45449,.T.);
#59990=ORIENTED_EDGE('',*,*,#45446,.T.);
#59991=ORIENTED_EDGE('',*,*,#45450,.F.);
#59992=ORIENTED_EDGE('',*,*,#45451,.F.);
#59993=ORIENTED_EDGE('',*,*,#45452,.T.);
#59994=ORIENTED_EDGE('',*,*,#45453,.T.);
#59995=ORIENTED_EDGE('',*,*,#45454,.F.);
#59996=ORIENTED_EDGE('',*,*,#45455,.F.);
#59997=ORIENTED_EDGE('',*,*,#45456,.T.);
#59998=ORIENTED_EDGE('',*,*,#45451,.T.);
#59999=ORIENTED_EDGE('',*,*,#45457,.F.);
#60000=ORIENTED_EDGE('',*,*,#45458,.F.);
#60001=ORIENTED_EDGE('',*,*,#45459,.T.);
#60002=ORIENTED_EDGE('',*,*,#45455,.T.);
#60003=ORIENTED_EDGE('',*,*,#45460,.F.);
#60004=ORIENTED_EDGE('',*,*,#45453,.F.);
#60005=ORIENTED_EDGE('',*,*,#45461,.T.);
#60006=ORIENTED_EDGE('',*,*,#45458,.T.);
#60007=ORIENTED_EDGE('',*,*,#45462,.F.);
#60008=ORIENTED_EDGE('',*,*,#45463,.F.);
#60009=ORIENTED_EDGE('',*,*,#45464,.T.);
#60010=ORIENTED_EDGE('',*,*,#45465,.T.);
#60011=ORIENTED_EDGE('',*,*,#45466,.F.);
#60012=ORIENTED_EDGE('',*,*,#45467,.F.);
#60013=ORIENTED_EDGE('',*,*,#45468,.T.);
#60014=ORIENTED_EDGE('',*,*,#45463,.T.);
#60015=ORIENTED_EDGE('',*,*,#45469,.F.);
#60016=ORIENTED_EDGE('',*,*,#45470,.F.);
#60017=ORIENTED_EDGE('',*,*,#45471,.F.);
#60018=ORIENTED_EDGE('',*,*,#45472,.T.);
#60019=ORIENTED_EDGE('',*,*,#45467,.T.);
#60020=ORIENTED_EDGE('',*,*,#45473,.F.);
#60021=ORIENTED_EDGE('',*,*,#45465,.F.);
#60022=ORIENTED_EDGE('',*,*,#45474,.T.);
#60023=ORIENTED_EDGE('',*,*,#45475,.F.);
#60024=ORIENTED_EDGE('',*,*,#45470,.T.);
#60025=ORIENTED_EDGE('',*,*,#45476,.F.);
#60026=ORIENTED_EDGE('',*,*,#45471,.T.);
#60027=ORIENTED_EDGE('',*,*,#45475,.T.);
#60028=ORIENTED_EDGE('',*,*,#45477,.T.);
#60029=ORIENTED_EDGE('',*,*,#45478,.F.);
#60030=ORIENTED_EDGE('',*,*,#45479,.T.);
#60031=ORIENTED_EDGE('',*,*,#45480,.T.);
#60032=ORIENTED_EDGE('',*,*,#45481,.F.);
#60033=ORIENTED_EDGE('',*,*,#45482,.F.);
#60034=ORIENTED_EDGE('',*,*,#45483,.F.);
#60035=ORIENTED_EDGE('',*,*,#45484,.T.);
#60036=ORIENTED_EDGE('',*,*,#45478,.T.);
#60037=ORIENTED_EDGE('',*,*,#45485,.F.);
#60038=ORIENTED_EDGE('',*,*,#45486,.F.);
#60039=ORIENTED_EDGE('',*,*,#45487,.F.);
#60040=ORIENTED_EDGE('',*,*,#45482,.T.);
#60041=ORIENTED_EDGE('',*,*,#45488,.F.);
#60042=ORIENTED_EDGE('',*,*,#45480,.F.);
#60043=ORIENTED_EDGE('',*,*,#45489,.T.);
#60044=ORIENTED_EDGE('',*,*,#45490,.F.);
#60045=ORIENTED_EDGE('',*,*,#45486,.T.);
#60046=ORIENTED_EDGE('',*,*,#45491,.F.);
#60047=ORIENTED_EDGE('',*,*,#45483,.T.);
#60048=ORIENTED_EDGE('',*,*,#45487,.T.);
#60049=ORIENTED_EDGE('',*,*,#45490,.T.);
#60050=ORIENTED_EDGE('',*,*,#45492,.T.);
#60051=ORIENTED_EDGE('',*,*,#45493,.F.);
#60052=ORIENTED_EDGE('',*,*,#45494,.T.);
#60053=ORIENTED_EDGE('',*,*,#45495,.T.);
#60054=ORIENTED_EDGE('',*,*,#45496,.F.);
#60055=ORIENTED_EDGE('',*,*,#45497,.F.);
#60056=ORIENTED_EDGE('',*,*,#45498,.F.);
#60057=ORIENTED_EDGE('',*,*,#45499,.T.);
#60058=ORIENTED_EDGE('',*,*,#45493,.T.);
#60059=ORIENTED_EDGE('',*,*,#45500,.F.);
#60060=ORIENTED_EDGE('',*,*,#45501,.F.);
#60061=ORIENTED_EDGE('',*,*,#45502,.F.);
#60062=ORIENTED_EDGE('',*,*,#45497,.T.);
#60063=ORIENTED_EDGE('',*,*,#45503,.F.);
#60064=ORIENTED_EDGE('',*,*,#45495,.F.);
#60065=ORIENTED_EDGE('',*,*,#45504,.T.);
#60066=ORIENTED_EDGE('',*,*,#45505,.F.);
#60067=ORIENTED_EDGE('',*,*,#45501,.T.);
#60068=ORIENTED_EDGE('',*,*,#45506,.F.);
#60069=ORIENTED_EDGE('',*,*,#45498,.T.);
#60070=ORIENTED_EDGE('',*,*,#45502,.T.);
#60071=ORIENTED_EDGE('',*,*,#45505,.T.);
#60072=ORIENTED_EDGE('',*,*,#45507,.T.);
#60073=ORIENTED_EDGE('',*,*,#45508,.F.);
#60074=ORIENTED_EDGE('',*,*,#45509,.T.);
#60075=ORIENTED_EDGE('',*,*,#45510,.T.);
#60076=ORIENTED_EDGE('',*,*,#45511,.F.);
#60077=ORIENTED_EDGE('',*,*,#45512,.F.);
#60078=ORIENTED_EDGE('',*,*,#45513,.T.);
#60079=ORIENTED_EDGE('',*,*,#45508,.T.);
#60080=ORIENTED_EDGE('',*,*,#45514,.F.);
#60081=ORIENTED_EDGE('',*,*,#45515,.F.);
#60082=ORIENTED_EDGE('',*,*,#45516,.F.);
#60083=ORIENTED_EDGE('',*,*,#45517,.T.);
#60084=ORIENTED_EDGE('',*,*,#45512,.T.);
#60085=ORIENTED_EDGE('',*,*,#45518,.F.);
#60086=ORIENTED_EDGE('',*,*,#45510,.F.);
#60087=ORIENTED_EDGE('',*,*,#45519,.T.);
#60088=ORIENTED_EDGE('',*,*,#45520,.F.);
#60089=ORIENTED_EDGE('',*,*,#45515,.T.);
#60090=ORIENTED_EDGE('',*,*,#45521,.F.);
#60091=ORIENTED_EDGE('',*,*,#45516,.T.);
#60092=ORIENTED_EDGE('',*,*,#45520,.T.);
#60093=ORIENTED_EDGE('',*,*,#45522,.T.);
#60094=ORIENTED_EDGE('',*,*,#45523,.F.);
#60095=ORIENTED_EDGE('',*,*,#45524,.T.);
#60096=ORIENTED_EDGE('',*,*,#45525,.T.);
#60097=ORIENTED_EDGE('',*,*,#45526,.F.);
#60098=ORIENTED_EDGE('',*,*,#45527,.F.);
#60099=ORIENTED_EDGE('',*,*,#45528,.T.);
#60100=ORIENTED_EDGE('',*,*,#45523,.T.);
#60101=ORIENTED_EDGE('',*,*,#45529,.F.);
#60102=ORIENTED_EDGE('',*,*,#45530,.F.);
#60103=ORIENTED_EDGE('',*,*,#45531,.T.);
#60104=ORIENTED_EDGE('',*,*,#45527,.T.);
#60105=ORIENTED_EDGE('',*,*,#45532,.F.);
#60106=ORIENTED_EDGE('',*,*,#45525,.F.);
#60107=ORIENTED_EDGE('',*,*,#45533,.T.);
#60108=ORIENTED_EDGE('',*,*,#45530,.T.);
#60109=ORIENTED_EDGE('',*,*,#45534,.F.);
#60110=ORIENTED_EDGE('',*,*,#45535,.F.);
#60111=ORIENTED_EDGE('',*,*,#45536,.T.);
#60112=ORIENTED_EDGE('',*,*,#45537,.T.);
#60113=ORIENTED_EDGE('',*,*,#45538,.F.);
#60114=ORIENTED_EDGE('',*,*,#45539,.F.);
#60115=ORIENTED_EDGE('',*,*,#45540,.T.);
#60116=ORIENTED_EDGE('',*,*,#45535,.T.);
#60117=ORIENTED_EDGE('',*,*,#45541,.F.);
#60118=ORIENTED_EDGE('',*,*,#45542,.F.);
#60119=ORIENTED_EDGE('',*,*,#45543,.T.);
#60120=ORIENTED_EDGE('',*,*,#45539,.T.);
#60121=ORIENTED_EDGE('',*,*,#45544,.F.);
#60122=ORIENTED_EDGE('',*,*,#45537,.F.);
#60123=ORIENTED_EDGE('',*,*,#45545,.T.);
#60124=ORIENTED_EDGE('',*,*,#45542,.T.);
#60125=ORIENTED_EDGE('',*,*,#45546,.F.);
#60126=ORIENTED_EDGE('',*,*,#45547,.F.);
#60127=ORIENTED_EDGE('',*,*,#45548,.T.);
#60128=ORIENTED_EDGE('',*,*,#45549,.T.);
#60129=ORIENTED_EDGE('',*,*,#45550,.F.);
#60130=ORIENTED_EDGE('',*,*,#45551,.F.);
#60131=ORIENTED_EDGE('',*,*,#45552,.T.);
#60132=ORIENTED_EDGE('',*,*,#45547,.T.);
#60133=ORIENTED_EDGE('',*,*,#45553,.F.);
#60134=ORIENTED_EDGE('',*,*,#45554,.F.);
#60135=ORIENTED_EDGE('',*,*,#45555,.T.);
#60136=ORIENTED_EDGE('',*,*,#45551,.T.);
#60137=ORIENTED_EDGE('',*,*,#45556,.F.);
#60138=ORIENTED_EDGE('',*,*,#45549,.F.);
#60139=ORIENTED_EDGE('',*,*,#45557,.T.);
#60140=ORIENTED_EDGE('',*,*,#45554,.T.);
#60141=ORIENTED_EDGE('',*,*,#45558,.F.);
#60142=ORIENTED_EDGE('',*,*,#45559,.F.);
#60143=ORIENTED_EDGE('',*,*,#45560,.T.);
#60144=ORIENTED_EDGE('',*,*,#45561,.T.);
#60145=ORIENTED_EDGE('',*,*,#45562,.F.);
#60146=ORIENTED_EDGE('',*,*,#45563,.F.);
#60147=ORIENTED_EDGE('',*,*,#45564,.T.);
#60148=ORIENTED_EDGE('',*,*,#45559,.T.);
#60149=ORIENTED_EDGE('',*,*,#45565,.F.);
#60150=ORIENTED_EDGE('',*,*,#45566,.F.);
#60151=ORIENTED_EDGE('',*,*,#45567,.T.);
#60152=ORIENTED_EDGE('',*,*,#45563,.T.);
#60153=ORIENTED_EDGE('',*,*,#45568,.F.);
#60154=ORIENTED_EDGE('',*,*,#45561,.F.);
#60155=ORIENTED_EDGE('',*,*,#45569,.T.);
#60156=ORIENTED_EDGE('',*,*,#45566,.T.);
#60157=ORIENTED_EDGE('',*,*,#45570,.F.);
#60158=ORIENTED_EDGE('',*,*,#45571,.F.);
#60159=ORIENTED_EDGE('',*,*,#45572,.T.);
#60160=ORIENTED_EDGE('',*,*,#45573,.T.);
#60161=ORIENTED_EDGE('',*,*,#45574,.F.);
#60162=ORIENTED_EDGE('',*,*,#45575,.F.);
#60163=ORIENTED_EDGE('',*,*,#45576,.T.);
#60164=ORIENTED_EDGE('',*,*,#45571,.T.);
#60165=ORIENTED_EDGE('',*,*,#45577,.F.);
#60166=ORIENTED_EDGE('',*,*,#45578,.F.);
#60167=ORIENTED_EDGE('',*,*,#45579,.T.);
#60168=ORIENTED_EDGE('',*,*,#45575,.T.);
#60169=ORIENTED_EDGE('',*,*,#45580,.F.);
#60170=ORIENTED_EDGE('',*,*,#45573,.F.);
#60171=ORIENTED_EDGE('',*,*,#45581,.T.);
#60172=ORIENTED_EDGE('',*,*,#45578,.T.);
#60173=ORIENTED_EDGE('',*,*,#45582,.F.);
#60174=ORIENTED_EDGE('',*,*,#45583,.F.);
#60175=ORIENTED_EDGE('',*,*,#45584,.T.);
#60176=ORIENTED_EDGE('',*,*,#45585,.T.);
#60177=ORIENTED_EDGE('',*,*,#45586,.F.);
#60178=ORIENTED_EDGE('',*,*,#45587,.F.);
#60179=ORIENTED_EDGE('',*,*,#45588,.T.);
#60180=ORIENTED_EDGE('',*,*,#45583,.T.);
#60181=ORIENTED_EDGE('',*,*,#45589,.F.);
#60182=ORIENTED_EDGE('',*,*,#45590,.F.);
#60183=ORIENTED_EDGE('',*,*,#45591,.T.);
#60184=ORIENTED_EDGE('',*,*,#45587,.T.);
#60185=ORIENTED_EDGE('',*,*,#45592,.F.);
#60186=ORIENTED_EDGE('',*,*,#45585,.F.);
#60187=ORIENTED_EDGE('',*,*,#45593,.T.);
#60188=ORIENTED_EDGE('',*,*,#45590,.T.);
#60189=ORIENTED_EDGE('',*,*,#45594,.F.);
#60190=ORIENTED_EDGE('',*,*,#45595,.F.);
#60191=ORIENTED_EDGE('',*,*,#45596,.T.);
#60192=ORIENTED_EDGE('',*,*,#45597,.T.);
#60193=ORIENTED_EDGE('',*,*,#45598,.F.);
#60194=ORIENTED_EDGE('',*,*,#45599,.F.);
#60195=ORIENTED_EDGE('',*,*,#45600,.T.);
#60196=ORIENTED_EDGE('',*,*,#45595,.T.);
#60197=ORIENTED_EDGE('',*,*,#45601,.F.);
#60198=ORIENTED_EDGE('',*,*,#45602,.F.);
#60199=ORIENTED_EDGE('',*,*,#45603,.T.);
#60200=ORIENTED_EDGE('',*,*,#45599,.T.);
#60201=ORIENTED_EDGE('',*,*,#45604,.F.);
#60202=ORIENTED_EDGE('',*,*,#45597,.F.);
#60203=ORIENTED_EDGE('',*,*,#45605,.T.);
#60204=ORIENTED_EDGE('',*,*,#45602,.T.);
#60205=ORIENTED_EDGE('',*,*,#45606,.F.);
#60206=ORIENTED_EDGE('',*,*,#45607,.F.);
#60207=ORIENTED_EDGE('',*,*,#45608,.T.);
#60208=ORIENTED_EDGE('',*,*,#45609,.T.);
#60209=ORIENTED_EDGE('',*,*,#45610,.F.);
#60210=ORIENTED_EDGE('',*,*,#45611,.F.);
#60211=ORIENTED_EDGE('',*,*,#45612,.T.);
#60212=ORIENTED_EDGE('',*,*,#45607,.T.);
#60213=ORIENTED_EDGE('',*,*,#45613,.F.);
#60214=ORIENTED_EDGE('',*,*,#45614,.F.);
#60215=ORIENTED_EDGE('',*,*,#45615,.T.);
#60216=ORIENTED_EDGE('',*,*,#45611,.T.);
#60217=ORIENTED_EDGE('',*,*,#45616,.F.);
#60218=ORIENTED_EDGE('',*,*,#45609,.F.);
#60219=ORIENTED_EDGE('',*,*,#45617,.T.);
#60220=ORIENTED_EDGE('',*,*,#45614,.T.);
#60221=ORIENTED_EDGE('',*,*,#45618,.F.);
#60222=ORIENTED_EDGE('',*,*,#45619,.F.);
#60223=ORIENTED_EDGE('',*,*,#45620,.T.);
#60224=ORIENTED_EDGE('',*,*,#45621,.T.);
#60225=ORIENTED_EDGE('',*,*,#45622,.F.);
#60226=ORIENTED_EDGE('',*,*,#45623,.F.);
#60227=ORIENTED_EDGE('',*,*,#45624,.T.);
#60228=ORIENTED_EDGE('',*,*,#45619,.T.);
#60229=ORIENTED_EDGE('',*,*,#45625,.F.);
#60230=ORIENTED_EDGE('',*,*,#45626,.F.);
#60231=ORIENTED_EDGE('',*,*,#45627,.T.);
#60232=ORIENTED_EDGE('',*,*,#45623,.T.);
#60233=ORIENTED_EDGE('',*,*,#45628,.F.);
#60234=ORIENTED_EDGE('',*,*,#45621,.F.);
#60235=ORIENTED_EDGE('',*,*,#45629,.T.);
#60236=ORIENTED_EDGE('',*,*,#45626,.T.);
#60237=ORIENTED_EDGE('',*,*,#45630,.F.);
#60238=ORIENTED_EDGE('',*,*,#45631,.F.);
#60239=ORIENTED_EDGE('',*,*,#45632,.T.);
#60240=ORIENTED_EDGE('',*,*,#45633,.T.);
#60241=ORIENTED_EDGE('',*,*,#45634,.F.);
#60242=ORIENTED_EDGE('',*,*,#45635,.F.);
#60243=ORIENTED_EDGE('',*,*,#45636,.T.);
#60244=ORIENTED_EDGE('',*,*,#45631,.T.);
#60245=ORIENTED_EDGE('',*,*,#45637,.F.);
#60246=ORIENTED_EDGE('',*,*,#45638,.F.);
#60247=ORIENTED_EDGE('',*,*,#45639,.T.);
#60248=ORIENTED_EDGE('',*,*,#45635,.T.);
#60249=ORIENTED_EDGE('',*,*,#45640,.F.);
#60250=ORIENTED_EDGE('',*,*,#45633,.F.);
#60251=ORIENTED_EDGE('',*,*,#45641,.T.);
#60252=ORIENTED_EDGE('',*,*,#45638,.T.);
#60253=ORIENTED_EDGE('',*,*,#45642,.F.);
#60254=ORIENTED_EDGE('',*,*,#45643,.F.);
#60255=ORIENTED_EDGE('',*,*,#45644,.T.);
#60256=ORIENTED_EDGE('',*,*,#45645,.T.);
#60257=ORIENTED_EDGE('',*,*,#45646,.F.);
#60258=ORIENTED_EDGE('',*,*,#45647,.F.);
#60259=ORIENTED_EDGE('',*,*,#45648,.T.);
#60260=ORIENTED_EDGE('',*,*,#45643,.T.);
#60261=ORIENTED_EDGE('',*,*,#45649,.F.);
#60262=ORIENTED_EDGE('',*,*,#45650,.F.);
#60263=ORIENTED_EDGE('',*,*,#45651,.F.);
#60264=ORIENTED_EDGE('',*,*,#45652,.T.);
#60265=ORIENTED_EDGE('',*,*,#45647,.T.);
#60266=ORIENTED_EDGE('',*,*,#45653,.F.);
#60267=ORIENTED_EDGE('',*,*,#45645,.F.);
#60268=ORIENTED_EDGE('',*,*,#45654,.T.);
#60269=ORIENTED_EDGE('',*,*,#45655,.F.);
#60270=ORIENTED_EDGE('',*,*,#45650,.T.);
#60271=ORIENTED_EDGE('',*,*,#45656,.F.);
#60272=ORIENTED_EDGE('',*,*,#45651,.T.);
#60273=ORIENTED_EDGE('',*,*,#45655,.T.);
#60274=ORIENTED_EDGE('',*,*,#45657,.T.);
#60275=ORIENTED_EDGE('',*,*,#45658,.F.);
#60276=ORIENTED_EDGE('',*,*,#45659,.T.);
#60277=ORIENTED_EDGE('',*,*,#45660,.T.);
#60278=ORIENTED_EDGE('',*,*,#45661,.F.);
#60279=ORIENTED_EDGE('',*,*,#45662,.F.);
#60280=ORIENTED_EDGE('',*,*,#45663,.T.);
#60281=ORIENTED_EDGE('',*,*,#45658,.T.);
#60282=ORIENTED_EDGE('',*,*,#45664,.F.);
#60283=ORIENTED_EDGE('',*,*,#45665,.F.);
#60284=ORIENTED_EDGE('',*,*,#45666,.F.);
#60285=ORIENTED_EDGE('',*,*,#45667,.T.);
#60286=ORIENTED_EDGE('',*,*,#45662,.T.);
#60287=ORIENTED_EDGE('',*,*,#45668,.F.);
#60288=ORIENTED_EDGE('',*,*,#45660,.F.);
#60289=ORIENTED_EDGE('',*,*,#45669,.T.);
#60290=ORIENTED_EDGE('',*,*,#45670,.F.);
#60291=ORIENTED_EDGE('',*,*,#45665,.T.);
#60292=ORIENTED_EDGE('',*,*,#45671,.F.);
#60293=ORIENTED_EDGE('',*,*,#45666,.T.);
#60294=ORIENTED_EDGE('',*,*,#45670,.T.);
#60295=ORIENTED_EDGE('',*,*,#45672,.T.);
#60296=ORIENTED_EDGE('',*,*,#45673,.F.);
#60297=ORIENTED_EDGE('',*,*,#45674,.T.);
#60298=ORIENTED_EDGE('',*,*,#45675,.T.);
#60299=ORIENTED_EDGE('',*,*,#45676,.F.);
#60300=ORIENTED_EDGE('',*,*,#45677,.F.);
#60301=ORIENTED_EDGE('',*,*,#45678,.T.);
#60302=ORIENTED_EDGE('',*,*,#45673,.T.);
#60303=ORIENTED_EDGE('',*,*,#45679,.F.);
#60304=ORIENTED_EDGE('',*,*,#45680,.F.);
#60305=ORIENTED_EDGE('',*,*,#45681,.T.);
#60306=ORIENTED_EDGE('',*,*,#45677,.T.);
#60307=ORIENTED_EDGE('',*,*,#45682,.F.);
#60308=ORIENTED_EDGE('',*,*,#45675,.F.);
#60309=ORIENTED_EDGE('',*,*,#45683,.T.);
#60310=ORIENTED_EDGE('',*,*,#45680,.T.);
#60311=ORIENTED_EDGE('',*,*,#45684,.F.);
#60312=ORIENTED_EDGE('',*,*,#45685,.F.);
#60313=ORIENTED_EDGE('',*,*,#45686,.T.);
#60314=ORIENTED_EDGE('',*,*,#45687,.T.);
#60315=ORIENTED_EDGE('',*,*,#45688,.F.);
#60316=ORIENTED_EDGE('',*,*,#45689,.F.);
#60317=ORIENTED_EDGE('',*,*,#45690,.T.);
#60318=ORIENTED_EDGE('',*,*,#45685,.T.);
#60319=ORIENTED_EDGE('',*,*,#45691,.F.);
#60320=ORIENTED_EDGE('',*,*,#45692,.F.);
#60321=ORIENTED_EDGE('',*,*,#45693,.T.);
#60322=ORIENTED_EDGE('',*,*,#45689,.T.);
#60323=ORIENTED_EDGE('',*,*,#45694,.F.);
#60324=ORIENTED_EDGE('',*,*,#45687,.F.);
#60325=ORIENTED_EDGE('',*,*,#45695,.T.);
#60326=ORIENTED_EDGE('',*,*,#45692,.T.);
#60327=ORIENTED_EDGE('',*,*,#45696,.F.);
#60328=ORIENTED_EDGE('',*,*,#45697,.F.);
#60329=ORIENTED_EDGE('',*,*,#45698,.T.);
#60330=ORIENTED_EDGE('',*,*,#45699,.T.);
#60331=ORIENTED_EDGE('',*,*,#45700,.F.);
#60332=ORIENTED_EDGE('',*,*,#45701,.F.);
#60333=ORIENTED_EDGE('',*,*,#45702,.T.);
#60334=ORIENTED_EDGE('',*,*,#45697,.T.);
#60335=ORIENTED_EDGE('',*,*,#45703,.F.);
#60336=ORIENTED_EDGE('',*,*,#45704,.F.);
#60337=ORIENTED_EDGE('',*,*,#45705,.T.);
#60338=ORIENTED_EDGE('',*,*,#45701,.T.);
#60339=ORIENTED_EDGE('',*,*,#45706,.F.);
#60340=ORIENTED_EDGE('',*,*,#45699,.F.);
#60341=ORIENTED_EDGE('',*,*,#45707,.T.);
#60342=ORIENTED_EDGE('',*,*,#45704,.T.);
#60343=ORIENTED_EDGE('',*,*,#45708,.F.);
#60344=ORIENTED_EDGE('',*,*,#45709,.F.);
#60345=ORIENTED_EDGE('',*,*,#45710,.T.);
#60346=ORIENTED_EDGE('',*,*,#45711,.T.);
#60347=ORIENTED_EDGE('',*,*,#45712,.F.);
#60348=ORIENTED_EDGE('',*,*,#45713,.F.);
#60349=ORIENTED_EDGE('',*,*,#45714,.T.);
#60350=ORIENTED_EDGE('',*,*,#45709,.T.);
#60351=ORIENTED_EDGE('',*,*,#45715,.F.);
#60352=ORIENTED_EDGE('',*,*,#45716,.F.);
#60353=ORIENTED_EDGE('',*,*,#45717,.T.);
#60354=ORIENTED_EDGE('',*,*,#45713,.T.);
#60355=ORIENTED_EDGE('',*,*,#45718,.F.);
#60356=ORIENTED_EDGE('',*,*,#45711,.F.);
#60357=ORIENTED_EDGE('',*,*,#45719,.T.);
#60358=ORIENTED_EDGE('',*,*,#45716,.T.);
#60359=ORIENTED_EDGE('',*,*,#45720,.F.);
#60360=ORIENTED_EDGE('',*,*,#45721,.F.);
#60361=ORIENTED_EDGE('',*,*,#45722,.T.);
#60362=ORIENTED_EDGE('',*,*,#45723,.T.);
#60363=ORIENTED_EDGE('',*,*,#45724,.F.);
#60364=ORIENTED_EDGE('',*,*,#45725,.F.);
#60365=ORIENTED_EDGE('',*,*,#45726,.T.);
#60366=ORIENTED_EDGE('',*,*,#45721,.T.);
#60367=ORIENTED_EDGE('',*,*,#45727,.F.);
#60368=ORIENTED_EDGE('',*,*,#45728,.F.);
#60369=ORIENTED_EDGE('',*,*,#45729,.T.);
#60370=ORIENTED_EDGE('',*,*,#45725,.T.);
#60371=ORIENTED_EDGE('',*,*,#45730,.F.);
#60372=ORIENTED_EDGE('',*,*,#45723,.F.);
#60373=ORIENTED_EDGE('',*,*,#45731,.T.);
#60374=ORIENTED_EDGE('',*,*,#45728,.T.);
#60375=ORIENTED_EDGE('',*,*,#45732,.F.);
#60376=ORIENTED_EDGE('',*,*,#45733,.F.);
#60377=ORIENTED_EDGE('',*,*,#45734,.T.);
#60378=ORIENTED_EDGE('',*,*,#45735,.T.);
#60379=ORIENTED_EDGE('',*,*,#45736,.F.);
#60380=ORIENTED_EDGE('',*,*,#45737,.F.);
#60381=ORIENTED_EDGE('',*,*,#45738,.T.);
#60382=ORIENTED_EDGE('',*,*,#45733,.T.);
#60383=ORIENTED_EDGE('',*,*,#45739,.F.);
#60384=ORIENTED_EDGE('',*,*,#45740,.F.);
#60385=ORIENTED_EDGE('',*,*,#45741,.T.);
#60386=ORIENTED_EDGE('',*,*,#45737,.T.);
#60387=ORIENTED_EDGE('',*,*,#45742,.F.);
#60388=ORIENTED_EDGE('',*,*,#45735,.F.);
#60389=ORIENTED_EDGE('',*,*,#45743,.T.);
#60390=ORIENTED_EDGE('',*,*,#45740,.T.);
#60391=ORIENTED_EDGE('',*,*,#45744,.F.);
#60392=ORIENTED_EDGE('',*,*,#45745,.F.);
#60393=ORIENTED_EDGE('',*,*,#45746,.T.);
#60394=ORIENTED_EDGE('',*,*,#45747,.T.);
#60395=ORIENTED_EDGE('',*,*,#45748,.F.);
#60396=ORIENTED_EDGE('',*,*,#45749,.F.);
#60397=ORIENTED_EDGE('',*,*,#45750,.T.);
#60398=ORIENTED_EDGE('',*,*,#45745,.T.);
#60399=ORIENTED_EDGE('',*,*,#45751,.F.);
#60400=ORIENTED_EDGE('',*,*,#45752,.F.);
#60401=ORIENTED_EDGE('',*,*,#45753,.T.);
#60402=ORIENTED_EDGE('',*,*,#45749,.T.);
#60403=ORIENTED_EDGE('',*,*,#45754,.F.);
#60404=ORIENTED_EDGE('',*,*,#45747,.F.);
#60405=ORIENTED_EDGE('',*,*,#45755,.T.);
#60406=ORIENTED_EDGE('',*,*,#45752,.T.);
#60407=ORIENTED_EDGE('',*,*,#45756,.F.);
#60408=ORIENTED_EDGE('',*,*,#45757,.F.);
#60409=ORIENTED_EDGE('',*,*,#45758,.T.);
#60410=ORIENTED_EDGE('',*,*,#45759,.T.);
#60411=ORIENTED_EDGE('',*,*,#45760,.F.);
#60412=ORIENTED_EDGE('',*,*,#45761,.F.);
#60413=ORIENTED_EDGE('',*,*,#45762,.T.);
#60414=ORIENTED_EDGE('',*,*,#45757,.T.);
#60415=ORIENTED_EDGE('',*,*,#45763,.F.);
#60416=ORIENTED_EDGE('',*,*,#45764,.F.);
#60417=ORIENTED_EDGE('',*,*,#45765,.T.);
#60418=ORIENTED_EDGE('',*,*,#45761,.T.);
#60419=ORIENTED_EDGE('',*,*,#45766,.F.);
#60420=ORIENTED_EDGE('',*,*,#45759,.F.);
#60421=ORIENTED_EDGE('',*,*,#45767,.T.);
#60422=ORIENTED_EDGE('',*,*,#45764,.T.);
#60423=ORIENTED_EDGE('',*,*,#45768,.F.);
#60424=ORIENTED_EDGE('',*,*,#45769,.F.);
#60425=ORIENTED_EDGE('',*,*,#45770,.T.);
#60426=ORIENTED_EDGE('',*,*,#45771,.T.);
#60427=ORIENTED_EDGE('',*,*,#45772,.F.);
#60428=ORIENTED_EDGE('',*,*,#45773,.F.);
#60429=ORIENTED_EDGE('',*,*,#45774,.T.);
#60430=ORIENTED_EDGE('',*,*,#45769,.T.);
#60431=ORIENTED_EDGE('',*,*,#45775,.F.);
#60432=ORIENTED_EDGE('',*,*,#45776,.F.);
#60433=ORIENTED_EDGE('',*,*,#45777,.T.);
#60434=ORIENTED_EDGE('',*,*,#45773,.T.);
#60435=ORIENTED_EDGE('',*,*,#45778,.F.);
#60436=ORIENTED_EDGE('',*,*,#45771,.F.);
#60437=ORIENTED_EDGE('',*,*,#45779,.T.);
#60438=ORIENTED_EDGE('',*,*,#45776,.T.);
#60439=ORIENTED_EDGE('',*,*,#45780,.F.);
#60440=ORIENTED_EDGE('',*,*,#45781,.F.);
#60441=ORIENTED_EDGE('',*,*,#45782,.T.);
#60442=ORIENTED_EDGE('',*,*,#45783,.T.);
#60443=ORIENTED_EDGE('',*,*,#45784,.F.);
#60444=ORIENTED_EDGE('',*,*,#45785,.F.);
#60445=ORIENTED_EDGE('',*,*,#45786,.F.);
#60446=ORIENTED_EDGE('',*,*,#45787,.T.);
#60447=ORIENTED_EDGE('',*,*,#45781,.T.);
#60448=ORIENTED_EDGE('',*,*,#45788,.F.);
#60449=ORIENTED_EDGE('',*,*,#45789,.F.);
#60450=ORIENTED_EDGE('',*,*,#45790,.F.);
#60451=ORIENTED_EDGE('',*,*,#45785,.T.);
#60452=ORIENTED_EDGE('',*,*,#45791,.F.);
#60453=ORIENTED_EDGE('',*,*,#45783,.F.);
#60454=ORIENTED_EDGE('',*,*,#45792,.T.);
#60455=ORIENTED_EDGE('',*,*,#45793,.F.);
#60456=ORIENTED_EDGE('',*,*,#45789,.T.);
#60457=ORIENTED_EDGE('',*,*,#45794,.F.);
#60458=ORIENTED_EDGE('',*,*,#45786,.T.);
#60459=ORIENTED_EDGE('',*,*,#45790,.T.);
#60460=ORIENTED_EDGE('',*,*,#45793,.T.);
#60461=ORIENTED_EDGE('',*,*,#45795,.T.);
#60462=ORIENTED_EDGE('',*,*,#45796,.F.);
#60463=ORIENTED_EDGE('',*,*,#45797,.T.);
#60464=ORIENTED_EDGE('',*,*,#45798,.T.);
#60465=ORIENTED_EDGE('',*,*,#45799,.F.);
#60466=ORIENTED_EDGE('',*,*,#45800,.F.);
#60467=ORIENTED_EDGE('',*,*,#45801,.T.);
#60468=ORIENTED_EDGE('',*,*,#45796,.T.);
#60469=ORIENTED_EDGE('',*,*,#45802,.F.);
#60470=ORIENTED_EDGE('',*,*,#45803,.F.);
#60471=ORIENTED_EDGE('',*,*,#45804,.F.);
#60472=ORIENTED_EDGE('',*,*,#45805,.T.);
#60473=ORIENTED_EDGE('',*,*,#45800,.T.);
#60474=ORIENTED_EDGE('',*,*,#45806,.F.);
#60475=ORIENTED_EDGE('',*,*,#45798,.F.);
#60476=ORIENTED_EDGE('',*,*,#45807,.T.);
#60477=ORIENTED_EDGE('',*,*,#45808,.F.);
#60478=ORIENTED_EDGE('',*,*,#45803,.T.);
#60479=ORIENTED_EDGE('',*,*,#45809,.F.);
#60480=ORIENTED_EDGE('',*,*,#45804,.T.);
#60481=ORIENTED_EDGE('',*,*,#45808,.T.);
#60482=ORIENTED_EDGE('',*,*,#45810,.T.);
#60483=ORIENTED_EDGE('',*,*,#45811,.F.);
#60484=ORIENTED_EDGE('',*,*,#45812,.T.);
#60485=ORIENTED_EDGE('',*,*,#45813,.T.);
#60486=ORIENTED_EDGE('',*,*,#45814,.F.);
#60487=ORIENTED_EDGE('',*,*,#45815,.F.);
#60488=ORIENTED_EDGE('',*,*,#45816,.T.);
#60489=ORIENTED_EDGE('',*,*,#45811,.T.);
#60490=ORIENTED_EDGE('',*,*,#45817,.F.);
#60491=ORIENTED_EDGE('',*,*,#45818,.F.);
#60492=ORIENTED_EDGE('',*,*,#45819,.T.);
#60493=ORIENTED_EDGE('',*,*,#45815,.T.);
#60494=ORIENTED_EDGE('',*,*,#45820,.F.);
#60495=ORIENTED_EDGE('',*,*,#45813,.F.);
#60496=ORIENTED_EDGE('',*,*,#45821,.T.);
#60497=ORIENTED_EDGE('',*,*,#45818,.T.);
#60498=ORIENTED_EDGE('',*,*,#45822,.F.);
#60499=ORIENTED_EDGE('',*,*,#45823,.F.);
#60500=ORIENTED_EDGE('',*,*,#45824,.T.);
#60501=ORIENTED_EDGE('',*,*,#45825,.T.);
#60502=ORIENTED_EDGE('',*,*,#45826,.F.);
#60503=ORIENTED_EDGE('',*,*,#45827,.F.);
#60504=ORIENTED_EDGE('',*,*,#45828,.T.);
#60505=ORIENTED_EDGE('',*,*,#45823,.T.);
#60506=ORIENTED_EDGE('',*,*,#45829,.F.);
#60507=ORIENTED_EDGE('',*,*,#45830,.F.);
#60508=ORIENTED_EDGE('',*,*,#45831,.T.);
#60509=ORIENTED_EDGE('',*,*,#45827,.T.);
#60510=ORIENTED_EDGE('',*,*,#45832,.F.);
#60511=ORIENTED_EDGE('',*,*,#45825,.F.);
#60512=ORIENTED_EDGE('',*,*,#45833,.T.);
#60513=ORIENTED_EDGE('',*,*,#45830,.T.);
#60514=ORIENTED_EDGE('',*,*,#45834,.F.);
#60515=ORIENTED_EDGE('',*,*,#45835,.F.);
#60516=ORIENTED_EDGE('',*,*,#45836,.T.);
#60517=ORIENTED_EDGE('',*,*,#45837,.T.);
#60518=ORIENTED_EDGE('',*,*,#45838,.F.);
#60519=ORIENTED_EDGE('',*,*,#45839,.F.);
#60520=ORIENTED_EDGE('',*,*,#45840,.T.);
#60521=ORIENTED_EDGE('',*,*,#45835,.T.);
#60522=ORIENTED_EDGE('',*,*,#45841,.F.);
#60523=ORIENTED_EDGE('',*,*,#45842,.F.);
#60524=ORIENTED_EDGE('',*,*,#45843,.T.);
#60525=ORIENTED_EDGE('',*,*,#45839,.T.);
#60526=ORIENTED_EDGE('',*,*,#45844,.F.);
#60527=ORIENTED_EDGE('',*,*,#45837,.F.);
#60528=ORIENTED_EDGE('',*,*,#45845,.T.);
#60529=ORIENTED_EDGE('',*,*,#45842,.T.);
#60530=ORIENTED_EDGE('',*,*,#45846,.F.);
#60531=ORIENTED_EDGE('',*,*,#45847,.F.);
#60532=ORIENTED_EDGE('',*,*,#45848,.T.);
#60533=ORIENTED_EDGE('',*,*,#45849,.T.);
#60534=ORIENTED_EDGE('',*,*,#45850,.F.);
#60535=ORIENTED_EDGE('',*,*,#45851,.F.);
#60536=ORIENTED_EDGE('',*,*,#45852,.T.);
#60537=ORIENTED_EDGE('',*,*,#45847,.T.);
#60538=ORIENTED_EDGE('',*,*,#45853,.F.);
#60539=ORIENTED_EDGE('',*,*,#45854,.F.);
#60540=ORIENTED_EDGE('',*,*,#45855,.T.);
#60541=ORIENTED_EDGE('',*,*,#45851,.T.);
#60542=ORIENTED_EDGE('',*,*,#45856,.F.);
#60543=ORIENTED_EDGE('',*,*,#45849,.F.);
#60544=ORIENTED_EDGE('',*,*,#45857,.T.);
#60545=ORIENTED_EDGE('',*,*,#45854,.T.);
#60546=ORIENTED_EDGE('',*,*,#45858,.F.);
#60547=ORIENTED_EDGE('',*,*,#45859,.F.);
#60548=ORIENTED_EDGE('',*,*,#45860,.T.);
#60549=ORIENTED_EDGE('',*,*,#45861,.T.);
#60550=ORIENTED_EDGE('',*,*,#45862,.F.);
#60551=ORIENTED_EDGE('',*,*,#45863,.F.);
#60552=ORIENTED_EDGE('',*,*,#45864,.T.);
#60553=ORIENTED_EDGE('',*,*,#45859,.T.);
#60554=ORIENTED_EDGE('',*,*,#45865,.F.);
#60555=ORIENTED_EDGE('',*,*,#45866,.F.);
#60556=ORIENTED_EDGE('',*,*,#45867,.T.);
#60557=ORIENTED_EDGE('',*,*,#45863,.T.);
#60558=ORIENTED_EDGE('',*,*,#45868,.F.);
#60559=ORIENTED_EDGE('',*,*,#45861,.F.);
#60560=ORIENTED_EDGE('',*,*,#45869,.T.);
#60561=ORIENTED_EDGE('',*,*,#45866,.T.);
#60562=ORIENTED_EDGE('',*,*,#45870,.F.);
#60563=ORIENTED_EDGE('',*,*,#45871,.F.);
#60564=ORIENTED_EDGE('',*,*,#45872,.T.);
#60565=ORIENTED_EDGE('',*,*,#45873,.T.);
#60566=ORIENTED_EDGE('',*,*,#45874,.F.);
#60567=ORIENTED_EDGE('',*,*,#45875,.F.);
#60568=ORIENTED_EDGE('',*,*,#45876,.T.);
#60569=ORIENTED_EDGE('',*,*,#45871,.T.);
#60570=ORIENTED_EDGE('',*,*,#45877,.F.);
#60571=ORIENTED_EDGE('',*,*,#45878,.F.);
#60572=ORIENTED_EDGE('',*,*,#45879,.T.);
#60573=ORIENTED_EDGE('',*,*,#45875,.T.);
#60574=ORIENTED_EDGE('',*,*,#45880,.F.);
#60575=ORIENTED_EDGE('',*,*,#45873,.F.);
#60576=ORIENTED_EDGE('',*,*,#45881,.T.);
#60577=ORIENTED_EDGE('',*,*,#45878,.T.);
#60578=ORIENTED_EDGE('',*,*,#45882,.F.);
#60579=ORIENTED_EDGE('',*,*,#45883,.F.);
#60580=ORIENTED_EDGE('',*,*,#45884,.T.);
#60581=ORIENTED_EDGE('',*,*,#45885,.T.);
#60582=ORIENTED_EDGE('',*,*,#45886,.F.);
#60583=ORIENTED_EDGE('',*,*,#45887,.F.);
#60584=ORIENTED_EDGE('',*,*,#45888,.T.);
#60585=ORIENTED_EDGE('',*,*,#45883,.T.);
#60586=ORIENTED_EDGE('',*,*,#45889,.F.);
#60587=ORIENTED_EDGE('',*,*,#45890,.F.);
#60588=ORIENTED_EDGE('',*,*,#45891,.T.);
#60589=ORIENTED_EDGE('',*,*,#45887,.T.);
#60590=ORIENTED_EDGE('',*,*,#45892,.F.);
#60591=ORIENTED_EDGE('',*,*,#45885,.F.);
#60592=ORIENTED_EDGE('',*,*,#45893,.T.);
#60593=ORIENTED_EDGE('',*,*,#45890,.T.);
#60594=ORIENTED_EDGE('',*,*,#45894,.F.);
#60595=ORIENTED_EDGE('',*,*,#45895,.F.);
#60596=ORIENTED_EDGE('',*,*,#45896,.T.);
#60597=ORIENTED_EDGE('',*,*,#45897,.T.);
#60598=ORIENTED_EDGE('',*,*,#45898,.F.);
#60599=ORIENTED_EDGE('',*,*,#45899,.F.);
#60600=ORIENTED_EDGE('',*,*,#45900,.T.);
#60601=ORIENTED_EDGE('',*,*,#45895,.T.);
#60602=ORIENTED_EDGE('',*,*,#45901,.F.);
#60603=ORIENTED_EDGE('',*,*,#45902,.F.);
#60604=ORIENTED_EDGE('',*,*,#45903,.T.);
#60605=ORIENTED_EDGE('',*,*,#45899,.T.);
#60606=ORIENTED_EDGE('',*,*,#45904,.F.);
#60607=ORIENTED_EDGE('',*,*,#45897,.F.);
#60608=ORIENTED_EDGE('',*,*,#45905,.T.);
#60609=ORIENTED_EDGE('',*,*,#45902,.T.);
#60610=ORIENTED_EDGE('',*,*,#45906,.F.);
#60611=ORIENTED_EDGE('',*,*,#45907,.F.);
#60612=ORIENTED_EDGE('',*,*,#45908,.T.);
#60613=ORIENTED_EDGE('',*,*,#45909,.T.);
#60614=ORIENTED_EDGE('',*,*,#45910,.F.);
#60615=ORIENTED_EDGE('',*,*,#45911,.F.);
#60616=ORIENTED_EDGE('',*,*,#45912,.T.);
#60617=ORIENTED_EDGE('',*,*,#45907,.T.);
#60618=ORIENTED_EDGE('',*,*,#45913,.F.);
#60619=ORIENTED_EDGE('',*,*,#45914,.F.);
#60620=ORIENTED_EDGE('',*,*,#45915,.T.);
#60621=ORIENTED_EDGE('',*,*,#45911,.T.);
#60622=ORIENTED_EDGE('',*,*,#45916,.F.);
#60623=ORIENTED_EDGE('',*,*,#45909,.F.);
#60624=ORIENTED_EDGE('',*,*,#45917,.T.);
#60625=ORIENTED_EDGE('',*,*,#45914,.T.);
#60626=ORIENTED_EDGE('',*,*,#45918,.F.);
#60627=ORIENTED_EDGE('',*,*,#45919,.F.);
#60628=ORIENTED_EDGE('',*,*,#45920,.T.);
#60629=ORIENTED_EDGE('',*,*,#45921,.T.);
#60630=ORIENTED_EDGE('',*,*,#45922,.F.);
#60631=ORIENTED_EDGE('',*,*,#45923,.F.);
#60632=ORIENTED_EDGE('',*,*,#45924,.T.);
#60633=ORIENTED_EDGE('',*,*,#45919,.T.);
#60634=ORIENTED_EDGE('',*,*,#45925,.F.);
#60635=ORIENTED_EDGE('',*,*,#45926,.F.);
#60636=ORIENTED_EDGE('',*,*,#45927,.T.);
#60637=ORIENTED_EDGE('',*,*,#45923,.T.);
#60638=ORIENTED_EDGE('',*,*,#45928,.F.);
#60639=ORIENTED_EDGE('',*,*,#45921,.F.);
#60640=ORIENTED_EDGE('',*,*,#45929,.T.);
#60641=ORIENTED_EDGE('',*,*,#45926,.T.);
#60642=ORIENTED_EDGE('',*,*,#45930,.F.);
#60643=ORIENTED_EDGE('',*,*,#45931,.F.);
#60644=ORIENTED_EDGE('',*,*,#45932,.T.);
#60645=ORIENTED_EDGE('',*,*,#45933,.T.);
#60646=ORIENTED_EDGE('',*,*,#45934,.F.);
#60647=ORIENTED_EDGE('',*,*,#45935,.F.);
#60648=ORIENTED_EDGE('',*,*,#45936,.T.);
#60649=ORIENTED_EDGE('',*,*,#45931,.T.);
#60650=ORIENTED_EDGE('',*,*,#45937,.F.);
#60651=ORIENTED_EDGE('',*,*,#45938,.F.);
#60652=ORIENTED_EDGE('',*,*,#45939,.T.);
#60653=ORIENTED_EDGE('',*,*,#45935,.T.);
#60654=ORIENTED_EDGE('',*,*,#45940,.F.);
#60655=ORIENTED_EDGE('',*,*,#45933,.F.);
#60656=ORIENTED_EDGE('',*,*,#45941,.T.);
#60657=ORIENTED_EDGE('',*,*,#45938,.T.);
#60658=ORIENTED_EDGE('',*,*,#45942,.F.);
#60659=ORIENTED_EDGE('',*,*,#45943,.F.);
#60660=ORIENTED_EDGE('',*,*,#45944,.T.);
#60661=ORIENTED_EDGE('',*,*,#45945,.T.);
#60662=ORIENTED_EDGE('',*,*,#45946,.F.);
#60663=ORIENTED_EDGE('',*,*,#45947,.F.);
#60664=ORIENTED_EDGE('',*,*,#45948,.T.);
#60665=ORIENTED_EDGE('',*,*,#45943,.T.);
#60666=ORIENTED_EDGE('',*,*,#45949,.F.);
#60667=ORIENTED_EDGE('',*,*,#45950,.F.);
#60668=ORIENTED_EDGE('',*,*,#45951,.T.);
#60669=ORIENTED_EDGE('',*,*,#45947,.T.);
#60670=ORIENTED_EDGE('',*,*,#45952,.F.);
#60671=ORIENTED_EDGE('',*,*,#45945,.F.);
#60672=ORIENTED_EDGE('',*,*,#45953,.T.);
#60673=ORIENTED_EDGE('',*,*,#45950,.T.);
#60674=ORIENTED_EDGE('',*,*,#45954,.F.);
#60675=ORIENTED_EDGE('',*,*,#45955,.F.);
#60676=ORIENTED_EDGE('',*,*,#45956,.T.);
#60677=ORIENTED_EDGE('',*,*,#45957,.T.);
#60678=ORIENTED_EDGE('',*,*,#45958,.F.);
#60679=ORIENTED_EDGE('',*,*,#45959,.F.);
#60680=ORIENTED_EDGE('',*,*,#45960,.T.);
#60681=ORIENTED_EDGE('',*,*,#45955,.T.);
#60682=ORIENTED_EDGE('',*,*,#45961,.F.);
#60683=ORIENTED_EDGE('',*,*,#45962,.F.);
#60684=ORIENTED_EDGE('',*,*,#45963,.T.);
#60685=ORIENTED_EDGE('',*,*,#45959,.T.);
#60686=ORIENTED_EDGE('',*,*,#45964,.F.);
#60687=ORIENTED_EDGE('',*,*,#45957,.F.);
#60688=ORIENTED_EDGE('',*,*,#45965,.T.);
#60689=ORIENTED_EDGE('',*,*,#45962,.T.);
#60690=ORIENTED_EDGE('',*,*,#45966,.F.);
#60691=ORIENTED_EDGE('',*,*,#45967,.F.);
#60692=ORIENTED_EDGE('',*,*,#45968,.T.);
#60693=ORIENTED_EDGE('',*,*,#45969,.T.);
#60694=ORIENTED_EDGE('',*,*,#45970,.F.);
#60695=ORIENTED_EDGE('',*,*,#45971,.F.);
#60696=ORIENTED_EDGE('',*,*,#45972,.T.);
#60697=ORIENTED_EDGE('',*,*,#45967,.T.);
#60698=ORIENTED_EDGE('',*,*,#45973,.F.);
#60699=ORIENTED_EDGE('',*,*,#45974,.F.);
#60700=ORIENTED_EDGE('',*,*,#45975,.T.);
#60701=ORIENTED_EDGE('',*,*,#45971,.T.);
#60702=ORIENTED_EDGE('',*,*,#45976,.F.);
#60703=ORIENTED_EDGE('',*,*,#45969,.F.);
#60704=ORIENTED_EDGE('',*,*,#45977,.T.);
#60705=ORIENTED_EDGE('',*,*,#45974,.T.);
#60706=ORIENTED_EDGE('',*,*,#45978,.F.);
#60707=ORIENTED_EDGE('',*,*,#45979,.F.);
#60708=ORIENTED_EDGE('',*,*,#45980,.T.);
#60709=ORIENTED_EDGE('',*,*,#45981,.T.);
#60710=ORIENTED_EDGE('',*,*,#45982,.F.);
#60711=ORIENTED_EDGE('',*,*,#45983,.F.);
#60712=ORIENTED_EDGE('',*,*,#45984,.T.);
#60713=ORIENTED_EDGE('',*,*,#45979,.T.);
#60714=ORIENTED_EDGE('',*,*,#45985,.F.);
#60715=ORIENTED_EDGE('',*,*,#45986,.F.);
#60716=ORIENTED_EDGE('',*,*,#45987,.T.);
#60717=ORIENTED_EDGE('',*,*,#45983,.T.);
#60718=ORIENTED_EDGE('',*,*,#45988,.F.);
#60719=ORIENTED_EDGE('',*,*,#45981,.F.);
#60720=ORIENTED_EDGE('',*,*,#45989,.T.);
#60721=ORIENTED_EDGE('',*,*,#45986,.T.);
#60722=ORIENTED_EDGE('',*,*,#45990,.F.);
#60723=ORIENTED_EDGE('',*,*,#45991,.F.);
#60724=ORIENTED_EDGE('',*,*,#45992,.T.);
#60725=ORIENTED_EDGE('',*,*,#45993,.T.);
#60726=ORIENTED_EDGE('',*,*,#45994,.F.);
#60727=ORIENTED_EDGE('',*,*,#45995,.F.);
#60728=ORIENTED_EDGE('',*,*,#45996,.T.);
#60729=ORIENTED_EDGE('',*,*,#45991,.T.);
#60730=ORIENTED_EDGE('',*,*,#45997,.F.);
#60731=ORIENTED_EDGE('',*,*,#45998,.F.);
#60732=ORIENTED_EDGE('',*,*,#45999,.T.);
#60733=ORIENTED_EDGE('',*,*,#45995,.T.);
#60734=ORIENTED_EDGE('',*,*,#46000,.F.);
#60735=ORIENTED_EDGE('',*,*,#45993,.F.);
#60736=ORIENTED_EDGE('',*,*,#46001,.T.);
#60737=ORIENTED_EDGE('',*,*,#45998,.T.);
#60738=ORIENTED_EDGE('',*,*,#46002,.F.);
#60739=ORIENTED_EDGE('',*,*,#46003,.F.);
#60740=ORIENTED_EDGE('',*,*,#46004,.T.);
#60741=ORIENTED_EDGE('',*,*,#46005,.T.);
#60742=ORIENTED_EDGE('',*,*,#46006,.F.);
#60743=ORIENTED_EDGE('',*,*,#46007,.F.);
#60744=ORIENTED_EDGE('',*,*,#46008,.T.);
#60745=ORIENTED_EDGE('',*,*,#46003,.T.);
#60746=ORIENTED_EDGE('',*,*,#46009,.F.);
#60747=ORIENTED_EDGE('',*,*,#46010,.F.);
#60748=ORIENTED_EDGE('',*,*,#46011,.T.);
#60749=ORIENTED_EDGE('',*,*,#46007,.T.);
#60750=ORIENTED_EDGE('',*,*,#46012,.F.);
#60751=ORIENTED_EDGE('',*,*,#46005,.F.);
#60752=ORIENTED_EDGE('',*,*,#46013,.T.);
#60753=ORIENTED_EDGE('',*,*,#46010,.T.);
#60754=ORIENTED_EDGE('',*,*,#46014,.F.);
#60755=ORIENTED_EDGE('',*,*,#46015,.F.);
#60756=ORIENTED_EDGE('',*,*,#46016,.T.);
#60757=ORIENTED_EDGE('',*,*,#46017,.T.);
#60758=ORIENTED_EDGE('',*,*,#46018,.F.);
#60759=ORIENTED_EDGE('',*,*,#46019,.F.);
#60760=ORIENTED_EDGE('',*,*,#46020,.T.);
#60761=ORIENTED_EDGE('',*,*,#46015,.T.);
#60762=ORIENTED_EDGE('',*,*,#46021,.F.);
#60763=ORIENTED_EDGE('',*,*,#46022,.F.);
#60764=ORIENTED_EDGE('',*,*,#46023,.T.);
#60765=ORIENTED_EDGE('',*,*,#46019,.T.);
#60766=ORIENTED_EDGE('',*,*,#46024,.F.);
#60767=ORIENTED_EDGE('',*,*,#46017,.F.);
#60768=ORIENTED_EDGE('',*,*,#46025,.T.);
#60769=ORIENTED_EDGE('',*,*,#46022,.T.);
#60770=ORIENTED_EDGE('',*,*,#46026,.F.);
#60771=ORIENTED_EDGE('',*,*,#46027,.F.);
#60772=ORIENTED_EDGE('',*,*,#46028,.T.);
#60773=ORIENTED_EDGE('',*,*,#46029,.T.);
#60774=ORIENTED_EDGE('',*,*,#46030,.F.);
#60775=ORIENTED_EDGE('',*,*,#46031,.F.);
#60776=ORIENTED_EDGE('',*,*,#46032,.T.);
#60777=ORIENTED_EDGE('',*,*,#46027,.T.);
#60778=ORIENTED_EDGE('',*,*,#46033,.F.);
#60779=ORIENTED_EDGE('',*,*,#46034,.F.);
#60780=ORIENTED_EDGE('',*,*,#46035,.T.);
#60781=ORIENTED_EDGE('',*,*,#46031,.T.);
#60782=ORIENTED_EDGE('',*,*,#46036,.F.);
#60783=ORIENTED_EDGE('',*,*,#46029,.F.);
#60784=ORIENTED_EDGE('',*,*,#46037,.T.);
#60785=ORIENTED_EDGE('',*,*,#46034,.T.);
#60786=ORIENTED_EDGE('',*,*,#46038,.F.);
#60787=ORIENTED_EDGE('',*,*,#46039,.F.);
#60788=ORIENTED_EDGE('',*,*,#46040,.T.);
#60789=ORIENTED_EDGE('',*,*,#46041,.T.);
#60790=ORIENTED_EDGE('',*,*,#46042,.F.);
#60791=ORIENTED_EDGE('',*,*,#46043,.F.);
#60792=ORIENTED_EDGE('',*,*,#46044,.T.);
#60793=ORIENTED_EDGE('',*,*,#46039,.T.);
#60794=ORIENTED_EDGE('',*,*,#46045,.F.);
#60795=ORIENTED_EDGE('',*,*,#46046,.F.);
#60796=ORIENTED_EDGE('',*,*,#46047,.T.);
#60797=ORIENTED_EDGE('',*,*,#46043,.T.);
#60798=ORIENTED_EDGE('',*,*,#46048,.F.);
#60799=ORIENTED_EDGE('',*,*,#46041,.F.);
#60800=ORIENTED_EDGE('',*,*,#46049,.T.);
#60801=ORIENTED_EDGE('',*,*,#46046,.T.);
#60802=ORIENTED_EDGE('',*,*,#46050,.F.);
#60803=ORIENTED_EDGE('',*,*,#46051,.F.);
#60804=ORIENTED_EDGE('',*,*,#46052,.T.);
#60805=ORIENTED_EDGE('',*,*,#46053,.T.);
#60806=ORIENTED_EDGE('',*,*,#46054,.F.);
#60807=ORIENTED_EDGE('',*,*,#46055,.F.);
#60808=ORIENTED_EDGE('',*,*,#46056,.T.);
#60809=ORIENTED_EDGE('',*,*,#46051,.T.);
#60810=ORIENTED_EDGE('',*,*,#46057,.F.);
#60811=ORIENTED_EDGE('',*,*,#46058,.F.);
#60812=ORIENTED_EDGE('',*,*,#46059,.T.);
#60813=ORIENTED_EDGE('',*,*,#46055,.T.);
#60814=ORIENTED_EDGE('',*,*,#46060,.F.);
#60815=ORIENTED_EDGE('',*,*,#46053,.F.);
#60816=ORIENTED_EDGE('',*,*,#46061,.T.);
#60817=ORIENTED_EDGE('',*,*,#46058,.T.);
#60818=ORIENTED_EDGE('',*,*,#46062,.F.);
#60819=ORIENTED_EDGE('',*,*,#46063,.F.);
#60820=ORIENTED_EDGE('',*,*,#46064,.T.);
#60821=ORIENTED_EDGE('',*,*,#46065,.T.);
#60822=ORIENTED_EDGE('',*,*,#46066,.F.);
#60823=ORIENTED_EDGE('',*,*,#46067,.F.);
#60824=ORIENTED_EDGE('',*,*,#46068,.T.);
#60825=ORIENTED_EDGE('',*,*,#46063,.T.);
#60826=ORIENTED_EDGE('',*,*,#46069,.F.);
#60827=ORIENTED_EDGE('',*,*,#46070,.F.);
#60828=ORIENTED_EDGE('',*,*,#46071,.T.);
#60829=ORIENTED_EDGE('',*,*,#46067,.T.);
#60830=ORIENTED_EDGE('',*,*,#46072,.F.);
#60831=ORIENTED_EDGE('',*,*,#46065,.F.);
#60832=ORIENTED_EDGE('',*,*,#46073,.T.);
#60833=ORIENTED_EDGE('',*,*,#46070,.T.);
#60834=ORIENTED_EDGE('',*,*,#46074,.F.);
#60835=ORIENTED_EDGE('',*,*,#46075,.F.);
#60836=ORIENTED_EDGE('',*,*,#46076,.T.);
#60837=ORIENTED_EDGE('',*,*,#46077,.T.);
#60838=ORIENTED_EDGE('',*,*,#46078,.F.);
#60839=ORIENTED_EDGE('',*,*,#46079,.F.);
#60840=ORIENTED_EDGE('',*,*,#46080,.T.);
#60841=ORIENTED_EDGE('',*,*,#46075,.T.);
#60842=ORIENTED_EDGE('',*,*,#46081,.F.);
#60843=ORIENTED_EDGE('',*,*,#46082,.F.);
#60844=ORIENTED_EDGE('',*,*,#46083,.T.);
#60845=ORIENTED_EDGE('',*,*,#46079,.T.);
#60846=ORIENTED_EDGE('',*,*,#46084,.F.);
#60847=ORIENTED_EDGE('',*,*,#46077,.F.);
#60848=ORIENTED_EDGE('',*,*,#46085,.T.);
#60849=ORIENTED_EDGE('',*,*,#46082,.T.);
#60850=ORIENTED_EDGE('',*,*,#46086,.F.);
#60851=ORIENTED_EDGE('',*,*,#46087,.F.);
#60852=ORIENTED_EDGE('',*,*,#46088,.T.);
#60853=ORIENTED_EDGE('',*,*,#46089,.T.);
#60854=ORIENTED_EDGE('',*,*,#46090,.F.);
#60855=ORIENTED_EDGE('',*,*,#46091,.F.);
#60856=ORIENTED_EDGE('',*,*,#46092,.T.);
#60857=ORIENTED_EDGE('',*,*,#46087,.T.);
#60858=ORIENTED_EDGE('',*,*,#46093,.F.);
#60859=ORIENTED_EDGE('',*,*,#46094,.F.);
#60860=ORIENTED_EDGE('',*,*,#46095,.T.);
#60861=ORIENTED_EDGE('',*,*,#46091,.T.);
#60862=ORIENTED_EDGE('',*,*,#46096,.F.);
#60863=ORIENTED_EDGE('',*,*,#46089,.F.);
#60864=ORIENTED_EDGE('',*,*,#46097,.T.);
#60865=ORIENTED_EDGE('',*,*,#46094,.T.);
#60866=ORIENTED_EDGE('',*,*,#46098,.F.);
#60867=ORIENTED_EDGE('',*,*,#46099,.F.);
#60868=ORIENTED_EDGE('',*,*,#46100,.T.);
#60869=ORIENTED_EDGE('',*,*,#46101,.T.);
#60870=ORIENTED_EDGE('',*,*,#46102,.F.);
#60871=ORIENTED_EDGE('',*,*,#46103,.F.);
#60872=ORIENTED_EDGE('',*,*,#46104,.T.);
#60873=ORIENTED_EDGE('',*,*,#46099,.T.);
#60874=ORIENTED_EDGE('',*,*,#46105,.F.);
#60875=ORIENTED_EDGE('',*,*,#46106,.F.);
#60876=ORIENTED_EDGE('',*,*,#46107,.T.);
#60877=ORIENTED_EDGE('',*,*,#46103,.T.);
#60878=ORIENTED_EDGE('',*,*,#46108,.F.);
#60879=ORIENTED_EDGE('',*,*,#46101,.F.);
#60880=ORIENTED_EDGE('',*,*,#46109,.T.);
#60881=ORIENTED_EDGE('',*,*,#46106,.T.);
#60882=ORIENTED_EDGE('',*,*,#46110,.F.);
#60883=ORIENTED_EDGE('',*,*,#46111,.F.);
#60884=ORIENTED_EDGE('',*,*,#46112,.T.);
#60885=ORIENTED_EDGE('',*,*,#46113,.T.);
#60886=ORIENTED_EDGE('',*,*,#46114,.F.);
#60887=ORIENTED_EDGE('',*,*,#46115,.F.);
#60888=ORIENTED_EDGE('',*,*,#46116,.T.);
#60889=ORIENTED_EDGE('',*,*,#46111,.T.);
#60890=ORIENTED_EDGE('',*,*,#46117,.F.);
#60891=ORIENTED_EDGE('',*,*,#46118,.F.);
#60892=ORIENTED_EDGE('',*,*,#46119,.T.);
#60893=ORIENTED_EDGE('',*,*,#46115,.T.);
#60894=ORIENTED_EDGE('',*,*,#46120,.F.);
#60895=ORIENTED_EDGE('',*,*,#46113,.F.);
#60896=ORIENTED_EDGE('',*,*,#46121,.T.);
#60897=ORIENTED_EDGE('',*,*,#46118,.T.);
#60898=ORIENTED_EDGE('',*,*,#46122,.F.);
#60899=ORIENTED_EDGE('',*,*,#46123,.F.);
#60900=ORIENTED_EDGE('',*,*,#46124,.T.);
#60901=ORIENTED_EDGE('',*,*,#46125,.T.);
#60902=ORIENTED_EDGE('',*,*,#46126,.F.);
#60903=ORIENTED_EDGE('',*,*,#46127,.F.);
#60904=ORIENTED_EDGE('',*,*,#46128,.T.);
#60905=ORIENTED_EDGE('',*,*,#46123,.T.);
#60906=ORIENTED_EDGE('',*,*,#46129,.F.);
#60907=ORIENTED_EDGE('',*,*,#46130,.F.);
#60908=ORIENTED_EDGE('',*,*,#46131,.T.);
#60909=ORIENTED_EDGE('',*,*,#46127,.T.);
#60910=ORIENTED_EDGE('',*,*,#46132,.F.);
#60911=ORIENTED_EDGE('',*,*,#46125,.F.);
#60912=ORIENTED_EDGE('',*,*,#46133,.T.);
#60913=ORIENTED_EDGE('',*,*,#46130,.T.);
#60914=ORIENTED_EDGE('',*,*,#46134,.F.);
#60915=ORIENTED_EDGE('',*,*,#46135,.F.);
#60916=ORIENTED_EDGE('',*,*,#46136,.T.);
#60917=ORIENTED_EDGE('',*,*,#46137,.T.);
#60918=ORIENTED_EDGE('',*,*,#46138,.F.);
#60919=ORIENTED_EDGE('',*,*,#46139,.F.);
#60920=ORIENTED_EDGE('',*,*,#46140,.T.);
#60921=ORIENTED_EDGE('',*,*,#46135,.T.);
#60922=ORIENTED_EDGE('',*,*,#46141,.F.);
#60923=ORIENTED_EDGE('',*,*,#46142,.F.);
#60924=ORIENTED_EDGE('',*,*,#46143,.T.);
#60925=ORIENTED_EDGE('',*,*,#46139,.T.);
#60926=ORIENTED_EDGE('',*,*,#46144,.F.);
#60927=ORIENTED_EDGE('',*,*,#46137,.F.);
#60928=ORIENTED_EDGE('',*,*,#46145,.T.);
#60929=ORIENTED_EDGE('',*,*,#46142,.T.);
#60930=ORIENTED_EDGE('',*,*,#46146,.F.);
#60931=ORIENTED_EDGE('',*,*,#46147,.F.);
#60932=ORIENTED_EDGE('',*,*,#46148,.T.);
#60933=ORIENTED_EDGE('',*,*,#46149,.T.);
#60934=ORIENTED_EDGE('',*,*,#46150,.F.);
#60935=ORIENTED_EDGE('',*,*,#46151,.F.);
#60936=ORIENTED_EDGE('',*,*,#46152,.T.);
#60937=ORIENTED_EDGE('',*,*,#46147,.T.);
#60938=ORIENTED_EDGE('',*,*,#46153,.F.);
#60939=ORIENTED_EDGE('',*,*,#46154,.F.);
#60940=ORIENTED_EDGE('',*,*,#46155,.T.);
#60941=ORIENTED_EDGE('',*,*,#46151,.T.);
#60942=ORIENTED_EDGE('',*,*,#46156,.F.);
#60943=ORIENTED_EDGE('',*,*,#46149,.F.);
#60944=ORIENTED_EDGE('',*,*,#46157,.T.);
#60945=ORIENTED_EDGE('',*,*,#46154,.T.);
#60946=ORIENTED_EDGE('',*,*,#46158,.F.);
#60947=ORIENTED_EDGE('',*,*,#46159,.F.);
#60948=ORIENTED_EDGE('',*,*,#46160,.T.);
#60949=ORIENTED_EDGE('',*,*,#46161,.T.);
#60950=ORIENTED_EDGE('',*,*,#46162,.F.);
#60951=ORIENTED_EDGE('',*,*,#46163,.F.);
#60952=ORIENTED_EDGE('',*,*,#46164,.T.);
#60953=ORIENTED_EDGE('',*,*,#46159,.T.);
#60954=ORIENTED_EDGE('',*,*,#46165,.F.);
#60955=ORIENTED_EDGE('',*,*,#46166,.F.);
#60956=ORIENTED_EDGE('',*,*,#46167,.T.);
#60957=ORIENTED_EDGE('',*,*,#46163,.T.);
#60958=ORIENTED_EDGE('',*,*,#46168,.F.);
#60959=ORIENTED_EDGE('',*,*,#46161,.F.);
#60960=ORIENTED_EDGE('',*,*,#46169,.T.);
#60961=ORIENTED_EDGE('',*,*,#46166,.T.);
#60962=ORIENTED_EDGE('',*,*,#46170,.F.);
#60963=ORIENTED_EDGE('',*,*,#46171,.F.);
#60964=ORIENTED_EDGE('',*,*,#46172,.T.);
#60965=ORIENTED_EDGE('',*,*,#46173,.T.);
#60966=ORIENTED_EDGE('',*,*,#46174,.F.);
#60967=ORIENTED_EDGE('',*,*,#46175,.F.);
#60968=ORIENTED_EDGE('',*,*,#46176,.T.);
#60969=ORIENTED_EDGE('',*,*,#46171,.T.);
#60970=ORIENTED_EDGE('',*,*,#46177,.F.);
#60971=ORIENTED_EDGE('',*,*,#46178,.F.);
#60972=ORIENTED_EDGE('',*,*,#46179,.T.);
#60973=ORIENTED_EDGE('',*,*,#46175,.T.);
#60974=ORIENTED_EDGE('',*,*,#46180,.F.);
#60975=ORIENTED_EDGE('',*,*,#46173,.F.);
#60976=ORIENTED_EDGE('',*,*,#46181,.T.);
#60977=ORIENTED_EDGE('',*,*,#46178,.T.);
#60978=ORIENTED_EDGE('',*,*,#46182,.F.);
#60979=ORIENTED_EDGE('',*,*,#46183,.F.);
#60980=ORIENTED_EDGE('',*,*,#46184,.T.);
#60981=ORIENTED_EDGE('',*,*,#46185,.T.);
#60982=ORIENTED_EDGE('',*,*,#46186,.F.);
#60983=ORIENTED_EDGE('',*,*,#46187,.F.);
#60984=ORIENTED_EDGE('',*,*,#46188,.T.);
#60985=ORIENTED_EDGE('',*,*,#46183,.T.);
#60986=ORIENTED_EDGE('',*,*,#46189,.F.);
#60987=ORIENTED_EDGE('',*,*,#46190,.F.);
#60988=ORIENTED_EDGE('',*,*,#46191,.T.);
#60989=ORIENTED_EDGE('',*,*,#46187,.T.);
#60990=ORIENTED_EDGE('',*,*,#46192,.F.);
#60991=ORIENTED_EDGE('',*,*,#46185,.F.);
#60992=ORIENTED_EDGE('',*,*,#46193,.T.);
#60993=ORIENTED_EDGE('',*,*,#46190,.T.);
#60994=ORIENTED_EDGE('',*,*,#46194,.F.);
#60995=ORIENTED_EDGE('',*,*,#46195,.F.);
#60996=ORIENTED_EDGE('',*,*,#46196,.T.);
#60997=ORIENTED_EDGE('',*,*,#46197,.T.);
#60998=ORIENTED_EDGE('',*,*,#46198,.F.);
#60999=ORIENTED_EDGE('',*,*,#46199,.F.);
#61000=ORIENTED_EDGE('',*,*,#46200,.T.);
#61001=ORIENTED_EDGE('',*,*,#46195,.T.);
#61002=ORIENTED_EDGE('',*,*,#46201,.F.);
#61003=ORIENTED_EDGE('',*,*,#46202,.F.);
#61004=ORIENTED_EDGE('',*,*,#46203,.T.);
#61005=ORIENTED_EDGE('',*,*,#46199,.T.);
#61006=ORIENTED_EDGE('',*,*,#46204,.F.);
#61007=ORIENTED_EDGE('',*,*,#46197,.F.);
#61008=ORIENTED_EDGE('',*,*,#46205,.T.);
#61009=ORIENTED_EDGE('',*,*,#46202,.T.);
#61010=ORIENTED_EDGE('',*,*,#46206,.F.);
#61011=ORIENTED_EDGE('',*,*,#46207,.F.);
#61012=ORIENTED_EDGE('',*,*,#46208,.T.);
#61013=ORIENTED_EDGE('',*,*,#46209,.T.);
#61014=ORIENTED_EDGE('',*,*,#46210,.F.);
#61015=ORIENTED_EDGE('',*,*,#46211,.F.);
#61016=ORIENTED_EDGE('',*,*,#46212,.T.);
#61017=ORIENTED_EDGE('',*,*,#46207,.T.);
#61018=ORIENTED_EDGE('',*,*,#46213,.F.);
#61019=ORIENTED_EDGE('',*,*,#46214,.F.);
#61020=ORIENTED_EDGE('',*,*,#46215,.T.);
#61021=ORIENTED_EDGE('',*,*,#46211,.T.);
#61022=ORIENTED_EDGE('',*,*,#46216,.F.);
#61023=ORIENTED_EDGE('',*,*,#46209,.F.);
#61024=ORIENTED_EDGE('',*,*,#46217,.T.);
#61025=ORIENTED_EDGE('',*,*,#46214,.T.);
#61026=ORIENTED_EDGE('',*,*,#46218,.F.);
#61027=ORIENTED_EDGE('',*,*,#46219,.F.);
#61028=ORIENTED_EDGE('',*,*,#46220,.T.);
#61029=ORIENTED_EDGE('',*,*,#46221,.T.);
#61030=ORIENTED_EDGE('',*,*,#46222,.F.);
#61031=ORIENTED_EDGE('',*,*,#46223,.F.);
#61032=ORIENTED_EDGE('',*,*,#46224,.T.);
#61033=ORIENTED_EDGE('',*,*,#46219,.T.);
#61034=ORIENTED_EDGE('',*,*,#46225,.F.);
#61035=ORIENTED_EDGE('',*,*,#46226,.F.);
#61036=ORIENTED_EDGE('',*,*,#46227,.T.);
#61037=ORIENTED_EDGE('',*,*,#46223,.T.);
#61038=ORIENTED_EDGE('',*,*,#46228,.F.);
#61039=ORIENTED_EDGE('',*,*,#46221,.F.);
#61040=ORIENTED_EDGE('',*,*,#46229,.T.);
#61041=ORIENTED_EDGE('',*,*,#46226,.T.);
#61042=ORIENTED_EDGE('',*,*,#46230,.F.);
#61043=ORIENTED_EDGE('',*,*,#46231,.F.);
#61044=ORIENTED_EDGE('',*,*,#46232,.T.);
#61045=ORIENTED_EDGE('',*,*,#46233,.T.);
#61046=ORIENTED_EDGE('',*,*,#46234,.F.);
#61047=ORIENTED_EDGE('',*,*,#46235,.F.);
#61048=ORIENTED_EDGE('',*,*,#46236,.T.);
#61049=ORIENTED_EDGE('',*,*,#46231,.T.);
#61050=ORIENTED_EDGE('',*,*,#46237,.F.);
#61051=ORIENTED_EDGE('',*,*,#46238,.F.);
#61052=ORIENTED_EDGE('',*,*,#46239,.T.);
#61053=ORIENTED_EDGE('',*,*,#46235,.T.);
#61054=ORIENTED_EDGE('',*,*,#46240,.F.);
#61055=ORIENTED_EDGE('',*,*,#46233,.F.);
#61056=ORIENTED_EDGE('',*,*,#46241,.T.);
#61057=ORIENTED_EDGE('',*,*,#46238,.T.);
#61058=ORIENTED_EDGE('',*,*,#46242,.F.);
#61059=ORIENTED_EDGE('',*,*,#46243,.F.);
#61060=ORIENTED_EDGE('',*,*,#46244,.T.);
#61061=ORIENTED_EDGE('',*,*,#46245,.T.);
#61062=ORIENTED_EDGE('',*,*,#46246,.F.);
#61063=ORIENTED_EDGE('',*,*,#46247,.F.);
#61064=ORIENTED_EDGE('',*,*,#46248,.T.);
#61065=ORIENTED_EDGE('',*,*,#46243,.T.);
#61066=ORIENTED_EDGE('',*,*,#46249,.F.);
#61067=ORIENTED_EDGE('',*,*,#46250,.F.);
#61068=ORIENTED_EDGE('',*,*,#46251,.T.);
#61069=ORIENTED_EDGE('',*,*,#46247,.T.);
#61070=ORIENTED_EDGE('',*,*,#46252,.F.);
#61071=ORIENTED_EDGE('',*,*,#46245,.F.);
#61072=ORIENTED_EDGE('',*,*,#46253,.T.);
#61073=ORIENTED_EDGE('',*,*,#46250,.T.);
#61074=ORIENTED_EDGE('',*,*,#46254,.F.);
#61075=ORIENTED_EDGE('',*,*,#46255,.F.);
#61076=ORIENTED_EDGE('',*,*,#46256,.T.);
#61077=ORIENTED_EDGE('',*,*,#46257,.T.);
#61078=ORIENTED_EDGE('',*,*,#46258,.F.);
#61079=ORIENTED_EDGE('',*,*,#46259,.F.);
#61080=ORIENTED_EDGE('',*,*,#46260,.T.);
#61081=ORIENTED_EDGE('',*,*,#46255,.T.);
#61082=ORIENTED_EDGE('',*,*,#46261,.F.);
#61083=ORIENTED_EDGE('',*,*,#46262,.F.);
#61084=ORIENTED_EDGE('',*,*,#46263,.T.);
#61085=ORIENTED_EDGE('',*,*,#46259,.T.);
#61086=ORIENTED_EDGE('',*,*,#46264,.F.);
#61087=ORIENTED_EDGE('',*,*,#46257,.F.);
#61088=ORIENTED_EDGE('',*,*,#46265,.T.);
#61089=ORIENTED_EDGE('',*,*,#46262,.T.);
#61090=ORIENTED_EDGE('',*,*,#46266,.F.);
#61091=ORIENTED_EDGE('',*,*,#46267,.F.);
#61092=ORIENTED_EDGE('',*,*,#46268,.T.);
#61093=ORIENTED_EDGE('',*,*,#46269,.T.);
#61094=ORIENTED_EDGE('',*,*,#46270,.F.);
#61095=ORIENTED_EDGE('',*,*,#46271,.F.);
#61096=ORIENTED_EDGE('',*,*,#46272,.T.);
#61097=ORIENTED_EDGE('',*,*,#46267,.T.);
#61098=ORIENTED_EDGE('',*,*,#46273,.F.);
#61099=ORIENTED_EDGE('',*,*,#46274,.F.);
#61100=ORIENTED_EDGE('',*,*,#46275,.T.);
#61101=ORIENTED_EDGE('',*,*,#46271,.T.);
#61102=ORIENTED_EDGE('',*,*,#46276,.F.);
#61103=ORIENTED_EDGE('',*,*,#46269,.F.);
#61104=ORIENTED_EDGE('',*,*,#46277,.T.);
#61105=ORIENTED_EDGE('',*,*,#46274,.T.);
#61106=ORIENTED_EDGE('',*,*,#46278,.F.);
#61107=ORIENTED_EDGE('',*,*,#46279,.F.);
#61108=ORIENTED_EDGE('',*,*,#46280,.T.);
#61109=ORIENTED_EDGE('',*,*,#46281,.T.);
#61110=ORIENTED_EDGE('',*,*,#46282,.F.);
#61111=ORIENTED_EDGE('',*,*,#46283,.F.);
#61112=ORIENTED_EDGE('',*,*,#46284,.T.);
#61113=ORIENTED_EDGE('',*,*,#46279,.T.);
#61114=ORIENTED_EDGE('',*,*,#46285,.F.);
#61115=ORIENTED_EDGE('',*,*,#46286,.F.);
#61116=ORIENTED_EDGE('',*,*,#46287,.T.);
#61117=ORIENTED_EDGE('',*,*,#46283,.T.);
#61118=ORIENTED_EDGE('',*,*,#46288,.F.);
#61119=ORIENTED_EDGE('',*,*,#46281,.F.);
#61120=ORIENTED_EDGE('',*,*,#46289,.T.);
#61121=ORIENTED_EDGE('',*,*,#46286,.T.);
#61122=ORIENTED_EDGE('',*,*,#46290,.F.);
#61123=ORIENTED_EDGE('',*,*,#46291,.F.);
#61124=ORIENTED_EDGE('',*,*,#46292,.T.);
#61125=ORIENTED_EDGE('',*,*,#46293,.T.);
#61126=ORIENTED_EDGE('',*,*,#46294,.F.);
#61127=ORIENTED_EDGE('',*,*,#46295,.F.);
#61128=ORIENTED_EDGE('',*,*,#46296,.T.);
#61129=ORIENTED_EDGE('',*,*,#46291,.T.);
#61130=ORIENTED_EDGE('',*,*,#46297,.F.);
#61131=ORIENTED_EDGE('',*,*,#46298,.F.);
#61132=ORIENTED_EDGE('',*,*,#46299,.T.);
#61133=ORIENTED_EDGE('',*,*,#46295,.T.);
#61134=ORIENTED_EDGE('',*,*,#46300,.F.);
#61135=ORIENTED_EDGE('',*,*,#46293,.F.);
#61136=ORIENTED_EDGE('',*,*,#46301,.T.);
#61137=ORIENTED_EDGE('',*,*,#46298,.T.);
#61138=ORIENTED_EDGE('',*,*,#46302,.F.);
#61139=ORIENTED_EDGE('',*,*,#46303,.F.);
#61140=ORIENTED_EDGE('',*,*,#46304,.T.);
#61141=ORIENTED_EDGE('',*,*,#46305,.T.);
#61142=ORIENTED_EDGE('',*,*,#46306,.F.);
#61143=ORIENTED_EDGE('',*,*,#46307,.F.);
#61144=ORIENTED_EDGE('',*,*,#46308,.T.);
#61145=ORIENTED_EDGE('',*,*,#46303,.T.);
#61146=ORIENTED_EDGE('',*,*,#46309,.F.);
#61147=ORIENTED_EDGE('',*,*,#46310,.F.);
#61148=ORIENTED_EDGE('',*,*,#46311,.T.);
#61149=ORIENTED_EDGE('',*,*,#46307,.T.);
#61150=ORIENTED_EDGE('',*,*,#46312,.F.);
#61151=ORIENTED_EDGE('',*,*,#46305,.F.);
#61152=ORIENTED_EDGE('',*,*,#46313,.T.);
#61153=ORIENTED_EDGE('',*,*,#46310,.T.);
#61154=ORIENTED_EDGE('',*,*,#46314,.F.);
#61155=ORIENTED_EDGE('',*,*,#46315,.F.);
#61156=ORIENTED_EDGE('',*,*,#46316,.T.);
#61157=ORIENTED_EDGE('',*,*,#46317,.T.);
#61158=ORIENTED_EDGE('',*,*,#46318,.F.);
#61159=ORIENTED_EDGE('',*,*,#46319,.F.);
#61160=ORIENTED_EDGE('',*,*,#46320,.T.);
#61161=ORIENTED_EDGE('',*,*,#46315,.T.);
#61162=ORIENTED_EDGE('',*,*,#46321,.F.);
#61163=ORIENTED_EDGE('',*,*,#46322,.F.);
#61164=ORIENTED_EDGE('',*,*,#46323,.T.);
#61165=ORIENTED_EDGE('',*,*,#46319,.T.);
#61166=ORIENTED_EDGE('',*,*,#46324,.F.);
#61167=ORIENTED_EDGE('',*,*,#46317,.F.);
#61168=ORIENTED_EDGE('',*,*,#46325,.T.);
#61169=ORIENTED_EDGE('',*,*,#46322,.T.);
#61170=ORIENTED_EDGE('',*,*,#46326,.F.);
#61171=ORIENTED_EDGE('',*,*,#46327,.F.);
#61172=ORIENTED_EDGE('',*,*,#46328,.T.);
#61173=ORIENTED_EDGE('',*,*,#46329,.T.);
#61174=ORIENTED_EDGE('',*,*,#46330,.F.);
#61175=ORIENTED_EDGE('',*,*,#46331,.F.);
#61176=ORIENTED_EDGE('',*,*,#46332,.T.);
#61177=ORIENTED_EDGE('',*,*,#46327,.T.);
#61178=ORIENTED_EDGE('',*,*,#46333,.F.);
#61179=ORIENTED_EDGE('',*,*,#46334,.F.);
#61180=ORIENTED_EDGE('',*,*,#46335,.T.);
#61181=ORIENTED_EDGE('',*,*,#46331,.T.);
#61182=ORIENTED_EDGE('',*,*,#46336,.F.);
#61183=ORIENTED_EDGE('',*,*,#46329,.F.);
#61184=ORIENTED_EDGE('',*,*,#46337,.T.);
#61185=ORIENTED_EDGE('',*,*,#46334,.T.);
#61186=ORIENTED_EDGE('',*,*,#46338,.F.);
#61187=ORIENTED_EDGE('',*,*,#46339,.F.);
#61188=ORIENTED_EDGE('',*,*,#46340,.T.);
#61189=ORIENTED_EDGE('',*,*,#46341,.T.);
#61190=ORIENTED_EDGE('',*,*,#46342,.F.);
#61191=ORIENTED_EDGE('',*,*,#46343,.F.);
#61192=ORIENTED_EDGE('',*,*,#46344,.T.);
#61193=ORIENTED_EDGE('',*,*,#46339,.T.);
#61194=ORIENTED_EDGE('',*,*,#46345,.F.);
#61195=ORIENTED_EDGE('',*,*,#46346,.F.);
#61196=ORIENTED_EDGE('',*,*,#46347,.T.);
#61197=ORIENTED_EDGE('',*,*,#46343,.T.);
#61198=ORIENTED_EDGE('',*,*,#46348,.F.);
#61199=ORIENTED_EDGE('',*,*,#46341,.F.);
#61200=ORIENTED_EDGE('',*,*,#46349,.T.);
#61201=ORIENTED_EDGE('',*,*,#46346,.T.);
#61202=ORIENTED_EDGE('',*,*,#46350,.F.);
#61203=ORIENTED_EDGE('',*,*,#46351,.F.);
#61204=ORIENTED_EDGE('',*,*,#46352,.T.);
#61205=ORIENTED_EDGE('',*,*,#46353,.T.);
#61206=ORIENTED_EDGE('',*,*,#46354,.F.);
#61207=ORIENTED_EDGE('',*,*,#46355,.F.);
#61208=ORIENTED_EDGE('',*,*,#46356,.T.);
#61209=ORIENTED_EDGE('',*,*,#46351,.T.);
#61210=ORIENTED_EDGE('',*,*,#46357,.F.);
#61211=ORIENTED_EDGE('',*,*,#46358,.F.);
#61212=ORIENTED_EDGE('',*,*,#46359,.T.);
#61213=ORIENTED_EDGE('',*,*,#46355,.T.);
#61214=ORIENTED_EDGE('',*,*,#46360,.F.);
#61215=ORIENTED_EDGE('',*,*,#46353,.F.);
#61216=ORIENTED_EDGE('',*,*,#46361,.T.);
#61217=ORIENTED_EDGE('',*,*,#46358,.T.);
#61218=ORIENTED_EDGE('',*,*,#46362,.F.);
#61219=ORIENTED_EDGE('',*,*,#46363,.F.);
#61220=ORIENTED_EDGE('',*,*,#46364,.T.);
#61221=ORIENTED_EDGE('',*,*,#46365,.T.);
#61222=ORIENTED_EDGE('',*,*,#46366,.F.);
#61223=ORIENTED_EDGE('',*,*,#46367,.F.);
#61224=ORIENTED_EDGE('',*,*,#46368,.T.);
#61225=ORIENTED_EDGE('',*,*,#46363,.T.);
#61226=ORIENTED_EDGE('',*,*,#46369,.F.);
#61227=ORIENTED_EDGE('',*,*,#46370,.F.);
#61228=ORIENTED_EDGE('',*,*,#46371,.T.);
#61229=ORIENTED_EDGE('',*,*,#46367,.T.);
#61230=ORIENTED_EDGE('',*,*,#46372,.F.);
#61231=ORIENTED_EDGE('',*,*,#46365,.F.);
#61232=ORIENTED_EDGE('',*,*,#46373,.T.);
#61233=ORIENTED_EDGE('',*,*,#46370,.T.);
#61234=ORIENTED_EDGE('',*,*,#46374,.F.);
#61235=ORIENTED_EDGE('',*,*,#46375,.F.);
#61236=ORIENTED_EDGE('',*,*,#46376,.T.);
#61237=ORIENTED_EDGE('',*,*,#46377,.T.);
#61238=ORIENTED_EDGE('',*,*,#46378,.F.);
#61239=ORIENTED_EDGE('',*,*,#46379,.F.);
#61240=ORIENTED_EDGE('',*,*,#46380,.T.);
#61241=ORIENTED_EDGE('',*,*,#46375,.T.);
#61242=ORIENTED_EDGE('',*,*,#46381,.F.);
#61243=ORIENTED_EDGE('',*,*,#46382,.F.);
#61244=ORIENTED_EDGE('',*,*,#46383,.T.);
#61245=ORIENTED_EDGE('',*,*,#46379,.T.);
#61246=ORIENTED_EDGE('',*,*,#46384,.F.);
#61247=ORIENTED_EDGE('',*,*,#46377,.F.);
#61248=ORIENTED_EDGE('',*,*,#46385,.T.);
#61249=ORIENTED_EDGE('',*,*,#46382,.T.);
#61250=ORIENTED_EDGE('',*,*,#46386,.F.);
#61251=ORIENTED_EDGE('',*,*,#46387,.F.);
#61252=ORIENTED_EDGE('',*,*,#46388,.T.);
#61253=ORIENTED_EDGE('',*,*,#46389,.T.);
#61254=ORIENTED_EDGE('',*,*,#46390,.F.);
#61255=ORIENTED_EDGE('',*,*,#46391,.F.);
#61256=ORIENTED_EDGE('',*,*,#46392,.T.);
#61257=ORIENTED_EDGE('',*,*,#46387,.T.);
#61258=ORIENTED_EDGE('',*,*,#46393,.F.);
#61259=ORIENTED_EDGE('',*,*,#46394,.F.);
#61260=ORIENTED_EDGE('',*,*,#46395,.T.);
#61261=ORIENTED_EDGE('',*,*,#46391,.T.);
#61262=ORIENTED_EDGE('',*,*,#46396,.F.);
#61263=ORIENTED_EDGE('',*,*,#46389,.F.);
#61264=ORIENTED_EDGE('',*,*,#46397,.T.);
#61265=ORIENTED_EDGE('',*,*,#46394,.T.);
#61266=ORIENTED_EDGE('',*,*,#46398,.F.);
#61267=ORIENTED_EDGE('',*,*,#46399,.F.);
#61268=ORIENTED_EDGE('',*,*,#46400,.T.);
#61269=ORIENTED_EDGE('',*,*,#46401,.T.);
#61270=ORIENTED_EDGE('',*,*,#46402,.F.);
#61271=ORIENTED_EDGE('',*,*,#46403,.F.);
#61272=ORIENTED_EDGE('',*,*,#46404,.T.);
#61273=ORIENTED_EDGE('',*,*,#46399,.T.);
#61274=ORIENTED_EDGE('',*,*,#46405,.F.);
#61275=ORIENTED_EDGE('',*,*,#46406,.F.);
#61276=ORIENTED_EDGE('',*,*,#46407,.T.);
#61277=ORIENTED_EDGE('',*,*,#46403,.T.);
#61278=ORIENTED_EDGE('',*,*,#46408,.F.);
#61279=ORIENTED_EDGE('',*,*,#46401,.F.);
#61280=ORIENTED_EDGE('',*,*,#46409,.T.);
#61281=ORIENTED_EDGE('',*,*,#46406,.T.);
#61282=ORIENTED_EDGE('',*,*,#46410,.F.);
#61283=ORIENTED_EDGE('',*,*,#46411,.F.);
#61284=ORIENTED_EDGE('',*,*,#46412,.T.);
#61285=ORIENTED_EDGE('',*,*,#46413,.T.);
#61286=ORIENTED_EDGE('',*,*,#46414,.F.);
#61287=ORIENTED_EDGE('',*,*,#46415,.F.);
#61288=ORIENTED_EDGE('',*,*,#46416,.T.);
#61289=ORIENTED_EDGE('',*,*,#46411,.T.);
#61290=ORIENTED_EDGE('',*,*,#46417,.F.);
#61291=ORIENTED_EDGE('',*,*,#46418,.F.);
#61292=ORIENTED_EDGE('',*,*,#46419,.T.);
#61293=ORIENTED_EDGE('',*,*,#46415,.T.);
#61294=ORIENTED_EDGE('',*,*,#46420,.F.);
#61295=ORIENTED_EDGE('',*,*,#46413,.F.);
#61296=ORIENTED_EDGE('',*,*,#46421,.T.);
#61297=ORIENTED_EDGE('',*,*,#46418,.T.);
#61298=ORIENTED_EDGE('',*,*,#46422,.F.);
#61299=ORIENTED_EDGE('',*,*,#46423,.F.);
#61300=ORIENTED_EDGE('',*,*,#46424,.T.);
#61301=ORIENTED_EDGE('',*,*,#46425,.T.);
#61302=ORIENTED_EDGE('',*,*,#46426,.F.);
#61303=ORIENTED_EDGE('',*,*,#46427,.F.);
#61304=ORIENTED_EDGE('',*,*,#46428,.T.);
#61305=ORIENTED_EDGE('',*,*,#46423,.T.);
#61306=ORIENTED_EDGE('',*,*,#46429,.F.);
#61307=ORIENTED_EDGE('',*,*,#46430,.F.);
#61308=ORIENTED_EDGE('',*,*,#46431,.T.);
#61309=ORIENTED_EDGE('',*,*,#46427,.T.);
#61310=ORIENTED_EDGE('',*,*,#46432,.F.);
#61311=ORIENTED_EDGE('',*,*,#46425,.F.);
#61312=ORIENTED_EDGE('',*,*,#46433,.T.);
#61313=ORIENTED_EDGE('',*,*,#46430,.T.);
#61314=ORIENTED_EDGE('',*,*,#46434,.F.);
#61315=ORIENTED_EDGE('',*,*,#46435,.F.);
#61316=ORIENTED_EDGE('',*,*,#46436,.T.);
#61317=ORIENTED_EDGE('',*,*,#46437,.T.);
#61318=ORIENTED_EDGE('',*,*,#46438,.F.);
#61319=ORIENTED_EDGE('',*,*,#46439,.F.);
#61320=ORIENTED_EDGE('',*,*,#46440,.T.);
#61321=ORIENTED_EDGE('',*,*,#46435,.T.);
#61322=ORIENTED_EDGE('',*,*,#46441,.F.);
#61323=ORIENTED_EDGE('',*,*,#46442,.F.);
#61324=ORIENTED_EDGE('',*,*,#46443,.T.);
#61325=ORIENTED_EDGE('',*,*,#46439,.T.);
#61326=ORIENTED_EDGE('',*,*,#46444,.F.);
#61327=ORIENTED_EDGE('',*,*,#46437,.F.);
#61328=ORIENTED_EDGE('',*,*,#46445,.T.);
#61329=ORIENTED_EDGE('',*,*,#46442,.T.);
#61330=ORIENTED_EDGE('',*,*,#46446,.F.);
#61331=ORIENTED_EDGE('',*,*,#46447,.F.);
#61332=ORIENTED_EDGE('',*,*,#46448,.T.);
#61333=ORIENTED_EDGE('',*,*,#46449,.T.);
#61334=ORIENTED_EDGE('',*,*,#46450,.F.);
#61335=ORIENTED_EDGE('',*,*,#46451,.F.);
#61336=ORIENTED_EDGE('',*,*,#46452,.T.);
#61337=ORIENTED_EDGE('',*,*,#46447,.T.);
#61338=ORIENTED_EDGE('',*,*,#46453,.F.);
#61339=ORIENTED_EDGE('',*,*,#46454,.F.);
#61340=ORIENTED_EDGE('',*,*,#46455,.T.);
#61341=ORIENTED_EDGE('',*,*,#46451,.T.);
#61342=ORIENTED_EDGE('',*,*,#46456,.F.);
#61343=ORIENTED_EDGE('',*,*,#46449,.F.);
#61344=ORIENTED_EDGE('',*,*,#46457,.T.);
#61345=ORIENTED_EDGE('',*,*,#46454,.T.);
#61346=ORIENTED_EDGE('',*,*,#46458,.F.);
#61347=ORIENTED_EDGE('',*,*,#46459,.F.);
#61348=ORIENTED_EDGE('',*,*,#46460,.T.);
#61349=ORIENTED_EDGE('',*,*,#46461,.T.);
#61350=ORIENTED_EDGE('',*,*,#46462,.F.);
#61351=ORIENTED_EDGE('',*,*,#46463,.F.);
#61352=ORIENTED_EDGE('',*,*,#46464,.T.);
#61353=ORIENTED_EDGE('',*,*,#46459,.T.);
#61354=ORIENTED_EDGE('',*,*,#46465,.F.);
#61355=ORIENTED_EDGE('',*,*,#46466,.F.);
#61356=ORIENTED_EDGE('',*,*,#46467,.T.);
#61357=ORIENTED_EDGE('',*,*,#46463,.T.);
#61358=ORIENTED_EDGE('',*,*,#46468,.F.);
#61359=ORIENTED_EDGE('',*,*,#46461,.F.);
#61360=ORIENTED_EDGE('',*,*,#46469,.T.);
#61361=ORIENTED_EDGE('',*,*,#46466,.T.);
#61362=ORIENTED_EDGE('',*,*,#46470,.F.);
#61363=ORIENTED_EDGE('',*,*,#46471,.F.);
#61364=ORIENTED_EDGE('',*,*,#46472,.T.);
#61365=ORIENTED_EDGE('',*,*,#46473,.T.);
#61366=ORIENTED_EDGE('',*,*,#46474,.F.);
#61367=ORIENTED_EDGE('',*,*,#46475,.F.);
#61368=ORIENTED_EDGE('',*,*,#46476,.T.);
#61369=ORIENTED_EDGE('',*,*,#46471,.T.);
#61370=ORIENTED_EDGE('',*,*,#46477,.F.);
#61371=ORIENTED_EDGE('',*,*,#46478,.F.);
#61372=ORIENTED_EDGE('',*,*,#46479,.T.);
#61373=ORIENTED_EDGE('',*,*,#46475,.T.);
#61374=ORIENTED_EDGE('',*,*,#46480,.F.);
#61375=ORIENTED_EDGE('',*,*,#46473,.F.);
#61376=ORIENTED_EDGE('',*,*,#46481,.T.);
#61377=ORIENTED_EDGE('',*,*,#46478,.T.);
#61378=ORIENTED_EDGE('',*,*,#46482,.F.);
#61379=ORIENTED_EDGE('',*,*,#46483,.F.);
#61380=ORIENTED_EDGE('',*,*,#46484,.T.);
#61381=ORIENTED_EDGE('',*,*,#46485,.T.);
#61382=ORIENTED_EDGE('',*,*,#46486,.F.);
#61383=ORIENTED_EDGE('',*,*,#46487,.F.);
#61384=ORIENTED_EDGE('',*,*,#46488,.T.);
#61385=ORIENTED_EDGE('',*,*,#46483,.T.);
#61386=ORIENTED_EDGE('',*,*,#46489,.F.);
#61387=ORIENTED_EDGE('',*,*,#46490,.F.);
#61388=ORIENTED_EDGE('',*,*,#46491,.T.);
#61389=ORIENTED_EDGE('',*,*,#46487,.T.);
#61390=ORIENTED_EDGE('',*,*,#46492,.F.);
#61391=ORIENTED_EDGE('',*,*,#46485,.F.);
#61392=ORIENTED_EDGE('',*,*,#46493,.T.);
#61393=ORIENTED_EDGE('',*,*,#46490,.T.);
#61394=ORIENTED_EDGE('',*,*,#46494,.F.);
#61395=ORIENTED_EDGE('',*,*,#46495,.F.);
#61396=ORIENTED_EDGE('',*,*,#46496,.T.);
#61397=ORIENTED_EDGE('',*,*,#46497,.T.);
#61398=ORIENTED_EDGE('',*,*,#46498,.F.);
#61399=ORIENTED_EDGE('',*,*,#46499,.F.);
#61400=ORIENTED_EDGE('',*,*,#46500,.T.);
#61401=ORIENTED_EDGE('',*,*,#46495,.T.);
#61402=ORIENTED_EDGE('',*,*,#46501,.F.);
#61403=ORIENTED_EDGE('',*,*,#46502,.F.);
#61404=ORIENTED_EDGE('',*,*,#46503,.T.);
#61405=ORIENTED_EDGE('',*,*,#46499,.T.);
#61406=ORIENTED_EDGE('',*,*,#46504,.F.);
#61407=ORIENTED_EDGE('',*,*,#46497,.F.);
#61408=ORIENTED_EDGE('',*,*,#46505,.T.);
#61409=ORIENTED_EDGE('',*,*,#46502,.T.);
#61410=ORIENTED_EDGE('',*,*,#46506,.F.);
#61411=ORIENTED_EDGE('',*,*,#46507,.F.);
#61412=ORIENTED_EDGE('',*,*,#46508,.T.);
#61413=ORIENTED_EDGE('',*,*,#46509,.T.);
#61414=ORIENTED_EDGE('',*,*,#46510,.F.);
#61415=ORIENTED_EDGE('',*,*,#46511,.F.);
#61416=ORIENTED_EDGE('',*,*,#46512,.T.);
#61417=ORIENTED_EDGE('',*,*,#46507,.T.);
#61418=ORIENTED_EDGE('',*,*,#46513,.F.);
#61419=ORIENTED_EDGE('',*,*,#46514,.F.);
#61420=ORIENTED_EDGE('',*,*,#46515,.T.);
#61421=ORIENTED_EDGE('',*,*,#46511,.T.);
#61422=ORIENTED_EDGE('',*,*,#46516,.F.);
#61423=ORIENTED_EDGE('',*,*,#46509,.F.);
#61424=ORIENTED_EDGE('',*,*,#46517,.T.);
#61425=ORIENTED_EDGE('',*,*,#46514,.T.);
#61426=ORIENTED_EDGE('',*,*,#46518,.F.);
#61427=ORIENTED_EDGE('',*,*,#46519,.F.);
#61428=ORIENTED_EDGE('',*,*,#46520,.T.);
#61429=ORIENTED_EDGE('',*,*,#46521,.T.);
#61430=ORIENTED_EDGE('',*,*,#46522,.F.);
#61431=ORIENTED_EDGE('',*,*,#46523,.F.);
#61432=ORIENTED_EDGE('',*,*,#46524,.T.);
#61433=ORIENTED_EDGE('',*,*,#46519,.T.);
#61434=ORIENTED_EDGE('',*,*,#46525,.F.);
#61435=ORIENTED_EDGE('',*,*,#46526,.F.);
#61436=ORIENTED_EDGE('',*,*,#46527,.T.);
#61437=ORIENTED_EDGE('',*,*,#46523,.T.);
#61438=ORIENTED_EDGE('',*,*,#46528,.F.);
#61439=ORIENTED_EDGE('',*,*,#46521,.F.);
#61440=ORIENTED_EDGE('',*,*,#46529,.T.);
#61441=ORIENTED_EDGE('',*,*,#46526,.T.);
#61442=ORIENTED_EDGE('',*,*,#46530,.F.);
#61443=ORIENTED_EDGE('',*,*,#46531,.F.);
#61444=ORIENTED_EDGE('',*,*,#46532,.T.);
#61445=ORIENTED_EDGE('',*,*,#46533,.T.);
#61446=ORIENTED_EDGE('',*,*,#46534,.F.);
#61447=ORIENTED_EDGE('',*,*,#46535,.F.);
#61448=ORIENTED_EDGE('',*,*,#46536,.T.);
#61449=ORIENTED_EDGE('',*,*,#46531,.T.);
#61450=ORIENTED_EDGE('',*,*,#46537,.F.);
#61451=ORIENTED_EDGE('',*,*,#46538,.F.);
#61452=ORIENTED_EDGE('',*,*,#46539,.T.);
#61453=ORIENTED_EDGE('',*,*,#46535,.T.);
#61454=ORIENTED_EDGE('',*,*,#46540,.F.);
#61455=ORIENTED_EDGE('',*,*,#46533,.F.);
#61456=ORIENTED_EDGE('',*,*,#46541,.T.);
#61457=ORIENTED_EDGE('',*,*,#46538,.T.);
#61458=ORIENTED_EDGE('',*,*,#46542,.F.);
#61459=ORIENTED_EDGE('',*,*,#46543,.F.);
#61460=ORIENTED_EDGE('',*,*,#46544,.T.);
#61461=ORIENTED_EDGE('',*,*,#46545,.T.);
#61462=ORIENTED_EDGE('',*,*,#46546,.F.);
#61463=ORIENTED_EDGE('',*,*,#46547,.F.);
#61464=ORIENTED_EDGE('',*,*,#46548,.T.);
#61465=ORIENTED_EDGE('',*,*,#46543,.T.);
#61466=ORIENTED_EDGE('',*,*,#46549,.F.);
#61467=ORIENTED_EDGE('',*,*,#46550,.F.);
#61468=ORIENTED_EDGE('',*,*,#46551,.T.);
#61469=ORIENTED_EDGE('',*,*,#46547,.T.);
#61470=ORIENTED_EDGE('',*,*,#46552,.F.);
#61471=ORIENTED_EDGE('',*,*,#46545,.F.);
#61472=ORIENTED_EDGE('',*,*,#46553,.T.);
#61473=ORIENTED_EDGE('',*,*,#46550,.T.);
#61474=ORIENTED_EDGE('',*,*,#46554,.F.);
#61475=ORIENTED_EDGE('',*,*,#46555,.F.);
#61476=ORIENTED_EDGE('',*,*,#46556,.T.);
#61477=ORIENTED_EDGE('',*,*,#46557,.T.);
#61478=ORIENTED_EDGE('',*,*,#46558,.F.);
#61479=ORIENTED_EDGE('',*,*,#46559,.F.);
#61480=ORIENTED_EDGE('',*,*,#46560,.T.);
#61481=ORIENTED_EDGE('',*,*,#46555,.T.);
#61482=ORIENTED_EDGE('',*,*,#46561,.F.);
#61483=ORIENTED_EDGE('',*,*,#46562,.F.);
#61484=ORIENTED_EDGE('',*,*,#46563,.T.);
#61485=ORIENTED_EDGE('',*,*,#46559,.T.);
#61486=ORIENTED_EDGE('',*,*,#46564,.F.);
#61487=ORIENTED_EDGE('',*,*,#46557,.F.);
#61488=ORIENTED_EDGE('',*,*,#46565,.T.);
#61489=ORIENTED_EDGE('',*,*,#46562,.T.);
#61490=ORIENTED_EDGE('',*,*,#46566,.F.);
#61491=ORIENTED_EDGE('',*,*,#46567,.F.);
#61492=ORIENTED_EDGE('',*,*,#46568,.T.);
#61493=ORIENTED_EDGE('',*,*,#46569,.T.);
#61494=ORIENTED_EDGE('',*,*,#46570,.F.);
#61495=ORIENTED_EDGE('',*,*,#46571,.F.);
#61496=ORIENTED_EDGE('',*,*,#46572,.T.);
#61497=ORIENTED_EDGE('',*,*,#46567,.T.);
#61498=ORIENTED_EDGE('',*,*,#46573,.F.);
#61499=ORIENTED_EDGE('',*,*,#46574,.F.);
#61500=ORIENTED_EDGE('',*,*,#46575,.T.);
#61501=ORIENTED_EDGE('',*,*,#46571,.T.);
#61502=ORIENTED_EDGE('',*,*,#46576,.F.);
#61503=ORIENTED_EDGE('',*,*,#46569,.F.);
#61504=ORIENTED_EDGE('',*,*,#46577,.T.);
#61505=ORIENTED_EDGE('',*,*,#46574,.T.);
#61506=ORIENTED_EDGE('',*,*,#46578,.F.);
#61507=ORIENTED_EDGE('',*,*,#46579,.F.);
#61508=ORIENTED_EDGE('',*,*,#46580,.T.);
#61509=ORIENTED_EDGE('',*,*,#46581,.T.);
#61510=ORIENTED_EDGE('',*,*,#46582,.F.);
#61511=ORIENTED_EDGE('',*,*,#46583,.F.);
#61512=ORIENTED_EDGE('',*,*,#46584,.T.);
#61513=ORIENTED_EDGE('',*,*,#46579,.T.);
#61514=ORIENTED_EDGE('',*,*,#46585,.F.);
#61515=ORIENTED_EDGE('',*,*,#46586,.F.);
#61516=ORIENTED_EDGE('',*,*,#46587,.T.);
#61517=ORIENTED_EDGE('',*,*,#46583,.T.);
#61518=ORIENTED_EDGE('',*,*,#46588,.F.);
#61519=ORIENTED_EDGE('',*,*,#46581,.F.);
#61520=ORIENTED_EDGE('',*,*,#46589,.T.);
#61521=ORIENTED_EDGE('',*,*,#46586,.T.);
#61522=ORIENTED_EDGE('',*,*,#46590,.F.);
#61523=ORIENTED_EDGE('',*,*,#46591,.F.);
#61524=ORIENTED_EDGE('',*,*,#46592,.T.);
#61525=ORIENTED_EDGE('',*,*,#46593,.T.);
#61526=ORIENTED_EDGE('',*,*,#46594,.F.);
#61527=ORIENTED_EDGE('',*,*,#46595,.F.);
#61528=ORIENTED_EDGE('',*,*,#46596,.T.);
#61529=ORIENTED_EDGE('',*,*,#46591,.T.);
#61530=ORIENTED_EDGE('',*,*,#46597,.F.);
#61531=ORIENTED_EDGE('',*,*,#46598,.F.);
#61532=ORIENTED_EDGE('',*,*,#46599,.T.);
#61533=ORIENTED_EDGE('',*,*,#46595,.T.);
#61534=ORIENTED_EDGE('',*,*,#46600,.F.);
#61535=ORIENTED_EDGE('',*,*,#46593,.F.);
#61536=ORIENTED_EDGE('',*,*,#46601,.T.);
#61537=ORIENTED_EDGE('',*,*,#46598,.T.);
#61538=ORIENTED_EDGE('',*,*,#46602,.F.);
#61539=ORIENTED_EDGE('',*,*,#46603,.F.);
#61540=ORIENTED_EDGE('',*,*,#46604,.T.);
#61541=ORIENTED_EDGE('',*,*,#46605,.T.);
#61542=ORIENTED_EDGE('',*,*,#46606,.F.);
#61543=ORIENTED_EDGE('',*,*,#46607,.F.);
#61544=ORIENTED_EDGE('',*,*,#46608,.T.);
#61545=ORIENTED_EDGE('',*,*,#46603,.T.);
#61546=ORIENTED_EDGE('',*,*,#46609,.F.);
#61547=ORIENTED_EDGE('',*,*,#46610,.F.);
#61548=ORIENTED_EDGE('',*,*,#46611,.T.);
#61549=ORIENTED_EDGE('',*,*,#46607,.T.);
#61550=ORIENTED_EDGE('',*,*,#46612,.F.);
#61551=ORIENTED_EDGE('',*,*,#46605,.F.);
#61552=ORIENTED_EDGE('',*,*,#46613,.T.);
#61553=ORIENTED_EDGE('',*,*,#46610,.T.);
#61554=ORIENTED_EDGE('',*,*,#46614,.F.);
#61555=ORIENTED_EDGE('',*,*,#46615,.F.);
#61556=ORIENTED_EDGE('',*,*,#46616,.T.);
#61557=ORIENTED_EDGE('',*,*,#46617,.T.);
#61558=ORIENTED_EDGE('',*,*,#46618,.F.);
#61559=ORIENTED_EDGE('',*,*,#46619,.F.);
#61560=ORIENTED_EDGE('',*,*,#46620,.T.);
#61561=ORIENTED_EDGE('',*,*,#46615,.T.);
#61562=ORIENTED_EDGE('',*,*,#46621,.F.);
#61563=ORIENTED_EDGE('',*,*,#46622,.F.);
#61564=ORIENTED_EDGE('',*,*,#46623,.T.);
#61565=ORIENTED_EDGE('',*,*,#46619,.T.);
#61566=ORIENTED_EDGE('',*,*,#46624,.F.);
#61567=ORIENTED_EDGE('',*,*,#46617,.F.);
#61568=ORIENTED_EDGE('',*,*,#46625,.T.);
#61569=ORIENTED_EDGE('',*,*,#46622,.T.);
#61570=ORIENTED_EDGE('',*,*,#46626,.F.);
#61571=ORIENTED_EDGE('',*,*,#46627,.F.);
#61572=ORIENTED_EDGE('',*,*,#46628,.T.);
#61573=ORIENTED_EDGE('',*,*,#46629,.T.);
#61574=ORIENTED_EDGE('',*,*,#46630,.F.);
#61575=ORIENTED_EDGE('',*,*,#46631,.F.);
#61576=ORIENTED_EDGE('',*,*,#46632,.T.);
#61577=ORIENTED_EDGE('',*,*,#46627,.T.);
#61578=ORIENTED_EDGE('',*,*,#46633,.F.);
#61579=ORIENTED_EDGE('',*,*,#46634,.F.);
#61580=ORIENTED_EDGE('',*,*,#46635,.T.);
#61581=ORIENTED_EDGE('',*,*,#46631,.T.);
#61582=ORIENTED_EDGE('',*,*,#46636,.F.);
#61583=ORIENTED_EDGE('',*,*,#46629,.F.);
#61584=ORIENTED_EDGE('',*,*,#46637,.T.);
#61585=ORIENTED_EDGE('',*,*,#46634,.T.);
#61586=ORIENTED_EDGE('',*,*,#46638,.F.);
#61587=ORIENTED_EDGE('',*,*,#46639,.F.);
#61588=ORIENTED_EDGE('',*,*,#46640,.T.);
#61589=ORIENTED_EDGE('',*,*,#46641,.T.);
#61590=ORIENTED_EDGE('',*,*,#46642,.F.);
#61591=ORIENTED_EDGE('',*,*,#46643,.F.);
#61592=ORIENTED_EDGE('',*,*,#46644,.T.);
#61593=ORIENTED_EDGE('',*,*,#46639,.T.);
#61594=ORIENTED_EDGE('',*,*,#46645,.F.);
#61595=ORIENTED_EDGE('',*,*,#46646,.F.);
#61596=ORIENTED_EDGE('',*,*,#46647,.T.);
#61597=ORIENTED_EDGE('',*,*,#46643,.T.);
#61598=ORIENTED_EDGE('',*,*,#46648,.F.);
#61599=ORIENTED_EDGE('',*,*,#46641,.F.);
#61600=ORIENTED_EDGE('',*,*,#46649,.T.);
#61601=ORIENTED_EDGE('',*,*,#46646,.T.);
#61602=ORIENTED_EDGE('',*,*,#46650,.F.);
#61603=ORIENTED_EDGE('',*,*,#46651,.F.);
#61604=ORIENTED_EDGE('',*,*,#46652,.T.);
#61605=ORIENTED_EDGE('',*,*,#46653,.T.);
#61606=ORIENTED_EDGE('',*,*,#46654,.F.);
#61607=ORIENTED_EDGE('',*,*,#46655,.F.);
#61608=ORIENTED_EDGE('',*,*,#46656,.T.);
#61609=ORIENTED_EDGE('',*,*,#46651,.T.);
#61610=ORIENTED_EDGE('',*,*,#46657,.F.);
#61611=ORIENTED_EDGE('',*,*,#46658,.F.);
#61612=ORIENTED_EDGE('',*,*,#46659,.T.);
#61613=ORIENTED_EDGE('',*,*,#46655,.T.);
#61614=ORIENTED_EDGE('',*,*,#46660,.F.);
#61615=ORIENTED_EDGE('',*,*,#46653,.F.);
#61616=ORIENTED_EDGE('',*,*,#46661,.T.);
#61617=ORIENTED_EDGE('',*,*,#46658,.T.);
#61618=ORIENTED_EDGE('',*,*,#46662,.F.);
#61619=ORIENTED_EDGE('',*,*,#46663,.F.);
#61620=ORIENTED_EDGE('',*,*,#46664,.T.);
#61621=ORIENTED_EDGE('',*,*,#46665,.T.);
#61622=ORIENTED_EDGE('',*,*,#46666,.F.);
#61623=ORIENTED_EDGE('',*,*,#46667,.F.);
#61624=ORIENTED_EDGE('',*,*,#46668,.T.);
#61625=ORIENTED_EDGE('',*,*,#46663,.T.);
#61626=ORIENTED_EDGE('',*,*,#46669,.F.);
#61627=ORIENTED_EDGE('',*,*,#46670,.F.);
#61628=ORIENTED_EDGE('',*,*,#46671,.T.);
#61629=ORIENTED_EDGE('',*,*,#46667,.T.);
#61630=ORIENTED_EDGE('',*,*,#46672,.F.);
#61631=ORIENTED_EDGE('',*,*,#46665,.F.);
#61632=ORIENTED_EDGE('',*,*,#46673,.T.);
#61633=ORIENTED_EDGE('',*,*,#46670,.T.);
#61634=ORIENTED_EDGE('',*,*,#46674,.F.);
#61635=ORIENTED_EDGE('',*,*,#46675,.F.);
#61636=ORIENTED_EDGE('',*,*,#46676,.T.);
#61637=ORIENTED_EDGE('',*,*,#46677,.T.);
#61638=ORIENTED_EDGE('',*,*,#46678,.F.);
#61639=ORIENTED_EDGE('',*,*,#46679,.F.);
#61640=ORIENTED_EDGE('',*,*,#46680,.T.);
#61641=ORIENTED_EDGE('',*,*,#46675,.T.);
#61642=ORIENTED_EDGE('',*,*,#46681,.F.);
#61643=ORIENTED_EDGE('',*,*,#46682,.F.);
#61644=ORIENTED_EDGE('',*,*,#46683,.T.);
#61645=ORIENTED_EDGE('',*,*,#46679,.T.);
#61646=ORIENTED_EDGE('',*,*,#46684,.F.);
#61647=ORIENTED_EDGE('',*,*,#46677,.F.);
#61648=ORIENTED_EDGE('',*,*,#46685,.T.);
#61649=ORIENTED_EDGE('',*,*,#46682,.T.);
#61650=ORIENTED_EDGE('',*,*,#46686,.F.);
#61651=ORIENTED_EDGE('',*,*,#46687,.F.);
#61652=ORIENTED_EDGE('',*,*,#46688,.T.);
#61653=ORIENTED_EDGE('',*,*,#46689,.T.);
#61654=ORIENTED_EDGE('',*,*,#46690,.F.);
#61655=ORIENTED_EDGE('',*,*,#46691,.F.);
#61656=ORIENTED_EDGE('',*,*,#46692,.T.);
#61657=ORIENTED_EDGE('',*,*,#46687,.T.);
#61658=ORIENTED_EDGE('',*,*,#46693,.F.);
#61659=ORIENTED_EDGE('',*,*,#46694,.F.);
#61660=ORIENTED_EDGE('',*,*,#46695,.T.);
#61661=ORIENTED_EDGE('',*,*,#46691,.T.);
#61662=ORIENTED_EDGE('',*,*,#46696,.F.);
#61663=ORIENTED_EDGE('',*,*,#46689,.F.);
#61664=ORIENTED_EDGE('',*,*,#46697,.T.);
#61665=ORIENTED_EDGE('',*,*,#46694,.T.);
#61666=ORIENTED_EDGE('',*,*,#46698,.F.);
#61667=ORIENTED_EDGE('',*,*,#46699,.F.);
#61668=ORIENTED_EDGE('',*,*,#46700,.T.);
#61669=ORIENTED_EDGE('',*,*,#46701,.T.);
#61670=ORIENTED_EDGE('',*,*,#46702,.F.);
#61671=ORIENTED_EDGE('',*,*,#46703,.F.);
#61672=ORIENTED_EDGE('',*,*,#46704,.T.);
#61673=ORIENTED_EDGE('',*,*,#46699,.T.);
#61674=ORIENTED_EDGE('',*,*,#46705,.F.);
#61675=ORIENTED_EDGE('',*,*,#46706,.F.);
#61676=ORIENTED_EDGE('',*,*,#46707,.T.);
#61677=ORIENTED_EDGE('',*,*,#46703,.T.);
#61678=ORIENTED_EDGE('',*,*,#46708,.F.);
#61679=ORIENTED_EDGE('',*,*,#46701,.F.);
#61680=ORIENTED_EDGE('',*,*,#46709,.T.);
#61681=ORIENTED_EDGE('',*,*,#46706,.T.);
#61682=ORIENTED_EDGE('',*,*,#46710,.F.);
#61683=ORIENTED_EDGE('',*,*,#46711,.F.);
#61684=ORIENTED_EDGE('',*,*,#46712,.T.);
#61685=ORIENTED_EDGE('',*,*,#46713,.T.);
#61686=ORIENTED_EDGE('',*,*,#46714,.F.);
#61687=ORIENTED_EDGE('',*,*,#46715,.F.);
#61688=ORIENTED_EDGE('',*,*,#46716,.T.);
#61689=ORIENTED_EDGE('',*,*,#46711,.T.);
#61690=ORIENTED_EDGE('',*,*,#46717,.F.);
#61691=ORIENTED_EDGE('',*,*,#46718,.F.);
#61692=ORIENTED_EDGE('',*,*,#46719,.T.);
#61693=ORIENTED_EDGE('',*,*,#46715,.T.);
#61694=ORIENTED_EDGE('',*,*,#46720,.F.);
#61695=ORIENTED_EDGE('',*,*,#46713,.F.);
#61696=ORIENTED_EDGE('',*,*,#46721,.T.);
#61697=ORIENTED_EDGE('',*,*,#46718,.T.);
#61698=ORIENTED_EDGE('',*,*,#46722,.F.);
#61699=ORIENTED_EDGE('',*,*,#46723,.F.);
#61700=ORIENTED_EDGE('',*,*,#46724,.T.);
#61701=ORIENTED_EDGE('',*,*,#46725,.T.);
#61702=ORIENTED_EDGE('',*,*,#46726,.F.);
#61703=ORIENTED_EDGE('',*,*,#46727,.F.);
#61704=ORIENTED_EDGE('',*,*,#46728,.T.);
#61705=ORIENTED_EDGE('',*,*,#46723,.T.);
#61706=ORIENTED_EDGE('',*,*,#46729,.F.);
#61707=ORIENTED_EDGE('',*,*,#46730,.F.);
#61708=ORIENTED_EDGE('',*,*,#46731,.T.);
#61709=ORIENTED_EDGE('',*,*,#46727,.T.);
#61710=ORIENTED_EDGE('',*,*,#46732,.F.);
#61711=ORIENTED_EDGE('',*,*,#46725,.F.);
#61712=ORIENTED_EDGE('',*,*,#46733,.T.);
#61713=ORIENTED_EDGE('',*,*,#46730,.T.);
#61714=ORIENTED_EDGE('',*,*,#46734,.F.);
#61715=ORIENTED_EDGE('',*,*,#43509,.F.);
#61716=ORIENTED_EDGE('',*,*,#43504,.F.);
#61717=ORIENTED_EDGE('',*,*,#46735,.T.);
#61718=ORIENTED_EDGE('',*,*,#46736,.F.);
#61719=ORIENTED_EDGE('',*,*,#46737,.F.);
#61720=ORIENTED_EDGE('',*,*,#46738,.T.);
#61721=ORIENTED_EDGE('',*,*,#46739,.T.);
#61722=ORIENTED_EDGE('',*,*,#46740,.F.);
#61723=ORIENTED_EDGE('',*,*,#46735,.F.);
#61724=ORIENTED_EDGE('',*,*,#46741,.T.);
#61725=ORIENTED_EDGE('',*,*,#46742,.T.);
#61726=ORIENTED_EDGE('',*,*,#46743,.F.);
#61727=ORIENTED_EDGE('',*,*,#46739,.F.);
#61728=ORIENTED_EDGE('',*,*,#46744,.T.);
#61729=ORIENTED_EDGE('',*,*,#46737,.T.);
#61730=ORIENTED_EDGE('',*,*,#46745,.F.);
#61731=ORIENTED_EDGE('',*,*,#46742,.F.);
#61732=ORIENTED_EDGE('',*,*,#46746,.T.);
#61733=ORIENTED_EDGE('',*,*,#46747,.T.);
#61734=ORIENTED_EDGE('',*,*,#46748,.F.);
#61735=ORIENTED_EDGE('',*,*,#46749,.F.);
#61736=ORIENTED_EDGE('',*,*,#46750,.T.);
#61737=ORIENTED_EDGE('',*,*,#46751,.T.);
#61738=ORIENTED_EDGE('',*,*,#46752,.F.);
#61739=ORIENTED_EDGE('',*,*,#46747,.F.);
#61740=ORIENTED_EDGE('',*,*,#46753,.T.);
#61741=ORIENTED_EDGE('',*,*,#46754,.T.);
#61742=ORIENTED_EDGE('',*,*,#46755,.F.);
#61743=ORIENTED_EDGE('',*,*,#46751,.F.);
#61744=ORIENTED_EDGE('',*,*,#46756,.T.);
#61745=ORIENTED_EDGE('',*,*,#46749,.T.);
#61746=ORIENTED_EDGE('',*,*,#46757,.F.);
#61747=ORIENTED_EDGE('',*,*,#46754,.F.);
#61748=ORIENTED_EDGE('',*,*,#46758,.T.);
#61749=ORIENTED_EDGE('',*,*,#46759,.T.);
#61750=ORIENTED_EDGE('',*,*,#46760,.F.);
#61751=ORIENTED_EDGE('',*,*,#46761,.F.);
#61752=ORIENTED_EDGE('',*,*,#46762,.T.);
#61753=ORIENTED_EDGE('',*,*,#46763,.T.);
#61754=ORIENTED_EDGE('',*,*,#46764,.F.);
#61755=ORIENTED_EDGE('',*,*,#46759,.F.);
#61756=ORIENTED_EDGE('',*,*,#46765,.T.);
#61757=ORIENTED_EDGE('',*,*,#46766,.T.);
#61758=ORIENTED_EDGE('',*,*,#46767,.F.);
#61759=ORIENTED_EDGE('',*,*,#46763,.F.);
#61760=ORIENTED_EDGE('',*,*,#46768,.T.);
#61761=ORIENTED_EDGE('',*,*,#46761,.T.);
#61762=ORIENTED_EDGE('',*,*,#46769,.F.);
#61763=ORIENTED_EDGE('',*,*,#46766,.F.);
#61764=ORIENTED_EDGE('',*,*,#46770,.T.);
#61765=ORIENTED_EDGE('',*,*,#46771,.T.);
#61766=ORIENTED_EDGE('',*,*,#46772,.F.);
#61767=ORIENTED_EDGE('',*,*,#46773,.F.);
#61768=ORIENTED_EDGE('',*,*,#46774,.T.);
#61769=ORIENTED_EDGE('',*,*,#46775,.T.);
#61770=ORIENTED_EDGE('',*,*,#46776,.F.);
#61771=ORIENTED_EDGE('',*,*,#46771,.F.);
#61772=ORIENTED_EDGE('',*,*,#46777,.T.);
#61773=ORIENTED_EDGE('',*,*,#46778,.T.);
#61774=ORIENTED_EDGE('',*,*,#46779,.F.);
#61775=ORIENTED_EDGE('',*,*,#46775,.F.);
#61776=ORIENTED_EDGE('',*,*,#46780,.T.);
#61777=ORIENTED_EDGE('',*,*,#46773,.T.);
#61778=ORIENTED_EDGE('',*,*,#46781,.F.);
#61779=ORIENTED_EDGE('',*,*,#46778,.F.);
#61780=ORIENTED_EDGE('',*,*,#46782,.T.);
#61781=ORIENTED_EDGE('',*,*,#46783,.T.);
#61782=ORIENTED_EDGE('',*,*,#46784,.F.);
#61783=ORIENTED_EDGE('',*,*,#46785,.F.);
#61784=ORIENTED_EDGE('',*,*,#46786,.T.);
#61785=ORIENTED_EDGE('',*,*,#46787,.T.);
#61786=ORIENTED_EDGE('',*,*,#46788,.F.);
#61787=ORIENTED_EDGE('',*,*,#46783,.F.);
#61788=ORIENTED_EDGE('',*,*,#46789,.T.);
#61789=ORIENTED_EDGE('',*,*,#46790,.T.);
#61790=ORIENTED_EDGE('',*,*,#46791,.F.);
#61791=ORIENTED_EDGE('',*,*,#46787,.F.);
#61792=ORIENTED_EDGE('',*,*,#46792,.T.);
#61793=ORIENTED_EDGE('',*,*,#46785,.T.);
#61794=ORIENTED_EDGE('',*,*,#46793,.F.);
#61795=ORIENTED_EDGE('',*,*,#46790,.F.);
#61796=ORIENTED_EDGE('',*,*,#46794,.T.);
#61797=ORIENTED_EDGE('',*,*,#46795,.T.);
#61798=ORIENTED_EDGE('',*,*,#46796,.F.);
#61799=ORIENTED_EDGE('',*,*,#46797,.F.);
#61800=ORIENTED_EDGE('',*,*,#46798,.T.);
#61801=ORIENTED_EDGE('',*,*,#46799,.T.);
#61802=ORIENTED_EDGE('',*,*,#46800,.F.);
#61803=ORIENTED_EDGE('',*,*,#46795,.F.);
#61804=ORIENTED_EDGE('',*,*,#46801,.T.);
#61805=ORIENTED_EDGE('',*,*,#46802,.T.);
#61806=ORIENTED_EDGE('',*,*,#46803,.F.);
#61807=ORIENTED_EDGE('',*,*,#46799,.F.);
#61808=ORIENTED_EDGE('',*,*,#46804,.T.);
#61809=ORIENTED_EDGE('',*,*,#46797,.T.);
#61810=ORIENTED_EDGE('',*,*,#46805,.F.);
#61811=ORIENTED_EDGE('',*,*,#46802,.F.);
#61812=ORIENTED_EDGE('',*,*,#46806,.T.);
#61813=ORIENTED_EDGE('',*,*,#46807,.T.);
#61814=ORIENTED_EDGE('',*,*,#46808,.F.);
#61815=ORIENTED_EDGE('',*,*,#46809,.F.);
#61816=ORIENTED_EDGE('',*,*,#46810,.T.);
#61817=ORIENTED_EDGE('',*,*,#46811,.T.);
#61818=ORIENTED_EDGE('',*,*,#46812,.F.);
#61819=ORIENTED_EDGE('',*,*,#46807,.F.);
#61820=ORIENTED_EDGE('',*,*,#46813,.T.);
#61821=ORIENTED_EDGE('',*,*,#46814,.T.);
#61822=ORIENTED_EDGE('',*,*,#46815,.F.);
#61823=ORIENTED_EDGE('',*,*,#46811,.F.);
#61824=ORIENTED_EDGE('',*,*,#46816,.T.);
#61825=ORIENTED_EDGE('',*,*,#46809,.T.);
#61826=ORIENTED_EDGE('',*,*,#46817,.F.);
#61827=ORIENTED_EDGE('',*,*,#46814,.F.);
#61828=ORIENTED_EDGE('',*,*,#46818,.T.);
#61829=ORIENTED_EDGE('',*,*,#46819,.T.);
#61830=ORIENTED_EDGE('',*,*,#46820,.F.);
#61831=ORIENTED_EDGE('',*,*,#46821,.F.);
#61832=ORIENTED_EDGE('',*,*,#46822,.T.);
#61833=ORIENTED_EDGE('',*,*,#46823,.T.);
#61834=ORIENTED_EDGE('',*,*,#46824,.F.);
#61835=ORIENTED_EDGE('',*,*,#46819,.F.);
#61836=ORIENTED_EDGE('',*,*,#46825,.T.);
#61837=ORIENTED_EDGE('',*,*,#46826,.T.);
#61838=ORIENTED_EDGE('',*,*,#46827,.F.);
#61839=ORIENTED_EDGE('',*,*,#46823,.F.);
#61840=ORIENTED_EDGE('',*,*,#46828,.T.);
#61841=ORIENTED_EDGE('',*,*,#46821,.T.);
#61842=ORIENTED_EDGE('',*,*,#46829,.F.);
#61843=ORIENTED_EDGE('',*,*,#46826,.F.);
#61844=ORIENTED_EDGE('',*,*,#46830,.T.);
#61845=ORIENTED_EDGE('',*,*,#46831,.T.);
#61846=ORIENTED_EDGE('',*,*,#46832,.F.);
#61847=ORIENTED_EDGE('',*,*,#46833,.F.);
#61848=ORIENTED_EDGE('',*,*,#46834,.T.);
#61849=ORIENTED_EDGE('',*,*,#46835,.T.);
#61850=ORIENTED_EDGE('',*,*,#46836,.F.);
#61851=ORIENTED_EDGE('',*,*,#46831,.F.);
#61852=ORIENTED_EDGE('',*,*,#46837,.T.);
#61853=ORIENTED_EDGE('',*,*,#46838,.T.);
#61854=ORIENTED_EDGE('',*,*,#46839,.F.);
#61855=ORIENTED_EDGE('',*,*,#46835,.F.);
#61856=ORIENTED_EDGE('',*,*,#46840,.T.);
#61857=ORIENTED_EDGE('',*,*,#46833,.T.);
#61858=ORIENTED_EDGE('',*,*,#46841,.F.);
#61859=ORIENTED_EDGE('',*,*,#46838,.F.);
#61860=ORIENTED_EDGE('',*,*,#46842,.T.);
#61861=ORIENTED_EDGE('',*,*,#46843,.T.);
#61862=ORIENTED_EDGE('',*,*,#46844,.F.);
#61863=ORIENTED_EDGE('',*,*,#46845,.F.);
#61864=ORIENTED_EDGE('',*,*,#46846,.T.);
#61865=ORIENTED_EDGE('',*,*,#46847,.T.);
#61866=ORIENTED_EDGE('',*,*,#46848,.F.);
#61867=ORIENTED_EDGE('',*,*,#46843,.F.);
#61868=ORIENTED_EDGE('',*,*,#46849,.T.);
#61869=ORIENTED_EDGE('',*,*,#46850,.T.);
#61870=ORIENTED_EDGE('',*,*,#46851,.F.);
#61871=ORIENTED_EDGE('',*,*,#46847,.F.);
#61872=ORIENTED_EDGE('',*,*,#46852,.T.);
#61873=ORIENTED_EDGE('',*,*,#46845,.T.);
#61874=ORIENTED_EDGE('',*,*,#46853,.F.);
#61875=ORIENTED_EDGE('',*,*,#46850,.F.);
#61876=ORIENTED_EDGE('',*,*,#46854,.T.);
#61877=ORIENTED_EDGE('',*,*,#46855,.T.);
#61878=ORIENTED_EDGE('',*,*,#46856,.F.);
#61879=ORIENTED_EDGE('',*,*,#46857,.F.);
#61880=ORIENTED_EDGE('',*,*,#46858,.T.);
#61881=ORIENTED_EDGE('',*,*,#46859,.T.);
#61882=ORIENTED_EDGE('',*,*,#46860,.F.);
#61883=ORIENTED_EDGE('',*,*,#46855,.F.);
#61884=ORIENTED_EDGE('',*,*,#46861,.T.);
#61885=ORIENTED_EDGE('',*,*,#46862,.T.);
#61886=ORIENTED_EDGE('',*,*,#46863,.F.);
#61887=ORIENTED_EDGE('',*,*,#46859,.F.);
#61888=ORIENTED_EDGE('',*,*,#46864,.T.);
#61889=ORIENTED_EDGE('',*,*,#46857,.T.);
#61890=ORIENTED_EDGE('',*,*,#46865,.F.);
#61891=ORIENTED_EDGE('',*,*,#46862,.F.);
#61892=ORIENTED_EDGE('',*,*,#46866,.T.);
#61893=ORIENTED_EDGE('',*,*,#46867,.T.);
#61894=ORIENTED_EDGE('',*,*,#46868,.F.);
#61895=ORIENTED_EDGE('',*,*,#46869,.F.);
#61896=ORIENTED_EDGE('',*,*,#46870,.T.);
#61897=ORIENTED_EDGE('',*,*,#46871,.T.);
#61898=ORIENTED_EDGE('',*,*,#46872,.F.);
#61899=ORIENTED_EDGE('',*,*,#46867,.F.);
#61900=ORIENTED_EDGE('',*,*,#46873,.T.);
#61901=ORIENTED_EDGE('',*,*,#46874,.T.);
#61902=ORIENTED_EDGE('',*,*,#46875,.F.);
#61903=ORIENTED_EDGE('',*,*,#46871,.F.);
#61904=ORIENTED_EDGE('',*,*,#46876,.T.);
#61905=ORIENTED_EDGE('',*,*,#46869,.T.);
#61906=ORIENTED_EDGE('',*,*,#46877,.F.);
#61907=ORIENTED_EDGE('',*,*,#46874,.F.);
#61908=ORIENTED_EDGE('',*,*,#46878,.T.);
#61909=ORIENTED_EDGE('',*,*,#46879,.T.);
#61910=ORIENTED_EDGE('',*,*,#46880,.F.);
#61911=ORIENTED_EDGE('',*,*,#46881,.F.);
#61912=ORIENTED_EDGE('',*,*,#46882,.T.);
#61913=ORIENTED_EDGE('',*,*,#46883,.T.);
#61914=ORIENTED_EDGE('',*,*,#46884,.F.);
#61915=ORIENTED_EDGE('',*,*,#46879,.F.);
#61916=ORIENTED_EDGE('',*,*,#46885,.T.);
#61917=ORIENTED_EDGE('',*,*,#46886,.T.);
#61918=ORIENTED_EDGE('',*,*,#46887,.F.);
#61919=ORIENTED_EDGE('',*,*,#46883,.F.);
#61920=ORIENTED_EDGE('',*,*,#46888,.T.);
#61921=ORIENTED_EDGE('',*,*,#46881,.T.);
#61922=ORIENTED_EDGE('',*,*,#46889,.F.);
#61923=ORIENTED_EDGE('',*,*,#46886,.F.);
#61924=ORIENTED_EDGE('',*,*,#46890,.T.);
#61925=ORIENTED_EDGE('',*,*,#46891,.T.);
#61926=ORIENTED_EDGE('',*,*,#46892,.F.);
#61927=ORIENTED_EDGE('',*,*,#46893,.F.);
#61928=ORIENTED_EDGE('',*,*,#46894,.T.);
#61929=ORIENTED_EDGE('',*,*,#46895,.T.);
#61930=ORIENTED_EDGE('',*,*,#46896,.F.);
#61931=ORIENTED_EDGE('',*,*,#46891,.F.);
#61932=ORIENTED_EDGE('',*,*,#46897,.T.);
#61933=ORIENTED_EDGE('',*,*,#46898,.T.);
#61934=ORIENTED_EDGE('',*,*,#46899,.F.);
#61935=ORIENTED_EDGE('',*,*,#46895,.F.);
#61936=ORIENTED_EDGE('',*,*,#46900,.T.);
#61937=ORIENTED_EDGE('',*,*,#46893,.T.);
#61938=ORIENTED_EDGE('',*,*,#46901,.F.);
#61939=ORIENTED_EDGE('',*,*,#46898,.F.);
#61940=ORIENTED_EDGE('',*,*,#46902,.T.);
#61941=ORIENTED_EDGE('',*,*,#46903,.T.);
#61942=ORIENTED_EDGE('',*,*,#46904,.F.);
#61943=ORIENTED_EDGE('',*,*,#46905,.F.);
#61944=ORIENTED_EDGE('',*,*,#46906,.T.);
#61945=ORIENTED_EDGE('',*,*,#46907,.T.);
#61946=ORIENTED_EDGE('',*,*,#46908,.F.);
#61947=ORIENTED_EDGE('',*,*,#46903,.F.);
#61948=ORIENTED_EDGE('',*,*,#46909,.T.);
#61949=ORIENTED_EDGE('',*,*,#46910,.T.);
#61950=ORIENTED_EDGE('',*,*,#46911,.F.);
#61951=ORIENTED_EDGE('',*,*,#46907,.F.);
#61952=ORIENTED_EDGE('',*,*,#46912,.T.);
#61953=ORIENTED_EDGE('',*,*,#46905,.T.);
#61954=ORIENTED_EDGE('',*,*,#46913,.F.);
#61955=ORIENTED_EDGE('',*,*,#46910,.F.);
#61956=ORIENTED_EDGE('',*,*,#46914,.T.);
#61957=ORIENTED_EDGE('',*,*,#46915,.T.);
#61958=ORIENTED_EDGE('',*,*,#46916,.F.);
#61959=ORIENTED_EDGE('',*,*,#46917,.F.);
#61960=ORIENTED_EDGE('',*,*,#46918,.T.);
#61961=ORIENTED_EDGE('',*,*,#46919,.T.);
#61962=ORIENTED_EDGE('',*,*,#46920,.F.);
#61963=ORIENTED_EDGE('',*,*,#46915,.F.);
#61964=ORIENTED_EDGE('',*,*,#46921,.T.);
#61965=ORIENTED_EDGE('',*,*,#46922,.T.);
#61966=ORIENTED_EDGE('',*,*,#46923,.F.);
#61967=ORIENTED_EDGE('',*,*,#46919,.F.);
#61968=ORIENTED_EDGE('',*,*,#46924,.T.);
#61969=ORIENTED_EDGE('',*,*,#46917,.T.);
#61970=ORIENTED_EDGE('',*,*,#46925,.F.);
#61971=ORIENTED_EDGE('',*,*,#46922,.F.);
#61972=ORIENTED_EDGE('',*,*,#46926,.T.);
#61973=ORIENTED_EDGE('',*,*,#46927,.T.);
#61974=ORIENTED_EDGE('',*,*,#46928,.F.);
#61975=ORIENTED_EDGE('',*,*,#46929,.F.);
#61976=ORIENTED_EDGE('',*,*,#46930,.T.);
#61977=ORIENTED_EDGE('',*,*,#46931,.T.);
#61978=ORIENTED_EDGE('',*,*,#46932,.F.);
#61979=ORIENTED_EDGE('',*,*,#46927,.F.);
#61980=ORIENTED_EDGE('',*,*,#46933,.T.);
#61981=ORIENTED_EDGE('',*,*,#46934,.T.);
#61982=ORIENTED_EDGE('',*,*,#46935,.F.);
#61983=ORIENTED_EDGE('',*,*,#46931,.F.);
#61984=ORIENTED_EDGE('',*,*,#46936,.T.);
#61985=ORIENTED_EDGE('',*,*,#46929,.T.);
#61986=ORIENTED_EDGE('',*,*,#46937,.F.);
#61987=ORIENTED_EDGE('',*,*,#46934,.F.);
#61988=ORIENTED_EDGE('',*,*,#46938,.T.);
#61989=ORIENTED_EDGE('',*,*,#46939,.T.);
#61990=ORIENTED_EDGE('',*,*,#46940,.F.);
#61991=ORIENTED_EDGE('',*,*,#46941,.F.);
#61992=ORIENTED_EDGE('',*,*,#46942,.T.);
#61993=ORIENTED_EDGE('',*,*,#46943,.T.);
#61994=ORIENTED_EDGE('',*,*,#46944,.F.);
#61995=ORIENTED_EDGE('',*,*,#46939,.F.);
#61996=ORIENTED_EDGE('',*,*,#46945,.T.);
#61997=ORIENTED_EDGE('',*,*,#46946,.T.);
#61998=ORIENTED_EDGE('',*,*,#46947,.F.);
#61999=ORIENTED_EDGE('',*,*,#46943,.F.);
#62000=ORIENTED_EDGE('',*,*,#46948,.T.);
#62001=ORIENTED_EDGE('',*,*,#46941,.T.);
#62002=ORIENTED_EDGE('',*,*,#46949,.F.);
#62003=ORIENTED_EDGE('',*,*,#46946,.F.);
#62004=ORIENTED_EDGE('',*,*,#46950,.T.);
#62005=ORIENTED_EDGE('',*,*,#46951,.T.);
#62006=ORIENTED_EDGE('',*,*,#46952,.F.);
#62007=ORIENTED_EDGE('',*,*,#46953,.F.);
#62008=ORIENTED_EDGE('',*,*,#46954,.T.);
#62009=ORIENTED_EDGE('',*,*,#46955,.T.);
#62010=ORIENTED_EDGE('',*,*,#46956,.F.);
#62011=ORIENTED_EDGE('',*,*,#46951,.F.);
#62012=ORIENTED_EDGE('',*,*,#46957,.T.);
#62013=ORIENTED_EDGE('',*,*,#46958,.T.);
#62014=ORIENTED_EDGE('',*,*,#46959,.F.);
#62015=ORIENTED_EDGE('',*,*,#46955,.F.);
#62016=ORIENTED_EDGE('',*,*,#46960,.T.);
#62017=ORIENTED_EDGE('',*,*,#46953,.T.);
#62018=ORIENTED_EDGE('',*,*,#46961,.F.);
#62019=ORIENTED_EDGE('',*,*,#46958,.F.);
#62020=ORIENTED_EDGE('',*,*,#46962,.T.);
#62021=ORIENTED_EDGE('',*,*,#46963,.T.);
#62022=ORIENTED_EDGE('',*,*,#46964,.F.);
#62023=ORIENTED_EDGE('',*,*,#46965,.F.);
#62024=ORIENTED_EDGE('',*,*,#46966,.T.);
#62025=ORIENTED_EDGE('',*,*,#46967,.T.);
#62026=ORIENTED_EDGE('',*,*,#46968,.F.);
#62027=ORIENTED_EDGE('',*,*,#46963,.F.);
#62028=ORIENTED_EDGE('',*,*,#46969,.T.);
#62029=ORIENTED_EDGE('',*,*,#46970,.T.);
#62030=ORIENTED_EDGE('',*,*,#46971,.F.);
#62031=ORIENTED_EDGE('',*,*,#46967,.F.);
#62032=ORIENTED_EDGE('',*,*,#46972,.T.);
#62033=ORIENTED_EDGE('',*,*,#46965,.T.);
#62034=ORIENTED_EDGE('',*,*,#46973,.F.);
#62035=ORIENTED_EDGE('',*,*,#46970,.F.);
#62036=ORIENTED_EDGE('',*,*,#46974,.T.);
#62037=ORIENTED_EDGE('',*,*,#46975,.T.);
#62038=ORIENTED_EDGE('',*,*,#46976,.F.);
#62039=ORIENTED_EDGE('',*,*,#46977,.F.);
#62040=ORIENTED_EDGE('',*,*,#46978,.T.);
#62041=ORIENTED_EDGE('',*,*,#46979,.T.);
#62042=ORIENTED_EDGE('',*,*,#46980,.F.);
#62043=ORIENTED_EDGE('',*,*,#46975,.F.);
#62044=ORIENTED_EDGE('',*,*,#46981,.T.);
#62045=ORIENTED_EDGE('',*,*,#46982,.T.);
#62046=ORIENTED_EDGE('',*,*,#46983,.F.);
#62047=ORIENTED_EDGE('',*,*,#46979,.F.);
#62048=ORIENTED_EDGE('',*,*,#46984,.T.);
#62049=ORIENTED_EDGE('',*,*,#46977,.T.);
#62050=ORIENTED_EDGE('',*,*,#46985,.F.);
#62051=ORIENTED_EDGE('',*,*,#46982,.F.);
#62052=ORIENTED_EDGE('',*,*,#46986,.T.);
#62053=ORIENTED_EDGE('',*,*,#46987,.T.);
#62054=ORIENTED_EDGE('',*,*,#46988,.F.);
#62055=ORIENTED_EDGE('',*,*,#46989,.F.);
#62056=ORIENTED_EDGE('',*,*,#46990,.T.);
#62057=ORIENTED_EDGE('',*,*,#46991,.T.);
#62058=ORIENTED_EDGE('',*,*,#46992,.F.);
#62059=ORIENTED_EDGE('',*,*,#46987,.F.);
#62060=ORIENTED_EDGE('',*,*,#46993,.T.);
#62061=ORIENTED_EDGE('',*,*,#46994,.T.);
#62062=ORIENTED_EDGE('',*,*,#46995,.F.);
#62063=ORIENTED_EDGE('',*,*,#46991,.F.);
#62064=ORIENTED_EDGE('',*,*,#46996,.T.);
#62065=ORIENTED_EDGE('',*,*,#46989,.T.);
#62066=ORIENTED_EDGE('',*,*,#46997,.F.);
#62067=ORIENTED_EDGE('',*,*,#46994,.F.);
#62068=ORIENTED_EDGE('',*,*,#46998,.T.);
#62069=ORIENTED_EDGE('',*,*,#46999,.T.);
#62070=ORIENTED_EDGE('',*,*,#47000,.F.);
#62071=ORIENTED_EDGE('',*,*,#47001,.F.);
#62072=ORIENTED_EDGE('',*,*,#47002,.T.);
#62073=ORIENTED_EDGE('',*,*,#47003,.T.);
#62074=ORIENTED_EDGE('',*,*,#47004,.F.);
#62075=ORIENTED_EDGE('',*,*,#46999,.F.);
#62076=ORIENTED_EDGE('',*,*,#47005,.T.);
#62077=ORIENTED_EDGE('',*,*,#47006,.T.);
#62078=ORIENTED_EDGE('',*,*,#47007,.F.);
#62079=ORIENTED_EDGE('',*,*,#47003,.F.);
#62080=ORIENTED_EDGE('',*,*,#47008,.T.);
#62081=ORIENTED_EDGE('',*,*,#47001,.T.);
#62082=ORIENTED_EDGE('',*,*,#47009,.F.);
#62083=ORIENTED_EDGE('',*,*,#47006,.F.);
#62084=ORIENTED_EDGE('',*,*,#47010,.T.);
#62085=ORIENTED_EDGE('',*,*,#47011,.T.);
#62086=ORIENTED_EDGE('',*,*,#47012,.F.);
#62087=ORIENTED_EDGE('',*,*,#47013,.F.);
#62088=ORIENTED_EDGE('',*,*,#47014,.T.);
#62089=ORIENTED_EDGE('',*,*,#47015,.T.);
#62090=ORIENTED_EDGE('',*,*,#47016,.F.);
#62091=ORIENTED_EDGE('',*,*,#47011,.F.);
#62092=ORIENTED_EDGE('',*,*,#47017,.T.);
#62093=ORIENTED_EDGE('',*,*,#47018,.T.);
#62094=ORIENTED_EDGE('',*,*,#47019,.F.);
#62095=ORIENTED_EDGE('',*,*,#47015,.F.);
#62096=ORIENTED_EDGE('',*,*,#47020,.T.);
#62097=ORIENTED_EDGE('',*,*,#47013,.T.);
#62098=ORIENTED_EDGE('',*,*,#47021,.F.);
#62099=ORIENTED_EDGE('',*,*,#47018,.F.);
#62100=ORIENTED_EDGE('',*,*,#47022,.T.);
#62101=ORIENTED_EDGE('',*,*,#47023,.T.);
#62102=ORIENTED_EDGE('',*,*,#47024,.F.);
#62103=ORIENTED_EDGE('',*,*,#47025,.F.);
#62104=ORIENTED_EDGE('',*,*,#47026,.T.);
#62105=ORIENTED_EDGE('',*,*,#47027,.T.);
#62106=ORIENTED_EDGE('',*,*,#47028,.F.);
#62107=ORIENTED_EDGE('',*,*,#47023,.F.);
#62108=ORIENTED_EDGE('',*,*,#47029,.T.);
#62109=ORIENTED_EDGE('',*,*,#47030,.T.);
#62110=ORIENTED_EDGE('',*,*,#47031,.F.);
#62111=ORIENTED_EDGE('',*,*,#47027,.F.);
#62112=ORIENTED_EDGE('',*,*,#47032,.T.);
#62113=ORIENTED_EDGE('',*,*,#47025,.T.);
#62114=ORIENTED_EDGE('',*,*,#47033,.F.);
#62115=ORIENTED_EDGE('',*,*,#47030,.F.);
#62116=ORIENTED_EDGE('',*,*,#47034,.T.);
#62117=ORIENTED_EDGE('',*,*,#47035,.T.);
#62118=ORIENTED_EDGE('',*,*,#47036,.F.);
#62119=ORIENTED_EDGE('',*,*,#47037,.F.);
#62120=ORIENTED_EDGE('',*,*,#47038,.T.);
#62121=ORIENTED_EDGE('',*,*,#47039,.T.);
#62122=ORIENTED_EDGE('',*,*,#47040,.F.);
#62123=ORIENTED_EDGE('',*,*,#47035,.F.);
#62124=ORIENTED_EDGE('',*,*,#47041,.T.);
#62125=ORIENTED_EDGE('',*,*,#47042,.T.);
#62126=ORIENTED_EDGE('',*,*,#47043,.F.);
#62127=ORIENTED_EDGE('',*,*,#47039,.F.);
#62128=ORIENTED_EDGE('',*,*,#47044,.T.);
#62129=ORIENTED_EDGE('',*,*,#47037,.T.);
#62130=ORIENTED_EDGE('',*,*,#47045,.F.);
#62131=ORIENTED_EDGE('',*,*,#47042,.F.);
#62132=ORIENTED_EDGE('',*,*,#47046,.T.);
#62133=ORIENTED_EDGE('',*,*,#47047,.T.);
#62134=ORIENTED_EDGE('',*,*,#47048,.F.);
#62135=ORIENTED_EDGE('',*,*,#47049,.F.);
#62136=ORIENTED_EDGE('',*,*,#47050,.T.);
#62137=ORIENTED_EDGE('',*,*,#47051,.T.);
#62138=ORIENTED_EDGE('',*,*,#47052,.F.);
#62139=ORIENTED_EDGE('',*,*,#47047,.F.);
#62140=ORIENTED_EDGE('',*,*,#47053,.T.);
#62141=ORIENTED_EDGE('',*,*,#47054,.T.);
#62142=ORIENTED_EDGE('',*,*,#47055,.F.);
#62143=ORIENTED_EDGE('',*,*,#47051,.F.);
#62144=ORIENTED_EDGE('',*,*,#47056,.T.);
#62145=ORIENTED_EDGE('',*,*,#47049,.T.);
#62146=ORIENTED_EDGE('',*,*,#47057,.F.);
#62147=ORIENTED_EDGE('',*,*,#47054,.F.);
#62148=ORIENTED_EDGE('',*,*,#47058,.T.);
#62149=ORIENTED_EDGE('',*,*,#47059,.T.);
#62150=ORIENTED_EDGE('',*,*,#47060,.F.);
#62151=ORIENTED_EDGE('',*,*,#47061,.F.);
#62152=ORIENTED_EDGE('',*,*,#47062,.T.);
#62153=ORIENTED_EDGE('',*,*,#47063,.T.);
#62154=ORIENTED_EDGE('',*,*,#47064,.F.);
#62155=ORIENTED_EDGE('',*,*,#47059,.F.);
#62156=ORIENTED_EDGE('',*,*,#47065,.T.);
#62157=ORIENTED_EDGE('',*,*,#47066,.T.);
#62158=ORIENTED_EDGE('',*,*,#47067,.F.);
#62159=ORIENTED_EDGE('',*,*,#47063,.F.);
#62160=ORIENTED_EDGE('',*,*,#47068,.T.);
#62161=ORIENTED_EDGE('',*,*,#47061,.T.);
#62162=ORIENTED_EDGE('',*,*,#47069,.F.);
#62163=ORIENTED_EDGE('',*,*,#47066,.F.);
#62164=ORIENTED_EDGE('',*,*,#47070,.T.);
#62165=ORIENTED_EDGE('',*,*,#47071,.T.);
#62166=ORIENTED_EDGE('',*,*,#47072,.F.);
#62167=ORIENTED_EDGE('',*,*,#47073,.F.);
#62168=ORIENTED_EDGE('',*,*,#47074,.T.);
#62169=ORIENTED_EDGE('',*,*,#47075,.T.);
#62170=ORIENTED_EDGE('',*,*,#47076,.F.);
#62171=ORIENTED_EDGE('',*,*,#47071,.F.);
#62172=ORIENTED_EDGE('',*,*,#47077,.T.);
#62173=ORIENTED_EDGE('',*,*,#47078,.T.);
#62174=ORIENTED_EDGE('',*,*,#47079,.F.);
#62175=ORIENTED_EDGE('',*,*,#47075,.F.);
#62176=ORIENTED_EDGE('',*,*,#47080,.T.);
#62177=ORIENTED_EDGE('',*,*,#47073,.T.);
#62178=ORIENTED_EDGE('',*,*,#47081,.F.);
#62179=ORIENTED_EDGE('',*,*,#47078,.F.);
#62180=ORIENTED_EDGE('',*,*,#47082,.T.);
#62181=ORIENTED_EDGE('',*,*,#47083,.T.);
#62182=ORIENTED_EDGE('',*,*,#47084,.F.);
#62183=ORIENTED_EDGE('',*,*,#47085,.F.);
#62184=ORIENTED_EDGE('',*,*,#47086,.T.);
#62185=ORIENTED_EDGE('',*,*,#47087,.T.);
#62186=ORIENTED_EDGE('',*,*,#47088,.F.);
#62187=ORIENTED_EDGE('',*,*,#47083,.F.);
#62188=ORIENTED_EDGE('',*,*,#47089,.T.);
#62189=ORIENTED_EDGE('',*,*,#47090,.T.);
#62190=ORIENTED_EDGE('',*,*,#47091,.F.);
#62191=ORIENTED_EDGE('',*,*,#47087,.F.);
#62192=ORIENTED_EDGE('',*,*,#47092,.T.);
#62193=ORIENTED_EDGE('',*,*,#47085,.T.);
#62194=ORIENTED_EDGE('',*,*,#47093,.F.);
#62195=ORIENTED_EDGE('',*,*,#47090,.F.);
#62196=ORIENTED_EDGE('',*,*,#47094,.T.);
#62197=ORIENTED_EDGE('',*,*,#47095,.T.);
#62198=ORIENTED_EDGE('',*,*,#47096,.F.);
#62199=ORIENTED_EDGE('',*,*,#47097,.F.);
#62200=ORIENTED_EDGE('',*,*,#47098,.T.);
#62201=ORIENTED_EDGE('',*,*,#47099,.T.);
#62202=ORIENTED_EDGE('',*,*,#47100,.F.);
#62203=ORIENTED_EDGE('',*,*,#47095,.F.);
#62204=ORIENTED_EDGE('',*,*,#47101,.T.);
#62205=ORIENTED_EDGE('',*,*,#47102,.T.);
#62206=ORIENTED_EDGE('',*,*,#47103,.F.);
#62207=ORIENTED_EDGE('',*,*,#47099,.F.);
#62208=ORIENTED_EDGE('',*,*,#47104,.T.);
#62209=ORIENTED_EDGE('',*,*,#47097,.T.);
#62210=ORIENTED_EDGE('',*,*,#47105,.F.);
#62211=ORIENTED_EDGE('',*,*,#47102,.F.);
#62212=ORIENTED_EDGE('',*,*,#47106,.T.);
#62213=ORIENTED_EDGE('',*,*,#47107,.T.);
#62214=ORIENTED_EDGE('',*,*,#47108,.F.);
#62215=ORIENTED_EDGE('',*,*,#47109,.F.);
#62216=ORIENTED_EDGE('',*,*,#47110,.T.);
#62217=ORIENTED_EDGE('',*,*,#47111,.T.);
#62218=ORIENTED_EDGE('',*,*,#47112,.F.);
#62219=ORIENTED_EDGE('',*,*,#47107,.F.);
#62220=ORIENTED_EDGE('',*,*,#47113,.T.);
#62221=ORIENTED_EDGE('',*,*,#47114,.T.);
#62222=ORIENTED_EDGE('',*,*,#47115,.F.);
#62223=ORIENTED_EDGE('',*,*,#47111,.F.);
#62224=ORIENTED_EDGE('',*,*,#47116,.T.);
#62225=ORIENTED_EDGE('',*,*,#47109,.T.);
#62226=ORIENTED_EDGE('',*,*,#47117,.F.);
#62227=ORIENTED_EDGE('',*,*,#47114,.F.);
#62228=ORIENTED_EDGE('',*,*,#47118,.T.);
#62229=ORIENTED_EDGE('',*,*,#47119,.T.);
#62230=ORIENTED_EDGE('',*,*,#47120,.F.);
#62231=ORIENTED_EDGE('',*,*,#47121,.F.);
#62232=ORIENTED_EDGE('',*,*,#47122,.T.);
#62233=ORIENTED_EDGE('',*,*,#47123,.T.);
#62234=ORIENTED_EDGE('',*,*,#47124,.F.);
#62235=ORIENTED_EDGE('',*,*,#47119,.F.);
#62236=ORIENTED_EDGE('',*,*,#47125,.T.);
#62237=ORIENTED_EDGE('',*,*,#47126,.T.);
#62238=ORIENTED_EDGE('',*,*,#47127,.F.);
#62239=ORIENTED_EDGE('',*,*,#47123,.F.);
#62240=ORIENTED_EDGE('',*,*,#47128,.T.);
#62241=ORIENTED_EDGE('',*,*,#47121,.T.);
#62242=ORIENTED_EDGE('',*,*,#47129,.F.);
#62243=ORIENTED_EDGE('',*,*,#47126,.F.);
#62244=ORIENTED_EDGE('',*,*,#47130,.T.);
#62245=ORIENTED_EDGE('',*,*,#47131,.T.);
#62246=ORIENTED_EDGE('',*,*,#47132,.F.);
#62247=ORIENTED_EDGE('',*,*,#47133,.F.);
#62248=ORIENTED_EDGE('',*,*,#47134,.T.);
#62249=ORIENTED_EDGE('',*,*,#47135,.T.);
#62250=ORIENTED_EDGE('',*,*,#47136,.F.);
#62251=ORIENTED_EDGE('',*,*,#47131,.F.);
#62252=ORIENTED_EDGE('',*,*,#47137,.T.);
#62253=ORIENTED_EDGE('',*,*,#47138,.T.);
#62254=ORIENTED_EDGE('',*,*,#47139,.F.);
#62255=ORIENTED_EDGE('',*,*,#47135,.F.);
#62256=ORIENTED_EDGE('',*,*,#47140,.T.);
#62257=ORIENTED_EDGE('',*,*,#47133,.T.);
#62258=ORIENTED_EDGE('',*,*,#47141,.F.);
#62259=ORIENTED_EDGE('',*,*,#47138,.F.);
#62260=ORIENTED_EDGE('',*,*,#47142,.T.);
#62261=ORIENTED_EDGE('',*,*,#47143,.T.);
#62262=ORIENTED_EDGE('',*,*,#47144,.F.);
#62263=ORIENTED_EDGE('',*,*,#47145,.F.);
#62264=ORIENTED_EDGE('',*,*,#47146,.T.);
#62265=ORIENTED_EDGE('',*,*,#47147,.T.);
#62266=ORIENTED_EDGE('',*,*,#47148,.F.);
#62267=ORIENTED_EDGE('',*,*,#47143,.F.);
#62268=ORIENTED_EDGE('',*,*,#47149,.T.);
#62269=ORIENTED_EDGE('',*,*,#47150,.T.);
#62270=ORIENTED_EDGE('',*,*,#47151,.F.);
#62271=ORIENTED_EDGE('',*,*,#47147,.F.);
#62272=ORIENTED_EDGE('',*,*,#47152,.T.);
#62273=ORIENTED_EDGE('',*,*,#47145,.T.);
#62274=ORIENTED_EDGE('',*,*,#47153,.F.);
#62275=ORIENTED_EDGE('',*,*,#47150,.F.);
#62276=ORIENTED_EDGE('',*,*,#47154,.T.);
#62277=ORIENTED_EDGE('',*,*,#47155,.T.);
#62278=ORIENTED_EDGE('',*,*,#47156,.F.);
#62279=ORIENTED_EDGE('',*,*,#47157,.F.);
#62280=ORIENTED_EDGE('',*,*,#47158,.T.);
#62281=ORIENTED_EDGE('',*,*,#47159,.T.);
#62282=ORIENTED_EDGE('',*,*,#47160,.F.);
#62283=ORIENTED_EDGE('',*,*,#47155,.F.);
#62284=ORIENTED_EDGE('',*,*,#47161,.T.);
#62285=ORIENTED_EDGE('',*,*,#47162,.T.);
#62286=ORIENTED_EDGE('',*,*,#47163,.F.);
#62287=ORIENTED_EDGE('',*,*,#47159,.F.);
#62288=ORIENTED_EDGE('',*,*,#47164,.T.);
#62289=ORIENTED_EDGE('',*,*,#47157,.T.);
#62290=ORIENTED_EDGE('',*,*,#47165,.F.);
#62291=ORIENTED_EDGE('',*,*,#47162,.F.);
#62292=ORIENTED_EDGE('',*,*,#47166,.T.);
#62293=ORIENTED_EDGE('',*,*,#47167,.T.);
#62294=ORIENTED_EDGE('',*,*,#47168,.F.);
#62295=ORIENTED_EDGE('',*,*,#47169,.F.);
#62296=ORIENTED_EDGE('',*,*,#47170,.T.);
#62297=ORIENTED_EDGE('',*,*,#47171,.T.);
#62298=ORIENTED_EDGE('',*,*,#47172,.F.);
#62299=ORIENTED_EDGE('',*,*,#47167,.F.);
#62300=ORIENTED_EDGE('',*,*,#47173,.T.);
#62301=ORIENTED_EDGE('',*,*,#47174,.T.);
#62302=ORIENTED_EDGE('',*,*,#47175,.F.);
#62303=ORIENTED_EDGE('',*,*,#47171,.F.);
#62304=ORIENTED_EDGE('',*,*,#47176,.T.);
#62305=ORIENTED_EDGE('',*,*,#47169,.T.);
#62306=ORIENTED_EDGE('',*,*,#47177,.F.);
#62307=ORIENTED_EDGE('',*,*,#47174,.F.);
#62308=ORIENTED_EDGE('',*,*,#47178,.T.);
#62309=ORIENTED_EDGE('',*,*,#47179,.T.);
#62310=ORIENTED_EDGE('',*,*,#47180,.F.);
#62311=ORIENTED_EDGE('',*,*,#47181,.F.);
#62312=ORIENTED_EDGE('',*,*,#47182,.T.);
#62313=ORIENTED_EDGE('',*,*,#47183,.T.);
#62314=ORIENTED_EDGE('',*,*,#47184,.F.);
#62315=ORIENTED_EDGE('',*,*,#47179,.F.);
#62316=ORIENTED_EDGE('',*,*,#47185,.T.);
#62317=ORIENTED_EDGE('',*,*,#47186,.T.);
#62318=ORIENTED_EDGE('',*,*,#47187,.F.);
#62319=ORIENTED_EDGE('',*,*,#47183,.F.);
#62320=ORIENTED_EDGE('',*,*,#47188,.T.);
#62321=ORIENTED_EDGE('',*,*,#47181,.T.);
#62322=ORIENTED_EDGE('',*,*,#47189,.F.);
#62323=ORIENTED_EDGE('',*,*,#47186,.F.);
#62324=ORIENTED_EDGE('',*,*,#47190,.T.);
#62325=ORIENTED_EDGE('',*,*,#47191,.T.);
#62326=ORIENTED_EDGE('',*,*,#47192,.F.);
#62327=ORIENTED_EDGE('',*,*,#47193,.F.);
#62328=ORIENTED_EDGE('',*,*,#47194,.T.);
#62329=ORIENTED_EDGE('',*,*,#47195,.T.);
#62330=ORIENTED_EDGE('',*,*,#47196,.F.);
#62331=ORIENTED_EDGE('',*,*,#47191,.F.);
#62332=ORIENTED_EDGE('',*,*,#47197,.T.);
#62333=ORIENTED_EDGE('',*,*,#47198,.T.);
#62334=ORIENTED_EDGE('',*,*,#47199,.F.);
#62335=ORIENTED_EDGE('',*,*,#47195,.F.);
#62336=ORIENTED_EDGE('',*,*,#47200,.T.);
#62337=ORIENTED_EDGE('',*,*,#47193,.T.);
#62338=ORIENTED_EDGE('',*,*,#47201,.F.);
#62339=ORIENTED_EDGE('',*,*,#47198,.F.);
#62340=ORIENTED_EDGE('',*,*,#47202,.T.);
#62341=ORIENTED_EDGE('',*,*,#47203,.T.);
#62342=ORIENTED_EDGE('',*,*,#47204,.F.);
#62343=ORIENTED_EDGE('',*,*,#47205,.F.);
#62344=ORIENTED_EDGE('',*,*,#47206,.T.);
#62345=ORIENTED_EDGE('',*,*,#47207,.T.);
#62346=ORIENTED_EDGE('',*,*,#47208,.F.);
#62347=ORIENTED_EDGE('',*,*,#47203,.F.);
#62348=ORIENTED_EDGE('',*,*,#47209,.T.);
#62349=ORIENTED_EDGE('',*,*,#47210,.T.);
#62350=ORIENTED_EDGE('',*,*,#47211,.F.);
#62351=ORIENTED_EDGE('',*,*,#47207,.F.);
#62352=ORIENTED_EDGE('',*,*,#47212,.T.);
#62353=ORIENTED_EDGE('',*,*,#47205,.T.);
#62354=ORIENTED_EDGE('',*,*,#47213,.F.);
#62355=ORIENTED_EDGE('',*,*,#47210,.F.);
#62356=ORIENTED_EDGE('',*,*,#47214,.T.);
#62357=ORIENTED_EDGE('',*,*,#47215,.T.);
#62358=ORIENTED_EDGE('',*,*,#47216,.F.);
#62359=ORIENTED_EDGE('',*,*,#47217,.F.);
#62360=ORIENTED_EDGE('',*,*,#47218,.T.);
#62361=ORIENTED_EDGE('',*,*,#47219,.T.);
#62362=ORIENTED_EDGE('',*,*,#47220,.F.);
#62363=ORIENTED_EDGE('',*,*,#47215,.F.);
#62364=ORIENTED_EDGE('',*,*,#47221,.T.);
#62365=ORIENTED_EDGE('',*,*,#47222,.T.);
#62366=ORIENTED_EDGE('',*,*,#47223,.F.);
#62367=ORIENTED_EDGE('',*,*,#47219,.F.);
#62368=ORIENTED_EDGE('',*,*,#47224,.T.);
#62369=ORIENTED_EDGE('',*,*,#47217,.T.);
#62370=ORIENTED_EDGE('',*,*,#47225,.F.);
#62371=ORIENTED_EDGE('',*,*,#47222,.F.);
#62372=ORIENTED_EDGE('',*,*,#47226,.T.);
#62373=ORIENTED_EDGE('',*,*,#47227,.T.);
#62374=ORIENTED_EDGE('',*,*,#47228,.F.);
#62375=ORIENTED_EDGE('',*,*,#47229,.F.);
#62376=ORIENTED_EDGE('',*,*,#47230,.T.);
#62377=ORIENTED_EDGE('',*,*,#47231,.T.);
#62378=ORIENTED_EDGE('',*,*,#47232,.F.);
#62379=ORIENTED_EDGE('',*,*,#47227,.F.);
#62380=ORIENTED_EDGE('',*,*,#47233,.T.);
#62381=ORIENTED_EDGE('',*,*,#47234,.T.);
#62382=ORIENTED_EDGE('',*,*,#47235,.F.);
#62383=ORIENTED_EDGE('',*,*,#47231,.F.);
#62384=ORIENTED_EDGE('',*,*,#47236,.T.);
#62385=ORIENTED_EDGE('',*,*,#47229,.T.);
#62386=ORIENTED_EDGE('',*,*,#47237,.F.);
#62387=ORIENTED_EDGE('',*,*,#47234,.F.);
#62388=ORIENTED_EDGE('',*,*,#47238,.T.);
#62389=ORIENTED_EDGE('',*,*,#47239,.T.);
#62390=ORIENTED_EDGE('',*,*,#47240,.F.);
#62391=ORIENTED_EDGE('',*,*,#47241,.F.);
#62392=ORIENTED_EDGE('',*,*,#47242,.T.);
#62393=ORIENTED_EDGE('',*,*,#47243,.T.);
#62394=ORIENTED_EDGE('',*,*,#47244,.F.);
#62395=ORIENTED_EDGE('',*,*,#47239,.F.);
#62396=ORIENTED_EDGE('',*,*,#47245,.T.);
#62397=ORIENTED_EDGE('',*,*,#47246,.T.);
#62398=ORIENTED_EDGE('',*,*,#47247,.F.);
#62399=ORIENTED_EDGE('',*,*,#47243,.F.);
#62400=ORIENTED_EDGE('',*,*,#47248,.T.);
#62401=ORIENTED_EDGE('',*,*,#47241,.T.);
#62402=ORIENTED_EDGE('',*,*,#47249,.F.);
#62403=ORIENTED_EDGE('',*,*,#47246,.F.);
#62404=ORIENTED_EDGE('',*,*,#47250,.T.);
#62405=ORIENTED_EDGE('',*,*,#47251,.T.);
#62406=ORIENTED_EDGE('',*,*,#47252,.F.);
#62407=ORIENTED_EDGE('',*,*,#47253,.F.);
#62408=ORIENTED_EDGE('',*,*,#47254,.T.);
#62409=ORIENTED_EDGE('',*,*,#47255,.T.);
#62410=ORIENTED_EDGE('',*,*,#47256,.F.);
#62411=ORIENTED_EDGE('',*,*,#47251,.F.);
#62412=ORIENTED_EDGE('',*,*,#47257,.T.);
#62413=ORIENTED_EDGE('',*,*,#47258,.T.);
#62414=ORIENTED_EDGE('',*,*,#47259,.F.);
#62415=ORIENTED_EDGE('',*,*,#47255,.F.);
#62416=ORIENTED_EDGE('',*,*,#47260,.T.);
#62417=ORIENTED_EDGE('',*,*,#47253,.T.);
#62418=ORIENTED_EDGE('',*,*,#47261,.F.);
#62419=ORIENTED_EDGE('',*,*,#47258,.F.);
#62420=ORIENTED_EDGE('',*,*,#47262,.T.);
#62421=ORIENTED_EDGE('',*,*,#47263,.T.);
#62422=ORIENTED_EDGE('',*,*,#47264,.F.);
#62423=ORIENTED_EDGE('',*,*,#47265,.F.);
#62424=ORIENTED_EDGE('',*,*,#47266,.T.);
#62425=ORIENTED_EDGE('',*,*,#47267,.T.);
#62426=ORIENTED_EDGE('',*,*,#47268,.F.);
#62427=ORIENTED_EDGE('',*,*,#47263,.F.);
#62428=ORIENTED_EDGE('',*,*,#47269,.T.);
#62429=ORIENTED_EDGE('',*,*,#47270,.T.);
#62430=ORIENTED_EDGE('',*,*,#47271,.F.);
#62431=ORIENTED_EDGE('',*,*,#47267,.F.);
#62432=ORIENTED_EDGE('',*,*,#47272,.T.);
#62433=ORIENTED_EDGE('',*,*,#47265,.T.);
#62434=ORIENTED_EDGE('',*,*,#47273,.F.);
#62435=ORIENTED_EDGE('',*,*,#47270,.F.);
#62436=ORIENTED_EDGE('',*,*,#47274,.T.);
#62437=ORIENTED_EDGE('',*,*,#47275,.T.);
#62438=ORIENTED_EDGE('',*,*,#47276,.F.);
#62439=ORIENTED_EDGE('',*,*,#47277,.F.);
#62440=ORIENTED_EDGE('',*,*,#47278,.T.);
#62441=ORIENTED_EDGE('',*,*,#47279,.T.);
#62442=ORIENTED_EDGE('',*,*,#47280,.F.);
#62443=ORIENTED_EDGE('',*,*,#47275,.F.);
#62444=ORIENTED_EDGE('',*,*,#47281,.T.);
#62445=ORIENTED_EDGE('',*,*,#47282,.T.);
#62446=ORIENTED_EDGE('',*,*,#47283,.F.);
#62447=ORIENTED_EDGE('',*,*,#47279,.F.);
#62448=ORIENTED_EDGE('',*,*,#47284,.T.);
#62449=ORIENTED_EDGE('',*,*,#47277,.T.);
#62450=ORIENTED_EDGE('',*,*,#47285,.F.);
#62451=ORIENTED_EDGE('',*,*,#47282,.F.);
#62452=ORIENTED_EDGE('',*,*,#47286,.T.);
#62453=ORIENTED_EDGE('',*,*,#47287,.T.);
#62454=ORIENTED_EDGE('',*,*,#47288,.F.);
#62455=ORIENTED_EDGE('',*,*,#47289,.F.);
#62456=ORIENTED_EDGE('',*,*,#47290,.T.);
#62457=ORIENTED_EDGE('',*,*,#47291,.T.);
#62458=ORIENTED_EDGE('',*,*,#47292,.F.);
#62459=ORIENTED_EDGE('',*,*,#47287,.F.);
#62460=ORIENTED_EDGE('',*,*,#47293,.T.);
#62461=ORIENTED_EDGE('',*,*,#47294,.T.);
#62462=ORIENTED_EDGE('',*,*,#47295,.F.);
#62463=ORIENTED_EDGE('',*,*,#47291,.F.);
#62464=ORIENTED_EDGE('',*,*,#47296,.T.);
#62465=ORIENTED_EDGE('',*,*,#47289,.T.);
#62466=ORIENTED_EDGE('',*,*,#47297,.F.);
#62467=ORIENTED_EDGE('',*,*,#47294,.F.);
#62468=ORIENTED_EDGE('',*,*,#47298,.T.);
#62469=ORIENTED_EDGE('',*,*,#47299,.T.);
#62470=ORIENTED_EDGE('',*,*,#47300,.F.);
#62471=ORIENTED_EDGE('',*,*,#47301,.F.);
#62472=ORIENTED_EDGE('',*,*,#47302,.T.);
#62473=ORIENTED_EDGE('',*,*,#47303,.T.);
#62474=ORIENTED_EDGE('',*,*,#47304,.F.);
#62475=ORIENTED_EDGE('',*,*,#47299,.F.);
#62476=ORIENTED_EDGE('',*,*,#47305,.T.);
#62477=ORIENTED_EDGE('',*,*,#47306,.T.);
#62478=ORIENTED_EDGE('',*,*,#47307,.F.);
#62479=ORIENTED_EDGE('',*,*,#47303,.F.);
#62480=ORIENTED_EDGE('',*,*,#47308,.T.);
#62481=ORIENTED_EDGE('',*,*,#47301,.T.);
#62482=ORIENTED_EDGE('',*,*,#47309,.F.);
#62483=ORIENTED_EDGE('',*,*,#47306,.F.);
#62484=ORIENTED_EDGE('',*,*,#47310,.T.);
#62485=ORIENTED_EDGE('',*,*,#47311,.T.);
#62486=ORIENTED_EDGE('',*,*,#47312,.F.);
#62487=ORIENTED_EDGE('',*,*,#47313,.F.);
#62488=ORIENTED_EDGE('',*,*,#47314,.T.);
#62489=ORIENTED_EDGE('',*,*,#47315,.T.);
#62490=ORIENTED_EDGE('',*,*,#47316,.F.);
#62491=ORIENTED_EDGE('',*,*,#47311,.F.);
#62492=ORIENTED_EDGE('',*,*,#47317,.T.);
#62493=ORIENTED_EDGE('',*,*,#47318,.T.);
#62494=ORIENTED_EDGE('',*,*,#47319,.F.);
#62495=ORIENTED_EDGE('',*,*,#47315,.F.);
#62496=ORIENTED_EDGE('',*,*,#47320,.T.);
#62497=ORIENTED_EDGE('',*,*,#47313,.T.);
#62498=ORIENTED_EDGE('',*,*,#47321,.F.);
#62499=ORIENTED_EDGE('',*,*,#47318,.F.);
#62500=ORIENTED_EDGE('',*,*,#47322,.T.);
#62501=ORIENTED_EDGE('',*,*,#47323,.T.);
#62502=ORIENTED_EDGE('',*,*,#47324,.F.);
#62503=ORIENTED_EDGE('',*,*,#47325,.F.);
#62504=ORIENTED_EDGE('',*,*,#47326,.T.);
#62505=ORIENTED_EDGE('',*,*,#47327,.T.);
#62506=ORIENTED_EDGE('',*,*,#47328,.F.);
#62507=ORIENTED_EDGE('',*,*,#47323,.F.);
#62508=ORIENTED_EDGE('',*,*,#47329,.T.);
#62509=ORIENTED_EDGE('',*,*,#47330,.T.);
#62510=ORIENTED_EDGE('',*,*,#47331,.F.);
#62511=ORIENTED_EDGE('',*,*,#47327,.F.);
#62512=ORIENTED_EDGE('',*,*,#47332,.T.);
#62513=ORIENTED_EDGE('',*,*,#47325,.T.);
#62514=ORIENTED_EDGE('',*,*,#47333,.F.);
#62515=ORIENTED_EDGE('',*,*,#47330,.F.);
#62516=ORIENTED_EDGE('',*,*,#47334,.T.);
#62517=ORIENTED_EDGE('',*,*,#47335,.T.);
#62518=ORIENTED_EDGE('',*,*,#47336,.F.);
#62519=ORIENTED_EDGE('',*,*,#47337,.F.);
#62520=ORIENTED_EDGE('',*,*,#47338,.T.);
#62521=ORIENTED_EDGE('',*,*,#47339,.T.);
#62522=ORIENTED_EDGE('',*,*,#47340,.F.);
#62523=ORIENTED_EDGE('',*,*,#47335,.F.);
#62524=ORIENTED_EDGE('',*,*,#47341,.T.);
#62525=ORIENTED_EDGE('',*,*,#47342,.T.);
#62526=ORIENTED_EDGE('',*,*,#47343,.F.);
#62527=ORIENTED_EDGE('',*,*,#47339,.F.);
#62528=ORIENTED_EDGE('',*,*,#47344,.T.);
#62529=ORIENTED_EDGE('',*,*,#47337,.T.);
#62530=ORIENTED_EDGE('',*,*,#47345,.F.);
#62531=ORIENTED_EDGE('',*,*,#47342,.F.);
#62532=ORIENTED_EDGE('',*,*,#47346,.T.);
#62533=ORIENTED_EDGE('',*,*,#47347,.T.);
#62534=ORIENTED_EDGE('',*,*,#47348,.F.);
#62535=ORIENTED_EDGE('',*,*,#47349,.F.);
#62536=ORIENTED_EDGE('',*,*,#47350,.T.);
#62537=ORIENTED_EDGE('',*,*,#47351,.T.);
#62538=ORIENTED_EDGE('',*,*,#47352,.F.);
#62539=ORIENTED_EDGE('',*,*,#47347,.F.);
#62540=ORIENTED_EDGE('',*,*,#47353,.T.);
#62541=ORIENTED_EDGE('',*,*,#47354,.T.);
#62542=ORIENTED_EDGE('',*,*,#47355,.F.);
#62543=ORIENTED_EDGE('',*,*,#47351,.F.);
#62544=ORIENTED_EDGE('',*,*,#47356,.T.);
#62545=ORIENTED_EDGE('',*,*,#47349,.T.);
#62546=ORIENTED_EDGE('',*,*,#47357,.F.);
#62547=ORIENTED_EDGE('',*,*,#47354,.F.);
#62548=ORIENTED_EDGE('',*,*,#47358,.T.);
#62549=ORIENTED_EDGE('',*,*,#47359,.T.);
#62550=ORIENTED_EDGE('',*,*,#47360,.F.);
#62551=ORIENTED_EDGE('',*,*,#47361,.F.);
#62552=ORIENTED_EDGE('',*,*,#47362,.T.);
#62553=ORIENTED_EDGE('',*,*,#47363,.T.);
#62554=ORIENTED_EDGE('',*,*,#47364,.F.);
#62555=ORIENTED_EDGE('',*,*,#47359,.F.);
#62556=ORIENTED_EDGE('',*,*,#47365,.T.);
#62557=ORIENTED_EDGE('',*,*,#47366,.T.);
#62558=ORIENTED_EDGE('',*,*,#47367,.F.);
#62559=ORIENTED_EDGE('',*,*,#47363,.F.);
#62560=ORIENTED_EDGE('',*,*,#47368,.T.);
#62561=ORIENTED_EDGE('',*,*,#47361,.T.);
#62562=ORIENTED_EDGE('',*,*,#47369,.F.);
#62563=ORIENTED_EDGE('',*,*,#47366,.F.);
#62564=ORIENTED_EDGE('',*,*,#47370,.T.);
#62565=ORIENTED_EDGE('',*,*,#47371,.T.);
#62566=ORIENTED_EDGE('',*,*,#47372,.F.);
#62567=ORIENTED_EDGE('',*,*,#47373,.F.);
#62568=ORIENTED_EDGE('',*,*,#47374,.T.);
#62569=ORIENTED_EDGE('',*,*,#47375,.T.);
#62570=ORIENTED_EDGE('',*,*,#47376,.F.);
#62571=ORIENTED_EDGE('',*,*,#47371,.F.);
#62572=ORIENTED_EDGE('',*,*,#47377,.T.);
#62573=ORIENTED_EDGE('',*,*,#47378,.T.);
#62574=ORIENTED_EDGE('',*,*,#47379,.F.);
#62575=ORIENTED_EDGE('',*,*,#47375,.F.);
#62576=ORIENTED_EDGE('',*,*,#47380,.T.);
#62577=ORIENTED_EDGE('',*,*,#47373,.T.);
#62578=ORIENTED_EDGE('',*,*,#47381,.F.);
#62579=ORIENTED_EDGE('',*,*,#47378,.F.);
#62580=ORIENTED_EDGE('',*,*,#47382,.T.);
#62581=ORIENTED_EDGE('',*,*,#47383,.T.);
#62582=ORIENTED_EDGE('',*,*,#47384,.F.);
#62583=ORIENTED_EDGE('',*,*,#47385,.F.);
#62584=ORIENTED_EDGE('',*,*,#47386,.T.);
#62585=ORIENTED_EDGE('',*,*,#47387,.T.);
#62586=ORIENTED_EDGE('',*,*,#47388,.F.);
#62587=ORIENTED_EDGE('',*,*,#47383,.F.);
#62588=ORIENTED_EDGE('',*,*,#47389,.T.);
#62589=ORIENTED_EDGE('',*,*,#47390,.T.);
#62590=ORIENTED_EDGE('',*,*,#47391,.F.);
#62591=ORIENTED_EDGE('',*,*,#47387,.F.);
#62592=ORIENTED_EDGE('',*,*,#47392,.T.);
#62593=ORIENTED_EDGE('',*,*,#47385,.T.);
#62594=ORIENTED_EDGE('',*,*,#47393,.F.);
#62595=ORIENTED_EDGE('',*,*,#47390,.F.);
#62596=ORIENTED_EDGE('',*,*,#47394,.T.);
#62597=ORIENTED_EDGE('',*,*,#47395,.T.);
#62598=ORIENTED_EDGE('',*,*,#47396,.F.);
#62599=ORIENTED_EDGE('',*,*,#47397,.F.);
#62600=ORIENTED_EDGE('',*,*,#47398,.T.);
#62601=ORIENTED_EDGE('',*,*,#47399,.T.);
#62602=ORIENTED_EDGE('',*,*,#47400,.F.);
#62603=ORIENTED_EDGE('',*,*,#47395,.F.);
#62604=ORIENTED_EDGE('',*,*,#47401,.T.);
#62605=ORIENTED_EDGE('',*,*,#47402,.T.);
#62606=ORIENTED_EDGE('',*,*,#47403,.F.);
#62607=ORIENTED_EDGE('',*,*,#47399,.F.);
#62608=ORIENTED_EDGE('',*,*,#47404,.T.);
#62609=ORIENTED_EDGE('',*,*,#47397,.T.);
#62610=ORIENTED_EDGE('',*,*,#47405,.F.);
#62611=ORIENTED_EDGE('',*,*,#47402,.F.);
#62612=ORIENTED_EDGE('',*,*,#47406,.T.);
#62613=ORIENTED_EDGE('',*,*,#47407,.T.);
#62614=ORIENTED_EDGE('',*,*,#47408,.F.);
#62615=ORIENTED_EDGE('',*,*,#47409,.F.);
#62616=ORIENTED_EDGE('',*,*,#47410,.T.);
#62617=ORIENTED_EDGE('',*,*,#47411,.T.);
#62618=ORIENTED_EDGE('',*,*,#47412,.F.);
#62619=ORIENTED_EDGE('',*,*,#47407,.F.);
#62620=ORIENTED_EDGE('',*,*,#47413,.T.);
#62621=ORIENTED_EDGE('',*,*,#47414,.T.);
#62622=ORIENTED_EDGE('',*,*,#47415,.F.);
#62623=ORIENTED_EDGE('',*,*,#47411,.F.);
#62624=ORIENTED_EDGE('',*,*,#47416,.T.);
#62625=ORIENTED_EDGE('',*,*,#47409,.T.);
#62626=ORIENTED_EDGE('',*,*,#47417,.F.);
#62627=ORIENTED_EDGE('',*,*,#47414,.F.);
#62628=ORIENTED_EDGE('',*,*,#47418,.T.);
#62629=ORIENTED_EDGE('',*,*,#47419,.T.);
#62630=ORIENTED_EDGE('',*,*,#47420,.F.);
#62631=ORIENTED_EDGE('',*,*,#47421,.F.);
#62632=ORIENTED_EDGE('',*,*,#47422,.T.);
#62633=ORIENTED_EDGE('',*,*,#47423,.T.);
#62634=ORIENTED_EDGE('',*,*,#47424,.F.);
#62635=ORIENTED_EDGE('',*,*,#47419,.F.);
#62636=ORIENTED_EDGE('',*,*,#47425,.T.);
#62637=ORIENTED_EDGE('',*,*,#47426,.T.);
#62638=ORIENTED_EDGE('',*,*,#47427,.F.);
#62639=ORIENTED_EDGE('',*,*,#47423,.F.);
#62640=ORIENTED_EDGE('',*,*,#47428,.T.);
#62641=ORIENTED_EDGE('',*,*,#47421,.T.);
#62642=ORIENTED_EDGE('',*,*,#47429,.F.);
#62643=ORIENTED_EDGE('',*,*,#47426,.F.);
#62644=ORIENTED_EDGE('',*,*,#47430,.T.);
#62645=ORIENTED_EDGE('',*,*,#47431,.T.);
#62646=ORIENTED_EDGE('',*,*,#47432,.F.);
#62647=ORIENTED_EDGE('',*,*,#47433,.F.);
#62648=ORIENTED_EDGE('',*,*,#47434,.T.);
#62649=ORIENTED_EDGE('',*,*,#47435,.T.);
#62650=ORIENTED_EDGE('',*,*,#47436,.F.);
#62651=ORIENTED_EDGE('',*,*,#47431,.F.);
#62652=ORIENTED_EDGE('',*,*,#47437,.T.);
#62653=ORIENTED_EDGE('',*,*,#47438,.T.);
#62654=ORIENTED_EDGE('',*,*,#47439,.F.);
#62655=ORIENTED_EDGE('',*,*,#47435,.F.);
#62656=ORIENTED_EDGE('',*,*,#47440,.T.);
#62657=ORIENTED_EDGE('',*,*,#47433,.T.);
#62658=ORIENTED_EDGE('',*,*,#47441,.F.);
#62659=ORIENTED_EDGE('',*,*,#47438,.F.);
#62660=ORIENTED_EDGE('',*,*,#47442,.T.);
#62661=ORIENTED_EDGE('',*,*,#47443,.T.);
#62662=ORIENTED_EDGE('',*,*,#47444,.F.);
#62663=ORIENTED_EDGE('',*,*,#47445,.F.);
#62664=ORIENTED_EDGE('',*,*,#47446,.T.);
#62665=ORIENTED_EDGE('',*,*,#47447,.T.);
#62666=ORIENTED_EDGE('',*,*,#47448,.F.);
#62667=ORIENTED_EDGE('',*,*,#47443,.F.);
#62668=ORIENTED_EDGE('',*,*,#47449,.T.);
#62669=ORIENTED_EDGE('',*,*,#47450,.T.);
#62670=ORIENTED_EDGE('',*,*,#47451,.F.);
#62671=ORIENTED_EDGE('',*,*,#47447,.F.);
#62672=ORIENTED_EDGE('',*,*,#47452,.T.);
#62673=ORIENTED_EDGE('',*,*,#47445,.T.);
#62674=ORIENTED_EDGE('',*,*,#47453,.F.);
#62675=ORIENTED_EDGE('',*,*,#47450,.F.);
#62676=ORIENTED_EDGE('',*,*,#47454,.T.);
#62677=ORIENTED_EDGE('',*,*,#47455,.T.);
#62678=ORIENTED_EDGE('',*,*,#47456,.F.);
#62679=ORIENTED_EDGE('',*,*,#47457,.F.);
#62680=ORIENTED_EDGE('',*,*,#47458,.T.);
#62681=ORIENTED_EDGE('',*,*,#47459,.T.);
#62682=ORIENTED_EDGE('',*,*,#47460,.F.);
#62683=ORIENTED_EDGE('',*,*,#47455,.F.);
#62684=ORIENTED_EDGE('',*,*,#47461,.T.);
#62685=ORIENTED_EDGE('',*,*,#47462,.T.);
#62686=ORIENTED_EDGE('',*,*,#47463,.F.);
#62687=ORIENTED_EDGE('',*,*,#47459,.F.);
#62688=ORIENTED_EDGE('',*,*,#47464,.T.);
#62689=ORIENTED_EDGE('',*,*,#47457,.T.);
#62690=ORIENTED_EDGE('',*,*,#47465,.F.);
#62691=ORIENTED_EDGE('',*,*,#47462,.F.);
#62692=ORIENTED_EDGE('',*,*,#47466,.T.);
#62693=ORIENTED_EDGE('',*,*,#47467,.T.);
#62694=ORIENTED_EDGE('',*,*,#47468,.F.);
#62695=ORIENTED_EDGE('',*,*,#47469,.F.);
#62696=ORIENTED_EDGE('',*,*,#47470,.T.);
#62697=ORIENTED_EDGE('',*,*,#47471,.T.);
#62698=ORIENTED_EDGE('',*,*,#47472,.F.);
#62699=ORIENTED_EDGE('',*,*,#47467,.F.);
#62700=ORIENTED_EDGE('',*,*,#47473,.T.);
#62701=ORIENTED_EDGE('',*,*,#47474,.T.);
#62702=ORIENTED_EDGE('',*,*,#47475,.F.);
#62703=ORIENTED_EDGE('',*,*,#47471,.F.);
#62704=ORIENTED_EDGE('',*,*,#47476,.T.);
#62705=ORIENTED_EDGE('',*,*,#47469,.T.);
#62706=ORIENTED_EDGE('',*,*,#47477,.F.);
#62707=ORIENTED_EDGE('',*,*,#47474,.F.);
#62708=ORIENTED_EDGE('',*,*,#47478,.T.);
#62709=ORIENTED_EDGE('',*,*,#47479,.T.);
#62710=ORIENTED_EDGE('',*,*,#47480,.F.);
#62711=ORIENTED_EDGE('',*,*,#47481,.F.);
#62712=ORIENTED_EDGE('',*,*,#47482,.T.);
#62713=ORIENTED_EDGE('',*,*,#47483,.T.);
#62714=ORIENTED_EDGE('',*,*,#47484,.F.);
#62715=ORIENTED_EDGE('',*,*,#47479,.F.);
#62716=ORIENTED_EDGE('',*,*,#47485,.T.);
#62717=ORIENTED_EDGE('',*,*,#47486,.T.);
#62718=ORIENTED_EDGE('',*,*,#47487,.F.);
#62719=ORIENTED_EDGE('',*,*,#47483,.F.);
#62720=ORIENTED_EDGE('',*,*,#47488,.T.);
#62721=ORIENTED_EDGE('',*,*,#47481,.T.);
#62722=ORIENTED_EDGE('',*,*,#47489,.F.);
#62723=ORIENTED_EDGE('',*,*,#47486,.F.);
#62724=ORIENTED_EDGE('',*,*,#47490,.T.);
#62725=ORIENTED_EDGE('',*,*,#47491,.T.);
#62726=ORIENTED_EDGE('',*,*,#47492,.F.);
#62727=ORIENTED_EDGE('',*,*,#47493,.F.);
#62728=ORIENTED_EDGE('',*,*,#47494,.T.);
#62729=ORIENTED_EDGE('',*,*,#47495,.T.);
#62730=ORIENTED_EDGE('',*,*,#47496,.F.);
#62731=ORIENTED_EDGE('',*,*,#47491,.F.);
#62732=ORIENTED_EDGE('',*,*,#47497,.T.);
#62733=ORIENTED_EDGE('',*,*,#47498,.T.);
#62734=ORIENTED_EDGE('',*,*,#47499,.F.);
#62735=ORIENTED_EDGE('',*,*,#47495,.F.);
#62736=ORIENTED_EDGE('',*,*,#47500,.T.);
#62737=ORIENTED_EDGE('',*,*,#47493,.T.);
#62738=ORIENTED_EDGE('',*,*,#47501,.F.);
#62739=ORIENTED_EDGE('',*,*,#47498,.F.);
#62740=ORIENTED_EDGE('',*,*,#47502,.T.);
#62741=ORIENTED_EDGE('',*,*,#47503,.T.);
#62742=ORIENTED_EDGE('',*,*,#47504,.F.);
#62743=ORIENTED_EDGE('',*,*,#47505,.F.);
#62744=ORIENTED_EDGE('',*,*,#47506,.T.);
#62745=ORIENTED_EDGE('',*,*,#47507,.T.);
#62746=ORIENTED_EDGE('',*,*,#47508,.F.);
#62747=ORIENTED_EDGE('',*,*,#47503,.F.);
#62748=ORIENTED_EDGE('',*,*,#47509,.T.);
#62749=ORIENTED_EDGE('',*,*,#47510,.T.);
#62750=ORIENTED_EDGE('',*,*,#47511,.F.);
#62751=ORIENTED_EDGE('',*,*,#47507,.F.);
#62752=ORIENTED_EDGE('',*,*,#47512,.T.);
#62753=ORIENTED_EDGE('',*,*,#47505,.T.);
#62754=ORIENTED_EDGE('',*,*,#47513,.F.);
#62755=ORIENTED_EDGE('',*,*,#47510,.F.);
#62756=ORIENTED_EDGE('',*,*,#47514,.T.);
#62757=ORIENTED_EDGE('',*,*,#47515,.T.);
#62758=ORIENTED_EDGE('',*,*,#47516,.F.);
#62759=ORIENTED_EDGE('',*,*,#47517,.F.);
#62760=ORIENTED_EDGE('',*,*,#47518,.T.);
#62761=ORIENTED_EDGE('',*,*,#47519,.T.);
#62762=ORIENTED_EDGE('',*,*,#47520,.F.);
#62763=ORIENTED_EDGE('',*,*,#47515,.F.);
#62764=ORIENTED_EDGE('',*,*,#47521,.T.);
#62765=ORIENTED_EDGE('',*,*,#47522,.T.);
#62766=ORIENTED_EDGE('',*,*,#47523,.F.);
#62767=ORIENTED_EDGE('',*,*,#47519,.F.);
#62768=ORIENTED_EDGE('',*,*,#47524,.T.);
#62769=ORIENTED_EDGE('',*,*,#47517,.T.);
#62770=ORIENTED_EDGE('',*,*,#47525,.F.);
#62771=ORIENTED_EDGE('',*,*,#47522,.F.);
#62772=ORIENTED_EDGE('',*,*,#47526,.T.);
#62773=ORIENTED_EDGE('',*,*,#47527,.T.);
#62774=ORIENTED_EDGE('',*,*,#47528,.F.);
#62775=ORIENTED_EDGE('',*,*,#47529,.F.);
#62776=ORIENTED_EDGE('',*,*,#47530,.T.);
#62777=ORIENTED_EDGE('',*,*,#47531,.T.);
#62778=ORIENTED_EDGE('',*,*,#47532,.F.);
#62779=ORIENTED_EDGE('',*,*,#47527,.F.);
#62780=ORIENTED_EDGE('',*,*,#47533,.T.);
#62781=ORIENTED_EDGE('',*,*,#47534,.T.);
#62782=ORIENTED_EDGE('',*,*,#47535,.F.);
#62783=ORIENTED_EDGE('',*,*,#47531,.F.);
#62784=ORIENTED_EDGE('',*,*,#47536,.T.);
#62785=ORIENTED_EDGE('',*,*,#47529,.T.);
#62786=ORIENTED_EDGE('',*,*,#47537,.F.);
#62787=ORIENTED_EDGE('',*,*,#47534,.F.);
#62788=ORIENTED_EDGE('',*,*,#47538,.T.);
#62789=ORIENTED_EDGE('',*,*,#47539,.T.);
#62790=ORIENTED_EDGE('',*,*,#47540,.F.);
#62791=ORIENTED_EDGE('',*,*,#47541,.F.);
#62792=ORIENTED_EDGE('',*,*,#47542,.T.);
#62793=ORIENTED_EDGE('',*,*,#47543,.T.);
#62794=ORIENTED_EDGE('',*,*,#47544,.F.);
#62795=ORIENTED_EDGE('',*,*,#47539,.F.);
#62796=ORIENTED_EDGE('',*,*,#47545,.T.);
#62797=ORIENTED_EDGE('',*,*,#47546,.T.);
#62798=ORIENTED_EDGE('',*,*,#47547,.F.);
#62799=ORIENTED_EDGE('',*,*,#47543,.F.);
#62800=ORIENTED_EDGE('',*,*,#47548,.T.);
#62801=ORIENTED_EDGE('',*,*,#47541,.T.);
#62802=ORIENTED_EDGE('',*,*,#47549,.F.);
#62803=ORIENTED_EDGE('',*,*,#47546,.F.);
#62804=ORIENTED_EDGE('',*,*,#47550,.T.);
#62805=ORIENTED_EDGE('',*,*,#47551,.T.);
#62806=ORIENTED_EDGE('',*,*,#47552,.F.);
#62807=ORIENTED_EDGE('',*,*,#47553,.F.);
#62808=ORIENTED_EDGE('',*,*,#47554,.T.);
#62809=ORIENTED_EDGE('',*,*,#47555,.T.);
#62810=ORIENTED_EDGE('',*,*,#47556,.F.);
#62811=ORIENTED_EDGE('',*,*,#47551,.F.);
#62812=ORIENTED_EDGE('',*,*,#47557,.T.);
#62813=ORIENTED_EDGE('',*,*,#47558,.T.);
#62814=ORIENTED_EDGE('',*,*,#47559,.F.);
#62815=ORIENTED_EDGE('',*,*,#47555,.F.);
#62816=ORIENTED_EDGE('',*,*,#47560,.T.);
#62817=ORIENTED_EDGE('',*,*,#47553,.T.);
#62818=ORIENTED_EDGE('',*,*,#47561,.F.);
#62819=ORIENTED_EDGE('',*,*,#47558,.F.);
#62820=ORIENTED_EDGE('',*,*,#47562,.T.);
#62821=ORIENTED_EDGE('',*,*,#47563,.T.);
#62822=ORIENTED_EDGE('',*,*,#47564,.F.);
#62823=ORIENTED_EDGE('',*,*,#47565,.F.);
#62824=ORIENTED_EDGE('',*,*,#47566,.T.);
#62825=ORIENTED_EDGE('',*,*,#47567,.T.);
#62826=ORIENTED_EDGE('',*,*,#47568,.F.);
#62827=ORIENTED_EDGE('',*,*,#47563,.F.);
#62828=ORIENTED_EDGE('',*,*,#47569,.T.);
#62829=ORIENTED_EDGE('',*,*,#47570,.T.);
#62830=ORIENTED_EDGE('',*,*,#47571,.F.);
#62831=ORIENTED_EDGE('',*,*,#47567,.F.);
#62832=ORIENTED_EDGE('',*,*,#47572,.T.);
#62833=ORIENTED_EDGE('',*,*,#47565,.T.);
#62834=ORIENTED_EDGE('',*,*,#47573,.F.);
#62835=ORIENTED_EDGE('',*,*,#47570,.F.);
#62836=ORIENTED_EDGE('',*,*,#47574,.T.);
#62837=ORIENTED_EDGE('',*,*,#47575,.T.);
#62838=ORIENTED_EDGE('',*,*,#47576,.F.);
#62839=ORIENTED_EDGE('',*,*,#47577,.F.);
#62840=ORIENTED_EDGE('',*,*,#47578,.T.);
#62841=ORIENTED_EDGE('',*,*,#47579,.T.);
#62842=ORIENTED_EDGE('',*,*,#47580,.F.);
#62843=ORIENTED_EDGE('',*,*,#47575,.F.);
#62844=ORIENTED_EDGE('',*,*,#47581,.T.);
#62845=ORIENTED_EDGE('',*,*,#47582,.T.);
#62846=ORIENTED_EDGE('',*,*,#47583,.F.);
#62847=ORIENTED_EDGE('',*,*,#47579,.F.);
#62848=ORIENTED_EDGE('',*,*,#47584,.T.);
#62849=ORIENTED_EDGE('',*,*,#47577,.T.);
#62850=ORIENTED_EDGE('',*,*,#47585,.F.);
#62851=ORIENTED_EDGE('',*,*,#47582,.F.);
#62852=ORIENTED_EDGE('',*,*,#47586,.T.);
#62853=ORIENTED_EDGE('',*,*,#47587,.T.);
#62854=ORIENTED_EDGE('',*,*,#47588,.F.);
#62855=ORIENTED_EDGE('',*,*,#47589,.F.);
#62856=ORIENTED_EDGE('',*,*,#47590,.T.);
#62857=ORIENTED_EDGE('',*,*,#47591,.T.);
#62858=ORIENTED_EDGE('',*,*,#47592,.F.);
#62859=ORIENTED_EDGE('',*,*,#47587,.F.);
#62860=ORIENTED_EDGE('',*,*,#47593,.T.);
#62861=ORIENTED_EDGE('',*,*,#47594,.T.);
#62862=ORIENTED_EDGE('',*,*,#47595,.F.);
#62863=ORIENTED_EDGE('',*,*,#47591,.F.);
#62864=ORIENTED_EDGE('',*,*,#47596,.T.);
#62865=ORIENTED_EDGE('',*,*,#47589,.T.);
#62866=ORIENTED_EDGE('',*,*,#47597,.F.);
#62867=ORIENTED_EDGE('',*,*,#47594,.F.);
#62868=ORIENTED_EDGE('',*,*,#47598,.T.);
#62869=ORIENTED_EDGE('',*,*,#47599,.T.);
#62870=ORIENTED_EDGE('',*,*,#47600,.F.);
#62871=ORIENTED_EDGE('',*,*,#47601,.F.);
#62872=ORIENTED_EDGE('',*,*,#47602,.T.);
#62873=ORIENTED_EDGE('',*,*,#47603,.T.);
#62874=ORIENTED_EDGE('',*,*,#47604,.F.);
#62875=ORIENTED_EDGE('',*,*,#47599,.F.);
#62876=ORIENTED_EDGE('',*,*,#47605,.T.);
#62877=ORIENTED_EDGE('',*,*,#47606,.T.);
#62878=ORIENTED_EDGE('',*,*,#47607,.F.);
#62879=ORIENTED_EDGE('',*,*,#47603,.F.);
#62880=ORIENTED_EDGE('',*,*,#47608,.T.);
#62881=ORIENTED_EDGE('',*,*,#47601,.T.);
#62882=ORIENTED_EDGE('',*,*,#47609,.F.);
#62883=ORIENTED_EDGE('',*,*,#47606,.F.);
#62884=ORIENTED_EDGE('',*,*,#47610,.T.);
#62885=ORIENTED_EDGE('',*,*,#47611,.T.);
#62886=ORIENTED_EDGE('',*,*,#47612,.F.);
#62887=ORIENTED_EDGE('',*,*,#47613,.F.);
#62888=ORIENTED_EDGE('',*,*,#47614,.T.);
#62889=ORIENTED_EDGE('',*,*,#47615,.T.);
#62890=ORIENTED_EDGE('',*,*,#47616,.F.);
#62891=ORIENTED_EDGE('',*,*,#47611,.F.);
#62892=ORIENTED_EDGE('',*,*,#47617,.T.);
#62893=ORIENTED_EDGE('',*,*,#47618,.T.);
#62894=ORIENTED_EDGE('',*,*,#47619,.F.);
#62895=ORIENTED_EDGE('',*,*,#47615,.F.);
#62896=ORIENTED_EDGE('',*,*,#47620,.T.);
#62897=ORIENTED_EDGE('',*,*,#47613,.T.);
#62898=ORIENTED_EDGE('',*,*,#47621,.F.);
#62899=ORIENTED_EDGE('',*,*,#47618,.F.);
#62900=ORIENTED_EDGE('',*,*,#47622,.T.);
#62901=ORIENTED_EDGE('',*,*,#47623,.T.);
#62902=ORIENTED_EDGE('',*,*,#47624,.F.);
#62903=ORIENTED_EDGE('',*,*,#47625,.F.);
#62904=ORIENTED_EDGE('',*,*,#47626,.T.);
#62905=ORIENTED_EDGE('',*,*,#47627,.T.);
#62906=ORIENTED_EDGE('',*,*,#47628,.F.);
#62907=ORIENTED_EDGE('',*,*,#47623,.F.);
#62908=ORIENTED_EDGE('',*,*,#47629,.T.);
#62909=ORIENTED_EDGE('',*,*,#47630,.T.);
#62910=ORIENTED_EDGE('',*,*,#47631,.F.);
#62911=ORIENTED_EDGE('',*,*,#47627,.F.);
#62912=ORIENTED_EDGE('',*,*,#47632,.T.);
#62913=ORIENTED_EDGE('',*,*,#47625,.T.);
#62914=ORIENTED_EDGE('',*,*,#47633,.F.);
#62915=ORIENTED_EDGE('',*,*,#47630,.F.);
#62916=ORIENTED_EDGE('',*,*,#47634,.T.);
#62917=ORIENTED_EDGE('',*,*,#47635,.T.);
#62918=ORIENTED_EDGE('',*,*,#47636,.F.);
#62919=ORIENTED_EDGE('',*,*,#47637,.F.);
#62920=ORIENTED_EDGE('',*,*,#47638,.T.);
#62921=ORIENTED_EDGE('',*,*,#47639,.T.);
#62922=ORIENTED_EDGE('',*,*,#47640,.F.);
#62923=ORIENTED_EDGE('',*,*,#47635,.F.);
#62924=ORIENTED_EDGE('',*,*,#47641,.T.);
#62925=ORIENTED_EDGE('',*,*,#47642,.T.);
#62926=ORIENTED_EDGE('',*,*,#47643,.F.);
#62927=ORIENTED_EDGE('',*,*,#47639,.F.);
#62928=ORIENTED_EDGE('',*,*,#47644,.T.);
#62929=ORIENTED_EDGE('',*,*,#47637,.T.);
#62930=ORIENTED_EDGE('',*,*,#47645,.F.);
#62931=ORIENTED_EDGE('',*,*,#47642,.F.);
#62932=ORIENTED_EDGE('',*,*,#47646,.T.);
#62933=ORIENTED_EDGE('',*,*,#47647,.T.);
#62934=ORIENTED_EDGE('',*,*,#47648,.F.);
#62935=ORIENTED_EDGE('',*,*,#47649,.F.);
#62936=ORIENTED_EDGE('',*,*,#47650,.T.);
#62937=ORIENTED_EDGE('',*,*,#47651,.T.);
#62938=ORIENTED_EDGE('',*,*,#47652,.F.);
#62939=ORIENTED_EDGE('',*,*,#47647,.F.);
#62940=ORIENTED_EDGE('',*,*,#47653,.T.);
#62941=ORIENTED_EDGE('',*,*,#47654,.T.);
#62942=ORIENTED_EDGE('',*,*,#47655,.F.);
#62943=ORIENTED_EDGE('',*,*,#47651,.F.);
#62944=ORIENTED_EDGE('',*,*,#47656,.T.);
#62945=ORIENTED_EDGE('',*,*,#47649,.T.);
#62946=ORIENTED_EDGE('',*,*,#47657,.F.);
#62947=ORIENTED_EDGE('',*,*,#47654,.F.);
#62948=ORIENTED_EDGE('',*,*,#47658,.T.);
#62949=ORIENTED_EDGE('',*,*,#47659,.T.);
#62950=ORIENTED_EDGE('',*,*,#47660,.F.);
#62951=ORIENTED_EDGE('',*,*,#47661,.F.);
#62952=ORIENTED_EDGE('',*,*,#47662,.T.);
#62953=ORIENTED_EDGE('',*,*,#47663,.T.);
#62954=ORIENTED_EDGE('',*,*,#47664,.F.);
#62955=ORIENTED_EDGE('',*,*,#47659,.F.);
#62956=ORIENTED_EDGE('',*,*,#47665,.T.);
#62957=ORIENTED_EDGE('',*,*,#47666,.T.);
#62958=ORIENTED_EDGE('',*,*,#47667,.F.);
#62959=ORIENTED_EDGE('',*,*,#47663,.F.);
#62960=ORIENTED_EDGE('',*,*,#47668,.T.);
#62961=ORIENTED_EDGE('',*,*,#47661,.T.);
#62962=ORIENTED_EDGE('',*,*,#47669,.F.);
#62963=ORIENTED_EDGE('',*,*,#47666,.F.);
#62964=ORIENTED_EDGE('',*,*,#47670,.T.);
#62965=ORIENTED_EDGE('',*,*,#47671,.T.);
#62966=ORIENTED_EDGE('',*,*,#47672,.F.);
#62967=ORIENTED_EDGE('',*,*,#47673,.F.);
#62968=ORIENTED_EDGE('',*,*,#47674,.T.);
#62969=ORIENTED_EDGE('',*,*,#47675,.T.);
#62970=ORIENTED_EDGE('',*,*,#47676,.F.);
#62971=ORIENTED_EDGE('',*,*,#47671,.F.);
#62972=ORIENTED_EDGE('',*,*,#47677,.T.);
#62973=ORIENTED_EDGE('',*,*,#47678,.T.);
#62974=ORIENTED_EDGE('',*,*,#47679,.F.);
#62975=ORIENTED_EDGE('',*,*,#47675,.F.);
#62976=ORIENTED_EDGE('',*,*,#47680,.T.);
#62977=ORIENTED_EDGE('',*,*,#47673,.T.);
#62978=ORIENTED_EDGE('',*,*,#47681,.F.);
#62979=ORIENTED_EDGE('',*,*,#47678,.F.);
#62980=ORIENTED_EDGE('',*,*,#47682,.T.);
#62981=ORIENTED_EDGE('',*,*,#47683,.T.);
#62982=ORIENTED_EDGE('',*,*,#47684,.F.);
#62983=ORIENTED_EDGE('',*,*,#47685,.F.);
#62984=ORIENTED_EDGE('',*,*,#47686,.T.);
#62985=ORIENTED_EDGE('',*,*,#47687,.T.);
#62986=ORIENTED_EDGE('',*,*,#47688,.F.);
#62987=ORIENTED_EDGE('',*,*,#47683,.F.);
#62988=ORIENTED_EDGE('',*,*,#47689,.T.);
#62989=ORIENTED_EDGE('',*,*,#47690,.T.);
#62990=ORIENTED_EDGE('',*,*,#47691,.F.);
#62991=ORIENTED_EDGE('',*,*,#47687,.F.);
#62992=ORIENTED_EDGE('',*,*,#47692,.T.);
#62993=ORIENTED_EDGE('',*,*,#47685,.T.);
#62994=ORIENTED_EDGE('',*,*,#47693,.F.);
#62995=ORIENTED_EDGE('',*,*,#47690,.F.);
#62996=ORIENTED_EDGE('',*,*,#47694,.T.);
#62997=ORIENTED_EDGE('',*,*,#47695,.T.);
#62998=ORIENTED_EDGE('',*,*,#47696,.F.);
#62999=ORIENTED_EDGE('',*,*,#47697,.F.);
#63000=ORIENTED_EDGE('',*,*,#47698,.T.);
#63001=ORIENTED_EDGE('',*,*,#47699,.T.);
#63002=ORIENTED_EDGE('',*,*,#47700,.F.);
#63003=ORIENTED_EDGE('',*,*,#47695,.F.);
#63004=ORIENTED_EDGE('',*,*,#47701,.T.);
#63005=ORIENTED_EDGE('',*,*,#47702,.T.);
#63006=ORIENTED_EDGE('',*,*,#47703,.F.);
#63007=ORIENTED_EDGE('',*,*,#47699,.F.);
#63008=ORIENTED_EDGE('',*,*,#47704,.T.);
#63009=ORIENTED_EDGE('',*,*,#47697,.T.);
#63010=ORIENTED_EDGE('',*,*,#47705,.F.);
#63011=ORIENTED_EDGE('',*,*,#47702,.F.);
#63012=ORIENTED_EDGE('',*,*,#47706,.T.);
#63013=ORIENTED_EDGE('',*,*,#47707,.T.);
#63014=ORIENTED_EDGE('',*,*,#47708,.F.);
#63015=ORIENTED_EDGE('',*,*,#47709,.F.);
#63016=ORIENTED_EDGE('',*,*,#47710,.T.);
#63017=ORIENTED_EDGE('',*,*,#47711,.T.);
#63018=ORIENTED_EDGE('',*,*,#47712,.F.);
#63019=ORIENTED_EDGE('',*,*,#47707,.F.);
#63020=ORIENTED_EDGE('',*,*,#47713,.T.);
#63021=ORIENTED_EDGE('',*,*,#47714,.T.);
#63022=ORIENTED_EDGE('',*,*,#47715,.F.);
#63023=ORIENTED_EDGE('',*,*,#47711,.F.);
#63024=ORIENTED_EDGE('',*,*,#47716,.T.);
#63025=ORIENTED_EDGE('',*,*,#47709,.T.);
#63026=ORIENTED_EDGE('',*,*,#47717,.F.);
#63027=ORIENTED_EDGE('',*,*,#47714,.F.);
#63028=ORIENTED_EDGE('',*,*,#47718,.T.);
#63029=ORIENTED_EDGE('',*,*,#47719,.T.);
#63030=ORIENTED_EDGE('',*,*,#47720,.F.);
#63031=ORIENTED_EDGE('',*,*,#47721,.F.);
#63032=ORIENTED_EDGE('',*,*,#47722,.T.);
#63033=ORIENTED_EDGE('',*,*,#47723,.T.);
#63034=ORIENTED_EDGE('',*,*,#47724,.F.);
#63035=ORIENTED_EDGE('',*,*,#47719,.F.);
#63036=ORIENTED_EDGE('',*,*,#47725,.T.);
#63037=ORIENTED_EDGE('',*,*,#47726,.T.);
#63038=ORIENTED_EDGE('',*,*,#47727,.F.);
#63039=ORIENTED_EDGE('',*,*,#47723,.F.);
#63040=ORIENTED_EDGE('',*,*,#47728,.T.);
#63041=ORIENTED_EDGE('',*,*,#47721,.T.);
#63042=ORIENTED_EDGE('',*,*,#47729,.F.);
#63043=ORIENTED_EDGE('',*,*,#47726,.F.);
#63044=ORIENTED_EDGE('',*,*,#47730,.T.);
#63045=ORIENTED_EDGE('',*,*,#47731,.T.);
#63046=ORIENTED_EDGE('',*,*,#47732,.F.);
#63047=ORIENTED_EDGE('',*,*,#47733,.F.);
#63048=ORIENTED_EDGE('',*,*,#47734,.T.);
#63049=ORIENTED_EDGE('',*,*,#47735,.T.);
#63050=ORIENTED_EDGE('',*,*,#47736,.F.);
#63051=ORIENTED_EDGE('',*,*,#47731,.F.);
#63052=ORIENTED_EDGE('',*,*,#47737,.T.);
#63053=ORIENTED_EDGE('',*,*,#47738,.T.);
#63054=ORIENTED_EDGE('',*,*,#47739,.F.);
#63055=ORIENTED_EDGE('',*,*,#47735,.F.);
#63056=ORIENTED_EDGE('',*,*,#47740,.T.);
#63057=ORIENTED_EDGE('',*,*,#47733,.T.);
#63058=ORIENTED_EDGE('',*,*,#47741,.F.);
#63059=ORIENTED_EDGE('',*,*,#47738,.F.);
#63060=ORIENTED_EDGE('',*,*,#47742,.T.);
#63061=ORIENTED_EDGE('',*,*,#47743,.T.);
#63062=ORIENTED_EDGE('',*,*,#47744,.F.);
#63063=ORIENTED_EDGE('',*,*,#47745,.F.);
#63064=ORIENTED_EDGE('',*,*,#47746,.T.);
#63065=ORIENTED_EDGE('',*,*,#47747,.T.);
#63066=ORIENTED_EDGE('',*,*,#47748,.F.);
#63067=ORIENTED_EDGE('',*,*,#47743,.F.);
#63068=ORIENTED_EDGE('',*,*,#47749,.T.);
#63069=ORIENTED_EDGE('',*,*,#47750,.T.);
#63070=ORIENTED_EDGE('',*,*,#47751,.F.);
#63071=ORIENTED_EDGE('',*,*,#47747,.F.);
#63072=ORIENTED_EDGE('',*,*,#47752,.T.);
#63073=ORIENTED_EDGE('',*,*,#47745,.T.);
#63074=ORIENTED_EDGE('',*,*,#47753,.F.);
#63075=ORIENTED_EDGE('',*,*,#47750,.F.);
#63076=ORIENTED_EDGE('',*,*,#47754,.T.);
#63077=ORIENTED_EDGE('',*,*,#47755,.T.);
#63078=ORIENTED_EDGE('',*,*,#47756,.F.);
#63079=ORIENTED_EDGE('',*,*,#47757,.F.);
#63080=ORIENTED_EDGE('',*,*,#47758,.T.);
#63081=ORIENTED_EDGE('',*,*,#47759,.T.);
#63082=ORIENTED_EDGE('',*,*,#47760,.F.);
#63083=ORIENTED_EDGE('',*,*,#47755,.F.);
#63084=ORIENTED_EDGE('',*,*,#47761,.T.);
#63085=ORIENTED_EDGE('',*,*,#47762,.T.);
#63086=ORIENTED_EDGE('',*,*,#47763,.F.);
#63087=ORIENTED_EDGE('',*,*,#47759,.F.);
#63088=ORIENTED_EDGE('',*,*,#47764,.T.);
#63089=ORIENTED_EDGE('',*,*,#47757,.T.);
#63090=ORIENTED_EDGE('',*,*,#47765,.F.);
#63091=ORIENTED_EDGE('',*,*,#47762,.F.);
#63092=ORIENTED_EDGE('',*,*,#47766,.T.);
#63093=ORIENTED_EDGE('',*,*,#47767,.T.);
#63094=ORIENTED_EDGE('',*,*,#47768,.F.);
#63095=ORIENTED_EDGE('',*,*,#47769,.F.);
#63096=ORIENTED_EDGE('',*,*,#47770,.T.);
#63097=ORIENTED_EDGE('',*,*,#47771,.T.);
#63098=ORIENTED_EDGE('',*,*,#47772,.F.);
#63099=ORIENTED_EDGE('',*,*,#47767,.F.);
#63100=ORIENTED_EDGE('',*,*,#47773,.T.);
#63101=ORIENTED_EDGE('',*,*,#47774,.T.);
#63102=ORIENTED_EDGE('',*,*,#47775,.F.);
#63103=ORIENTED_EDGE('',*,*,#47771,.F.);
#63104=ORIENTED_EDGE('',*,*,#47776,.T.);
#63105=ORIENTED_EDGE('',*,*,#47769,.T.);
#63106=ORIENTED_EDGE('',*,*,#47777,.F.);
#63107=ORIENTED_EDGE('',*,*,#47774,.F.);
#63108=ORIENTED_EDGE('',*,*,#47778,.T.);
#63109=ORIENTED_EDGE('',*,*,#47779,.T.);
#63110=ORIENTED_EDGE('',*,*,#47780,.F.);
#63111=ORIENTED_EDGE('',*,*,#47781,.F.);
#63112=ORIENTED_EDGE('',*,*,#47782,.T.);
#63113=ORIENTED_EDGE('',*,*,#47783,.T.);
#63114=ORIENTED_EDGE('',*,*,#47784,.F.);
#63115=ORIENTED_EDGE('',*,*,#47779,.F.);
#63116=ORIENTED_EDGE('',*,*,#47785,.T.);
#63117=ORIENTED_EDGE('',*,*,#47786,.T.);
#63118=ORIENTED_EDGE('',*,*,#47787,.F.);
#63119=ORIENTED_EDGE('',*,*,#47783,.F.);
#63120=ORIENTED_EDGE('',*,*,#47788,.T.);
#63121=ORIENTED_EDGE('',*,*,#47781,.T.);
#63122=ORIENTED_EDGE('',*,*,#47789,.F.);
#63123=ORIENTED_EDGE('',*,*,#47786,.F.);
#63124=ORIENTED_EDGE('',*,*,#47790,.T.);
#63125=ORIENTED_EDGE('',*,*,#47791,.T.);
#63126=ORIENTED_EDGE('',*,*,#47792,.F.);
#63127=ORIENTED_EDGE('',*,*,#47793,.F.);
#63128=ORIENTED_EDGE('',*,*,#47794,.T.);
#63129=ORIENTED_EDGE('',*,*,#47795,.T.);
#63130=ORIENTED_EDGE('',*,*,#47796,.F.);
#63131=ORIENTED_EDGE('',*,*,#47791,.F.);
#63132=ORIENTED_EDGE('',*,*,#47797,.T.);
#63133=ORIENTED_EDGE('',*,*,#47798,.T.);
#63134=ORIENTED_EDGE('',*,*,#47799,.F.);
#63135=ORIENTED_EDGE('',*,*,#47795,.F.);
#63136=ORIENTED_EDGE('',*,*,#47800,.T.);
#63137=ORIENTED_EDGE('',*,*,#47793,.T.);
#63138=ORIENTED_EDGE('',*,*,#47801,.F.);
#63139=ORIENTED_EDGE('',*,*,#47798,.F.);
#63140=ORIENTED_EDGE('',*,*,#47802,.T.);
#63141=ORIENTED_EDGE('',*,*,#47803,.T.);
#63142=ORIENTED_EDGE('',*,*,#47804,.F.);
#63143=ORIENTED_EDGE('',*,*,#47805,.F.);
#63144=ORIENTED_EDGE('',*,*,#47806,.T.);
#63145=ORIENTED_EDGE('',*,*,#47807,.T.);
#63146=ORIENTED_EDGE('',*,*,#47808,.F.);
#63147=ORIENTED_EDGE('',*,*,#47803,.F.);
#63148=ORIENTED_EDGE('',*,*,#47809,.T.);
#63149=ORIENTED_EDGE('',*,*,#47810,.T.);
#63150=ORIENTED_EDGE('',*,*,#47811,.F.);
#63151=ORIENTED_EDGE('',*,*,#47807,.F.);
#63152=ORIENTED_EDGE('',*,*,#47812,.T.);
#63153=ORIENTED_EDGE('',*,*,#47805,.T.);
#63154=ORIENTED_EDGE('',*,*,#47813,.F.);
#63155=ORIENTED_EDGE('',*,*,#47810,.F.);
#63156=ORIENTED_EDGE('',*,*,#47814,.T.);
#63157=ORIENTED_EDGE('',*,*,#47815,.T.);
#63158=ORIENTED_EDGE('',*,*,#47816,.F.);
#63159=ORIENTED_EDGE('',*,*,#47817,.F.);
#63160=ORIENTED_EDGE('',*,*,#47818,.T.);
#63161=ORIENTED_EDGE('',*,*,#47819,.T.);
#63162=ORIENTED_EDGE('',*,*,#47820,.F.);
#63163=ORIENTED_EDGE('',*,*,#47815,.F.);
#63164=ORIENTED_EDGE('',*,*,#47821,.T.);
#63165=ORIENTED_EDGE('',*,*,#47822,.T.);
#63166=ORIENTED_EDGE('',*,*,#47823,.F.);
#63167=ORIENTED_EDGE('',*,*,#47819,.F.);
#63168=ORIENTED_EDGE('',*,*,#47824,.T.);
#63169=ORIENTED_EDGE('',*,*,#47817,.T.);
#63170=ORIENTED_EDGE('',*,*,#47825,.F.);
#63171=ORIENTED_EDGE('',*,*,#47822,.F.);
#63172=ORIENTED_EDGE('',*,*,#47826,.T.);
#63173=ORIENTED_EDGE('',*,*,#47827,.T.);
#63174=ORIENTED_EDGE('',*,*,#47828,.F.);
#63175=ORIENTED_EDGE('',*,*,#47829,.F.);
#63176=ORIENTED_EDGE('',*,*,#47830,.T.);
#63177=ORIENTED_EDGE('',*,*,#47831,.T.);
#63178=ORIENTED_EDGE('',*,*,#47832,.F.);
#63179=ORIENTED_EDGE('',*,*,#47827,.F.);
#63180=ORIENTED_EDGE('',*,*,#47833,.T.);
#63181=ORIENTED_EDGE('',*,*,#47834,.T.);
#63182=ORIENTED_EDGE('',*,*,#47835,.F.);
#63183=ORIENTED_EDGE('',*,*,#47831,.F.);
#63184=ORIENTED_EDGE('',*,*,#47836,.T.);
#63185=ORIENTED_EDGE('',*,*,#47829,.T.);
#63186=ORIENTED_EDGE('',*,*,#47837,.F.);
#63187=ORIENTED_EDGE('',*,*,#47834,.F.);
#63188=ORIENTED_EDGE('',*,*,#47838,.T.);
#63189=ORIENTED_EDGE('',*,*,#47839,.T.);
#63190=ORIENTED_EDGE('',*,*,#47840,.F.);
#63191=ORIENTED_EDGE('',*,*,#47841,.F.);
#63192=ORIENTED_EDGE('',*,*,#47842,.T.);
#63193=ORIENTED_EDGE('',*,*,#47843,.T.);
#63194=ORIENTED_EDGE('',*,*,#47844,.F.);
#63195=ORIENTED_EDGE('',*,*,#47839,.F.);
#63196=ORIENTED_EDGE('',*,*,#47845,.T.);
#63197=ORIENTED_EDGE('',*,*,#47846,.T.);
#63198=ORIENTED_EDGE('',*,*,#47847,.F.);
#63199=ORIENTED_EDGE('',*,*,#47843,.F.);
#63200=ORIENTED_EDGE('',*,*,#47848,.T.);
#63201=ORIENTED_EDGE('',*,*,#47841,.T.);
#63202=ORIENTED_EDGE('',*,*,#47849,.F.);
#63203=ORIENTED_EDGE('',*,*,#47846,.F.);
#63204=ORIENTED_EDGE('',*,*,#47850,.T.);
#63205=ORIENTED_EDGE('',*,*,#47851,.T.);
#63206=ORIENTED_EDGE('',*,*,#47852,.F.);
#63207=ORIENTED_EDGE('',*,*,#47853,.F.);
#63208=ORIENTED_EDGE('',*,*,#47854,.T.);
#63209=ORIENTED_EDGE('',*,*,#47855,.T.);
#63210=ORIENTED_EDGE('',*,*,#47856,.F.);
#63211=ORIENTED_EDGE('',*,*,#47851,.F.);
#63212=ORIENTED_EDGE('',*,*,#47857,.T.);
#63213=ORIENTED_EDGE('',*,*,#47858,.T.);
#63214=ORIENTED_EDGE('',*,*,#47859,.F.);
#63215=ORIENTED_EDGE('',*,*,#47855,.F.);
#63216=ORIENTED_EDGE('',*,*,#47860,.T.);
#63217=ORIENTED_EDGE('',*,*,#47853,.T.);
#63218=ORIENTED_EDGE('',*,*,#47861,.F.);
#63219=ORIENTED_EDGE('',*,*,#47858,.F.);
#63220=ORIENTED_EDGE('',*,*,#47862,.T.);
#63221=ORIENTED_EDGE('',*,*,#47863,.T.);
#63222=ORIENTED_EDGE('',*,*,#47864,.F.);
#63223=ORIENTED_EDGE('',*,*,#47865,.F.);
#63224=ORIENTED_EDGE('',*,*,#47866,.T.);
#63225=ORIENTED_EDGE('',*,*,#47867,.T.);
#63226=ORIENTED_EDGE('',*,*,#47868,.F.);
#63227=ORIENTED_EDGE('',*,*,#47863,.F.);
#63228=ORIENTED_EDGE('',*,*,#47869,.T.);
#63229=ORIENTED_EDGE('',*,*,#47870,.T.);
#63230=ORIENTED_EDGE('',*,*,#47871,.F.);
#63231=ORIENTED_EDGE('',*,*,#47867,.F.);
#63232=ORIENTED_EDGE('',*,*,#47872,.T.);
#63233=ORIENTED_EDGE('',*,*,#47865,.T.);
#63234=ORIENTED_EDGE('',*,*,#47873,.F.);
#63235=ORIENTED_EDGE('',*,*,#47870,.F.);
#63236=ORIENTED_EDGE('',*,*,#47874,.T.);
#63237=ORIENTED_EDGE('',*,*,#47875,.T.);
#63238=ORIENTED_EDGE('',*,*,#47876,.F.);
#63239=ORIENTED_EDGE('',*,*,#47877,.F.);
#63240=ORIENTED_EDGE('',*,*,#47878,.T.);
#63241=ORIENTED_EDGE('',*,*,#47879,.T.);
#63242=ORIENTED_EDGE('',*,*,#47880,.F.);
#63243=ORIENTED_EDGE('',*,*,#47875,.F.);
#63244=ORIENTED_EDGE('',*,*,#47881,.T.);
#63245=ORIENTED_EDGE('',*,*,#47882,.T.);
#63246=ORIENTED_EDGE('',*,*,#47883,.F.);
#63247=ORIENTED_EDGE('',*,*,#47879,.F.);
#63248=ORIENTED_EDGE('',*,*,#47884,.T.);
#63249=ORIENTED_EDGE('',*,*,#47877,.T.);
#63250=ORIENTED_EDGE('',*,*,#47885,.F.);
#63251=ORIENTED_EDGE('',*,*,#47882,.F.);
#63252=ORIENTED_EDGE('',*,*,#47886,.T.);
#63253=ORIENTED_EDGE('',*,*,#47887,.T.);
#63254=ORIENTED_EDGE('',*,*,#47888,.F.);
#63255=ORIENTED_EDGE('',*,*,#47889,.F.);
#63256=ORIENTED_EDGE('',*,*,#47890,.T.);
#63257=ORIENTED_EDGE('',*,*,#47891,.T.);
#63258=ORIENTED_EDGE('',*,*,#47892,.F.);
#63259=ORIENTED_EDGE('',*,*,#47887,.F.);
#63260=ORIENTED_EDGE('',*,*,#47893,.T.);
#63261=ORIENTED_EDGE('',*,*,#47894,.T.);
#63262=ORIENTED_EDGE('',*,*,#47895,.F.);
#63263=ORIENTED_EDGE('',*,*,#47891,.F.);
#63264=ORIENTED_EDGE('',*,*,#47896,.T.);
#63265=ORIENTED_EDGE('',*,*,#47889,.T.);
#63266=ORIENTED_EDGE('',*,*,#47897,.F.);
#63267=ORIENTED_EDGE('',*,*,#47894,.F.);
#63268=ORIENTED_EDGE('',*,*,#47898,.T.);
#63269=ORIENTED_EDGE('',*,*,#47899,.T.);
#63270=ORIENTED_EDGE('',*,*,#47900,.F.);
#63271=ORIENTED_EDGE('',*,*,#47901,.F.);
#63272=ORIENTED_EDGE('',*,*,#47902,.T.);
#63273=ORIENTED_EDGE('',*,*,#47903,.T.);
#63274=ORIENTED_EDGE('',*,*,#47904,.F.);
#63275=ORIENTED_EDGE('',*,*,#47899,.F.);
#63276=ORIENTED_EDGE('',*,*,#47905,.T.);
#63277=ORIENTED_EDGE('',*,*,#47906,.T.);
#63278=ORIENTED_EDGE('',*,*,#47907,.F.);
#63279=ORIENTED_EDGE('',*,*,#47903,.F.);
#63280=ORIENTED_EDGE('',*,*,#47908,.T.);
#63281=ORIENTED_EDGE('',*,*,#47901,.T.);
#63282=ORIENTED_EDGE('',*,*,#47909,.F.);
#63283=ORIENTED_EDGE('',*,*,#47906,.F.);
#63284=ORIENTED_EDGE('',*,*,#47910,.T.);
#63285=ORIENTED_EDGE('',*,*,#47911,.T.);
#63286=ORIENTED_EDGE('',*,*,#47912,.F.);
#63287=ORIENTED_EDGE('',*,*,#47913,.F.);
#63288=ORIENTED_EDGE('',*,*,#47914,.T.);
#63289=ORIENTED_EDGE('',*,*,#47915,.T.);
#63290=ORIENTED_EDGE('',*,*,#47916,.F.);
#63291=ORIENTED_EDGE('',*,*,#47911,.F.);
#63292=ORIENTED_EDGE('',*,*,#47917,.T.);
#63293=ORIENTED_EDGE('',*,*,#47918,.T.);
#63294=ORIENTED_EDGE('',*,*,#47919,.F.);
#63295=ORIENTED_EDGE('',*,*,#47915,.F.);
#63296=ORIENTED_EDGE('',*,*,#47920,.T.);
#63297=ORIENTED_EDGE('',*,*,#47913,.T.);
#63298=ORIENTED_EDGE('',*,*,#47921,.F.);
#63299=ORIENTED_EDGE('',*,*,#47918,.F.);
#63300=ORIENTED_EDGE('',*,*,#47922,.T.);
#63301=ORIENTED_EDGE('',*,*,#47923,.T.);
#63302=ORIENTED_EDGE('',*,*,#47924,.F.);
#63303=ORIENTED_EDGE('',*,*,#47925,.F.);
#63304=ORIENTED_EDGE('',*,*,#47926,.T.);
#63305=ORIENTED_EDGE('',*,*,#47927,.T.);
#63306=ORIENTED_EDGE('',*,*,#47928,.F.);
#63307=ORIENTED_EDGE('',*,*,#47923,.F.);
#63308=ORIENTED_EDGE('',*,*,#47929,.T.);
#63309=ORIENTED_EDGE('',*,*,#47930,.T.);
#63310=ORIENTED_EDGE('',*,*,#47931,.F.);
#63311=ORIENTED_EDGE('',*,*,#47927,.F.);
#63312=ORIENTED_EDGE('',*,*,#47932,.T.);
#63313=ORIENTED_EDGE('',*,*,#47925,.T.);
#63314=ORIENTED_EDGE('',*,*,#47933,.F.);
#63315=ORIENTED_EDGE('',*,*,#47930,.F.);
#63316=ORIENTED_EDGE('',*,*,#47934,.T.);
#63317=ORIENTED_EDGE('',*,*,#47935,.T.);
#63318=ORIENTED_EDGE('',*,*,#47936,.F.);
#63319=ORIENTED_EDGE('',*,*,#47937,.F.);
#63320=ORIENTED_EDGE('',*,*,#47938,.T.);
#63321=ORIENTED_EDGE('',*,*,#47939,.T.);
#63322=ORIENTED_EDGE('',*,*,#47940,.F.);
#63323=ORIENTED_EDGE('',*,*,#47935,.F.);
#63324=ORIENTED_EDGE('',*,*,#47941,.T.);
#63325=ORIENTED_EDGE('',*,*,#47942,.T.);
#63326=ORIENTED_EDGE('',*,*,#47943,.F.);
#63327=ORIENTED_EDGE('',*,*,#47939,.F.);
#63328=ORIENTED_EDGE('',*,*,#47944,.T.);
#63329=ORIENTED_EDGE('',*,*,#47937,.T.);
#63330=ORIENTED_EDGE('',*,*,#47945,.F.);
#63331=ORIENTED_EDGE('',*,*,#47942,.F.);
#63332=ORIENTED_EDGE('',*,*,#47946,.T.);
#63333=ORIENTED_EDGE('',*,*,#47947,.T.);
#63334=ORIENTED_EDGE('',*,*,#47948,.F.);
#63335=ORIENTED_EDGE('',*,*,#47949,.F.);
#63336=ORIENTED_EDGE('',*,*,#47950,.T.);
#63337=ORIENTED_EDGE('',*,*,#47951,.T.);
#63338=ORIENTED_EDGE('',*,*,#47952,.F.);
#63339=ORIENTED_EDGE('',*,*,#47947,.F.);
#63340=ORIENTED_EDGE('',*,*,#47953,.T.);
#63341=ORIENTED_EDGE('',*,*,#47954,.T.);
#63342=ORIENTED_EDGE('',*,*,#47955,.F.);
#63343=ORIENTED_EDGE('',*,*,#47951,.F.);
#63344=ORIENTED_EDGE('',*,*,#47956,.T.);
#63345=ORIENTED_EDGE('',*,*,#47949,.T.);
#63346=ORIENTED_EDGE('',*,*,#47957,.F.);
#63347=ORIENTED_EDGE('',*,*,#47954,.F.);
#63348=ORIENTED_EDGE('',*,*,#47958,.T.);
#63349=ORIENTED_EDGE('',*,*,#47959,.T.);
#63350=ORIENTED_EDGE('',*,*,#47960,.F.);
#63351=ORIENTED_EDGE('',*,*,#47961,.F.);
#63352=ORIENTED_EDGE('',*,*,#47962,.T.);
#63353=ORIENTED_EDGE('',*,*,#47963,.T.);
#63354=ORIENTED_EDGE('',*,*,#47964,.F.);
#63355=ORIENTED_EDGE('',*,*,#47959,.F.);
#63356=ORIENTED_EDGE('',*,*,#47965,.T.);
#63357=ORIENTED_EDGE('',*,*,#47966,.T.);
#63358=ORIENTED_EDGE('',*,*,#47967,.F.);
#63359=ORIENTED_EDGE('',*,*,#47963,.F.);
#63360=ORIENTED_EDGE('',*,*,#47968,.T.);
#63361=ORIENTED_EDGE('',*,*,#47961,.T.);
#63362=ORIENTED_EDGE('',*,*,#47969,.F.);
#63363=ORIENTED_EDGE('',*,*,#47966,.F.);
#63364=ORIENTED_EDGE('',*,*,#47970,.T.);
#63365=ORIENTED_EDGE('',*,*,#47971,.T.);
#63366=ORIENTED_EDGE('',*,*,#47972,.F.);
#63367=ORIENTED_EDGE('',*,*,#47973,.F.);
#63368=ORIENTED_EDGE('',*,*,#47974,.T.);
#63369=ORIENTED_EDGE('',*,*,#47975,.T.);
#63370=ORIENTED_EDGE('',*,*,#47976,.F.);
#63371=ORIENTED_EDGE('',*,*,#47971,.F.);
#63372=ORIENTED_EDGE('',*,*,#47977,.T.);
#63373=ORIENTED_EDGE('',*,*,#47978,.T.);
#63374=ORIENTED_EDGE('',*,*,#47979,.F.);
#63375=ORIENTED_EDGE('',*,*,#47975,.F.);
#63376=ORIENTED_EDGE('',*,*,#47980,.T.);
#63377=ORIENTED_EDGE('',*,*,#47973,.T.);
#63378=ORIENTED_EDGE('',*,*,#47981,.F.);
#63379=ORIENTED_EDGE('',*,*,#47978,.F.);
#63380=ORIENTED_EDGE('',*,*,#47982,.T.);
#63381=ORIENTED_EDGE('',*,*,#47983,.T.);
#63382=ORIENTED_EDGE('',*,*,#47984,.F.);
#63383=ORIENTED_EDGE('',*,*,#47985,.F.);
#63384=ORIENTED_EDGE('',*,*,#47986,.T.);
#63385=ORIENTED_EDGE('',*,*,#47987,.T.);
#63386=ORIENTED_EDGE('',*,*,#47988,.F.);
#63387=ORIENTED_EDGE('',*,*,#47983,.F.);
#63388=ORIENTED_EDGE('',*,*,#47989,.T.);
#63389=ORIENTED_EDGE('',*,*,#47990,.T.);
#63390=ORIENTED_EDGE('',*,*,#47991,.F.);
#63391=ORIENTED_EDGE('',*,*,#47987,.F.);
#63392=ORIENTED_EDGE('',*,*,#47992,.T.);
#63393=ORIENTED_EDGE('',*,*,#47985,.T.);
#63394=ORIENTED_EDGE('',*,*,#47993,.F.);
#63395=ORIENTED_EDGE('',*,*,#47990,.F.);
#63396=ORIENTED_EDGE('',*,*,#47994,.T.);
#63397=ORIENTED_EDGE('',*,*,#47995,.T.);
#63398=ORIENTED_EDGE('',*,*,#47996,.F.);
#63399=ORIENTED_EDGE('',*,*,#47997,.F.);
#63400=ORIENTED_EDGE('',*,*,#47998,.T.);
#63401=ORIENTED_EDGE('',*,*,#47999,.T.);
#63402=ORIENTED_EDGE('',*,*,#48000,.F.);
#63403=ORIENTED_EDGE('',*,*,#47995,.F.);
#63404=ORIENTED_EDGE('',*,*,#48001,.T.);
#63405=ORIENTED_EDGE('',*,*,#48002,.T.);
#63406=ORIENTED_EDGE('',*,*,#48003,.F.);
#63407=ORIENTED_EDGE('',*,*,#47999,.F.);
#63408=ORIENTED_EDGE('',*,*,#48004,.T.);
#63409=ORIENTED_EDGE('',*,*,#47997,.T.);
#63410=ORIENTED_EDGE('',*,*,#48005,.F.);
#63411=ORIENTED_EDGE('',*,*,#48002,.F.);
#63412=ORIENTED_EDGE('',*,*,#48006,.T.);
#63413=ORIENTED_EDGE('',*,*,#48007,.T.);
#63414=ORIENTED_EDGE('',*,*,#48008,.F.);
#63415=ORIENTED_EDGE('',*,*,#48009,.F.);
#63416=ORIENTED_EDGE('',*,*,#48010,.T.);
#63417=ORIENTED_EDGE('',*,*,#48011,.T.);
#63418=ORIENTED_EDGE('',*,*,#48012,.F.);
#63419=ORIENTED_EDGE('',*,*,#48007,.F.);
#63420=ORIENTED_EDGE('',*,*,#48013,.T.);
#63421=ORIENTED_EDGE('',*,*,#48014,.T.);
#63422=ORIENTED_EDGE('',*,*,#48015,.F.);
#63423=ORIENTED_EDGE('',*,*,#48011,.F.);
#63424=ORIENTED_EDGE('',*,*,#48016,.T.);
#63425=ORIENTED_EDGE('',*,*,#48009,.T.);
#63426=ORIENTED_EDGE('',*,*,#48017,.F.);
#63427=ORIENTED_EDGE('',*,*,#48014,.F.);
#63428=ORIENTED_EDGE('',*,*,#48018,.T.);
#63429=ORIENTED_EDGE('',*,*,#48019,.T.);
#63430=ORIENTED_EDGE('',*,*,#48020,.F.);
#63431=ORIENTED_EDGE('',*,*,#48021,.F.);
#63432=ORIENTED_EDGE('',*,*,#48022,.T.);
#63433=ORIENTED_EDGE('',*,*,#48023,.T.);
#63434=ORIENTED_EDGE('',*,*,#48024,.F.);
#63435=ORIENTED_EDGE('',*,*,#48019,.F.);
#63436=ORIENTED_EDGE('',*,*,#48025,.T.);
#63437=ORIENTED_EDGE('',*,*,#48026,.T.);
#63438=ORIENTED_EDGE('',*,*,#48027,.F.);
#63439=ORIENTED_EDGE('',*,*,#48023,.F.);
#63440=ORIENTED_EDGE('',*,*,#48028,.T.);
#63441=ORIENTED_EDGE('',*,*,#48021,.T.);
#63442=ORIENTED_EDGE('',*,*,#48029,.F.);
#63443=ORIENTED_EDGE('',*,*,#48026,.F.);
#63444=ORIENTED_EDGE('',*,*,#48030,.T.);
#63445=ORIENTED_EDGE('',*,*,#48031,.T.);
#63446=ORIENTED_EDGE('',*,*,#48032,.F.);
#63447=ORIENTED_EDGE('',*,*,#48033,.F.);
#63448=ORIENTED_EDGE('',*,*,#48034,.T.);
#63449=ORIENTED_EDGE('',*,*,#48035,.T.);
#63450=ORIENTED_EDGE('',*,*,#48036,.F.);
#63451=ORIENTED_EDGE('',*,*,#48031,.F.);
#63452=ORIENTED_EDGE('',*,*,#48037,.T.);
#63453=ORIENTED_EDGE('',*,*,#48038,.T.);
#63454=ORIENTED_EDGE('',*,*,#48039,.F.);
#63455=ORIENTED_EDGE('',*,*,#48035,.F.);
#63456=ORIENTED_EDGE('',*,*,#48040,.T.);
#63457=ORIENTED_EDGE('',*,*,#48033,.T.);
#63458=ORIENTED_EDGE('',*,*,#48041,.F.);
#63459=ORIENTED_EDGE('',*,*,#48038,.F.);
#63460=ORIENTED_EDGE('',*,*,#48042,.T.);
#63461=ORIENTED_EDGE('',*,*,#48043,.T.);
#63462=ORIENTED_EDGE('',*,*,#48044,.F.);
#63463=ORIENTED_EDGE('',*,*,#48045,.F.);
#63464=ORIENTED_EDGE('',*,*,#48046,.T.);
#63465=ORIENTED_EDGE('',*,*,#48047,.T.);
#63466=ORIENTED_EDGE('',*,*,#48048,.F.);
#63467=ORIENTED_EDGE('',*,*,#48043,.F.);
#63468=ORIENTED_EDGE('',*,*,#48049,.T.);
#63469=ORIENTED_EDGE('',*,*,#48050,.T.);
#63470=ORIENTED_EDGE('',*,*,#48051,.F.);
#63471=ORIENTED_EDGE('',*,*,#48047,.F.);
#63472=ORIENTED_EDGE('',*,*,#48052,.T.);
#63473=ORIENTED_EDGE('',*,*,#48045,.T.);
#63474=ORIENTED_EDGE('',*,*,#48053,.F.);
#63475=ORIENTED_EDGE('',*,*,#48050,.F.);
#63476=ORIENTED_EDGE('',*,*,#48054,.T.);
#63477=ORIENTED_EDGE('',*,*,#48055,.T.);
#63478=ORIENTED_EDGE('',*,*,#48056,.F.);
#63479=ORIENTED_EDGE('',*,*,#48057,.F.);
#63480=ORIENTED_EDGE('',*,*,#48058,.T.);
#63481=ORIENTED_EDGE('',*,*,#48059,.T.);
#63482=ORIENTED_EDGE('',*,*,#48060,.F.);
#63483=ORIENTED_EDGE('',*,*,#48055,.F.);
#63484=ORIENTED_EDGE('',*,*,#48061,.T.);
#63485=ORIENTED_EDGE('',*,*,#48062,.T.);
#63486=ORIENTED_EDGE('',*,*,#48063,.F.);
#63487=ORIENTED_EDGE('',*,*,#48059,.F.);
#63488=ORIENTED_EDGE('',*,*,#48064,.T.);
#63489=ORIENTED_EDGE('',*,*,#48057,.T.);
#63490=ORIENTED_EDGE('',*,*,#48065,.F.);
#63491=ORIENTED_EDGE('',*,*,#48062,.F.);
#63492=ORIENTED_EDGE('',*,*,#48066,.T.);
#63493=ORIENTED_EDGE('',*,*,#48067,.T.);
#63494=ORIENTED_EDGE('',*,*,#48068,.F.);
#63495=ORIENTED_EDGE('',*,*,#48069,.F.);
#63496=ORIENTED_EDGE('',*,*,#48070,.T.);
#63497=ORIENTED_EDGE('',*,*,#48071,.T.);
#63498=ORIENTED_EDGE('',*,*,#48072,.F.);
#63499=ORIENTED_EDGE('',*,*,#48067,.F.);
#63500=ORIENTED_EDGE('',*,*,#48073,.T.);
#63501=ORIENTED_EDGE('',*,*,#48074,.T.);
#63502=ORIENTED_EDGE('',*,*,#48075,.F.);
#63503=ORIENTED_EDGE('',*,*,#48071,.F.);
#63504=ORIENTED_EDGE('',*,*,#48076,.T.);
#63505=ORIENTED_EDGE('',*,*,#48069,.T.);
#63506=ORIENTED_EDGE('',*,*,#48077,.F.);
#63507=ORIENTED_EDGE('',*,*,#48074,.F.);
#63508=ORIENTED_EDGE('',*,*,#48078,.T.);
#63509=ORIENTED_EDGE('',*,*,#48079,.T.);
#63510=ORIENTED_EDGE('',*,*,#48080,.F.);
#63511=ORIENTED_EDGE('',*,*,#48081,.F.);
#63512=ORIENTED_EDGE('',*,*,#48082,.T.);
#63513=ORIENTED_EDGE('',*,*,#48083,.T.);
#63514=ORIENTED_EDGE('',*,*,#48084,.F.);
#63515=ORIENTED_EDGE('',*,*,#48079,.F.);
#63516=ORIENTED_EDGE('',*,*,#48085,.T.);
#63517=ORIENTED_EDGE('',*,*,#48086,.T.);
#63518=ORIENTED_EDGE('',*,*,#48087,.F.);
#63519=ORIENTED_EDGE('',*,*,#48083,.F.);
#63520=ORIENTED_EDGE('',*,*,#48088,.T.);
#63521=ORIENTED_EDGE('',*,*,#48081,.T.);
#63522=ORIENTED_EDGE('',*,*,#48089,.F.);
#63523=ORIENTED_EDGE('',*,*,#48086,.F.);
#63524=ORIENTED_EDGE('',*,*,#48090,.T.);
#63525=ORIENTED_EDGE('',*,*,#48091,.T.);
#63526=ORIENTED_EDGE('',*,*,#48092,.F.);
#63527=ORIENTED_EDGE('',*,*,#48093,.F.);
#63528=ORIENTED_EDGE('',*,*,#48094,.T.);
#63529=ORIENTED_EDGE('',*,*,#48095,.T.);
#63530=ORIENTED_EDGE('',*,*,#48096,.F.);
#63531=ORIENTED_EDGE('',*,*,#48091,.F.);
#63532=ORIENTED_EDGE('',*,*,#48097,.T.);
#63533=ORIENTED_EDGE('',*,*,#48098,.T.);
#63534=ORIENTED_EDGE('',*,*,#48099,.F.);
#63535=ORIENTED_EDGE('',*,*,#48095,.F.);
#63536=ORIENTED_EDGE('',*,*,#48100,.T.);
#63537=ORIENTED_EDGE('',*,*,#48093,.T.);
#63538=ORIENTED_EDGE('',*,*,#48101,.F.);
#63539=ORIENTED_EDGE('',*,*,#48098,.F.);
#63540=ORIENTED_EDGE('',*,*,#48102,.T.);
#63541=ORIENTED_EDGE('',*,*,#48103,.T.);
#63542=ORIENTED_EDGE('',*,*,#48104,.F.);
#63543=ORIENTED_EDGE('',*,*,#48105,.F.);
#63544=ORIENTED_EDGE('',*,*,#48106,.T.);
#63545=ORIENTED_EDGE('',*,*,#48107,.T.);
#63546=ORIENTED_EDGE('',*,*,#48108,.F.);
#63547=ORIENTED_EDGE('',*,*,#48103,.F.);
#63548=ORIENTED_EDGE('',*,*,#48109,.T.);
#63549=ORIENTED_EDGE('',*,*,#48110,.T.);
#63550=ORIENTED_EDGE('',*,*,#48111,.F.);
#63551=ORIENTED_EDGE('',*,*,#48107,.F.);
#63552=ORIENTED_EDGE('',*,*,#48112,.T.);
#63553=ORIENTED_EDGE('',*,*,#48105,.T.);
#63554=ORIENTED_EDGE('',*,*,#48113,.F.);
#63555=ORIENTED_EDGE('',*,*,#48110,.F.);
#63556=ORIENTED_EDGE('',*,*,#48114,.T.);
#63557=ORIENTED_EDGE('',*,*,#48115,.T.);
#63558=ORIENTED_EDGE('',*,*,#48116,.F.);
#63559=ORIENTED_EDGE('',*,*,#48117,.F.);
#63560=ORIENTED_EDGE('',*,*,#48118,.T.);
#63561=ORIENTED_EDGE('',*,*,#48119,.T.);
#63562=ORIENTED_EDGE('',*,*,#48120,.F.);
#63563=ORIENTED_EDGE('',*,*,#48115,.F.);
#63564=ORIENTED_EDGE('',*,*,#48121,.T.);
#63565=ORIENTED_EDGE('',*,*,#48122,.T.);
#63566=ORIENTED_EDGE('',*,*,#48123,.F.);
#63567=ORIENTED_EDGE('',*,*,#48119,.F.);
#63568=ORIENTED_EDGE('',*,*,#48124,.T.);
#63569=ORIENTED_EDGE('',*,*,#48117,.T.);
#63570=ORIENTED_EDGE('',*,*,#48125,.F.);
#63571=ORIENTED_EDGE('',*,*,#48122,.F.);
#63572=ORIENTED_EDGE('',*,*,#48126,.T.);
#63573=ORIENTED_EDGE('',*,*,#48127,.T.);
#63574=ORIENTED_EDGE('',*,*,#48128,.F.);
#63575=ORIENTED_EDGE('',*,*,#48129,.F.);
#63576=ORIENTED_EDGE('',*,*,#48130,.T.);
#63577=ORIENTED_EDGE('',*,*,#48131,.T.);
#63578=ORIENTED_EDGE('',*,*,#48132,.F.);
#63579=ORIENTED_EDGE('',*,*,#48127,.F.);
#63580=ORIENTED_EDGE('',*,*,#48133,.T.);
#63581=ORIENTED_EDGE('',*,*,#48134,.T.);
#63582=ORIENTED_EDGE('',*,*,#48135,.F.);
#63583=ORIENTED_EDGE('',*,*,#48131,.F.);
#63584=ORIENTED_EDGE('',*,*,#48136,.T.);
#63585=ORIENTED_EDGE('',*,*,#48129,.T.);
#63586=ORIENTED_EDGE('',*,*,#48137,.F.);
#63587=ORIENTED_EDGE('',*,*,#48134,.F.);
#63588=ORIENTED_EDGE('',*,*,#48138,.T.);
#63589=ORIENTED_EDGE('',*,*,#48139,.T.);
#63590=ORIENTED_EDGE('',*,*,#48140,.F.);
#63591=ORIENTED_EDGE('',*,*,#48141,.F.);
#63592=ORIENTED_EDGE('',*,*,#48142,.T.);
#63593=ORIENTED_EDGE('',*,*,#48143,.T.);
#63594=ORIENTED_EDGE('',*,*,#48144,.F.);
#63595=ORIENTED_EDGE('',*,*,#48139,.F.);
#63596=ORIENTED_EDGE('',*,*,#48145,.T.);
#63597=ORIENTED_EDGE('',*,*,#48146,.T.);
#63598=ORIENTED_EDGE('',*,*,#48147,.F.);
#63599=ORIENTED_EDGE('',*,*,#48143,.F.);
#63600=ORIENTED_EDGE('',*,*,#48148,.T.);
#63601=ORIENTED_EDGE('',*,*,#48141,.T.);
#63602=ORIENTED_EDGE('',*,*,#48149,.F.);
#63603=ORIENTED_EDGE('',*,*,#48146,.F.);
#63604=ORIENTED_EDGE('',*,*,#48150,.T.);
#63605=ORIENTED_EDGE('',*,*,#48151,.T.);
#63606=ORIENTED_EDGE('',*,*,#48152,.F.);
#63607=ORIENTED_EDGE('',*,*,#48153,.F.);
#63608=ORIENTED_EDGE('',*,*,#48154,.T.);
#63609=ORIENTED_EDGE('',*,*,#48155,.T.);
#63610=ORIENTED_EDGE('',*,*,#48156,.F.);
#63611=ORIENTED_EDGE('',*,*,#48151,.F.);
#63612=ORIENTED_EDGE('',*,*,#48157,.T.);
#63613=ORIENTED_EDGE('',*,*,#48158,.T.);
#63614=ORIENTED_EDGE('',*,*,#48159,.F.);
#63615=ORIENTED_EDGE('',*,*,#48155,.F.);
#63616=ORIENTED_EDGE('',*,*,#48160,.T.);
#63617=ORIENTED_EDGE('',*,*,#48153,.T.);
#63618=ORIENTED_EDGE('',*,*,#48161,.F.);
#63619=ORIENTED_EDGE('',*,*,#48158,.F.);
#63620=ORIENTED_EDGE('',*,*,#48162,.T.);
#63621=ORIENTED_EDGE('',*,*,#48163,.T.);
#63622=ORIENTED_EDGE('',*,*,#48164,.F.);
#63623=ORIENTED_EDGE('',*,*,#48165,.F.);
#63624=ORIENTED_EDGE('',*,*,#48166,.T.);
#63625=ORIENTED_EDGE('',*,*,#48167,.T.);
#63626=ORIENTED_EDGE('',*,*,#48168,.F.);
#63627=ORIENTED_EDGE('',*,*,#48163,.F.);
#63628=ORIENTED_EDGE('',*,*,#48169,.T.);
#63629=ORIENTED_EDGE('',*,*,#48170,.T.);
#63630=ORIENTED_EDGE('',*,*,#48171,.F.);
#63631=ORIENTED_EDGE('',*,*,#48167,.F.);
#63632=ORIENTED_EDGE('',*,*,#48172,.T.);
#63633=ORIENTED_EDGE('',*,*,#48165,.T.);
#63634=ORIENTED_EDGE('',*,*,#48173,.F.);
#63635=ORIENTED_EDGE('',*,*,#48170,.F.);
#63636=ORIENTED_EDGE('',*,*,#48174,.T.);
#63637=ORIENTED_EDGE('',*,*,#48175,.T.);
#63638=ORIENTED_EDGE('',*,*,#48176,.F.);
#63639=ORIENTED_EDGE('',*,*,#48177,.F.);
#63640=ORIENTED_EDGE('',*,*,#48178,.T.);
#63641=ORIENTED_EDGE('',*,*,#48179,.T.);
#63642=ORIENTED_EDGE('',*,*,#48180,.F.);
#63643=ORIENTED_EDGE('',*,*,#48175,.F.);
#63644=ORIENTED_EDGE('',*,*,#48181,.T.);
#63645=ORIENTED_EDGE('',*,*,#48182,.T.);
#63646=ORIENTED_EDGE('',*,*,#48183,.F.);
#63647=ORIENTED_EDGE('',*,*,#48179,.F.);
#63648=ORIENTED_EDGE('',*,*,#48184,.T.);
#63649=ORIENTED_EDGE('',*,*,#48177,.T.);
#63650=ORIENTED_EDGE('',*,*,#48185,.F.);
#63651=ORIENTED_EDGE('',*,*,#48182,.F.);
#63652=ORIENTED_EDGE('',*,*,#48186,.T.);
#63653=ORIENTED_EDGE('',*,*,#48187,.T.);
#63654=ORIENTED_EDGE('',*,*,#48188,.F.);
#63655=ORIENTED_EDGE('',*,*,#48189,.F.);
#63656=ORIENTED_EDGE('',*,*,#48190,.T.);
#63657=ORIENTED_EDGE('',*,*,#48191,.T.);
#63658=ORIENTED_EDGE('',*,*,#48192,.F.);
#63659=ORIENTED_EDGE('',*,*,#48187,.F.);
#63660=ORIENTED_EDGE('',*,*,#48193,.T.);
#63661=ORIENTED_EDGE('',*,*,#48194,.T.);
#63662=ORIENTED_EDGE('',*,*,#48195,.F.);
#63663=ORIENTED_EDGE('',*,*,#48191,.F.);
#63664=ORIENTED_EDGE('',*,*,#48196,.T.);
#63665=ORIENTED_EDGE('',*,*,#48189,.T.);
#63666=ORIENTED_EDGE('',*,*,#48197,.F.);
#63667=ORIENTED_EDGE('',*,*,#48194,.F.);
#63668=ORIENTED_EDGE('',*,*,#48198,.T.);
#63669=ORIENTED_EDGE('',*,*,#48199,.T.);
#63670=ORIENTED_EDGE('',*,*,#48200,.F.);
#63671=ORIENTED_EDGE('',*,*,#48201,.F.);
#63672=ORIENTED_EDGE('',*,*,#48202,.T.);
#63673=ORIENTED_EDGE('',*,*,#48203,.T.);
#63674=ORIENTED_EDGE('',*,*,#48204,.F.);
#63675=ORIENTED_EDGE('',*,*,#48199,.F.);
#63676=ORIENTED_EDGE('',*,*,#48205,.T.);
#63677=ORIENTED_EDGE('',*,*,#48206,.T.);
#63678=ORIENTED_EDGE('',*,*,#48207,.F.);
#63679=ORIENTED_EDGE('',*,*,#48203,.F.);
#63680=ORIENTED_EDGE('',*,*,#48208,.T.);
#63681=ORIENTED_EDGE('',*,*,#48201,.T.);
#63682=ORIENTED_EDGE('',*,*,#48209,.F.);
#63683=ORIENTED_EDGE('',*,*,#48206,.F.);
#63684=ORIENTED_EDGE('',*,*,#48210,.T.);
#63685=ORIENTED_EDGE('',*,*,#48211,.T.);
#63686=ORIENTED_EDGE('',*,*,#48212,.F.);
#63687=ORIENTED_EDGE('',*,*,#48213,.F.);
#63688=ORIENTED_EDGE('',*,*,#48214,.T.);
#63689=ORIENTED_EDGE('',*,*,#48215,.T.);
#63690=ORIENTED_EDGE('',*,*,#48216,.F.);
#63691=ORIENTED_EDGE('',*,*,#48211,.F.);
#63692=ORIENTED_EDGE('',*,*,#48217,.T.);
#63693=ORIENTED_EDGE('',*,*,#48218,.T.);
#63694=ORIENTED_EDGE('',*,*,#48219,.F.);
#63695=ORIENTED_EDGE('',*,*,#48215,.F.);
#63696=ORIENTED_EDGE('',*,*,#48220,.T.);
#63697=ORIENTED_EDGE('',*,*,#48213,.T.);
#63698=ORIENTED_EDGE('',*,*,#48221,.F.);
#63699=ORIENTED_EDGE('',*,*,#48218,.F.);
#63700=ORIENTED_EDGE('',*,*,#48222,.T.);
#63701=ORIENTED_EDGE('',*,*,#48223,.T.);
#63702=ORIENTED_EDGE('',*,*,#48224,.F.);
#63703=ORIENTED_EDGE('',*,*,#48225,.F.);
#63704=ORIENTED_EDGE('',*,*,#48226,.T.);
#63705=ORIENTED_EDGE('',*,*,#48227,.T.);
#63706=ORIENTED_EDGE('',*,*,#48228,.F.);
#63707=ORIENTED_EDGE('',*,*,#48223,.F.);
#63708=ORIENTED_EDGE('',*,*,#48229,.T.);
#63709=ORIENTED_EDGE('',*,*,#48230,.T.);
#63710=ORIENTED_EDGE('',*,*,#48231,.F.);
#63711=ORIENTED_EDGE('',*,*,#48227,.F.);
#63712=ORIENTED_EDGE('',*,*,#48232,.T.);
#63713=ORIENTED_EDGE('',*,*,#48225,.T.);
#63714=ORIENTED_EDGE('',*,*,#48233,.F.);
#63715=ORIENTED_EDGE('',*,*,#48230,.F.);
#63716=ORIENTED_EDGE('',*,*,#48234,.T.);
#63717=ORIENTED_EDGE('',*,*,#48235,.T.);
#63718=ORIENTED_EDGE('',*,*,#48236,.F.);
#63719=ORIENTED_EDGE('',*,*,#48237,.F.);
#63720=ORIENTED_EDGE('',*,*,#48238,.T.);
#63721=ORIENTED_EDGE('',*,*,#48239,.T.);
#63722=ORIENTED_EDGE('',*,*,#48240,.F.);
#63723=ORIENTED_EDGE('',*,*,#48235,.F.);
#63724=ORIENTED_EDGE('',*,*,#48241,.T.);
#63725=ORIENTED_EDGE('',*,*,#48242,.T.);
#63726=ORIENTED_EDGE('',*,*,#48243,.F.);
#63727=ORIENTED_EDGE('',*,*,#48239,.F.);
#63728=ORIENTED_EDGE('',*,*,#48244,.T.);
#63729=ORIENTED_EDGE('',*,*,#48237,.T.);
#63730=ORIENTED_EDGE('',*,*,#48245,.F.);
#63731=ORIENTED_EDGE('',*,*,#48242,.F.);
#63732=ORIENTED_EDGE('',*,*,#48246,.T.);
#63733=ORIENTED_EDGE('',*,*,#48247,.T.);
#63734=ORIENTED_EDGE('',*,*,#48248,.F.);
#63735=ORIENTED_EDGE('',*,*,#48249,.F.);
#63736=ORIENTED_EDGE('',*,*,#48250,.T.);
#63737=ORIENTED_EDGE('',*,*,#48251,.T.);
#63738=ORIENTED_EDGE('',*,*,#48252,.F.);
#63739=ORIENTED_EDGE('',*,*,#48247,.F.);
#63740=ORIENTED_EDGE('',*,*,#48253,.T.);
#63741=ORIENTED_EDGE('',*,*,#48254,.T.);
#63742=ORIENTED_EDGE('',*,*,#48255,.F.);
#63743=ORIENTED_EDGE('',*,*,#48251,.F.);
#63744=ORIENTED_EDGE('',*,*,#48256,.T.);
#63745=ORIENTED_EDGE('',*,*,#48249,.T.);
#63746=ORIENTED_EDGE('',*,*,#48257,.F.);
#63747=ORIENTED_EDGE('',*,*,#48254,.F.);
#63748=ORIENTED_EDGE('',*,*,#48258,.T.);
#63749=ORIENTED_EDGE('',*,*,#48259,.T.);
#63750=ORIENTED_EDGE('',*,*,#48260,.F.);
#63751=ORIENTED_EDGE('',*,*,#48261,.F.);
#63752=ORIENTED_EDGE('',*,*,#48262,.T.);
#63753=ORIENTED_EDGE('',*,*,#48263,.T.);
#63754=ORIENTED_EDGE('',*,*,#48264,.F.);
#63755=ORIENTED_EDGE('',*,*,#48259,.F.);
#63756=ORIENTED_EDGE('',*,*,#48265,.T.);
#63757=ORIENTED_EDGE('',*,*,#48266,.T.);
#63758=ORIENTED_EDGE('',*,*,#48267,.F.);
#63759=ORIENTED_EDGE('',*,*,#48263,.F.);
#63760=ORIENTED_EDGE('',*,*,#48268,.T.);
#63761=ORIENTED_EDGE('',*,*,#48261,.T.);
#63762=ORIENTED_EDGE('',*,*,#48269,.F.);
#63763=ORIENTED_EDGE('',*,*,#48266,.F.);
#63764=ORIENTED_EDGE('',*,*,#48270,.T.);
#63765=ORIENTED_EDGE('',*,*,#48271,.T.);
#63766=ORIENTED_EDGE('',*,*,#48272,.F.);
#63767=ORIENTED_EDGE('',*,*,#48273,.F.);
#63768=ORIENTED_EDGE('',*,*,#48274,.T.);
#63769=ORIENTED_EDGE('',*,*,#48275,.T.);
#63770=ORIENTED_EDGE('',*,*,#48276,.F.);
#63771=ORIENTED_EDGE('',*,*,#48271,.F.);
#63772=ORIENTED_EDGE('',*,*,#48277,.T.);
#63773=ORIENTED_EDGE('',*,*,#48278,.T.);
#63774=ORIENTED_EDGE('',*,*,#48279,.F.);
#63775=ORIENTED_EDGE('',*,*,#48275,.F.);
#63776=ORIENTED_EDGE('',*,*,#48280,.T.);
#63777=ORIENTED_EDGE('',*,*,#48273,.T.);
#63778=ORIENTED_EDGE('',*,*,#48281,.F.);
#63779=ORIENTED_EDGE('',*,*,#48278,.F.);
#63780=ORIENTED_EDGE('',*,*,#48282,.T.);
#63781=ORIENTED_EDGE('',*,*,#48283,.T.);
#63782=ORIENTED_EDGE('',*,*,#48284,.F.);
#63783=ORIENTED_EDGE('',*,*,#48285,.F.);
#63784=ORIENTED_EDGE('',*,*,#48286,.T.);
#63785=ORIENTED_EDGE('',*,*,#48287,.T.);
#63786=ORIENTED_EDGE('',*,*,#48288,.F.);
#63787=ORIENTED_EDGE('',*,*,#48283,.F.);
#63788=ORIENTED_EDGE('',*,*,#48289,.T.);
#63789=ORIENTED_EDGE('',*,*,#48290,.T.);
#63790=ORIENTED_EDGE('',*,*,#48291,.F.);
#63791=ORIENTED_EDGE('',*,*,#48287,.F.);
#63792=ORIENTED_EDGE('',*,*,#48292,.T.);
#63793=ORIENTED_EDGE('',*,*,#48285,.T.);
#63794=ORIENTED_EDGE('',*,*,#48293,.F.);
#63795=ORIENTED_EDGE('',*,*,#48290,.F.);
#63796=ORIENTED_EDGE('',*,*,#48294,.T.);
#63797=ORIENTED_EDGE('',*,*,#48295,.T.);
#63798=ORIENTED_EDGE('',*,*,#48296,.F.);
#63799=ORIENTED_EDGE('',*,*,#48297,.F.);
#63800=ORIENTED_EDGE('',*,*,#48298,.T.);
#63801=ORIENTED_EDGE('',*,*,#48299,.T.);
#63802=ORIENTED_EDGE('',*,*,#48300,.F.);
#63803=ORIENTED_EDGE('',*,*,#48295,.F.);
#63804=ORIENTED_EDGE('',*,*,#48301,.T.);
#63805=ORIENTED_EDGE('',*,*,#48302,.T.);
#63806=ORIENTED_EDGE('',*,*,#48303,.F.);
#63807=ORIENTED_EDGE('',*,*,#48299,.F.);
#63808=ORIENTED_EDGE('',*,*,#48304,.T.);
#63809=ORIENTED_EDGE('',*,*,#48297,.T.);
#63810=ORIENTED_EDGE('',*,*,#48305,.F.);
#63811=ORIENTED_EDGE('',*,*,#48302,.F.);
#63812=ORIENTED_EDGE('',*,*,#48306,.T.);
#63813=ORIENTED_EDGE('',*,*,#48307,.T.);
#63814=ORIENTED_EDGE('',*,*,#48308,.F.);
#63815=ORIENTED_EDGE('',*,*,#48309,.F.);
#63816=ORIENTED_EDGE('',*,*,#48310,.T.);
#63817=ORIENTED_EDGE('',*,*,#48311,.T.);
#63818=ORIENTED_EDGE('',*,*,#48312,.F.);
#63819=ORIENTED_EDGE('',*,*,#48307,.F.);
#63820=ORIENTED_EDGE('',*,*,#48313,.T.);
#63821=ORIENTED_EDGE('',*,*,#48314,.T.);
#63822=ORIENTED_EDGE('',*,*,#48315,.F.);
#63823=ORIENTED_EDGE('',*,*,#48311,.F.);
#63824=ORIENTED_EDGE('',*,*,#48316,.T.);
#63825=ORIENTED_EDGE('',*,*,#48309,.T.);
#63826=ORIENTED_EDGE('',*,*,#48317,.F.);
#63827=ORIENTED_EDGE('',*,*,#48314,.F.);
#63828=ORIENTED_EDGE('',*,*,#48318,.T.);
#63829=ORIENTED_EDGE('',*,*,#48319,.T.);
#63830=ORIENTED_EDGE('',*,*,#48320,.F.);
#63831=ORIENTED_EDGE('',*,*,#48321,.F.);
#63832=ORIENTED_EDGE('',*,*,#48322,.T.);
#63833=ORIENTED_EDGE('',*,*,#48323,.T.);
#63834=ORIENTED_EDGE('',*,*,#48324,.F.);
#63835=ORIENTED_EDGE('',*,*,#48319,.F.);
#63836=ORIENTED_EDGE('',*,*,#48325,.T.);
#63837=ORIENTED_EDGE('',*,*,#48326,.T.);
#63838=ORIENTED_EDGE('',*,*,#48327,.F.);
#63839=ORIENTED_EDGE('',*,*,#48323,.F.);
#63840=ORIENTED_EDGE('',*,*,#48328,.T.);
#63841=ORIENTED_EDGE('',*,*,#48321,.T.);
#63842=ORIENTED_EDGE('',*,*,#48329,.F.);
#63843=ORIENTED_EDGE('',*,*,#48326,.F.);
#63844=ORIENTED_EDGE('',*,*,#48330,.T.);
#63845=ORIENTED_EDGE('',*,*,#48331,.T.);
#63846=ORIENTED_EDGE('',*,*,#48332,.F.);
#63847=ORIENTED_EDGE('',*,*,#48333,.F.);
#63848=ORIENTED_EDGE('',*,*,#48334,.T.);
#63849=ORIENTED_EDGE('',*,*,#48335,.T.);
#63850=ORIENTED_EDGE('',*,*,#48336,.F.);
#63851=ORIENTED_EDGE('',*,*,#48331,.F.);
#63852=ORIENTED_EDGE('',*,*,#48337,.T.);
#63853=ORIENTED_EDGE('',*,*,#48338,.T.);
#63854=ORIENTED_EDGE('',*,*,#48339,.F.);
#63855=ORIENTED_EDGE('',*,*,#48335,.F.);
#63856=ORIENTED_EDGE('',*,*,#48340,.T.);
#63857=ORIENTED_EDGE('',*,*,#48333,.T.);
#63858=ORIENTED_EDGE('',*,*,#48341,.F.);
#63859=ORIENTED_EDGE('',*,*,#48338,.F.);
#63860=ORIENTED_EDGE('',*,*,#48342,.T.);
#63861=ORIENTED_EDGE('',*,*,#48343,.T.);
#63862=ORIENTED_EDGE('',*,*,#48344,.F.);
#63863=ORIENTED_EDGE('',*,*,#48345,.F.);
#63864=ORIENTED_EDGE('',*,*,#48346,.T.);
#63865=ORIENTED_EDGE('',*,*,#48347,.T.);
#63866=ORIENTED_EDGE('',*,*,#48348,.F.);
#63867=ORIENTED_EDGE('',*,*,#48343,.F.);
#63868=ORIENTED_EDGE('',*,*,#48349,.T.);
#63869=ORIENTED_EDGE('',*,*,#48350,.T.);
#63870=ORIENTED_EDGE('',*,*,#48351,.F.);
#63871=ORIENTED_EDGE('',*,*,#48347,.F.);
#63872=ORIENTED_EDGE('',*,*,#48352,.T.);
#63873=ORIENTED_EDGE('',*,*,#48345,.T.);
#63874=ORIENTED_EDGE('',*,*,#48353,.F.);
#63875=ORIENTED_EDGE('',*,*,#48350,.F.);
#63876=ORIENTED_EDGE('',*,*,#48354,.T.);
#63877=ORIENTED_EDGE('',*,*,#48355,.T.);
#63878=ORIENTED_EDGE('',*,*,#48356,.F.);
#63879=ORIENTED_EDGE('',*,*,#48357,.F.);
#63880=ORIENTED_EDGE('',*,*,#48358,.T.);
#63881=ORIENTED_EDGE('',*,*,#48359,.T.);
#63882=ORIENTED_EDGE('',*,*,#48360,.F.);
#63883=ORIENTED_EDGE('',*,*,#48355,.F.);
#63884=ORIENTED_EDGE('',*,*,#48361,.T.);
#63885=ORIENTED_EDGE('',*,*,#48362,.T.);
#63886=ORIENTED_EDGE('',*,*,#48363,.F.);
#63887=ORIENTED_EDGE('',*,*,#48359,.F.);
#63888=ORIENTED_EDGE('',*,*,#48364,.T.);
#63889=ORIENTED_EDGE('',*,*,#48357,.T.);
#63890=ORIENTED_EDGE('',*,*,#48365,.F.);
#63891=ORIENTED_EDGE('',*,*,#48362,.F.);
#63892=ORIENTED_EDGE('',*,*,#48366,.T.);
#63893=ORIENTED_EDGE('',*,*,#48367,.T.);
#63894=ORIENTED_EDGE('',*,*,#48368,.F.);
#63895=ORIENTED_EDGE('',*,*,#48369,.F.);
#63896=ORIENTED_EDGE('',*,*,#48370,.T.);
#63897=ORIENTED_EDGE('',*,*,#48371,.T.);
#63898=ORIENTED_EDGE('',*,*,#48372,.F.);
#63899=ORIENTED_EDGE('',*,*,#48367,.F.);
#63900=ORIENTED_EDGE('',*,*,#48373,.T.);
#63901=ORIENTED_EDGE('',*,*,#48374,.T.);
#63902=ORIENTED_EDGE('',*,*,#48375,.F.);
#63903=ORIENTED_EDGE('',*,*,#48371,.F.);
#63904=ORIENTED_EDGE('',*,*,#48376,.T.);
#63905=ORIENTED_EDGE('',*,*,#48369,.T.);
#63906=ORIENTED_EDGE('',*,*,#48377,.F.);
#63907=ORIENTED_EDGE('',*,*,#48374,.F.);
#63908=ORIENTED_EDGE('',*,*,#48378,.T.);
#63909=ORIENTED_EDGE('',*,*,#48379,.T.);
#63910=ORIENTED_EDGE('',*,*,#48380,.F.);
#63911=ORIENTED_EDGE('',*,*,#48381,.F.);
#63912=ORIENTED_EDGE('',*,*,#48382,.T.);
#63913=ORIENTED_EDGE('',*,*,#48383,.T.);
#63914=ORIENTED_EDGE('',*,*,#48384,.F.);
#63915=ORIENTED_EDGE('',*,*,#48379,.F.);
#63916=ORIENTED_EDGE('',*,*,#48385,.T.);
#63917=ORIENTED_EDGE('',*,*,#48386,.T.);
#63918=ORIENTED_EDGE('',*,*,#48387,.F.);
#63919=ORIENTED_EDGE('',*,*,#48383,.F.);
#63920=ORIENTED_EDGE('',*,*,#48388,.T.);
#63921=ORIENTED_EDGE('',*,*,#48381,.T.);
#63922=ORIENTED_EDGE('',*,*,#48389,.F.);
#63923=ORIENTED_EDGE('',*,*,#48386,.F.);
#63924=ORIENTED_EDGE('',*,*,#48390,.T.);
#63925=ORIENTED_EDGE('',*,*,#48391,.T.);
#63926=ORIENTED_EDGE('',*,*,#48392,.F.);
#63927=ORIENTED_EDGE('',*,*,#48393,.F.);
#63928=ORIENTED_EDGE('',*,*,#48394,.T.);
#63929=ORIENTED_EDGE('',*,*,#48395,.T.);
#63930=ORIENTED_EDGE('',*,*,#48396,.F.);
#63931=ORIENTED_EDGE('',*,*,#48391,.F.);
#63932=ORIENTED_EDGE('',*,*,#48397,.T.);
#63933=ORIENTED_EDGE('',*,*,#48398,.T.);
#63934=ORIENTED_EDGE('',*,*,#48399,.F.);
#63935=ORIENTED_EDGE('',*,*,#48395,.F.);
#63936=ORIENTED_EDGE('',*,*,#48400,.T.);
#63937=ORIENTED_EDGE('',*,*,#48393,.T.);
#63938=ORIENTED_EDGE('',*,*,#48401,.F.);
#63939=ORIENTED_EDGE('',*,*,#48398,.F.);
#63940=ORIENTED_EDGE('',*,*,#48402,.T.);
#63941=ORIENTED_EDGE('',*,*,#48403,.T.);
#63942=ORIENTED_EDGE('',*,*,#48404,.F.);
#63943=ORIENTED_EDGE('',*,*,#48405,.F.);
#63944=ORIENTED_EDGE('',*,*,#48406,.T.);
#63945=ORIENTED_EDGE('',*,*,#48407,.T.);
#63946=ORIENTED_EDGE('',*,*,#48408,.F.);
#63947=ORIENTED_EDGE('',*,*,#48403,.F.);
#63948=ORIENTED_EDGE('',*,*,#48409,.T.);
#63949=ORIENTED_EDGE('',*,*,#48410,.T.);
#63950=ORIENTED_EDGE('',*,*,#48411,.F.);
#63951=ORIENTED_EDGE('',*,*,#48407,.F.);
#63952=ORIENTED_EDGE('',*,*,#48412,.T.);
#63953=ORIENTED_EDGE('',*,*,#48405,.T.);
#63954=ORIENTED_EDGE('',*,*,#48413,.F.);
#63955=ORIENTED_EDGE('',*,*,#48410,.F.);
#63956=ORIENTED_EDGE('',*,*,#48414,.T.);
#63957=ORIENTED_EDGE('',*,*,#48415,.T.);
#63958=ORIENTED_EDGE('',*,*,#48416,.F.);
#63959=ORIENTED_EDGE('',*,*,#48417,.F.);
#63960=ORIENTED_EDGE('',*,*,#48418,.T.);
#63961=ORIENTED_EDGE('',*,*,#48419,.T.);
#63962=ORIENTED_EDGE('',*,*,#48420,.F.);
#63963=ORIENTED_EDGE('',*,*,#48415,.F.);
#63964=ORIENTED_EDGE('',*,*,#48421,.T.);
#63965=ORIENTED_EDGE('',*,*,#48422,.T.);
#63966=ORIENTED_EDGE('',*,*,#48423,.F.);
#63967=ORIENTED_EDGE('',*,*,#48419,.F.);
#63968=ORIENTED_EDGE('',*,*,#48424,.T.);
#63969=ORIENTED_EDGE('',*,*,#48417,.T.);
#63970=ORIENTED_EDGE('',*,*,#48425,.F.);
#63971=ORIENTED_EDGE('',*,*,#48422,.F.);
#63972=ORIENTED_EDGE('',*,*,#48426,.T.);
#63973=ORIENTED_EDGE('',*,*,#48427,.T.);
#63974=ORIENTED_EDGE('',*,*,#48428,.F.);
#63975=ORIENTED_EDGE('',*,*,#48429,.F.);
#63976=ORIENTED_EDGE('',*,*,#48430,.T.);
#63977=ORIENTED_EDGE('',*,*,#48431,.T.);
#63978=ORIENTED_EDGE('',*,*,#48432,.F.);
#63979=ORIENTED_EDGE('',*,*,#48427,.F.);
#63980=ORIENTED_EDGE('',*,*,#48433,.T.);
#63981=ORIENTED_EDGE('',*,*,#48434,.T.);
#63982=ORIENTED_EDGE('',*,*,#48435,.F.);
#63983=ORIENTED_EDGE('',*,*,#48431,.F.);
#63984=ORIENTED_EDGE('',*,*,#48436,.T.);
#63985=ORIENTED_EDGE('',*,*,#48429,.T.);
#63986=ORIENTED_EDGE('',*,*,#48437,.F.);
#63987=ORIENTED_EDGE('',*,*,#48434,.F.);
#63988=ORIENTED_EDGE('',*,*,#48438,.T.);
#63989=ORIENTED_EDGE('',*,*,#48439,.T.);
#63990=ORIENTED_EDGE('',*,*,#48440,.F.);
#63991=ORIENTED_EDGE('',*,*,#48441,.F.);
#63992=ORIENTED_EDGE('',*,*,#48442,.T.);
#63993=ORIENTED_EDGE('',*,*,#48443,.T.);
#63994=ORIENTED_EDGE('',*,*,#48444,.F.);
#63995=ORIENTED_EDGE('',*,*,#48439,.F.);
#63996=ORIENTED_EDGE('',*,*,#48445,.T.);
#63997=ORIENTED_EDGE('',*,*,#48446,.T.);
#63998=ORIENTED_EDGE('',*,*,#48447,.F.);
#63999=ORIENTED_EDGE('',*,*,#48443,.F.);
#64000=ORIENTED_EDGE('',*,*,#48448,.T.);
#64001=ORIENTED_EDGE('',*,*,#48441,.T.);
#64002=ORIENTED_EDGE('',*,*,#48449,.F.);
#64003=ORIENTED_EDGE('',*,*,#48446,.F.);
#64004=ORIENTED_EDGE('',*,*,#48450,.T.);
#64005=ORIENTED_EDGE('',*,*,#48451,.T.);
#64006=ORIENTED_EDGE('',*,*,#48452,.F.);
#64007=ORIENTED_EDGE('',*,*,#48453,.F.);
#64008=ORIENTED_EDGE('',*,*,#48454,.T.);
#64009=ORIENTED_EDGE('',*,*,#48455,.T.);
#64010=ORIENTED_EDGE('',*,*,#48456,.F.);
#64011=ORIENTED_EDGE('',*,*,#48451,.F.);
#64012=ORIENTED_EDGE('',*,*,#48457,.T.);
#64013=ORIENTED_EDGE('',*,*,#48458,.T.);
#64014=ORIENTED_EDGE('',*,*,#48459,.F.);
#64015=ORIENTED_EDGE('',*,*,#48455,.F.);
#64016=ORIENTED_EDGE('',*,*,#48460,.T.);
#64017=ORIENTED_EDGE('',*,*,#48453,.T.);
#64018=ORIENTED_EDGE('',*,*,#48461,.F.);
#64019=ORIENTED_EDGE('',*,*,#48458,.F.);
#64020=ORIENTED_EDGE('',*,*,#48462,.T.);
#64021=ORIENTED_EDGE('',*,*,#48463,.T.);
#64022=ORIENTED_EDGE('',*,*,#48464,.F.);
#64023=ORIENTED_EDGE('',*,*,#48465,.F.);
#64024=ORIENTED_EDGE('',*,*,#48466,.T.);
#64025=ORIENTED_EDGE('',*,*,#48467,.T.);
#64026=ORIENTED_EDGE('',*,*,#48468,.F.);
#64027=ORIENTED_EDGE('',*,*,#48463,.F.);
#64028=ORIENTED_EDGE('',*,*,#48469,.T.);
#64029=ORIENTED_EDGE('',*,*,#48470,.T.);
#64030=ORIENTED_EDGE('',*,*,#48471,.F.);
#64031=ORIENTED_EDGE('',*,*,#48467,.F.);
#64032=ORIENTED_EDGE('',*,*,#48472,.T.);
#64033=ORIENTED_EDGE('',*,*,#48465,.T.);
#64034=ORIENTED_EDGE('',*,*,#48473,.F.);
#64035=ORIENTED_EDGE('',*,*,#48470,.F.);
#64036=ORIENTED_EDGE('',*,*,#48474,.T.);
#64037=ORIENTED_EDGE('',*,*,#48475,.T.);
#64038=ORIENTED_EDGE('',*,*,#48476,.F.);
#64039=ORIENTED_EDGE('',*,*,#48477,.F.);
#64040=ORIENTED_EDGE('',*,*,#48478,.T.);
#64041=ORIENTED_EDGE('',*,*,#48479,.T.);
#64042=ORIENTED_EDGE('',*,*,#48480,.F.);
#64043=ORIENTED_EDGE('',*,*,#48475,.F.);
#64044=ORIENTED_EDGE('',*,*,#48481,.T.);
#64045=ORIENTED_EDGE('',*,*,#48482,.T.);
#64046=ORIENTED_EDGE('',*,*,#48483,.F.);
#64047=ORIENTED_EDGE('',*,*,#48479,.F.);
#64048=ORIENTED_EDGE('',*,*,#48484,.T.);
#64049=ORIENTED_EDGE('',*,*,#48477,.T.);
#64050=ORIENTED_EDGE('',*,*,#48485,.F.);
#64051=ORIENTED_EDGE('',*,*,#48482,.F.);
#64052=ORIENTED_EDGE('',*,*,#48486,.T.);
#64053=ORIENTED_EDGE('',*,*,#48487,.T.);
#64054=ORIENTED_EDGE('',*,*,#48488,.F.);
#64055=ORIENTED_EDGE('',*,*,#48489,.F.);
#64056=ORIENTED_EDGE('',*,*,#48490,.T.);
#64057=ORIENTED_EDGE('',*,*,#48491,.T.);
#64058=ORIENTED_EDGE('',*,*,#48492,.F.);
#64059=ORIENTED_EDGE('',*,*,#48487,.F.);
#64060=ORIENTED_EDGE('',*,*,#48493,.T.);
#64061=ORIENTED_EDGE('',*,*,#48494,.T.);
#64062=ORIENTED_EDGE('',*,*,#48495,.F.);
#64063=ORIENTED_EDGE('',*,*,#48491,.F.);
#64064=ORIENTED_EDGE('',*,*,#48496,.T.);
#64065=ORIENTED_EDGE('',*,*,#48489,.T.);
#64066=ORIENTED_EDGE('',*,*,#48497,.F.);
#64067=ORIENTED_EDGE('',*,*,#48494,.F.);
#64068=ORIENTED_EDGE('',*,*,#48498,.T.);
#64069=ORIENTED_EDGE('',*,*,#48499,.T.);
#64070=ORIENTED_EDGE('',*,*,#48500,.F.);
#64071=ORIENTED_EDGE('',*,*,#48501,.F.);
#64072=ORIENTED_EDGE('',*,*,#48502,.T.);
#64073=ORIENTED_EDGE('',*,*,#48503,.T.);
#64074=ORIENTED_EDGE('',*,*,#48504,.F.);
#64075=ORIENTED_EDGE('',*,*,#48499,.F.);
#64076=ORIENTED_EDGE('',*,*,#48505,.T.);
#64077=ORIENTED_EDGE('',*,*,#48506,.T.);
#64078=ORIENTED_EDGE('',*,*,#48507,.F.);
#64079=ORIENTED_EDGE('',*,*,#48503,.F.);
#64080=ORIENTED_EDGE('',*,*,#48508,.T.);
#64081=ORIENTED_EDGE('',*,*,#48501,.T.);
#64082=ORIENTED_EDGE('',*,*,#48509,.F.);
#64083=ORIENTED_EDGE('',*,*,#48506,.F.);
#64084=ORIENTED_EDGE('',*,*,#48510,.T.);
#64085=ORIENTED_EDGE('',*,*,#48511,.T.);
#64086=ORIENTED_EDGE('',*,*,#48512,.F.);
#64087=ORIENTED_EDGE('',*,*,#48513,.F.);
#64088=ORIENTED_EDGE('',*,*,#48514,.T.);
#64089=ORIENTED_EDGE('',*,*,#48515,.T.);
#64090=ORIENTED_EDGE('',*,*,#48516,.F.);
#64091=ORIENTED_EDGE('',*,*,#48511,.F.);
#64092=ORIENTED_EDGE('',*,*,#48517,.T.);
#64093=ORIENTED_EDGE('',*,*,#48518,.T.);
#64094=ORIENTED_EDGE('',*,*,#48519,.F.);
#64095=ORIENTED_EDGE('',*,*,#48515,.F.);
#64096=ORIENTED_EDGE('',*,*,#48520,.T.);
#64097=ORIENTED_EDGE('',*,*,#48513,.T.);
#64098=ORIENTED_EDGE('',*,*,#48521,.F.);
#64099=ORIENTED_EDGE('',*,*,#48518,.F.);
#64100=ORIENTED_EDGE('',*,*,#48522,.T.);
#64101=ORIENTED_EDGE('',*,*,#48523,.T.);
#64102=ORIENTED_EDGE('',*,*,#48524,.F.);
#64103=ORIENTED_EDGE('',*,*,#48525,.F.);
#64104=ORIENTED_EDGE('',*,*,#48526,.T.);
#64105=ORIENTED_EDGE('',*,*,#48527,.T.);
#64106=ORIENTED_EDGE('',*,*,#48528,.F.);
#64107=ORIENTED_EDGE('',*,*,#48523,.F.);
#64108=ORIENTED_EDGE('',*,*,#48529,.T.);
#64109=ORIENTED_EDGE('',*,*,#48530,.T.);
#64110=ORIENTED_EDGE('',*,*,#48531,.F.);
#64111=ORIENTED_EDGE('',*,*,#48527,.F.);
#64112=ORIENTED_EDGE('',*,*,#48532,.T.);
#64113=ORIENTED_EDGE('',*,*,#48525,.T.);
#64114=ORIENTED_EDGE('',*,*,#48533,.F.);
#64115=ORIENTED_EDGE('',*,*,#48530,.F.);
#64116=ORIENTED_EDGE('',*,*,#48534,.T.);
#64117=ORIENTED_EDGE('',*,*,#48535,.T.);
#64118=ORIENTED_EDGE('',*,*,#48536,.F.);
#64119=ORIENTED_EDGE('',*,*,#48537,.F.);
#64120=ORIENTED_EDGE('',*,*,#48538,.T.);
#64121=ORIENTED_EDGE('',*,*,#48539,.T.);
#64122=ORIENTED_EDGE('',*,*,#48540,.F.);
#64123=ORIENTED_EDGE('',*,*,#48535,.F.);
#64124=ORIENTED_EDGE('',*,*,#48541,.T.);
#64125=ORIENTED_EDGE('',*,*,#48542,.T.);
#64126=ORIENTED_EDGE('',*,*,#48543,.F.);
#64127=ORIENTED_EDGE('',*,*,#48539,.F.);
#64128=ORIENTED_EDGE('',*,*,#48544,.T.);
#64129=ORIENTED_EDGE('',*,*,#48537,.T.);
#64130=ORIENTED_EDGE('',*,*,#48545,.F.);
#64131=ORIENTED_EDGE('',*,*,#48542,.F.);
#64132=ORIENTED_EDGE('',*,*,#48546,.T.);
#64133=ORIENTED_EDGE('',*,*,#48547,.T.);
#64134=ORIENTED_EDGE('',*,*,#48548,.F.);
#64135=ORIENTED_EDGE('',*,*,#48549,.F.);
#64136=ORIENTED_EDGE('',*,*,#48550,.T.);
#64137=ORIENTED_EDGE('',*,*,#48551,.T.);
#64138=ORIENTED_EDGE('',*,*,#48552,.F.);
#64139=ORIENTED_EDGE('',*,*,#48547,.F.);
#64140=ORIENTED_EDGE('',*,*,#48553,.T.);
#64141=ORIENTED_EDGE('',*,*,#48554,.T.);
#64142=ORIENTED_EDGE('',*,*,#48555,.F.);
#64143=ORIENTED_EDGE('',*,*,#48551,.F.);
#64144=ORIENTED_EDGE('',*,*,#48556,.T.);
#64145=ORIENTED_EDGE('',*,*,#48549,.T.);
#64146=ORIENTED_EDGE('',*,*,#48557,.F.);
#64147=ORIENTED_EDGE('',*,*,#48554,.F.);
#64148=ORIENTED_EDGE('',*,*,#48558,.T.);
#64149=ORIENTED_EDGE('',*,*,#48559,.T.);
#64150=ORIENTED_EDGE('',*,*,#48560,.F.);
#64151=ORIENTED_EDGE('',*,*,#48561,.F.);
#64152=ORIENTED_EDGE('',*,*,#48562,.T.);
#64153=ORIENTED_EDGE('',*,*,#48563,.T.);
#64154=ORIENTED_EDGE('',*,*,#48564,.F.);
#64155=ORIENTED_EDGE('',*,*,#48559,.F.);
#64156=ORIENTED_EDGE('',*,*,#48565,.T.);
#64157=ORIENTED_EDGE('',*,*,#48566,.T.);
#64158=ORIENTED_EDGE('',*,*,#48567,.F.);
#64159=ORIENTED_EDGE('',*,*,#48563,.F.);
#64160=ORIENTED_EDGE('',*,*,#48568,.T.);
#64161=ORIENTED_EDGE('',*,*,#48561,.T.);
#64162=ORIENTED_EDGE('',*,*,#48569,.F.);
#64163=ORIENTED_EDGE('',*,*,#48566,.F.);
#64164=ORIENTED_EDGE('',*,*,#48570,.T.);
#64165=ORIENTED_EDGE('',*,*,#48571,.T.);
#64166=ORIENTED_EDGE('',*,*,#48572,.F.);
#64167=ORIENTED_EDGE('',*,*,#48573,.F.);
#64168=ORIENTED_EDGE('',*,*,#48574,.T.);
#64169=ORIENTED_EDGE('',*,*,#48575,.T.);
#64170=ORIENTED_EDGE('',*,*,#48576,.F.);
#64171=ORIENTED_EDGE('',*,*,#48571,.F.);
#64172=ORIENTED_EDGE('',*,*,#48577,.T.);
#64173=ORIENTED_EDGE('',*,*,#48578,.T.);
#64174=ORIENTED_EDGE('',*,*,#48579,.F.);
#64175=ORIENTED_EDGE('',*,*,#48575,.F.);
#64176=ORIENTED_EDGE('',*,*,#48580,.T.);
#64177=ORIENTED_EDGE('',*,*,#48573,.T.);
#64178=ORIENTED_EDGE('',*,*,#48581,.F.);
#64179=ORIENTED_EDGE('',*,*,#48578,.F.);
#64180=ORIENTED_EDGE('',*,*,#48582,.T.);
#64181=ORIENTED_EDGE('',*,*,#48583,.T.);
#64182=ORIENTED_EDGE('',*,*,#48584,.F.);
#64183=ORIENTED_EDGE('',*,*,#48585,.F.);
#64184=ORIENTED_EDGE('',*,*,#48586,.T.);
#64185=ORIENTED_EDGE('',*,*,#48587,.T.);
#64186=ORIENTED_EDGE('',*,*,#48588,.F.);
#64187=ORIENTED_EDGE('',*,*,#48583,.F.);
#64188=ORIENTED_EDGE('',*,*,#48589,.T.);
#64189=ORIENTED_EDGE('',*,*,#48590,.T.);
#64190=ORIENTED_EDGE('',*,*,#48591,.F.);
#64191=ORIENTED_EDGE('',*,*,#48587,.F.);
#64192=ORIENTED_EDGE('',*,*,#48592,.T.);
#64193=ORIENTED_EDGE('',*,*,#48585,.T.);
#64194=ORIENTED_EDGE('',*,*,#48593,.F.);
#64195=ORIENTED_EDGE('',*,*,#48590,.F.);
#64196=ORIENTED_EDGE('',*,*,#48594,.T.);
#64197=ORIENTED_EDGE('',*,*,#48595,.T.);
#64198=ORIENTED_EDGE('',*,*,#48596,.F.);
#64199=ORIENTED_EDGE('',*,*,#48597,.F.);
#64200=ORIENTED_EDGE('',*,*,#48598,.T.);
#64201=ORIENTED_EDGE('',*,*,#48599,.T.);
#64202=ORIENTED_EDGE('',*,*,#48600,.F.);
#64203=ORIENTED_EDGE('',*,*,#48595,.F.);
#64204=ORIENTED_EDGE('',*,*,#48601,.T.);
#64205=ORIENTED_EDGE('',*,*,#48602,.T.);
#64206=ORIENTED_EDGE('',*,*,#48603,.F.);
#64207=ORIENTED_EDGE('',*,*,#48599,.F.);
#64208=ORIENTED_EDGE('',*,*,#48604,.T.);
#64209=ORIENTED_EDGE('',*,*,#48597,.T.);
#64210=ORIENTED_EDGE('',*,*,#48605,.F.);
#64211=ORIENTED_EDGE('',*,*,#48602,.F.);
#64212=ORIENTED_EDGE('',*,*,#48606,.T.);
#64213=ORIENTED_EDGE('',*,*,#48607,.T.);
#64214=ORIENTED_EDGE('',*,*,#48608,.F.);
#64215=ORIENTED_EDGE('',*,*,#48609,.F.);
#64216=ORIENTED_EDGE('',*,*,#48610,.T.);
#64217=ORIENTED_EDGE('',*,*,#48611,.T.);
#64218=ORIENTED_EDGE('',*,*,#48612,.F.);
#64219=ORIENTED_EDGE('',*,*,#48607,.F.);
#64220=ORIENTED_EDGE('',*,*,#48613,.T.);
#64221=ORIENTED_EDGE('',*,*,#48614,.T.);
#64222=ORIENTED_EDGE('',*,*,#48615,.F.);
#64223=ORIENTED_EDGE('',*,*,#48611,.F.);
#64224=ORIENTED_EDGE('',*,*,#48616,.T.);
#64225=ORIENTED_EDGE('',*,*,#48609,.T.);
#64226=ORIENTED_EDGE('',*,*,#48617,.F.);
#64227=ORIENTED_EDGE('',*,*,#48614,.F.);
#64228=ORIENTED_EDGE('',*,*,#48618,.T.);
#64229=ORIENTED_EDGE('',*,*,#48619,.T.);
#64230=ORIENTED_EDGE('',*,*,#48620,.F.);
#64231=ORIENTED_EDGE('',*,*,#48621,.F.);
#64232=ORIENTED_EDGE('',*,*,#48622,.T.);
#64233=ORIENTED_EDGE('',*,*,#48623,.T.);
#64234=ORIENTED_EDGE('',*,*,#48624,.F.);
#64235=ORIENTED_EDGE('',*,*,#48619,.F.);
#64236=ORIENTED_EDGE('',*,*,#48625,.T.);
#64237=ORIENTED_EDGE('',*,*,#48626,.T.);
#64238=ORIENTED_EDGE('',*,*,#48627,.F.);
#64239=ORIENTED_EDGE('',*,*,#48623,.F.);
#64240=ORIENTED_EDGE('',*,*,#48628,.T.);
#64241=ORIENTED_EDGE('',*,*,#48621,.T.);
#64242=ORIENTED_EDGE('',*,*,#48629,.F.);
#64243=ORIENTED_EDGE('',*,*,#48626,.F.);
#64244=ORIENTED_EDGE('',*,*,#48630,.T.);
#64245=ORIENTED_EDGE('',*,*,#48631,.T.);
#64246=ORIENTED_EDGE('',*,*,#48632,.F.);
#64247=ORIENTED_EDGE('',*,*,#48633,.F.);
#64248=ORIENTED_EDGE('',*,*,#48634,.T.);
#64249=ORIENTED_EDGE('',*,*,#48635,.T.);
#64250=ORIENTED_EDGE('',*,*,#48636,.F.);
#64251=ORIENTED_EDGE('',*,*,#48631,.F.);
#64252=ORIENTED_EDGE('',*,*,#48637,.T.);
#64253=ORIENTED_EDGE('',*,*,#48638,.T.);
#64254=ORIENTED_EDGE('',*,*,#48639,.F.);
#64255=ORIENTED_EDGE('',*,*,#48635,.F.);
#64256=ORIENTED_EDGE('',*,*,#48640,.T.);
#64257=ORIENTED_EDGE('',*,*,#48633,.T.);
#64258=ORIENTED_EDGE('',*,*,#48641,.F.);
#64259=ORIENTED_EDGE('',*,*,#48638,.F.);
#64260=ORIENTED_EDGE('',*,*,#48642,.T.);
#64261=ORIENTED_EDGE('',*,*,#48643,.T.);
#64262=ORIENTED_EDGE('',*,*,#48644,.F.);
#64263=ORIENTED_EDGE('',*,*,#48645,.F.);
#64264=ORIENTED_EDGE('',*,*,#48646,.T.);
#64265=ORIENTED_EDGE('',*,*,#48647,.T.);
#64266=ORIENTED_EDGE('',*,*,#48648,.F.);
#64267=ORIENTED_EDGE('',*,*,#48643,.F.);
#64268=ORIENTED_EDGE('',*,*,#48649,.T.);
#64269=ORIENTED_EDGE('',*,*,#48650,.T.);
#64270=ORIENTED_EDGE('',*,*,#48651,.F.);
#64271=ORIENTED_EDGE('',*,*,#48647,.F.);
#64272=ORIENTED_EDGE('',*,*,#48652,.T.);
#64273=ORIENTED_EDGE('',*,*,#48645,.T.);
#64274=ORIENTED_EDGE('',*,*,#48653,.F.);
#64275=ORIENTED_EDGE('',*,*,#48650,.F.);
#64276=ORIENTED_EDGE('',*,*,#48654,.T.);
#64277=ORIENTED_EDGE('',*,*,#48655,.T.);
#64278=ORIENTED_EDGE('',*,*,#48656,.F.);
#64279=ORIENTED_EDGE('',*,*,#48657,.F.);
#64280=ORIENTED_EDGE('',*,*,#48658,.T.);
#64281=ORIENTED_EDGE('',*,*,#48659,.T.);
#64282=ORIENTED_EDGE('',*,*,#48660,.F.);
#64283=ORIENTED_EDGE('',*,*,#48655,.F.);
#64284=ORIENTED_EDGE('',*,*,#48661,.T.);
#64285=ORIENTED_EDGE('',*,*,#48662,.T.);
#64286=ORIENTED_EDGE('',*,*,#48663,.F.);
#64287=ORIENTED_EDGE('',*,*,#48659,.F.);
#64288=ORIENTED_EDGE('',*,*,#48664,.T.);
#64289=ORIENTED_EDGE('',*,*,#48657,.T.);
#64290=ORIENTED_EDGE('',*,*,#48665,.F.);
#64291=ORIENTED_EDGE('',*,*,#48662,.F.);
#64292=ORIENTED_EDGE('',*,*,#48666,.T.);
#64293=ORIENTED_EDGE('',*,*,#48667,.T.);
#64294=ORIENTED_EDGE('',*,*,#48668,.F.);
#64295=ORIENTED_EDGE('',*,*,#48669,.F.);
#64296=ORIENTED_EDGE('',*,*,#48670,.T.);
#64297=ORIENTED_EDGE('',*,*,#48671,.T.);
#64298=ORIENTED_EDGE('',*,*,#48672,.F.);
#64299=ORIENTED_EDGE('',*,*,#48667,.F.);
#64300=ORIENTED_EDGE('',*,*,#48673,.T.);
#64301=ORIENTED_EDGE('',*,*,#48674,.T.);
#64302=ORIENTED_EDGE('',*,*,#48675,.F.);
#64303=ORIENTED_EDGE('',*,*,#48671,.F.);
#64304=ORIENTED_EDGE('',*,*,#48676,.T.);
#64305=ORIENTED_EDGE('',*,*,#48669,.T.);
#64306=ORIENTED_EDGE('',*,*,#48677,.F.);
#64307=ORIENTED_EDGE('',*,*,#48674,.F.);
#64308=ORIENTED_EDGE('',*,*,#48678,.T.);
#64309=ORIENTED_EDGE('',*,*,#48679,.T.);
#64310=ORIENTED_EDGE('',*,*,#48680,.F.);
#64311=ORIENTED_EDGE('',*,*,#48681,.F.);
#64312=ORIENTED_EDGE('',*,*,#48682,.T.);
#64313=ORIENTED_EDGE('',*,*,#48683,.T.);
#64314=ORIENTED_EDGE('',*,*,#48684,.F.);
#64315=ORIENTED_EDGE('',*,*,#48679,.F.);
#64316=ORIENTED_EDGE('',*,*,#48685,.T.);
#64317=ORIENTED_EDGE('',*,*,#48686,.T.);
#64318=ORIENTED_EDGE('',*,*,#48687,.F.);
#64319=ORIENTED_EDGE('',*,*,#48683,.F.);
#64320=ORIENTED_EDGE('',*,*,#48688,.T.);
#64321=ORIENTED_EDGE('',*,*,#48681,.T.);
#64322=ORIENTED_EDGE('',*,*,#48689,.F.);
#64323=ORIENTED_EDGE('',*,*,#48686,.F.);
#64324=ORIENTED_EDGE('',*,*,#48690,.T.);
#64325=ORIENTED_EDGE('',*,*,#48691,.T.);
#64326=ORIENTED_EDGE('',*,*,#48692,.F.);
#64327=ORIENTED_EDGE('',*,*,#48693,.F.);
#64328=ORIENTED_EDGE('',*,*,#48694,.T.);
#64329=ORIENTED_EDGE('',*,*,#48695,.T.);
#64330=ORIENTED_EDGE('',*,*,#48696,.F.);
#64331=ORIENTED_EDGE('',*,*,#48691,.F.);
#64332=ORIENTED_EDGE('',*,*,#48697,.T.);
#64333=ORIENTED_EDGE('',*,*,#48698,.T.);
#64334=ORIENTED_EDGE('',*,*,#48699,.F.);
#64335=ORIENTED_EDGE('',*,*,#48695,.F.);
#64336=ORIENTED_EDGE('',*,*,#48700,.T.);
#64337=ORIENTED_EDGE('',*,*,#48693,.T.);
#64338=ORIENTED_EDGE('',*,*,#48701,.F.);
#64339=ORIENTED_EDGE('',*,*,#48698,.F.);
#64340=ORIENTED_EDGE('',*,*,#48702,.T.);
#64341=ORIENTED_EDGE('',*,*,#48703,.T.);
#64342=ORIENTED_EDGE('',*,*,#48704,.F.);
#64343=ORIENTED_EDGE('',*,*,#48705,.F.);
#64344=ORIENTED_EDGE('',*,*,#48706,.T.);
#64345=ORIENTED_EDGE('',*,*,#48707,.T.);
#64346=ORIENTED_EDGE('',*,*,#48708,.F.);
#64347=ORIENTED_EDGE('',*,*,#48703,.F.);
#64348=ORIENTED_EDGE('',*,*,#48709,.T.);
#64349=ORIENTED_EDGE('',*,*,#48710,.T.);
#64350=ORIENTED_EDGE('',*,*,#48711,.F.);
#64351=ORIENTED_EDGE('',*,*,#48707,.F.);
#64352=ORIENTED_EDGE('',*,*,#48712,.T.);
#64353=ORIENTED_EDGE('',*,*,#48705,.T.);
#64354=ORIENTED_EDGE('',*,*,#48713,.F.);
#64355=ORIENTED_EDGE('',*,*,#48710,.F.);
#64356=ORIENTED_EDGE('',*,*,#48714,.T.);
#64357=ORIENTED_EDGE('',*,*,#48715,.T.);
#64358=ORIENTED_EDGE('',*,*,#48716,.F.);
#64359=ORIENTED_EDGE('',*,*,#48717,.F.);
#64360=ORIENTED_EDGE('',*,*,#48718,.T.);
#64361=ORIENTED_EDGE('',*,*,#48719,.T.);
#64362=ORIENTED_EDGE('',*,*,#48720,.F.);
#64363=ORIENTED_EDGE('',*,*,#48715,.F.);
#64364=ORIENTED_EDGE('',*,*,#48721,.T.);
#64365=ORIENTED_EDGE('',*,*,#48722,.T.);
#64366=ORIENTED_EDGE('',*,*,#48723,.F.);
#64367=ORIENTED_EDGE('',*,*,#48719,.F.);
#64368=ORIENTED_EDGE('',*,*,#48724,.T.);
#64369=ORIENTED_EDGE('',*,*,#48717,.T.);
#64370=ORIENTED_EDGE('',*,*,#48725,.F.);
#64371=ORIENTED_EDGE('',*,*,#48722,.F.);
#64372=ORIENTED_EDGE('',*,*,#48726,.T.);
#64373=ORIENTED_EDGE('',*,*,#48727,.T.);
#64374=ORIENTED_EDGE('',*,*,#48728,.F.);
#64375=ORIENTED_EDGE('',*,*,#48729,.F.);
#64376=ORIENTED_EDGE('',*,*,#48730,.T.);
#64377=ORIENTED_EDGE('',*,*,#48731,.T.);
#64378=ORIENTED_EDGE('',*,*,#48732,.F.);
#64379=ORIENTED_EDGE('',*,*,#48727,.F.);
#64380=ORIENTED_EDGE('',*,*,#48733,.T.);
#64381=ORIENTED_EDGE('',*,*,#48734,.T.);
#64382=ORIENTED_EDGE('',*,*,#48735,.F.);
#64383=ORIENTED_EDGE('',*,*,#48731,.F.);
#64384=ORIENTED_EDGE('',*,*,#48736,.T.);
#64385=ORIENTED_EDGE('',*,*,#48729,.T.);
#64386=ORIENTED_EDGE('',*,*,#48737,.F.);
#64387=ORIENTED_EDGE('',*,*,#48734,.F.);
#64388=ORIENTED_EDGE('',*,*,#48738,.T.);
#64389=ORIENTED_EDGE('',*,*,#48739,.T.);
#64390=ORIENTED_EDGE('',*,*,#48740,.F.);
#64391=ORIENTED_EDGE('',*,*,#48741,.F.);
#64392=ORIENTED_EDGE('',*,*,#48742,.T.);
#64393=ORIENTED_EDGE('',*,*,#48743,.T.);
#64394=ORIENTED_EDGE('',*,*,#48744,.F.);
#64395=ORIENTED_EDGE('',*,*,#48739,.F.);
#64396=ORIENTED_EDGE('',*,*,#48745,.T.);
#64397=ORIENTED_EDGE('',*,*,#48746,.T.);
#64398=ORIENTED_EDGE('',*,*,#48747,.F.);
#64399=ORIENTED_EDGE('',*,*,#48743,.F.);
#64400=ORIENTED_EDGE('',*,*,#48748,.T.);
#64401=ORIENTED_EDGE('',*,*,#48741,.T.);
#64402=ORIENTED_EDGE('',*,*,#48749,.F.);
#64403=ORIENTED_EDGE('',*,*,#48746,.F.);
#64404=ORIENTED_EDGE('',*,*,#48750,.T.);
#64405=ORIENTED_EDGE('',*,*,#48751,.T.);
#64406=ORIENTED_EDGE('',*,*,#48752,.F.);
#64407=ORIENTED_EDGE('',*,*,#48753,.F.);
#64408=ORIENTED_EDGE('',*,*,#48754,.T.);
#64409=ORIENTED_EDGE('',*,*,#48755,.T.);
#64410=ORIENTED_EDGE('',*,*,#48756,.F.);
#64411=ORIENTED_EDGE('',*,*,#48751,.F.);
#64412=ORIENTED_EDGE('',*,*,#48757,.T.);
#64413=ORIENTED_EDGE('',*,*,#48758,.T.);
#64414=ORIENTED_EDGE('',*,*,#48759,.F.);
#64415=ORIENTED_EDGE('',*,*,#48755,.F.);
#64416=ORIENTED_EDGE('',*,*,#48760,.T.);
#64417=ORIENTED_EDGE('',*,*,#48753,.T.);
#64418=ORIENTED_EDGE('',*,*,#48761,.F.);
#64419=ORIENTED_EDGE('',*,*,#48758,.F.);
#64420=ORIENTED_EDGE('',*,*,#48762,.T.);
#64421=ORIENTED_EDGE('',*,*,#48763,.T.);
#64422=ORIENTED_EDGE('',*,*,#48764,.F.);
#64423=ORIENTED_EDGE('',*,*,#48765,.F.);
#64424=ORIENTED_EDGE('',*,*,#48766,.T.);
#64425=ORIENTED_EDGE('',*,*,#48767,.T.);
#64426=ORIENTED_EDGE('',*,*,#48768,.F.);
#64427=ORIENTED_EDGE('',*,*,#48763,.F.);
#64428=ORIENTED_EDGE('',*,*,#48769,.T.);
#64429=ORIENTED_EDGE('',*,*,#48770,.T.);
#64430=ORIENTED_EDGE('',*,*,#48771,.F.);
#64431=ORIENTED_EDGE('',*,*,#48767,.F.);
#64432=ORIENTED_EDGE('',*,*,#48772,.T.);
#64433=ORIENTED_EDGE('',*,*,#48765,.T.);
#64434=ORIENTED_EDGE('',*,*,#48773,.F.);
#64435=ORIENTED_EDGE('',*,*,#48770,.F.);
#64436=ORIENTED_EDGE('',*,*,#48774,.T.);
#64437=ORIENTED_EDGE('',*,*,#48775,.T.);
#64438=ORIENTED_EDGE('',*,*,#48776,.F.);
#64439=ORIENTED_EDGE('',*,*,#48777,.F.);
#64440=ORIENTED_EDGE('',*,*,#48778,.T.);
#64441=ORIENTED_EDGE('',*,*,#48779,.T.);
#64442=ORIENTED_EDGE('',*,*,#48780,.F.);
#64443=ORIENTED_EDGE('',*,*,#48775,.F.);
#64444=ORIENTED_EDGE('',*,*,#48781,.T.);
#64445=ORIENTED_EDGE('',*,*,#48782,.T.);
#64446=ORIENTED_EDGE('',*,*,#48783,.F.);
#64447=ORIENTED_EDGE('',*,*,#48779,.F.);
#64448=ORIENTED_EDGE('',*,*,#48784,.T.);
#64449=ORIENTED_EDGE('',*,*,#48777,.T.);
#64450=ORIENTED_EDGE('',*,*,#48785,.F.);
#64451=ORIENTED_EDGE('',*,*,#48782,.F.);
#64452=ORIENTED_EDGE('',*,*,#48786,.T.);
#64453=ORIENTED_EDGE('',*,*,#48787,.T.);
#64454=ORIENTED_EDGE('',*,*,#48788,.F.);
#64455=ORIENTED_EDGE('',*,*,#48789,.F.);
#64456=ORIENTED_EDGE('',*,*,#48790,.T.);
#64457=ORIENTED_EDGE('',*,*,#48791,.T.);
#64458=ORIENTED_EDGE('',*,*,#48792,.F.);
#64459=ORIENTED_EDGE('',*,*,#48787,.F.);
#64460=ORIENTED_EDGE('',*,*,#48793,.T.);
#64461=ORIENTED_EDGE('',*,*,#48794,.T.);
#64462=ORIENTED_EDGE('',*,*,#48795,.F.);
#64463=ORIENTED_EDGE('',*,*,#48791,.F.);
#64464=ORIENTED_EDGE('',*,*,#48796,.T.);
#64465=ORIENTED_EDGE('',*,*,#48789,.T.);
#64466=ORIENTED_EDGE('',*,*,#48797,.F.);
#64467=ORIENTED_EDGE('',*,*,#48794,.F.);
#64468=ORIENTED_EDGE('',*,*,#48798,.T.);
#64469=ORIENTED_EDGE('',*,*,#48799,.T.);
#64470=ORIENTED_EDGE('',*,*,#48800,.F.);
#64471=ORIENTED_EDGE('',*,*,#48801,.F.);
#64472=ORIENTED_EDGE('',*,*,#48802,.T.);
#64473=ORIENTED_EDGE('',*,*,#48803,.T.);
#64474=ORIENTED_EDGE('',*,*,#48804,.F.);
#64475=ORIENTED_EDGE('',*,*,#48799,.F.);
#64476=ORIENTED_EDGE('',*,*,#48805,.T.);
#64477=ORIENTED_EDGE('',*,*,#48806,.T.);
#64478=ORIENTED_EDGE('',*,*,#48807,.F.);
#64479=ORIENTED_EDGE('',*,*,#48803,.F.);
#64480=ORIENTED_EDGE('',*,*,#48808,.T.);
#64481=ORIENTED_EDGE('',*,*,#48801,.T.);
#64482=ORIENTED_EDGE('',*,*,#48809,.F.);
#64483=ORIENTED_EDGE('',*,*,#48806,.F.);
#64484=ORIENTED_EDGE('',*,*,#48810,.T.);
#64485=ORIENTED_EDGE('',*,*,#48811,.T.);
#64486=ORIENTED_EDGE('',*,*,#48812,.F.);
#64487=ORIENTED_EDGE('',*,*,#48813,.F.);
#64488=ORIENTED_EDGE('',*,*,#48814,.T.);
#64489=ORIENTED_EDGE('',*,*,#48815,.T.);
#64490=ORIENTED_EDGE('',*,*,#48816,.F.);
#64491=ORIENTED_EDGE('',*,*,#48811,.F.);
#64492=ORIENTED_EDGE('',*,*,#48817,.T.);
#64493=ORIENTED_EDGE('',*,*,#48818,.T.);
#64494=ORIENTED_EDGE('',*,*,#48819,.F.);
#64495=ORIENTED_EDGE('',*,*,#48815,.F.);
#64496=ORIENTED_EDGE('',*,*,#48820,.T.);
#64497=ORIENTED_EDGE('',*,*,#48813,.T.);
#64498=ORIENTED_EDGE('',*,*,#48821,.F.);
#64499=ORIENTED_EDGE('',*,*,#48818,.F.);
#64500=ORIENTED_EDGE('',*,*,#48822,.T.);
#64501=ORIENTED_EDGE('',*,*,#48823,.T.);
#64502=ORIENTED_EDGE('',*,*,#48824,.F.);
#64503=ORIENTED_EDGE('',*,*,#48825,.F.);
#64504=ORIENTED_EDGE('',*,*,#48826,.T.);
#64505=ORIENTED_EDGE('',*,*,#48827,.T.);
#64506=ORIENTED_EDGE('',*,*,#48828,.F.);
#64507=ORIENTED_EDGE('',*,*,#48823,.F.);
#64508=ORIENTED_EDGE('',*,*,#48829,.T.);
#64509=ORIENTED_EDGE('',*,*,#48830,.T.);
#64510=ORIENTED_EDGE('',*,*,#48831,.F.);
#64511=ORIENTED_EDGE('',*,*,#48827,.F.);
#64512=ORIENTED_EDGE('',*,*,#48832,.T.);
#64513=ORIENTED_EDGE('',*,*,#48825,.T.);
#64514=ORIENTED_EDGE('',*,*,#48833,.F.);
#64515=ORIENTED_EDGE('',*,*,#48830,.F.);
#64516=ORIENTED_EDGE('',*,*,#48834,.T.);
#64517=ORIENTED_EDGE('',*,*,#48835,.T.);
#64518=ORIENTED_EDGE('',*,*,#48836,.F.);
#64519=ORIENTED_EDGE('',*,*,#48837,.F.);
#64520=ORIENTED_EDGE('',*,*,#48838,.T.);
#64521=ORIENTED_EDGE('',*,*,#48839,.T.);
#64522=ORIENTED_EDGE('',*,*,#48840,.F.);
#64523=ORIENTED_EDGE('',*,*,#48835,.F.);
#64524=ORIENTED_EDGE('',*,*,#48841,.T.);
#64525=ORIENTED_EDGE('',*,*,#48842,.T.);
#64526=ORIENTED_EDGE('',*,*,#48843,.F.);
#64527=ORIENTED_EDGE('',*,*,#48839,.F.);
#64528=ORIENTED_EDGE('',*,*,#48844,.T.);
#64529=ORIENTED_EDGE('',*,*,#48837,.T.);
#64530=ORIENTED_EDGE('',*,*,#48845,.F.);
#64531=ORIENTED_EDGE('',*,*,#48842,.F.);
#64532=ORIENTED_EDGE('',*,*,#48846,.T.);
#64533=ORIENTED_EDGE('',*,*,#48847,.T.);
#64534=ORIENTED_EDGE('',*,*,#48848,.F.);
#64535=ORIENTED_EDGE('',*,*,#48849,.F.);
#64536=ORIENTED_EDGE('',*,*,#48850,.T.);
#64537=ORIENTED_EDGE('',*,*,#48851,.T.);
#64538=ORIENTED_EDGE('',*,*,#48852,.F.);
#64539=ORIENTED_EDGE('',*,*,#48847,.F.);
#64540=ORIENTED_EDGE('',*,*,#48853,.T.);
#64541=ORIENTED_EDGE('',*,*,#48854,.T.);
#64542=ORIENTED_EDGE('',*,*,#48855,.F.);
#64543=ORIENTED_EDGE('',*,*,#48851,.F.);
#64544=ORIENTED_EDGE('',*,*,#48856,.T.);
#64545=ORIENTED_EDGE('',*,*,#48849,.T.);
#64546=ORIENTED_EDGE('',*,*,#48857,.F.);
#64547=ORIENTED_EDGE('',*,*,#48854,.F.);
#64548=ORIENTED_EDGE('',*,*,#48858,.T.);
#64549=ORIENTED_EDGE('',*,*,#48859,.T.);
#64550=ORIENTED_EDGE('',*,*,#48860,.F.);
#64551=ORIENTED_EDGE('',*,*,#48861,.F.);
#64552=ORIENTED_EDGE('',*,*,#48862,.T.);
#64553=ORIENTED_EDGE('',*,*,#48863,.T.);
#64554=ORIENTED_EDGE('',*,*,#48864,.F.);
#64555=ORIENTED_EDGE('',*,*,#48859,.F.);
#64556=ORIENTED_EDGE('',*,*,#48865,.T.);
#64557=ORIENTED_EDGE('',*,*,#48866,.T.);
#64558=ORIENTED_EDGE('',*,*,#48867,.F.);
#64559=ORIENTED_EDGE('',*,*,#48863,.F.);
#64560=ORIENTED_EDGE('',*,*,#48868,.T.);
#64561=ORIENTED_EDGE('',*,*,#48861,.T.);
#64562=ORIENTED_EDGE('',*,*,#48869,.F.);
#64563=ORIENTED_EDGE('',*,*,#48866,.F.);
#64564=ORIENTED_EDGE('',*,*,#48870,.T.);
#64565=ORIENTED_EDGE('',*,*,#48871,.T.);
#64566=ORIENTED_EDGE('',*,*,#48872,.F.);
#64567=ORIENTED_EDGE('',*,*,#48873,.F.);
#64568=ORIENTED_EDGE('',*,*,#48874,.T.);
#64569=ORIENTED_EDGE('',*,*,#48875,.T.);
#64570=ORIENTED_EDGE('',*,*,#48876,.F.);
#64571=ORIENTED_EDGE('',*,*,#48871,.F.);
#64572=ORIENTED_EDGE('',*,*,#48877,.T.);
#64573=ORIENTED_EDGE('',*,*,#48878,.T.);
#64574=ORIENTED_EDGE('',*,*,#48879,.F.);
#64575=ORIENTED_EDGE('',*,*,#48875,.F.);
#64576=ORIENTED_EDGE('',*,*,#48880,.T.);
#64577=ORIENTED_EDGE('',*,*,#48873,.T.);
#64578=ORIENTED_EDGE('',*,*,#48881,.F.);
#64579=ORIENTED_EDGE('',*,*,#48878,.F.);
#64580=ORIENTED_EDGE('',*,*,#48882,.T.);
#64581=ORIENTED_EDGE('',*,*,#48883,.T.);
#64582=ORIENTED_EDGE('',*,*,#48884,.F.);
#64583=ORIENTED_EDGE('',*,*,#48885,.F.);
#64584=ORIENTED_EDGE('',*,*,#48886,.T.);
#64585=ORIENTED_EDGE('',*,*,#48887,.T.);
#64586=ORIENTED_EDGE('',*,*,#48888,.F.);
#64587=ORIENTED_EDGE('',*,*,#48883,.F.);
#64588=ORIENTED_EDGE('',*,*,#48889,.T.);
#64589=ORIENTED_EDGE('',*,*,#48890,.T.);
#64590=ORIENTED_EDGE('',*,*,#48891,.F.);
#64591=ORIENTED_EDGE('',*,*,#48887,.F.);
#64592=ORIENTED_EDGE('',*,*,#48892,.T.);
#64593=ORIENTED_EDGE('',*,*,#48885,.T.);
#64594=ORIENTED_EDGE('',*,*,#48893,.F.);
#64595=ORIENTED_EDGE('',*,*,#48890,.F.);
#64596=ORIENTED_EDGE('',*,*,#48894,.T.);
#64597=ORIENTED_EDGE('',*,*,#48895,.T.);
#64598=ORIENTED_EDGE('',*,*,#48896,.F.);
#64599=ORIENTED_EDGE('',*,*,#48897,.F.);
#64600=ORIENTED_EDGE('',*,*,#48898,.T.);
#64601=ORIENTED_EDGE('',*,*,#48899,.T.);
#64602=ORIENTED_EDGE('',*,*,#48900,.F.);
#64603=ORIENTED_EDGE('',*,*,#48895,.F.);
#64604=ORIENTED_EDGE('',*,*,#48901,.T.);
#64605=ORIENTED_EDGE('',*,*,#48902,.T.);
#64606=ORIENTED_EDGE('',*,*,#48903,.F.);
#64607=ORIENTED_EDGE('',*,*,#48899,.F.);
#64608=ORIENTED_EDGE('',*,*,#48904,.T.);
#64609=ORIENTED_EDGE('',*,*,#48897,.T.);
#64610=ORIENTED_EDGE('',*,*,#48905,.F.);
#64611=ORIENTED_EDGE('',*,*,#48902,.F.);
#64612=ORIENTED_EDGE('',*,*,#48906,.T.);
#64613=ORIENTED_EDGE('',*,*,#48907,.T.);
#64614=ORIENTED_EDGE('',*,*,#48908,.F.);
#64615=ORIENTED_EDGE('',*,*,#48909,.F.);
#64616=ORIENTED_EDGE('',*,*,#48910,.T.);
#64617=ORIENTED_EDGE('',*,*,#48911,.T.);
#64618=ORIENTED_EDGE('',*,*,#48912,.F.);
#64619=ORIENTED_EDGE('',*,*,#48907,.F.);
#64620=ORIENTED_EDGE('',*,*,#48913,.T.);
#64621=ORIENTED_EDGE('',*,*,#48914,.T.);
#64622=ORIENTED_EDGE('',*,*,#48915,.F.);
#64623=ORIENTED_EDGE('',*,*,#48911,.F.);
#64624=ORIENTED_EDGE('',*,*,#48916,.T.);
#64625=ORIENTED_EDGE('',*,*,#48909,.T.);
#64626=ORIENTED_EDGE('',*,*,#48917,.F.);
#64627=ORIENTED_EDGE('',*,*,#48914,.F.);
#64628=ORIENTED_EDGE('',*,*,#48918,.T.);
#64629=ORIENTED_EDGE('',*,*,#48919,.T.);
#64630=ORIENTED_EDGE('',*,*,#48920,.F.);
#64631=ORIENTED_EDGE('',*,*,#48921,.F.);
#64632=ORIENTED_EDGE('',*,*,#48922,.T.);
#64633=ORIENTED_EDGE('',*,*,#48923,.T.);
#64634=ORIENTED_EDGE('',*,*,#48924,.F.);
#64635=ORIENTED_EDGE('',*,*,#48919,.F.);
#64636=ORIENTED_EDGE('',*,*,#48925,.T.);
#64637=ORIENTED_EDGE('',*,*,#48926,.T.);
#64638=ORIENTED_EDGE('',*,*,#48927,.F.);
#64639=ORIENTED_EDGE('',*,*,#48923,.F.);
#64640=ORIENTED_EDGE('',*,*,#48928,.T.);
#64641=ORIENTED_EDGE('',*,*,#48921,.T.);
#64642=ORIENTED_EDGE('',*,*,#48929,.F.);
#64643=ORIENTED_EDGE('',*,*,#48926,.F.);
#64644=ORIENTED_EDGE('',*,*,#48930,.T.);
#64645=ORIENTED_EDGE('',*,*,#48931,.T.);
#64646=ORIENTED_EDGE('',*,*,#48932,.F.);
#64647=ORIENTED_EDGE('',*,*,#48933,.F.);
#64648=ORIENTED_EDGE('',*,*,#48934,.T.);
#64649=ORIENTED_EDGE('',*,*,#48935,.T.);
#64650=ORIENTED_EDGE('',*,*,#48936,.F.);
#64651=ORIENTED_EDGE('',*,*,#48931,.F.);
#64652=ORIENTED_EDGE('',*,*,#48937,.T.);
#64653=ORIENTED_EDGE('',*,*,#48938,.T.);
#64654=ORIENTED_EDGE('',*,*,#48939,.F.);
#64655=ORIENTED_EDGE('',*,*,#48935,.F.);
#64656=ORIENTED_EDGE('',*,*,#48940,.T.);
#64657=ORIENTED_EDGE('',*,*,#48933,.T.);
#64658=ORIENTED_EDGE('',*,*,#48941,.F.);
#64659=ORIENTED_EDGE('',*,*,#48938,.F.);
#64660=ORIENTED_EDGE('',*,*,#48942,.T.);
#64661=ORIENTED_EDGE('',*,*,#48943,.T.);
#64662=ORIENTED_EDGE('',*,*,#48944,.F.);
#64663=ORIENTED_EDGE('',*,*,#48945,.F.);
#64664=ORIENTED_EDGE('',*,*,#48946,.T.);
#64665=ORIENTED_EDGE('',*,*,#48947,.T.);
#64666=ORIENTED_EDGE('',*,*,#48948,.F.);
#64667=ORIENTED_EDGE('',*,*,#48943,.F.);
#64668=ORIENTED_EDGE('',*,*,#48949,.T.);
#64669=ORIENTED_EDGE('',*,*,#48950,.T.);
#64670=ORIENTED_EDGE('',*,*,#48951,.F.);
#64671=ORIENTED_EDGE('',*,*,#48947,.F.);
#64672=ORIENTED_EDGE('',*,*,#48952,.T.);
#64673=ORIENTED_EDGE('',*,*,#48945,.T.);
#64674=ORIENTED_EDGE('',*,*,#48953,.F.);
#64675=ORIENTED_EDGE('',*,*,#48950,.F.);
#64676=ORIENTED_EDGE('',*,*,#48954,.T.);
#64677=ORIENTED_EDGE('',*,*,#48955,.T.);
#64678=ORIENTED_EDGE('',*,*,#48956,.F.);
#64679=ORIENTED_EDGE('',*,*,#48957,.F.);
#64680=ORIENTED_EDGE('',*,*,#48958,.T.);
#64681=ORIENTED_EDGE('',*,*,#48959,.T.);
#64682=ORIENTED_EDGE('',*,*,#48960,.F.);
#64683=ORIENTED_EDGE('',*,*,#48955,.F.);
#64684=ORIENTED_EDGE('',*,*,#48961,.T.);
#64685=ORIENTED_EDGE('',*,*,#48962,.T.);
#64686=ORIENTED_EDGE('',*,*,#48963,.F.);
#64687=ORIENTED_EDGE('',*,*,#48959,.F.);
#64688=ORIENTED_EDGE('',*,*,#48964,.T.);
#64689=ORIENTED_EDGE('',*,*,#48957,.T.);
#64690=ORIENTED_EDGE('',*,*,#48965,.F.);
#64691=ORIENTED_EDGE('',*,*,#48962,.F.);
#64692=ORIENTED_EDGE('',*,*,#48966,.T.);
#64693=ORIENTED_EDGE('',*,*,#48967,.T.);
#64694=ORIENTED_EDGE('',*,*,#48968,.F.);
#64695=ORIENTED_EDGE('',*,*,#48969,.F.);
#64696=ORIENTED_EDGE('',*,*,#48970,.T.);
#64697=ORIENTED_EDGE('',*,*,#48971,.T.);
#64698=ORIENTED_EDGE('',*,*,#48972,.F.);
#64699=ORIENTED_EDGE('',*,*,#48967,.F.);
#64700=ORIENTED_EDGE('',*,*,#48973,.T.);
#64701=ORIENTED_EDGE('',*,*,#48974,.T.);
#64702=ORIENTED_EDGE('',*,*,#48975,.F.);
#64703=ORIENTED_EDGE('',*,*,#48971,.F.);
#64704=ORIENTED_EDGE('',*,*,#48976,.T.);
#64705=ORIENTED_EDGE('',*,*,#48969,.T.);
#64706=ORIENTED_EDGE('',*,*,#48977,.F.);
#64707=ORIENTED_EDGE('',*,*,#48974,.F.);
#64708=ORIENTED_EDGE('',*,*,#48978,.T.);
#64709=ORIENTED_EDGE('',*,*,#48979,.T.);
#64710=ORIENTED_EDGE('',*,*,#48980,.F.);
#64711=ORIENTED_EDGE('',*,*,#48981,.F.);
#64712=ORIENTED_EDGE('',*,*,#48982,.T.);
#64713=ORIENTED_EDGE('',*,*,#48983,.T.);
#64714=ORIENTED_EDGE('',*,*,#48984,.F.);
#64715=ORIENTED_EDGE('',*,*,#48979,.F.);
#64716=ORIENTED_EDGE('',*,*,#48985,.T.);
#64717=ORIENTED_EDGE('',*,*,#48986,.T.);
#64718=ORIENTED_EDGE('',*,*,#48987,.F.);
#64719=ORIENTED_EDGE('',*,*,#48983,.F.);
#64720=ORIENTED_EDGE('',*,*,#48988,.T.);
#64721=ORIENTED_EDGE('',*,*,#48981,.T.);
#64722=ORIENTED_EDGE('',*,*,#48989,.F.);
#64723=ORIENTED_EDGE('',*,*,#48986,.F.);
#64724=ORIENTED_EDGE('',*,*,#48990,.T.);
#64725=ORIENTED_EDGE('',*,*,#48991,.T.);
#64726=ORIENTED_EDGE('',*,*,#48992,.F.);
#64727=ORIENTED_EDGE('',*,*,#48993,.F.);
#64728=ORIENTED_EDGE('',*,*,#48994,.T.);
#64729=ORIENTED_EDGE('',*,*,#48995,.T.);
#64730=ORIENTED_EDGE('',*,*,#48996,.F.);
#64731=ORIENTED_EDGE('',*,*,#48991,.F.);
#64732=ORIENTED_EDGE('',*,*,#48997,.T.);
#64733=ORIENTED_EDGE('',*,*,#48998,.T.);
#64734=ORIENTED_EDGE('',*,*,#48999,.F.);
#64735=ORIENTED_EDGE('',*,*,#48995,.F.);
#64736=ORIENTED_EDGE('',*,*,#49000,.T.);
#64737=ORIENTED_EDGE('',*,*,#48993,.T.);
#64738=ORIENTED_EDGE('',*,*,#49001,.F.);
#64739=ORIENTED_EDGE('',*,*,#48998,.F.);
#64740=ORIENTED_EDGE('',*,*,#49002,.T.);
#64741=ORIENTED_EDGE('',*,*,#49003,.T.);
#64742=ORIENTED_EDGE('',*,*,#49004,.F.);
#64743=ORIENTED_EDGE('',*,*,#49005,.F.);
#64744=ORIENTED_EDGE('',*,*,#49006,.T.);
#64745=ORIENTED_EDGE('',*,*,#49007,.T.);
#64746=ORIENTED_EDGE('',*,*,#49008,.F.);
#64747=ORIENTED_EDGE('',*,*,#49003,.F.);
#64748=ORIENTED_EDGE('',*,*,#49009,.T.);
#64749=ORIENTED_EDGE('',*,*,#49010,.T.);
#64750=ORIENTED_EDGE('',*,*,#49011,.F.);
#64751=ORIENTED_EDGE('',*,*,#49007,.F.);
#64752=ORIENTED_EDGE('',*,*,#49012,.T.);
#64753=ORIENTED_EDGE('',*,*,#49005,.T.);
#64754=ORIENTED_EDGE('',*,*,#49013,.F.);
#64755=ORIENTED_EDGE('',*,*,#49010,.F.);
#64756=ORIENTED_EDGE('',*,*,#49014,.T.);
#64757=ORIENTED_EDGE('',*,*,#49015,.T.);
#64758=ORIENTED_EDGE('',*,*,#49016,.F.);
#64759=ORIENTED_EDGE('',*,*,#49017,.F.);
#64760=ORIENTED_EDGE('',*,*,#49018,.T.);
#64761=ORIENTED_EDGE('',*,*,#49019,.T.);
#64762=ORIENTED_EDGE('',*,*,#49020,.F.);
#64763=ORIENTED_EDGE('',*,*,#49015,.F.);
#64764=ORIENTED_EDGE('',*,*,#49021,.T.);
#64765=ORIENTED_EDGE('',*,*,#49022,.T.);
#64766=ORIENTED_EDGE('',*,*,#49023,.F.);
#64767=ORIENTED_EDGE('',*,*,#49019,.F.);
#64768=ORIENTED_EDGE('',*,*,#49024,.T.);
#64769=ORIENTED_EDGE('',*,*,#49017,.T.);
#64770=ORIENTED_EDGE('',*,*,#49025,.F.);
#64771=ORIENTED_EDGE('',*,*,#49022,.F.);
#64772=ORIENTED_EDGE('',*,*,#49026,.T.);
#64773=ORIENTED_EDGE('',*,*,#49027,.T.);
#64774=ORIENTED_EDGE('',*,*,#49028,.F.);
#64775=ORIENTED_EDGE('',*,*,#49029,.F.);
#64776=ORIENTED_EDGE('',*,*,#49030,.T.);
#64777=ORIENTED_EDGE('',*,*,#49031,.T.);
#64778=ORIENTED_EDGE('',*,*,#49032,.F.);
#64779=ORIENTED_EDGE('',*,*,#49027,.F.);
#64780=ORIENTED_EDGE('',*,*,#49033,.T.);
#64781=ORIENTED_EDGE('',*,*,#49034,.T.);
#64782=ORIENTED_EDGE('',*,*,#49035,.F.);
#64783=ORIENTED_EDGE('',*,*,#49031,.F.);
#64784=ORIENTED_EDGE('',*,*,#49036,.T.);
#64785=ORIENTED_EDGE('',*,*,#49029,.T.);
#64786=ORIENTED_EDGE('',*,*,#49037,.F.);
#64787=ORIENTED_EDGE('',*,*,#49034,.F.);
#64788=ORIENTED_EDGE('',*,*,#49038,.T.);
#64789=ORIENTED_EDGE('',*,*,#49039,.T.);
#64790=ORIENTED_EDGE('',*,*,#49040,.F.);
#64791=ORIENTED_EDGE('',*,*,#49041,.F.);
#64792=ORIENTED_EDGE('',*,*,#49042,.T.);
#64793=ORIENTED_EDGE('',*,*,#49043,.T.);
#64794=ORIENTED_EDGE('',*,*,#49044,.F.);
#64795=ORIENTED_EDGE('',*,*,#49039,.F.);
#64796=ORIENTED_EDGE('',*,*,#49045,.T.);
#64797=ORIENTED_EDGE('',*,*,#49046,.T.);
#64798=ORIENTED_EDGE('',*,*,#49047,.F.);
#64799=ORIENTED_EDGE('',*,*,#49043,.F.);
#64800=ORIENTED_EDGE('',*,*,#49048,.T.);
#64801=ORIENTED_EDGE('',*,*,#49041,.T.);
#64802=ORIENTED_EDGE('',*,*,#49049,.F.);
#64803=ORIENTED_EDGE('',*,*,#49046,.F.);
#64804=ORIENTED_EDGE('',*,*,#49050,.T.);
#64805=ORIENTED_EDGE('',*,*,#49051,.T.);
#64806=ORIENTED_EDGE('',*,*,#49052,.F.);
#64807=ORIENTED_EDGE('',*,*,#49053,.F.);
#64808=ORIENTED_EDGE('',*,*,#49054,.T.);
#64809=ORIENTED_EDGE('',*,*,#49055,.T.);
#64810=ORIENTED_EDGE('',*,*,#49056,.F.);
#64811=ORIENTED_EDGE('',*,*,#49051,.F.);
#64812=ORIENTED_EDGE('',*,*,#49057,.T.);
#64813=ORIENTED_EDGE('',*,*,#49058,.T.);
#64814=ORIENTED_EDGE('',*,*,#49059,.F.);
#64815=ORIENTED_EDGE('',*,*,#49055,.F.);
#64816=ORIENTED_EDGE('',*,*,#49060,.T.);
#64817=ORIENTED_EDGE('',*,*,#49053,.T.);
#64818=ORIENTED_EDGE('',*,*,#49061,.F.);
#64819=ORIENTED_EDGE('',*,*,#49058,.F.);
#64820=ORIENTED_EDGE('',*,*,#49062,.T.);
#64821=ORIENTED_EDGE('',*,*,#49063,.T.);
#64822=ORIENTED_EDGE('',*,*,#49064,.F.);
#64823=ORIENTED_EDGE('',*,*,#49065,.F.);
#64824=ORIENTED_EDGE('',*,*,#49066,.T.);
#64825=ORIENTED_EDGE('',*,*,#49067,.T.);
#64826=ORIENTED_EDGE('',*,*,#49068,.F.);
#64827=ORIENTED_EDGE('',*,*,#49063,.F.);
#64828=ORIENTED_EDGE('',*,*,#49069,.T.);
#64829=ORIENTED_EDGE('',*,*,#49070,.T.);
#64830=ORIENTED_EDGE('',*,*,#49071,.F.);
#64831=ORIENTED_EDGE('',*,*,#49067,.F.);
#64832=ORIENTED_EDGE('',*,*,#49072,.T.);
#64833=ORIENTED_EDGE('',*,*,#49065,.T.);
#64834=ORIENTED_EDGE('',*,*,#49073,.F.);
#64835=ORIENTED_EDGE('',*,*,#49070,.F.);
#64836=ORIENTED_EDGE('',*,*,#49074,.T.);
#64837=ORIENTED_EDGE('',*,*,#49075,.T.);
#64838=ORIENTED_EDGE('',*,*,#49076,.F.);
#64839=ORIENTED_EDGE('',*,*,#49077,.F.);
#64840=ORIENTED_EDGE('',*,*,#49078,.T.);
#64841=ORIENTED_EDGE('',*,*,#49079,.T.);
#64842=ORIENTED_EDGE('',*,*,#49080,.F.);
#64843=ORIENTED_EDGE('',*,*,#49075,.F.);
#64844=ORIENTED_EDGE('',*,*,#49081,.T.);
#64845=ORIENTED_EDGE('',*,*,#49082,.T.);
#64846=ORIENTED_EDGE('',*,*,#49083,.F.);
#64847=ORIENTED_EDGE('',*,*,#49079,.F.);
#64848=ORIENTED_EDGE('',*,*,#49084,.T.);
#64849=ORIENTED_EDGE('',*,*,#49077,.T.);
#64850=ORIENTED_EDGE('',*,*,#49085,.F.);
#64851=ORIENTED_EDGE('',*,*,#49082,.F.);
#64852=ORIENTED_EDGE('',*,*,#49086,.T.);
#64853=ORIENTED_EDGE('',*,*,#49087,.T.);
#64854=ORIENTED_EDGE('',*,*,#49088,.F.);
#64855=ORIENTED_EDGE('',*,*,#49089,.F.);
#64856=ORIENTED_EDGE('',*,*,#49090,.T.);
#64857=ORIENTED_EDGE('',*,*,#49091,.T.);
#64858=ORIENTED_EDGE('',*,*,#49092,.F.);
#64859=ORIENTED_EDGE('',*,*,#49087,.F.);
#64860=ORIENTED_EDGE('',*,*,#49093,.T.);
#64861=ORIENTED_EDGE('',*,*,#49094,.T.);
#64862=ORIENTED_EDGE('',*,*,#49095,.F.);
#64863=ORIENTED_EDGE('',*,*,#49091,.F.);
#64864=ORIENTED_EDGE('',*,*,#49096,.T.);
#64865=ORIENTED_EDGE('',*,*,#49089,.T.);
#64866=ORIENTED_EDGE('',*,*,#49097,.F.);
#64867=ORIENTED_EDGE('',*,*,#49094,.F.);
#64868=ORIENTED_EDGE('',*,*,#49098,.T.);
#64869=ORIENTED_EDGE('',*,*,#49099,.T.);
#64870=ORIENTED_EDGE('',*,*,#49100,.F.);
#64871=ORIENTED_EDGE('',*,*,#49101,.F.);
#64872=ORIENTED_EDGE('',*,*,#49102,.T.);
#64873=ORIENTED_EDGE('',*,*,#49103,.T.);
#64874=ORIENTED_EDGE('',*,*,#49104,.F.);
#64875=ORIENTED_EDGE('',*,*,#49099,.F.);
#64876=ORIENTED_EDGE('',*,*,#49105,.T.);
#64877=ORIENTED_EDGE('',*,*,#49106,.T.);
#64878=ORIENTED_EDGE('',*,*,#49107,.F.);
#64879=ORIENTED_EDGE('',*,*,#49103,.F.);
#64880=ORIENTED_EDGE('',*,*,#49108,.T.);
#64881=ORIENTED_EDGE('',*,*,#49101,.T.);
#64882=ORIENTED_EDGE('',*,*,#49109,.F.);
#64883=ORIENTED_EDGE('',*,*,#49106,.F.);
#64884=ORIENTED_EDGE('',*,*,#49110,.T.);
#64885=ORIENTED_EDGE('',*,*,#49111,.T.);
#64886=ORIENTED_EDGE('',*,*,#49112,.F.);
#64887=ORIENTED_EDGE('',*,*,#49113,.F.);
#64888=ORIENTED_EDGE('',*,*,#49114,.T.);
#64889=ORIENTED_EDGE('',*,*,#49115,.T.);
#64890=ORIENTED_EDGE('',*,*,#49116,.F.);
#64891=ORIENTED_EDGE('',*,*,#49111,.F.);
#64892=ORIENTED_EDGE('',*,*,#49117,.T.);
#64893=ORIENTED_EDGE('',*,*,#49118,.T.);
#64894=ORIENTED_EDGE('',*,*,#49119,.F.);
#64895=ORIENTED_EDGE('',*,*,#49115,.F.);
#64896=ORIENTED_EDGE('',*,*,#49120,.T.);
#64897=ORIENTED_EDGE('',*,*,#49113,.T.);
#64898=ORIENTED_EDGE('',*,*,#49121,.F.);
#64899=ORIENTED_EDGE('',*,*,#49118,.F.);
#64900=ORIENTED_EDGE('',*,*,#49122,.T.);
#64901=ORIENTED_EDGE('',*,*,#49123,.T.);
#64902=ORIENTED_EDGE('',*,*,#49124,.F.);
#64903=ORIENTED_EDGE('',*,*,#49125,.F.);
#64904=ORIENTED_EDGE('',*,*,#49126,.T.);
#64905=ORIENTED_EDGE('',*,*,#49127,.T.);
#64906=ORIENTED_EDGE('',*,*,#49128,.F.);
#64907=ORIENTED_EDGE('',*,*,#49123,.F.);
#64908=ORIENTED_EDGE('',*,*,#49129,.T.);
#64909=ORIENTED_EDGE('',*,*,#49130,.T.);
#64910=ORIENTED_EDGE('',*,*,#49131,.F.);
#64911=ORIENTED_EDGE('',*,*,#49127,.F.);
#64912=ORIENTED_EDGE('',*,*,#49132,.T.);
#64913=ORIENTED_EDGE('',*,*,#49125,.T.);
#64914=ORIENTED_EDGE('',*,*,#49133,.F.);
#64915=ORIENTED_EDGE('',*,*,#49130,.F.);
#64916=ORIENTED_EDGE('',*,*,#49134,.T.);
#64917=ORIENTED_EDGE('',*,*,#49135,.T.);
#64918=ORIENTED_EDGE('',*,*,#49136,.F.);
#64919=ORIENTED_EDGE('',*,*,#49137,.F.);
#64920=ORIENTED_EDGE('',*,*,#49138,.T.);
#64921=ORIENTED_EDGE('',*,*,#49139,.T.);
#64922=ORIENTED_EDGE('',*,*,#49140,.F.);
#64923=ORIENTED_EDGE('',*,*,#49135,.F.);
#64924=ORIENTED_EDGE('',*,*,#49141,.T.);
#64925=ORIENTED_EDGE('',*,*,#49142,.T.);
#64926=ORIENTED_EDGE('',*,*,#49143,.F.);
#64927=ORIENTED_EDGE('',*,*,#49139,.F.);
#64928=ORIENTED_EDGE('',*,*,#49144,.T.);
#64929=ORIENTED_EDGE('',*,*,#49137,.T.);
#64930=ORIENTED_EDGE('',*,*,#49145,.F.);
#64931=ORIENTED_EDGE('',*,*,#49142,.F.);
#64932=ORIENTED_EDGE('',*,*,#49146,.T.);
#64933=ORIENTED_EDGE('',*,*,#49147,.T.);
#64934=ORIENTED_EDGE('',*,*,#49148,.F.);
#64935=ORIENTED_EDGE('',*,*,#49149,.F.);
#64936=ORIENTED_EDGE('',*,*,#49150,.T.);
#64937=ORIENTED_EDGE('',*,*,#49151,.T.);
#64938=ORIENTED_EDGE('',*,*,#49152,.F.);
#64939=ORIENTED_EDGE('',*,*,#49147,.F.);
#64940=ORIENTED_EDGE('',*,*,#49153,.T.);
#64941=ORIENTED_EDGE('',*,*,#49154,.T.);
#64942=ORIENTED_EDGE('',*,*,#49155,.F.);
#64943=ORIENTED_EDGE('',*,*,#49151,.F.);
#64944=ORIENTED_EDGE('',*,*,#49156,.T.);
#64945=ORIENTED_EDGE('',*,*,#49149,.T.);
#64946=ORIENTED_EDGE('',*,*,#49157,.F.);
#64947=ORIENTED_EDGE('',*,*,#49154,.F.);
#64948=ORIENTED_EDGE('',*,*,#49158,.T.);
#64949=ORIENTED_EDGE('',*,*,#49159,.T.);
#64950=ORIENTED_EDGE('',*,*,#49160,.F.);
#64951=ORIENTED_EDGE('',*,*,#49161,.F.);
#64952=ORIENTED_EDGE('',*,*,#49162,.T.);
#64953=ORIENTED_EDGE('',*,*,#49163,.T.);
#64954=ORIENTED_EDGE('',*,*,#49164,.F.);
#64955=ORIENTED_EDGE('',*,*,#49159,.F.);
#64956=ORIENTED_EDGE('',*,*,#49165,.T.);
#64957=ORIENTED_EDGE('',*,*,#49166,.T.);
#64958=ORIENTED_EDGE('',*,*,#49167,.F.);
#64959=ORIENTED_EDGE('',*,*,#49163,.F.);
#64960=ORIENTED_EDGE('',*,*,#49168,.T.);
#64961=ORIENTED_EDGE('',*,*,#49161,.T.);
#64962=ORIENTED_EDGE('',*,*,#49169,.F.);
#64963=ORIENTED_EDGE('',*,*,#49166,.F.);
#64964=ORIENTED_EDGE('',*,*,#49170,.T.);
#64965=ORIENTED_EDGE('',*,*,#49171,.T.);
#64966=ORIENTED_EDGE('',*,*,#49172,.F.);
#64967=ORIENTED_EDGE('',*,*,#49173,.F.);
#64968=ORIENTED_EDGE('',*,*,#49174,.T.);
#64969=ORIENTED_EDGE('',*,*,#49175,.T.);
#64970=ORIENTED_EDGE('',*,*,#49176,.F.);
#64971=ORIENTED_EDGE('',*,*,#49171,.F.);
#64972=ORIENTED_EDGE('',*,*,#49177,.T.);
#64973=ORIENTED_EDGE('',*,*,#49178,.T.);
#64974=ORIENTED_EDGE('',*,*,#49179,.F.);
#64975=ORIENTED_EDGE('',*,*,#49175,.F.);
#64976=ORIENTED_EDGE('',*,*,#49180,.T.);
#64977=ORIENTED_EDGE('',*,*,#49173,.T.);
#64978=ORIENTED_EDGE('',*,*,#49181,.F.);
#64979=ORIENTED_EDGE('',*,*,#49178,.F.);
#64980=ORIENTED_EDGE('',*,*,#49182,.T.);
#64981=ORIENTED_EDGE('',*,*,#49183,.T.);
#64982=ORIENTED_EDGE('',*,*,#49184,.F.);
#64983=ORIENTED_EDGE('',*,*,#49185,.F.);
#64984=ORIENTED_EDGE('',*,*,#49186,.T.);
#64985=ORIENTED_EDGE('',*,*,#49187,.T.);
#64986=ORIENTED_EDGE('',*,*,#49188,.F.);
#64987=ORIENTED_EDGE('',*,*,#49183,.F.);
#64988=ORIENTED_EDGE('',*,*,#49189,.T.);
#64989=ORIENTED_EDGE('',*,*,#49190,.T.);
#64990=ORIENTED_EDGE('',*,*,#49191,.F.);
#64991=ORIENTED_EDGE('',*,*,#49187,.F.);
#64992=ORIENTED_EDGE('',*,*,#49192,.T.);
#64993=ORIENTED_EDGE('',*,*,#49185,.T.);
#64994=ORIENTED_EDGE('',*,*,#49193,.F.);
#64995=ORIENTED_EDGE('',*,*,#49190,.F.);
#64996=ORIENTED_EDGE('',*,*,#49194,.T.);
#64997=ORIENTED_EDGE('',*,*,#49195,.T.);
#64998=ORIENTED_EDGE('',*,*,#49196,.F.);
#64999=ORIENTED_EDGE('',*,*,#49197,.F.);
#65000=ORIENTED_EDGE('',*,*,#49198,.T.);
#65001=ORIENTED_EDGE('',*,*,#49199,.T.);
#65002=ORIENTED_EDGE('',*,*,#49200,.F.);
#65003=ORIENTED_EDGE('',*,*,#49195,.F.);
#65004=ORIENTED_EDGE('',*,*,#49201,.T.);
#65005=ORIENTED_EDGE('',*,*,#49202,.T.);
#65006=ORIENTED_EDGE('',*,*,#49203,.F.);
#65007=ORIENTED_EDGE('',*,*,#49199,.F.);
#65008=ORIENTED_EDGE('',*,*,#49204,.T.);
#65009=ORIENTED_EDGE('',*,*,#49197,.T.);
#65010=ORIENTED_EDGE('',*,*,#49205,.F.);
#65011=ORIENTED_EDGE('',*,*,#49202,.F.);
#65012=ORIENTED_EDGE('',*,*,#49206,.T.);
#65013=ORIENTED_EDGE('',*,*,#49207,.T.);
#65014=ORIENTED_EDGE('',*,*,#49208,.F.);
#65015=ORIENTED_EDGE('',*,*,#49209,.F.);
#65016=ORIENTED_EDGE('',*,*,#49210,.T.);
#65017=ORIENTED_EDGE('',*,*,#49211,.T.);
#65018=ORIENTED_EDGE('',*,*,#49212,.F.);
#65019=ORIENTED_EDGE('',*,*,#49207,.F.);
#65020=ORIENTED_EDGE('',*,*,#49213,.T.);
#65021=ORIENTED_EDGE('',*,*,#49214,.T.);
#65022=ORIENTED_EDGE('',*,*,#49215,.F.);
#65023=ORIENTED_EDGE('',*,*,#49211,.F.);
#65024=ORIENTED_EDGE('',*,*,#49216,.T.);
#65025=ORIENTED_EDGE('',*,*,#49209,.T.);
#65026=ORIENTED_EDGE('',*,*,#49217,.F.);
#65027=ORIENTED_EDGE('',*,*,#49214,.F.);
#65028=ORIENTED_EDGE('',*,*,#49218,.T.);
#65029=ORIENTED_EDGE('',*,*,#49219,.T.);
#65030=ORIENTED_EDGE('',*,*,#49220,.F.);
#65031=ORIENTED_EDGE('',*,*,#49221,.F.);
#65032=ORIENTED_EDGE('',*,*,#49222,.T.);
#65033=ORIENTED_EDGE('',*,*,#49223,.T.);
#65034=ORIENTED_EDGE('',*,*,#49224,.F.);
#65035=ORIENTED_EDGE('',*,*,#49219,.F.);
#65036=ORIENTED_EDGE('',*,*,#49225,.T.);
#65037=ORIENTED_EDGE('',*,*,#49226,.T.);
#65038=ORIENTED_EDGE('',*,*,#49227,.F.);
#65039=ORIENTED_EDGE('',*,*,#49223,.F.);
#65040=ORIENTED_EDGE('',*,*,#49228,.T.);
#65041=ORIENTED_EDGE('',*,*,#49221,.T.);
#65042=ORIENTED_EDGE('',*,*,#49229,.F.);
#65043=ORIENTED_EDGE('',*,*,#49226,.F.);
#65044=ORIENTED_EDGE('',*,*,#49230,.T.);
#65045=ORIENTED_EDGE('',*,*,#49231,.T.);
#65046=ORIENTED_EDGE('',*,*,#49232,.F.);
#65047=ORIENTED_EDGE('',*,*,#49233,.F.);
#65048=ORIENTED_EDGE('',*,*,#49234,.T.);
#65049=ORIENTED_EDGE('',*,*,#49235,.T.);
#65050=ORIENTED_EDGE('',*,*,#49236,.F.);
#65051=ORIENTED_EDGE('',*,*,#49231,.F.);
#65052=ORIENTED_EDGE('',*,*,#49237,.T.);
#65053=ORIENTED_EDGE('',*,*,#49238,.T.);
#65054=ORIENTED_EDGE('',*,*,#49239,.F.);
#65055=ORIENTED_EDGE('',*,*,#49235,.F.);
#65056=ORIENTED_EDGE('',*,*,#49240,.T.);
#65057=ORIENTED_EDGE('',*,*,#49233,.T.);
#65058=ORIENTED_EDGE('',*,*,#49241,.F.);
#65059=ORIENTED_EDGE('',*,*,#49238,.F.);
#65060=ORIENTED_EDGE('',*,*,#49242,.T.);
#65061=ORIENTED_EDGE('',*,*,#49243,.T.);
#65062=ORIENTED_EDGE('',*,*,#49244,.F.);
#65063=ORIENTED_EDGE('',*,*,#49245,.F.);
#65064=ORIENTED_EDGE('',*,*,#49246,.T.);
#65065=ORIENTED_EDGE('',*,*,#49247,.T.);
#65066=ORIENTED_EDGE('',*,*,#49248,.F.);
#65067=ORIENTED_EDGE('',*,*,#49243,.F.);
#65068=ORIENTED_EDGE('',*,*,#49249,.T.);
#65069=ORIENTED_EDGE('',*,*,#49250,.T.);
#65070=ORIENTED_EDGE('',*,*,#49251,.F.);
#65071=ORIENTED_EDGE('',*,*,#49247,.F.);
#65072=ORIENTED_EDGE('',*,*,#49252,.T.);
#65073=ORIENTED_EDGE('',*,*,#49245,.T.);
#65074=ORIENTED_EDGE('',*,*,#49253,.F.);
#65075=ORIENTED_EDGE('',*,*,#49250,.F.);
#65076=ORIENTED_EDGE('',*,*,#49254,.T.);
#65077=ORIENTED_EDGE('',*,*,#49255,.T.);
#65078=ORIENTED_EDGE('',*,*,#49256,.F.);
#65079=ORIENTED_EDGE('',*,*,#49257,.F.);
#65080=ORIENTED_EDGE('',*,*,#49258,.T.);
#65081=ORIENTED_EDGE('',*,*,#49259,.T.);
#65082=ORIENTED_EDGE('',*,*,#49260,.F.);
#65083=ORIENTED_EDGE('',*,*,#49255,.F.);
#65084=ORIENTED_EDGE('',*,*,#49261,.T.);
#65085=ORIENTED_EDGE('',*,*,#49262,.T.);
#65086=ORIENTED_EDGE('',*,*,#49263,.F.);
#65087=ORIENTED_EDGE('',*,*,#49259,.F.);
#65088=ORIENTED_EDGE('',*,*,#49264,.T.);
#65089=ORIENTED_EDGE('',*,*,#49257,.T.);
#65090=ORIENTED_EDGE('',*,*,#49265,.F.);
#65091=ORIENTED_EDGE('',*,*,#49262,.F.);
#65092=ORIENTED_EDGE('',*,*,#49266,.T.);
#65093=ORIENTED_EDGE('',*,*,#49267,.T.);
#65094=ORIENTED_EDGE('',*,*,#49268,.F.);
#65095=ORIENTED_EDGE('',*,*,#49269,.F.);
#65096=ORIENTED_EDGE('',*,*,#49270,.T.);
#65097=ORIENTED_EDGE('',*,*,#49271,.T.);
#65098=ORIENTED_EDGE('',*,*,#49272,.F.);
#65099=ORIENTED_EDGE('',*,*,#49267,.F.);
#65100=ORIENTED_EDGE('',*,*,#49273,.T.);
#65101=ORIENTED_EDGE('',*,*,#49274,.T.);
#65102=ORIENTED_EDGE('',*,*,#49275,.F.);
#65103=ORIENTED_EDGE('',*,*,#49271,.F.);
#65104=ORIENTED_EDGE('',*,*,#49276,.T.);
#65105=ORIENTED_EDGE('',*,*,#49269,.T.);
#65106=ORIENTED_EDGE('',*,*,#49277,.F.);
#65107=ORIENTED_EDGE('',*,*,#49274,.F.);
#65108=ORIENTED_EDGE('',*,*,#49278,.T.);
#65109=ORIENTED_EDGE('',*,*,#49279,.T.);
#65110=ORIENTED_EDGE('',*,*,#49280,.F.);
#65111=ORIENTED_EDGE('',*,*,#49281,.F.);
#65112=ORIENTED_EDGE('',*,*,#49282,.T.);
#65113=ORIENTED_EDGE('',*,*,#49283,.T.);
#65114=ORIENTED_EDGE('',*,*,#49284,.F.);
#65115=ORIENTED_EDGE('',*,*,#49279,.F.);
#65116=ORIENTED_EDGE('',*,*,#49285,.T.);
#65117=ORIENTED_EDGE('',*,*,#49286,.T.);
#65118=ORIENTED_EDGE('',*,*,#49287,.F.);
#65119=ORIENTED_EDGE('',*,*,#49283,.F.);
#65120=ORIENTED_EDGE('',*,*,#49288,.T.);
#65121=ORIENTED_EDGE('',*,*,#49281,.T.);
#65122=ORIENTED_EDGE('',*,*,#49289,.F.);
#65123=ORIENTED_EDGE('',*,*,#49286,.F.);
#65124=ORIENTED_EDGE('',*,*,#49290,.T.);
#65125=ORIENTED_EDGE('',*,*,#49291,.T.);
#65126=ORIENTED_EDGE('',*,*,#49292,.F.);
#65127=ORIENTED_EDGE('',*,*,#49293,.F.);
#65128=ORIENTED_EDGE('',*,*,#49294,.T.);
#65129=ORIENTED_EDGE('',*,*,#49295,.T.);
#65130=ORIENTED_EDGE('',*,*,#49296,.F.);
#65131=ORIENTED_EDGE('',*,*,#49291,.F.);
#65132=ORIENTED_EDGE('',*,*,#49297,.T.);
#65133=ORIENTED_EDGE('',*,*,#49298,.T.);
#65134=ORIENTED_EDGE('',*,*,#49299,.F.);
#65135=ORIENTED_EDGE('',*,*,#49295,.F.);
#65136=ORIENTED_EDGE('',*,*,#49300,.T.);
#65137=ORIENTED_EDGE('',*,*,#49293,.T.);
#65138=ORIENTED_EDGE('',*,*,#49301,.F.);
#65139=ORIENTED_EDGE('',*,*,#49298,.F.);
#65140=ORIENTED_EDGE('',*,*,#49302,.T.);
#65141=ORIENTED_EDGE('',*,*,#49303,.T.);
#65142=ORIENTED_EDGE('',*,*,#49304,.F.);
#65143=ORIENTED_EDGE('',*,*,#49305,.F.);
#65144=ORIENTED_EDGE('',*,*,#49306,.T.);
#65145=ORIENTED_EDGE('',*,*,#49307,.T.);
#65146=ORIENTED_EDGE('',*,*,#49308,.F.);
#65147=ORIENTED_EDGE('',*,*,#49303,.F.);
#65148=ORIENTED_EDGE('',*,*,#49309,.T.);
#65149=ORIENTED_EDGE('',*,*,#49310,.T.);
#65150=ORIENTED_EDGE('',*,*,#49311,.F.);
#65151=ORIENTED_EDGE('',*,*,#49307,.F.);
#65152=ORIENTED_EDGE('',*,*,#49312,.T.);
#65153=ORIENTED_EDGE('',*,*,#49305,.T.);
#65154=ORIENTED_EDGE('',*,*,#49313,.F.);
#65155=ORIENTED_EDGE('',*,*,#49310,.F.);
#65156=ORIENTED_EDGE('',*,*,#49314,.T.);
#65157=ORIENTED_EDGE('',*,*,#49315,.T.);
#65158=ORIENTED_EDGE('',*,*,#49316,.F.);
#65159=ORIENTED_EDGE('',*,*,#49317,.F.);
#65160=ORIENTED_EDGE('',*,*,#49318,.T.);
#65161=ORIENTED_EDGE('',*,*,#49319,.T.);
#65162=ORIENTED_EDGE('',*,*,#49320,.F.);
#65163=ORIENTED_EDGE('',*,*,#49315,.F.);
#65164=ORIENTED_EDGE('',*,*,#49321,.T.);
#65165=ORIENTED_EDGE('',*,*,#49322,.T.);
#65166=ORIENTED_EDGE('',*,*,#49323,.F.);
#65167=ORIENTED_EDGE('',*,*,#49319,.F.);
#65168=ORIENTED_EDGE('',*,*,#49324,.T.);
#65169=ORIENTED_EDGE('',*,*,#49317,.T.);
#65170=ORIENTED_EDGE('',*,*,#49325,.F.);
#65171=ORIENTED_EDGE('',*,*,#49322,.F.);
#65172=ORIENTED_EDGE('',*,*,#49326,.T.);
#65173=ORIENTED_EDGE('',*,*,#49327,.T.);
#65174=ORIENTED_EDGE('',*,*,#49328,.F.);
#65175=ORIENTED_EDGE('',*,*,#49329,.F.);
#65176=ORIENTED_EDGE('',*,*,#49330,.T.);
#65177=ORIENTED_EDGE('',*,*,#49331,.T.);
#65178=ORIENTED_EDGE('',*,*,#49332,.F.);
#65179=ORIENTED_EDGE('',*,*,#49327,.F.);
#65180=ORIENTED_EDGE('',*,*,#49333,.T.);
#65181=ORIENTED_EDGE('',*,*,#49334,.T.);
#65182=ORIENTED_EDGE('',*,*,#49335,.F.);
#65183=ORIENTED_EDGE('',*,*,#49331,.F.);
#65184=ORIENTED_EDGE('',*,*,#49336,.T.);
#65185=ORIENTED_EDGE('',*,*,#49329,.T.);
#65186=ORIENTED_EDGE('',*,*,#49337,.F.);
#65187=ORIENTED_EDGE('',*,*,#49334,.F.);
#65188=ORIENTED_EDGE('',*,*,#49338,.T.);
#65189=ORIENTED_EDGE('',*,*,#49339,.T.);
#65190=ORIENTED_EDGE('',*,*,#49340,.F.);
#65191=ORIENTED_EDGE('',*,*,#49341,.F.);
#65192=ORIENTED_EDGE('',*,*,#49342,.T.);
#65193=ORIENTED_EDGE('',*,*,#49343,.T.);
#65194=ORIENTED_EDGE('',*,*,#49344,.F.);
#65195=ORIENTED_EDGE('',*,*,#49339,.F.);
#65196=ORIENTED_EDGE('',*,*,#49345,.T.);
#65197=ORIENTED_EDGE('',*,*,#49346,.T.);
#65198=ORIENTED_EDGE('',*,*,#49347,.F.);
#65199=ORIENTED_EDGE('',*,*,#49343,.F.);
#65200=ORIENTED_EDGE('',*,*,#49348,.T.);
#65201=ORIENTED_EDGE('',*,*,#49341,.T.);
#65202=ORIENTED_EDGE('',*,*,#49349,.F.);
#65203=ORIENTED_EDGE('',*,*,#49346,.F.);
#65204=ORIENTED_EDGE('',*,*,#49350,.T.);
#65205=ORIENTED_EDGE('',*,*,#49351,.T.);
#65206=ORIENTED_EDGE('',*,*,#49352,.F.);
#65207=ORIENTED_EDGE('',*,*,#49353,.F.);
#65208=ORIENTED_EDGE('',*,*,#49354,.T.);
#65209=ORIENTED_EDGE('',*,*,#49355,.T.);
#65210=ORIENTED_EDGE('',*,*,#49356,.F.);
#65211=ORIENTED_EDGE('',*,*,#49351,.F.);
#65212=ORIENTED_EDGE('',*,*,#49357,.T.);
#65213=ORIENTED_EDGE('',*,*,#49358,.T.);
#65214=ORIENTED_EDGE('',*,*,#49359,.F.);
#65215=ORIENTED_EDGE('',*,*,#49355,.F.);
#65216=ORIENTED_EDGE('',*,*,#49360,.T.);
#65217=ORIENTED_EDGE('',*,*,#49353,.T.);
#65218=ORIENTED_EDGE('',*,*,#49361,.F.);
#65219=ORIENTED_EDGE('',*,*,#49358,.F.);
#65220=ORIENTED_EDGE('',*,*,#49362,.T.);
#65221=ORIENTED_EDGE('',*,*,#49363,.T.);
#65222=ORIENTED_EDGE('',*,*,#49364,.F.);
#65223=ORIENTED_EDGE('',*,*,#49365,.F.);
#65224=ORIENTED_EDGE('',*,*,#49366,.T.);
#65225=ORIENTED_EDGE('',*,*,#49367,.T.);
#65226=ORIENTED_EDGE('',*,*,#49368,.F.);
#65227=ORIENTED_EDGE('',*,*,#49363,.F.);
#65228=ORIENTED_EDGE('',*,*,#49369,.T.);
#65229=ORIENTED_EDGE('',*,*,#49370,.T.);
#65230=ORIENTED_EDGE('',*,*,#49371,.F.);
#65231=ORIENTED_EDGE('',*,*,#49367,.F.);
#65232=ORIENTED_EDGE('',*,*,#49372,.T.);
#65233=ORIENTED_EDGE('',*,*,#49365,.T.);
#65234=ORIENTED_EDGE('',*,*,#49373,.F.);
#65235=ORIENTED_EDGE('',*,*,#49370,.F.);
#65236=ORIENTED_EDGE('',*,*,#49374,.T.);
#65237=ORIENTED_EDGE('',*,*,#49375,.T.);
#65238=ORIENTED_EDGE('',*,*,#49376,.F.);
#65239=ORIENTED_EDGE('',*,*,#49377,.F.);
#65240=ORIENTED_EDGE('',*,*,#49378,.T.);
#65241=ORIENTED_EDGE('',*,*,#49379,.T.);
#65242=ORIENTED_EDGE('',*,*,#49380,.F.);
#65243=ORIENTED_EDGE('',*,*,#49375,.F.);
#65244=ORIENTED_EDGE('',*,*,#49381,.T.);
#65245=ORIENTED_EDGE('',*,*,#49382,.T.);
#65246=ORIENTED_EDGE('',*,*,#49383,.F.);
#65247=ORIENTED_EDGE('',*,*,#49379,.F.);
#65248=ORIENTED_EDGE('',*,*,#49384,.T.);
#65249=ORIENTED_EDGE('',*,*,#49377,.T.);
#65250=ORIENTED_EDGE('',*,*,#49385,.F.);
#65251=ORIENTED_EDGE('',*,*,#49382,.F.);
#65252=ORIENTED_EDGE('',*,*,#49386,.T.);
#65253=ORIENTED_EDGE('',*,*,#49387,.T.);
#65254=ORIENTED_EDGE('',*,*,#49388,.F.);
#65255=ORIENTED_EDGE('',*,*,#49389,.F.);
#65256=ORIENTED_EDGE('',*,*,#49390,.T.);
#65257=ORIENTED_EDGE('',*,*,#49391,.T.);
#65258=ORIENTED_EDGE('',*,*,#49392,.F.);
#65259=ORIENTED_EDGE('',*,*,#49387,.F.);
#65260=ORIENTED_EDGE('',*,*,#49393,.T.);
#65261=ORIENTED_EDGE('',*,*,#49394,.T.);
#65262=ORIENTED_EDGE('',*,*,#49395,.F.);
#65263=ORIENTED_EDGE('',*,*,#49391,.F.);
#65264=ORIENTED_EDGE('',*,*,#49396,.T.);
#65265=ORIENTED_EDGE('',*,*,#49389,.T.);
#65266=ORIENTED_EDGE('',*,*,#49397,.F.);
#65267=ORIENTED_EDGE('',*,*,#49394,.F.);
#65268=ORIENTED_EDGE('',*,*,#49398,.T.);
#65269=ORIENTED_EDGE('',*,*,#49399,.T.);
#65270=ORIENTED_EDGE('',*,*,#49400,.F.);
#65271=ORIENTED_EDGE('',*,*,#49401,.F.);
#65272=ORIENTED_EDGE('',*,*,#49402,.T.);
#65273=ORIENTED_EDGE('',*,*,#49403,.T.);
#65274=ORIENTED_EDGE('',*,*,#49404,.F.);
#65275=ORIENTED_EDGE('',*,*,#49399,.F.);
#65276=ORIENTED_EDGE('',*,*,#49405,.T.);
#65277=ORIENTED_EDGE('',*,*,#49406,.T.);
#65278=ORIENTED_EDGE('',*,*,#49407,.F.);
#65279=ORIENTED_EDGE('',*,*,#49403,.F.);
#65280=ORIENTED_EDGE('',*,*,#49408,.T.);
#65281=ORIENTED_EDGE('',*,*,#49401,.T.);
#65282=ORIENTED_EDGE('',*,*,#49409,.F.);
#65283=ORIENTED_EDGE('',*,*,#49406,.F.);
#65284=ORIENTED_EDGE('',*,*,#49410,.T.);
#65285=ORIENTED_EDGE('',*,*,#49411,.T.);
#65286=ORIENTED_EDGE('',*,*,#49412,.F.);
#65287=ORIENTED_EDGE('',*,*,#49413,.F.);
#65288=ORIENTED_EDGE('',*,*,#49414,.T.);
#65289=ORIENTED_EDGE('',*,*,#49415,.T.);
#65290=ORIENTED_EDGE('',*,*,#49416,.F.);
#65291=ORIENTED_EDGE('',*,*,#49411,.F.);
#65292=ORIENTED_EDGE('',*,*,#49417,.T.);
#65293=ORIENTED_EDGE('',*,*,#49418,.T.);
#65294=ORIENTED_EDGE('',*,*,#49419,.F.);
#65295=ORIENTED_EDGE('',*,*,#49415,.F.);
#65296=ORIENTED_EDGE('',*,*,#49420,.T.);
#65297=ORIENTED_EDGE('',*,*,#49413,.T.);
#65298=ORIENTED_EDGE('',*,*,#49421,.F.);
#65299=ORIENTED_EDGE('',*,*,#49418,.F.);
#65300=ORIENTED_EDGE('',*,*,#49422,.T.);
#65301=ORIENTED_EDGE('',*,*,#49423,.T.);
#65302=ORIENTED_EDGE('',*,*,#49424,.F.);
#65303=ORIENTED_EDGE('',*,*,#49425,.F.);
#65304=ORIENTED_EDGE('',*,*,#49426,.T.);
#65305=ORIENTED_EDGE('',*,*,#49427,.T.);
#65306=ORIENTED_EDGE('',*,*,#49428,.F.);
#65307=ORIENTED_EDGE('',*,*,#49423,.F.);
#65308=ORIENTED_EDGE('',*,*,#49429,.T.);
#65309=ORIENTED_EDGE('',*,*,#49430,.T.);
#65310=ORIENTED_EDGE('',*,*,#49431,.F.);
#65311=ORIENTED_EDGE('',*,*,#49427,.F.);
#65312=ORIENTED_EDGE('',*,*,#49432,.T.);
#65313=ORIENTED_EDGE('',*,*,#49425,.T.);
#65314=ORIENTED_EDGE('',*,*,#49433,.F.);
#65315=ORIENTED_EDGE('',*,*,#49430,.F.);
#65316=ORIENTED_EDGE('',*,*,#49434,.T.);
#65317=ORIENTED_EDGE('',*,*,#49435,.T.);
#65318=ORIENTED_EDGE('',*,*,#49436,.F.);
#65319=ORIENTED_EDGE('',*,*,#49437,.F.);
#65320=ORIENTED_EDGE('',*,*,#49438,.T.);
#65321=ORIENTED_EDGE('',*,*,#49439,.T.);
#65322=ORIENTED_EDGE('',*,*,#49440,.F.);
#65323=ORIENTED_EDGE('',*,*,#49435,.F.);
#65324=ORIENTED_EDGE('',*,*,#49441,.T.);
#65325=ORIENTED_EDGE('',*,*,#49442,.T.);
#65326=ORIENTED_EDGE('',*,*,#49443,.F.);
#65327=ORIENTED_EDGE('',*,*,#49439,.F.);
#65328=ORIENTED_EDGE('',*,*,#49444,.T.);
#65329=ORIENTED_EDGE('',*,*,#49437,.T.);
#65330=ORIENTED_EDGE('',*,*,#49445,.F.);
#65331=ORIENTED_EDGE('',*,*,#49442,.F.);
#65332=ORIENTED_EDGE('',*,*,#49446,.T.);
#65333=ORIENTED_EDGE('',*,*,#49447,.T.);
#65334=ORIENTED_EDGE('',*,*,#49448,.F.);
#65335=ORIENTED_EDGE('',*,*,#49449,.F.);
#65336=ORIENTED_EDGE('',*,*,#49450,.T.);
#65337=ORIENTED_EDGE('',*,*,#49451,.T.);
#65338=ORIENTED_EDGE('',*,*,#49452,.F.);
#65339=ORIENTED_EDGE('',*,*,#49447,.F.);
#65340=ORIENTED_EDGE('',*,*,#49453,.T.);
#65341=ORIENTED_EDGE('',*,*,#49454,.T.);
#65342=ORIENTED_EDGE('',*,*,#49455,.F.);
#65343=ORIENTED_EDGE('',*,*,#49451,.F.);
#65344=ORIENTED_EDGE('',*,*,#49456,.T.);
#65345=ORIENTED_EDGE('',*,*,#49449,.T.);
#65346=ORIENTED_EDGE('',*,*,#49457,.F.);
#65347=ORIENTED_EDGE('',*,*,#49454,.F.);
#65348=ORIENTED_EDGE('',*,*,#49458,.T.);
#65349=ORIENTED_EDGE('',*,*,#49459,.T.);
#65350=ORIENTED_EDGE('',*,*,#49460,.F.);
#65351=ORIENTED_EDGE('',*,*,#49461,.F.);
#65352=ORIENTED_EDGE('',*,*,#49462,.T.);
#65353=ORIENTED_EDGE('',*,*,#49463,.T.);
#65354=ORIENTED_EDGE('',*,*,#49464,.F.);
#65355=ORIENTED_EDGE('',*,*,#49459,.F.);
#65356=ORIENTED_EDGE('',*,*,#49465,.T.);
#65357=ORIENTED_EDGE('',*,*,#49466,.T.);
#65358=ORIENTED_EDGE('',*,*,#49467,.F.);
#65359=ORIENTED_EDGE('',*,*,#49463,.F.);
#65360=ORIENTED_EDGE('',*,*,#49468,.T.);
#65361=ORIENTED_EDGE('',*,*,#49461,.T.);
#65362=ORIENTED_EDGE('',*,*,#49469,.F.);
#65363=ORIENTED_EDGE('',*,*,#49466,.F.);
#65364=ORIENTED_EDGE('',*,*,#49470,.T.);
#65365=ORIENTED_EDGE('',*,*,#49471,.T.);
#65366=ORIENTED_EDGE('',*,*,#49472,.F.);
#65367=ORIENTED_EDGE('',*,*,#49473,.F.);
#65368=ORIENTED_EDGE('',*,*,#49474,.T.);
#65369=ORIENTED_EDGE('',*,*,#49475,.T.);
#65370=ORIENTED_EDGE('',*,*,#49476,.F.);
#65371=ORIENTED_EDGE('',*,*,#49471,.F.);
#65372=ORIENTED_EDGE('',*,*,#49477,.T.);
#65373=ORIENTED_EDGE('',*,*,#49478,.T.);
#65374=ORIENTED_EDGE('',*,*,#49479,.F.);
#65375=ORIENTED_EDGE('',*,*,#49475,.F.);
#65376=ORIENTED_EDGE('',*,*,#49480,.T.);
#65377=ORIENTED_EDGE('',*,*,#49473,.T.);
#65378=ORIENTED_EDGE('',*,*,#49481,.F.);
#65379=ORIENTED_EDGE('',*,*,#49478,.F.);
#65380=ORIENTED_EDGE('',*,*,#49482,.T.);
#65381=ORIENTED_EDGE('',*,*,#49483,.T.);
#65382=ORIENTED_EDGE('',*,*,#49484,.F.);
#65383=ORIENTED_EDGE('',*,*,#49485,.F.);
#65384=ORIENTED_EDGE('',*,*,#49486,.T.);
#65385=ORIENTED_EDGE('',*,*,#49487,.T.);
#65386=ORIENTED_EDGE('',*,*,#49488,.F.);
#65387=ORIENTED_EDGE('',*,*,#49483,.F.);
#65388=ORIENTED_EDGE('',*,*,#49489,.T.);
#65389=ORIENTED_EDGE('',*,*,#49490,.T.);
#65390=ORIENTED_EDGE('',*,*,#49491,.F.);
#65391=ORIENTED_EDGE('',*,*,#49487,.F.);
#65392=ORIENTED_EDGE('',*,*,#49492,.T.);
#65393=ORIENTED_EDGE('',*,*,#49485,.T.);
#65394=ORIENTED_EDGE('',*,*,#49493,.F.);
#65395=ORIENTED_EDGE('',*,*,#49490,.F.);
#65396=ORIENTED_EDGE('',*,*,#49494,.T.);
#65397=ORIENTED_EDGE('',*,*,#49495,.T.);
#65398=ORIENTED_EDGE('',*,*,#49496,.F.);
#65399=ORIENTED_EDGE('',*,*,#49497,.F.);
#65400=ORIENTED_EDGE('',*,*,#49498,.T.);
#65401=ORIENTED_EDGE('',*,*,#49499,.T.);
#65402=ORIENTED_EDGE('',*,*,#49500,.F.);
#65403=ORIENTED_EDGE('',*,*,#49495,.F.);
#65404=ORIENTED_EDGE('',*,*,#49501,.T.);
#65405=ORIENTED_EDGE('',*,*,#49502,.T.);
#65406=ORIENTED_EDGE('',*,*,#49503,.F.);
#65407=ORIENTED_EDGE('',*,*,#49499,.F.);
#65408=ORIENTED_EDGE('',*,*,#49504,.T.);
#65409=ORIENTED_EDGE('',*,*,#49497,.T.);
#65410=ORIENTED_EDGE('',*,*,#49505,.F.);
#65411=ORIENTED_EDGE('',*,*,#49502,.F.);
#65412=ORIENTED_EDGE('',*,*,#49506,.T.);
#65413=ORIENTED_EDGE('',*,*,#49507,.T.);
#65414=ORIENTED_EDGE('',*,*,#49508,.F.);
#65415=ORIENTED_EDGE('',*,*,#49509,.F.);
#65416=ORIENTED_EDGE('',*,*,#49510,.T.);
#65417=ORIENTED_EDGE('',*,*,#49511,.T.);
#65418=ORIENTED_EDGE('',*,*,#49512,.F.);
#65419=ORIENTED_EDGE('',*,*,#49507,.F.);
#65420=ORIENTED_EDGE('',*,*,#49513,.T.);
#65421=ORIENTED_EDGE('',*,*,#49514,.T.);
#65422=ORIENTED_EDGE('',*,*,#49515,.F.);
#65423=ORIENTED_EDGE('',*,*,#49511,.F.);
#65424=ORIENTED_EDGE('',*,*,#49516,.T.);
#65425=ORIENTED_EDGE('',*,*,#49509,.T.);
#65426=ORIENTED_EDGE('',*,*,#49517,.F.);
#65427=ORIENTED_EDGE('',*,*,#49514,.F.);
#65428=ORIENTED_EDGE('',*,*,#49518,.T.);
#65429=ORIENTED_EDGE('',*,*,#49519,.T.);
#65430=ORIENTED_EDGE('',*,*,#49520,.F.);
#65431=ORIENTED_EDGE('',*,*,#49521,.F.);
#65432=ORIENTED_EDGE('',*,*,#49522,.T.);
#65433=ORIENTED_EDGE('',*,*,#49523,.T.);
#65434=ORIENTED_EDGE('',*,*,#49524,.F.);
#65435=ORIENTED_EDGE('',*,*,#49519,.F.);
#65436=ORIENTED_EDGE('',*,*,#49525,.T.);
#65437=ORIENTED_EDGE('',*,*,#49526,.T.);
#65438=ORIENTED_EDGE('',*,*,#49527,.F.);
#65439=ORIENTED_EDGE('',*,*,#49523,.F.);
#65440=ORIENTED_EDGE('',*,*,#49528,.T.);
#65441=ORIENTED_EDGE('',*,*,#49521,.T.);
#65442=ORIENTED_EDGE('',*,*,#49529,.F.);
#65443=ORIENTED_EDGE('',*,*,#49526,.F.);
#65444=ORIENTED_EDGE('',*,*,#49530,.T.);
#65445=ORIENTED_EDGE('',*,*,#49531,.T.);
#65446=ORIENTED_EDGE('',*,*,#49532,.F.);
#65447=ORIENTED_EDGE('',*,*,#49533,.F.);
#65448=ORIENTED_EDGE('',*,*,#49534,.T.);
#65449=ORIENTED_EDGE('',*,*,#49535,.T.);
#65450=ORIENTED_EDGE('',*,*,#49536,.F.);
#65451=ORIENTED_EDGE('',*,*,#49531,.F.);
#65452=ORIENTED_EDGE('',*,*,#49537,.T.);
#65453=ORIENTED_EDGE('',*,*,#49538,.T.);
#65454=ORIENTED_EDGE('',*,*,#49539,.F.);
#65455=ORIENTED_EDGE('',*,*,#49535,.F.);
#65456=ORIENTED_EDGE('',*,*,#49540,.T.);
#65457=ORIENTED_EDGE('',*,*,#49533,.T.);
#65458=ORIENTED_EDGE('',*,*,#49541,.F.);
#65459=ORIENTED_EDGE('',*,*,#49538,.F.);
#65460=ORIENTED_EDGE('',*,*,#49542,.T.);
#65461=ORIENTED_EDGE('',*,*,#49543,.T.);
#65462=ORIENTED_EDGE('',*,*,#49544,.F.);
#65463=ORIENTED_EDGE('',*,*,#49545,.F.);
#65464=ORIENTED_EDGE('',*,*,#49546,.T.);
#65465=ORIENTED_EDGE('',*,*,#49547,.T.);
#65466=ORIENTED_EDGE('',*,*,#49548,.F.);
#65467=ORIENTED_EDGE('',*,*,#49543,.F.);
#65468=ORIENTED_EDGE('',*,*,#49549,.T.);
#65469=ORIENTED_EDGE('',*,*,#49550,.T.);
#65470=ORIENTED_EDGE('',*,*,#49551,.F.);
#65471=ORIENTED_EDGE('',*,*,#49547,.F.);
#65472=ORIENTED_EDGE('',*,*,#49552,.T.);
#65473=ORIENTED_EDGE('',*,*,#49545,.T.);
#65474=ORIENTED_EDGE('',*,*,#49553,.F.);
#65475=ORIENTED_EDGE('',*,*,#49550,.F.);
#65476=ORIENTED_EDGE('',*,*,#49554,.T.);
#65477=ORIENTED_EDGE('',*,*,#49555,.T.);
#65478=ORIENTED_EDGE('',*,*,#49556,.F.);
#65479=ORIENTED_EDGE('',*,*,#49557,.F.);
#65480=ORIENTED_EDGE('',*,*,#49558,.T.);
#65481=ORIENTED_EDGE('',*,*,#49559,.T.);
#65482=ORIENTED_EDGE('',*,*,#49560,.F.);
#65483=ORIENTED_EDGE('',*,*,#49555,.F.);
#65484=ORIENTED_EDGE('',*,*,#49561,.T.);
#65485=ORIENTED_EDGE('',*,*,#49562,.T.);
#65486=ORIENTED_EDGE('',*,*,#49563,.F.);
#65487=ORIENTED_EDGE('',*,*,#49559,.F.);
#65488=ORIENTED_EDGE('',*,*,#49564,.T.);
#65489=ORIENTED_EDGE('',*,*,#49557,.T.);
#65490=ORIENTED_EDGE('',*,*,#49565,.F.);
#65491=ORIENTED_EDGE('',*,*,#49562,.F.);
#65492=ORIENTED_EDGE('',*,*,#49566,.T.);
#65493=ORIENTED_EDGE('',*,*,#49567,.T.);
#65494=ORIENTED_EDGE('',*,*,#49568,.F.);
#65495=ORIENTED_EDGE('',*,*,#49569,.F.);
#65496=ORIENTED_EDGE('',*,*,#49570,.T.);
#65497=ORIENTED_EDGE('',*,*,#49571,.T.);
#65498=ORIENTED_EDGE('',*,*,#49572,.F.);
#65499=ORIENTED_EDGE('',*,*,#49567,.F.);
#65500=ORIENTED_EDGE('',*,*,#49573,.T.);
#65501=ORIENTED_EDGE('',*,*,#49574,.T.);
#65502=ORIENTED_EDGE('',*,*,#49575,.F.);
#65503=ORIENTED_EDGE('',*,*,#49571,.F.);
#65504=ORIENTED_EDGE('',*,*,#49576,.T.);
#65505=ORIENTED_EDGE('',*,*,#49569,.T.);
#65506=ORIENTED_EDGE('',*,*,#49577,.F.);
#65507=ORIENTED_EDGE('',*,*,#49574,.F.);
#65508=ORIENTED_EDGE('',*,*,#49578,.T.);
#65509=ORIENTED_EDGE('',*,*,#49579,.T.);
#65510=ORIENTED_EDGE('',*,*,#49580,.F.);
#65511=ORIENTED_EDGE('',*,*,#49581,.F.);
#65512=ORIENTED_EDGE('',*,*,#49582,.T.);
#65513=ORIENTED_EDGE('',*,*,#49583,.T.);
#65514=ORIENTED_EDGE('',*,*,#49584,.F.);
#65515=ORIENTED_EDGE('',*,*,#49579,.F.);
#65516=ORIENTED_EDGE('',*,*,#49585,.T.);
#65517=ORIENTED_EDGE('',*,*,#49586,.T.);
#65518=ORIENTED_EDGE('',*,*,#49587,.F.);
#65519=ORIENTED_EDGE('',*,*,#49583,.F.);
#65520=ORIENTED_EDGE('',*,*,#49588,.T.);
#65521=ORIENTED_EDGE('',*,*,#49581,.T.);
#65522=ORIENTED_EDGE('',*,*,#49589,.F.);
#65523=ORIENTED_EDGE('',*,*,#49586,.F.);
#65524=ORIENTED_EDGE('',*,*,#49590,.T.);
#65525=ORIENTED_EDGE('',*,*,#49591,.T.);
#65526=ORIENTED_EDGE('',*,*,#49592,.F.);
#65527=ORIENTED_EDGE('',*,*,#49593,.F.);
#65528=ORIENTED_EDGE('',*,*,#49594,.T.);
#65529=ORIENTED_EDGE('',*,*,#49595,.T.);
#65530=ORIENTED_EDGE('',*,*,#49596,.F.);
#65531=ORIENTED_EDGE('',*,*,#49591,.F.);
#65532=ORIENTED_EDGE('',*,*,#49597,.T.);
#65533=ORIENTED_EDGE('',*,*,#49598,.T.);
#65534=ORIENTED_EDGE('',*,*,#49599,.F.);
#65535=ORIENTED_EDGE('',*,*,#49595,.F.);
#65536=ORIENTED_EDGE('',*,*,#49600,.T.);
#65537=ORIENTED_EDGE('',*,*,#49593,.T.);
#65538=ORIENTED_EDGE('',*,*,#49601,.F.);
#65539=ORIENTED_EDGE('',*,*,#49598,.F.);
#65540=ORIENTED_EDGE('',*,*,#49602,.T.);
#65541=ORIENTED_EDGE('',*,*,#49603,.T.);
#65542=ORIENTED_EDGE('',*,*,#49604,.F.);
#65543=ORIENTED_EDGE('',*,*,#49605,.F.);
#65544=ORIENTED_EDGE('',*,*,#49606,.T.);
#65545=ORIENTED_EDGE('',*,*,#49607,.T.);
#65546=ORIENTED_EDGE('',*,*,#49608,.F.);
#65547=ORIENTED_EDGE('',*,*,#49603,.F.);
#65548=ORIENTED_EDGE('',*,*,#49609,.T.);
#65549=ORIENTED_EDGE('',*,*,#49610,.T.);
#65550=ORIENTED_EDGE('',*,*,#49611,.F.);
#65551=ORIENTED_EDGE('',*,*,#49607,.F.);
#65552=ORIENTED_EDGE('',*,*,#49612,.T.);
#65553=ORIENTED_EDGE('',*,*,#49605,.T.);
#65554=ORIENTED_EDGE('',*,*,#49613,.F.);
#65555=ORIENTED_EDGE('',*,*,#49610,.F.);
#65556=ORIENTED_EDGE('',*,*,#49614,.T.);
#65557=ORIENTED_EDGE('',*,*,#49615,.T.);
#65558=ORIENTED_EDGE('',*,*,#49616,.F.);
#65559=ORIENTED_EDGE('',*,*,#49617,.F.);
#65560=ORIENTED_EDGE('',*,*,#49618,.T.);
#65561=ORIENTED_EDGE('',*,*,#49619,.T.);
#65562=ORIENTED_EDGE('',*,*,#49620,.F.);
#65563=ORIENTED_EDGE('',*,*,#49615,.F.);
#65564=ORIENTED_EDGE('',*,*,#49621,.T.);
#65565=ORIENTED_EDGE('',*,*,#49622,.T.);
#65566=ORIENTED_EDGE('',*,*,#49623,.F.);
#65567=ORIENTED_EDGE('',*,*,#49619,.F.);
#65568=ORIENTED_EDGE('',*,*,#49624,.T.);
#65569=ORIENTED_EDGE('',*,*,#49617,.T.);
#65570=ORIENTED_EDGE('',*,*,#49625,.F.);
#65571=ORIENTED_EDGE('',*,*,#49622,.F.);
#65572=ORIENTED_EDGE('',*,*,#49626,.T.);
#65573=ORIENTED_EDGE('',*,*,#49627,.T.);
#65574=ORIENTED_EDGE('',*,*,#49628,.F.);
#65575=ORIENTED_EDGE('',*,*,#49629,.F.);
#65576=ORIENTED_EDGE('',*,*,#49630,.T.);
#65577=ORIENTED_EDGE('',*,*,#49631,.T.);
#65578=ORIENTED_EDGE('',*,*,#49632,.F.);
#65579=ORIENTED_EDGE('',*,*,#49627,.F.);
#65580=ORIENTED_EDGE('',*,*,#49633,.T.);
#65581=ORIENTED_EDGE('',*,*,#49634,.T.);
#65582=ORIENTED_EDGE('',*,*,#49635,.F.);
#65583=ORIENTED_EDGE('',*,*,#49631,.F.);
#65584=ORIENTED_EDGE('',*,*,#49636,.T.);
#65585=ORIENTED_EDGE('',*,*,#49629,.T.);
#65586=ORIENTED_EDGE('',*,*,#49637,.F.);
#65587=ORIENTED_EDGE('',*,*,#49634,.F.);
#65588=ORIENTED_EDGE('',*,*,#49638,.T.);
#65589=ORIENTED_EDGE('',*,*,#49639,.T.);
#65590=ORIENTED_EDGE('',*,*,#49640,.F.);
#65591=ORIENTED_EDGE('',*,*,#49641,.F.);
#65592=ORIENTED_EDGE('',*,*,#49642,.T.);
#65593=ORIENTED_EDGE('',*,*,#49643,.T.);
#65594=ORIENTED_EDGE('',*,*,#49644,.F.);
#65595=ORIENTED_EDGE('',*,*,#49639,.F.);
#65596=ORIENTED_EDGE('',*,*,#49645,.T.);
#65597=ORIENTED_EDGE('',*,*,#49646,.T.);
#65598=ORIENTED_EDGE('',*,*,#49647,.F.);
#65599=ORIENTED_EDGE('',*,*,#49643,.F.);
#65600=ORIENTED_EDGE('',*,*,#49648,.T.);
#65601=ORIENTED_EDGE('',*,*,#49641,.T.);
#65602=ORIENTED_EDGE('',*,*,#49649,.F.);
#65603=ORIENTED_EDGE('',*,*,#49646,.F.);
#65604=ORIENTED_EDGE('',*,*,#49650,.T.);
#65605=ORIENTED_EDGE('',*,*,#49651,.T.);
#65606=ORIENTED_EDGE('',*,*,#49652,.F.);
#65607=ORIENTED_EDGE('',*,*,#49653,.F.);
#65608=ORIENTED_EDGE('',*,*,#49654,.T.);
#65609=ORIENTED_EDGE('',*,*,#49655,.T.);
#65610=ORIENTED_EDGE('',*,*,#49656,.F.);
#65611=ORIENTED_EDGE('',*,*,#49651,.F.);
#65612=ORIENTED_EDGE('',*,*,#49657,.T.);
#65613=ORIENTED_EDGE('',*,*,#49658,.T.);
#65614=ORIENTED_EDGE('',*,*,#49659,.F.);
#65615=ORIENTED_EDGE('',*,*,#49655,.F.);
#65616=ORIENTED_EDGE('',*,*,#49660,.T.);
#65617=ORIENTED_EDGE('',*,*,#49653,.T.);
#65618=ORIENTED_EDGE('',*,*,#49661,.F.);
#65619=ORIENTED_EDGE('',*,*,#49658,.F.);
#65620=ORIENTED_EDGE('',*,*,#49662,.T.);
#65621=ORIENTED_EDGE('',*,*,#49663,.T.);
#65622=ORIENTED_EDGE('',*,*,#49664,.F.);
#65623=ORIENTED_EDGE('',*,*,#49665,.F.);
#65624=ORIENTED_EDGE('',*,*,#49666,.T.);
#65625=ORIENTED_EDGE('',*,*,#49667,.T.);
#65626=ORIENTED_EDGE('',*,*,#49668,.F.);
#65627=ORIENTED_EDGE('',*,*,#49663,.F.);
#65628=ORIENTED_EDGE('',*,*,#49669,.T.);
#65629=ORIENTED_EDGE('',*,*,#49670,.T.);
#65630=ORIENTED_EDGE('',*,*,#49671,.F.);
#65631=ORIENTED_EDGE('',*,*,#49667,.F.);
#65632=ORIENTED_EDGE('',*,*,#49672,.T.);
#65633=ORIENTED_EDGE('',*,*,#49665,.T.);
#65634=ORIENTED_EDGE('',*,*,#49673,.F.);
#65635=ORIENTED_EDGE('',*,*,#49670,.F.);
#65636=ORIENTED_EDGE('',*,*,#49674,.T.);
#65637=ORIENTED_EDGE('',*,*,#49675,.T.);
#65638=ORIENTED_EDGE('',*,*,#49676,.F.);
#65639=ORIENTED_EDGE('',*,*,#49677,.F.);
#65640=ORIENTED_EDGE('',*,*,#49678,.T.);
#65641=ORIENTED_EDGE('',*,*,#49679,.T.);
#65642=ORIENTED_EDGE('',*,*,#49680,.F.);
#65643=ORIENTED_EDGE('',*,*,#49675,.F.);
#65644=ORIENTED_EDGE('',*,*,#49681,.T.);
#65645=ORIENTED_EDGE('',*,*,#49682,.T.);
#65646=ORIENTED_EDGE('',*,*,#49683,.F.);
#65647=ORIENTED_EDGE('',*,*,#49679,.F.);
#65648=ORIENTED_EDGE('',*,*,#49684,.T.);
#65649=ORIENTED_EDGE('',*,*,#49677,.T.);
#65650=ORIENTED_EDGE('',*,*,#49685,.F.);
#65651=ORIENTED_EDGE('',*,*,#49682,.F.);
#65652=ORIENTED_EDGE('',*,*,#49686,.T.);
#65653=ORIENTED_EDGE('',*,*,#49687,.T.);
#65654=ORIENTED_EDGE('',*,*,#49688,.F.);
#65655=ORIENTED_EDGE('',*,*,#49689,.F.);
#65656=ORIENTED_EDGE('',*,*,#49690,.T.);
#65657=ORIENTED_EDGE('',*,*,#49691,.T.);
#65658=ORIENTED_EDGE('',*,*,#49692,.F.);
#65659=ORIENTED_EDGE('',*,*,#49687,.F.);
#65660=ORIENTED_EDGE('',*,*,#49693,.T.);
#65661=ORIENTED_EDGE('',*,*,#49694,.T.);
#65662=ORIENTED_EDGE('',*,*,#49695,.F.);
#65663=ORIENTED_EDGE('',*,*,#49691,.F.);
#65664=ORIENTED_EDGE('',*,*,#49696,.T.);
#65665=ORIENTED_EDGE('',*,*,#49689,.T.);
#65666=ORIENTED_EDGE('',*,*,#49697,.F.);
#65667=ORIENTED_EDGE('',*,*,#49694,.F.);
#65668=ORIENTED_EDGE('',*,*,#49698,.T.);
#65669=ORIENTED_EDGE('',*,*,#49699,.T.);
#65670=ORIENTED_EDGE('',*,*,#49700,.F.);
#65671=ORIENTED_EDGE('',*,*,#49701,.F.);
#65672=ORIENTED_EDGE('',*,*,#49702,.T.);
#65673=ORIENTED_EDGE('',*,*,#49703,.T.);
#65674=ORIENTED_EDGE('',*,*,#49704,.F.);
#65675=ORIENTED_EDGE('',*,*,#49699,.F.);
#65676=ORIENTED_EDGE('',*,*,#49705,.T.);
#65677=ORIENTED_EDGE('',*,*,#49706,.T.);
#65678=ORIENTED_EDGE('',*,*,#49707,.F.);
#65679=ORIENTED_EDGE('',*,*,#49703,.F.);
#65680=ORIENTED_EDGE('',*,*,#49708,.T.);
#65681=ORIENTED_EDGE('',*,*,#49701,.T.);
#65682=ORIENTED_EDGE('',*,*,#49709,.F.);
#65683=ORIENTED_EDGE('',*,*,#49706,.F.);
#65684=ORIENTED_EDGE('',*,*,#49710,.T.);
#65685=ORIENTED_EDGE('',*,*,#49711,.T.);
#65686=ORIENTED_EDGE('',*,*,#49712,.F.);
#65687=ORIENTED_EDGE('',*,*,#49713,.F.);
#65688=ORIENTED_EDGE('',*,*,#49714,.T.);
#65689=ORIENTED_EDGE('',*,*,#49715,.T.);
#65690=ORIENTED_EDGE('',*,*,#49716,.F.);
#65691=ORIENTED_EDGE('',*,*,#49711,.F.);
#65692=ORIENTED_EDGE('',*,*,#49717,.T.);
#65693=ORIENTED_EDGE('',*,*,#49718,.T.);
#65694=ORIENTED_EDGE('',*,*,#49719,.F.);
#65695=ORIENTED_EDGE('',*,*,#49715,.F.);
#65696=ORIENTED_EDGE('',*,*,#49720,.T.);
#65697=ORIENTED_EDGE('',*,*,#49713,.T.);
#65698=ORIENTED_EDGE('',*,*,#49721,.F.);
#65699=ORIENTED_EDGE('',*,*,#49718,.F.);
#65700=ORIENTED_EDGE('',*,*,#49722,.T.);
#65701=ORIENTED_EDGE('',*,*,#49723,.T.);
#65702=ORIENTED_EDGE('',*,*,#49724,.F.);
#65703=ORIENTED_EDGE('',*,*,#49725,.F.);
#65704=ORIENTED_EDGE('',*,*,#49726,.T.);
#65705=ORIENTED_EDGE('',*,*,#49727,.T.);
#65706=ORIENTED_EDGE('',*,*,#49728,.F.);
#65707=ORIENTED_EDGE('',*,*,#49723,.F.);
#65708=ORIENTED_EDGE('',*,*,#49729,.T.);
#65709=ORIENTED_EDGE('',*,*,#49730,.T.);
#65710=ORIENTED_EDGE('',*,*,#49731,.F.);
#65711=ORIENTED_EDGE('',*,*,#49727,.F.);
#65712=ORIENTED_EDGE('',*,*,#49732,.T.);
#65713=ORIENTED_EDGE('',*,*,#49725,.T.);
#65714=ORIENTED_EDGE('',*,*,#49733,.F.);
#65715=ORIENTED_EDGE('',*,*,#49730,.F.);
#65716=ORIENTED_EDGE('',*,*,#49734,.T.);
#65717=ORIENTED_EDGE('',*,*,#49735,.T.);
#65718=ORIENTED_EDGE('',*,*,#49736,.F.);
#65719=ORIENTED_EDGE('',*,*,#49737,.F.);
#65720=ORIENTED_EDGE('',*,*,#49738,.T.);
#65721=ORIENTED_EDGE('',*,*,#49739,.T.);
#65722=ORIENTED_EDGE('',*,*,#49740,.F.);
#65723=ORIENTED_EDGE('',*,*,#49735,.F.);
#65724=ORIENTED_EDGE('',*,*,#49741,.T.);
#65725=ORIENTED_EDGE('',*,*,#49742,.T.);
#65726=ORIENTED_EDGE('',*,*,#49743,.F.);
#65727=ORIENTED_EDGE('',*,*,#49739,.F.);
#65728=ORIENTED_EDGE('',*,*,#49744,.T.);
#65729=ORIENTED_EDGE('',*,*,#49737,.T.);
#65730=ORIENTED_EDGE('',*,*,#49745,.F.);
#65731=ORIENTED_EDGE('',*,*,#49742,.F.);
#65732=ORIENTED_EDGE('',*,*,#49746,.T.);
#65733=ORIENTED_EDGE('',*,*,#49747,.T.);
#65734=ORIENTED_EDGE('',*,*,#49748,.F.);
#65735=ORIENTED_EDGE('',*,*,#49749,.F.);
#65736=ORIENTED_EDGE('',*,*,#49750,.T.);
#65737=ORIENTED_EDGE('',*,*,#49751,.T.);
#65738=ORIENTED_EDGE('',*,*,#49752,.F.);
#65739=ORIENTED_EDGE('',*,*,#49747,.F.);
#65740=ORIENTED_EDGE('',*,*,#49753,.T.);
#65741=ORIENTED_EDGE('',*,*,#49754,.T.);
#65742=ORIENTED_EDGE('',*,*,#49755,.F.);
#65743=ORIENTED_EDGE('',*,*,#49751,.F.);
#65744=ORIENTED_EDGE('',*,*,#49756,.T.);
#65745=ORIENTED_EDGE('',*,*,#49749,.T.);
#65746=ORIENTED_EDGE('',*,*,#49757,.F.);
#65747=ORIENTED_EDGE('',*,*,#49754,.F.);
#65748=ORIENTED_EDGE('',*,*,#49758,.T.);
#65749=ORIENTED_EDGE('',*,*,#49759,.T.);
#65750=ORIENTED_EDGE('',*,*,#49760,.F.);
#65751=ORIENTED_EDGE('',*,*,#49761,.F.);
#65752=ORIENTED_EDGE('',*,*,#49762,.T.);
#65753=ORIENTED_EDGE('',*,*,#49763,.T.);
#65754=ORIENTED_EDGE('',*,*,#49764,.F.);
#65755=ORIENTED_EDGE('',*,*,#49759,.F.);
#65756=ORIENTED_EDGE('',*,*,#49765,.T.);
#65757=ORIENTED_EDGE('',*,*,#49766,.T.);
#65758=ORIENTED_EDGE('',*,*,#49767,.F.);
#65759=ORIENTED_EDGE('',*,*,#49763,.F.);
#65760=ORIENTED_EDGE('',*,*,#49768,.T.);
#65761=ORIENTED_EDGE('',*,*,#49761,.T.);
#65762=ORIENTED_EDGE('',*,*,#49769,.F.);
#65763=ORIENTED_EDGE('',*,*,#49766,.F.);
#65764=ORIENTED_EDGE('',*,*,#49770,.T.);
#65765=ORIENTED_EDGE('',*,*,#49771,.T.);
#65766=ORIENTED_EDGE('',*,*,#49772,.F.);
#65767=ORIENTED_EDGE('',*,*,#49773,.F.);
#65768=ORIENTED_EDGE('',*,*,#49774,.T.);
#65769=ORIENTED_EDGE('',*,*,#49775,.T.);
#65770=ORIENTED_EDGE('',*,*,#49776,.F.);
#65771=ORIENTED_EDGE('',*,*,#49771,.F.);
#65772=ORIENTED_EDGE('',*,*,#49777,.T.);
#65773=ORIENTED_EDGE('',*,*,#49778,.T.);
#65774=ORIENTED_EDGE('',*,*,#49779,.F.);
#65775=ORIENTED_EDGE('',*,*,#49775,.F.);
#65776=ORIENTED_EDGE('',*,*,#49780,.T.);
#65777=ORIENTED_EDGE('',*,*,#49773,.T.);
#65778=ORIENTED_EDGE('',*,*,#49781,.F.);
#65779=ORIENTED_EDGE('',*,*,#49778,.F.);
#65780=ORIENTED_EDGE('',*,*,#49782,.T.);
#65781=ORIENTED_EDGE('',*,*,#49783,.T.);
#65782=ORIENTED_EDGE('',*,*,#49784,.F.);
#65783=ORIENTED_EDGE('',*,*,#49785,.F.);
#65784=ORIENTED_EDGE('',*,*,#49786,.T.);
#65785=ORIENTED_EDGE('',*,*,#49787,.T.);
#65786=ORIENTED_EDGE('',*,*,#49788,.F.);
#65787=ORIENTED_EDGE('',*,*,#49783,.F.);
#65788=ORIENTED_EDGE('',*,*,#49789,.T.);
#65789=ORIENTED_EDGE('',*,*,#49790,.T.);
#65790=ORIENTED_EDGE('',*,*,#49791,.F.);
#65791=ORIENTED_EDGE('',*,*,#49787,.F.);
#65792=ORIENTED_EDGE('',*,*,#49792,.T.);
#65793=ORIENTED_EDGE('',*,*,#49785,.T.);
#65794=ORIENTED_EDGE('',*,*,#49793,.F.);
#65795=ORIENTED_EDGE('',*,*,#49790,.F.);
#65796=ORIENTED_EDGE('',*,*,#49794,.T.);
#65797=ORIENTED_EDGE('',*,*,#49795,.T.);
#65798=ORIENTED_EDGE('',*,*,#49796,.F.);
#65799=ORIENTED_EDGE('',*,*,#49797,.F.);
#65800=ORIENTED_EDGE('',*,*,#49798,.T.);
#65801=ORIENTED_EDGE('',*,*,#49799,.T.);
#65802=ORIENTED_EDGE('',*,*,#49800,.F.);
#65803=ORIENTED_EDGE('',*,*,#49795,.F.);
#65804=ORIENTED_EDGE('',*,*,#49801,.T.);
#65805=ORIENTED_EDGE('',*,*,#49802,.T.);
#65806=ORIENTED_EDGE('',*,*,#49803,.F.);
#65807=ORIENTED_EDGE('',*,*,#49799,.F.);
#65808=ORIENTED_EDGE('',*,*,#49804,.T.);
#65809=ORIENTED_EDGE('',*,*,#49797,.T.);
#65810=ORIENTED_EDGE('',*,*,#49805,.F.);
#65811=ORIENTED_EDGE('',*,*,#49802,.F.);
#65812=ORIENTED_EDGE('',*,*,#49806,.T.);
#65813=ORIENTED_EDGE('',*,*,#49807,.T.);
#65814=ORIENTED_EDGE('',*,*,#49808,.F.);
#65815=ORIENTED_EDGE('',*,*,#49809,.F.);
#65816=ORIENTED_EDGE('',*,*,#49810,.T.);
#65817=ORIENTED_EDGE('',*,*,#49811,.T.);
#65818=ORIENTED_EDGE('',*,*,#49812,.F.);
#65819=ORIENTED_EDGE('',*,*,#49807,.F.);
#65820=ORIENTED_EDGE('',*,*,#49813,.T.);
#65821=ORIENTED_EDGE('',*,*,#49814,.T.);
#65822=ORIENTED_EDGE('',*,*,#49815,.F.);
#65823=ORIENTED_EDGE('',*,*,#49811,.F.);
#65824=ORIENTED_EDGE('',*,*,#49816,.T.);
#65825=ORIENTED_EDGE('',*,*,#49809,.T.);
#65826=ORIENTED_EDGE('',*,*,#49817,.F.);
#65827=ORIENTED_EDGE('',*,*,#49814,.F.);
#65828=ORIENTED_EDGE('',*,*,#49818,.T.);
#65829=ORIENTED_EDGE('',*,*,#49819,.T.);
#65830=ORIENTED_EDGE('',*,*,#49820,.F.);
#65831=ORIENTED_EDGE('',*,*,#49821,.F.);
#65832=ORIENTED_EDGE('',*,*,#49822,.T.);
#65833=ORIENTED_EDGE('',*,*,#49823,.T.);
#65834=ORIENTED_EDGE('',*,*,#49824,.F.);
#65835=ORIENTED_EDGE('',*,*,#49819,.F.);
#65836=ORIENTED_EDGE('',*,*,#49825,.T.);
#65837=ORIENTED_EDGE('',*,*,#49826,.T.);
#65838=ORIENTED_EDGE('',*,*,#49827,.F.);
#65839=ORIENTED_EDGE('',*,*,#49823,.F.);
#65840=ORIENTED_EDGE('',*,*,#49828,.T.);
#65841=ORIENTED_EDGE('',*,*,#49821,.T.);
#65842=ORIENTED_EDGE('',*,*,#49829,.F.);
#65843=ORIENTED_EDGE('',*,*,#49826,.F.);
#65844=ORIENTED_EDGE('',*,*,#49830,.T.);
#65845=ORIENTED_EDGE('',*,*,#49831,.T.);
#65846=ORIENTED_EDGE('',*,*,#49832,.F.);
#65847=ORIENTED_EDGE('',*,*,#49833,.F.);
#65848=ORIENTED_EDGE('',*,*,#49834,.T.);
#65849=ORIENTED_EDGE('',*,*,#49835,.T.);
#65850=ORIENTED_EDGE('',*,*,#49836,.F.);
#65851=ORIENTED_EDGE('',*,*,#49831,.F.);
#65852=ORIENTED_EDGE('',*,*,#49837,.T.);
#65853=ORIENTED_EDGE('',*,*,#49838,.T.);
#65854=ORIENTED_EDGE('',*,*,#49839,.F.);
#65855=ORIENTED_EDGE('',*,*,#49835,.F.);
#65856=ORIENTED_EDGE('',*,*,#49840,.T.);
#65857=ORIENTED_EDGE('',*,*,#49833,.T.);
#65858=ORIENTED_EDGE('',*,*,#49841,.F.);
#65859=ORIENTED_EDGE('',*,*,#49838,.F.);
#65860=ORIENTED_EDGE('',*,*,#49842,.T.);
#65861=ORIENTED_EDGE('',*,*,#49843,.T.);
#65862=ORIENTED_EDGE('',*,*,#49844,.F.);
#65863=ORIENTED_EDGE('',*,*,#49845,.F.);
#65864=ORIENTED_EDGE('',*,*,#49846,.T.);
#65865=ORIENTED_EDGE('',*,*,#49847,.T.);
#65866=ORIENTED_EDGE('',*,*,#49848,.F.);
#65867=ORIENTED_EDGE('',*,*,#49843,.F.);
#65868=ORIENTED_EDGE('',*,*,#49849,.T.);
#65869=ORIENTED_EDGE('',*,*,#49850,.T.);
#65870=ORIENTED_EDGE('',*,*,#49851,.F.);
#65871=ORIENTED_EDGE('',*,*,#49847,.F.);
#65872=ORIENTED_EDGE('',*,*,#49852,.T.);
#65873=ORIENTED_EDGE('',*,*,#49845,.T.);
#65874=ORIENTED_EDGE('',*,*,#49853,.F.);
#65875=ORIENTED_EDGE('',*,*,#49850,.F.);
#65876=ORIENTED_EDGE('',*,*,#49854,.T.);
#65877=ORIENTED_EDGE('',*,*,#49855,.T.);
#65878=ORIENTED_EDGE('',*,*,#49856,.F.);
#65879=ORIENTED_EDGE('',*,*,#49857,.F.);
#65880=ORIENTED_EDGE('',*,*,#49858,.T.);
#65881=ORIENTED_EDGE('',*,*,#49859,.T.);
#65882=ORIENTED_EDGE('',*,*,#49860,.F.);
#65883=ORIENTED_EDGE('',*,*,#49855,.F.);
#65884=ORIENTED_EDGE('',*,*,#49861,.T.);
#65885=ORIENTED_EDGE('',*,*,#49862,.T.);
#65886=ORIENTED_EDGE('',*,*,#49863,.F.);
#65887=ORIENTED_EDGE('',*,*,#49859,.F.);
#65888=ORIENTED_EDGE('',*,*,#49864,.T.);
#65889=ORIENTED_EDGE('',*,*,#49857,.T.);
#65890=ORIENTED_EDGE('',*,*,#49865,.F.);
#65891=ORIENTED_EDGE('',*,*,#49862,.F.);
#65892=ORIENTED_EDGE('',*,*,#49866,.T.);
#65893=ORIENTED_EDGE('',*,*,#49867,.T.);
#65894=ORIENTED_EDGE('',*,*,#49868,.F.);
#65895=ORIENTED_EDGE('',*,*,#49869,.F.);
#65896=ORIENTED_EDGE('',*,*,#49870,.T.);
#65897=ORIENTED_EDGE('',*,*,#49871,.T.);
#65898=ORIENTED_EDGE('',*,*,#49872,.F.);
#65899=ORIENTED_EDGE('',*,*,#49867,.F.);
#65900=ORIENTED_EDGE('',*,*,#49873,.T.);
#65901=ORIENTED_EDGE('',*,*,#49874,.T.);
#65902=ORIENTED_EDGE('',*,*,#49875,.F.);
#65903=ORIENTED_EDGE('',*,*,#49871,.F.);
#65904=ORIENTED_EDGE('',*,*,#49876,.T.);
#65905=ORIENTED_EDGE('',*,*,#49869,.T.);
#65906=ORIENTED_EDGE('',*,*,#49877,.F.);
#65907=ORIENTED_EDGE('',*,*,#49874,.F.);
#65908=ORIENTED_EDGE('',*,*,#49878,.T.);
#65909=ORIENTED_EDGE('',*,*,#49879,.T.);
#65910=ORIENTED_EDGE('',*,*,#49880,.F.);
#65911=ORIENTED_EDGE('',*,*,#49881,.F.);
#65912=ORIENTED_EDGE('',*,*,#49882,.T.);
#65913=ORIENTED_EDGE('',*,*,#49883,.T.);
#65914=ORIENTED_EDGE('',*,*,#49884,.F.);
#65915=ORIENTED_EDGE('',*,*,#49879,.F.);
#65916=ORIENTED_EDGE('',*,*,#49885,.T.);
#65917=ORIENTED_EDGE('',*,*,#49886,.T.);
#65918=ORIENTED_EDGE('',*,*,#49887,.F.);
#65919=ORIENTED_EDGE('',*,*,#49883,.F.);
#65920=ORIENTED_EDGE('',*,*,#49888,.T.);
#65921=ORIENTED_EDGE('',*,*,#49881,.T.);
#65922=ORIENTED_EDGE('',*,*,#49889,.F.);
#65923=ORIENTED_EDGE('',*,*,#49886,.F.);
#65924=ORIENTED_EDGE('',*,*,#49890,.T.);
#65925=ORIENTED_EDGE('',*,*,#49891,.T.);
#65926=ORIENTED_EDGE('',*,*,#49892,.F.);
#65927=ORIENTED_EDGE('',*,*,#49893,.F.);
#65928=ORIENTED_EDGE('',*,*,#49894,.T.);
#65929=ORIENTED_EDGE('',*,*,#49895,.T.);
#65930=ORIENTED_EDGE('',*,*,#49896,.F.);
#65931=ORIENTED_EDGE('',*,*,#49891,.F.);
#65932=ORIENTED_EDGE('',*,*,#49897,.T.);
#65933=ORIENTED_EDGE('',*,*,#49898,.T.);
#65934=ORIENTED_EDGE('',*,*,#49899,.F.);
#65935=ORIENTED_EDGE('',*,*,#49895,.F.);
#65936=ORIENTED_EDGE('',*,*,#49900,.T.);
#65937=ORIENTED_EDGE('',*,*,#49893,.T.);
#65938=ORIENTED_EDGE('',*,*,#49901,.F.);
#65939=ORIENTED_EDGE('',*,*,#49898,.F.);
#65940=ORIENTED_EDGE('',*,*,#49902,.T.);
#65941=ORIENTED_EDGE('',*,*,#49903,.T.);
#65942=ORIENTED_EDGE('',*,*,#49904,.F.);
#65943=ORIENTED_EDGE('',*,*,#49905,.F.);
#65944=ORIENTED_EDGE('',*,*,#49906,.T.);
#65945=ORIENTED_EDGE('',*,*,#49907,.T.);
#65946=ORIENTED_EDGE('',*,*,#49908,.F.);
#65947=ORIENTED_EDGE('',*,*,#49903,.F.);
#65948=ORIENTED_EDGE('',*,*,#49909,.T.);
#65949=ORIENTED_EDGE('',*,*,#49910,.T.);
#65950=ORIENTED_EDGE('',*,*,#49911,.F.);
#65951=ORIENTED_EDGE('',*,*,#49907,.F.);
#65952=ORIENTED_EDGE('',*,*,#49912,.T.);
#65953=ORIENTED_EDGE('',*,*,#49905,.T.);
#65954=ORIENTED_EDGE('',*,*,#49913,.F.);
#65955=ORIENTED_EDGE('',*,*,#49910,.F.);
#65956=ORIENTED_EDGE('',*,*,#49914,.T.);
#65957=ORIENTED_EDGE('',*,*,#49915,.T.);
#65958=ORIENTED_EDGE('',*,*,#49916,.F.);
#65959=ORIENTED_EDGE('',*,*,#49917,.F.);
#65960=ORIENTED_EDGE('',*,*,#49918,.T.);
#65961=ORIENTED_EDGE('',*,*,#49919,.T.);
#65962=ORIENTED_EDGE('',*,*,#49920,.F.);
#65963=ORIENTED_EDGE('',*,*,#49915,.F.);
#65964=ORIENTED_EDGE('',*,*,#49921,.T.);
#65965=ORIENTED_EDGE('',*,*,#49922,.T.);
#65966=ORIENTED_EDGE('',*,*,#49923,.F.);
#65967=ORIENTED_EDGE('',*,*,#49919,.F.);
#65968=ORIENTED_EDGE('',*,*,#49924,.T.);
#65969=ORIENTED_EDGE('',*,*,#49917,.T.);
#65970=ORIENTED_EDGE('',*,*,#49925,.F.);
#65971=ORIENTED_EDGE('',*,*,#49922,.F.);
#65972=ORIENTED_EDGE('',*,*,#49926,.T.);
#65973=ORIENTED_EDGE('',*,*,#49927,.T.);
#65974=ORIENTED_EDGE('',*,*,#49928,.F.);
#65975=ORIENTED_EDGE('',*,*,#49929,.F.);
#65976=ORIENTED_EDGE('',*,*,#49930,.T.);
#65977=ORIENTED_EDGE('',*,*,#49931,.T.);
#65978=ORIENTED_EDGE('',*,*,#49932,.F.);
#65979=ORIENTED_EDGE('',*,*,#49927,.F.);
#65980=ORIENTED_EDGE('',*,*,#49933,.T.);
#65981=ORIENTED_EDGE('',*,*,#49934,.T.);
#65982=ORIENTED_EDGE('',*,*,#49935,.F.);
#65983=ORIENTED_EDGE('',*,*,#49931,.F.);
#65984=ORIENTED_EDGE('',*,*,#49936,.T.);
#65985=ORIENTED_EDGE('',*,*,#49929,.T.);
#65986=ORIENTED_EDGE('',*,*,#49937,.F.);
#65987=ORIENTED_EDGE('',*,*,#49934,.F.);
#65988=ORIENTED_EDGE('',*,*,#49938,.T.);
#65989=ORIENTED_EDGE('',*,*,#49939,.T.);
#65990=ORIENTED_EDGE('',*,*,#49940,.F.);
#65991=ORIENTED_EDGE('',*,*,#49941,.F.);
#65992=ORIENTED_EDGE('',*,*,#49942,.T.);
#65993=ORIENTED_EDGE('',*,*,#49943,.T.);
#65994=ORIENTED_EDGE('',*,*,#49944,.F.);
#65995=ORIENTED_EDGE('',*,*,#49939,.F.);
#65996=ORIENTED_EDGE('',*,*,#49945,.T.);
#65997=ORIENTED_EDGE('',*,*,#49946,.T.);
#65998=ORIENTED_EDGE('',*,*,#49947,.F.);
#65999=ORIENTED_EDGE('',*,*,#49943,.F.);
#66000=ORIENTED_EDGE('',*,*,#49948,.T.);
#66001=ORIENTED_EDGE('',*,*,#49941,.T.);
#66002=ORIENTED_EDGE('',*,*,#49949,.F.);
#66003=ORIENTED_EDGE('',*,*,#49946,.F.);
#66004=ORIENTED_EDGE('',*,*,#49950,.T.);
#66005=ORIENTED_EDGE('',*,*,#49951,.T.);
#66006=ORIENTED_EDGE('',*,*,#49952,.F.);
#66007=ORIENTED_EDGE('',*,*,#49953,.F.);
#66008=ORIENTED_EDGE('',*,*,#49954,.T.);
#66009=ORIENTED_EDGE('',*,*,#49955,.T.);
#66010=ORIENTED_EDGE('',*,*,#49956,.F.);
#66011=ORIENTED_EDGE('',*,*,#49951,.F.);
#66012=ORIENTED_EDGE('',*,*,#49957,.T.);
#66013=ORIENTED_EDGE('',*,*,#49958,.T.);
#66014=ORIENTED_EDGE('',*,*,#49959,.F.);
#66015=ORIENTED_EDGE('',*,*,#49955,.F.);
#66016=ORIENTED_EDGE('',*,*,#49960,.T.);
#66017=ORIENTED_EDGE('',*,*,#49953,.T.);
#66018=ORIENTED_EDGE('',*,*,#49961,.F.);
#66019=ORIENTED_EDGE('',*,*,#49958,.F.);
#66020=ORIENTED_EDGE('',*,*,#49962,.T.);
#66021=ORIENTED_EDGE('',*,*,#49963,.T.);
#66022=ORIENTED_EDGE('',*,*,#49964,.F.);
#66023=ORIENTED_EDGE('',*,*,#49965,.F.);
#66024=ORIENTED_EDGE('',*,*,#49966,.T.);
#66025=ORIENTED_EDGE('',*,*,#49967,.T.);
#66026=ORIENTED_EDGE('',*,*,#49968,.F.);
#66027=ORIENTED_EDGE('',*,*,#49963,.F.);
#66028=ORIENTED_EDGE('',*,*,#49969,.T.);
#66029=ORIENTED_EDGE('',*,*,#49970,.T.);
#66030=ORIENTED_EDGE('',*,*,#49971,.F.);
#66031=ORIENTED_EDGE('',*,*,#49967,.F.);
#66032=ORIENTED_EDGE('',*,*,#49972,.T.);
#66033=ORIENTED_EDGE('',*,*,#49965,.T.);
#66034=ORIENTED_EDGE('',*,*,#49973,.F.);
#66035=ORIENTED_EDGE('',*,*,#49970,.F.);
#66036=ORIENTED_EDGE('',*,*,#49974,.T.);
#66037=ORIENTED_EDGE('',*,*,#49975,.T.);
#66038=ORIENTED_EDGE('',*,*,#49976,.F.);
#66039=ORIENTED_EDGE('',*,*,#49977,.F.);
#66040=ORIENTED_EDGE('',*,*,#49978,.T.);
#66041=ORIENTED_EDGE('',*,*,#49979,.T.);
#66042=ORIENTED_EDGE('',*,*,#49980,.F.);
#66043=ORIENTED_EDGE('',*,*,#49975,.F.);
#66044=ORIENTED_EDGE('',*,*,#49981,.T.);
#66045=ORIENTED_EDGE('',*,*,#49982,.T.);
#66046=ORIENTED_EDGE('',*,*,#49983,.F.);
#66047=ORIENTED_EDGE('',*,*,#49979,.F.);
#66048=ORIENTED_EDGE('',*,*,#49984,.T.);
#66049=ORIENTED_EDGE('',*,*,#49977,.T.);
#66050=ORIENTED_EDGE('',*,*,#49985,.F.);
#66051=ORIENTED_EDGE('',*,*,#49982,.F.);
#66052=ORIENTED_EDGE('',*,*,#49986,.T.);
#66053=ORIENTED_EDGE('',*,*,#49987,.T.);
#66054=ORIENTED_EDGE('',*,*,#49988,.F.);
#66055=ORIENTED_EDGE('',*,*,#49989,.F.);
#66056=ORIENTED_EDGE('',*,*,#49990,.T.);
#66057=ORIENTED_EDGE('',*,*,#49991,.T.);
#66058=ORIENTED_EDGE('',*,*,#49992,.F.);
#66059=ORIENTED_EDGE('',*,*,#49987,.F.);
#66060=ORIENTED_EDGE('',*,*,#49993,.T.);
#66061=ORIENTED_EDGE('',*,*,#49994,.T.);
#66062=ORIENTED_EDGE('',*,*,#49995,.F.);
#66063=ORIENTED_EDGE('',*,*,#49991,.F.);
#66064=ORIENTED_EDGE('',*,*,#49996,.T.);
#66065=ORIENTED_EDGE('',*,*,#49989,.T.);
#66066=ORIENTED_EDGE('',*,*,#49997,.F.);
#66067=ORIENTED_EDGE('',*,*,#49994,.F.);
#66068=ORIENTED_EDGE('',*,*,#49998,.T.);
#66069=ORIENTED_EDGE('',*,*,#49999,.T.);
#66070=ORIENTED_EDGE('',*,*,#50000,.F.);
#66071=ORIENTED_EDGE('',*,*,#50001,.F.);
#66072=ORIENTED_EDGE('',*,*,#50002,.T.);
#66073=ORIENTED_EDGE('',*,*,#50003,.T.);
#66074=ORIENTED_EDGE('',*,*,#50004,.F.);
#66075=ORIENTED_EDGE('',*,*,#49999,.F.);
#66076=ORIENTED_EDGE('',*,*,#50005,.T.);
#66077=ORIENTED_EDGE('',*,*,#50006,.T.);
#66078=ORIENTED_EDGE('',*,*,#50007,.F.);
#66079=ORIENTED_EDGE('',*,*,#50003,.F.);
#66080=ORIENTED_EDGE('',*,*,#50008,.T.);
#66081=ORIENTED_EDGE('',*,*,#50001,.T.);
#66082=ORIENTED_EDGE('',*,*,#50009,.F.);
#66083=ORIENTED_EDGE('',*,*,#50006,.F.);
#66084=ORIENTED_EDGE('',*,*,#50010,.T.);
#66085=ORIENTED_EDGE('',*,*,#50011,.T.);
#66086=ORIENTED_EDGE('',*,*,#50012,.F.);
#66087=ORIENTED_EDGE('',*,*,#50013,.F.);
#66088=ORIENTED_EDGE('',*,*,#50014,.T.);
#66089=ORIENTED_EDGE('',*,*,#50015,.T.);
#66090=ORIENTED_EDGE('',*,*,#50016,.F.);
#66091=ORIENTED_EDGE('',*,*,#50011,.F.);
#66092=ORIENTED_EDGE('',*,*,#50017,.T.);
#66093=ORIENTED_EDGE('',*,*,#50018,.T.);
#66094=ORIENTED_EDGE('',*,*,#50019,.F.);
#66095=ORIENTED_EDGE('',*,*,#50015,.F.);
#66096=ORIENTED_EDGE('',*,*,#50020,.T.);
#66097=ORIENTED_EDGE('',*,*,#50013,.T.);
#66098=ORIENTED_EDGE('',*,*,#50021,.F.);
#66099=ORIENTED_EDGE('',*,*,#50018,.F.);
#66100=ORIENTED_EDGE('',*,*,#50022,.T.);
#66101=ORIENTED_EDGE('',*,*,#50023,.T.);
#66102=ORIENTED_EDGE('',*,*,#50024,.F.);
#66103=ORIENTED_EDGE('',*,*,#50025,.F.);
#66104=ORIENTED_EDGE('',*,*,#50026,.T.);
#66105=ORIENTED_EDGE('',*,*,#50027,.T.);
#66106=ORIENTED_EDGE('',*,*,#50028,.F.);
#66107=ORIENTED_EDGE('',*,*,#50023,.F.);
#66108=ORIENTED_EDGE('',*,*,#50029,.T.);
#66109=ORIENTED_EDGE('',*,*,#50030,.T.);
#66110=ORIENTED_EDGE('',*,*,#50031,.F.);
#66111=ORIENTED_EDGE('',*,*,#50027,.F.);
#66112=ORIENTED_EDGE('',*,*,#50032,.T.);
#66113=ORIENTED_EDGE('',*,*,#50025,.T.);
#66114=ORIENTED_EDGE('',*,*,#50033,.F.);
#66115=ORIENTED_EDGE('',*,*,#50030,.F.);
#66116=ORIENTED_EDGE('',*,*,#50034,.T.);
#66117=ORIENTED_EDGE('',*,*,#50035,.T.);
#66118=ORIENTED_EDGE('',*,*,#50036,.F.);
#66119=ORIENTED_EDGE('',*,*,#50037,.F.);
#66120=ORIENTED_EDGE('',*,*,#50038,.T.);
#66121=ORIENTED_EDGE('',*,*,#50039,.T.);
#66122=ORIENTED_EDGE('',*,*,#50040,.F.);
#66123=ORIENTED_EDGE('',*,*,#50035,.F.);
#66124=ORIENTED_EDGE('',*,*,#50041,.T.);
#66125=ORIENTED_EDGE('',*,*,#50042,.T.);
#66126=ORIENTED_EDGE('',*,*,#50043,.F.);
#66127=ORIENTED_EDGE('',*,*,#50039,.F.);
#66128=ORIENTED_EDGE('',*,*,#50044,.T.);
#66129=ORIENTED_EDGE('',*,*,#50037,.T.);
#66130=ORIENTED_EDGE('',*,*,#50045,.F.);
#66131=ORIENTED_EDGE('',*,*,#50042,.F.);
#66132=ORIENTED_EDGE('',*,*,#50046,.T.);
#66133=ORIENTED_EDGE('',*,*,#50047,.T.);
#66134=ORIENTED_EDGE('',*,*,#50048,.F.);
#66135=ORIENTED_EDGE('',*,*,#50049,.F.);
#66136=ORIENTED_EDGE('',*,*,#50050,.T.);
#66137=ORIENTED_EDGE('',*,*,#50051,.T.);
#66138=ORIENTED_EDGE('',*,*,#50052,.F.);
#66139=ORIENTED_EDGE('',*,*,#50047,.F.);
#66140=ORIENTED_EDGE('',*,*,#50053,.T.);
#66141=ORIENTED_EDGE('',*,*,#50054,.T.);
#66142=ORIENTED_EDGE('',*,*,#50055,.F.);
#66143=ORIENTED_EDGE('',*,*,#50051,.F.);
#66144=ORIENTED_EDGE('',*,*,#50056,.T.);
#66145=ORIENTED_EDGE('',*,*,#50049,.T.);
#66146=ORIENTED_EDGE('',*,*,#50057,.F.);
#66147=ORIENTED_EDGE('',*,*,#50054,.F.);
#66148=ORIENTED_EDGE('',*,*,#50058,.T.);
#66149=ORIENTED_EDGE('',*,*,#50059,.T.);
#66150=ORIENTED_EDGE('',*,*,#50060,.F.);
#66151=ORIENTED_EDGE('',*,*,#50061,.F.);
#66152=ORIENTED_EDGE('',*,*,#50062,.T.);
#66153=ORIENTED_EDGE('',*,*,#50063,.T.);
#66154=ORIENTED_EDGE('',*,*,#50064,.F.);
#66155=ORIENTED_EDGE('',*,*,#50059,.F.);
#66156=ORIENTED_EDGE('',*,*,#50065,.T.);
#66157=ORIENTED_EDGE('',*,*,#50066,.T.);
#66158=ORIENTED_EDGE('',*,*,#50067,.F.);
#66159=ORIENTED_EDGE('',*,*,#50063,.F.);
#66160=ORIENTED_EDGE('',*,*,#50068,.T.);
#66161=ORIENTED_EDGE('',*,*,#50061,.T.);
#66162=ORIENTED_EDGE('',*,*,#50069,.F.);
#66163=ORIENTED_EDGE('',*,*,#50066,.F.);
#66164=ORIENTED_EDGE('',*,*,#50070,.T.);
#66165=ORIENTED_EDGE('',*,*,#50071,.T.);
#66166=ORIENTED_EDGE('',*,*,#50072,.F.);
#66167=ORIENTED_EDGE('',*,*,#50073,.F.);
#66168=ORIENTED_EDGE('',*,*,#50074,.T.);
#66169=ORIENTED_EDGE('',*,*,#50075,.T.);
#66170=ORIENTED_EDGE('',*,*,#50076,.F.);
#66171=ORIENTED_EDGE('',*,*,#50071,.F.);
#66172=ORIENTED_EDGE('',*,*,#50077,.T.);
#66173=ORIENTED_EDGE('',*,*,#50078,.T.);
#66174=ORIENTED_EDGE('',*,*,#50079,.F.);
#66175=ORIENTED_EDGE('',*,*,#50075,.F.);
#66176=ORIENTED_EDGE('',*,*,#50080,.T.);
#66177=ORIENTED_EDGE('',*,*,#50073,.T.);
#66178=ORIENTED_EDGE('',*,*,#50081,.F.);
#66179=ORIENTED_EDGE('',*,*,#50078,.F.);
#66180=ORIENTED_EDGE('',*,*,#50082,.T.);
#66181=ORIENTED_EDGE('',*,*,#50083,.T.);
#66182=ORIENTED_EDGE('',*,*,#50084,.F.);
#66183=ORIENTED_EDGE('',*,*,#50085,.F.);
#66184=ORIENTED_EDGE('',*,*,#50086,.T.);
#66185=ORIENTED_EDGE('',*,*,#50087,.T.);
#66186=ORIENTED_EDGE('',*,*,#50088,.F.);
#66187=ORIENTED_EDGE('',*,*,#50083,.F.);
#66188=ORIENTED_EDGE('',*,*,#50089,.T.);
#66189=ORIENTED_EDGE('',*,*,#50090,.T.);
#66190=ORIENTED_EDGE('',*,*,#50091,.F.);
#66191=ORIENTED_EDGE('',*,*,#50087,.F.);
#66192=ORIENTED_EDGE('',*,*,#50092,.T.);
#66193=ORIENTED_EDGE('',*,*,#50085,.T.);
#66194=ORIENTED_EDGE('',*,*,#50093,.F.);
#66195=ORIENTED_EDGE('',*,*,#50090,.F.);
#66196=ORIENTED_EDGE('',*,*,#50094,.T.);
#66197=ORIENTED_EDGE('',*,*,#50095,.T.);
#66198=ORIENTED_EDGE('',*,*,#50096,.F.);
#66199=ORIENTED_EDGE('',*,*,#50097,.F.);
#66200=ORIENTED_EDGE('',*,*,#50098,.T.);
#66201=ORIENTED_EDGE('',*,*,#50099,.T.);
#66202=ORIENTED_EDGE('',*,*,#50100,.F.);
#66203=ORIENTED_EDGE('',*,*,#50095,.F.);
#66204=ORIENTED_EDGE('',*,*,#50101,.T.);
#66205=ORIENTED_EDGE('',*,*,#50102,.T.);
#66206=ORIENTED_EDGE('',*,*,#50103,.F.);
#66207=ORIENTED_EDGE('',*,*,#50099,.F.);
#66208=ORIENTED_EDGE('',*,*,#50104,.T.);
#66209=ORIENTED_EDGE('',*,*,#50097,.T.);
#66210=ORIENTED_EDGE('',*,*,#50105,.F.);
#66211=ORIENTED_EDGE('',*,*,#50102,.F.);
#66212=ORIENTED_EDGE('',*,*,#50106,.T.);
#66213=ORIENTED_EDGE('',*,*,#50107,.T.);
#66214=ORIENTED_EDGE('',*,*,#50108,.F.);
#66215=ORIENTED_EDGE('',*,*,#50109,.F.);
#66216=ORIENTED_EDGE('',*,*,#50110,.T.);
#66217=ORIENTED_EDGE('',*,*,#50111,.T.);
#66218=ORIENTED_EDGE('',*,*,#50112,.F.);
#66219=ORIENTED_EDGE('',*,*,#50107,.F.);
#66220=ORIENTED_EDGE('',*,*,#50113,.T.);
#66221=ORIENTED_EDGE('',*,*,#50114,.T.);
#66222=ORIENTED_EDGE('',*,*,#50115,.F.);
#66223=ORIENTED_EDGE('',*,*,#50111,.F.);
#66224=ORIENTED_EDGE('',*,*,#50116,.T.);
#66225=ORIENTED_EDGE('',*,*,#50109,.T.);
#66226=ORIENTED_EDGE('',*,*,#50117,.F.);
#66227=ORIENTED_EDGE('',*,*,#50114,.F.);
#66228=ORIENTED_EDGE('',*,*,#50118,.T.);
#66229=ORIENTED_EDGE('',*,*,#50119,.T.);
#66230=ORIENTED_EDGE('',*,*,#50120,.F.);
#66231=ORIENTED_EDGE('',*,*,#50121,.F.);
#66232=ORIENTED_EDGE('',*,*,#50122,.T.);
#66233=ORIENTED_EDGE('',*,*,#50123,.T.);
#66234=ORIENTED_EDGE('',*,*,#50124,.F.);
#66235=ORIENTED_EDGE('',*,*,#50119,.F.);
#66236=ORIENTED_EDGE('',*,*,#50125,.T.);
#66237=ORIENTED_EDGE('',*,*,#50126,.T.);
#66238=ORIENTED_EDGE('',*,*,#50127,.F.);
#66239=ORIENTED_EDGE('',*,*,#50123,.F.);
#66240=ORIENTED_EDGE('',*,*,#50128,.T.);
#66241=ORIENTED_EDGE('',*,*,#50121,.T.);
#66242=ORIENTED_EDGE('',*,*,#50129,.F.);
#66243=ORIENTED_EDGE('',*,*,#50126,.F.);
#66244=ORIENTED_EDGE('',*,*,#50130,.T.);
#66245=ORIENTED_EDGE('',*,*,#50131,.T.);
#66246=ORIENTED_EDGE('',*,*,#50132,.F.);
#66247=ORIENTED_EDGE('',*,*,#50133,.F.);
#66248=ORIENTED_EDGE('',*,*,#50134,.T.);
#66249=ORIENTED_EDGE('',*,*,#50135,.T.);
#66250=ORIENTED_EDGE('',*,*,#50136,.F.);
#66251=ORIENTED_EDGE('',*,*,#50131,.F.);
#66252=ORIENTED_EDGE('',*,*,#50137,.T.);
#66253=ORIENTED_EDGE('',*,*,#50138,.T.);
#66254=ORIENTED_EDGE('',*,*,#50139,.F.);
#66255=ORIENTED_EDGE('',*,*,#50135,.F.);
#66256=ORIENTED_EDGE('',*,*,#50140,.T.);
#66257=ORIENTED_EDGE('',*,*,#50133,.T.);
#66258=ORIENTED_EDGE('',*,*,#50141,.F.);
#66259=ORIENTED_EDGE('',*,*,#50138,.F.);
#66260=ORIENTED_EDGE('',*,*,#50142,.T.);
#66261=ORIENTED_EDGE('',*,*,#50143,.T.);
#66262=ORIENTED_EDGE('',*,*,#50144,.F.);
#66263=ORIENTED_EDGE('',*,*,#50145,.F.);
#66264=ORIENTED_EDGE('',*,*,#50146,.T.);
#66265=ORIENTED_EDGE('',*,*,#50147,.T.);
#66266=ORIENTED_EDGE('',*,*,#50148,.F.);
#66267=ORIENTED_EDGE('',*,*,#50143,.F.);
#66268=ORIENTED_EDGE('',*,*,#50149,.T.);
#66269=ORIENTED_EDGE('',*,*,#50150,.T.);
#66270=ORIENTED_EDGE('',*,*,#50151,.F.);
#66271=ORIENTED_EDGE('',*,*,#50147,.F.);
#66272=ORIENTED_EDGE('',*,*,#50152,.T.);
#66273=ORIENTED_EDGE('',*,*,#50145,.T.);
#66274=ORIENTED_EDGE('',*,*,#50153,.F.);
#66275=ORIENTED_EDGE('',*,*,#50150,.F.);
#66276=ORIENTED_EDGE('',*,*,#50154,.T.);
#66277=ORIENTED_EDGE('',*,*,#50155,.T.);
#66278=ORIENTED_EDGE('',*,*,#50156,.F.);
#66279=ORIENTED_EDGE('',*,*,#50157,.F.);
#66280=ORIENTED_EDGE('',*,*,#50158,.T.);
#66281=ORIENTED_EDGE('',*,*,#50159,.T.);
#66282=ORIENTED_EDGE('',*,*,#50160,.F.);
#66283=ORIENTED_EDGE('',*,*,#50155,.F.);
#66284=ORIENTED_EDGE('',*,*,#50161,.T.);
#66285=ORIENTED_EDGE('',*,*,#50162,.T.);
#66286=ORIENTED_EDGE('',*,*,#50163,.F.);
#66287=ORIENTED_EDGE('',*,*,#50159,.F.);
#66288=ORIENTED_EDGE('',*,*,#50164,.T.);
#66289=ORIENTED_EDGE('',*,*,#50157,.T.);
#66290=ORIENTED_EDGE('',*,*,#50165,.F.);
#66291=ORIENTED_EDGE('',*,*,#50162,.F.);
#66292=ORIENTED_EDGE('',*,*,#50166,.T.);
#66293=ORIENTED_EDGE('',*,*,#50167,.T.);
#66294=ORIENTED_EDGE('',*,*,#50168,.F.);
#66295=ORIENTED_EDGE('',*,*,#50169,.F.);
#66296=ORIENTED_EDGE('',*,*,#50170,.T.);
#66297=ORIENTED_EDGE('',*,*,#50171,.T.);
#66298=ORIENTED_EDGE('',*,*,#50172,.F.);
#66299=ORIENTED_EDGE('',*,*,#50167,.F.);
#66300=ORIENTED_EDGE('',*,*,#50173,.T.);
#66301=ORIENTED_EDGE('',*,*,#50174,.T.);
#66302=ORIENTED_EDGE('',*,*,#50175,.F.);
#66303=ORIENTED_EDGE('',*,*,#50171,.F.);
#66304=ORIENTED_EDGE('',*,*,#50176,.T.);
#66305=ORIENTED_EDGE('',*,*,#50169,.T.);
#66306=ORIENTED_EDGE('',*,*,#50177,.F.);
#66307=ORIENTED_EDGE('',*,*,#50174,.F.);
#66308=ORIENTED_EDGE('',*,*,#50178,.T.);
#66309=ORIENTED_EDGE('',*,*,#50179,.T.);
#66310=ORIENTED_EDGE('',*,*,#50180,.F.);
#66311=ORIENTED_EDGE('',*,*,#50181,.F.);
#66312=ORIENTED_EDGE('',*,*,#50182,.T.);
#66313=ORIENTED_EDGE('',*,*,#50183,.T.);
#66314=ORIENTED_EDGE('',*,*,#50184,.F.);
#66315=ORIENTED_EDGE('',*,*,#50179,.F.);
#66316=ORIENTED_EDGE('',*,*,#50185,.T.);
#66317=ORIENTED_EDGE('',*,*,#50186,.T.);
#66318=ORIENTED_EDGE('',*,*,#50187,.F.);
#66319=ORIENTED_EDGE('',*,*,#50183,.F.);
#66320=ORIENTED_EDGE('',*,*,#50188,.T.);
#66321=ORIENTED_EDGE('',*,*,#50181,.T.);
#66322=ORIENTED_EDGE('',*,*,#50189,.F.);
#66323=ORIENTED_EDGE('',*,*,#50186,.F.);
#66324=ORIENTED_EDGE('',*,*,#50190,.T.);
#66325=ORIENTED_EDGE('',*,*,#50191,.T.);
#66326=ORIENTED_EDGE('',*,*,#50192,.F.);
#66327=ORIENTED_EDGE('',*,*,#50193,.F.);
#66328=ORIENTED_EDGE('',*,*,#50194,.T.);
#66329=ORIENTED_EDGE('',*,*,#50195,.T.);
#66330=ORIENTED_EDGE('',*,*,#50196,.F.);
#66331=ORIENTED_EDGE('',*,*,#50191,.F.);
#66332=ORIENTED_EDGE('',*,*,#50197,.T.);
#66333=ORIENTED_EDGE('',*,*,#50198,.T.);
#66334=ORIENTED_EDGE('',*,*,#50199,.F.);
#66335=ORIENTED_EDGE('',*,*,#50195,.F.);
#66336=ORIENTED_EDGE('',*,*,#50200,.T.);
#66337=ORIENTED_EDGE('',*,*,#50193,.T.);
#66338=ORIENTED_EDGE('',*,*,#50201,.F.);
#66339=ORIENTED_EDGE('',*,*,#50198,.F.);
#66340=ORIENTED_EDGE('',*,*,#50202,.T.);
#66341=ORIENTED_EDGE('',*,*,#50203,.T.);
#66342=ORIENTED_EDGE('',*,*,#50204,.F.);
#66343=ORIENTED_EDGE('',*,*,#50205,.F.);
#66344=ORIENTED_EDGE('',*,*,#50206,.T.);
#66345=ORIENTED_EDGE('',*,*,#50207,.T.);
#66346=ORIENTED_EDGE('',*,*,#50208,.F.);
#66347=ORIENTED_EDGE('',*,*,#50203,.F.);
#66348=ORIENTED_EDGE('',*,*,#50209,.T.);
#66349=ORIENTED_EDGE('',*,*,#50210,.T.);
#66350=ORIENTED_EDGE('',*,*,#50211,.F.);
#66351=ORIENTED_EDGE('',*,*,#50207,.F.);
#66352=ORIENTED_EDGE('',*,*,#50212,.T.);
#66353=ORIENTED_EDGE('',*,*,#50205,.T.);
#66354=ORIENTED_EDGE('',*,*,#50213,.F.);
#66355=ORIENTED_EDGE('',*,*,#50210,.F.);
#66356=ORIENTED_EDGE('',*,*,#50214,.T.);
#66357=ORIENTED_EDGE('',*,*,#50215,.T.);
#66358=ORIENTED_EDGE('',*,*,#50216,.F.);
#66359=ORIENTED_EDGE('',*,*,#50217,.F.);
#66360=ORIENTED_EDGE('',*,*,#50218,.T.);
#66361=ORIENTED_EDGE('',*,*,#50219,.T.);
#66362=ORIENTED_EDGE('',*,*,#50220,.F.);
#66363=ORIENTED_EDGE('',*,*,#50215,.F.);
#66364=ORIENTED_EDGE('',*,*,#50221,.T.);
#66365=ORIENTED_EDGE('',*,*,#50222,.T.);
#66366=ORIENTED_EDGE('',*,*,#50223,.F.);
#66367=ORIENTED_EDGE('',*,*,#50219,.F.);
#66368=ORIENTED_EDGE('',*,*,#50224,.T.);
#66369=ORIENTED_EDGE('',*,*,#50217,.T.);
#66370=ORIENTED_EDGE('',*,*,#50225,.F.);
#66371=ORIENTED_EDGE('',*,*,#50222,.F.);
#66372=ORIENTED_EDGE('',*,*,#50226,.T.);
#66373=ORIENTED_EDGE('',*,*,#50227,.T.);
#66374=ORIENTED_EDGE('',*,*,#50228,.F.);
#66375=ORIENTED_EDGE('',*,*,#50229,.F.);
#66376=ORIENTED_EDGE('',*,*,#50230,.T.);
#66377=ORIENTED_EDGE('',*,*,#50231,.T.);
#66378=ORIENTED_EDGE('',*,*,#50232,.F.);
#66379=ORIENTED_EDGE('',*,*,#50227,.F.);
#66380=ORIENTED_EDGE('',*,*,#50233,.T.);
#66381=ORIENTED_EDGE('',*,*,#50234,.T.);
#66382=ORIENTED_EDGE('',*,*,#50235,.F.);
#66383=ORIENTED_EDGE('',*,*,#50231,.F.);
#66384=ORIENTED_EDGE('',*,*,#50236,.T.);
#66385=ORIENTED_EDGE('',*,*,#50229,.T.);
#66386=ORIENTED_EDGE('',*,*,#50237,.F.);
#66387=ORIENTED_EDGE('',*,*,#50234,.F.);
#66388=ORIENTED_EDGE('',*,*,#50238,.T.);
#66389=ORIENTED_EDGE('',*,*,#50239,.T.);
#66390=ORIENTED_EDGE('',*,*,#50240,.F.);
#66391=ORIENTED_EDGE('',*,*,#50241,.F.);
#66392=ORIENTED_EDGE('',*,*,#50242,.T.);
#66393=ORIENTED_EDGE('',*,*,#50243,.T.);
#66394=ORIENTED_EDGE('',*,*,#50244,.F.);
#66395=ORIENTED_EDGE('',*,*,#50239,.F.);
#66396=ORIENTED_EDGE('',*,*,#50245,.T.);
#66397=ORIENTED_EDGE('',*,*,#50246,.T.);
#66398=ORIENTED_EDGE('',*,*,#50247,.F.);
#66399=ORIENTED_EDGE('',*,*,#50243,.F.);
#66400=ORIENTED_EDGE('',*,*,#50248,.T.);
#66401=ORIENTED_EDGE('',*,*,#50241,.T.);
#66402=ORIENTED_EDGE('',*,*,#50249,.F.);
#66403=ORIENTED_EDGE('',*,*,#50246,.F.);
#66404=ORIENTED_EDGE('',*,*,#50250,.T.);
#66405=ORIENTED_EDGE('',*,*,#50251,.T.);
#66406=ORIENTED_EDGE('',*,*,#50252,.F.);
#66407=ORIENTED_EDGE('',*,*,#50253,.F.);
#66408=ORIENTED_EDGE('',*,*,#50254,.T.);
#66409=ORIENTED_EDGE('',*,*,#50255,.T.);
#66410=ORIENTED_EDGE('',*,*,#50256,.F.);
#66411=ORIENTED_EDGE('',*,*,#50251,.F.);
#66412=ORIENTED_EDGE('',*,*,#50257,.T.);
#66413=ORIENTED_EDGE('',*,*,#50258,.T.);
#66414=ORIENTED_EDGE('',*,*,#50259,.F.);
#66415=ORIENTED_EDGE('',*,*,#50255,.F.);
#66416=ORIENTED_EDGE('',*,*,#50260,.T.);
#66417=ORIENTED_EDGE('',*,*,#50253,.T.);
#66418=ORIENTED_EDGE('',*,*,#50261,.F.);
#66419=ORIENTED_EDGE('',*,*,#50258,.F.);
#66420=ORIENTED_EDGE('',*,*,#50262,.T.);
#66421=ORIENTED_EDGE('',*,*,#50263,.T.);
#66422=ORIENTED_EDGE('',*,*,#50264,.F.);
#66423=ORIENTED_EDGE('',*,*,#50265,.F.);
#66424=ORIENTED_EDGE('',*,*,#50266,.T.);
#66425=ORIENTED_EDGE('',*,*,#50267,.T.);
#66426=ORIENTED_EDGE('',*,*,#50268,.F.);
#66427=ORIENTED_EDGE('',*,*,#50263,.F.);
#66428=ORIENTED_EDGE('',*,*,#50269,.T.);
#66429=ORIENTED_EDGE('',*,*,#50270,.T.);
#66430=ORIENTED_EDGE('',*,*,#50271,.F.);
#66431=ORIENTED_EDGE('',*,*,#50267,.F.);
#66432=ORIENTED_EDGE('',*,*,#50272,.T.);
#66433=ORIENTED_EDGE('',*,*,#50265,.T.);
#66434=ORIENTED_EDGE('',*,*,#50273,.F.);
#66435=ORIENTED_EDGE('',*,*,#50270,.F.);
#66436=ORIENTED_EDGE('',*,*,#50274,.T.);
#66437=ORIENTED_EDGE('',*,*,#50275,.T.);
#66438=ORIENTED_EDGE('',*,*,#50276,.F.);
#66439=ORIENTED_EDGE('',*,*,#50277,.F.);
#66440=ORIENTED_EDGE('',*,*,#50278,.T.);
#66441=ORIENTED_EDGE('',*,*,#50279,.T.);
#66442=ORIENTED_EDGE('',*,*,#50280,.F.);
#66443=ORIENTED_EDGE('',*,*,#50275,.F.);
#66444=ORIENTED_EDGE('',*,*,#50281,.T.);
#66445=ORIENTED_EDGE('',*,*,#50282,.T.);
#66446=ORIENTED_EDGE('',*,*,#50283,.F.);
#66447=ORIENTED_EDGE('',*,*,#50279,.F.);
#66448=ORIENTED_EDGE('',*,*,#50284,.T.);
#66449=ORIENTED_EDGE('',*,*,#50277,.T.);
#66450=ORIENTED_EDGE('',*,*,#50285,.F.);
#66451=ORIENTED_EDGE('',*,*,#50282,.F.);
#66452=ORIENTED_EDGE('',*,*,#50286,.T.);
#66453=ORIENTED_EDGE('',*,*,#50287,.T.);
#66454=ORIENTED_EDGE('',*,*,#50288,.F.);
#66455=ORIENTED_EDGE('',*,*,#50289,.F.);
#66456=ORIENTED_EDGE('',*,*,#50290,.T.);
#66457=ORIENTED_EDGE('',*,*,#50291,.T.);
#66458=ORIENTED_EDGE('',*,*,#50292,.F.);
#66459=ORIENTED_EDGE('',*,*,#50287,.F.);
#66460=ORIENTED_EDGE('',*,*,#50293,.T.);
#66461=ORIENTED_EDGE('',*,*,#50294,.T.);
#66462=ORIENTED_EDGE('',*,*,#50295,.F.);
#66463=ORIENTED_EDGE('',*,*,#50291,.F.);
#66464=ORIENTED_EDGE('',*,*,#50296,.T.);
#66465=ORIENTED_EDGE('',*,*,#50289,.T.);
#66466=ORIENTED_EDGE('',*,*,#50297,.F.);
#66467=ORIENTED_EDGE('',*,*,#50294,.F.);
#66468=ORIENTED_EDGE('',*,*,#50298,.T.);
#66469=ORIENTED_EDGE('',*,*,#50299,.T.);
#66470=ORIENTED_EDGE('',*,*,#50300,.F.);
#66471=ORIENTED_EDGE('',*,*,#50301,.F.);
#66472=ORIENTED_EDGE('',*,*,#50302,.T.);
#66473=ORIENTED_EDGE('',*,*,#50303,.T.);
#66474=ORIENTED_EDGE('',*,*,#50304,.F.);
#66475=ORIENTED_EDGE('',*,*,#50299,.F.);
#66476=ORIENTED_EDGE('',*,*,#50305,.T.);
#66477=ORIENTED_EDGE('',*,*,#50306,.T.);
#66478=ORIENTED_EDGE('',*,*,#50307,.F.);
#66479=ORIENTED_EDGE('',*,*,#50303,.F.);
#66480=ORIENTED_EDGE('',*,*,#50308,.T.);
#66481=ORIENTED_EDGE('',*,*,#50301,.T.);
#66482=ORIENTED_EDGE('',*,*,#50309,.F.);
#66483=ORIENTED_EDGE('',*,*,#50306,.F.);
#66484=ORIENTED_EDGE('',*,*,#50310,.T.);
#66485=ORIENTED_EDGE('',*,*,#50311,.T.);
#66486=ORIENTED_EDGE('',*,*,#50312,.F.);
#66487=ORIENTED_EDGE('',*,*,#50313,.F.);
#66488=ORIENTED_EDGE('',*,*,#50314,.T.);
#66489=ORIENTED_EDGE('',*,*,#50315,.T.);
#66490=ORIENTED_EDGE('',*,*,#50316,.F.);
#66491=ORIENTED_EDGE('',*,*,#50311,.F.);
#66492=ORIENTED_EDGE('',*,*,#50317,.T.);
#66493=ORIENTED_EDGE('',*,*,#50318,.T.);
#66494=ORIENTED_EDGE('',*,*,#50319,.F.);
#66495=ORIENTED_EDGE('',*,*,#50315,.F.);
#66496=ORIENTED_EDGE('',*,*,#50320,.T.);
#66497=ORIENTED_EDGE('',*,*,#50313,.T.);
#66498=ORIENTED_EDGE('',*,*,#50321,.F.);
#66499=ORIENTED_EDGE('',*,*,#50318,.F.);
#66500=ORIENTED_EDGE('',*,*,#50322,.T.);
#66501=ORIENTED_EDGE('',*,*,#50323,.T.);
#66502=ORIENTED_EDGE('',*,*,#50324,.F.);
#66503=ORIENTED_EDGE('',*,*,#50325,.F.);
#66504=ORIENTED_EDGE('',*,*,#50326,.T.);
#66505=ORIENTED_EDGE('',*,*,#50327,.T.);
#66506=ORIENTED_EDGE('',*,*,#50328,.F.);
#66507=ORIENTED_EDGE('',*,*,#50323,.F.);
#66508=ORIENTED_EDGE('',*,*,#50329,.T.);
#66509=ORIENTED_EDGE('',*,*,#50330,.T.);
#66510=ORIENTED_EDGE('',*,*,#50331,.F.);
#66511=ORIENTED_EDGE('',*,*,#50327,.F.);
#66512=ORIENTED_EDGE('',*,*,#50332,.T.);
#66513=ORIENTED_EDGE('',*,*,#50325,.T.);
#66514=ORIENTED_EDGE('',*,*,#50333,.F.);
#66515=ORIENTED_EDGE('',*,*,#50330,.F.);
#66516=ORIENTED_EDGE('',*,*,#50334,.T.);
#66517=ORIENTED_EDGE('',*,*,#50335,.T.);
#66518=ORIENTED_EDGE('',*,*,#50336,.F.);
#66519=ORIENTED_EDGE('',*,*,#50337,.F.);
#66520=ORIENTED_EDGE('',*,*,#50338,.T.);
#66521=ORIENTED_EDGE('',*,*,#50339,.T.);
#66522=ORIENTED_EDGE('',*,*,#50340,.F.);
#66523=ORIENTED_EDGE('',*,*,#50335,.F.);
#66524=ORIENTED_EDGE('',*,*,#50341,.T.);
#66525=ORIENTED_EDGE('',*,*,#50342,.T.);
#66526=ORIENTED_EDGE('',*,*,#50343,.F.);
#66527=ORIENTED_EDGE('',*,*,#50339,.F.);
#66528=ORIENTED_EDGE('',*,*,#50344,.T.);
#66529=ORIENTED_EDGE('',*,*,#50337,.T.);
#66530=ORIENTED_EDGE('',*,*,#50345,.F.);
#66531=ORIENTED_EDGE('',*,*,#50342,.F.);
#66532=ORIENTED_EDGE('',*,*,#50346,.T.);
#66533=ORIENTED_EDGE('',*,*,#50347,.T.);
#66534=ORIENTED_EDGE('',*,*,#50348,.F.);
#66535=ORIENTED_EDGE('',*,*,#50349,.F.);
#66536=ORIENTED_EDGE('',*,*,#50350,.T.);
#66537=ORIENTED_EDGE('',*,*,#50351,.T.);
#66538=ORIENTED_EDGE('',*,*,#50352,.F.);
#66539=ORIENTED_EDGE('',*,*,#50347,.F.);
#66540=ORIENTED_EDGE('',*,*,#50353,.T.);
#66541=ORIENTED_EDGE('',*,*,#50354,.T.);
#66542=ORIENTED_EDGE('',*,*,#50355,.F.);
#66543=ORIENTED_EDGE('',*,*,#50351,.F.);
#66544=ORIENTED_EDGE('',*,*,#50356,.T.);
#66545=ORIENTED_EDGE('',*,*,#50349,.T.);
#66546=ORIENTED_EDGE('',*,*,#50357,.F.);
#66547=ORIENTED_EDGE('',*,*,#50354,.F.);
#66548=ORIENTED_EDGE('',*,*,#50358,.T.);
#66549=ORIENTED_EDGE('',*,*,#50359,.T.);
#66550=ORIENTED_EDGE('',*,*,#50360,.F.);
#66551=ORIENTED_EDGE('',*,*,#50361,.F.);
#66552=ORIENTED_EDGE('',*,*,#50362,.T.);
#66553=ORIENTED_EDGE('',*,*,#50363,.T.);
#66554=ORIENTED_EDGE('',*,*,#50364,.F.);
#66555=ORIENTED_EDGE('',*,*,#50359,.F.);
#66556=ORIENTED_EDGE('',*,*,#50365,.T.);
#66557=ORIENTED_EDGE('',*,*,#50366,.T.);
#66558=ORIENTED_EDGE('',*,*,#50367,.F.);
#66559=ORIENTED_EDGE('',*,*,#50363,.F.);
#66560=ORIENTED_EDGE('',*,*,#50368,.T.);
#66561=ORIENTED_EDGE('',*,*,#50361,.T.);
#66562=ORIENTED_EDGE('',*,*,#50369,.F.);
#66563=ORIENTED_EDGE('',*,*,#50366,.F.);
#66564=ORIENTED_EDGE('',*,*,#50370,.T.);
#66565=ORIENTED_EDGE('',*,*,#50371,.T.);
#66566=ORIENTED_EDGE('',*,*,#50372,.F.);
#66567=ORIENTED_EDGE('',*,*,#50373,.F.);
#66568=ORIENTED_EDGE('',*,*,#50374,.T.);
#66569=ORIENTED_EDGE('',*,*,#50375,.T.);
#66570=ORIENTED_EDGE('',*,*,#50376,.F.);
#66571=ORIENTED_EDGE('',*,*,#50371,.F.);
#66572=ORIENTED_EDGE('',*,*,#50377,.T.);
#66573=ORIENTED_EDGE('',*,*,#50378,.T.);
#66574=ORIENTED_EDGE('',*,*,#50379,.F.);
#66575=ORIENTED_EDGE('',*,*,#50375,.F.);
#66576=ORIENTED_EDGE('',*,*,#50380,.T.);
#66577=ORIENTED_EDGE('',*,*,#50373,.T.);
#66578=ORIENTED_EDGE('',*,*,#50381,.F.);
#66579=ORIENTED_EDGE('',*,*,#50378,.F.);
#66580=ORIENTED_EDGE('',*,*,#50382,.T.);
#66581=ORIENTED_EDGE('',*,*,#50383,.T.);
#66582=ORIENTED_EDGE('',*,*,#50384,.F.);
#66583=ORIENTED_EDGE('',*,*,#50385,.F.);
#66584=ORIENTED_EDGE('',*,*,#50386,.T.);
#66585=ORIENTED_EDGE('',*,*,#50387,.T.);
#66586=ORIENTED_EDGE('',*,*,#50388,.F.);
#66587=ORIENTED_EDGE('',*,*,#50383,.F.);
#66588=ORIENTED_EDGE('',*,*,#50389,.T.);
#66589=ORIENTED_EDGE('',*,*,#50390,.T.);
#66590=ORIENTED_EDGE('',*,*,#50391,.F.);
#66591=ORIENTED_EDGE('',*,*,#50387,.F.);
#66592=ORIENTED_EDGE('',*,*,#50392,.T.);
#66593=ORIENTED_EDGE('',*,*,#50385,.T.);
#66594=ORIENTED_EDGE('',*,*,#50393,.F.);
#66595=ORIENTED_EDGE('',*,*,#50390,.F.);
#66596=ORIENTED_EDGE('',*,*,#50394,.T.);
#66597=ORIENTED_EDGE('',*,*,#50395,.T.);
#66598=ORIENTED_EDGE('',*,*,#50396,.F.);
#66599=ORIENTED_EDGE('',*,*,#50397,.F.);
#66600=ORIENTED_EDGE('',*,*,#50398,.T.);
#66601=ORIENTED_EDGE('',*,*,#50399,.T.);
#66602=ORIENTED_EDGE('',*,*,#50400,.F.);
#66603=ORIENTED_EDGE('',*,*,#50395,.F.);
#66604=ORIENTED_EDGE('',*,*,#50401,.T.);
#66605=ORIENTED_EDGE('',*,*,#50402,.T.);
#66606=ORIENTED_EDGE('',*,*,#50403,.F.);
#66607=ORIENTED_EDGE('',*,*,#50399,.F.);
#66608=ORIENTED_EDGE('',*,*,#50404,.T.);
#66609=ORIENTED_EDGE('',*,*,#50397,.T.);
#66610=ORIENTED_EDGE('',*,*,#50405,.F.);
#66611=ORIENTED_EDGE('',*,*,#50402,.F.);
#66612=ORIENTED_EDGE('',*,*,#50406,.T.);
#66613=ORIENTED_EDGE('',*,*,#50407,.T.);
#66614=ORIENTED_EDGE('',*,*,#50408,.F.);
#66615=ORIENTED_EDGE('',*,*,#50409,.F.);
#66616=ORIENTED_EDGE('',*,*,#50410,.T.);
#66617=ORIENTED_EDGE('',*,*,#50411,.T.);
#66618=ORIENTED_EDGE('',*,*,#50412,.F.);
#66619=ORIENTED_EDGE('',*,*,#50407,.F.);
#66620=ORIENTED_EDGE('',*,*,#50413,.T.);
#66621=ORIENTED_EDGE('',*,*,#50414,.T.);
#66622=ORIENTED_EDGE('',*,*,#50415,.F.);
#66623=ORIENTED_EDGE('',*,*,#50411,.F.);
#66624=ORIENTED_EDGE('',*,*,#50416,.T.);
#66625=ORIENTED_EDGE('',*,*,#50409,.T.);
#66626=ORIENTED_EDGE('',*,*,#50417,.F.);
#66627=ORIENTED_EDGE('',*,*,#50414,.F.);
#66628=ORIENTED_EDGE('',*,*,#50418,.T.);
#66629=ORIENTED_EDGE('',*,*,#50419,.T.);
#66630=ORIENTED_EDGE('',*,*,#50420,.F.);
#66631=ORIENTED_EDGE('',*,*,#50421,.F.);
#66632=ORIENTED_EDGE('',*,*,#50422,.T.);
#66633=ORIENTED_EDGE('',*,*,#50423,.T.);
#66634=ORIENTED_EDGE('',*,*,#50424,.F.);
#66635=ORIENTED_EDGE('',*,*,#50419,.F.);
#66636=ORIENTED_EDGE('',*,*,#50425,.T.);
#66637=ORIENTED_EDGE('',*,*,#50426,.T.);
#66638=ORIENTED_EDGE('',*,*,#50427,.F.);
#66639=ORIENTED_EDGE('',*,*,#50423,.F.);
#66640=ORIENTED_EDGE('',*,*,#50428,.T.);
#66641=ORIENTED_EDGE('',*,*,#50421,.T.);
#66642=ORIENTED_EDGE('',*,*,#50429,.F.);
#66643=ORIENTED_EDGE('',*,*,#50426,.F.);
#66644=ORIENTED_EDGE('',*,*,#50430,.T.);
#66645=ORIENTED_EDGE('',*,*,#50431,.T.);
#66646=ORIENTED_EDGE('',*,*,#50432,.F.);
#66647=ORIENTED_EDGE('',*,*,#50433,.F.);
#66648=ORIENTED_EDGE('',*,*,#50434,.T.);
#66649=ORIENTED_EDGE('',*,*,#50435,.T.);
#66650=ORIENTED_EDGE('',*,*,#50436,.F.);
#66651=ORIENTED_EDGE('',*,*,#50431,.F.);
#66652=ORIENTED_EDGE('',*,*,#50437,.T.);
#66653=ORIENTED_EDGE('',*,*,#50438,.T.);
#66654=ORIENTED_EDGE('',*,*,#50439,.F.);
#66655=ORIENTED_EDGE('',*,*,#50435,.F.);
#66656=ORIENTED_EDGE('',*,*,#50440,.T.);
#66657=ORIENTED_EDGE('',*,*,#50433,.T.);
#66658=ORIENTED_EDGE('',*,*,#50441,.F.);
#66659=ORIENTED_EDGE('',*,*,#50438,.F.);
#66660=ORIENTED_EDGE('',*,*,#50442,.T.);
#66661=ORIENTED_EDGE('',*,*,#50443,.T.);
#66662=ORIENTED_EDGE('',*,*,#50444,.F.);
#66663=ORIENTED_EDGE('',*,*,#50445,.F.);
#66664=ORIENTED_EDGE('',*,*,#50446,.T.);
#66665=ORIENTED_EDGE('',*,*,#50447,.T.);
#66666=ORIENTED_EDGE('',*,*,#50448,.F.);
#66667=ORIENTED_EDGE('',*,*,#50443,.F.);
#66668=ORIENTED_EDGE('',*,*,#50449,.T.);
#66669=ORIENTED_EDGE('',*,*,#50450,.T.);
#66670=ORIENTED_EDGE('',*,*,#50451,.F.);
#66671=ORIENTED_EDGE('',*,*,#50447,.F.);
#66672=ORIENTED_EDGE('',*,*,#50452,.T.);
#66673=ORIENTED_EDGE('',*,*,#50445,.T.);
#66674=ORIENTED_EDGE('',*,*,#50453,.F.);
#66675=ORIENTED_EDGE('',*,*,#50450,.F.);
#66676=ORIENTED_EDGE('',*,*,#50454,.T.);
#66677=ORIENTED_EDGE('',*,*,#50455,.T.);
#66678=ORIENTED_EDGE('',*,*,#50456,.F.);
#66679=ORIENTED_EDGE('',*,*,#50457,.F.);
#66680=ORIENTED_EDGE('',*,*,#50458,.T.);
#66681=ORIENTED_EDGE('',*,*,#50459,.T.);
#66682=ORIENTED_EDGE('',*,*,#50460,.F.);
#66683=ORIENTED_EDGE('',*,*,#50455,.F.);
#66684=ORIENTED_EDGE('',*,*,#50461,.T.);
#66685=ORIENTED_EDGE('',*,*,#50462,.T.);
#66686=ORIENTED_EDGE('',*,*,#50463,.F.);
#66687=ORIENTED_EDGE('',*,*,#50459,.F.);
#66688=ORIENTED_EDGE('',*,*,#50464,.T.);
#66689=ORIENTED_EDGE('',*,*,#50457,.T.);
#66690=ORIENTED_EDGE('',*,*,#50465,.F.);
#66691=ORIENTED_EDGE('',*,*,#50462,.F.);
#66692=ORIENTED_EDGE('',*,*,#50466,.T.);
#66693=ORIENTED_EDGE('',*,*,#50467,.T.);
#66694=ORIENTED_EDGE('',*,*,#50468,.F.);
#66695=ORIENTED_EDGE('',*,*,#50469,.F.);
#66696=ORIENTED_EDGE('',*,*,#50470,.T.);
#66697=ORIENTED_EDGE('',*,*,#50471,.T.);
#66698=ORIENTED_EDGE('',*,*,#50472,.F.);
#66699=ORIENTED_EDGE('',*,*,#50467,.F.);
#66700=ORIENTED_EDGE('',*,*,#50473,.T.);
#66701=ORIENTED_EDGE('',*,*,#50474,.T.);
#66702=ORIENTED_EDGE('',*,*,#50475,.F.);
#66703=ORIENTED_EDGE('',*,*,#50471,.F.);
#66704=ORIENTED_EDGE('',*,*,#50476,.T.);
#66705=ORIENTED_EDGE('',*,*,#50469,.T.);
#66706=ORIENTED_EDGE('',*,*,#50477,.F.);
#66707=ORIENTED_EDGE('',*,*,#50474,.F.);
#66708=ORIENTED_EDGE('',*,*,#50478,.T.);
#66709=ORIENTED_EDGE('',*,*,#50479,.T.);
#66710=ORIENTED_EDGE('',*,*,#50480,.F.);
#66711=ORIENTED_EDGE('',*,*,#50481,.F.);
#66712=ORIENTED_EDGE('',*,*,#50482,.T.);
#66713=ORIENTED_EDGE('',*,*,#50483,.T.);
#66714=ORIENTED_EDGE('',*,*,#50484,.F.);
#66715=ORIENTED_EDGE('',*,*,#50479,.F.);
#66716=ORIENTED_EDGE('',*,*,#50485,.T.);
#66717=ORIENTED_EDGE('',*,*,#50486,.T.);
#66718=ORIENTED_EDGE('',*,*,#50487,.F.);
#66719=ORIENTED_EDGE('',*,*,#50483,.F.);
#66720=ORIENTED_EDGE('',*,*,#50488,.T.);
#66721=ORIENTED_EDGE('',*,*,#50481,.T.);
#66722=ORIENTED_EDGE('',*,*,#50489,.F.);
#66723=ORIENTED_EDGE('',*,*,#50486,.F.);
#66724=ORIENTED_EDGE('',*,*,#50490,.T.);
#66725=ORIENTED_EDGE('',*,*,#50491,.T.);
#66726=ORIENTED_EDGE('',*,*,#50492,.F.);
#66727=ORIENTED_EDGE('',*,*,#50493,.F.);
#66728=ORIENTED_EDGE('',*,*,#50494,.T.);
#66729=ORIENTED_EDGE('',*,*,#50495,.T.);
#66730=ORIENTED_EDGE('',*,*,#50496,.F.);
#66731=ORIENTED_EDGE('',*,*,#50491,.F.);
#66732=ORIENTED_EDGE('',*,*,#50497,.T.);
#66733=ORIENTED_EDGE('',*,*,#50498,.T.);
#66734=ORIENTED_EDGE('',*,*,#50499,.F.);
#66735=ORIENTED_EDGE('',*,*,#50495,.F.);
#66736=ORIENTED_EDGE('',*,*,#50500,.T.);
#66737=ORIENTED_EDGE('',*,*,#50493,.T.);
#66738=ORIENTED_EDGE('',*,*,#50501,.F.);
#66739=ORIENTED_EDGE('',*,*,#50498,.F.);
#66740=ORIENTED_EDGE('',*,*,#50502,.T.);
#66741=ORIENTED_EDGE('',*,*,#50503,.T.);
#66742=ORIENTED_EDGE('',*,*,#50504,.F.);
#66743=ORIENTED_EDGE('',*,*,#50505,.F.);
#66744=ORIENTED_EDGE('',*,*,#50506,.T.);
#66745=ORIENTED_EDGE('',*,*,#50507,.T.);
#66746=ORIENTED_EDGE('',*,*,#50508,.F.);
#66747=ORIENTED_EDGE('',*,*,#50503,.F.);
#66748=ORIENTED_EDGE('',*,*,#50509,.T.);
#66749=ORIENTED_EDGE('',*,*,#50510,.T.);
#66750=ORIENTED_EDGE('',*,*,#50511,.F.);
#66751=ORIENTED_EDGE('',*,*,#50507,.F.);
#66752=ORIENTED_EDGE('',*,*,#50512,.T.);
#66753=ORIENTED_EDGE('',*,*,#50505,.T.);
#66754=ORIENTED_EDGE('',*,*,#50513,.F.);
#66755=ORIENTED_EDGE('',*,*,#50510,.F.);
#66756=ORIENTED_EDGE('',*,*,#50514,.T.);
#66757=ORIENTED_EDGE('',*,*,#50515,.T.);
#66758=ORIENTED_EDGE('',*,*,#50516,.F.);
#66759=ORIENTED_EDGE('',*,*,#50517,.F.);
#66760=ORIENTED_EDGE('',*,*,#50518,.T.);
#66761=ORIENTED_EDGE('',*,*,#50519,.T.);
#66762=ORIENTED_EDGE('',*,*,#50520,.F.);
#66763=ORIENTED_EDGE('',*,*,#50515,.F.);
#66764=ORIENTED_EDGE('',*,*,#50521,.T.);
#66765=ORIENTED_EDGE('',*,*,#50522,.T.);
#66766=ORIENTED_EDGE('',*,*,#50523,.F.);
#66767=ORIENTED_EDGE('',*,*,#50519,.F.);
#66768=ORIENTED_EDGE('',*,*,#50524,.T.);
#66769=ORIENTED_EDGE('',*,*,#50517,.T.);
#66770=ORIENTED_EDGE('',*,*,#50525,.F.);
#66771=ORIENTED_EDGE('',*,*,#50522,.F.);
#66772=ORIENTED_EDGE('',*,*,#50526,.T.);
#66773=ORIENTED_EDGE('',*,*,#50527,.T.);
#66774=ORIENTED_EDGE('',*,*,#50528,.F.);
#66775=ORIENTED_EDGE('',*,*,#50529,.F.);
#66776=ORIENTED_EDGE('',*,*,#50530,.T.);
#66777=ORIENTED_EDGE('',*,*,#50531,.T.);
#66778=ORIENTED_EDGE('',*,*,#50532,.F.);
#66779=ORIENTED_EDGE('',*,*,#50527,.F.);
#66780=ORIENTED_EDGE('',*,*,#50533,.T.);
#66781=ORIENTED_EDGE('',*,*,#50534,.T.);
#66782=ORIENTED_EDGE('',*,*,#50535,.F.);
#66783=ORIENTED_EDGE('',*,*,#50531,.F.);
#66784=ORIENTED_EDGE('',*,*,#50536,.T.);
#66785=ORIENTED_EDGE('',*,*,#50529,.T.);
#66786=ORIENTED_EDGE('',*,*,#50537,.F.);
#66787=ORIENTED_EDGE('',*,*,#50534,.F.);
#66788=ORIENTED_EDGE('',*,*,#50538,.T.);
#66789=ORIENTED_EDGE('',*,*,#50539,.T.);
#66790=ORIENTED_EDGE('',*,*,#50540,.F.);
#66791=ORIENTED_EDGE('',*,*,#50541,.F.);
#66792=ORIENTED_EDGE('',*,*,#50542,.T.);
#66793=ORIENTED_EDGE('',*,*,#50543,.T.);
#66794=ORIENTED_EDGE('',*,*,#50544,.F.);
#66795=ORIENTED_EDGE('',*,*,#50539,.F.);
#66796=ORIENTED_EDGE('',*,*,#50545,.T.);
#66797=ORIENTED_EDGE('',*,*,#50546,.T.);
#66798=ORIENTED_EDGE('',*,*,#50547,.F.);
#66799=ORIENTED_EDGE('',*,*,#50543,.F.);
#66800=ORIENTED_EDGE('',*,*,#50548,.T.);
#66801=ORIENTED_EDGE('',*,*,#50541,.T.);
#66802=ORIENTED_EDGE('',*,*,#50549,.F.);
#66803=ORIENTED_EDGE('',*,*,#50546,.F.);
#66804=ORIENTED_EDGE('',*,*,#50550,.T.);
#66805=ORIENTED_EDGE('',*,*,#50551,.T.);
#66806=ORIENTED_EDGE('',*,*,#50552,.F.);
#66807=ORIENTED_EDGE('',*,*,#50553,.F.);
#66808=ORIENTED_EDGE('',*,*,#50554,.T.);
#66809=ORIENTED_EDGE('',*,*,#50555,.T.);
#66810=ORIENTED_EDGE('',*,*,#50556,.F.);
#66811=ORIENTED_EDGE('',*,*,#50551,.F.);
#66812=ORIENTED_EDGE('',*,*,#50557,.T.);
#66813=ORIENTED_EDGE('',*,*,#50558,.T.);
#66814=ORIENTED_EDGE('',*,*,#50559,.F.);
#66815=ORIENTED_EDGE('',*,*,#50555,.F.);
#66816=ORIENTED_EDGE('',*,*,#50560,.T.);
#66817=ORIENTED_EDGE('',*,*,#50553,.T.);
#66818=ORIENTED_EDGE('',*,*,#50561,.F.);
#66819=ORIENTED_EDGE('',*,*,#50558,.F.);
#66820=ORIENTED_EDGE('',*,*,#50562,.T.);
#66821=ORIENTED_EDGE('',*,*,#50563,.T.);
#66822=ORIENTED_EDGE('',*,*,#50564,.F.);
#66823=ORIENTED_EDGE('',*,*,#50565,.F.);
#66824=ORIENTED_EDGE('',*,*,#50566,.T.);
#66825=ORIENTED_EDGE('',*,*,#50567,.T.);
#66826=ORIENTED_EDGE('',*,*,#50568,.F.);
#66827=ORIENTED_EDGE('',*,*,#50563,.F.);
#66828=ORIENTED_EDGE('',*,*,#50569,.T.);
#66829=ORIENTED_EDGE('',*,*,#50570,.T.);
#66830=ORIENTED_EDGE('',*,*,#50571,.F.);
#66831=ORIENTED_EDGE('',*,*,#50567,.F.);
#66832=ORIENTED_EDGE('',*,*,#50572,.T.);
#66833=ORIENTED_EDGE('',*,*,#50565,.T.);
#66834=ORIENTED_EDGE('',*,*,#50573,.F.);
#66835=ORIENTED_EDGE('',*,*,#50570,.F.);
#66836=ORIENTED_EDGE('',*,*,#50574,.T.);
#66837=ORIENTED_EDGE('',*,*,#50575,.T.);
#66838=ORIENTED_EDGE('',*,*,#50576,.F.);
#66839=ORIENTED_EDGE('',*,*,#50577,.F.);
#66840=ORIENTED_EDGE('',*,*,#50578,.T.);
#66841=ORIENTED_EDGE('',*,*,#50579,.T.);
#66842=ORIENTED_EDGE('',*,*,#50580,.F.);
#66843=ORIENTED_EDGE('',*,*,#50575,.F.);
#66844=ORIENTED_EDGE('',*,*,#50581,.T.);
#66845=ORIENTED_EDGE('',*,*,#50582,.T.);
#66846=ORIENTED_EDGE('',*,*,#50583,.F.);
#66847=ORIENTED_EDGE('',*,*,#50579,.F.);
#66848=ORIENTED_EDGE('',*,*,#50584,.T.);
#66849=ORIENTED_EDGE('',*,*,#50577,.T.);
#66850=ORIENTED_EDGE('',*,*,#50585,.F.);
#66851=ORIENTED_EDGE('',*,*,#50582,.F.);
#66852=ORIENTED_EDGE('',*,*,#50586,.T.);
#66853=ORIENTED_EDGE('',*,*,#50587,.T.);
#66854=ORIENTED_EDGE('',*,*,#50588,.F.);
#66855=ORIENTED_EDGE('',*,*,#50589,.F.);
#66856=ORIENTED_EDGE('',*,*,#50590,.T.);
#66857=ORIENTED_EDGE('',*,*,#50591,.T.);
#66858=ORIENTED_EDGE('',*,*,#50592,.F.);
#66859=ORIENTED_EDGE('',*,*,#50587,.F.);
#66860=ORIENTED_EDGE('',*,*,#50593,.T.);
#66861=ORIENTED_EDGE('',*,*,#50594,.T.);
#66862=ORIENTED_EDGE('',*,*,#50595,.F.);
#66863=ORIENTED_EDGE('',*,*,#50591,.F.);
#66864=ORIENTED_EDGE('',*,*,#50596,.T.);
#66865=ORIENTED_EDGE('',*,*,#50589,.T.);
#66866=ORIENTED_EDGE('',*,*,#50597,.F.);
#66867=ORIENTED_EDGE('',*,*,#50594,.F.);
#66868=ORIENTED_EDGE('',*,*,#50598,.T.);
#66869=ORIENTED_EDGE('',*,*,#50599,.T.);
#66870=ORIENTED_EDGE('',*,*,#50600,.F.);
#66871=ORIENTED_EDGE('',*,*,#50601,.F.);
#66872=ORIENTED_EDGE('',*,*,#50602,.T.);
#66873=ORIENTED_EDGE('',*,*,#50603,.T.);
#66874=ORIENTED_EDGE('',*,*,#50604,.F.);
#66875=ORIENTED_EDGE('',*,*,#50599,.F.);
#66876=ORIENTED_EDGE('',*,*,#50605,.T.);
#66877=ORIENTED_EDGE('',*,*,#50606,.T.);
#66878=ORIENTED_EDGE('',*,*,#50607,.F.);
#66879=ORIENTED_EDGE('',*,*,#50603,.F.);
#66880=ORIENTED_EDGE('',*,*,#50608,.T.);
#66881=ORIENTED_EDGE('',*,*,#50601,.T.);
#66882=ORIENTED_EDGE('',*,*,#50609,.F.);
#66883=ORIENTED_EDGE('',*,*,#50606,.F.);
#66884=ORIENTED_EDGE('',*,*,#50610,.T.);
#66885=ORIENTED_EDGE('',*,*,#50611,.T.);
#66886=ORIENTED_EDGE('',*,*,#50612,.F.);
#66887=ORIENTED_EDGE('',*,*,#50613,.F.);
#66888=ORIENTED_EDGE('',*,*,#50614,.T.);
#66889=ORIENTED_EDGE('',*,*,#50615,.T.);
#66890=ORIENTED_EDGE('',*,*,#50616,.F.);
#66891=ORIENTED_EDGE('',*,*,#50611,.F.);
#66892=ORIENTED_EDGE('',*,*,#50617,.T.);
#66893=ORIENTED_EDGE('',*,*,#50618,.T.);
#66894=ORIENTED_EDGE('',*,*,#50619,.F.);
#66895=ORIENTED_EDGE('',*,*,#50615,.F.);
#66896=ORIENTED_EDGE('',*,*,#50620,.T.);
#66897=ORIENTED_EDGE('',*,*,#50613,.T.);
#66898=ORIENTED_EDGE('',*,*,#50621,.F.);
#66899=ORIENTED_EDGE('',*,*,#50618,.F.);
#66900=ORIENTED_EDGE('',*,*,#50622,.T.);
#66901=ORIENTED_EDGE('',*,*,#50623,.T.);
#66902=ORIENTED_EDGE('',*,*,#50624,.F.);
#66903=ORIENTED_EDGE('',*,*,#50625,.F.);
#66904=ORIENTED_EDGE('',*,*,#50626,.T.);
#66905=ORIENTED_EDGE('',*,*,#50627,.T.);
#66906=ORIENTED_EDGE('',*,*,#50628,.F.);
#66907=ORIENTED_EDGE('',*,*,#50623,.F.);
#66908=ORIENTED_EDGE('',*,*,#50629,.T.);
#66909=ORIENTED_EDGE('',*,*,#50630,.T.);
#66910=ORIENTED_EDGE('',*,*,#50631,.F.);
#66911=ORIENTED_EDGE('',*,*,#50627,.F.);
#66912=ORIENTED_EDGE('',*,*,#50632,.T.);
#66913=ORIENTED_EDGE('',*,*,#50625,.T.);
#66914=ORIENTED_EDGE('',*,*,#50633,.F.);
#66915=ORIENTED_EDGE('',*,*,#50630,.F.);
#66916=ORIENTED_EDGE('',*,*,#50634,.T.);
#66917=ORIENTED_EDGE('',*,*,#50635,.T.);
#66918=ORIENTED_EDGE('',*,*,#50636,.F.);
#66919=ORIENTED_EDGE('',*,*,#50637,.F.);
#66920=ORIENTED_EDGE('',*,*,#50638,.T.);
#66921=ORIENTED_EDGE('',*,*,#50639,.T.);
#66922=ORIENTED_EDGE('',*,*,#50640,.F.);
#66923=ORIENTED_EDGE('',*,*,#50635,.F.);
#66924=ORIENTED_EDGE('',*,*,#50641,.T.);
#66925=ORIENTED_EDGE('',*,*,#50642,.T.);
#66926=ORIENTED_EDGE('',*,*,#50643,.F.);
#66927=ORIENTED_EDGE('',*,*,#50639,.F.);
#66928=ORIENTED_EDGE('',*,*,#50644,.T.);
#66929=ORIENTED_EDGE('',*,*,#50637,.T.);
#66930=ORIENTED_EDGE('',*,*,#50645,.F.);
#66931=ORIENTED_EDGE('',*,*,#50642,.F.);
#66932=ORIENTED_EDGE('',*,*,#50646,.T.);
#66933=ORIENTED_EDGE('',*,*,#50647,.T.);
#66934=ORIENTED_EDGE('',*,*,#50648,.F.);
#66935=ORIENTED_EDGE('',*,*,#50649,.F.);
#66936=ORIENTED_EDGE('',*,*,#50650,.T.);
#66937=ORIENTED_EDGE('',*,*,#50651,.T.);
#66938=ORIENTED_EDGE('',*,*,#50652,.F.);
#66939=ORIENTED_EDGE('',*,*,#50647,.F.);
#66940=ORIENTED_EDGE('',*,*,#50653,.T.);
#66941=ORIENTED_EDGE('',*,*,#50654,.T.);
#66942=ORIENTED_EDGE('',*,*,#50655,.F.);
#66943=ORIENTED_EDGE('',*,*,#50651,.F.);
#66944=ORIENTED_EDGE('',*,*,#50656,.T.);
#66945=ORIENTED_EDGE('',*,*,#50649,.T.);
#66946=ORIENTED_EDGE('',*,*,#50657,.F.);
#66947=ORIENTED_EDGE('',*,*,#50654,.F.);
#66948=ORIENTED_EDGE('',*,*,#50658,.T.);
#66949=ORIENTED_EDGE('',*,*,#50659,.T.);
#66950=ORIENTED_EDGE('',*,*,#50660,.F.);
#66951=ORIENTED_EDGE('',*,*,#50661,.F.);
#66952=ORIENTED_EDGE('',*,*,#50662,.T.);
#66953=ORIENTED_EDGE('',*,*,#50663,.T.);
#66954=ORIENTED_EDGE('',*,*,#50664,.F.);
#66955=ORIENTED_EDGE('',*,*,#50659,.F.);
#66956=ORIENTED_EDGE('',*,*,#50665,.T.);
#66957=ORIENTED_EDGE('',*,*,#50666,.T.);
#66958=ORIENTED_EDGE('',*,*,#50667,.F.);
#66959=ORIENTED_EDGE('',*,*,#50663,.F.);
#66960=ORIENTED_EDGE('',*,*,#50668,.T.);
#66961=ORIENTED_EDGE('',*,*,#50661,.T.);
#66962=ORIENTED_EDGE('',*,*,#50669,.F.);
#66963=ORIENTED_EDGE('',*,*,#50666,.F.);
#66964=ORIENTED_EDGE('',*,*,#50670,.T.);
#66965=ORIENTED_EDGE('',*,*,#50671,.T.);
#66966=ORIENTED_EDGE('',*,*,#50672,.F.);
#66967=ORIENTED_EDGE('',*,*,#50673,.F.);
#66968=ORIENTED_EDGE('',*,*,#50674,.T.);
#66969=ORIENTED_EDGE('',*,*,#50675,.T.);
#66970=ORIENTED_EDGE('',*,*,#50676,.F.);
#66971=ORIENTED_EDGE('',*,*,#50671,.F.);
#66972=ORIENTED_EDGE('',*,*,#50677,.T.);
#66973=ORIENTED_EDGE('',*,*,#50678,.T.);
#66974=ORIENTED_EDGE('',*,*,#50679,.F.);
#66975=ORIENTED_EDGE('',*,*,#50675,.F.);
#66976=ORIENTED_EDGE('',*,*,#50680,.T.);
#66977=ORIENTED_EDGE('',*,*,#50673,.T.);
#66978=ORIENTED_EDGE('',*,*,#50681,.F.);
#66979=ORIENTED_EDGE('',*,*,#50678,.F.);
#66980=ORIENTED_EDGE('',*,*,#50682,.T.);
#66981=ORIENTED_EDGE('',*,*,#50683,.T.);
#66982=ORIENTED_EDGE('',*,*,#50684,.F.);
#66983=ORIENTED_EDGE('',*,*,#50685,.F.);
#66984=ORIENTED_EDGE('',*,*,#50686,.T.);
#66985=ORIENTED_EDGE('',*,*,#50687,.T.);
#66986=ORIENTED_EDGE('',*,*,#50688,.F.);
#66987=ORIENTED_EDGE('',*,*,#50683,.F.);
#66988=ORIENTED_EDGE('',*,*,#50689,.T.);
#66989=ORIENTED_EDGE('',*,*,#50690,.T.);
#66990=ORIENTED_EDGE('',*,*,#50691,.F.);
#66991=ORIENTED_EDGE('',*,*,#50687,.F.);
#66992=ORIENTED_EDGE('',*,*,#50692,.T.);
#66993=ORIENTED_EDGE('',*,*,#50685,.T.);
#66994=ORIENTED_EDGE('',*,*,#50693,.F.);
#66995=ORIENTED_EDGE('',*,*,#50690,.F.);
#66996=ORIENTED_EDGE('',*,*,#50694,.T.);
#66997=ORIENTED_EDGE('',*,*,#50695,.T.);
#66998=ORIENTED_EDGE('',*,*,#50696,.F.);
#66999=ORIENTED_EDGE('',*,*,#50697,.F.);
#67000=ORIENTED_EDGE('',*,*,#50698,.T.);
#67001=ORIENTED_EDGE('',*,*,#50699,.T.);
#67002=ORIENTED_EDGE('',*,*,#50700,.F.);
#67003=ORIENTED_EDGE('',*,*,#50695,.F.);
#67004=ORIENTED_EDGE('',*,*,#50701,.T.);
#67005=ORIENTED_EDGE('',*,*,#50702,.T.);
#67006=ORIENTED_EDGE('',*,*,#50703,.F.);
#67007=ORIENTED_EDGE('',*,*,#50699,.F.);
#67008=ORIENTED_EDGE('',*,*,#50704,.T.);
#67009=ORIENTED_EDGE('',*,*,#50697,.T.);
#67010=ORIENTED_EDGE('',*,*,#50705,.F.);
#67011=ORIENTED_EDGE('',*,*,#50702,.F.);
#67012=ORIENTED_EDGE('',*,*,#50706,.T.);
#67013=ORIENTED_EDGE('',*,*,#50707,.T.);
#67014=ORIENTED_EDGE('',*,*,#50708,.F.);
#67015=ORIENTED_EDGE('',*,*,#50709,.F.);
#67016=ORIENTED_EDGE('',*,*,#50710,.T.);
#67017=ORIENTED_EDGE('',*,*,#50711,.T.);
#67018=ORIENTED_EDGE('',*,*,#50712,.F.);
#67019=ORIENTED_EDGE('',*,*,#50707,.F.);
#67020=ORIENTED_EDGE('',*,*,#50713,.T.);
#67021=ORIENTED_EDGE('',*,*,#50714,.T.);
#67022=ORIENTED_EDGE('',*,*,#50715,.F.);
#67023=ORIENTED_EDGE('',*,*,#50711,.F.);
#67024=ORIENTED_EDGE('',*,*,#50716,.T.);
#67025=ORIENTED_EDGE('',*,*,#50709,.T.);
#67026=ORIENTED_EDGE('',*,*,#50717,.F.);
#67027=ORIENTED_EDGE('',*,*,#50714,.F.);
#67028=ORIENTED_EDGE('',*,*,#50718,.T.);
#67029=ORIENTED_EDGE('',*,*,#50719,.T.);
#67030=ORIENTED_EDGE('',*,*,#50720,.F.);
#67031=ORIENTED_EDGE('',*,*,#50721,.F.);
#67032=ORIENTED_EDGE('',*,*,#50722,.T.);
#67033=ORIENTED_EDGE('',*,*,#50723,.T.);
#67034=ORIENTED_EDGE('',*,*,#50724,.F.);
#67035=ORIENTED_EDGE('',*,*,#50719,.F.);
#67036=ORIENTED_EDGE('',*,*,#50725,.T.);
#67037=ORIENTED_EDGE('',*,*,#50726,.T.);
#67038=ORIENTED_EDGE('',*,*,#50727,.F.);
#67039=ORIENTED_EDGE('',*,*,#50723,.F.);
#67040=ORIENTED_EDGE('',*,*,#50728,.T.);
#67041=ORIENTED_EDGE('',*,*,#50721,.T.);
#67042=ORIENTED_EDGE('',*,*,#50729,.F.);
#67043=ORIENTED_EDGE('',*,*,#50726,.F.);
#67044=ORIENTED_EDGE('',*,*,#50730,.T.);
#67045=ORIENTED_EDGE('',*,*,#50731,.T.);
#67046=ORIENTED_EDGE('',*,*,#50732,.F.);
#67047=ORIENTED_EDGE('',*,*,#50733,.F.);
#67048=ORIENTED_EDGE('',*,*,#50734,.T.);
#67049=ORIENTED_EDGE('',*,*,#50735,.T.);
#67050=ORIENTED_EDGE('',*,*,#50736,.F.);
#67051=ORIENTED_EDGE('',*,*,#50731,.F.);
#67052=ORIENTED_EDGE('',*,*,#50737,.T.);
#67053=ORIENTED_EDGE('',*,*,#50738,.T.);
#67054=ORIENTED_EDGE('',*,*,#50739,.F.);
#67055=ORIENTED_EDGE('',*,*,#50735,.F.);
#67056=ORIENTED_EDGE('',*,*,#50740,.T.);
#67057=ORIENTED_EDGE('',*,*,#50733,.T.);
#67058=ORIENTED_EDGE('',*,*,#50741,.F.);
#67059=ORIENTED_EDGE('',*,*,#50738,.F.);
#67060=ORIENTED_EDGE('',*,*,#50742,.T.);
#67061=ORIENTED_EDGE('',*,*,#50743,.T.);
#67062=ORIENTED_EDGE('',*,*,#50744,.F.);
#67063=ORIENTED_EDGE('',*,*,#50745,.F.);
#67064=ORIENTED_EDGE('',*,*,#50746,.T.);
#67065=ORIENTED_EDGE('',*,*,#50747,.T.);
#67066=ORIENTED_EDGE('',*,*,#50748,.F.);
#67067=ORIENTED_EDGE('',*,*,#50743,.F.);
#67068=ORIENTED_EDGE('',*,*,#50749,.T.);
#67069=ORIENTED_EDGE('',*,*,#50750,.T.);
#67070=ORIENTED_EDGE('',*,*,#50751,.F.);
#67071=ORIENTED_EDGE('',*,*,#50747,.F.);
#67072=ORIENTED_EDGE('',*,*,#50752,.T.);
#67073=ORIENTED_EDGE('',*,*,#50745,.T.);
#67074=ORIENTED_EDGE('',*,*,#50753,.F.);
#67075=ORIENTED_EDGE('',*,*,#50750,.F.);
#67076=ORIENTED_EDGE('',*,*,#50754,.T.);
#67077=ORIENTED_EDGE('',*,*,#50755,.T.);
#67078=ORIENTED_EDGE('',*,*,#50756,.F.);
#67079=ORIENTED_EDGE('',*,*,#50757,.F.);
#67080=ORIENTED_EDGE('',*,*,#50758,.T.);
#67081=ORIENTED_EDGE('',*,*,#50759,.T.);
#67082=ORIENTED_EDGE('',*,*,#50760,.F.);
#67083=ORIENTED_EDGE('',*,*,#50755,.F.);
#67084=ORIENTED_EDGE('',*,*,#50761,.T.);
#67085=ORIENTED_EDGE('',*,*,#50762,.T.);
#67086=ORIENTED_EDGE('',*,*,#50763,.F.);
#67087=ORIENTED_EDGE('',*,*,#50759,.F.);
#67088=ORIENTED_EDGE('',*,*,#50764,.T.);
#67089=ORIENTED_EDGE('',*,*,#50757,.T.);
#67090=ORIENTED_EDGE('',*,*,#50765,.F.);
#67091=ORIENTED_EDGE('',*,*,#50762,.F.);
#67092=ORIENTED_EDGE('',*,*,#50766,.T.);
#67093=ORIENTED_EDGE('',*,*,#50767,.T.);
#67094=ORIENTED_EDGE('',*,*,#50768,.F.);
#67095=ORIENTED_EDGE('',*,*,#50769,.F.);
#67096=ORIENTED_EDGE('',*,*,#50770,.T.);
#67097=ORIENTED_EDGE('',*,*,#50771,.T.);
#67098=ORIENTED_EDGE('',*,*,#50772,.F.);
#67099=ORIENTED_EDGE('',*,*,#50767,.F.);
#67100=ORIENTED_EDGE('',*,*,#50773,.T.);
#67101=ORIENTED_EDGE('',*,*,#50774,.T.);
#67102=ORIENTED_EDGE('',*,*,#50775,.F.);
#67103=ORIENTED_EDGE('',*,*,#50771,.F.);
#67104=ORIENTED_EDGE('',*,*,#50776,.T.);
#67105=ORIENTED_EDGE('',*,*,#50769,.T.);
#67106=ORIENTED_EDGE('',*,*,#50777,.F.);
#67107=ORIENTED_EDGE('',*,*,#50774,.F.);
#67108=ORIENTED_EDGE('',*,*,#50778,.T.);
#67109=ORIENTED_EDGE('',*,*,#50779,.T.);
#67110=ORIENTED_EDGE('',*,*,#50780,.F.);
#67111=ORIENTED_EDGE('',*,*,#50781,.F.);
#67112=ORIENTED_EDGE('',*,*,#50782,.T.);
#67113=ORIENTED_EDGE('',*,*,#50783,.T.);
#67114=ORIENTED_EDGE('',*,*,#50784,.F.);
#67115=ORIENTED_EDGE('',*,*,#50779,.F.);
#67116=ORIENTED_EDGE('',*,*,#50785,.T.);
#67117=ORIENTED_EDGE('',*,*,#50786,.T.);
#67118=ORIENTED_EDGE('',*,*,#50787,.F.);
#67119=ORIENTED_EDGE('',*,*,#50783,.F.);
#67120=ORIENTED_EDGE('',*,*,#50788,.T.);
#67121=ORIENTED_EDGE('',*,*,#50781,.T.);
#67122=ORIENTED_EDGE('',*,*,#50789,.F.);
#67123=ORIENTED_EDGE('',*,*,#50786,.F.);
#67124=ORIENTED_EDGE('',*,*,#50790,.T.);
#67125=ORIENTED_EDGE('',*,*,#50791,.T.);
#67126=ORIENTED_EDGE('',*,*,#50792,.F.);
#67127=ORIENTED_EDGE('',*,*,#50793,.F.);
#67128=ORIENTED_EDGE('',*,*,#50794,.T.);
#67129=ORIENTED_EDGE('',*,*,#50795,.T.);
#67130=ORIENTED_EDGE('',*,*,#50796,.F.);
#67131=ORIENTED_EDGE('',*,*,#50791,.F.);
#67132=ORIENTED_EDGE('',*,*,#50797,.T.);
#67133=ORIENTED_EDGE('',*,*,#50798,.T.);
#67134=ORIENTED_EDGE('',*,*,#50799,.F.);
#67135=ORIENTED_EDGE('',*,*,#50795,.F.);
#67136=ORIENTED_EDGE('',*,*,#50800,.T.);
#67137=ORIENTED_EDGE('',*,*,#50793,.T.);
#67138=ORIENTED_EDGE('',*,*,#50801,.F.);
#67139=ORIENTED_EDGE('',*,*,#50798,.F.);
#67140=ORIENTED_EDGE('',*,*,#50802,.T.);
#67141=ORIENTED_EDGE('',*,*,#50803,.T.);
#67142=ORIENTED_EDGE('',*,*,#50804,.F.);
#67143=ORIENTED_EDGE('',*,*,#50805,.F.);
#67144=ORIENTED_EDGE('',*,*,#50806,.T.);
#67145=ORIENTED_EDGE('',*,*,#50807,.T.);
#67146=ORIENTED_EDGE('',*,*,#50808,.F.);
#67147=ORIENTED_EDGE('',*,*,#50803,.F.);
#67148=ORIENTED_EDGE('',*,*,#50809,.T.);
#67149=ORIENTED_EDGE('',*,*,#50810,.T.);
#67150=ORIENTED_EDGE('',*,*,#50811,.F.);
#67151=ORIENTED_EDGE('',*,*,#50807,.F.);
#67152=ORIENTED_EDGE('',*,*,#50812,.T.);
#67153=ORIENTED_EDGE('',*,*,#50805,.T.);
#67154=ORIENTED_EDGE('',*,*,#50813,.F.);
#67155=ORIENTED_EDGE('',*,*,#50810,.F.);
#67156=ORIENTED_EDGE('',*,*,#50814,.T.);
#67157=ORIENTED_EDGE('',*,*,#50815,.T.);
#67158=ORIENTED_EDGE('',*,*,#50816,.F.);
#67159=ORIENTED_EDGE('',*,*,#50817,.F.);
#67160=ORIENTED_EDGE('',*,*,#50818,.T.);
#67161=ORIENTED_EDGE('',*,*,#50819,.T.);
#67162=ORIENTED_EDGE('',*,*,#50820,.F.);
#67163=ORIENTED_EDGE('',*,*,#50815,.F.);
#67164=ORIENTED_EDGE('',*,*,#50821,.T.);
#67165=ORIENTED_EDGE('',*,*,#50822,.T.);
#67166=ORIENTED_EDGE('',*,*,#50823,.F.);
#67167=ORIENTED_EDGE('',*,*,#50819,.F.);
#67168=ORIENTED_EDGE('',*,*,#50824,.T.);
#67169=ORIENTED_EDGE('',*,*,#50817,.T.);
#67170=ORIENTED_EDGE('',*,*,#50825,.F.);
#67171=ORIENTED_EDGE('',*,*,#50822,.F.);
#67172=ORIENTED_EDGE('',*,*,#50826,.T.);
#67173=ORIENTED_EDGE('',*,*,#50827,.T.);
#67174=ORIENTED_EDGE('',*,*,#50828,.F.);
#67175=ORIENTED_EDGE('',*,*,#50829,.F.);
#67176=ORIENTED_EDGE('',*,*,#50830,.T.);
#67177=ORIENTED_EDGE('',*,*,#50831,.T.);
#67178=ORIENTED_EDGE('',*,*,#50832,.F.);
#67179=ORIENTED_EDGE('',*,*,#50827,.F.);
#67180=ORIENTED_EDGE('',*,*,#50833,.T.);
#67181=ORIENTED_EDGE('',*,*,#50834,.T.);
#67182=ORIENTED_EDGE('',*,*,#50835,.F.);
#67183=ORIENTED_EDGE('',*,*,#50831,.F.);
#67184=ORIENTED_EDGE('',*,*,#50836,.T.);
#67185=ORIENTED_EDGE('',*,*,#50829,.T.);
#67186=ORIENTED_EDGE('',*,*,#50837,.F.);
#67187=ORIENTED_EDGE('',*,*,#50834,.F.);
#67188=ORIENTED_EDGE('',*,*,#50838,.T.);
#67189=ORIENTED_EDGE('',*,*,#50839,.T.);
#67190=ORIENTED_EDGE('',*,*,#50840,.F.);
#67191=ORIENTED_EDGE('',*,*,#50841,.F.);
#67192=ORIENTED_EDGE('',*,*,#50842,.T.);
#67193=ORIENTED_EDGE('',*,*,#50843,.T.);
#67194=ORIENTED_EDGE('',*,*,#50844,.F.);
#67195=ORIENTED_EDGE('',*,*,#50839,.F.);
#67196=ORIENTED_EDGE('',*,*,#50845,.T.);
#67197=ORIENTED_EDGE('',*,*,#50846,.T.);
#67198=ORIENTED_EDGE('',*,*,#50847,.F.);
#67199=ORIENTED_EDGE('',*,*,#50843,.F.);
#67200=ORIENTED_EDGE('',*,*,#50848,.T.);
#67201=ORIENTED_EDGE('',*,*,#50841,.T.);
#67202=ORIENTED_EDGE('',*,*,#50849,.F.);
#67203=ORIENTED_EDGE('',*,*,#50846,.F.);
#67204=ORIENTED_EDGE('',*,*,#50850,.T.);
#67205=ORIENTED_EDGE('',*,*,#50851,.T.);
#67206=ORIENTED_EDGE('',*,*,#50852,.F.);
#67207=ORIENTED_EDGE('',*,*,#50853,.F.);
#67208=ORIENTED_EDGE('',*,*,#50854,.T.);
#67209=ORIENTED_EDGE('',*,*,#50855,.T.);
#67210=ORIENTED_EDGE('',*,*,#50856,.F.);
#67211=ORIENTED_EDGE('',*,*,#50851,.F.);
#67212=ORIENTED_EDGE('',*,*,#50857,.T.);
#67213=ORIENTED_EDGE('',*,*,#50858,.T.);
#67214=ORIENTED_EDGE('',*,*,#50859,.F.);
#67215=ORIENTED_EDGE('',*,*,#50855,.F.);
#67216=ORIENTED_EDGE('',*,*,#50860,.T.);
#67217=ORIENTED_EDGE('',*,*,#50853,.T.);
#67218=ORIENTED_EDGE('',*,*,#50861,.F.);
#67219=ORIENTED_EDGE('',*,*,#50858,.F.);
#67220=ORIENTED_EDGE('',*,*,#50862,.T.);
#67221=ORIENTED_EDGE('',*,*,#50863,.T.);
#67222=ORIENTED_EDGE('',*,*,#50864,.F.);
#67223=ORIENTED_EDGE('',*,*,#50865,.F.);
#67224=ORIENTED_EDGE('',*,*,#50866,.T.);
#67225=ORIENTED_EDGE('',*,*,#50867,.T.);
#67226=ORIENTED_EDGE('',*,*,#50868,.F.);
#67227=ORIENTED_EDGE('',*,*,#50863,.F.);
#67228=ORIENTED_EDGE('',*,*,#50869,.T.);
#67229=ORIENTED_EDGE('',*,*,#50870,.T.);
#67230=ORIENTED_EDGE('',*,*,#50871,.F.);
#67231=ORIENTED_EDGE('',*,*,#50867,.F.);
#67232=ORIENTED_EDGE('',*,*,#50872,.T.);
#67233=ORIENTED_EDGE('',*,*,#50865,.T.);
#67234=ORIENTED_EDGE('',*,*,#50873,.F.);
#67235=ORIENTED_EDGE('',*,*,#50870,.F.);
#67236=ORIENTED_EDGE('',*,*,#50874,.T.);
#67237=ORIENTED_EDGE('',*,*,#50875,.T.);
#67238=ORIENTED_EDGE('',*,*,#50876,.F.);
#67239=ORIENTED_EDGE('',*,*,#50877,.F.);
#67240=ORIENTED_EDGE('',*,*,#50878,.T.);
#67241=ORIENTED_EDGE('',*,*,#50879,.T.);
#67242=ORIENTED_EDGE('',*,*,#50880,.F.);
#67243=ORIENTED_EDGE('',*,*,#50875,.F.);
#67244=ORIENTED_EDGE('',*,*,#50881,.T.);
#67245=ORIENTED_EDGE('',*,*,#50882,.T.);
#67246=ORIENTED_EDGE('',*,*,#50883,.F.);
#67247=ORIENTED_EDGE('',*,*,#50879,.F.);
#67248=ORIENTED_EDGE('',*,*,#50884,.T.);
#67249=ORIENTED_EDGE('',*,*,#50877,.T.);
#67250=ORIENTED_EDGE('',*,*,#50885,.F.);
#67251=ORIENTED_EDGE('',*,*,#50882,.F.);
#67252=ORIENTED_EDGE('',*,*,#50886,.T.);
#67253=ORIENTED_EDGE('',*,*,#50887,.T.);
#67254=ORIENTED_EDGE('',*,*,#50888,.F.);
#67255=ORIENTED_EDGE('',*,*,#50889,.F.);
#67256=ORIENTED_EDGE('',*,*,#50890,.T.);
#67257=ORIENTED_EDGE('',*,*,#50891,.T.);
#67258=ORIENTED_EDGE('',*,*,#50892,.F.);
#67259=ORIENTED_EDGE('',*,*,#50887,.F.);
#67260=ORIENTED_EDGE('',*,*,#50893,.T.);
#67261=ORIENTED_EDGE('',*,*,#50894,.T.);
#67262=ORIENTED_EDGE('',*,*,#50895,.F.);
#67263=ORIENTED_EDGE('',*,*,#50891,.F.);
#67264=ORIENTED_EDGE('',*,*,#50896,.T.);
#67265=ORIENTED_EDGE('',*,*,#50889,.T.);
#67266=ORIENTED_EDGE('',*,*,#50897,.F.);
#67267=ORIENTED_EDGE('',*,*,#50894,.F.);
#67268=ORIENTED_EDGE('',*,*,#50898,.T.);
#67269=ORIENTED_EDGE('',*,*,#50899,.T.);
#67270=ORIENTED_EDGE('',*,*,#50900,.F.);
#67271=ORIENTED_EDGE('',*,*,#50901,.F.);
#67272=ORIENTED_EDGE('',*,*,#50902,.T.);
#67273=ORIENTED_EDGE('',*,*,#50903,.T.);
#67274=ORIENTED_EDGE('',*,*,#50904,.F.);
#67275=ORIENTED_EDGE('',*,*,#50899,.F.);
#67276=ORIENTED_EDGE('',*,*,#50905,.T.);
#67277=ORIENTED_EDGE('',*,*,#50906,.T.);
#67278=ORIENTED_EDGE('',*,*,#50907,.F.);
#67279=ORIENTED_EDGE('',*,*,#50903,.F.);
#67280=ORIENTED_EDGE('',*,*,#50908,.T.);
#67281=ORIENTED_EDGE('',*,*,#50901,.T.);
#67282=ORIENTED_EDGE('',*,*,#50909,.F.);
#67283=ORIENTED_EDGE('',*,*,#50906,.F.);
#67284=ORIENTED_EDGE('',*,*,#50910,.T.);
#67285=ORIENTED_EDGE('',*,*,#50911,.T.);
#67286=ORIENTED_EDGE('',*,*,#50912,.F.);
#67287=ORIENTED_EDGE('',*,*,#50913,.F.);
#67288=ORIENTED_EDGE('',*,*,#50914,.T.);
#67289=ORIENTED_EDGE('',*,*,#50915,.T.);
#67290=ORIENTED_EDGE('',*,*,#50916,.F.);
#67291=ORIENTED_EDGE('',*,*,#50911,.F.);
#67292=ORIENTED_EDGE('',*,*,#50917,.T.);
#67293=ORIENTED_EDGE('',*,*,#50918,.T.);
#67294=ORIENTED_EDGE('',*,*,#50919,.F.);
#67295=ORIENTED_EDGE('',*,*,#50915,.F.);
#67296=ORIENTED_EDGE('',*,*,#50920,.T.);
#67297=ORIENTED_EDGE('',*,*,#50913,.T.);
#67298=ORIENTED_EDGE('',*,*,#50921,.F.);
#67299=ORIENTED_EDGE('',*,*,#50918,.F.);
#67300=ORIENTED_EDGE('',*,*,#50922,.T.);
#67301=ORIENTED_EDGE('',*,*,#50923,.T.);
#67302=ORIENTED_EDGE('',*,*,#50924,.F.);
#67303=ORIENTED_EDGE('',*,*,#50925,.F.);
#67304=ORIENTED_EDGE('',*,*,#50926,.T.);
#67305=ORIENTED_EDGE('',*,*,#50927,.T.);
#67306=ORIENTED_EDGE('',*,*,#50928,.F.);
#67307=ORIENTED_EDGE('',*,*,#50923,.F.);
#67308=ORIENTED_EDGE('',*,*,#50929,.T.);
#67309=ORIENTED_EDGE('',*,*,#50930,.T.);
#67310=ORIENTED_EDGE('',*,*,#50931,.F.);
#67311=ORIENTED_EDGE('',*,*,#50927,.F.);
#67312=ORIENTED_EDGE('',*,*,#50932,.T.);
#67313=ORIENTED_EDGE('',*,*,#50925,.T.);
#67314=ORIENTED_EDGE('',*,*,#50933,.F.);
#67315=ORIENTED_EDGE('',*,*,#50930,.F.);
#67316=ORIENTED_EDGE('',*,*,#50934,.T.);
#67317=ORIENTED_EDGE('',*,*,#50935,.T.);
#67318=ORIENTED_EDGE('',*,*,#50936,.F.);
#67319=ORIENTED_EDGE('',*,*,#50937,.F.);
#67320=ORIENTED_EDGE('',*,*,#50938,.T.);
#67321=ORIENTED_EDGE('',*,*,#50939,.T.);
#67322=ORIENTED_EDGE('',*,*,#50940,.F.);
#67323=ORIENTED_EDGE('',*,*,#50935,.F.);
#67324=ORIENTED_EDGE('',*,*,#50941,.T.);
#67325=ORIENTED_EDGE('',*,*,#50942,.T.);
#67326=ORIENTED_EDGE('',*,*,#50943,.F.);
#67327=ORIENTED_EDGE('',*,*,#50939,.F.);
#67328=ORIENTED_EDGE('',*,*,#50944,.T.);
#67329=ORIENTED_EDGE('',*,*,#50937,.T.);
#67330=ORIENTED_EDGE('',*,*,#50945,.F.);
#67331=ORIENTED_EDGE('',*,*,#50942,.F.);
#67332=ORIENTED_EDGE('',*,*,#50946,.T.);
#67333=ORIENTED_EDGE('',*,*,#50947,.T.);
#67334=ORIENTED_EDGE('',*,*,#50948,.F.);
#67335=ORIENTED_EDGE('',*,*,#50949,.F.);
#67336=ORIENTED_EDGE('',*,*,#50950,.T.);
#67337=ORIENTED_EDGE('',*,*,#50951,.T.);
#67338=ORIENTED_EDGE('',*,*,#50952,.F.);
#67339=ORIENTED_EDGE('',*,*,#50947,.F.);
#67340=ORIENTED_EDGE('',*,*,#50953,.T.);
#67341=ORIENTED_EDGE('',*,*,#50954,.T.);
#67342=ORIENTED_EDGE('',*,*,#50955,.F.);
#67343=ORIENTED_EDGE('',*,*,#50951,.F.);
#67344=ORIENTED_EDGE('',*,*,#50956,.T.);
#67345=ORIENTED_EDGE('',*,*,#50949,.T.);
#67346=ORIENTED_EDGE('',*,*,#50957,.F.);
#67347=ORIENTED_EDGE('',*,*,#50954,.F.);
#67348=ORIENTED_EDGE('',*,*,#50958,.T.);
#67349=ORIENTED_EDGE('',*,*,#50959,.T.);
#67350=ORIENTED_EDGE('',*,*,#50960,.F.);
#67351=ORIENTED_EDGE('',*,*,#50961,.F.);
#67352=ORIENTED_EDGE('',*,*,#50962,.T.);
#67353=ORIENTED_EDGE('',*,*,#50963,.T.);
#67354=ORIENTED_EDGE('',*,*,#50964,.F.);
#67355=ORIENTED_EDGE('',*,*,#50959,.F.);
#67356=ORIENTED_EDGE('',*,*,#50965,.T.);
#67357=ORIENTED_EDGE('',*,*,#50966,.T.);
#67358=ORIENTED_EDGE('',*,*,#50967,.F.);
#67359=ORIENTED_EDGE('',*,*,#50963,.F.);
#67360=ORIENTED_EDGE('',*,*,#50968,.T.);
#67361=ORIENTED_EDGE('',*,*,#50961,.T.);
#67362=ORIENTED_EDGE('',*,*,#50969,.F.);
#67363=ORIENTED_EDGE('',*,*,#50966,.F.);
#67364=ORIENTED_EDGE('',*,*,#50970,.T.);
#67365=ORIENTED_EDGE('',*,*,#50971,.T.);
#67366=ORIENTED_EDGE('',*,*,#50972,.F.);
#67367=ORIENTED_EDGE('',*,*,#50973,.F.);
#67368=ORIENTED_EDGE('',*,*,#50974,.T.);
#67369=ORIENTED_EDGE('',*,*,#50975,.T.);
#67370=ORIENTED_EDGE('',*,*,#50976,.F.);
#67371=ORIENTED_EDGE('',*,*,#50971,.F.);
#67372=ORIENTED_EDGE('',*,*,#50977,.T.);
#67373=ORIENTED_EDGE('',*,*,#50978,.T.);
#67374=ORIENTED_EDGE('',*,*,#50979,.F.);
#67375=ORIENTED_EDGE('',*,*,#50975,.F.);
#67376=ORIENTED_EDGE('',*,*,#50980,.T.);
#67377=ORIENTED_EDGE('',*,*,#50973,.T.);
#67378=ORIENTED_EDGE('',*,*,#50981,.F.);
#67379=ORIENTED_EDGE('',*,*,#50978,.F.);
#67380=ORIENTED_EDGE('',*,*,#50982,.T.);
#67381=ORIENTED_EDGE('',*,*,#50983,.T.);
#67382=ORIENTED_EDGE('',*,*,#50984,.F.);
#67383=ORIENTED_EDGE('',*,*,#50985,.F.);
#67384=ORIENTED_EDGE('',*,*,#50986,.T.);
#67385=ORIENTED_EDGE('',*,*,#50987,.T.);
#67386=ORIENTED_EDGE('',*,*,#50988,.F.);
#67387=ORIENTED_EDGE('',*,*,#50983,.F.);
#67388=ORIENTED_EDGE('',*,*,#50989,.T.);
#67389=ORIENTED_EDGE('',*,*,#50990,.T.);
#67390=ORIENTED_EDGE('',*,*,#50991,.F.);
#67391=ORIENTED_EDGE('',*,*,#50987,.F.);
#67392=ORIENTED_EDGE('',*,*,#50992,.T.);
#67393=ORIENTED_EDGE('',*,*,#50985,.T.);
#67394=ORIENTED_EDGE('',*,*,#50993,.F.);
#67395=ORIENTED_EDGE('',*,*,#50990,.F.);
#67396=ORIENTED_EDGE('',*,*,#50994,.T.);
#67397=ORIENTED_EDGE('',*,*,#50995,.T.);
#67398=ORIENTED_EDGE('',*,*,#50996,.F.);
#67399=ORIENTED_EDGE('',*,*,#50997,.F.);
#67400=ORIENTED_EDGE('',*,*,#50998,.T.);
#67401=ORIENTED_EDGE('',*,*,#50999,.T.);
#67402=ORIENTED_EDGE('',*,*,#51000,.F.);
#67403=ORIENTED_EDGE('',*,*,#50995,.F.);
#67404=ORIENTED_EDGE('',*,*,#51001,.T.);
#67405=ORIENTED_EDGE('',*,*,#51002,.T.);
#67406=ORIENTED_EDGE('',*,*,#51003,.F.);
#67407=ORIENTED_EDGE('',*,*,#50999,.F.);
#67408=ORIENTED_EDGE('',*,*,#51004,.T.);
#67409=ORIENTED_EDGE('',*,*,#50997,.T.);
#67410=ORIENTED_EDGE('',*,*,#51005,.F.);
#67411=ORIENTED_EDGE('',*,*,#51002,.F.);
#67412=ORIENTED_EDGE('',*,*,#51006,.T.);
#67413=ORIENTED_EDGE('',*,*,#51007,.T.);
#67414=ORIENTED_EDGE('',*,*,#51008,.F.);
#67415=ORIENTED_EDGE('',*,*,#51009,.F.);
#67416=ORIENTED_EDGE('',*,*,#51010,.T.);
#67417=ORIENTED_EDGE('',*,*,#51011,.T.);
#67418=ORIENTED_EDGE('',*,*,#51012,.F.);
#67419=ORIENTED_EDGE('',*,*,#51007,.F.);
#67420=ORIENTED_EDGE('',*,*,#51013,.T.);
#67421=ORIENTED_EDGE('',*,*,#51014,.T.);
#67422=ORIENTED_EDGE('',*,*,#51015,.F.);
#67423=ORIENTED_EDGE('',*,*,#51011,.F.);
#67424=ORIENTED_EDGE('',*,*,#51016,.T.);
#67425=ORIENTED_EDGE('',*,*,#51009,.T.);
#67426=ORIENTED_EDGE('',*,*,#51017,.F.);
#67427=ORIENTED_EDGE('',*,*,#51014,.F.);
#67428=ORIENTED_EDGE('',*,*,#51018,.T.);
#67429=ORIENTED_EDGE('',*,*,#51019,.T.);
#67430=ORIENTED_EDGE('',*,*,#51020,.F.);
#67431=ORIENTED_EDGE('',*,*,#51021,.F.);
#67432=ORIENTED_EDGE('',*,*,#51022,.T.);
#67433=ORIENTED_EDGE('',*,*,#51023,.T.);
#67434=ORIENTED_EDGE('',*,*,#51024,.F.);
#67435=ORIENTED_EDGE('',*,*,#51019,.F.);
#67436=ORIENTED_EDGE('',*,*,#51025,.T.);
#67437=ORIENTED_EDGE('',*,*,#51026,.T.);
#67438=ORIENTED_EDGE('',*,*,#51027,.F.);
#67439=ORIENTED_EDGE('',*,*,#51023,.F.);
#67440=ORIENTED_EDGE('',*,*,#51028,.T.);
#67441=ORIENTED_EDGE('',*,*,#51021,.T.);
#67442=ORIENTED_EDGE('',*,*,#51029,.F.);
#67443=ORIENTED_EDGE('',*,*,#51026,.F.);
#67444=ORIENTED_EDGE('',*,*,#51030,.T.);
#67445=ORIENTED_EDGE('',*,*,#51031,.T.);
#67446=ORIENTED_EDGE('',*,*,#51032,.F.);
#67447=ORIENTED_EDGE('',*,*,#51033,.F.);
#67448=ORIENTED_EDGE('',*,*,#51034,.T.);
#67449=ORIENTED_EDGE('',*,*,#51035,.T.);
#67450=ORIENTED_EDGE('',*,*,#51036,.F.);
#67451=ORIENTED_EDGE('',*,*,#51031,.F.);
#67452=ORIENTED_EDGE('',*,*,#51037,.T.);
#67453=ORIENTED_EDGE('',*,*,#51038,.T.);
#67454=ORIENTED_EDGE('',*,*,#51039,.F.);
#67455=ORIENTED_EDGE('',*,*,#51035,.F.);
#67456=ORIENTED_EDGE('',*,*,#51040,.T.);
#67457=ORIENTED_EDGE('',*,*,#51033,.T.);
#67458=ORIENTED_EDGE('',*,*,#51041,.F.);
#67459=ORIENTED_EDGE('',*,*,#51038,.F.);
#67460=ORIENTED_EDGE('',*,*,#51042,.T.);
#67461=ORIENTED_EDGE('',*,*,#51043,.T.);
#67462=ORIENTED_EDGE('',*,*,#51044,.F.);
#67463=ORIENTED_EDGE('',*,*,#51045,.F.);
#67464=ORIENTED_EDGE('',*,*,#51046,.T.);
#67465=ORIENTED_EDGE('',*,*,#51047,.T.);
#67466=ORIENTED_EDGE('',*,*,#51048,.F.);
#67467=ORIENTED_EDGE('',*,*,#51043,.F.);
#67468=ORIENTED_EDGE('',*,*,#51049,.T.);
#67469=ORIENTED_EDGE('',*,*,#51050,.T.);
#67470=ORIENTED_EDGE('',*,*,#51051,.F.);
#67471=ORIENTED_EDGE('',*,*,#51047,.F.);
#67472=ORIENTED_EDGE('',*,*,#51052,.T.);
#67473=ORIENTED_EDGE('',*,*,#51045,.T.);
#67474=ORIENTED_EDGE('',*,*,#51053,.F.);
#67475=ORIENTED_EDGE('',*,*,#51050,.F.);
#67476=ORIENTED_EDGE('',*,*,#51054,.T.);
#67477=ORIENTED_EDGE('',*,*,#51055,.T.);
#67478=ORIENTED_EDGE('',*,*,#51056,.F.);
#67479=ORIENTED_EDGE('',*,*,#51057,.F.);
#67480=ORIENTED_EDGE('',*,*,#51058,.T.);
#67481=ORIENTED_EDGE('',*,*,#51059,.T.);
#67482=ORIENTED_EDGE('',*,*,#51060,.F.);
#67483=ORIENTED_EDGE('',*,*,#51055,.F.);
#67484=ORIENTED_EDGE('',*,*,#51061,.T.);
#67485=ORIENTED_EDGE('',*,*,#51062,.T.);
#67486=ORIENTED_EDGE('',*,*,#51063,.F.);
#67487=ORIENTED_EDGE('',*,*,#51059,.F.);
#67488=ORIENTED_EDGE('',*,*,#51064,.T.);
#67489=ORIENTED_EDGE('',*,*,#51057,.T.);
#67490=ORIENTED_EDGE('',*,*,#51065,.F.);
#67491=ORIENTED_EDGE('',*,*,#51062,.F.);
#67492=ORIENTED_EDGE('',*,*,#51066,.T.);
#67493=ORIENTED_EDGE('',*,*,#51067,.T.);
#67494=ORIENTED_EDGE('',*,*,#51068,.F.);
#67495=ORIENTED_EDGE('',*,*,#51069,.F.);
#67496=ORIENTED_EDGE('',*,*,#51070,.T.);
#67497=ORIENTED_EDGE('',*,*,#51071,.T.);
#67498=ORIENTED_EDGE('',*,*,#51072,.F.);
#67499=ORIENTED_EDGE('',*,*,#51067,.F.);
#67500=ORIENTED_EDGE('',*,*,#51073,.T.);
#67501=ORIENTED_EDGE('',*,*,#51074,.T.);
#67502=ORIENTED_EDGE('',*,*,#51075,.F.);
#67503=ORIENTED_EDGE('',*,*,#51071,.F.);
#67504=ORIENTED_EDGE('',*,*,#51076,.T.);
#67505=ORIENTED_EDGE('',*,*,#51069,.T.);
#67506=ORIENTED_EDGE('',*,*,#51077,.F.);
#67507=ORIENTED_EDGE('',*,*,#51074,.F.);
#67508=ORIENTED_EDGE('',*,*,#51078,.T.);
#67509=ORIENTED_EDGE('',*,*,#51079,.T.);
#67510=ORIENTED_EDGE('',*,*,#51080,.F.);
#67511=ORIENTED_EDGE('',*,*,#51081,.F.);
#67512=ORIENTED_EDGE('',*,*,#51082,.T.);
#67513=ORIENTED_EDGE('',*,*,#51083,.T.);
#67514=ORIENTED_EDGE('',*,*,#51084,.F.);
#67515=ORIENTED_EDGE('',*,*,#51079,.F.);
#67516=ORIENTED_EDGE('',*,*,#51085,.T.);
#67517=ORIENTED_EDGE('',*,*,#51086,.T.);
#67518=ORIENTED_EDGE('',*,*,#51087,.F.);
#67519=ORIENTED_EDGE('',*,*,#51083,.F.);
#67520=ORIENTED_EDGE('',*,*,#51088,.T.);
#67521=ORIENTED_EDGE('',*,*,#51081,.T.);
#67522=ORIENTED_EDGE('',*,*,#51089,.F.);
#67523=ORIENTED_EDGE('',*,*,#51086,.F.);
#67524=ORIENTED_EDGE('',*,*,#51090,.T.);
#67525=ORIENTED_EDGE('',*,*,#51091,.T.);
#67526=ORIENTED_EDGE('',*,*,#51092,.F.);
#67527=ORIENTED_EDGE('',*,*,#51093,.F.);
#67528=ORIENTED_EDGE('',*,*,#51094,.T.);
#67529=ORIENTED_EDGE('',*,*,#51095,.T.);
#67530=ORIENTED_EDGE('',*,*,#51096,.F.);
#67531=ORIENTED_EDGE('',*,*,#51091,.F.);
#67532=ORIENTED_EDGE('',*,*,#51097,.T.);
#67533=ORIENTED_EDGE('',*,*,#51098,.T.);
#67534=ORIENTED_EDGE('',*,*,#51099,.F.);
#67535=ORIENTED_EDGE('',*,*,#51095,.F.);
#67536=ORIENTED_EDGE('',*,*,#51100,.T.);
#67537=ORIENTED_EDGE('',*,*,#51093,.T.);
#67538=ORIENTED_EDGE('',*,*,#51101,.F.);
#67539=ORIENTED_EDGE('',*,*,#51098,.F.);
#67540=ORIENTED_EDGE('',*,*,#51102,.T.);
#67541=ORIENTED_EDGE('',*,*,#51103,.T.);
#67542=ORIENTED_EDGE('',*,*,#51104,.F.);
#67543=ORIENTED_EDGE('',*,*,#51105,.F.);
#67544=ORIENTED_EDGE('',*,*,#51106,.T.);
#67545=ORIENTED_EDGE('',*,*,#51107,.T.);
#67546=ORIENTED_EDGE('',*,*,#51108,.F.);
#67547=ORIENTED_EDGE('',*,*,#51103,.F.);
#67548=ORIENTED_EDGE('',*,*,#51109,.T.);
#67549=ORIENTED_EDGE('',*,*,#51110,.T.);
#67550=ORIENTED_EDGE('',*,*,#51111,.F.);
#67551=ORIENTED_EDGE('',*,*,#51107,.F.);
#67552=ORIENTED_EDGE('',*,*,#51112,.T.);
#67553=ORIENTED_EDGE('',*,*,#51105,.T.);
#67554=ORIENTED_EDGE('',*,*,#51113,.F.);
#67555=ORIENTED_EDGE('',*,*,#51110,.F.);
#67556=ORIENTED_EDGE('',*,*,#51114,.T.);
#67557=ORIENTED_EDGE('',*,*,#51115,.T.);
#67558=ORIENTED_EDGE('',*,*,#51116,.F.);
#67559=ORIENTED_EDGE('',*,*,#51117,.F.);
#67560=ORIENTED_EDGE('',*,*,#51118,.T.);
#67561=ORIENTED_EDGE('',*,*,#51119,.T.);
#67562=ORIENTED_EDGE('',*,*,#51120,.F.);
#67563=ORIENTED_EDGE('',*,*,#51115,.F.);
#67564=ORIENTED_EDGE('',*,*,#51121,.T.);
#67565=ORIENTED_EDGE('',*,*,#51122,.T.);
#67566=ORIENTED_EDGE('',*,*,#51123,.F.);
#67567=ORIENTED_EDGE('',*,*,#51119,.F.);
#67568=ORIENTED_EDGE('',*,*,#51124,.T.);
#67569=ORIENTED_EDGE('',*,*,#51117,.T.);
#67570=ORIENTED_EDGE('',*,*,#51125,.F.);
#67571=ORIENTED_EDGE('',*,*,#51122,.F.);
#67572=ORIENTED_EDGE('',*,*,#51126,.T.);
#67573=ORIENTED_EDGE('',*,*,#51127,.T.);
#67574=ORIENTED_EDGE('',*,*,#51128,.F.);
#67575=ORIENTED_EDGE('',*,*,#51129,.F.);
#67576=ORIENTED_EDGE('',*,*,#51130,.T.);
#67577=ORIENTED_EDGE('',*,*,#51131,.T.);
#67578=ORIENTED_EDGE('',*,*,#51132,.F.);
#67579=ORIENTED_EDGE('',*,*,#51127,.F.);
#67580=ORIENTED_EDGE('',*,*,#51133,.T.);
#67581=ORIENTED_EDGE('',*,*,#51134,.T.);
#67582=ORIENTED_EDGE('',*,*,#51135,.F.);
#67583=ORIENTED_EDGE('',*,*,#51131,.F.);
#67584=ORIENTED_EDGE('',*,*,#51136,.T.);
#67585=ORIENTED_EDGE('',*,*,#51129,.T.);
#67586=ORIENTED_EDGE('',*,*,#51137,.F.);
#67587=ORIENTED_EDGE('',*,*,#51134,.F.);
#67588=ORIENTED_EDGE('',*,*,#51138,.T.);
#67589=ORIENTED_EDGE('',*,*,#51139,.T.);
#67590=ORIENTED_EDGE('',*,*,#51140,.F.);
#67591=ORIENTED_EDGE('',*,*,#51141,.F.);
#67592=ORIENTED_EDGE('',*,*,#51142,.T.);
#67593=ORIENTED_EDGE('',*,*,#51143,.T.);
#67594=ORIENTED_EDGE('',*,*,#51144,.F.);
#67595=ORIENTED_EDGE('',*,*,#51139,.F.);
#67596=ORIENTED_EDGE('',*,*,#51145,.T.);
#67597=ORIENTED_EDGE('',*,*,#51146,.T.);
#67598=ORIENTED_EDGE('',*,*,#51147,.F.);
#67599=ORIENTED_EDGE('',*,*,#51143,.F.);
#67600=ORIENTED_EDGE('',*,*,#51148,.T.);
#67601=ORIENTED_EDGE('',*,*,#51141,.T.);
#67602=ORIENTED_EDGE('',*,*,#51149,.F.);
#67603=ORIENTED_EDGE('',*,*,#51146,.F.);
#67604=ORIENTED_EDGE('',*,*,#51150,.T.);
#67605=ORIENTED_EDGE('',*,*,#51151,.T.);
#67606=ORIENTED_EDGE('',*,*,#51152,.F.);
#67607=ORIENTED_EDGE('',*,*,#51153,.F.);
#67608=ORIENTED_EDGE('',*,*,#51154,.T.);
#67609=ORIENTED_EDGE('',*,*,#51155,.T.);
#67610=ORIENTED_EDGE('',*,*,#51156,.F.);
#67611=ORIENTED_EDGE('',*,*,#51151,.F.);
#67612=ORIENTED_EDGE('',*,*,#51157,.T.);
#67613=ORIENTED_EDGE('',*,*,#51158,.T.);
#67614=ORIENTED_EDGE('',*,*,#51159,.F.);
#67615=ORIENTED_EDGE('',*,*,#51155,.F.);
#67616=ORIENTED_EDGE('',*,*,#51160,.T.);
#67617=ORIENTED_EDGE('',*,*,#51153,.T.);
#67618=ORIENTED_EDGE('',*,*,#51161,.F.);
#67619=ORIENTED_EDGE('',*,*,#51158,.F.);
#67620=ORIENTED_EDGE('',*,*,#51162,.T.);
#67621=ORIENTED_EDGE('',*,*,#51163,.T.);
#67622=ORIENTED_EDGE('',*,*,#51164,.F.);
#67623=ORIENTED_EDGE('',*,*,#51165,.F.);
#67624=ORIENTED_EDGE('',*,*,#51166,.T.);
#67625=ORIENTED_EDGE('',*,*,#51167,.T.);
#67626=ORIENTED_EDGE('',*,*,#51168,.F.);
#67627=ORIENTED_EDGE('',*,*,#51163,.F.);
#67628=ORIENTED_EDGE('',*,*,#51169,.T.);
#67629=ORIENTED_EDGE('',*,*,#51170,.T.);
#67630=ORIENTED_EDGE('',*,*,#51171,.F.);
#67631=ORIENTED_EDGE('',*,*,#51167,.F.);
#67632=ORIENTED_EDGE('',*,*,#51172,.T.);
#67633=ORIENTED_EDGE('',*,*,#51165,.T.);
#67634=ORIENTED_EDGE('',*,*,#51173,.F.);
#67635=ORIENTED_EDGE('',*,*,#51170,.F.);
#67636=ORIENTED_EDGE('',*,*,#51174,.T.);
#67637=ORIENTED_EDGE('',*,*,#51175,.T.);
#67638=ORIENTED_EDGE('',*,*,#51176,.F.);
#67639=ORIENTED_EDGE('',*,*,#51177,.F.);
#67640=ORIENTED_EDGE('',*,*,#51178,.T.);
#67641=ORIENTED_EDGE('',*,*,#51179,.T.);
#67642=ORIENTED_EDGE('',*,*,#51180,.F.);
#67643=ORIENTED_EDGE('',*,*,#51175,.F.);
#67644=ORIENTED_EDGE('',*,*,#51181,.T.);
#67645=ORIENTED_EDGE('',*,*,#51182,.T.);
#67646=ORIENTED_EDGE('',*,*,#51183,.F.);
#67647=ORIENTED_EDGE('',*,*,#51179,.F.);
#67648=ORIENTED_EDGE('',*,*,#51184,.T.);
#67649=ORIENTED_EDGE('',*,*,#51177,.T.);
#67650=ORIENTED_EDGE('',*,*,#51185,.F.);
#67651=ORIENTED_EDGE('',*,*,#51182,.F.);
#67652=ORIENTED_EDGE('',*,*,#51186,.T.);
#67653=ORIENTED_EDGE('',*,*,#51187,.T.);
#67654=ORIENTED_EDGE('',*,*,#51188,.F.);
#67655=ORIENTED_EDGE('',*,*,#51189,.F.);
#67656=ORIENTED_EDGE('',*,*,#51190,.T.);
#67657=ORIENTED_EDGE('',*,*,#51191,.T.);
#67658=ORIENTED_EDGE('',*,*,#51192,.F.);
#67659=ORIENTED_EDGE('',*,*,#51187,.F.);
#67660=ORIENTED_EDGE('',*,*,#51193,.T.);
#67661=ORIENTED_EDGE('',*,*,#51194,.T.);
#67662=ORIENTED_EDGE('',*,*,#51195,.F.);
#67663=ORIENTED_EDGE('',*,*,#51191,.F.);
#67664=ORIENTED_EDGE('',*,*,#51196,.T.);
#67665=ORIENTED_EDGE('',*,*,#51189,.T.);
#67666=ORIENTED_EDGE('',*,*,#51197,.F.);
#67667=ORIENTED_EDGE('',*,*,#51194,.F.);
#67668=ORIENTED_EDGE('',*,*,#51198,.T.);
#67669=ORIENTED_EDGE('',*,*,#51199,.T.);
#67670=ORIENTED_EDGE('',*,*,#51200,.F.);
#67671=ORIENTED_EDGE('',*,*,#51201,.F.);
#67672=ORIENTED_EDGE('',*,*,#51202,.T.);
#67673=ORIENTED_EDGE('',*,*,#51203,.T.);
#67674=ORIENTED_EDGE('',*,*,#51204,.F.);
#67675=ORIENTED_EDGE('',*,*,#51199,.F.);
#67676=ORIENTED_EDGE('',*,*,#51205,.T.);
#67677=ORIENTED_EDGE('',*,*,#51206,.T.);
#67678=ORIENTED_EDGE('',*,*,#51207,.F.);
#67679=ORIENTED_EDGE('',*,*,#51203,.F.);
#67680=ORIENTED_EDGE('',*,*,#51208,.T.);
#67681=ORIENTED_EDGE('',*,*,#51201,.T.);
#67682=ORIENTED_EDGE('',*,*,#51209,.F.);
#67683=ORIENTED_EDGE('',*,*,#51206,.F.);
#67684=ORIENTED_EDGE('',*,*,#51210,.T.);
#67685=ORIENTED_EDGE('',*,*,#51211,.T.);
#67686=ORIENTED_EDGE('',*,*,#51212,.F.);
#67687=ORIENTED_EDGE('',*,*,#51213,.F.);
#67688=ORIENTED_EDGE('',*,*,#51214,.T.);
#67689=ORIENTED_EDGE('',*,*,#51215,.T.);
#67690=ORIENTED_EDGE('',*,*,#51216,.F.);
#67691=ORIENTED_EDGE('',*,*,#51211,.F.);
#67692=ORIENTED_EDGE('',*,*,#51217,.T.);
#67693=ORIENTED_EDGE('',*,*,#51218,.T.);
#67694=ORIENTED_EDGE('',*,*,#51219,.F.);
#67695=ORIENTED_EDGE('',*,*,#51215,.F.);
#67696=ORIENTED_EDGE('',*,*,#51220,.T.);
#67697=ORIENTED_EDGE('',*,*,#51213,.T.);
#67698=ORIENTED_EDGE('',*,*,#51221,.F.);
#67699=ORIENTED_EDGE('',*,*,#51218,.F.);
#67700=ORIENTED_EDGE('',*,*,#51222,.T.);
#67701=ORIENTED_EDGE('',*,*,#51223,.T.);
#67702=ORIENTED_EDGE('',*,*,#51224,.F.);
#67703=ORIENTED_EDGE('',*,*,#51225,.F.);
#67704=ORIENTED_EDGE('',*,*,#51226,.T.);
#67705=ORIENTED_EDGE('',*,*,#51227,.T.);
#67706=ORIENTED_EDGE('',*,*,#51228,.F.);
#67707=ORIENTED_EDGE('',*,*,#51223,.F.);
#67708=ORIENTED_EDGE('',*,*,#51229,.T.);
#67709=ORIENTED_EDGE('',*,*,#51230,.T.);
#67710=ORIENTED_EDGE('',*,*,#51231,.F.);
#67711=ORIENTED_EDGE('',*,*,#51227,.F.);
#67712=ORIENTED_EDGE('',*,*,#51232,.T.);
#67713=ORIENTED_EDGE('',*,*,#51225,.T.);
#67714=ORIENTED_EDGE('',*,*,#51233,.F.);
#67715=ORIENTED_EDGE('',*,*,#51230,.F.);
#67716=ORIENTED_EDGE('',*,*,#51234,.T.);
#67717=ORIENTED_EDGE('',*,*,#51235,.T.);
#67718=ORIENTED_EDGE('',*,*,#51236,.F.);
#67719=ORIENTED_EDGE('',*,*,#51237,.F.);
#67720=ORIENTED_EDGE('',*,*,#51238,.T.);
#67721=ORIENTED_EDGE('',*,*,#51239,.T.);
#67722=ORIENTED_EDGE('',*,*,#51240,.F.);
#67723=ORIENTED_EDGE('',*,*,#51235,.F.);
#67724=ORIENTED_EDGE('',*,*,#51241,.T.);
#67725=ORIENTED_EDGE('',*,*,#51242,.T.);
#67726=ORIENTED_EDGE('',*,*,#51243,.F.);
#67727=ORIENTED_EDGE('',*,*,#51239,.F.);
#67728=ORIENTED_EDGE('',*,*,#51244,.T.);
#67729=ORIENTED_EDGE('',*,*,#51237,.T.);
#67730=ORIENTED_EDGE('',*,*,#51245,.F.);
#67731=ORIENTED_EDGE('',*,*,#51242,.F.);
#67732=ORIENTED_EDGE('',*,*,#51246,.T.);
#67733=ORIENTED_EDGE('',*,*,#51247,.T.);
#67734=ORIENTED_EDGE('',*,*,#51248,.F.);
#67735=ORIENTED_EDGE('',*,*,#51249,.F.);
#67736=ORIENTED_EDGE('',*,*,#51250,.T.);
#67737=ORIENTED_EDGE('',*,*,#51251,.T.);
#67738=ORIENTED_EDGE('',*,*,#51252,.F.);
#67739=ORIENTED_EDGE('',*,*,#51247,.F.);
#67740=ORIENTED_EDGE('',*,*,#51253,.T.);
#67741=ORIENTED_EDGE('',*,*,#51254,.T.);
#67742=ORIENTED_EDGE('',*,*,#51255,.F.);
#67743=ORIENTED_EDGE('',*,*,#51251,.F.);
#67744=ORIENTED_EDGE('',*,*,#51256,.T.);
#67745=ORIENTED_EDGE('',*,*,#51249,.T.);
#67746=ORIENTED_EDGE('',*,*,#51257,.F.);
#67747=ORIENTED_EDGE('',*,*,#51254,.F.);
#67748=ORIENTED_EDGE('',*,*,#51258,.T.);
#67749=ORIENTED_EDGE('',*,*,#51259,.T.);
#67750=ORIENTED_EDGE('',*,*,#51260,.F.);
#67751=ORIENTED_EDGE('',*,*,#51261,.F.);
#67752=ORIENTED_EDGE('',*,*,#51262,.T.);
#67753=ORIENTED_EDGE('',*,*,#51263,.T.);
#67754=ORIENTED_EDGE('',*,*,#51264,.F.);
#67755=ORIENTED_EDGE('',*,*,#51259,.F.);
#67756=ORIENTED_EDGE('',*,*,#51265,.T.);
#67757=ORIENTED_EDGE('',*,*,#51266,.T.);
#67758=ORIENTED_EDGE('',*,*,#51267,.F.);
#67759=ORIENTED_EDGE('',*,*,#51263,.F.);
#67760=ORIENTED_EDGE('',*,*,#51268,.T.);
#67761=ORIENTED_EDGE('',*,*,#51261,.T.);
#67762=ORIENTED_EDGE('',*,*,#51269,.F.);
#67763=ORIENTED_EDGE('',*,*,#51266,.F.);
#67764=ORIENTED_EDGE('',*,*,#51270,.T.);
#67765=ORIENTED_EDGE('',*,*,#51271,.T.);
#67766=ORIENTED_EDGE('',*,*,#51272,.F.);
#67767=ORIENTED_EDGE('',*,*,#51273,.F.);
#67768=ORIENTED_EDGE('',*,*,#51274,.T.);
#67769=ORIENTED_EDGE('',*,*,#51275,.T.);
#67770=ORIENTED_EDGE('',*,*,#51276,.F.);
#67771=ORIENTED_EDGE('',*,*,#51271,.F.);
#67772=ORIENTED_EDGE('',*,*,#51277,.T.);
#67773=ORIENTED_EDGE('',*,*,#51278,.T.);
#67774=ORIENTED_EDGE('',*,*,#51279,.F.);
#67775=ORIENTED_EDGE('',*,*,#51275,.F.);
#67776=ORIENTED_EDGE('',*,*,#51280,.T.);
#67777=ORIENTED_EDGE('',*,*,#51273,.T.);
#67778=ORIENTED_EDGE('',*,*,#51281,.F.);
#67779=ORIENTED_EDGE('',*,*,#51278,.F.);
#67780=ORIENTED_EDGE('',*,*,#51282,.T.);
#67781=ORIENTED_EDGE('',*,*,#51283,.T.);
#67782=ORIENTED_EDGE('',*,*,#51284,.F.);
#67783=ORIENTED_EDGE('',*,*,#51285,.F.);
#67784=ORIENTED_EDGE('',*,*,#51286,.T.);
#67785=ORIENTED_EDGE('',*,*,#51287,.T.);
#67786=ORIENTED_EDGE('',*,*,#51288,.F.);
#67787=ORIENTED_EDGE('',*,*,#51283,.F.);
#67788=ORIENTED_EDGE('',*,*,#51289,.T.);
#67789=ORIENTED_EDGE('',*,*,#51290,.T.);
#67790=ORIENTED_EDGE('',*,*,#51291,.F.);
#67791=ORIENTED_EDGE('',*,*,#51287,.F.);
#67792=ORIENTED_EDGE('',*,*,#51292,.T.);
#67793=ORIENTED_EDGE('',*,*,#51285,.T.);
#67794=ORIENTED_EDGE('',*,*,#51293,.F.);
#67795=ORIENTED_EDGE('',*,*,#51290,.F.);
#67796=ORIENTED_EDGE('',*,*,#51294,.T.);
#67797=ORIENTED_EDGE('',*,*,#51295,.T.);
#67798=ORIENTED_EDGE('',*,*,#51296,.F.);
#67799=ORIENTED_EDGE('',*,*,#51297,.F.);
#67800=ORIENTED_EDGE('',*,*,#51298,.T.);
#67801=ORIENTED_EDGE('',*,*,#51299,.T.);
#67802=ORIENTED_EDGE('',*,*,#51300,.F.);
#67803=ORIENTED_EDGE('',*,*,#51295,.F.);
#67804=ORIENTED_EDGE('',*,*,#51301,.T.);
#67805=ORIENTED_EDGE('',*,*,#51302,.T.);
#67806=ORIENTED_EDGE('',*,*,#51303,.F.);
#67807=ORIENTED_EDGE('',*,*,#51299,.F.);
#67808=ORIENTED_EDGE('',*,*,#51304,.T.);
#67809=ORIENTED_EDGE('',*,*,#51297,.T.);
#67810=ORIENTED_EDGE('',*,*,#51305,.F.);
#67811=ORIENTED_EDGE('',*,*,#51302,.F.);
#67812=ORIENTED_EDGE('',*,*,#51306,.T.);
#67813=ORIENTED_EDGE('',*,*,#51307,.T.);
#67814=ORIENTED_EDGE('',*,*,#51308,.F.);
#67815=ORIENTED_EDGE('',*,*,#51309,.F.);
#67816=ORIENTED_EDGE('',*,*,#51310,.T.);
#67817=ORIENTED_EDGE('',*,*,#51311,.T.);
#67818=ORIENTED_EDGE('',*,*,#51312,.F.);
#67819=ORIENTED_EDGE('',*,*,#51307,.F.);
#67820=ORIENTED_EDGE('',*,*,#51313,.T.);
#67821=ORIENTED_EDGE('',*,*,#51314,.T.);
#67822=ORIENTED_EDGE('',*,*,#51315,.F.);
#67823=ORIENTED_EDGE('',*,*,#51311,.F.);
#67824=ORIENTED_EDGE('',*,*,#51316,.T.);
#67825=ORIENTED_EDGE('',*,*,#51309,.T.);
#67826=ORIENTED_EDGE('',*,*,#51317,.F.);
#67827=ORIENTED_EDGE('',*,*,#51314,.F.);
#67828=ORIENTED_EDGE('',*,*,#51318,.T.);
#67829=ORIENTED_EDGE('',*,*,#51319,.T.);
#67830=ORIENTED_EDGE('',*,*,#51320,.F.);
#67831=ORIENTED_EDGE('',*,*,#51321,.F.);
#67832=ORIENTED_EDGE('',*,*,#51322,.T.);
#67833=ORIENTED_EDGE('',*,*,#51323,.T.);
#67834=ORIENTED_EDGE('',*,*,#51324,.F.);
#67835=ORIENTED_EDGE('',*,*,#51319,.F.);
#67836=ORIENTED_EDGE('',*,*,#51325,.T.);
#67837=ORIENTED_EDGE('',*,*,#51326,.T.);
#67838=ORIENTED_EDGE('',*,*,#51327,.F.);
#67839=ORIENTED_EDGE('',*,*,#51323,.F.);
#67840=ORIENTED_EDGE('',*,*,#51328,.T.);
#67841=ORIENTED_EDGE('',*,*,#51321,.T.);
#67842=ORIENTED_EDGE('',*,*,#51329,.F.);
#67843=ORIENTED_EDGE('',*,*,#51326,.F.);
#67844=ORIENTED_EDGE('',*,*,#51330,.T.);
#67845=ORIENTED_EDGE('',*,*,#51331,.T.);
#67846=ORIENTED_EDGE('',*,*,#51332,.F.);
#67847=ORIENTED_EDGE('',*,*,#51333,.F.);
#67848=ORIENTED_EDGE('',*,*,#51334,.T.);
#67849=ORIENTED_EDGE('',*,*,#51335,.T.);
#67850=ORIENTED_EDGE('',*,*,#51336,.F.);
#67851=ORIENTED_EDGE('',*,*,#51331,.F.);
#67852=ORIENTED_EDGE('',*,*,#51337,.T.);
#67853=ORIENTED_EDGE('',*,*,#51338,.T.);
#67854=ORIENTED_EDGE('',*,*,#51339,.F.);
#67855=ORIENTED_EDGE('',*,*,#51335,.F.);
#67856=ORIENTED_EDGE('',*,*,#51340,.T.);
#67857=ORIENTED_EDGE('',*,*,#51333,.T.);
#67858=ORIENTED_EDGE('',*,*,#51341,.F.);
#67859=ORIENTED_EDGE('',*,*,#51338,.F.);
#67860=ORIENTED_EDGE('',*,*,#51342,.T.);
#67861=ORIENTED_EDGE('',*,*,#51343,.T.);
#67862=ORIENTED_EDGE('',*,*,#51344,.F.);
#67863=ORIENTED_EDGE('',*,*,#51345,.F.);
#67864=ORIENTED_EDGE('',*,*,#51346,.T.);
#67865=ORIENTED_EDGE('',*,*,#51347,.T.);
#67866=ORIENTED_EDGE('',*,*,#51348,.F.);
#67867=ORIENTED_EDGE('',*,*,#51343,.F.);
#67868=ORIENTED_EDGE('',*,*,#51349,.T.);
#67869=ORIENTED_EDGE('',*,*,#51350,.T.);
#67870=ORIENTED_EDGE('',*,*,#51351,.F.);
#67871=ORIENTED_EDGE('',*,*,#51347,.F.);
#67872=ORIENTED_EDGE('',*,*,#51352,.T.);
#67873=ORIENTED_EDGE('',*,*,#51345,.T.);
#67874=ORIENTED_EDGE('',*,*,#51353,.F.);
#67875=ORIENTED_EDGE('',*,*,#51350,.F.);
#67876=ORIENTED_EDGE('',*,*,#51354,.T.);
#67877=ORIENTED_EDGE('',*,*,#51355,.T.);
#67878=ORIENTED_EDGE('',*,*,#51356,.F.);
#67879=ORIENTED_EDGE('',*,*,#51357,.F.);
#67880=ORIENTED_EDGE('',*,*,#51358,.T.);
#67881=ORIENTED_EDGE('',*,*,#51359,.T.);
#67882=ORIENTED_EDGE('',*,*,#51360,.F.);
#67883=ORIENTED_EDGE('',*,*,#51355,.F.);
#67884=ORIENTED_EDGE('',*,*,#51361,.T.);
#67885=ORIENTED_EDGE('',*,*,#51362,.T.);
#67886=ORIENTED_EDGE('',*,*,#51363,.F.);
#67887=ORIENTED_EDGE('',*,*,#51359,.F.);
#67888=ORIENTED_EDGE('',*,*,#51364,.T.);
#67889=ORIENTED_EDGE('',*,*,#51357,.T.);
#67890=ORIENTED_EDGE('',*,*,#51365,.F.);
#67891=ORIENTED_EDGE('',*,*,#51362,.F.);
#67892=ORIENTED_EDGE('',*,*,#51366,.T.);
#67893=ORIENTED_EDGE('',*,*,#51367,.T.);
#67894=ORIENTED_EDGE('',*,*,#51368,.F.);
#67895=ORIENTED_EDGE('',*,*,#51369,.F.);
#67896=ORIENTED_EDGE('',*,*,#51370,.T.);
#67897=ORIENTED_EDGE('',*,*,#51371,.T.);
#67898=ORIENTED_EDGE('',*,*,#51372,.F.);
#67899=ORIENTED_EDGE('',*,*,#51367,.F.);
#67900=ORIENTED_EDGE('',*,*,#51373,.T.);
#67901=ORIENTED_EDGE('',*,*,#51374,.T.);
#67902=ORIENTED_EDGE('',*,*,#51375,.F.);
#67903=ORIENTED_EDGE('',*,*,#51371,.F.);
#67904=ORIENTED_EDGE('',*,*,#51376,.T.);
#67905=ORIENTED_EDGE('',*,*,#51369,.T.);
#67906=ORIENTED_EDGE('',*,*,#51377,.F.);
#67907=ORIENTED_EDGE('',*,*,#51374,.F.);
#67908=ORIENTED_EDGE('',*,*,#51378,.T.);
#67909=ORIENTED_EDGE('',*,*,#51379,.T.);
#67910=ORIENTED_EDGE('',*,*,#51380,.F.);
#67911=ORIENTED_EDGE('',*,*,#51381,.F.);
#67912=ORIENTED_EDGE('',*,*,#51382,.T.);
#67913=ORIENTED_EDGE('',*,*,#51383,.T.);
#67914=ORIENTED_EDGE('',*,*,#51384,.F.);
#67915=ORIENTED_EDGE('',*,*,#51379,.F.);
#67916=ORIENTED_EDGE('',*,*,#51385,.T.);
#67917=ORIENTED_EDGE('',*,*,#51386,.T.);
#67918=ORIENTED_EDGE('',*,*,#51387,.F.);
#67919=ORIENTED_EDGE('',*,*,#51383,.F.);
#67920=ORIENTED_EDGE('',*,*,#51388,.T.);
#67921=ORIENTED_EDGE('',*,*,#51381,.T.);
#67922=ORIENTED_EDGE('',*,*,#51389,.F.);
#67923=ORIENTED_EDGE('',*,*,#51386,.F.);
#67924=ORIENTED_EDGE('',*,*,#51390,.T.);
#67925=ORIENTED_EDGE('',*,*,#51391,.T.);
#67926=ORIENTED_EDGE('',*,*,#51392,.F.);
#67927=ORIENTED_EDGE('',*,*,#51393,.F.);
#67928=ORIENTED_EDGE('',*,*,#51394,.T.);
#67929=ORIENTED_EDGE('',*,*,#51395,.T.);
#67930=ORIENTED_EDGE('',*,*,#51396,.F.);
#67931=ORIENTED_EDGE('',*,*,#51391,.F.);
#67932=ORIENTED_EDGE('',*,*,#51397,.T.);
#67933=ORIENTED_EDGE('',*,*,#51398,.T.);
#67934=ORIENTED_EDGE('',*,*,#51399,.F.);
#67935=ORIENTED_EDGE('',*,*,#51395,.F.);
#67936=ORIENTED_EDGE('',*,*,#51400,.T.);
#67937=ORIENTED_EDGE('',*,*,#51393,.T.);
#67938=ORIENTED_EDGE('',*,*,#51401,.F.);
#67939=ORIENTED_EDGE('',*,*,#51398,.F.);
#67940=ORIENTED_EDGE('',*,*,#51402,.T.);
#67941=ORIENTED_EDGE('',*,*,#51403,.T.);
#67942=ORIENTED_EDGE('',*,*,#51404,.F.);
#67943=ORIENTED_EDGE('',*,*,#51405,.F.);
#67944=ORIENTED_EDGE('',*,*,#51406,.T.);
#67945=ORIENTED_EDGE('',*,*,#51407,.T.);
#67946=ORIENTED_EDGE('',*,*,#51408,.F.);
#67947=ORIENTED_EDGE('',*,*,#51403,.F.);
#67948=ORIENTED_EDGE('',*,*,#51409,.T.);
#67949=ORIENTED_EDGE('',*,*,#51410,.T.);
#67950=ORIENTED_EDGE('',*,*,#51411,.F.);
#67951=ORIENTED_EDGE('',*,*,#51407,.F.);
#67952=ORIENTED_EDGE('',*,*,#51412,.T.);
#67953=ORIENTED_EDGE('',*,*,#51405,.T.);
#67954=ORIENTED_EDGE('',*,*,#51413,.F.);
#67955=ORIENTED_EDGE('',*,*,#51410,.F.);
#67956=ORIENTED_EDGE('',*,*,#51414,.T.);
#67957=ORIENTED_EDGE('',*,*,#51415,.T.);
#67958=ORIENTED_EDGE('',*,*,#51416,.F.);
#67959=ORIENTED_EDGE('',*,*,#51417,.F.);
#67960=ORIENTED_EDGE('',*,*,#51418,.T.);
#67961=ORIENTED_EDGE('',*,*,#51419,.T.);
#67962=ORIENTED_EDGE('',*,*,#51420,.F.);
#67963=ORIENTED_EDGE('',*,*,#51415,.F.);
#67964=ORIENTED_EDGE('',*,*,#51421,.T.);
#67965=ORIENTED_EDGE('',*,*,#51422,.T.);
#67966=ORIENTED_EDGE('',*,*,#51423,.F.);
#67967=ORIENTED_EDGE('',*,*,#51419,.F.);
#67968=ORIENTED_EDGE('',*,*,#51424,.T.);
#67969=ORIENTED_EDGE('',*,*,#51417,.T.);
#67970=ORIENTED_EDGE('',*,*,#51425,.F.);
#67971=ORIENTED_EDGE('',*,*,#51422,.F.);
#67972=ORIENTED_EDGE('',*,*,#51426,.T.);
#67973=ORIENTED_EDGE('',*,*,#51427,.T.);
#67974=ORIENTED_EDGE('',*,*,#51428,.F.);
#67975=ORIENTED_EDGE('',*,*,#51429,.F.);
#67976=ORIENTED_EDGE('',*,*,#51430,.T.);
#67977=ORIENTED_EDGE('',*,*,#51431,.T.);
#67978=ORIENTED_EDGE('',*,*,#51432,.F.);
#67979=ORIENTED_EDGE('',*,*,#51427,.F.);
#67980=ORIENTED_EDGE('',*,*,#51433,.T.);
#67981=ORIENTED_EDGE('',*,*,#51434,.T.);
#67982=ORIENTED_EDGE('',*,*,#51435,.F.);
#67983=ORIENTED_EDGE('',*,*,#51431,.F.);
#67984=ORIENTED_EDGE('',*,*,#51436,.T.);
#67985=ORIENTED_EDGE('',*,*,#51429,.T.);
#67986=ORIENTED_EDGE('',*,*,#51437,.F.);
#67987=ORIENTED_EDGE('',*,*,#51434,.F.);
#67988=ORIENTED_EDGE('',*,*,#51438,.T.);
#67989=ORIENTED_EDGE('',*,*,#51439,.T.);
#67990=ORIENTED_EDGE('',*,*,#51440,.F.);
#67991=ORIENTED_EDGE('',*,*,#51441,.F.);
#67992=ORIENTED_EDGE('',*,*,#51442,.T.);
#67993=ORIENTED_EDGE('',*,*,#51443,.T.);
#67994=ORIENTED_EDGE('',*,*,#51444,.F.);
#67995=ORIENTED_EDGE('',*,*,#51439,.F.);
#67996=ORIENTED_EDGE('',*,*,#51445,.T.);
#67997=ORIENTED_EDGE('',*,*,#51446,.T.);
#67998=ORIENTED_EDGE('',*,*,#51447,.F.);
#67999=ORIENTED_EDGE('',*,*,#51443,.F.);
#68000=ORIENTED_EDGE('',*,*,#51448,.T.);
#68001=ORIENTED_EDGE('',*,*,#51441,.T.);
#68002=ORIENTED_EDGE('',*,*,#51449,.F.);
#68003=ORIENTED_EDGE('',*,*,#51446,.F.);
#68004=ORIENTED_EDGE('',*,*,#51450,.T.);
#68005=ORIENTED_EDGE('',*,*,#51451,.T.);
#68006=ORIENTED_EDGE('',*,*,#51452,.F.);
#68007=ORIENTED_EDGE('',*,*,#51453,.F.);
#68008=ORIENTED_EDGE('',*,*,#51454,.T.);
#68009=ORIENTED_EDGE('',*,*,#51455,.T.);
#68010=ORIENTED_EDGE('',*,*,#51456,.F.);
#68011=ORIENTED_EDGE('',*,*,#51451,.F.);
#68012=ORIENTED_EDGE('',*,*,#51457,.T.);
#68013=ORIENTED_EDGE('',*,*,#51458,.T.);
#68014=ORIENTED_EDGE('',*,*,#51459,.F.);
#68015=ORIENTED_EDGE('',*,*,#51455,.F.);
#68016=ORIENTED_EDGE('',*,*,#51460,.T.);
#68017=ORIENTED_EDGE('',*,*,#51453,.T.);
#68018=ORIENTED_EDGE('',*,*,#51461,.F.);
#68019=ORIENTED_EDGE('',*,*,#51458,.F.);
#68020=ORIENTED_EDGE('',*,*,#51462,.T.);
#68021=ORIENTED_EDGE('',*,*,#51463,.T.);
#68022=ORIENTED_EDGE('',*,*,#51464,.F.);
#68023=ORIENTED_EDGE('',*,*,#51465,.F.);
#68024=ORIENTED_EDGE('',*,*,#51466,.T.);
#68025=ORIENTED_EDGE('',*,*,#51467,.T.);
#68026=ORIENTED_EDGE('',*,*,#51468,.F.);
#68027=ORIENTED_EDGE('',*,*,#51463,.F.);
#68028=ORIENTED_EDGE('',*,*,#51469,.T.);
#68029=ORIENTED_EDGE('',*,*,#51470,.T.);
#68030=ORIENTED_EDGE('',*,*,#51471,.F.);
#68031=ORIENTED_EDGE('',*,*,#51467,.F.);
#68032=ORIENTED_EDGE('',*,*,#51472,.T.);
#68033=ORIENTED_EDGE('',*,*,#51465,.T.);
#68034=ORIENTED_EDGE('',*,*,#51473,.F.);
#68035=ORIENTED_EDGE('',*,*,#51470,.F.);
#68036=ORIENTED_EDGE('',*,*,#51474,.T.);
#68037=ORIENTED_EDGE('',*,*,#51475,.T.);
#68038=ORIENTED_EDGE('',*,*,#51476,.F.);
#68039=ORIENTED_EDGE('',*,*,#51477,.F.);
#68040=ORIENTED_EDGE('',*,*,#51478,.T.);
#68041=ORIENTED_EDGE('',*,*,#51479,.T.);
#68042=ORIENTED_EDGE('',*,*,#51480,.F.);
#68043=ORIENTED_EDGE('',*,*,#51475,.F.);
#68044=ORIENTED_EDGE('',*,*,#51481,.T.);
#68045=ORIENTED_EDGE('',*,*,#51482,.T.);
#68046=ORIENTED_EDGE('',*,*,#51483,.F.);
#68047=ORIENTED_EDGE('',*,*,#51479,.F.);
#68048=ORIENTED_EDGE('',*,*,#51484,.T.);
#68049=ORIENTED_EDGE('',*,*,#51477,.T.);
#68050=ORIENTED_EDGE('',*,*,#51485,.F.);
#68051=ORIENTED_EDGE('',*,*,#51482,.F.);
#68052=ORIENTED_EDGE('',*,*,#51486,.T.);
#68053=ORIENTED_EDGE('',*,*,#51487,.T.);
#68054=ORIENTED_EDGE('',*,*,#51488,.F.);
#68055=ORIENTED_EDGE('',*,*,#51489,.F.);
#68056=ORIENTED_EDGE('',*,*,#51490,.T.);
#68057=ORIENTED_EDGE('',*,*,#51491,.T.);
#68058=ORIENTED_EDGE('',*,*,#51492,.F.);
#68059=ORIENTED_EDGE('',*,*,#51487,.F.);
#68060=ORIENTED_EDGE('',*,*,#51493,.T.);
#68061=ORIENTED_EDGE('',*,*,#51494,.T.);
#68062=ORIENTED_EDGE('',*,*,#51495,.F.);
#68063=ORIENTED_EDGE('',*,*,#51491,.F.);
#68064=ORIENTED_EDGE('',*,*,#51496,.T.);
#68065=ORIENTED_EDGE('',*,*,#51489,.T.);
#68066=ORIENTED_EDGE('',*,*,#51497,.F.);
#68067=ORIENTED_EDGE('',*,*,#51494,.F.);
#68068=ORIENTED_EDGE('',*,*,#51498,.T.);
#68069=ORIENTED_EDGE('',*,*,#51499,.T.);
#68070=ORIENTED_EDGE('',*,*,#51500,.F.);
#68071=ORIENTED_EDGE('',*,*,#51501,.F.);
#68072=ORIENTED_EDGE('',*,*,#51502,.T.);
#68073=ORIENTED_EDGE('',*,*,#51503,.T.);
#68074=ORIENTED_EDGE('',*,*,#51504,.F.);
#68075=ORIENTED_EDGE('',*,*,#51499,.F.);
#68076=ORIENTED_EDGE('',*,*,#51505,.T.);
#68077=ORIENTED_EDGE('',*,*,#51506,.T.);
#68078=ORIENTED_EDGE('',*,*,#51507,.F.);
#68079=ORIENTED_EDGE('',*,*,#51503,.F.);
#68080=ORIENTED_EDGE('',*,*,#51508,.T.);
#68081=ORIENTED_EDGE('',*,*,#51501,.T.);
#68082=ORIENTED_EDGE('',*,*,#51509,.F.);
#68083=ORIENTED_EDGE('',*,*,#51506,.F.);
#68084=ORIENTED_EDGE('',*,*,#51510,.T.);
#68085=ORIENTED_EDGE('',*,*,#51511,.T.);
#68086=ORIENTED_EDGE('',*,*,#51512,.F.);
#68087=ORIENTED_EDGE('',*,*,#51513,.F.);
#68088=ORIENTED_EDGE('',*,*,#51514,.T.);
#68089=ORIENTED_EDGE('',*,*,#51515,.T.);
#68090=ORIENTED_EDGE('',*,*,#51516,.F.);
#68091=ORIENTED_EDGE('',*,*,#51511,.F.);
#68092=ORIENTED_EDGE('',*,*,#51517,.T.);
#68093=ORIENTED_EDGE('',*,*,#51518,.T.);
#68094=ORIENTED_EDGE('',*,*,#51519,.F.);
#68095=ORIENTED_EDGE('',*,*,#51515,.F.);
#68096=ORIENTED_EDGE('',*,*,#51520,.T.);
#68097=ORIENTED_EDGE('',*,*,#51513,.T.);
#68098=ORIENTED_EDGE('',*,*,#51521,.F.);
#68099=ORIENTED_EDGE('',*,*,#51518,.F.);
#68100=ORIENTED_EDGE('',*,*,#51522,.T.);
#68101=ORIENTED_EDGE('',*,*,#51523,.T.);
#68102=ORIENTED_EDGE('',*,*,#51524,.F.);
#68103=ORIENTED_EDGE('',*,*,#51525,.F.);
#68104=ORIENTED_EDGE('',*,*,#51526,.T.);
#68105=ORIENTED_EDGE('',*,*,#51527,.T.);
#68106=ORIENTED_EDGE('',*,*,#51528,.F.);
#68107=ORIENTED_EDGE('',*,*,#51523,.F.);
#68108=ORIENTED_EDGE('',*,*,#51529,.T.);
#68109=ORIENTED_EDGE('',*,*,#51530,.T.);
#68110=ORIENTED_EDGE('',*,*,#51531,.F.);
#68111=ORIENTED_EDGE('',*,*,#51527,.F.);
#68112=ORIENTED_EDGE('',*,*,#51532,.T.);
#68113=ORIENTED_EDGE('',*,*,#51525,.T.);
#68114=ORIENTED_EDGE('',*,*,#51533,.F.);
#68115=ORIENTED_EDGE('',*,*,#51530,.F.);
#68116=ORIENTED_EDGE('',*,*,#51534,.T.);
#68117=ORIENTED_EDGE('',*,*,#51535,.T.);
#68118=ORIENTED_EDGE('',*,*,#51536,.F.);
#68119=ORIENTED_EDGE('',*,*,#51537,.F.);
#68120=ORIENTED_EDGE('',*,*,#51538,.T.);
#68121=ORIENTED_EDGE('',*,*,#51539,.T.);
#68122=ORIENTED_EDGE('',*,*,#51540,.F.);
#68123=ORIENTED_EDGE('',*,*,#51535,.F.);
#68124=ORIENTED_EDGE('',*,*,#51541,.T.);
#68125=ORIENTED_EDGE('',*,*,#51542,.T.);
#68126=ORIENTED_EDGE('',*,*,#51543,.F.);
#68127=ORIENTED_EDGE('',*,*,#51539,.F.);
#68128=ORIENTED_EDGE('',*,*,#51544,.T.);
#68129=ORIENTED_EDGE('',*,*,#51537,.T.);
#68130=ORIENTED_EDGE('',*,*,#51545,.F.);
#68131=ORIENTED_EDGE('',*,*,#51542,.F.);
#68132=ORIENTED_EDGE('',*,*,#51546,.T.);
#68133=ORIENTED_EDGE('',*,*,#51547,.T.);
#68134=ORIENTED_EDGE('',*,*,#51548,.F.);
#68135=ORIENTED_EDGE('',*,*,#51549,.F.);
#68136=ORIENTED_EDGE('',*,*,#51550,.T.);
#68137=ORIENTED_EDGE('',*,*,#51551,.T.);
#68138=ORIENTED_EDGE('',*,*,#51552,.F.);
#68139=ORIENTED_EDGE('',*,*,#51547,.F.);
#68140=ORIENTED_EDGE('',*,*,#51553,.T.);
#68141=ORIENTED_EDGE('',*,*,#51554,.T.);
#68142=ORIENTED_EDGE('',*,*,#51555,.F.);
#68143=ORIENTED_EDGE('',*,*,#51551,.F.);
#68144=ORIENTED_EDGE('',*,*,#51556,.T.);
#68145=ORIENTED_EDGE('',*,*,#51549,.T.);
#68146=ORIENTED_EDGE('',*,*,#51557,.F.);
#68147=ORIENTED_EDGE('',*,*,#51554,.F.);
#68148=ORIENTED_EDGE('',*,*,#51558,.T.);
#68149=ORIENTED_EDGE('',*,*,#51559,.T.);
#68150=ORIENTED_EDGE('',*,*,#51560,.F.);
#68151=ORIENTED_EDGE('',*,*,#51561,.F.);
#68152=ORIENTED_EDGE('',*,*,#51562,.T.);
#68153=ORIENTED_EDGE('',*,*,#51563,.T.);
#68154=ORIENTED_EDGE('',*,*,#51564,.F.);
#68155=ORIENTED_EDGE('',*,*,#51559,.F.);
#68156=ORIENTED_EDGE('',*,*,#51565,.T.);
#68157=ORIENTED_EDGE('',*,*,#51566,.T.);
#68158=ORIENTED_EDGE('',*,*,#51567,.F.);
#68159=ORIENTED_EDGE('',*,*,#51563,.F.);
#68160=ORIENTED_EDGE('',*,*,#51568,.T.);
#68161=ORIENTED_EDGE('',*,*,#51561,.T.);
#68162=ORIENTED_EDGE('',*,*,#51569,.F.);
#68163=ORIENTED_EDGE('',*,*,#51566,.F.);
#68164=ORIENTED_EDGE('',*,*,#51570,.T.);
#68165=ORIENTED_EDGE('',*,*,#51571,.T.);
#68166=ORIENTED_EDGE('',*,*,#51572,.F.);
#68167=ORIENTED_EDGE('',*,*,#51573,.F.);
#68168=ORIENTED_EDGE('',*,*,#51574,.T.);
#68169=ORIENTED_EDGE('',*,*,#51575,.T.);
#68170=ORIENTED_EDGE('',*,*,#51576,.F.);
#68171=ORIENTED_EDGE('',*,*,#51571,.F.);
#68172=ORIENTED_EDGE('',*,*,#51577,.T.);
#68173=ORIENTED_EDGE('',*,*,#51578,.T.);
#68174=ORIENTED_EDGE('',*,*,#51579,.F.);
#68175=ORIENTED_EDGE('',*,*,#51575,.F.);
#68176=ORIENTED_EDGE('',*,*,#51580,.T.);
#68177=ORIENTED_EDGE('',*,*,#51573,.T.);
#68178=ORIENTED_EDGE('',*,*,#51581,.F.);
#68179=ORIENTED_EDGE('',*,*,#51578,.F.);
#68180=ORIENTED_EDGE('',*,*,#51582,.T.);
#68181=ORIENTED_EDGE('',*,*,#51583,.T.);
#68182=ORIENTED_EDGE('',*,*,#51584,.F.);
#68183=ORIENTED_EDGE('',*,*,#51585,.F.);
#68184=ORIENTED_EDGE('',*,*,#51586,.T.);
#68185=ORIENTED_EDGE('',*,*,#51587,.T.);
#68186=ORIENTED_EDGE('',*,*,#51588,.F.);
#68187=ORIENTED_EDGE('',*,*,#51583,.F.);
#68188=ORIENTED_EDGE('',*,*,#51589,.T.);
#68189=ORIENTED_EDGE('',*,*,#51590,.T.);
#68190=ORIENTED_EDGE('',*,*,#51591,.F.);
#68191=ORIENTED_EDGE('',*,*,#51587,.F.);
#68192=ORIENTED_EDGE('',*,*,#51592,.T.);
#68193=ORIENTED_EDGE('',*,*,#51585,.T.);
#68194=ORIENTED_EDGE('',*,*,#51593,.F.);
#68195=ORIENTED_EDGE('',*,*,#51590,.F.);
#68196=ORIENTED_EDGE('',*,*,#51594,.T.);
#68197=ORIENTED_EDGE('',*,*,#51595,.T.);
#68198=ORIENTED_EDGE('',*,*,#51596,.F.);
#68199=ORIENTED_EDGE('',*,*,#51597,.F.);
#68200=ORIENTED_EDGE('',*,*,#51598,.T.);
#68201=ORIENTED_EDGE('',*,*,#51599,.T.);
#68202=ORIENTED_EDGE('',*,*,#51600,.F.);
#68203=ORIENTED_EDGE('',*,*,#51595,.F.);
#68204=ORIENTED_EDGE('',*,*,#51601,.T.);
#68205=ORIENTED_EDGE('',*,*,#51602,.T.);
#68206=ORIENTED_EDGE('',*,*,#51603,.F.);
#68207=ORIENTED_EDGE('',*,*,#51599,.F.);
#68208=ORIENTED_EDGE('',*,*,#51604,.T.);
#68209=ORIENTED_EDGE('',*,*,#51597,.T.);
#68210=ORIENTED_EDGE('',*,*,#51605,.F.);
#68211=ORIENTED_EDGE('',*,*,#51602,.F.);
#68212=ORIENTED_EDGE('',*,*,#51606,.T.);
#68213=ORIENTED_EDGE('',*,*,#51607,.T.);
#68214=ORIENTED_EDGE('',*,*,#51608,.F.);
#68215=ORIENTED_EDGE('',*,*,#51609,.F.);
#68216=ORIENTED_EDGE('',*,*,#51610,.T.);
#68217=ORIENTED_EDGE('',*,*,#51611,.T.);
#68218=ORIENTED_EDGE('',*,*,#51612,.F.);
#68219=ORIENTED_EDGE('',*,*,#51607,.F.);
#68220=ORIENTED_EDGE('',*,*,#51613,.T.);
#68221=ORIENTED_EDGE('',*,*,#51614,.T.);
#68222=ORIENTED_EDGE('',*,*,#51615,.F.);
#68223=ORIENTED_EDGE('',*,*,#51611,.F.);
#68224=ORIENTED_EDGE('',*,*,#51616,.T.);
#68225=ORIENTED_EDGE('',*,*,#51609,.T.);
#68226=ORIENTED_EDGE('',*,*,#51617,.F.);
#68227=ORIENTED_EDGE('',*,*,#51614,.F.);
#68228=ORIENTED_EDGE('',*,*,#51618,.T.);
#68229=ORIENTED_EDGE('',*,*,#51619,.T.);
#68230=ORIENTED_EDGE('',*,*,#51620,.F.);
#68231=ORIENTED_EDGE('',*,*,#51621,.F.);
#68232=ORIENTED_EDGE('',*,*,#51622,.T.);
#68233=ORIENTED_EDGE('',*,*,#51623,.T.);
#68234=ORIENTED_EDGE('',*,*,#51624,.F.);
#68235=ORIENTED_EDGE('',*,*,#51619,.F.);
#68236=ORIENTED_EDGE('',*,*,#51625,.T.);
#68237=ORIENTED_EDGE('',*,*,#51626,.T.);
#68238=ORIENTED_EDGE('',*,*,#51627,.F.);
#68239=ORIENTED_EDGE('',*,*,#51623,.F.);
#68240=ORIENTED_EDGE('',*,*,#51628,.T.);
#68241=ORIENTED_EDGE('',*,*,#51621,.T.);
#68242=ORIENTED_EDGE('',*,*,#51629,.F.);
#68243=ORIENTED_EDGE('',*,*,#51626,.F.);
#68244=ORIENTED_EDGE('',*,*,#51630,.T.);
#68245=ORIENTED_EDGE('',*,*,#51631,.T.);
#68246=ORIENTED_EDGE('',*,*,#51632,.F.);
#68247=ORIENTED_EDGE('',*,*,#51633,.F.);
#68248=ORIENTED_EDGE('',*,*,#51634,.T.);
#68249=ORIENTED_EDGE('',*,*,#51635,.T.);
#68250=ORIENTED_EDGE('',*,*,#51636,.F.);
#68251=ORIENTED_EDGE('',*,*,#51631,.F.);
#68252=ORIENTED_EDGE('',*,*,#51637,.T.);
#68253=ORIENTED_EDGE('',*,*,#51638,.T.);
#68254=ORIENTED_EDGE('',*,*,#51639,.F.);
#68255=ORIENTED_EDGE('',*,*,#51635,.F.);
#68256=ORIENTED_EDGE('',*,*,#51640,.T.);
#68257=ORIENTED_EDGE('',*,*,#51633,.T.);
#68258=ORIENTED_EDGE('',*,*,#51641,.F.);
#68259=ORIENTED_EDGE('',*,*,#51638,.F.);
#68260=ORIENTED_EDGE('',*,*,#51642,.T.);
#68261=ORIENTED_EDGE('',*,*,#51643,.T.);
#68262=ORIENTED_EDGE('',*,*,#51644,.F.);
#68263=ORIENTED_EDGE('',*,*,#51645,.F.);
#68264=ORIENTED_EDGE('',*,*,#51646,.T.);
#68265=ORIENTED_EDGE('',*,*,#51647,.T.);
#68266=ORIENTED_EDGE('',*,*,#51648,.F.);
#68267=ORIENTED_EDGE('',*,*,#51643,.F.);
#68268=ORIENTED_EDGE('',*,*,#51649,.T.);
#68269=ORIENTED_EDGE('',*,*,#51650,.T.);
#68270=ORIENTED_EDGE('',*,*,#51651,.F.);
#68271=ORIENTED_EDGE('',*,*,#51647,.F.);
#68272=ORIENTED_EDGE('',*,*,#51652,.T.);
#68273=ORIENTED_EDGE('',*,*,#51645,.T.);
#68274=ORIENTED_EDGE('',*,*,#51653,.F.);
#68275=ORIENTED_EDGE('',*,*,#51650,.F.);
#68276=ORIENTED_EDGE('',*,*,#51654,.T.);
#68277=ORIENTED_EDGE('',*,*,#51655,.T.);
#68278=ORIENTED_EDGE('',*,*,#51656,.F.);
#68279=ORIENTED_EDGE('',*,*,#51657,.F.);
#68280=ORIENTED_EDGE('',*,*,#51658,.T.);
#68281=ORIENTED_EDGE('',*,*,#51659,.T.);
#68282=ORIENTED_EDGE('',*,*,#51660,.F.);
#68283=ORIENTED_EDGE('',*,*,#51655,.F.);
#68284=ORIENTED_EDGE('',*,*,#51661,.T.);
#68285=ORIENTED_EDGE('',*,*,#51662,.T.);
#68286=ORIENTED_EDGE('',*,*,#51663,.F.);
#68287=ORIENTED_EDGE('',*,*,#51659,.F.);
#68288=ORIENTED_EDGE('',*,*,#51664,.T.);
#68289=ORIENTED_EDGE('',*,*,#51657,.T.);
#68290=ORIENTED_EDGE('',*,*,#51665,.F.);
#68291=ORIENTED_EDGE('',*,*,#51662,.F.);
#68292=ORIENTED_EDGE('',*,*,#51666,.T.);
#68293=ORIENTED_EDGE('',*,*,#51667,.T.);
#68294=ORIENTED_EDGE('',*,*,#51668,.F.);
#68295=ORIENTED_EDGE('',*,*,#51669,.F.);
#68296=ORIENTED_EDGE('',*,*,#51670,.T.);
#68297=ORIENTED_EDGE('',*,*,#51671,.T.);
#68298=ORIENTED_EDGE('',*,*,#51672,.F.);
#68299=ORIENTED_EDGE('',*,*,#51667,.F.);
#68300=ORIENTED_EDGE('',*,*,#51673,.T.);
#68301=ORIENTED_EDGE('',*,*,#51674,.T.);
#68302=ORIENTED_EDGE('',*,*,#51675,.F.);
#68303=ORIENTED_EDGE('',*,*,#51671,.F.);
#68304=ORIENTED_EDGE('',*,*,#51676,.T.);
#68305=ORIENTED_EDGE('',*,*,#51669,.T.);
#68306=ORIENTED_EDGE('',*,*,#51677,.F.);
#68307=ORIENTED_EDGE('',*,*,#51674,.F.);
#68308=ORIENTED_EDGE('',*,*,#51678,.T.);
#68309=ORIENTED_EDGE('',*,*,#51679,.T.);
#68310=ORIENTED_EDGE('',*,*,#51680,.F.);
#68311=ORIENTED_EDGE('',*,*,#51681,.F.);
#68312=ORIENTED_EDGE('',*,*,#51682,.T.);
#68313=ORIENTED_EDGE('',*,*,#51683,.T.);
#68314=ORIENTED_EDGE('',*,*,#51684,.F.);
#68315=ORIENTED_EDGE('',*,*,#51679,.F.);
#68316=ORIENTED_EDGE('',*,*,#51685,.T.);
#68317=ORIENTED_EDGE('',*,*,#51686,.T.);
#68318=ORIENTED_EDGE('',*,*,#51687,.F.);
#68319=ORIENTED_EDGE('',*,*,#51683,.F.);
#68320=ORIENTED_EDGE('',*,*,#51688,.T.);
#68321=ORIENTED_EDGE('',*,*,#51681,.T.);
#68322=ORIENTED_EDGE('',*,*,#51689,.F.);
#68323=ORIENTED_EDGE('',*,*,#51686,.F.);
#68324=ORIENTED_EDGE('',*,*,#51690,.T.);
#68325=ORIENTED_EDGE('',*,*,#51691,.T.);
#68326=ORIENTED_EDGE('',*,*,#51692,.F.);
#68327=ORIENTED_EDGE('',*,*,#51693,.F.);
#68328=ORIENTED_EDGE('',*,*,#51694,.T.);
#68329=ORIENTED_EDGE('',*,*,#51695,.T.);
#68330=ORIENTED_EDGE('',*,*,#51696,.F.);
#68331=ORIENTED_EDGE('',*,*,#51691,.F.);
#68332=ORIENTED_EDGE('',*,*,#51697,.T.);
#68333=ORIENTED_EDGE('',*,*,#51698,.T.);
#68334=ORIENTED_EDGE('',*,*,#51699,.F.);
#68335=ORIENTED_EDGE('',*,*,#51695,.F.);
#68336=ORIENTED_EDGE('',*,*,#51700,.T.);
#68337=ORIENTED_EDGE('',*,*,#51693,.T.);
#68338=ORIENTED_EDGE('',*,*,#51701,.F.);
#68339=ORIENTED_EDGE('',*,*,#51698,.F.);
#68340=ORIENTED_EDGE('',*,*,#51702,.T.);
#68341=ORIENTED_EDGE('',*,*,#51703,.T.);
#68342=ORIENTED_EDGE('',*,*,#51704,.F.);
#68343=ORIENTED_EDGE('',*,*,#51705,.F.);
#68344=ORIENTED_EDGE('',*,*,#51706,.T.);
#68345=ORIENTED_EDGE('',*,*,#51707,.T.);
#68346=ORIENTED_EDGE('',*,*,#51708,.F.);
#68347=ORIENTED_EDGE('',*,*,#51703,.F.);
#68348=ORIENTED_EDGE('',*,*,#51709,.T.);
#68349=ORIENTED_EDGE('',*,*,#51710,.T.);
#68350=ORIENTED_EDGE('',*,*,#51711,.F.);
#68351=ORIENTED_EDGE('',*,*,#51707,.F.);
#68352=ORIENTED_EDGE('',*,*,#51712,.T.);
#68353=ORIENTED_EDGE('',*,*,#51705,.T.);
#68354=ORIENTED_EDGE('',*,*,#51713,.F.);
#68355=ORIENTED_EDGE('',*,*,#51710,.F.);
#68356=ORIENTED_EDGE('',*,*,#51714,.T.);
#68357=ORIENTED_EDGE('',*,*,#51715,.T.);
#68358=ORIENTED_EDGE('',*,*,#51716,.F.);
#68359=ORIENTED_EDGE('',*,*,#51717,.F.);
#68360=ORIENTED_EDGE('',*,*,#51718,.T.);
#68361=ORIENTED_EDGE('',*,*,#51719,.T.);
#68362=ORIENTED_EDGE('',*,*,#51720,.F.);
#68363=ORIENTED_EDGE('',*,*,#51715,.F.);
#68364=ORIENTED_EDGE('',*,*,#51721,.T.);
#68365=ORIENTED_EDGE('',*,*,#51722,.T.);
#68366=ORIENTED_EDGE('',*,*,#51723,.F.);
#68367=ORIENTED_EDGE('',*,*,#51719,.F.);
#68368=ORIENTED_EDGE('',*,*,#51724,.T.);
#68369=ORIENTED_EDGE('',*,*,#51717,.T.);
#68370=ORIENTED_EDGE('',*,*,#51725,.F.);
#68371=ORIENTED_EDGE('',*,*,#51722,.F.);
#68372=ORIENTED_EDGE('',*,*,#51726,.T.);
#68373=ORIENTED_EDGE('',*,*,#51727,.T.);
#68374=ORIENTED_EDGE('',*,*,#51728,.F.);
#68375=ORIENTED_EDGE('',*,*,#51729,.F.);
#68376=ORIENTED_EDGE('',*,*,#51730,.T.);
#68377=ORIENTED_EDGE('',*,*,#51731,.T.);
#68378=ORIENTED_EDGE('',*,*,#51732,.F.);
#68379=ORIENTED_EDGE('',*,*,#51727,.F.);
#68380=ORIENTED_EDGE('',*,*,#51733,.T.);
#68381=ORIENTED_EDGE('',*,*,#51734,.T.);
#68382=ORIENTED_EDGE('',*,*,#51735,.F.);
#68383=ORIENTED_EDGE('',*,*,#51731,.F.);
#68384=ORIENTED_EDGE('',*,*,#51736,.T.);
#68385=ORIENTED_EDGE('',*,*,#51729,.T.);
#68386=ORIENTED_EDGE('',*,*,#51737,.F.);
#68387=ORIENTED_EDGE('',*,*,#51734,.F.);
#68388=ORIENTED_EDGE('',*,*,#51738,.T.);
#68389=ORIENTED_EDGE('',*,*,#51739,.T.);
#68390=ORIENTED_EDGE('',*,*,#51740,.F.);
#68391=ORIENTED_EDGE('',*,*,#51741,.F.);
#68392=ORIENTED_EDGE('',*,*,#51742,.T.);
#68393=ORIENTED_EDGE('',*,*,#51743,.T.);
#68394=ORIENTED_EDGE('',*,*,#51744,.F.);
#68395=ORIENTED_EDGE('',*,*,#51739,.F.);
#68396=ORIENTED_EDGE('',*,*,#51745,.T.);
#68397=ORIENTED_EDGE('',*,*,#51746,.T.);
#68398=ORIENTED_EDGE('',*,*,#51747,.F.);
#68399=ORIENTED_EDGE('',*,*,#51743,.F.);
#68400=ORIENTED_EDGE('',*,*,#51748,.T.);
#68401=ORIENTED_EDGE('',*,*,#51741,.T.);
#68402=ORIENTED_EDGE('',*,*,#51749,.F.);
#68403=ORIENTED_EDGE('',*,*,#51746,.F.);
#68404=ORIENTED_EDGE('',*,*,#51750,.T.);
#68405=ORIENTED_EDGE('',*,*,#51751,.T.);
#68406=ORIENTED_EDGE('',*,*,#51752,.F.);
#68407=ORIENTED_EDGE('',*,*,#51753,.F.);
#68408=ORIENTED_EDGE('',*,*,#51754,.T.);
#68409=ORIENTED_EDGE('',*,*,#51755,.T.);
#68410=ORIENTED_EDGE('',*,*,#51756,.F.);
#68411=ORIENTED_EDGE('',*,*,#51751,.F.);
#68412=ORIENTED_EDGE('',*,*,#51757,.T.);
#68413=ORIENTED_EDGE('',*,*,#51758,.T.);
#68414=ORIENTED_EDGE('',*,*,#51759,.F.);
#68415=ORIENTED_EDGE('',*,*,#51755,.F.);
#68416=ORIENTED_EDGE('',*,*,#51760,.T.);
#68417=ORIENTED_EDGE('',*,*,#51753,.T.);
#68418=ORIENTED_EDGE('',*,*,#51761,.F.);
#68419=ORIENTED_EDGE('',*,*,#51758,.F.);
#68420=ORIENTED_EDGE('',*,*,#51762,.T.);
#68421=ORIENTED_EDGE('',*,*,#51763,.T.);
#68422=ORIENTED_EDGE('',*,*,#51764,.F.);
#68423=ORIENTED_EDGE('',*,*,#51765,.F.);
#68424=ORIENTED_EDGE('',*,*,#51766,.T.);
#68425=ORIENTED_EDGE('',*,*,#51767,.T.);
#68426=ORIENTED_EDGE('',*,*,#51768,.F.);
#68427=ORIENTED_EDGE('',*,*,#51763,.F.);
#68428=ORIENTED_EDGE('',*,*,#51769,.T.);
#68429=ORIENTED_EDGE('',*,*,#51770,.T.);
#68430=ORIENTED_EDGE('',*,*,#51771,.F.);
#68431=ORIENTED_EDGE('',*,*,#51767,.F.);
#68432=ORIENTED_EDGE('',*,*,#51772,.T.);
#68433=ORIENTED_EDGE('',*,*,#51765,.T.);
#68434=ORIENTED_EDGE('',*,*,#51773,.F.);
#68435=ORIENTED_EDGE('',*,*,#51770,.F.);
#68436=ORIENTED_EDGE('',*,*,#51774,.T.);
#68437=ORIENTED_EDGE('',*,*,#51775,.T.);
#68438=ORIENTED_EDGE('',*,*,#51776,.F.);
#68439=ORIENTED_EDGE('',*,*,#51777,.F.);
#68440=ORIENTED_EDGE('',*,*,#51778,.T.);
#68441=ORIENTED_EDGE('',*,*,#51779,.T.);
#68442=ORIENTED_EDGE('',*,*,#51780,.F.);
#68443=ORIENTED_EDGE('',*,*,#51775,.F.);
#68444=ORIENTED_EDGE('',*,*,#51781,.T.);
#68445=ORIENTED_EDGE('',*,*,#51782,.T.);
#68446=ORIENTED_EDGE('',*,*,#51783,.F.);
#68447=ORIENTED_EDGE('',*,*,#51779,.F.);
#68448=ORIENTED_EDGE('',*,*,#51784,.T.);
#68449=ORIENTED_EDGE('',*,*,#51777,.T.);
#68450=ORIENTED_EDGE('',*,*,#51785,.F.);
#68451=ORIENTED_EDGE('',*,*,#51782,.F.);
#68452=ORIENTED_EDGE('',*,*,#51786,.T.);
#68453=ORIENTED_EDGE('',*,*,#51787,.T.);
#68454=ORIENTED_EDGE('',*,*,#51788,.F.);
#68455=ORIENTED_EDGE('',*,*,#51789,.F.);
#68456=ORIENTED_EDGE('',*,*,#51790,.T.);
#68457=ORIENTED_EDGE('',*,*,#51791,.T.);
#68458=ORIENTED_EDGE('',*,*,#51792,.F.);
#68459=ORIENTED_EDGE('',*,*,#51787,.F.);
#68460=ORIENTED_EDGE('',*,*,#51793,.T.);
#68461=ORIENTED_EDGE('',*,*,#51794,.T.);
#68462=ORIENTED_EDGE('',*,*,#51795,.F.);
#68463=ORIENTED_EDGE('',*,*,#51791,.F.);
#68464=ORIENTED_EDGE('',*,*,#51796,.T.);
#68465=ORIENTED_EDGE('',*,*,#51789,.T.);
#68466=ORIENTED_EDGE('',*,*,#51797,.F.);
#68467=ORIENTED_EDGE('',*,*,#51794,.F.);
#68468=ORIENTED_EDGE('',*,*,#51798,.T.);
#68469=ORIENTED_EDGE('',*,*,#51799,.T.);
#68470=ORIENTED_EDGE('',*,*,#51800,.F.);
#68471=ORIENTED_EDGE('',*,*,#51801,.F.);
#68472=ORIENTED_EDGE('',*,*,#51802,.T.);
#68473=ORIENTED_EDGE('',*,*,#51803,.T.);
#68474=ORIENTED_EDGE('',*,*,#51804,.F.);
#68475=ORIENTED_EDGE('',*,*,#51799,.F.);
#68476=ORIENTED_EDGE('',*,*,#51805,.T.);
#68477=ORIENTED_EDGE('',*,*,#51806,.T.);
#68478=ORIENTED_EDGE('',*,*,#51807,.F.);
#68479=ORIENTED_EDGE('',*,*,#51803,.F.);
#68480=ORIENTED_EDGE('',*,*,#51808,.T.);
#68481=ORIENTED_EDGE('',*,*,#51801,.T.);
#68482=ORIENTED_EDGE('',*,*,#51809,.F.);
#68483=ORIENTED_EDGE('',*,*,#51806,.F.);
#68484=ORIENTED_EDGE('',*,*,#51810,.T.);
#68485=ORIENTED_EDGE('',*,*,#51811,.T.);
#68486=ORIENTED_EDGE('',*,*,#51812,.F.);
#68487=ORIENTED_EDGE('',*,*,#51813,.F.);
#68488=ORIENTED_EDGE('',*,*,#51814,.T.);
#68489=ORIENTED_EDGE('',*,*,#51815,.T.);
#68490=ORIENTED_EDGE('',*,*,#51816,.F.);
#68491=ORIENTED_EDGE('',*,*,#51811,.F.);
#68492=ORIENTED_EDGE('',*,*,#51817,.T.);
#68493=ORIENTED_EDGE('',*,*,#51818,.T.);
#68494=ORIENTED_EDGE('',*,*,#51819,.F.);
#68495=ORIENTED_EDGE('',*,*,#51815,.F.);
#68496=ORIENTED_EDGE('',*,*,#51820,.T.);
#68497=ORIENTED_EDGE('',*,*,#51813,.T.);
#68498=ORIENTED_EDGE('',*,*,#51821,.F.);
#68499=ORIENTED_EDGE('',*,*,#51818,.F.);
#68500=ORIENTED_EDGE('',*,*,#51822,.T.);
#68501=ORIENTED_EDGE('',*,*,#51823,.T.);
#68502=ORIENTED_EDGE('',*,*,#51824,.F.);
#68503=ORIENTED_EDGE('',*,*,#51825,.F.);
#68504=ORIENTED_EDGE('',*,*,#51826,.T.);
#68505=ORIENTED_EDGE('',*,*,#51827,.T.);
#68506=ORIENTED_EDGE('',*,*,#51828,.F.);
#68507=ORIENTED_EDGE('',*,*,#51823,.F.);
#68508=ORIENTED_EDGE('',*,*,#51829,.T.);
#68509=ORIENTED_EDGE('',*,*,#51830,.T.);
#68510=ORIENTED_EDGE('',*,*,#51831,.F.);
#68511=ORIENTED_EDGE('',*,*,#51827,.F.);
#68512=ORIENTED_EDGE('',*,*,#51832,.T.);
#68513=ORIENTED_EDGE('',*,*,#51825,.T.);
#68514=ORIENTED_EDGE('',*,*,#51833,.F.);
#68515=ORIENTED_EDGE('',*,*,#51830,.F.);
#68516=ORIENTED_EDGE('',*,*,#51834,.T.);
#68517=ORIENTED_EDGE('',*,*,#51835,.T.);
#68518=ORIENTED_EDGE('',*,*,#51836,.F.);
#68519=ORIENTED_EDGE('',*,*,#51837,.F.);
#68520=ORIENTED_EDGE('',*,*,#51838,.T.);
#68521=ORIENTED_EDGE('',*,*,#51839,.T.);
#68522=ORIENTED_EDGE('',*,*,#51840,.F.);
#68523=ORIENTED_EDGE('',*,*,#51835,.F.);
#68524=ORIENTED_EDGE('',*,*,#51841,.T.);
#68525=ORIENTED_EDGE('',*,*,#51842,.T.);
#68526=ORIENTED_EDGE('',*,*,#51843,.F.);
#68527=ORIENTED_EDGE('',*,*,#51839,.F.);
#68528=ORIENTED_EDGE('',*,*,#51844,.T.);
#68529=ORIENTED_EDGE('',*,*,#51837,.T.);
#68530=ORIENTED_EDGE('',*,*,#51845,.F.);
#68531=ORIENTED_EDGE('',*,*,#51842,.F.);
#68532=ORIENTED_EDGE('',*,*,#51846,.T.);
#68533=ORIENTED_EDGE('',*,*,#51847,.T.);
#68534=ORIENTED_EDGE('',*,*,#51848,.F.);
#68535=ORIENTED_EDGE('',*,*,#51849,.F.);
#68536=ORIENTED_EDGE('',*,*,#51850,.T.);
#68537=ORIENTED_EDGE('',*,*,#51851,.T.);
#68538=ORIENTED_EDGE('',*,*,#51852,.F.);
#68539=ORIENTED_EDGE('',*,*,#51847,.F.);
#68540=ORIENTED_EDGE('',*,*,#51853,.T.);
#68541=ORIENTED_EDGE('',*,*,#51854,.T.);
#68542=ORIENTED_EDGE('',*,*,#51855,.F.);
#68543=ORIENTED_EDGE('',*,*,#51851,.F.);
#68544=ORIENTED_EDGE('',*,*,#51856,.T.);
#68545=ORIENTED_EDGE('',*,*,#51849,.T.);
#68546=ORIENTED_EDGE('',*,*,#51857,.F.);
#68547=ORIENTED_EDGE('',*,*,#51854,.F.);
#68548=ORIENTED_EDGE('',*,*,#51858,.T.);
#68549=ORIENTED_EDGE('',*,*,#51859,.T.);
#68550=ORIENTED_EDGE('',*,*,#51860,.F.);
#68551=ORIENTED_EDGE('',*,*,#51861,.F.);
#68552=ORIENTED_EDGE('',*,*,#51862,.T.);
#68553=ORIENTED_EDGE('',*,*,#51863,.T.);
#68554=ORIENTED_EDGE('',*,*,#51864,.F.);
#68555=ORIENTED_EDGE('',*,*,#51859,.F.);
#68556=ORIENTED_EDGE('',*,*,#51865,.T.);
#68557=ORIENTED_EDGE('',*,*,#51866,.T.);
#68558=ORIENTED_EDGE('',*,*,#51867,.F.);
#68559=ORIENTED_EDGE('',*,*,#51863,.F.);
#68560=ORIENTED_EDGE('',*,*,#51868,.T.);
#68561=ORIENTED_EDGE('',*,*,#51861,.T.);
#68562=ORIENTED_EDGE('',*,*,#51869,.F.);
#68563=ORIENTED_EDGE('',*,*,#51866,.F.);
#68564=ORIENTED_EDGE('',*,*,#51870,.T.);
#68565=ORIENTED_EDGE('',*,*,#51871,.T.);
#68566=ORIENTED_EDGE('',*,*,#51872,.F.);
#68567=ORIENTED_EDGE('',*,*,#51873,.F.);
#68568=ORIENTED_EDGE('',*,*,#51874,.T.);
#68569=ORIENTED_EDGE('',*,*,#51875,.T.);
#68570=ORIENTED_EDGE('',*,*,#51876,.F.);
#68571=ORIENTED_EDGE('',*,*,#51871,.F.);
#68572=ORIENTED_EDGE('',*,*,#51877,.T.);
#68573=ORIENTED_EDGE('',*,*,#51878,.T.);
#68574=ORIENTED_EDGE('',*,*,#51879,.F.);
#68575=ORIENTED_EDGE('',*,*,#51875,.F.);
#68576=ORIENTED_EDGE('',*,*,#51880,.T.);
#68577=ORIENTED_EDGE('',*,*,#51873,.T.);
#68578=ORIENTED_EDGE('',*,*,#51881,.F.);
#68579=ORIENTED_EDGE('',*,*,#51878,.F.);
#68580=ORIENTED_EDGE('',*,*,#51882,.T.);
#68581=ORIENTED_EDGE('',*,*,#51883,.T.);
#68582=ORIENTED_EDGE('',*,*,#51884,.F.);
#68583=ORIENTED_EDGE('',*,*,#51885,.F.);
#68584=ORIENTED_EDGE('',*,*,#51886,.T.);
#68585=ORIENTED_EDGE('',*,*,#51887,.T.);
#68586=ORIENTED_EDGE('',*,*,#51888,.F.);
#68587=ORIENTED_EDGE('',*,*,#51883,.F.);
#68588=ORIENTED_EDGE('',*,*,#51889,.T.);
#68589=ORIENTED_EDGE('',*,*,#51890,.T.);
#68590=ORIENTED_EDGE('',*,*,#51891,.F.);
#68591=ORIENTED_EDGE('',*,*,#51887,.F.);
#68592=ORIENTED_EDGE('',*,*,#51892,.T.);
#68593=ORIENTED_EDGE('',*,*,#51885,.T.);
#68594=ORIENTED_EDGE('',*,*,#51893,.F.);
#68595=ORIENTED_EDGE('',*,*,#51890,.F.);
#68596=ORIENTED_EDGE('',*,*,#51894,.T.);
#68597=ORIENTED_EDGE('',*,*,#51895,.T.);
#68598=ORIENTED_EDGE('',*,*,#51896,.F.);
#68599=ORIENTED_EDGE('',*,*,#51897,.F.);
#68600=ORIENTED_EDGE('',*,*,#51898,.T.);
#68601=ORIENTED_EDGE('',*,*,#51899,.T.);
#68602=ORIENTED_EDGE('',*,*,#51900,.F.);
#68603=ORIENTED_EDGE('',*,*,#51895,.F.);
#68604=ORIENTED_EDGE('',*,*,#51901,.T.);
#68605=ORIENTED_EDGE('',*,*,#51902,.T.);
#68606=ORIENTED_EDGE('',*,*,#51903,.F.);
#68607=ORIENTED_EDGE('',*,*,#51899,.F.);
#68608=ORIENTED_EDGE('',*,*,#51904,.T.);
#68609=ORIENTED_EDGE('',*,*,#51897,.T.);
#68610=ORIENTED_EDGE('',*,*,#51905,.F.);
#68611=ORIENTED_EDGE('',*,*,#51902,.F.);
#68612=ORIENTED_EDGE('',*,*,#51906,.T.);
#68613=ORIENTED_EDGE('',*,*,#51907,.T.);
#68614=ORIENTED_EDGE('',*,*,#51908,.F.);
#68615=ORIENTED_EDGE('',*,*,#51909,.F.);
#68616=ORIENTED_EDGE('',*,*,#51910,.T.);
#68617=ORIENTED_EDGE('',*,*,#51911,.T.);
#68618=ORIENTED_EDGE('',*,*,#51912,.F.);
#68619=ORIENTED_EDGE('',*,*,#51907,.F.);
#68620=ORIENTED_EDGE('',*,*,#51913,.T.);
#68621=ORIENTED_EDGE('',*,*,#51914,.T.);
#68622=ORIENTED_EDGE('',*,*,#51915,.F.);
#68623=ORIENTED_EDGE('',*,*,#51911,.F.);
#68624=ORIENTED_EDGE('',*,*,#51916,.T.);
#68625=ORIENTED_EDGE('',*,*,#51909,.T.);
#68626=ORIENTED_EDGE('',*,*,#51917,.F.);
#68627=ORIENTED_EDGE('',*,*,#51914,.F.);
#68628=ORIENTED_EDGE('',*,*,#51918,.T.);
#68629=ORIENTED_EDGE('',*,*,#51919,.T.);
#68630=ORIENTED_EDGE('',*,*,#51920,.F.);
#68631=ORIENTED_EDGE('',*,*,#51921,.F.);
#68632=ORIENTED_EDGE('',*,*,#51922,.T.);
#68633=ORIENTED_EDGE('',*,*,#51923,.T.);
#68634=ORIENTED_EDGE('',*,*,#51924,.F.);
#68635=ORIENTED_EDGE('',*,*,#51919,.F.);
#68636=ORIENTED_EDGE('',*,*,#51925,.T.);
#68637=ORIENTED_EDGE('',*,*,#51926,.T.);
#68638=ORIENTED_EDGE('',*,*,#51927,.F.);
#68639=ORIENTED_EDGE('',*,*,#51923,.F.);
#68640=ORIENTED_EDGE('',*,*,#51928,.T.);
#68641=ORIENTED_EDGE('',*,*,#51921,.T.);
#68642=ORIENTED_EDGE('',*,*,#51929,.F.);
#68643=ORIENTED_EDGE('',*,*,#51926,.F.);
#68644=ORIENTED_EDGE('',*,*,#51930,.T.);
#68645=ORIENTED_EDGE('',*,*,#51931,.T.);
#68646=ORIENTED_EDGE('',*,*,#51932,.F.);
#68647=ORIENTED_EDGE('',*,*,#51933,.F.);
#68648=ORIENTED_EDGE('',*,*,#51934,.T.);
#68649=ORIENTED_EDGE('',*,*,#51935,.T.);
#68650=ORIENTED_EDGE('',*,*,#51936,.F.);
#68651=ORIENTED_EDGE('',*,*,#51931,.F.);
#68652=ORIENTED_EDGE('',*,*,#51937,.T.);
#68653=ORIENTED_EDGE('',*,*,#51938,.T.);
#68654=ORIENTED_EDGE('',*,*,#51939,.F.);
#68655=ORIENTED_EDGE('',*,*,#51935,.F.);
#68656=ORIENTED_EDGE('',*,*,#51940,.T.);
#68657=ORIENTED_EDGE('',*,*,#51933,.T.);
#68658=ORIENTED_EDGE('',*,*,#51941,.F.);
#68659=ORIENTED_EDGE('',*,*,#51938,.F.);
#68660=ORIENTED_EDGE('',*,*,#51942,.T.);
#68661=ORIENTED_EDGE('',*,*,#51943,.T.);
#68662=ORIENTED_EDGE('',*,*,#51944,.F.);
#68663=ORIENTED_EDGE('',*,*,#51945,.F.);
#68664=ORIENTED_EDGE('',*,*,#51946,.T.);
#68665=ORIENTED_EDGE('',*,*,#51947,.T.);
#68666=ORIENTED_EDGE('',*,*,#51948,.F.);
#68667=ORIENTED_EDGE('',*,*,#51943,.F.);
#68668=ORIENTED_EDGE('',*,*,#51949,.T.);
#68669=ORIENTED_EDGE('',*,*,#51950,.T.);
#68670=ORIENTED_EDGE('',*,*,#51951,.F.);
#68671=ORIENTED_EDGE('',*,*,#51947,.F.);
#68672=ORIENTED_EDGE('',*,*,#51952,.T.);
#68673=ORIENTED_EDGE('',*,*,#51945,.T.);
#68674=ORIENTED_EDGE('',*,*,#51953,.F.);
#68675=ORIENTED_EDGE('',*,*,#51950,.F.);
#68676=ORIENTED_EDGE('',*,*,#51954,.T.);
#68677=ORIENTED_EDGE('',*,*,#51955,.T.);
#68678=ORIENTED_EDGE('',*,*,#51956,.F.);
#68679=ORIENTED_EDGE('',*,*,#51957,.F.);
#68680=ORIENTED_EDGE('',*,*,#51958,.T.);
#68681=ORIENTED_EDGE('',*,*,#51959,.T.);
#68682=ORIENTED_EDGE('',*,*,#51960,.F.);
#68683=ORIENTED_EDGE('',*,*,#51955,.F.);
#68684=ORIENTED_EDGE('',*,*,#51961,.T.);
#68685=ORIENTED_EDGE('',*,*,#51962,.T.);
#68686=ORIENTED_EDGE('',*,*,#51963,.F.);
#68687=ORIENTED_EDGE('',*,*,#51959,.F.);
#68688=ORIENTED_EDGE('',*,*,#51964,.T.);
#68689=ORIENTED_EDGE('',*,*,#51957,.T.);
#68690=ORIENTED_EDGE('',*,*,#51965,.F.);
#68691=ORIENTED_EDGE('',*,*,#51962,.F.);
#68692=ORIENTED_EDGE('',*,*,#51966,.T.);
#68693=ORIENTED_EDGE('',*,*,#43453,.T.);
#68694=ORIENTED_EDGE('',*,*,#43496,.F.);
#68695=ORIENTED_EDGE('',*,*,#43498,.T.);
#68696=ORIENTED_EDGE('',*,*,#46736,.T.);
#68697=ORIENTED_EDGE('',*,*,#46740,.T.);
#68698=ORIENTED_EDGE('',*,*,#46743,.T.);
#68699=ORIENTED_EDGE('',*,*,#46745,.T.);
#68700=ORIENTED_EDGE('',*,*,#46748,.T.);
#68701=ORIENTED_EDGE('',*,*,#46752,.T.);
#68702=ORIENTED_EDGE('',*,*,#46755,.T.);
#68703=ORIENTED_EDGE('',*,*,#46757,.T.);
#68704=ORIENTED_EDGE('',*,*,#46760,.T.);
#68705=ORIENTED_EDGE('',*,*,#46764,.T.);
#68706=ORIENTED_EDGE('',*,*,#46767,.T.);
#68707=ORIENTED_EDGE('',*,*,#46769,.T.);
#68708=ORIENTED_EDGE('',*,*,#46772,.T.);
#68709=ORIENTED_EDGE('',*,*,#46776,.T.);
#68710=ORIENTED_EDGE('',*,*,#46779,.T.);
#68711=ORIENTED_EDGE('',*,*,#46781,.T.);
#68712=ORIENTED_EDGE('',*,*,#46784,.T.);
#68713=ORIENTED_EDGE('',*,*,#46788,.T.);
#68714=ORIENTED_EDGE('',*,*,#46791,.T.);
#68715=ORIENTED_EDGE('',*,*,#46793,.T.);
#68716=ORIENTED_EDGE('',*,*,#46796,.T.);
#68717=ORIENTED_EDGE('',*,*,#46800,.T.);
#68718=ORIENTED_EDGE('',*,*,#46803,.T.);
#68719=ORIENTED_EDGE('',*,*,#46805,.T.);
#68720=ORIENTED_EDGE('',*,*,#46808,.T.);
#68721=ORIENTED_EDGE('',*,*,#46812,.T.);
#68722=ORIENTED_EDGE('',*,*,#46815,.T.);
#68723=ORIENTED_EDGE('',*,*,#46817,.T.);
#68724=ORIENTED_EDGE('',*,*,#46820,.T.);
#68725=ORIENTED_EDGE('',*,*,#46824,.T.);
#68726=ORIENTED_EDGE('',*,*,#46827,.T.);
#68727=ORIENTED_EDGE('',*,*,#46829,.T.);
#68728=ORIENTED_EDGE('',*,*,#46832,.T.);
#68729=ORIENTED_EDGE('',*,*,#46836,.T.);
#68730=ORIENTED_EDGE('',*,*,#46839,.T.);
#68731=ORIENTED_EDGE('',*,*,#46841,.T.);
#68732=ORIENTED_EDGE('',*,*,#46844,.T.);
#68733=ORIENTED_EDGE('',*,*,#46848,.T.);
#68734=ORIENTED_EDGE('',*,*,#46851,.T.);
#68735=ORIENTED_EDGE('',*,*,#46853,.T.);
#68736=ORIENTED_EDGE('',*,*,#46856,.T.);
#68737=ORIENTED_EDGE('',*,*,#46860,.T.);
#68738=ORIENTED_EDGE('',*,*,#46863,.T.);
#68739=ORIENTED_EDGE('',*,*,#46865,.T.);
#68740=ORIENTED_EDGE('',*,*,#46868,.T.);
#68741=ORIENTED_EDGE('',*,*,#46872,.T.);
#68742=ORIENTED_EDGE('',*,*,#46875,.T.);
#68743=ORIENTED_EDGE('',*,*,#46877,.T.);
#68744=ORIENTED_EDGE('',*,*,#46880,.T.);
#68745=ORIENTED_EDGE('',*,*,#46884,.T.);
#68746=ORIENTED_EDGE('',*,*,#46887,.T.);
#68747=ORIENTED_EDGE('',*,*,#46889,.T.);
#68748=ORIENTED_EDGE('',*,*,#46892,.T.);
#68749=ORIENTED_EDGE('',*,*,#46896,.T.);
#68750=ORIENTED_EDGE('',*,*,#46899,.T.);
#68751=ORIENTED_EDGE('',*,*,#46901,.T.);
#68752=ORIENTED_EDGE('',*,*,#46904,.T.);
#68753=ORIENTED_EDGE('',*,*,#46908,.T.);
#68754=ORIENTED_EDGE('',*,*,#46911,.T.);
#68755=ORIENTED_EDGE('',*,*,#46913,.T.);
#68756=ORIENTED_EDGE('',*,*,#46916,.T.);
#68757=ORIENTED_EDGE('',*,*,#46920,.T.);
#68758=ORIENTED_EDGE('',*,*,#46923,.T.);
#68759=ORIENTED_EDGE('',*,*,#46925,.T.);
#68760=ORIENTED_EDGE('',*,*,#46928,.T.);
#68761=ORIENTED_EDGE('',*,*,#46932,.T.);
#68762=ORIENTED_EDGE('',*,*,#46935,.T.);
#68763=ORIENTED_EDGE('',*,*,#46937,.T.);
#68764=ORIENTED_EDGE('',*,*,#46940,.T.);
#68765=ORIENTED_EDGE('',*,*,#46944,.T.);
#68766=ORIENTED_EDGE('',*,*,#46947,.T.);
#68767=ORIENTED_EDGE('',*,*,#46949,.T.);
#68768=ORIENTED_EDGE('',*,*,#46952,.T.);
#68769=ORIENTED_EDGE('',*,*,#46956,.T.);
#68770=ORIENTED_EDGE('',*,*,#46959,.T.);
#68771=ORIENTED_EDGE('',*,*,#46961,.T.);
#68772=ORIENTED_EDGE('',*,*,#46964,.T.);
#68773=ORIENTED_EDGE('',*,*,#46968,.T.);
#68774=ORIENTED_EDGE('',*,*,#46971,.T.);
#68775=ORIENTED_EDGE('',*,*,#46973,.T.);
#68776=ORIENTED_EDGE('',*,*,#46976,.T.);
#68777=ORIENTED_EDGE('',*,*,#46980,.T.);
#68778=ORIENTED_EDGE('',*,*,#46983,.T.);
#68779=ORIENTED_EDGE('',*,*,#46985,.T.);
#68780=ORIENTED_EDGE('',*,*,#46988,.T.);
#68781=ORIENTED_EDGE('',*,*,#46992,.T.);
#68782=ORIENTED_EDGE('',*,*,#46995,.T.);
#68783=ORIENTED_EDGE('',*,*,#46997,.T.);
#68784=ORIENTED_EDGE('',*,*,#47000,.T.);
#68785=ORIENTED_EDGE('',*,*,#47004,.T.);
#68786=ORIENTED_EDGE('',*,*,#47007,.T.);
#68787=ORIENTED_EDGE('',*,*,#47009,.T.);
#68788=ORIENTED_EDGE('',*,*,#47012,.T.);
#68789=ORIENTED_EDGE('',*,*,#47016,.T.);
#68790=ORIENTED_EDGE('',*,*,#47019,.T.);
#68791=ORIENTED_EDGE('',*,*,#47021,.T.);
#68792=ORIENTED_EDGE('',*,*,#47024,.T.);
#68793=ORIENTED_EDGE('',*,*,#47028,.T.);
#68794=ORIENTED_EDGE('',*,*,#47031,.T.);
#68795=ORIENTED_EDGE('',*,*,#47033,.T.);
#68796=ORIENTED_EDGE('',*,*,#47036,.T.);
#68797=ORIENTED_EDGE('',*,*,#47040,.T.);
#68798=ORIENTED_EDGE('',*,*,#47043,.T.);
#68799=ORIENTED_EDGE('',*,*,#47045,.T.);
#68800=ORIENTED_EDGE('',*,*,#47048,.T.);
#68801=ORIENTED_EDGE('',*,*,#47052,.T.);
#68802=ORIENTED_EDGE('',*,*,#47055,.T.);
#68803=ORIENTED_EDGE('',*,*,#47057,.T.);
#68804=ORIENTED_EDGE('',*,*,#47060,.T.);
#68805=ORIENTED_EDGE('',*,*,#47064,.T.);
#68806=ORIENTED_EDGE('',*,*,#47067,.T.);
#68807=ORIENTED_EDGE('',*,*,#47069,.T.);
#68808=ORIENTED_EDGE('',*,*,#47072,.T.);
#68809=ORIENTED_EDGE('',*,*,#47076,.T.);
#68810=ORIENTED_EDGE('',*,*,#47079,.T.);
#68811=ORIENTED_EDGE('',*,*,#47081,.T.);
#68812=ORIENTED_EDGE('',*,*,#47084,.T.);
#68813=ORIENTED_EDGE('',*,*,#47088,.T.);
#68814=ORIENTED_EDGE('',*,*,#47091,.T.);
#68815=ORIENTED_EDGE('',*,*,#47093,.T.);
#68816=ORIENTED_EDGE('',*,*,#47096,.T.);
#68817=ORIENTED_EDGE('',*,*,#47100,.T.);
#68818=ORIENTED_EDGE('',*,*,#47103,.T.);
#68819=ORIENTED_EDGE('',*,*,#47105,.T.);
#68820=ORIENTED_EDGE('',*,*,#47108,.T.);
#68821=ORIENTED_EDGE('',*,*,#47112,.T.);
#68822=ORIENTED_EDGE('',*,*,#47115,.T.);
#68823=ORIENTED_EDGE('',*,*,#47117,.T.);
#68824=ORIENTED_EDGE('',*,*,#47120,.T.);
#68825=ORIENTED_EDGE('',*,*,#47124,.T.);
#68826=ORIENTED_EDGE('',*,*,#47127,.T.);
#68827=ORIENTED_EDGE('',*,*,#47129,.T.);
#68828=ORIENTED_EDGE('',*,*,#47132,.T.);
#68829=ORIENTED_EDGE('',*,*,#47136,.T.);
#68830=ORIENTED_EDGE('',*,*,#47139,.T.);
#68831=ORIENTED_EDGE('',*,*,#47141,.T.);
#68832=ORIENTED_EDGE('',*,*,#47144,.T.);
#68833=ORIENTED_EDGE('',*,*,#47148,.T.);
#68834=ORIENTED_EDGE('',*,*,#47151,.T.);
#68835=ORIENTED_EDGE('',*,*,#47153,.T.);
#68836=ORIENTED_EDGE('',*,*,#47156,.T.);
#68837=ORIENTED_EDGE('',*,*,#47160,.T.);
#68838=ORIENTED_EDGE('',*,*,#47163,.T.);
#68839=ORIENTED_EDGE('',*,*,#47165,.T.);
#68840=ORIENTED_EDGE('',*,*,#47168,.T.);
#68841=ORIENTED_EDGE('',*,*,#47172,.T.);
#68842=ORIENTED_EDGE('',*,*,#47175,.T.);
#68843=ORIENTED_EDGE('',*,*,#47177,.T.);
#68844=ORIENTED_EDGE('',*,*,#47180,.T.);
#68845=ORIENTED_EDGE('',*,*,#47184,.T.);
#68846=ORIENTED_EDGE('',*,*,#47187,.T.);
#68847=ORIENTED_EDGE('',*,*,#47189,.T.);
#68848=ORIENTED_EDGE('',*,*,#47192,.T.);
#68849=ORIENTED_EDGE('',*,*,#47196,.T.);
#68850=ORIENTED_EDGE('',*,*,#47199,.T.);
#68851=ORIENTED_EDGE('',*,*,#47201,.T.);
#68852=ORIENTED_EDGE('',*,*,#47204,.T.);
#68853=ORIENTED_EDGE('',*,*,#47208,.T.);
#68854=ORIENTED_EDGE('',*,*,#47211,.T.);
#68855=ORIENTED_EDGE('',*,*,#47213,.T.);
#68856=ORIENTED_EDGE('',*,*,#47216,.T.);
#68857=ORIENTED_EDGE('',*,*,#47220,.T.);
#68858=ORIENTED_EDGE('',*,*,#47223,.T.);
#68859=ORIENTED_EDGE('',*,*,#47225,.T.);
#68860=ORIENTED_EDGE('',*,*,#47228,.T.);
#68861=ORIENTED_EDGE('',*,*,#47232,.T.);
#68862=ORIENTED_EDGE('',*,*,#47235,.T.);
#68863=ORIENTED_EDGE('',*,*,#47237,.T.);
#68864=ORIENTED_EDGE('',*,*,#47240,.T.);
#68865=ORIENTED_EDGE('',*,*,#47244,.T.);
#68866=ORIENTED_EDGE('',*,*,#47247,.T.);
#68867=ORIENTED_EDGE('',*,*,#47249,.T.);
#68868=ORIENTED_EDGE('',*,*,#47252,.T.);
#68869=ORIENTED_EDGE('',*,*,#47256,.T.);
#68870=ORIENTED_EDGE('',*,*,#47259,.T.);
#68871=ORIENTED_EDGE('',*,*,#47261,.T.);
#68872=ORIENTED_EDGE('',*,*,#47264,.T.);
#68873=ORIENTED_EDGE('',*,*,#47268,.T.);
#68874=ORIENTED_EDGE('',*,*,#47271,.T.);
#68875=ORIENTED_EDGE('',*,*,#47273,.T.);
#68876=ORIENTED_EDGE('',*,*,#47276,.T.);
#68877=ORIENTED_EDGE('',*,*,#47280,.T.);
#68878=ORIENTED_EDGE('',*,*,#47283,.T.);
#68879=ORIENTED_EDGE('',*,*,#47285,.T.);
#68880=ORIENTED_EDGE('',*,*,#47288,.T.);
#68881=ORIENTED_EDGE('',*,*,#47292,.T.);
#68882=ORIENTED_EDGE('',*,*,#47295,.T.);
#68883=ORIENTED_EDGE('',*,*,#47297,.T.);
#68884=ORIENTED_EDGE('',*,*,#47300,.T.);
#68885=ORIENTED_EDGE('',*,*,#47304,.T.);
#68886=ORIENTED_EDGE('',*,*,#47307,.T.);
#68887=ORIENTED_EDGE('',*,*,#47309,.T.);
#68888=ORIENTED_EDGE('',*,*,#47312,.T.);
#68889=ORIENTED_EDGE('',*,*,#47316,.T.);
#68890=ORIENTED_EDGE('',*,*,#47319,.T.);
#68891=ORIENTED_EDGE('',*,*,#47321,.T.);
#68892=ORIENTED_EDGE('',*,*,#47324,.T.);
#68893=ORIENTED_EDGE('',*,*,#47328,.T.);
#68894=ORIENTED_EDGE('',*,*,#47331,.T.);
#68895=ORIENTED_EDGE('',*,*,#47333,.T.);
#68896=ORIENTED_EDGE('',*,*,#47336,.T.);
#68897=ORIENTED_EDGE('',*,*,#47340,.T.);
#68898=ORIENTED_EDGE('',*,*,#47343,.T.);
#68899=ORIENTED_EDGE('',*,*,#47345,.T.);
#68900=ORIENTED_EDGE('',*,*,#47348,.T.);
#68901=ORIENTED_EDGE('',*,*,#47352,.T.);
#68902=ORIENTED_EDGE('',*,*,#47355,.T.);
#68903=ORIENTED_EDGE('',*,*,#47357,.T.);
#68904=ORIENTED_EDGE('',*,*,#47360,.T.);
#68905=ORIENTED_EDGE('',*,*,#47364,.T.);
#68906=ORIENTED_EDGE('',*,*,#47367,.T.);
#68907=ORIENTED_EDGE('',*,*,#47369,.T.);
#68908=ORIENTED_EDGE('',*,*,#47372,.T.);
#68909=ORIENTED_EDGE('',*,*,#47376,.T.);
#68910=ORIENTED_EDGE('',*,*,#47379,.T.);
#68911=ORIENTED_EDGE('',*,*,#47381,.T.);
#68912=ORIENTED_EDGE('',*,*,#47384,.T.);
#68913=ORIENTED_EDGE('',*,*,#47388,.T.);
#68914=ORIENTED_EDGE('',*,*,#47391,.T.);
#68915=ORIENTED_EDGE('',*,*,#47393,.T.);
#68916=ORIENTED_EDGE('',*,*,#47396,.T.);
#68917=ORIENTED_EDGE('',*,*,#47400,.T.);
#68918=ORIENTED_EDGE('',*,*,#47403,.T.);
#68919=ORIENTED_EDGE('',*,*,#47405,.T.);
#68920=ORIENTED_EDGE('',*,*,#47408,.T.);
#68921=ORIENTED_EDGE('',*,*,#47412,.T.);
#68922=ORIENTED_EDGE('',*,*,#47415,.T.);
#68923=ORIENTED_EDGE('',*,*,#47417,.T.);
#68924=ORIENTED_EDGE('',*,*,#47420,.T.);
#68925=ORIENTED_EDGE('',*,*,#47424,.T.);
#68926=ORIENTED_EDGE('',*,*,#47427,.T.);
#68927=ORIENTED_EDGE('',*,*,#47429,.T.);
#68928=ORIENTED_EDGE('',*,*,#47432,.T.);
#68929=ORIENTED_EDGE('',*,*,#47436,.T.);
#68930=ORIENTED_EDGE('',*,*,#47439,.T.);
#68931=ORIENTED_EDGE('',*,*,#47441,.T.);
#68932=ORIENTED_EDGE('',*,*,#47444,.T.);
#68933=ORIENTED_EDGE('',*,*,#47448,.T.);
#68934=ORIENTED_EDGE('',*,*,#47451,.T.);
#68935=ORIENTED_EDGE('',*,*,#47453,.T.);
#68936=ORIENTED_EDGE('',*,*,#47456,.T.);
#68937=ORIENTED_EDGE('',*,*,#47460,.T.);
#68938=ORIENTED_EDGE('',*,*,#47463,.T.);
#68939=ORIENTED_EDGE('',*,*,#47465,.T.);
#68940=ORIENTED_EDGE('',*,*,#47468,.T.);
#68941=ORIENTED_EDGE('',*,*,#47472,.T.);
#68942=ORIENTED_EDGE('',*,*,#47475,.T.);
#68943=ORIENTED_EDGE('',*,*,#47477,.T.);
#68944=ORIENTED_EDGE('',*,*,#47480,.T.);
#68945=ORIENTED_EDGE('',*,*,#47484,.T.);
#68946=ORIENTED_EDGE('',*,*,#47487,.T.);
#68947=ORIENTED_EDGE('',*,*,#47489,.T.);
#68948=ORIENTED_EDGE('',*,*,#47492,.T.);
#68949=ORIENTED_EDGE('',*,*,#47496,.T.);
#68950=ORIENTED_EDGE('',*,*,#47499,.T.);
#68951=ORIENTED_EDGE('',*,*,#47501,.T.);
#68952=ORIENTED_EDGE('',*,*,#47504,.T.);
#68953=ORIENTED_EDGE('',*,*,#47508,.T.);
#68954=ORIENTED_EDGE('',*,*,#47511,.T.);
#68955=ORIENTED_EDGE('',*,*,#47513,.T.);
#68956=ORIENTED_EDGE('',*,*,#47516,.T.);
#68957=ORIENTED_EDGE('',*,*,#47520,.T.);
#68958=ORIENTED_EDGE('',*,*,#47523,.T.);
#68959=ORIENTED_EDGE('',*,*,#47525,.T.);
#68960=ORIENTED_EDGE('',*,*,#47528,.T.);
#68961=ORIENTED_EDGE('',*,*,#47532,.T.);
#68962=ORIENTED_EDGE('',*,*,#47535,.T.);
#68963=ORIENTED_EDGE('',*,*,#47537,.T.);
#68964=ORIENTED_EDGE('',*,*,#47540,.T.);
#68965=ORIENTED_EDGE('',*,*,#47544,.T.);
#68966=ORIENTED_EDGE('',*,*,#47547,.T.);
#68967=ORIENTED_EDGE('',*,*,#47549,.T.);
#68968=ORIENTED_EDGE('',*,*,#47552,.T.);
#68969=ORIENTED_EDGE('',*,*,#47556,.T.);
#68970=ORIENTED_EDGE('',*,*,#47559,.T.);
#68971=ORIENTED_EDGE('',*,*,#47561,.T.);
#68972=ORIENTED_EDGE('',*,*,#47564,.T.);
#68973=ORIENTED_EDGE('',*,*,#47568,.T.);
#68974=ORIENTED_EDGE('',*,*,#47571,.T.);
#68975=ORIENTED_EDGE('',*,*,#47573,.T.);
#68976=ORIENTED_EDGE('',*,*,#47576,.T.);
#68977=ORIENTED_EDGE('',*,*,#47580,.T.);
#68978=ORIENTED_EDGE('',*,*,#47583,.T.);
#68979=ORIENTED_EDGE('',*,*,#47585,.T.);
#68980=ORIENTED_EDGE('',*,*,#47588,.T.);
#68981=ORIENTED_EDGE('',*,*,#47592,.T.);
#68982=ORIENTED_EDGE('',*,*,#47595,.T.);
#68983=ORIENTED_EDGE('',*,*,#47597,.T.);
#68984=ORIENTED_EDGE('',*,*,#47600,.T.);
#68985=ORIENTED_EDGE('',*,*,#47604,.T.);
#68986=ORIENTED_EDGE('',*,*,#47607,.T.);
#68987=ORIENTED_EDGE('',*,*,#47609,.T.);
#68988=ORIENTED_EDGE('',*,*,#47612,.T.);
#68989=ORIENTED_EDGE('',*,*,#47616,.T.);
#68990=ORIENTED_EDGE('',*,*,#47619,.T.);
#68991=ORIENTED_EDGE('',*,*,#47621,.T.);
#68992=ORIENTED_EDGE('',*,*,#47624,.T.);
#68993=ORIENTED_EDGE('',*,*,#47628,.T.);
#68994=ORIENTED_EDGE('',*,*,#47631,.T.);
#68995=ORIENTED_EDGE('',*,*,#47633,.T.);
#68996=ORIENTED_EDGE('',*,*,#47636,.T.);
#68997=ORIENTED_EDGE('',*,*,#47640,.T.);
#68998=ORIENTED_EDGE('',*,*,#47643,.T.);
#68999=ORIENTED_EDGE('',*,*,#47645,.T.);
#69000=ORIENTED_EDGE('',*,*,#47648,.T.);
#69001=ORIENTED_EDGE('',*,*,#47652,.T.);
#69002=ORIENTED_EDGE('',*,*,#47655,.T.);
#69003=ORIENTED_EDGE('',*,*,#47657,.T.);
#69004=ORIENTED_EDGE('',*,*,#47660,.T.);
#69005=ORIENTED_EDGE('',*,*,#47664,.T.);
#69006=ORIENTED_EDGE('',*,*,#47667,.T.);
#69007=ORIENTED_EDGE('',*,*,#47669,.T.);
#69008=ORIENTED_EDGE('',*,*,#47672,.T.);
#69009=ORIENTED_EDGE('',*,*,#47676,.T.);
#69010=ORIENTED_EDGE('',*,*,#47679,.T.);
#69011=ORIENTED_EDGE('',*,*,#47681,.T.);
#69012=ORIENTED_EDGE('',*,*,#47684,.T.);
#69013=ORIENTED_EDGE('',*,*,#47688,.T.);
#69014=ORIENTED_EDGE('',*,*,#47691,.T.);
#69015=ORIENTED_EDGE('',*,*,#47693,.T.);
#69016=ORIENTED_EDGE('',*,*,#47696,.T.);
#69017=ORIENTED_EDGE('',*,*,#47700,.T.);
#69018=ORIENTED_EDGE('',*,*,#47703,.T.);
#69019=ORIENTED_EDGE('',*,*,#47705,.T.);
#69020=ORIENTED_EDGE('',*,*,#47708,.T.);
#69021=ORIENTED_EDGE('',*,*,#47712,.T.);
#69022=ORIENTED_EDGE('',*,*,#47715,.T.);
#69023=ORIENTED_EDGE('',*,*,#47717,.T.);
#69024=ORIENTED_EDGE('',*,*,#47720,.T.);
#69025=ORIENTED_EDGE('',*,*,#47724,.T.);
#69026=ORIENTED_EDGE('',*,*,#47727,.T.);
#69027=ORIENTED_EDGE('',*,*,#47729,.T.);
#69028=ORIENTED_EDGE('',*,*,#47732,.T.);
#69029=ORIENTED_EDGE('',*,*,#47736,.T.);
#69030=ORIENTED_EDGE('',*,*,#47739,.T.);
#69031=ORIENTED_EDGE('',*,*,#47741,.T.);
#69032=ORIENTED_EDGE('',*,*,#47744,.T.);
#69033=ORIENTED_EDGE('',*,*,#47748,.T.);
#69034=ORIENTED_EDGE('',*,*,#47751,.T.);
#69035=ORIENTED_EDGE('',*,*,#47753,.T.);
#69036=ORIENTED_EDGE('',*,*,#47756,.T.);
#69037=ORIENTED_EDGE('',*,*,#47760,.T.);
#69038=ORIENTED_EDGE('',*,*,#47763,.T.);
#69039=ORIENTED_EDGE('',*,*,#47765,.T.);
#69040=ORIENTED_EDGE('',*,*,#47768,.T.);
#69041=ORIENTED_EDGE('',*,*,#47772,.T.);
#69042=ORIENTED_EDGE('',*,*,#47775,.T.);
#69043=ORIENTED_EDGE('',*,*,#47777,.T.);
#69044=ORIENTED_EDGE('',*,*,#47780,.T.);
#69045=ORIENTED_EDGE('',*,*,#47784,.T.);
#69046=ORIENTED_EDGE('',*,*,#47787,.T.);
#69047=ORIENTED_EDGE('',*,*,#47789,.T.);
#69048=ORIENTED_EDGE('',*,*,#47792,.T.);
#69049=ORIENTED_EDGE('',*,*,#47796,.T.);
#69050=ORIENTED_EDGE('',*,*,#47799,.T.);
#69051=ORIENTED_EDGE('',*,*,#47801,.T.);
#69052=ORIENTED_EDGE('',*,*,#47804,.T.);
#69053=ORIENTED_EDGE('',*,*,#47808,.T.);
#69054=ORIENTED_EDGE('',*,*,#47811,.T.);
#69055=ORIENTED_EDGE('',*,*,#47813,.T.);
#69056=ORIENTED_EDGE('',*,*,#47816,.T.);
#69057=ORIENTED_EDGE('',*,*,#47820,.T.);
#69058=ORIENTED_EDGE('',*,*,#47823,.T.);
#69059=ORIENTED_EDGE('',*,*,#47825,.T.);
#69060=ORIENTED_EDGE('',*,*,#47828,.T.);
#69061=ORIENTED_EDGE('',*,*,#47832,.T.);
#69062=ORIENTED_EDGE('',*,*,#47835,.T.);
#69063=ORIENTED_EDGE('',*,*,#47837,.T.);
#69064=ORIENTED_EDGE('',*,*,#47840,.T.);
#69065=ORIENTED_EDGE('',*,*,#47844,.T.);
#69066=ORIENTED_EDGE('',*,*,#47847,.T.);
#69067=ORIENTED_EDGE('',*,*,#47849,.T.);
#69068=ORIENTED_EDGE('',*,*,#47852,.T.);
#69069=ORIENTED_EDGE('',*,*,#47856,.T.);
#69070=ORIENTED_EDGE('',*,*,#47859,.T.);
#69071=ORIENTED_EDGE('',*,*,#47861,.T.);
#69072=ORIENTED_EDGE('',*,*,#47864,.T.);
#69073=ORIENTED_EDGE('',*,*,#47868,.T.);
#69074=ORIENTED_EDGE('',*,*,#47871,.T.);
#69075=ORIENTED_EDGE('',*,*,#47873,.T.);
#69076=ORIENTED_EDGE('',*,*,#47876,.T.);
#69077=ORIENTED_EDGE('',*,*,#47880,.T.);
#69078=ORIENTED_EDGE('',*,*,#47883,.T.);
#69079=ORIENTED_EDGE('',*,*,#47885,.T.);
#69080=ORIENTED_EDGE('',*,*,#47888,.T.);
#69081=ORIENTED_EDGE('',*,*,#47892,.T.);
#69082=ORIENTED_EDGE('',*,*,#47895,.T.);
#69083=ORIENTED_EDGE('',*,*,#47897,.T.);
#69084=ORIENTED_EDGE('',*,*,#47900,.T.);
#69085=ORIENTED_EDGE('',*,*,#47904,.T.);
#69086=ORIENTED_EDGE('',*,*,#47907,.T.);
#69087=ORIENTED_EDGE('',*,*,#47909,.T.);
#69088=ORIENTED_EDGE('',*,*,#47912,.T.);
#69089=ORIENTED_EDGE('',*,*,#47916,.T.);
#69090=ORIENTED_EDGE('',*,*,#47919,.T.);
#69091=ORIENTED_EDGE('',*,*,#47921,.T.);
#69092=ORIENTED_EDGE('',*,*,#47924,.T.);
#69093=ORIENTED_EDGE('',*,*,#47928,.T.);
#69094=ORIENTED_EDGE('',*,*,#47931,.T.);
#69095=ORIENTED_EDGE('',*,*,#47933,.T.);
#69096=ORIENTED_EDGE('',*,*,#47936,.T.);
#69097=ORIENTED_EDGE('',*,*,#47940,.T.);
#69098=ORIENTED_EDGE('',*,*,#47943,.T.);
#69099=ORIENTED_EDGE('',*,*,#47945,.T.);
#69100=ORIENTED_EDGE('',*,*,#47948,.T.);
#69101=ORIENTED_EDGE('',*,*,#47952,.T.);
#69102=ORIENTED_EDGE('',*,*,#47955,.T.);
#69103=ORIENTED_EDGE('',*,*,#47957,.T.);
#69104=ORIENTED_EDGE('',*,*,#47960,.T.);
#69105=ORIENTED_EDGE('',*,*,#47964,.T.);
#69106=ORIENTED_EDGE('',*,*,#47967,.T.);
#69107=ORIENTED_EDGE('',*,*,#47969,.T.);
#69108=ORIENTED_EDGE('',*,*,#47972,.T.);
#69109=ORIENTED_EDGE('',*,*,#47976,.T.);
#69110=ORIENTED_EDGE('',*,*,#47979,.T.);
#69111=ORIENTED_EDGE('',*,*,#47981,.T.);
#69112=ORIENTED_EDGE('',*,*,#47984,.T.);
#69113=ORIENTED_EDGE('',*,*,#47988,.T.);
#69114=ORIENTED_EDGE('',*,*,#47991,.T.);
#69115=ORIENTED_EDGE('',*,*,#47993,.T.);
#69116=ORIENTED_EDGE('',*,*,#47996,.T.);
#69117=ORIENTED_EDGE('',*,*,#48000,.T.);
#69118=ORIENTED_EDGE('',*,*,#48003,.T.);
#69119=ORIENTED_EDGE('',*,*,#48005,.T.);
#69120=ORIENTED_EDGE('',*,*,#48008,.T.);
#69121=ORIENTED_EDGE('',*,*,#48012,.T.);
#69122=ORIENTED_EDGE('',*,*,#48015,.T.);
#69123=ORIENTED_EDGE('',*,*,#48017,.T.);
#69124=ORIENTED_EDGE('',*,*,#48020,.T.);
#69125=ORIENTED_EDGE('',*,*,#48024,.T.);
#69126=ORIENTED_EDGE('',*,*,#48027,.T.);
#69127=ORIENTED_EDGE('',*,*,#48029,.T.);
#69128=ORIENTED_EDGE('',*,*,#48032,.T.);
#69129=ORIENTED_EDGE('',*,*,#48036,.T.);
#69130=ORIENTED_EDGE('',*,*,#48039,.T.);
#69131=ORIENTED_EDGE('',*,*,#48041,.T.);
#69132=ORIENTED_EDGE('',*,*,#48044,.T.);
#69133=ORIENTED_EDGE('',*,*,#48048,.T.);
#69134=ORIENTED_EDGE('',*,*,#48051,.T.);
#69135=ORIENTED_EDGE('',*,*,#48053,.T.);
#69136=ORIENTED_EDGE('',*,*,#48056,.T.);
#69137=ORIENTED_EDGE('',*,*,#48060,.T.);
#69138=ORIENTED_EDGE('',*,*,#48063,.T.);
#69139=ORIENTED_EDGE('',*,*,#48065,.T.);
#69140=ORIENTED_EDGE('',*,*,#48068,.T.);
#69141=ORIENTED_EDGE('',*,*,#48072,.T.);
#69142=ORIENTED_EDGE('',*,*,#48075,.T.);
#69143=ORIENTED_EDGE('',*,*,#48077,.T.);
#69144=ORIENTED_EDGE('',*,*,#48080,.T.);
#69145=ORIENTED_EDGE('',*,*,#48084,.T.);
#69146=ORIENTED_EDGE('',*,*,#48087,.T.);
#69147=ORIENTED_EDGE('',*,*,#48089,.T.);
#69148=ORIENTED_EDGE('',*,*,#48092,.T.);
#69149=ORIENTED_EDGE('',*,*,#48096,.T.);
#69150=ORIENTED_EDGE('',*,*,#48099,.T.);
#69151=ORIENTED_EDGE('',*,*,#48101,.T.);
#69152=ORIENTED_EDGE('',*,*,#48104,.T.);
#69153=ORIENTED_EDGE('',*,*,#48108,.T.);
#69154=ORIENTED_EDGE('',*,*,#48111,.T.);
#69155=ORIENTED_EDGE('',*,*,#48113,.T.);
#69156=ORIENTED_EDGE('',*,*,#48116,.T.);
#69157=ORIENTED_EDGE('',*,*,#48120,.T.);
#69158=ORIENTED_EDGE('',*,*,#48123,.T.);
#69159=ORIENTED_EDGE('',*,*,#48125,.T.);
#69160=ORIENTED_EDGE('',*,*,#48128,.T.);
#69161=ORIENTED_EDGE('',*,*,#48132,.T.);
#69162=ORIENTED_EDGE('',*,*,#48135,.T.);
#69163=ORIENTED_EDGE('',*,*,#48137,.T.);
#69164=ORIENTED_EDGE('',*,*,#48140,.T.);
#69165=ORIENTED_EDGE('',*,*,#48144,.T.);
#69166=ORIENTED_EDGE('',*,*,#48147,.T.);
#69167=ORIENTED_EDGE('',*,*,#48149,.T.);
#69168=ORIENTED_EDGE('',*,*,#48152,.T.);
#69169=ORIENTED_EDGE('',*,*,#48156,.T.);
#69170=ORIENTED_EDGE('',*,*,#48159,.T.);
#69171=ORIENTED_EDGE('',*,*,#48161,.T.);
#69172=ORIENTED_EDGE('',*,*,#48164,.T.);
#69173=ORIENTED_EDGE('',*,*,#48168,.T.);
#69174=ORIENTED_EDGE('',*,*,#48171,.T.);
#69175=ORIENTED_EDGE('',*,*,#48173,.T.);
#69176=ORIENTED_EDGE('',*,*,#48176,.T.);
#69177=ORIENTED_EDGE('',*,*,#48180,.T.);
#69178=ORIENTED_EDGE('',*,*,#48183,.T.);
#69179=ORIENTED_EDGE('',*,*,#48185,.T.);
#69180=ORIENTED_EDGE('',*,*,#48188,.T.);
#69181=ORIENTED_EDGE('',*,*,#48192,.T.);
#69182=ORIENTED_EDGE('',*,*,#48195,.T.);
#69183=ORIENTED_EDGE('',*,*,#48197,.T.);
#69184=ORIENTED_EDGE('',*,*,#48200,.T.);
#69185=ORIENTED_EDGE('',*,*,#48204,.T.);
#69186=ORIENTED_EDGE('',*,*,#48207,.T.);
#69187=ORIENTED_EDGE('',*,*,#48209,.T.);
#69188=ORIENTED_EDGE('',*,*,#48212,.T.);
#69189=ORIENTED_EDGE('',*,*,#48216,.T.);
#69190=ORIENTED_EDGE('',*,*,#48219,.T.);
#69191=ORIENTED_EDGE('',*,*,#48221,.T.);
#69192=ORIENTED_EDGE('',*,*,#48224,.T.);
#69193=ORIENTED_EDGE('',*,*,#48228,.T.);
#69194=ORIENTED_EDGE('',*,*,#48231,.T.);
#69195=ORIENTED_EDGE('',*,*,#48233,.T.);
#69196=ORIENTED_EDGE('',*,*,#48236,.T.);
#69197=ORIENTED_EDGE('',*,*,#48240,.T.);
#69198=ORIENTED_EDGE('',*,*,#48243,.T.);
#69199=ORIENTED_EDGE('',*,*,#48245,.T.);
#69200=ORIENTED_EDGE('',*,*,#48248,.T.);
#69201=ORIENTED_EDGE('',*,*,#48252,.T.);
#69202=ORIENTED_EDGE('',*,*,#48255,.T.);
#69203=ORIENTED_EDGE('',*,*,#48257,.T.);
#69204=ORIENTED_EDGE('',*,*,#48260,.T.);
#69205=ORIENTED_EDGE('',*,*,#48264,.T.);
#69206=ORIENTED_EDGE('',*,*,#48267,.T.);
#69207=ORIENTED_EDGE('',*,*,#48269,.T.);
#69208=ORIENTED_EDGE('',*,*,#48272,.T.);
#69209=ORIENTED_EDGE('',*,*,#48276,.T.);
#69210=ORIENTED_EDGE('',*,*,#48279,.T.);
#69211=ORIENTED_EDGE('',*,*,#48281,.T.);
#69212=ORIENTED_EDGE('',*,*,#48284,.T.);
#69213=ORIENTED_EDGE('',*,*,#48288,.T.);
#69214=ORIENTED_EDGE('',*,*,#48291,.T.);
#69215=ORIENTED_EDGE('',*,*,#48293,.T.);
#69216=ORIENTED_EDGE('',*,*,#48296,.T.);
#69217=ORIENTED_EDGE('',*,*,#48300,.T.);
#69218=ORIENTED_EDGE('',*,*,#48303,.T.);
#69219=ORIENTED_EDGE('',*,*,#48305,.T.);
#69220=ORIENTED_EDGE('',*,*,#48308,.T.);
#69221=ORIENTED_EDGE('',*,*,#48312,.T.);
#69222=ORIENTED_EDGE('',*,*,#48315,.T.);
#69223=ORIENTED_EDGE('',*,*,#48317,.T.);
#69224=ORIENTED_EDGE('',*,*,#48320,.T.);
#69225=ORIENTED_EDGE('',*,*,#48324,.T.);
#69226=ORIENTED_EDGE('',*,*,#48327,.T.);
#69227=ORIENTED_EDGE('',*,*,#48329,.T.);
#69228=ORIENTED_EDGE('',*,*,#48332,.T.);
#69229=ORIENTED_EDGE('',*,*,#48336,.T.);
#69230=ORIENTED_EDGE('',*,*,#48339,.T.);
#69231=ORIENTED_EDGE('',*,*,#48341,.T.);
#69232=ORIENTED_EDGE('',*,*,#48344,.T.);
#69233=ORIENTED_EDGE('',*,*,#48348,.T.);
#69234=ORIENTED_EDGE('',*,*,#48351,.T.);
#69235=ORIENTED_EDGE('',*,*,#48353,.T.);
#69236=ORIENTED_EDGE('',*,*,#48356,.T.);
#69237=ORIENTED_EDGE('',*,*,#48360,.T.);
#69238=ORIENTED_EDGE('',*,*,#48363,.T.);
#69239=ORIENTED_EDGE('',*,*,#48365,.T.);
#69240=ORIENTED_EDGE('',*,*,#48368,.T.);
#69241=ORIENTED_EDGE('',*,*,#48372,.T.);
#69242=ORIENTED_EDGE('',*,*,#48375,.T.);
#69243=ORIENTED_EDGE('',*,*,#48377,.T.);
#69244=ORIENTED_EDGE('',*,*,#48380,.T.);
#69245=ORIENTED_EDGE('',*,*,#48384,.T.);
#69246=ORIENTED_EDGE('',*,*,#48387,.T.);
#69247=ORIENTED_EDGE('',*,*,#48389,.T.);
#69248=ORIENTED_EDGE('',*,*,#48392,.T.);
#69249=ORIENTED_EDGE('',*,*,#48396,.T.);
#69250=ORIENTED_EDGE('',*,*,#48399,.T.);
#69251=ORIENTED_EDGE('',*,*,#48401,.T.);
#69252=ORIENTED_EDGE('',*,*,#48404,.T.);
#69253=ORIENTED_EDGE('',*,*,#48408,.T.);
#69254=ORIENTED_EDGE('',*,*,#48411,.T.);
#69255=ORIENTED_EDGE('',*,*,#48413,.T.);
#69256=ORIENTED_EDGE('',*,*,#48416,.T.);
#69257=ORIENTED_EDGE('',*,*,#48420,.T.);
#69258=ORIENTED_EDGE('',*,*,#48423,.T.);
#69259=ORIENTED_EDGE('',*,*,#48425,.T.);
#69260=ORIENTED_EDGE('',*,*,#48428,.T.);
#69261=ORIENTED_EDGE('',*,*,#48432,.T.);
#69262=ORIENTED_EDGE('',*,*,#48435,.T.);
#69263=ORIENTED_EDGE('',*,*,#48437,.T.);
#69264=ORIENTED_EDGE('',*,*,#48440,.T.);
#69265=ORIENTED_EDGE('',*,*,#48444,.T.);
#69266=ORIENTED_EDGE('',*,*,#48447,.T.);
#69267=ORIENTED_EDGE('',*,*,#48449,.T.);
#69268=ORIENTED_EDGE('',*,*,#48452,.T.);
#69269=ORIENTED_EDGE('',*,*,#48456,.T.);
#69270=ORIENTED_EDGE('',*,*,#48459,.T.);
#69271=ORIENTED_EDGE('',*,*,#48461,.T.);
#69272=ORIENTED_EDGE('',*,*,#48464,.T.);
#69273=ORIENTED_EDGE('',*,*,#48468,.T.);
#69274=ORIENTED_EDGE('',*,*,#48471,.T.);
#69275=ORIENTED_EDGE('',*,*,#48473,.T.);
#69276=ORIENTED_EDGE('',*,*,#48476,.T.);
#69277=ORIENTED_EDGE('',*,*,#48480,.T.);
#69278=ORIENTED_EDGE('',*,*,#48483,.T.);
#69279=ORIENTED_EDGE('',*,*,#48485,.T.);
#69280=ORIENTED_EDGE('',*,*,#48488,.T.);
#69281=ORIENTED_EDGE('',*,*,#48492,.T.);
#69282=ORIENTED_EDGE('',*,*,#48495,.T.);
#69283=ORIENTED_EDGE('',*,*,#48497,.T.);
#69284=ORIENTED_EDGE('',*,*,#48500,.T.);
#69285=ORIENTED_EDGE('',*,*,#48504,.T.);
#69286=ORIENTED_EDGE('',*,*,#48507,.T.);
#69287=ORIENTED_EDGE('',*,*,#48509,.T.);
#69288=ORIENTED_EDGE('',*,*,#48512,.T.);
#69289=ORIENTED_EDGE('',*,*,#48516,.T.);
#69290=ORIENTED_EDGE('',*,*,#48519,.T.);
#69291=ORIENTED_EDGE('',*,*,#48521,.T.);
#69292=ORIENTED_EDGE('',*,*,#48524,.T.);
#69293=ORIENTED_EDGE('',*,*,#48528,.T.);
#69294=ORIENTED_EDGE('',*,*,#48531,.T.);
#69295=ORIENTED_EDGE('',*,*,#48533,.T.);
#69296=ORIENTED_EDGE('',*,*,#48536,.T.);
#69297=ORIENTED_EDGE('',*,*,#48540,.T.);
#69298=ORIENTED_EDGE('',*,*,#48543,.T.);
#69299=ORIENTED_EDGE('',*,*,#48545,.T.);
#69300=ORIENTED_EDGE('',*,*,#48548,.T.);
#69301=ORIENTED_EDGE('',*,*,#48552,.T.);
#69302=ORIENTED_EDGE('',*,*,#48555,.T.);
#69303=ORIENTED_EDGE('',*,*,#48557,.T.);
#69304=ORIENTED_EDGE('',*,*,#48560,.T.);
#69305=ORIENTED_EDGE('',*,*,#48564,.T.);
#69306=ORIENTED_EDGE('',*,*,#48567,.T.);
#69307=ORIENTED_EDGE('',*,*,#48569,.T.);
#69308=ORIENTED_EDGE('',*,*,#48572,.T.);
#69309=ORIENTED_EDGE('',*,*,#48576,.T.);
#69310=ORIENTED_EDGE('',*,*,#48579,.T.);
#69311=ORIENTED_EDGE('',*,*,#48581,.T.);
#69312=ORIENTED_EDGE('',*,*,#48584,.T.);
#69313=ORIENTED_EDGE('',*,*,#48588,.T.);
#69314=ORIENTED_EDGE('',*,*,#48591,.T.);
#69315=ORIENTED_EDGE('',*,*,#48593,.T.);
#69316=ORIENTED_EDGE('',*,*,#48596,.T.);
#69317=ORIENTED_EDGE('',*,*,#48600,.T.);
#69318=ORIENTED_EDGE('',*,*,#48603,.T.);
#69319=ORIENTED_EDGE('',*,*,#48605,.T.);
#69320=ORIENTED_EDGE('',*,*,#48608,.T.);
#69321=ORIENTED_EDGE('',*,*,#48612,.T.);
#69322=ORIENTED_EDGE('',*,*,#48615,.T.);
#69323=ORIENTED_EDGE('',*,*,#48617,.T.);
#69324=ORIENTED_EDGE('',*,*,#48620,.T.);
#69325=ORIENTED_EDGE('',*,*,#48624,.T.);
#69326=ORIENTED_EDGE('',*,*,#48627,.T.);
#69327=ORIENTED_EDGE('',*,*,#48629,.T.);
#69328=ORIENTED_EDGE('',*,*,#48632,.T.);
#69329=ORIENTED_EDGE('',*,*,#48636,.T.);
#69330=ORIENTED_EDGE('',*,*,#48639,.T.);
#69331=ORIENTED_EDGE('',*,*,#48641,.T.);
#69332=ORIENTED_EDGE('',*,*,#48644,.T.);
#69333=ORIENTED_EDGE('',*,*,#48648,.T.);
#69334=ORIENTED_EDGE('',*,*,#48651,.T.);
#69335=ORIENTED_EDGE('',*,*,#48653,.T.);
#69336=ORIENTED_EDGE('',*,*,#48656,.T.);
#69337=ORIENTED_EDGE('',*,*,#48660,.T.);
#69338=ORIENTED_EDGE('',*,*,#48663,.T.);
#69339=ORIENTED_EDGE('',*,*,#48665,.T.);
#69340=ORIENTED_EDGE('',*,*,#48668,.T.);
#69341=ORIENTED_EDGE('',*,*,#48672,.T.);
#69342=ORIENTED_EDGE('',*,*,#48675,.T.);
#69343=ORIENTED_EDGE('',*,*,#48677,.T.);
#69344=ORIENTED_EDGE('',*,*,#48680,.T.);
#69345=ORIENTED_EDGE('',*,*,#48684,.T.);
#69346=ORIENTED_EDGE('',*,*,#48687,.T.);
#69347=ORIENTED_EDGE('',*,*,#48689,.T.);
#69348=ORIENTED_EDGE('',*,*,#48692,.T.);
#69349=ORIENTED_EDGE('',*,*,#48696,.T.);
#69350=ORIENTED_EDGE('',*,*,#48699,.T.);
#69351=ORIENTED_EDGE('',*,*,#48701,.T.);
#69352=ORIENTED_EDGE('',*,*,#48704,.T.);
#69353=ORIENTED_EDGE('',*,*,#48708,.T.);
#69354=ORIENTED_EDGE('',*,*,#48711,.T.);
#69355=ORIENTED_EDGE('',*,*,#48713,.T.);
#69356=ORIENTED_EDGE('',*,*,#48716,.T.);
#69357=ORIENTED_EDGE('',*,*,#48720,.T.);
#69358=ORIENTED_EDGE('',*,*,#48723,.T.);
#69359=ORIENTED_EDGE('',*,*,#48725,.T.);
#69360=ORIENTED_EDGE('',*,*,#48728,.T.);
#69361=ORIENTED_EDGE('',*,*,#48732,.T.);
#69362=ORIENTED_EDGE('',*,*,#48735,.T.);
#69363=ORIENTED_EDGE('',*,*,#48737,.T.);
#69364=ORIENTED_EDGE('',*,*,#48740,.T.);
#69365=ORIENTED_EDGE('',*,*,#48744,.T.);
#69366=ORIENTED_EDGE('',*,*,#48747,.T.);
#69367=ORIENTED_EDGE('',*,*,#48749,.T.);
#69368=ORIENTED_EDGE('',*,*,#48752,.T.);
#69369=ORIENTED_EDGE('',*,*,#48756,.T.);
#69370=ORIENTED_EDGE('',*,*,#48759,.T.);
#69371=ORIENTED_EDGE('',*,*,#48761,.T.);
#69372=ORIENTED_EDGE('',*,*,#48764,.T.);
#69373=ORIENTED_EDGE('',*,*,#48768,.T.);
#69374=ORIENTED_EDGE('',*,*,#48771,.T.);
#69375=ORIENTED_EDGE('',*,*,#48773,.T.);
#69376=ORIENTED_EDGE('',*,*,#48776,.T.);
#69377=ORIENTED_EDGE('',*,*,#48780,.T.);
#69378=ORIENTED_EDGE('',*,*,#48783,.T.);
#69379=ORIENTED_EDGE('',*,*,#48785,.T.);
#69380=ORIENTED_EDGE('',*,*,#48788,.T.);
#69381=ORIENTED_EDGE('',*,*,#48792,.T.);
#69382=ORIENTED_EDGE('',*,*,#48795,.T.);
#69383=ORIENTED_EDGE('',*,*,#48797,.T.);
#69384=ORIENTED_EDGE('',*,*,#48800,.T.);
#69385=ORIENTED_EDGE('',*,*,#48804,.T.);
#69386=ORIENTED_EDGE('',*,*,#48807,.T.);
#69387=ORIENTED_EDGE('',*,*,#48809,.T.);
#69388=ORIENTED_EDGE('',*,*,#48812,.T.);
#69389=ORIENTED_EDGE('',*,*,#48816,.T.);
#69390=ORIENTED_EDGE('',*,*,#48819,.T.);
#69391=ORIENTED_EDGE('',*,*,#48821,.T.);
#69392=ORIENTED_EDGE('',*,*,#48824,.T.);
#69393=ORIENTED_EDGE('',*,*,#48828,.T.);
#69394=ORIENTED_EDGE('',*,*,#48831,.T.);
#69395=ORIENTED_EDGE('',*,*,#48833,.T.);
#69396=ORIENTED_EDGE('',*,*,#48836,.T.);
#69397=ORIENTED_EDGE('',*,*,#48840,.T.);
#69398=ORIENTED_EDGE('',*,*,#48843,.T.);
#69399=ORIENTED_EDGE('',*,*,#48845,.T.);
#69400=ORIENTED_EDGE('',*,*,#48848,.T.);
#69401=ORIENTED_EDGE('',*,*,#48852,.T.);
#69402=ORIENTED_EDGE('',*,*,#48855,.T.);
#69403=ORIENTED_EDGE('',*,*,#48857,.T.);
#69404=ORIENTED_EDGE('',*,*,#48860,.T.);
#69405=ORIENTED_EDGE('',*,*,#48864,.T.);
#69406=ORIENTED_EDGE('',*,*,#48867,.T.);
#69407=ORIENTED_EDGE('',*,*,#48869,.T.);
#69408=ORIENTED_EDGE('',*,*,#48872,.T.);
#69409=ORIENTED_EDGE('',*,*,#48876,.T.);
#69410=ORIENTED_EDGE('',*,*,#48879,.T.);
#69411=ORIENTED_EDGE('',*,*,#48881,.T.);
#69412=ORIENTED_EDGE('',*,*,#48884,.T.);
#69413=ORIENTED_EDGE('',*,*,#48888,.T.);
#69414=ORIENTED_EDGE('',*,*,#48891,.T.);
#69415=ORIENTED_EDGE('',*,*,#48893,.T.);
#69416=ORIENTED_EDGE('',*,*,#48896,.T.);
#69417=ORIENTED_EDGE('',*,*,#48900,.T.);
#69418=ORIENTED_EDGE('',*,*,#48903,.T.);
#69419=ORIENTED_EDGE('',*,*,#48905,.T.);
#69420=ORIENTED_EDGE('',*,*,#48908,.T.);
#69421=ORIENTED_EDGE('',*,*,#48912,.T.);
#69422=ORIENTED_EDGE('',*,*,#48915,.T.);
#69423=ORIENTED_EDGE('',*,*,#48917,.T.);
#69424=ORIENTED_EDGE('',*,*,#48920,.T.);
#69425=ORIENTED_EDGE('',*,*,#48924,.T.);
#69426=ORIENTED_EDGE('',*,*,#48927,.T.);
#69427=ORIENTED_EDGE('',*,*,#48929,.T.);
#69428=ORIENTED_EDGE('',*,*,#48932,.T.);
#69429=ORIENTED_EDGE('',*,*,#48936,.T.);
#69430=ORIENTED_EDGE('',*,*,#48939,.T.);
#69431=ORIENTED_EDGE('',*,*,#48941,.T.);
#69432=ORIENTED_EDGE('',*,*,#48944,.T.);
#69433=ORIENTED_EDGE('',*,*,#48948,.T.);
#69434=ORIENTED_EDGE('',*,*,#48951,.T.);
#69435=ORIENTED_EDGE('',*,*,#48953,.T.);
#69436=ORIENTED_EDGE('',*,*,#48956,.T.);
#69437=ORIENTED_EDGE('',*,*,#48960,.T.);
#69438=ORIENTED_EDGE('',*,*,#48963,.T.);
#69439=ORIENTED_EDGE('',*,*,#48965,.T.);
#69440=ORIENTED_EDGE('',*,*,#48968,.T.);
#69441=ORIENTED_EDGE('',*,*,#48972,.T.);
#69442=ORIENTED_EDGE('',*,*,#48975,.T.);
#69443=ORIENTED_EDGE('',*,*,#48977,.T.);
#69444=ORIENTED_EDGE('',*,*,#48980,.T.);
#69445=ORIENTED_EDGE('',*,*,#48984,.T.);
#69446=ORIENTED_EDGE('',*,*,#48987,.T.);
#69447=ORIENTED_EDGE('',*,*,#48989,.T.);
#69448=ORIENTED_EDGE('',*,*,#48992,.T.);
#69449=ORIENTED_EDGE('',*,*,#48996,.T.);
#69450=ORIENTED_EDGE('',*,*,#48999,.T.);
#69451=ORIENTED_EDGE('',*,*,#49001,.T.);
#69452=ORIENTED_EDGE('',*,*,#49004,.T.);
#69453=ORIENTED_EDGE('',*,*,#49008,.T.);
#69454=ORIENTED_EDGE('',*,*,#49011,.T.);
#69455=ORIENTED_EDGE('',*,*,#49013,.T.);
#69456=ORIENTED_EDGE('',*,*,#49016,.T.);
#69457=ORIENTED_EDGE('',*,*,#49020,.T.);
#69458=ORIENTED_EDGE('',*,*,#49023,.T.);
#69459=ORIENTED_EDGE('',*,*,#49025,.T.);
#69460=ORIENTED_EDGE('',*,*,#49028,.T.);
#69461=ORIENTED_EDGE('',*,*,#49032,.T.);
#69462=ORIENTED_EDGE('',*,*,#49035,.T.);
#69463=ORIENTED_EDGE('',*,*,#49037,.T.);
#69464=ORIENTED_EDGE('',*,*,#49040,.T.);
#69465=ORIENTED_EDGE('',*,*,#49044,.T.);
#69466=ORIENTED_EDGE('',*,*,#49047,.T.);
#69467=ORIENTED_EDGE('',*,*,#49049,.T.);
#69468=ORIENTED_EDGE('',*,*,#49052,.T.);
#69469=ORIENTED_EDGE('',*,*,#49056,.T.);
#69470=ORIENTED_EDGE('',*,*,#49059,.T.);
#69471=ORIENTED_EDGE('',*,*,#49061,.T.);
#69472=ORIENTED_EDGE('',*,*,#49064,.T.);
#69473=ORIENTED_EDGE('',*,*,#49068,.T.);
#69474=ORIENTED_EDGE('',*,*,#49071,.T.);
#69475=ORIENTED_EDGE('',*,*,#49073,.T.);
#69476=ORIENTED_EDGE('',*,*,#49076,.T.);
#69477=ORIENTED_EDGE('',*,*,#49080,.T.);
#69478=ORIENTED_EDGE('',*,*,#49083,.T.);
#69479=ORIENTED_EDGE('',*,*,#49085,.T.);
#69480=ORIENTED_EDGE('',*,*,#49088,.T.);
#69481=ORIENTED_EDGE('',*,*,#49092,.T.);
#69482=ORIENTED_EDGE('',*,*,#49095,.T.);
#69483=ORIENTED_EDGE('',*,*,#49097,.T.);
#69484=ORIENTED_EDGE('',*,*,#49100,.T.);
#69485=ORIENTED_EDGE('',*,*,#49104,.T.);
#69486=ORIENTED_EDGE('',*,*,#49107,.T.);
#69487=ORIENTED_EDGE('',*,*,#49109,.T.);
#69488=ORIENTED_EDGE('',*,*,#49112,.T.);
#69489=ORIENTED_EDGE('',*,*,#49116,.T.);
#69490=ORIENTED_EDGE('',*,*,#49119,.T.);
#69491=ORIENTED_EDGE('',*,*,#49121,.T.);
#69492=ORIENTED_EDGE('',*,*,#49124,.T.);
#69493=ORIENTED_EDGE('',*,*,#49128,.T.);
#69494=ORIENTED_EDGE('',*,*,#49131,.T.);
#69495=ORIENTED_EDGE('',*,*,#49133,.T.);
#69496=ORIENTED_EDGE('',*,*,#49136,.T.);
#69497=ORIENTED_EDGE('',*,*,#49140,.T.);
#69498=ORIENTED_EDGE('',*,*,#49143,.T.);
#69499=ORIENTED_EDGE('',*,*,#49145,.T.);
#69500=ORIENTED_EDGE('',*,*,#49148,.T.);
#69501=ORIENTED_EDGE('',*,*,#49152,.T.);
#69502=ORIENTED_EDGE('',*,*,#49155,.T.);
#69503=ORIENTED_EDGE('',*,*,#49157,.T.);
#69504=ORIENTED_EDGE('',*,*,#49160,.T.);
#69505=ORIENTED_EDGE('',*,*,#49164,.T.);
#69506=ORIENTED_EDGE('',*,*,#49167,.T.);
#69507=ORIENTED_EDGE('',*,*,#49169,.T.);
#69508=ORIENTED_EDGE('',*,*,#49172,.T.);
#69509=ORIENTED_EDGE('',*,*,#49176,.T.);
#69510=ORIENTED_EDGE('',*,*,#49179,.T.);
#69511=ORIENTED_EDGE('',*,*,#49181,.T.);
#69512=ORIENTED_EDGE('',*,*,#49184,.T.);
#69513=ORIENTED_EDGE('',*,*,#49188,.T.);
#69514=ORIENTED_EDGE('',*,*,#49191,.T.);
#69515=ORIENTED_EDGE('',*,*,#49193,.T.);
#69516=ORIENTED_EDGE('',*,*,#49196,.T.);
#69517=ORIENTED_EDGE('',*,*,#49200,.T.);
#69518=ORIENTED_EDGE('',*,*,#49203,.T.);
#69519=ORIENTED_EDGE('',*,*,#49205,.T.);
#69520=ORIENTED_EDGE('',*,*,#49208,.T.);
#69521=ORIENTED_EDGE('',*,*,#49212,.T.);
#69522=ORIENTED_EDGE('',*,*,#49215,.T.);
#69523=ORIENTED_EDGE('',*,*,#49217,.T.);
#69524=ORIENTED_EDGE('',*,*,#49220,.T.);
#69525=ORIENTED_EDGE('',*,*,#49224,.T.);
#69526=ORIENTED_EDGE('',*,*,#49227,.T.);
#69527=ORIENTED_EDGE('',*,*,#49229,.T.);
#69528=ORIENTED_EDGE('',*,*,#49232,.T.);
#69529=ORIENTED_EDGE('',*,*,#49236,.T.);
#69530=ORIENTED_EDGE('',*,*,#49239,.T.);
#69531=ORIENTED_EDGE('',*,*,#49241,.T.);
#69532=ORIENTED_EDGE('',*,*,#49244,.T.);
#69533=ORIENTED_EDGE('',*,*,#49248,.T.);
#69534=ORIENTED_EDGE('',*,*,#49251,.T.);
#69535=ORIENTED_EDGE('',*,*,#49253,.T.);
#69536=ORIENTED_EDGE('',*,*,#49256,.T.);
#69537=ORIENTED_EDGE('',*,*,#49260,.T.);
#69538=ORIENTED_EDGE('',*,*,#49263,.T.);
#69539=ORIENTED_EDGE('',*,*,#49265,.T.);
#69540=ORIENTED_EDGE('',*,*,#49268,.T.);
#69541=ORIENTED_EDGE('',*,*,#49272,.T.);
#69542=ORIENTED_EDGE('',*,*,#49275,.T.);
#69543=ORIENTED_EDGE('',*,*,#49277,.T.);
#69544=ORIENTED_EDGE('',*,*,#49280,.T.);
#69545=ORIENTED_EDGE('',*,*,#49284,.T.);
#69546=ORIENTED_EDGE('',*,*,#49287,.T.);
#69547=ORIENTED_EDGE('',*,*,#49289,.T.);
#69548=ORIENTED_EDGE('',*,*,#49292,.T.);
#69549=ORIENTED_EDGE('',*,*,#49296,.T.);
#69550=ORIENTED_EDGE('',*,*,#49299,.T.);
#69551=ORIENTED_EDGE('',*,*,#49301,.T.);
#69552=ORIENTED_EDGE('',*,*,#49304,.T.);
#69553=ORIENTED_EDGE('',*,*,#49308,.T.);
#69554=ORIENTED_EDGE('',*,*,#49311,.T.);
#69555=ORIENTED_EDGE('',*,*,#49313,.T.);
#69556=ORIENTED_EDGE('',*,*,#49316,.T.);
#69557=ORIENTED_EDGE('',*,*,#49320,.T.);
#69558=ORIENTED_EDGE('',*,*,#49323,.T.);
#69559=ORIENTED_EDGE('',*,*,#49325,.T.);
#69560=ORIENTED_EDGE('',*,*,#49328,.T.);
#69561=ORIENTED_EDGE('',*,*,#49332,.T.);
#69562=ORIENTED_EDGE('',*,*,#49335,.T.);
#69563=ORIENTED_EDGE('',*,*,#49337,.T.);
#69564=ORIENTED_EDGE('',*,*,#49340,.T.);
#69565=ORIENTED_EDGE('',*,*,#49344,.T.);
#69566=ORIENTED_EDGE('',*,*,#49347,.T.);
#69567=ORIENTED_EDGE('',*,*,#49349,.T.);
#69568=ORIENTED_EDGE('',*,*,#49352,.T.);
#69569=ORIENTED_EDGE('',*,*,#49356,.T.);
#69570=ORIENTED_EDGE('',*,*,#49359,.T.);
#69571=ORIENTED_EDGE('',*,*,#49361,.T.);
#69572=ORIENTED_EDGE('',*,*,#49364,.T.);
#69573=ORIENTED_EDGE('',*,*,#49368,.T.);
#69574=ORIENTED_EDGE('',*,*,#49371,.T.);
#69575=ORIENTED_EDGE('',*,*,#49373,.T.);
#69576=ORIENTED_EDGE('',*,*,#49376,.T.);
#69577=ORIENTED_EDGE('',*,*,#49380,.T.);
#69578=ORIENTED_EDGE('',*,*,#49383,.T.);
#69579=ORIENTED_EDGE('',*,*,#49385,.T.);
#69580=ORIENTED_EDGE('',*,*,#49388,.T.);
#69581=ORIENTED_EDGE('',*,*,#49392,.T.);
#69582=ORIENTED_EDGE('',*,*,#49395,.T.);
#69583=ORIENTED_EDGE('',*,*,#49397,.T.);
#69584=ORIENTED_EDGE('',*,*,#49400,.T.);
#69585=ORIENTED_EDGE('',*,*,#49404,.T.);
#69586=ORIENTED_EDGE('',*,*,#49407,.T.);
#69587=ORIENTED_EDGE('',*,*,#49409,.T.);
#69588=ORIENTED_EDGE('',*,*,#49412,.T.);
#69589=ORIENTED_EDGE('',*,*,#49416,.T.);
#69590=ORIENTED_EDGE('',*,*,#49419,.T.);
#69591=ORIENTED_EDGE('',*,*,#49421,.T.);
#69592=ORIENTED_EDGE('',*,*,#49424,.T.);
#69593=ORIENTED_EDGE('',*,*,#49428,.T.);
#69594=ORIENTED_EDGE('',*,*,#49431,.T.);
#69595=ORIENTED_EDGE('',*,*,#49433,.T.);
#69596=ORIENTED_EDGE('',*,*,#49436,.T.);
#69597=ORIENTED_EDGE('',*,*,#49440,.T.);
#69598=ORIENTED_EDGE('',*,*,#49443,.T.);
#69599=ORIENTED_EDGE('',*,*,#49445,.T.);
#69600=ORIENTED_EDGE('',*,*,#49448,.T.);
#69601=ORIENTED_EDGE('',*,*,#49452,.T.);
#69602=ORIENTED_EDGE('',*,*,#49455,.T.);
#69603=ORIENTED_EDGE('',*,*,#49457,.T.);
#69604=ORIENTED_EDGE('',*,*,#49460,.T.);
#69605=ORIENTED_EDGE('',*,*,#49464,.T.);
#69606=ORIENTED_EDGE('',*,*,#49467,.T.);
#69607=ORIENTED_EDGE('',*,*,#49469,.T.);
#69608=ORIENTED_EDGE('',*,*,#49472,.T.);
#69609=ORIENTED_EDGE('',*,*,#49476,.T.);
#69610=ORIENTED_EDGE('',*,*,#49479,.T.);
#69611=ORIENTED_EDGE('',*,*,#49481,.T.);
#69612=ORIENTED_EDGE('',*,*,#49484,.T.);
#69613=ORIENTED_EDGE('',*,*,#49488,.T.);
#69614=ORIENTED_EDGE('',*,*,#49491,.T.);
#69615=ORIENTED_EDGE('',*,*,#49493,.T.);
#69616=ORIENTED_EDGE('',*,*,#49496,.T.);
#69617=ORIENTED_EDGE('',*,*,#49500,.T.);
#69618=ORIENTED_EDGE('',*,*,#49503,.T.);
#69619=ORIENTED_EDGE('',*,*,#49505,.T.);
#69620=ORIENTED_EDGE('',*,*,#49508,.T.);
#69621=ORIENTED_EDGE('',*,*,#49512,.T.);
#69622=ORIENTED_EDGE('',*,*,#49515,.T.);
#69623=ORIENTED_EDGE('',*,*,#49517,.T.);
#69624=ORIENTED_EDGE('',*,*,#49520,.T.);
#69625=ORIENTED_EDGE('',*,*,#49524,.T.);
#69626=ORIENTED_EDGE('',*,*,#49527,.T.);
#69627=ORIENTED_EDGE('',*,*,#49529,.T.);
#69628=ORIENTED_EDGE('',*,*,#49532,.T.);
#69629=ORIENTED_EDGE('',*,*,#49536,.T.);
#69630=ORIENTED_EDGE('',*,*,#49539,.T.);
#69631=ORIENTED_EDGE('',*,*,#49541,.T.);
#69632=ORIENTED_EDGE('',*,*,#49544,.T.);
#69633=ORIENTED_EDGE('',*,*,#49548,.T.);
#69634=ORIENTED_EDGE('',*,*,#49551,.T.);
#69635=ORIENTED_EDGE('',*,*,#49553,.T.);
#69636=ORIENTED_EDGE('',*,*,#49556,.T.);
#69637=ORIENTED_EDGE('',*,*,#49560,.T.);
#69638=ORIENTED_EDGE('',*,*,#49563,.T.);
#69639=ORIENTED_EDGE('',*,*,#49565,.T.);
#69640=ORIENTED_EDGE('',*,*,#49568,.T.);
#69641=ORIENTED_EDGE('',*,*,#49572,.T.);
#69642=ORIENTED_EDGE('',*,*,#49575,.T.);
#69643=ORIENTED_EDGE('',*,*,#49577,.T.);
#69644=ORIENTED_EDGE('',*,*,#49580,.T.);
#69645=ORIENTED_EDGE('',*,*,#49584,.T.);
#69646=ORIENTED_EDGE('',*,*,#49587,.T.);
#69647=ORIENTED_EDGE('',*,*,#49589,.T.);
#69648=ORIENTED_EDGE('',*,*,#49592,.T.);
#69649=ORIENTED_EDGE('',*,*,#49596,.T.);
#69650=ORIENTED_EDGE('',*,*,#49599,.T.);
#69651=ORIENTED_EDGE('',*,*,#49601,.T.);
#69652=ORIENTED_EDGE('',*,*,#49604,.T.);
#69653=ORIENTED_EDGE('',*,*,#49608,.T.);
#69654=ORIENTED_EDGE('',*,*,#49611,.T.);
#69655=ORIENTED_EDGE('',*,*,#49613,.T.);
#69656=ORIENTED_EDGE('',*,*,#49616,.T.);
#69657=ORIENTED_EDGE('',*,*,#49620,.T.);
#69658=ORIENTED_EDGE('',*,*,#49623,.T.);
#69659=ORIENTED_EDGE('',*,*,#49625,.T.);
#69660=ORIENTED_EDGE('',*,*,#49628,.T.);
#69661=ORIENTED_EDGE('',*,*,#49632,.T.);
#69662=ORIENTED_EDGE('',*,*,#49635,.T.);
#69663=ORIENTED_EDGE('',*,*,#49637,.T.);
#69664=ORIENTED_EDGE('',*,*,#49640,.T.);
#69665=ORIENTED_EDGE('',*,*,#49644,.T.);
#69666=ORIENTED_EDGE('',*,*,#49647,.T.);
#69667=ORIENTED_EDGE('',*,*,#49649,.T.);
#69668=ORIENTED_EDGE('',*,*,#49652,.T.);
#69669=ORIENTED_EDGE('',*,*,#49656,.T.);
#69670=ORIENTED_EDGE('',*,*,#49659,.T.);
#69671=ORIENTED_EDGE('',*,*,#49661,.T.);
#69672=ORIENTED_EDGE('',*,*,#49664,.T.);
#69673=ORIENTED_EDGE('',*,*,#49668,.T.);
#69674=ORIENTED_EDGE('',*,*,#49671,.T.);
#69675=ORIENTED_EDGE('',*,*,#49673,.T.);
#69676=ORIENTED_EDGE('',*,*,#49676,.T.);
#69677=ORIENTED_EDGE('',*,*,#49680,.T.);
#69678=ORIENTED_EDGE('',*,*,#49683,.T.);
#69679=ORIENTED_EDGE('',*,*,#49685,.T.);
#69680=ORIENTED_EDGE('',*,*,#49688,.T.);
#69681=ORIENTED_EDGE('',*,*,#49692,.T.);
#69682=ORIENTED_EDGE('',*,*,#49695,.T.);
#69683=ORIENTED_EDGE('',*,*,#49697,.T.);
#69684=ORIENTED_EDGE('',*,*,#49700,.T.);
#69685=ORIENTED_EDGE('',*,*,#49704,.T.);
#69686=ORIENTED_EDGE('',*,*,#49707,.T.);
#69687=ORIENTED_EDGE('',*,*,#49709,.T.);
#69688=ORIENTED_EDGE('',*,*,#49712,.T.);
#69689=ORIENTED_EDGE('',*,*,#49716,.T.);
#69690=ORIENTED_EDGE('',*,*,#49719,.T.);
#69691=ORIENTED_EDGE('',*,*,#49721,.T.);
#69692=ORIENTED_EDGE('',*,*,#49724,.T.);
#69693=ORIENTED_EDGE('',*,*,#49728,.T.);
#69694=ORIENTED_EDGE('',*,*,#49731,.T.);
#69695=ORIENTED_EDGE('',*,*,#49733,.T.);
#69696=ORIENTED_EDGE('',*,*,#49736,.T.);
#69697=ORIENTED_EDGE('',*,*,#49740,.T.);
#69698=ORIENTED_EDGE('',*,*,#49743,.T.);
#69699=ORIENTED_EDGE('',*,*,#49745,.T.);
#69700=ORIENTED_EDGE('',*,*,#49748,.T.);
#69701=ORIENTED_EDGE('',*,*,#49752,.T.);
#69702=ORIENTED_EDGE('',*,*,#49755,.T.);
#69703=ORIENTED_EDGE('',*,*,#49757,.T.);
#69704=ORIENTED_EDGE('',*,*,#49760,.T.);
#69705=ORIENTED_EDGE('',*,*,#49764,.T.);
#69706=ORIENTED_EDGE('',*,*,#49767,.T.);
#69707=ORIENTED_EDGE('',*,*,#49769,.T.);
#69708=ORIENTED_EDGE('',*,*,#49772,.T.);
#69709=ORIENTED_EDGE('',*,*,#49776,.T.);
#69710=ORIENTED_EDGE('',*,*,#49779,.T.);
#69711=ORIENTED_EDGE('',*,*,#49781,.T.);
#69712=ORIENTED_EDGE('',*,*,#49784,.T.);
#69713=ORIENTED_EDGE('',*,*,#49788,.T.);
#69714=ORIENTED_EDGE('',*,*,#49791,.T.);
#69715=ORIENTED_EDGE('',*,*,#49793,.T.);
#69716=ORIENTED_EDGE('',*,*,#49796,.T.);
#69717=ORIENTED_EDGE('',*,*,#49800,.T.);
#69718=ORIENTED_EDGE('',*,*,#49803,.T.);
#69719=ORIENTED_EDGE('',*,*,#49805,.T.);
#69720=ORIENTED_EDGE('',*,*,#49808,.T.);
#69721=ORIENTED_EDGE('',*,*,#49812,.T.);
#69722=ORIENTED_EDGE('',*,*,#49815,.T.);
#69723=ORIENTED_EDGE('',*,*,#49817,.T.);
#69724=ORIENTED_EDGE('',*,*,#49820,.T.);
#69725=ORIENTED_EDGE('',*,*,#49824,.T.);
#69726=ORIENTED_EDGE('',*,*,#49827,.T.);
#69727=ORIENTED_EDGE('',*,*,#49829,.T.);
#69728=ORIENTED_EDGE('',*,*,#49832,.T.);
#69729=ORIENTED_EDGE('',*,*,#49836,.T.);
#69730=ORIENTED_EDGE('',*,*,#49839,.T.);
#69731=ORIENTED_EDGE('',*,*,#49841,.T.);
#69732=ORIENTED_EDGE('',*,*,#49844,.T.);
#69733=ORIENTED_EDGE('',*,*,#49848,.T.);
#69734=ORIENTED_EDGE('',*,*,#49851,.T.);
#69735=ORIENTED_EDGE('',*,*,#49853,.T.);
#69736=ORIENTED_EDGE('',*,*,#49856,.T.);
#69737=ORIENTED_EDGE('',*,*,#49860,.T.);
#69738=ORIENTED_EDGE('',*,*,#49863,.T.);
#69739=ORIENTED_EDGE('',*,*,#49865,.T.);
#69740=ORIENTED_EDGE('',*,*,#49868,.T.);
#69741=ORIENTED_EDGE('',*,*,#49872,.T.);
#69742=ORIENTED_EDGE('',*,*,#49875,.T.);
#69743=ORIENTED_EDGE('',*,*,#49877,.T.);
#69744=ORIENTED_EDGE('',*,*,#49880,.T.);
#69745=ORIENTED_EDGE('',*,*,#49884,.T.);
#69746=ORIENTED_EDGE('',*,*,#49887,.T.);
#69747=ORIENTED_EDGE('',*,*,#49889,.T.);
#69748=ORIENTED_EDGE('',*,*,#49892,.T.);
#69749=ORIENTED_EDGE('',*,*,#49896,.T.);
#69750=ORIENTED_EDGE('',*,*,#49899,.T.);
#69751=ORIENTED_EDGE('',*,*,#49901,.T.);
#69752=ORIENTED_EDGE('',*,*,#49904,.T.);
#69753=ORIENTED_EDGE('',*,*,#49908,.T.);
#69754=ORIENTED_EDGE('',*,*,#49911,.T.);
#69755=ORIENTED_EDGE('',*,*,#49913,.T.);
#69756=ORIENTED_EDGE('',*,*,#49916,.T.);
#69757=ORIENTED_EDGE('',*,*,#49920,.T.);
#69758=ORIENTED_EDGE('',*,*,#49923,.T.);
#69759=ORIENTED_EDGE('',*,*,#49925,.T.);
#69760=ORIENTED_EDGE('',*,*,#49928,.T.);
#69761=ORIENTED_EDGE('',*,*,#49932,.T.);
#69762=ORIENTED_EDGE('',*,*,#49935,.T.);
#69763=ORIENTED_EDGE('',*,*,#49937,.T.);
#69764=ORIENTED_EDGE('',*,*,#49940,.T.);
#69765=ORIENTED_EDGE('',*,*,#49944,.T.);
#69766=ORIENTED_EDGE('',*,*,#49947,.T.);
#69767=ORIENTED_EDGE('',*,*,#49949,.T.);
#69768=ORIENTED_EDGE('',*,*,#49952,.T.);
#69769=ORIENTED_EDGE('',*,*,#49956,.T.);
#69770=ORIENTED_EDGE('',*,*,#49959,.T.);
#69771=ORIENTED_EDGE('',*,*,#49961,.T.);
#69772=ORIENTED_EDGE('',*,*,#49964,.T.);
#69773=ORIENTED_EDGE('',*,*,#49968,.T.);
#69774=ORIENTED_EDGE('',*,*,#49971,.T.);
#69775=ORIENTED_EDGE('',*,*,#49973,.T.);
#69776=ORIENTED_EDGE('',*,*,#49976,.T.);
#69777=ORIENTED_EDGE('',*,*,#49980,.T.);
#69778=ORIENTED_EDGE('',*,*,#49983,.T.);
#69779=ORIENTED_EDGE('',*,*,#49985,.T.);
#69780=ORIENTED_EDGE('',*,*,#49988,.T.);
#69781=ORIENTED_EDGE('',*,*,#49992,.T.);
#69782=ORIENTED_EDGE('',*,*,#49995,.T.);
#69783=ORIENTED_EDGE('',*,*,#49997,.T.);
#69784=ORIENTED_EDGE('',*,*,#50000,.T.);
#69785=ORIENTED_EDGE('',*,*,#50004,.T.);
#69786=ORIENTED_EDGE('',*,*,#50007,.T.);
#69787=ORIENTED_EDGE('',*,*,#50009,.T.);
#69788=ORIENTED_EDGE('',*,*,#50012,.T.);
#69789=ORIENTED_EDGE('',*,*,#50016,.T.);
#69790=ORIENTED_EDGE('',*,*,#50019,.T.);
#69791=ORIENTED_EDGE('',*,*,#50021,.T.);
#69792=ORIENTED_EDGE('',*,*,#50024,.T.);
#69793=ORIENTED_EDGE('',*,*,#50028,.T.);
#69794=ORIENTED_EDGE('',*,*,#50031,.T.);
#69795=ORIENTED_EDGE('',*,*,#50033,.T.);
#69796=ORIENTED_EDGE('',*,*,#50036,.T.);
#69797=ORIENTED_EDGE('',*,*,#50040,.T.);
#69798=ORIENTED_EDGE('',*,*,#50043,.T.);
#69799=ORIENTED_EDGE('',*,*,#50045,.T.);
#69800=ORIENTED_EDGE('',*,*,#50048,.T.);
#69801=ORIENTED_EDGE('',*,*,#50052,.T.);
#69802=ORIENTED_EDGE('',*,*,#50055,.T.);
#69803=ORIENTED_EDGE('',*,*,#50057,.T.);
#69804=ORIENTED_EDGE('',*,*,#50060,.T.);
#69805=ORIENTED_EDGE('',*,*,#50064,.T.);
#69806=ORIENTED_EDGE('',*,*,#50067,.T.);
#69807=ORIENTED_EDGE('',*,*,#50069,.T.);
#69808=ORIENTED_EDGE('',*,*,#50072,.T.);
#69809=ORIENTED_EDGE('',*,*,#50076,.T.);
#69810=ORIENTED_EDGE('',*,*,#50079,.T.);
#69811=ORIENTED_EDGE('',*,*,#50081,.T.);
#69812=ORIENTED_EDGE('',*,*,#50084,.T.);
#69813=ORIENTED_EDGE('',*,*,#50088,.T.);
#69814=ORIENTED_EDGE('',*,*,#50091,.T.);
#69815=ORIENTED_EDGE('',*,*,#50093,.T.);
#69816=ORIENTED_EDGE('',*,*,#50096,.T.);
#69817=ORIENTED_EDGE('',*,*,#50100,.T.);
#69818=ORIENTED_EDGE('',*,*,#50103,.T.);
#69819=ORIENTED_EDGE('',*,*,#50105,.T.);
#69820=ORIENTED_EDGE('',*,*,#50108,.T.);
#69821=ORIENTED_EDGE('',*,*,#50112,.T.);
#69822=ORIENTED_EDGE('',*,*,#50115,.T.);
#69823=ORIENTED_EDGE('',*,*,#50117,.T.);
#69824=ORIENTED_EDGE('',*,*,#50120,.T.);
#69825=ORIENTED_EDGE('',*,*,#50124,.T.);
#69826=ORIENTED_EDGE('',*,*,#50127,.T.);
#69827=ORIENTED_EDGE('',*,*,#50129,.T.);
#69828=ORIENTED_EDGE('',*,*,#50132,.T.);
#69829=ORIENTED_EDGE('',*,*,#50136,.T.);
#69830=ORIENTED_EDGE('',*,*,#50139,.T.);
#69831=ORIENTED_EDGE('',*,*,#50141,.T.);
#69832=ORIENTED_EDGE('',*,*,#50144,.T.);
#69833=ORIENTED_EDGE('',*,*,#50148,.T.);
#69834=ORIENTED_EDGE('',*,*,#50151,.T.);
#69835=ORIENTED_EDGE('',*,*,#50153,.T.);
#69836=ORIENTED_EDGE('',*,*,#50156,.T.);
#69837=ORIENTED_EDGE('',*,*,#50160,.T.);
#69838=ORIENTED_EDGE('',*,*,#50163,.T.);
#69839=ORIENTED_EDGE('',*,*,#50165,.T.);
#69840=ORIENTED_EDGE('',*,*,#50168,.T.);
#69841=ORIENTED_EDGE('',*,*,#50172,.T.);
#69842=ORIENTED_EDGE('',*,*,#50175,.T.);
#69843=ORIENTED_EDGE('',*,*,#50177,.T.);
#69844=ORIENTED_EDGE('',*,*,#50180,.T.);
#69845=ORIENTED_EDGE('',*,*,#50184,.T.);
#69846=ORIENTED_EDGE('',*,*,#50187,.T.);
#69847=ORIENTED_EDGE('',*,*,#50189,.T.);
#69848=ORIENTED_EDGE('',*,*,#50192,.T.);
#69849=ORIENTED_EDGE('',*,*,#50196,.T.);
#69850=ORIENTED_EDGE('',*,*,#50199,.T.);
#69851=ORIENTED_EDGE('',*,*,#50201,.T.);
#69852=ORIENTED_EDGE('',*,*,#50204,.T.);
#69853=ORIENTED_EDGE('',*,*,#50208,.T.);
#69854=ORIENTED_EDGE('',*,*,#50211,.T.);
#69855=ORIENTED_EDGE('',*,*,#50213,.T.);
#69856=ORIENTED_EDGE('',*,*,#50216,.T.);
#69857=ORIENTED_EDGE('',*,*,#50220,.T.);
#69858=ORIENTED_EDGE('',*,*,#50223,.T.);
#69859=ORIENTED_EDGE('',*,*,#50225,.T.);
#69860=ORIENTED_EDGE('',*,*,#50228,.T.);
#69861=ORIENTED_EDGE('',*,*,#50232,.T.);
#69862=ORIENTED_EDGE('',*,*,#50235,.T.);
#69863=ORIENTED_EDGE('',*,*,#50237,.T.);
#69864=ORIENTED_EDGE('',*,*,#50240,.T.);
#69865=ORIENTED_EDGE('',*,*,#50244,.T.);
#69866=ORIENTED_EDGE('',*,*,#50247,.T.);
#69867=ORIENTED_EDGE('',*,*,#50249,.T.);
#69868=ORIENTED_EDGE('',*,*,#50252,.T.);
#69869=ORIENTED_EDGE('',*,*,#50256,.T.);
#69870=ORIENTED_EDGE('',*,*,#50259,.T.);
#69871=ORIENTED_EDGE('',*,*,#50261,.T.);
#69872=ORIENTED_EDGE('',*,*,#50264,.T.);
#69873=ORIENTED_EDGE('',*,*,#50268,.T.);
#69874=ORIENTED_EDGE('',*,*,#50271,.T.);
#69875=ORIENTED_EDGE('',*,*,#50273,.T.);
#69876=ORIENTED_EDGE('',*,*,#50276,.T.);
#69877=ORIENTED_EDGE('',*,*,#50280,.T.);
#69878=ORIENTED_EDGE('',*,*,#50283,.T.);
#69879=ORIENTED_EDGE('',*,*,#50285,.T.);
#69880=ORIENTED_EDGE('',*,*,#50288,.T.);
#69881=ORIENTED_EDGE('',*,*,#50292,.T.);
#69882=ORIENTED_EDGE('',*,*,#50295,.T.);
#69883=ORIENTED_EDGE('',*,*,#50297,.T.);
#69884=ORIENTED_EDGE('',*,*,#50300,.T.);
#69885=ORIENTED_EDGE('',*,*,#50304,.T.);
#69886=ORIENTED_EDGE('',*,*,#50307,.T.);
#69887=ORIENTED_EDGE('',*,*,#50309,.T.);
#69888=ORIENTED_EDGE('',*,*,#50312,.T.);
#69889=ORIENTED_EDGE('',*,*,#50316,.T.);
#69890=ORIENTED_EDGE('',*,*,#50319,.T.);
#69891=ORIENTED_EDGE('',*,*,#50321,.T.);
#69892=ORIENTED_EDGE('',*,*,#50324,.T.);
#69893=ORIENTED_EDGE('',*,*,#50328,.T.);
#69894=ORIENTED_EDGE('',*,*,#50331,.T.);
#69895=ORIENTED_EDGE('',*,*,#50333,.T.);
#69896=ORIENTED_EDGE('',*,*,#50336,.T.);
#69897=ORIENTED_EDGE('',*,*,#50340,.T.);
#69898=ORIENTED_EDGE('',*,*,#50343,.T.);
#69899=ORIENTED_EDGE('',*,*,#50345,.T.);
#69900=ORIENTED_EDGE('',*,*,#50348,.T.);
#69901=ORIENTED_EDGE('',*,*,#50352,.T.);
#69902=ORIENTED_EDGE('',*,*,#50355,.T.);
#69903=ORIENTED_EDGE('',*,*,#50357,.T.);
#69904=ORIENTED_EDGE('',*,*,#50360,.T.);
#69905=ORIENTED_EDGE('',*,*,#50364,.T.);
#69906=ORIENTED_EDGE('',*,*,#50367,.T.);
#69907=ORIENTED_EDGE('',*,*,#50369,.T.);
#69908=ORIENTED_EDGE('',*,*,#50372,.T.);
#69909=ORIENTED_EDGE('',*,*,#50376,.T.);
#69910=ORIENTED_EDGE('',*,*,#50379,.T.);
#69911=ORIENTED_EDGE('',*,*,#50381,.T.);
#69912=ORIENTED_EDGE('',*,*,#50384,.T.);
#69913=ORIENTED_EDGE('',*,*,#50388,.T.);
#69914=ORIENTED_EDGE('',*,*,#50391,.T.);
#69915=ORIENTED_EDGE('',*,*,#50393,.T.);
#69916=ORIENTED_EDGE('',*,*,#50396,.T.);
#69917=ORIENTED_EDGE('',*,*,#50400,.T.);
#69918=ORIENTED_EDGE('',*,*,#50403,.T.);
#69919=ORIENTED_EDGE('',*,*,#50405,.T.);
#69920=ORIENTED_EDGE('',*,*,#50408,.T.);
#69921=ORIENTED_EDGE('',*,*,#50412,.T.);
#69922=ORIENTED_EDGE('',*,*,#50415,.T.);
#69923=ORIENTED_EDGE('',*,*,#50417,.T.);
#69924=ORIENTED_EDGE('',*,*,#50420,.T.);
#69925=ORIENTED_EDGE('',*,*,#50424,.T.);
#69926=ORIENTED_EDGE('',*,*,#50427,.T.);
#69927=ORIENTED_EDGE('',*,*,#50429,.T.);
#69928=ORIENTED_EDGE('',*,*,#50432,.T.);
#69929=ORIENTED_EDGE('',*,*,#50436,.T.);
#69930=ORIENTED_EDGE('',*,*,#50439,.T.);
#69931=ORIENTED_EDGE('',*,*,#50441,.T.);
#69932=ORIENTED_EDGE('',*,*,#50444,.T.);
#69933=ORIENTED_EDGE('',*,*,#50448,.T.);
#69934=ORIENTED_EDGE('',*,*,#50451,.T.);
#69935=ORIENTED_EDGE('',*,*,#50453,.T.);
#69936=ORIENTED_EDGE('',*,*,#50456,.T.);
#69937=ORIENTED_EDGE('',*,*,#50460,.T.);
#69938=ORIENTED_EDGE('',*,*,#50463,.T.);
#69939=ORIENTED_EDGE('',*,*,#50465,.T.);
#69940=ORIENTED_EDGE('',*,*,#50468,.T.);
#69941=ORIENTED_EDGE('',*,*,#50472,.T.);
#69942=ORIENTED_EDGE('',*,*,#50475,.T.);
#69943=ORIENTED_EDGE('',*,*,#50477,.T.);
#69944=ORIENTED_EDGE('',*,*,#50480,.T.);
#69945=ORIENTED_EDGE('',*,*,#50484,.T.);
#69946=ORIENTED_EDGE('',*,*,#50487,.T.);
#69947=ORIENTED_EDGE('',*,*,#50489,.T.);
#69948=ORIENTED_EDGE('',*,*,#50492,.T.);
#69949=ORIENTED_EDGE('',*,*,#50496,.T.);
#69950=ORIENTED_EDGE('',*,*,#50499,.T.);
#69951=ORIENTED_EDGE('',*,*,#50501,.T.);
#69952=ORIENTED_EDGE('',*,*,#50504,.T.);
#69953=ORIENTED_EDGE('',*,*,#50508,.T.);
#69954=ORIENTED_EDGE('',*,*,#50511,.T.);
#69955=ORIENTED_EDGE('',*,*,#50513,.T.);
#69956=ORIENTED_EDGE('',*,*,#50516,.T.);
#69957=ORIENTED_EDGE('',*,*,#50520,.T.);
#69958=ORIENTED_EDGE('',*,*,#50523,.T.);
#69959=ORIENTED_EDGE('',*,*,#50525,.T.);
#69960=ORIENTED_EDGE('',*,*,#50528,.T.);
#69961=ORIENTED_EDGE('',*,*,#50532,.T.);
#69962=ORIENTED_EDGE('',*,*,#50535,.T.);
#69963=ORIENTED_EDGE('',*,*,#50537,.T.);
#69964=ORIENTED_EDGE('',*,*,#50540,.T.);
#69965=ORIENTED_EDGE('',*,*,#50544,.T.);
#69966=ORIENTED_EDGE('',*,*,#50547,.T.);
#69967=ORIENTED_EDGE('',*,*,#50549,.T.);
#69968=ORIENTED_EDGE('',*,*,#50552,.T.);
#69969=ORIENTED_EDGE('',*,*,#50556,.T.);
#69970=ORIENTED_EDGE('',*,*,#50559,.T.);
#69971=ORIENTED_EDGE('',*,*,#50561,.T.);
#69972=ORIENTED_EDGE('',*,*,#50564,.T.);
#69973=ORIENTED_EDGE('',*,*,#50568,.T.);
#69974=ORIENTED_EDGE('',*,*,#50571,.T.);
#69975=ORIENTED_EDGE('',*,*,#50573,.T.);
#69976=ORIENTED_EDGE('',*,*,#50576,.T.);
#69977=ORIENTED_EDGE('',*,*,#50580,.T.);
#69978=ORIENTED_EDGE('',*,*,#50583,.T.);
#69979=ORIENTED_EDGE('',*,*,#50585,.T.);
#69980=ORIENTED_EDGE('',*,*,#50588,.T.);
#69981=ORIENTED_EDGE('',*,*,#50592,.T.);
#69982=ORIENTED_EDGE('',*,*,#50595,.T.);
#69983=ORIENTED_EDGE('',*,*,#50597,.T.);
#69984=ORIENTED_EDGE('',*,*,#50600,.T.);
#69985=ORIENTED_EDGE('',*,*,#50604,.T.);
#69986=ORIENTED_EDGE('',*,*,#50607,.T.);
#69987=ORIENTED_EDGE('',*,*,#50609,.T.);
#69988=ORIENTED_EDGE('',*,*,#50612,.T.);
#69989=ORIENTED_EDGE('',*,*,#50616,.T.);
#69990=ORIENTED_EDGE('',*,*,#50619,.T.);
#69991=ORIENTED_EDGE('',*,*,#50621,.T.);
#69992=ORIENTED_EDGE('',*,*,#50624,.T.);
#69993=ORIENTED_EDGE('',*,*,#50628,.T.);
#69994=ORIENTED_EDGE('',*,*,#50631,.T.);
#69995=ORIENTED_EDGE('',*,*,#50633,.T.);
#69996=ORIENTED_EDGE('',*,*,#50636,.T.);
#69997=ORIENTED_EDGE('',*,*,#50640,.T.);
#69998=ORIENTED_EDGE('',*,*,#50643,.T.);
#69999=ORIENTED_EDGE('',*,*,#50645,.T.);
#70000=ORIENTED_EDGE('',*,*,#50648,.T.);
#70001=ORIENTED_EDGE('',*,*,#50652,.T.);
#70002=ORIENTED_EDGE('',*,*,#50655,.T.);
#70003=ORIENTED_EDGE('',*,*,#50657,.T.);
#70004=ORIENTED_EDGE('',*,*,#50660,.T.);
#70005=ORIENTED_EDGE('',*,*,#50664,.T.);
#70006=ORIENTED_EDGE('',*,*,#50667,.T.);
#70007=ORIENTED_EDGE('',*,*,#50669,.T.);
#70008=ORIENTED_EDGE('',*,*,#50672,.T.);
#70009=ORIENTED_EDGE('',*,*,#50676,.T.);
#70010=ORIENTED_EDGE('',*,*,#50679,.T.);
#70011=ORIENTED_EDGE('',*,*,#50681,.T.);
#70012=ORIENTED_EDGE('',*,*,#50684,.T.);
#70013=ORIENTED_EDGE('',*,*,#50688,.T.);
#70014=ORIENTED_EDGE('',*,*,#50691,.T.);
#70015=ORIENTED_EDGE('',*,*,#50693,.T.);
#70016=ORIENTED_EDGE('',*,*,#50696,.T.);
#70017=ORIENTED_EDGE('',*,*,#50700,.T.);
#70018=ORIENTED_EDGE('',*,*,#50703,.T.);
#70019=ORIENTED_EDGE('',*,*,#50705,.T.);
#70020=ORIENTED_EDGE('',*,*,#50708,.T.);
#70021=ORIENTED_EDGE('',*,*,#50712,.T.);
#70022=ORIENTED_EDGE('',*,*,#50715,.T.);
#70023=ORIENTED_EDGE('',*,*,#50717,.T.);
#70024=ORIENTED_EDGE('',*,*,#50720,.T.);
#70025=ORIENTED_EDGE('',*,*,#50724,.T.);
#70026=ORIENTED_EDGE('',*,*,#50727,.T.);
#70027=ORIENTED_EDGE('',*,*,#50729,.T.);
#70028=ORIENTED_EDGE('',*,*,#50732,.T.);
#70029=ORIENTED_EDGE('',*,*,#50736,.T.);
#70030=ORIENTED_EDGE('',*,*,#50739,.T.);
#70031=ORIENTED_EDGE('',*,*,#50741,.T.);
#70032=ORIENTED_EDGE('',*,*,#50744,.T.);
#70033=ORIENTED_EDGE('',*,*,#50748,.T.);
#70034=ORIENTED_EDGE('',*,*,#50751,.T.);
#70035=ORIENTED_EDGE('',*,*,#50753,.T.);
#70036=ORIENTED_EDGE('',*,*,#50756,.T.);
#70037=ORIENTED_EDGE('',*,*,#50760,.T.);
#70038=ORIENTED_EDGE('',*,*,#50763,.T.);
#70039=ORIENTED_EDGE('',*,*,#50765,.T.);
#70040=ORIENTED_EDGE('',*,*,#50768,.T.);
#70041=ORIENTED_EDGE('',*,*,#50772,.T.);
#70042=ORIENTED_EDGE('',*,*,#50775,.T.);
#70043=ORIENTED_EDGE('',*,*,#50777,.T.);
#70044=ORIENTED_EDGE('',*,*,#50780,.T.);
#70045=ORIENTED_EDGE('',*,*,#50784,.T.);
#70046=ORIENTED_EDGE('',*,*,#50787,.T.);
#70047=ORIENTED_EDGE('',*,*,#50789,.T.);
#70048=ORIENTED_EDGE('',*,*,#50792,.T.);
#70049=ORIENTED_EDGE('',*,*,#50796,.T.);
#70050=ORIENTED_EDGE('',*,*,#50799,.T.);
#70051=ORIENTED_EDGE('',*,*,#50801,.T.);
#70052=ORIENTED_EDGE('',*,*,#50804,.T.);
#70053=ORIENTED_EDGE('',*,*,#50808,.T.);
#70054=ORIENTED_EDGE('',*,*,#50811,.T.);
#70055=ORIENTED_EDGE('',*,*,#50813,.T.);
#70056=ORIENTED_EDGE('',*,*,#50816,.T.);
#70057=ORIENTED_EDGE('',*,*,#50820,.T.);
#70058=ORIENTED_EDGE('',*,*,#50823,.T.);
#70059=ORIENTED_EDGE('',*,*,#50825,.T.);
#70060=ORIENTED_EDGE('',*,*,#50828,.T.);
#70061=ORIENTED_EDGE('',*,*,#50832,.T.);
#70062=ORIENTED_EDGE('',*,*,#50835,.T.);
#70063=ORIENTED_EDGE('',*,*,#50837,.T.);
#70064=ORIENTED_EDGE('',*,*,#50840,.T.);
#70065=ORIENTED_EDGE('',*,*,#50844,.T.);
#70066=ORIENTED_EDGE('',*,*,#50847,.T.);
#70067=ORIENTED_EDGE('',*,*,#50849,.T.);
#70068=ORIENTED_EDGE('',*,*,#50852,.T.);
#70069=ORIENTED_EDGE('',*,*,#50856,.T.);
#70070=ORIENTED_EDGE('',*,*,#50859,.T.);
#70071=ORIENTED_EDGE('',*,*,#50861,.T.);
#70072=ORIENTED_EDGE('',*,*,#50864,.T.);
#70073=ORIENTED_EDGE('',*,*,#50868,.T.);
#70074=ORIENTED_EDGE('',*,*,#50871,.T.);
#70075=ORIENTED_EDGE('',*,*,#50873,.T.);
#70076=ORIENTED_EDGE('',*,*,#50876,.T.);
#70077=ORIENTED_EDGE('',*,*,#50880,.T.);
#70078=ORIENTED_EDGE('',*,*,#50883,.T.);
#70079=ORIENTED_EDGE('',*,*,#50885,.T.);
#70080=ORIENTED_EDGE('',*,*,#50888,.T.);
#70081=ORIENTED_EDGE('',*,*,#50892,.T.);
#70082=ORIENTED_EDGE('',*,*,#50895,.T.);
#70083=ORIENTED_EDGE('',*,*,#50897,.T.);
#70084=ORIENTED_EDGE('',*,*,#50900,.T.);
#70085=ORIENTED_EDGE('',*,*,#50904,.T.);
#70086=ORIENTED_EDGE('',*,*,#50907,.T.);
#70087=ORIENTED_EDGE('',*,*,#50909,.T.);
#70088=ORIENTED_EDGE('',*,*,#50912,.T.);
#70089=ORIENTED_EDGE('',*,*,#50916,.T.);
#70090=ORIENTED_EDGE('',*,*,#50919,.T.);
#70091=ORIENTED_EDGE('',*,*,#50921,.T.);
#70092=ORIENTED_EDGE('',*,*,#50924,.T.);
#70093=ORIENTED_EDGE('',*,*,#50928,.T.);
#70094=ORIENTED_EDGE('',*,*,#50931,.T.);
#70095=ORIENTED_EDGE('',*,*,#50933,.T.);
#70096=ORIENTED_EDGE('',*,*,#50936,.T.);
#70097=ORIENTED_EDGE('',*,*,#50940,.T.);
#70098=ORIENTED_EDGE('',*,*,#50943,.T.);
#70099=ORIENTED_EDGE('',*,*,#50945,.T.);
#70100=ORIENTED_EDGE('',*,*,#50948,.T.);
#70101=ORIENTED_EDGE('',*,*,#50952,.T.);
#70102=ORIENTED_EDGE('',*,*,#50955,.T.);
#70103=ORIENTED_EDGE('',*,*,#50957,.T.);
#70104=ORIENTED_EDGE('',*,*,#50960,.T.);
#70105=ORIENTED_EDGE('',*,*,#50964,.T.);
#70106=ORIENTED_EDGE('',*,*,#50967,.T.);
#70107=ORIENTED_EDGE('',*,*,#50969,.T.);
#70108=ORIENTED_EDGE('',*,*,#50972,.T.);
#70109=ORIENTED_EDGE('',*,*,#50976,.T.);
#70110=ORIENTED_EDGE('',*,*,#50979,.T.);
#70111=ORIENTED_EDGE('',*,*,#50981,.T.);
#70112=ORIENTED_EDGE('',*,*,#50984,.T.);
#70113=ORIENTED_EDGE('',*,*,#50988,.T.);
#70114=ORIENTED_EDGE('',*,*,#50991,.T.);
#70115=ORIENTED_EDGE('',*,*,#50993,.T.);
#70116=ORIENTED_EDGE('',*,*,#50996,.T.);
#70117=ORIENTED_EDGE('',*,*,#51000,.T.);
#70118=ORIENTED_EDGE('',*,*,#51003,.T.);
#70119=ORIENTED_EDGE('',*,*,#51005,.T.);
#70120=ORIENTED_EDGE('',*,*,#51008,.T.);
#70121=ORIENTED_EDGE('',*,*,#51012,.T.);
#70122=ORIENTED_EDGE('',*,*,#51015,.T.);
#70123=ORIENTED_EDGE('',*,*,#51017,.T.);
#70124=ORIENTED_EDGE('',*,*,#51020,.T.);
#70125=ORIENTED_EDGE('',*,*,#51024,.T.);
#70126=ORIENTED_EDGE('',*,*,#51027,.T.);
#70127=ORIENTED_EDGE('',*,*,#51029,.T.);
#70128=ORIENTED_EDGE('',*,*,#51032,.T.);
#70129=ORIENTED_EDGE('',*,*,#51036,.T.);
#70130=ORIENTED_EDGE('',*,*,#51039,.T.);
#70131=ORIENTED_EDGE('',*,*,#51041,.T.);
#70132=ORIENTED_EDGE('',*,*,#51044,.T.);
#70133=ORIENTED_EDGE('',*,*,#51048,.T.);
#70134=ORIENTED_EDGE('',*,*,#51051,.T.);
#70135=ORIENTED_EDGE('',*,*,#51053,.T.);
#70136=ORIENTED_EDGE('',*,*,#51056,.T.);
#70137=ORIENTED_EDGE('',*,*,#51060,.T.);
#70138=ORIENTED_EDGE('',*,*,#51063,.T.);
#70139=ORIENTED_EDGE('',*,*,#51065,.T.);
#70140=ORIENTED_EDGE('',*,*,#51068,.T.);
#70141=ORIENTED_EDGE('',*,*,#51072,.T.);
#70142=ORIENTED_EDGE('',*,*,#51075,.T.);
#70143=ORIENTED_EDGE('',*,*,#51077,.T.);
#70144=ORIENTED_EDGE('',*,*,#51080,.T.);
#70145=ORIENTED_EDGE('',*,*,#51084,.T.);
#70146=ORIENTED_EDGE('',*,*,#51087,.T.);
#70147=ORIENTED_EDGE('',*,*,#51089,.T.);
#70148=ORIENTED_EDGE('',*,*,#51092,.T.);
#70149=ORIENTED_EDGE('',*,*,#51096,.T.);
#70150=ORIENTED_EDGE('',*,*,#51099,.T.);
#70151=ORIENTED_EDGE('',*,*,#51101,.T.);
#70152=ORIENTED_EDGE('',*,*,#51104,.T.);
#70153=ORIENTED_EDGE('',*,*,#51108,.T.);
#70154=ORIENTED_EDGE('',*,*,#51111,.T.);
#70155=ORIENTED_EDGE('',*,*,#51113,.T.);
#70156=ORIENTED_EDGE('',*,*,#51116,.T.);
#70157=ORIENTED_EDGE('',*,*,#51120,.T.);
#70158=ORIENTED_EDGE('',*,*,#51123,.T.);
#70159=ORIENTED_EDGE('',*,*,#51125,.T.);
#70160=ORIENTED_EDGE('',*,*,#51128,.T.);
#70161=ORIENTED_EDGE('',*,*,#51132,.T.);
#70162=ORIENTED_EDGE('',*,*,#51135,.T.);
#70163=ORIENTED_EDGE('',*,*,#51137,.T.);
#70164=ORIENTED_EDGE('',*,*,#51140,.T.);
#70165=ORIENTED_EDGE('',*,*,#51144,.T.);
#70166=ORIENTED_EDGE('',*,*,#51147,.T.);
#70167=ORIENTED_EDGE('',*,*,#51149,.T.);
#70168=ORIENTED_EDGE('',*,*,#51152,.T.);
#70169=ORIENTED_EDGE('',*,*,#51156,.T.);
#70170=ORIENTED_EDGE('',*,*,#51159,.T.);
#70171=ORIENTED_EDGE('',*,*,#51161,.T.);
#70172=ORIENTED_EDGE('',*,*,#51164,.T.);
#70173=ORIENTED_EDGE('',*,*,#51168,.T.);
#70174=ORIENTED_EDGE('',*,*,#51171,.T.);
#70175=ORIENTED_EDGE('',*,*,#51173,.T.);
#70176=ORIENTED_EDGE('',*,*,#51176,.T.);
#70177=ORIENTED_EDGE('',*,*,#51180,.T.);
#70178=ORIENTED_EDGE('',*,*,#51183,.T.);
#70179=ORIENTED_EDGE('',*,*,#51185,.T.);
#70180=ORIENTED_EDGE('',*,*,#51188,.T.);
#70181=ORIENTED_EDGE('',*,*,#51192,.T.);
#70182=ORIENTED_EDGE('',*,*,#51195,.T.);
#70183=ORIENTED_EDGE('',*,*,#51197,.T.);
#70184=ORIENTED_EDGE('',*,*,#51200,.T.);
#70185=ORIENTED_EDGE('',*,*,#51204,.T.);
#70186=ORIENTED_EDGE('',*,*,#51207,.T.);
#70187=ORIENTED_EDGE('',*,*,#51209,.T.);
#70188=ORIENTED_EDGE('',*,*,#51212,.T.);
#70189=ORIENTED_EDGE('',*,*,#51216,.T.);
#70190=ORIENTED_EDGE('',*,*,#51219,.T.);
#70191=ORIENTED_EDGE('',*,*,#51221,.T.);
#70192=ORIENTED_EDGE('',*,*,#51224,.T.);
#70193=ORIENTED_EDGE('',*,*,#51228,.T.);
#70194=ORIENTED_EDGE('',*,*,#51231,.T.);
#70195=ORIENTED_EDGE('',*,*,#51233,.T.);
#70196=ORIENTED_EDGE('',*,*,#51236,.T.);
#70197=ORIENTED_EDGE('',*,*,#51240,.T.);
#70198=ORIENTED_EDGE('',*,*,#51243,.T.);
#70199=ORIENTED_EDGE('',*,*,#51245,.T.);
#70200=ORIENTED_EDGE('',*,*,#51248,.T.);
#70201=ORIENTED_EDGE('',*,*,#51252,.T.);
#70202=ORIENTED_EDGE('',*,*,#51255,.T.);
#70203=ORIENTED_EDGE('',*,*,#51257,.T.);
#70204=ORIENTED_EDGE('',*,*,#51260,.T.);
#70205=ORIENTED_EDGE('',*,*,#51264,.T.);
#70206=ORIENTED_EDGE('',*,*,#51267,.T.);
#70207=ORIENTED_EDGE('',*,*,#51269,.T.);
#70208=ORIENTED_EDGE('',*,*,#51272,.T.);
#70209=ORIENTED_EDGE('',*,*,#51276,.T.);
#70210=ORIENTED_EDGE('',*,*,#51279,.T.);
#70211=ORIENTED_EDGE('',*,*,#51281,.T.);
#70212=ORIENTED_EDGE('',*,*,#51284,.T.);
#70213=ORIENTED_EDGE('',*,*,#51288,.T.);
#70214=ORIENTED_EDGE('',*,*,#51291,.T.);
#70215=ORIENTED_EDGE('',*,*,#51293,.T.);
#70216=ORIENTED_EDGE('',*,*,#51296,.T.);
#70217=ORIENTED_EDGE('',*,*,#51300,.T.);
#70218=ORIENTED_EDGE('',*,*,#51303,.T.);
#70219=ORIENTED_EDGE('',*,*,#51305,.T.);
#70220=ORIENTED_EDGE('',*,*,#51308,.T.);
#70221=ORIENTED_EDGE('',*,*,#51312,.T.);
#70222=ORIENTED_EDGE('',*,*,#51315,.T.);
#70223=ORIENTED_EDGE('',*,*,#51317,.T.);
#70224=ORIENTED_EDGE('',*,*,#51320,.T.);
#70225=ORIENTED_EDGE('',*,*,#51324,.T.);
#70226=ORIENTED_EDGE('',*,*,#51327,.T.);
#70227=ORIENTED_EDGE('',*,*,#51329,.T.);
#70228=ORIENTED_EDGE('',*,*,#51332,.T.);
#70229=ORIENTED_EDGE('',*,*,#51336,.T.);
#70230=ORIENTED_EDGE('',*,*,#51339,.T.);
#70231=ORIENTED_EDGE('',*,*,#51341,.T.);
#70232=ORIENTED_EDGE('',*,*,#51344,.T.);
#70233=ORIENTED_EDGE('',*,*,#51348,.T.);
#70234=ORIENTED_EDGE('',*,*,#51351,.T.);
#70235=ORIENTED_EDGE('',*,*,#51353,.T.);
#70236=ORIENTED_EDGE('',*,*,#51356,.T.);
#70237=ORIENTED_EDGE('',*,*,#51360,.T.);
#70238=ORIENTED_EDGE('',*,*,#51363,.T.);
#70239=ORIENTED_EDGE('',*,*,#51365,.T.);
#70240=ORIENTED_EDGE('',*,*,#51368,.T.);
#70241=ORIENTED_EDGE('',*,*,#51372,.T.);
#70242=ORIENTED_EDGE('',*,*,#51375,.T.);
#70243=ORIENTED_EDGE('',*,*,#51377,.T.);
#70244=ORIENTED_EDGE('',*,*,#51380,.T.);
#70245=ORIENTED_EDGE('',*,*,#51384,.T.);
#70246=ORIENTED_EDGE('',*,*,#51387,.T.);
#70247=ORIENTED_EDGE('',*,*,#51389,.T.);
#70248=ORIENTED_EDGE('',*,*,#51392,.T.);
#70249=ORIENTED_EDGE('',*,*,#51396,.T.);
#70250=ORIENTED_EDGE('',*,*,#51399,.T.);
#70251=ORIENTED_EDGE('',*,*,#51401,.T.);
#70252=ORIENTED_EDGE('',*,*,#51404,.T.);
#70253=ORIENTED_EDGE('',*,*,#51408,.T.);
#70254=ORIENTED_EDGE('',*,*,#51411,.T.);
#70255=ORIENTED_EDGE('',*,*,#51413,.T.);
#70256=ORIENTED_EDGE('',*,*,#51416,.T.);
#70257=ORIENTED_EDGE('',*,*,#51420,.T.);
#70258=ORIENTED_EDGE('',*,*,#51423,.T.);
#70259=ORIENTED_EDGE('',*,*,#51425,.T.);
#70260=ORIENTED_EDGE('',*,*,#51428,.T.);
#70261=ORIENTED_EDGE('',*,*,#51432,.T.);
#70262=ORIENTED_EDGE('',*,*,#51435,.T.);
#70263=ORIENTED_EDGE('',*,*,#51437,.T.);
#70264=ORIENTED_EDGE('',*,*,#51440,.T.);
#70265=ORIENTED_EDGE('',*,*,#51444,.T.);
#70266=ORIENTED_EDGE('',*,*,#51447,.T.);
#70267=ORIENTED_EDGE('',*,*,#51449,.T.);
#70268=ORIENTED_EDGE('',*,*,#51452,.T.);
#70269=ORIENTED_EDGE('',*,*,#51456,.T.);
#70270=ORIENTED_EDGE('',*,*,#51459,.T.);
#70271=ORIENTED_EDGE('',*,*,#51461,.T.);
#70272=ORIENTED_EDGE('',*,*,#51464,.T.);
#70273=ORIENTED_EDGE('',*,*,#51468,.T.);
#70274=ORIENTED_EDGE('',*,*,#51471,.T.);
#70275=ORIENTED_EDGE('',*,*,#51473,.T.);
#70276=ORIENTED_EDGE('',*,*,#51476,.T.);
#70277=ORIENTED_EDGE('',*,*,#51480,.T.);
#70278=ORIENTED_EDGE('',*,*,#51483,.T.);
#70279=ORIENTED_EDGE('',*,*,#51485,.T.);
#70280=ORIENTED_EDGE('',*,*,#51488,.T.);
#70281=ORIENTED_EDGE('',*,*,#51492,.T.);
#70282=ORIENTED_EDGE('',*,*,#51495,.T.);
#70283=ORIENTED_EDGE('',*,*,#51497,.T.);
#70284=ORIENTED_EDGE('',*,*,#51500,.T.);
#70285=ORIENTED_EDGE('',*,*,#51504,.T.);
#70286=ORIENTED_EDGE('',*,*,#51507,.T.);
#70287=ORIENTED_EDGE('',*,*,#51509,.T.);
#70288=ORIENTED_EDGE('',*,*,#51512,.T.);
#70289=ORIENTED_EDGE('',*,*,#51516,.T.);
#70290=ORIENTED_EDGE('',*,*,#51519,.T.);
#70291=ORIENTED_EDGE('',*,*,#51521,.T.);
#70292=ORIENTED_EDGE('',*,*,#51524,.T.);
#70293=ORIENTED_EDGE('',*,*,#51528,.T.);
#70294=ORIENTED_EDGE('',*,*,#51531,.T.);
#70295=ORIENTED_EDGE('',*,*,#51533,.T.);
#70296=ORIENTED_EDGE('',*,*,#51536,.T.);
#70297=ORIENTED_EDGE('',*,*,#51540,.T.);
#70298=ORIENTED_EDGE('',*,*,#51543,.T.);
#70299=ORIENTED_EDGE('',*,*,#51545,.T.);
#70300=ORIENTED_EDGE('',*,*,#51548,.T.);
#70301=ORIENTED_EDGE('',*,*,#51552,.T.);
#70302=ORIENTED_EDGE('',*,*,#51555,.T.);
#70303=ORIENTED_EDGE('',*,*,#51557,.T.);
#70304=ORIENTED_EDGE('',*,*,#51560,.T.);
#70305=ORIENTED_EDGE('',*,*,#51564,.T.);
#70306=ORIENTED_EDGE('',*,*,#51567,.T.);
#70307=ORIENTED_EDGE('',*,*,#51569,.T.);
#70308=ORIENTED_EDGE('',*,*,#51572,.T.);
#70309=ORIENTED_EDGE('',*,*,#51576,.T.);
#70310=ORIENTED_EDGE('',*,*,#51579,.T.);
#70311=ORIENTED_EDGE('',*,*,#51581,.T.);
#70312=ORIENTED_EDGE('',*,*,#51584,.T.);
#70313=ORIENTED_EDGE('',*,*,#51588,.T.);
#70314=ORIENTED_EDGE('',*,*,#51591,.T.);
#70315=ORIENTED_EDGE('',*,*,#51593,.T.);
#70316=ORIENTED_EDGE('',*,*,#51596,.T.);
#70317=ORIENTED_EDGE('',*,*,#51600,.T.);
#70318=ORIENTED_EDGE('',*,*,#51603,.T.);
#70319=ORIENTED_EDGE('',*,*,#51605,.T.);
#70320=ORIENTED_EDGE('',*,*,#51608,.T.);
#70321=ORIENTED_EDGE('',*,*,#51612,.T.);
#70322=ORIENTED_EDGE('',*,*,#51615,.T.);
#70323=ORIENTED_EDGE('',*,*,#51617,.T.);
#70324=ORIENTED_EDGE('',*,*,#51620,.T.);
#70325=ORIENTED_EDGE('',*,*,#51624,.T.);
#70326=ORIENTED_EDGE('',*,*,#51627,.T.);
#70327=ORIENTED_EDGE('',*,*,#51629,.T.);
#70328=ORIENTED_EDGE('',*,*,#51632,.T.);
#70329=ORIENTED_EDGE('',*,*,#51636,.T.);
#70330=ORIENTED_EDGE('',*,*,#51639,.T.);
#70331=ORIENTED_EDGE('',*,*,#51641,.T.);
#70332=ORIENTED_EDGE('',*,*,#51644,.T.);
#70333=ORIENTED_EDGE('',*,*,#51648,.T.);
#70334=ORIENTED_EDGE('',*,*,#51651,.T.);
#70335=ORIENTED_EDGE('',*,*,#51653,.T.);
#70336=ORIENTED_EDGE('',*,*,#51656,.T.);
#70337=ORIENTED_EDGE('',*,*,#51660,.T.);
#70338=ORIENTED_EDGE('',*,*,#51663,.T.);
#70339=ORIENTED_EDGE('',*,*,#51665,.T.);
#70340=ORIENTED_EDGE('',*,*,#51668,.T.);
#70341=ORIENTED_EDGE('',*,*,#51672,.T.);
#70342=ORIENTED_EDGE('',*,*,#51675,.T.);
#70343=ORIENTED_EDGE('',*,*,#51677,.T.);
#70344=ORIENTED_EDGE('',*,*,#51680,.T.);
#70345=ORIENTED_EDGE('',*,*,#51684,.T.);
#70346=ORIENTED_EDGE('',*,*,#51687,.T.);
#70347=ORIENTED_EDGE('',*,*,#51689,.T.);
#70348=ORIENTED_EDGE('',*,*,#51692,.T.);
#70349=ORIENTED_EDGE('',*,*,#51696,.T.);
#70350=ORIENTED_EDGE('',*,*,#51699,.T.);
#70351=ORIENTED_EDGE('',*,*,#51701,.T.);
#70352=ORIENTED_EDGE('',*,*,#51704,.T.);
#70353=ORIENTED_EDGE('',*,*,#51708,.T.);
#70354=ORIENTED_EDGE('',*,*,#51711,.T.);
#70355=ORIENTED_EDGE('',*,*,#51713,.T.);
#70356=ORIENTED_EDGE('',*,*,#51716,.T.);
#70357=ORIENTED_EDGE('',*,*,#51720,.T.);
#70358=ORIENTED_EDGE('',*,*,#51723,.T.);
#70359=ORIENTED_EDGE('',*,*,#51725,.T.);
#70360=ORIENTED_EDGE('',*,*,#51728,.T.);
#70361=ORIENTED_EDGE('',*,*,#51732,.T.);
#70362=ORIENTED_EDGE('',*,*,#51735,.T.);
#70363=ORIENTED_EDGE('',*,*,#51737,.T.);
#70364=ORIENTED_EDGE('',*,*,#51740,.T.);
#70365=ORIENTED_EDGE('',*,*,#51744,.T.);
#70366=ORIENTED_EDGE('',*,*,#51747,.T.);
#70367=ORIENTED_EDGE('',*,*,#51749,.T.);
#70368=ORIENTED_EDGE('',*,*,#51752,.T.);
#70369=ORIENTED_EDGE('',*,*,#51756,.T.);
#70370=ORIENTED_EDGE('',*,*,#51759,.T.);
#70371=ORIENTED_EDGE('',*,*,#51761,.T.);
#70372=ORIENTED_EDGE('',*,*,#51764,.T.);
#70373=ORIENTED_EDGE('',*,*,#51768,.T.);
#70374=ORIENTED_EDGE('',*,*,#51771,.T.);
#70375=ORIENTED_EDGE('',*,*,#51773,.T.);
#70376=ORIENTED_EDGE('',*,*,#51776,.T.);
#70377=ORIENTED_EDGE('',*,*,#51780,.T.);
#70378=ORIENTED_EDGE('',*,*,#51783,.T.);
#70379=ORIENTED_EDGE('',*,*,#51785,.T.);
#70380=ORIENTED_EDGE('',*,*,#51788,.T.);
#70381=ORIENTED_EDGE('',*,*,#51792,.T.);
#70382=ORIENTED_EDGE('',*,*,#51795,.T.);
#70383=ORIENTED_EDGE('',*,*,#51797,.T.);
#70384=ORIENTED_EDGE('',*,*,#51800,.T.);
#70385=ORIENTED_EDGE('',*,*,#51804,.T.);
#70386=ORIENTED_EDGE('',*,*,#51807,.T.);
#70387=ORIENTED_EDGE('',*,*,#51809,.T.);
#70388=ORIENTED_EDGE('',*,*,#51812,.T.);
#70389=ORIENTED_EDGE('',*,*,#51816,.T.);
#70390=ORIENTED_EDGE('',*,*,#51819,.T.);
#70391=ORIENTED_EDGE('',*,*,#51821,.T.);
#70392=ORIENTED_EDGE('',*,*,#51824,.T.);
#70393=ORIENTED_EDGE('',*,*,#51828,.T.);
#70394=ORIENTED_EDGE('',*,*,#51831,.T.);
#70395=ORIENTED_EDGE('',*,*,#51833,.T.);
#70396=ORIENTED_EDGE('',*,*,#51836,.T.);
#70397=ORIENTED_EDGE('',*,*,#51840,.T.);
#70398=ORIENTED_EDGE('',*,*,#51843,.T.);
#70399=ORIENTED_EDGE('',*,*,#51845,.T.);
#70400=ORIENTED_EDGE('',*,*,#51848,.T.);
#70401=ORIENTED_EDGE('',*,*,#51852,.T.);
#70402=ORIENTED_EDGE('',*,*,#51855,.T.);
#70403=ORIENTED_EDGE('',*,*,#51857,.T.);
#70404=ORIENTED_EDGE('',*,*,#51860,.T.);
#70405=ORIENTED_EDGE('',*,*,#51864,.T.);
#70406=ORIENTED_EDGE('',*,*,#51867,.T.);
#70407=ORIENTED_EDGE('',*,*,#51869,.T.);
#70408=ORIENTED_EDGE('',*,*,#51872,.T.);
#70409=ORIENTED_EDGE('',*,*,#51876,.T.);
#70410=ORIENTED_EDGE('',*,*,#51879,.T.);
#70411=ORIENTED_EDGE('',*,*,#51881,.T.);
#70412=ORIENTED_EDGE('',*,*,#51884,.T.);
#70413=ORIENTED_EDGE('',*,*,#51888,.T.);
#70414=ORIENTED_EDGE('',*,*,#51891,.T.);
#70415=ORIENTED_EDGE('',*,*,#51893,.T.);
#70416=ORIENTED_EDGE('',*,*,#51896,.T.);
#70417=ORIENTED_EDGE('',*,*,#51900,.T.);
#70418=ORIENTED_EDGE('',*,*,#51903,.T.);
#70419=ORIENTED_EDGE('',*,*,#51905,.T.);
#70420=ORIENTED_EDGE('',*,*,#51908,.T.);
#70421=ORIENTED_EDGE('',*,*,#51912,.T.);
#70422=ORIENTED_EDGE('',*,*,#51915,.T.);
#70423=ORIENTED_EDGE('',*,*,#51917,.T.);
#70424=ORIENTED_EDGE('',*,*,#51920,.T.);
#70425=ORIENTED_EDGE('',*,*,#51924,.T.);
#70426=ORIENTED_EDGE('',*,*,#51927,.T.);
#70427=ORIENTED_EDGE('',*,*,#51929,.T.);
#70428=ORIENTED_EDGE('',*,*,#51932,.T.);
#70429=ORIENTED_EDGE('',*,*,#51936,.T.);
#70430=ORIENTED_EDGE('',*,*,#51939,.T.);
#70431=ORIENTED_EDGE('',*,*,#51941,.T.);
#70432=ORIENTED_EDGE('',*,*,#51944,.T.);
#70433=ORIENTED_EDGE('',*,*,#51948,.T.);
#70434=ORIENTED_EDGE('',*,*,#51951,.T.);
#70435=ORIENTED_EDGE('',*,*,#51953,.T.);
#70436=ORIENTED_EDGE('',*,*,#51956,.T.);
#70437=ORIENTED_EDGE('',*,*,#51960,.T.);
#70438=ORIENTED_EDGE('',*,*,#51963,.T.);
#70439=ORIENTED_EDGE('',*,*,#51965,.T.);
#70440=ORIENTED_EDGE('',*,*,#51967,.T.);
#70441=ORIENTED_EDGE('',*,*,#51968,.T.);
#70442=ORIENTED_EDGE('',*,*,#51969,.T.);
#70443=ORIENTED_EDGE('',*,*,#51970,.T.);
#70444=ORIENTED_EDGE('',*,*,#51971,.T.);
#70445=ORIENTED_EDGE('',*,*,#51967,.F.);
#70446=ORIENTED_EDGE('',*,*,#51972,.F.);
#70447=ORIENTED_EDGE('',*,*,#51973,.T.);
#70448=ORIENTED_EDGE('',*,*,#51974,.T.);
#70449=ORIENTED_EDGE('',*,*,#51968,.F.);
#70450=ORIENTED_EDGE('',*,*,#51971,.F.);
#70451=ORIENTED_EDGE('',*,*,#51975,.T.);
#70452=ORIENTED_EDGE('',*,*,#51976,.T.);
#70453=ORIENTED_EDGE('',*,*,#51969,.F.);
#70454=ORIENTED_EDGE('',*,*,#51974,.F.);
#70455=ORIENTED_EDGE('',*,*,#51977,.T.);
#70456=ORIENTED_EDGE('',*,*,#51972,.T.);
#70457=ORIENTED_EDGE('',*,*,#51970,.F.);
#70458=ORIENTED_EDGE('',*,*,#51976,.F.);
#70459=ORIENTED_EDGE('',*,*,#51978,.T.);
#70460=ORIENTED_EDGE('',*,*,#43493,.F.);
#70461=ORIENTED_EDGE('',*,*,#46744,.F.);
#70462=ORIENTED_EDGE('',*,*,#46741,.F.);
#70463=ORIENTED_EDGE('',*,*,#46738,.F.);
#70464=ORIENTED_EDGE('',*,*,#46746,.F.);
#70465=ORIENTED_EDGE('',*,*,#46756,.F.);
#70466=ORIENTED_EDGE('',*,*,#46753,.F.);
#70467=ORIENTED_EDGE('',*,*,#46750,.F.);
#70468=ORIENTED_EDGE('',*,*,#46758,.F.);
#70469=ORIENTED_EDGE('',*,*,#46768,.F.);
#70470=ORIENTED_EDGE('',*,*,#46765,.F.);
#70471=ORIENTED_EDGE('',*,*,#46762,.F.);
#70472=ORIENTED_EDGE('',*,*,#46770,.F.);
#70473=ORIENTED_EDGE('',*,*,#46780,.F.);
#70474=ORIENTED_EDGE('',*,*,#46777,.F.);
#70475=ORIENTED_EDGE('',*,*,#46774,.F.);
#70476=ORIENTED_EDGE('',*,*,#46782,.F.);
#70477=ORIENTED_EDGE('',*,*,#46792,.F.);
#70478=ORIENTED_EDGE('',*,*,#46789,.F.);
#70479=ORIENTED_EDGE('',*,*,#46786,.F.);
#70480=ORIENTED_EDGE('',*,*,#46794,.F.);
#70481=ORIENTED_EDGE('',*,*,#46804,.F.);
#70482=ORIENTED_EDGE('',*,*,#46801,.F.);
#70483=ORIENTED_EDGE('',*,*,#46798,.F.);
#70484=ORIENTED_EDGE('',*,*,#46806,.F.);
#70485=ORIENTED_EDGE('',*,*,#46816,.F.);
#70486=ORIENTED_EDGE('',*,*,#46813,.F.);
#70487=ORIENTED_EDGE('',*,*,#46810,.F.);
#70488=ORIENTED_EDGE('',*,*,#46818,.F.);
#70489=ORIENTED_EDGE('',*,*,#46828,.F.);
#70490=ORIENTED_EDGE('',*,*,#46825,.F.);
#70491=ORIENTED_EDGE('',*,*,#46822,.F.);
#70492=ORIENTED_EDGE('',*,*,#46830,.F.);
#70493=ORIENTED_EDGE('',*,*,#46840,.F.);
#70494=ORIENTED_EDGE('',*,*,#46837,.F.);
#70495=ORIENTED_EDGE('',*,*,#46834,.F.);
#70496=ORIENTED_EDGE('',*,*,#46842,.F.);
#70497=ORIENTED_EDGE('',*,*,#46852,.F.);
#70498=ORIENTED_EDGE('',*,*,#46849,.F.);
#70499=ORIENTED_EDGE('',*,*,#46846,.F.);
#70500=ORIENTED_EDGE('',*,*,#46854,.F.);
#70501=ORIENTED_EDGE('',*,*,#46864,.F.);
#70502=ORIENTED_EDGE('',*,*,#46861,.F.);
#70503=ORIENTED_EDGE('',*,*,#46858,.F.);
#70504=ORIENTED_EDGE('',*,*,#46866,.F.);
#70505=ORIENTED_EDGE('',*,*,#46876,.F.);
#70506=ORIENTED_EDGE('',*,*,#46873,.F.);
#70507=ORIENTED_EDGE('',*,*,#46870,.F.);
#70508=ORIENTED_EDGE('',*,*,#46878,.F.);
#70509=ORIENTED_EDGE('',*,*,#46888,.F.);
#70510=ORIENTED_EDGE('',*,*,#46885,.F.);
#70511=ORIENTED_EDGE('',*,*,#46882,.F.);
#70512=ORIENTED_EDGE('',*,*,#46890,.F.);
#70513=ORIENTED_EDGE('',*,*,#46900,.F.);
#70514=ORIENTED_EDGE('',*,*,#46897,.F.);
#70515=ORIENTED_EDGE('',*,*,#46894,.F.);
#70516=ORIENTED_EDGE('',*,*,#46902,.F.);
#70517=ORIENTED_EDGE('',*,*,#46912,.F.);
#70518=ORIENTED_EDGE('',*,*,#46909,.F.);
#70519=ORIENTED_EDGE('',*,*,#46906,.F.);
#70520=ORIENTED_EDGE('',*,*,#46914,.F.);
#70521=ORIENTED_EDGE('',*,*,#46924,.F.);
#70522=ORIENTED_EDGE('',*,*,#46921,.F.);
#70523=ORIENTED_EDGE('',*,*,#46918,.F.);
#70524=ORIENTED_EDGE('',*,*,#46926,.F.);
#70525=ORIENTED_EDGE('',*,*,#46936,.F.);
#70526=ORIENTED_EDGE('',*,*,#46933,.F.);
#70527=ORIENTED_EDGE('',*,*,#46930,.F.);
#70528=ORIENTED_EDGE('',*,*,#46938,.F.);
#70529=ORIENTED_EDGE('',*,*,#46948,.F.);
#70530=ORIENTED_EDGE('',*,*,#46945,.F.);
#70531=ORIENTED_EDGE('',*,*,#46942,.F.);
#70532=ORIENTED_EDGE('',*,*,#46950,.F.);
#70533=ORIENTED_EDGE('',*,*,#46960,.F.);
#70534=ORIENTED_EDGE('',*,*,#46957,.F.);
#70535=ORIENTED_EDGE('',*,*,#46954,.F.);
#70536=ORIENTED_EDGE('',*,*,#46962,.F.);
#70537=ORIENTED_EDGE('',*,*,#46972,.F.);
#70538=ORIENTED_EDGE('',*,*,#46969,.F.);
#70539=ORIENTED_EDGE('',*,*,#46966,.F.);
#70540=ORIENTED_EDGE('',*,*,#46974,.F.);
#70541=ORIENTED_EDGE('',*,*,#46984,.F.);
#70542=ORIENTED_EDGE('',*,*,#46981,.F.);
#70543=ORIENTED_EDGE('',*,*,#46978,.F.);
#70544=ORIENTED_EDGE('',*,*,#46986,.F.);
#70545=ORIENTED_EDGE('',*,*,#46996,.F.);
#70546=ORIENTED_EDGE('',*,*,#46993,.F.);
#70547=ORIENTED_EDGE('',*,*,#46990,.F.);
#70548=ORIENTED_EDGE('',*,*,#46998,.F.);
#70549=ORIENTED_EDGE('',*,*,#47008,.F.);
#70550=ORIENTED_EDGE('',*,*,#47005,.F.);
#70551=ORIENTED_EDGE('',*,*,#47002,.F.);
#70552=ORIENTED_EDGE('',*,*,#47010,.F.);
#70553=ORIENTED_EDGE('',*,*,#47020,.F.);
#70554=ORIENTED_EDGE('',*,*,#47017,.F.);
#70555=ORIENTED_EDGE('',*,*,#47014,.F.);
#70556=ORIENTED_EDGE('',*,*,#47022,.F.);
#70557=ORIENTED_EDGE('',*,*,#47032,.F.);
#70558=ORIENTED_EDGE('',*,*,#47029,.F.);
#70559=ORIENTED_EDGE('',*,*,#47026,.F.);
#70560=ORIENTED_EDGE('',*,*,#47034,.F.);
#70561=ORIENTED_EDGE('',*,*,#47044,.F.);
#70562=ORIENTED_EDGE('',*,*,#47041,.F.);
#70563=ORIENTED_EDGE('',*,*,#47038,.F.);
#70564=ORIENTED_EDGE('',*,*,#47046,.F.);
#70565=ORIENTED_EDGE('',*,*,#47056,.F.);
#70566=ORIENTED_EDGE('',*,*,#47053,.F.);
#70567=ORIENTED_EDGE('',*,*,#47050,.F.);
#70568=ORIENTED_EDGE('',*,*,#47058,.F.);
#70569=ORIENTED_EDGE('',*,*,#47068,.F.);
#70570=ORIENTED_EDGE('',*,*,#47065,.F.);
#70571=ORIENTED_EDGE('',*,*,#47062,.F.);
#70572=ORIENTED_EDGE('',*,*,#47070,.F.);
#70573=ORIENTED_EDGE('',*,*,#47080,.F.);
#70574=ORIENTED_EDGE('',*,*,#47077,.F.);
#70575=ORIENTED_EDGE('',*,*,#47074,.F.);
#70576=ORIENTED_EDGE('',*,*,#47082,.F.);
#70577=ORIENTED_EDGE('',*,*,#47092,.F.);
#70578=ORIENTED_EDGE('',*,*,#47089,.F.);
#70579=ORIENTED_EDGE('',*,*,#47086,.F.);
#70580=ORIENTED_EDGE('',*,*,#47094,.F.);
#70581=ORIENTED_EDGE('',*,*,#47104,.F.);
#70582=ORIENTED_EDGE('',*,*,#47101,.F.);
#70583=ORIENTED_EDGE('',*,*,#47098,.F.);
#70584=ORIENTED_EDGE('',*,*,#47106,.F.);
#70585=ORIENTED_EDGE('',*,*,#47116,.F.);
#70586=ORIENTED_EDGE('',*,*,#47113,.F.);
#70587=ORIENTED_EDGE('',*,*,#47110,.F.);
#70588=ORIENTED_EDGE('',*,*,#47118,.F.);
#70589=ORIENTED_EDGE('',*,*,#47128,.F.);
#70590=ORIENTED_EDGE('',*,*,#47125,.F.);
#70591=ORIENTED_EDGE('',*,*,#47122,.F.);
#70592=ORIENTED_EDGE('',*,*,#47130,.F.);
#70593=ORIENTED_EDGE('',*,*,#47140,.F.);
#70594=ORIENTED_EDGE('',*,*,#47137,.F.);
#70595=ORIENTED_EDGE('',*,*,#47134,.F.);
#70596=ORIENTED_EDGE('',*,*,#47142,.F.);
#70597=ORIENTED_EDGE('',*,*,#47152,.F.);
#70598=ORIENTED_EDGE('',*,*,#47149,.F.);
#70599=ORIENTED_EDGE('',*,*,#47146,.F.);
#70600=ORIENTED_EDGE('',*,*,#47154,.F.);
#70601=ORIENTED_EDGE('',*,*,#47164,.F.);
#70602=ORIENTED_EDGE('',*,*,#47161,.F.);
#70603=ORIENTED_EDGE('',*,*,#47158,.F.);
#70604=ORIENTED_EDGE('',*,*,#47166,.F.);
#70605=ORIENTED_EDGE('',*,*,#47176,.F.);
#70606=ORIENTED_EDGE('',*,*,#47173,.F.);
#70607=ORIENTED_EDGE('',*,*,#47170,.F.);
#70608=ORIENTED_EDGE('',*,*,#47178,.F.);
#70609=ORIENTED_EDGE('',*,*,#47188,.F.);
#70610=ORIENTED_EDGE('',*,*,#47185,.F.);
#70611=ORIENTED_EDGE('',*,*,#47182,.F.);
#70612=ORIENTED_EDGE('',*,*,#47190,.F.);
#70613=ORIENTED_EDGE('',*,*,#47200,.F.);
#70614=ORIENTED_EDGE('',*,*,#47197,.F.);
#70615=ORIENTED_EDGE('',*,*,#47194,.F.);
#70616=ORIENTED_EDGE('',*,*,#47202,.F.);
#70617=ORIENTED_EDGE('',*,*,#47212,.F.);
#70618=ORIENTED_EDGE('',*,*,#47209,.F.);
#70619=ORIENTED_EDGE('',*,*,#47206,.F.);
#70620=ORIENTED_EDGE('',*,*,#47214,.F.);
#70621=ORIENTED_EDGE('',*,*,#47224,.F.);
#70622=ORIENTED_EDGE('',*,*,#47221,.F.);
#70623=ORIENTED_EDGE('',*,*,#47218,.F.);
#70624=ORIENTED_EDGE('',*,*,#47226,.F.);
#70625=ORIENTED_EDGE('',*,*,#47236,.F.);
#70626=ORIENTED_EDGE('',*,*,#47233,.F.);
#70627=ORIENTED_EDGE('',*,*,#47230,.F.);
#70628=ORIENTED_EDGE('',*,*,#47238,.F.);
#70629=ORIENTED_EDGE('',*,*,#47248,.F.);
#70630=ORIENTED_EDGE('',*,*,#47245,.F.);
#70631=ORIENTED_EDGE('',*,*,#47242,.F.);
#70632=ORIENTED_EDGE('',*,*,#47250,.F.);
#70633=ORIENTED_EDGE('',*,*,#47260,.F.);
#70634=ORIENTED_EDGE('',*,*,#47257,.F.);
#70635=ORIENTED_EDGE('',*,*,#47254,.F.);
#70636=ORIENTED_EDGE('',*,*,#47262,.F.);
#70637=ORIENTED_EDGE('',*,*,#47272,.F.);
#70638=ORIENTED_EDGE('',*,*,#47269,.F.);
#70639=ORIENTED_EDGE('',*,*,#47266,.F.);
#70640=ORIENTED_EDGE('',*,*,#47274,.F.);
#70641=ORIENTED_EDGE('',*,*,#47284,.F.);
#70642=ORIENTED_EDGE('',*,*,#47281,.F.);
#70643=ORIENTED_EDGE('',*,*,#47278,.F.);
#70644=ORIENTED_EDGE('',*,*,#47286,.F.);
#70645=ORIENTED_EDGE('',*,*,#47296,.F.);
#70646=ORIENTED_EDGE('',*,*,#47293,.F.);
#70647=ORIENTED_EDGE('',*,*,#47290,.F.);
#70648=ORIENTED_EDGE('',*,*,#47298,.F.);
#70649=ORIENTED_EDGE('',*,*,#47308,.F.);
#70650=ORIENTED_EDGE('',*,*,#47305,.F.);
#70651=ORIENTED_EDGE('',*,*,#47302,.F.);
#70652=ORIENTED_EDGE('',*,*,#47310,.F.);
#70653=ORIENTED_EDGE('',*,*,#47320,.F.);
#70654=ORIENTED_EDGE('',*,*,#47317,.F.);
#70655=ORIENTED_EDGE('',*,*,#47314,.F.);
#70656=ORIENTED_EDGE('',*,*,#47322,.F.);
#70657=ORIENTED_EDGE('',*,*,#47332,.F.);
#70658=ORIENTED_EDGE('',*,*,#47329,.F.);
#70659=ORIENTED_EDGE('',*,*,#47326,.F.);
#70660=ORIENTED_EDGE('',*,*,#47334,.F.);
#70661=ORIENTED_EDGE('',*,*,#47344,.F.);
#70662=ORIENTED_EDGE('',*,*,#47341,.F.);
#70663=ORIENTED_EDGE('',*,*,#47338,.F.);
#70664=ORIENTED_EDGE('',*,*,#47346,.F.);
#70665=ORIENTED_EDGE('',*,*,#47356,.F.);
#70666=ORIENTED_EDGE('',*,*,#47353,.F.);
#70667=ORIENTED_EDGE('',*,*,#47350,.F.);
#70668=ORIENTED_EDGE('',*,*,#47358,.F.);
#70669=ORIENTED_EDGE('',*,*,#47368,.F.);
#70670=ORIENTED_EDGE('',*,*,#47365,.F.);
#70671=ORIENTED_EDGE('',*,*,#47362,.F.);
#70672=ORIENTED_EDGE('',*,*,#47370,.F.);
#70673=ORIENTED_EDGE('',*,*,#47380,.F.);
#70674=ORIENTED_EDGE('',*,*,#47377,.F.);
#70675=ORIENTED_EDGE('',*,*,#47374,.F.);
#70676=ORIENTED_EDGE('',*,*,#47382,.F.);
#70677=ORIENTED_EDGE('',*,*,#47392,.F.);
#70678=ORIENTED_EDGE('',*,*,#47389,.F.);
#70679=ORIENTED_EDGE('',*,*,#47386,.F.);
#70680=ORIENTED_EDGE('',*,*,#47394,.F.);
#70681=ORIENTED_EDGE('',*,*,#47404,.F.);
#70682=ORIENTED_EDGE('',*,*,#47401,.F.);
#70683=ORIENTED_EDGE('',*,*,#47398,.F.);
#70684=ORIENTED_EDGE('',*,*,#47406,.F.);
#70685=ORIENTED_EDGE('',*,*,#47416,.F.);
#70686=ORIENTED_EDGE('',*,*,#47413,.F.);
#70687=ORIENTED_EDGE('',*,*,#47410,.F.);
#70688=ORIENTED_EDGE('',*,*,#47418,.F.);
#70689=ORIENTED_EDGE('',*,*,#47428,.F.);
#70690=ORIENTED_EDGE('',*,*,#47425,.F.);
#70691=ORIENTED_EDGE('',*,*,#47422,.F.);
#70692=ORIENTED_EDGE('',*,*,#47430,.F.);
#70693=ORIENTED_EDGE('',*,*,#47440,.F.);
#70694=ORIENTED_EDGE('',*,*,#47437,.F.);
#70695=ORIENTED_EDGE('',*,*,#47434,.F.);
#70696=ORIENTED_EDGE('',*,*,#47442,.F.);
#70697=ORIENTED_EDGE('',*,*,#47452,.F.);
#70698=ORIENTED_EDGE('',*,*,#47449,.F.);
#70699=ORIENTED_EDGE('',*,*,#47446,.F.);
#70700=ORIENTED_EDGE('',*,*,#47454,.F.);
#70701=ORIENTED_EDGE('',*,*,#47464,.F.);
#70702=ORIENTED_EDGE('',*,*,#47461,.F.);
#70703=ORIENTED_EDGE('',*,*,#47458,.F.);
#70704=ORIENTED_EDGE('',*,*,#47466,.F.);
#70705=ORIENTED_EDGE('',*,*,#47476,.F.);
#70706=ORIENTED_EDGE('',*,*,#47473,.F.);
#70707=ORIENTED_EDGE('',*,*,#47470,.F.);
#70708=ORIENTED_EDGE('',*,*,#47478,.F.);
#70709=ORIENTED_EDGE('',*,*,#47488,.F.);
#70710=ORIENTED_EDGE('',*,*,#47485,.F.);
#70711=ORIENTED_EDGE('',*,*,#47482,.F.);
#70712=ORIENTED_EDGE('',*,*,#47490,.F.);
#70713=ORIENTED_EDGE('',*,*,#47500,.F.);
#70714=ORIENTED_EDGE('',*,*,#47497,.F.);
#70715=ORIENTED_EDGE('',*,*,#47494,.F.);
#70716=ORIENTED_EDGE('',*,*,#47502,.F.);
#70717=ORIENTED_EDGE('',*,*,#47512,.F.);
#70718=ORIENTED_EDGE('',*,*,#47509,.F.);
#70719=ORIENTED_EDGE('',*,*,#47506,.F.);
#70720=ORIENTED_EDGE('',*,*,#47514,.F.);
#70721=ORIENTED_EDGE('',*,*,#47524,.F.);
#70722=ORIENTED_EDGE('',*,*,#47521,.F.);
#70723=ORIENTED_EDGE('',*,*,#47518,.F.);
#70724=ORIENTED_EDGE('',*,*,#47526,.F.);
#70725=ORIENTED_EDGE('',*,*,#47536,.F.);
#70726=ORIENTED_EDGE('',*,*,#47533,.F.);
#70727=ORIENTED_EDGE('',*,*,#47530,.F.);
#70728=ORIENTED_EDGE('',*,*,#47538,.F.);
#70729=ORIENTED_EDGE('',*,*,#47548,.F.);
#70730=ORIENTED_EDGE('',*,*,#47545,.F.);
#70731=ORIENTED_EDGE('',*,*,#47542,.F.);
#70732=ORIENTED_EDGE('',*,*,#47550,.F.);
#70733=ORIENTED_EDGE('',*,*,#47560,.F.);
#70734=ORIENTED_EDGE('',*,*,#47557,.F.);
#70735=ORIENTED_EDGE('',*,*,#47554,.F.);
#70736=ORIENTED_EDGE('',*,*,#47562,.F.);
#70737=ORIENTED_EDGE('',*,*,#47572,.F.);
#70738=ORIENTED_EDGE('',*,*,#47569,.F.);
#70739=ORIENTED_EDGE('',*,*,#47566,.F.);
#70740=ORIENTED_EDGE('',*,*,#47574,.F.);
#70741=ORIENTED_EDGE('',*,*,#47584,.F.);
#70742=ORIENTED_EDGE('',*,*,#47581,.F.);
#70743=ORIENTED_EDGE('',*,*,#47578,.F.);
#70744=ORIENTED_EDGE('',*,*,#47586,.F.);
#70745=ORIENTED_EDGE('',*,*,#47596,.F.);
#70746=ORIENTED_EDGE('',*,*,#47593,.F.);
#70747=ORIENTED_EDGE('',*,*,#47590,.F.);
#70748=ORIENTED_EDGE('',*,*,#47598,.F.);
#70749=ORIENTED_EDGE('',*,*,#47608,.F.);
#70750=ORIENTED_EDGE('',*,*,#47605,.F.);
#70751=ORIENTED_EDGE('',*,*,#47602,.F.);
#70752=ORIENTED_EDGE('',*,*,#47610,.F.);
#70753=ORIENTED_EDGE('',*,*,#47620,.F.);
#70754=ORIENTED_EDGE('',*,*,#47617,.F.);
#70755=ORIENTED_EDGE('',*,*,#47614,.F.);
#70756=ORIENTED_EDGE('',*,*,#47622,.F.);
#70757=ORIENTED_EDGE('',*,*,#47632,.F.);
#70758=ORIENTED_EDGE('',*,*,#47629,.F.);
#70759=ORIENTED_EDGE('',*,*,#47626,.F.);
#70760=ORIENTED_EDGE('',*,*,#47634,.F.);
#70761=ORIENTED_EDGE('',*,*,#47644,.F.);
#70762=ORIENTED_EDGE('',*,*,#47641,.F.);
#70763=ORIENTED_EDGE('',*,*,#47638,.F.);
#70764=ORIENTED_EDGE('',*,*,#47646,.F.);
#70765=ORIENTED_EDGE('',*,*,#47656,.F.);
#70766=ORIENTED_EDGE('',*,*,#47653,.F.);
#70767=ORIENTED_EDGE('',*,*,#47650,.F.);
#70768=ORIENTED_EDGE('',*,*,#47658,.F.);
#70769=ORIENTED_EDGE('',*,*,#47668,.F.);
#70770=ORIENTED_EDGE('',*,*,#47665,.F.);
#70771=ORIENTED_EDGE('',*,*,#47662,.F.);
#70772=ORIENTED_EDGE('',*,*,#47670,.F.);
#70773=ORIENTED_EDGE('',*,*,#47680,.F.);
#70774=ORIENTED_EDGE('',*,*,#47677,.F.);
#70775=ORIENTED_EDGE('',*,*,#47674,.F.);
#70776=ORIENTED_EDGE('',*,*,#47682,.F.);
#70777=ORIENTED_EDGE('',*,*,#47692,.F.);
#70778=ORIENTED_EDGE('',*,*,#47689,.F.);
#70779=ORIENTED_EDGE('',*,*,#47686,.F.);
#70780=ORIENTED_EDGE('',*,*,#47694,.F.);
#70781=ORIENTED_EDGE('',*,*,#47704,.F.);
#70782=ORIENTED_EDGE('',*,*,#47701,.F.);
#70783=ORIENTED_EDGE('',*,*,#47698,.F.);
#70784=ORIENTED_EDGE('',*,*,#47706,.F.);
#70785=ORIENTED_EDGE('',*,*,#47716,.F.);
#70786=ORIENTED_EDGE('',*,*,#47713,.F.);
#70787=ORIENTED_EDGE('',*,*,#47710,.F.);
#70788=ORIENTED_EDGE('',*,*,#47718,.F.);
#70789=ORIENTED_EDGE('',*,*,#47728,.F.);
#70790=ORIENTED_EDGE('',*,*,#47725,.F.);
#70791=ORIENTED_EDGE('',*,*,#47722,.F.);
#70792=ORIENTED_EDGE('',*,*,#47730,.F.);
#70793=ORIENTED_EDGE('',*,*,#47740,.F.);
#70794=ORIENTED_EDGE('',*,*,#47737,.F.);
#70795=ORIENTED_EDGE('',*,*,#47734,.F.);
#70796=ORIENTED_EDGE('',*,*,#47742,.F.);
#70797=ORIENTED_EDGE('',*,*,#47752,.F.);
#70798=ORIENTED_EDGE('',*,*,#47749,.F.);
#70799=ORIENTED_EDGE('',*,*,#47746,.F.);
#70800=ORIENTED_EDGE('',*,*,#47754,.F.);
#70801=ORIENTED_EDGE('',*,*,#47764,.F.);
#70802=ORIENTED_EDGE('',*,*,#47761,.F.);
#70803=ORIENTED_EDGE('',*,*,#47758,.F.);
#70804=ORIENTED_EDGE('',*,*,#47766,.F.);
#70805=ORIENTED_EDGE('',*,*,#47776,.F.);
#70806=ORIENTED_EDGE('',*,*,#47773,.F.);
#70807=ORIENTED_EDGE('',*,*,#47770,.F.);
#70808=ORIENTED_EDGE('',*,*,#47778,.F.);
#70809=ORIENTED_EDGE('',*,*,#47788,.F.);
#70810=ORIENTED_EDGE('',*,*,#47785,.F.);
#70811=ORIENTED_EDGE('',*,*,#47782,.F.);
#70812=ORIENTED_EDGE('',*,*,#47790,.F.);
#70813=ORIENTED_EDGE('',*,*,#47800,.F.);
#70814=ORIENTED_EDGE('',*,*,#47797,.F.);
#70815=ORIENTED_EDGE('',*,*,#47794,.F.);
#70816=ORIENTED_EDGE('',*,*,#47802,.F.);
#70817=ORIENTED_EDGE('',*,*,#47812,.F.);
#70818=ORIENTED_EDGE('',*,*,#47809,.F.);
#70819=ORIENTED_EDGE('',*,*,#47806,.F.);
#70820=ORIENTED_EDGE('',*,*,#47814,.F.);
#70821=ORIENTED_EDGE('',*,*,#47824,.F.);
#70822=ORIENTED_EDGE('',*,*,#47821,.F.);
#70823=ORIENTED_EDGE('',*,*,#47818,.F.);
#70824=ORIENTED_EDGE('',*,*,#47826,.F.);
#70825=ORIENTED_EDGE('',*,*,#47836,.F.);
#70826=ORIENTED_EDGE('',*,*,#47833,.F.);
#70827=ORIENTED_EDGE('',*,*,#47830,.F.);
#70828=ORIENTED_EDGE('',*,*,#47838,.F.);
#70829=ORIENTED_EDGE('',*,*,#47848,.F.);
#70830=ORIENTED_EDGE('',*,*,#47845,.F.);
#70831=ORIENTED_EDGE('',*,*,#47842,.F.);
#70832=ORIENTED_EDGE('',*,*,#47850,.F.);
#70833=ORIENTED_EDGE('',*,*,#47860,.F.);
#70834=ORIENTED_EDGE('',*,*,#47857,.F.);
#70835=ORIENTED_EDGE('',*,*,#47854,.F.);
#70836=ORIENTED_EDGE('',*,*,#47862,.F.);
#70837=ORIENTED_EDGE('',*,*,#47872,.F.);
#70838=ORIENTED_EDGE('',*,*,#47869,.F.);
#70839=ORIENTED_EDGE('',*,*,#47866,.F.);
#70840=ORIENTED_EDGE('',*,*,#47874,.F.);
#70841=ORIENTED_EDGE('',*,*,#47884,.F.);
#70842=ORIENTED_EDGE('',*,*,#47881,.F.);
#70843=ORIENTED_EDGE('',*,*,#47878,.F.);
#70844=ORIENTED_EDGE('',*,*,#47886,.F.);
#70845=ORIENTED_EDGE('',*,*,#47896,.F.);
#70846=ORIENTED_EDGE('',*,*,#47893,.F.);
#70847=ORIENTED_EDGE('',*,*,#47890,.F.);
#70848=ORIENTED_EDGE('',*,*,#47898,.F.);
#70849=ORIENTED_EDGE('',*,*,#47908,.F.);
#70850=ORIENTED_EDGE('',*,*,#47905,.F.);
#70851=ORIENTED_EDGE('',*,*,#47902,.F.);
#70852=ORIENTED_EDGE('',*,*,#47910,.F.);
#70853=ORIENTED_EDGE('',*,*,#47920,.F.);
#70854=ORIENTED_EDGE('',*,*,#47917,.F.);
#70855=ORIENTED_EDGE('',*,*,#47914,.F.);
#70856=ORIENTED_EDGE('',*,*,#47922,.F.);
#70857=ORIENTED_EDGE('',*,*,#47932,.F.);
#70858=ORIENTED_EDGE('',*,*,#47929,.F.);
#70859=ORIENTED_EDGE('',*,*,#47926,.F.);
#70860=ORIENTED_EDGE('',*,*,#47934,.F.);
#70861=ORIENTED_EDGE('',*,*,#47944,.F.);
#70862=ORIENTED_EDGE('',*,*,#47941,.F.);
#70863=ORIENTED_EDGE('',*,*,#47938,.F.);
#70864=ORIENTED_EDGE('',*,*,#47946,.F.);
#70865=ORIENTED_EDGE('',*,*,#47956,.F.);
#70866=ORIENTED_EDGE('',*,*,#47953,.F.);
#70867=ORIENTED_EDGE('',*,*,#47950,.F.);
#70868=ORIENTED_EDGE('',*,*,#47958,.F.);
#70869=ORIENTED_EDGE('',*,*,#47968,.F.);
#70870=ORIENTED_EDGE('',*,*,#47965,.F.);
#70871=ORIENTED_EDGE('',*,*,#47962,.F.);
#70872=ORIENTED_EDGE('',*,*,#47970,.F.);
#70873=ORIENTED_EDGE('',*,*,#47980,.F.);
#70874=ORIENTED_EDGE('',*,*,#47977,.F.);
#70875=ORIENTED_EDGE('',*,*,#47974,.F.);
#70876=ORIENTED_EDGE('',*,*,#47982,.F.);
#70877=ORIENTED_EDGE('',*,*,#47992,.F.);
#70878=ORIENTED_EDGE('',*,*,#47989,.F.);
#70879=ORIENTED_EDGE('',*,*,#47986,.F.);
#70880=ORIENTED_EDGE('',*,*,#47994,.F.);
#70881=ORIENTED_EDGE('',*,*,#48004,.F.);
#70882=ORIENTED_EDGE('',*,*,#48001,.F.);
#70883=ORIENTED_EDGE('',*,*,#47998,.F.);
#70884=ORIENTED_EDGE('',*,*,#48006,.F.);
#70885=ORIENTED_EDGE('',*,*,#48016,.F.);
#70886=ORIENTED_EDGE('',*,*,#48013,.F.);
#70887=ORIENTED_EDGE('',*,*,#48010,.F.);
#70888=ORIENTED_EDGE('',*,*,#48018,.F.);
#70889=ORIENTED_EDGE('',*,*,#48028,.F.);
#70890=ORIENTED_EDGE('',*,*,#48025,.F.);
#70891=ORIENTED_EDGE('',*,*,#48022,.F.);
#70892=ORIENTED_EDGE('',*,*,#48030,.F.);
#70893=ORIENTED_EDGE('',*,*,#48040,.F.);
#70894=ORIENTED_EDGE('',*,*,#48037,.F.);
#70895=ORIENTED_EDGE('',*,*,#48034,.F.);
#70896=ORIENTED_EDGE('',*,*,#48042,.F.);
#70897=ORIENTED_EDGE('',*,*,#48052,.F.);
#70898=ORIENTED_EDGE('',*,*,#48049,.F.);
#70899=ORIENTED_EDGE('',*,*,#48046,.F.);
#70900=ORIENTED_EDGE('',*,*,#48054,.F.);
#70901=ORIENTED_EDGE('',*,*,#48064,.F.);
#70902=ORIENTED_EDGE('',*,*,#48061,.F.);
#70903=ORIENTED_EDGE('',*,*,#48058,.F.);
#70904=ORIENTED_EDGE('',*,*,#48066,.F.);
#70905=ORIENTED_EDGE('',*,*,#48076,.F.);
#70906=ORIENTED_EDGE('',*,*,#48073,.F.);
#70907=ORIENTED_EDGE('',*,*,#48070,.F.);
#70908=ORIENTED_EDGE('',*,*,#48078,.F.);
#70909=ORIENTED_EDGE('',*,*,#48088,.F.);
#70910=ORIENTED_EDGE('',*,*,#48085,.F.);
#70911=ORIENTED_EDGE('',*,*,#48082,.F.);
#70912=ORIENTED_EDGE('',*,*,#48090,.F.);
#70913=ORIENTED_EDGE('',*,*,#48100,.F.);
#70914=ORIENTED_EDGE('',*,*,#48097,.F.);
#70915=ORIENTED_EDGE('',*,*,#48094,.F.);
#70916=ORIENTED_EDGE('',*,*,#48102,.F.);
#70917=ORIENTED_EDGE('',*,*,#48112,.F.);
#70918=ORIENTED_EDGE('',*,*,#48109,.F.);
#70919=ORIENTED_EDGE('',*,*,#48106,.F.);
#70920=ORIENTED_EDGE('',*,*,#48114,.F.);
#70921=ORIENTED_EDGE('',*,*,#48124,.F.);
#70922=ORIENTED_EDGE('',*,*,#48121,.F.);
#70923=ORIENTED_EDGE('',*,*,#48118,.F.);
#70924=ORIENTED_EDGE('',*,*,#48126,.F.);
#70925=ORIENTED_EDGE('',*,*,#48136,.F.);
#70926=ORIENTED_EDGE('',*,*,#48133,.F.);
#70927=ORIENTED_EDGE('',*,*,#48130,.F.);
#70928=ORIENTED_EDGE('',*,*,#48138,.F.);
#70929=ORIENTED_EDGE('',*,*,#48148,.F.);
#70930=ORIENTED_EDGE('',*,*,#48145,.F.);
#70931=ORIENTED_EDGE('',*,*,#48142,.F.);
#70932=ORIENTED_EDGE('',*,*,#48150,.F.);
#70933=ORIENTED_EDGE('',*,*,#48160,.F.);
#70934=ORIENTED_EDGE('',*,*,#48157,.F.);
#70935=ORIENTED_EDGE('',*,*,#48154,.F.);
#70936=ORIENTED_EDGE('',*,*,#48162,.F.);
#70937=ORIENTED_EDGE('',*,*,#48172,.F.);
#70938=ORIENTED_EDGE('',*,*,#48169,.F.);
#70939=ORIENTED_EDGE('',*,*,#48166,.F.);
#70940=ORIENTED_EDGE('',*,*,#48174,.F.);
#70941=ORIENTED_EDGE('',*,*,#48184,.F.);
#70942=ORIENTED_EDGE('',*,*,#48181,.F.);
#70943=ORIENTED_EDGE('',*,*,#48178,.F.);
#70944=ORIENTED_EDGE('',*,*,#48186,.F.);
#70945=ORIENTED_EDGE('',*,*,#48196,.F.);
#70946=ORIENTED_EDGE('',*,*,#48193,.F.);
#70947=ORIENTED_EDGE('',*,*,#48190,.F.);
#70948=ORIENTED_EDGE('',*,*,#48198,.F.);
#70949=ORIENTED_EDGE('',*,*,#48208,.F.);
#70950=ORIENTED_EDGE('',*,*,#48205,.F.);
#70951=ORIENTED_EDGE('',*,*,#48202,.F.);
#70952=ORIENTED_EDGE('',*,*,#48210,.F.);
#70953=ORIENTED_EDGE('',*,*,#48220,.F.);
#70954=ORIENTED_EDGE('',*,*,#48217,.F.);
#70955=ORIENTED_EDGE('',*,*,#48214,.F.);
#70956=ORIENTED_EDGE('',*,*,#48222,.F.);
#70957=ORIENTED_EDGE('',*,*,#48232,.F.);
#70958=ORIENTED_EDGE('',*,*,#48229,.F.);
#70959=ORIENTED_EDGE('',*,*,#48226,.F.);
#70960=ORIENTED_EDGE('',*,*,#48234,.F.);
#70961=ORIENTED_EDGE('',*,*,#48244,.F.);
#70962=ORIENTED_EDGE('',*,*,#48241,.F.);
#70963=ORIENTED_EDGE('',*,*,#48238,.F.);
#70964=ORIENTED_EDGE('',*,*,#48246,.F.);
#70965=ORIENTED_EDGE('',*,*,#48256,.F.);
#70966=ORIENTED_EDGE('',*,*,#48253,.F.);
#70967=ORIENTED_EDGE('',*,*,#48250,.F.);
#70968=ORIENTED_EDGE('',*,*,#48258,.F.);
#70969=ORIENTED_EDGE('',*,*,#48268,.F.);
#70970=ORIENTED_EDGE('',*,*,#48265,.F.);
#70971=ORIENTED_EDGE('',*,*,#48262,.F.);
#70972=ORIENTED_EDGE('',*,*,#48270,.F.);
#70973=ORIENTED_EDGE('',*,*,#48280,.F.);
#70974=ORIENTED_EDGE('',*,*,#48277,.F.);
#70975=ORIENTED_EDGE('',*,*,#48274,.F.);
#70976=ORIENTED_EDGE('',*,*,#48282,.F.);
#70977=ORIENTED_EDGE('',*,*,#48292,.F.);
#70978=ORIENTED_EDGE('',*,*,#48289,.F.);
#70979=ORIENTED_EDGE('',*,*,#48286,.F.);
#70980=ORIENTED_EDGE('',*,*,#48294,.F.);
#70981=ORIENTED_EDGE('',*,*,#48304,.F.);
#70982=ORIENTED_EDGE('',*,*,#48301,.F.);
#70983=ORIENTED_EDGE('',*,*,#48298,.F.);
#70984=ORIENTED_EDGE('',*,*,#48306,.F.);
#70985=ORIENTED_EDGE('',*,*,#48316,.F.);
#70986=ORIENTED_EDGE('',*,*,#48313,.F.);
#70987=ORIENTED_EDGE('',*,*,#48310,.F.);
#70988=ORIENTED_EDGE('',*,*,#48318,.F.);
#70989=ORIENTED_EDGE('',*,*,#48328,.F.);
#70990=ORIENTED_EDGE('',*,*,#48325,.F.);
#70991=ORIENTED_EDGE('',*,*,#48322,.F.);
#70992=ORIENTED_EDGE('',*,*,#48330,.F.);
#70993=ORIENTED_EDGE('',*,*,#48340,.F.);
#70994=ORIENTED_EDGE('',*,*,#48337,.F.);
#70995=ORIENTED_EDGE('',*,*,#48334,.F.);
#70996=ORIENTED_EDGE('',*,*,#48342,.F.);
#70997=ORIENTED_EDGE('',*,*,#48352,.F.);
#70998=ORIENTED_EDGE('',*,*,#48349,.F.);
#70999=ORIENTED_EDGE('',*,*,#48346,.F.);
#71000=ORIENTED_EDGE('',*,*,#48354,.F.);
#71001=ORIENTED_EDGE('',*,*,#48364,.F.);
#71002=ORIENTED_EDGE('',*,*,#48361,.F.);
#71003=ORIENTED_EDGE('',*,*,#48358,.F.);
#71004=ORIENTED_EDGE('',*,*,#48366,.F.);
#71005=ORIENTED_EDGE('',*,*,#48376,.F.);
#71006=ORIENTED_EDGE('',*,*,#48373,.F.);
#71007=ORIENTED_EDGE('',*,*,#48370,.F.);
#71008=ORIENTED_EDGE('',*,*,#48378,.F.);
#71009=ORIENTED_EDGE('',*,*,#48388,.F.);
#71010=ORIENTED_EDGE('',*,*,#48385,.F.);
#71011=ORIENTED_EDGE('',*,*,#48382,.F.);
#71012=ORIENTED_EDGE('',*,*,#48390,.F.);
#71013=ORIENTED_EDGE('',*,*,#48400,.F.);
#71014=ORIENTED_EDGE('',*,*,#48397,.F.);
#71015=ORIENTED_EDGE('',*,*,#48394,.F.);
#71016=ORIENTED_EDGE('',*,*,#48402,.F.);
#71017=ORIENTED_EDGE('',*,*,#48412,.F.);
#71018=ORIENTED_EDGE('',*,*,#48409,.F.);
#71019=ORIENTED_EDGE('',*,*,#48406,.F.);
#71020=ORIENTED_EDGE('',*,*,#48414,.F.);
#71021=ORIENTED_EDGE('',*,*,#48424,.F.);
#71022=ORIENTED_EDGE('',*,*,#48421,.F.);
#71023=ORIENTED_EDGE('',*,*,#48418,.F.);
#71024=ORIENTED_EDGE('',*,*,#48426,.F.);
#71025=ORIENTED_EDGE('',*,*,#48436,.F.);
#71026=ORIENTED_EDGE('',*,*,#48433,.F.);
#71027=ORIENTED_EDGE('',*,*,#48430,.F.);
#71028=ORIENTED_EDGE('',*,*,#48438,.F.);
#71029=ORIENTED_EDGE('',*,*,#48448,.F.);
#71030=ORIENTED_EDGE('',*,*,#48445,.F.);
#71031=ORIENTED_EDGE('',*,*,#48442,.F.);
#71032=ORIENTED_EDGE('',*,*,#48450,.F.);
#71033=ORIENTED_EDGE('',*,*,#48460,.F.);
#71034=ORIENTED_EDGE('',*,*,#48457,.F.);
#71035=ORIENTED_EDGE('',*,*,#48454,.F.);
#71036=ORIENTED_EDGE('',*,*,#48462,.F.);
#71037=ORIENTED_EDGE('',*,*,#48472,.F.);
#71038=ORIENTED_EDGE('',*,*,#48469,.F.);
#71039=ORIENTED_EDGE('',*,*,#48466,.F.);
#71040=ORIENTED_EDGE('',*,*,#48474,.F.);
#71041=ORIENTED_EDGE('',*,*,#48484,.F.);
#71042=ORIENTED_EDGE('',*,*,#48481,.F.);
#71043=ORIENTED_EDGE('',*,*,#48478,.F.);
#71044=ORIENTED_EDGE('',*,*,#48486,.F.);
#71045=ORIENTED_EDGE('',*,*,#48496,.F.);
#71046=ORIENTED_EDGE('',*,*,#48493,.F.);
#71047=ORIENTED_EDGE('',*,*,#48490,.F.);
#71048=ORIENTED_EDGE('',*,*,#48498,.F.);
#71049=ORIENTED_EDGE('',*,*,#48508,.F.);
#71050=ORIENTED_EDGE('',*,*,#48505,.F.);
#71051=ORIENTED_EDGE('',*,*,#48502,.F.);
#71052=ORIENTED_EDGE('',*,*,#48510,.F.);
#71053=ORIENTED_EDGE('',*,*,#48520,.F.);
#71054=ORIENTED_EDGE('',*,*,#48517,.F.);
#71055=ORIENTED_EDGE('',*,*,#48514,.F.);
#71056=ORIENTED_EDGE('',*,*,#48522,.F.);
#71057=ORIENTED_EDGE('',*,*,#48532,.F.);
#71058=ORIENTED_EDGE('',*,*,#48529,.F.);
#71059=ORIENTED_EDGE('',*,*,#48526,.F.);
#71060=ORIENTED_EDGE('',*,*,#48534,.F.);
#71061=ORIENTED_EDGE('',*,*,#48544,.F.);
#71062=ORIENTED_EDGE('',*,*,#48541,.F.);
#71063=ORIENTED_EDGE('',*,*,#48538,.F.);
#71064=ORIENTED_EDGE('',*,*,#48546,.F.);
#71065=ORIENTED_EDGE('',*,*,#48556,.F.);
#71066=ORIENTED_EDGE('',*,*,#48553,.F.);
#71067=ORIENTED_EDGE('',*,*,#48550,.F.);
#71068=ORIENTED_EDGE('',*,*,#48558,.F.);
#71069=ORIENTED_EDGE('',*,*,#48568,.F.);
#71070=ORIENTED_EDGE('',*,*,#48565,.F.);
#71071=ORIENTED_EDGE('',*,*,#48562,.F.);
#71072=ORIENTED_EDGE('',*,*,#48570,.F.);
#71073=ORIENTED_EDGE('',*,*,#48580,.F.);
#71074=ORIENTED_EDGE('',*,*,#48577,.F.);
#71075=ORIENTED_EDGE('',*,*,#48574,.F.);
#71076=ORIENTED_EDGE('',*,*,#48582,.F.);
#71077=ORIENTED_EDGE('',*,*,#48592,.F.);
#71078=ORIENTED_EDGE('',*,*,#48589,.F.);
#71079=ORIENTED_EDGE('',*,*,#48586,.F.);
#71080=ORIENTED_EDGE('',*,*,#48594,.F.);
#71081=ORIENTED_EDGE('',*,*,#48604,.F.);
#71082=ORIENTED_EDGE('',*,*,#48601,.F.);
#71083=ORIENTED_EDGE('',*,*,#48598,.F.);
#71084=ORIENTED_EDGE('',*,*,#48606,.F.);
#71085=ORIENTED_EDGE('',*,*,#48616,.F.);
#71086=ORIENTED_EDGE('',*,*,#48613,.F.);
#71087=ORIENTED_EDGE('',*,*,#48610,.F.);
#71088=ORIENTED_EDGE('',*,*,#48618,.F.);
#71089=ORIENTED_EDGE('',*,*,#48628,.F.);
#71090=ORIENTED_EDGE('',*,*,#48625,.F.);
#71091=ORIENTED_EDGE('',*,*,#48622,.F.);
#71092=ORIENTED_EDGE('',*,*,#48630,.F.);
#71093=ORIENTED_EDGE('',*,*,#48640,.F.);
#71094=ORIENTED_EDGE('',*,*,#48637,.F.);
#71095=ORIENTED_EDGE('',*,*,#48634,.F.);
#71096=ORIENTED_EDGE('',*,*,#48642,.F.);
#71097=ORIENTED_EDGE('',*,*,#48652,.F.);
#71098=ORIENTED_EDGE('',*,*,#48649,.F.);
#71099=ORIENTED_EDGE('',*,*,#48646,.F.);
#71100=ORIENTED_EDGE('',*,*,#48654,.F.);
#71101=ORIENTED_EDGE('',*,*,#48664,.F.);
#71102=ORIENTED_EDGE('',*,*,#48661,.F.);
#71103=ORIENTED_EDGE('',*,*,#48658,.F.);
#71104=ORIENTED_EDGE('',*,*,#48666,.F.);
#71105=ORIENTED_EDGE('',*,*,#48676,.F.);
#71106=ORIENTED_EDGE('',*,*,#48673,.F.);
#71107=ORIENTED_EDGE('',*,*,#48670,.F.);
#71108=ORIENTED_EDGE('',*,*,#48678,.F.);
#71109=ORIENTED_EDGE('',*,*,#48688,.F.);
#71110=ORIENTED_EDGE('',*,*,#48685,.F.);
#71111=ORIENTED_EDGE('',*,*,#48682,.F.);
#71112=ORIENTED_EDGE('',*,*,#48690,.F.);
#71113=ORIENTED_EDGE('',*,*,#48700,.F.);
#71114=ORIENTED_EDGE('',*,*,#48697,.F.);
#71115=ORIENTED_EDGE('',*,*,#48694,.F.);
#71116=ORIENTED_EDGE('',*,*,#48702,.F.);
#71117=ORIENTED_EDGE('',*,*,#48712,.F.);
#71118=ORIENTED_EDGE('',*,*,#48709,.F.);
#71119=ORIENTED_EDGE('',*,*,#48706,.F.);
#71120=ORIENTED_EDGE('',*,*,#48714,.F.);
#71121=ORIENTED_EDGE('',*,*,#48724,.F.);
#71122=ORIENTED_EDGE('',*,*,#48721,.F.);
#71123=ORIENTED_EDGE('',*,*,#48718,.F.);
#71124=ORIENTED_EDGE('',*,*,#48726,.F.);
#71125=ORIENTED_EDGE('',*,*,#48736,.F.);
#71126=ORIENTED_EDGE('',*,*,#48733,.F.);
#71127=ORIENTED_EDGE('',*,*,#48730,.F.);
#71128=ORIENTED_EDGE('',*,*,#48738,.F.);
#71129=ORIENTED_EDGE('',*,*,#48748,.F.);
#71130=ORIENTED_EDGE('',*,*,#48745,.F.);
#71131=ORIENTED_EDGE('',*,*,#48742,.F.);
#71132=ORIENTED_EDGE('',*,*,#48750,.F.);
#71133=ORIENTED_EDGE('',*,*,#48760,.F.);
#71134=ORIENTED_EDGE('',*,*,#48757,.F.);
#71135=ORIENTED_EDGE('',*,*,#48754,.F.);
#71136=ORIENTED_EDGE('',*,*,#48762,.F.);
#71137=ORIENTED_EDGE('',*,*,#48772,.F.);
#71138=ORIENTED_EDGE('',*,*,#48769,.F.);
#71139=ORIENTED_EDGE('',*,*,#48766,.F.);
#71140=ORIENTED_EDGE('',*,*,#48774,.F.);
#71141=ORIENTED_EDGE('',*,*,#48784,.F.);
#71142=ORIENTED_EDGE('',*,*,#48781,.F.);
#71143=ORIENTED_EDGE('',*,*,#48778,.F.);
#71144=ORIENTED_EDGE('',*,*,#48786,.F.);
#71145=ORIENTED_EDGE('',*,*,#48796,.F.);
#71146=ORIENTED_EDGE('',*,*,#48793,.F.);
#71147=ORIENTED_EDGE('',*,*,#48790,.F.);
#71148=ORIENTED_EDGE('',*,*,#48798,.F.);
#71149=ORIENTED_EDGE('',*,*,#48808,.F.);
#71150=ORIENTED_EDGE('',*,*,#48805,.F.);
#71151=ORIENTED_EDGE('',*,*,#48802,.F.);
#71152=ORIENTED_EDGE('',*,*,#48810,.F.);
#71153=ORIENTED_EDGE('',*,*,#48820,.F.);
#71154=ORIENTED_EDGE('',*,*,#48817,.F.);
#71155=ORIENTED_EDGE('',*,*,#48814,.F.);
#71156=ORIENTED_EDGE('',*,*,#48822,.F.);
#71157=ORIENTED_EDGE('',*,*,#48832,.F.);
#71158=ORIENTED_EDGE('',*,*,#48829,.F.);
#71159=ORIENTED_EDGE('',*,*,#48826,.F.);
#71160=ORIENTED_EDGE('',*,*,#48834,.F.);
#71161=ORIENTED_EDGE('',*,*,#48844,.F.);
#71162=ORIENTED_EDGE('',*,*,#48841,.F.);
#71163=ORIENTED_EDGE('',*,*,#48838,.F.);
#71164=ORIENTED_EDGE('',*,*,#48846,.F.);
#71165=ORIENTED_EDGE('',*,*,#48856,.F.);
#71166=ORIENTED_EDGE('',*,*,#48853,.F.);
#71167=ORIENTED_EDGE('',*,*,#48850,.F.);
#71168=ORIENTED_EDGE('',*,*,#48858,.F.);
#71169=ORIENTED_EDGE('',*,*,#48868,.F.);
#71170=ORIENTED_EDGE('',*,*,#48865,.F.);
#71171=ORIENTED_EDGE('',*,*,#48862,.F.);
#71172=ORIENTED_EDGE('',*,*,#48870,.F.);
#71173=ORIENTED_EDGE('',*,*,#48880,.F.);
#71174=ORIENTED_EDGE('',*,*,#48877,.F.);
#71175=ORIENTED_EDGE('',*,*,#48874,.F.);
#71176=ORIENTED_EDGE('',*,*,#48882,.F.);
#71177=ORIENTED_EDGE('',*,*,#48892,.F.);
#71178=ORIENTED_EDGE('',*,*,#48889,.F.);
#71179=ORIENTED_EDGE('',*,*,#48886,.F.);
#71180=ORIENTED_EDGE('',*,*,#48894,.F.);
#71181=ORIENTED_EDGE('',*,*,#48904,.F.);
#71182=ORIENTED_EDGE('',*,*,#48901,.F.);
#71183=ORIENTED_EDGE('',*,*,#48898,.F.);
#71184=ORIENTED_EDGE('',*,*,#48906,.F.);
#71185=ORIENTED_EDGE('',*,*,#48916,.F.);
#71186=ORIENTED_EDGE('',*,*,#48913,.F.);
#71187=ORIENTED_EDGE('',*,*,#48910,.F.);
#71188=ORIENTED_EDGE('',*,*,#48918,.F.);
#71189=ORIENTED_EDGE('',*,*,#48928,.F.);
#71190=ORIENTED_EDGE('',*,*,#48925,.F.);
#71191=ORIENTED_EDGE('',*,*,#48922,.F.);
#71192=ORIENTED_EDGE('',*,*,#48930,.F.);
#71193=ORIENTED_EDGE('',*,*,#48940,.F.);
#71194=ORIENTED_EDGE('',*,*,#48937,.F.);
#71195=ORIENTED_EDGE('',*,*,#48934,.F.);
#71196=ORIENTED_EDGE('',*,*,#48942,.F.);
#71197=ORIENTED_EDGE('',*,*,#48952,.F.);
#71198=ORIENTED_EDGE('',*,*,#48949,.F.);
#71199=ORIENTED_EDGE('',*,*,#48946,.F.);
#71200=ORIENTED_EDGE('',*,*,#48954,.F.);
#71201=ORIENTED_EDGE('',*,*,#48964,.F.);
#71202=ORIENTED_EDGE('',*,*,#48961,.F.);
#71203=ORIENTED_EDGE('',*,*,#48958,.F.);
#71204=ORIENTED_EDGE('',*,*,#48966,.F.);
#71205=ORIENTED_EDGE('',*,*,#48976,.F.);
#71206=ORIENTED_EDGE('',*,*,#48973,.F.);
#71207=ORIENTED_EDGE('',*,*,#48970,.F.);
#71208=ORIENTED_EDGE('',*,*,#48978,.F.);
#71209=ORIENTED_EDGE('',*,*,#48988,.F.);
#71210=ORIENTED_EDGE('',*,*,#48985,.F.);
#71211=ORIENTED_EDGE('',*,*,#48982,.F.);
#71212=ORIENTED_EDGE('',*,*,#48990,.F.);
#71213=ORIENTED_EDGE('',*,*,#49000,.F.);
#71214=ORIENTED_EDGE('',*,*,#48997,.F.);
#71215=ORIENTED_EDGE('',*,*,#48994,.F.);
#71216=ORIENTED_EDGE('',*,*,#49002,.F.);
#71217=ORIENTED_EDGE('',*,*,#49012,.F.);
#71218=ORIENTED_EDGE('',*,*,#49009,.F.);
#71219=ORIENTED_EDGE('',*,*,#49006,.F.);
#71220=ORIENTED_EDGE('',*,*,#49014,.F.);
#71221=ORIENTED_EDGE('',*,*,#49024,.F.);
#71222=ORIENTED_EDGE('',*,*,#49021,.F.);
#71223=ORIENTED_EDGE('',*,*,#49018,.F.);
#71224=ORIENTED_EDGE('',*,*,#49026,.F.);
#71225=ORIENTED_EDGE('',*,*,#49036,.F.);
#71226=ORIENTED_EDGE('',*,*,#49033,.F.);
#71227=ORIENTED_EDGE('',*,*,#49030,.F.);
#71228=ORIENTED_EDGE('',*,*,#49038,.F.);
#71229=ORIENTED_EDGE('',*,*,#49048,.F.);
#71230=ORIENTED_EDGE('',*,*,#49045,.F.);
#71231=ORIENTED_EDGE('',*,*,#49042,.F.);
#71232=ORIENTED_EDGE('',*,*,#49050,.F.);
#71233=ORIENTED_EDGE('',*,*,#49060,.F.);
#71234=ORIENTED_EDGE('',*,*,#49057,.F.);
#71235=ORIENTED_EDGE('',*,*,#49054,.F.);
#71236=ORIENTED_EDGE('',*,*,#49062,.F.);
#71237=ORIENTED_EDGE('',*,*,#49072,.F.);
#71238=ORIENTED_EDGE('',*,*,#49069,.F.);
#71239=ORIENTED_EDGE('',*,*,#49066,.F.);
#71240=ORIENTED_EDGE('',*,*,#49074,.F.);
#71241=ORIENTED_EDGE('',*,*,#49084,.F.);
#71242=ORIENTED_EDGE('',*,*,#49081,.F.);
#71243=ORIENTED_EDGE('',*,*,#49078,.F.);
#71244=ORIENTED_EDGE('',*,*,#49086,.F.);
#71245=ORIENTED_EDGE('',*,*,#49096,.F.);
#71246=ORIENTED_EDGE('',*,*,#49093,.F.);
#71247=ORIENTED_EDGE('',*,*,#49090,.F.);
#71248=ORIENTED_EDGE('',*,*,#49098,.F.);
#71249=ORIENTED_EDGE('',*,*,#49108,.F.);
#71250=ORIENTED_EDGE('',*,*,#49105,.F.);
#71251=ORIENTED_EDGE('',*,*,#49102,.F.);
#71252=ORIENTED_EDGE('',*,*,#49110,.F.);
#71253=ORIENTED_EDGE('',*,*,#49120,.F.);
#71254=ORIENTED_EDGE('',*,*,#49117,.F.);
#71255=ORIENTED_EDGE('',*,*,#49114,.F.);
#71256=ORIENTED_EDGE('',*,*,#49122,.F.);
#71257=ORIENTED_EDGE('',*,*,#49132,.F.);
#71258=ORIENTED_EDGE('',*,*,#49129,.F.);
#71259=ORIENTED_EDGE('',*,*,#49126,.F.);
#71260=ORIENTED_EDGE('',*,*,#49134,.F.);
#71261=ORIENTED_EDGE('',*,*,#49144,.F.);
#71262=ORIENTED_EDGE('',*,*,#49141,.F.);
#71263=ORIENTED_EDGE('',*,*,#49138,.F.);
#71264=ORIENTED_EDGE('',*,*,#49146,.F.);
#71265=ORIENTED_EDGE('',*,*,#49156,.F.);
#71266=ORIENTED_EDGE('',*,*,#49153,.F.);
#71267=ORIENTED_EDGE('',*,*,#49150,.F.);
#71268=ORIENTED_EDGE('',*,*,#49158,.F.);
#71269=ORIENTED_EDGE('',*,*,#49168,.F.);
#71270=ORIENTED_EDGE('',*,*,#49165,.F.);
#71271=ORIENTED_EDGE('',*,*,#49162,.F.);
#71272=ORIENTED_EDGE('',*,*,#49170,.F.);
#71273=ORIENTED_EDGE('',*,*,#49180,.F.);
#71274=ORIENTED_EDGE('',*,*,#49177,.F.);
#71275=ORIENTED_EDGE('',*,*,#49174,.F.);
#71276=ORIENTED_EDGE('',*,*,#49182,.F.);
#71277=ORIENTED_EDGE('',*,*,#49192,.F.);
#71278=ORIENTED_EDGE('',*,*,#49189,.F.);
#71279=ORIENTED_EDGE('',*,*,#49186,.F.);
#71280=ORIENTED_EDGE('',*,*,#49194,.F.);
#71281=ORIENTED_EDGE('',*,*,#49204,.F.);
#71282=ORIENTED_EDGE('',*,*,#49201,.F.);
#71283=ORIENTED_EDGE('',*,*,#49198,.F.);
#71284=ORIENTED_EDGE('',*,*,#49206,.F.);
#71285=ORIENTED_EDGE('',*,*,#49216,.F.);
#71286=ORIENTED_EDGE('',*,*,#49213,.F.);
#71287=ORIENTED_EDGE('',*,*,#49210,.F.);
#71288=ORIENTED_EDGE('',*,*,#49218,.F.);
#71289=ORIENTED_EDGE('',*,*,#49228,.F.);
#71290=ORIENTED_EDGE('',*,*,#49225,.F.);
#71291=ORIENTED_EDGE('',*,*,#49222,.F.);
#71292=ORIENTED_EDGE('',*,*,#49230,.F.);
#71293=ORIENTED_EDGE('',*,*,#49240,.F.);
#71294=ORIENTED_EDGE('',*,*,#49237,.F.);
#71295=ORIENTED_EDGE('',*,*,#49234,.F.);
#71296=ORIENTED_EDGE('',*,*,#49242,.F.);
#71297=ORIENTED_EDGE('',*,*,#49252,.F.);
#71298=ORIENTED_EDGE('',*,*,#49249,.F.);
#71299=ORIENTED_EDGE('',*,*,#49246,.F.);
#71300=ORIENTED_EDGE('',*,*,#49254,.F.);
#71301=ORIENTED_EDGE('',*,*,#49264,.F.);
#71302=ORIENTED_EDGE('',*,*,#49261,.F.);
#71303=ORIENTED_EDGE('',*,*,#49258,.F.);
#71304=ORIENTED_EDGE('',*,*,#49266,.F.);
#71305=ORIENTED_EDGE('',*,*,#49276,.F.);
#71306=ORIENTED_EDGE('',*,*,#49273,.F.);
#71307=ORIENTED_EDGE('',*,*,#49270,.F.);
#71308=ORIENTED_EDGE('',*,*,#49278,.F.);
#71309=ORIENTED_EDGE('',*,*,#49288,.F.);
#71310=ORIENTED_EDGE('',*,*,#49285,.F.);
#71311=ORIENTED_EDGE('',*,*,#49282,.F.);
#71312=ORIENTED_EDGE('',*,*,#49290,.F.);
#71313=ORIENTED_EDGE('',*,*,#49300,.F.);
#71314=ORIENTED_EDGE('',*,*,#49297,.F.);
#71315=ORIENTED_EDGE('',*,*,#49294,.F.);
#71316=ORIENTED_EDGE('',*,*,#49302,.F.);
#71317=ORIENTED_EDGE('',*,*,#49312,.F.);
#71318=ORIENTED_EDGE('',*,*,#49309,.F.);
#71319=ORIENTED_EDGE('',*,*,#49306,.F.);
#71320=ORIENTED_EDGE('',*,*,#49314,.F.);
#71321=ORIENTED_EDGE('',*,*,#49324,.F.);
#71322=ORIENTED_EDGE('',*,*,#49321,.F.);
#71323=ORIENTED_EDGE('',*,*,#49318,.F.);
#71324=ORIENTED_EDGE('',*,*,#49326,.F.);
#71325=ORIENTED_EDGE('',*,*,#49336,.F.);
#71326=ORIENTED_EDGE('',*,*,#49333,.F.);
#71327=ORIENTED_EDGE('',*,*,#49330,.F.);
#71328=ORIENTED_EDGE('',*,*,#49338,.F.);
#71329=ORIENTED_EDGE('',*,*,#49348,.F.);
#71330=ORIENTED_EDGE('',*,*,#49345,.F.);
#71331=ORIENTED_EDGE('',*,*,#49342,.F.);
#71332=ORIENTED_EDGE('',*,*,#49350,.F.);
#71333=ORIENTED_EDGE('',*,*,#49360,.F.);
#71334=ORIENTED_EDGE('',*,*,#49357,.F.);
#71335=ORIENTED_EDGE('',*,*,#49354,.F.);
#71336=ORIENTED_EDGE('',*,*,#49362,.F.);
#71337=ORIENTED_EDGE('',*,*,#49372,.F.);
#71338=ORIENTED_EDGE('',*,*,#49369,.F.);
#71339=ORIENTED_EDGE('',*,*,#49366,.F.);
#71340=ORIENTED_EDGE('',*,*,#49374,.F.);
#71341=ORIENTED_EDGE('',*,*,#49384,.F.);
#71342=ORIENTED_EDGE('',*,*,#49381,.F.);
#71343=ORIENTED_EDGE('',*,*,#49378,.F.);
#71344=ORIENTED_EDGE('',*,*,#49386,.F.);
#71345=ORIENTED_EDGE('',*,*,#49396,.F.);
#71346=ORIENTED_EDGE('',*,*,#49393,.F.);
#71347=ORIENTED_EDGE('',*,*,#49390,.F.);
#71348=ORIENTED_EDGE('',*,*,#49398,.F.);
#71349=ORIENTED_EDGE('',*,*,#49408,.F.);
#71350=ORIENTED_EDGE('',*,*,#49405,.F.);
#71351=ORIENTED_EDGE('',*,*,#49402,.F.);
#71352=ORIENTED_EDGE('',*,*,#49410,.F.);
#71353=ORIENTED_EDGE('',*,*,#49420,.F.);
#71354=ORIENTED_EDGE('',*,*,#49417,.F.);
#71355=ORIENTED_EDGE('',*,*,#49414,.F.);
#71356=ORIENTED_EDGE('',*,*,#49422,.F.);
#71357=ORIENTED_EDGE('',*,*,#49432,.F.);
#71358=ORIENTED_EDGE('',*,*,#49429,.F.);
#71359=ORIENTED_EDGE('',*,*,#49426,.F.);
#71360=ORIENTED_EDGE('',*,*,#49434,.F.);
#71361=ORIENTED_EDGE('',*,*,#49444,.F.);
#71362=ORIENTED_EDGE('',*,*,#49441,.F.);
#71363=ORIENTED_EDGE('',*,*,#49438,.F.);
#71364=ORIENTED_EDGE('',*,*,#49446,.F.);
#71365=ORIENTED_EDGE('',*,*,#49456,.F.);
#71366=ORIENTED_EDGE('',*,*,#49453,.F.);
#71367=ORIENTED_EDGE('',*,*,#49450,.F.);
#71368=ORIENTED_EDGE('',*,*,#49458,.F.);
#71369=ORIENTED_EDGE('',*,*,#49468,.F.);
#71370=ORIENTED_EDGE('',*,*,#49465,.F.);
#71371=ORIENTED_EDGE('',*,*,#49462,.F.);
#71372=ORIENTED_EDGE('',*,*,#49470,.F.);
#71373=ORIENTED_EDGE('',*,*,#49480,.F.);
#71374=ORIENTED_EDGE('',*,*,#49477,.F.);
#71375=ORIENTED_EDGE('',*,*,#49474,.F.);
#71376=ORIENTED_EDGE('',*,*,#49482,.F.);
#71377=ORIENTED_EDGE('',*,*,#49492,.F.);
#71378=ORIENTED_EDGE('',*,*,#49489,.F.);
#71379=ORIENTED_EDGE('',*,*,#49486,.F.);
#71380=ORIENTED_EDGE('',*,*,#49494,.F.);
#71381=ORIENTED_EDGE('',*,*,#49504,.F.);
#71382=ORIENTED_EDGE('',*,*,#49501,.F.);
#71383=ORIENTED_EDGE('',*,*,#49498,.F.);
#71384=ORIENTED_EDGE('',*,*,#49506,.F.);
#71385=ORIENTED_EDGE('',*,*,#49516,.F.);
#71386=ORIENTED_EDGE('',*,*,#49513,.F.);
#71387=ORIENTED_EDGE('',*,*,#49510,.F.);
#71388=ORIENTED_EDGE('',*,*,#49518,.F.);
#71389=ORIENTED_EDGE('',*,*,#49528,.F.);
#71390=ORIENTED_EDGE('',*,*,#49525,.F.);
#71391=ORIENTED_EDGE('',*,*,#49522,.F.);
#71392=ORIENTED_EDGE('',*,*,#49530,.F.);
#71393=ORIENTED_EDGE('',*,*,#49540,.F.);
#71394=ORIENTED_EDGE('',*,*,#49537,.F.);
#71395=ORIENTED_EDGE('',*,*,#49534,.F.);
#71396=ORIENTED_EDGE('',*,*,#49542,.F.);
#71397=ORIENTED_EDGE('',*,*,#49552,.F.);
#71398=ORIENTED_EDGE('',*,*,#49549,.F.);
#71399=ORIENTED_EDGE('',*,*,#49546,.F.);
#71400=ORIENTED_EDGE('',*,*,#49554,.F.);
#71401=ORIENTED_EDGE('',*,*,#49564,.F.);
#71402=ORIENTED_EDGE('',*,*,#49561,.F.);
#71403=ORIENTED_EDGE('',*,*,#49558,.F.);
#71404=ORIENTED_EDGE('',*,*,#49566,.F.);
#71405=ORIENTED_EDGE('',*,*,#49576,.F.);
#71406=ORIENTED_EDGE('',*,*,#49573,.F.);
#71407=ORIENTED_EDGE('',*,*,#49570,.F.);
#71408=ORIENTED_EDGE('',*,*,#49578,.F.);
#71409=ORIENTED_EDGE('',*,*,#49588,.F.);
#71410=ORIENTED_EDGE('',*,*,#49585,.F.);
#71411=ORIENTED_EDGE('',*,*,#49582,.F.);
#71412=ORIENTED_EDGE('',*,*,#49590,.F.);
#71413=ORIENTED_EDGE('',*,*,#49600,.F.);
#71414=ORIENTED_EDGE('',*,*,#49597,.F.);
#71415=ORIENTED_EDGE('',*,*,#49594,.F.);
#71416=ORIENTED_EDGE('',*,*,#49602,.F.);
#71417=ORIENTED_EDGE('',*,*,#49612,.F.);
#71418=ORIENTED_EDGE('',*,*,#49609,.F.);
#71419=ORIENTED_EDGE('',*,*,#49606,.F.);
#71420=ORIENTED_EDGE('',*,*,#49614,.F.);
#71421=ORIENTED_EDGE('',*,*,#49624,.F.);
#71422=ORIENTED_EDGE('',*,*,#49621,.F.);
#71423=ORIENTED_EDGE('',*,*,#49618,.F.);
#71424=ORIENTED_EDGE('',*,*,#49626,.F.);
#71425=ORIENTED_EDGE('',*,*,#49636,.F.);
#71426=ORIENTED_EDGE('',*,*,#49633,.F.);
#71427=ORIENTED_EDGE('',*,*,#49630,.F.);
#71428=ORIENTED_EDGE('',*,*,#49638,.F.);
#71429=ORIENTED_EDGE('',*,*,#49648,.F.);
#71430=ORIENTED_EDGE('',*,*,#49645,.F.);
#71431=ORIENTED_EDGE('',*,*,#49642,.F.);
#71432=ORIENTED_EDGE('',*,*,#49650,.F.);
#71433=ORIENTED_EDGE('',*,*,#49660,.F.);
#71434=ORIENTED_EDGE('',*,*,#49657,.F.);
#71435=ORIENTED_EDGE('',*,*,#49654,.F.);
#71436=ORIENTED_EDGE('',*,*,#49662,.F.);
#71437=ORIENTED_EDGE('',*,*,#49672,.F.);
#71438=ORIENTED_EDGE('',*,*,#49669,.F.);
#71439=ORIENTED_EDGE('',*,*,#49666,.F.);
#71440=ORIENTED_EDGE('',*,*,#49674,.F.);
#71441=ORIENTED_EDGE('',*,*,#49684,.F.);
#71442=ORIENTED_EDGE('',*,*,#49681,.F.);
#71443=ORIENTED_EDGE('',*,*,#49678,.F.);
#71444=ORIENTED_EDGE('',*,*,#49686,.F.);
#71445=ORIENTED_EDGE('',*,*,#49696,.F.);
#71446=ORIENTED_EDGE('',*,*,#49693,.F.);
#71447=ORIENTED_EDGE('',*,*,#49690,.F.);
#71448=ORIENTED_EDGE('',*,*,#49698,.F.);
#71449=ORIENTED_EDGE('',*,*,#49708,.F.);
#71450=ORIENTED_EDGE('',*,*,#49705,.F.);
#71451=ORIENTED_EDGE('',*,*,#49702,.F.);
#71452=ORIENTED_EDGE('',*,*,#49710,.F.);
#71453=ORIENTED_EDGE('',*,*,#49720,.F.);
#71454=ORIENTED_EDGE('',*,*,#49717,.F.);
#71455=ORIENTED_EDGE('',*,*,#49714,.F.);
#71456=ORIENTED_EDGE('',*,*,#49722,.F.);
#71457=ORIENTED_EDGE('',*,*,#49732,.F.);
#71458=ORIENTED_EDGE('',*,*,#49729,.F.);
#71459=ORIENTED_EDGE('',*,*,#49726,.F.);
#71460=ORIENTED_EDGE('',*,*,#49734,.F.);
#71461=ORIENTED_EDGE('',*,*,#49744,.F.);
#71462=ORIENTED_EDGE('',*,*,#49741,.F.);
#71463=ORIENTED_EDGE('',*,*,#49738,.F.);
#71464=ORIENTED_EDGE('',*,*,#49746,.F.);
#71465=ORIENTED_EDGE('',*,*,#49756,.F.);
#71466=ORIENTED_EDGE('',*,*,#49753,.F.);
#71467=ORIENTED_EDGE('',*,*,#49750,.F.);
#71468=ORIENTED_EDGE('',*,*,#49758,.F.);
#71469=ORIENTED_EDGE('',*,*,#49768,.F.);
#71470=ORIENTED_EDGE('',*,*,#49765,.F.);
#71471=ORIENTED_EDGE('',*,*,#49762,.F.);
#71472=ORIENTED_EDGE('',*,*,#49770,.F.);
#71473=ORIENTED_EDGE('',*,*,#49780,.F.);
#71474=ORIENTED_EDGE('',*,*,#49777,.F.);
#71475=ORIENTED_EDGE('',*,*,#49774,.F.);
#71476=ORIENTED_EDGE('',*,*,#49782,.F.);
#71477=ORIENTED_EDGE('',*,*,#49792,.F.);
#71478=ORIENTED_EDGE('',*,*,#49789,.F.);
#71479=ORIENTED_EDGE('',*,*,#49786,.F.);
#71480=ORIENTED_EDGE('',*,*,#49794,.F.);
#71481=ORIENTED_EDGE('',*,*,#49804,.F.);
#71482=ORIENTED_EDGE('',*,*,#49801,.F.);
#71483=ORIENTED_EDGE('',*,*,#49798,.F.);
#71484=ORIENTED_EDGE('',*,*,#49806,.F.);
#71485=ORIENTED_EDGE('',*,*,#49816,.F.);
#71486=ORIENTED_EDGE('',*,*,#49813,.F.);
#71487=ORIENTED_EDGE('',*,*,#49810,.F.);
#71488=ORIENTED_EDGE('',*,*,#49818,.F.);
#71489=ORIENTED_EDGE('',*,*,#49828,.F.);
#71490=ORIENTED_EDGE('',*,*,#49825,.F.);
#71491=ORIENTED_EDGE('',*,*,#49822,.F.);
#71492=ORIENTED_EDGE('',*,*,#49830,.F.);
#71493=ORIENTED_EDGE('',*,*,#49840,.F.);
#71494=ORIENTED_EDGE('',*,*,#49837,.F.);
#71495=ORIENTED_EDGE('',*,*,#49834,.F.);
#71496=ORIENTED_EDGE('',*,*,#49842,.F.);
#71497=ORIENTED_EDGE('',*,*,#49852,.F.);
#71498=ORIENTED_EDGE('',*,*,#49849,.F.);
#71499=ORIENTED_EDGE('',*,*,#49846,.F.);
#71500=ORIENTED_EDGE('',*,*,#49854,.F.);
#71501=ORIENTED_EDGE('',*,*,#49864,.F.);
#71502=ORIENTED_EDGE('',*,*,#49861,.F.);
#71503=ORIENTED_EDGE('',*,*,#49858,.F.);
#71504=ORIENTED_EDGE('',*,*,#49866,.F.);
#71505=ORIENTED_EDGE('',*,*,#49876,.F.);
#71506=ORIENTED_EDGE('',*,*,#49873,.F.);
#71507=ORIENTED_EDGE('',*,*,#49870,.F.);
#71508=ORIENTED_EDGE('',*,*,#49878,.F.);
#71509=ORIENTED_EDGE('',*,*,#49888,.F.);
#71510=ORIENTED_EDGE('',*,*,#49885,.F.);
#71511=ORIENTED_EDGE('',*,*,#49882,.F.);
#71512=ORIENTED_EDGE('',*,*,#49890,.F.);
#71513=ORIENTED_EDGE('',*,*,#49900,.F.);
#71514=ORIENTED_EDGE('',*,*,#49897,.F.);
#71515=ORIENTED_EDGE('',*,*,#49894,.F.);
#71516=ORIENTED_EDGE('',*,*,#49902,.F.);
#71517=ORIENTED_EDGE('',*,*,#49912,.F.);
#71518=ORIENTED_EDGE('',*,*,#49909,.F.);
#71519=ORIENTED_EDGE('',*,*,#49906,.F.);
#71520=ORIENTED_EDGE('',*,*,#49914,.F.);
#71521=ORIENTED_EDGE('',*,*,#49924,.F.);
#71522=ORIENTED_EDGE('',*,*,#49921,.F.);
#71523=ORIENTED_EDGE('',*,*,#49918,.F.);
#71524=ORIENTED_EDGE('',*,*,#49926,.F.);
#71525=ORIENTED_EDGE('',*,*,#49936,.F.);
#71526=ORIENTED_EDGE('',*,*,#49933,.F.);
#71527=ORIENTED_EDGE('',*,*,#49930,.F.);
#71528=ORIENTED_EDGE('',*,*,#49938,.F.);
#71529=ORIENTED_EDGE('',*,*,#49948,.F.);
#71530=ORIENTED_EDGE('',*,*,#49945,.F.);
#71531=ORIENTED_EDGE('',*,*,#49942,.F.);
#71532=ORIENTED_EDGE('',*,*,#49950,.F.);
#71533=ORIENTED_EDGE('',*,*,#49960,.F.);
#71534=ORIENTED_EDGE('',*,*,#49957,.F.);
#71535=ORIENTED_EDGE('',*,*,#49954,.F.);
#71536=ORIENTED_EDGE('',*,*,#49962,.F.);
#71537=ORIENTED_EDGE('',*,*,#49972,.F.);
#71538=ORIENTED_EDGE('',*,*,#49969,.F.);
#71539=ORIENTED_EDGE('',*,*,#49966,.F.);
#71540=ORIENTED_EDGE('',*,*,#49974,.F.);
#71541=ORIENTED_EDGE('',*,*,#49984,.F.);
#71542=ORIENTED_EDGE('',*,*,#49981,.F.);
#71543=ORIENTED_EDGE('',*,*,#49978,.F.);
#71544=ORIENTED_EDGE('',*,*,#49986,.F.);
#71545=ORIENTED_EDGE('',*,*,#49996,.F.);
#71546=ORIENTED_EDGE('',*,*,#49993,.F.);
#71547=ORIENTED_EDGE('',*,*,#49990,.F.);
#71548=ORIENTED_EDGE('',*,*,#49998,.F.);
#71549=ORIENTED_EDGE('',*,*,#50008,.F.);
#71550=ORIENTED_EDGE('',*,*,#50005,.F.);
#71551=ORIENTED_EDGE('',*,*,#50002,.F.);
#71552=ORIENTED_EDGE('',*,*,#50010,.F.);
#71553=ORIENTED_EDGE('',*,*,#50020,.F.);
#71554=ORIENTED_EDGE('',*,*,#50017,.F.);
#71555=ORIENTED_EDGE('',*,*,#50014,.F.);
#71556=ORIENTED_EDGE('',*,*,#50022,.F.);
#71557=ORIENTED_EDGE('',*,*,#50032,.F.);
#71558=ORIENTED_EDGE('',*,*,#50029,.F.);
#71559=ORIENTED_EDGE('',*,*,#50026,.F.);
#71560=ORIENTED_EDGE('',*,*,#50034,.F.);
#71561=ORIENTED_EDGE('',*,*,#50044,.F.);
#71562=ORIENTED_EDGE('',*,*,#50041,.F.);
#71563=ORIENTED_EDGE('',*,*,#50038,.F.);
#71564=ORIENTED_EDGE('',*,*,#50046,.F.);
#71565=ORIENTED_EDGE('',*,*,#50056,.F.);
#71566=ORIENTED_EDGE('',*,*,#50053,.F.);
#71567=ORIENTED_EDGE('',*,*,#50050,.F.);
#71568=ORIENTED_EDGE('',*,*,#50058,.F.);
#71569=ORIENTED_EDGE('',*,*,#50068,.F.);
#71570=ORIENTED_EDGE('',*,*,#50065,.F.);
#71571=ORIENTED_EDGE('',*,*,#50062,.F.);
#71572=ORIENTED_EDGE('',*,*,#50070,.F.);
#71573=ORIENTED_EDGE('',*,*,#50080,.F.);
#71574=ORIENTED_EDGE('',*,*,#50077,.F.);
#71575=ORIENTED_EDGE('',*,*,#50074,.F.);
#71576=ORIENTED_EDGE('',*,*,#50082,.F.);
#71577=ORIENTED_EDGE('',*,*,#50092,.F.);
#71578=ORIENTED_EDGE('',*,*,#50089,.F.);
#71579=ORIENTED_EDGE('',*,*,#50086,.F.);
#71580=ORIENTED_EDGE('',*,*,#50094,.F.);
#71581=ORIENTED_EDGE('',*,*,#50104,.F.);
#71582=ORIENTED_EDGE('',*,*,#50101,.F.);
#71583=ORIENTED_EDGE('',*,*,#50098,.F.);
#71584=ORIENTED_EDGE('',*,*,#50106,.F.);
#71585=ORIENTED_EDGE('',*,*,#50116,.F.);
#71586=ORIENTED_EDGE('',*,*,#50113,.F.);
#71587=ORIENTED_EDGE('',*,*,#50110,.F.);
#71588=ORIENTED_EDGE('',*,*,#50118,.F.);
#71589=ORIENTED_EDGE('',*,*,#50128,.F.);
#71590=ORIENTED_EDGE('',*,*,#50125,.F.);
#71591=ORIENTED_EDGE('',*,*,#50122,.F.);
#71592=ORIENTED_EDGE('',*,*,#50130,.F.);
#71593=ORIENTED_EDGE('',*,*,#50140,.F.);
#71594=ORIENTED_EDGE('',*,*,#50137,.F.);
#71595=ORIENTED_EDGE('',*,*,#50134,.F.);
#71596=ORIENTED_EDGE('',*,*,#50142,.F.);
#71597=ORIENTED_EDGE('',*,*,#50152,.F.);
#71598=ORIENTED_EDGE('',*,*,#50149,.F.);
#71599=ORIENTED_EDGE('',*,*,#50146,.F.);
#71600=ORIENTED_EDGE('',*,*,#50154,.F.);
#71601=ORIENTED_EDGE('',*,*,#50164,.F.);
#71602=ORIENTED_EDGE('',*,*,#50161,.F.);
#71603=ORIENTED_EDGE('',*,*,#50158,.F.);
#71604=ORIENTED_EDGE('',*,*,#50166,.F.);
#71605=ORIENTED_EDGE('',*,*,#50176,.F.);
#71606=ORIENTED_EDGE('',*,*,#50173,.F.);
#71607=ORIENTED_EDGE('',*,*,#50170,.F.);
#71608=ORIENTED_EDGE('',*,*,#50178,.F.);
#71609=ORIENTED_EDGE('',*,*,#50188,.F.);
#71610=ORIENTED_EDGE('',*,*,#50185,.F.);
#71611=ORIENTED_EDGE('',*,*,#50182,.F.);
#71612=ORIENTED_EDGE('',*,*,#50190,.F.);
#71613=ORIENTED_EDGE('',*,*,#50200,.F.);
#71614=ORIENTED_EDGE('',*,*,#50197,.F.);
#71615=ORIENTED_EDGE('',*,*,#50194,.F.);
#71616=ORIENTED_EDGE('',*,*,#50202,.F.);
#71617=ORIENTED_EDGE('',*,*,#50212,.F.);
#71618=ORIENTED_EDGE('',*,*,#50209,.F.);
#71619=ORIENTED_EDGE('',*,*,#50206,.F.);
#71620=ORIENTED_EDGE('',*,*,#50214,.F.);
#71621=ORIENTED_EDGE('',*,*,#50224,.F.);
#71622=ORIENTED_EDGE('',*,*,#50221,.F.);
#71623=ORIENTED_EDGE('',*,*,#50218,.F.);
#71624=ORIENTED_EDGE('',*,*,#50226,.F.);
#71625=ORIENTED_EDGE('',*,*,#50236,.F.);
#71626=ORIENTED_EDGE('',*,*,#50233,.F.);
#71627=ORIENTED_EDGE('',*,*,#50230,.F.);
#71628=ORIENTED_EDGE('',*,*,#50238,.F.);
#71629=ORIENTED_EDGE('',*,*,#50248,.F.);
#71630=ORIENTED_EDGE('',*,*,#50245,.F.);
#71631=ORIENTED_EDGE('',*,*,#50242,.F.);
#71632=ORIENTED_EDGE('',*,*,#50250,.F.);
#71633=ORIENTED_EDGE('',*,*,#50260,.F.);
#71634=ORIENTED_EDGE('',*,*,#50257,.F.);
#71635=ORIENTED_EDGE('',*,*,#50254,.F.);
#71636=ORIENTED_EDGE('',*,*,#50262,.F.);
#71637=ORIENTED_EDGE('',*,*,#50272,.F.);
#71638=ORIENTED_EDGE('',*,*,#50269,.F.);
#71639=ORIENTED_EDGE('',*,*,#50266,.F.);
#71640=ORIENTED_EDGE('',*,*,#50274,.F.);
#71641=ORIENTED_EDGE('',*,*,#50284,.F.);
#71642=ORIENTED_EDGE('',*,*,#50281,.F.);
#71643=ORIENTED_EDGE('',*,*,#50278,.F.);
#71644=ORIENTED_EDGE('',*,*,#50286,.F.);
#71645=ORIENTED_EDGE('',*,*,#50296,.F.);
#71646=ORIENTED_EDGE('',*,*,#50293,.F.);
#71647=ORIENTED_EDGE('',*,*,#50290,.F.);
#71648=ORIENTED_EDGE('',*,*,#50298,.F.);
#71649=ORIENTED_EDGE('',*,*,#50308,.F.);
#71650=ORIENTED_EDGE('',*,*,#50305,.F.);
#71651=ORIENTED_EDGE('',*,*,#50302,.F.);
#71652=ORIENTED_EDGE('',*,*,#50310,.F.);
#71653=ORIENTED_EDGE('',*,*,#50320,.F.);
#71654=ORIENTED_EDGE('',*,*,#50317,.F.);
#71655=ORIENTED_EDGE('',*,*,#50314,.F.);
#71656=ORIENTED_EDGE('',*,*,#50322,.F.);
#71657=ORIENTED_EDGE('',*,*,#50332,.F.);
#71658=ORIENTED_EDGE('',*,*,#50329,.F.);
#71659=ORIENTED_EDGE('',*,*,#50326,.F.);
#71660=ORIENTED_EDGE('',*,*,#50334,.F.);
#71661=ORIENTED_EDGE('',*,*,#50344,.F.);
#71662=ORIENTED_EDGE('',*,*,#50341,.F.);
#71663=ORIENTED_EDGE('',*,*,#50338,.F.);
#71664=ORIENTED_EDGE('',*,*,#50346,.F.);
#71665=ORIENTED_EDGE('',*,*,#50356,.F.);
#71666=ORIENTED_EDGE('',*,*,#50353,.F.);
#71667=ORIENTED_EDGE('',*,*,#50350,.F.);
#71668=ORIENTED_EDGE('',*,*,#50358,.F.);
#71669=ORIENTED_EDGE('',*,*,#50368,.F.);
#71670=ORIENTED_EDGE('',*,*,#50365,.F.);
#71671=ORIENTED_EDGE('',*,*,#50362,.F.);
#71672=ORIENTED_EDGE('',*,*,#50370,.F.);
#71673=ORIENTED_EDGE('',*,*,#50380,.F.);
#71674=ORIENTED_EDGE('',*,*,#50377,.F.);
#71675=ORIENTED_EDGE('',*,*,#50374,.F.);
#71676=ORIENTED_EDGE('',*,*,#50382,.F.);
#71677=ORIENTED_EDGE('',*,*,#50392,.F.);
#71678=ORIENTED_EDGE('',*,*,#50389,.F.);
#71679=ORIENTED_EDGE('',*,*,#50386,.F.);
#71680=ORIENTED_EDGE('',*,*,#50394,.F.);
#71681=ORIENTED_EDGE('',*,*,#50404,.F.);
#71682=ORIENTED_EDGE('',*,*,#50401,.F.);
#71683=ORIENTED_EDGE('',*,*,#50398,.F.);
#71684=ORIENTED_EDGE('',*,*,#50406,.F.);
#71685=ORIENTED_EDGE('',*,*,#50416,.F.);
#71686=ORIENTED_EDGE('',*,*,#50413,.F.);
#71687=ORIENTED_EDGE('',*,*,#50410,.F.);
#71688=ORIENTED_EDGE('',*,*,#50418,.F.);
#71689=ORIENTED_EDGE('',*,*,#50428,.F.);
#71690=ORIENTED_EDGE('',*,*,#50425,.F.);
#71691=ORIENTED_EDGE('',*,*,#50422,.F.);
#71692=ORIENTED_EDGE('',*,*,#50430,.F.);
#71693=ORIENTED_EDGE('',*,*,#50440,.F.);
#71694=ORIENTED_EDGE('',*,*,#50437,.F.);
#71695=ORIENTED_EDGE('',*,*,#50434,.F.);
#71696=ORIENTED_EDGE('',*,*,#50442,.F.);
#71697=ORIENTED_EDGE('',*,*,#50452,.F.);
#71698=ORIENTED_EDGE('',*,*,#50449,.F.);
#71699=ORIENTED_EDGE('',*,*,#50446,.F.);
#71700=ORIENTED_EDGE('',*,*,#50454,.F.);
#71701=ORIENTED_EDGE('',*,*,#50464,.F.);
#71702=ORIENTED_EDGE('',*,*,#50461,.F.);
#71703=ORIENTED_EDGE('',*,*,#50458,.F.);
#71704=ORIENTED_EDGE('',*,*,#50466,.F.);
#71705=ORIENTED_EDGE('',*,*,#50476,.F.);
#71706=ORIENTED_EDGE('',*,*,#50473,.F.);
#71707=ORIENTED_EDGE('',*,*,#50470,.F.);
#71708=ORIENTED_EDGE('',*,*,#50478,.F.);
#71709=ORIENTED_EDGE('',*,*,#50488,.F.);
#71710=ORIENTED_EDGE('',*,*,#50485,.F.);
#71711=ORIENTED_EDGE('',*,*,#50482,.F.);
#71712=ORIENTED_EDGE('',*,*,#50490,.F.);
#71713=ORIENTED_EDGE('',*,*,#50500,.F.);
#71714=ORIENTED_EDGE('',*,*,#50497,.F.);
#71715=ORIENTED_EDGE('',*,*,#50494,.F.);
#71716=ORIENTED_EDGE('',*,*,#50502,.F.);
#71717=ORIENTED_EDGE('',*,*,#50512,.F.);
#71718=ORIENTED_EDGE('',*,*,#50509,.F.);
#71719=ORIENTED_EDGE('',*,*,#50506,.F.);
#71720=ORIENTED_EDGE('',*,*,#50514,.F.);
#71721=ORIENTED_EDGE('',*,*,#50524,.F.);
#71722=ORIENTED_EDGE('',*,*,#50521,.F.);
#71723=ORIENTED_EDGE('',*,*,#50518,.F.);
#71724=ORIENTED_EDGE('',*,*,#50526,.F.);
#71725=ORIENTED_EDGE('',*,*,#50536,.F.);
#71726=ORIENTED_EDGE('',*,*,#50533,.F.);
#71727=ORIENTED_EDGE('',*,*,#50530,.F.);
#71728=ORIENTED_EDGE('',*,*,#50538,.F.);
#71729=ORIENTED_EDGE('',*,*,#50548,.F.);
#71730=ORIENTED_EDGE('',*,*,#50545,.F.);
#71731=ORIENTED_EDGE('',*,*,#50542,.F.);
#71732=ORIENTED_EDGE('',*,*,#50550,.F.);
#71733=ORIENTED_EDGE('',*,*,#50560,.F.);
#71734=ORIENTED_EDGE('',*,*,#50557,.F.);
#71735=ORIENTED_EDGE('',*,*,#50554,.F.);
#71736=ORIENTED_EDGE('',*,*,#50562,.F.);
#71737=ORIENTED_EDGE('',*,*,#50572,.F.);
#71738=ORIENTED_EDGE('',*,*,#50569,.F.);
#71739=ORIENTED_EDGE('',*,*,#50566,.F.);
#71740=ORIENTED_EDGE('',*,*,#50574,.F.);
#71741=ORIENTED_EDGE('',*,*,#50584,.F.);
#71742=ORIENTED_EDGE('',*,*,#50581,.F.);
#71743=ORIENTED_EDGE('',*,*,#50578,.F.);
#71744=ORIENTED_EDGE('',*,*,#50586,.F.);
#71745=ORIENTED_EDGE('',*,*,#50596,.F.);
#71746=ORIENTED_EDGE('',*,*,#50593,.F.);
#71747=ORIENTED_EDGE('',*,*,#50590,.F.);
#71748=ORIENTED_EDGE('',*,*,#50598,.F.);
#71749=ORIENTED_EDGE('',*,*,#50608,.F.);
#71750=ORIENTED_EDGE('',*,*,#50605,.F.);
#71751=ORIENTED_EDGE('',*,*,#50602,.F.);
#71752=ORIENTED_EDGE('',*,*,#50610,.F.);
#71753=ORIENTED_EDGE('',*,*,#50620,.F.);
#71754=ORIENTED_EDGE('',*,*,#50617,.F.);
#71755=ORIENTED_EDGE('',*,*,#50614,.F.);
#71756=ORIENTED_EDGE('',*,*,#50622,.F.);
#71757=ORIENTED_EDGE('',*,*,#50632,.F.);
#71758=ORIENTED_EDGE('',*,*,#50629,.F.);
#71759=ORIENTED_EDGE('',*,*,#50626,.F.);
#71760=ORIENTED_EDGE('',*,*,#50634,.F.);
#71761=ORIENTED_EDGE('',*,*,#50644,.F.);
#71762=ORIENTED_EDGE('',*,*,#50641,.F.);
#71763=ORIENTED_EDGE('',*,*,#50638,.F.);
#71764=ORIENTED_EDGE('',*,*,#50646,.F.);
#71765=ORIENTED_EDGE('',*,*,#50656,.F.);
#71766=ORIENTED_EDGE('',*,*,#50653,.F.);
#71767=ORIENTED_EDGE('',*,*,#50650,.F.);
#71768=ORIENTED_EDGE('',*,*,#50658,.F.);
#71769=ORIENTED_EDGE('',*,*,#50668,.F.);
#71770=ORIENTED_EDGE('',*,*,#50665,.F.);
#71771=ORIENTED_EDGE('',*,*,#50662,.F.);
#71772=ORIENTED_EDGE('',*,*,#50670,.F.);
#71773=ORIENTED_EDGE('',*,*,#50680,.F.);
#71774=ORIENTED_EDGE('',*,*,#50677,.F.);
#71775=ORIENTED_EDGE('',*,*,#50674,.F.);
#71776=ORIENTED_EDGE('',*,*,#50682,.F.);
#71777=ORIENTED_EDGE('',*,*,#50692,.F.);
#71778=ORIENTED_EDGE('',*,*,#50689,.F.);
#71779=ORIENTED_EDGE('',*,*,#50686,.F.);
#71780=ORIENTED_EDGE('',*,*,#50694,.F.);
#71781=ORIENTED_EDGE('',*,*,#50704,.F.);
#71782=ORIENTED_EDGE('',*,*,#50701,.F.);
#71783=ORIENTED_EDGE('',*,*,#50698,.F.);
#71784=ORIENTED_EDGE('',*,*,#50706,.F.);
#71785=ORIENTED_EDGE('',*,*,#50716,.F.);
#71786=ORIENTED_EDGE('',*,*,#50713,.F.);
#71787=ORIENTED_EDGE('',*,*,#50710,.F.);
#71788=ORIENTED_EDGE('',*,*,#50718,.F.);
#71789=ORIENTED_EDGE('',*,*,#50728,.F.);
#71790=ORIENTED_EDGE('',*,*,#50725,.F.);
#71791=ORIENTED_EDGE('',*,*,#50722,.F.);
#71792=ORIENTED_EDGE('',*,*,#50730,.F.);
#71793=ORIENTED_EDGE('',*,*,#50740,.F.);
#71794=ORIENTED_EDGE('',*,*,#50737,.F.);
#71795=ORIENTED_EDGE('',*,*,#50734,.F.);
#71796=ORIENTED_EDGE('',*,*,#50742,.F.);
#71797=ORIENTED_EDGE('',*,*,#50752,.F.);
#71798=ORIENTED_EDGE('',*,*,#50749,.F.);
#71799=ORIENTED_EDGE('',*,*,#50746,.F.);
#71800=ORIENTED_EDGE('',*,*,#50754,.F.);
#71801=ORIENTED_EDGE('',*,*,#50764,.F.);
#71802=ORIENTED_EDGE('',*,*,#50761,.F.);
#71803=ORIENTED_EDGE('',*,*,#50758,.F.);
#71804=ORIENTED_EDGE('',*,*,#50766,.F.);
#71805=ORIENTED_EDGE('',*,*,#50776,.F.);
#71806=ORIENTED_EDGE('',*,*,#50773,.F.);
#71807=ORIENTED_EDGE('',*,*,#50770,.F.);
#71808=ORIENTED_EDGE('',*,*,#50778,.F.);
#71809=ORIENTED_EDGE('',*,*,#50788,.F.);
#71810=ORIENTED_EDGE('',*,*,#50785,.F.);
#71811=ORIENTED_EDGE('',*,*,#50782,.F.);
#71812=ORIENTED_EDGE('',*,*,#50790,.F.);
#71813=ORIENTED_EDGE('',*,*,#50800,.F.);
#71814=ORIENTED_EDGE('',*,*,#50797,.F.);
#71815=ORIENTED_EDGE('',*,*,#50794,.F.);
#71816=ORIENTED_EDGE('',*,*,#50802,.F.);
#71817=ORIENTED_EDGE('',*,*,#50812,.F.);
#71818=ORIENTED_EDGE('',*,*,#50809,.F.);
#71819=ORIENTED_EDGE('',*,*,#50806,.F.);
#71820=ORIENTED_EDGE('',*,*,#50814,.F.);
#71821=ORIENTED_EDGE('',*,*,#50824,.F.);
#71822=ORIENTED_EDGE('',*,*,#50821,.F.);
#71823=ORIENTED_EDGE('',*,*,#50818,.F.);
#71824=ORIENTED_EDGE('',*,*,#50826,.F.);
#71825=ORIENTED_EDGE('',*,*,#50836,.F.);
#71826=ORIENTED_EDGE('',*,*,#50833,.F.);
#71827=ORIENTED_EDGE('',*,*,#50830,.F.);
#71828=ORIENTED_EDGE('',*,*,#50838,.F.);
#71829=ORIENTED_EDGE('',*,*,#50848,.F.);
#71830=ORIENTED_EDGE('',*,*,#50845,.F.);
#71831=ORIENTED_EDGE('',*,*,#50842,.F.);
#71832=ORIENTED_EDGE('',*,*,#50850,.F.);
#71833=ORIENTED_EDGE('',*,*,#50860,.F.);
#71834=ORIENTED_EDGE('',*,*,#50857,.F.);
#71835=ORIENTED_EDGE('',*,*,#50854,.F.);
#71836=ORIENTED_EDGE('',*,*,#50862,.F.);
#71837=ORIENTED_EDGE('',*,*,#50872,.F.);
#71838=ORIENTED_EDGE('',*,*,#50869,.F.);
#71839=ORIENTED_EDGE('',*,*,#50866,.F.);
#71840=ORIENTED_EDGE('',*,*,#50874,.F.);
#71841=ORIENTED_EDGE('',*,*,#50884,.F.);
#71842=ORIENTED_EDGE('',*,*,#50881,.F.);
#71843=ORIENTED_EDGE('',*,*,#50878,.F.);
#71844=ORIENTED_EDGE('',*,*,#50886,.F.);
#71845=ORIENTED_EDGE('',*,*,#50896,.F.);
#71846=ORIENTED_EDGE('',*,*,#50893,.F.);
#71847=ORIENTED_EDGE('',*,*,#50890,.F.);
#71848=ORIENTED_EDGE('',*,*,#50898,.F.);
#71849=ORIENTED_EDGE('',*,*,#50908,.F.);
#71850=ORIENTED_EDGE('',*,*,#50905,.F.);
#71851=ORIENTED_EDGE('',*,*,#50902,.F.);
#71852=ORIENTED_EDGE('',*,*,#50910,.F.);
#71853=ORIENTED_EDGE('',*,*,#50920,.F.);
#71854=ORIENTED_EDGE('',*,*,#50917,.F.);
#71855=ORIENTED_EDGE('',*,*,#50914,.F.);
#71856=ORIENTED_EDGE('',*,*,#50922,.F.);
#71857=ORIENTED_EDGE('',*,*,#50932,.F.);
#71858=ORIENTED_EDGE('',*,*,#50929,.F.);
#71859=ORIENTED_EDGE('',*,*,#50926,.F.);
#71860=ORIENTED_EDGE('',*,*,#50934,.F.);
#71861=ORIENTED_EDGE('',*,*,#50944,.F.);
#71862=ORIENTED_EDGE('',*,*,#50941,.F.);
#71863=ORIENTED_EDGE('',*,*,#50938,.F.);
#71864=ORIENTED_EDGE('',*,*,#50946,.F.);
#71865=ORIENTED_EDGE('',*,*,#50956,.F.);
#71866=ORIENTED_EDGE('',*,*,#50953,.F.);
#71867=ORIENTED_EDGE('',*,*,#50950,.F.);
#71868=ORIENTED_EDGE('',*,*,#50958,.F.);
#71869=ORIENTED_EDGE('',*,*,#50968,.F.);
#71870=ORIENTED_EDGE('',*,*,#50965,.F.);
#71871=ORIENTED_EDGE('',*,*,#50962,.F.);
#71872=ORIENTED_EDGE('',*,*,#50970,.F.);
#71873=ORIENTED_EDGE('',*,*,#50980,.F.);
#71874=ORIENTED_EDGE('',*,*,#50977,.F.);
#71875=ORIENTED_EDGE('',*,*,#50974,.F.);
#71876=ORIENTED_EDGE('',*,*,#50982,.F.);
#71877=ORIENTED_EDGE('',*,*,#50992,.F.);
#71878=ORIENTED_EDGE('',*,*,#50989,.F.);
#71879=ORIENTED_EDGE('',*,*,#50986,.F.);
#71880=ORIENTED_EDGE('',*,*,#50994,.F.);
#71881=ORIENTED_EDGE('',*,*,#51004,.F.);
#71882=ORIENTED_EDGE('',*,*,#51001,.F.);
#71883=ORIENTED_EDGE('',*,*,#50998,.F.);
#71884=ORIENTED_EDGE('',*,*,#51006,.F.);
#71885=ORIENTED_EDGE('',*,*,#51016,.F.);
#71886=ORIENTED_EDGE('',*,*,#51013,.F.);
#71887=ORIENTED_EDGE('',*,*,#51010,.F.);
#71888=ORIENTED_EDGE('',*,*,#51018,.F.);
#71889=ORIENTED_EDGE('',*,*,#51028,.F.);
#71890=ORIENTED_EDGE('',*,*,#51025,.F.);
#71891=ORIENTED_EDGE('',*,*,#51022,.F.);
#71892=ORIENTED_EDGE('',*,*,#51030,.F.);
#71893=ORIENTED_EDGE('',*,*,#51040,.F.);
#71894=ORIENTED_EDGE('',*,*,#51037,.F.);
#71895=ORIENTED_EDGE('',*,*,#51034,.F.);
#71896=ORIENTED_EDGE('',*,*,#51042,.F.);
#71897=ORIENTED_EDGE('',*,*,#51052,.F.);
#71898=ORIENTED_EDGE('',*,*,#51049,.F.);
#71899=ORIENTED_EDGE('',*,*,#51046,.F.);
#71900=ORIENTED_EDGE('',*,*,#51054,.F.);
#71901=ORIENTED_EDGE('',*,*,#51064,.F.);
#71902=ORIENTED_EDGE('',*,*,#51061,.F.);
#71903=ORIENTED_EDGE('',*,*,#51058,.F.);
#71904=ORIENTED_EDGE('',*,*,#51066,.F.);
#71905=ORIENTED_EDGE('',*,*,#51076,.F.);
#71906=ORIENTED_EDGE('',*,*,#51073,.F.);
#71907=ORIENTED_EDGE('',*,*,#51070,.F.);
#71908=ORIENTED_EDGE('',*,*,#51078,.F.);
#71909=ORIENTED_EDGE('',*,*,#51088,.F.);
#71910=ORIENTED_EDGE('',*,*,#51085,.F.);
#71911=ORIENTED_EDGE('',*,*,#51082,.F.);
#71912=ORIENTED_EDGE('',*,*,#51090,.F.);
#71913=ORIENTED_EDGE('',*,*,#51100,.F.);
#71914=ORIENTED_EDGE('',*,*,#51097,.F.);
#71915=ORIENTED_EDGE('',*,*,#51094,.F.);
#71916=ORIENTED_EDGE('',*,*,#51102,.F.);
#71917=ORIENTED_EDGE('',*,*,#51112,.F.);
#71918=ORIENTED_EDGE('',*,*,#51109,.F.);
#71919=ORIENTED_EDGE('',*,*,#51106,.F.);
#71920=ORIENTED_EDGE('',*,*,#51114,.F.);
#71921=ORIENTED_EDGE('',*,*,#51124,.F.);
#71922=ORIENTED_EDGE('',*,*,#51121,.F.);
#71923=ORIENTED_EDGE('',*,*,#51118,.F.);
#71924=ORIENTED_EDGE('',*,*,#51126,.F.);
#71925=ORIENTED_EDGE('',*,*,#51136,.F.);
#71926=ORIENTED_EDGE('',*,*,#51133,.F.);
#71927=ORIENTED_EDGE('',*,*,#51130,.F.);
#71928=ORIENTED_EDGE('',*,*,#51138,.F.);
#71929=ORIENTED_EDGE('',*,*,#51148,.F.);
#71930=ORIENTED_EDGE('',*,*,#51145,.F.);
#71931=ORIENTED_EDGE('',*,*,#51142,.F.);
#71932=ORIENTED_EDGE('',*,*,#51150,.F.);
#71933=ORIENTED_EDGE('',*,*,#51160,.F.);
#71934=ORIENTED_EDGE('',*,*,#51157,.F.);
#71935=ORIENTED_EDGE('',*,*,#51154,.F.);
#71936=ORIENTED_EDGE('',*,*,#51162,.F.);
#71937=ORIENTED_EDGE('',*,*,#51172,.F.);
#71938=ORIENTED_EDGE('',*,*,#51169,.F.);
#71939=ORIENTED_EDGE('',*,*,#51166,.F.);
#71940=ORIENTED_EDGE('',*,*,#51174,.F.);
#71941=ORIENTED_EDGE('',*,*,#51184,.F.);
#71942=ORIENTED_EDGE('',*,*,#51181,.F.);
#71943=ORIENTED_EDGE('',*,*,#51178,.F.);
#71944=ORIENTED_EDGE('',*,*,#51186,.F.);
#71945=ORIENTED_EDGE('',*,*,#51196,.F.);
#71946=ORIENTED_EDGE('',*,*,#51193,.F.);
#71947=ORIENTED_EDGE('',*,*,#51190,.F.);
#71948=ORIENTED_EDGE('',*,*,#51198,.F.);
#71949=ORIENTED_EDGE('',*,*,#51208,.F.);
#71950=ORIENTED_EDGE('',*,*,#51205,.F.);
#71951=ORIENTED_EDGE('',*,*,#51202,.F.);
#71952=ORIENTED_EDGE('',*,*,#51210,.F.);
#71953=ORIENTED_EDGE('',*,*,#51220,.F.);
#71954=ORIENTED_EDGE('',*,*,#51217,.F.);
#71955=ORIENTED_EDGE('',*,*,#51214,.F.);
#71956=ORIENTED_EDGE('',*,*,#51222,.F.);
#71957=ORIENTED_EDGE('',*,*,#51232,.F.);
#71958=ORIENTED_EDGE('',*,*,#51229,.F.);
#71959=ORIENTED_EDGE('',*,*,#51226,.F.);
#71960=ORIENTED_EDGE('',*,*,#51234,.F.);
#71961=ORIENTED_EDGE('',*,*,#51244,.F.);
#71962=ORIENTED_EDGE('',*,*,#51241,.F.);
#71963=ORIENTED_EDGE('',*,*,#51238,.F.);
#71964=ORIENTED_EDGE('',*,*,#51246,.F.);
#71965=ORIENTED_EDGE('',*,*,#51256,.F.);
#71966=ORIENTED_EDGE('',*,*,#51253,.F.);
#71967=ORIENTED_EDGE('',*,*,#51250,.F.);
#71968=ORIENTED_EDGE('',*,*,#51258,.F.);
#71969=ORIENTED_EDGE('',*,*,#51268,.F.);
#71970=ORIENTED_EDGE('',*,*,#51265,.F.);
#71971=ORIENTED_EDGE('',*,*,#51262,.F.);
#71972=ORIENTED_EDGE('',*,*,#51270,.F.);
#71973=ORIENTED_EDGE('',*,*,#51280,.F.);
#71974=ORIENTED_EDGE('',*,*,#51277,.F.);
#71975=ORIENTED_EDGE('',*,*,#51274,.F.);
#71976=ORIENTED_EDGE('',*,*,#51282,.F.);
#71977=ORIENTED_EDGE('',*,*,#51292,.F.);
#71978=ORIENTED_EDGE('',*,*,#51289,.F.);
#71979=ORIENTED_EDGE('',*,*,#51286,.F.);
#71980=ORIENTED_EDGE('',*,*,#51294,.F.);
#71981=ORIENTED_EDGE('',*,*,#51304,.F.);
#71982=ORIENTED_EDGE('',*,*,#51301,.F.);
#71983=ORIENTED_EDGE('',*,*,#51298,.F.);
#71984=ORIENTED_EDGE('',*,*,#51306,.F.);
#71985=ORIENTED_EDGE('',*,*,#51316,.F.);
#71986=ORIENTED_EDGE('',*,*,#51313,.F.);
#71987=ORIENTED_EDGE('',*,*,#51310,.F.);
#71988=ORIENTED_EDGE('',*,*,#51318,.F.);
#71989=ORIENTED_EDGE('',*,*,#51328,.F.);
#71990=ORIENTED_EDGE('',*,*,#51325,.F.);
#71991=ORIENTED_EDGE('',*,*,#51322,.F.);
#71992=ORIENTED_EDGE('',*,*,#51330,.F.);
#71993=ORIENTED_EDGE('',*,*,#51340,.F.);
#71994=ORIENTED_EDGE('',*,*,#51337,.F.);
#71995=ORIENTED_EDGE('',*,*,#51334,.F.);
#71996=ORIENTED_EDGE('',*,*,#51342,.F.);
#71997=ORIENTED_EDGE('',*,*,#51352,.F.);
#71998=ORIENTED_EDGE('',*,*,#51349,.F.);
#71999=ORIENTED_EDGE('',*,*,#51346,.F.);
#72000=ORIENTED_EDGE('',*,*,#51354,.F.);
#72001=ORIENTED_EDGE('',*,*,#51364,.F.);
#72002=ORIENTED_EDGE('',*,*,#51361,.F.);
#72003=ORIENTED_EDGE('',*,*,#51358,.F.);
#72004=ORIENTED_EDGE('',*,*,#51366,.F.);
#72005=ORIENTED_EDGE('',*,*,#51376,.F.);
#72006=ORIENTED_EDGE('',*,*,#51373,.F.);
#72007=ORIENTED_EDGE('',*,*,#51370,.F.);
#72008=ORIENTED_EDGE('',*,*,#51378,.F.);
#72009=ORIENTED_EDGE('',*,*,#51388,.F.);
#72010=ORIENTED_EDGE('',*,*,#51385,.F.);
#72011=ORIENTED_EDGE('',*,*,#51382,.F.);
#72012=ORIENTED_EDGE('',*,*,#51390,.F.);
#72013=ORIENTED_EDGE('',*,*,#51400,.F.);
#72014=ORIENTED_EDGE('',*,*,#51397,.F.);
#72015=ORIENTED_EDGE('',*,*,#51394,.F.);
#72016=ORIENTED_EDGE('',*,*,#51402,.F.);
#72017=ORIENTED_EDGE('',*,*,#51412,.F.);
#72018=ORIENTED_EDGE('',*,*,#51409,.F.);
#72019=ORIENTED_EDGE('',*,*,#51406,.F.);
#72020=ORIENTED_EDGE('',*,*,#51414,.F.);
#72021=ORIENTED_EDGE('',*,*,#51424,.F.);
#72022=ORIENTED_EDGE('',*,*,#51421,.F.);
#72023=ORIENTED_EDGE('',*,*,#51418,.F.);
#72024=ORIENTED_EDGE('',*,*,#51426,.F.);
#72025=ORIENTED_EDGE('',*,*,#51436,.F.);
#72026=ORIENTED_EDGE('',*,*,#51433,.F.);
#72027=ORIENTED_EDGE('',*,*,#51430,.F.);
#72028=ORIENTED_EDGE('',*,*,#51438,.F.);
#72029=ORIENTED_EDGE('',*,*,#51448,.F.);
#72030=ORIENTED_EDGE('',*,*,#51445,.F.);
#72031=ORIENTED_EDGE('',*,*,#51442,.F.);
#72032=ORIENTED_EDGE('',*,*,#51450,.F.);
#72033=ORIENTED_EDGE('',*,*,#51460,.F.);
#72034=ORIENTED_EDGE('',*,*,#51457,.F.);
#72035=ORIENTED_EDGE('',*,*,#51454,.F.);
#72036=ORIENTED_EDGE('',*,*,#51462,.F.);
#72037=ORIENTED_EDGE('',*,*,#51472,.F.);
#72038=ORIENTED_EDGE('',*,*,#51469,.F.);
#72039=ORIENTED_EDGE('',*,*,#51466,.F.);
#72040=ORIENTED_EDGE('',*,*,#51474,.F.);
#72041=ORIENTED_EDGE('',*,*,#51484,.F.);
#72042=ORIENTED_EDGE('',*,*,#51481,.F.);
#72043=ORIENTED_EDGE('',*,*,#51478,.F.);
#72044=ORIENTED_EDGE('',*,*,#51486,.F.);
#72045=ORIENTED_EDGE('',*,*,#51496,.F.);
#72046=ORIENTED_EDGE('',*,*,#51493,.F.);
#72047=ORIENTED_EDGE('',*,*,#51490,.F.);
#72048=ORIENTED_EDGE('',*,*,#51498,.F.);
#72049=ORIENTED_EDGE('',*,*,#51508,.F.);
#72050=ORIENTED_EDGE('',*,*,#51505,.F.);
#72051=ORIENTED_EDGE('',*,*,#51502,.F.);
#72052=ORIENTED_EDGE('',*,*,#51510,.F.);
#72053=ORIENTED_EDGE('',*,*,#51520,.F.);
#72054=ORIENTED_EDGE('',*,*,#51517,.F.);
#72055=ORIENTED_EDGE('',*,*,#51514,.F.);
#72056=ORIENTED_EDGE('',*,*,#51522,.F.);
#72057=ORIENTED_EDGE('',*,*,#51532,.F.);
#72058=ORIENTED_EDGE('',*,*,#51529,.F.);
#72059=ORIENTED_EDGE('',*,*,#51526,.F.);
#72060=ORIENTED_EDGE('',*,*,#51534,.F.);
#72061=ORIENTED_EDGE('',*,*,#51544,.F.);
#72062=ORIENTED_EDGE('',*,*,#51541,.F.);
#72063=ORIENTED_EDGE('',*,*,#51538,.F.);
#72064=ORIENTED_EDGE('',*,*,#51546,.F.);
#72065=ORIENTED_EDGE('',*,*,#51556,.F.);
#72066=ORIENTED_EDGE('',*,*,#51553,.F.);
#72067=ORIENTED_EDGE('',*,*,#51550,.F.);
#72068=ORIENTED_EDGE('',*,*,#51558,.F.);
#72069=ORIENTED_EDGE('',*,*,#51568,.F.);
#72070=ORIENTED_EDGE('',*,*,#51565,.F.);
#72071=ORIENTED_EDGE('',*,*,#51562,.F.);
#72072=ORIENTED_EDGE('',*,*,#51570,.F.);
#72073=ORIENTED_EDGE('',*,*,#51580,.F.);
#72074=ORIENTED_EDGE('',*,*,#51577,.F.);
#72075=ORIENTED_EDGE('',*,*,#51574,.F.);
#72076=ORIENTED_EDGE('',*,*,#51582,.F.);
#72077=ORIENTED_EDGE('',*,*,#51592,.F.);
#72078=ORIENTED_EDGE('',*,*,#51589,.F.);
#72079=ORIENTED_EDGE('',*,*,#51586,.F.);
#72080=ORIENTED_EDGE('',*,*,#51594,.F.);
#72081=ORIENTED_EDGE('',*,*,#51604,.F.);
#72082=ORIENTED_EDGE('',*,*,#51601,.F.);
#72083=ORIENTED_EDGE('',*,*,#51598,.F.);
#72084=ORIENTED_EDGE('',*,*,#51606,.F.);
#72085=ORIENTED_EDGE('',*,*,#51616,.F.);
#72086=ORIENTED_EDGE('',*,*,#51613,.F.);
#72087=ORIENTED_EDGE('',*,*,#51610,.F.);
#72088=ORIENTED_EDGE('',*,*,#51618,.F.);
#72089=ORIENTED_EDGE('',*,*,#51628,.F.);
#72090=ORIENTED_EDGE('',*,*,#51625,.F.);
#72091=ORIENTED_EDGE('',*,*,#51622,.F.);
#72092=ORIENTED_EDGE('',*,*,#51630,.F.);
#72093=ORIENTED_EDGE('',*,*,#51640,.F.);
#72094=ORIENTED_EDGE('',*,*,#51637,.F.);
#72095=ORIENTED_EDGE('',*,*,#51634,.F.);
#72096=ORIENTED_EDGE('',*,*,#51642,.F.);
#72097=ORIENTED_EDGE('',*,*,#51652,.F.);
#72098=ORIENTED_EDGE('',*,*,#51649,.F.);
#72099=ORIENTED_EDGE('',*,*,#51646,.F.);
#72100=ORIENTED_EDGE('',*,*,#51654,.F.);
#72101=ORIENTED_EDGE('',*,*,#51664,.F.);
#72102=ORIENTED_EDGE('',*,*,#51661,.F.);
#72103=ORIENTED_EDGE('',*,*,#51658,.F.);
#72104=ORIENTED_EDGE('',*,*,#51666,.F.);
#72105=ORIENTED_EDGE('',*,*,#51676,.F.);
#72106=ORIENTED_EDGE('',*,*,#51673,.F.);
#72107=ORIENTED_EDGE('',*,*,#51670,.F.);
#72108=ORIENTED_EDGE('',*,*,#51678,.F.);
#72109=ORIENTED_EDGE('',*,*,#51688,.F.);
#72110=ORIENTED_EDGE('',*,*,#51685,.F.);
#72111=ORIENTED_EDGE('',*,*,#51682,.F.);
#72112=ORIENTED_EDGE('',*,*,#51690,.F.);
#72113=ORIENTED_EDGE('',*,*,#51700,.F.);
#72114=ORIENTED_EDGE('',*,*,#51697,.F.);
#72115=ORIENTED_EDGE('',*,*,#51694,.F.);
#72116=ORIENTED_EDGE('',*,*,#51702,.F.);
#72117=ORIENTED_EDGE('',*,*,#51712,.F.);
#72118=ORIENTED_EDGE('',*,*,#51709,.F.);
#72119=ORIENTED_EDGE('',*,*,#51706,.F.);
#72120=ORIENTED_EDGE('',*,*,#51714,.F.);
#72121=ORIENTED_EDGE('',*,*,#51724,.F.);
#72122=ORIENTED_EDGE('',*,*,#51721,.F.);
#72123=ORIENTED_EDGE('',*,*,#51718,.F.);
#72124=ORIENTED_EDGE('',*,*,#51726,.F.);
#72125=ORIENTED_EDGE('',*,*,#51736,.F.);
#72126=ORIENTED_EDGE('',*,*,#51733,.F.);
#72127=ORIENTED_EDGE('',*,*,#51730,.F.);
#72128=ORIENTED_EDGE('',*,*,#51738,.F.);
#72129=ORIENTED_EDGE('',*,*,#51748,.F.);
#72130=ORIENTED_EDGE('',*,*,#51745,.F.);
#72131=ORIENTED_EDGE('',*,*,#51742,.F.);
#72132=ORIENTED_EDGE('',*,*,#51750,.F.);
#72133=ORIENTED_EDGE('',*,*,#51760,.F.);
#72134=ORIENTED_EDGE('',*,*,#51757,.F.);
#72135=ORIENTED_EDGE('',*,*,#51754,.F.);
#72136=ORIENTED_EDGE('',*,*,#51762,.F.);
#72137=ORIENTED_EDGE('',*,*,#51772,.F.);
#72138=ORIENTED_EDGE('',*,*,#51769,.F.);
#72139=ORIENTED_EDGE('',*,*,#51766,.F.);
#72140=ORIENTED_EDGE('',*,*,#51774,.F.);
#72141=ORIENTED_EDGE('',*,*,#51784,.F.);
#72142=ORIENTED_EDGE('',*,*,#51781,.F.);
#72143=ORIENTED_EDGE('',*,*,#51778,.F.);
#72144=ORIENTED_EDGE('',*,*,#51786,.F.);
#72145=ORIENTED_EDGE('',*,*,#51796,.F.);
#72146=ORIENTED_EDGE('',*,*,#51793,.F.);
#72147=ORIENTED_EDGE('',*,*,#51790,.F.);
#72148=ORIENTED_EDGE('',*,*,#51798,.F.);
#72149=ORIENTED_EDGE('',*,*,#51808,.F.);
#72150=ORIENTED_EDGE('',*,*,#51805,.F.);
#72151=ORIENTED_EDGE('',*,*,#51802,.F.);
#72152=ORIENTED_EDGE('',*,*,#51810,.F.);
#72153=ORIENTED_EDGE('',*,*,#51820,.F.);
#72154=ORIENTED_EDGE('',*,*,#51817,.F.);
#72155=ORIENTED_EDGE('',*,*,#51814,.F.);
#72156=ORIENTED_EDGE('',*,*,#51822,.F.);
#72157=ORIENTED_EDGE('',*,*,#51832,.F.);
#72158=ORIENTED_EDGE('',*,*,#51829,.F.);
#72159=ORIENTED_EDGE('',*,*,#51826,.F.);
#72160=ORIENTED_EDGE('',*,*,#51834,.F.);
#72161=ORIENTED_EDGE('',*,*,#51844,.F.);
#72162=ORIENTED_EDGE('',*,*,#51841,.F.);
#72163=ORIENTED_EDGE('',*,*,#51838,.F.);
#72164=ORIENTED_EDGE('',*,*,#51846,.F.);
#72165=ORIENTED_EDGE('',*,*,#51856,.F.);
#72166=ORIENTED_EDGE('',*,*,#51853,.F.);
#72167=ORIENTED_EDGE('',*,*,#51850,.F.);
#72168=ORIENTED_EDGE('',*,*,#51858,.F.);
#72169=ORIENTED_EDGE('',*,*,#51868,.F.);
#72170=ORIENTED_EDGE('',*,*,#51865,.F.);
#72171=ORIENTED_EDGE('',*,*,#51862,.F.);
#72172=ORIENTED_EDGE('',*,*,#51870,.F.);
#72173=ORIENTED_EDGE('',*,*,#51880,.F.);
#72174=ORIENTED_EDGE('',*,*,#51877,.F.);
#72175=ORIENTED_EDGE('',*,*,#51874,.F.);
#72176=ORIENTED_EDGE('',*,*,#51882,.F.);
#72177=ORIENTED_EDGE('',*,*,#51892,.F.);
#72178=ORIENTED_EDGE('',*,*,#51889,.F.);
#72179=ORIENTED_EDGE('',*,*,#51886,.F.);
#72180=ORIENTED_EDGE('',*,*,#51894,.F.);
#72181=ORIENTED_EDGE('',*,*,#51904,.F.);
#72182=ORIENTED_EDGE('',*,*,#51901,.F.);
#72183=ORIENTED_EDGE('',*,*,#51898,.F.);
#72184=ORIENTED_EDGE('',*,*,#51906,.F.);
#72185=ORIENTED_EDGE('',*,*,#51916,.F.);
#72186=ORIENTED_EDGE('',*,*,#51913,.F.);
#72187=ORIENTED_EDGE('',*,*,#51910,.F.);
#72188=ORIENTED_EDGE('',*,*,#51918,.F.);
#72189=ORIENTED_EDGE('',*,*,#51928,.F.);
#72190=ORIENTED_EDGE('',*,*,#51925,.F.);
#72191=ORIENTED_EDGE('',*,*,#51922,.F.);
#72192=ORIENTED_EDGE('',*,*,#51930,.F.);
#72193=ORIENTED_EDGE('',*,*,#51940,.F.);
#72194=ORIENTED_EDGE('',*,*,#51937,.F.);
#72195=ORIENTED_EDGE('',*,*,#51934,.F.);
#72196=ORIENTED_EDGE('',*,*,#51942,.F.);
#72197=ORIENTED_EDGE('',*,*,#51952,.F.);
#72198=ORIENTED_EDGE('',*,*,#51949,.F.);
#72199=ORIENTED_EDGE('',*,*,#51946,.F.);
#72200=ORIENTED_EDGE('',*,*,#51954,.F.);
#72201=ORIENTED_EDGE('',*,*,#51964,.F.);
#72202=ORIENTED_EDGE('',*,*,#51961,.F.);
#72203=ORIENTED_EDGE('',*,*,#51958,.F.);
#72204=ORIENTED_EDGE('',*,*,#51966,.F.);
#72205=ORIENTED_EDGE('',*,*,#51977,.F.);
#72206=ORIENTED_EDGE('',*,*,#51975,.F.);
#72207=ORIENTED_EDGE('',*,*,#51973,.F.);
#72208=ORIENTED_EDGE('',*,*,#51978,.F.);
#72209=ORIENTED_EDGE('',*,*,#43491,.F.);
#72210=ORIENTED_EDGE('',*,*,#43495,.T.);
#72211=ORIENTED_EDGE('',*,*,#43486,.F.);
#72212=ORIENTED_EDGE('',*,*,#43470,.F.);
#72213=ORIENTED_EDGE('',*,*,#43456,.T.);
#72214=ORIENTED_EDGE('',*,*,#51979,.T.);
#72215=ORIENTED_EDGE('',*,*,#43462,.T.);
#72216=ORIENTED_EDGE('',*,*,#43468,.F.);
#72217=ORIENTED_EDGE('',*,*,#43482,.F.);
#72218=ORIENTED_EDGE('',*,*,#51980,.T.);
#72219=ORIENTED_EDGE('',*,*,#43458,.F.);
#72220=ORIENTED_EDGE('',*,*,#43472,.T.);
#72221=ORIENTED_EDGE('',*,*,#43485,.T.);
#72222=ORIENTED_EDGE('',*,*,#51981,.F.);
#72223=ORIENTED_EDGE('',*,*,#43483,.T.);
#72224=ORIENTED_EDGE('',*,*,#43469,.T.);
#72225=ORIENTED_EDGE('',*,*,#43460,.F.);
#72226=ORIENTED_EDGE('',*,*,#51982,.F.);
#72227=ORIENTED_EDGE('',*,*,#43487,.F.);
#72228=ORIENTED_EDGE('',*,*,#51979,.F.);
#72229=ORIENTED_EDGE('',*,*,#43459,.F.);
#72230=ORIENTED_EDGE('',*,*,#51981,.T.);
#72231=ORIENTED_EDGE('',*,*,#43463,.F.);
#72232=ORIENTED_EDGE('',*,*,#51980,.F.);
#72233=ORIENTED_EDGE('',*,*,#43484,.F.);
#72234=ORIENTED_EDGE('',*,*,#51982,.T.);
#72235=ORIENTED_EDGE('',*,*,#43489,.T.);
#72236=ORIENTED_EDGE('',*,*,#43447,.T.);
#72237=ORIENTED_EDGE('',*,*,#43466,.F.);
#72238=ORIENTED_EDGE('',*,*,#51983,.F.);
#72239=ORIENTED_EDGE('',*,*,#51984,.F.);
#72240=ORIENTED_EDGE('',*,*,#43449,.F.);
#72241=ORIENTED_EDGE('',*,*,#43455,.F.);
#72242=ORIENTED_EDGE('',*,*,#43443,.T.);
#72243=ORIENTED_EDGE('',*,*,#43480,.T.);
#72244=ORIENTED_EDGE('',*,*,#43477,.T.);
#72245=ORIENTED_EDGE('',*,*,#43464,.T.);
#72246=ORIENTED_EDGE('',*,*,#43445,.F.);
#72247=ORIENTED_EDGE('',*,*,#43488,.F.);
#72248=ORIENTED_EDGE('',*,*,#51985,.T.);
#72249=ORIENTED_EDGE('',*,*,#43441,.F.);
#72250=ORIENTED_EDGE('',*,*,#43454,.T.);
#72251=ORIENTED_EDGE('',*,*,#43451,.T.);
#72252=ORIENTED_EDGE('',*,*,#51986,.T.);
#72253=ORIENTED_EDGE('',*,*,#43475,.F.);
#72254=ORIENTED_EDGE('',*,*,#43481,.F.);
#72255=ORIENTED_EDGE('',*,*,#43465,.F.);
#72256=ORIENTED_EDGE('',*,*,#51985,.F.);
#72257=ORIENTED_EDGE('',*,*,#43490,.F.);
#72258=ORIENTED_EDGE('',*,*,#51983,.T.);
#72259=ORIENTED_EDGE('',*,*,#51986,.F.);
#72260=ORIENTED_EDGE('',*,*,#43450,.F.);
#72261=ORIENTED_EDGE('',*,*,#51984,.T.);
#72262=ORIENTED_EDGE('',*,*,#43476,.F.);
#72263=ORIENTED_EDGE('',*,*,#43434,.F.);
#72264=ORIENTED_EDGE('',*,*,#51987,.T.);
#72265=ORIENTED_EDGE('',*,*,#51987,.F.);
#72266=ORIENTED_EDGE('',*,*,#51988,.F.);
#72267=ORIENTED_EDGE('',*,*,#51989,.F.);
#72268=ORIENTED_EDGE('',*,*,#51990,.F.);
#72269=ORIENTED_EDGE('',*,*,#51991,.F.);
#72270=ORIENTED_EDGE('',*,*,#45129,.F.);
#72271=ORIENTED_EDGE('',*,*,#45133,.F.);
#72272=ORIENTED_EDGE('',*,*,#45136,.F.);
#72273=ORIENTED_EDGE('',*,*,#45138,.F.);
#72274=ORIENTED_EDGE('',*,*,#45117,.F.);
#72275=ORIENTED_EDGE('',*,*,#45121,.F.);
#72276=ORIENTED_EDGE('',*,*,#45124,.F.);
#72277=ORIENTED_EDGE('',*,*,#45126,.F.);
#72278=ORIENTED_EDGE('',*,*,#45105,.F.);
#72279=ORIENTED_EDGE('',*,*,#45109,.F.);
#72280=ORIENTED_EDGE('',*,*,#45112,.F.);
#72281=ORIENTED_EDGE('',*,*,#45114,.F.);
#72282=ORIENTED_EDGE('',*,*,#45093,.F.);
#72283=ORIENTED_EDGE('',*,*,#45097,.F.);
#72284=ORIENTED_EDGE('',*,*,#45100,.F.);
#72285=ORIENTED_EDGE('',*,*,#45102,.F.);
#72286=ORIENTED_EDGE('',*,*,#45081,.F.);
#72287=ORIENTED_EDGE('',*,*,#45085,.F.);
#72288=ORIENTED_EDGE('',*,*,#45088,.F.);
#72289=ORIENTED_EDGE('',*,*,#45090,.F.);
#72290=ORIENTED_EDGE('',*,*,#45069,.F.);
#72291=ORIENTED_EDGE('',*,*,#45073,.F.);
#72292=ORIENTED_EDGE('',*,*,#45076,.F.);
#72293=ORIENTED_EDGE('',*,*,#45078,.F.);
#72294=ORIENTED_EDGE('',*,*,#45057,.F.);
#72295=ORIENTED_EDGE('',*,*,#45061,.F.);
#72296=ORIENTED_EDGE('',*,*,#45064,.F.);
#72297=ORIENTED_EDGE('',*,*,#45066,.F.);
#72298=ORIENTED_EDGE('',*,*,#45045,.F.);
#72299=ORIENTED_EDGE('',*,*,#45049,.F.);
#72300=ORIENTED_EDGE('',*,*,#45052,.F.);
#72301=ORIENTED_EDGE('',*,*,#45054,.F.);
#72302=ORIENTED_EDGE('',*,*,#45033,.F.);
#72303=ORIENTED_EDGE('',*,*,#45037,.F.);
#72304=ORIENTED_EDGE('',*,*,#45040,.F.);
#72305=ORIENTED_EDGE('',*,*,#45042,.F.);
#72306=ORIENTED_EDGE('',*,*,#45021,.F.);
#72307=ORIENTED_EDGE('',*,*,#45025,.F.);
#72308=ORIENTED_EDGE('',*,*,#45028,.F.);
#72309=ORIENTED_EDGE('',*,*,#45030,.F.);
#72310=ORIENTED_EDGE('',*,*,#45009,.F.);
#72311=ORIENTED_EDGE('',*,*,#45013,.F.);
#72312=ORIENTED_EDGE('',*,*,#45016,.F.);
#72313=ORIENTED_EDGE('',*,*,#45018,.F.);
#72314=ORIENTED_EDGE('',*,*,#44997,.F.);
#72315=ORIENTED_EDGE('',*,*,#45001,.F.);
#72316=ORIENTED_EDGE('',*,*,#45004,.F.);
#72317=ORIENTED_EDGE('',*,*,#45006,.F.);
#72318=ORIENTED_EDGE('',*,*,#44985,.F.);
#72319=ORIENTED_EDGE('',*,*,#44989,.F.);
#72320=ORIENTED_EDGE('',*,*,#44992,.F.);
#72321=ORIENTED_EDGE('',*,*,#44994,.F.);
#72322=ORIENTED_EDGE('',*,*,#44973,.F.);
#72323=ORIENTED_EDGE('',*,*,#44977,.F.);
#72324=ORIENTED_EDGE('',*,*,#44980,.F.);
#72325=ORIENTED_EDGE('',*,*,#44982,.F.);
#72326=ORIENTED_EDGE('',*,*,#44961,.F.);
#72327=ORIENTED_EDGE('',*,*,#44965,.F.);
#72328=ORIENTED_EDGE('',*,*,#44968,.F.);
#72329=ORIENTED_EDGE('',*,*,#44970,.F.);
#72330=ORIENTED_EDGE('',*,*,#44949,.F.);
#72331=ORIENTED_EDGE('',*,*,#44953,.F.);
#72332=ORIENTED_EDGE('',*,*,#44956,.F.);
#72333=ORIENTED_EDGE('',*,*,#44958,.F.);
#72334=ORIENTED_EDGE('',*,*,#44937,.F.);
#72335=ORIENTED_EDGE('',*,*,#44941,.F.);
#72336=ORIENTED_EDGE('',*,*,#44944,.F.);
#72337=ORIENTED_EDGE('',*,*,#44946,.F.);
#72338=ORIENTED_EDGE('',*,*,#44925,.F.);
#72339=ORIENTED_EDGE('',*,*,#44929,.F.);
#72340=ORIENTED_EDGE('',*,*,#44932,.F.);
#72341=ORIENTED_EDGE('',*,*,#44934,.F.);
#72342=ORIENTED_EDGE('',*,*,#44913,.F.);
#72343=ORIENTED_EDGE('',*,*,#44917,.F.);
#72344=ORIENTED_EDGE('',*,*,#44920,.F.);
#72345=ORIENTED_EDGE('',*,*,#44922,.F.);
#72346=ORIENTED_EDGE('',*,*,#44901,.F.);
#72347=ORIENTED_EDGE('',*,*,#44905,.F.);
#72348=ORIENTED_EDGE('',*,*,#44908,.F.);
#72349=ORIENTED_EDGE('',*,*,#44910,.F.);
#72350=ORIENTED_EDGE('',*,*,#44889,.F.);
#72351=ORIENTED_EDGE('',*,*,#44893,.F.);
#72352=ORIENTED_EDGE('',*,*,#44896,.F.);
#72353=ORIENTED_EDGE('',*,*,#44898,.F.);
#72354=ORIENTED_EDGE('',*,*,#44877,.F.);
#72355=ORIENTED_EDGE('',*,*,#44881,.F.);
#72356=ORIENTED_EDGE('',*,*,#44884,.F.);
#72357=ORIENTED_EDGE('',*,*,#44886,.F.);
#72358=ORIENTED_EDGE('',*,*,#44865,.F.);
#72359=ORIENTED_EDGE('',*,*,#44869,.F.);
#72360=ORIENTED_EDGE('',*,*,#44872,.F.);
#72361=ORIENTED_EDGE('',*,*,#44874,.F.);
#72362=ORIENTED_EDGE('',*,*,#44853,.F.);
#72363=ORIENTED_EDGE('',*,*,#44857,.F.);
#72364=ORIENTED_EDGE('',*,*,#44860,.F.);
#72365=ORIENTED_EDGE('',*,*,#44862,.F.);
#72366=ORIENTED_EDGE('',*,*,#44841,.F.);
#72367=ORIENTED_EDGE('',*,*,#44845,.F.);
#72368=ORIENTED_EDGE('',*,*,#44848,.F.);
#72369=ORIENTED_EDGE('',*,*,#44850,.F.);
#72370=ORIENTED_EDGE('',*,*,#44829,.F.);
#72371=ORIENTED_EDGE('',*,*,#44833,.F.);
#72372=ORIENTED_EDGE('',*,*,#44836,.F.);
#72373=ORIENTED_EDGE('',*,*,#44838,.F.);
#72374=ORIENTED_EDGE('',*,*,#44817,.F.);
#72375=ORIENTED_EDGE('',*,*,#44821,.F.);
#72376=ORIENTED_EDGE('',*,*,#44824,.F.);
#72377=ORIENTED_EDGE('',*,*,#44826,.F.);
#72378=ORIENTED_EDGE('',*,*,#44805,.F.);
#72379=ORIENTED_EDGE('',*,*,#44809,.F.);
#72380=ORIENTED_EDGE('',*,*,#44812,.F.);
#72381=ORIENTED_EDGE('',*,*,#44814,.F.);
#72382=ORIENTED_EDGE('',*,*,#44793,.F.);
#72383=ORIENTED_EDGE('',*,*,#44797,.F.);
#72384=ORIENTED_EDGE('',*,*,#44800,.F.);
#72385=ORIENTED_EDGE('',*,*,#44802,.F.);
#72386=ORIENTED_EDGE('',*,*,#44781,.F.);
#72387=ORIENTED_EDGE('',*,*,#44785,.F.);
#72388=ORIENTED_EDGE('',*,*,#44788,.F.);
#72389=ORIENTED_EDGE('',*,*,#44790,.F.);
#72390=ORIENTED_EDGE('',*,*,#44769,.F.);
#72391=ORIENTED_EDGE('',*,*,#44773,.F.);
#72392=ORIENTED_EDGE('',*,*,#44776,.F.);
#72393=ORIENTED_EDGE('',*,*,#44778,.F.);
#72394=ORIENTED_EDGE('',*,*,#44757,.F.);
#72395=ORIENTED_EDGE('',*,*,#44761,.F.);
#72396=ORIENTED_EDGE('',*,*,#44764,.F.);
#72397=ORIENTED_EDGE('',*,*,#44766,.F.);
#72398=ORIENTED_EDGE('',*,*,#44745,.F.);
#72399=ORIENTED_EDGE('',*,*,#44749,.F.);
#72400=ORIENTED_EDGE('',*,*,#44752,.F.);
#72401=ORIENTED_EDGE('',*,*,#44754,.F.);
#72402=ORIENTED_EDGE('',*,*,#44733,.F.);
#72403=ORIENTED_EDGE('',*,*,#44737,.F.);
#72404=ORIENTED_EDGE('',*,*,#44740,.F.);
#72405=ORIENTED_EDGE('',*,*,#44742,.F.);
#72406=ORIENTED_EDGE('',*,*,#44721,.F.);
#72407=ORIENTED_EDGE('',*,*,#44725,.F.);
#72408=ORIENTED_EDGE('',*,*,#44728,.F.);
#72409=ORIENTED_EDGE('',*,*,#44730,.F.);
#72410=ORIENTED_EDGE('',*,*,#44709,.F.);
#72411=ORIENTED_EDGE('',*,*,#44713,.F.);
#72412=ORIENTED_EDGE('',*,*,#44716,.F.);
#72413=ORIENTED_EDGE('',*,*,#44718,.F.);
#72414=ORIENTED_EDGE('',*,*,#44697,.F.);
#72415=ORIENTED_EDGE('',*,*,#44701,.F.);
#72416=ORIENTED_EDGE('',*,*,#44704,.F.);
#72417=ORIENTED_EDGE('',*,*,#44706,.F.);
#72418=ORIENTED_EDGE('',*,*,#44685,.F.);
#72419=ORIENTED_EDGE('',*,*,#44689,.F.);
#72420=ORIENTED_EDGE('',*,*,#44692,.F.);
#72421=ORIENTED_EDGE('',*,*,#44694,.F.);
#72422=ORIENTED_EDGE('',*,*,#44673,.F.);
#72423=ORIENTED_EDGE('',*,*,#44677,.F.);
#72424=ORIENTED_EDGE('',*,*,#44680,.F.);
#72425=ORIENTED_EDGE('',*,*,#44682,.F.);
#72426=ORIENTED_EDGE('',*,*,#44661,.F.);
#72427=ORIENTED_EDGE('',*,*,#44665,.F.);
#72428=ORIENTED_EDGE('',*,*,#44668,.F.);
#72429=ORIENTED_EDGE('',*,*,#44670,.F.);
#72430=ORIENTED_EDGE('',*,*,#44649,.F.);
#72431=ORIENTED_EDGE('',*,*,#44653,.F.);
#72432=ORIENTED_EDGE('',*,*,#44656,.F.);
#72433=ORIENTED_EDGE('',*,*,#44658,.F.);
#72434=ORIENTED_EDGE('',*,*,#44637,.F.);
#72435=ORIENTED_EDGE('',*,*,#44641,.F.);
#72436=ORIENTED_EDGE('',*,*,#44644,.F.);
#72437=ORIENTED_EDGE('',*,*,#44646,.F.);
#72438=ORIENTED_EDGE('',*,*,#44625,.F.);
#72439=ORIENTED_EDGE('',*,*,#44629,.F.);
#72440=ORIENTED_EDGE('',*,*,#44632,.F.);
#72441=ORIENTED_EDGE('',*,*,#44634,.F.);
#72442=ORIENTED_EDGE('',*,*,#44613,.F.);
#72443=ORIENTED_EDGE('',*,*,#44617,.F.);
#72444=ORIENTED_EDGE('',*,*,#44620,.F.);
#72445=ORIENTED_EDGE('',*,*,#44622,.F.);
#72446=ORIENTED_EDGE('',*,*,#44601,.F.);
#72447=ORIENTED_EDGE('',*,*,#44605,.F.);
#72448=ORIENTED_EDGE('',*,*,#44608,.F.);
#72449=ORIENTED_EDGE('',*,*,#44610,.F.);
#72450=ORIENTED_EDGE('',*,*,#44589,.F.);
#72451=ORIENTED_EDGE('',*,*,#44593,.F.);
#72452=ORIENTED_EDGE('',*,*,#44596,.F.);
#72453=ORIENTED_EDGE('',*,*,#44598,.F.);
#72454=ORIENTED_EDGE('',*,*,#44577,.F.);
#72455=ORIENTED_EDGE('',*,*,#44581,.F.);
#72456=ORIENTED_EDGE('',*,*,#44584,.F.);
#72457=ORIENTED_EDGE('',*,*,#44586,.F.);
#72458=ORIENTED_EDGE('',*,*,#44565,.F.);
#72459=ORIENTED_EDGE('',*,*,#44569,.F.);
#72460=ORIENTED_EDGE('',*,*,#44572,.F.);
#72461=ORIENTED_EDGE('',*,*,#44574,.F.);
#72462=ORIENTED_EDGE('',*,*,#44553,.F.);
#72463=ORIENTED_EDGE('',*,*,#44557,.F.);
#72464=ORIENTED_EDGE('',*,*,#44560,.F.);
#72465=ORIENTED_EDGE('',*,*,#44562,.F.);
#72466=ORIENTED_EDGE('',*,*,#44541,.F.);
#72467=ORIENTED_EDGE('',*,*,#44545,.F.);
#72468=ORIENTED_EDGE('',*,*,#44548,.F.);
#72469=ORIENTED_EDGE('',*,*,#44550,.F.);
#72470=ORIENTED_EDGE('',*,*,#44529,.F.);
#72471=ORIENTED_EDGE('',*,*,#44533,.F.);
#72472=ORIENTED_EDGE('',*,*,#44536,.F.);
#72473=ORIENTED_EDGE('',*,*,#44538,.F.);
#72474=ORIENTED_EDGE('',*,*,#44517,.F.);
#72475=ORIENTED_EDGE('',*,*,#44521,.F.);
#72476=ORIENTED_EDGE('',*,*,#44524,.F.);
#72477=ORIENTED_EDGE('',*,*,#44526,.F.);
#72478=ORIENTED_EDGE('',*,*,#44505,.F.);
#72479=ORIENTED_EDGE('',*,*,#44509,.F.);
#72480=ORIENTED_EDGE('',*,*,#44512,.F.);
#72481=ORIENTED_EDGE('',*,*,#44514,.F.);
#72482=ORIENTED_EDGE('',*,*,#44493,.F.);
#72483=ORIENTED_EDGE('',*,*,#44497,.F.);
#72484=ORIENTED_EDGE('',*,*,#44500,.F.);
#72485=ORIENTED_EDGE('',*,*,#44502,.F.);
#72486=ORIENTED_EDGE('',*,*,#44481,.F.);
#72487=ORIENTED_EDGE('',*,*,#44485,.F.);
#72488=ORIENTED_EDGE('',*,*,#44488,.F.);
#72489=ORIENTED_EDGE('',*,*,#44490,.F.);
#72490=ORIENTED_EDGE('',*,*,#44469,.F.);
#72491=ORIENTED_EDGE('',*,*,#44473,.F.);
#72492=ORIENTED_EDGE('',*,*,#44476,.F.);
#72493=ORIENTED_EDGE('',*,*,#44478,.F.);
#72494=ORIENTED_EDGE('',*,*,#44457,.F.);
#72495=ORIENTED_EDGE('',*,*,#44461,.F.);
#72496=ORIENTED_EDGE('',*,*,#44464,.F.);
#72497=ORIENTED_EDGE('',*,*,#44466,.F.);
#72498=ORIENTED_EDGE('',*,*,#44445,.F.);
#72499=ORIENTED_EDGE('',*,*,#44449,.F.);
#72500=ORIENTED_EDGE('',*,*,#44452,.F.);
#72501=ORIENTED_EDGE('',*,*,#44454,.F.);
#72502=ORIENTED_EDGE('',*,*,#44433,.F.);
#72503=ORIENTED_EDGE('',*,*,#44437,.F.);
#72504=ORIENTED_EDGE('',*,*,#44440,.F.);
#72505=ORIENTED_EDGE('',*,*,#44442,.F.);
#72506=ORIENTED_EDGE('',*,*,#44421,.F.);
#72507=ORIENTED_EDGE('',*,*,#44425,.F.);
#72508=ORIENTED_EDGE('',*,*,#44428,.F.);
#72509=ORIENTED_EDGE('',*,*,#44430,.F.);
#72510=ORIENTED_EDGE('',*,*,#44409,.F.);
#72511=ORIENTED_EDGE('',*,*,#44413,.F.);
#72512=ORIENTED_EDGE('',*,*,#44416,.F.);
#72513=ORIENTED_EDGE('',*,*,#44418,.F.);
#72514=ORIENTED_EDGE('',*,*,#44397,.F.);
#72515=ORIENTED_EDGE('',*,*,#44401,.F.);
#72516=ORIENTED_EDGE('',*,*,#44404,.F.);
#72517=ORIENTED_EDGE('',*,*,#44406,.F.);
#72518=ORIENTED_EDGE('',*,*,#44385,.F.);
#72519=ORIENTED_EDGE('',*,*,#44389,.F.);
#72520=ORIENTED_EDGE('',*,*,#44392,.F.);
#72521=ORIENTED_EDGE('',*,*,#44394,.F.);
#72522=ORIENTED_EDGE('',*,*,#44373,.F.);
#72523=ORIENTED_EDGE('',*,*,#44377,.F.);
#72524=ORIENTED_EDGE('',*,*,#44380,.F.);
#72525=ORIENTED_EDGE('',*,*,#44382,.F.);
#72526=ORIENTED_EDGE('',*,*,#44361,.F.);
#72527=ORIENTED_EDGE('',*,*,#44365,.F.);
#72528=ORIENTED_EDGE('',*,*,#44368,.F.);
#72529=ORIENTED_EDGE('',*,*,#44370,.F.);
#72530=ORIENTED_EDGE('',*,*,#44349,.F.);
#72531=ORIENTED_EDGE('',*,*,#44353,.F.);
#72532=ORIENTED_EDGE('',*,*,#44356,.F.);
#72533=ORIENTED_EDGE('',*,*,#44358,.F.);
#72534=ORIENTED_EDGE('',*,*,#44337,.F.);
#72535=ORIENTED_EDGE('',*,*,#44341,.F.);
#72536=ORIENTED_EDGE('',*,*,#44344,.F.);
#72537=ORIENTED_EDGE('',*,*,#44346,.F.);
#72538=ORIENTED_EDGE('',*,*,#44325,.F.);
#72539=ORIENTED_EDGE('',*,*,#44329,.F.);
#72540=ORIENTED_EDGE('',*,*,#44332,.F.);
#72541=ORIENTED_EDGE('',*,*,#44334,.F.);
#72542=ORIENTED_EDGE('',*,*,#44313,.F.);
#72543=ORIENTED_EDGE('',*,*,#44317,.F.);
#72544=ORIENTED_EDGE('',*,*,#44320,.F.);
#72545=ORIENTED_EDGE('',*,*,#44322,.F.);
#72546=ORIENTED_EDGE('',*,*,#44301,.F.);
#72547=ORIENTED_EDGE('',*,*,#44305,.F.);
#72548=ORIENTED_EDGE('',*,*,#44308,.F.);
#72549=ORIENTED_EDGE('',*,*,#44310,.F.);
#72550=ORIENTED_EDGE('',*,*,#44296,.F.);
#72551=ORIENTED_EDGE('',*,*,#44286,.F.);
#72552=ORIENTED_EDGE('',*,*,#44290,.F.);
#72553=ORIENTED_EDGE('',*,*,#44294,.F.);
#72554=ORIENTED_EDGE('',*,*,#44299,.F.);
#72555=ORIENTED_EDGE('',*,*,#44281,.F.);
#72556=ORIENTED_EDGE('',*,*,#44271,.F.);
#72557=ORIENTED_EDGE('',*,*,#44275,.F.);
#72558=ORIENTED_EDGE('',*,*,#44279,.F.);
#72559=ORIENTED_EDGE('',*,*,#44284,.F.);
#72560=ORIENTED_EDGE('',*,*,#44259,.F.);
#72561=ORIENTED_EDGE('',*,*,#44263,.F.);
#72562=ORIENTED_EDGE('',*,*,#44266,.F.);
#72563=ORIENTED_EDGE('',*,*,#44268,.F.);
#72564=ORIENTED_EDGE('',*,*,#44247,.F.);
#72565=ORIENTED_EDGE('',*,*,#44251,.F.);
#72566=ORIENTED_EDGE('',*,*,#44254,.F.);
#72567=ORIENTED_EDGE('',*,*,#44256,.F.);
#72568=ORIENTED_EDGE('',*,*,#44235,.F.);
#72569=ORIENTED_EDGE('',*,*,#44239,.F.);
#72570=ORIENTED_EDGE('',*,*,#44242,.F.);
#72571=ORIENTED_EDGE('',*,*,#44244,.F.);
#72572=ORIENTED_EDGE('',*,*,#44223,.F.);
#72573=ORIENTED_EDGE('',*,*,#44227,.F.);
#72574=ORIENTED_EDGE('',*,*,#44230,.F.);
#72575=ORIENTED_EDGE('',*,*,#44232,.F.);
#72576=ORIENTED_EDGE('',*,*,#44211,.F.);
#72577=ORIENTED_EDGE('',*,*,#44215,.F.);
#72578=ORIENTED_EDGE('',*,*,#44218,.F.);
#72579=ORIENTED_EDGE('',*,*,#44220,.F.);
#72580=ORIENTED_EDGE('',*,*,#44199,.F.);
#72581=ORIENTED_EDGE('',*,*,#44203,.F.);
#72582=ORIENTED_EDGE('',*,*,#44206,.F.);
#72583=ORIENTED_EDGE('',*,*,#44208,.F.);
#72584=ORIENTED_EDGE('',*,*,#44187,.F.);
#72585=ORIENTED_EDGE('',*,*,#44191,.F.);
#72586=ORIENTED_EDGE('',*,*,#44194,.F.);
#72587=ORIENTED_EDGE('',*,*,#44196,.F.);
#72588=ORIENTED_EDGE('',*,*,#44175,.F.);
#72589=ORIENTED_EDGE('',*,*,#44179,.F.);
#72590=ORIENTED_EDGE('',*,*,#44182,.F.);
#72591=ORIENTED_EDGE('',*,*,#44184,.F.);
#72592=ORIENTED_EDGE('',*,*,#44163,.F.);
#72593=ORIENTED_EDGE('',*,*,#44167,.F.);
#72594=ORIENTED_EDGE('',*,*,#44170,.F.);
#72595=ORIENTED_EDGE('',*,*,#44172,.F.);
#72596=ORIENTED_EDGE('',*,*,#44151,.F.);
#72597=ORIENTED_EDGE('',*,*,#44155,.F.);
#72598=ORIENTED_EDGE('',*,*,#44158,.F.);
#72599=ORIENTED_EDGE('',*,*,#44160,.F.);
#72600=ORIENTED_EDGE('',*,*,#44139,.F.);
#72601=ORIENTED_EDGE('',*,*,#44143,.F.);
#72602=ORIENTED_EDGE('',*,*,#44146,.F.);
#72603=ORIENTED_EDGE('',*,*,#44137,.F.);
#72604=ORIENTED_EDGE('',*,*,#44148,.F.);
#72605=ORIENTED_EDGE('',*,*,#44124,.F.);
#72606=ORIENTED_EDGE('',*,*,#44128,.F.);
#72607=ORIENTED_EDGE('',*,*,#44131,.F.);
#72608=ORIENTED_EDGE('',*,*,#44133,.F.);
#72609=ORIENTED_EDGE('',*,*,#44112,.F.);
#72610=ORIENTED_EDGE('',*,*,#44116,.F.);
#72611=ORIENTED_EDGE('',*,*,#44119,.F.);
#72612=ORIENTED_EDGE('',*,*,#44121,.F.);
#72613=ORIENTED_EDGE('',*,*,#44100,.F.);
#72614=ORIENTED_EDGE('',*,*,#44104,.F.);
#72615=ORIENTED_EDGE('',*,*,#44107,.F.);
#72616=ORIENTED_EDGE('',*,*,#44109,.F.);
#72617=ORIENTED_EDGE('',*,*,#44088,.F.);
#72618=ORIENTED_EDGE('',*,*,#44092,.F.);
#72619=ORIENTED_EDGE('',*,*,#44095,.F.);
#72620=ORIENTED_EDGE('',*,*,#44097,.F.);
#72621=ORIENTED_EDGE('',*,*,#44076,.F.);
#72622=ORIENTED_EDGE('',*,*,#44080,.F.);
#72623=ORIENTED_EDGE('',*,*,#44083,.F.);
#72624=ORIENTED_EDGE('',*,*,#44085,.F.);
#72625=ORIENTED_EDGE('',*,*,#44064,.F.);
#72626=ORIENTED_EDGE('',*,*,#44068,.F.);
#72627=ORIENTED_EDGE('',*,*,#44071,.F.);
#72628=ORIENTED_EDGE('',*,*,#44073,.F.);
#72629=ORIENTED_EDGE('',*,*,#44052,.F.);
#72630=ORIENTED_EDGE('',*,*,#44056,.F.);
#72631=ORIENTED_EDGE('',*,*,#44059,.F.);
#72632=ORIENTED_EDGE('',*,*,#44061,.F.);
#72633=ORIENTED_EDGE('',*,*,#44040,.F.);
#72634=ORIENTED_EDGE('',*,*,#44044,.F.);
#72635=ORIENTED_EDGE('',*,*,#44047,.F.);
#72636=ORIENTED_EDGE('',*,*,#44049,.F.);
#72637=ORIENTED_EDGE('',*,*,#44028,.F.);
#72638=ORIENTED_EDGE('',*,*,#44032,.F.);
#72639=ORIENTED_EDGE('',*,*,#44035,.F.);
#72640=ORIENTED_EDGE('',*,*,#44037,.F.);
#72641=ORIENTED_EDGE('',*,*,#44016,.F.);
#72642=ORIENTED_EDGE('',*,*,#44020,.F.);
#72643=ORIENTED_EDGE('',*,*,#44023,.F.);
#72644=ORIENTED_EDGE('',*,*,#44025,.F.);
#72645=ORIENTED_EDGE('',*,*,#44011,.F.);
#72646=ORIENTED_EDGE('',*,*,#44001,.F.);
#72647=ORIENTED_EDGE('',*,*,#44006,.F.);
#72648=ORIENTED_EDGE('',*,*,#44014,.F.);
#72649=ORIENTED_EDGE('',*,*,#43996,.F.);
#72650=ORIENTED_EDGE('',*,*,#43986,.F.);
#72651=ORIENTED_EDGE('',*,*,#43991,.F.);
#72652=ORIENTED_EDGE('',*,*,#43999,.F.);
#72653=ORIENTED_EDGE('',*,*,#43974,.F.);
#72654=ORIENTED_EDGE('',*,*,#43978,.F.);
#72655=ORIENTED_EDGE('',*,*,#43981,.F.);
#72656=ORIENTED_EDGE('',*,*,#43983,.F.);
#72657=ORIENTED_EDGE('',*,*,#43962,.F.);
#72658=ORIENTED_EDGE('',*,*,#43966,.F.);
#72659=ORIENTED_EDGE('',*,*,#43969,.F.);
#72660=ORIENTED_EDGE('',*,*,#43971,.F.);
#72661=ORIENTED_EDGE('',*,*,#43950,.F.);
#72662=ORIENTED_EDGE('',*,*,#43954,.F.);
#72663=ORIENTED_EDGE('',*,*,#43957,.F.);
#72664=ORIENTED_EDGE('',*,*,#43959,.F.);
#72665=ORIENTED_EDGE('',*,*,#43938,.F.);
#72666=ORIENTED_EDGE('',*,*,#43942,.F.);
#72667=ORIENTED_EDGE('',*,*,#43945,.F.);
#72668=ORIENTED_EDGE('',*,*,#43947,.F.);
#72669=ORIENTED_EDGE('',*,*,#43926,.F.);
#72670=ORIENTED_EDGE('',*,*,#43930,.F.);
#72671=ORIENTED_EDGE('',*,*,#43933,.F.);
#72672=ORIENTED_EDGE('',*,*,#43935,.F.);
#72673=ORIENTED_EDGE('',*,*,#43914,.F.);
#72674=ORIENTED_EDGE('',*,*,#43918,.F.);
#72675=ORIENTED_EDGE('',*,*,#43921,.F.);
#72676=ORIENTED_EDGE('',*,*,#43923,.F.);
#72677=ORIENTED_EDGE('',*,*,#43902,.F.);
#72678=ORIENTED_EDGE('',*,*,#43906,.F.);
#72679=ORIENTED_EDGE('',*,*,#43909,.F.);
#72680=ORIENTED_EDGE('',*,*,#43911,.F.);
#72681=ORIENTED_EDGE('',*,*,#43890,.F.);
#72682=ORIENTED_EDGE('',*,*,#43894,.F.);
#72683=ORIENTED_EDGE('',*,*,#43897,.F.);
#72684=ORIENTED_EDGE('',*,*,#43899,.F.);
#72685=ORIENTED_EDGE('',*,*,#43885,.F.);
#72686=ORIENTED_EDGE('',*,*,#43875,.F.);
#72687=ORIENTED_EDGE('',*,*,#43880,.F.);
#72688=ORIENTED_EDGE('',*,*,#43888,.F.);
#72689=ORIENTED_EDGE('',*,*,#43871,.F.);
#72690=ORIENTED_EDGE('',*,*,#43861,.F.);
#72691=ORIENTED_EDGE('',*,*,#43865,.F.);
#72692=ORIENTED_EDGE('',*,*,#43867,.F.);
#72693=ORIENTED_EDGE('',*,*,#43873,.F.);
#72694=ORIENTED_EDGE('',*,*,#43848,.F.);
#72695=ORIENTED_EDGE('',*,*,#43852,.F.);
#72696=ORIENTED_EDGE('',*,*,#43855,.F.);
#72697=ORIENTED_EDGE('',*,*,#43857,.F.);
#72698=ORIENTED_EDGE('',*,*,#43836,.F.);
#72699=ORIENTED_EDGE('',*,*,#43840,.F.);
#72700=ORIENTED_EDGE('',*,*,#43843,.F.);
#72701=ORIENTED_EDGE('',*,*,#43845,.F.);
#72702=ORIENTED_EDGE('',*,*,#43824,.F.);
#72703=ORIENTED_EDGE('',*,*,#43828,.F.);
#72704=ORIENTED_EDGE('',*,*,#43831,.F.);
#72705=ORIENTED_EDGE('',*,*,#43833,.F.);
#72706=ORIENTED_EDGE('',*,*,#43812,.F.);
#72707=ORIENTED_EDGE('',*,*,#43816,.F.);
#72708=ORIENTED_EDGE('',*,*,#43819,.F.);
#72709=ORIENTED_EDGE('',*,*,#43821,.F.);
#72710=ORIENTED_EDGE('',*,*,#43800,.F.);
#72711=ORIENTED_EDGE('',*,*,#43804,.F.);
#72712=ORIENTED_EDGE('',*,*,#43807,.F.);
#72713=ORIENTED_EDGE('',*,*,#43809,.F.);
#72714=ORIENTED_EDGE('',*,*,#43788,.F.);
#72715=ORIENTED_EDGE('',*,*,#43792,.F.);
#72716=ORIENTED_EDGE('',*,*,#43795,.F.);
#72717=ORIENTED_EDGE('',*,*,#43797,.F.);
#72718=ORIENTED_EDGE('',*,*,#43783,.F.);
#72719=ORIENTED_EDGE('',*,*,#43773,.F.);
#72720=ORIENTED_EDGE('',*,*,#43778,.F.);
#72721=ORIENTED_EDGE('',*,*,#43786,.F.);
#72722=ORIENTED_EDGE('',*,*,#43768,.F.);
#72723=ORIENTED_EDGE('',*,*,#43758,.F.);
#72724=ORIENTED_EDGE('',*,*,#43763,.F.);
#72725=ORIENTED_EDGE('',*,*,#43771,.F.);
#72726=ORIENTED_EDGE('',*,*,#43753,.F.);
#72727=ORIENTED_EDGE('',*,*,#43743,.F.);
#72728=ORIENTED_EDGE('',*,*,#43748,.F.);
#72729=ORIENTED_EDGE('',*,*,#43756,.F.);
#72730=ORIENTED_EDGE('',*,*,#43738,.F.);
#72731=ORIENTED_EDGE('',*,*,#43728,.F.);
#72732=ORIENTED_EDGE('',*,*,#43733,.F.);
#72733=ORIENTED_EDGE('',*,*,#43741,.F.);
#72734=ORIENTED_EDGE('',*,*,#43716,.F.);
#72735=ORIENTED_EDGE('',*,*,#43720,.F.);
#72736=ORIENTED_EDGE('',*,*,#43723,.F.);
#72737=ORIENTED_EDGE('',*,*,#43725,.F.);
#72738=ORIENTED_EDGE('',*,*,#43711,.F.);
#72739=ORIENTED_EDGE('',*,*,#43701,.F.);
#72740=ORIENTED_EDGE('',*,*,#43705,.F.);
#72741=ORIENTED_EDGE('',*,*,#43709,.F.);
#72742=ORIENTED_EDGE('',*,*,#43714,.F.);
#72743=ORIENTED_EDGE('',*,*,#43696,.F.);
#72744=ORIENTED_EDGE('',*,*,#43686,.F.);
#72745=ORIENTED_EDGE('',*,*,#43691,.F.);
#72746=ORIENTED_EDGE('',*,*,#43699,.F.);
#72747=ORIENTED_EDGE('',*,*,#43681,.F.);
#72748=ORIENTED_EDGE('',*,*,#43671,.F.);
#72749=ORIENTED_EDGE('',*,*,#43676,.F.);
#72750=ORIENTED_EDGE('',*,*,#43684,.F.);
#72751=ORIENTED_EDGE('',*,*,#43667,.F.);
#72752=ORIENTED_EDGE('',*,*,#43664,.F.);
#72753=ORIENTED_EDGE('',*,*,#43659,.F.);
#72754=ORIENTED_EDGE('',*,*,#43669,.F.);
#72755=ORIENTED_EDGE('',*,*,#43644,.F.);
#72756=ORIENTED_EDGE('',*,*,#43648,.F.);
#72757=ORIENTED_EDGE('',*,*,#43651,.F.);
#72758=ORIENTED_EDGE('',*,*,#43653,.F.);
#72759=ORIENTED_EDGE('',*,*,#43632,.F.);
#72760=ORIENTED_EDGE('',*,*,#43636,.F.);
#72761=ORIENTED_EDGE('',*,*,#43639,.F.);
#72762=ORIENTED_EDGE('',*,*,#43641,.F.);
#72763=ORIENTED_EDGE('',*,*,#43620,.F.);
#72764=ORIENTED_EDGE('',*,*,#43624,.F.);
#72765=ORIENTED_EDGE('',*,*,#43627,.F.);
#72766=ORIENTED_EDGE('',*,*,#43629,.F.);
#72767=ORIENTED_EDGE('',*,*,#43608,.F.);
#72768=ORIENTED_EDGE('',*,*,#43612,.F.);
#72769=ORIENTED_EDGE('',*,*,#43615,.F.);
#72770=ORIENTED_EDGE('',*,*,#43617,.F.);
#72771=ORIENTED_EDGE('',*,*,#43603,.F.);
#72772=ORIENTED_EDGE('',*,*,#43594,.F.);
#72773=ORIENTED_EDGE('',*,*,#43606,.F.);
#72774=ORIENTED_EDGE('',*,*,#43590,.F.);
#72775=ORIENTED_EDGE('',*,*,#43587,.F.);
#72776=ORIENTED_EDGE('',*,*,#43582,.F.);
#72777=ORIENTED_EDGE('',*,*,#43592,.F.);
#72778=ORIENTED_EDGE('',*,*,#43575,.F.);
#72779=ORIENTED_EDGE('',*,*,#43572,.F.);
#72780=ORIENTED_EDGE('',*,*,#43568,.F.);
#72781=ORIENTED_EDGE('',*,*,#43577,.F.);
#72782=ORIENTED_EDGE('',*,*,#45141,.F.);
#72783=ORIENTED_EDGE('',*,*,#45146,.F.);
#72784=ORIENTED_EDGE('',*,*,#45153,.F.);
#72785=ORIENTED_EDGE('',*,*,#45165,.F.);
#72786=ORIENTED_EDGE('',*,*,#45155,.F.);
#72787=ORIENTED_EDGE('',*,*,#45160,.F.);
#72788=ORIENTED_EDGE('',*,*,#45168,.F.);
#72789=ORIENTED_EDGE('',*,*,#45180,.F.);
#72790=ORIENTED_EDGE('',*,*,#45170,.F.);
#72791=ORIENTED_EDGE('',*,*,#45175,.F.);
#72792=ORIENTED_EDGE('',*,*,#45183,.F.);
#72793=ORIENTED_EDGE('',*,*,#45195,.F.);
#72794=ORIENTED_EDGE('',*,*,#45185,.F.);
#72795=ORIENTED_EDGE('',*,*,#45190,.F.);
#72796=ORIENTED_EDGE('',*,*,#45198,.F.);
#72797=ORIENTED_EDGE('',*,*,#45210,.F.);
#72798=ORIENTED_EDGE('',*,*,#45200,.F.);
#72799=ORIENTED_EDGE('',*,*,#45205,.F.);
#72800=ORIENTED_EDGE('',*,*,#45213,.F.);
#72801=ORIENTED_EDGE('',*,*,#45225,.F.);
#72802=ORIENTED_EDGE('',*,*,#45216,.F.);
#72803=ORIENTED_EDGE('',*,*,#45228,.F.);
#72804=ORIENTED_EDGE('',*,*,#45240,.F.);
#72805=ORIENTED_EDGE('',*,*,#45231,.F.);
#72806=ORIENTED_EDGE('',*,*,#45243,.F.);
#72807=ORIENTED_EDGE('',*,*,#45255,.F.);
#72808=ORIENTED_EDGE('',*,*,#45245,.F.);
#72809=ORIENTED_EDGE('',*,*,#45250,.F.);
#72810=ORIENTED_EDGE('',*,*,#45258,.F.);
#72811=ORIENTED_EDGE('',*,*,#45270,.F.);
#72812=ORIENTED_EDGE('',*,*,#45260,.F.);
#72813=ORIENTED_EDGE('',*,*,#45265,.F.);
#72814=ORIENTED_EDGE('',*,*,#45273,.F.);
#72815=ORIENTED_EDGE('',*,*,#45285,.F.);
#72816=ORIENTED_EDGE('',*,*,#45275,.F.);
#72817=ORIENTED_EDGE('',*,*,#45280,.F.);
#72818=ORIENTED_EDGE('',*,*,#45288,.F.);
#72819=ORIENTED_EDGE('',*,*,#45290,.F.);
#72820=ORIENTED_EDGE('',*,*,#45294,.F.);
#72821=ORIENTED_EDGE('',*,*,#45297,.F.);
#72822=ORIENTED_EDGE('',*,*,#45299,.F.);
#72823=ORIENTED_EDGE('',*,*,#45302,.F.);
#72824=ORIENTED_EDGE('',*,*,#45306,.F.);
#72825=ORIENTED_EDGE('',*,*,#45309,.F.);
#72826=ORIENTED_EDGE('',*,*,#45311,.F.);
#72827=ORIENTED_EDGE('',*,*,#45314,.F.);
#72828=ORIENTED_EDGE('',*,*,#45318,.F.);
#72829=ORIENTED_EDGE('',*,*,#45321,.F.);
#72830=ORIENTED_EDGE('',*,*,#45323,.F.);
#72831=ORIENTED_EDGE('',*,*,#45326,.F.);
#72832=ORIENTED_EDGE('',*,*,#45330,.F.);
#72833=ORIENTED_EDGE('',*,*,#45333,.F.);
#72834=ORIENTED_EDGE('',*,*,#45335,.F.);
#72835=ORIENTED_EDGE('',*,*,#45338,.F.);
#72836=ORIENTED_EDGE('',*,*,#45342,.F.);
#72837=ORIENTED_EDGE('',*,*,#45345,.F.);
#72838=ORIENTED_EDGE('',*,*,#45347,.F.);
#72839=ORIENTED_EDGE('',*,*,#45350,.F.);
#72840=ORIENTED_EDGE('',*,*,#45354,.F.);
#72841=ORIENTED_EDGE('',*,*,#45357,.F.);
#72842=ORIENTED_EDGE('',*,*,#45359,.F.);
#72843=ORIENTED_EDGE('',*,*,#45362,.F.);
#72844=ORIENTED_EDGE('',*,*,#45366,.F.);
#72845=ORIENTED_EDGE('',*,*,#45369,.F.);
#72846=ORIENTED_EDGE('',*,*,#45371,.F.);
#72847=ORIENTED_EDGE('',*,*,#45374,.F.);
#72848=ORIENTED_EDGE('',*,*,#45378,.F.);
#72849=ORIENTED_EDGE('',*,*,#45381,.F.);
#72850=ORIENTED_EDGE('',*,*,#45383,.F.);
#72851=ORIENTED_EDGE('',*,*,#45396,.F.);
#72852=ORIENTED_EDGE('',*,*,#45387,.F.);
#72853=ORIENTED_EDGE('',*,*,#45399,.F.);
#72854=ORIENTED_EDGE('',*,*,#45411,.F.);
#72855=ORIENTED_EDGE('',*,*,#45402,.F.);
#72856=ORIENTED_EDGE('',*,*,#45414,.F.);
#72857=ORIENTED_EDGE('',*,*,#45416,.F.);
#72858=ORIENTED_EDGE('',*,*,#45420,.F.);
#72859=ORIENTED_EDGE('',*,*,#45423,.F.);
#72860=ORIENTED_EDGE('',*,*,#45425,.F.);
#72861=ORIENTED_EDGE('',*,*,#45428,.F.);
#72862=ORIENTED_EDGE('',*,*,#45432,.F.);
#72863=ORIENTED_EDGE('',*,*,#45435,.F.);
#72864=ORIENTED_EDGE('',*,*,#45437,.F.);
#72865=ORIENTED_EDGE('',*,*,#45440,.F.);
#72866=ORIENTED_EDGE('',*,*,#45444,.F.);
#72867=ORIENTED_EDGE('',*,*,#45447,.F.);
#72868=ORIENTED_EDGE('',*,*,#45449,.F.);
#72869=ORIENTED_EDGE('',*,*,#45452,.F.);
#72870=ORIENTED_EDGE('',*,*,#45456,.F.);
#72871=ORIENTED_EDGE('',*,*,#45459,.F.);
#72872=ORIENTED_EDGE('',*,*,#45461,.F.);
#72873=ORIENTED_EDGE('',*,*,#45474,.F.);
#72874=ORIENTED_EDGE('',*,*,#45464,.F.);
#72875=ORIENTED_EDGE('',*,*,#45468,.F.);
#72876=ORIENTED_EDGE('',*,*,#45472,.F.);
#72877=ORIENTED_EDGE('',*,*,#45477,.F.);
#72878=ORIENTED_EDGE('',*,*,#45489,.F.);
#72879=ORIENTED_EDGE('',*,*,#45479,.F.);
#72880=ORIENTED_EDGE('',*,*,#45484,.F.);
#72881=ORIENTED_EDGE('',*,*,#45492,.F.);
#72882=ORIENTED_EDGE('',*,*,#45504,.F.);
#72883=ORIENTED_EDGE('',*,*,#45494,.F.);
#72884=ORIENTED_EDGE('',*,*,#45499,.F.);
#72885=ORIENTED_EDGE('',*,*,#45507,.F.);
#72886=ORIENTED_EDGE('',*,*,#45519,.F.);
#72887=ORIENTED_EDGE('',*,*,#45509,.F.);
#72888=ORIENTED_EDGE('',*,*,#45513,.F.);
#72889=ORIENTED_EDGE('',*,*,#45517,.F.);
#72890=ORIENTED_EDGE('',*,*,#45522,.F.);
#72891=ORIENTED_EDGE('',*,*,#45524,.F.);
#72892=ORIENTED_EDGE('',*,*,#45528,.F.);
#72893=ORIENTED_EDGE('',*,*,#45531,.F.);
#72894=ORIENTED_EDGE('',*,*,#45533,.F.);
#72895=ORIENTED_EDGE('',*,*,#45536,.F.);
#72896=ORIENTED_EDGE('',*,*,#45540,.F.);
#72897=ORIENTED_EDGE('',*,*,#45543,.F.);
#72898=ORIENTED_EDGE('',*,*,#45545,.F.);
#72899=ORIENTED_EDGE('',*,*,#45548,.F.);
#72900=ORIENTED_EDGE('',*,*,#45552,.F.);
#72901=ORIENTED_EDGE('',*,*,#45555,.F.);
#72902=ORIENTED_EDGE('',*,*,#45557,.F.);
#72903=ORIENTED_EDGE('',*,*,#45560,.F.);
#72904=ORIENTED_EDGE('',*,*,#45564,.F.);
#72905=ORIENTED_EDGE('',*,*,#45567,.F.);
#72906=ORIENTED_EDGE('',*,*,#45569,.F.);
#72907=ORIENTED_EDGE('',*,*,#45572,.F.);
#72908=ORIENTED_EDGE('',*,*,#45576,.F.);
#72909=ORIENTED_EDGE('',*,*,#45579,.F.);
#72910=ORIENTED_EDGE('',*,*,#45581,.F.);
#72911=ORIENTED_EDGE('',*,*,#45584,.F.);
#72912=ORIENTED_EDGE('',*,*,#45588,.F.);
#72913=ORIENTED_EDGE('',*,*,#45591,.F.);
#72914=ORIENTED_EDGE('',*,*,#45593,.F.);
#72915=ORIENTED_EDGE('',*,*,#45596,.F.);
#72916=ORIENTED_EDGE('',*,*,#45600,.F.);
#72917=ORIENTED_EDGE('',*,*,#45603,.F.);
#72918=ORIENTED_EDGE('',*,*,#45605,.F.);
#72919=ORIENTED_EDGE('',*,*,#45608,.F.);
#72920=ORIENTED_EDGE('',*,*,#45612,.F.);
#72921=ORIENTED_EDGE('',*,*,#45615,.F.);
#72922=ORIENTED_EDGE('',*,*,#45617,.F.);
#72923=ORIENTED_EDGE('',*,*,#45620,.F.);
#72924=ORIENTED_EDGE('',*,*,#45624,.F.);
#72925=ORIENTED_EDGE('',*,*,#45627,.F.);
#72926=ORIENTED_EDGE('',*,*,#45629,.F.);
#72927=ORIENTED_EDGE('',*,*,#45632,.F.);
#72928=ORIENTED_EDGE('',*,*,#45636,.F.);
#72929=ORIENTED_EDGE('',*,*,#45639,.F.);
#72930=ORIENTED_EDGE('',*,*,#45641,.F.);
#72931=ORIENTED_EDGE('',*,*,#45654,.F.);
#72932=ORIENTED_EDGE('',*,*,#45644,.F.);
#72933=ORIENTED_EDGE('',*,*,#45648,.F.);
#72934=ORIENTED_EDGE('',*,*,#45652,.F.);
#72935=ORIENTED_EDGE('',*,*,#45657,.F.);
#72936=ORIENTED_EDGE('',*,*,#45669,.F.);
#72937=ORIENTED_EDGE('',*,*,#45659,.F.);
#72938=ORIENTED_EDGE('',*,*,#45663,.F.);
#72939=ORIENTED_EDGE('',*,*,#45667,.F.);
#72940=ORIENTED_EDGE('',*,*,#45672,.F.);
#72941=ORIENTED_EDGE('',*,*,#45674,.F.);
#72942=ORIENTED_EDGE('',*,*,#45678,.F.);
#72943=ORIENTED_EDGE('',*,*,#45681,.F.);
#72944=ORIENTED_EDGE('',*,*,#45683,.F.);
#72945=ORIENTED_EDGE('',*,*,#45686,.F.);
#72946=ORIENTED_EDGE('',*,*,#45690,.F.);
#72947=ORIENTED_EDGE('',*,*,#45693,.F.);
#72948=ORIENTED_EDGE('',*,*,#45695,.F.);
#72949=ORIENTED_EDGE('',*,*,#45698,.F.);
#72950=ORIENTED_EDGE('',*,*,#45702,.F.);
#72951=ORIENTED_EDGE('',*,*,#45705,.F.);
#72952=ORIENTED_EDGE('',*,*,#45707,.F.);
#72953=ORIENTED_EDGE('',*,*,#45710,.F.);
#72954=ORIENTED_EDGE('',*,*,#45714,.F.);
#72955=ORIENTED_EDGE('',*,*,#45717,.F.);
#72956=ORIENTED_EDGE('',*,*,#45719,.F.);
#72957=ORIENTED_EDGE('',*,*,#45722,.F.);
#72958=ORIENTED_EDGE('',*,*,#45726,.F.);
#72959=ORIENTED_EDGE('',*,*,#45729,.F.);
#72960=ORIENTED_EDGE('',*,*,#45731,.F.);
#72961=ORIENTED_EDGE('',*,*,#45734,.F.);
#72962=ORIENTED_EDGE('',*,*,#45738,.F.);
#72963=ORIENTED_EDGE('',*,*,#45741,.F.);
#72964=ORIENTED_EDGE('',*,*,#45743,.F.);
#72965=ORIENTED_EDGE('',*,*,#45746,.F.);
#72966=ORIENTED_EDGE('',*,*,#45750,.F.);
#72967=ORIENTED_EDGE('',*,*,#45753,.F.);
#72968=ORIENTED_EDGE('',*,*,#45755,.F.);
#72969=ORIENTED_EDGE('',*,*,#45758,.F.);
#72970=ORIENTED_EDGE('',*,*,#45762,.F.);
#72971=ORIENTED_EDGE('',*,*,#45765,.F.);
#72972=ORIENTED_EDGE('',*,*,#45767,.F.);
#72973=ORIENTED_EDGE('',*,*,#45770,.F.);
#72974=ORIENTED_EDGE('',*,*,#45774,.F.);
#72975=ORIENTED_EDGE('',*,*,#45777,.F.);
#72976=ORIENTED_EDGE('',*,*,#45779,.F.);
#72977=ORIENTED_EDGE('',*,*,#45792,.F.);
#72978=ORIENTED_EDGE('',*,*,#45782,.F.);
#72979=ORIENTED_EDGE('',*,*,#45787,.F.);
#72980=ORIENTED_EDGE('',*,*,#45795,.F.);
#72981=ORIENTED_EDGE('',*,*,#45807,.F.);
#72982=ORIENTED_EDGE('',*,*,#45797,.F.);
#72983=ORIENTED_EDGE('',*,*,#45801,.F.);
#72984=ORIENTED_EDGE('',*,*,#45805,.F.);
#72985=ORIENTED_EDGE('',*,*,#45810,.F.);
#72986=ORIENTED_EDGE('',*,*,#45812,.F.);
#72987=ORIENTED_EDGE('',*,*,#45816,.F.);
#72988=ORIENTED_EDGE('',*,*,#45819,.F.);
#72989=ORIENTED_EDGE('',*,*,#45821,.F.);
#72990=ORIENTED_EDGE('',*,*,#45824,.F.);
#72991=ORIENTED_EDGE('',*,*,#45828,.F.);
#72992=ORIENTED_EDGE('',*,*,#45831,.F.);
#72993=ORIENTED_EDGE('',*,*,#45833,.F.);
#72994=ORIENTED_EDGE('',*,*,#45836,.F.);
#72995=ORIENTED_EDGE('',*,*,#45840,.F.);
#72996=ORIENTED_EDGE('',*,*,#45843,.F.);
#72997=ORIENTED_EDGE('',*,*,#45845,.F.);
#72998=ORIENTED_EDGE('',*,*,#45848,.F.);
#72999=ORIENTED_EDGE('',*,*,#45852,.F.);
#73000=ORIENTED_EDGE('',*,*,#45855,.F.);
#73001=ORIENTED_EDGE('',*,*,#45857,.F.);
#73002=ORIENTED_EDGE('',*,*,#45860,.F.);
#73003=ORIENTED_EDGE('',*,*,#45864,.F.);
#73004=ORIENTED_EDGE('',*,*,#45867,.F.);
#73005=ORIENTED_EDGE('',*,*,#45869,.F.);
#73006=ORIENTED_EDGE('',*,*,#45872,.F.);
#73007=ORIENTED_EDGE('',*,*,#45876,.F.);
#73008=ORIENTED_EDGE('',*,*,#45879,.F.);
#73009=ORIENTED_EDGE('',*,*,#45881,.F.);
#73010=ORIENTED_EDGE('',*,*,#45884,.F.);
#73011=ORIENTED_EDGE('',*,*,#45888,.F.);
#73012=ORIENTED_EDGE('',*,*,#45891,.F.);
#73013=ORIENTED_EDGE('',*,*,#45893,.F.);
#73014=ORIENTED_EDGE('',*,*,#45896,.F.);
#73015=ORIENTED_EDGE('',*,*,#45900,.F.);
#73016=ORIENTED_EDGE('',*,*,#45903,.F.);
#73017=ORIENTED_EDGE('',*,*,#45905,.F.);
#73018=ORIENTED_EDGE('',*,*,#45908,.F.);
#73019=ORIENTED_EDGE('',*,*,#45912,.F.);
#73020=ORIENTED_EDGE('',*,*,#45915,.F.);
#73021=ORIENTED_EDGE('',*,*,#45917,.F.);
#73022=ORIENTED_EDGE('',*,*,#45920,.F.);
#73023=ORIENTED_EDGE('',*,*,#45924,.F.);
#73024=ORIENTED_EDGE('',*,*,#45927,.F.);
#73025=ORIENTED_EDGE('',*,*,#45929,.F.);
#73026=ORIENTED_EDGE('',*,*,#45932,.F.);
#73027=ORIENTED_EDGE('',*,*,#45936,.F.);
#73028=ORIENTED_EDGE('',*,*,#45939,.F.);
#73029=ORIENTED_EDGE('',*,*,#45941,.F.);
#73030=ORIENTED_EDGE('',*,*,#45944,.F.);
#73031=ORIENTED_EDGE('',*,*,#45948,.F.);
#73032=ORIENTED_EDGE('',*,*,#45951,.F.);
#73033=ORIENTED_EDGE('',*,*,#45953,.F.);
#73034=ORIENTED_EDGE('',*,*,#45956,.F.);
#73035=ORIENTED_EDGE('',*,*,#45960,.F.);
#73036=ORIENTED_EDGE('',*,*,#45963,.F.);
#73037=ORIENTED_EDGE('',*,*,#45965,.F.);
#73038=ORIENTED_EDGE('',*,*,#45968,.F.);
#73039=ORIENTED_EDGE('',*,*,#45972,.F.);
#73040=ORIENTED_EDGE('',*,*,#45975,.F.);
#73041=ORIENTED_EDGE('',*,*,#45977,.F.);
#73042=ORIENTED_EDGE('',*,*,#45980,.F.);
#73043=ORIENTED_EDGE('',*,*,#45984,.F.);
#73044=ORIENTED_EDGE('',*,*,#45987,.F.);
#73045=ORIENTED_EDGE('',*,*,#45989,.F.);
#73046=ORIENTED_EDGE('',*,*,#45992,.F.);
#73047=ORIENTED_EDGE('',*,*,#45996,.F.);
#73048=ORIENTED_EDGE('',*,*,#45999,.F.);
#73049=ORIENTED_EDGE('',*,*,#46001,.F.);
#73050=ORIENTED_EDGE('',*,*,#46004,.F.);
#73051=ORIENTED_EDGE('',*,*,#46008,.F.);
#73052=ORIENTED_EDGE('',*,*,#46011,.F.);
#73053=ORIENTED_EDGE('',*,*,#46013,.F.);
#73054=ORIENTED_EDGE('',*,*,#46016,.F.);
#73055=ORIENTED_EDGE('',*,*,#46020,.F.);
#73056=ORIENTED_EDGE('',*,*,#46023,.F.);
#73057=ORIENTED_EDGE('',*,*,#46025,.F.);
#73058=ORIENTED_EDGE('',*,*,#46028,.F.);
#73059=ORIENTED_EDGE('',*,*,#46032,.F.);
#73060=ORIENTED_EDGE('',*,*,#46035,.F.);
#73061=ORIENTED_EDGE('',*,*,#46037,.F.);
#73062=ORIENTED_EDGE('',*,*,#46040,.F.);
#73063=ORIENTED_EDGE('',*,*,#46044,.F.);
#73064=ORIENTED_EDGE('',*,*,#46047,.F.);
#73065=ORIENTED_EDGE('',*,*,#46049,.F.);
#73066=ORIENTED_EDGE('',*,*,#46052,.F.);
#73067=ORIENTED_EDGE('',*,*,#46056,.F.);
#73068=ORIENTED_EDGE('',*,*,#46059,.F.);
#73069=ORIENTED_EDGE('',*,*,#46061,.F.);
#73070=ORIENTED_EDGE('',*,*,#46064,.F.);
#73071=ORIENTED_EDGE('',*,*,#46068,.F.);
#73072=ORIENTED_EDGE('',*,*,#46071,.F.);
#73073=ORIENTED_EDGE('',*,*,#46073,.F.);
#73074=ORIENTED_EDGE('',*,*,#46076,.F.);
#73075=ORIENTED_EDGE('',*,*,#46080,.F.);
#73076=ORIENTED_EDGE('',*,*,#46083,.F.);
#73077=ORIENTED_EDGE('',*,*,#46085,.F.);
#73078=ORIENTED_EDGE('',*,*,#46088,.F.);
#73079=ORIENTED_EDGE('',*,*,#46092,.F.);
#73080=ORIENTED_EDGE('',*,*,#46095,.F.);
#73081=ORIENTED_EDGE('',*,*,#46097,.F.);
#73082=ORIENTED_EDGE('',*,*,#46100,.F.);
#73083=ORIENTED_EDGE('',*,*,#46104,.F.);
#73084=ORIENTED_EDGE('',*,*,#46107,.F.);
#73085=ORIENTED_EDGE('',*,*,#46109,.F.);
#73086=ORIENTED_EDGE('',*,*,#46112,.F.);
#73087=ORIENTED_EDGE('',*,*,#46116,.F.);
#73088=ORIENTED_EDGE('',*,*,#46119,.F.);
#73089=ORIENTED_EDGE('',*,*,#46121,.F.);
#73090=ORIENTED_EDGE('',*,*,#46124,.F.);
#73091=ORIENTED_EDGE('',*,*,#46128,.F.);
#73092=ORIENTED_EDGE('',*,*,#46131,.F.);
#73093=ORIENTED_EDGE('',*,*,#46133,.F.);
#73094=ORIENTED_EDGE('',*,*,#46136,.F.);
#73095=ORIENTED_EDGE('',*,*,#46140,.F.);
#73096=ORIENTED_EDGE('',*,*,#46143,.F.);
#73097=ORIENTED_EDGE('',*,*,#46145,.F.);
#73098=ORIENTED_EDGE('',*,*,#46148,.F.);
#73099=ORIENTED_EDGE('',*,*,#46152,.F.);
#73100=ORIENTED_EDGE('',*,*,#46155,.F.);
#73101=ORIENTED_EDGE('',*,*,#46157,.F.);
#73102=ORIENTED_EDGE('',*,*,#46160,.F.);
#73103=ORIENTED_EDGE('',*,*,#46164,.F.);
#73104=ORIENTED_EDGE('',*,*,#46167,.F.);
#73105=ORIENTED_EDGE('',*,*,#46169,.F.);
#73106=ORIENTED_EDGE('',*,*,#46172,.F.);
#73107=ORIENTED_EDGE('',*,*,#46176,.F.);
#73108=ORIENTED_EDGE('',*,*,#46179,.F.);
#73109=ORIENTED_EDGE('',*,*,#46181,.F.);
#73110=ORIENTED_EDGE('',*,*,#46184,.F.);
#73111=ORIENTED_EDGE('',*,*,#46188,.F.);
#73112=ORIENTED_EDGE('',*,*,#46191,.F.);
#73113=ORIENTED_EDGE('',*,*,#46193,.F.);
#73114=ORIENTED_EDGE('',*,*,#46196,.F.);
#73115=ORIENTED_EDGE('',*,*,#46200,.F.);
#73116=ORIENTED_EDGE('',*,*,#46203,.F.);
#73117=ORIENTED_EDGE('',*,*,#46205,.F.);
#73118=ORIENTED_EDGE('',*,*,#46208,.F.);
#73119=ORIENTED_EDGE('',*,*,#46212,.F.);
#73120=ORIENTED_EDGE('',*,*,#46215,.F.);
#73121=ORIENTED_EDGE('',*,*,#46217,.F.);
#73122=ORIENTED_EDGE('',*,*,#46220,.F.);
#73123=ORIENTED_EDGE('',*,*,#46224,.F.);
#73124=ORIENTED_EDGE('',*,*,#46227,.F.);
#73125=ORIENTED_EDGE('',*,*,#46229,.F.);
#73126=ORIENTED_EDGE('',*,*,#46232,.F.);
#73127=ORIENTED_EDGE('',*,*,#46236,.F.);
#73128=ORIENTED_EDGE('',*,*,#46239,.F.);
#73129=ORIENTED_EDGE('',*,*,#46241,.F.);
#73130=ORIENTED_EDGE('',*,*,#46244,.F.);
#73131=ORIENTED_EDGE('',*,*,#46248,.F.);
#73132=ORIENTED_EDGE('',*,*,#46251,.F.);
#73133=ORIENTED_EDGE('',*,*,#46253,.F.);
#73134=ORIENTED_EDGE('',*,*,#46256,.F.);
#73135=ORIENTED_EDGE('',*,*,#46260,.F.);
#73136=ORIENTED_EDGE('',*,*,#46263,.F.);
#73137=ORIENTED_EDGE('',*,*,#46265,.F.);
#73138=ORIENTED_EDGE('',*,*,#46268,.F.);
#73139=ORIENTED_EDGE('',*,*,#46272,.F.);
#73140=ORIENTED_EDGE('',*,*,#46275,.F.);
#73141=ORIENTED_EDGE('',*,*,#46277,.F.);
#73142=ORIENTED_EDGE('',*,*,#46280,.F.);
#73143=ORIENTED_EDGE('',*,*,#46284,.F.);
#73144=ORIENTED_EDGE('',*,*,#46287,.F.);
#73145=ORIENTED_EDGE('',*,*,#46289,.F.);
#73146=ORIENTED_EDGE('',*,*,#46292,.F.);
#73147=ORIENTED_EDGE('',*,*,#46296,.F.);
#73148=ORIENTED_EDGE('',*,*,#46299,.F.);
#73149=ORIENTED_EDGE('',*,*,#46301,.F.);
#73150=ORIENTED_EDGE('',*,*,#46304,.F.);
#73151=ORIENTED_EDGE('',*,*,#46308,.F.);
#73152=ORIENTED_EDGE('',*,*,#46311,.F.);
#73153=ORIENTED_EDGE('',*,*,#46313,.F.);
#73154=ORIENTED_EDGE('',*,*,#46316,.F.);
#73155=ORIENTED_EDGE('',*,*,#46320,.F.);
#73156=ORIENTED_EDGE('',*,*,#46323,.F.);
#73157=ORIENTED_EDGE('',*,*,#46325,.F.);
#73158=ORIENTED_EDGE('',*,*,#46328,.F.);
#73159=ORIENTED_EDGE('',*,*,#46332,.F.);
#73160=ORIENTED_EDGE('',*,*,#46335,.F.);
#73161=ORIENTED_EDGE('',*,*,#46337,.F.);
#73162=ORIENTED_EDGE('',*,*,#46340,.F.);
#73163=ORIENTED_EDGE('',*,*,#46344,.F.);
#73164=ORIENTED_EDGE('',*,*,#46347,.F.);
#73165=ORIENTED_EDGE('',*,*,#46349,.F.);
#73166=ORIENTED_EDGE('',*,*,#46352,.F.);
#73167=ORIENTED_EDGE('',*,*,#46356,.F.);
#73168=ORIENTED_EDGE('',*,*,#46359,.F.);
#73169=ORIENTED_EDGE('',*,*,#46361,.F.);
#73170=ORIENTED_EDGE('',*,*,#46364,.F.);
#73171=ORIENTED_EDGE('',*,*,#46368,.F.);
#73172=ORIENTED_EDGE('',*,*,#46371,.F.);
#73173=ORIENTED_EDGE('',*,*,#46373,.F.);
#73174=ORIENTED_EDGE('',*,*,#46376,.F.);
#73175=ORIENTED_EDGE('',*,*,#46380,.F.);
#73176=ORIENTED_EDGE('',*,*,#46383,.F.);
#73177=ORIENTED_EDGE('',*,*,#46385,.F.);
#73178=ORIENTED_EDGE('',*,*,#46388,.F.);
#73179=ORIENTED_EDGE('',*,*,#46392,.F.);
#73180=ORIENTED_EDGE('',*,*,#46395,.F.);
#73181=ORIENTED_EDGE('',*,*,#46397,.F.);
#73182=ORIENTED_EDGE('',*,*,#46400,.F.);
#73183=ORIENTED_EDGE('',*,*,#46404,.F.);
#73184=ORIENTED_EDGE('',*,*,#46407,.F.);
#73185=ORIENTED_EDGE('',*,*,#46409,.F.);
#73186=ORIENTED_EDGE('',*,*,#46412,.F.);
#73187=ORIENTED_EDGE('',*,*,#46416,.F.);
#73188=ORIENTED_EDGE('',*,*,#46419,.F.);
#73189=ORIENTED_EDGE('',*,*,#46421,.F.);
#73190=ORIENTED_EDGE('',*,*,#46424,.F.);
#73191=ORIENTED_EDGE('',*,*,#46428,.F.);
#73192=ORIENTED_EDGE('',*,*,#46431,.F.);
#73193=ORIENTED_EDGE('',*,*,#46433,.F.);
#73194=ORIENTED_EDGE('',*,*,#46436,.F.);
#73195=ORIENTED_EDGE('',*,*,#46440,.F.);
#73196=ORIENTED_EDGE('',*,*,#46443,.F.);
#73197=ORIENTED_EDGE('',*,*,#46445,.F.);
#73198=ORIENTED_EDGE('',*,*,#46448,.F.);
#73199=ORIENTED_EDGE('',*,*,#46452,.F.);
#73200=ORIENTED_EDGE('',*,*,#46455,.F.);
#73201=ORIENTED_EDGE('',*,*,#46457,.F.);
#73202=ORIENTED_EDGE('',*,*,#46460,.F.);
#73203=ORIENTED_EDGE('',*,*,#46464,.F.);
#73204=ORIENTED_EDGE('',*,*,#46467,.F.);
#73205=ORIENTED_EDGE('',*,*,#46469,.F.);
#73206=ORIENTED_EDGE('',*,*,#46472,.F.);
#73207=ORIENTED_EDGE('',*,*,#46476,.F.);
#73208=ORIENTED_EDGE('',*,*,#46479,.F.);
#73209=ORIENTED_EDGE('',*,*,#46481,.F.);
#73210=ORIENTED_EDGE('',*,*,#46484,.F.);
#73211=ORIENTED_EDGE('',*,*,#46488,.F.);
#73212=ORIENTED_EDGE('',*,*,#46491,.F.);
#73213=ORIENTED_EDGE('',*,*,#46493,.F.);
#73214=ORIENTED_EDGE('',*,*,#46496,.F.);
#73215=ORIENTED_EDGE('',*,*,#46500,.F.);
#73216=ORIENTED_EDGE('',*,*,#46503,.F.);
#73217=ORIENTED_EDGE('',*,*,#46505,.F.);
#73218=ORIENTED_EDGE('',*,*,#46508,.F.);
#73219=ORIENTED_EDGE('',*,*,#46512,.F.);
#73220=ORIENTED_EDGE('',*,*,#46515,.F.);
#73221=ORIENTED_EDGE('',*,*,#46517,.F.);
#73222=ORIENTED_EDGE('',*,*,#46520,.F.);
#73223=ORIENTED_EDGE('',*,*,#46524,.F.);
#73224=ORIENTED_EDGE('',*,*,#46527,.F.);
#73225=ORIENTED_EDGE('',*,*,#46529,.F.);
#73226=ORIENTED_EDGE('',*,*,#46532,.F.);
#73227=ORIENTED_EDGE('',*,*,#46536,.F.);
#73228=ORIENTED_EDGE('',*,*,#46539,.F.);
#73229=ORIENTED_EDGE('',*,*,#46541,.F.);
#73230=ORIENTED_EDGE('',*,*,#46544,.F.);
#73231=ORIENTED_EDGE('',*,*,#46548,.F.);
#73232=ORIENTED_EDGE('',*,*,#46551,.F.);
#73233=ORIENTED_EDGE('',*,*,#46553,.F.);
#73234=ORIENTED_EDGE('',*,*,#46556,.F.);
#73235=ORIENTED_EDGE('',*,*,#46560,.F.);
#73236=ORIENTED_EDGE('',*,*,#46563,.F.);
#73237=ORIENTED_EDGE('',*,*,#46565,.F.);
#73238=ORIENTED_EDGE('',*,*,#46568,.F.);
#73239=ORIENTED_EDGE('',*,*,#46572,.F.);
#73240=ORIENTED_EDGE('',*,*,#46575,.F.);
#73241=ORIENTED_EDGE('',*,*,#46577,.F.);
#73242=ORIENTED_EDGE('',*,*,#46580,.F.);
#73243=ORIENTED_EDGE('',*,*,#46584,.F.);
#73244=ORIENTED_EDGE('',*,*,#46587,.F.);
#73245=ORIENTED_EDGE('',*,*,#46589,.F.);
#73246=ORIENTED_EDGE('',*,*,#46592,.F.);
#73247=ORIENTED_EDGE('',*,*,#46596,.F.);
#73248=ORIENTED_EDGE('',*,*,#46599,.F.);
#73249=ORIENTED_EDGE('',*,*,#46601,.F.);
#73250=ORIENTED_EDGE('',*,*,#46604,.F.);
#73251=ORIENTED_EDGE('',*,*,#46608,.F.);
#73252=ORIENTED_EDGE('',*,*,#46611,.F.);
#73253=ORIENTED_EDGE('',*,*,#46613,.F.);
#73254=ORIENTED_EDGE('',*,*,#46616,.F.);
#73255=ORIENTED_EDGE('',*,*,#46620,.F.);
#73256=ORIENTED_EDGE('',*,*,#46623,.F.);
#73257=ORIENTED_EDGE('',*,*,#46625,.F.);
#73258=ORIENTED_EDGE('',*,*,#46628,.F.);
#73259=ORIENTED_EDGE('',*,*,#46632,.F.);
#73260=ORIENTED_EDGE('',*,*,#46635,.F.);
#73261=ORIENTED_EDGE('',*,*,#46637,.F.);
#73262=ORIENTED_EDGE('',*,*,#46640,.F.);
#73263=ORIENTED_EDGE('',*,*,#46644,.F.);
#73264=ORIENTED_EDGE('',*,*,#46647,.F.);
#73265=ORIENTED_EDGE('',*,*,#46649,.F.);
#73266=ORIENTED_EDGE('',*,*,#46652,.F.);
#73267=ORIENTED_EDGE('',*,*,#46656,.F.);
#73268=ORIENTED_EDGE('',*,*,#46659,.F.);
#73269=ORIENTED_EDGE('',*,*,#46661,.F.);
#73270=ORIENTED_EDGE('',*,*,#46664,.F.);
#73271=ORIENTED_EDGE('',*,*,#46668,.F.);
#73272=ORIENTED_EDGE('',*,*,#46671,.F.);
#73273=ORIENTED_EDGE('',*,*,#46673,.F.);
#73274=ORIENTED_EDGE('',*,*,#46676,.F.);
#73275=ORIENTED_EDGE('',*,*,#46680,.F.);
#73276=ORIENTED_EDGE('',*,*,#46683,.F.);
#73277=ORIENTED_EDGE('',*,*,#46685,.F.);
#73278=ORIENTED_EDGE('',*,*,#46688,.F.);
#73279=ORIENTED_EDGE('',*,*,#46692,.F.);
#73280=ORIENTED_EDGE('',*,*,#46695,.F.);
#73281=ORIENTED_EDGE('',*,*,#46697,.F.);
#73282=ORIENTED_EDGE('',*,*,#46700,.F.);
#73283=ORIENTED_EDGE('',*,*,#46704,.F.);
#73284=ORIENTED_EDGE('',*,*,#46707,.F.);
#73285=ORIENTED_EDGE('',*,*,#46709,.F.);
#73286=ORIENTED_EDGE('',*,*,#46712,.F.);
#73287=ORIENTED_EDGE('',*,*,#46716,.F.);
#73288=ORIENTED_EDGE('',*,*,#46719,.F.);
#73289=ORIENTED_EDGE('',*,*,#46721,.F.);
#73290=ORIENTED_EDGE('',*,*,#46724,.F.);
#73291=ORIENTED_EDGE('',*,*,#46728,.F.);
#73292=ORIENTED_EDGE('',*,*,#46731,.F.);
#73293=ORIENTED_EDGE('',*,*,#46733,.F.);
#73294=ORIENTED_EDGE('',*,*,#51992,.F.);
#73295=ORIENTED_EDGE('',*,*,#51988,.T.);
#73296=ORIENTED_EDGE('',*,*,#51993,.T.);
#73297=ORIENTED_EDGE('',*,*,#51994,.F.);
#73298=ORIENTED_EDGE('',*,*,#51995,.F.);
#73299=ORIENTED_EDGE('',*,*,#51989,.T.);
#73300=ORIENTED_EDGE('',*,*,#51992,.T.);
#73301=ORIENTED_EDGE('',*,*,#51996,.F.);
#73302=ORIENTED_EDGE('',*,*,#51997,.F.);
#73303=ORIENTED_EDGE('',*,*,#51990,.T.);
#73304=ORIENTED_EDGE('',*,*,#51995,.T.);
#73305=ORIENTED_EDGE('',*,*,#51998,.F.);
#73306=ORIENTED_EDGE('',*,*,#51993,.F.);
#73307=ORIENTED_EDGE('',*,*,#51991,.T.);
#73308=ORIENTED_EDGE('',*,*,#51997,.T.);
#73309=ORIENTED_EDGE('',*,*,#51999,.F.);
#73310=ORIENTED_EDGE('',*,*,#52000,.T.);
#73311=ORIENTED_EDGE('',*,*,#46732,.T.);
#73312=ORIENTED_EDGE('',*,*,#46729,.T.);
#73313=ORIENTED_EDGE('',*,*,#46726,.T.);
#73314=ORIENTED_EDGE('',*,*,#46734,.T.);
#73315=ORIENTED_EDGE('',*,*,#46720,.T.);
#73316=ORIENTED_EDGE('',*,*,#46717,.T.);
#73317=ORIENTED_EDGE('',*,*,#46714,.T.);
#73318=ORIENTED_EDGE('',*,*,#46722,.T.);
#73319=ORIENTED_EDGE('',*,*,#46708,.T.);
#73320=ORIENTED_EDGE('',*,*,#46705,.T.);
#73321=ORIENTED_EDGE('',*,*,#46702,.T.);
#73322=ORIENTED_EDGE('',*,*,#46710,.T.);
#73323=ORIENTED_EDGE('',*,*,#46696,.T.);
#73324=ORIENTED_EDGE('',*,*,#46693,.T.);
#73325=ORIENTED_EDGE('',*,*,#46690,.T.);
#73326=ORIENTED_EDGE('',*,*,#46698,.T.);
#73327=ORIENTED_EDGE('',*,*,#46684,.T.);
#73328=ORIENTED_EDGE('',*,*,#46681,.T.);
#73329=ORIENTED_EDGE('',*,*,#46678,.T.);
#73330=ORIENTED_EDGE('',*,*,#46686,.T.);
#73331=ORIENTED_EDGE('',*,*,#46672,.T.);
#73332=ORIENTED_EDGE('',*,*,#46669,.T.);
#73333=ORIENTED_EDGE('',*,*,#46666,.T.);
#73334=ORIENTED_EDGE('',*,*,#46674,.T.);
#73335=ORIENTED_EDGE('',*,*,#46660,.T.);
#73336=ORIENTED_EDGE('',*,*,#46657,.T.);
#73337=ORIENTED_EDGE('',*,*,#46654,.T.);
#73338=ORIENTED_EDGE('',*,*,#46662,.T.);
#73339=ORIENTED_EDGE('',*,*,#46648,.T.);
#73340=ORIENTED_EDGE('',*,*,#46645,.T.);
#73341=ORIENTED_EDGE('',*,*,#46642,.T.);
#73342=ORIENTED_EDGE('',*,*,#46650,.T.);
#73343=ORIENTED_EDGE('',*,*,#46636,.T.);
#73344=ORIENTED_EDGE('',*,*,#46633,.T.);
#73345=ORIENTED_EDGE('',*,*,#46630,.T.);
#73346=ORIENTED_EDGE('',*,*,#46638,.T.);
#73347=ORIENTED_EDGE('',*,*,#46624,.T.);
#73348=ORIENTED_EDGE('',*,*,#46621,.T.);
#73349=ORIENTED_EDGE('',*,*,#46618,.T.);
#73350=ORIENTED_EDGE('',*,*,#46626,.T.);
#73351=ORIENTED_EDGE('',*,*,#46612,.T.);
#73352=ORIENTED_EDGE('',*,*,#46609,.T.);
#73353=ORIENTED_EDGE('',*,*,#46606,.T.);
#73354=ORIENTED_EDGE('',*,*,#46614,.T.);
#73355=ORIENTED_EDGE('',*,*,#46600,.T.);
#73356=ORIENTED_EDGE('',*,*,#46597,.T.);
#73357=ORIENTED_EDGE('',*,*,#46594,.T.);
#73358=ORIENTED_EDGE('',*,*,#46602,.T.);
#73359=ORIENTED_EDGE('',*,*,#46588,.T.);
#73360=ORIENTED_EDGE('',*,*,#46585,.T.);
#73361=ORIENTED_EDGE('',*,*,#46582,.T.);
#73362=ORIENTED_EDGE('',*,*,#46590,.T.);
#73363=ORIENTED_EDGE('',*,*,#46576,.T.);
#73364=ORIENTED_EDGE('',*,*,#46573,.T.);
#73365=ORIENTED_EDGE('',*,*,#46570,.T.);
#73366=ORIENTED_EDGE('',*,*,#46578,.T.);
#73367=ORIENTED_EDGE('',*,*,#46564,.T.);
#73368=ORIENTED_EDGE('',*,*,#46561,.T.);
#73369=ORIENTED_EDGE('',*,*,#46558,.T.);
#73370=ORIENTED_EDGE('',*,*,#46566,.T.);
#73371=ORIENTED_EDGE('',*,*,#46552,.T.);
#73372=ORIENTED_EDGE('',*,*,#46549,.T.);
#73373=ORIENTED_EDGE('',*,*,#46546,.T.);
#73374=ORIENTED_EDGE('',*,*,#46554,.T.);
#73375=ORIENTED_EDGE('',*,*,#46540,.T.);
#73376=ORIENTED_EDGE('',*,*,#46537,.T.);
#73377=ORIENTED_EDGE('',*,*,#46534,.T.);
#73378=ORIENTED_EDGE('',*,*,#46542,.T.);
#73379=ORIENTED_EDGE('',*,*,#46528,.T.);
#73380=ORIENTED_EDGE('',*,*,#46525,.T.);
#73381=ORIENTED_EDGE('',*,*,#46522,.T.);
#73382=ORIENTED_EDGE('',*,*,#46530,.T.);
#73383=ORIENTED_EDGE('',*,*,#46516,.T.);
#73384=ORIENTED_EDGE('',*,*,#46513,.T.);
#73385=ORIENTED_EDGE('',*,*,#46510,.T.);
#73386=ORIENTED_EDGE('',*,*,#46518,.T.);
#73387=ORIENTED_EDGE('',*,*,#46504,.T.);
#73388=ORIENTED_EDGE('',*,*,#46501,.T.);
#73389=ORIENTED_EDGE('',*,*,#46498,.T.);
#73390=ORIENTED_EDGE('',*,*,#46506,.T.);
#73391=ORIENTED_EDGE('',*,*,#46492,.T.);
#73392=ORIENTED_EDGE('',*,*,#46489,.T.);
#73393=ORIENTED_EDGE('',*,*,#46486,.T.);
#73394=ORIENTED_EDGE('',*,*,#46494,.T.);
#73395=ORIENTED_EDGE('',*,*,#46480,.T.);
#73396=ORIENTED_EDGE('',*,*,#46477,.T.);
#73397=ORIENTED_EDGE('',*,*,#46474,.T.);
#73398=ORIENTED_EDGE('',*,*,#46482,.T.);
#73399=ORIENTED_EDGE('',*,*,#46468,.T.);
#73400=ORIENTED_EDGE('',*,*,#46465,.T.);
#73401=ORIENTED_EDGE('',*,*,#46462,.T.);
#73402=ORIENTED_EDGE('',*,*,#46470,.T.);
#73403=ORIENTED_EDGE('',*,*,#46456,.T.);
#73404=ORIENTED_EDGE('',*,*,#46453,.T.);
#73405=ORIENTED_EDGE('',*,*,#46450,.T.);
#73406=ORIENTED_EDGE('',*,*,#46458,.T.);
#73407=ORIENTED_EDGE('',*,*,#46441,.T.);
#73408=ORIENTED_EDGE('',*,*,#46438,.T.);
#73409=ORIENTED_EDGE('',*,*,#46446,.T.);
#73410=ORIENTED_EDGE('',*,*,#46444,.T.);
#73411=ORIENTED_EDGE('',*,*,#46432,.T.);
#73412=ORIENTED_EDGE('',*,*,#46429,.T.);
#73413=ORIENTED_EDGE('',*,*,#46426,.T.);
#73414=ORIENTED_EDGE('',*,*,#46434,.T.);
#73415=ORIENTED_EDGE('',*,*,#46420,.T.);
#73416=ORIENTED_EDGE('',*,*,#46417,.T.);
#73417=ORIENTED_EDGE('',*,*,#46414,.T.);
#73418=ORIENTED_EDGE('',*,*,#46422,.T.);
#73419=ORIENTED_EDGE('',*,*,#46408,.T.);
#73420=ORIENTED_EDGE('',*,*,#46405,.T.);
#73421=ORIENTED_EDGE('',*,*,#46402,.T.);
#73422=ORIENTED_EDGE('',*,*,#46410,.T.);
#73423=ORIENTED_EDGE('',*,*,#46396,.T.);
#73424=ORIENTED_EDGE('',*,*,#46393,.T.);
#73425=ORIENTED_EDGE('',*,*,#46390,.T.);
#73426=ORIENTED_EDGE('',*,*,#46398,.T.);
#73427=ORIENTED_EDGE('',*,*,#46384,.T.);
#73428=ORIENTED_EDGE('',*,*,#46381,.T.);
#73429=ORIENTED_EDGE('',*,*,#46378,.T.);
#73430=ORIENTED_EDGE('',*,*,#46386,.T.);
#73431=ORIENTED_EDGE('',*,*,#46372,.T.);
#73432=ORIENTED_EDGE('',*,*,#46369,.T.);
#73433=ORIENTED_EDGE('',*,*,#46366,.T.);
#73434=ORIENTED_EDGE('',*,*,#46374,.T.);
#73435=ORIENTED_EDGE('',*,*,#46360,.T.);
#73436=ORIENTED_EDGE('',*,*,#46357,.T.);
#73437=ORIENTED_EDGE('',*,*,#46354,.T.);
#73438=ORIENTED_EDGE('',*,*,#46362,.T.);
#73439=ORIENTED_EDGE('',*,*,#46348,.T.);
#73440=ORIENTED_EDGE('',*,*,#46345,.T.);
#73441=ORIENTED_EDGE('',*,*,#46342,.T.);
#73442=ORIENTED_EDGE('',*,*,#46350,.T.);
#73443=ORIENTED_EDGE('',*,*,#46336,.T.);
#73444=ORIENTED_EDGE('',*,*,#46333,.T.);
#73445=ORIENTED_EDGE('',*,*,#46330,.T.);
#73446=ORIENTED_EDGE('',*,*,#46338,.T.);
#73447=ORIENTED_EDGE('',*,*,#46324,.T.);
#73448=ORIENTED_EDGE('',*,*,#46321,.T.);
#73449=ORIENTED_EDGE('',*,*,#46318,.T.);
#73450=ORIENTED_EDGE('',*,*,#46326,.T.);
#73451=ORIENTED_EDGE('',*,*,#46312,.T.);
#73452=ORIENTED_EDGE('',*,*,#46309,.T.);
#73453=ORIENTED_EDGE('',*,*,#46306,.T.);
#73454=ORIENTED_EDGE('',*,*,#46314,.T.);
#73455=ORIENTED_EDGE('',*,*,#46300,.T.);
#73456=ORIENTED_EDGE('',*,*,#46297,.T.);
#73457=ORIENTED_EDGE('',*,*,#46294,.T.);
#73458=ORIENTED_EDGE('',*,*,#46302,.T.);
#73459=ORIENTED_EDGE('',*,*,#46288,.T.);
#73460=ORIENTED_EDGE('',*,*,#46285,.T.);
#73461=ORIENTED_EDGE('',*,*,#46282,.T.);
#73462=ORIENTED_EDGE('',*,*,#46290,.T.);
#73463=ORIENTED_EDGE('',*,*,#46276,.T.);
#73464=ORIENTED_EDGE('',*,*,#46273,.T.);
#73465=ORIENTED_EDGE('',*,*,#46270,.T.);
#73466=ORIENTED_EDGE('',*,*,#46278,.T.);
#73467=ORIENTED_EDGE('',*,*,#46264,.T.);
#73468=ORIENTED_EDGE('',*,*,#46261,.T.);
#73469=ORIENTED_EDGE('',*,*,#46258,.T.);
#73470=ORIENTED_EDGE('',*,*,#46266,.T.);
#73471=ORIENTED_EDGE('',*,*,#46252,.T.);
#73472=ORIENTED_EDGE('',*,*,#46249,.T.);
#73473=ORIENTED_EDGE('',*,*,#46246,.T.);
#73474=ORIENTED_EDGE('',*,*,#46254,.T.);
#73475=ORIENTED_EDGE('',*,*,#46240,.T.);
#73476=ORIENTED_EDGE('',*,*,#46237,.T.);
#73477=ORIENTED_EDGE('',*,*,#46234,.T.);
#73478=ORIENTED_EDGE('',*,*,#46242,.T.);
#73479=ORIENTED_EDGE('',*,*,#46228,.T.);
#73480=ORIENTED_EDGE('',*,*,#46225,.T.);
#73481=ORIENTED_EDGE('',*,*,#46222,.T.);
#73482=ORIENTED_EDGE('',*,*,#46230,.T.);
#73483=ORIENTED_EDGE('',*,*,#46216,.T.);
#73484=ORIENTED_EDGE('',*,*,#46213,.T.);
#73485=ORIENTED_EDGE('',*,*,#46210,.T.);
#73486=ORIENTED_EDGE('',*,*,#46218,.T.);
#73487=ORIENTED_EDGE('',*,*,#46204,.T.);
#73488=ORIENTED_EDGE('',*,*,#46201,.T.);
#73489=ORIENTED_EDGE('',*,*,#46198,.T.);
#73490=ORIENTED_EDGE('',*,*,#46206,.T.);
#73491=ORIENTED_EDGE('',*,*,#46192,.T.);
#73492=ORIENTED_EDGE('',*,*,#46189,.T.);
#73493=ORIENTED_EDGE('',*,*,#46186,.T.);
#73494=ORIENTED_EDGE('',*,*,#46194,.T.);
#73495=ORIENTED_EDGE('',*,*,#46180,.T.);
#73496=ORIENTED_EDGE('',*,*,#46177,.T.);
#73497=ORIENTED_EDGE('',*,*,#46174,.T.);
#73498=ORIENTED_EDGE('',*,*,#46182,.T.);
#73499=ORIENTED_EDGE('',*,*,#46168,.T.);
#73500=ORIENTED_EDGE('',*,*,#46165,.T.);
#73501=ORIENTED_EDGE('',*,*,#46162,.T.);
#73502=ORIENTED_EDGE('',*,*,#46170,.T.);
#73503=ORIENTED_EDGE('',*,*,#46156,.T.);
#73504=ORIENTED_EDGE('',*,*,#46153,.T.);
#73505=ORIENTED_EDGE('',*,*,#46150,.T.);
#73506=ORIENTED_EDGE('',*,*,#46158,.T.);
#73507=ORIENTED_EDGE('',*,*,#46144,.T.);
#73508=ORIENTED_EDGE('',*,*,#46141,.T.);
#73509=ORIENTED_EDGE('',*,*,#46138,.T.);
#73510=ORIENTED_EDGE('',*,*,#46146,.T.);
#73511=ORIENTED_EDGE('',*,*,#46132,.T.);
#73512=ORIENTED_EDGE('',*,*,#46129,.T.);
#73513=ORIENTED_EDGE('',*,*,#46126,.T.);
#73514=ORIENTED_EDGE('',*,*,#46134,.T.);
#73515=ORIENTED_EDGE('',*,*,#46120,.T.);
#73516=ORIENTED_EDGE('',*,*,#46117,.T.);
#73517=ORIENTED_EDGE('',*,*,#46114,.T.);
#73518=ORIENTED_EDGE('',*,*,#46122,.T.);
#73519=ORIENTED_EDGE('',*,*,#46108,.T.);
#73520=ORIENTED_EDGE('',*,*,#46105,.T.);
#73521=ORIENTED_EDGE('',*,*,#46102,.T.);
#73522=ORIENTED_EDGE('',*,*,#46110,.T.);
#73523=ORIENTED_EDGE('',*,*,#46096,.T.);
#73524=ORIENTED_EDGE('',*,*,#46093,.T.);
#73525=ORIENTED_EDGE('',*,*,#46090,.T.);
#73526=ORIENTED_EDGE('',*,*,#46098,.T.);
#73527=ORIENTED_EDGE('',*,*,#46084,.T.);
#73528=ORIENTED_EDGE('',*,*,#46081,.T.);
#73529=ORIENTED_EDGE('',*,*,#46078,.T.);
#73530=ORIENTED_EDGE('',*,*,#46086,.T.);
#73531=ORIENTED_EDGE('',*,*,#46072,.T.);
#73532=ORIENTED_EDGE('',*,*,#46069,.T.);
#73533=ORIENTED_EDGE('',*,*,#46066,.T.);
#73534=ORIENTED_EDGE('',*,*,#46074,.T.);
#73535=ORIENTED_EDGE('',*,*,#46060,.T.);
#73536=ORIENTED_EDGE('',*,*,#46057,.T.);
#73537=ORIENTED_EDGE('',*,*,#46054,.T.);
#73538=ORIENTED_EDGE('',*,*,#46062,.T.);
#73539=ORIENTED_EDGE('',*,*,#46048,.T.);
#73540=ORIENTED_EDGE('',*,*,#46045,.T.);
#73541=ORIENTED_EDGE('',*,*,#46042,.T.);
#73542=ORIENTED_EDGE('',*,*,#46050,.T.);
#73543=ORIENTED_EDGE('',*,*,#46036,.T.);
#73544=ORIENTED_EDGE('',*,*,#46033,.T.);
#73545=ORIENTED_EDGE('',*,*,#46030,.T.);
#73546=ORIENTED_EDGE('',*,*,#46038,.T.);
#73547=ORIENTED_EDGE('',*,*,#46024,.T.);
#73548=ORIENTED_EDGE('',*,*,#46021,.T.);
#73549=ORIENTED_EDGE('',*,*,#46018,.T.);
#73550=ORIENTED_EDGE('',*,*,#46026,.T.);
#73551=ORIENTED_EDGE('',*,*,#46012,.T.);
#73552=ORIENTED_EDGE('',*,*,#46009,.T.);
#73553=ORIENTED_EDGE('',*,*,#46006,.T.);
#73554=ORIENTED_EDGE('',*,*,#46014,.T.);
#73555=ORIENTED_EDGE('',*,*,#46000,.T.);
#73556=ORIENTED_EDGE('',*,*,#45997,.T.);
#73557=ORIENTED_EDGE('',*,*,#45994,.T.);
#73558=ORIENTED_EDGE('',*,*,#46002,.T.);
#73559=ORIENTED_EDGE('',*,*,#45988,.T.);
#73560=ORIENTED_EDGE('',*,*,#45985,.T.);
#73561=ORIENTED_EDGE('',*,*,#45982,.T.);
#73562=ORIENTED_EDGE('',*,*,#45990,.T.);
#73563=ORIENTED_EDGE('',*,*,#45976,.T.);
#73564=ORIENTED_EDGE('',*,*,#45973,.T.);
#73565=ORIENTED_EDGE('',*,*,#45970,.T.);
#73566=ORIENTED_EDGE('',*,*,#45978,.T.);
#73567=ORIENTED_EDGE('',*,*,#45964,.T.);
#73568=ORIENTED_EDGE('',*,*,#45961,.T.);
#73569=ORIENTED_EDGE('',*,*,#45958,.T.);
#73570=ORIENTED_EDGE('',*,*,#45966,.T.);
#73571=ORIENTED_EDGE('',*,*,#45952,.T.);
#73572=ORIENTED_EDGE('',*,*,#45949,.T.);
#73573=ORIENTED_EDGE('',*,*,#45946,.T.);
#73574=ORIENTED_EDGE('',*,*,#45954,.T.);
#73575=ORIENTED_EDGE('',*,*,#45940,.T.);
#73576=ORIENTED_EDGE('',*,*,#45937,.T.);
#73577=ORIENTED_EDGE('',*,*,#45934,.T.);
#73578=ORIENTED_EDGE('',*,*,#45942,.T.);
#73579=ORIENTED_EDGE('',*,*,#45928,.T.);
#73580=ORIENTED_EDGE('',*,*,#45925,.T.);
#73581=ORIENTED_EDGE('',*,*,#45922,.T.);
#73582=ORIENTED_EDGE('',*,*,#45930,.T.);
#73583=ORIENTED_EDGE('',*,*,#45916,.T.);
#73584=ORIENTED_EDGE('',*,*,#45913,.T.);
#73585=ORIENTED_EDGE('',*,*,#45910,.T.);
#73586=ORIENTED_EDGE('',*,*,#45918,.T.);
#73587=ORIENTED_EDGE('',*,*,#45904,.T.);
#73588=ORIENTED_EDGE('',*,*,#45901,.T.);
#73589=ORIENTED_EDGE('',*,*,#45898,.T.);
#73590=ORIENTED_EDGE('',*,*,#45906,.T.);
#73591=ORIENTED_EDGE('',*,*,#45892,.T.);
#73592=ORIENTED_EDGE('',*,*,#45889,.T.);
#73593=ORIENTED_EDGE('',*,*,#45886,.T.);
#73594=ORIENTED_EDGE('',*,*,#45894,.T.);
#73595=ORIENTED_EDGE('',*,*,#45880,.T.);
#73596=ORIENTED_EDGE('',*,*,#45877,.T.);
#73597=ORIENTED_EDGE('',*,*,#45874,.T.);
#73598=ORIENTED_EDGE('',*,*,#45882,.T.);
#73599=ORIENTED_EDGE('',*,*,#45868,.T.);
#73600=ORIENTED_EDGE('',*,*,#45865,.T.);
#73601=ORIENTED_EDGE('',*,*,#45862,.T.);
#73602=ORIENTED_EDGE('',*,*,#45870,.T.);
#73603=ORIENTED_EDGE('',*,*,#45856,.T.);
#73604=ORIENTED_EDGE('',*,*,#45853,.T.);
#73605=ORIENTED_EDGE('',*,*,#45850,.T.);
#73606=ORIENTED_EDGE('',*,*,#45858,.T.);
#73607=ORIENTED_EDGE('',*,*,#45844,.T.);
#73608=ORIENTED_EDGE('',*,*,#45841,.T.);
#73609=ORIENTED_EDGE('',*,*,#45838,.T.);
#73610=ORIENTED_EDGE('',*,*,#45846,.T.);
#73611=ORIENTED_EDGE('',*,*,#45832,.T.);
#73612=ORIENTED_EDGE('',*,*,#45829,.T.);
#73613=ORIENTED_EDGE('',*,*,#45826,.T.);
#73614=ORIENTED_EDGE('',*,*,#45834,.T.);
#73615=ORIENTED_EDGE('',*,*,#45820,.T.);
#73616=ORIENTED_EDGE('',*,*,#45817,.T.);
#73617=ORIENTED_EDGE('',*,*,#45814,.T.);
#73618=ORIENTED_EDGE('',*,*,#45822,.T.);
#73619=ORIENTED_EDGE('',*,*,#45799,.T.);
#73620=ORIENTED_EDGE('',*,*,#45809,.T.);
#73621=ORIENTED_EDGE('',*,*,#45806,.T.);
#73622=ORIENTED_EDGE('',*,*,#45802,.T.);
#73623=ORIENTED_EDGE('',*,*,#45794,.T.);
#73624=ORIENTED_EDGE('',*,*,#45791,.T.);
#73625=ORIENTED_EDGE('',*,*,#45788,.T.);
#73626=ORIENTED_EDGE('',*,*,#45784,.T.);
#73627=ORIENTED_EDGE('',*,*,#45778,.T.);
#73628=ORIENTED_EDGE('',*,*,#45775,.T.);
#73629=ORIENTED_EDGE('',*,*,#45772,.T.);
#73630=ORIENTED_EDGE('',*,*,#45780,.T.);
#73631=ORIENTED_EDGE('',*,*,#45766,.T.);
#73632=ORIENTED_EDGE('',*,*,#45763,.T.);
#73633=ORIENTED_EDGE('',*,*,#45760,.T.);
#73634=ORIENTED_EDGE('',*,*,#45768,.T.);
#73635=ORIENTED_EDGE('',*,*,#45754,.T.);
#73636=ORIENTED_EDGE('',*,*,#45751,.T.);
#73637=ORIENTED_EDGE('',*,*,#45748,.T.);
#73638=ORIENTED_EDGE('',*,*,#45756,.T.);
#73639=ORIENTED_EDGE('',*,*,#45742,.T.);
#73640=ORIENTED_EDGE('',*,*,#45739,.T.);
#73641=ORIENTED_EDGE('',*,*,#45736,.T.);
#73642=ORIENTED_EDGE('',*,*,#45744,.T.);
#73643=ORIENTED_EDGE('',*,*,#45730,.T.);
#73644=ORIENTED_EDGE('',*,*,#45727,.T.);
#73645=ORIENTED_EDGE('',*,*,#45724,.T.);
#73646=ORIENTED_EDGE('',*,*,#45732,.T.);
#73647=ORIENTED_EDGE('',*,*,#45718,.T.);
#73648=ORIENTED_EDGE('',*,*,#45715,.T.);
#73649=ORIENTED_EDGE('',*,*,#45712,.T.);
#73650=ORIENTED_EDGE('',*,*,#45720,.T.);
#73651=ORIENTED_EDGE('',*,*,#45706,.T.);
#73652=ORIENTED_EDGE('',*,*,#45703,.T.);
#73653=ORIENTED_EDGE('',*,*,#45700,.T.);
#73654=ORIENTED_EDGE('',*,*,#45708,.T.);
#73655=ORIENTED_EDGE('',*,*,#45694,.T.);
#73656=ORIENTED_EDGE('',*,*,#45691,.T.);
#73657=ORIENTED_EDGE('',*,*,#45688,.T.);
#73658=ORIENTED_EDGE('',*,*,#45696,.T.);
#73659=ORIENTED_EDGE('',*,*,#45682,.T.);
#73660=ORIENTED_EDGE('',*,*,#45679,.T.);
#73661=ORIENTED_EDGE('',*,*,#45676,.T.);
#73662=ORIENTED_EDGE('',*,*,#45684,.T.);
#73663=ORIENTED_EDGE('',*,*,#45664,.T.);
#73664=ORIENTED_EDGE('',*,*,#45661,.T.);
#73665=ORIENTED_EDGE('',*,*,#45671,.T.);
#73666=ORIENTED_EDGE('',*,*,#45668,.T.);
#73667=ORIENTED_EDGE('',*,*,#45649,.T.);
#73668=ORIENTED_EDGE('',*,*,#45646,.T.);
#73669=ORIENTED_EDGE('',*,*,#45656,.T.);
#73670=ORIENTED_EDGE('',*,*,#45653,.T.);
#73671=ORIENTED_EDGE('',*,*,#45640,.T.);
#73672=ORIENTED_EDGE('',*,*,#45637,.T.);
#73673=ORIENTED_EDGE('',*,*,#45634,.T.);
#73674=ORIENTED_EDGE('',*,*,#45642,.T.);
#73675=ORIENTED_EDGE('',*,*,#45628,.T.);
#73676=ORIENTED_EDGE('',*,*,#45625,.T.);
#73677=ORIENTED_EDGE('',*,*,#45622,.T.);
#73678=ORIENTED_EDGE('',*,*,#45630,.T.);
#73679=ORIENTED_EDGE('',*,*,#45616,.T.);
#73680=ORIENTED_EDGE('',*,*,#45613,.T.);
#73681=ORIENTED_EDGE('',*,*,#45610,.T.);
#73682=ORIENTED_EDGE('',*,*,#45618,.T.);
#73683=ORIENTED_EDGE('',*,*,#45604,.T.);
#73684=ORIENTED_EDGE('',*,*,#45601,.T.);
#73685=ORIENTED_EDGE('',*,*,#45598,.T.);
#73686=ORIENTED_EDGE('',*,*,#45606,.T.);
#73687=ORIENTED_EDGE('',*,*,#45592,.T.);
#73688=ORIENTED_EDGE('',*,*,#45589,.T.);
#73689=ORIENTED_EDGE('',*,*,#45586,.T.);
#73690=ORIENTED_EDGE('',*,*,#45594,.T.);
#73691=ORIENTED_EDGE('',*,*,#45580,.T.);
#73692=ORIENTED_EDGE('',*,*,#45577,.T.);
#73693=ORIENTED_EDGE('',*,*,#45574,.T.);
#73694=ORIENTED_EDGE('',*,*,#45582,.T.);
#73695=ORIENTED_EDGE('',*,*,#45568,.T.);
#73696=ORIENTED_EDGE('',*,*,#45565,.T.);
#73697=ORIENTED_EDGE('',*,*,#45562,.T.);
#73698=ORIENTED_EDGE('',*,*,#45570,.T.);
#73699=ORIENTED_EDGE('',*,*,#45556,.T.);
#73700=ORIENTED_EDGE('',*,*,#45553,.T.);
#73701=ORIENTED_EDGE('',*,*,#45550,.T.);
#73702=ORIENTED_EDGE('',*,*,#45558,.T.);
#73703=ORIENTED_EDGE('',*,*,#45544,.T.);
#73704=ORIENTED_EDGE('',*,*,#45541,.T.);
#73705=ORIENTED_EDGE('',*,*,#45538,.T.);
#73706=ORIENTED_EDGE('',*,*,#45546,.T.);
#73707=ORIENTED_EDGE('',*,*,#45532,.T.);
#73708=ORIENTED_EDGE('',*,*,#45529,.T.);
#73709=ORIENTED_EDGE('',*,*,#45526,.T.);
#73710=ORIENTED_EDGE('',*,*,#45534,.T.);
#73711=ORIENTED_EDGE('',*,*,#45511,.T.);
#73712=ORIENTED_EDGE('',*,*,#45521,.T.);
#73713=ORIENTED_EDGE('',*,*,#45518,.T.);
#73714=ORIENTED_EDGE('',*,*,#45514,.T.);
#73715=ORIENTED_EDGE('',*,*,#45506,.T.);
#73716=ORIENTED_EDGE('',*,*,#45503,.T.);
#73717=ORIENTED_EDGE('',*,*,#45500,.T.);
#73718=ORIENTED_EDGE('',*,*,#45496,.T.);
#73719=ORIENTED_EDGE('',*,*,#45491,.T.);
#73720=ORIENTED_EDGE('',*,*,#45488,.T.);
#73721=ORIENTED_EDGE('',*,*,#45485,.T.);
#73722=ORIENTED_EDGE('',*,*,#45481,.T.);
#73723=ORIENTED_EDGE('',*,*,#45466,.T.);
#73724=ORIENTED_EDGE('',*,*,#45476,.T.);
#73725=ORIENTED_EDGE('',*,*,#45473,.T.);
#73726=ORIENTED_EDGE('',*,*,#45469,.T.);
#73727=ORIENTED_EDGE('',*,*,#45460,.T.);
#73728=ORIENTED_EDGE('',*,*,#45457,.T.);
#73729=ORIENTED_EDGE('',*,*,#45454,.T.);
#73730=ORIENTED_EDGE('',*,*,#45462,.T.);
#73731=ORIENTED_EDGE('',*,*,#45448,.T.);
#73732=ORIENTED_EDGE('',*,*,#45445,.T.);
#73733=ORIENTED_EDGE('',*,*,#45442,.T.);
#73734=ORIENTED_EDGE('',*,*,#45450,.T.);
#73735=ORIENTED_EDGE('',*,*,#45436,.T.);
#73736=ORIENTED_EDGE('',*,*,#45433,.T.);
#73737=ORIENTED_EDGE('',*,*,#45430,.T.);
#73738=ORIENTED_EDGE('',*,*,#45438,.T.);
#73739=ORIENTED_EDGE('',*,*,#45421,.T.);
#73740=ORIENTED_EDGE('',*,*,#45418,.T.);
#73741=ORIENTED_EDGE('',*,*,#45426,.T.);
#73742=ORIENTED_EDGE('',*,*,#45424,.T.);
#73743=ORIENTED_EDGE('',*,*,#45404,.T.);
#73744=ORIENTED_EDGE('',*,*,#45413,.T.);
#73745=ORIENTED_EDGE('',*,*,#45410,.T.);
#73746=ORIENTED_EDGE('',*,*,#45407,.T.);
#73747=ORIENTED_EDGE('',*,*,#45389,.T.);
#73748=ORIENTED_EDGE('',*,*,#45398,.T.);
#73749=ORIENTED_EDGE('',*,*,#45395,.T.);
#73750=ORIENTED_EDGE('',*,*,#45392,.T.);
#73751=ORIENTED_EDGE('',*,*,#45382,.T.);
#73752=ORIENTED_EDGE('',*,*,#45379,.T.);
#73753=ORIENTED_EDGE('',*,*,#45376,.T.);
#73754=ORIENTED_EDGE('',*,*,#45384,.T.);
#73755=ORIENTED_EDGE('',*,*,#45370,.T.);
#73756=ORIENTED_EDGE('',*,*,#45367,.T.);
#73757=ORIENTED_EDGE('',*,*,#45364,.T.);
#73758=ORIENTED_EDGE('',*,*,#45372,.T.);
#73759=ORIENTED_EDGE('',*,*,#45358,.T.);
#73760=ORIENTED_EDGE('',*,*,#45355,.T.);
#73761=ORIENTED_EDGE('',*,*,#45352,.T.);
#73762=ORIENTED_EDGE('',*,*,#45360,.T.);
#73763=ORIENTED_EDGE('',*,*,#45346,.T.);
#73764=ORIENTED_EDGE('',*,*,#45343,.T.);
#73765=ORIENTED_EDGE('',*,*,#45340,.T.);
#73766=ORIENTED_EDGE('',*,*,#45348,.T.);
#73767=ORIENTED_EDGE('',*,*,#45334,.T.);
#73768=ORIENTED_EDGE('',*,*,#45331,.T.);
#73769=ORIENTED_EDGE('',*,*,#45328,.T.);
#73770=ORIENTED_EDGE('',*,*,#45336,.T.);
#73771=ORIENTED_EDGE('',*,*,#45322,.T.);
#73772=ORIENTED_EDGE('',*,*,#45319,.T.);
#73773=ORIENTED_EDGE('',*,*,#45316,.T.);
#73774=ORIENTED_EDGE('',*,*,#45324,.T.);
#73775=ORIENTED_EDGE('',*,*,#45310,.T.);
#73776=ORIENTED_EDGE('',*,*,#45307,.T.);
#73777=ORIENTED_EDGE('',*,*,#45304,.T.);
#73778=ORIENTED_EDGE('',*,*,#45312,.T.);
#73779=ORIENTED_EDGE('',*,*,#45298,.T.);
#73780=ORIENTED_EDGE('',*,*,#45295,.T.);
#73781=ORIENTED_EDGE('',*,*,#45292,.T.);
#73782=ORIENTED_EDGE('',*,*,#45300,.T.);
#73783=ORIENTED_EDGE('',*,*,#45277,.T.);
#73784=ORIENTED_EDGE('',*,*,#45287,.T.);
#73785=ORIENTED_EDGE('',*,*,#45284,.T.);
#73786=ORIENTED_EDGE('',*,*,#45281,.T.);
#73787=ORIENTED_EDGE('',*,*,#45266,.T.);
#73788=ORIENTED_EDGE('',*,*,#45262,.T.);
#73789=ORIENTED_EDGE('',*,*,#45272,.T.);
#73790=ORIENTED_EDGE('',*,*,#45269,.T.);
#73791=ORIENTED_EDGE('',*,*,#45251,.T.);
#73792=ORIENTED_EDGE('',*,*,#45247,.T.);
#73793=ORIENTED_EDGE('',*,*,#45257,.T.);
#73794=ORIENTED_EDGE('',*,*,#45254,.T.);
#73795=ORIENTED_EDGE('',*,*,#45233,.T.);
#73796=ORIENTED_EDGE('',*,*,#45242,.T.);
#73797=ORIENTED_EDGE('',*,*,#45239,.T.);
#73798=ORIENTED_EDGE('',*,*,#45236,.T.);
#73799=ORIENTED_EDGE('',*,*,#45218,.T.);
#73800=ORIENTED_EDGE('',*,*,#45227,.T.);
#73801=ORIENTED_EDGE('',*,*,#45224,.T.);
#73802=ORIENTED_EDGE('',*,*,#45221,.T.);
#73803=ORIENTED_EDGE('',*,*,#45202,.T.);
#73804=ORIENTED_EDGE('',*,*,#45212,.T.);
#73805=ORIENTED_EDGE('',*,*,#45209,.T.);
#73806=ORIENTED_EDGE('',*,*,#45206,.T.);
#73807=ORIENTED_EDGE('',*,*,#45187,.T.);
#73808=ORIENTED_EDGE('',*,*,#45197,.T.);
#73809=ORIENTED_EDGE('',*,*,#45194,.T.);
#73810=ORIENTED_EDGE('',*,*,#45191,.T.);
#73811=ORIENTED_EDGE('',*,*,#45172,.T.);
#73812=ORIENTED_EDGE('',*,*,#45182,.T.);
#73813=ORIENTED_EDGE('',*,*,#45179,.T.);
#73814=ORIENTED_EDGE('',*,*,#45176,.T.);
#73815=ORIENTED_EDGE('',*,*,#45157,.T.);
#73816=ORIENTED_EDGE('',*,*,#45167,.T.);
#73817=ORIENTED_EDGE('',*,*,#45164,.T.);
#73818=ORIENTED_EDGE('',*,*,#45161,.T.);
#73819=ORIENTED_EDGE('',*,*,#45143,.T.);
#73820=ORIENTED_EDGE('',*,*,#45152,.T.);
#73821=ORIENTED_EDGE('',*,*,#45150,.T.);
#73822=ORIENTED_EDGE('',*,*,#45147,.T.);
#73823=ORIENTED_EDGE('',*,*,#43570,.T.);
#73824=ORIENTED_EDGE('',*,*,#43571,.T.);
#73825=ORIENTED_EDGE('',*,*,#43574,.T.);
#73826=ORIENTED_EDGE('',*,*,#43563,.T.);
#73827=ORIENTED_EDGE('',*,*,#43584,.T.);
#73828=ORIENTED_EDGE('',*,*,#43586,.T.);
#73829=ORIENTED_EDGE('',*,*,#43589,.T.);
#73830=ORIENTED_EDGE('',*,*,#43578,.T.);
#73831=ORIENTED_EDGE('',*,*,#43599,.T.);
#73832=ORIENTED_EDGE('',*,*,#43596,.T.);
#73833=ORIENTED_EDGE('',*,*,#43605,.T.);
#73834=ORIENTED_EDGE('',*,*,#43602,.T.);
#73835=ORIENTED_EDGE('',*,*,#43616,.T.);
#73836=ORIENTED_EDGE('',*,*,#43613,.T.);
#73837=ORIENTED_EDGE('',*,*,#43610,.T.);
#73838=ORIENTED_EDGE('',*,*,#43618,.T.);
#73839=ORIENTED_EDGE('',*,*,#43628,.T.);
#73840=ORIENTED_EDGE('',*,*,#43625,.T.);
#73841=ORIENTED_EDGE('',*,*,#43622,.T.);
#73842=ORIENTED_EDGE('',*,*,#43630,.T.);
#73843=ORIENTED_EDGE('',*,*,#43640,.T.);
#73844=ORIENTED_EDGE('',*,*,#43637,.T.);
#73845=ORIENTED_EDGE('',*,*,#43634,.T.);
#73846=ORIENTED_EDGE('',*,*,#43642,.T.);
#73847=ORIENTED_EDGE('',*,*,#43649,.T.);
#73848=ORIENTED_EDGE('',*,*,#43646,.T.);
#73849=ORIENTED_EDGE('',*,*,#43654,.T.);
#73850=ORIENTED_EDGE('',*,*,#43652,.T.);
#73851=ORIENTED_EDGE('',*,*,#43661,.T.);
#73852=ORIENTED_EDGE('',*,*,#43663,.T.);
#73853=ORIENTED_EDGE('',*,*,#43666,.T.);
#73854=ORIENTED_EDGE('',*,*,#43655,.T.);
#73855=ORIENTED_EDGE('',*,*,#43680,.T.);
#73856=ORIENTED_EDGE('',*,*,#43677,.T.);
#73857=ORIENTED_EDGE('',*,*,#43673,.T.);
#73858=ORIENTED_EDGE('',*,*,#43683,.T.);
#73859=ORIENTED_EDGE('',*,*,#43695,.T.);
#73860=ORIENTED_EDGE('',*,*,#43692,.T.);
#73861=ORIENTED_EDGE('',*,*,#43688,.T.);
#73862=ORIENTED_EDGE('',*,*,#43698,.T.);
#73863=ORIENTED_EDGE('',*,*,#43710,.T.);
#73864=ORIENTED_EDGE('',*,*,#43706,.T.);
#73865=ORIENTED_EDGE('',*,*,#43703,.T.);
#73866=ORIENTED_EDGE('',*,*,#43713,.T.);
#73867=ORIENTED_EDGE('',*,*,#43724,.T.);
#73868=ORIENTED_EDGE('',*,*,#43721,.T.);
#73869=ORIENTED_EDGE('',*,*,#43718,.T.);
#73870=ORIENTED_EDGE('',*,*,#43726,.T.);
#73871=ORIENTED_EDGE('',*,*,#43737,.T.);
#73872=ORIENTED_EDGE('',*,*,#43734,.T.);
#73873=ORIENTED_EDGE('',*,*,#43730,.T.);
#73874=ORIENTED_EDGE('',*,*,#43740,.T.);
#73875=ORIENTED_EDGE('',*,*,#43752,.T.);
#73876=ORIENTED_EDGE('',*,*,#43749,.T.);
#73877=ORIENTED_EDGE('',*,*,#43745,.T.);
#73878=ORIENTED_EDGE('',*,*,#43755,.T.);
#73879=ORIENTED_EDGE('',*,*,#43770,.T.);
#73880=ORIENTED_EDGE('',*,*,#43767,.T.);
#73881=ORIENTED_EDGE('',*,*,#43764,.T.);
#73882=ORIENTED_EDGE('',*,*,#43760,.T.);
#73883=ORIENTED_EDGE('',*,*,#43785,.T.);
#73884=ORIENTED_EDGE('',*,*,#43782,.T.);
#73885=ORIENTED_EDGE('',*,*,#43779,.T.);
#73886=ORIENTED_EDGE('',*,*,#43775,.T.);
#73887=ORIENTED_EDGE('',*,*,#43796,.T.);
#73888=ORIENTED_EDGE('',*,*,#43793,.T.);
#73889=ORIENTED_EDGE('',*,*,#43790,.T.);
#73890=ORIENTED_EDGE('',*,*,#43798,.T.);
#73891=ORIENTED_EDGE('',*,*,#43808,.T.);
#73892=ORIENTED_EDGE('',*,*,#43805,.T.);
#73893=ORIENTED_EDGE('',*,*,#43802,.T.);
#73894=ORIENTED_EDGE('',*,*,#43810,.T.);
#73895=ORIENTED_EDGE('',*,*,#43820,.T.);
#73896=ORIENTED_EDGE('',*,*,#43817,.T.);
#73897=ORIENTED_EDGE('',*,*,#43814,.T.);
#73898=ORIENTED_EDGE('',*,*,#43822,.T.);
#73899=ORIENTED_EDGE('',*,*,#43832,.T.);
#73900=ORIENTED_EDGE('',*,*,#43829,.T.);
#73901=ORIENTED_EDGE('',*,*,#43826,.T.);
#73902=ORIENTED_EDGE('',*,*,#43834,.T.);
#73903=ORIENTED_EDGE('',*,*,#43844,.T.);
#73904=ORIENTED_EDGE('',*,*,#43841,.T.);
#73905=ORIENTED_EDGE('',*,*,#43838,.T.);
#73906=ORIENTED_EDGE('',*,*,#43846,.T.);
#73907=ORIENTED_EDGE('',*,*,#43856,.T.);
#73908=ORIENTED_EDGE('',*,*,#43853,.T.);
#73909=ORIENTED_EDGE('',*,*,#43850,.T.);
#73910=ORIENTED_EDGE('',*,*,#43858,.T.);
#73911=ORIENTED_EDGE('',*,*,#43868,.T.);
#73912=ORIENTED_EDGE('',*,*,#43863,.T.);
#73913=ORIENTED_EDGE('',*,*,#43859,.T.);
#73914=ORIENTED_EDGE('',*,*,#43870,.T.);
#73915=ORIENTED_EDGE('',*,*,#43884,.T.);
#73916=ORIENTED_EDGE('',*,*,#43881,.T.);
#73917=ORIENTED_EDGE('',*,*,#43877,.T.);
#73918=ORIENTED_EDGE('',*,*,#43887,.T.);
#73919=ORIENTED_EDGE('',*,*,#43898,.T.);
#73920=ORIENTED_EDGE('',*,*,#43895,.T.);
#73921=ORIENTED_EDGE('',*,*,#43892,.T.);
#73922=ORIENTED_EDGE('',*,*,#43900,.T.);
#73923=ORIENTED_EDGE('',*,*,#43910,.T.);
#73924=ORIENTED_EDGE('',*,*,#43907,.T.);
#73925=ORIENTED_EDGE('',*,*,#43904,.T.);
#73926=ORIENTED_EDGE('',*,*,#43912,.T.);
#73927=ORIENTED_EDGE('',*,*,#43922,.T.);
#73928=ORIENTED_EDGE('',*,*,#43919,.T.);
#73929=ORIENTED_EDGE('',*,*,#43916,.T.);
#73930=ORIENTED_EDGE('',*,*,#43924,.T.);
#73931=ORIENTED_EDGE('',*,*,#43934,.T.);
#73932=ORIENTED_EDGE('',*,*,#43931,.T.);
#73933=ORIENTED_EDGE('',*,*,#43928,.T.);
#73934=ORIENTED_EDGE('',*,*,#43936,.T.);
#73935=ORIENTED_EDGE('',*,*,#43946,.T.);
#73936=ORIENTED_EDGE('',*,*,#43943,.T.);
#73937=ORIENTED_EDGE('',*,*,#43940,.T.);
#73938=ORIENTED_EDGE('',*,*,#43948,.T.);
#73939=ORIENTED_EDGE('',*,*,#43958,.T.);
#73940=ORIENTED_EDGE('',*,*,#43955,.T.);
#73941=ORIENTED_EDGE('',*,*,#43952,.T.);
#73942=ORIENTED_EDGE('',*,*,#43960,.T.);
#73943=ORIENTED_EDGE('',*,*,#43970,.T.);
#73944=ORIENTED_EDGE('',*,*,#43967,.T.);
#73945=ORIENTED_EDGE('',*,*,#43964,.T.);
#73946=ORIENTED_EDGE('',*,*,#43972,.T.);
#73947=ORIENTED_EDGE('',*,*,#43982,.T.);
#73948=ORIENTED_EDGE('',*,*,#43979,.T.);
#73949=ORIENTED_EDGE('',*,*,#43976,.T.);
#73950=ORIENTED_EDGE('',*,*,#43984,.T.);
#73951=ORIENTED_EDGE('',*,*,#43995,.T.);
#73952=ORIENTED_EDGE('',*,*,#43992,.T.);
#73953=ORIENTED_EDGE('',*,*,#43988,.T.);
#73954=ORIENTED_EDGE('',*,*,#43998,.T.);
#73955=ORIENTED_EDGE('',*,*,#44013,.T.);
#73956=ORIENTED_EDGE('',*,*,#44010,.T.);
#73957=ORIENTED_EDGE('',*,*,#44007,.T.);
#73958=ORIENTED_EDGE('',*,*,#44003,.T.);
#73959=ORIENTED_EDGE('',*,*,#44024,.T.);
#73960=ORIENTED_EDGE('',*,*,#44021,.T.);
#73961=ORIENTED_EDGE('',*,*,#44018,.T.);
#73962=ORIENTED_EDGE('',*,*,#44026,.T.);
#73963=ORIENTED_EDGE('',*,*,#44036,.T.);
#73964=ORIENTED_EDGE('',*,*,#44033,.T.);
#73965=ORIENTED_EDGE('',*,*,#44030,.T.);
#73966=ORIENTED_EDGE('',*,*,#44038,.T.);
#73967=ORIENTED_EDGE('',*,*,#44048,.T.);
#73968=ORIENTED_EDGE('',*,*,#44045,.T.);
#73969=ORIENTED_EDGE('',*,*,#44042,.T.);
#73970=ORIENTED_EDGE('',*,*,#44050,.T.);
#73971=ORIENTED_EDGE('',*,*,#44060,.T.);
#73972=ORIENTED_EDGE('',*,*,#44057,.T.);
#73973=ORIENTED_EDGE('',*,*,#44054,.T.);
#73974=ORIENTED_EDGE('',*,*,#44062,.T.);
#73975=ORIENTED_EDGE('',*,*,#44072,.T.);
#73976=ORIENTED_EDGE('',*,*,#44069,.T.);
#73977=ORIENTED_EDGE('',*,*,#44066,.T.);
#73978=ORIENTED_EDGE('',*,*,#44074,.T.);
#73979=ORIENTED_EDGE('',*,*,#44084,.T.);
#73980=ORIENTED_EDGE('',*,*,#44081,.T.);
#73981=ORIENTED_EDGE('',*,*,#44078,.T.);
#73982=ORIENTED_EDGE('',*,*,#44086,.T.);
#73983=ORIENTED_EDGE('',*,*,#44096,.T.);
#73984=ORIENTED_EDGE('',*,*,#44093,.T.);
#73985=ORIENTED_EDGE('',*,*,#44090,.T.);
#73986=ORIENTED_EDGE('',*,*,#44098,.T.);
#73987=ORIENTED_EDGE('',*,*,#44108,.T.);
#73988=ORIENTED_EDGE('',*,*,#44105,.T.);
#73989=ORIENTED_EDGE('',*,*,#44102,.T.);
#73990=ORIENTED_EDGE('',*,*,#44110,.T.);
#73991=ORIENTED_EDGE('',*,*,#44120,.T.);
#73992=ORIENTED_EDGE('',*,*,#44117,.T.);
#73993=ORIENTED_EDGE('',*,*,#44114,.T.);
#73994=ORIENTED_EDGE('',*,*,#44122,.T.);
#73995=ORIENTED_EDGE('',*,*,#44132,.T.);
#73996=ORIENTED_EDGE('',*,*,#44129,.T.);
#73997=ORIENTED_EDGE('',*,*,#44126,.T.);
#73998=ORIENTED_EDGE('',*,*,#44134,.T.);
#73999=ORIENTED_EDGE('',*,*,#44147,.T.);
#74000=ORIENTED_EDGE('',*,*,#44144,.T.);
#74001=ORIENTED_EDGE('',*,*,#44141,.T.);
#74002=ORIENTED_EDGE('',*,*,#44149,.T.);
#74003=ORIENTED_EDGE('',*,*,#44159,.T.);
#74004=ORIENTED_EDGE('',*,*,#44156,.T.);
#74005=ORIENTED_EDGE('',*,*,#44153,.T.);
#74006=ORIENTED_EDGE('',*,*,#44161,.T.);
#74007=ORIENTED_EDGE('',*,*,#44171,.T.);
#74008=ORIENTED_EDGE('',*,*,#44168,.T.);
#74009=ORIENTED_EDGE('',*,*,#44165,.T.);
#74010=ORIENTED_EDGE('',*,*,#44173,.T.);
#74011=ORIENTED_EDGE('',*,*,#44183,.T.);
#74012=ORIENTED_EDGE('',*,*,#44180,.T.);
#74013=ORIENTED_EDGE('',*,*,#44177,.T.);
#74014=ORIENTED_EDGE('',*,*,#44185,.T.);
#74015=ORIENTED_EDGE('',*,*,#44195,.T.);
#74016=ORIENTED_EDGE('',*,*,#44192,.T.);
#74017=ORIENTED_EDGE('',*,*,#44189,.T.);
#74018=ORIENTED_EDGE('',*,*,#44197,.T.);
#74019=ORIENTED_EDGE('',*,*,#44207,.T.);
#74020=ORIENTED_EDGE('',*,*,#44204,.T.);
#74021=ORIENTED_EDGE('',*,*,#44201,.T.);
#74022=ORIENTED_EDGE('',*,*,#44209,.T.);
#74023=ORIENTED_EDGE('',*,*,#44219,.T.);
#74024=ORIENTED_EDGE('',*,*,#44216,.T.);
#74025=ORIENTED_EDGE('',*,*,#44213,.T.);
#74026=ORIENTED_EDGE('',*,*,#44221,.T.);
#74027=ORIENTED_EDGE('',*,*,#44231,.T.);
#74028=ORIENTED_EDGE('',*,*,#44228,.T.);
#74029=ORIENTED_EDGE('',*,*,#44225,.T.);
#74030=ORIENTED_EDGE('',*,*,#44233,.T.);
#74031=ORIENTED_EDGE('',*,*,#44243,.T.);
#74032=ORIENTED_EDGE('',*,*,#44240,.T.);
#74033=ORIENTED_EDGE('',*,*,#44237,.T.);
#74034=ORIENTED_EDGE('',*,*,#44245,.T.);
#74035=ORIENTED_EDGE('',*,*,#44255,.T.);
#74036=ORIENTED_EDGE('',*,*,#44252,.T.);
#74037=ORIENTED_EDGE('',*,*,#44249,.T.);
#74038=ORIENTED_EDGE('',*,*,#44257,.T.);
#74039=ORIENTED_EDGE('',*,*,#44267,.T.);
#74040=ORIENTED_EDGE('',*,*,#44264,.T.);
#74041=ORIENTED_EDGE('',*,*,#44261,.T.);
#74042=ORIENTED_EDGE('',*,*,#44269,.T.);
#74043=ORIENTED_EDGE('',*,*,#44283,.T.);
#74044=ORIENTED_EDGE('',*,*,#44280,.T.);
#74045=ORIENTED_EDGE('',*,*,#44276,.T.);
#74046=ORIENTED_EDGE('',*,*,#44273,.T.);
#74047=ORIENTED_EDGE('',*,*,#44298,.T.);
#74048=ORIENTED_EDGE('',*,*,#44295,.T.);
#74049=ORIENTED_EDGE('',*,*,#44291,.T.);
#74050=ORIENTED_EDGE('',*,*,#44288,.T.);
#74051=ORIENTED_EDGE('',*,*,#44309,.T.);
#74052=ORIENTED_EDGE('',*,*,#44306,.T.);
#74053=ORIENTED_EDGE('',*,*,#44303,.T.);
#74054=ORIENTED_EDGE('',*,*,#44311,.T.);
#74055=ORIENTED_EDGE('',*,*,#44321,.T.);
#74056=ORIENTED_EDGE('',*,*,#44318,.T.);
#74057=ORIENTED_EDGE('',*,*,#44315,.T.);
#74058=ORIENTED_EDGE('',*,*,#44323,.T.);
#74059=ORIENTED_EDGE('',*,*,#44333,.T.);
#74060=ORIENTED_EDGE('',*,*,#44330,.T.);
#74061=ORIENTED_EDGE('',*,*,#44327,.T.);
#74062=ORIENTED_EDGE('',*,*,#44335,.T.);
#74063=ORIENTED_EDGE('',*,*,#44345,.T.);
#74064=ORIENTED_EDGE('',*,*,#44342,.T.);
#74065=ORIENTED_EDGE('',*,*,#44339,.T.);
#74066=ORIENTED_EDGE('',*,*,#44347,.T.);
#74067=ORIENTED_EDGE('',*,*,#44357,.T.);
#74068=ORIENTED_EDGE('',*,*,#44354,.T.);
#74069=ORIENTED_EDGE('',*,*,#44351,.T.);
#74070=ORIENTED_EDGE('',*,*,#44359,.T.);
#74071=ORIENTED_EDGE('',*,*,#44369,.T.);
#74072=ORIENTED_EDGE('',*,*,#44366,.T.);
#74073=ORIENTED_EDGE('',*,*,#44363,.T.);
#74074=ORIENTED_EDGE('',*,*,#44371,.T.);
#74075=ORIENTED_EDGE('',*,*,#44381,.T.);
#74076=ORIENTED_EDGE('',*,*,#44378,.T.);
#74077=ORIENTED_EDGE('',*,*,#44375,.T.);
#74078=ORIENTED_EDGE('',*,*,#44383,.T.);
#74079=ORIENTED_EDGE('',*,*,#44393,.T.);
#74080=ORIENTED_EDGE('',*,*,#44390,.T.);
#74081=ORIENTED_EDGE('',*,*,#44387,.T.);
#74082=ORIENTED_EDGE('',*,*,#44395,.T.);
#74083=ORIENTED_EDGE('',*,*,#44405,.T.);
#74084=ORIENTED_EDGE('',*,*,#44402,.T.);
#74085=ORIENTED_EDGE('',*,*,#44399,.T.);
#74086=ORIENTED_EDGE('',*,*,#44407,.T.);
#74087=ORIENTED_EDGE('',*,*,#44417,.T.);
#74088=ORIENTED_EDGE('',*,*,#44414,.T.);
#74089=ORIENTED_EDGE('',*,*,#44411,.T.);
#74090=ORIENTED_EDGE('',*,*,#44419,.T.);
#74091=ORIENTED_EDGE('',*,*,#44429,.T.);
#74092=ORIENTED_EDGE('',*,*,#44426,.T.);
#74093=ORIENTED_EDGE('',*,*,#44423,.T.);
#74094=ORIENTED_EDGE('',*,*,#44431,.T.);
#74095=ORIENTED_EDGE('',*,*,#44441,.T.);
#74096=ORIENTED_EDGE('',*,*,#44438,.T.);
#74097=ORIENTED_EDGE('',*,*,#44435,.T.);
#74098=ORIENTED_EDGE('',*,*,#44443,.T.);
#74099=ORIENTED_EDGE('',*,*,#44453,.T.);
#74100=ORIENTED_EDGE('',*,*,#44450,.T.);
#74101=ORIENTED_EDGE('',*,*,#44447,.T.);
#74102=ORIENTED_EDGE('',*,*,#44455,.T.);
#74103=ORIENTED_EDGE('',*,*,#44465,.T.);
#74104=ORIENTED_EDGE('',*,*,#44462,.T.);
#74105=ORIENTED_EDGE('',*,*,#44459,.T.);
#74106=ORIENTED_EDGE('',*,*,#44467,.T.);
#74107=ORIENTED_EDGE('',*,*,#44477,.T.);
#74108=ORIENTED_EDGE('',*,*,#44474,.T.);
#74109=ORIENTED_EDGE('',*,*,#44471,.T.);
#74110=ORIENTED_EDGE('',*,*,#44479,.T.);
#74111=ORIENTED_EDGE('',*,*,#44489,.T.);
#74112=ORIENTED_EDGE('',*,*,#44486,.T.);
#74113=ORIENTED_EDGE('',*,*,#44483,.T.);
#74114=ORIENTED_EDGE('',*,*,#44491,.T.);
#74115=ORIENTED_EDGE('',*,*,#44501,.T.);
#74116=ORIENTED_EDGE('',*,*,#44498,.T.);
#74117=ORIENTED_EDGE('',*,*,#44495,.T.);
#74118=ORIENTED_EDGE('',*,*,#44503,.T.);
#74119=ORIENTED_EDGE('',*,*,#44513,.T.);
#74120=ORIENTED_EDGE('',*,*,#44510,.T.);
#74121=ORIENTED_EDGE('',*,*,#44507,.T.);
#74122=ORIENTED_EDGE('',*,*,#44515,.T.);
#74123=ORIENTED_EDGE('',*,*,#44525,.T.);
#74124=ORIENTED_EDGE('',*,*,#44522,.T.);
#74125=ORIENTED_EDGE('',*,*,#44519,.T.);
#74126=ORIENTED_EDGE('',*,*,#44527,.T.);
#74127=ORIENTED_EDGE('',*,*,#44537,.T.);
#74128=ORIENTED_EDGE('',*,*,#44534,.T.);
#74129=ORIENTED_EDGE('',*,*,#44531,.T.);
#74130=ORIENTED_EDGE('',*,*,#44539,.T.);
#74131=ORIENTED_EDGE('',*,*,#44549,.T.);
#74132=ORIENTED_EDGE('',*,*,#44546,.T.);
#74133=ORIENTED_EDGE('',*,*,#44543,.T.);
#74134=ORIENTED_EDGE('',*,*,#44551,.T.);
#74135=ORIENTED_EDGE('',*,*,#44561,.T.);
#74136=ORIENTED_EDGE('',*,*,#44558,.T.);
#74137=ORIENTED_EDGE('',*,*,#44555,.T.);
#74138=ORIENTED_EDGE('',*,*,#44563,.T.);
#74139=ORIENTED_EDGE('',*,*,#44573,.T.);
#74140=ORIENTED_EDGE('',*,*,#44570,.T.);
#74141=ORIENTED_EDGE('',*,*,#44567,.T.);
#74142=ORIENTED_EDGE('',*,*,#44575,.T.);
#74143=ORIENTED_EDGE('',*,*,#44585,.T.);
#74144=ORIENTED_EDGE('',*,*,#44582,.T.);
#74145=ORIENTED_EDGE('',*,*,#44579,.T.);
#74146=ORIENTED_EDGE('',*,*,#44587,.T.);
#74147=ORIENTED_EDGE('',*,*,#44597,.T.);
#74148=ORIENTED_EDGE('',*,*,#44594,.T.);
#74149=ORIENTED_EDGE('',*,*,#44591,.T.);
#74150=ORIENTED_EDGE('',*,*,#44599,.T.);
#74151=ORIENTED_EDGE('',*,*,#44609,.T.);
#74152=ORIENTED_EDGE('',*,*,#44606,.T.);
#74153=ORIENTED_EDGE('',*,*,#44603,.T.);
#74154=ORIENTED_EDGE('',*,*,#44611,.T.);
#74155=ORIENTED_EDGE('',*,*,#44618,.T.);
#74156=ORIENTED_EDGE('',*,*,#44615,.T.);
#74157=ORIENTED_EDGE('',*,*,#44623,.T.);
#74158=ORIENTED_EDGE('',*,*,#44621,.T.);
#74159=ORIENTED_EDGE('',*,*,#44633,.T.);
#74160=ORIENTED_EDGE('',*,*,#44630,.T.);
#74161=ORIENTED_EDGE('',*,*,#44627,.T.);
#74162=ORIENTED_EDGE('',*,*,#44635,.T.);
#74163=ORIENTED_EDGE('',*,*,#44645,.T.);
#74164=ORIENTED_EDGE('',*,*,#44642,.T.);
#74165=ORIENTED_EDGE('',*,*,#44639,.T.);
#74166=ORIENTED_EDGE('',*,*,#44647,.T.);
#74167=ORIENTED_EDGE('',*,*,#44657,.T.);
#74168=ORIENTED_EDGE('',*,*,#44654,.T.);
#74169=ORIENTED_EDGE('',*,*,#44651,.T.);
#74170=ORIENTED_EDGE('',*,*,#44659,.T.);
#74171=ORIENTED_EDGE('',*,*,#44669,.T.);
#74172=ORIENTED_EDGE('',*,*,#44666,.T.);
#74173=ORIENTED_EDGE('',*,*,#44663,.T.);
#74174=ORIENTED_EDGE('',*,*,#44671,.T.);
#74175=ORIENTED_EDGE('',*,*,#44681,.T.);
#74176=ORIENTED_EDGE('',*,*,#44678,.T.);
#74177=ORIENTED_EDGE('',*,*,#44675,.T.);
#74178=ORIENTED_EDGE('',*,*,#44683,.T.);
#74179=ORIENTED_EDGE('',*,*,#44693,.T.);
#74180=ORIENTED_EDGE('',*,*,#44690,.T.);
#74181=ORIENTED_EDGE('',*,*,#44687,.T.);
#74182=ORIENTED_EDGE('',*,*,#44695,.T.);
#74183=ORIENTED_EDGE('',*,*,#44705,.T.);
#74184=ORIENTED_EDGE('',*,*,#44702,.T.);
#74185=ORIENTED_EDGE('',*,*,#44699,.T.);
#74186=ORIENTED_EDGE('',*,*,#44707,.T.);
#74187=ORIENTED_EDGE('',*,*,#44717,.T.);
#74188=ORIENTED_EDGE('',*,*,#44714,.T.);
#74189=ORIENTED_EDGE('',*,*,#44711,.T.);
#74190=ORIENTED_EDGE('',*,*,#44719,.T.);
#74191=ORIENTED_EDGE('',*,*,#44729,.T.);
#74192=ORIENTED_EDGE('',*,*,#44726,.T.);
#74193=ORIENTED_EDGE('',*,*,#44723,.T.);
#74194=ORIENTED_EDGE('',*,*,#44731,.T.);
#74195=ORIENTED_EDGE('',*,*,#44741,.T.);
#74196=ORIENTED_EDGE('',*,*,#44738,.T.);
#74197=ORIENTED_EDGE('',*,*,#44735,.T.);
#74198=ORIENTED_EDGE('',*,*,#44743,.T.);
#74199=ORIENTED_EDGE('',*,*,#44753,.T.);
#74200=ORIENTED_EDGE('',*,*,#44750,.T.);
#74201=ORIENTED_EDGE('',*,*,#44747,.T.);
#74202=ORIENTED_EDGE('',*,*,#44755,.T.);
#74203=ORIENTED_EDGE('',*,*,#44765,.T.);
#74204=ORIENTED_EDGE('',*,*,#44762,.T.);
#74205=ORIENTED_EDGE('',*,*,#44759,.T.);
#74206=ORIENTED_EDGE('',*,*,#44767,.T.);
#74207=ORIENTED_EDGE('',*,*,#44777,.T.);
#74208=ORIENTED_EDGE('',*,*,#44774,.T.);
#74209=ORIENTED_EDGE('',*,*,#44771,.T.);
#74210=ORIENTED_EDGE('',*,*,#44779,.T.);
#74211=ORIENTED_EDGE('',*,*,#44789,.T.);
#74212=ORIENTED_EDGE('',*,*,#44786,.T.);
#74213=ORIENTED_EDGE('',*,*,#44783,.T.);
#74214=ORIENTED_EDGE('',*,*,#44791,.T.);
#74215=ORIENTED_EDGE('',*,*,#44801,.T.);
#74216=ORIENTED_EDGE('',*,*,#44798,.T.);
#74217=ORIENTED_EDGE('',*,*,#44795,.T.);
#74218=ORIENTED_EDGE('',*,*,#44803,.T.);
#74219=ORIENTED_EDGE('',*,*,#44813,.T.);
#74220=ORIENTED_EDGE('',*,*,#44810,.T.);
#74221=ORIENTED_EDGE('',*,*,#44807,.T.);
#74222=ORIENTED_EDGE('',*,*,#44815,.T.);
#74223=ORIENTED_EDGE('',*,*,#44825,.T.);
#74224=ORIENTED_EDGE('',*,*,#44822,.T.);
#74225=ORIENTED_EDGE('',*,*,#44819,.T.);
#74226=ORIENTED_EDGE('',*,*,#44827,.T.);
#74227=ORIENTED_EDGE('',*,*,#44837,.T.);
#74228=ORIENTED_EDGE('',*,*,#44834,.T.);
#74229=ORIENTED_EDGE('',*,*,#44831,.T.);
#74230=ORIENTED_EDGE('',*,*,#44839,.T.);
#74231=ORIENTED_EDGE('',*,*,#44849,.T.);
#74232=ORIENTED_EDGE('',*,*,#44846,.T.);
#74233=ORIENTED_EDGE('',*,*,#44843,.T.);
#74234=ORIENTED_EDGE('',*,*,#44851,.T.);
#74235=ORIENTED_EDGE('',*,*,#44861,.T.);
#74236=ORIENTED_EDGE('',*,*,#44858,.T.);
#74237=ORIENTED_EDGE('',*,*,#44855,.T.);
#74238=ORIENTED_EDGE('',*,*,#44863,.T.);
#74239=ORIENTED_EDGE('',*,*,#44873,.T.);
#74240=ORIENTED_EDGE('',*,*,#44870,.T.);
#74241=ORIENTED_EDGE('',*,*,#44867,.T.);
#74242=ORIENTED_EDGE('',*,*,#44875,.T.);
#74243=ORIENTED_EDGE('',*,*,#44885,.T.);
#74244=ORIENTED_EDGE('',*,*,#44882,.T.);
#74245=ORIENTED_EDGE('',*,*,#44879,.T.);
#74246=ORIENTED_EDGE('',*,*,#44887,.T.);
#74247=ORIENTED_EDGE('',*,*,#44897,.T.);
#74248=ORIENTED_EDGE('',*,*,#44894,.T.);
#74249=ORIENTED_EDGE('',*,*,#44891,.T.);
#74250=ORIENTED_EDGE('',*,*,#44899,.T.);
#74251=ORIENTED_EDGE('',*,*,#44909,.T.);
#74252=ORIENTED_EDGE('',*,*,#44906,.T.);
#74253=ORIENTED_EDGE('',*,*,#44903,.T.);
#74254=ORIENTED_EDGE('',*,*,#44911,.T.);
#74255=ORIENTED_EDGE('',*,*,#44921,.T.);
#74256=ORIENTED_EDGE('',*,*,#44918,.T.);
#74257=ORIENTED_EDGE('',*,*,#44915,.T.);
#74258=ORIENTED_EDGE('',*,*,#44923,.T.);
#74259=ORIENTED_EDGE('',*,*,#44933,.T.);
#74260=ORIENTED_EDGE('',*,*,#44930,.T.);
#74261=ORIENTED_EDGE('',*,*,#44927,.T.);
#74262=ORIENTED_EDGE('',*,*,#44935,.T.);
#74263=ORIENTED_EDGE('',*,*,#44945,.T.);
#74264=ORIENTED_EDGE('',*,*,#44942,.T.);
#74265=ORIENTED_EDGE('',*,*,#44939,.T.);
#74266=ORIENTED_EDGE('',*,*,#44947,.T.);
#74267=ORIENTED_EDGE('',*,*,#44957,.T.);
#74268=ORIENTED_EDGE('',*,*,#44954,.T.);
#74269=ORIENTED_EDGE('',*,*,#44951,.T.);
#74270=ORIENTED_EDGE('',*,*,#44959,.T.);
#74271=ORIENTED_EDGE('',*,*,#44969,.T.);
#74272=ORIENTED_EDGE('',*,*,#44966,.T.);
#74273=ORIENTED_EDGE('',*,*,#44963,.T.);
#74274=ORIENTED_EDGE('',*,*,#44971,.T.);
#74275=ORIENTED_EDGE('',*,*,#44981,.T.);
#74276=ORIENTED_EDGE('',*,*,#44978,.T.);
#74277=ORIENTED_EDGE('',*,*,#44975,.T.);
#74278=ORIENTED_EDGE('',*,*,#44983,.T.);
#74279=ORIENTED_EDGE('',*,*,#44993,.T.);
#74280=ORIENTED_EDGE('',*,*,#44990,.T.);
#74281=ORIENTED_EDGE('',*,*,#44987,.T.);
#74282=ORIENTED_EDGE('',*,*,#44995,.T.);
#74283=ORIENTED_EDGE('',*,*,#45005,.T.);
#74284=ORIENTED_EDGE('',*,*,#45002,.T.);
#74285=ORIENTED_EDGE('',*,*,#44999,.T.);
#74286=ORIENTED_EDGE('',*,*,#45007,.T.);
#74287=ORIENTED_EDGE('',*,*,#45017,.T.);
#74288=ORIENTED_EDGE('',*,*,#45014,.T.);
#74289=ORIENTED_EDGE('',*,*,#45011,.T.);
#74290=ORIENTED_EDGE('',*,*,#45019,.T.);
#74291=ORIENTED_EDGE('',*,*,#45029,.T.);
#74292=ORIENTED_EDGE('',*,*,#45026,.T.);
#74293=ORIENTED_EDGE('',*,*,#45023,.T.);
#74294=ORIENTED_EDGE('',*,*,#45031,.T.);
#74295=ORIENTED_EDGE('',*,*,#45041,.T.);
#74296=ORIENTED_EDGE('',*,*,#45038,.T.);
#74297=ORIENTED_EDGE('',*,*,#45035,.T.);
#74298=ORIENTED_EDGE('',*,*,#45043,.T.);
#74299=ORIENTED_EDGE('',*,*,#45053,.T.);
#74300=ORIENTED_EDGE('',*,*,#45050,.T.);
#74301=ORIENTED_EDGE('',*,*,#45047,.T.);
#74302=ORIENTED_EDGE('',*,*,#45055,.T.);
#74303=ORIENTED_EDGE('',*,*,#45065,.T.);
#74304=ORIENTED_EDGE('',*,*,#45062,.T.);
#74305=ORIENTED_EDGE('',*,*,#45059,.T.);
#74306=ORIENTED_EDGE('',*,*,#45067,.T.);
#74307=ORIENTED_EDGE('',*,*,#45077,.T.);
#74308=ORIENTED_EDGE('',*,*,#45074,.T.);
#74309=ORIENTED_EDGE('',*,*,#45071,.T.);
#74310=ORIENTED_EDGE('',*,*,#45079,.T.);
#74311=ORIENTED_EDGE('',*,*,#45089,.T.);
#74312=ORIENTED_EDGE('',*,*,#45086,.T.);
#74313=ORIENTED_EDGE('',*,*,#45083,.T.);
#74314=ORIENTED_EDGE('',*,*,#45091,.T.);
#74315=ORIENTED_EDGE('',*,*,#45101,.T.);
#74316=ORIENTED_EDGE('',*,*,#45098,.T.);
#74317=ORIENTED_EDGE('',*,*,#45095,.T.);
#74318=ORIENTED_EDGE('',*,*,#45103,.T.);
#74319=ORIENTED_EDGE('',*,*,#45113,.T.);
#74320=ORIENTED_EDGE('',*,*,#45110,.T.);
#74321=ORIENTED_EDGE('',*,*,#45107,.T.);
#74322=ORIENTED_EDGE('',*,*,#45115,.T.);
#74323=ORIENTED_EDGE('',*,*,#45125,.T.);
#74324=ORIENTED_EDGE('',*,*,#45122,.T.);
#74325=ORIENTED_EDGE('',*,*,#45119,.T.);
#74326=ORIENTED_EDGE('',*,*,#45127,.T.);
#74327=ORIENTED_EDGE('',*,*,#45137,.T.);
#74328=ORIENTED_EDGE('',*,*,#45134,.T.);
#74329=ORIENTED_EDGE('',*,*,#45131,.T.);
#74330=ORIENTED_EDGE('',*,*,#45139,.T.);
#74331=ORIENTED_EDGE('',*,*,#51998,.T.);
#74332=ORIENTED_EDGE('',*,*,#51996,.T.);
#74333=ORIENTED_EDGE('',*,*,#51994,.T.);
#74334=ORIENTED_EDGE('',*,*,#51999,.T.);
#74335=ORIENTED_EDGE('',*,*,#43532,.T.);
#74336=ORIENTED_EDGE('',*,*,#52000,.F.);
#74337=ORIENTED_EDGE('',*,*,#52001,.F.);
#74338=ORIENTED_EDGE('',*,*,#52002,.T.);
#74339=ORIENTED_EDGE('',*,*,#52003,.T.);
#74340=ORIENTED_EDGE('',*,*,#52004,.T.);
#74341=ORIENTED_EDGE('',*,*,#52005,.T.);
#74342=ORIENTED_EDGE('',*,*,#52003,.F.);
#74343=ORIENTED_EDGE('',*,*,#52006,.T.);
#74344=ORIENTED_EDGE('',*,*,#52007,.T.);
#74345=ORIENTED_EDGE('',*,*,#52008,.T.);
#74346=ORIENTED_EDGE('',*,*,#52009,.T.);
#74347=ORIENTED_EDGE('',*,*,#52010,.T.);
#74348=ORIENTED_EDGE('',*,*,#52011,.T.);
#74349=ORIENTED_EDGE('',*,*,#52012,.T.);
#74350=ORIENTED_EDGE('',*,*,#52013,.F.);
#74351=ORIENTED_EDGE('',*,*,#52014,.T.);
#74352=ORIENTED_EDGE('',*,*,#52001,.T.);
#74353=ORIENTED_EDGE('',*,*,#52015,.T.);
#74354=ORIENTED_EDGE('',*,*,#52016,.F.);
#74355=ORIENTED_EDGE('',*,*,#52017,.T.);
#74356=ORIENTED_EDGE('',*,*,#52013,.T.);
#74357=ORIENTED_EDGE('',*,*,#52018,.T.);
#74358=ORIENTED_EDGE('',*,*,#52019,.F.);
#74359=ORIENTED_EDGE('',*,*,#52020,.T.);
#74360=ORIENTED_EDGE('',*,*,#52021,.T.);
#74361=ORIENTED_EDGE('',*,*,#52016,.T.);
#74362=ORIENTED_EDGE('',*,*,#52022,.T.);
#74363=ORIENTED_EDGE('',*,*,#52023,.F.);
#74364=ORIENTED_EDGE('',*,*,#52024,.T.);
#74365=ORIENTED_EDGE('',*,*,#52019,.T.);
#74366=ORIENTED_EDGE('',*,*,#52025,.T.);
#74367=ORIENTED_EDGE('',*,*,#52026,.T.);
#74368=ORIENTED_EDGE('',*,*,#52027,.F.);
#74369=ORIENTED_EDGE('',*,*,#52028,.T.);
#74370=ORIENTED_EDGE('',*,*,#52023,.T.);
#74371=ORIENTED_EDGE('',*,*,#52029,.T.);
#74372=ORIENTED_EDGE('',*,*,#52030,.F.);
#74373=ORIENTED_EDGE('',*,*,#52031,.T.);
#74374=ORIENTED_EDGE('',*,*,#52027,.T.);
#74375=ORIENTED_EDGE('',*,*,#52032,.T.);
#74376=ORIENTED_EDGE('',*,*,#52033,.F.);
#74377=ORIENTED_EDGE('',*,*,#52034,.T.);
#74378=ORIENTED_EDGE('',*,*,#52035,.T.);
#74379=ORIENTED_EDGE('',*,*,#52030,.T.);
#74380=ORIENTED_EDGE('',*,*,#52036,.T.);
#74381=ORIENTED_EDGE('',*,*,#52037,.F.);
#74382=ORIENTED_EDGE('',*,*,#52038,.T.);
#74383=ORIENTED_EDGE('',*,*,#52039,.F.);
#74384=ORIENTED_EDGE('',*,*,#52040,.F.);
#74385=ORIENTED_EDGE('',*,*,#52041,.T.);
#74386=ORIENTED_EDGE('',*,*,#52037,.T.);
#74387=ORIENTED_EDGE('',*,*,#52042,.F.);
#74388=ORIENTED_EDGE('',*,*,#52043,.T.);
#74389=ORIENTED_EDGE('',*,*,#52044,.T.);
#74390=ORIENTED_EDGE('',*,*,#52045,.T.);
#74391=ORIENTED_EDGE('',*,*,#52046,.F.);
#74392=ORIENTED_EDGE('',*,*,#52047,.T.);
#74393=ORIENTED_EDGE('',*,*,#52048,.T.);
#74394=ORIENTED_EDGE('',*,*,#52040,.T.);
#74395=ORIENTED_EDGE('',*,*,#52049,.T.);
#74396=ORIENTED_EDGE('',*,*,#52050,.F.);
#74397=ORIENTED_EDGE('',*,*,#52051,.T.);
#74398=ORIENTED_EDGE('',*,*,#52046,.T.);
#74399=ORIENTED_EDGE('',*,*,#52052,.T.);
#74400=ORIENTED_EDGE('',*,*,#52053,.T.);
#74401=ORIENTED_EDGE('',*,*,#52054,.F.);
#74402=ORIENTED_EDGE('',*,*,#52055,.T.);
#74403=ORIENTED_EDGE('',*,*,#52050,.T.);
#74404=ORIENTED_EDGE('',*,*,#52056,.T.);
#74405=ORIENTED_EDGE('',*,*,#52057,.F.);
#74406=ORIENTED_EDGE('',*,*,#52058,.T.);
#74407=ORIENTED_EDGE('',*,*,#52059,.T.);
#74408=ORIENTED_EDGE('',*,*,#52054,.T.);
#74409=ORIENTED_EDGE('',*,*,#52060,.T.);
#74410=ORIENTED_EDGE('',*,*,#52061,.F.);
#74411=ORIENTED_EDGE('',*,*,#52062,.T.);
#74412=ORIENTED_EDGE('',*,*,#52057,.T.);
#74413=ORIENTED_EDGE('',*,*,#52063,.T.);
#74414=ORIENTED_EDGE('',*,*,#52064,.T.);
#74415=ORIENTED_EDGE('',*,*,#52065,.F.);
#74416=ORIENTED_EDGE('',*,*,#52066,.T.);
#74417=ORIENTED_EDGE('',*,*,#52061,.T.);
#74418=ORIENTED_EDGE('',*,*,#52067,.T.);
#74419=ORIENTED_EDGE('',*,*,#52068,.T.);
#74420=ORIENTED_EDGE('',*,*,#52069,.T.);
#74421=ORIENTED_EDGE('',*,*,#52070,.T.);
#74422=ORIENTED_EDGE('',*,*,#52071,.T.);
#74423=ORIENTED_EDGE('',*,*,#52072,.F.);
#74424=ORIENTED_EDGE('',*,*,#52073,.T.);
#74425=ORIENTED_EDGE('',*,*,#52074,.T.);
#74426=ORIENTED_EDGE('',*,*,#52075,.T.);
#74427=ORIENTED_EDGE('',*,*,#52076,.T.);
#74428=ORIENTED_EDGE('',*,*,#52070,.F.);
#74429=ORIENTED_EDGE('',*,*,#52077,.F.);
#74430=ORIENTED_EDGE('',*,*,#52039,.T.);
#74431=ORIENTED_EDGE('',*,*,#52078,.F.);
#74432=ORIENTED_EDGE('',*,*,#52079,.F.);
#74433=ORIENTED_EDGE('',*,*,#52080,.F.);
#74434=ORIENTED_EDGE('',*,*,#52081,.T.);
#74435=ORIENTED_EDGE('',*,*,#52082,.F.);
#74436=ORIENTED_EDGE('',*,*,#52083,.F.);
#74437=ORIENTED_EDGE('',*,*,#52084,.F.);
#74438=ORIENTED_EDGE('',*,*,#52085,.F.);
#74439=ORIENTED_EDGE('',*,*,#52086,.T.);
#74440=ORIENTED_EDGE('',*,*,#52087,.T.);
#74441=ORIENTED_EDGE('',*,*,#52088,.F.);
#74442=ORIENTED_EDGE('',*,*,#52089,.F.);
#74443=ORIENTED_EDGE('',*,*,#52082,.T.);
#74444=ORIENTED_EDGE('',*,*,#52090,.F.);
#74445=ORIENTED_EDGE('',*,*,#52091,.F.);
#74446=ORIENTED_EDGE('',*,*,#52088,.T.);
#74447=ORIENTED_EDGE('',*,*,#52092,.T.);
#74448=ORIENTED_EDGE('',*,*,#52093,.F.);
#74449=ORIENTED_EDGE('',*,*,#52094,.F.);
#74450=ORIENTED_EDGE('',*,*,#52090,.T.);
#74451=ORIENTED_EDGE('',*,*,#52095,.T.);
#74452=ORIENTED_EDGE('',*,*,#52096,.F.);
#74453=ORIENTED_EDGE('',*,*,#52097,.F.);
#74454=ORIENTED_EDGE('',*,*,#52098,.F.);
#74455=ORIENTED_EDGE('',*,*,#52099,.F.);
#74456=ORIENTED_EDGE('',*,*,#52100,.T.);
#74457=ORIENTED_EDGE('',*,*,#52101,.T.);
#74458=ORIENTED_EDGE('',*,*,#52102,.F.);
#74459=ORIENTED_EDGE('',*,*,#52103,.F.);
#74460=ORIENTED_EDGE('',*,*,#52096,.T.);
#74461=ORIENTED_EDGE('',*,*,#52104,.F.);
#74462=ORIENTED_EDGE('',*,*,#52105,.F.);
#74463=ORIENTED_EDGE('',*,*,#52102,.T.);
#74464=ORIENTED_EDGE('',*,*,#52106,.T.);
#74465=ORIENTED_EDGE('',*,*,#52107,.F.);
#74466=ORIENTED_EDGE('',*,*,#52108,.F.);
#74467=ORIENTED_EDGE('',*,*,#52104,.T.);
#74468=ORIENTED_EDGE('',*,*,#52109,.T.);
#74469=ORIENTED_EDGE('',*,*,#52110,.F.);
#74470=ORIENTED_EDGE('',*,*,#52111,.F.);
#74471=ORIENTED_EDGE('',*,*,#52112,.F.);
#74472=ORIENTED_EDGE('',*,*,#52113,.F.);
#74473=ORIENTED_EDGE('',*,*,#52114,.F.);
#74474=ORIENTED_EDGE('',*,*,#52115,.T.);
#74475=ORIENTED_EDGE('',*,*,#52116,.T.);
#74476=ORIENTED_EDGE('',*,*,#52117,.F.);
#74477=ORIENTED_EDGE('',*,*,#52118,.F.);
#74478=ORIENTED_EDGE('',*,*,#52119,.T.);
#74479=ORIENTED_EDGE('',*,*,#52114,.T.);
#74480=ORIENTED_EDGE('',*,*,#52120,.F.);
#74481=ORIENTED_EDGE('',*,*,#52121,.F.);
#74482=ORIENTED_EDGE('',*,*,#52122,.T.);
#74483=ORIENTED_EDGE('',*,*,#52118,.T.);
#74484=ORIENTED_EDGE('',*,*,#52123,.F.);
#74485=ORIENTED_EDGE('',*,*,#52124,.F.);
#74486=ORIENTED_EDGE('',*,*,#52125,.T.);
#74487=ORIENTED_EDGE('',*,*,#52126,.T.);
#74488=ORIENTED_EDGE('',*,*,#52127,.T.);
#74489=ORIENTED_EDGE('',*,*,#52128,.F.);
#74490=ORIENTED_EDGE('',*,*,#52129,.F.);
#74491=ORIENTED_EDGE('',*,*,#52130,.F.);
#74492=ORIENTED_EDGE('',*,*,#52131,.T.);
#74493=ORIENTED_EDGE('',*,*,#52124,.T.);
#74494=ORIENTED_EDGE('',*,*,#52132,.F.);
#74495=ORIENTED_EDGE('',*,*,#52133,.T.);
#74496=ORIENTED_EDGE('',*,*,#52130,.T.);
#74497=ORIENTED_EDGE('',*,*,#52134,.F.);
#74498=ORIENTED_EDGE('',*,*,#52135,.F.);
#74499=ORIENTED_EDGE('',*,*,#52136,.T.);
#74500=ORIENTED_EDGE('',*,*,#52132,.T.);
#74501=ORIENTED_EDGE('',*,*,#52137,.F.);
#74502=ORIENTED_EDGE('',*,*,#52138,.F.);
#74503=ORIENTED_EDGE('',*,*,#52139,.T.);
#74504=ORIENTED_EDGE('',*,*,#52140,.T.);
#74505=ORIENTED_EDGE('',*,*,#52141,.F.);
#74506=ORIENTED_EDGE('',*,*,#52142,.F.);
#74507=ORIENTED_EDGE('',*,*,#52143,.F.);
#74508=ORIENTED_EDGE('',*,*,#52144,.T.);
#74509=ORIENTED_EDGE('',*,*,#52138,.T.);
#74510=ORIENTED_EDGE('',*,*,#52145,.T.);
#74511=ORIENTED_EDGE('',*,*,#52146,.T.);
#74512=ORIENTED_EDGE('',*,*,#52147,.F.);
#74513=ORIENTED_EDGE('',*,*,#52148,.T.);
#74514=ORIENTED_EDGE('',*,*,#52149,.T.);
#74515=ORIENTED_EDGE('',*,*,#52148,.F.);
#74516=ORIENTED_EDGE('',*,*,#52135,.T.);
#74517=ORIENTED_EDGE('',*,*,#52150,.F.);
#74518=ORIENTED_EDGE('',*,*,#52116,.F.);
#74519=ORIENTED_EDGE('',*,*,#52151,.T.);
#74520=ORIENTED_EDGE('',*,*,#52121,.T.);
#74521=ORIENTED_EDGE('',*,*,#52152,.F.);
#74522=ORIENTED_EDGE('',*,*,#52153,.F.);
#74523=ORIENTED_EDGE('',*,*,#52154,.T.);
#74524=ORIENTED_EDGE('',*,*,#52155,.T.);
#74525=ORIENTED_EDGE('',*,*,#52156,.T.);
#74526=ORIENTED_EDGE('',*,*,#52157,.T.);
#74527=ORIENTED_EDGE('',*,*,#52158,.T.);
#74528=ORIENTED_EDGE('',*,*,#52159,.F.);
#74529=ORIENTED_EDGE('',*,*,#52110,.T.);
#74530=ORIENTED_EDGE('',*,*,#52160,.F.);
#74531=ORIENTED_EDGE('',*,*,#52161,.T.);
#74532=ORIENTED_EDGE('',*,*,#52162,.T.);
#74533=ORIENTED_EDGE('',*,*,#52099,.T.);
#74534=ORIENTED_EDGE('',*,*,#52163,.F.);
#74535=ORIENTED_EDGE('',*,*,#52164,.F.);
#74536=ORIENTED_EDGE('',*,*,#52107,.T.);
#74537=ORIENTED_EDGE('',*,*,#52165,.T.);
#74538=ORIENTED_EDGE('',*,*,#52166,.T.);
#74539=ORIENTED_EDGE('',*,*,#52085,.T.);
#74540=ORIENTED_EDGE('',*,*,#52167,.F.);
#74541=ORIENTED_EDGE('',*,*,#52168,.F.);
#74542=ORIENTED_EDGE('',*,*,#52093,.T.);
#74543=ORIENTED_EDGE('',*,*,#52169,.T.);
#74544=ORIENTED_EDGE('',*,*,#52170,.T.);
#74545=ORIENTED_EDGE('',*,*,#52171,.T.);
#74546=ORIENTED_EDGE('',*,*,#52172,.F.);
#74547=ORIENTED_EDGE('',*,*,#52173,.F.);
#74548=ORIENTED_EDGE('',*,*,#52174,.T.);
#74549=ORIENTED_EDGE('',*,*,#52175,.T.);
#74550=ORIENTED_EDGE('',*,*,#52176,.F.);
#74551=ORIENTED_EDGE('',*,*,#52171,.F.);
#74552=ORIENTED_EDGE('',*,*,#52100,.F.);
#74553=ORIENTED_EDGE('',*,*,#52177,.F.);
#74554=ORIENTED_EDGE('',*,*,#52178,.F.);
#74555=ORIENTED_EDGE('',*,*,#52036,.F.);
#74556=ORIENTED_EDGE('',*,*,#52032,.F.);
#74557=ORIENTED_EDGE('',*,*,#52029,.F.);
#74558=ORIENTED_EDGE('',*,*,#52026,.F.);
#74559=ORIENTED_EDGE('',*,*,#52179,.T.);
#74560=ORIENTED_EDGE('',*,*,#52166,.F.);
#74561=ORIENTED_EDGE('',*,*,#52165,.F.);
#74562=ORIENTED_EDGE('',*,*,#52109,.F.);
#74563=ORIENTED_EDGE('',*,*,#52106,.F.);
#74564=ORIENTED_EDGE('',*,*,#52101,.F.);
#74565=ORIENTED_EDGE('',*,*,#52086,.F.);
#74566=ORIENTED_EDGE('',*,*,#52179,.F.);
#74567=ORIENTED_EDGE('',*,*,#52025,.F.);
#74568=ORIENTED_EDGE('',*,*,#52022,.F.);
#74569=ORIENTED_EDGE('',*,*,#52018,.F.);
#74570=ORIENTED_EDGE('',*,*,#52015,.F.);
#74571=ORIENTED_EDGE('',*,*,#52012,.F.);
#74572=ORIENTED_EDGE('',*,*,#52180,.T.);
#74573=ORIENTED_EDGE('',*,*,#52170,.F.);
#74574=ORIENTED_EDGE('',*,*,#52169,.F.);
#74575=ORIENTED_EDGE('',*,*,#52095,.F.);
#74576=ORIENTED_EDGE('',*,*,#52092,.F.);
#74577=ORIENTED_EDGE('',*,*,#52087,.F.);
#74578=ORIENTED_EDGE('',*,*,#52181,.T.);
#74579=ORIENTED_EDGE('',*,*,#52174,.F.);
#74580=ORIENTED_EDGE('',*,*,#52180,.F.);
#74581=ORIENTED_EDGE('',*,*,#52011,.F.);
#74582=ORIENTED_EDGE('',*,*,#52010,.F.);
#74583=ORIENTED_EDGE('',*,*,#52009,.F.);
#74584=ORIENTED_EDGE('',*,*,#52182,.F.);
#74585=ORIENTED_EDGE('',*,*,#52175,.F.);
#74586=ORIENTED_EDGE('',*,*,#52181,.F.);
#74587=ORIENTED_EDGE('',*,*,#52007,.F.);
#74588=ORIENTED_EDGE('',*,*,#52183,.F.);
#74589=ORIENTED_EDGE('',*,*,#52176,.T.);
#74590=ORIENTED_EDGE('',*,*,#52182,.T.);
#74591=ORIENTED_EDGE('',*,*,#52008,.F.);
#74592=ORIENTED_EDGE('',*,*,#52021,.F.);
#74593=ORIENTED_EDGE('',*,*,#52184,.F.);
#74594=ORIENTED_EDGE('',*,*,#52084,.T.);
#74595=ORIENTED_EDGE('',*,*,#52083,.T.);
#74596=ORIENTED_EDGE('',*,*,#52089,.T.);
#74597=ORIENTED_EDGE('',*,*,#52091,.T.);
#74598=ORIENTED_EDGE('',*,*,#52094,.T.);
#74599=ORIENTED_EDGE('',*,*,#52173,.T.);
#74600=ORIENTED_EDGE('',*,*,#52172,.T.);
#74601=ORIENTED_EDGE('',*,*,#52183,.T.);
#74602=ORIENTED_EDGE('',*,*,#52006,.F.);
#74603=ORIENTED_EDGE('',*,*,#52002,.F.);
#74604=ORIENTED_EDGE('',*,*,#52014,.F.);
#74605=ORIENTED_EDGE('',*,*,#52017,.F.);
#74606=ORIENTED_EDGE('',*,*,#52035,.F.);
#74607=ORIENTED_EDGE('',*,*,#52185,.F.);
#74608=ORIENTED_EDGE('',*,*,#52098,.T.);
#74609=ORIENTED_EDGE('',*,*,#52097,.T.);
#74610=ORIENTED_EDGE('',*,*,#52103,.T.);
#74611=ORIENTED_EDGE('',*,*,#52105,.T.);
#74612=ORIENTED_EDGE('',*,*,#52108,.T.);
#74613=ORIENTED_EDGE('',*,*,#52168,.T.);
#74614=ORIENTED_EDGE('',*,*,#52167,.T.);
#74615=ORIENTED_EDGE('',*,*,#52184,.T.);
#74616=ORIENTED_EDGE('',*,*,#52020,.F.);
#74617=ORIENTED_EDGE('',*,*,#52024,.F.);
#74618=ORIENTED_EDGE('',*,*,#52028,.F.);
#74619=ORIENTED_EDGE('',*,*,#52031,.F.);
#74620=ORIENTED_EDGE('',*,*,#52177,.T.);
#74621=ORIENTED_EDGE('',*,*,#52162,.F.);
#74622=ORIENTED_EDGE('',*,*,#52161,.F.);
#74623=ORIENTED_EDGE('',*,*,#52186,.F.);
#74624=ORIENTED_EDGE('',*,*,#52142,.T.);
#74625=ORIENTED_EDGE('',*,*,#52141,.T.);
#74626=ORIENTED_EDGE('',*,*,#52140,.F.);
#74627=ORIENTED_EDGE('',*,*,#52187,.F.);
#74628=ORIENTED_EDGE('',*,*,#52188,.F.);
#74629=ORIENTED_EDGE('',*,*,#52189,.F.);
#74630=ORIENTED_EDGE('',*,*,#52190,.F.);
#74631=ORIENTED_EDGE('',*,*,#52159,.T.);
#74632=ORIENTED_EDGE('',*,*,#52191,.F.);
#74633=ORIENTED_EDGE('',*,*,#52068,.F.);
#74634=ORIENTED_EDGE('',*,*,#52069,.F.);
#74635=ORIENTED_EDGE('',*,*,#52192,.T.);
#74636=ORIENTED_EDGE('',*,*,#52157,.F.);
#74637=ORIENTED_EDGE('',*,*,#52193,.T.);
#74638=ORIENTED_EDGE('',*,*,#52194,.F.);
#74639=ORIENTED_EDGE('',*,*,#52191,.T.);
#74640=ORIENTED_EDGE('',*,*,#52158,.F.);
#74641=ORIENTED_EDGE('',*,*,#52192,.F.);
#74642=ORIENTED_EDGE('',*,*,#52077,.T.);
#74643=ORIENTED_EDGE('',*,*,#52195,.T.);
#74644=ORIENTED_EDGE('',*,*,#52042,.T.);
#74645=ORIENTED_EDGE('',*,*,#52196,.T.);
#74646=ORIENTED_EDGE('',*,*,#52197,.T.);
#74647=ORIENTED_EDGE('',*,*,#52198,.F.);
#74648=ORIENTED_EDGE('',*,*,#52127,.F.);
#74649=ORIENTED_EDGE('',*,*,#52199,.F.);
#74650=ORIENTED_EDGE('',*,*,#52200,.F.);
#74651=ORIENTED_EDGE('',*,*,#52201,.T.);
#74652=ORIENTED_EDGE('',*,*,#52202,.T.);
#74653=ORIENTED_EDGE('',*,*,#52153,.T.);
#74654=ORIENTED_EDGE('',*,*,#52203,.T.);
#74655=ORIENTED_EDGE('',*,*,#52126,.F.);
#74656=ORIENTED_EDGE('',*,*,#52125,.F.);
#74657=ORIENTED_EDGE('',*,*,#52131,.F.);
#74658=ORIENTED_EDGE('',*,*,#52133,.F.);
#74659=ORIENTED_EDGE('',*,*,#52136,.F.);
#74660=ORIENTED_EDGE('',*,*,#52151,.F.);
#74661=ORIENTED_EDGE('',*,*,#52204,.F.);
#74662=ORIENTED_EDGE('',*,*,#52058,.F.);
#74663=ORIENTED_EDGE('',*,*,#52062,.F.);
#74664=ORIENTED_EDGE('',*,*,#52066,.F.);
#74665=ORIENTED_EDGE('',*,*,#52205,.F.);
#74666=ORIENTED_EDGE('',*,*,#52073,.F.);
#74667=ORIENTED_EDGE('',*,*,#52206,.T.);
#74668=ORIENTED_EDGE('',*,*,#52196,.F.);
#74669=ORIENTED_EDGE('',*,*,#52203,.F.);
#74670=ORIENTED_EDGE('',*,*,#52207,.F.);
#74671=ORIENTED_EDGE('',*,*,#52072,.T.);
#74672=ORIENTED_EDGE('',*,*,#52208,.F.);
#74673=ORIENTED_EDGE('',*,*,#52197,.F.);
#74674=ORIENTED_EDGE('',*,*,#52206,.F.);
#74675=ORIENTED_EDGE('',*,*,#52209,.F.);
#74676=ORIENTED_EDGE('',*,*,#52198,.T.);
#74677=ORIENTED_EDGE('',*,*,#52208,.T.);
#74678=ORIENTED_EDGE('',*,*,#52071,.F.);
#74679=ORIENTED_EDGE('',*,*,#52076,.F.);
#74680=ORIENTED_EDGE('',*,*,#52128,.T.);
#74681=ORIENTED_EDGE('',*,*,#52209,.T.);
#74682=ORIENTED_EDGE('',*,*,#52075,.F.);
#74683=ORIENTED_EDGE('',*,*,#52210,.F.);
#74684=ORIENTED_EDGE('',*,*,#52067,.F.);
#74685=ORIENTED_EDGE('',*,*,#52064,.F.);
#74686=ORIENTED_EDGE('',*,*,#52211,.F.);
#74687=ORIENTED_EDGE('',*,*,#52150,.T.);
#74688=ORIENTED_EDGE('',*,*,#52137,.T.);
#74689=ORIENTED_EDGE('',*,*,#52134,.T.);
#74690=ORIENTED_EDGE('',*,*,#52129,.T.);
#74691=ORIENTED_EDGE('',*,*,#52053,.F.);
#74692=ORIENTED_EDGE('',*,*,#52212,.F.);
#74693=ORIENTED_EDGE('',*,*,#52152,.T.);
#74694=ORIENTED_EDGE('',*,*,#52123,.T.);
#74695=ORIENTED_EDGE('',*,*,#52120,.T.);
#74696=ORIENTED_EDGE('',*,*,#52117,.T.);
#74697=ORIENTED_EDGE('',*,*,#52211,.T.);
#74698=ORIENTED_EDGE('',*,*,#52063,.F.);
#74699=ORIENTED_EDGE('',*,*,#52060,.F.);
#74700=ORIENTED_EDGE('',*,*,#52056,.F.);
#74701=ORIENTED_EDGE('',*,*,#52044,.F.);
#74702=ORIENTED_EDGE('',*,*,#52043,.F.);
#74703=ORIENTED_EDGE('',*,*,#52195,.F.);
#74704=ORIENTED_EDGE('',*,*,#52081,.F.);
#74705=ORIENTED_EDGE('',*,*,#52213,.F.);
#74706=ORIENTED_EDGE('',*,*,#52214,.T.);
#74707=ORIENTED_EDGE('',*,*,#52199,.T.);
#74708=ORIENTED_EDGE('',*,*,#52212,.T.);
#74709=ORIENTED_EDGE('',*,*,#52052,.F.);
#74710=ORIENTED_EDGE('',*,*,#52049,.F.);
#74711=ORIENTED_EDGE('',*,*,#52045,.F.);
#74712=ORIENTED_EDGE('',*,*,#52074,.F.);
#74713=ORIENTED_EDGE('',*,*,#52207,.T.);
#74714=ORIENTED_EDGE('',*,*,#52205,.T.);
#74715=ORIENTED_EDGE('',*,*,#52065,.T.);
#74716=ORIENTED_EDGE('',*,*,#52210,.T.);
#74717=ORIENTED_EDGE('',*,*,#52059,.F.);
#74718=ORIENTED_EDGE('',*,*,#52204,.T.);
#74719=ORIENTED_EDGE('',*,*,#52115,.F.);
#74720=ORIENTED_EDGE('',*,*,#52119,.F.);
#74721=ORIENTED_EDGE('',*,*,#52122,.F.);
#74722=ORIENTED_EDGE('',*,*,#52154,.F.);
#74723=ORIENTED_EDGE('',*,*,#52215,.F.);
#74724=ORIENTED_EDGE('',*,*,#52047,.F.);
#74725=ORIENTED_EDGE('',*,*,#52051,.F.);
#74726=ORIENTED_EDGE('',*,*,#52055,.F.);
#74727=ORIENTED_EDGE('',*,*,#52202,.F.);
#74728=ORIENTED_EDGE('',*,*,#52216,.F.);
#74729=ORIENTED_EDGE('',*,*,#52217,.T.);
#74730=ORIENTED_EDGE('',*,*,#52079,.T.);
#74731=ORIENTED_EDGE('',*,*,#52078,.T.);
#74732=ORIENTED_EDGE('',*,*,#52038,.F.);
#74733=ORIENTED_EDGE('',*,*,#52041,.F.);
#74734=ORIENTED_EDGE('',*,*,#52048,.F.);
#74735=ORIENTED_EDGE('',*,*,#52215,.T.);
#74736=ORIENTED_EDGE('',*,*,#52218,.F.);
#74737=ORIENTED_EDGE('',*,*,#52219,.T.);
#74738=ORIENTED_EDGE('',*,*,#52220,.T.);
#74739=ORIENTED_EDGE('',*,*,#52219,.F.);
#74740=ORIENTED_EDGE('',*,*,#52221,.F.);
#74741=ORIENTED_EDGE('',*,*,#52218,.T.);
#74742=ORIENTED_EDGE('',*,*,#52222,.T.);
#74743=ORIENTED_EDGE('',*,*,#52223,.F.);
#74744=ORIENTED_EDGE('',*,*,#52222,.F.);
#74745=ORIENTED_EDGE('',*,*,#52221,.T.);
#74746=ORIENTED_EDGE('',*,*,#52214,.F.);
#74747=ORIENTED_EDGE('',*,*,#52213,.T.);
#74748=ORIENTED_EDGE('',*,*,#52080,.T.);
#74749=ORIENTED_EDGE('',*,*,#52217,.F.);
#74750=ORIENTED_EDGE('',*,*,#52216,.T.);
#74751=ORIENTED_EDGE('',*,*,#52201,.F.);
#74752=ORIENTED_EDGE('',*,*,#52200,.T.);
#74753=ORIENTED_EDGE('',*,*,#52223,.T.);
#74754=ORIENTED_EDGE('',*,*,#52220,.F.);
#74755=ORIENTED_EDGE('',*,*,#52149,.F.);
#74756=ORIENTED_EDGE('',*,*,#52224,.T.);
#74757=ORIENTED_EDGE('',*,*,#52147,.T.);
#74758=ORIENTED_EDGE('',*,*,#52224,.F.);
#74759=ORIENTED_EDGE('',*,*,#52225,.T.);
#74760=ORIENTED_EDGE('',*,*,#52226,.F.);
#74761=ORIENTED_EDGE('',*,*,#52225,.F.);
#74762=ORIENTED_EDGE('',*,*,#52226,.T.);
#74763=ORIENTED_EDGE('',*,*,#52227,.T.);
#74764=ORIENTED_EDGE('',*,*,#52228,.F.);
#74765=ORIENTED_EDGE('',*,*,#52227,.F.);
#74766=ORIENTED_EDGE('',*,*,#52160,.T.);
#74767=ORIENTED_EDGE('',*,*,#52113,.T.);
#74768=ORIENTED_EDGE('',*,*,#52229,.T.);
#74769=ORIENTED_EDGE('',*,*,#52143,.T.);
#74770=ORIENTED_EDGE('',*,*,#52186,.T.);
#74771=ORIENTED_EDGE('',*,*,#52228,.T.);
#74772=ORIENTED_EDGE('',*,*,#52033,.T.);
#74773=ORIENTED_EDGE('',*,*,#52178,.T.);
#74774=ORIENTED_EDGE('',*,*,#52187,.T.);
#74775=ORIENTED_EDGE('',*,*,#52139,.F.);
#74776=ORIENTED_EDGE('',*,*,#52146,.F.);
#74777=ORIENTED_EDGE('',*,*,#52230,.T.);
#74778=ORIENTED_EDGE('',*,*,#52231,.T.);
#74779=ORIENTED_EDGE('',*,*,#52232,.T.);
#74780=ORIENTED_EDGE('',*,*,#52230,.F.);
#74781=ORIENTED_EDGE('',*,*,#52145,.F.);
#74782=ORIENTED_EDGE('',*,*,#52144,.F.);
#74783=ORIENTED_EDGE('',*,*,#52229,.F.);
#74784=ORIENTED_EDGE('',*,*,#52112,.T.);
#74785=ORIENTED_EDGE('',*,*,#52111,.T.);
#74786=ORIENTED_EDGE('',*,*,#52164,.T.);
#74787=ORIENTED_EDGE('',*,*,#52163,.T.);
#74788=ORIENTED_EDGE('',*,*,#52185,.T.);
#74789=ORIENTED_EDGE('',*,*,#52034,.F.);
#74790=ORIENTED_EDGE('',*,*,#52232,.F.);
#74791=ORIENTED_EDGE('',*,*,#52231,.F.);
#74792=ORIENTED_EDGE('',*,*,#52233,.F.);
#74793=ORIENTED_EDGE('',*,*,#52234,.T.);
#74794=ORIENTED_EDGE('',*,*,#52155,.F.);
#74795=ORIENTED_EDGE('',*,*,#52190,.T.);
#74796=ORIENTED_EDGE('',*,*,#52235,.T.);
#74797=ORIENTED_EDGE('',*,*,#52004,.F.);
#74798=ORIENTED_EDGE('',*,*,#52005,.F.);
#74799=ORIENTED_EDGE('',*,*,#52235,.F.);
#74800=ORIENTED_EDGE('',*,*,#52189,.T.);
#74801=ORIENTED_EDGE('',*,*,#52156,.F.);
#74802=ORIENTED_EDGE('',*,*,#52234,.F.);
#74803=ORIENTED_EDGE('',*,*,#52236,.T.);
#74804=ORIENTED_EDGE('',*,*,#52193,.F.);
#74805=ORIENTED_EDGE('',*,*,#52236,.F.);
#74806=ORIENTED_EDGE('',*,*,#52233,.T.);
#74807=ORIENTED_EDGE('',*,*,#52188,.T.);
#74808=ORIENTED_EDGE('',*,*,#52194,.T.);
#74809=ORIENTED_EDGE('',*,*,#52237,.F.);
#74810=ORIENTED_EDGE('',*,*,#52238,.T.);
#74811=ORIENTED_EDGE('',*,*,#52239,.T.);
#74812=ORIENTED_EDGE('',*,*,#52240,.T.);
#74813=ORIENTED_EDGE('',*,*,#52241,.T.);
#74814=ORIENTED_EDGE('',*,*,#52239,.F.);
#74815=ORIENTED_EDGE('',*,*,#52242,.T.);
#74816=ORIENTED_EDGE('',*,*,#52243,.T.);
#74817=ORIENTED_EDGE('',*,*,#52244,.T.);
#74818=ORIENTED_EDGE('',*,*,#52245,.T.);
#74819=ORIENTED_EDGE('',*,*,#52246,.T.);
#74820=ORIENTED_EDGE('',*,*,#52247,.T.);
#74821=ORIENTED_EDGE('',*,*,#52248,.T.);
#74822=ORIENTED_EDGE('',*,*,#52249,.F.);
#74823=ORIENTED_EDGE('',*,*,#52250,.T.);
#74824=ORIENTED_EDGE('',*,*,#52237,.T.);
#74825=ORIENTED_EDGE('',*,*,#52251,.T.);
#74826=ORIENTED_EDGE('',*,*,#52252,.F.);
#74827=ORIENTED_EDGE('',*,*,#52253,.T.);
#74828=ORIENTED_EDGE('',*,*,#52249,.T.);
#74829=ORIENTED_EDGE('',*,*,#52254,.T.);
#74830=ORIENTED_EDGE('',*,*,#52255,.F.);
#74831=ORIENTED_EDGE('',*,*,#52256,.T.);
#74832=ORIENTED_EDGE('',*,*,#52257,.T.);
#74833=ORIENTED_EDGE('',*,*,#52252,.T.);
#74834=ORIENTED_EDGE('',*,*,#52258,.T.);
#74835=ORIENTED_EDGE('',*,*,#52259,.F.);
#74836=ORIENTED_EDGE('',*,*,#52260,.T.);
#74837=ORIENTED_EDGE('',*,*,#52255,.T.);
#74838=ORIENTED_EDGE('',*,*,#52261,.T.);
#74839=ORIENTED_EDGE('',*,*,#52262,.T.);
#74840=ORIENTED_EDGE('',*,*,#52263,.F.);
#74841=ORIENTED_EDGE('',*,*,#52264,.T.);
#74842=ORIENTED_EDGE('',*,*,#52259,.T.);
#74843=ORIENTED_EDGE('',*,*,#52265,.T.);
#74844=ORIENTED_EDGE('',*,*,#52266,.F.);
#74845=ORIENTED_EDGE('',*,*,#52267,.T.);
#74846=ORIENTED_EDGE('',*,*,#52263,.T.);
#74847=ORIENTED_EDGE('',*,*,#52268,.T.);
#74848=ORIENTED_EDGE('',*,*,#52269,.F.);
#74849=ORIENTED_EDGE('',*,*,#52270,.T.);
#74850=ORIENTED_EDGE('',*,*,#52271,.T.);
#74851=ORIENTED_EDGE('',*,*,#52266,.T.);
#74852=ORIENTED_EDGE('',*,*,#52272,.T.);
#74853=ORIENTED_EDGE('',*,*,#52273,.F.);
#74854=ORIENTED_EDGE('',*,*,#52274,.T.);
#74855=ORIENTED_EDGE('',*,*,#52275,.F.);
#74856=ORIENTED_EDGE('',*,*,#52276,.F.);
#74857=ORIENTED_EDGE('',*,*,#52277,.T.);
#74858=ORIENTED_EDGE('',*,*,#52273,.T.);
#74859=ORIENTED_EDGE('',*,*,#52278,.F.);
#74860=ORIENTED_EDGE('',*,*,#52279,.T.);
#74861=ORIENTED_EDGE('',*,*,#52280,.T.);
#74862=ORIENTED_EDGE('',*,*,#52281,.T.);
#74863=ORIENTED_EDGE('',*,*,#52282,.F.);
#74864=ORIENTED_EDGE('',*,*,#52283,.T.);
#74865=ORIENTED_EDGE('',*,*,#52284,.T.);
#74866=ORIENTED_EDGE('',*,*,#52276,.T.);
#74867=ORIENTED_EDGE('',*,*,#52285,.T.);
#74868=ORIENTED_EDGE('',*,*,#52286,.F.);
#74869=ORIENTED_EDGE('',*,*,#52287,.T.);
#74870=ORIENTED_EDGE('',*,*,#52282,.T.);
#74871=ORIENTED_EDGE('',*,*,#52288,.T.);
#74872=ORIENTED_EDGE('',*,*,#52289,.T.);
#74873=ORIENTED_EDGE('',*,*,#52290,.F.);
#74874=ORIENTED_EDGE('',*,*,#52291,.T.);
#74875=ORIENTED_EDGE('',*,*,#52286,.T.);
#74876=ORIENTED_EDGE('',*,*,#52292,.T.);
#74877=ORIENTED_EDGE('',*,*,#52293,.F.);
#74878=ORIENTED_EDGE('',*,*,#52294,.T.);
#74879=ORIENTED_EDGE('',*,*,#52295,.T.);
#74880=ORIENTED_EDGE('',*,*,#52290,.T.);
#74881=ORIENTED_EDGE('',*,*,#52296,.T.);
#74882=ORIENTED_EDGE('',*,*,#52297,.F.);
#74883=ORIENTED_EDGE('',*,*,#52298,.T.);
#74884=ORIENTED_EDGE('',*,*,#52293,.T.);
#74885=ORIENTED_EDGE('',*,*,#52299,.T.);
#74886=ORIENTED_EDGE('',*,*,#52300,.T.);
#74887=ORIENTED_EDGE('',*,*,#52301,.F.);
#74888=ORIENTED_EDGE('',*,*,#52302,.T.);
#74889=ORIENTED_EDGE('',*,*,#52297,.T.);
#74890=ORIENTED_EDGE('',*,*,#52303,.T.);
#74891=ORIENTED_EDGE('',*,*,#52304,.T.);
#74892=ORIENTED_EDGE('',*,*,#52305,.T.);
#74893=ORIENTED_EDGE('',*,*,#52306,.T.);
#74894=ORIENTED_EDGE('',*,*,#52307,.T.);
#74895=ORIENTED_EDGE('',*,*,#52308,.F.);
#74896=ORIENTED_EDGE('',*,*,#52309,.T.);
#74897=ORIENTED_EDGE('',*,*,#52310,.T.);
#74898=ORIENTED_EDGE('',*,*,#52311,.T.);
#74899=ORIENTED_EDGE('',*,*,#52312,.T.);
#74900=ORIENTED_EDGE('',*,*,#52306,.F.);
#74901=ORIENTED_EDGE('',*,*,#52313,.F.);
#74902=ORIENTED_EDGE('',*,*,#52275,.T.);
#74903=ORIENTED_EDGE('',*,*,#52314,.F.);
#74904=ORIENTED_EDGE('',*,*,#52315,.F.);
#74905=ORIENTED_EDGE('',*,*,#52316,.F.);
#74906=ORIENTED_EDGE('',*,*,#52317,.T.);
#74907=ORIENTED_EDGE('',*,*,#52318,.F.);
#74908=ORIENTED_EDGE('',*,*,#52319,.F.);
#74909=ORIENTED_EDGE('',*,*,#52320,.F.);
#74910=ORIENTED_EDGE('',*,*,#52321,.F.);
#74911=ORIENTED_EDGE('',*,*,#52322,.T.);
#74912=ORIENTED_EDGE('',*,*,#52323,.T.);
#74913=ORIENTED_EDGE('',*,*,#52324,.F.);
#74914=ORIENTED_EDGE('',*,*,#52325,.F.);
#74915=ORIENTED_EDGE('',*,*,#52318,.T.);
#74916=ORIENTED_EDGE('',*,*,#52326,.F.);
#74917=ORIENTED_EDGE('',*,*,#52327,.F.);
#74918=ORIENTED_EDGE('',*,*,#52324,.T.);
#74919=ORIENTED_EDGE('',*,*,#52328,.T.);
#74920=ORIENTED_EDGE('',*,*,#52329,.F.);
#74921=ORIENTED_EDGE('',*,*,#52330,.F.);
#74922=ORIENTED_EDGE('',*,*,#52326,.T.);
#74923=ORIENTED_EDGE('',*,*,#52331,.T.);
#74924=ORIENTED_EDGE('',*,*,#52332,.F.);
#74925=ORIENTED_EDGE('',*,*,#52333,.F.);
#74926=ORIENTED_EDGE('',*,*,#52334,.F.);
#74927=ORIENTED_EDGE('',*,*,#52335,.F.);
#74928=ORIENTED_EDGE('',*,*,#52336,.T.);
#74929=ORIENTED_EDGE('',*,*,#52337,.T.);
#74930=ORIENTED_EDGE('',*,*,#52338,.F.);
#74931=ORIENTED_EDGE('',*,*,#52339,.F.);
#74932=ORIENTED_EDGE('',*,*,#52332,.T.);
#74933=ORIENTED_EDGE('',*,*,#52340,.F.);
#74934=ORIENTED_EDGE('',*,*,#52341,.F.);
#74935=ORIENTED_EDGE('',*,*,#52338,.T.);
#74936=ORIENTED_EDGE('',*,*,#52342,.T.);
#74937=ORIENTED_EDGE('',*,*,#52343,.F.);
#74938=ORIENTED_EDGE('',*,*,#52344,.F.);
#74939=ORIENTED_EDGE('',*,*,#52340,.T.);
#74940=ORIENTED_EDGE('',*,*,#52345,.T.);
#74941=ORIENTED_EDGE('',*,*,#52346,.F.);
#74942=ORIENTED_EDGE('',*,*,#52347,.F.);
#74943=ORIENTED_EDGE('',*,*,#52348,.F.);
#74944=ORIENTED_EDGE('',*,*,#52349,.F.);
#74945=ORIENTED_EDGE('',*,*,#52350,.F.);
#74946=ORIENTED_EDGE('',*,*,#52351,.T.);
#74947=ORIENTED_EDGE('',*,*,#52352,.T.);
#74948=ORIENTED_EDGE('',*,*,#52353,.F.);
#74949=ORIENTED_EDGE('',*,*,#52354,.F.);
#74950=ORIENTED_EDGE('',*,*,#52355,.T.);
#74951=ORIENTED_EDGE('',*,*,#52350,.T.);
#74952=ORIENTED_EDGE('',*,*,#52356,.F.);
#74953=ORIENTED_EDGE('',*,*,#52357,.F.);
#74954=ORIENTED_EDGE('',*,*,#52358,.T.);
#74955=ORIENTED_EDGE('',*,*,#52354,.T.);
#74956=ORIENTED_EDGE('',*,*,#52359,.F.);
#74957=ORIENTED_EDGE('',*,*,#52360,.F.);
#74958=ORIENTED_EDGE('',*,*,#52361,.T.);
#74959=ORIENTED_EDGE('',*,*,#52362,.T.);
#74960=ORIENTED_EDGE('',*,*,#52363,.T.);
#74961=ORIENTED_EDGE('',*,*,#52364,.F.);
#74962=ORIENTED_EDGE('',*,*,#52365,.F.);
#74963=ORIENTED_EDGE('',*,*,#52366,.F.);
#74964=ORIENTED_EDGE('',*,*,#52367,.T.);
#74965=ORIENTED_EDGE('',*,*,#52360,.T.);
#74966=ORIENTED_EDGE('',*,*,#52368,.F.);
#74967=ORIENTED_EDGE('',*,*,#52369,.T.);
#74968=ORIENTED_EDGE('',*,*,#52366,.T.);
#74969=ORIENTED_EDGE('',*,*,#52370,.F.);
#74970=ORIENTED_EDGE('',*,*,#52371,.F.);
#74971=ORIENTED_EDGE('',*,*,#52372,.T.);
#74972=ORIENTED_EDGE('',*,*,#52368,.T.);
#74973=ORIENTED_EDGE('',*,*,#52373,.F.);
#74974=ORIENTED_EDGE('',*,*,#52374,.F.);
#74975=ORIENTED_EDGE('',*,*,#52375,.T.);
#74976=ORIENTED_EDGE('',*,*,#52376,.T.);
#74977=ORIENTED_EDGE('',*,*,#52377,.F.);
#74978=ORIENTED_EDGE('',*,*,#52378,.F.);
#74979=ORIENTED_EDGE('',*,*,#52379,.F.);
#74980=ORIENTED_EDGE('',*,*,#52380,.T.);
#74981=ORIENTED_EDGE('',*,*,#52374,.T.);
#74982=ORIENTED_EDGE('',*,*,#52381,.T.);
#74983=ORIENTED_EDGE('',*,*,#52382,.T.);
#74984=ORIENTED_EDGE('',*,*,#52383,.F.);
#74985=ORIENTED_EDGE('',*,*,#52384,.T.);
#74986=ORIENTED_EDGE('',*,*,#52385,.T.);
#74987=ORIENTED_EDGE('',*,*,#52384,.F.);
#74988=ORIENTED_EDGE('',*,*,#52371,.T.);
#74989=ORIENTED_EDGE('',*,*,#52386,.F.);
#74990=ORIENTED_EDGE('',*,*,#52352,.F.);
#74991=ORIENTED_EDGE('',*,*,#52387,.T.);
#74992=ORIENTED_EDGE('',*,*,#52357,.T.);
#74993=ORIENTED_EDGE('',*,*,#52388,.F.);
#74994=ORIENTED_EDGE('',*,*,#52389,.F.);
#74995=ORIENTED_EDGE('',*,*,#52390,.T.);
#74996=ORIENTED_EDGE('',*,*,#52391,.T.);
#74997=ORIENTED_EDGE('',*,*,#52392,.T.);
#74998=ORIENTED_EDGE('',*,*,#52393,.T.);
#74999=ORIENTED_EDGE('',*,*,#52394,.T.);
#75000=ORIENTED_EDGE('',*,*,#52395,.F.);
#75001=ORIENTED_EDGE('',*,*,#52346,.T.);
#75002=ORIENTED_EDGE('',*,*,#52396,.F.);
#75003=ORIENTED_EDGE('',*,*,#52397,.T.);
#75004=ORIENTED_EDGE('',*,*,#52398,.T.);
#75005=ORIENTED_EDGE('',*,*,#52335,.T.);
#75006=ORIENTED_EDGE('',*,*,#52399,.F.);
#75007=ORIENTED_EDGE('',*,*,#52400,.F.);
#75008=ORIENTED_EDGE('',*,*,#52343,.T.);
#75009=ORIENTED_EDGE('',*,*,#52401,.T.);
#75010=ORIENTED_EDGE('',*,*,#52402,.T.);
#75011=ORIENTED_EDGE('',*,*,#52321,.T.);
#75012=ORIENTED_EDGE('',*,*,#52403,.F.);
#75013=ORIENTED_EDGE('',*,*,#52404,.F.);
#75014=ORIENTED_EDGE('',*,*,#52329,.T.);
#75015=ORIENTED_EDGE('',*,*,#52405,.T.);
#75016=ORIENTED_EDGE('',*,*,#52406,.T.);
#75017=ORIENTED_EDGE('',*,*,#52407,.T.);
#75018=ORIENTED_EDGE('',*,*,#52408,.F.);
#75019=ORIENTED_EDGE('',*,*,#52409,.F.);
#75020=ORIENTED_EDGE('',*,*,#52410,.T.);
#75021=ORIENTED_EDGE('',*,*,#52411,.T.);
#75022=ORIENTED_EDGE('',*,*,#52412,.F.);
#75023=ORIENTED_EDGE('',*,*,#52407,.F.);
#75024=ORIENTED_EDGE('',*,*,#52336,.F.);
#75025=ORIENTED_EDGE('',*,*,#52413,.F.);
#75026=ORIENTED_EDGE('',*,*,#52414,.F.);
#75027=ORIENTED_EDGE('',*,*,#52272,.F.);
#75028=ORIENTED_EDGE('',*,*,#52268,.F.);
#75029=ORIENTED_EDGE('',*,*,#52265,.F.);
#75030=ORIENTED_EDGE('',*,*,#52262,.F.);
#75031=ORIENTED_EDGE('',*,*,#52415,.T.);
#75032=ORIENTED_EDGE('',*,*,#52402,.F.);
#75033=ORIENTED_EDGE('',*,*,#52401,.F.);
#75034=ORIENTED_EDGE('',*,*,#52345,.F.);
#75035=ORIENTED_EDGE('',*,*,#52342,.F.);
#75036=ORIENTED_EDGE('',*,*,#52337,.F.);
#75037=ORIENTED_EDGE('',*,*,#52322,.F.);
#75038=ORIENTED_EDGE('',*,*,#52415,.F.);
#75039=ORIENTED_EDGE('',*,*,#52261,.F.);
#75040=ORIENTED_EDGE('',*,*,#52258,.F.);
#75041=ORIENTED_EDGE('',*,*,#52254,.F.);
#75042=ORIENTED_EDGE('',*,*,#52251,.F.);
#75043=ORIENTED_EDGE('',*,*,#52248,.F.);
#75044=ORIENTED_EDGE('',*,*,#52416,.T.);
#75045=ORIENTED_EDGE('',*,*,#52406,.F.);
#75046=ORIENTED_EDGE('',*,*,#52405,.F.);
#75047=ORIENTED_EDGE('',*,*,#52331,.F.);
#75048=ORIENTED_EDGE('',*,*,#52328,.F.);
#75049=ORIENTED_EDGE('',*,*,#52323,.F.);
#75050=ORIENTED_EDGE('',*,*,#52417,.T.);
#75051=ORIENTED_EDGE('',*,*,#52410,.F.);
#75052=ORIENTED_EDGE('',*,*,#52416,.F.);
#75053=ORIENTED_EDGE('',*,*,#52247,.F.);
#75054=ORIENTED_EDGE('',*,*,#52246,.F.);
#75055=ORIENTED_EDGE('',*,*,#52245,.F.);
#75056=ORIENTED_EDGE('',*,*,#52418,.F.);
#75057=ORIENTED_EDGE('',*,*,#52411,.F.);
#75058=ORIENTED_EDGE('',*,*,#52417,.F.);
#75059=ORIENTED_EDGE('',*,*,#52243,.F.);
#75060=ORIENTED_EDGE('',*,*,#52419,.F.);
#75061=ORIENTED_EDGE('',*,*,#52412,.T.);
#75062=ORIENTED_EDGE('',*,*,#52418,.T.);
#75063=ORIENTED_EDGE('',*,*,#52244,.F.);
#75064=ORIENTED_EDGE('',*,*,#52257,.F.);
#75065=ORIENTED_EDGE('',*,*,#52420,.F.);
#75066=ORIENTED_EDGE('',*,*,#52320,.T.);
#75067=ORIENTED_EDGE('',*,*,#52319,.T.);
#75068=ORIENTED_EDGE('',*,*,#52325,.T.);
#75069=ORIENTED_EDGE('',*,*,#52327,.T.);
#75070=ORIENTED_EDGE('',*,*,#52330,.T.);
#75071=ORIENTED_EDGE('',*,*,#52409,.T.);
#75072=ORIENTED_EDGE('',*,*,#52408,.T.);
#75073=ORIENTED_EDGE('',*,*,#52419,.T.);
#75074=ORIENTED_EDGE('',*,*,#52242,.F.);
#75075=ORIENTED_EDGE('',*,*,#52238,.F.);
#75076=ORIENTED_EDGE('',*,*,#52250,.F.);
#75077=ORIENTED_EDGE('',*,*,#52253,.F.);
#75078=ORIENTED_EDGE('',*,*,#52271,.F.);
#75079=ORIENTED_EDGE('',*,*,#52421,.F.);
#75080=ORIENTED_EDGE('',*,*,#52334,.T.);
#75081=ORIENTED_EDGE('',*,*,#52333,.T.);
#75082=ORIENTED_EDGE('',*,*,#52339,.T.);
#75083=ORIENTED_EDGE('',*,*,#52341,.T.);
#75084=ORIENTED_EDGE('',*,*,#52344,.T.);
#75085=ORIENTED_EDGE('',*,*,#52404,.T.);
#75086=ORIENTED_EDGE('',*,*,#52403,.T.);
#75087=ORIENTED_EDGE('',*,*,#52420,.T.);
#75088=ORIENTED_EDGE('',*,*,#52256,.F.);
#75089=ORIENTED_EDGE('',*,*,#52260,.F.);
#75090=ORIENTED_EDGE('',*,*,#52264,.F.);
#75091=ORIENTED_EDGE('',*,*,#52267,.F.);
#75092=ORIENTED_EDGE('',*,*,#52413,.T.);
#75093=ORIENTED_EDGE('',*,*,#52398,.F.);
#75094=ORIENTED_EDGE('',*,*,#52397,.F.);
#75095=ORIENTED_EDGE('',*,*,#52422,.F.);
#75096=ORIENTED_EDGE('',*,*,#52378,.T.);
#75097=ORIENTED_EDGE('',*,*,#52377,.T.);
#75098=ORIENTED_EDGE('',*,*,#52376,.F.);
#75099=ORIENTED_EDGE('',*,*,#52423,.F.);
#75100=ORIENTED_EDGE('',*,*,#52424,.F.);
#75101=ORIENTED_EDGE('',*,*,#52425,.F.);
#75102=ORIENTED_EDGE('',*,*,#52426,.F.);
#75103=ORIENTED_EDGE('',*,*,#52395,.T.);
#75104=ORIENTED_EDGE('',*,*,#52427,.F.);
#75105=ORIENTED_EDGE('',*,*,#52304,.F.);
#75106=ORIENTED_EDGE('',*,*,#52305,.F.);
#75107=ORIENTED_EDGE('',*,*,#52428,.T.);
#75108=ORIENTED_EDGE('',*,*,#52393,.F.);
#75109=ORIENTED_EDGE('',*,*,#52429,.T.);
#75110=ORIENTED_EDGE('',*,*,#52430,.F.);
#75111=ORIENTED_EDGE('',*,*,#52427,.T.);
#75112=ORIENTED_EDGE('',*,*,#52394,.F.);
#75113=ORIENTED_EDGE('',*,*,#52428,.F.);
#75114=ORIENTED_EDGE('',*,*,#52313,.T.);
#75115=ORIENTED_EDGE('',*,*,#52431,.T.);
#75116=ORIENTED_EDGE('',*,*,#52278,.T.);
#75117=ORIENTED_EDGE('',*,*,#52432,.T.);
#75118=ORIENTED_EDGE('',*,*,#52433,.T.);
#75119=ORIENTED_EDGE('',*,*,#52434,.F.);
#75120=ORIENTED_EDGE('',*,*,#52363,.F.);
#75121=ORIENTED_EDGE('',*,*,#52435,.F.);
#75122=ORIENTED_EDGE('',*,*,#52436,.F.);
#75123=ORIENTED_EDGE('',*,*,#52437,.T.);
#75124=ORIENTED_EDGE('',*,*,#52438,.T.);
#75125=ORIENTED_EDGE('',*,*,#52389,.T.);
#75126=ORIENTED_EDGE('',*,*,#52439,.T.);
#75127=ORIENTED_EDGE('',*,*,#52362,.F.);
#75128=ORIENTED_EDGE('',*,*,#52361,.F.);
#75129=ORIENTED_EDGE('',*,*,#52367,.F.);
#75130=ORIENTED_EDGE('',*,*,#52369,.F.);
#75131=ORIENTED_EDGE('',*,*,#52372,.F.);
#75132=ORIENTED_EDGE('',*,*,#52387,.F.);
#75133=ORIENTED_EDGE('',*,*,#52440,.F.);
#75134=ORIENTED_EDGE('',*,*,#52294,.F.);
#75135=ORIENTED_EDGE('',*,*,#52298,.F.);
#75136=ORIENTED_EDGE('',*,*,#52302,.F.);
#75137=ORIENTED_EDGE('',*,*,#52441,.F.);
#75138=ORIENTED_EDGE('',*,*,#52309,.F.);
#75139=ORIENTED_EDGE('',*,*,#52442,.T.);
#75140=ORIENTED_EDGE('',*,*,#52432,.F.);
#75141=ORIENTED_EDGE('',*,*,#52439,.F.);
#75142=ORIENTED_EDGE('',*,*,#52443,.F.);
#75143=ORIENTED_EDGE('',*,*,#52308,.T.);
#75144=ORIENTED_EDGE('',*,*,#52444,.F.);
#75145=ORIENTED_EDGE('',*,*,#52433,.F.);
#75146=ORIENTED_EDGE('',*,*,#52442,.F.);
#75147=ORIENTED_EDGE('',*,*,#52445,.F.);
#75148=ORIENTED_EDGE('',*,*,#52434,.T.);
#75149=ORIENTED_EDGE('',*,*,#52444,.T.);
#75150=ORIENTED_EDGE('',*,*,#52307,.F.);
#75151=ORIENTED_EDGE('',*,*,#52312,.F.);
#75152=ORIENTED_EDGE('',*,*,#52364,.T.);
#75153=ORIENTED_EDGE('',*,*,#52445,.T.);
#75154=ORIENTED_EDGE('',*,*,#52311,.F.);
#75155=ORIENTED_EDGE('',*,*,#52446,.F.);
#75156=ORIENTED_EDGE('',*,*,#52303,.F.);
#75157=ORIENTED_EDGE('',*,*,#52300,.F.);
#75158=ORIENTED_EDGE('',*,*,#52447,.F.);
#75159=ORIENTED_EDGE('',*,*,#52386,.T.);
#75160=ORIENTED_EDGE('',*,*,#52373,.T.);
#75161=ORIENTED_EDGE('',*,*,#52370,.T.);
#75162=ORIENTED_EDGE('',*,*,#52365,.T.);
#75163=ORIENTED_EDGE('',*,*,#52289,.F.);
#75164=ORIENTED_EDGE('',*,*,#52448,.F.);
#75165=ORIENTED_EDGE('',*,*,#52388,.T.);
#75166=ORIENTED_EDGE('',*,*,#52359,.T.);
#75167=ORIENTED_EDGE('',*,*,#52356,.T.);
#75168=ORIENTED_EDGE('',*,*,#52353,.T.);
#75169=ORIENTED_EDGE('',*,*,#52447,.T.);
#75170=ORIENTED_EDGE('',*,*,#52299,.F.);
#75171=ORIENTED_EDGE('',*,*,#52296,.F.);
#75172=ORIENTED_EDGE('',*,*,#52292,.F.);
#75173=ORIENTED_EDGE('',*,*,#52280,.F.);
#75174=ORIENTED_EDGE('',*,*,#52279,.F.);
#75175=ORIENTED_EDGE('',*,*,#52431,.F.);
#75176=ORIENTED_EDGE('',*,*,#52317,.F.);
#75177=ORIENTED_EDGE('',*,*,#52449,.F.);
#75178=ORIENTED_EDGE('',*,*,#52450,.T.);
#75179=ORIENTED_EDGE('',*,*,#52435,.T.);
#75180=ORIENTED_EDGE('',*,*,#52448,.T.);
#75181=ORIENTED_EDGE('',*,*,#52288,.F.);
#75182=ORIENTED_EDGE('',*,*,#52285,.F.);
#75183=ORIENTED_EDGE('',*,*,#52281,.F.);
#75184=ORIENTED_EDGE('',*,*,#52310,.F.);
#75185=ORIENTED_EDGE('',*,*,#52443,.T.);
#75186=ORIENTED_EDGE('',*,*,#52441,.T.);
#75187=ORIENTED_EDGE('',*,*,#52301,.T.);
#75188=ORIENTED_EDGE('',*,*,#52446,.T.);
#75189=ORIENTED_EDGE('',*,*,#52295,.F.);
#75190=ORIENTED_EDGE('',*,*,#52440,.T.);
#75191=ORIENTED_EDGE('',*,*,#52351,.F.);
#75192=ORIENTED_EDGE('',*,*,#52355,.F.);
#75193=ORIENTED_EDGE('',*,*,#52358,.F.);
#75194=ORIENTED_EDGE('',*,*,#52390,.F.);
#75195=ORIENTED_EDGE('',*,*,#52451,.F.);
#75196=ORIENTED_EDGE('',*,*,#52283,.F.);
#75197=ORIENTED_EDGE('',*,*,#52287,.F.);
#75198=ORIENTED_EDGE('',*,*,#52291,.F.);
#75199=ORIENTED_EDGE('',*,*,#52438,.F.);
#75200=ORIENTED_EDGE('',*,*,#52452,.F.);
#75201=ORIENTED_EDGE('',*,*,#52453,.T.);
#75202=ORIENTED_EDGE('',*,*,#52315,.T.);
#75203=ORIENTED_EDGE('',*,*,#52314,.T.);
#75204=ORIENTED_EDGE('',*,*,#52274,.F.);
#75205=ORIENTED_EDGE('',*,*,#52277,.F.);
#75206=ORIENTED_EDGE('',*,*,#52284,.F.);
#75207=ORIENTED_EDGE('',*,*,#52451,.T.);
#75208=ORIENTED_EDGE('',*,*,#52454,.F.);
#75209=ORIENTED_EDGE('',*,*,#52455,.T.);
#75210=ORIENTED_EDGE('',*,*,#52456,.T.);
#75211=ORIENTED_EDGE('',*,*,#52455,.F.);
#75212=ORIENTED_EDGE('',*,*,#52457,.F.);
#75213=ORIENTED_EDGE('',*,*,#52454,.T.);
#75214=ORIENTED_EDGE('',*,*,#52458,.T.);
#75215=ORIENTED_EDGE('',*,*,#52459,.F.);
#75216=ORIENTED_EDGE('',*,*,#52458,.F.);
#75217=ORIENTED_EDGE('',*,*,#52457,.T.);
#75218=ORIENTED_EDGE('',*,*,#52450,.F.);
#75219=ORIENTED_EDGE('',*,*,#52449,.T.);
#75220=ORIENTED_EDGE('',*,*,#52316,.T.);
#75221=ORIENTED_EDGE('',*,*,#52453,.F.);
#75222=ORIENTED_EDGE('',*,*,#52452,.T.);
#75223=ORIENTED_EDGE('',*,*,#52437,.F.);
#75224=ORIENTED_EDGE('',*,*,#52436,.T.);
#75225=ORIENTED_EDGE('',*,*,#52459,.T.);
#75226=ORIENTED_EDGE('',*,*,#52456,.F.);
#75227=ORIENTED_EDGE('',*,*,#52385,.F.);
#75228=ORIENTED_EDGE('',*,*,#52460,.T.);
#75229=ORIENTED_EDGE('',*,*,#52383,.T.);
#75230=ORIENTED_EDGE('',*,*,#52460,.F.);
#75231=ORIENTED_EDGE('',*,*,#52461,.T.);
#75232=ORIENTED_EDGE('',*,*,#52462,.F.);
#75233=ORIENTED_EDGE('',*,*,#52461,.F.);
#75234=ORIENTED_EDGE('',*,*,#52462,.T.);
#75235=ORIENTED_EDGE('',*,*,#52463,.T.);
#75236=ORIENTED_EDGE('',*,*,#52464,.F.);
#75237=ORIENTED_EDGE('',*,*,#52463,.F.);
#75238=ORIENTED_EDGE('',*,*,#52396,.T.);
#75239=ORIENTED_EDGE('',*,*,#52349,.T.);
#75240=ORIENTED_EDGE('',*,*,#52465,.T.);
#75241=ORIENTED_EDGE('',*,*,#52379,.T.);
#75242=ORIENTED_EDGE('',*,*,#52422,.T.);
#75243=ORIENTED_EDGE('',*,*,#52464,.T.);
#75244=ORIENTED_EDGE('',*,*,#52269,.T.);
#75245=ORIENTED_EDGE('',*,*,#52414,.T.);
#75246=ORIENTED_EDGE('',*,*,#52423,.T.);
#75247=ORIENTED_EDGE('',*,*,#52375,.F.);
#75248=ORIENTED_EDGE('',*,*,#52382,.F.);
#75249=ORIENTED_EDGE('',*,*,#52466,.T.);
#75250=ORIENTED_EDGE('',*,*,#52467,.T.);
#75251=ORIENTED_EDGE('',*,*,#52468,.T.);
#75252=ORIENTED_EDGE('',*,*,#52466,.F.);
#75253=ORIENTED_EDGE('',*,*,#52381,.F.);
#75254=ORIENTED_EDGE('',*,*,#52380,.F.);
#75255=ORIENTED_EDGE('',*,*,#52465,.F.);
#75256=ORIENTED_EDGE('',*,*,#52348,.T.);
#75257=ORIENTED_EDGE('',*,*,#52347,.T.);
#75258=ORIENTED_EDGE('',*,*,#52400,.T.);
#75259=ORIENTED_EDGE('',*,*,#52399,.T.);
#75260=ORIENTED_EDGE('',*,*,#52421,.T.);
#75261=ORIENTED_EDGE('',*,*,#52270,.F.);
#75262=ORIENTED_EDGE('',*,*,#52468,.F.);
#75263=ORIENTED_EDGE('',*,*,#52467,.F.);
#75264=ORIENTED_EDGE('',*,*,#52469,.F.);
#75265=ORIENTED_EDGE('',*,*,#52470,.T.);
#75266=ORIENTED_EDGE('',*,*,#52391,.F.);
#75267=ORIENTED_EDGE('',*,*,#52426,.T.);
#75268=ORIENTED_EDGE('',*,*,#52471,.T.);
#75269=ORIENTED_EDGE('',*,*,#52240,.F.);
#75270=ORIENTED_EDGE('',*,*,#52241,.F.);
#75271=ORIENTED_EDGE('',*,*,#52471,.F.);
#75272=ORIENTED_EDGE('',*,*,#52425,.T.);
#75273=ORIENTED_EDGE('',*,*,#52392,.F.);
#75274=ORIENTED_EDGE('',*,*,#52470,.F.);
#75275=ORIENTED_EDGE('',*,*,#52472,.T.);
#75276=ORIENTED_EDGE('',*,*,#52429,.F.);
#75277=ORIENTED_EDGE('',*,*,#52472,.F.);
#75278=ORIENTED_EDGE('',*,*,#52469,.T.);
#75279=ORIENTED_EDGE('',*,*,#52424,.T.);
#75280=ORIENTED_EDGE('',*,*,#52430,.T.);
#75281=SPHERICAL_SURFACE('',#79484,1.5);
#75282=SPHERICAL_SURFACE('',#79492,1.5);
#75283=SPHERICAL_SURFACE('',#79502,1.5);
#75284=SPHERICAL_SURFACE('',#79509,1.5);
#75285=SPHERICAL_SURFACE('',#79543,1.5);
#75286=SPHERICAL_SURFACE('',#79551,1.5);
#75287=SPHERICAL_SURFACE('',#79587,1.5);
#75288=SPHERICAL_SURFACE('',#79742,1.5);
#75289=SPHERICAL_SURFACE('',#79783,1.5);
#75290=SPHERICAL_SURFACE('',#79858,1.5);
#75291=SPHERICAL_SURFACE('',#79878,1.5);
#75292=SPHERICAL_SURFACE('',#80177,1.5);
#75293=SPHERICAL_SURFACE('',#80194,1.5);
#75294=SPHERICAL_SURFACE('',#80323,1.5);
#75295=SPHERICAL_SURFACE('',#80328,1.5);
#75296=SPHERICAL_SURFACE('',#80339,1.5);
#75297=SPHERICAL_SURFACE('',#85951,15.46041666667);
#75298=SPHERICAL_SURFACE('',#85964,15.76041666667);
#75299=SPHERICAL_SURFACE('',#86032,68.);
#75300=SPHERICAL_SURFACE('',#86054,67.);
#75301=SPHERICAL_SURFACE('',#86124,68.);
#75302=SPHERICAL_SURFACE('',#86146,67.);
#75303=ADVANCED_FACE('',(#19873),#75281,.F.);
#75304=ADVANCED_FACE('',(#19874),#16835,.T.);
#75305=ADVANCED_FACE('',(#19875),#2389,.F.);
#75306=ADVANCED_FACE('',(#19876),#2390,.T.);
#75307=ADVANCED_FACE('',(#19877),#2391,.F.);
#75308=ADVANCED_FACE('',(#19878),#1980,.F.);
#75309=ADVANCED_FACE('',(#19879),#1981,.T.);
#75310=ADVANCED_FACE('',(#19880),#75282,.F.);
#75311=ADVANCED_FACE('',(#19881),#2392,.F.);
#75312=ADVANCED_FACE('',(#19882),#16836,.T.);
#75313=ADVANCED_FACE('',(#19883),#2393,.F.);
#75314=ADVANCED_FACE('',(#19884),#2394,.T.);
#75315=ADVANCED_FACE('',(#19885),#1982,.F.);
#75316=ADVANCED_FACE('',(#19886),#1983,.T.);
#75317=ADVANCED_FACE('',(#19887),#1984,.T.);
#75318=ADVANCED_FACE('',(#19888),#2395,.F.);
#75319=ADVANCED_FACE('',(#19889),#75283,.F.);
#75320=ADVANCED_FACE('',(#19890),#1985,.F.);
#75321=ADVANCED_FACE('',(#19891),#16837,.T.);
#75322=ADVANCED_FACE('',(#19892),#2396,.F.);
#75323=ADVANCED_FACE('',(#19893),#2397,.T.);
#75324=ADVANCED_FACE('',(#19894),#2398,.F.);
#75325=ADVANCED_FACE('',(#19895),#2399,.T.);
#75326=ADVANCED_FACE('',(#19896),#16838,.T.);
#75327=ADVANCED_FACE('',(#19897),#1986,.T.);
#75328=ADVANCED_FACE('',(#19898),#75284,.F.);
#75329=ADVANCED_FACE('',(#19899),#2400,.F.);
#75330=ADVANCED_FACE('',(#19900),#2401,.F.);
#75331=ADVANCED_FACE('',(#19901),#16839,.T.);
#75332=ADVANCED_FACE('',(#19902),#1987,.F.);
#75333=ADVANCED_FACE('',(#19903),#2402,.T.);
#75334=ADVANCED_FACE('',(#19904),#2403,.T.);
#75335=ADVANCED_FACE('',(#19905),#2404,.F.);
#75336=ADVANCED_FACE('',(#19906),#16840,.T.);
#75337=ADVANCED_FACE('',(#19907),#1988,.F.);
#75338=ADVANCED_FACE('',(#19908),#1989,.F.);
#75339=ADVANCED_FACE('',(#19909),#1990,.F.);
#75340=ADVANCED_FACE('',(#19910),#1991,.F.);
#75341=ADVANCED_FACE('',(#19911),#1992,.F.);
#75342=ADVANCED_FACE('',(#19912),#1993,.F.);
#75343=ADVANCED_FACE('',(#19913),#1994,.F.);
#75344=ADVANCED_FACE('',(#19914),#1995,.F.);
#75345=ADVANCED_FACE('',(#19915),#1996,.F.);
#75346=ADVANCED_FACE('',(#19916),#1997,.F.);
#75347=ADVANCED_FACE('',(#19917),#1998,.F.);
#75348=ADVANCED_FACE('',(#19918),#1999,.F.);
#75349=ADVANCED_FACE('',(#19919),#2000,.F.);
#75350=ADVANCED_FACE('',(#19920),#2001,.F.);
#75351=ADVANCED_FACE('',(#19921),#2405,.F.);
#75352=ADVANCED_FACE('',(#19922),#2002,.T.);
#75353=ADVANCED_FACE('',(#19923),#75285,.F.);
#75354=ADVANCED_FACE('',(#19924),#2003,.T.);
#75355=ADVANCED_FACE('',(#19925),#75286,.F.);
#75356=ADVANCED_FACE('',(#19926),#1910,.F.);
#75357=ADVANCED_FACE('',(#19927),#2004,.F.);
#75358=ADVANCED_FACE('',(#19928),#1806,.T.);
#75359=ADVANCED_FACE('',(#19929),#2005,.F.);
#75360=ADVANCED_FACE('',(#19930),#1807,.T.);
#75361=ADVANCED_FACE('',(#19931),#1808,.T.);
#75362=ADVANCED_FACE('',(#19932),#2006,.T.);
#75363=ADVANCED_FACE('',(#19933),#2007,.T.);
#75364=ADVANCED_FACE('',(#19934),#1809,.T.);
#75365=ADVANCED_FACE('',(#19935),#2008,.T.);
#75366=ADVANCED_FACE('',(#19936),#75287,.F.);
#75367=ADVANCED_FACE('',(#19937),#2009,.F.);
#75368=ADVANCED_FACE('',(#19938),#1810,.T.);
#75369=ADVANCED_FACE('',(#19939),#2010,.F.);
#75370=ADVANCED_FACE('',(#19940),#2011,.F.);
#75371=ADVANCED_FACE('',(#19941),#2012,.F.);
#75372=ADVANCED_FACE('',(#19942),#2013,.F.);
#75373=ADVANCED_FACE('',(#19943),#1911,.F.);
#75374=ADVANCED_FACE('',(#19944),#2014,.F.);
#75375=ADVANCED_FACE('',(#19945),#2015,.F.);
#75376=ADVANCED_FACE('',(#19946),#1811,.T.);
#75377=ADVANCED_FACE('',(#19947),#2016,.F.);
#75378=ADVANCED_FACE('',(#19948),#1912,.F.);
#75379=ADVANCED_FACE('',(#19949),#2017,.F.);
#75380=ADVANCED_FACE('',(#19950),#2018,.T.);
#75381=ADVANCED_FACE('',(#19951),#2019,.F.);
#75382=ADVANCED_FACE('',(#19952),#2020,.F.);
#75383=ADVANCED_FACE('',(#19953),#2021,.F.);
#75384=ADVANCED_FACE('',(#19954),#1913,.F.);
#75385=ADVANCED_FACE('',(#19955),#1914,.F.);
#75386=ADVANCED_FACE('',(#19956),#2022,.F.);
#75387=ADVANCED_FACE('',(#19957),#1812,.T.);
#75388=ADVANCED_FACE('',(#19958),#2023,.F.);
#75389=ADVANCED_FACE('',(#19959),#1915,.F.);
#75390=ADVANCED_FACE('',(#19960),#2024,.F.);
#75391=ADVANCED_FACE('',(#19961),#2025,.T.);
#75392=ADVANCED_FACE('',(#19962),#2026,.F.);
#75393=ADVANCED_FACE('',(#19963),#2027,.F.);
#75394=ADVANCED_FACE('',(#19964),#2028,.T.);
#75395=ADVANCED_FACE('',(#19965),#2029,.T.);
#75396=ADVANCED_FACE('',(#19966),#1916,.T.);
#75397=ADVANCED_FACE('',(#19967),#2030,.F.);
#75398=ADVANCED_FACE('',(#19968),#1917,.F.);
#75399=ADVANCED_FACE('',(#19969),#1918,.F.);
#75400=ADVANCED_FACE('',(#19970),#1813,.T.);
#75401=ADVANCED_FACE('',(#19971),#2031,.F.);
#75402=ADVANCED_FACE('',(#19972),#1919,.F.);
#75403=ADVANCED_FACE('',(#19973),#2032,.F.);
#75404=ADVANCED_FACE('',(#19974),#2033,.T.);
#75405=ADVANCED_FACE('',(#19975),#2034,.F.);
#75406=ADVANCED_FACE('',(#19976),#2035,.F.);
#75407=ADVANCED_FACE('',(#19977),#2036,.T.);
#75408=ADVANCED_FACE('',(#19978),#2037,.T.);
#75409=ADVANCED_FACE('',(#19979),#1920,.T.);
#75410=ADVANCED_FACE('',(#19980),#2038,.F.);
#75411=ADVANCED_FACE('',(#19981),#1921,.F.);
#75412=ADVANCED_FACE('',(#19982),#1922,.F.);
#75413=ADVANCED_FACE('',(#19983,#245),#16841,.T.);
#75414=ADVANCED_FACE('',(#19984),#16842,.F.);
#75415=ADVANCED_FACE('',(#19985),#16843,.F.);
#75416=ADVANCED_FACE('',(#19986),#16844,.F.);
#75417=ADVANCED_FACE('',(#19987),#16845,.F.);
#75418=ADVANCED_FACE('',(#19988),#16846,.F.);
#75419=ADVANCED_FACE('',(#19989),#16847,.F.);
#75420=ADVANCED_FACE('',(#19990,#246),#16848,.T.);
#75421=ADVANCED_FACE('',(#19991,#247),#16849,.T.);
#75422=ADVANCED_FACE('',(#19992),#2039,.F.);
#75423=ADVANCED_FACE('',(#19993),#2406,.T.);
#75424=ADVANCED_FACE('',(#19994),#2407,.T.);
#75425=ADVANCED_FACE('',(#19995),#2040,.F.);
#75426=ADVANCED_FACE('',(#19996),#75288,.F.);
#75427=ADVANCED_FACE('',(#19997),#16850,.T.);
#75428=ADVANCED_FACE('',(#19998),#2408,.F.);
#75429=ADVANCED_FACE('',(#19999),#2409,.F.);
#75430=ADVANCED_FACE('',(#20000),#2041,.F.);
#75431=ADVANCED_FACE('',(#20001),#16851,.T.);
#75432=ADVANCED_FACE('',(#20002),#2410,.T.);
#75433=ADVANCED_FACE('',(#20003),#2042,.F.);
#75434=ADVANCED_FACE('',(#20004),#2043,.T.);
#75435=ADVANCED_FACE('',(#20005),#2411,.F.);
#75436=ADVANCED_FACE('',(#20006),#2044,.T.);
#75437=ADVANCED_FACE('',(#20007),#2412,.F.);
#75438=ADVANCED_FACE('',(#20008),#2413,.F.);
#75439=ADVANCED_FACE('',(#20009),#2414,.T.);
#75440=ADVANCED_FACE('',(#20010),#1814,.F.);
#75441=ADVANCED_FACE('',(#20011),#1815,.F.);
#75442=ADVANCED_FACE('',(#20012),#1816,.F.);
#75443=ADVANCED_FACE('',(#20013),#2415,.T.);
#75444=ADVANCED_FACE('',(#20014),#2416,.T.);
#75445=ADVANCED_FACE('',(#20015),#2417,.F.);
#75446=ADVANCED_FACE('',(#20016),#2045,.F.);
#75447=ADVANCED_FACE('',(#20017),#1817,.F.);
#75448=ADVANCED_FACE('',(#20018),#16852,.T.);
#75449=ADVANCED_FACE('',(#20019),#75289,.F.);
#75450=ADVANCED_FACE('',(#20020),#16853,.T.);
#75451=ADVANCED_FACE('',(#20021),#2418,.T.);
#75452=ADVANCED_FACE('',(#20022),#16854,.T.);
#75453=ADVANCED_FACE('',(#20023),#2419,.T.);
#75454=ADVANCED_FACE('',(#20024),#1818,.F.);
#75455=ADVANCED_FACE('',(#20025),#2420,.T.);
#75456=ADVANCED_FACE('',(#20026),#2046,.F.);
#75457=ADVANCED_FACE('',(#20027),#1819,.F.);
#75458=ADVANCED_FACE('',(#20028),#16855,.F.);
#75459=ADVANCED_FACE('',(#20029),#1820,.F.);
#75460=ADVANCED_FACE('',(#20030),#2047,.F.);
#75461=ADVANCED_FACE('',(#20031),#2421,.T.);
#75462=ADVANCED_FACE('',(#20032),#2048,.F.);
#75463=ADVANCED_FACE('',(#20033),#1821,.F.);
#75464=ADVANCED_FACE('',(#20034),#1822,.F.);
#75465=ADVANCED_FACE('',(#20035),#2049,.F.);
#75466=ADVANCED_FACE('',(#20036),#1823,.F.);
#75467=ADVANCED_FACE('',(#20037),#2050,.F.);
#75468=ADVANCED_FACE('',(#20038),#2051,.F.);
#75469=ADVANCED_FACE('',(#20039),#1824,.F.);
#75470=ADVANCED_FACE('',(#20040),#2052,.F.);
#75471=ADVANCED_FACE('',(#20041),#2053,.F.);
#75472=ADVANCED_FACE('',(#20042),#2422,.T.);
#75473=ADVANCED_FACE('',(#20043),#2423,.T.);
#75474=ADVANCED_FACE('',(#20044),#2424,.T.);
#75475=ADVANCED_FACE('',(#20045),#2425,.T.);
#75476=ADVANCED_FACE('',(#20046),#2426,.T.);
#75477=ADVANCED_FACE('',(#20047),#2427,.T.);
#75478=ADVANCED_FACE('',(#20048),#2428,.T.);
#75479=ADVANCED_FACE('',(#20049),#2429,.T.);
#75480=ADVANCED_FACE('',(#20050),#2430,.F.);
#75481=ADVANCED_FACE('',(#20051),#2431,.F.);
#75482=ADVANCED_FACE('',(#20052),#2432,.F.);
#75483=ADVANCED_FACE('',(#20053),#2433,.F.);
#75484=ADVANCED_FACE('',(#20054),#2434,.F.);
#75485=ADVANCED_FACE('',(#20055),#2435,.F.);
#75486=ADVANCED_FACE('',(#20056),#2436,.F.);
#75487=ADVANCED_FACE('',(#20057),#2437,.F.);
#75488=ADVANCED_FACE('',(#20058),#2438,.F.);
#75489=ADVANCED_FACE('',(#20059,#248),#16856,.F.);
#75490=ADVANCED_FACE('',(#20060),#113,.T.);
#75491=ADVANCED_FACE('',(#20061),#114,.T.);
#75492=ADVANCED_FACE('',(#20062),#115,.T.);
#75493=ADVANCED_FACE('',(#20063),#116,.T.);
#75494=ADVANCED_FACE('',(#20064),#117,.T.);
#75495=ADVANCED_FACE('',(#20065),#118,.T.);
#75496=ADVANCED_FACE('',(#20066,#249),#16857,.T.);
#75497=ADVANCED_FACE('',(#20067,#250),#16858,.T.);
#75498=ADVANCED_FACE('',(#20068),#16859,.F.);
#75499=ADVANCED_FACE('',(#20069),#16860,.F.);
#75500=ADVANCED_FACE('',(#20070),#16861,.F.);
#75501=ADVANCED_FACE('',(#20071),#16862,.F.);
#75502=ADVANCED_FACE('',(#20072),#16863,.F.);
#75503=ADVANCED_FACE('',(#20073),#16864,.F.);
#75504=ADVANCED_FACE('',(#20074,#251),#16865,.T.);
#75505=ADVANCED_FACE('',(#20075,#252),#16866,.T.);
#75506=ADVANCED_FACE('',(#20076),#2439,.T.);
#75507=ADVANCED_FACE('',(#20077),#2054,.F.);
#75508=ADVANCED_FACE('',(#20078),#2440,.F.);
#75509=ADVANCED_FACE('',(#20079),#2055,.T.);
#75510=ADVANCED_FACE('',(#20080),#2441,.T.);
#75511=ADVANCED_FACE('',(#20081),#2442,.F.);
#75512=ADVANCED_FACE('',(#20082),#2056,.F.);
#75513=ADVANCED_FACE('',(#20083),#2057,.F.);
#75514=ADVANCED_FACE('',(#20084),#2443,.F.);
#75515=ADVANCED_FACE('',(#20085),#16867,.T.);
#75516=ADVANCED_FACE('',(#20086),#2444,.F.);
#75517=ADVANCED_FACE('',(#20087),#75290,.F.);
#75518=ADVANCED_FACE('',(#20088),#2058,.F.);
#75519=ADVANCED_FACE('',(#20089),#16868,.T.);
#75520=ADVANCED_FACE('',(#20090),#2059,.T.);
#75521=ADVANCED_FACE('',(#20091),#2445,.T.);
#75522=ADVANCED_FACE('',(#20092),#2446,.T.);
#75523=ADVANCED_FACE('',(#20093),#2447,.F.);
#75524=ADVANCED_FACE('',(#20094),#2448,.T.);
#75525=ADVANCED_FACE('',(#20095),#16869,.T.);
#75526=ADVANCED_FACE('',(#20096),#2449,.T.);
#75527=ADVANCED_FACE('',(#20097),#16870,.T.);
#75528=ADVANCED_FACE('',(#20098),#75291,.F.);
#75529=ADVANCED_FACE('',(#20099),#16871,.T.);
#75530=ADVANCED_FACE('',(#20100),#1825,.F.);
#75531=ADVANCED_FACE('',(#20101),#2060,.F.);
#75532=ADVANCED_FACE('',(#20102),#2450,.F.);
#75533=ADVANCED_FACE('',(#20103),#2451,.T.);
#75534=ADVANCED_FACE('',(#20104),#2452,.T.);
#75535=ADVANCED_FACE('',(#20105),#1826,.F.);
#75536=ADVANCED_FACE('',(#20106),#1827,.F.);
#75537=ADVANCED_FACE('',(#20107),#1828,.F.);
#75538=ADVANCED_FACE('',(#20108),#2061,.F.);
#75539=ADVANCED_FACE('',(#20109),#2453,.T.);
#75540=ADVANCED_FACE('',(#20110),#1829,.F.);
#75541=ADVANCED_FACE('',(#20111),#1830,.F.);
#75542=ADVANCED_FACE('',(#20112),#2062,.F.);
#75543=ADVANCED_FACE('',(#20113),#1831,.F.);
#75544=ADVANCED_FACE('',(#20114),#1832,.F.);
#75545=ADVANCED_FACE('',(#20115),#2063,.F.);
#75546=ADVANCED_FACE('',(#20116),#2454,.T.);
#75547=ADVANCED_FACE('',(#20117),#2064,.F.);
#75548=ADVANCED_FACE('',(#20118),#1833,.F.);
#75549=ADVANCED_FACE('',(#20119),#16872,.T.);
#75550=ADVANCED_FACE('',(#20120),#1834,.F.);
#75551=ADVANCED_FACE('',(#20121),#2065,.F.);
#75552=ADVANCED_FACE('',(#20122),#2066,.F.);
#75553=ADVANCED_FACE('',(#20123),#2067,.F.);
#75554=ADVANCED_FACE('',(#20124),#1835,.F.);
#75555=ADVANCED_FACE('',(#20125),#2068,.F.);
#75556=ADVANCED_FACE('',(#20126),#2455,.T.);
#75557=ADVANCED_FACE('',(#20127),#2456,.T.);
#75558=ADVANCED_FACE('',(#20128),#2457,.T.);
#75559=ADVANCED_FACE('',(#20129),#2458,.T.);
#75560=ADVANCED_FACE('',(#20130),#2459,.T.);
#75561=ADVANCED_FACE('',(#20131),#2460,.T.);
#75562=ADVANCED_FACE('',(#20132),#2461,.T.);
#75563=ADVANCED_FACE('',(#20133),#2462,.T.);
#75564=ADVANCED_FACE('',(#20134),#2463,.F.);
#75565=ADVANCED_FACE('',(#20135),#2464,.F.);
#75566=ADVANCED_FACE('',(#20136),#2465,.F.);
#75567=ADVANCED_FACE('',(#20137),#2466,.F.);
#75568=ADVANCED_FACE('',(#20138),#2467,.F.);
#75569=ADVANCED_FACE('',(#20139),#2468,.F.);
#75570=ADVANCED_FACE('',(#20140),#2469,.F.);
#75571=ADVANCED_FACE('',(#20141),#2470,.F.);
#75572=ADVANCED_FACE('',(#20142),#2471,.F.);
#75573=ADVANCED_FACE('',(#20143,#253),#16873,.F.);
#75574=ADVANCED_FACE('',(#20144),#119,.F.);
#75575=ADVANCED_FACE('',(#20145),#120,.F.);
#75576=ADVANCED_FACE('',(#20146),#121,.F.);
#75577=ADVANCED_FACE('',(#20147),#122,.F.);
#75578=ADVANCED_FACE('',(#20148),#123,.F.);
#75579=ADVANCED_FACE('',(#20149),#124,.F.);
#75580=ADVANCED_FACE('',(#20150,#254),#16874,.F.);
#75581=ADVANCED_FACE('',(#20151),#125,.F.);
#75582=ADVANCED_FACE('',(#20152),#126,.F.);
#75583=ADVANCED_FACE('',(#20153),#16875,.T.);
#75584=ADVANCED_FACE('',(#20154,#255),#16876,.T.);
#75585=ADVANCED_FACE('',(#20155),#16877,.F.);
#75586=ADVANCED_FACE('',(#20156),#16878,.T.);
#75587=ADVANCED_FACE('',(#20157),#16879,.T.);
#75588=ADVANCED_FACE('',(#20158),#16880,.T.);
#75589=ADVANCED_FACE('',(#20159),#16881,.T.);
#75590=ADVANCED_FACE('',(#20160),#2069,.F.);
#75591=ADVANCED_FACE('',(#20161),#2472,.F.);
#75592=ADVANCED_FACE('',(#20162),#16882,.T.);
#75593=ADVANCED_FACE('',(#20163),#2473,.T.);
#75594=ADVANCED_FACE('',(#20164),#2070,.F.);
#75595=ADVANCED_FACE('',(#20165),#2071,.F.);
#75596=ADVANCED_FACE('',(#20166),#2072,.F.);
#75597=ADVANCED_FACE('',(#20167),#2073,.F.);
#75598=ADVANCED_FACE('',(#20168),#2474,.T.);
#75599=ADVANCED_FACE('',(#20169),#2475,.T.);
#75600=ADVANCED_FACE('',(#20170),#2476,.T.);
#75601=ADVANCED_FACE('',(#20171),#2477,.T.);
#75602=ADVANCED_FACE('',(#20172),#2074,.F.);
#75603=ADVANCED_FACE('',(#20173),#2075,.F.);
#75604=ADVANCED_FACE('',(#20174),#2478,.T.);
#75605=ADVANCED_FACE('',(#20175),#2479,.T.);
#75606=ADVANCED_FACE('',(#20176),#2480,.T.);
#75607=ADVANCED_FACE('',(#20177),#2481,.F.);
#75608=ADVANCED_FACE('',(#20178),#2076,.F.);
#75609=ADVANCED_FACE('',(#20179),#2077,.T.);
#75610=ADVANCED_FACE('',(#20180),#127,.F.);
#75611=ADVANCED_FACE('',(#20181),#2482,.F.);
#75612=ADVANCED_FACE('',(#20182),#2483,.F.);
#75613=ADVANCED_FACE('',(#20183),#2484,.F.);
#75614=ADVANCED_FACE('',(#20184),#2485,.T.);
#75615=ADVANCED_FACE('',(#20185),#2486,.T.);
#75616=ADVANCED_FACE('',(#20186),#2487,.T.);
#75617=ADVANCED_FACE('',(#20187),#2488,.T.);
#75618=ADVANCED_FACE('',(#20188),#2489,.T.);
#75619=ADVANCED_FACE('',(#20189),#2490,.T.);
#75620=ADVANCED_FACE('',(#20190),#2491,.T.);
#75621=ADVANCED_FACE('',(#20191),#2492,.T.);
#75622=ADVANCED_FACE('',(#20192),#1836,.F.);
#75623=ADVANCED_FACE('',(#20193),#1837,.F.);
#75624=ADVANCED_FACE('',(#20194),#1838,.F.);
#75625=ADVANCED_FACE('',(#20195),#2078,.F.);
#75626=ADVANCED_FACE('',(#20196),#1839,.F.);
#75627=ADVANCED_FACE('',(#20197),#16883,.T.);
#75628=ADVANCED_FACE('',(#20198),#16884,.T.);
#75629=ADVANCED_FACE('',(#20199),#2079,.T.);
#75630=ADVANCED_FACE('',(#20200),#2493,.T.);
#75631=ADVANCED_FACE('',(#20201),#2494,.F.);
#75632=ADVANCED_FACE('',(#20202),#1840,.F.);
#75633=ADVANCED_FACE('',(#20203),#2495,.T.);
#75634=ADVANCED_FACE('',(#20204),#2496,.F.);
#75635=ADVANCED_FACE('',(#20205),#2080,.F.);
#75636=ADVANCED_FACE('',(#20206),#1841,.F.);
#75637=ADVANCED_FACE('',(#20207),#1842,.F.);
#75638=ADVANCED_FACE('',(#20208),#2081,.F.);
#75639=ADVANCED_FACE('',(#20209),#2082,.F.);
#75640=ADVANCED_FACE('',(#20210),#2497,.F.);
#75641=ADVANCED_FACE('',(#20211),#2498,.F.);
#75642=ADVANCED_FACE('',(#20212),#2499,.F.);
#75643=ADVANCED_FACE('',(#20213),#2500,.T.);
#75644=ADVANCED_FACE('',(#20214),#16885,.T.);
#75645=ADVANCED_FACE('',(#20215,#256),#16886,.T.);
#75646=ADVANCED_FACE('',(#20216,#257),#16887,.T.);
#75647=ADVANCED_FACE('',(#20217),#2501,.T.);
#75648=ADVANCED_FACE('',(#20218),#2083,.T.);
#75649=ADVANCED_FACE('',(#20219),#2084,.T.);
#75650=ADVANCED_FACE('',(#20220),#2085,.T.);
#75651=ADVANCED_FACE('',(#20221),#2502,.T.);
#75652=ADVANCED_FACE('',(#20222),#2503,.T.);
#75653=ADVANCED_FACE('',(#20223),#2504,.T.);
#75654=ADVANCED_FACE('',(#20224),#2505,.T.);
#75655=ADVANCED_FACE('',(#20225),#2506,.T.);
#75656=ADVANCED_FACE('',(#20226),#2086,.T.);
#75657=ADVANCED_FACE('',(#20227),#128,.T.);
#75658=ADVANCED_FACE('',(#20228),#129,.F.);
#75659=ADVANCED_FACE('',(#20229),#130,.T.);
#75660=ADVANCED_FACE('',(#20230),#2087,.T.);
#75661=ADVANCED_FACE('',(#20231),#131,.T.);
#75662=ADVANCED_FACE('',(#20232),#132,.T.);
#75663=ADVANCED_FACE('',(#20233),#2507,.T.);
#75664=ADVANCED_FACE('',(#20234),#133,.T.);
#75665=ADVANCED_FACE('',(#20235),#134,.T.);
#75666=ADVANCED_FACE('',(#20236),#2088,.T.);
#75667=ADVANCED_FACE('',(#20237),#135,.F.);
#75668=ADVANCED_FACE('',(#20238,#258),#16888,.F.);
#75669=ADVANCED_FACE('',(#20239,#259),#16889,.T.);
#75670=ADVANCED_FACE('',(#20240,#260),#16890,.T.);
#75671=ADVANCED_FACE('',(#20241),#16891,.T.);
#75672=ADVANCED_FACE('',(#20242),#16892,.T.);
#75673=ADVANCED_FACE('',(#20243),#2508,.F.);
#75674=ADVANCED_FACE('',(#20244),#2509,.F.);
#75675=ADVANCED_FACE('',(#20245),#2510,.F.);
#75676=ADVANCED_FACE('',(#20246),#2511,.F.);
#75677=ADVANCED_FACE('',(#20247),#136,.T.);
#75678=ADVANCED_FACE('',(#20248),#2512,.F.);
#75679=ADVANCED_FACE('',(#20249),#16893,.T.);
#75680=ADVANCED_FACE('',(#20250),#2089,.T.);
#75681=ADVANCED_FACE('',(#20251),#2513,.F.);
#75682=ADVANCED_FACE('',(#20252),#137,.T.);
#75683=ADVANCED_FACE('',(#20253),#2514,.F.);
#75684=ADVANCED_FACE('',(#20254),#2515,.F.);
#75685=ADVANCED_FACE('',(#20255),#138,.T.);
#75686=ADVANCED_FACE('',(#20256),#139,.T.);
#75687=ADVANCED_FACE('',(#20257),#140,.T.);
#75688=ADVANCED_FACE('',(#20258),#2090,.F.);
#75689=ADVANCED_FACE('',(#20259),#2516,.F.);
#75690=ADVANCED_FACE('',(#20260),#2517,.F.);
#75691=ADVANCED_FACE('',(#20261),#2091,.F.);
#75692=ADVANCED_FACE('',(#20262),#1843,.F.);
#75693=ADVANCED_FACE('',(#20263),#1844,.F.);
#75694=ADVANCED_FACE('',(#20264),#2518,.F.);
#75695=ADVANCED_FACE('',(#20265),#2092,.F.);
#75696=ADVANCED_FACE('',(#20266),#2519,.F.);
#75697=ADVANCED_FACE('',(#20267),#1845,.F.);
#75698=ADVANCED_FACE('',(#20268),#2520,.F.);
#75699=ADVANCED_FACE('',(#20269),#2093,.F.);
#75700=ADVANCED_FACE('',(#20270),#2521,.T.);
#75701=ADVANCED_FACE('',(#20271),#2094,.F.);
#75702=ADVANCED_FACE('',(#20272),#2522,.F.);
#75703=ADVANCED_FACE('',(#20273),#1846,.F.);
#75704=ADVANCED_FACE('',(#20274),#2523,.F.);
#75705=ADVANCED_FACE('',(#20275),#2095,.F.);
#75706=ADVANCED_FACE('',(#20276),#2524,.F.);
#75707=ADVANCED_FACE('',(#20277),#1847,.F.);
#75708=ADVANCED_FACE('',(#20278),#1848,.F.);
#75709=ADVANCED_FACE('',(#20279),#2096,.F.);
#75710=ADVANCED_FACE('',(#20280),#2097,.F.);
#75711=ADVANCED_FACE('',(#20281),#141,.T.);
#75712=ADVANCED_FACE('',(#20282),#142,.T.);
#75713=ADVANCED_FACE('',(#20283),#143,.T.);
#75714=ADVANCED_FACE('',(#20284),#144,.T.);
#75715=ADVANCED_FACE('',(#20285),#2098,.F.);
#75716=ADVANCED_FACE('',(#20286),#145,.T.);
#75717=ADVANCED_FACE('',(#20287),#2525,.F.);
#75718=ADVANCED_FACE('',(#20288),#2526,.F.);
#75719=ADVANCED_FACE('',(#20289),#146,.T.);
#75720=ADVANCED_FACE('',(#20290),#147,.T.);
#75721=ADVANCED_FACE('',(#20291),#2527,.F.);
#75722=ADVANCED_FACE('',(#20292),#2528,.F.);
#75723=ADVANCED_FACE('',(#20293),#148,.T.);
#75724=ADVANCED_FACE('',(#20294),#2529,.F.);
#75725=ADVANCED_FACE('',(#20295),#2530,.F.);
#75726=ADVANCED_FACE('',(#20296),#149,.T.);
#75727=ADVANCED_FACE('',(#20297),#150,.T.);
#75728=ADVANCED_FACE('',(#20298),#2531,.F.);
#75729=ADVANCED_FACE('',(#20299),#2532,.F.);
#75730=ADVANCED_FACE('',(#20300),#151,.T.);
#75731=ADVANCED_FACE('',(#20301),#1849,.F.);
#75732=ADVANCED_FACE('',(#20302),#16894,.T.);
#75733=ADVANCED_FACE('',(#20303),#2099,.T.);
#75734=ADVANCED_FACE('',(#20304),#16895,.T.);
#75735=ADVANCED_FACE('',(#20305),#2100,.F.);
#75736=ADVANCED_FACE('',(#20306),#16896,.T.);
#75737=ADVANCED_FACE('',(#20307,#261),#16897,.F.);
#75738=ADVANCED_FACE('',(#20308,#262),#16898,.F.);
#75739=ADVANCED_FACE('',(#20309),#2101,.T.);
#75740=ADVANCED_FACE('',(#20310),#2102,.F.);
#75741=ADVANCED_FACE('',(#20311),#16899,.T.);
#75742=ADVANCED_FACE('',(#20312),#16900,.T.);
#75743=ADVANCED_FACE('',(#20313),#1850,.T.);
#75744=ADVANCED_FACE('',(#20314),#2533,.T.);
#75745=ADVANCED_FACE('',(#20315),#2103,.T.);
#75746=ADVANCED_FACE('',(#20316),#2104,.T.);
#75747=ADVANCED_FACE('',(#20317),#2105,.T.);
#75748=ADVANCED_FACE('',(#20318),#16901,.T.);
#75749=ADVANCED_FACE('',(#20319),#2106,.T.);
#75750=ADVANCED_FACE('',(#20320),#2534,.T.);
#75751=ADVANCED_FACE('',(#20321),#1851,.T.);
#75752=ADVANCED_FACE('',(#20322),#2535,.T.);
#75753=ADVANCED_FACE('',(#20323),#1852,.T.);
#75754=ADVANCED_FACE('',(#20324),#1853,.T.);
#75755=ADVANCED_FACE('',(#20325),#2536,.T.);
#75756=ADVANCED_FACE('',(#20326),#2537,.T.);
#75757=ADVANCED_FACE('',(#20327),#2107,.F.);
#75758=ADVANCED_FACE('',(#20328),#16902,.T.);
#75759=ADVANCED_FACE('',(#20329),#2108,.F.);
#75760=ADVANCED_FACE('',(#20330),#2538,.T.);
#75761=ADVANCED_FACE('',(#20331),#75292,.F.);
#75762=ADVANCED_FACE('',(#20332),#1854,.T.);
#75763=ADVANCED_FACE('',(#20333),#1855,.T.);
#75764=ADVANCED_FACE('',(#20334),#1856,.F.);
#75765=ADVANCED_FACE('',(#20335),#2539,.F.);
#75766=ADVANCED_FACE('',(#20336),#2540,.T.);
#75767=ADVANCED_FACE('',(#20337),#2109,.T.);
#75768=ADVANCED_FACE('',(#20338),#16903,.T.);
#75769=ADVANCED_FACE('',(#20339),#16904,.T.);
#75770=ADVANCED_FACE('',(#20340),#2110,.F.);
#75771=ADVANCED_FACE('',(#20341),#75293,.F.);
#75772=ADVANCED_FACE('',(#20342),#1857,.F.);
#75773=ADVANCED_FACE('',(#20343),#2541,.F.);
#75774=ADVANCED_FACE('',(#20344),#152,.T.);
#75775=ADVANCED_FACE('',(#20345),#2542,.F.);
#75776=ADVANCED_FACE('',(#20346),#2543,.F.);
#75777=ADVANCED_FACE('',(#20347),#2544,.T.);
#75778=ADVANCED_FACE('',(#20348),#2111,.F.);
#75779=ADVANCED_FACE('',(#20349),#2545,.F.);
#75780=ADVANCED_FACE('',(#20350),#2112,.F.);
#75781=ADVANCED_FACE('',(#20351),#2113,.F.);
#75782=ADVANCED_FACE('',(#20352),#2114,.F.);
#75783=ADVANCED_FACE('',(#20353),#2546,.T.);
#75784=ADVANCED_FACE('',(#20354),#2547,.F.);
#75785=ADVANCED_FACE('',(#20355),#2548,.T.);
#75786=ADVANCED_FACE('',(#20356),#2549,.T.);
#75787=ADVANCED_FACE('',(#20357),#2550,.F.);
#75788=ADVANCED_FACE('',(#20358),#2551,.F.);
#75789=ADVANCED_FACE('',(#20359),#2552,.T.);
#75790=ADVANCED_FACE('',(#20360,#263),#16905,.T.);
#75791=ADVANCED_FACE('',(#20361),#2553,.T.);
#75792=ADVANCED_FACE('',(#20362),#2554,.T.);
#75793=ADVANCED_FACE('',(#20363),#153,.T.);
#75794=ADVANCED_FACE('',(#20364),#2115,.T.);
#75795=ADVANCED_FACE('',(#20365),#2555,.T.);
#75796=ADVANCED_FACE('',(#20366),#154,.T.);
#75797=ADVANCED_FACE('',(#20367),#2556,.T.);
#75798=ADVANCED_FACE('',(#20368),#2116,.T.);
#75799=ADVANCED_FACE('',(#20369),#155,.T.);
#75800=ADVANCED_FACE('',(#20370),#2557,.T.);
#75801=ADVANCED_FACE('',(#20371),#2558,.T.);
#75802=ADVANCED_FACE('',(#20372),#156,.T.);
#75803=ADVANCED_FACE('',(#20373),#1858,.T.);
#75804=ADVANCED_FACE('',(#20374),#2117,.T.);
#75805=ADVANCED_FACE('',(#20375),#2118,.T.);
#75806=ADVANCED_FACE('',(#20376),#2119,.T.);
#75807=ADVANCED_FACE('',(#20377),#1859,.T.);
#75808=ADVANCED_FACE('',(#20378),#2120,.T.);
#75809=ADVANCED_FACE('',(#20379),#2121,.T.);
#75810=ADVANCED_FACE('',(#20380),#2559,.T.);
#75811=ADVANCED_FACE('',(#20381),#157,.T.);
#75812=ADVANCED_FACE('',(#20382),#2560,.T.);
#75813=ADVANCED_FACE('',(#20383),#2561,.T.);
#75814=ADVANCED_FACE('',(#20384),#158,.T.);
#75815=ADVANCED_FACE('',(#20385),#2562,.T.);
#75816=ADVANCED_FACE('',(#20386),#2563,.T.);
#75817=ADVANCED_FACE('',(#20387),#159,.T.);
#75818=ADVANCED_FACE('',(#20388),#2564,.T.);
#75819=ADVANCED_FACE('',(#20389),#160,.T.);
#75820=ADVANCED_FACE('',(#20390,#264),#16906,.T.);
#75821=ADVANCED_FACE('',(#20391),#2122,.T.);
#75822=ADVANCED_FACE('',(#20392),#2123,.T.);
#75823=ADVANCED_FACE('',(#20393),#2124,.T.);
#75824=ADVANCED_FACE('',(#20394),#1860,.T.);
#75825=ADVANCED_FACE('',(#20395),#1861,.T.);
#75826=ADVANCED_FACE('',(#20396),#1862,.T.);
#75827=ADVANCED_FACE('',(#20397),#16907,.F.);
#75828=ADVANCED_FACE('',(#20398),#1863,.T.);
#75829=ADVANCED_FACE('',(#20399),#2125,.T.);
#75830=ADVANCED_FACE('',(#20400),#161,.T.);
#75831=ADVANCED_FACE('',(#20401),#162,.T.);
#75832=ADVANCED_FACE('',(#20402),#2565,.T.);
#75833=ADVANCED_FACE('',(#20403),#163,.T.);
#75834=ADVANCED_FACE('',(#20404),#2566,.T.);
#75835=ADVANCED_FACE('',(#20405),#164,.T.);
#75836=ADVANCED_FACE('',(#20406),#165,.T.);
#75837=ADVANCED_FACE('',(#20407),#166,.T.);
#75838=ADVANCED_FACE('',(#20408),#2126,.T.);
#75839=ADVANCED_FACE('',(#20409),#2127,.T.);
#75840=ADVANCED_FACE('',(#20410),#167,.T.);
#75841=ADVANCED_FACE('',(#20411),#2567,.T.);
#75842=ADVANCED_FACE('',(#20412),#168,.T.);
#75843=ADVANCED_FACE('',(#20413),#2568,.T.);
#75844=ADVANCED_FACE('',(#20414),#1864,.T.);
#75845=ADVANCED_FACE('',(#20415),#1865,.T.);
#75846=ADVANCED_FACE('',(#20416),#1866,.T.);
#75847=ADVANCED_FACE('',(#20417),#16908,.T.);
#75848=ADVANCED_FACE('',(#20418),#1867,.T.);
#75849=ADVANCED_FACE('',(#20419,#265),#16909,.F.);
#75850=ADVANCED_FACE('',(#20420),#2569,.T.);
#75851=ADVANCED_FACE('',(#20421),#169,.T.);
#75852=ADVANCED_FACE('',(#20422),#2570,.T.);
#75853=ADVANCED_FACE('',(#20423),#2128,.T.);
#75854=ADVANCED_FACE('',(#20424),#2571,.T.);
#75855=ADVANCED_FACE('',(#20425),#170,.T.);
#75856=ADVANCED_FACE('',(#20426),#2572,.T.);
#75857=ADVANCED_FACE('',(#20427),#2129,.T.);
#75858=ADVANCED_FACE('',(#20428),#2573,.T.);
#75859=ADVANCED_FACE('',(#20429),#171,.T.);
#75860=ADVANCED_FACE('',(#20430),#2574,.T.);
#75861=ADVANCED_FACE('',(#20431),#2575,.T.);
#75862=ADVANCED_FACE('',(#20432),#2130,.T.);
#75863=ADVANCED_FACE('',(#20433),#2576,.T.);
#75864=ADVANCED_FACE('',(#20434),#172,.T.);
#75865=ADVANCED_FACE('',(#20435),#2577,.T.);
#75866=ADVANCED_FACE('',(#20436),#173,.T.);
#75867=ADVANCED_FACE('',(#20437,#266),#16910,.T.);
#75868=ADVANCED_FACE('',(#20438),#2131,.T.);
#75869=ADVANCED_FACE('',(#20439),#2132,.T.);
#75870=ADVANCED_FACE('',(#20440,#267),#16911,.F.);
#75871=ADVANCED_FACE('',(#20441,#268),#16912,.F.);
#75872=ADVANCED_FACE('',(#20442),#1923,.F.);
#75873=ADVANCED_FACE('',(#20443),#2133,.F.);
#75874=ADVANCED_FACE('',(#20444),#16913,.T.);
#75875=ADVANCED_FACE('',(#20445),#2578,.F.);
#75876=ADVANCED_FACE('',(#20446),#2579,.T.);
#75877=ADVANCED_FACE('',(#20447),#2580,.F.);
#75878=ADVANCED_FACE('',(#20448),#75294,.F.);
#75879=ADVANCED_FACE('',(#20449),#2581,.F.);
#75880=ADVANCED_FACE('',(#20450),#174,.T.);
#75881=ADVANCED_FACE('',(#20451),#2582,.F.);
#75882=ADVANCED_FACE('',(#20452),#2583,.F.);
#75883=ADVANCED_FACE('',(#20453),#2584,.T.);
#75884=ADVANCED_FACE('',(#20454),#175,.T.);
#75885=ADVANCED_FACE('',(#20455),#2585,.F.);
#75886=ADVANCED_FACE('',(#20456),#1868,.F.);
#75887=ADVANCED_FACE('',(#20457),#75295,.F.);
#75888=ADVANCED_FACE('',(#20458),#2134,.F.);
#75889=ADVANCED_FACE('',(#20459),#2586,.F.);
#75890=ADVANCED_FACE('',(#20460),#2587,.F.);
#75891=ADVANCED_FACE('',(#20461),#2135,.T.);
#75892=ADVANCED_FACE('',(#20462),#2588,.F.);
#75893=ADVANCED_FACE('',(#20463),#2589,.T.);
#75894=ADVANCED_FACE('',(#20464),#1869,.F.);
#75895=ADVANCED_FACE('',(#20465),#2136,.F.);
#75896=ADVANCED_FACE('',(#20466),#2590,.F.);
#75897=ADVANCED_FACE('',(#20467),#2591,.T.);
#75898=ADVANCED_FACE('',(#20468),#2592,.F.);
#75899=ADVANCED_FACE('',(#20469),#75296,.F.);
#75900=ADVANCED_FACE('',(#20470),#2593,.F.);
#75901=ADVANCED_FACE('',(#20471),#2594,.F.);
#75902=ADVANCED_FACE('',(#20472),#2137,.T.);
#75903=ADVANCED_FACE('',(#20473),#2138,.T.);
#75904=ADVANCED_FACE('',(#20474),#2139,.T.);
#75905=ADVANCED_FACE('',(#20475),#2595,.F.);
#75906=ADVANCED_FACE('',(#20476),#2140,.F.);
#75907=ADVANCED_FACE('',(#20477),#1870,.T.);
#75908=ADVANCED_FACE('',(#20478),#2596,.F.);
#75909=ADVANCED_FACE('',(#20479),#2141,.F.);
#75910=ADVANCED_FACE('',(#20480),#2142,.F.);
#75911=ADVANCED_FACE('',(#20481),#2597,.T.);
#75912=ADVANCED_FACE('',(#20482),#2143,.T.);
#75913=ADVANCED_FACE('',(#20483),#1871,.T.);
#75914=ADVANCED_FACE('',(#20484),#2598,.F.);
#75915=ADVANCED_FACE('',(#20485),#2144,.F.);
#75916=ADVANCED_FACE('',(#20486),#2599,.T.);
#75917=ADVANCED_FACE('',(#20487),#1872,.F.);
#75918=ADVANCED_FACE('',(#20488),#1873,.F.);
#75919=ADVANCED_FACE('',(#20489),#2145,.F.);
#75920=ADVANCED_FACE('',(#20490),#2600,.F.);
#75921=ADVANCED_FACE('',(#20491),#2601,.T.);
#75922=ADVANCED_FACE('',(#20492),#2602,.T.);
#75923=ADVANCED_FACE('',(#20493),#2603,.T.);
#75924=ADVANCED_FACE('',(#20494),#2604,.F.);
#75925=ADVANCED_FACE('',(#20495),#16914,.T.);
#75926=ADVANCED_FACE('',(#20496),#2605,.T.);
#75927=ADVANCED_FACE('',(#20497),#2606,.F.);
#75928=ADVANCED_FACE('',(#20498),#1874,.F.);
#75929=ADVANCED_FACE('',(#20499),#2146,.F.);
#75930=ADVANCED_FACE('',(#20500),#2607,.T.);
#75931=ADVANCED_FACE('',(#20501),#2147,.F.);
#75932=ADVANCED_FACE('',(#20502),#2608,.T.);
#75933=ADVANCED_FACE('',(#20503),#1875,.F.);
#75934=ADVANCED_FACE('',(#20504),#1876,.F.);
#75935=ADVANCED_FACE('',(#20505),#2609,.F.);
#75936=ADVANCED_FACE('',(#20506),#2610,.F.);
#75937=ADVANCED_FACE('',(#20507),#2611,.F.);
#75938=ADVANCED_FACE('',(#20508),#2612,.F.);
#75939=ADVANCED_FACE('',(#20509),#2148,.F.);
#75940=ADVANCED_FACE('',(#20510),#2613,.T.);
#75941=ADVANCED_FACE('',(#20511),#2614,.T.);
#75942=ADVANCED_FACE('',(#20512),#1877,.T.);
#75943=ADVANCED_FACE('',(#20513),#16915,.T.);
#75944=ADVANCED_FACE('',(#20514),#2149,.T.);
#75945=ADVANCED_FACE('',(#20515),#1878,.T.);
#75946=ADVANCED_FACE('',(#20516),#2150,.T.);
#75947=ADVANCED_FACE('',(#20517),#2151,.T.);
#75948=ADVANCED_FACE('',(#20518),#2152,.F.);
#75949=ADVANCED_FACE('',(#20519),#2153,.F.);
#75950=ADVANCED_FACE('',(#20520),#1924,.F.);
#75951=ADVANCED_FACE('',(#20521),#1879,.F.);
#75952=ADVANCED_FACE('',(#20522),#1880,.F.);
#75953=ADVANCED_FACE('',(#20523),#1881,.F.);
#75954=ADVANCED_FACE('',(#20524),#2154,.F.);
#75955=ADVANCED_FACE('',(#20525),#16916,.F.);
#75956=ADVANCED_FACE('',(#20526),#2155,.T.);
#75957=ADVANCED_FACE('',(#20527),#16917,.F.);
#75958=ADVANCED_FACE('',(#20528),#2156,.F.);
#75959=ADVANCED_FACE('',(#20529),#16918,.F.);
#75960=ADVANCED_FACE('',(#20530),#16919,.T.);
#75961=ADVANCED_FACE('',(#20531),#2157,.T.);
#75962=ADVANCED_FACE('',(#20532),#16920,.T.);
#75963=ADVANCED_FACE('',(#20533),#2158,.F.);
#75964=ADVANCED_FACE('',(#20534),#16921,.T.);
#75965=ADVANCED_FACE('',(#20535),#16922,.T.);
#75966=ADVANCED_FACE('',(#20536),#1925,.T.);
#75967=ADVANCED_FACE('',(#20537),#16923,.T.);
#75968=ADVANCED_FACE('',(#20538),#1926,.T.);
#75969=ADVANCED_FACE('',(#20539),#16924,.T.);
#75970=ADVANCED_FACE('',(#20540),#2159,.F.);
#75971=ADVANCED_FACE('',(#20541),#1882,.F.);
#75972=ADVANCED_FACE('',(#20542),#2160,.F.);
#75973=ADVANCED_FACE('',(#20543),#1883,.F.);
#75974=ADVANCED_FACE('',(#20544),#2161,.F.);
#75975=ADVANCED_FACE('',(#20545),#1884,.F.);
#75976=ADVANCED_FACE('',(#20546),#1927,.T.);
#75977=ADVANCED_FACE('',(#20547),#16925,.T.);
#75978=ADVANCED_FACE('',(#20548),#2162,.F.);
#75979=ADVANCED_FACE('',(#20549),#2615,.F.);
#75980=ADVANCED_FACE('',(#20550),#1928,.F.);
#75981=ADVANCED_FACE('',(#20551),#176,.F.);
#75982=ADVANCED_FACE('',(#20552),#177,.F.);
#75983=ADVANCED_FACE('',(#20553),#1929,.T.);
#75984=ADVANCED_FACE('',(#20554,#269),#16926,.T.);
#75985=ADVANCED_FACE('',(#20555),#1930,.T.);
#75986=ADVANCED_FACE('',(#20556),#2163,.F.);
#75987=ADVANCED_FACE('',(#20557),#2616,.F.);
#75988=ADVANCED_FACE('',(#20558),#2164,.F.);
#75989=ADVANCED_FACE('',(#20559),#1885,.F.);
#75990=ADVANCED_FACE('',(#20560),#1931,.T.);
#75991=ADVANCED_FACE('',(#20561),#16927,.T.);
#75992=ADVANCED_FACE('',(#20562),#1932,.F.);
#75993=ADVANCED_FACE('',(#20563),#16928,.F.);
#75994=ADVANCED_FACE('',(#20564,#270),#16929,.T.);
#75995=ADVANCED_FACE('',(#20565),#16930,.T.);
#75996=ADVANCED_FACE('',(#20566),#16931,.T.);
#75997=ADVANCED_FACE('',(#20567),#16932,.T.);
#75998=ADVANCED_FACE('',(#20568),#16933,.T.);
#75999=ADVANCED_FACE('',(#20569,#271),#16934,.T.);
#76000=ADVANCED_FACE('',(#20570),#16935,.T.);
#76001=ADVANCED_FACE('',(#20571),#16936,.T.);
#76002=ADVANCED_FACE('',(#20572),#16937,.T.);
#76003=ADVANCED_FACE('',(#20573,#272),#16938,.F.);
#76004=ADVANCED_FACE('',(#20574),#16939,.F.);
#76005=ADVANCED_FACE('',(#20575),#16940,.F.);
#76006=ADVANCED_FACE('',(#20576),#16941,.F.);
#76007=ADVANCED_FACE('',(#20577),#2617,.T.);
#76008=ADVANCED_FACE('',(#20578),#178,.F.);
#76009=ADVANCED_FACE('',(#20579),#2618,.T.);
#76010=ADVANCED_FACE('',(#20580),#2619,.F.);
#76011=ADVANCED_FACE('',(#20581),#2165,.T.);
#76012=ADVANCED_FACE('',(#20582),#2620,.F.);
#76013=ADVANCED_FACE('',(#20583),#2166,.T.);
#76014=ADVANCED_FACE('',(#20584),#2621,.T.);
#76015=ADVANCED_FACE('',(#20585),#2622,.T.);
#76016=ADVANCED_FACE('',(#20586),#2623,.T.);
#76017=ADVANCED_FACE('',(#20587),#2624,.T.);
#76018=ADVANCED_FACE('',(#20588),#2167,.T.);
#76019=ADVANCED_FACE('',(#20589),#2625,.F.);
#76020=ADVANCED_FACE('',(#20590),#2626,.F.);
#76021=ADVANCED_FACE('',(#20591),#2627,.F.);
#76022=ADVANCED_FACE('',(#20592),#2628,.F.);
#76023=ADVANCED_FACE('',(#20593),#2168,.T.);
#76024=ADVANCED_FACE('',(#20594),#2169,.T.);
#76025=ADVANCED_FACE('',(#20595),#2629,.F.);
#76026=ADVANCED_FACE('',(#20596),#2630,.F.);
#76027=ADVANCED_FACE('',(#20597),#2631,.F.);
#76028=ADVANCED_FACE('',(#20598),#2632,.F.);
#76029=ADVANCED_FACE('',(#20599),#2633,.F.);
#76030=ADVANCED_FACE('',(#20600,#273,#274),#16942,.T.);
#76031=ADVANCED_FACE('',(#20601),#2170,.T.);
#76032=ADVANCED_FACE('',(#20602),#2171,.T.);
#76033=ADVANCED_FACE('',(#20603),#2172,.T.);
#76034=ADVANCED_FACE('',(#20604),#2173,.T.);
#76035=ADVANCED_FACE('',(#20605),#2174,.T.);
#76036=ADVANCED_FACE('',(#20606),#2175,.T.);
#76037=ADVANCED_FACE('',(#20607),#2176,.T.);
#76038=ADVANCED_FACE('',(#20608),#2177,.T.);
#76039=ADVANCED_FACE('',(#20609),#2178,.T.);
#76040=ADVANCED_FACE('',(#20610),#2179,.T.);
#76041=ADVANCED_FACE('',(#20611),#2180,.T.);
#76042=ADVANCED_FACE('',(#20612),#2181,.T.);
#76043=ADVANCED_FACE('',(#20613),#2182,.T.);
#76044=ADVANCED_FACE('',(#20614),#2183,.T.);
#76045=ADVANCED_FACE('',(#20615),#1933,.T.);
#76046=ADVANCED_FACE('',(#20616),#2184,.T.);
#76047=ADVANCED_FACE('',(#20617),#2185,.T.);
#76048=ADVANCED_FACE('',(#20618),#2186,.T.);
#76049=ADVANCED_FACE('',(#20619),#2187,.T.);
#76050=ADVANCED_FACE('',(#20620),#2188,.T.);
#76051=ADVANCED_FACE('',(#20621),#2189,.T.);
#76052=ADVANCED_FACE('',(#20622),#2190,.T.);
#76053=ADVANCED_FACE('',(#20623),#2191,.T.);
#76054=ADVANCED_FACE('',(#20624),#2192,.T.);
#76055=ADVANCED_FACE('',(#20625),#2193,.T.);
#76056=ADVANCED_FACE('',(#20626),#2194,.T.);
#76057=ADVANCED_FACE('',(#20627),#1934,.F.);
#76058=ADVANCED_FACE('',(#20628),#2195,.T.);
#76059=ADVANCED_FACE('',(#20629),#2196,.T.);
#76060=ADVANCED_FACE('',(#20630),#2197,.T.);
#76061=ADVANCED_FACE('',(#20631),#2198,.T.);
#76062=ADVANCED_FACE('',(#20632),#2199,.T.);
#76063=ADVANCED_FACE('',(#20633),#1935,.T.);
#76064=ADVANCED_FACE('',(#20634),#1936,.T.);
#76065=ADVANCED_FACE('',(#20635),#2200,.F.);
#76066=ADVANCED_FACE('',(#20636),#2201,.F.);
#76067=ADVANCED_FACE('',(#20637),#1886,.T.);
#76068=ADVANCED_FACE('',(#20638),#1887,.T.);
#76069=ADVANCED_FACE('',(#20639),#2202,.F.);
#76070=ADVANCED_FACE('',(#20640),#1937,.T.);
#76071=ADVANCED_FACE('',(#20641),#1938,.T.);
#76072=ADVANCED_FACE('',(#20642),#2203,.T.);
#76073=ADVANCED_FACE('',(#20643),#2204,.T.);
#76074=ADVANCED_FACE('',(#20644),#179,.F.);
#76075=ADVANCED_FACE('',(#20645),#180,.F.);
#76076=ADVANCED_FACE('',(#20646),#181,.F.);
#76077=ADVANCED_FACE('',(#20647),#182,.F.);
#76078=ADVANCED_FACE('',(#20648),#16943,.F.);
#76079=ADVANCED_FACE('',(#20649),#16944,.F.);
#76080=ADVANCED_FACE('',(#20650),#16945,.F.);
#76081=ADVANCED_FACE('',(#20651),#2205,.F.);
#76082=ADVANCED_FACE('',(#20652),#16946,.F.);
#76083=ADVANCED_FACE('',(#20653),#16947,.F.);
#76084=ADVANCED_FACE('',(#20654),#16948,.F.);
#76085=ADVANCED_FACE('',(#20655,#275),#16949,.F.);
#76086=ADVANCED_FACE('',(#20656,#276),#16950,.F.);
#76087=ADVANCED_FACE('',(#20657,#277),#16951,.F.);
#76088=ADVANCED_FACE('',(#20658),#16952,.T.);
#76089=ADVANCED_FACE('',(#20659),#16953,.T.);
#76090=ADVANCED_FACE('',(#20660),#16954,.T.);
#76091=ADVANCED_FACE('',(#20661),#16955,.T.);
#76092=ADVANCED_FACE('',(#20662),#16956,.T.);
#76093=ADVANCED_FACE('',(#20663),#16957,.T.);
#76094=ADVANCED_FACE('',(#20664,#278),#16958,.T.);
#76095=ADVANCED_FACE('',(#20665,#279),#16959,.T.);
#76096=ADVANCED_FACE('',(#20666,#280),#16960,.T.);
#76097=ADVANCED_FACE('',(#20667,#281),#16961,.T.);
#76098=ADVANCED_FACE('',(#20668),#1888,.T.);
#76099=ADVANCED_FACE('',(#20669),#1889,.T.);
#76100=ADVANCED_FACE('',(#20670),#2206,.T.);
#76101=ADVANCED_FACE('',(#20671),#1890,.T.);
#76102=ADVANCED_FACE('',(#20672),#1891,.T.);
#76103=ADVANCED_FACE('',(#20673),#2207,.F.);
#76104=ADVANCED_FACE('',(#20674),#2208,.T.);
#76105=ADVANCED_FACE('',(#20675),#2209,.T.);
#76106=ADVANCED_FACE('',(#20676),#16962,.F.);
#76107=ADVANCED_FACE('',(#20677),#16963,.F.);
#76108=ADVANCED_FACE('',(#20678),#2210,.T.);
#76109=ADVANCED_FACE('',(#20679),#16964,.F.);
#76110=ADVANCED_FACE('',(#20680,#282),#16965,.T.);
#76111=ADVANCED_FACE('',(#20681,#283),#16966,.T.);
#76112=ADVANCED_FACE('',(#20682,#284),#16967,.T.);
#76113=ADVANCED_FACE('',(#20683,#285),#16968,.T.);
#76114=ADVANCED_FACE('',(#20684,#286),#16969,.T.);
#76115=ADVANCED_FACE('',(#20685,#287),#16970,.T.);
#76116=ADVANCED_FACE('',(#20686),#2211,.F.);
#76117=ADVANCED_FACE('',(#20687),#2212,.F.);
#76118=ADVANCED_FACE('',(#20688),#2213,.F.);
#76119=ADVANCED_FACE('',(#20689),#2214,.F.);
#76120=ADVANCED_FACE('',(#20690),#2215,.F.);
#76121=ADVANCED_FACE('',(#20691),#2216,.F.);
#76122=ADVANCED_FACE('',(#20692),#2217,.F.);
#76123=ADVANCED_FACE('',(#20693),#2218,.F.);
#76124=ADVANCED_FACE('',(#20694),#2219,.F.);
#76125=ADVANCED_FACE('',(#20695),#2220,.F.);
#76126=ADVANCED_FACE('',(#20696),#2221,.F.);
#76127=ADVANCED_FACE('',(#20697),#1939,.F.);
#76128=ADVANCED_FACE('',(#20698),#1940,.T.);
#76129=ADVANCED_FACE('',(#20699),#1941,.T.);
#76130=ADVANCED_FACE('',(#20700),#2222,.T.);
#76131=ADVANCED_FACE('',(#20701),#16971,.T.);
#76132=ADVANCED_FACE('',(#20702),#16972,.T.);
#76133=ADVANCED_FACE('',(#20703),#16973,.T.);
#76134=ADVANCED_FACE('',(#20704),#2223,.T.);
#76135=ADVANCED_FACE('',(#20705),#2224,.T.);
#76136=ADVANCED_FACE('',(#20706),#16974,.T.);
#76137=ADVANCED_FACE('',(#20707),#16975,.T.);
#76138=ADVANCED_FACE('',(#20708),#2225,.T.);
#76139=ADVANCED_FACE('',(#20709),#2226,.T.);
#76140=ADVANCED_FACE('',(#20710),#2227,.T.);
#76141=ADVANCED_FACE('',(#20711),#16976,.T.);
#76142=ADVANCED_FACE('',(#20712,#288),#16977,.T.);
#76143=ADVANCED_FACE('',(#20713),#183,.F.);
#76144=ADVANCED_FACE('',(#20714),#184,.F.);
#76145=ADVANCED_FACE('',(#20715),#185,.F.);
#76146=ADVANCED_FACE('',(#20716),#186,.F.);
#76147=ADVANCED_FACE('',(#20717),#187,.F.);
#76148=ADVANCED_FACE('',(#20718),#188,.F.);
#76149=ADVANCED_FACE('',(#20719),#189,.F.);
#76150=ADVANCED_FACE('',(#20720),#190,.F.);
#76151=ADVANCED_FACE('',(#20721,#289),#16978,.F.);
#76152=ADVANCED_FACE('',(#20722,#290),#16979,.F.);
#76153=ADVANCED_FACE('',(#20723),#1892,.T.);
#76154=ADVANCED_FACE('',(#20724),#1893,.T.);
#76155=ADVANCED_FACE('',(#20725),#2228,.T.);
#76156=ADVANCED_FACE('',(#20726),#1894,.T.);
#76157=ADVANCED_FACE('',(#20727),#1895,.T.);
#76158=ADVANCED_FACE('',(#20728),#2229,.F.);
#76159=ADVANCED_FACE('',(#20729),#2230,.T.);
#76160=ADVANCED_FACE('',(#20730),#2231,.T.);
#76161=ADVANCED_FACE('',(#20731),#16980,.F.);
#76162=ADVANCED_FACE('',(#20732),#16981,.F.);
#76163=ADVANCED_FACE('',(#20733),#2232,.T.);
#76164=ADVANCED_FACE('',(#20734),#16982,.F.);
#76165=ADVANCED_FACE('',(#20735,#291),#16983,.T.);
#76166=ADVANCED_FACE('',(#20736,#292),#16984,.T.);
#76167=ADVANCED_FACE('',(#20737,#293),#16985,.T.);
#76168=ADVANCED_FACE('',(#20738,#294),#16986,.T.);
#76169=ADVANCED_FACE('',(#20739,#295),#16987,.T.);
#76170=ADVANCED_FACE('',(#20740,#296),#16988,.T.);
#76171=ADVANCED_FACE('',(#20741),#1896,.T.);
#76172=ADVANCED_FACE('',(#20742),#2233,.T.);
#76173=ADVANCED_FACE('',(#20743),#2234,.F.);
#76174=ADVANCED_FACE('',(#20744),#2235,.F.);
#76175=ADVANCED_FACE('',(#20745),#1897,.F.);
#76176=ADVANCED_FACE('',(#20746),#2236,.F.);
#76177=ADVANCED_FACE('',(#20747),#1942,.T.);
#76178=ADVANCED_FACE('',(#20748,#297),#16989,.F.);
#76179=ADVANCED_FACE('',(#20749,#298),#16990,.F.);
#76180=ADVANCED_FACE('',(#20750,#299),#16991,.T.);
#76181=ADVANCED_FACE('',(#20751),#1943,.F.);
#76182=ADVANCED_FACE('',(#20752,#300),#16992,.T.);
#76183=ADVANCED_FACE('',(#20753,#301),#16993,.F.);
#76184=ADVANCED_FACE('',(#20754),#2237,.F.);
#76185=ADVANCED_FACE('',(#20755),#2238,.F.);
#76186=ADVANCED_FACE('',(#20756),#2239,.F.);
#76187=ADVANCED_FACE('',(#20757),#2240,.F.);
#76188=ADVANCED_FACE('',(#20758),#2241,.F.);
#76189=ADVANCED_FACE('',(#20759),#2242,.F.);
#76190=ADVANCED_FACE('',(#20760),#2243,.F.);
#76191=ADVANCED_FACE('',(#20761),#2244,.F.);
#76192=ADVANCED_FACE('',(#20762),#2245,.F.);
#76193=ADVANCED_FACE('',(#20763),#2246,.F.);
#76194=ADVANCED_FACE('',(#20764),#2247,.F.);
#76195=ADVANCED_FACE('',(#20765),#1944,.F.);
#76196=ADVANCED_FACE('',(#20766),#1945,.T.);
#76197=ADVANCED_FACE('',(#20767),#1946,.T.);
#76198=ADVANCED_FACE('',(#20768),#2248,.T.);
#76199=ADVANCED_FACE('',(#20769),#16994,.T.);
#76200=ADVANCED_FACE('',(#20770),#16995,.T.);
#76201=ADVANCED_FACE('',(#20771),#16996,.T.);
#76202=ADVANCED_FACE('',(#20772),#2249,.T.);
#76203=ADVANCED_FACE('',(#20773),#2250,.T.);
#76204=ADVANCED_FACE('',(#20774),#16997,.T.);
#76205=ADVANCED_FACE('',(#20775),#16998,.T.);
#76206=ADVANCED_FACE('',(#20776),#2251,.T.);
#76207=ADVANCED_FACE('',(#20777),#2252,.T.);
#76208=ADVANCED_FACE('',(#20778),#2253,.T.);
#76209=ADVANCED_FACE('',(#20779),#16999,.T.);
#76210=ADVANCED_FACE('',(#20780,#302),#17000,.T.);
#76211=ADVANCED_FACE('',(#20781),#191,.F.);
#76212=ADVANCED_FACE('',(#20782),#192,.F.);
#76213=ADVANCED_FACE('',(#20783),#193,.F.);
#76214=ADVANCED_FACE('',(#20784),#194,.F.);
#76215=ADVANCED_FACE('',(#20785),#195,.F.);
#76216=ADVANCED_FACE('',(#20786),#196,.F.);
#76217=ADVANCED_FACE('',(#20787),#197,.F.);
#76218=ADVANCED_FACE('',(#20788),#198,.F.);
#76219=ADVANCED_FACE('',(#20789,#303),#17001,.F.);
#76220=ADVANCED_FACE('',(#20790,#304),#17002,.F.);
#76221=ADVANCED_FACE('',(#20791),#2254,.F.);
#76222=ADVANCED_FACE('',(#20792),#1947,.F.);
#76223=ADVANCED_FACE('',(#20793),#17003,.T.);
#76224=ADVANCED_FACE('',(#20794),#2255,.T.);
#76225=ADVANCED_FACE('',(#20795),#2256,.T.);
#76226=ADVANCED_FACE('',(#20796),#2257,.T.);
#76227=ADVANCED_FACE('',(#20797),#1948,.T.);
#76228=ADVANCED_FACE('',(#20798),#2258,.T.);
#76229=ADVANCED_FACE('',(#20799),#2259,.T.);
#76230=ADVANCED_FACE('',(#20800),#2260,.T.);
#76231=ADVANCED_FACE('',(#20801),#1949,.T.);
#76232=ADVANCED_FACE('',(#20802),#2261,.T.);
#76233=ADVANCED_FACE('',(#20803),#2262,.T.);
#76234=ADVANCED_FACE('',(#20804),#1950,.T.);
#76235=ADVANCED_FACE('',(#20805),#2263,.F.);
#76236=ADVANCED_FACE('',(#20806),#2264,.F.);
#76237=ADVANCED_FACE('',(#20807),#1951,.F.);
#76238=ADVANCED_FACE('',(#20808),#1952,.F.);
#76239=ADVANCED_FACE('',(#20809),#1953,.T.);
#76240=ADVANCED_FACE('',(#20810),#1954,.F.);
#76241=ADVANCED_FACE('',(#20811),#2265,.T.);
#76242=ADVANCED_FACE('',(#20812),#2266,.T.);
#76243=ADVANCED_FACE('',(#20813),#1898,.T.);
#76244=ADVANCED_FACE('',(#20814),#2267,.T.);
#76245=ADVANCED_FACE('',(#20815),#2268,.T.);
#76246=ADVANCED_FACE('',(#20816),#2269,.T.);
#76247=ADVANCED_FACE('',(#20817),#1899,.T.);
#76248=ADVANCED_FACE('',(#20818),#1900,.T.);
#76249=ADVANCED_FACE('',(#20819),#1901,.F.);
#76250=ADVANCED_FACE('',(#20820),#2270,.F.);
#76251=ADVANCED_FACE('',(#20821),#1902,.F.);
#76252=ADVANCED_FACE('',(#20822),#2271,.T.);
#76253=ADVANCED_FACE('',(#20823,#305),#2272,.T.);
#76254=ADVANCED_FACE('',(#20824,#306),#17004,.T.);
#76255=ADVANCED_FACE('',(#20825,#307),#17005,.F.);
#76256=ADVANCED_FACE('',(#20826),#17006,.T.);
#76257=ADVANCED_FACE('',(#20827,#308),#17007,.T.);
#76258=ADVANCED_FACE('',(#20828),#17008,.T.);
#76259=ADVANCED_FACE('',(#20829,#309),#17009,.T.);
#76260=ADVANCED_FACE('',(#20830),#199,.F.);
#76261=ADVANCED_FACE('',(#20831),#200,.F.);
#76262=ADVANCED_FACE('',(#20832),#17010,.F.);
#76263=ADVANCED_FACE('',(#20833),#17011,.T.);
#76264=ADVANCED_FACE('',(#20834),#17012,.F.);
#76265=ADVANCED_FACE('',(#20835),#17013,.T.);
#76266=ADVANCED_FACE('',(#20836,#310),#17014,.F.);
#76267=ADVANCED_FACE('',(#20837,#311),#17015,.T.);
#76268=ADVANCED_FACE('',(#20838,#312),#17016,.T.);
#76269=ADVANCED_FACE('',(#20839),#1955,.T.);
#76270=ADVANCED_FACE('',(#20840,#313),#17017,.T.);
#76271=ADVANCED_FACE('',(#20841),#1903,.T.);
#76272=ADVANCED_FACE('',(#20842),#2273,.T.);
#76273=ADVANCED_FACE('',(#20843),#2274,.F.);
#76274=ADVANCED_FACE('',(#20844),#2275,.F.);
#76275=ADVANCED_FACE('',(#20845),#1904,.F.);
#76276=ADVANCED_FACE('',(#20846),#2276,.F.);
#76277=ADVANCED_FACE('',(#20847),#1956,.T.);
#76278=ADVANCED_FACE('',(#20848,#314),#17018,.F.);
#76279=ADVANCED_FACE('',(#20849,#315),#17019,.F.);
#76280=ADVANCED_FACE('',(#20850,#316),#17020,.T.);
#76281=ADVANCED_FACE('',(#20851),#1957,.F.);
#76282=ADVANCED_FACE('',(#20852,#317),#17021,.T.);
#76283=ADVANCED_FACE('',(#20853,#318),#17022,.F.);
#76284=ADVANCED_FACE('',(#20854),#2277,.T.);
#76285=ADVANCED_FACE('',(#20855),#2278,.T.);
#76286=ADVANCED_FACE('',(#20856),#2279,.T.);
#76287=ADVANCED_FACE('',(#20857),#2280,.T.);
#76288=ADVANCED_FACE('',(#20858),#1958,.F.);
#76289=ADVANCED_FACE('',(#20859),#1905,.F.);
#76290=ADVANCED_FACE('',(#20860),#1906,.T.);
#76291=ADVANCED_FACE('',(#20861),#2281,.F.);
#76292=ADVANCED_FACE('',(#20862),#2282,.F.);
#76293=ADVANCED_FACE('',(#20863,#319,#320,#321),#2283,.F.);
#76294=ADVANCED_FACE('',(#20864),#2284,.F.);
#76295=ADVANCED_FACE('',(#20865),#2285,.F.);
#76296=ADVANCED_FACE('',(#20866,#322,#323,#324),#2286,.T.);
#76297=ADVANCED_FACE('',(#20867),#1907,.T.);
#76298=ADVANCED_FACE('',(#20868),#2287,.F.);
#76299=ADVANCED_FACE('',(#20869),#2288,.T.);
#76300=ADVANCED_FACE('',(#20870),#1908,.F.);
#76301=ADVANCED_FACE('',(#20871),#1909,.T.);
#76302=ADVANCED_FACE('',(#20872),#1959,.T.);
#76303=ADVANCED_FACE('',(#20873),#2289,.F.);
#76304=ADVANCED_FACE('',(#20874),#2290,.F.);
#76305=ADVANCED_FACE('',(#20875),#2291,.T.);
#76306=ADVANCED_FACE('',(#20876),#2292,.T.);
#76307=ADVANCED_FACE('',(#20877),#1960,.T.);
#76308=ADVANCED_FACE('',(#20878),#2293,.F.);
#76309=ADVANCED_FACE('',(#20879),#201,.F.);
#76310=ADVANCED_FACE('',(#20880),#202,.F.);
#76311=ADVANCED_FACE('',(#20881),#203,.F.);
#76312=ADVANCED_FACE('',(#20882),#17023,.F.);
#76313=ADVANCED_FACE('',(#20883),#1961,.T.);
#76314=ADVANCED_FACE('',(#20884),#1962,.T.);
#76315=ADVANCED_FACE('',(#20885),#17024,.F.);
#76316=ADVANCED_FACE('',(#20886),#17025,.T.);
#76317=ADVANCED_FACE('',(#20887),#17026,.T.);
#76318=ADVANCED_FACE('',(#20888,#325),#17027,.F.);
#76319=ADVANCED_FACE('',(#20889,#326),#17028,.T.);
#76320=ADVANCED_FACE('',(#20890),#204,.F.);
#76321=ADVANCED_FACE('',(#20891),#2294,.T.);
#76322=ADVANCED_FACE('',(#20892),#205,.F.);
#76323=ADVANCED_FACE('',(#20893),#206,.F.);
#76324=ADVANCED_FACE('',(#20894,#327),#17029,.F.);
#76325=ADVANCED_FACE('',(#20895,#328),#17030,.F.);
#76326=ADVANCED_FACE('',(#20896,#329),#17031,.T.);
#76327=ADVANCED_FACE('',(#20897),#17032,.F.);
#76328=ADVANCED_FACE('',(#20898),#17033,.F.);
#76329=ADVANCED_FACE('',(#20899),#17034,.F.);
#76330=ADVANCED_FACE('',(#20900),#17035,.F.);
#76331=ADVANCED_FACE('',(#20901),#17036,.T.);
#76332=ADVANCED_FACE('',(#20902),#17037,.F.);
#76333=ADVANCED_FACE('',(#20903),#17038,.F.);
#76334=ADVANCED_FACE('',(#20904),#17039,.F.);
#76335=ADVANCED_FACE('',(#20905),#17040,.F.);
#76336=ADVANCED_FACE('',(#20906),#17041,.T.);
#76337=ADVANCED_FACE('',(#20907),#17042,.F.);
#76338=ADVANCED_FACE('',(#20908),#17043,.F.);
#76339=ADVANCED_FACE('',(#20909),#17044,.F.);
#76340=ADVANCED_FACE('',(#20910),#17045,.F.);
#76341=ADVANCED_FACE('',(#20911),#17046,.T.);
#76342=ADVANCED_FACE('',(#20912),#17047,.F.);
#76343=ADVANCED_FACE('',(#20913),#17048,.F.);
#76344=ADVANCED_FACE('',(#20914),#17049,.F.);
#76345=ADVANCED_FACE('',(#20915),#17050,.F.);
#76346=ADVANCED_FACE('',(#20916),#17051,.F.);
#76347=ADVANCED_FACE('',(#20917),#17052,.F.);
#76348=ADVANCED_FACE('',(#20918),#17053,.F.);
#76349=ADVANCED_FACE('',(#20919),#17054,.F.);
#76350=ADVANCED_FACE('',(#20920),#17055,.F.);
#76351=ADVANCED_FACE('',(#20921),#17056,.F.);
#76352=ADVANCED_FACE('',(#20922),#17057,.F.);
#76353=ADVANCED_FACE('',(#20923),#17058,.F.);
#76354=ADVANCED_FACE('',(#20924),#17059,.F.);
#76355=ADVANCED_FACE('',(#20925),#17060,.F.);
#76356=ADVANCED_FACE('',(#20926),#17061,.F.);
#76357=ADVANCED_FACE('',(#20927),#17062,.F.);
#76358=ADVANCED_FACE('',(#20928),#17063,.F.);
#76359=ADVANCED_FACE('',(#20929),#17064,.F.);
#76360=ADVANCED_FACE('',(#20930),#17065,.F.);
#76361=ADVANCED_FACE('',(#20931),#17066,.F.);
#76362=ADVANCED_FACE('',(#20932),#17067,.T.);
#76363=ADVANCED_FACE('',(#20933),#17068,.F.);
#76364=ADVANCED_FACE('',(#20934),#17069,.F.);
#76365=ADVANCED_FACE('',(#20935),#17070,.F.);
#76366=ADVANCED_FACE('',(#20936),#17071,.F.);
#76367=ADVANCED_FACE('',(#20937),#17072,.T.);
#76368=ADVANCED_FACE('',(#20938),#17073,.F.);
#76369=ADVANCED_FACE('',(#20939),#17074,.F.);
#76370=ADVANCED_FACE('',(#20940),#17075,.F.);
#76371=ADVANCED_FACE('',(#20941),#17076,.F.);
#76372=ADVANCED_FACE('',(#20942),#17077,.T.);
#76373=ADVANCED_FACE('',(#20943),#17078,.F.);
#76374=ADVANCED_FACE('',(#20944),#17079,.F.);
#76375=ADVANCED_FACE('',(#20945),#17080,.F.);
#76376=ADVANCED_FACE('',(#20946),#17081,.F.);
#76377=ADVANCED_FACE('',(#20947),#17082,.T.);
#76378=ADVANCED_FACE('',(#20948),#17083,.F.);
#76379=ADVANCED_FACE('',(#20949),#17084,.F.);
#76380=ADVANCED_FACE('',(#20950),#17085,.F.);
#76381=ADVANCED_FACE('',(#20951),#17086,.F.);
#76382=ADVANCED_FACE('',(#20952),#17087,.F.);
#76383=ADVANCED_FACE('',(#20953),#17088,.F.);
#76384=ADVANCED_FACE('',(#20954),#17089,.F.);
#76385=ADVANCED_FACE('',(#20955),#17090,.F.);
#76386=ADVANCED_FACE('',(#20956),#17091,.T.);
#76387=ADVANCED_FACE('',(#20957),#17092,.F.);
#76388=ADVANCED_FACE('',(#20958),#17093,.F.);
#76389=ADVANCED_FACE('',(#20959),#17094,.F.);
#76390=ADVANCED_FACE('',(#20960),#17095,.F.);
#76391=ADVANCED_FACE('',(#20961),#17096,.T.);
#76392=ADVANCED_FACE('',(#20962),#17097,.F.);
#76393=ADVANCED_FACE('',(#20963),#17098,.F.);
#76394=ADVANCED_FACE('',(#20964),#17099,.F.);
#76395=ADVANCED_FACE('',(#20965),#17100,.F.);
#76396=ADVANCED_FACE('',(#20966),#17101,.T.);
#76397=ADVANCED_FACE('',(#20967),#17102,.F.);
#76398=ADVANCED_FACE('',(#20968),#17103,.F.);
#76399=ADVANCED_FACE('',(#20969),#17104,.F.);
#76400=ADVANCED_FACE('',(#20970),#17105,.F.);
#76401=ADVANCED_FACE('',(#20971),#17106,.T.);
#76402=ADVANCED_FACE('',(#20972),#17107,.F.);
#76403=ADVANCED_FACE('',(#20973),#17108,.F.);
#76404=ADVANCED_FACE('',(#20974),#17109,.F.);
#76405=ADVANCED_FACE('',(#20975),#17110,.F.);
#76406=ADVANCED_FACE('',(#20976),#17111,.F.);
#76407=ADVANCED_FACE('',(#20977),#17112,.F.);
#76408=ADVANCED_FACE('',(#20978),#17113,.F.);
#76409=ADVANCED_FACE('',(#20979),#17114,.F.);
#76410=ADVANCED_FACE('',(#20980),#17115,.F.);
#76411=ADVANCED_FACE('',(#20981),#17116,.F.);
#76412=ADVANCED_FACE('',(#20982),#17117,.F.);
#76413=ADVANCED_FACE('',(#20983),#17118,.F.);
#76414=ADVANCED_FACE('',(#20984),#17119,.F.);
#76415=ADVANCED_FACE('',(#20985),#17120,.F.);
#76416=ADVANCED_FACE('',(#20986),#17121,.F.);
#76417=ADVANCED_FACE('',(#20987),#17122,.F.);
#76418=ADVANCED_FACE('',(#20988),#17123,.F.);
#76419=ADVANCED_FACE('',(#20989),#17124,.F.);
#76420=ADVANCED_FACE('',(#20990),#17125,.F.);
#76421=ADVANCED_FACE('',(#20991),#17126,.F.);
#76422=ADVANCED_FACE('',(#20992),#17127,.F.);
#76423=ADVANCED_FACE('',(#20993),#17128,.F.);
#76424=ADVANCED_FACE('',(#20994),#17129,.F.);
#76425=ADVANCED_FACE('',(#20995),#17130,.F.);
#76426=ADVANCED_FACE('',(#20996),#17131,.F.);
#76427=ADVANCED_FACE('',(#20997),#17132,.F.);
#76428=ADVANCED_FACE('',(#20998),#17133,.F.);
#76429=ADVANCED_FACE('',(#20999),#17134,.F.);
#76430=ADVANCED_FACE('',(#21000),#17135,.T.);
#76431=ADVANCED_FACE('',(#21001),#17136,.F.);
#76432=ADVANCED_FACE('',(#21002),#17137,.F.);
#76433=ADVANCED_FACE('',(#21003),#17138,.F.);
#76434=ADVANCED_FACE('',(#21004),#17139,.F.);
#76435=ADVANCED_FACE('',(#21005),#17140,.T.);
#76436=ADVANCED_FACE('',(#21006),#17141,.F.);
#76437=ADVANCED_FACE('',(#21007),#17142,.F.);
#76438=ADVANCED_FACE('',(#21008),#17143,.F.);
#76439=ADVANCED_FACE('',(#21009),#17144,.F.);
#76440=ADVANCED_FACE('',(#21010),#17145,.F.);
#76441=ADVANCED_FACE('',(#21011),#17146,.F.);
#76442=ADVANCED_FACE('',(#21012),#17147,.F.);
#76443=ADVANCED_FACE('',(#21013),#17148,.F.);
#76444=ADVANCED_FACE('',(#21014),#17149,.F.);
#76445=ADVANCED_FACE('',(#21015),#17150,.F.);
#76446=ADVANCED_FACE('',(#21016),#17151,.F.);
#76447=ADVANCED_FACE('',(#21017),#17152,.F.);
#76448=ADVANCED_FACE('',(#21018),#17153,.F.);
#76449=ADVANCED_FACE('',(#21019),#17154,.F.);
#76450=ADVANCED_FACE('',(#21020),#17155,.F.);
#76451=ADVANCED_FACE('',(#21021),#17156,.F.);
#76452=ADVANCED_FACE('',(#21022),#17157,.F.);
#76453=ADVANCED_FACE('',(#21023),#17158,.F.);
#76454=ADVANCED_FACE('',(#21024),#17159,.F.);
#76455=ADVANCED_FACE('',(#21025),#17160,.F.);
#76456=ADVANCED_FACE('',(#21026),#17161,.F.);
#76457=ADVANCED_FACE('',(#21027),#17162,.F.);
#76458=ADVANCED_FACE('',(#21028),#17163,.F.);
#76459=ADVANCED_FACE('',(#21029),#17164,.F.);
#76460=ADVANCED_FACE('',(#21030),#17165,.F.);
#76461=ADVANCED_FACE('',(#21031),#17166,.F.);
#76462=ADVANCED_FACE('',(#21032),#17167,.F.);
#76463=ADVANCED_FACE('',(#21033),#17168,.F.);
#76464=ADVANCED_FACE('',(#21034),#17169,.F.);
#76465=ADVANCED_FACE('',(#21035),#17170,.F.);
#76466=ADVANCED_FACE('',(#21036),#17171,.F.);
#76467=ADVANCED_FACE('',(#21037),#17172,.F.);
#76468=ADVANCED_FACE('',(#21038),#17173,.F.);
#76469=ADVANCED_FACE('',(#21039),#17174,.F.);
#76470=ADVANCED_FACE('',(#21040),#17175,.F.);
#76471=ADVANCED_FACE('',(#21041),#17176,.F.);
#76472=ADVANCED_FACE('',(#21042),#17177,.T.);
#76473=ADVANCED_FACE('',(#21043),#17178,.F.);
#76474=ADVANCED_FACE('',(#21044),#17179,.F.);
#76475=ADVANCED_FACE('',(#21045),#17180,.F.);
#76476=ADVANCED_FACE('',(#21046),#17181,.F.);
#76477=ADVANCED_FACE('',(#21047),#17182,.T.);
#76478=ADVANCED_FACE('',(#21048),#17183,.F.);
#76479=ADVANCED_FACE('',(#21049),#17184,.F.);
#76480=ADVANCED_FACE('',(#21050),#17185,.F.);
#76481=ADVANCED_FACE('',(#21051),#17186,.F.);
#76482=ADVANCED_FACE('',(#21052),#17187,.F.);
#76483=ADVANCED_FACE('',(#21053),#17188,.F.);
#76484=ADVANCED_FACE('',(#21054),#17189,.F.);
#76485=ADVANCED_FACE('',(#21055),#17190,.F.);
#76486=ADVANCED_FACE('',(#21056),#17191,.F.);
#76487=ADVANCED_FACE('',(#21057),#17192,.F.);
#76488=ADVANCED_FACE('',(#21058),#17193,.F.);
#76489=ADVANCED_FACE('',(#21059),#17194,.F.);
#76490=ADVANCED_FACE('',(#21060),#17195,.F.);
#76491=ADVANCED_FACE('',(#21061),#17196,.F.);
#76492=ADVANCED_FACE('',(#21062),#17197,.F.);
#76493=ADVANCED_FACE('',(#21063),#17198,.F.);
#76494=ADVANCED_FACE('',(#21064),#17199,.F.);
#76495=ADVANCED_FACE('',(#21065),#17200,.F.);
#76496=ADVANCED_FACE('',(#21066),#17201,.F.);
#76497=ADVANCED_FACE('',(#21067),#17202,.F.);
#76498=ADVANCED_FACE('',(#21068),#17203,.F.);
#76499=ADVANCED_FACE('',(#21069),#17204,.F.);
#76500=ADVANCED_FACE('',(#21070),#17205,.F.);
#76501=ADVANCED_FACE('',(#21071),#17206,.F.);
#76502=ADVANCED_FACE('',(#21072),#17207,.F.);
#76503=ADVANCED_FACE('',(#21073),#17208,.F.);
#76504=ADVANCED_FACE('',(#21074),#17209,.F.);
#76505=ADVANCED_FACE('',(#21075),#17210,.F.);
#76506=ADVANCED_FACE('',(#21076),#17211,.F.);
#76507=ADVANCED_FACE('',(#21077),#17212,.F.);
#76508=ADVANCED_FACE('',(#21078),#17213,.F.);
#76509=ADVANCED_FACE('',(#21079),#17214,.F.);
#76510=ADVANCED_FACE('',(#21080),#17215,.F.);
#76511=ADVANCED_FACE('',(#21081),#17216,.F.);
#76512=ADVANCED_FACE('',(#21082),#17217,.F.);
#76513=ADVANCED_FACE('',(#21083),#17218,.F.);
#76514=ADVANCED_FACE('',(#21084),#17219,.F.);
#76515=ADVANCED_FACE('',(#21085),#17220,.F.);
#76516=ADVANCED_FACE('',(#21086),#17221,.F.);
#76517=ADVANCED_FACE('',(#21087),#17222,.F.);
#76518=ADVANCED_FACE('',(#21088),#17223,.T.);
#76519=ADVANCED_FACE('',(#21089),#17224,.F.);
#76520=ADVANCED_FACE('',(#21090),#17225,.F.);
#76521=ADVANCED_FACE('',(#21091),#17226,.F.);
#76522=ADVANCED_FACE('',(#21092),#17227,.F.);
#76523=ADVANCED_FACE('',(#21093),#17228,.F.);
#76524=ADVANCED_FACE('',(#21094),#17229,.F.);
#76525=ADVANCED_FACE('',(#21095),#17230,.F.);
#76526=ADVANCED_FACE('',(#21096),#17231,.F.);
#76527=ADVANCED_FACE('',(#21097),#17232,.F.);
#76528=ADVANCED_FACE('',(#21098),#17233,.F.);
#76529=ADVANCED_FACE('',(#21099),#17234,.F.);
#76530=ADVANCED_FACE('',(#21100),#17235,.F.);
#76531=ADVANCED_FACE('',(#21101),#17236,.F.);
#76532=ADVANCED_FACE('',(#21102),#17237,.F.);
#76533=ADVANCED_FACE('',(#21103),#17238,.F.);
#76534=ADVANCED_FACE('',(#21104),#17239,.F.);
#76535=ADVANCED_FACE('',(#21105),#17240,.F.);
#76536=ADVANCED_FACE('',(#21106),#17241,.F.);
#76537=ADVANCED_FACE('',(#21107),#17242,.F.);
#76538=ADVANCED_FACE('',(#21108),#17243,.F.);
#76539=ADVANCED_FACE('',(#21109),#17244,.F.);
#76540=ADVANCED_FACE('',(#21110),#17245,.F.);
#76541=ADVANCED_FACE('',(#21111),#17246,.F.);
#76542=ADVANCED_FACE('',(#21112),#17247,.F.);
#76543=ADVANCED_FACE('',(#21113),#17248,.F.);
#76544=ADVANCED_FACE('',(#21114),#17249,.F.);
#76545=ADVANCED_FACE('',(#21115),#17250,.F.);
#76546=ADVANCED_FACE('',(#21116),#17251,.F.);
#76547=ADVANCED_FACE('',(#21117),#17252,.F.);
#76548=ADVANCED_FACE('',(#21118),#17253,.F.);
#76549=ADVANCED_FACE('',(#21119),#17254,.F.);
#76550=ADVANCED_FACE('',(#21120),#17255,.F.);
#76551=ADVANCED_FACE('',(#21121),#17256,.F.);
#76552=ADVANCED_FACE('',(#21122),#17257,.F.);
#76553=ADVANCED_FACE('',(#21123),#17258,.F.);
#76554=ADVANCED_FACE('',(#21124),#17259,.F.);
#76555=ADVANCED_FACE('',(#21125),#17260,.F.);
#76556=ADVANCED_FACE('',(#21126),#17261,.F.);
#76557=ADVANCED_FACE('',(#21127),#17262,.F.);
#76558=ADVANCED_FACE('',(#21128),#17263,.F.);
#76559=ADVANCED_FACE('',(#21129),#17264,.F.);
#76560=ADVANCED_FACE('',(#21130),#17265,.F.);
#76561=ADVANCED_FACE('',(#21131),#17266,.F.);
#76562=ADVANCED_FACE('',(#21132),#17267,.F.);
#76563=ADVANCED_FACE('',(#21133),#17268,.F.);
#76564=ADVANCED_FACE('',(#21134),#17269,.F.);
#76565=ADVANCED_FACE('',(#21135),#17270,.F.);
#76566=ADVANCED_FACE('',(#21136),#17271,.F.);
#76567=ADVANCED_FACE('',(#21137),#17272,.T.);
#76568=ADVANCED_FACE('',(#21138),#17273,.F.);
#76569=ADVANCED_FACE('',(#21139),#17274,.F.);
#76570=ADVANCED_FACE('',(#21140),#17275,.F.);
#76571=ADVANCED_FACE('',(#21141),#17276,.F.);
#76572=ADVANCED_FACE('',(#21142),#17277,.T.);
#76573=ADVANCED_FACE('',(#21143),#17278,.F.);
#76574=ADVANCED_FACE('',(#21144),#17279,.F.);
#76575=ADVANCED_FACE('',(#21145),#17280,.F.);
#76576=ADVANCED_FACE('',(#21146),#17281,.F.);
#76577=ADVANCED_FACE('',(#21147),#17282,.F.);
#76578=ADVANCED_FACE('',(#21148),#17283,.F.);
#76579=ADVANCED_FACE('',(#21149),#17284,.F.);
#76580=ADVANCED_FACE('',(#21150),#17285,.F.);
#76581=ADVANCED_FACE('',(#21151),#17286,.F.);
#76582=ADVANCED_FACE('',(#21152),#17287,.F.);
#76583=ADVANCED_FACE('',(#21153),#17288,.F.);
#76584=ADVANCED_FACE('',(#21154),#17289,.F.);
#76585=ADVANCED_FACE('',(#21155),#17290,.F.);
#76586=ADVANCED_FACE('',(#21156),#17291,.F.);
#76587=ADVANCED_FACE('',(#21157),#17292,.F.);
#76588=ADVANCED_FACE('',(#21158),#17293,.F.);
#76589=ADVANCED_FACE('',(#21159),#17294,.F.);
#76590=ADVANCED_FACE('',(#21160),#17295,.F.);
#76591=ADVANCED_FACE('',(#21161),#17296,.F.);
#76592=ADVANCED_FACE('',(#21162),#17297,.F.);
#76593=ADVANCED_FACE('',(#21163),#17298,.F.);
#76594=ADVANCED_FACE('',(#21164),#17299,.F.);
#76595=ADVANCED_FACE('',(#21165),#17300,.F.);
#76596=ADVANCED_FACE('',(#21166),#17301,.F.);
#76597=ADVANCED_FACE('',(#21167),#17302,.F.);
#76598=ADVANCED_FACE('',(#21168),#17303,.F.);
#76599=ADVANCED_FACE('',(#21169),#17304,.F.);
#76600=ADVANCED_FACE('',(#21170),#17305,.F.);
#76601=ADVANCED_FACE('',(#21171),#17306,.F.);
#76602=ADVANCED_FACE('',(#21172),#17307,.F.);
#76603=ADVANCED_FACE('',(#21173),#17308,.F.);
#76604=ADVANCED_FACE('',(#21174),#17309,.F.);
#76605=ADVANCED_FACE('',(#21175),#17310,.F.);
#76606=ADVANCED_FACE('',(#21176),#17311,.F.);
#76607=ADVANCED_FACE('',(#21177),#17312,.F.);
#76608=ADVANCED_FACE('',(#21178),#17313,.F.);
#76609=ADVANCED_FACE('',(#21179),#17314,.F.);
#76610=ADVANCED_FACE('',(#21180),#17315,.F.);
#76611=ADVANCED_FACE('',(#21181),#17316,.F.);
#76612=ADVANCED_FACE('',(#21182),#17317,.F.);
#76613=ADVANCED_FACE('',(#21183),#17318,.F.);
#76614=ADVANCED_FACE('',(#21184),#17319,.F.);
#76615=ADVANCED_FACE('',(#21185),#17320,.F.);
#76616=ADVANCED_FACE('',(#21186),#17321,.F.);
#76617=ADVANCED_FACE('',(#21187),#17322,.F.);
#76618=ADVANCED_FACE('',(#21188),#17323,.F.);
#76619=ADVANCED_FACE('',(#21189),#17324,.F.);
#76620=ADVANCED_FACE('',(#21190),#17325,.F.);
#76621=ADVANCED_FACE('',(#21191),#17326,.F.);
#76622=ADVANCED_FACE('',(#21192),#17327,.F.);
#76623=ADVANCED_FACE('',(#21193),#17328,.F.);
#76624=ADVANCED_FACE('',(#21194),#17329,.F.);
#76625=ADVANCED_FACE('',(#21195),#17330,.F.);
#76626=ADVANCED_FACE('',(#21196),#17331,.F.);
#76627=ADVANCED_FACE('',(#21197),#17332,.F.);
#76628=ADVANCED_FACE('',(#21198),#17333,.F.);
#76629=ADVANCED_FACE('',(#21199),#17334,.F.);
#76630=ADVANCED_FACE('',(#21200),#17335,.F.);
#76631=ADVANCED_FACE('',(#21201),#17336,.F.);
#76632=ADVANCED_FACE('',(#21202),#17337,.F.);
#76633=ADVANCED_FACE('',(#21203),#17338,.F.);
#76634=ADVANCED_FACE('',(#21204),#17339,.F.);
#76635=ADVANCED_FACE('',(#21205),#17340,.F.);
#76636=ADVANCED_FACE('',(#21206),#17341,.F.);
#76637=ADVANCED_FACE('',(#21207),#17342,.F.);
#76638=ADVANCED_FACE('',(#21208),#17343,.F.);
#76639=ADVANCED_FACE('',(#21209),#17344,.F.);
#76640=ADVANCED_FACE('',(#21210),#17345,.F.);
#76641=ADVANCED_FACE('',(#21211),#17346,.F.);
#76642=ADVANCED_FACE('',(#21212),#17347,.F.);
#76643=ADVANCED_FACE('',(#21213),#17348,.F.);
#76644=ADVANCED_FACE('',(#21214),#17349,.F.);
#76645=ADVANCED_FACE('',(#21215),#17350,.F.);
#76646=ADVANCED_FACE('',(#21216),#17351,.F.);
#76647=ADVANCED_FACE('',(#21217),#17352,.F.);
#76648=ADVANCED_FACE('',(#21218),#17353,.F.);
#76649=ADVANCED_FACE('',(#21219),#17354,.F.);
#76650=ADVANCED_FACE('',(#21220),#17355,.F.);
#76651=ADVANCED_FACE('',(#21221),#17356,.F.);
#76652=ADVANCED_FACE('',(#21222),#17357,.F.);
#76653=ADVANCED_FACE('',(#21223),#17358,.F.);
#76654=ADVANCED_FACE('',(#21224),#17359,.F.);
#76655=ADVANCED_FACE('',(#21225),#17360,.F.);
#76656=ADVANCED_FACE('',(#21226),#17361,.F.);
#76657=ADVANCED_FACE('',(#21227),#17362,.F.);
#76658=ADVANCED_FACE('',(#21228),#17363,.F.);
#76659=ADVANCED_FACE('',(#21229),#17364,.F.);
#76660=ADVANCED_FACE('',(#21230),#17365,.F.);
#76661=ADVANCED_FACE('',(#21231),#17366,.F.);
#76662=ADVANCED_FACE('',(#21232),#17367,.F.);
#76663=ADVANCED_FACE('',(#21233),#17368,.F.);
#76664=ADVANCED_FACE('',(#21234),#17369,.F.);
#76665=ADVANCED_FACE('',(#21235),#17370,.F.);
#76666=ADVANCED_FACE('',(#21236),#17371,.F.);
#76667=ADVANCED_FACE('',(#21237),#17372,.F.);
#76668=ADVANCED_FACE('',(#21238),#17373,.F.);
#76669=ADVANCED_FACE('',(#21239),#17374,.F.);
#76670=ADVANCED_FACE('',(#21240),#17375,.F.);
#76671=ADVANCED_FACE('',(#21241),#17376,.F.);
#76672=ADVANCED_FACE('',(#21242),#17377,.F.);
#76673=ADVANCED_FACE('',(#21243),#17378,.F.);
#76674=ADVANCED_FACE('',(#21244),#17379,.F.);
#76675=ADVANCED_FACE('',(#21245),#17380,.F.);
#76676=ADVANCED_FACE('',(#21246),#17381,.F.);
#76677=ADVANCED_FACE('',(#21247),#17382,.F.);
#76678=ADVANCED_FACE('',(#21248),#17383,.F.);
#76679=ADVANCED_FACE('',(#21249),#17384,.F.);
#76680=ADVANCED_FACE('',(#21250),#17385,.F.);
#76681=ADVANCED_FACE('',(#21251),#17386,.F.);
#76682=ADVANCED_FACE('',(#21252),#17387,.F.);
#76683=ADVANCED_FACE('',(#21253),#17388,.F.);
#76684=ADVANCED_FACE('',(#21254),#17389,.F.);
#76685=ADVANCED_FACE('',(#21255),#17390,.F.);
#76686=ADVANCED_FACE('',(#21256),#17391,.F.);
#76687=ADVANCED_FACE('',(#21257),#17392,.F.);
#76688=ADVANCED_FACE('',(#21258),#17393,.F.);
#76689=ADVANCED_FACE('',(#21259),#17394,.F.);
#76690=ADVANCED_FACE('',(#21260),#17395,.F.);
#76691=ADVANCED_FACE('',(#21261),#17396,.F.);
#76692=ADVANCED_FACE('',(#21262),#17397,.F.);
#76693=ADVANCED_FACE('',(#21263),#17398,.F.);
#76694=ADVANCED_FACE('',(#21264),#17399,.F.);
#76695=ADVANCED_FACE('',(#21265),#17400,.F.);
#76696=ADVANCED_FACE('',(#21266),#17401,.F.);
#76697=ADVANCED_FACE('',(#21267),#17402,.F.);
#76698=ADVANCED_FACE('',(#21268),#17403,.F.);
#76699=ADVANCED_FACE('',(#21269),#17404,.F.);
#76700=ADVANCED_FACE('',(#21270),#17405,.F.);
#76701=ADVANCED_FACE('',(#21271),#17406,.F.);
#76702=ADVANCED_FACE('',(#21272),#17407,.F.);
#76703=ADVANCED_FACE('',(#21273),#17408,.F.);
#76704=ADVANCED_FACE('',(#21274),#17409,.F.);
#76705=ADVANCED_FACE('',(#21275),#17410,.F.);
#76706=ADVANCED_FACE('',(#21276),#17411,.F.);
#76707=ADVANCED_FACE('',(#21277),#17412,.F.);
#76708=ADVANCED_FACE('',(#21278),#17413,.F.);
#76709=ADVANCED_FACE('',(#21279),#17414,.F.);
#76710=ADVANCED_FACE('',(#21280),#17415,.F.);
#76711=ADVANCED_FACE('',(#21281),#17416,.F.);
#76712=ADVANCED_FACE('',(#21282),#17417,.F.);
#76713=ADVANCED_FACE('',(#21283),#17418,.F.);
#76714=ADVANCED_FACE('',(#21284),#17419,.F.);
#76715=ADVANCED_FACE('',(#21285),#17420,.F.);
#76716=ADVANCED_FACE('',(#21286),#17421,.F.);
#76717=ADVANCED_FACE('',(#21287),#17422,.F.);
#76718=ADVANCED_FACE('',(#21288),#17423,.F.);
#76719=ADVANCED_FACE('',(#21289),#17424,.F.);
#76720=ADVANCED_FACE('',(#21290),#17425,.F.);
#76721=ADVANCED_FACE('',(#21291),#17426,.F.);
#76722=ADVANCED_FACE('',(#21292),#17427,.F.);
#76723=ADVANCED_FACE('',(#21293),#17428,.F.);
#76724=ADVANCED_FACE('',(#21294),#17429,.F.);
#76725=ADVANCED_FACE('',(#21295),#17430,.F.);
#76726=ADVANCED_FACE('',(#21296),#17431,.F.);
#76727=ADVANCED_FACE('',(#21297),#17432,.F.);
#76728=ADVANCED_FACE('',(#21298),#17433,.F.);
#76729=ADVANCED_FACE('',(#21299),#17434,.F.);
#76730=ADVANCED_FACE('',(#21300),#17435,.F.);
#76731=ADVANCED_FACE('',(#21301),#17436,.F.);
#76732=ADVANCED_FACE('',(#21302),#17437,.F.);
#76733=ADVANCED_FACE('',(#21303),#17438,.F.);
#76734=ADVANCED_FACE('',(#21304),#17439,.F.);
#76735=ADVANCED_FACE('',(#21305),#17440,.F.);
#76736=ADVANCED_FACE('',(#21306),#17441,.F.);
#76737=ADVANCED_FACE('',(#21307),#17442,.F.);
#76738=ADVANCED_FACE('',(#21308),#17443,.F.);
#76739=ADVANCED_FACE('',(#21309),#17444,.F.);
#76740=ADVANCED_FACE('',(#21310),#17445,.F.);
#76741=ADVANCED_FACE('',(#21311),#17446,.F.);
#76742=ADVANCED_FACE('',(#21312),#17447,.F.);
#76743=ADVANCED_FACE('',(#21313),#17448,.F.);
#76744=ADVANCED_FACE('',(#21314),#17449,.F.);
#76745=ADVANCED_FACE('',(#21315),#17450,.F.);
#76746=ADVANCED_FACE('',(#21316),#17451,.F.);
#76747=ADVANCED_FACE('',(#21317),#17452,.F.);
#76748=ADVANCED_FACE('',(#21318),#17453,.F.);
#76749=ADVANCED_FACE('',(#21319),#17454,.F.);
#76750=ADVANCED_FACE('',(#21320),#17455,.F.);
#76751=ADVANCED_FACE('',(#21321),#17456,.F.);
#76752=ADVANCED_FACE('',(#21322),#17457,.F.);
#76753=ADVANCED_FACE('',(#21323),#17458,.F.);
#76754=ADVANCED_FACE('',(#21324),#17459,.F.);
#76755=ADVANCED_FACE('',(#21325),#17460,.F.);
#76756=ADVANCED_FACE('',(#21326),#17461,.F.);
#76757=ADVANCED_FACE('',(#21327),#17462,.F.);
#76758=ADVANCED_FACE('',(#21328),#17463,.F.);
#76759=ADVANCED_FACE('',(#21329),#17464,.F.);
#76760=ADVANCED_FACE('',(#21330),#17465,.F.);
#76761=ADVANCED_FACE('',(#21331),#17466,.F.);
#76762=ADVANCED_FACE('',(#21332),#17467,.F.);
#76763=ADVANCED_FACE('',(#21333),#17468,.F.);
#76764=ADVANCED_FACE('',(#21334),#17469,.F.);
#76765=ADVANCED_FACE('',(#21335),#17470,.F.);
#76766=ADVANCED_FACE('',(#21336),#17471,.F.);
#76767=ADVANCED_FACE('',(#21337),#17472,.F.);
#76768=ADVANCED_FACE('',(#21338),#17473,.F.);
#76769=ADVANCED_FACE('',(#21339),#17474,.F.);
#76770=ADVANCED_FACE('',(#21340),#17475,.F.);
#76771=ADVANCED_FACE('',(#21341),#17476,.F.);
#76772=ADVANCED_FACE('',(#21342),#17477,.F.);
#76773=ADVANCED_FACE('',(#21343),#17478,.F.);
#76774=ADVANCED_FACE('',(#21344),#17479,.F.);
#76775=ADVANCED_FACE('',(#21345),#17480,.F.);
#76776=ADVANCED_FACE('',(#21346),#17481,.F.);
#76777=ADVANCED_FACE('',(#21347),#17482,.F.);
#76778=ADVANCED_FACE('',(#21348),#17483,.F.);
#76779=ADVANCED_FACE('',(#21349),#17484,.F.);
#76780=ADVANCED_FACE('',(#21350),#17485,.F.);
#76781=ADVANCED_FACE('',(#21351),#17486,.F.);
#76782=ADVANCED_FACE('',(#21352),#17487,.F.);
#76783=ADVANCED_FACE('',(#21353),#17488,.F.);
#76784=ADVANCED_FACE('',(#21354),#17489,.F.);
#76785=ADVANCED_FACE('',(#21355),#17490,.F.);
#76786=ADVANCED_FACE('',(#21356),#17491,.F.);
#76787=ADVANCED_FACE('',(#21357),#17492,.F.);
#76788=ADVANCED_FACE('',(#21358),#17493,.F.);
#76789=ADVANCED_FACE('',(#21359),#17494,.F.);
#76790=ADVANCED_FACE('',(#21360),#17495,.F.);
#76791=ADVANCED_FACE('',(#21361),#17496,.F.);
#76792=ADVANCED_FACE('',(#21362),#17497,.F.);
#76793=ADVANCED_FACE('',(#21363),#17498,.F.);
#76794=ADVANCED_FACE('',(#21364),#17499,.F.);
#76795=ADVANCED_FACE('',(#21365),#17500,.F.);
#76796=ADVANCED_FACE('',(#21366),#17501,.F.);
#76797=ADVANCED_FACE('',(#21367),#17502,.F.);
#76798=ADVANCED_FACE('',(#21368),#17503,.F.);
#76799=ADVANCED_FACE('',(#21369),#17504,.F.);
#76800=ADVANCED_FACE('',(#21370),#17505,.F.);
#76801=ADVANCED_FACE('',(#21371),#17506,.F.);
#76802=ADVANCED_FACE('',(#21372),#17507,.F.);
#76803=ADVANCED_FACE('',(#21373),#17508,.F.);
#76804=ADVANCED_FACE('',(#21374),#17509,.F.);
#76805=ADVANCED_FACE('',(#21375),#17510,.F.);
#76806=ADVANCED_FACE('',(#21376),#17511,.F.);
#76807=ADVANCED_FACE('',(#21377),#17512,.F.);
#76808=ADVANCED_FACE('',(#21378),#17513,.F.);
#76809=ADVANCED_FACE('',(#21379),#17514,.F.);
#76810=ADVANCED_FACE('',(#21380),#17515,.F.);
#76811=ADVANCED_FACE('',(#21381),#17516,.F.);
#76812=ADVANCED_FACE('',(#21382),#17517,.F.);
#76813=ADVANCED_FACE('',(#21383),#17518,.F.);
#76814=ADVANCED_FACE('',(#21384),#17519,.F.);
#76815=ADVANCED_FACE('',(#21385),#17520,.F.);
#76816=ADVANCED_FACE('',(#21386),#17521,.F.);
#76817=ADVANCED_FACE('',(#21387),#17522,.F.);
#76818=ADVANCED_FACE('',(#21388),#17523,.F.);
#76819=ADVANCED_FACE('',(#21389),#17524,.F.);
#76820=ADVANCED_FACE('',(#21390),#17525,.F.);
#76821=ADVANCED_FACE('',(#21391),#17526,.F.);
#76822=ADVANCED_FACE('',(#21392),#17527,.F.);
#76823=ADVANCED_FACE('',(#21393),#17528,.F.);
#76824=ADVANCED_FACE('',(#21394),#17529,.F.);
#76825=ADVANCED_FACE('',(#21395),#17530,.F.);
#76826=ADVANCED_FACE('',(#21396),#17531,.F.);
#76827=ADVANCED_FACE('',(#21397),#17532,.F.);
#76828=ADVANCED_FACE('',(#21398),#17533,.F.);
#76829=ADVANCED_FACE('',(#21399),#17534,.F.);
#76830=ADVANCED_FACE('',(#21400),#17535,.F.);
#76831=ADVANCED_FACE('',(#21401),#17536,.F.);
#76832=ADVANCED_FACE('',(#21402),#17537,.F.);
#76833=ADVANCED_FACE('',(#21403),#17538,.F.);
#76834=ADVANCED_FACE('',(#21404),#17539,.F.);
#76835=ADVANCED_FACE('',(#21405),#17540,.F.);
#76836=ADVANCED_FACE('',(#21406),#17541,.F.);
#76837=ADVANCED_FACE('',(#21407),#17542,.F.);
#76838=ADVANCED_FACE('',(#21408),#17543,.F.);
#76839=ADVANCED_FACE('',(#21409),#17544,.F.);
#76840=ADVANCED_FACE('',(#21410),#17545,.F.);
#76841=ADVANCED_FACE('',(#21411),#17546,.F.);
#76842=ADVANCED_FACE('',(#21412),#17547,.F.);
#76843=ADVANCED_FACE('',(#21413),#17548,.F.);
#76844=ADVANCED_FACE('',(#21414),#17549,.F.);
#76845=ADVANCED_FACE('',(#21415),#17550,.F.);
#76846=ADVANCED_FACE('',(#21416),#17551,.F.);
#76847=ADVANCED_FACE('',(#21417),#17552,.F.);
#76848=ADVANCED_FACE('',(#21418),#17553,.F.);
#76849=ADVANCED_FACE('',(#21419),#17554,.F.);
#76850=ADVANCED_FACE('',(#21420),#17555,.F.);
#76851=ADVANCED_FACE('',(#21421),#17556,.F.);
#76852=ADVANCED_FACE('',(#21422),#17557,.F.);
#76853=ADVANCED_FACE('',(#21423),#17558,.F.);
#76854=ADVANCED_FACE('',(#21424),#17559,.F.);
#76855=ADVANCED_FACE('',(#21425),#17560,.F.);
#76856=ADVANCED_FACE('',(#21426),#17561,.F.);
#76857=ADVANCED_FACE('',(#21427),#17562,.T.);
#76858=ADVANCED_FACE('',(#21428),#17563,.F.);
#76859=ADVANCED_FACE('',(#21429),#17564,.F.);
#76860=ADVANCED_FACE('',(#21430),#17565,.F.);
#76861=ADVANCED_FACE('',(#21431),#17566,.F.);
#76862=ADVANCED_FACE('',(#21432),#17567,.T.);
#76863=ADVANCED_FACE('',(#21433),#17568,.F.);
#76864=ADVANCED_FACE('',(#21434),#17569,.F.);
#76865=ADVANCED_FACE('',(#21435),#17570,.F.);
#76866=ADVANCED_FACE('',(#21436),#17571,.F.);
#76867=ADVANCED_FACE('',(#21437),#17572,.T.);
#76868=ADVANCED_FACE('',(#21438),#17573,.F.);
#76869=ADVANCED_FACE('',(#21439),#17574,.F.);
#76870=ADVANCED_FACE('',(#21440),#17575,.F.);
#76871=ADVANCED_FACE('',(#21441),#17576,.F.);
#76872=ADVANCED_FACE('',(#21442),#17577,.T.);
#76873=ADVANCED_FACE('',(#21443),#17578,.F.);
#76874=ADVANCED_FACE('',(#21444),#17579,.F.);
#76875=ADVANCED_FACE('',(#21445),#17580,.F.);
#76876=ADVANCED_FACE('',(#21446),#17581,.F.);
#76877=ADVANCED_FACE('',(#21447),#17582,.T.);
#76878=ADVANCED_FACE('',(#21448),#17583,.F.);
#76879=ADVANCED_FACE('',(#21449),#17584,.F.);
#76880=ADVANCED_FACE('',(#21450),#17585,.F.);
#76881=ADVANCED_FACE('',(#21451),#17586,.F.);
#76882=ADVANCED_FACE('',(#21452),#17587,.T.);
#76883=ADVANCED_FACE('',(#21453),#17588,.F.);
#76884=ADVANCED_FACE('',(#21454),#17589,.F.);
#76885=ADVANCED_FACE('',(#21455),#17590,.F.);
#76886=ADVANCED_FACE('',(#21456),#17591,.F.);
#76887=ADVANCED_FACE('',(#21457),#17592,.T.);
#76888=ADVANCED_FACE('',(#21458),#17593,.F.);
#76889=ADVANCED_FACE('',(#21459),#17594,.F.);
#76890=ADVANCED_FACE('',(#21460),#17595,.F.);
#76891=ADVANCED_FACE('',(#21461),#17596,.F.);
#76892=ADVANCED_FACE('',(#21462),#17597,.T.);
#76893=ADVANCED_FACE('',(#21463),#17598,.F.);
#76894=ADVANCED_FACE('',(#21464),#17599,.F.);
#76895=ADVANCED_FACE('',(#21465),#17600,.F.);
#76896=ADVANCED_FACE('',(#21466),#17601,.F.);
#76897=ADVANCED_FACE('',(#21467),#17602,.T.);
#76898=ADVANCED_FACE('',(#21468),#17603,.F.);
#76899=ADVANCED_FACE('',(#21469),#17604,.F.);
#76900=ADVANCED_FACE('',(#21470),#17605,.F.);
#76901=ADVANCED_FACE('',(#21471),#17606,.F.);
#76902=ADVANCED_FACE('',(#21472),#17607,.T.);
#76903=ADVANCED_FACE('',(#21473),#17608,.F.);
#76904=ADVANCED_FACE('',(#21474),#17609,.F.);
#76905=ADVANCED_FACE('',(#21475),#17610,.F.);
#76906=ADVANCED_FACE('',(#21476),#17611,.F.);
#76907=ADVANCED_FACE('',(#21477),#17612,.F.);
#76908=ADVANCED_FACE('',(#21478),#17613,.F.);
#76909=ADVANCED_FACE('',(#21479),#17614,.F.);
#76910=ADVANCED_FACE('',(#21480),#17615,.F.);
#76911=ADVANCED_FACE('',(#21481),#17616,.F.);
#76912=ADVANCED_FACE('',(#21482),#17617,.F.);
#76913=ADVANCED_FACE('',(#21483),#17618,.F.);
#76914=ADVANCED_FACE('',(#21484),#17619,.F.);
#76915=ADVANCED_FACE('',(#21485),#17620,.F.);
#76916=ADVANCED_FACE('',(#21486),#17621,.F.);
#76917=ADVANCED_FACE('',(#21487),#17622,.F.);
#76918=ADVANCED_FACE('',(#21488),#17623,.F.);
#76919=ADVANCED_FACE('',(#21489),#17624,.F.);
#76920=ADVANCED_FACE('',(#21490),#17625,.F.);
#76921=ADVANCED_FACE('',(#21491),#17626,.F.);
#76922=ADVANCED_FACE('',(#21492),#17627,.F.);
#76923=ADVANCED_FACE('',(#21493),#17628,.F.);
#76924=ADVANCED_FACE('',(#21494),#17629,.F.);
#76925=ADVANCED_FACE('',(#21495),#17630,.F.);
#76926=ADVANCED_FACE('',(#21496),#17631,.F.);
#76927=ADVANCED_FACE('',(#21497),#17632,.F.);
#76928=ADVANCED_FACE('',(#21498),#17633,.F.);
#76929=ADVANCED_FACE('',(#21499),#17634,.F.);
#76930=ADVANCED_FACE('',(#21500),#17635,.F.);
#76931=ADVANCED_FACE('',(#21501),#17636,.F.);
#76932=ADVANCED_FACE('',(#21502),#17637,.F.);
#76933=ADVANCED_FACE('',(#21503),#17638,.F.);
#76934=ADVANCED_FACE('',(#21504),#17639,.F.);
#76935=ADVANCED_FACE('',(#21505),#17640,.F.);
#76936=ADVANCED_FACE('',(#21506),#17641,.F.);
#76937=ADVANCED_FACE('',(#21507),#17642,.F.);
#76938=ADVANCED_FACE('',(#21508),#17643,.F.);
#76939=ADVANCED_FACE('',(#21509),#17644,.T.);
#76940=ADVANCED_FACE('',(#21510),#17645,.F.);
#76941=ADVANCED_FACE('',(#21511),#17646,.F.);
#76942=ADVANCED_FACE('',(#21512),#17647,.F.);
#76943=ADVANCED_FACE('',(#21513),#17648,.F.);
#76944=ADVANCED_FACE('',(#21514),#17649,.T.);
#76945=ADVANCED_FACE('',(#21515),#17650,.F.);
#76946=ADVANCED_FACE('',(#21516),#17651,.F.);
#76947=ADVANCED_FACE('',(#21517),#17652,.F.);
#76948=ADVANCED_FACE('',(#21518),#17653,.F.);
#76949=ADVANCED_FACE('',(#21519),#17654,.F.);
#76950=ADVANCED_FACE('',(#21520),#17655,.F.);
#76951=ADVANCED_FACE('',(#21521),#17656,.F.);
#76952=ADVANCED_FACE('',(#21522),#17657,.F.);
#76953=ADVANCED_FACE('',(#21523),#17658,.F.);
#76954=ADVANCED_FACE('',(#21524),#17659,.F.);
#76955=ADVANCED_FACE('',(#21525),#17660,.F.);
#76956=ADVANCED_FACE('',(#21526),#17661,.F.);
#76957=ADVANCED_FACE('',(#21527),#17662,.F.);
#76958=ADVANCED_FACE('',(#21528),#17663,.F.);
#76959=ADVANCED_FACE('',(#21529),#17664,.F.);
#76960=ADVANCED_FACE('',(#21530),#17665,.F.);
#76961=ADVANCED_FACE('',(#21531),#17666,.F.);
#76962=ADVANCED_FACE('',(#21532),#17667,.F.);
#76963=ADVANCED_FACE('',(#21533),#17668,.F.);
#76964=ADVANCED_FACE('',(#21534),#17669,.F.);
#76965=ADVANCED_FACE('',(#21535),#17670,.T.);
#76966=ADVANCED_FACE('',(#21536),#17671,.F.);
#76967=ADVANCED_FACE('',(#21537),#17672,.F.);
#76968=ADVANCED_FACE('',(#21538),#17673,.F.);
#76969=ADVANCED_FACE('',(#21539),#17674,.F.);
#76970=ADVANCED_FACE('',(#21540),#17675,.T.);
#76971=ADVANCED_FACE('',(#21541),#17676,.F.);
#76972=ADVANCED_FACE('',(#21542),#17677,.F.);
#76973=ADVANCED_FACE('',(#21543),#17678,.F.);
#76974=ADVANCED_FACE('',(#21544),#17679,.F.);
#76975=ADVANCED_FACE('',(#21545),#17680,.T.);
#76976=ADVANCED_FACE('',(#21546),#17681,.F.);
#76977=ADVANCED_FACE('',(#21547),#17682,.F.);
#76978=ADVANCED_FACE('',(#21548),#17683,.F.);
#76979=ADVANCED_FACE('',(#21549),#17684,.F.);
#76980=ADVANCED_FACE('',(#21550),#17685,.T.);
#76981=ADVANCED_FACE('',(#21551),#17686,.F.);
#76982=ADVANCED_FACE('',(#21552),#17687,.F.);
#76983=ADVANCED_FACE('',(#21553),#17688,.F.);
#76984=ADVANCED_FACE('',(#21554),#17689,.F.);
#76985=ADVANCED_FACE('',(#21555),#17690,.F.);
#76986=ADVANCED_FACE('',(#21556),#17691,.F.);
#76987=ADVANCED_FACE('',(#21557),#17692,.F.);
#76988=ADVANCED_FACE('',(#21558),#17693,.F.);
#76989=ADVANCED_FACE('',(#21559),#17694,.F.);
#76990=ADVANCED_FACE('',(#21560),#17695,.F.);
#76991=ADVANCED_FACE('',(#21561),#17696,.F.);
#76992=ADVANCED_FACE('',(#21562),#17697,.F.);
#76993=ADVANCED_FACE('',(#21563),#17698,.F.);
#76994=ADVANCED_FACE('',(#21564),#17699,.F.);
#76995=ADVANCED_FACE('',(#21565),#17700,.F.);
#76996=ADVANCED_FACE('',(#21566),#17701,.F.);
#76997=ADVANCED_FACE('',(#21567),#17702,.F.);
#76998=ADVANCED_FACE('',(#21568),#17703,.F.);
#76999=ADVANCED_FACE('',(#21569),#17704,.F.);
#77000=ADVANCED_FACE('',(#21570),#17705,.F.);
#77001=ADVANCED_FACE('',(#21571),#17706,.F.);
#77002=ADVANCED_FACE('',(#21572),#17707,.F.);
#77003=ADVANCED_FACE('',(#21573),#17708,.F.);
#77004=ADVANCED_FACE('',(#21574),#17709,.F.);
#77005=ADVANCED_FACE('',(#21575),#17710,.F.);
#77006=ADVANCED_FACE('',(#21576),#17711,.F.);
#77007=ADVANCED_FACE('',(#21577),#17712,.F.);
#77008=ADVANCED_FACE('',(#21578),#17713,.F.);
#77009=ADVANCED_FACE('',(#21579),#17714,.F.);
#77010=ADVANCED_FACE('',(#21580),#17715,.F.);
#77011=ADVANCED_FACE('',(#21581),#17716,.F.);
#77012=ADVANCED_FACE('',(#21582),#17717,.F.);
#77013=ADVANCED_FACE('',(#21583),#17718,.F.);
#77014=ADVANCED_FACE('',(#21584),#17719,.F.);
#77015=ADVANCED_FACE('',(#21585),#17720,.F.);
#77016=ADVANCED_FACE('',(#21586),#17721,.F.);
#77017=ADVANCED_FACE('',(#21587),#17722,.F.);
#77018=ADVANCED_FACE('',(#21588),#17723,.F.);
#77019=ADVANCED_FACE('',(#21589),#17724,.F.);
#77020=ADVANCED_FACE('',(#21590),#17725,.F.);
#77021=ADVANCED_FACE('',(#21591),#17726,.F.);
#77022=ADVANCED_FACE('',(#21592),#17727,.F.);
#77023=ADVANCED_FACE('',(#21593),#17728,.F.);
#77024=ADVANCED_FACE('',(#21594),#17729,.F.);
#77025=ADVANCED_FACE('',(#21595),#17730,.T.);
#77026=ADVANCED_FACE('',(#21596),#17731,.F.);
#77027=ADVANCED_FACE('',(#21597),#17732,.F.);
#77028=ADVANCED_FACE('',(#21598),#17733,.F.);
#77029=ADVANCED_FACE('',(#21599),#17734,.F.);
#77030=ADVANCED_FACE('',(#21600),#17735,.T.);
#77031=ADVANCED_FACE('',(#21601),#17736,.F.);
#77032=ADVANCED_FACE('',(#21602),#17737,.F.);
#77033=ADVANCED_FACE('',(#21603),#17738,.F.);
#77034=ADVANCED_FACE('',(#21604),#17739,.F.);
#77035=ADVANCED_FACE('',(#21605),#17740,.F.);
#77036=ADVANCED_FACE('',(#21606),#17741,.F.);
#77037=ADVANCED_FACE('',(#21607),#17742,.F.);
#77038=ADVANCED_FACE('',(#21608),#17743,.F.);
#77039=ADVANCED_FACE('',(#21609),#17744,.F.);
#77040=ADVANCED_FACE('',(#21610),#17745,.F.);
#77041=ADVANCED_FACE('',(#21611),#17746,.F.);
#77042=ADVANCED_FACE('',(#21612),#17747,.F.);
#77043=ADVANCED_FACE('',(#21613),#17748,.F.);
#77044=ADVANCED_FACE('',(#21614),#17749,.F.);
#77045=ADVANCED_FACE('',(#21615),#17750,.F.);
#77046=ADVANCED_FACE('',(#21616),#17751,.F.);
#77047=ADVANCED_FACE('',(#21617),#17752,.F.);
#77048=ADVANCED_FACE('',(#21618),#17753,.F.);
#77049=ADVANCED_FACE('',(#21619),#17754,.F.);
#77050=ADVANCED_FACE('',(#21620),#17755,.F.);
#77051=ADVANCED_FACE('',(#21621),#17756,.F.);
#77052=ADVANCED_FACE('',(#21622),#17757,.F.);
#77053=ADVANCED_FACE('',(#21623),#17758,.F.);
#77054=ADVANCED_FACE('',(#21624),#17759,.F.);
#77055=ADVANCED_FACE('',(#21625),#17760,.F.);
#77056=ADVANCED_FACE('',(#21626),#17761,.F.);
#77057=ADVANCED_FACE('',(#21627),#17762,.F.);
#77058=ADVANCED_FACE('',(#21628),#17763,.F.);
#77059=ADVANCED_FACE('',(#21629),#17764,.F.);
#77060=ADVANCED_FACE('',(#21630),#17765,.F.);
#77061=ADVANCED_FACE('',(#21631),#17766,.F.);
#77062=ADVANCED_FACE('',(#21632),#17767,.F.);
#77063=ADVANCED_FACE('',(#21633),#17768,.F.);
#77064=ADVANCED_FACE('',(#21634),#17769,.F.);
#77065=ADVANCED_FACE('',(#21635),#17770,.F.);
#77066=ADVANCED_FACE('',(#21636),#17771,.F.);
#77067=ADVANCED_FACE('',(#21637),#17772,.F.);
#77068=ADVANCED_FACE('',(#21638),#17773,.F.);
#77069=ADVANCED_FACE('',(#21639),#17774,.F.);
#77070=ADVANCED_FACE('',(#21640),#17775,.F.);
#77071=ADVANCED_FACE('',(#21641),#17776,.T.);
#77072=ADVANCED_FACE('',(#21642),#17777,.F.);
#77073=ADVANCED_FACE('',(#21643),#17778,.F.);
#77074=ADVANCED_FACE('',(#21644),#17779,.F.);
#77075=ADVANCED_FACE('',(#21645),#17780,.F.);
#77076=ADVANCED_FACE('',(#21646),#17781,.T.);
#77077=ADVANCED_FACE('',(#21647),#17782,.F.);
#77078=ADVANCED_FACE('',(#21648),#17783,.F.);
#77079=ADVANCED_FACE('',(#21649),#17784,.F.);
#77080=ADVANCED_FACE('',(#21650),#17785,.F.);
#77081=ADVANCED_FACE('',(#21651),#17786,.F.);
#77082=ADVANCED_FACE('',(#21652),#17787,.F.);
#77083=ADVANCED_FACE('',(#21653),#17788,.F.);
#77084=ADVANCED_FACE('',(#21654),#17789,.F.);
#77085=ADVANCED_FACE('',(#21655),#17790,.F.);
#77086=ADVANCED_FACE('',(#21656),#17791,.F.);
#77087=ADVANCED_FACE('',(#21657),#17792,.F.);
#77088=ADVANCED_FACE('',(#21658),#17793,.F.);
#77089=ADVANCED_FACE('',(#21659),#17794,.F.);
#77090=ADVANCED_FACE('',(#21660),#17795,.F.);
#77091=ADVANCED_FACE('',(#21661),#17796,.F.);
#77092=ADVANCED_FACE('',(#21662),#17797,.F.);
#77093=ADVANCED_FACE('',(#21663),#17798,.F.);
#77094=ADVANCED_FACE('',(#21664),#17799,.F.);
#77095=ADVANCED_FACE('',(#21665),#17800,.F.);
#77096=ADVANCED_FACE('',(#21666),#17801,.F.);
#77097=ADVANCED_FACE('',(#21667),#17802,.F.);
#77098=ADVANCED_FACE('',(#21668),#17803,.F.);
#77099=ADVANCED_FACE('',(#21669),#17804,.F.);
#77100=ADVANCED_FACE('',(#21670),#17805,.F.);
#77101=ADVANCED_FACE('',(#21671),#17806,.F.);
#77102=ADVANCED_FACE('',(#21672),#17807,.F.);
#77103=ADVANCED_FACE('',(#21673),#17808,.F.);
#77104=ADVANCED_FACE('',(#21674),#17809,.F.);
#77105=ADVANCED_FACE('',(#21675),#17810,.F.);
#77106=ADVANCED_FACE('',(#21676),#17811,.F.);
#77107=ADVANCED_FACE('',(#21677),#17812,.F.);
#77108=ADVANCED_FACE('',(#21678),#17813,.F.);
#77109=ADVANCED_FACE('',(#21679),#17814,.F.);
#77110=ADVANCED_FACE('',(#21680),#17815,.F.);
#77111=ADVANCED_FACE('',(#21681),#17816,.F.);
#77112=ADVANCED_FACE('',(#21682),#17817,.F.);
#77113=ADVANCED_FACE('',(#21683),#17818,.F.);
#77114=ADVANCED_FACE('',(#21684),#17819,.F.);
#77115=ADVANCED_FACE('',(#21685),#17820,.F.);
#77116=ADVANCED_FACE('',(#21686),#17821,.F.);
#77117=ADVANCED_FACE('',(#21687),#17822,.F.);
#77118=ADVANCED_FACE('',(#21688),#17823,.F.);
#77119=ADVANCED_FACE('',(#21689),#17824,.F.);
#77120=ADVANCED_FACE('',(#21690),#17825,.F.);
#77121=ADVANCED_FACE('',(#21691),#17826,.F.);
#77122=ADVANCED_FACE('',(#21692),#17827,.F.);
#77123=ADVANCED_FACE('',(#21693),#17828,.F.);
#77124=ADVANCED_FACE('',(#21694),#17829,.F.);
#77125=ADVANCED_FACE('',(#21695),#17830,.F.);
#77126=ADVANCED_FACE('',(#21696),#17831,.F.);
#77127=ADVANCED_FACE('',(#21697),#17832,.F.);
#77128=ADVANCED_FACE('',(#21698),#17833,.F.);
#77129=ADVANCED_FACE('',(#21699),#17834,.F.);
#77130=ADVANCED_FACE('',(#21700),#17835,.F.);
#77131=ADVANCED_FACE('',(#21701),#17836,.F.);
#77132=ADVANCED_FACE('',(#21702),#17837,.F.);
#77133=ADVANCED_FACE('',(#21703),#17838,.F.);
#77134=ADVANCED_FACE('',(#21704),#17839,.F.);
#77135=ADVANCED_FACE('',(#21705),#17840,.F.);
#77136=ADVANCED_FACE('',(#21706),#17841,.F.);
#77137=ADVANCED_FACE('',(#21707),#17842,.F.);
#77138=ADVANCED_FACE('',(#21708),#17843,.F.);
#77139=ADVANCED_FACE('',(#21709),#17844,.F.);
#77140=ADVANCED_FACE('',(#21710),#17845,.F.);
#77141=ADVANCED_FACE('',(#21711),#17846,.F.);
#77142=ADVANCED_FACE('',(#21712),#17847,.F.);
#77143=ADVANCED_FACE('',(#21713),#17848,.F.);
#77144=ADVANCED_FACE('',(#21714),#17849,.F.);
#77145=ADVANCED_FACE('',(#21715),#17850,.F.);
#77146=ADVANCED_FACE('',(#21716),#17851,.F.);
#77147=ADVANCED_FACE('',(#21717),#17852,.F.);
#77148=ADVANCED_FACE('',(#21718),#17853,.F.);
#77149=ADVANCED_FACE('',(#21719),#17854,.F.);
#77150=ADVANCED_FACE('',(#21720),#17855,.F.);
#77151=ADVANCED_FACE('',(#21721),#17856,.F.);
#77152=ADVANCED_FACE('',(#21722),#17857,.F.);
#77153=ADVANCED_FACE('',(#21723),#17858,.F.);
#77154=ADVANCED_FACE('',(#21724),#17859,.F.);
#77155=ADVANCED_FACE('',(#21725),#17860,.F.);
#77156=ADVANCED_FACE('',(#21726),#17861,.F.);
#77157=ADVANCED_FACE('',(#21727),#17862,.F.);
#77158=ADVANCED_FACE('',(#21728),#17863,.F.);
#77159=ADVANCED_FACE('',(#21729),#17864,.F.);
#77160=ADVANCED_FACE('',(#21730),#17865,.F.);
#77161=ADVANCED_FACE('',(#21731),#17866,.F.);
#77162=ADVANCED_FACE('',(#21732),#17867,.F.);
#77163=ADVANCED_FACE('',(#21733),#17868,.F.);
#77164=ADVANCED_FACE('',(#21734),#17869,.F.);
#77165=ADVANCED_FACE('',(#21735),#17870,.F.);
#77166=ADVANCED_FACE('',(#21736),#17871,.F.);
#77167=ADVANCED_FACE('',(#21737),#17872,.F.);
#77168=ADVANCED_FACE('',(#21738),#17873,.F.);
#77169=ADVANCED_FACE('',(#21739),#17874,.F.);
#77170=ADVANCED_FACE('',(#21740),#17875,.F.);
#77171=ADVANCED_FACE('',(#21741),#17876,.F.);
#77172=ADVANCED_FACE('',(#21742),#17877,.F.);
#77173=ADVANCED_FACE('',(#21743),#17878,.F.);
#77174=ADVANCED_FACE('',(#21744),#17879,.F.);
#77175=ADVANCED_FACE('',(#21745),#17880,.F.);
#77176=ADVANCED_FACE('',(#21746),#17881,.F.);
#77177=ADVANCED_FACE('',(#21747),#17882,.F.);
#77178=ADVANCED_FACE('',(#21748),#17883,.F.);
#77179=ADVANCED_FACE('',(#21749),#17884,.F.);
#77180=ADVANCED_FACE('',(#21750),#17885,.F.);
#77181=ADVANCED_FACE('',(#21751),#17886,.F.);
#77182=ADVANCED_FACE('',(#21752),#17887,.F.);
#77183=ADVANCED_FACE('',(#21753),#17888,.F.);
#77184=ADVANCED_FACE('',(#21754),#17889,.F.);
#77185=ADVANCED_FACE('',(#21755),#17890,.F.);
#77186=ADVANCED_FACE('',(#21756),#17891,.F.);
#77187=ADVANCED_FACE('',(#21757),#17892,.F.);
#77188=ADVANCED_FACE('',(#21758),#17893,.F.);
#77189=ADVANCED_FACE('',(#21759),#17894,.F.);
#77190=ADVANCED_FACE('',(#21760),#17895,.F.);
#77191=ADVANCED_FACE('',(#21761),#17896,.F.);
#77192=ADVANCED_FACE('',(#21762),#17897,.F.);
#77193=ADVANCED_FACE('',(#21763),#17898,.F.);
#77194=ADVANCED_FACE('',(#21764),#17899,.F.);
#77195=ADVANCED_FACE('',(#21765),#17900,.F.);
#77196=ADVANCED_FACE('',(#21766),#17901,.F.);
#77197=ADVANCED_FACE('',(#21767),#17902,.F.);
#77198=ADVANCED_FACE('',(#21768),#17903,.F.);
#77199=ADVANCED_FACE('',(#21769),#17904,.F.);
#77200=ADVANCED_FACE('',(#21770),#17905,.F.);
#77201=ADVANCED_FACE('',(#21771),#17906,.F.);
#77202=ADVANCED_FACE('',(#21772),#17907,.F.);
#77203=ADVANCED_FACE('',(#21773),#17908,.F.);
#77204=ADVANCED_FACE('',(#21774),#17909,.F.);
#77205=ADVANCED_FACE('',(#21775),#17910,.F.);
#77206=ADVANCED_FACE('',(#21776),#17911,.F.);
#77207=ADVANCED_FACE('',(#21777),#17912,.F.);
#77208=ADVANCED_FACE('',(#21778),#17913,.F.);
#77209=ADVANCED_FACE('',(#21779),#17914,.F.);
#77210=ADVANCED_FACE('',(#21780),#17915,.F.);
#77211=ADVANCED_FACE('',(#21781),#17916,.F.);
#77212=ADVANCED_FACE('',(#21782),#17917,.F.);
#77213=ADVANCED_FACE('',(#21783),#17918,.F.);
#77214=ADVANCED_FACE('',(#21784),#17919,.F.);
#77215=ADVANCED_FACE('',(#21785),#17920,.F.);
#77216=ADVANCED_FACE('',(#21786),#17921,.F.);
#77217=ADVANCED_FACE('',(#21787),#17922,.F.);
#77218=ADVANCED_FACE('',(#21788),#17923,.F.);
#77219=ADVANCED_FACE('',(#21789),#17924,.F.);
#77220=ADVANCED_FACE('',(#21790),#17925,.F.);
#77221=ADVANCED_FACE('',(#21791),#17926,.F.);
#77222=ADVANCED_FACE('',(#21792),#17927,.F.);
#77223=ADVANCED_FACE('',(#21793),#17928,.F.);
#77224=ADVANCED_FACE('',(#21794),#17929,.F.);
#77225=ADVANCED_FACE('',(#21795),#17930,.F.);
#77226=ADVANCED_FACE('',(#21796),#17931,.F.);
#77227=ADVANCED_FACE('',(#21797),#17932,.F.);
#77228=ADVANCED_FACE('',(#21798),#17933,.F.);
#77229=ADVANCED_FACE('',(#21799),#17934,.F.);
#77230=ADVANCED_FACE('',(#21800),#17935,.F.);
#77231=ADVANCED_FACE('',(#21801),#17936,.F.);
#77232=ADVANCED_FACE('',(#21802),#17937,.F.);
#77233=ADVANCED_FACE('',(#21803),#17938,.F.);
#77234=ADVANCED_FACE('',(#21804),#17939,.F.);
#77235=ADVANCED_FACE('',(#21805),#17940,.F.);
#77236=ADVANCED_FACE('',(#21806),#17941,.F.);
#77237=ADVANCED_FACE('',(#21807),#17942,.F.);
#77238=ADVANCED_FACE('',(#21808),#17943,.F.);
#77239=ADVANCED_FACE('',(#21809),#17944,.F.);
#77240=ADVANCED_FACE('',(#21810),#17945,.F.);
#77241=ADVANCED_FACE('',(#21811),#17946,.F.);
#77242=ADVANCED_FACE('',(#21812),#17947,.F.);
#77243=ADVANCED_FACE('',(#21813),#17948,.F.);
#77244=ADVANCED_FACE('',(#21814),#17949,.F.);
#77245=ADVANCED_FACE('',(#21815),#17950,.F.);
#77246=ADVANCED_FACE('',(#21816),#17951,.F.);
#77247=ADVANCED_FACE('',(#21817),#17952,.F.);
#77248=ADVANCED_FACE('',(#21818),#17953,.F.);
#77249=ADVANCED_FACE('',(#21819),#17954,.F.);
#77250=ADVANCED_FACE('',(#21820),#17955,.F.);
#77251=ADVANCED_FACE('',(#21821),#17956,.F.);
#77252=ADVANCED_FACE('',(#21822),#17957,.F.);
#77253=ADVANCED_FACE('',(#21823),#17958,.F.);
#77254=ADVANCED_FACE('',(#21824),#17959,.F.);
#77255=ADVANCED_FACE('',(#21825),#17960,.F.);
#77256=ADVANCED_FACE('',(#21826),#17961,.F.);
#77257=ADVANCED_FACE('',(#21827),#17962,.F.);
#77258=ADVANCED_FACE('',(#21828),#17963,.F.);
#77259=ADVANCED_FACE('',(#21829),#17964,.F.);
#77260=ADVANCED_FACE('',(#21830),#17965,.F.);
#77261=ADVANCED_FACE('',(#21831),#17966,.F.);
#77262=ADVANCED_FACE('',(#21832),#17967,.F.);
#77263=ADVANCED_FACE('',(#21833),#17968,.F.);
#77264=ADVANCED_FACE('',(#21834),#17969,.F.);
#77265=ADVANCED_FACE('',(#21835),#17970,.F.);
#77266=ADVANCED_FACE('',(#21836),#17971,.F.);
#77267=ADVANCED_FACE('',(#21837),#17972,.F.);
#77268=ADVANCED_FACE('',(#21838),#17973,.F.);
#77269=ADVANCED_FACE('',(#21839),#17974,.F.);
#77270=ADVANCED_FACE('',(#21840),#17975,.F.);
#77271=ADVANCED_FACE('',(#21841),#17976,.F.);
#77272=ADVANCED_FACE('',(#21842),#17977,.F.);
#77273=ADVANCED_FACE('',(#21843),#17978,.F.);
#77274=ADVANCED_FACE('',(#21844),#17979,.F.);
#77275=ADVANCED_FACE('',(#21845),#17980,.F.);
#77276=ADVANCED_FACE('',(#21846),#17981,.F.);
#77277=ADVANCED_FACE('',(#21847),#17982,.F.);
#77278=ADVANCED_FACE('',(#21848),#17983,.F.);
#77279=ADVANCED_FACE('',(#21849),#17984,.F.);
#77280=ADVANCED_FACE('',(#21850),#17985,.F.);
#77281=ADVANCED_FACE('',(#21851),#17986,.F.);
#77282=ADVANCED_FACE('',(#21852),#17987,.F.);
#77283=ADVANCED_FACE('',(#21853),#17988,.F.);
#77284=ADVANCED_FACE('',(#21854),#17989,.F.);
#77285=ADVANCED_FACE('',(#21855),#17990,.F.);
#77286=ADVANCED_FACE('',(#21856),#17991,.F.);
#77287=ADVANCED_FACE('',(#21857),#17992,.F.);
#77288=ADVANCED_FACE('',(#21858),#17993,.F.);
#77289=ADVANCED_FACE('',(#21859),#17994,.F.);
#77290=ADVANCED_FACE('',(#21860),#17995,.F.);
#77291=ADVANCED_FACE('',(#21861),#17996,.F.);
#77292=ADVANCED_FACE('',(#21862),#17997,.F.);
#77293=ADVANCED_FACE('',(#21863),#17998,.F.);
#77294=ADVANCED_FACE('',(#21864),#17999,.F.);
#77295=ADVANCED_FACE('',(#21865),#18000,.F.);
#77296=ADVANCED_FACE('',(#21866),#18001,.F.);
#77297=ADVANCED_FACE('',(#21867),#18002,.F.);
#77298=ADVANCED_FACE('',(#21868),#18003,.F.);
#77299=ADVANCED_FACE('',(#21869),#18004,.F.);
#77300=ADVANCED_FACE('',(#21870),#18005,.F.);
#77301=ADVANCED_FACE('',(#21871),#18006,.F.);
#77302=ADVANCED_FACE('',(#21872),#18007,.F.);
#77303=ADVANCED_FACE('',(#21873),#18008,.F.);
#77304=ADVANCED_FACE('',(#21874),#18009,.F.);
#77305=ADVANCED_FACE('',(#21875),#18010,.F.);
#77306=ADVANCED_FACE('',(#21876),#18011,.F.);
#77307=ADVANCED_FACE('',(#21877),#18012,.F.);
#77308=ADVANCED_FACE('',(#21878),#18013,.F.);
#77309=ADVANCED_FACE('',(#21879),#18014,.F.);
#77310=ADVANCED_FACE('',(#21880),#18015,.F.);
#77311=ADVANCED_FACE('',(#21881),#18016,.F.);
#77312=ADVANCED_FACE('',(#21882),#18017,.F.);
#77313=ADVANCED_FACE('',(#21883),#18018,.F.);
#77314=ADVANCED_FACE('',(#21884),#18019,.F.);
#77315=ADVANCED_FACE('',(#21885),#18020,.F.);
#77316=ADVANCED_FACE('',(#21886),#18021,.F.);
#77317=ADVANCED_FACE('',(#21887),#18022,.F.);
#77318=ADVANCED_FACE('',(#21888),#18023,.F.);
#77319=ADVANCED_FACE('',(#21889),#18024,.F.);
#77320=ADVANCED_FACE('',(#21890),#18025,.F.);
#77321=ADVANCED_FACE('',(#21891),#18026,.F.);
#77322=ADVANCED_FACE('',(#21892),#18027,.F.);
#77323=ADVANCED_FACE('',(#21893),#18028,.F.);
#77324=ADVANCED_FACE('',(#21894),#18029,.F.);
#77325=ADVANCED_FACE('',(#21895),#18030,.F.);
#77326=ADVANCED_FACE('',(#21896),#18031,.F.);
#77327=ADVANCED_FACE('',(#21897),#18032,.F.);
#77328=ADVANCED_FACE('',(#21898),#18033,.F.);
#77329=ADVANCED_FACE('',(#21899),#18034,.F.);
#77330=ADVANCED_FACE('',(#21900),#18035,.F.);
#77331=ADVANCED_FACE('',(#21901),#18036,.F.);
#77332=ADVANCED_FACE('',(#21902),#18037,.F.);
#77333=ADVANCED_FACE('',(#21903),#18038,.F.);
#77334=ADVANCED_FACE('',(#21904),#18039,.F.);
#77335=ADVANCED_FACE('',(#21905),#18040,.F.);
#77336=ADVANCED_FACE('',(#21906),#18041,.F.);
#77337=ADVANCED_FACE('',(#21907),#18042,.F.);
#77338=ADVANCED_FACE('',(#21908),#18043,.F.);
#77339=ADVANCED_FACE('',(#21909),#18044,.F.);
#77340=ADVANCED_FACE('',(#21910),#18045,.F.);
#77341=ADVANCED_FACE('',(#21911),#18046,.F.);
#77342=ADVANCED_FACE('',(#21912),#18047,.F.);
#77343=ADVANCED_FACE('',(#21913),#18048,.F.);
#77344=ADVANCED_FACE('',(#21914),#18049,.F.);
#77345=ADVANCED_FACE('',(#21915),#18050,.F.);
#77346=ADVANCED_FACE('',(#21916),#18051,.F.);
#77347=ADVANCED_FACE('',(#21917),#18052,.F.);
#77348=ADVANCED_FACE('',(#21918),#18053,.F.);
#77349=ADVANCED_FACE('',(#21919),#18054,.F.);
#77350=ADVANCED_FACE('',(#21920),#18055,.F.);
#77351=ADVANCED_FACE('',(#21921),#18056,.F.);
#77352=ADVANCED_FACE('',(#21922),#18057,.F.);
#77353=ADVANCED_FACE('',(#21923),#18058,.F.);
#77354=ADVANCED_FACE('',(#21924),#18059,.F.);
#77355=ADVANCED_FACE('',(#21925),#18060,.F.);
#77356=ADVANCED_FACE('',(#21926),#18061,.F.);
#77357=ADVANCED_FACE('',(#21927),#18062,.F.);
#77358=ADVANCED_FACE('',(#21928),#18063,.F.);
#77359=ADVANCED_FACE('',(#21929),#18064,.F.);
#77360=ADVANCED_FACE('',(#21930),#18065,.F.);
#77361=ADVANCED_FACE('',(#21931),#18066,.F.);
#77362=ADVANCED_FACE('',(#21932),#18067,.F.);
#77363=ADVANCED_FACE('',(#21933),#18068,.F.);
#77364=ADVANCED_FACE('',(#21934),#18069,.F.);
#77365=ADVANCED_FACE('',(#21935),#18070,.F.);
#77366=ADVANCED_FACE('',(#21936),#18071,.F.);
#77367=ADVANCED_FACE('',(#21937),#18072,.F.);
#77368=ADVANCED_FACE('',(#21938),#18073,.F.);
#77369=ADVANCED_FACE('',(#21939),#18074,.F.);
#77370=ADVANCED_FACE('',(#21940),#18075,.F.);
#77371=ADVANCED_FACE('',(#21941),#18076,.F.);
#77372=ADVANCED_FACE('',(#21942),#18077,.F.);
#77373=ADVANCED_FACE('',(#21943),#18078,.F.);
#77374=ADVANCED_FACE('',(#21944),#18079,.F.);
#77375=ADVANCED_FACE('',(#21945),#18080,.F.);
#77376=ADVANCED_FACE('',(#21946),#18081,.F.);
#77377=ADVANCED_FACE('',(#21947),#18082,.F.);
#77378=ADVANCED_FACE('',(#21948),#18083,.F.);
#77379=ADVANCED_FACE('',(#21949),#18084,.F.);
#77380=ADVANCED_FACE('',(#21950),#18085,.F.);
#77381=ADVANCED_FACE('',(#21951),#18086,.F.);
#77382=ADVANCED_FACE('',(#21952),#18087,.F.);
#77383=ADVANCED_FACE('',(#21953),#18088,.F.);
#77384=ADVANCED_FACE('',(#21954),#18089,.F.);
#77385=ADVANCED_FACE('',(#21955,#330),#18090,.T.);
#77386=ADVANCED_FACE('',(#21956),#18091,.F.);
#77387=ADVANCED_FACE('',(#21957),#18092,.F.);
#77388=ADVANCED_FACE('',(#21958),#18093,.F.);
#77389=ADVANCED_FACE('',(#21959),#18094,.F.);
#77390=ADVANCED_FACE('',(#21960),#18095,.F.);
#77391=ADVANCED_FACE('',(#21961),#18096,.F.);
#77392=ADVANCED_FACE('',(#21962),#18097,.F.);
#77393=ADVANCED_FACE('',(#21963),#18098,.F.);
#77394=ADVANCED_FACE('',(#21964),#18099,.F.);
#77395=ADVANCED_FACE('',(#21965),#18100,.F.);
#77396=ADVANCED_FACE('',(#21966),#18101,.F.);
#77397=ADVANCED_FACE('',(#21967),#18102,.F.);
#77398=ADVANCED_FACE('',(#21968),#18103,.F.);
#77399=ADVANCED_FACE('',(#21969),#18104,.F.);
#77400=ADVANCED_FACE('',(#21970),#18105,.F.);
#77401=ADVANCED_FACE('',(#21971),#18106,.F.);
#77402=ADVANCED_FACE('',(#21972),#18107,.F.);
#77403=ADVANCED_FACE('',(#21973),#18108,.F.);
#77404=ADVANCED_FACE('',(#21974),#18109,.F.);
#77405=ADVANCED_FACE('',(#21975),#18110,.F.);
#77406=ADVANCED_FACE('',(#21976),#18111,.F.);
#77407=ADVANCED_FACE('',(#21977),#18112,.F.);
#77408=ADVANCED_FACE('',(#21978),#18113,.F.);
#77409=ADVANCED_FACE('',(#21979),#18114,.F.);
#77410=ADVANCED_FACE('',(#21980),#18115,.F.);
#77411=ADVANCED_FACE('',(#21981),#18116,.F.);
#77412=ADVANCED_FACE('',(#21982),#18117,.F.);
#77413=ADVANCED_FACE('',(#21983),#18118,.F.);
#77414=ADVANCED_FACE('',(#21984),#18119,.F.);
#77415=ADVANCED_FACE('',(#21985),#18120,.F.);
#77416=ADVANCED_FACE('',(#21986),#18121,.F.);
#77417=ADVANCED_FACE('',(#21987),#18122,.F.);
#77418=ADVANCED_FACE('',(#21988),#18123,.F.);
#77419=ADVANCED_FACE('',(#21989),#18124,.F.);
#77420=ADVANCED_FACE('',(#21990),#18125,.F.);
#77421=ADVANCED_FACE('',(#21991),#18126,.F.);
#77422=ADVANCED_FACE('',(#21992),#18127,.F.);
#77423=ADVANCED_FACE('',(#21993),#18128,.F.);
#77424=ADVANCED_FACE('',(#21994),#18129,.F.);
#77425=ADVANCED_FACE('',(#21995),#18130,.F.);
#77426=ADVANCED_FACE('',(#21996),#18131,.F.);
#77427=ADVANCED_FACE('',(#21997),#18132,.F.);
#77428=ADVANCED_FACE('',(#21998),#18133,.F.);
#77429=ADVANCED_FACE('',(#21999),#18134,.F.);
#77430=ADVANCED_FACE('',(#22000),#18135,.F.);
#77431=ADVANCED_FACE('',(#22001),#18136,.F.);
#77432=ADVANCED_FACE('',(#22002),#18137,.F.);
#77433=ADVANCED_FACE('',(#22003),#18138,.F.);
#77434=ADVANCED_FACE('',(#22004),#18139,.F.);
#77435=ADVANCED_FACE('',(#22005),#18140,.F.);
#77436=ADVANCED_FACE('',(#22006),#18141,.F.);
#77437=ADVANCED_FACE('',(#22007),#18142,.F.);
#77438=ADVANCED_FACE('',(#22008),#18143,.F.);
#77439=ADVANCED_FACE('',(#22009),#18144,.F.);
#77440=ADVANCED_FACE('',(#22010),#18145,.F.);
#77441=ADVANCED_FACE('',(#22011),#18146,.F.);
#77442=ADVANCED_FACE('',(#22012),#18147,.F.);
#77443=ADVANCED_FACE('',(#22013),#18148,.F.);
#77444=ADVANCED_FACE('',(#22014),#18149,.F.);
#77445=ADVANCED_FACE('',(#22015),#18150,.F.);
#77446=ADVANCED_FACE('',(#22016),#18151,.F.);
#77447=ADVANCED_FACE('',(#22017),#18152,.F.);
#77448=ADVANCED_FACE('',(#22018),#18153,.F.);
#77449=ADVANCED_FACE('',(#22019),#18154,.F.);
#77450=ADVANCED_FACE('',(#22020),#18155,.F.);
#77451=ADVANCED_FACE('',(#22021),#18156,.F.);
#77452=ADVANCED_FACE('',(#22022),#18157,.F.);
#77453=ADVANCED_FACE('',(#22023),#18158,.F.);
#77454=ADVANCED_FACE('',(#22024),#18159,.F.);
#77455=ADVANCED_FACE('',(#22025),#18160,.F.);
#77456=ADVANCED_FACE('',(#22026),#18161,.F.);
#77457=ADVANCED_FACE('',(#22027),#18162,.F.);
#77458=ADVANCED_FACE('',(#22028),#18163,.F.);
#77459=ADVANCED_FACE('',(#22029),#18164,.F.);
#77460=ADVANCED_FACE('',(#22030),#18165,.F.);
#77461=ADVANCED_FACE('',(#22031),#18166,.F.);
#77462=ADVANCED_FACE('',(#22032),#18167,.F.);
#77463=ADVANCED_FACE('',(#22033),#18168,.F.);
#77464=ADVANCED_FACE('',(#22034),#18169,.F.);
#77465=ADVANCED_FACE('',(#22035),#18170,.F.);
#77466=ADVANCED_FACE('',(#22036),#18171,.F.);
#77467=ADVANCED_FACE('',(#22037),#18172,.F.);
#77468=ADVANCED_FACE('',(#22038),#18173,.F.);
#77469=ADVANCED_FACE('',(#22039),#18174,.F.);
#77470=ADVANCED_FACE('',(#22040),#18175,.F.);
#77471=ADVANCED_FACE('',(#22041),#18176,.F.);
#77472=ADVANCED_FACE('',(#22042),#18177,.F.);
#77473=ADVANCED_FACE('',(#22043),#18178,.F.);
#77474=ADVANCED_FACE('',(#22044),#18179,.F.);
#77475=ADVANCED_FACE('',(#22045),#18180,.F.);
#77476=ADVANCED_FACE('',(#22046),#18181,.F.);
#77477=ADVANCED_FACE('',(#22047),#18182,.F.);
#77478=ADVANCED_FACE('',(#22048),#18183,.F.);
#77479=ADVANCED_FACE('',(#22049),#18184,.F.);
#77480=ADVANCED_FACE('',(#22050),#18185,.F.);
#77481=ADVANCED_FACE('',(#22051),#18186,.F.);
#77482=ADVANCED_FACE('',(#22052),#18187,.F.);
#77483=ADVANCED_FACE('',(#22053),#18188,.F.);
#77484=ADVANCED_FACE('',(#22054),#18189,.F.);
#77485=ADVANCED_FACE('',(#22055),#18190,.F.);
#77486=ADVANCED_FACE('',(#22056),#18191,.F.);
#77487=ADVANCED_FACE('',(#22057),#18192,.F.);
#77488=ADVANCED_FACE('',(#22058),#18193,.F.);
#77489=ADVANCED_FACE('',(#22059),#18194,.F.);
#77490=ADVANCED_FACE('',(#22060),#18195,.F.);
#77491=ADVANCED_FACE('',(#22061),#18196,.F.);
#77492=ADVANCED_FACE('',(#22062),#18197,.F.);
#77493=ADVANCED_FACE('',(#22063),#18198,.F.);
#77494=ADVANCED_FACE('',(#22064),#18199,.F.);
#77495=ADVANCED_FACE('',(#22065),#18200,.F.);
#77496=ADVANCED_FACE('',(#22066),#18201,.F.);
#77497=ADVANCED_FACE('',(#22067),#18202,.F.);
#77498=ADVANCED_FACE('',(#22068),#18203,.F.);
#77499=ADVANCED_FACE('',(#22069),#18204,.F.);
#77500=ADVANCED_FACE('',(#22070),#18205,.F.);
#77501=ADVANCED_FACE('',(#22071),#18206,.F.);
#77502=ADVANCED_FACE('',(#22072),#18207,.F.);
#77503=ADVANCED_FACE('',(#22073),#18208,.F.);
#77504=ADVANCED_FACE('',(#22074),#18209,.F.);
#77505=ADVANCED_FACE('',(#22075),#18210,.F.);
#77506=ADVANCED_FACE('',(#22076),#18211,.F.);
#77507=ADVANCED_FACE('',(#22077),#18212,.F.);
#77508=ADVANCED_FACE('',(#22078),#18213,.F.);
#77509=ADVANCED_FACE('',(#22079),#18214,.F.);
#77510=ADVANCED_FACE('',(#22080),#18215,.F.);
#77511=ADVANCED_FACE('',(#22081),#18216,.F.);
#77512=ADVANCED_FACE('',(#22082),#18217,.F.);
#77513=ADVANCED_FACE('',(#22083),#18218,.F.);
#77514=ADVANCED_FACE('',(#22084),#18219,.F.);
#77515=ADVANCED_FACE('',(#22085),#18220,.F.);
#77516=ADVANCED_FACE('',(#22086),#18221,.F.);
#77517=ADVANCED_FACE('',(#22087),#18222,.F.);
#77518=ADVANCED_FACE('',(#22088),#18223,.F.);
#77519=ADVANCED_FACE('',(#22089),#18224,.F.);
#77520=ADVANCED_FACE('',(#22090),#18225,.F.);
#77521=ADVANCED_FACE('',(#22091),#18226,.F.);
#77522=ADVANCED_FACE('',(#22092),#18227,.F.);
#77523=ADVANCED_FACE('',(#22093),#18228,.F.);
#77524=ADVANCED_FACE('',(#22094),#18229,.F.);
#77525=ADVANCED_FACE('',(#22095),#18230,.F.);
#77526=ADVANCED_FACE('',(#22096),#18231,.F.);
#77527=ADVANCED_FACE('',(#22097),#18232,.F.);
#77528=ADVANCED_FACE('',(#22098),#18233,.F.);
#77529=ADVANCED_FACE('',(#22099),#18234,.F.);
#77530=ADVANCED_FACE('',(#22100),#18235,.F.);
#77531=ADVANCED_FACE('',(#22101),#18236,.F.);
#77532=ADVANCED_FACE('',(#22102),#18237,.F.);
#77533=ADVANCED_FACE('',(#22103),#18238,.F.);
#77534=ADVANCED_FACE('',(#22104),#18239,.F.);
#77535=ADVANCED_FACE('',(#22105),#18240,.F.);
#77536=ADVANCED_FACE('',(#22106),#18241,.F.);
#77537=ADVANCED_FACE('',(#22107),#18242,.F.);
#77538=ADVANCED_FACE('',(#22108),#18243,.F.);
#77539=ADVANCED_FACE('',(#22109),#18244,.F.);
#77540=ADVANCED_FACE('',(#22110),#18245,.F.);
#77541=ADVANCED_FACE('',(#22111),#18246,.F.);
#77542=ADVANCED_FACE('',(#22112),#18247,.F.);
#77543=ADVANCED_FACE('',(#22113),#18248,.F.);
#77544=ADVANCED_FACE('',(#22114),#18249,.F.);
#77545=ADVANCED_FACE('',(#22115),#18250,.F.);
#77546=ADVANCED_FACE('',(#22116),#18251,.F.);
#77547=ADVANCED_FACE('',(#22117),#18252,.F.);
#77548=ADVANCED_FACE('',(#22118),#18253,.F.);
#77549=ADVANCED_FACE('',(#22119),#18254,.F.);
#77550=ADVANCED_FACE('',(#22120),#18255,.F.);
#77551=ADVANCED_FACE('',(#22121),#18256,.F.);
#77552=ADVANCED_FACE('',(#22122),#18257,.F.);
#77553=ADVANCED_FACE('',(#22123),#18258,.F.);
#77554=ADVANCED_FACE('',(#22124),#18259,.F.);
#77555=ADVANCED_FACE('',(#22125),#18260,.F.);
#77556=ADVANCED_FACE('',(#22126),#18261,.F.);
#77557=ADVANCED_FACE('',(#22127),#18262,.F.);
#77558=ADVANCED_FACE('',(#22128),#18263,.F.);
#77559=ADVANCED_FACE('',(#22129),#18264,.F.);
#77560=ADVANCED_FACE('',(#22130),#18265,.F.);
#77561=ADVANCED_FACE('',(#22131),#18266,.F.);
#77562=ADVANCED_FACE('',(#22132),#18267,.F.);
#77563=ADVANCED_FACE('',(#22133),#18268,.F.);
#77564=ADVANCED_FACE('',(#22134),#18269,.F.);
#77565=ADVANCED_FACE('',(#22135),#18270,.F.);
#77566=ADVANCED_FACE('',(#22136),#18271,.F.);
#77567=ADVANCED_FACE('',(#22137),#18272,.F.);
#77568=ADVANCED_FACE('',(#22138),#18273,.F.);
#77569=ADVANCED_FACE('',(#22139),#18274,.F.);
#77570=ADVANCED_FACE('',(#22140),#18275,.F.);
#77571=ADVANCED_FACE('',(#22141),#18276,.F.);
#77572=ADVANCED_FACE('',(#22142),#18277,.F.);
#77573=ADVANCED_FACE('',(#22143),#18278,.F.);
#77574=ADVANCED_FACE('',(#22144),#18279,.F.);
#77575=ADVANCED_FACE('',(#22145),#18280,.F.);
#77576=ADVANCED_FACE('',(#22146),#18281,.F.);
#77577=ADVANCED_FACE('',(#22147),#18282,.F.);
#77578=ADVANCED_FACE('',(#22148),#18283,.F.);
#77579=ADVANCED_FACE('',(#22149),#18284,.F.);
#77580=ADVANCED_FACE('',(#22150),#18285,.F.);
#77581=ADVANCED_FACE('',(#22151),#18286,.F.);
#77582=ADVANCED_FACE('',(#22152),#18287,.F.);
#77583=ADVANCED_FACE('',(#22153),#18288,.F.);
#77584=ADVANCED_FACE('',(#22154),#18289,.F.);
#77585=ADVANCED_FACE('',(#22155),#18290,.F.);
#77586=ADVANCED_FACE('',(#22156),#18291,.F.);
#77587=ADVANCED_FACE('',(#22157),#18292,.F.);
#77588=ADVANCED_FACE('',(#22158),#18293,.F.);
#77589=ADVANCED_FACE('',(#22159),#18294,.F.);
#77590=ADVANCED_FACE('',(#22160),#18295,.F.);
#77591=ADVANCED_FACE('',(#22161),#18296,.F.);
#77592=ADVANCED_FACE('',(#22162),#18297,.F.);
#77593=ADVANCED_FACE('',(#22163),#18298,.F.);
#77594=ADVANCED_FACE('',(#22164),#18299,.F.);
#77595=ADVANCED_FACE('',(#22165),#18300,.F.);
#77596=ADVANCED_FACE('',(#22166),#18301,.F.);
#77597=ADVANCED_FACE('',(#22167),#18302,.F.);
#77598=ADVANCED_FACE('',(#22168),#18303,.F.);
#77599=ADVANCED_FACE('',(#22169),#18304,.F.);
#77600=ADVANCED_FACE('',(#22170),#18305,.F.);
#77601=ADVANCED_FACE('',(#22171),#18306,.F.);
#77602=ADVANCED_FACE('',(#22172),#18307,.F.);
#77603=ADVANCED_FACE('',(#22173),#18308,.F.);
#77604=ADVANCED_FACE('',(#22174),#18309,.F.);
#77605=ADVANCED_FACE('',(#22175),#18310,.F.);
#77606=ADVANCED_FACE('',(#22176),#18311,.F.);
#77607=ADVANCED_FACE('',(#22177),#18312,.F.);
#77608=ADVANCED_FACE('',(#22178),#18313,.F.);
#77609=ADVANCED_FACE('',(#22179),#18314,.F.);
#77610=ADVANCED_FACE('',(#22180),#18315,.F.);
#77611=ADVANCED_FACE('',(#22181),#18316,.F.);
#77612=ADVANCED_FACE('',(#22182),#18317,.F.);
#77613=ADVANCED_FACE('',(#22183),#18318,.F.);
#77614=ADVANCED_FACE('',(#22184),#18319,.F.);
#77615=ADVANCED_FACE('',(#22185),#18320,.F.);
#77616=ADVANCED_FACE('',(#22186),#18321,.F.);
#77617=ADVANCED_FACE('',(#22187),#18322,.F.);
#77618=ADVANCED_FACE('',(#22188),#18323,.F.);
#77619=ADVANCED_FACE('',(#22189),#18324,.F.);
#77620=ADVANCED_FACE('',(#22190),#18325,.F.);
#77621=ADVANCED_FACE('',(#22191),#18326,.F.);
#77622=ADVANCED_FACE('',(#22192),#18327,.F.);
#77623=ADVANCED_FACE('',(#22193),#18328,.F.);
#77624=ADVANCED_FACE('',(#22194),#18329,.F.);
#77625=ADVANCED_FACE('',(#22195),#18330,.F.);
#77626=ADVANCED_FACE('',(#22196),#18331,.F.);
#77627=ADVANCED_FACE('',(#22197),#18332,.F.);
#77628=ADVANCED_FACE('',(#22198),#18333,.F.);
#77629=ADVANCED_FACE('',(#22199),#18334,.F.);
#77630=ADVANCED_FACE('',(#22200),#18335,.F.);
#77631=ADVANCED_FACE('',(#22201),#18336,.F.);
#77632=ADVANCED_FACE('',(#22202),#18337,.F.);
#77633=ADVANCED_FACE('',(#22203),#18338,.F.);
#77634=ADVANCED_FACE('',(#22204),#18339,.F.);
#77635=ADVANCED_FACE('',(#22205),#18340,.F.);
#77636=ADVANCED_FACE('',(#22206),#18341,.F.);
#77637=ADVANCED_FACE('',(#22207),#18342,.F.);
#77638=ADVANCED_FACE('',(#22208),#18343,.F.);
#77639=ADVANCED_FACE('',(#22209),#18344,.F.);
#77640=ADVANCED_FACE('',(#22210),#18345,.F.);
#77641=ADVANCED_FACE('',(#22211),#18346,.F.);
#77642=ADVANCED_FACE('',(#22212),#18347,.F.);
#77643=ADVANCED_FACE('',(#22213),#18348,.F.);
#77644=ADVANCED_FACE('',(#22214),#18349,.F.);
#77645=ADVANCED_FACE('',(#22215),#18350,.F.);
#77646=ADVANCED_FACE('',(#22216),#18351,.F.);
#77647=ADVANCED_FACE('',(#22217),#18352,.F.);
#77648=ADVANCED_FACE('',(#22218),#18353,.F.);
#77649=ADVANCED_FACE('',(#22219),#18354,.F.);
#77650=ADVANCED_FACE('',(#22220),#18355,.F.);
#77651=ADVANCED_FACE('',(#22221),#18356,.F.);
#77652=ADVANCED_FACE('',(#22222),#18357,.F.);
#77653=ADVANCED_FACE('',(#22223),#18358,.F.);
#77654=ADVANCED_FACE('',(#22224),#18359,.F.);
#77655=ADVANCED_FACE('',(#22225),#18360,.F.);
#77656=ADVANCED_FACE('',(#22226),#18361,.F.);
#77657=ADVANCED_FACE('',(#22227),#18362,.F.);
#77658=ADVANCED_FACE('',(#22228),#18363,.F.);
#77659=ADVANCED_FACE('',(#22229),#18364,.F.);
#77660=ADVANCED_FACE('',(#22230),#18365,.F.);
#77661=ADVANCED_FACE('',(#22231),#18366,.F.);
#77662=ADVANCED_FACE('',(#22232),#18367,.F.);
#77663=ADVANCED_FACE('',(#22233),#18368,.F.);
#77664=ADVANCED_FACE('',(#22234),#18369,.F.);
#77665=ADVANCED_FACE('',(#22235),#18370,.F.);
#77666=ADVANCED_FACE('',(#22236),#18371,.F.);
#77667=ADVANCED_FACE('',(#22237),#18372,.F.);
#77668=ADVANCED_FACE('',(#22238),#18373,.F.);
#77669=ADVANCED_FACE('',(#22239),#18374,.F.);
#77670=ADVANCED_FACE('',(#22240),#18375,.F.);
#77671=ADVANCED_FACE('',(#22241),#18376,.F.);
#77672=ADVANCED_FACE('',(#22242),#18377,.F.);
#77673=ADVANCED_FACE('',(#22243),#18378,.F.);
#77674=ADVANCED_FACE('',(#22244),#18379,.F.);
#77675=ADVANCED_FACE('',(#22245),#18380,.F.);
#77676=ADVANCED_FACE('',(#22246),#18381,.F.);
#77677=ADVANCED_FACE('',(#22247),#18382,.F.);
#77678=ADVANCED_FACE('',(#22248),#18383,.F.);
#77679=ADVANCED_FACE('',(#22249),#18384,.F.);
#77680=ADVANCED_FACE('',(#22250),#18385,.F.);
#77681=ADVANCED_FACE('',(#22251),#18386,.F.);
#77682=ADVANCED_FACE('',(#22252),#18387,.F.);
#77683=ADVANCED_FACE('',(#22253),#18388,.F.);
#77684=ADVANCED_FACE('',(#22254),#18389,.F.);
#77685=ADVANCED_FACE('',(#22255),#18390,.F.);
#77686=ADVANCED_FACE('',(#22256),#18391,.F.);
#77687=ADVANCED_FACE('',(#22257),#18392,.F.);
#77688=ADVANCED_FACE('',(#22258),#18393,.F.);
#77689=ADVANCED_FACE('',(#22259),#18394,.F.);
#77690=ADVANCED_FACE('',(#22260),#18395,.F.);
#77691=ADVANCED_FACE('',(#22261),#18396,.F.);
#77692=ADVANCED_FACE('',(#22262),#18397,.F.);
#77693=ADVANCED_FACE('',(#22263),#18398,.F.);
#77694=ADVANCED_FACE('',(#22264),#18399,.F.);
#77695=ADVANCED_FACE('',(#22265),#18400,.F.);
#77696=ADVANCED_FACE('',(#22266),#18401,.F.);
#77697=ADVANCED_FACE('',(#22267),#18402,.F.);
#77698=ADVANCED_FACE('',(#22268),#18403,.F.);
#77699=ADVANCED_FACE('',(#22269),#18404,.F.);
#77700=ADVANCED_FACE('',(#22270),#18405,.F.);
#77701=ADVANCED_FACE('',(#22271),#18406,.F.);
#77702=ADVANCED_FACE('',(#22272),#18407,.F.);
#77703=ADVANCED_FACE('',(#22273),#18408,.F.);
#77704=ADVANCED_FACE('',(#22274),#18409,.F.);
#77705=ADVANCED_FACE('',(#22275),#18410,.F.);
#77706=ADVANCED_FACE('',(#22276),#18411,.F.);
#77707=ADVANCED_FACE('',(#22277),#18412,.F.);
#77708=ADVANCED_FACE('',(#22278),#18413,.F.);
#77709=ADVANCED_FACE('',(#22279),#18414,.F.);
#77710=ADVANCED_FACE('',(#22280),#18415,.F.);
#77711=ADVANCED_FACE('',(#22281),#18416,.F.);
#77712=ADVANCED_FACE('',(#22282),#18417,.F.);
#77713=ADVANCED_FACE('',(#22283),#18418,.F.);
#77714=ADVANCED_FACE('',(#22284),#18419,.F.);
#77715=ADVANCED_FACE('',(#22285),#18420,.F.);
#77716=ADVANCED_FACE('',(#22286),#18421,.F.);
#77717=ADVANCED_FACE('',(#22287),#18422,.F.);
#77718=ADVANCED_FACE('',(#22288),#18423,.F.);
#77719=ADVANCED_FACE('',(#22289),#18424,.F.);
#77720=ADVANCED_FACE('',(#22290),#18425,.F.);
#77721=ADVANCED_FACE('',(#22291),#18426,.F.);
#77722=ADVANCED_FACE('',(#22292),#18427,.F.);
#77723=ADVANCED_FACE('',(#22293),#18428,.F.);
#77724=ADVANCED_FACE('',(#22294),#18429,.F.);
#77725=ADVANCED_FACE('',(#22295),#18430,.F.);
#77726=ADVANCED_FACE('',(#22296),#18431,.F.);
#77727=ADVANCED_FACE('',(#22297),#18432,.F.);
#77728=ADVANCED_FACE('',(#22298),#18433,.F.);
#77729=ADVANCED_FACE('',(#22299),#18434,.F.);
#77730=ADVANCED_FACE('',(#22300),#18435,.F.);
#77731=ADVANCED_FACE('',(#22301),#18436,.F.);
#77732=ADVANCED_FACE('',(#22302),#18437,.F.);
#77733=ADVANCED_FACE('',(#22303),#18438,.F.);
#77734=ADVANCED_FACE('',(#22304),#18439,.F.);
#77735=ADVANCED_FACE('',(#22305),#18440,.F.);
#77736=ADVANCED_FACE('',(#22306),#18441,.F.);
#77737=ADVANCED_FACE('',(#22307),#18442,.F.);
#77738=ADVANCED_FACE('',(#22308),#18443,.F.);
#77739=ADVANCED_FACE('',(#22309),#18444,.F.);
#77740=ADVANCED_FACE('',(#22310),#18445,.F.);
#77741=ADVANCED_FACE('',(#22311),#18446,.F.);
#77742=ADVANCED_FACE('',(#22312),#18447,.F.);
#77743=ADVANCED_FACE('',(#22313),#18448,.F.);
#77744=ADVANCED_FACE('',(#22314),#18449,.F.);
#77745=ADVANCED_FACE('',(#22315),#18450,.F.);
#77746=ADVANCED_FACE('',(#22316),#18451,.F.);
#77747=ADVANCED_FACE('',(#22317),#18452,.F.);
#77748=ADVANCED_FACE('',(#22318),#18453,.F.);
#77749=ADVANCED_FACE('',(#22319),#18454,.F.);
#77750=ADVANCED_FACE('',(#22320),#18455,.F.);
#77751=ADVANCED_FACE('',(#22321),#18456,.F.);
#77752=ADVANCED_FACE('',(#22322),#18457,.F.);
#77753=ADVANCED_FACE('',(#22323),#18458,.F.);
#77754=ADVANCED_FACE('',(#22324),#18459,.F.);
#77755=ADVANCED_FACE('',(#22325),#18460,.F.);
#77756=ADVANCED_FACE('',(#22326),#18461,.F.);
#77757=ADVANCED_FACE('',(#22327),#18462,.F.);
#77758=ADVANCED_FACE('',(#22328),#18463,.F.);
#77759=ADVANCED_FACE('',(#22329),#18464,.F.);
#77760=ADVANCED_FACE('',(#22330),#18465,.F.);
#77761=ADVANCED_FACE('',(#22331),#18466,.F.);
#77762=ADVANCED_FACE('',(#22332),#18467,.F.);
#77763=ADVANCED_FACE('',(#22333),#18468,.F.);
#77764=ADVANCED_FACE('',(#22334),#18469,.F.);
#77765=ADVANCED_FACE('',(#22335),#18470,.F.);
#77766=ADVANCED_FACE('',(#22336),#18471,.F.);
#77767=ADVANCED_FACE('',(#22337),#18472,.F.);
#77768=ADVANCED_FACE('',(#22338),#18473,.F.);
#77769=ADVANCED_FACE('',(#22339),#18474,.F.);
#77770=ADVANCED_FACE('',(#22340),#18475,.F.);
#77771=ADVANCED_FACE('',(#22341),#18476,.F.);
#77772=ADVANCED_FACE('',(#22342),#18477,.F.);
#77773=ADVANCED_FACE('',(#22343),#18478,.F.);
#77774=ADVANCED_FACE('',(#22344),#18479,.F.);
#77775=ADVANCED_FACE('',(#22345),#18480,.F.);
#77776=ADVANCED_FACE('',(#22346),#18481,.F.);
#77777=ADVANCED_FACE('',(#22347),#18482,.F.);
#77778=ADVANCED_FACE('',(#22348),#18483,.F.);
#77779=ADVANCED_FACE('',(#22349),#18484,.F.);
#77780=ADVANCED_FACE('',(#22350),#18485,.F.);
#77781=ADVANCED_FACE('',(#22351),#18486,.F.);
#77782=ADVANCED_FACE('',(#22352),#18487,.F.);
#77783=ADVANCED_FACE('',(#22353),#18488,.F.);
#77784=ADVANCED_FACE('',(#22354),#18489,.F.);
#77785=ADVANCED_FACE('',(#22355),#18490,.F.);
#77786=ADVANCED_FACE('',(#22356),#18491,.F.);
#77787=ADVANCED_FACE('',(#22357),#18492,.F.);
#77788=ADVANCED_FACE('',(#22358),#18493,.F.);
#77789=ADVANCED_FACE('',(#22359),#18494,.F.);
#77790=ADVANCED_FACE('',(#22360),#18495,.F.);
#77791=ADVANCED_FACE('',(#22361),#18496,.F.);
#77792=ADVANCED_FACE('',(#22362),#18497,.F.);
#77793=ADVANCED_FACE('',(#22363),#18498,.F.);
#77794=ADVANCED_FACE('',(#22364),#18499,.F.);
#77795=ADVANCED_FACE('',(#22365),#18500,.F.);
#77796=ADVANCED_FACE('',(#22366),#18501,.F.);
#77797=ADVANCED_FACE('',(#22367),#18502,.F.);
#77798=ADVANCED_FACE('',(#22368),#18503,.F.);
#77799=ADVANCED_FACE('',(#22369),#18504,.F.);
#77800=ADVANCED_FACE('',(#22370),#18505,.F.);
#77801=ADVANCED_FACE('',(#22371),#18506,.F.);
#77802=ADVANCED_FACE('',(#22372),#18507,.F.);
#77803=ADVANCED_FACE('',(#22373),#18508,.F.);
#77804=ADVANCED_FACE('',(#22374),#18509,.F.);
#77805=ADVANCED_FACE('',(#22375),#18510,.F.);
#77806=ADVANCED_FACE('',(#22376),#18511,.F.);
#77807=ADVANCED_FACE('',(#22377),#18512,.F.);
#77808=ADVANCED_FACE('',(#22378),#18513,.F.);
#77809=ADVANCED_FACE('',(#22379),#18514,.F.);
#77810=ADVANCED_FACE('',(#22380),#18515,.F.);
#77811=ADVANCED_FACE('',(#22381),#18516,.F.);
#77812=ADVANCED_FACE('',(#22382),#18517,.F.);
#77813=ADVANCED_FACE('',(#22383),#18518,.F.);
#77814=ADVANCED_FACE('',(#22384),#18519,.F.);
#77815=ADVANCED_FACE('',(#22385),#18520,.F.);
#77816=ADVANCED_FACE('',(#22386),#18521,.F.);
#77817=ADVANCED_FACE('',(#22387),#18522,.F.);
#77818=ADVANCED_FACE('',(#22388),#18523,.F.);
#77819=ADVANCED_FACE('',(#22389),#18524,.F.);
#77820=ADVANCED_FACE('',(#22390),#18525,.F.);
#77821=ADVANCED_FACE('',(#22391),#18526,.F.);
#77822=ADVANCED_FACE('',(#22392),#18527,.F.);
#77823=ADVANCED_FACE('',(#22393),#18528,.F.);
#77824=ADVANCED_FACE('',(#22394),#18529,.F.);
#77825=ADVANCED_FACE('',(#22395),#18530,.F.);
#77826=ADVANCED_FACE('',(#22396),#18531,.F.);
#77827=ADVANCED_FACE('',(#22397),#18532,.F.);
#77828=ADVANCED_FACE('',(#22398),#18533,.F.);
#77829=ADVANCED_FACE('',(#22399),#18534,.F.);
#77830=ADVANCED_FACE('',(#22400),#18535,.F.);
#77831=ADVANCED_FACE('',(#22401),#18536,.F.);
#77832=ADVANCED_FACE('',(#22402),#18537,.F.);
#77833=ADVANCED_FACE('',(#22403),#18538,.F.);
#77834=ADVANCED_FACE('',(#22404),#18539,.F.);
#77835=ADVANCED_FACE('',(#22405),#18540,.F.);
#77836=ADVANCED_FACE('',(#22406),#18541,.F.);
#77837=ADVANCED_FACE('',(#22407),#18542,.F.);
#77838=ADVANCED_FACE('',(#22408),#18543,.F.);
#77839=ADVANCED_FACE('',(#22409),#18544,.F.);
#77840=ADVANCED_FACE('',(#22410),#18545,.F.);
#77841=ADVANCED_FACE('',(#22411),#18546,.F.);
#77842=ADVANCED_FACE('',(#22412),#18547,.F.);
#77843=ADVANCED_FACE('',(#22413),#18548,.F.);
#77844=ADVANCED_FACE('',(#22414),#18549,.F.);
#77845=ADVANCED_FACE('',(#22415),#18550,.F.);
#77846=ADVANCED_FACE('',(#22416),#18551,.F.);
#77847=ADVANCED_FACE('',(#22417),#18552,.F.);
#77848=ADVANCED_FACE('',(#22418),#18553,.F.);
#77849=ADVANCED_FACE('',(#22419),#18554,.F.);
#77850=ADVANCED_FACE('',(#22420),#18555,.F.);
#77851=ADVANCED_FACE('',(#22421),#18556,.F.);
#77852=ADVANCED_FACE('',(#22422),#18557,.F.);
#77853=ADVANCED_FACE('',(#22423),#18558,.F.);
#77854=ADVANCED_FACE('',(#22424),#18559,.F.);
#77855=ADVANCED_FACE('',(#22425),#18560,.F.);
#77856=ADVANCED_FACE('',(#22426),#18561,.F.);
#77857=ADVANCED_FACE('',(#22427),#18562,.F.);
#77858=ADVANCED_FACE('',(#22428),#18563,.F.);
#77859=ADVANCED_FACE('',(#22429),#18564,.F.);
#77860=ADVANCED_FACE('',(#22430),#18565,.F.);
#77861=ADVANCED_FACE('',(#22431),#18566,.F.);
#77862=ADVANCED_FACE('',(#22432),#18567,.F.);
#77863=ADVANCED_FACE('',(#22433),#18568,.F.);
#77864=ADVANCED_FACE('',(#22434),#18569,.F.);
#77865=ADVANCED_FACE('',(#22435),#18570,.F.);
#77866=ADVANCED_FACE('',(#22436),#18571,.F.);
#77867=ADVANCED_FACE('',(#22437),#18572,.F.);
#77868=ADVANCED_FACE('',(#22438),#18573,.F.);
#77869=ADVANCED_FACE('',(#22439),#18574,.F.);
#77870=ADVANCED_FACE('',(#22440),#18575,.F.);
#77871=ADVANCED_FACE('',(#22441),#18576,.F.);
#77872=ADVANCED_FACE('',(#22442),#18577,.F.);
#77873=ADVANCED_FACE('',(#22443),#18578,.F.);
#77874=ADVANCED_FACE('',(#22444),#18579,.F.);
#77875=ADVANCED_FACE('',(#22445),#18580,.F.);
#77876=ADVANCED_FACE('',(#22446),#18581,.F.);
#77877=ADVANCED_FACE('',(#22447),#18582,.F.);
#77878=ADVANCED_FACE('',(#22448),#18583,.F.);
#77879=ADVANCED_FACE('',(#22449),#18584,.F.);
#77880=ADVANCED_FACE('',(#22450),#18585,.F.);
#77881=ADVANCED_FACE('',(#22451),#18586,.F.);
#77882=ADVANCED_FACE('',(#22452),#18587,.F.);
#77883=ADVANCED_FACE('',(#22453),#18588,.F.);
#77884=ADVANCED_FACE('',(#22454),#18589,.F.);
#77885=ADVANCED_FACE('',(#22455),#18590,.F.);
#77886=ADVANCED_FACE('',(#22456),#18591,.F.);
#77887=ADVANCED_FACE('',(#22457),#18592,.F.);
#77888=ADVANCED_FACE('',(#22458),#18593,.F.);
#77889=ADVANCED_FACE('',(#22459),#18594,.F.);
#77890=ADVANCED_FACE('',(#22460),#18595,.F.);
#77891=ADVANCED_FACE('',(#22461),#18596,.F.);
#77892=ADVANCED_FACE('',(#22462),#18597,.F.);
#77893=ADVANCED_FACE('',(#22463),#18598,.F.);
#77894=ADVANCED_FACE('',(#22464),#18599,.F.);
#77895=ADVANCED_FACE('',(#22465),#18600,.F.);
#77896=ADVANCED_FACE('',(#22466),#18601,.F.);
#77897=ADVANCED_FACE('',(#22467),#18602,.F.);
#77898=ADVANCED_FACE('',(#22468),#18603,.F.);
#77899=ADVANCED_FACE('',(#22469),#18604,.F.);
#77900=ADVANCED_FACE('',(#22470),#18605,.F.);
#77901=ADVANCED_FACE('',(#22471),#18606,.F.);
#77902=ADVANCED_FACE('',(#22472),#18607,.F.);
#77903=ADVANCED_FACE('',(#22473),#18608,.F.);
#77904=ADVANCED_FACE('',(#22474),#18609,.F.);
#77905=ADVANCED_FACE('',(#22475),#18610,.F.);
#77906=ADVANCED_FACE('',(#22476),#18611,.F.);
#77907=ADVANCED_FACE('',(#22477),#18612,.F.);
#77908=ADVANCED_FACE('',(#22478),#18613,.F.);
#77909=ADVANCED_FACE('',(#22479),#18614,.F.);
#77910=ADVANCED_FACE('',(#22480),#18615,.F.);
#77911=ADVANCED_FACE('',(#22481),#18616,.F.);
#77912=ADVANCED_FACE('',(#22482),#18617,.F.);
#77913=ADVANCED_FACE('',(#22483),#18618,.F.);
#77914=ADVANCED_FACE('',(#22484),#18619,.F.);
#77915=ADVANCED_FACE('',(#22485),#18620,.F.);
#77916=ADVANCED_FACE('',(#22486),#18621,.F.);
#77917=ADVANCED_FACE('',(#22487),#18622,.F.);
#77918=ADVANCED_FACE('',(#22488),#18623,.F.);
#77919=ADVANCED_FACE('',(#22489),#18624,.F.);
#77920=ADVANCED_FACE('',(#22490),#18625,.F.);
#77921=ADVANCED_FACE('',(#22491),#18626,.F.);
#77922=ADVANCED_FACE('',(#22492),#18627,.F.);
#77923=ADVANCED_FACE('',(#22493),#18628,.F.);
#77924=ADVANCED_FACE('',(#22494),#18629,.F.);
#77925=ADVANCED_FACE('',(#22495),#18630,.F.);
#77926=ADVANCED_FACE('',(#22496),#18631,.F.);
#77927=ADVANCED_FACE('',(#22497),#18632,.F.);
#77928=ADVANCED_FACE('',(#22498),#18633,.F.);
#77929=ADVANCED_FACE('',(#22499),#18634,.F.);
#77930=ADVANCED_FACE('',(#22500),#18635,.F.);
#77931=ADVANCED_FACE('',(#22501),#18636,.F.);
#77932=ADVANCED_FACE('',(#22502),#18637,.F.);
#77933=ADVANCED_FACE('',(#22503),#18638,.F.);
#77934=ADVANCED_FACE('',(#22504),#18639,.F.);
#77935=ADVANCED_FACE('',(#22505),#18640,.F.);
#77936=ADVANCED_FACE('',(#22506),#18641,.F.);
#77937=ADVANCED_FACE('',(#22507),#18642,.F.);
#77938=ADVANCED_FACE('',(#22508),#18643,.F.);
#77939=ADVANCED_FACE('',(#22509),#18644,.F.);
#77940=ADVANCED_FACE('',(#22510),#18645,.F.);
#77941=ADVANCED_FACE('',(#22511),#18646,.F.);
#77942=ADVANCED_FACE('',(#22512),#18647,.F.);
#77943=ADVANCED_FACE('',(#22513),#18648,.F.);
#77944=ADVANCED_FACE('',(#22514),#18649,.F.);
#77945=ADVANCED_FACE('',(#22515),#18650,.F.);
#77946=ADVANCED_FACE('',(#22516),#18651,.F.);
#77947=ADVANCED_FACE('',(#22517),#18652,.F.);
#77948=ADVANCED_FACE('',(#22518),#18653,.F.);
#77949=ADVANCED_FACE('',(#22519),#18654,.F.);
#77950=ADVANCED_FACE('',(#22520),#18655,.F.);
#77951=ADVANCED_FACE('',(#22521),#18656,.F.);
#77952=ADVANCED_FACE('',(#22522),#18657,.F.);
#77953=ADVANCED_FACE('',(#22523),#18658,.F.);
#77954=ADVANCED_FACE('',(#22524),#18659,.F.);
#77955=ADVANCED_FACE('',(#22525),#18660,.F.);
#77956=ADVANCED_FACE('',(#22526),#18661,.F.);
#77957=ADVANCED_FACE('',(#22527),#18662,.F.);
#77958=ADVANCED_FACE('',(#22528),#18663,.F.);
#77959=ADVANCED_FACE('',(#22529),#18664,.F.);
#77960=ADVANCED_FACE('',(#22530),#18665,.F.);
#77961=ADVANCED_FACE('',(#22531),#18666,.F.);
#77962=ADVANCED_FACE('',(#22532),#18667,.F.);
#77963=ADVANCED_FACE('',(#22533),#18668,.F.);
#77964=ADVANCED_FACE('',(#22534),#18669,.F.);
#77965=ADVANCED_FACE('',(#22535),#18670,.F.);
#77966=ADVANCED_FACE('',(#22536),#18671,.F.);
#77967=ADVANCED_FACE('',(#22537),#18672,.F.);
#77968=ADVANCED_FACE('',(#22538),#18673,.F.);
#77969=ADVANCED_FACE('',(#22539),#18674,.F.);
#77970=ADVANCED_FACE('',(#22540),#18675,.F.);
#77971=ADVANCED_FACE('',(#22541),#18676,.F.);
#77972=ADVANCED_FACE('',(#22542),#18677,.F.);
#77973=ADVANCED_FACE('',(#22543),#18678,.F.);
#77974=ADVANCED_FACE('',(#22544),#18679,.F.);
#77975=ADVANCED_FACE('',(#22545),#18680,.F.);
#77976=ADVANCED_FACE('',(#22546),#18681,.F.);
#77977=ADVANCED_FACE('',(#22547),#18682,.F.);
#77978=ADVANCED_FACE('',(#22548),#18683,.F.);
#77979=ADVANCED_FACE('',(#22549),#18684,.F.);
#77980=ADVANCED_FACE('',(#22550),#18685,.F.);
#77981=ADVANCED_FACE('',(#22551),#18686,.F.);
#77982=ADVANCED_FACE('',(#22552),#18687,.F.);
#77983=ADVANCED_FACE('',(#22553),#18688,.F.);
#77984=ADVANCED_FACE('',(#22554),#18689,.F.);
#77985=ADVANCED_FACE('',(#22555),#18690,.F.);
#77986=ADVANCED_FACE('',(#22556),#18691,.F.);
#77987=ADVANCED_FACE('',(#22557),#18692,.F.);
#77988=ADVANCED_FACE('',(#22558),#18693,.F.);
#77989=ADVANCED_FACE('',(#22559),#18694,.F.);
#77990=ADVANCED_FACE('',(#22560),#18695,.F.);
#77991=ADVANCED_FACE('',(#22561),#18696,.F.);
#77992=ADVANCED_FACE('',(#22562),#18697,.F.);
#77993=ADVANCED_FACE('',(#22563),#18698,.F.);
#77994=ADVANCED_FACE('',(#22564),#18699,.F.);
#77995=ADVANCED_FACE('',(#22565),#18700,.F.);
#77996=ADVANCED_FACE('',(#22566),#18701,.F.);
#77997=ADVANCED_FACE('',(#22567),#18702,.F.);
#77998=ADVANCED_FACE('',(#22568),#18703,.F.);
#77999=ADVANCED_FACE('',(#22569),#18704,.F.);
#78000=ADVANCED_FACE('',(#22570),#18705,.F.);
#78001=ADVANCED_FACE('',(#22571),#18706,.F.);
#78002=ADVANCED_FACE('',(#22572),#18707,.F.);
#78003=ADVANCED_FACE('',(#22573),#18708,.F.);
#78004=ADVANCED_FACE('',(#22574),#18709,.F.);
#78005=ADVANCED_FACE('',(#22575),#18710,.F.);
#78006=ADVANCED_FACE('',(#22576),#18711,.F.);
#78007=ADVANCED_FACE('',(#22577),#18712,.F.);
#78008=ADVANCED_FACE('',(#22578),#18713,.F.);
#78009=ADVANCED_FACE('',(#22579),#18714,.F.);
#78010=ADVANCED_FACE('',(#22580),#18715,.F.);
#78011=ADVANCED_FACE('',(#22581),#18716,.F.);
#78012=ADVANCED_FACE('',(#22582),#18717,.F.);
#78013=ADVANCED_FACE('',(#22583),#18718,.F.);
#78014=ADVANCED_FACE('',(#22584),#18719,.F.);
#78015=ADVANCED_FACE('',(#22585),#18720,.F.);
#78016=ADVANCED_FACE('',(#22586),#18721,.F.);
#78017=ADVANCED_FACE('',(#22587),#18722,.F.);
#78018=ADVANCED_FACE('',(#22588),#18723,.F.);
#78019=ADVANCED_FACE('',(#22589),#18724,.F.);
#78020=ADVANCED_FACE('',(#22590),#18725,.F.);
#78021=ADVANCED_FACE('',(#22591),#18726,.F.);
#78022=ADVANCED_FACE('',(#22592),#18727,.F.);
#78023=ADVANCED_FACE('',(#22593),#18728,.F.);
#78024=ADVANCED_FACE('',(#22594),#18729,.F.);
#78025=ADVANCED_FACE('',(#22595),#18730,.F.);
#78026=ADVANCED_FACE('',(#22596),#18731,.F.);
#78027=ADVANCED_FACE('',(#22597),#18732,.F.);
#78028=ADVANCED_FACE('',(#22598),#18733,.F.);
#78029=ADVANCED_FACE('',(#22599),#18734,.F.);
#78030=ADVANCED_FACE('',(#22600),#18735,.F.);
#78031=ADVANCED_FACE('',(#22601),#18736,.F.);
#78032=ADVANCED_FACE('',(#22602),#18737,.F.);
#78033=ADVANCED_FACE('',(#22603),#18738,.F.);
#78034=ADVANCED_FACE('',(#22604),#18739,.F.);
#78035=ADVANCED_FACE('',(#22605),#18740,.F.);
#78036=ADVANCED_FACE('',(#22606),#18741,.F.);
#78037=ADVANCED_FACE('',(#22607),#18742,.F.);
#78038=ADVANCED_FACE('',(#22608),#18743,.F.);
#78039=ADVANCED_FACE('',(#22609),#18744,.F.);
#78040=ADVANCED_FACE('',(#22610),#18745,.F.);
#78041=ADVANCED_FACE('',(#22611),#18746,.F.);
#78042=ADVANCED_FACE('',(#22612),#18747,.F.);
#78043=ADVANCED_FACE('',(#22613),#18748,.F.);
#78044=ADVANCED_FACE('',(#22614),#18749,.F.);
#78045=ADVANCED_FACE('',(#22615),#18750,.F.);
#78046=ADVANCED_FACE('',(#22616),#18751,.F.);
#78047=ADVANCED_FACE('',(#22617),#18752,.F.);
#78048=ADVANCED_FACE('',(#22618),#18753,.F.);
#78049=ADVANCED_FACE('',(#22619),#18754,.F.);
#78050=ADVANCED_FACE('',(#22620),#18755,.F.);
#78051=ADVANCED_FACE('',(#22621),#18756,.F.);
#78052=ADVANCED_FACE('',(#22622),#18757,.F.);
#78053=ADVANCED_FACE('',(#22623),#18758,.F.);
#78054=ADVANCED_FACE('',(#22624),#18759,.F.);
#78055=ADVANCED_FACE('',(#22625),#18760,.F.);
#78056=ADVANCED_FACE('',(#22626),#18761,.F.);
#78057=ADVANCED_FACE('',(#22627),#18762,.F.);
#78058=ADVANCED_FACE('',(#22628),#18763,.F.);
#78059=ADVANCED_FACE('',(#22629),#18764,.F.);
#78060=ADVANCED_FACE('',(#22630),#18765,.F.);
#78061=ADVANCED_FACE('',(#22631),#18766,.F.);
#78062=ADVANCED_FACE('',(#22632),#18767,.F.);
#78063=ADVANCED_FACE('',(#22633),#18768,.F.);
#78064=ADVANCED_FACE('',(#22634),#18769,.F.);
#78065=ADVANCED_FACE('',(#22635),#18770,.F.);
#78066=ADVANCED_FACE('',(#22636),#18771,.F.);
#78067=ADVANCED_FACE('',(#22637),#18772,.F.);
#78068=ADVANCED_FACE('',(#22638),#18773,.F.);
#78069=ADVANCED_FACE('',(#22639),#18774,.F.);
#78070=ADVANCED_FACE('',(#22640),#18775,.F.);
#78071=ADVANCED_FACE('',(#22641),#18776,.F.);
#78072=ADVANCED_FACE('',(#22642),#18777,.F.);
#78073=ADVANCED_FACE('',(#22643),#18778,.F.);
#78074=ADVANCED_FACE('',(#22644),#18779,.F.);
#78075=ADVANCED_FACE('',(#22645),#18780,.F.);
#78076=ADVANCED_FACE('',(#22646),#18781,.F.);
#78077=ADVANCED_FACE('',(#22647),#18782,.F.);
#78078=ADVANCED_FACE('',(#22648),#18783,.F.);
#78079=ADVANCED_FACE('',(#22649),#18784,.F.);
#78080=ADVANCED_FACE('',(#22650),#18785,.F.);
#78081=ADVANCED_FACE('',(#22651),#18786,.F.);
#78082=ADVANCED_FACE('',(#22652),#18787,.F.);
#78083=ADVANCED_FACE('',(#22653),#18788,.F.);
#78084=ADVANCED_FACE('',(#22654),#18789,.F.);
#78085=ADVANCED_FACE('',(#22655),#18790,.F.);
#78086=ADVANCED_FACE('',(#22656),#18791,.F.);
#78087=ADVANCED_FACE('',(#22657),#18792,.F.);
#78088=ADVANCED_FACE('',(#22658),#18793,.F.);
#78089=ADVANCED_FACE('',(#22659),#18794,.F.);
#78090=ADVANCED_FACE('',(#22660),#18795,.F.);
#78091=ADVANCED_FACE('',(#22661),#18796,.F.);
#78092=ADVANCED_FACE('',(#22662),#18797,.F.);
#78093=ADVANCED_FACE('',(#22663),#18798,.F.);
#78094=ADVANCED_FACE('',(#22664),#18799,.F.);
#78095=ADVANCED_FACE('',(#22665),#18800,.F.);
#78096=ADVANCED_FACE('',(#22666),#18801,.F.);
#78097=ADVANCED_FACE('',(#22667),#18802,.F.);
#78098=ADVANCED_FACE('',(#22668),#18803,.F.);
#78099=ADVANCED_FACE('',(#22669),#18804,.F.);
#78100=ADVANCED_FACE('',(#22670),#18805,.F.);
#78101=ADVANCED_FACE('',(#22671),#18806,.F.);
#78102=ADVANCED_FACE('',(#22672),#18807,.F.);
#78103=ADVANCED_FACE('',(#22673),#18808,.F.);
#78104=ADVANCED_FACE('',(#22674),#18809,.F.);
#78105=ADVANCED_FACE('',(#22675),#18810,.F.);
#78106=ADVANCED_FACE('',(#22676),#18811,.F.);
#78107=ADVANCED_FACE('',(#22677),#18812,.F.);
#78108=ADVANCED_FACE('',(#22678),#18813,.F.);
#78109=ADVANCED_FACE('',(#22679),#18814,.F.);
#78110=ADVANCED_FACE('',(#22680),#18815,.F.);
#78111=ADVANCED_FACE('',(#22681),#18816,.F.);
#78112=ADVANCED_FACE('',(#22682),#18817,.F.);
#78113=ADVANCED_FACE('',(#22683),#18818,.F.);
#78114=ADVANCED_FACE('',(#22684),#18819,.F.);
#78115=ADVANCED_FACE('',(#22685),#18820,.F.);
#78116=ADVANCED_FACE('',(#22686),#18821,.F.);
#78117=ADVANCED_FACE('',(#22687),#18822,.F.);
#78118=ADVANCED_FACE('',(#22688),#18823,.F.);
#78119=ADVANCED_FACE('',(#22689),#18824,.F.);
#78120=ADVANCED_FACE('',(#22690),#18825,.F.);
#78121=ADVANCED_FACE('',(#22691),#18826,.F.);
#78122=ADVANCED_FACE('',(#22692),#18827,.F.);
#78123=ADVANCED_FACE('',(#22693),#18828,.F.);
#78124=ADVANCED_FACE('',(#22694),#18829,.F.);
#78125=ADVANCED_FACE('',(#22695),#18830,.F.);
#78126=ADVANCED_FACE('',(#22696),#18831,.F.);
#78127=ADVANCED_FACE('',(#22697),#18832,.F.);
#78128=ADVANCED_FACE('',(#22698),#18833,.F.);
#78129=ADVANCED_FACE('',(#22699),#18834,.F.);
#78130=ADVANCED_FACE('',(#22700),#18835,.F.);
#78131=ADVANCED_FACE('',(#22701),#18836,.F.);
#78132=ADVANCED_FACE('',(#22702),#18837,.F.);
#78133=ADVANCED_FACE('',(#22703),#18838,.F.);
#78134=ADVANCED_FACE('',(#22704),#18839,.F.);
#78135=ADVANCED_FACE('',(#22705),#18840,.F.);
#78136=ADVANCED_FACE('',(#22706),#18841,.F.);
#78137=ADVANCED_FACE('',(#22707),#18842,.F.);
#78138=ADVANCED_FACE('',(#22708),#18843,.F.);
#78139=ADVANCED_FACE('',(#22709),#18844,.F.);
#78140=ADVANCED_FACE('',(#22710),#18845,.F.);
#78141=ADVANCED_FACE('',(#22711),#18846,.F.);
#78142=ADVANCED_FACE('',(#22712),#18847,.F.);
#78143=ADVANCED_FACE('',(#22713),#18848,.F.);
#78144=ADVANCED_FACE('',(#22714),#18849,.F.);
#78145=ADVANCED_FACE('',(#22715),#18850,.F.);
#78146=ADVANCED_FACE('',(#22716),#18851,.F.);
#78147=ADVANCED_FACE('',(#22717),#18852,.F.);
#78148=ADVANCED_FACE('',(#22718),#18853,.F.);
#78149=ADVANCED_FACE('',(#22719),#18854,.F.);
#78150=ADVANCED_FACE('',(#22720),#18855,.F.);
#78151=ADVANCED_FACE('',(#22721),#18856,.F.);
#78152=ADVANCED_FACE('',(#22722),#18857,.F.);
#78153=ADVANCED_FACE('',(#22723),#18858,.F.);
#78154=ADVANCED_FACE('',(#22724),#18859,.F.);
#78155=ADVANCED_FACE('',(#22725),#18860,.F.);
#78156=ADVANCED_FACE('',(#22726),#18861,.F.);
#78157=ADVANCED_FACE('',(#22727),#18862,.F.);
#78158=ADVANCED_FACE('',(#22728),#18863,.F.);
#78159=ADVANCED_FACE('',(#22729),#18864,.F.);
#78160=ADVANCED_FACE('',(#22730),#18865,.F.);
#78161=ADVANCED_FACE('',(#22731),#18866,.F.);
#78162=ADVANCED_FACE('',(#22732),#18867,.F.);
#78163=ADVANCED_FACE('',(#22733),#18868,.F.);
#78164=ADVANCED_FACE('',(#22734),#18869,.F.);
#78165=ADVANCED_FACE('',(#22735),#18870,.F.);
#78166=ADVANCED_FACE('',(#22736),#18871,.F.);
#78167=ADVANCED_FACE('',(#22737),#18872,.F.);
#78168=ADVANCED_FACE('',(#22738),#18873,.F.);
#78169=ADVANCED_FACE('',(#22739),#18874,.F.);
#78170=ADVANCED_FACE('',(#22740),#18875,.F.);
#78171=ADVANCED_FACE('',(#22741),#18876,.F.);
#78172=ADVANCED_FACE('',(#22742),#18877,.F.);
#78173=ADVANCED_FACE('',(#22743),#18878,.F.);
#78174=ADVANCED_FACE('',(#22744),#18879,.F.);
#78175=ADVANCED_FACE('',(#22745),#18880,.F.);
#78176=ADVANCED_FACE('',(#22746),#18881,.F.);
#78177=ADVANCED_FACE('',(#22747),#18882,.F.);
#78178=ADVANCED_FACE('',(#22748),#18883,.F.);
#78179=ADVANCED_FACE('',(#22749),#18884,.F.);
#78180=ADVANCED_FACE('',(#22750),#18885,.F.);
#78181=ADVANCED_FACE('',(#22751),#18886,.F.);
#78182=ADVANCED_FACE('',(#22752),#18887,.F.);
#78183=ADVANCED_FACE('',(#22753),#18888,.F.);
#78184=ADVANCED_FACE('',(#22754),#18889,.F.);
#78185=ADVANCED_FACE('',(#22755),#18890,.F.);
#78186=ADVANCED_FACE('',(#22756),#18891,.F.);
#78187=ADVANCED_FACE('',(#22757),#18892,.F.);
#78188=ADVANCED_FACE('',(#22758),#18893,.F.);
#78189=ADVANCED_FACE('',(#22759),#18894,.F.);
#78190=ADVANCED_FACE('',(#22760),#18895,.F.);
#78191=ADVANCED_FACE('',(#22761),#18896,.F.);
#78192=ADVANCED_FACE('',(#22762),#18897,.F.);
#78193=ADVANCED_FACE('',(#22763),#18898,.F.);
#78194=ADVANCED_FACE('',(#22764),#18899,.F.);
#78195=ADVANCED_FACE('',(#22765),#18900,.F.);
#78196=ADVANCED_FACE('',(#22766),#18901,.F.);
#78197=ADVANCED_FACE('',(#22767),#18902,.F.);
#78198=ADVANCED_FACE('',(#22768),#18903,.F.);
#78199=ADVANCED_FACE('',(#22769),#18904,.F.);
#78200=ADVANCED_FACE('',(#22770),#18905,.F.);
#78201=ADVANCED_FACE('',(#22771),#18906,.F.);
#78202=ADVANCED_FACE('',(#22772),#18907,.F.);
#78203=ADVANCED_FACE('',(#22773),#18908,.F.);
#78204=ADVANCED_FACE('',(#22774),#18909,.F.);
#78205=ADVANCED_FACE('',(#22775),#18910,.F.);
#78206=ADVANCED_FACE('',(#22776),#18911,.F.);
#78207=ADVANCED_FACE('',(#22777),#18912,.F.);
#78208=ADVANCED_FACE('',(#22778),#18913,.F.);
#78209=ADVANCED_FACE('',(#22779),#18914,.F.);
#78210=ADVANCED_FACE('',(#22780),#18915,.F.);
#78211=ADVANCED_FACE('',(#22781),#18916,.F.);
#78212=ADVANCED_FACE('',(#22782),#18917,.F.);
#78213=ADVANCED_FACE('',(#22783),#18918,.F.);
#78214=ADVANCED_FACE('',(#22784),#18919,.F.);
#78215=ADVANCED_FACE('',(#22785),#18920,.F.);
#78216=ADVANCED_FACE('',(#22786),#18921,.F.);
#78217=ADVANCED_FACE('',(#22787),#18922,.F.);
#78218=ADVANCED_FACE('',(#22788),#18923,.F.);
#78219=ADVANCED_FACE('',(#22789),#18924,.F.);
#78220=ADVANCED_FACE('',(#22790),#18925,.F.);
#78221=ADVANCED_FACE('',(#22791),#18926,.F.);
#78222=ADVANCED_FACE('',(#22792),#18927,.F.);
#78223=ADVANCED_FACE('',(#22793),#18928,.F.);
#78224=ADVANCED_FACE('',(#22794),#18929,.F.);
#78225=ADVANCED_FACE('',(#22795),#18930,.F.);
#78226=ADVANCED_FACE('',(#22796),#18931,.F.);
#78227=ADVANCED_FACE('',(#22797),#18932,.F.);
#78228=ADVANCED_FACE('',(#22798),#18933,.F.);
#78229=ADVANCED_FACE('',(#22799),#18934,.F.);
#78230=ADVANCED_FACE('',(#22800),#18935,.F.);
#78231=ADVANCED_FACE('',(#22801),#18936,.F.);
#78232=ADVANCED_FACE('',(#22802),#18937,.F.);
#78233=ADVANCED_FACE('',(#22803),#18938,.F.);
#78234=ADVANCED_FACE('',(#22804),#18939,.F.);
#78235=ADVANCED_FACE('',(#22805),#18940,.F.);
#78236=ADVANCED_FACE('',(#22806),#18941,.F.);
#78237=ADVANCED_FACE('',(#22807),#18942,.F.);
#78238=ADVANCED_FACE('',(#22808),#18943,.F.);
#78239=ADVANCED_FACE('',(#22809),#18944,.F.);
#78240=ADVANCED_FACE('',(#22810),#18945,.F.);
#78241=ADVANCED_FACE('',(#22811),#18946,.F.);
#78242=ADVANCED_FACE('',(#22812),#18947,.F.);
#78243=ADVANCED_FACE('',(#22813),#18948,.F.);
#78244=ADVANCED_FACE('',(#22814),#18949,.F.);
#78245=ADVANCED_FACE('',(#22815),#18950,.F.);
#78246=ADVANCED_FACE('',(#22816),#18951,.F.);
#78247=ADVANCED_FACE('',(#22817),#18952,.F.);
#78248=ADVANCED_FACE('',(#22818),#18953,.F.);
#78249=ADVANCED_FACE('',(#22819),#18954,.F.);
#78250=ADVANCED_FACE('',(#22820),#18955,.F.);
#78251=ADVANCED_FACE('',(#22821),#18956,.F.);
#78252=ADVANCED_FACE('',(#22822),#18957,.F.);
#78253=ADVANCED_FACE('',(#22823),#18958,.F.);
#78254=ADVANCED_FACE('',(#22824),#18959,.F.);
#78255=ADVANCED_FACE('',(#22825),#18960,.F.);
#78256=ADVANCED_FACE('',(#22826),#18961,.F.);
#78257=ADVANCED_FACE('',(#22827),#18962,.F.);
#78258=ADVANCED_FACE('',(#22828),#18963,.F.);
#78259=ADVANCED_FACE('',(#22829),#18964,.F.);
#78260=ADVANCED_FACE('',(#22830),#18965,.F.);
#78261=ADVANCED_FACE('',(#22831),#18966,.F.);
#78262=ADVANCED_FACE('',(#22832),#18967,.F.);
#78263=ADVANCED_FACE('',(#22833),#18968,.F.);
#78264=ADVANCED_FACE('',(#22834),#18969,.F.);
#78265=ADVANCED_FACE('',(#22835),#18970,.F.);
#78266=ADVANCED_FACE('',(#22836),#18971,.F.);
#78267=ADVANCED_FACE('',(#22837),#18972,.F.);
#78268=ADVANCED_FACE('',(#22838),#18973,.F.);
#78269=ADVANCED_FACE('',(#22839),#18974,.F.);
#78270=ADVANCED_FACE('',(#22840),#18975,.F.);
#78271=ADVANCED_FACE('',(#22841),#18976,.F.);
#78272=ADVANCED_FACE('',(#22842),#18977,.F.);
#78273=ADVANCED_FACE('',(#22843),#18978,.F.);
#78274=ADVANCED_FACE('',(#22844),#18979,.F.);
#78275=ADVANCED_FACE('',(#22845),#18980,.F.);
#78276=ADVANCED_FACE('',(#22846),#18981,.F.);
#78277=ADVANCED_FACE('',(#22847),#18982,.F.);
#78278=ADVANCED_FACE('',(#22848),#18983,.F.);
#78279=ADVANCED_FACE('',(#22849),#18984,.F.);
#78280=ADVANCED_FACE('',(#22850),#18985,.F.);
#78281=ADVANCED_FACE('',(#22851),#18986,.F.);
#78282=ADVANCED_FACE('',(#22852),#18987,.F.);
#78283=ADVANCED_FACE('',(#22853),#18988,.F.);
#78284=ADVANCED_FACE('',(#22854),#18989,.F.);
#78285=ADVANCED_FACE('',(#22855),#18990,.F.);
#78286=ADVANCED_FACE('',(#22856),#18991,.F.);
#78287=ADVANCED_FACE('',(#22857),#18992,.F.);
#78288=ADVANCED_FACE('',(#22858),#18993,.F.);
#78289=ADVANCED_FACE('',(#22859),#18994,.F.);
#78290=ADVANCED_FACE('',(#22860),#18995,.F.);
#78291=ADVANCED_FACE('',(#22861),#18996,.F.);
#78292=ADVANCED_FACE('',(#22862),#18997,.F.);
#78293=ADVANCED_FACE('',(#22863),#18998,.F.);
#78294=ADVANCED_FACE('',(#22864),#18999,.F.);
#78295=ADVANCED_FACE('',(#22865),#19000,.F.);
#78296=ADVANCED_FACE('',(#22866),#19001,.F.);
#78297=ADVANCED_FACE('',(#22867),#19002,.F.);
#78298=ADVANCED_FACE('',(#22868),#19003,.F.);
#78299=ADVANCED_FACE('',(#22869),#19004,.F.);
#78300=ADVANCED_FACE('',(#22870),#19005,.F.);
#78301=ADVANCED_FACE('',(#22871),#19006,.F.);
#78302=ADVANCED_FACE('',(#22872),#19007,.F.);
#78303=ADVANCED_FACE('',(#22873),#19008,.F.);
#78304=ADVANCED_FACE('',(#22874),#19009,.F.);
#78305=ADVANCED_FACE('',(#22875),#19010,.F.);
#78306=ADVANCED_FACE('',(#22876),#19011,.F.);
#78307=ADVANCED_FACE('',(#22877),#19012,.F.);
#78308=ADVANCED_FACE('',(#22878),#19013,.F.);
#78309=ADVANCED_FACE('',(#22879),#19014,.F.);
#78310=ADVANCED_FACE('',(#22880),#19015,.F.);
#78311=ADVANCED_FACE('',(#22881),#19016,.F.);
#78312=ADVANCED_FACE('',(#22882),#19017,.F.);
#78313=ADVANCED_FACE('',(#22883),#19018,.F.);
#78314=ADVANCED_FACE('',(#22884),#19019,.F.);
#78315=ADVANCED_FACE('',(#22885),#19020,.F.);
#78316=ADVANCED_FACE('',(#22886),#19021,.F.);
#78317=ADVANCED_FACE('',(#22887),#19022,.F.);
#78318=ADVANCED_FACE('',(#22888),#19023,.F.);
#78319=ADVANCED_FACE('',(#22889),#19024,.F.);
#78320=ADVANCED_FACE('',(#22890),#19025,.F.);
#78321=ADVANCED_FACE('',(#22891),#19026,.F.);
#78322=ADVANCED_FACE('',(#22892),#19027,.F.);
#78323=ADVANCED_FACE('',(#22893),#19028,.F.);
#78324=ADVANCED_FACE('',(#22894),#19029,.F.);
#78325=ADVANCED_FACE('',(#22895),#19030,.F.);
#78326=ADVANCED_FACE('',(#22896),#19031,.F.);
#78327=ADVANCED_FACE('',(#22897),#19032,.F.);
#78328=ADVANCED_FACE('',(#22898),#19033,.F.);
#78329=ADVANCED_FACE('',(#22899),#19034,.F.);
#78330=ADVANCED_FACE('',(#22900),#19035,.F.);
#78331=ADVANCED_FACE('',(#22901),#19036,.F.);
#78332=ADVANCED_FACE('',(#22902),#19037,.F.);
#78333=ADVANCED_FACE('',(#22903),#19038,.F.);
#78334=ADVANCED_FACE('',(#22904),#19039,.F.);
#78335=ADVANCED_FACE('',(#22905),#19040,.F.);
#78336=ADVANCED_FACE('',(#22906),#19041,.F.);
#78337=ADVANCED_FACE('',(#22907),#19042,.F.);
#78338=ADVANCED_FACE('',(#22908),#19043,.F.);
#78339=ADVANCED_FACE('',(#22909),#19044,.F.);
#78340=ADVANCED_FACE('',(#22910),#19045,.F.);
#78341=ADVANCED_FACE('',(#22911),#19046,.F.);
#78342=ADVANCED_FACE('',(#22912),#19047,.F.);
#78343=ADVANCED_FACE('',(#22913),#19048,.F.);
#78344=ADVANCED_FACE('',(#22914),#19049,.F.);
#78345=ADVANCED_FACE('',(#22915),#19050,.F.);
#78346=ADVANCED_FACE('',(#22916),#19051,.F.);
#78347=ADVANCED_FACE('',(#22917),#19052,.F.);
#78348=ADVANCED_FACE('',(#22918),#19053,.F.);
#78349=ADVANCED_FACE('',(#22919),#19054,.F.);
#78350=ADVANCED_FACE('',(#22920),#19055,.F.);
#78351=ADVANCED_FACE('',(#22921),#19056,.F.);
#78352=ADVANCED_FACE('',(#22922),#19057,.F.);
#78353=ADVANCED_FACE('',(#22923),#19058,.F.);
#78354=ADVANCED_FACE('',(#22924),#19059,.F.);
#78355=ADVANCED_FACE('',(#22925),#19060,.F.);
#78356=ADVANCED_FACE('',(#22926),#19061,.F.);
#78357=ADVANCED_FACE('',(#22927),#19062,.F.);
#78358=ADVANCED_FACE('',(#22928),#19063,.F.);
#78359=ADVANCED_FACE('',(#22929),#19064,.F.);
#78360=ADVANCED_FACE('',(#22930),#19065,.F.);
#78361=ADVANCED_FACE('',(#22931),#19066,.F.);
#78362=ADVANCED_FACE('',(#22932),#19067,.F.);
#78363=ADVANCED_FACE('',(#22933),#19068,.F.);
#78364=ADVANCED_FACE('',(#22934),#19069,.F.);
#78365=ADVANCED_FACE('',(#22935),#19070,.F.);
#78366=ADVANCED_FACE('',(#22936),#19071,.F.);
#78367=ADVANCED_FACE('',(#22937),#19072,.F.);
#78368=ADVANCED_FACE('',(#22938),#19073,.F.);
#78369=ADVANCED_FACE('',(#22939),#19074,.F.);
#78370=ADVANCED_FACE('',(#22940),#19075,.F.);
#78371=ADVANCED_FACE('',(#22941),#19076,.F.);
#78372=ADVANCED_FACE('',(#22942),#19077,.F.);
#78373=ADVANCED_FACE('',(#22943),#19078,.F.);
#78374=ADVANCED_FACE('',(#22944),#19079,.F.);
#78375=ADVANCED_FACE('',(#22945),#19080,.F.);
#78376=ADVANCED_FACE('',(#22946),#19081,.F.);
#78377=ADVANCED_FACE('',(#22947),#19082,.F.);
#78378=ADVANCED_FACE('',(#22948),#19083,.F.);
#78379=ADVANCED_FACE('',(#22949),#19084,.F.);
#78380=ADVANCED_FACE('',(#22950),#19085,.F.);
#78381=ADVANCED_FACE('',(#22951),#19086,.F.);
#78382=ADVANCED_FACE('',(#22952),#19087,.F.);
#78383=ADVANCED_FACE('',(#22953),#19088,.F.);
#78384=ADVANCED_FACE('',(#22954),#19089,.F.);
#78385=ADVANCED_FACE('',(#22955),#19090,.F.);
#78386=ADVANCED_FACE('',(#22956),#19091,.F.);
#78387=ADVANCED_FACE('',(#22957),#19092,.F.);
#78388=ADVANCED_FACE('',(#22958),#19093,.F.);
#78389=ADVANCED_FACE('',(#22959),#19094,.F.);
#78390=ADVANCED_FACE('',(#22960),#19095,.F.);
#78391=ADVANCED_FACE('',(#22961),#19096,.F.);
#78392=ADVANCED_FACE('',(#22962),#19097,.F.);
#78393=ADVANCED_FACE('',(#22963),#19098,.F.);
#78394=ADVANCED_FACE('',(#22964),#19099,.F.);
#78395=ADVANCED_FACE('',(#22965),#19100,.F.);
#78396=ADVANCED_FACE('',(#22966),#19101,.F.);
#78397=ADVANCED_FACE('',(#22967),#19102,.F.);
#78398=ADVANCED_FACE('',(#22968),#19103,.F.);
#78399=ADVANCED_FACE('',(#22969),#19104,.F.);
#78400=ADVANCED_FACE('',(#22970),#19105,.F.);
#78401=ADVANCED_FACE('',(#22971),#19106,.F.);
#78402=ADVANCED_FACE('',(#22972),#19107,.F.);
#78403=ADVANCED_FACE('',(#22973),#19108,.F.);
#78404=ADVANCED_FACE('',(#22974),#19109,.F.);
#78405=ADVANCED_FACE('',(#22975),#19110,.F.);
#78406=ADVANCED_FACE('',(#22976),#19111,.F.);
#78407=ADVANCED_FACE('',(#22977),#19112,.F.);
#78408=ADVANCED_FACE('',(#22978),#19113,.F.);
#78409=ADVANCED_FACE('',(#22979),#19114,.F.);
#78410=ADVANCED_FACE('',(#22980),#19115,.F.);
#78411=ADVANCED_FACE('',(#22981),#19116,.F.);
#78412=ADVANCED_FACE('',(#22982),#19117,.F.);
#78413=ADVANCED_FACE('',(#22983),#19118,.F.);
#78414=ADVANCED_FACE('',(#22984),#19119,.F.);
#78415=ADVANCED_FACE('',(#22985),#19120,.F.);
#78416=ADVANCED_FACE('',(#22986),#19121,.F.);
#78417=ADVANCED_FACE('',(#22987),#19122,.F.);
#78418=ADVANCED_FACE('',(#22988),#19123,.F.);
#78419=ADVANCED_FACE('',(#22989),#19124,.F.);
#78420=ADVANCED_FACE('',(#22990),#19125,.F.);
#78421=ADVANCED_FACE('',(#22991),#19126,.F.);
#78422=ADVANCED_FACE('',(#22992),#19127,.F.);
#78423=ADVANCED_FACE('',(#22993),#19128,.F.);
#78424=ADVANCED_FACE('',(#22994),#19129,.F.);
#78425=ADVANCED_FACE('',(#22995),#19130,.F.);
#78426=ADVANCED_FACE('',(#22996),#19131,.F.);
#78427=ADVANCED_FACE('',(#22997),#19132,.F.);
#78428=ADVANCED_FACE('',(#22998),#19133,.F.);
#78429=ADVANCED_FACE('',(#22999),#19134,.F.);
#78430=ADVANCED_FACE('',(#23000),#19135,.F.);
#78431=ADVANCED_FACE('',(#23001),#19136,.F.);
#78432=ADVANCED_FACE('',(#23002),#19137,.F.);
#78433=ADVANCED_FACE('',(#23003),#19138,.F.);
#78434=ADVANCED_FACE('',(#23004),#19139,.F.);
#78435=ADVANCED_FACE('',(#23005),#19140,.F.);
#78436=ADVANCED_FACE('',(#23006),#19141,.F.);
#78437=ADVANCED_FACE('',(#23007),#19142,.F.);
#78438=ADVANCED_FACE('',(#23008),#19143,.F.);
#78439=ADVANCED_FACE('',(#23009),#19144,.F.);
#78440=ADVANCED_FACE('',(#23010),#19145,.F.);
#78441=ADVANCED_FACE('',(#23011),#19146,.F.);
#78442=ADVANCED_FACE('',(#23012),#19147,.F.);
#78443=ADVANCED_FACE('',(#23013),#19148,.F.);
#78444=ADVANCED_FACE('',(#23014),#19149,.F.);
#78445=ADVANCED_FACE('',(#23015),#19150,.F.);
#78446=ADVANCED_FACE('',(#23016),#19151,.F.);
#78447=ADVANCED_FACE('',(#23017),#19152,.F.);
#78448=ADVANCED_FACE('',(#23018),#19153,.F.);
#78449=ADVANCED_FACE('',(#23019),#19154,.F.);
#78450=ADVANCED_FACE('',(#23020),#19155,.F.);
#78451=ADVANCED_FACE('',(#23021),#19156,.F.);
#78452=ADVANCED_FACE('',(#23022),#19157,.F.);
#78453=ADVANCED_FACE('',(#23023),#19158,.F.);
#78454=ADVANCED_FACE('',(#23024),#19159,.F.);
#78455=ADVANCED_FACE('',(#23025),#19160,.F.);
#78456=ADVANCED_FACE('',(#23026),#19161,.F.);
#78457=ADVANCED_FACE('',(#23027),#19162,.F.);
#78458=ADVANCED_FACE('',(#23028),#19163,.F.);
#78459=ADVANCED_FACE('',(#23029),#19164,.F.);
#78460=ADVANCED_FACE('',(#23030),#19165,.F.);
#78461=ADVANCED_FACE('',(#23031),#19166,.F.);
#78462=ADVANCED_FACE('',(#23032),#19167,.F.);
#78463=ADVANCED_FACE('',(#23033),#19168,.F.);
#78464=ADVANCED_FACE('',(#23034),#19169,.F.);
#78465=ADVANCED_FACE('',(#23035),#19170,.F.);
#78466=ADVANCED_FACE('',(#23036),#19171,.F.);
#78467=ADVANCED_FACE('',(#23037),#19172,.F.);
#78468=ADVANCED_FACE('',(#23038),#19173,.F.);
#78469=ADVANCED_FACE('',(#23039),#19174,.F.);
#78470=ADVANCED_FACE('',(#23040),#19175,.F.);
#78471=ADVANCED_FACE('',(#23041),#19176,.F.);
#78472=ADVANCED_FACE('',(#23042),#19177,.F.);
#78473=ADVANCED_FACE('',(#23043),#19178,.F.);
#78474=ADVANCED_FACE('',(#23044),#19179,.F.);
#78475=ADVANCED_FACE('',(#23045),#19180,.F.);
#78476=ADVANCED_FACE('',(#23046),#19181,.F.);
#78477=ADVANCED_FACE('',(#23047),#19182,.F.);
#78478=ADVANCED_FACE('',(#23048),#19183,.F.);
#78479=ADVANCED_FACE('',(#23049),#19184,.F.);
#78480=ADVANCED_FACE('',(#23050),#19185,.F.);
#78481=ADVANCED_FACE('',(#23051),#19186,.F.);
#78482=ADVANCED_FACE('',(#23052),#19187,.F.);
#78483=ADVANCED_FACE('',(#23053),#19188,.F.);
#78484=ADVANCED_FACE('',(#23054),#19189,.F.);
#78485=ADVANCED_FACE('',(#23055),#19190,.F.);
#78486=ADVANCED_FACE('',(#23056),#19191,.F.);
#78487=ADVANCED_FACE('',(#23057),#19192,.F.);
#78488=ADVANCED_FACE('',(#23058),#19193,.F.);
#78489=ADVANCED_FACE('',(#23059),#19194,.F.);
#78490=ADVANCED_FACE('',(#23060),#19195,.F.);
#78491=ADVANCED_FACE('',(#23061),#19196,.F.);
#78492=ADVANCED_FACE('',(#23062),#19197,.F.);
#78493=ADVANCED_FACE('',(#23063),#19198,.F.);
#78494=ADVANCED_FACE('',(#23064),#19199,.F.);
#78495=ADVANCED_FACE('',(#23065),#19200,.F.);
#78496=ADVANCED_FACE('',(#23066),#19201,.F.);
#78497=ADVANCED_FACE('',(#23067),#19202,.F.);
#78498=ADVANCED_FACE('',(#23068),#19203,.F.);
#78499=ADVANCED_FACE('',(#23069),#19204,.F.);
#78500=ADVANCED_FACE('',(#23070),#19205,.F.);
#78501=ADVANCED_FACE('',(#23071),#19206,.F.);
#78502=ADVANCED_FACE('',(#23072),#19207,.F.);
#78503=ADVANCED_FACE('',(#23073),#19208,.F.);
#78504=ADVANCED_FACE('',(#23074),#19209,.F.);
#78505=ADVANCED_FACE('',(#23075),#19210,.F.);
#78506=ADVANCED_FACE('',(#23076),#19211,.F.);
#78507=ADVANCED_FACE('',(#23077),#19212,.F.);
#78508=ADVANCED_FACE('',(#23078),#19213,.F.);
#78509=ADVANCED_FACE('',(#23079),#19214,.F.);
#78510=ADVANCED_FACE('',(#23080),#19215,.F.);
#78511=ADVANCED_FACE('',(#23081),#19216,.F.);
#78512=ADVANCED_FACE('',(#23082),#19217,.F.);
#78513=ADVANCED_FACE('',(#23083),#19218,.F.);
#78514=ADVANCED_FACE('',(#23084),#19219,.F.);
#78515=ADVANCED_FACE('',(#23085),#19220,.F.);
#78516=ADVANCED_FACE('',(#23086),#19221,.F.);
#78517=ADVANCED_FACE('',(#23087),#19222,.F.);
#78518=ADVANCED_FACE('',(#23088),#19223,.F.);
#78519=ADVANCED_FACE('',(#23089),#19224,.F.);
#78520=ADVANCED_FACE('',(#23090),#19225,.F.);
#78521=ADVANCED_FACE('',(#23091),#19226,.F.);
#78522=ADVANCED_FACE('',(#23092),#19227,.F.);
#78523=ADVANCED_FACE('',(#23093),#19228,.F.);
#78524=ADVANCED_FACE('',(#23094),#19229,.F.);
#78525=ADVANCED_FACE('',(#23095),#19230,.F.);
#78526=ADVANCED_FACE('',(#23096),#19231,.F.);
#78527=ADVANCED_FACE('',(#23097),#19232,.F.);
#78528=ADVANCED_FACE('',(#23098),#19233,.F.);
#78529=ADVANCED_FACE('',(#23099),#19234,.F.);
#78530=ADVANCED_FACE('',(#23100),#19235,.F.);
#78531=ADVANCED_FACE('',(#23101),#19236,.F.);
#78532=ADVANCED_FACE('',(#23102),#19237,.F.);
#78533=ADVANCED_FACE('',(#23103),#19238,.F.);
#78534=ADVANCED_FACE('',(#23104),#19239,.F.);
#78535=ADVANCED_FACE('',(#23105),#19240,.F.);
#78536=ADVANCED_FACE('',(#23106),#19241,.F.);
#78537=ADVANCED_FACE('',(#23107),#19242,.F.);
#78538=ADVANCED_FACE('',(#23108),#19243,.F.);
#78539=ADVANCED_FACE('',(#23109),#19244,.F.);
#78540=ADVANCED_FACE('',(#23110),#19245,.F.);
#78541=ADVANCED_FACE('',(#23111),#19246,.F.);
#78542=ADVANCED_FACE('',(#23112),#19247,.F.);
#78543=ADVANCED_FACE('',(#23113),#19248,.F.);
#78544=ADVANCED_FACE('',(#23114),#19249,.F.);
#78545=ADVANCED_FACE('',(#23115),#19250,.F.);
#78546=ADVANCED_FACE('',(#23116),#19251,.F.);
#78547=ADVANCED_FACE('',(#23117),#19252,.F.);
#78548=ADVANCED_FACE('',(#23118),#19253,.F.);
#78549=ADVANCED_FACE('',(#23119),#19254,.F.);
#78550=ADVANCED_FACE('',(#23120),#19255,.F.);
#78551=ADVANCED_FACE('',(#23121),#19256,.F.);
#78552=ADVANCED_FACE('',(#23122),#19257,.F.);
#78553=ADVANCED_FACE('',(#23123),#19258,.F.);
#78554=ADVANCED_FACE('',(#23124),#19259,.F.);
#78555=ADVANCED_FACE('',(#23125),#19260,.F.);
#78556=ADVANCED_FACE('',(#23126),#19261,.F.);
#78557=ADVANCED_FACE('',(#23127),#19262,.F.);
#78558=ADVANCED_FACE('',(#23128),#19263,.F.);
#78559=ADVANCED_FACE('',(#23129),#19264,.F.);
#78560=ADVANCED_FACE('',(#23130),#19265,.F.);
#78561=ADVANCED_FACE('',(#23131),#19266,.F.);
#78562=ADVANCED_FACE('',(#23132),#19267,.F.);
#78563=ADVANCED_FACE('',(#23133),#19268,.F.);
#78564=ADVANCED_FACE('',(#23134),#19269,.F.);
#78565=ADVANCED_FACE('',(#23135),#19270,.F.);
#78566=ADVANCED_FACE('',(#23136),#19271,.F.);
#78567=ADVANCED_FACE('',(#23137),#19272,.F.);
#78568=ADVANCED_FACE('',(#23138),#19273,.F.);
#78569=ADVANCED_FACE('',(#23139),#19274,.F.);
#78570=ADVANCED_FACE('',(#23140),#19275,.F.);
#78571=ADVANCED_FACE('',(#23141),#19276,.F.);
#78572=ADVANCED_FACE('',(#23142),#19277,.F.);
#78573=ADVANCED_FACE('',(#23143),#19278,.F.);
#78574=ADVANCED_FACE('',(#23144),#19279,.F.);
#78575=ADVANCED_FACE('',(#23145),#19280,.F.);
#78576=ADVANCED_FACE('',(#23146),#19281,.F.);
#78577=ADVANCED_FACE('',(#23147),#19282,.F.);
#78578=ADVANCED_FACE('',(#23148),#19283,.F.);
#78579=ADVANCED_FACE('',(#23149),#19284,.F.);
#78580=ADVANCED_FACE('',(#23150),#19285,.F.);
#78581=ADVANCED_FACE('',(#23151),#19286,.F.);
#78582=ADVANCED_FACE('',(#23152),#19287,.F.);
#78583=ADVANCED_FACE('',(#23153),#19288,.F.);
#78584=ADVANCED_FACE('',(#23154),#19289,.F.);
#78585=ADVANCED_FACE('',(#23155),#19290,.F.);
#78586=ADVANCED_FACE('',(#23156),#19291,.F.);
#78587=ADVANCED_FACE('',(#23157),#19292,.F.);
#78588=ADVANCED_FACE('',(#23158),#19293,.F.);
#78589=ADVANCED_FACE('',(#23159),#19294,.F.);
#78590=ADVANCED_FACE('',(#23160),#19295,.F.);
#78591=ADVANCED_FACE('',(#23161),#19296,.F.);
#78592=ADVANCED_FACE('',(#23162),#19297,.F.);
#78593=ADVANCED_FACE('',(#23163),#19298,.F.);
#78594=ADVANCED_FACE('',(#23164),#19299,.F.);
#78595=ADVANCED_FACE('',(#23165),#19300,.F.);
#78596=ADVANCED_FACE('',(#23166),#19301,.F.);
#78597=ADVANCED_FACE('',(#23167),#19302,.F.);
#78598=ADVANCED_FACE('',(#23168),#19303,.F.);
#78599=ADVANCED_FACE('',(#23169),#19304,.F.);
#78600=ADVANCED_FACE('',(#23170),#19305,.F.);
#78601=ADVANCED_FACE('',(#23171),#19306,.F.);
#78602=ADVANCED_FACE('',(#23172),#19307,.F.);
#78603=ADVANCED_FACE('',(#23173),#19308,.F.);
#78604=ADVANCED_FACE('',(#23174),#19309,.F.);
#78605=ADVANCED_FACE('',(#23175),#19310,.F.);
#78606=ADVANCED_FACE('',(#23176),#19311,.F.);
#78607=ADVANCED_FACE('',(#23177),#19312,.F.);
#78608=ADVANCED_FACE('',(#23178),#19313,.F.);
#78609=ADVANCED_FACE('',(#23179),#19314,.F.);
#78610=ADVANCED_FACE('',(#23180),#19315,.F.);
#78611=ADVANCED_FACE('',(#23181),#19316,.F.);
#78612=ADVANCED_FACE('',(#23182),#19317,.F.);
#78613=ADVANCED_FACE('',(#23183),#19318,.F.);
#78614=ADVANCED_FACE('',(#23184),#19319,.F.);
#78615=ADVANCED_FACE('',(#23185),#19320,.F.);
#78616=ADVANCED_FACE('',(#23186),#19321,.F.);
#78617=ADVANCED_FACE('',(#23187),#19322,.F.);
#78618=ADVANCED_FACE('',(#23188),#19323,.F.);
#78619=ADVANCED_FACE('',(#23189),#19324,.F.);
#78620=ADVANCED_FACE('',(#23190),#19325,.F.);
#78621=ADVANCED_FACE('',(#23191),#19326,.F.);
#78622=ADVANCED_FACE('',(#23192),#19327,.F.);
#78623=ADVANCED_FACE('',(#23193),#19328,.F.);
#78624=ADVANCED_FACE('',(#23194),#19329,.F.);
#78625=ADVANCED_FACE('',(#23195),#19330,.F.);
#78626=ADVANCED_FACE('',(#23196),#19331,.F.);
#78627=ADVANCED_FACE('',(#23197),#19332,.F.);
#78628=ADVANCED_FACE('',(#23198),#19333,.F.);
#78629=ADVANCED_FACE('',(#23199),#19334,.F.);
#78630=ADVANCED_FACE('',(#23200),#19335,.F.);
#78631=ADVANCED_FACE('',(#23201),#19336,.F.);
#78632=ADVANCED_FACE('',(#23202),#19337,.F.);
#78633=ADVANCED_FACE('',(#23203),#19338,.F.);
#78634=ADVANCED_FACE('',(#23204),#19339,.F.);
#78635=ADVANCED_FACE('',(#23205),#19340,.F.);
#78636=ADVANCED_FACE('',(#23206),#19341,.F.);
#78637=ADVANCED_FACE('',(#23207),#19342,.F.);
#78638=ADVANCED_FACE('',(#23208),#19343,.F.);
#78639=ADVANCED_FACE('',(#23209),#19344,.F.);
#78640=ADVANCED_FACE('',(#23210),#19345,.F.);
#78641=ADVANCED_FACE('',(#23211),#19346,.F.);
#78642=ADVANCED_FACE('',(#23212),#19347,.F.);
#78643=ADVANCED_FACE('',(#23213),#19348,.F.);
#78644=ADVANCED_FACE('',(#23214),#19349,.F.);
#78645=ADVANCED_FACE('',(#23215),#19350,.F.);
#78646=ADVANCED_FACE('',(#23216),#19351,.F.);
#78647=ADVANCED_FACE('',(#23217),#19352,.F.);
#78648=ADVANCED_FACE('',(#23218),#19353,.F.);
#78649=ADVANCED_FACE('',(#23219),#19354,.F.);
#78650=ADVANCED_FACE('',(#23220),#19355,.F.);
#78651=ADVANCED_FACE('',(#23221),#19356,.F.);
#78652=ADVANCED_FACE('',(#23222),#19357,.F.);
#78653=ADVANCED_FACE('',(#23223),#19358,.F.);
#78654=ADVANCED_FACE('',(#23224),#19359,.F.);
#78655=ADVANCED_FACE('',(#23225),#19360,.F.);
#78656=ADVANCED_FACE('',(#23226),#19361,.F.);
#78657=ADVANCED_FACE('',(#23227),#19362,.F.);
#78658=ADVANCED_FACE('',(#23228),#19363,.F.);
#78659=ADVANCED_FACE('',(#23229),#19364,.F.);
#78660=ADVANCED_FACE('',(#23230),#19365,.F.);
#78661=ADVANCED_FACE('',(#23231),#19366,.F.);
#78662=ADVANCED_FACE('',(#23232),#19367,.F.);
#78663=ADVANCED_FACE('',(#23233),#19368,.F.);
#78664=ADVANCED_FACE('',(#23234),#19369,.F.);
#78665=ADVANCED_FACE('',(#23235),#19370,.F.);
#78666=ADVANCED_FACE('',(#23236),#19371,.F.);
#78667=ADVANCED_FACE('',(#23237),#19372,.F.);
#78668=ADVANCED_FACE('',(#23238),#19373,.F.);
#78669=ADVANCED_FACE('',(#23239),#19374,.F.);
#78670=ADVANCED_FACE('',(#23240),#19375,.F.);
#78671=ADVANCED_FACE('',(#23241),#19376,.F.);
#78672=ADVANCED_FACE('',(#23242),#19377,.F.);
#78673=ADVANCED_FACE('',(#23243),#19378,.F.);
#78674=ADVANCED_FACE('',(#23244),#19379,.F.);
#78675=ADVANCED_FACE('',(#23245),#19380,.F.);
#78676=ADVANCED_FACE('',(#23246),#19381,.F.);
#78677=ADVANCED_FACE('',(#23247),#19382,.F.);
#78678=ADVANCED_FACE('',(#23248),#19383,.F.);
#78679=ADVANCED_FACE('',(#23249),#19384,.F.);
#78680=ADVANCED_FACE('',(#23250),#19385,.F.);
#78681=ADVANCED_FACE('',(#23251),#19386,.F.);
#78682=ADVANCED_FACE('',(#23252),#19387,.F.);
#78683=ADVANCED_FACE('',(#23253),#19388,.F.);
#78684=ADVANCED_FACE('',(#23254),#19389,.F.);
#78685=ADVANCED_FACE('',(#23255),#19390,.F.);
#78686=ADVANCED_FACE('',(#23256),#19391,.F.);
#78687=ADVANCED_FACE('',(#23257),#19392,.F.);
#78688=ADVANCED_FACE('',(#23258),#19393,.F.);
#78689=ADVANCED_FACE('',(#23259),#19394,.F.);
#78690=ADVANCED_FACE('',(#23260),#19395,.F.);
#78691=ADVANCED_FACE('',(#23261),#19396,.F.);
#78692=ADVANCED_FACE('',(#23262),#19397,.F.);
#78693=ADVANCED_FACE('',(#23263),#19398,.F.);
#78694=ADVANCED_FACE('',(#23264),#19399,.F.);
#78695=ADVANCED_FACE('',(#23265),#19400,.F.);
#78696=ADVANCED_FACE('',(#23266),#19401,.F.);
#78697=ADVANCED_FACE('',(#23267),#19402,.F.);
#78698=ADVANCED_FACE('',(#23268),#19403,.F.);
#78699=ADVANCED_FACE('',(#23269),#19404,.F.);
#78700=ADVANCED_FACE('',(#23270),#19405,.F.);
#78701=ADVANCED_FACE('',(#23271),#19406,.F.);
#78702=ADVANCED_FACE('',(#23272),#19407,.F.);
#78703=ADVANCED_FACE('',(#23273),#19408,.F.);
#78704=ADVANCED_FACE('',(#23274),#19409,.F.);
#78705=ADVANCED_FACE('',(#23275),#19410,.F.);
#78706=ADVANCED_FACE('',(#23276),#19411,.F.);
#78707=ADVANCED_FACE('',(#23277),#19412,.F.);
#78708=ADVANCED_FACE('',(#23278),#19413,.F.);
#78709=ADVANCED_FACE('',(#23279),#19414,.F.);
#78710=ADVANCED_FACE('',(#23280),#19415,.F.);
#78711=ADVANCED_FACE('',(#23281),#19416,.F.);
#78712=ADVANCED_FACE('',(#23282),#19417,.F.);
#78713=ADVANCED_FACE('',(#23283),#19418,.F.);
#78714=ADVANCED_FACE('',(#23284),#19419,.F.);
#78715=ADVANCED_FACE('',(#23285),#19420,.F.);
#78716=ADVANCED_FACE('',(#23286),#19421,.F.);
#78717=ADVANCED_FACE('',(#23287),#19422,.F.);
#78718=ADVANCED_FACE('',(#23288),#19423,.F.);
#78719=ADVANCED_FACE('',(#23289),#19424,.F.);
#78720=ADVANCED_FACE('',(#23290),#19425,.F.);
#78721=ADVANCED_FACE('',(#23291),#19426,.F.);
#78722=ADVANCED_FACE('',(#23292),#19427,.F.);
#78723=ADVANCED_FACE('',(#23293),#19428,.F.);
#78724=ADVANCED_FACE('',(#23294),#19429,.F.);
#78725=ADVANCED_FACE('',(#23295),#19430,.F.);
#78726=ADVANCED_FACE('',(#23296),#19431,.F.);
#78727=ADVANCED_FACE('',(#23297),#19432,.F.);
#78728=ADVANCED_FACE('',(#23298),#19433,.F.);
#78729=ADVANCED_FACE('',(#23299),#19434,.F.);
#78730=ADVANCED_FACE('',(#23300),#19435,.F.);
#78731=ADVANCED_FACE('',(#23301),#19436,.F.);
#78732=ADVANCED_FACE('',(#23302),#19437,.F.);
#78733=ADVANCED_FACE('',(#23303),#19438,.F.);
#78734=ADVANCED_FACE('',(#23304),#19439,.F.);
#78735=ADVANCED_FACE('',(#23305),#19440,.F.);
#78736=ADVANCED_FACE('',(#23306),#19441,.F.);
#78737=ADVANCED_FACE('',(#23307),#19442,.F.);
#78738=ADVANCED_FACE('',(#23308),#19443,.F.);
#78739=ADVANCED_FACE('',(#23309),#19444,.F.);
#78740=ADVANCED_FACE('',(#23310),#19445,.F.);
#78741=ADVANCED_FACE('',(#23311),#19446,.F.);
#78742=ADVANCED_FACE('',(#23312),#19447,.F.);
#78743=ADVANCED_FACE('',(#23313),#19448,.F.);
#78744=ADVANCED_FACE('',(#23314),#19449,.F.);
#78745=ADVANCED_FACE('',(#23315),#19450,.F.);
#78746=ADVANCED_FACE('',(#23316),#19451,.F.);
#78747=ADVANCED_FACE('',(#23317),#19452,.F.);
#78748=ADVANCED_FACE('',(#23318),#19453,.F.);
#78749=ADVANCED_FACE('',(#23319),#19454,.F.);
#78750=ADVANCED_FACE('',(#23320),#19455,.F.);
#78751=ADVANCED_FACE('',(#23321),#19456,.F.);
#78752=ADVANCED_FACE('',(#23322),#19457,.F.);
#78753=ADVANCED_FACE('',(#23323),#19458,.F.);
#78754=ADVANCED_FACE('',(#23324),#19459,.F.);
#78755=ADVANCED_FACE('',(#23325),#19460,.F.);
#78756=ADVANCED_FACE('',(#23326),#19461,.F.);
#78757=ADVANCED_FACE('',(#23327),#19462,.F.);
#78758=ADVANCED_FACE('',(#23328),#19463,.F.);
#78759=ADVANCED_FACE('',(#23329),#19464,.F.);
#78760=ADVANCED_FACE('',(#23330),#19465,.F.);
#78761=ADVANCED_FACE('',(#23331),#19466,.F.);
#78762=ADVANCED_FACE('',(#23332),#19467,.F.);
#78763=ADVANCED_FACE('',(#23333),#19468,.F.);
#78764=ADVANCED_FACE('',(#23334),#19469,.F.);
#78765=ADVANCED_FACE('',(#23335),#19470,.F.);
#78766=ADVANCED_FACE('',(#23336),#19471,.F.);
#78767=ADVANCED_FACE('',(#23337),#19472,.F.);
#78768=ADVANCED_FACE('',(#23338),#19473,.F.);
#78769=ADVANCED_FACE('',(#23339),#19474,.F.);
#78770=ADVANCED_FACE('',(#23340),#19475,.F.);
#78771=ADVANCED_FACE('',(#23341),#19476,.F.);
#78772=ADVANCED_FACE('',(#23342),#19477,.F.);
#78773=ADVANCED_FACE('',(#23343),#19478,.F.);
#78774=ADVANCED_FACE('',(#23344),#19479,.F.);
#78775=ADVANCED_FACE('',(#23345),#19480,.F.);
#78776=ADVANCED_FACE('',(#23346),#19481,.F.);
#78777=ADVANCED_FACE('',(#23347),#19482,.F.);
#78778=ADVANCED_FACE('',(#23348),#19483,.F.);
#78779=ADVANCED_FACE('',(#23349),#19484,.F.);
#78780=ADVANCED_FACE('',(#23350),#19485,.F.);
#78781=ADVANCED_FACE('',(#23351),#19486,.F.);
#78782=ADVANCED_FACE('',(#23352),#19487,.F.);
#78783=ADVANCED_FACE('',(#23353),#19488,.F.);
#78784=ADVANCED_FACE('',(#23354),#19489,.F.);
#78785=ADVANCED_FACE('',(#23355),#19490,.F.);
#78786=ADVANCED_FACE('',(#23356),#19491,.F.);
#78787=ADVANCED_FACE('',(#23357),#19492,.F.);
#78788=ADVANCED_FACE('',(#23358),#19493,.F.);
#78789=ADVANCED_FACE('',(#23359),#19494,.F.);
#78790=ADVANCED_FACE('',(#23360),#19495,.F.);
#78791=ADVANCED_FACE('',(#23361),#19496,.F.);
#78792=ADVANCED_FACE('',(#23362),#19497,.F.);
#78793=ADVANCED_FACE('',(#23363),#19498,.F.);
#78794=ADVANCED_FACE('',(#23364),#19499,.F.);
#78795=ADVANCED_FACE('',(#23365),#19500,.F.);
#78796=ADVANCED_FACE('',(#23366),#19501,.F.);
#78797=ADVANCED_FACE('',(#23367),#19502,.F.);
#78798=ADVANCED_FACE('',(#23368),#19503,.F.);
#78799=ADVANCED_FACE('',(#23369),#19504,.F.);
#78800=ADVANCED_FACE('',(#23370),#19505,.F.);
#78801=ADVANCED_FACE('',(#23371),#19506,.F.);
#78802=ADVANCED_FACE('',(#23372),#19507,.F.);
#78803=ADVANCED_FACE('',(#23373),#19508,.F.);
#78804=ADVANCED_FACE('',(#23374),#19509,.F.);
#78805=ADVANCED_FACE('',(#23375),#19510,.F.);
#78806=ADVANCED_FACE('',(#23376),#19511,.F.);
#78807=ADVANCED_FACE('',(#23377),#19512,.F.);
#78808=ADVANCED_FACE('',(#23378),#19513,.F.);
#78809=ADVANCED_FACE('',(#23379),#19514,.F.);
#78810=ADVANCED_FACE('',(#23380),#19515,.F.);
#78811=ADVANCED_FACE('',(#23381),#19516,.F.);
#78812=ADVANCED_FACE('',(#23382),#19517,.F.);
#78813=ADVANCED_FACE('',(#23383),#19518,.F.);
#78814=ADVANCED_FACE('',(#23384),#19519,.F.);
#78815=ADVANCED_FACE('',(#23385),#19520,.F.);
#78816=ADVANCED_FACE('',(#23386),#19521,.F.);
#78817=ADVANCED_FACE('',(#23387),#19522,.F.);
#78818=ADVANCED_FACE('',(#23388),#19523,.F.);
#78819=ADVANCED_FACE('',(#23389),#19524,.F.);
#78820=ADVANCED_FACE('',(#23390),#19525,.F.);
#78821=ADVANCED_FACE('',(#23391),#19526,.F.);
#78822=ADVANCED_FACE('',(#23392),#19527,.F.);
#78823=ADVANCED_FACE('',(#23393),#19528,.F.);
#78824=ADVANCED_FACE('',(#23394),#19529,.F.);
#78825=ADVANCED_FACE('',(#23395),#19530,.F.);
#78826=ADVANCED_FACE('',(#23396),#19531,.F.);
#78827=ADVANCED_FACE('',(#23397),#19532,.F.);
#78828=ADVANCED_FACE('',(#23398),#19533,.F.);
#78829=ADVANCED_FACE('',(#23399),#19534,.F.);
#78830=ADVANCED_FACE('',(#23400),#19535,.F.);
#78831=ADVANCED_FACE('',(#23401),#19536,.F.);
#78832=ADVANCED_FACE('',(#23402),#19537,.F.);
#78833=ADVANCED_FACE('',(#23403),#19538,.F.);
#78834=ADVANCED_FACE('',(#23404),#19539,.F.);
#78835=ADVANCED_FACE('',(#23405),#19540,.F.);
#78836=ADVANCED_FACE('',(#23406),#19541,.F.);
#78837=ADVANCED_FACE('',(#23407),#19542,.F.);
#78838=ADVANCED_FACE('',(#23408),#19543,.F.);
#78839=ADVANCED_FACE('',(#23409),#19544,.F.);
#78840=ADVANCED_FACE('',(#23410),#19545,.F.);
#78841=ADVANCED_FACE('',(#23411),#19546,.F.);
#78842=ADVANCED_FACE('',(#23412),#19547,.F.);
#78843=ADVANCED_FACE('',(#23413),#19548,.F.);
#78844=ADVANCED_FACE('',(#23414),#19549,.F.);
#78845=ADVANCED_FACE('',(#23415),#19550,.F.);
#78846=ADVANCED_FACE('',(#23416),#19551,.F.);
#78847=ADVANCED_FACE('',(#23417),#19552,.F.);
#78848=ADVANCED_FACE('',(#23418),#19553,.F.);
#78849=ADVANCED_FACE('',(#23419),#19554,.F.);
#78850=ADVANCED_FACE('',(#23420),#19555,.F.);
#78851=ADVANCED_FACE('',(#23421),#19556,.F.);
#78852=ADVANCED_FACE('',(#23422),#19557,.F.);
#78853=ADVANCED_FACE('',(#23423),#19558,.F.);
#78854=ADVANCED_FACE('',(#23424),#19559,.F.);
#78855=ADVANCED_FACE('',(#23425),#19560,.F.);
#78856=ADVANCED_FACE('',(#23426),#19561,.F.);
#78857=ADVANCED_FACE('',(#23427),#19562,.F.);
#78858=ADVANCED_FACE('',(#23428),#19563,.F.);
#78859=ADVANCED_FACE('',(#23429),#19564,.F.);
#78860=ADVANCED_FACE('',(#23430),#19565,.F.);
#78861=ADVANCED_FACE('',(#23431),#19566,.F.);
#78862=ADVANCED_FACE('',(#23432),#19567,.F.);
#78863=ADVANCED_FACE('',(#23433),#19568,.F.);
#78864=ADVANCED_FACE('',(#23434),#19569,.F.);
#78865=ADVANCED_FACE('',(#23435),#19570,.F.);
#78866=ADVANCED_FACE('',(#23436),#19571,.F.);
#78867=ADVANCED_FACE('',(#23437),#19572,.F.);
#78868=ADVANCED_FACE('',(#23438),#19573,.F.);
#78869=ADVANCED_FACE('',(#23439),#19574,.F.);
#78870=ADVANCED_FACE('',(#23440),#19575,.F.);
#78871=ADVANCED_FACE('',(#23441),#19576,.F.);
#78872=ADVANCED_FACE('',(#23442),#19577,.F.);
#78873=ADVANCED_FACE('',(#23443),#19578,.F.);
#78874=ADVANCED_FACE('',(#23444),#19579,.F.);
#78875=ADVANCED_FACE('',(#23445),#19580,.F.);
#78876=ADVANCED_FACE('',(#23446),#19581,.F.);
#78877=ADVANCED_FACE('',(#23447),#19582,.F.);
#78878=ADVANCED_FACE('',(#23448),#19583,.F.);
#78879=ADVANCED_FACE('',(#23449),#19584,.F.);
#78880=ADVANCED_FACE('',(#23450),#19585,.F.);
#78881=ADVANCED_FACE('',(#23451),#19586,.F.);
#78882=ADVANCED_FACE('',(#23452),#19587,.F.);
#78883=ADVANCED_FACE('',(#23453),#19588,.F.);
#78884=ADVANCED_FACE('',(#23454),#19589,.F.);
#78885=ADVANCED_FACE('',(#23455),#19590,.F.);
#78886=ADVANCED_FACE('',(#23456),#19591,.F.);
#78887=ADVANCED_FACE('',(#23457),#19592,.F.);
#78888=ADVANCED_FACE('',(#23458),#19593,.F.);
#78889=ADVANCED_FACE('',(#23459),#19594,.F.);
#78890=ADVANCED_FACE('',(#23460),#19595,.F.);
#78891=ADVANCED_FACE('',(#23461),#19596,.F.);
#78892=ADVANCED_FACE('',(#23462),#19597,.F.);
#78893=ADVANCED_FACE('',(#23463),#19598,.F.);
#78894=ADVANCED_FACE('',(#23464),#19599,.F.);
#78895=ADVANCED_FACE('',(#23465),#19600,.F.);
#78896=ADVANCED_FACE('',(#23466),#19601,.F.);
#78897=ADVANCED_FACE('',(#23467),#19602,.F.);
#78898=ADVANCED_FACE('',(#23468),#19603,.F.);
#78899=ADVANCED_FACE('',(#23469),#19604,.F.);
#78900=ADVANCED_FACE('',(#23470),#19605,.F.);
#78901=ADVANCED_FACE('',(#23471),#19606,.F.);
#78902=ADVANCED_FACE('',(#23472),#19607,.F.);
#78903=ADVANCED_FACE('',(#23473),#19608,.F.);
#78904=ADVANCED_FACE('',(#23474),#19609,.F.);
#78905=ADVANCED_FACE('',(#23475),#19610,.F.);
#78906=ADVANCED_FACE('',(#23476),#19611,.F.);
#78907=ADVANCED_FACE('',(#23477),#19612,.F.);
#78908=ADVANCED_FACE('',(#23478),#19613,.F.);
#78909=ADVANCED_FACE('',(#23479),#19614,.F.);
#78910=ADVANCED_FACE('',(#23480),#19615,.F.);
#78911=ADVANCED_FACE('',(#23481),#19616,.F.);
#78912=ADVANCED_FACE('',(#23482),#19617,.F.);
#78913=ADVANCED_FACE('',(#23483),#19618,.F.);
#78914=ADVANCED_FACE('',(#23484),#19619,.F.);
#78915=ADVANCED_FACE('',(#23485),#19620,.F.);
#78916=ADVANCED_FACE('',(#23486),#19621,.F.);
#78917=ADVANCED_FACE('',(#23487),#19622,.F.);
#78918=ADVANCED_FACE('',(#23488),#19623,.F.);
#78919=ADVANCED_FACE('',(#23489),#19624,.F.);
#78920=ADVANCED_FACE('',(#23490),#19625,.F.);
#78921=ADVANCED_FACE('',(#23491),#19626,.F.);
#78922=ADVANCED_FACE('',(#23492),#19627,.F.);
#78923=ADVANCED_FACE('',(#23493),#19628,.F.);
#78924=ADVANCED_FACE('',(#23494),#19629,.F.);
#78925=ADVANCED_FACE('',(#23495),#19630,.F.);
#78926=ADVANCED_FACE('',(#23496),#19631,.F.);
#78927=ADVANCED_FACE('',(#23497),#19632,.F.);
#78928=ADVANCED_FACE('',(#23498),#19633,.F.);
#78929=ADVANCED_FACE('',(#23499),#19634,.F.);
#78930=ADVANCED_FACE('',(#23500),#19635,.F.);
#78931=ADVANCED_FACE('',(#23501),#19636,.F.);
#78932=ADVANCED_FACE('',(#23502),#19637,.F.);
#78933=ADVANCED_FACE('',(#23503),#19638,.F.);
#78934=ADVANCED_FACE('',(#23504),#19639,.F.);
#78935=ADVANCED_FACE('',(#23505),#19640,.F.);
#78936=ADVANCED_FACE('',(#23506),#19641,.F.);
#78937=ADVANCED_FACE('',(#23507),#19642,.F.);
#78938=ADVANCED_FACE('',(#23508),#19643,.F.);
#78939=ADVANCED_FACE('',(#23509),#19644,.F.);
#78940=ADVANCED_FACE('',(#23510),#19645,.F.);
#78941=ADVANCED_FACE('',(#23511),#19646,.F.);
#78942=ADVANCED_FACE('',(#23512),#19647,.F.);
#78943=ADVANCED_FACE('',(#23513),#19648,.F.);
#78944=ADVANCED_FACE('',(#23514),#19649,.F.);
#78945=ADVANCED_FACE('',(#23515),#19650,.F.);
#78946=ADVANCED_FACE('',(#23516),#19651,.F.);
#78947=ADVANCED_FACE('',(#23517),#19652,.F.);
#78948=ADVANCED_FACE('',(#23518),#19653,.F.);
#78949=ADVANCED_FACE('',(#23519),#19654,.F.);
#78950=ADVANCED_FACE('',(#23520),#19655,.F.);
#78951=ADVANCED_FACE('',(#23521),#19656,.F.);
#78952=ADVANCED_FACE('',(#23522),#19657,.F.);
#78953=ADVANCED_FACE('',(#23523),#19658,.F.);
#78954=ADVANCED_FACE('',(#23524),#19659,.F.);
#78955=ADVANCED_FACE('',(#23525),#19660,.F.);
#78956=ADVANCED_FACE('',(#23526),#19661,.F.);
#78957=ADVANCED_FACE('',(#23527),#19662,.F.);
#78958=ADVANCED_FACE('',(#23528),#19663,.F.);
#78959=ADVANCED_FACE('',(#23529),#19664,.F.);
#78960=ADVANCED_FACE('',(#23530),#19665,.F.);
#78961=ADVANCED_FACE('',(#23531),#19666,.F.);
#78962=ADVANCED_FACE('',(#23532),#19667,.F.);
#78963=ADVANCED_FACE('',(#23533),#19668,.F.);
#78964=ADVANCED_FACE('',(#23534),#19669,.F.);
#78965=ADVANCED_FACE('',(#23535),#19670,.F.);
#78966=ADVANCED_FACE('',(#23536),#19671,.F.);
#78967=ADVANCED_FACE('',(#23537),#19672,.F.);
#78968=ADVANCED_FACE('',(#23538),#19673,.F.);
#78969=ADVANCED_FACE('',(#23539),#19674,.F.);
#78970=ADVANCED_FACE('',(#23540),#19675,.F.);
#78971=ADVANCED_FACE('',(#23541),#19676,.F.);
#78972=ADVANCED_FACE('',(#23542),#19677,.F.);
#78973=ADVANCED_FACE('',(#23543),#19678,.F.);
#78974=ADVANCED_FACE('',(#23544),#19679,.F.);
#78975=ADVANCED_FACE('',(#23545),#19680,.F.);
#78976=ADVANCED_FACE('',(#23546),#19681,.F.);
#78977=ADVANCED_FACE('',(#23547),#19682,.F.);
#78978=ADVANCED_FACE('',(#23548),#19683,.F.);
#78979=ADVANCED_FACE('',(#23549),#19684,.F.);
#78980=ADVANCED_FACE('',(#23550),#19685,.F.);
#78981=ADVANCED_FACE('',(#23551),#19686,.F.);
#78982=ADVANCED_FACE('',(#23552),#19687,.F.);
#78983=ADVANCED_FACE('',(#23553),#19688,.F.);
#78984=ADVANCED_FACE('',(#23554),#19689,.F.);
#78985=ADVANCED_FACE('',(#23555),#19690,.F.);
#78986=ADVANCED_FACE('',(#23556),#19691,.F.);
#78987=ADVANCED_FACE('',(#23557),#19692,.F.);
#78988=ADVANCED_FACE('',(#23558),#19693,.F.);
#78989=ADVANCED_FACE('',(#23559),#19694,.F.);
#78990=ADVANCED_FACE('',(#23560),#19695,.F.);
#78991=ADVANCED_FACE('',(#23561),#19696,.F.);
#78992=ADVANCED_FACE('',(#23562),#19697,.F.);
#78993=ADVANCED_FACE('',(#23563),#19698,.F.);
#78994=ADVANCED_FACE('',(#23564),#19699,.F.);
#78995=ADVANCED_FACE('',(#23565),#19700,.F.);
#78996=ADVANCED_FACE('',(#23566),#19701,.F.);
#78997=ADVANCED_FACE('',(#23567),#19702,.F.);
#78998=ADVANCED_FACE('',(#23568),#19703,.F.);
#78999=ADVANCED_FACE('',(#23569),#19704,.F.);
#79000=ADVANCED_FACE('',(#23570),#19705,.F.);
#79001=ADVANCED_FACE('',(#23571),#19706,.F.);
#79002=ADVANCED_FACE('',(#23572),#19707,.F.);
#79003=ADVANCED_FACE('',(#23573),#19708,.F.);
#79004=ADVANCED_FACE('',(#23574),#19709,.F.);
#79005=ADVANCED_FACE('',(#23575),#19710,.F.);
#79006=ADVANCED_FACE('',(#23576),#19711,.F.);
#79007=ADVANCED_FACE('',(#23577),#19712,.F.);
#79008=ADVANCED_FACE('',(#23578),#19713,.F.);
#79009=ADVANCED_FACE('',(#23579),#19714,.F.);
#79010=ADVANCED_FACE('',(#23580),#19715,.F.);
#79011=ADVANCED_FACE('',(#23581),#19716,.F.);
#79012=ADVANCED_FACE('',(#23582),#19717,.F.);
#79013=ADVANCED_FACE('',(#23583),#19718,.F.);
#79014=ADVANCED_FACE('',(#23584),#19719,.F.);
#79015=ADVANCED_FACE('',(#23585),#19720,.F.);
#79016=ADVANCED_FACE('',(#23586),#19721,.F.);
#79017=ADVANCED_FACE('',(#23587),#19722,.F.);
#79018=ADVANCED_FACE('',(#23588),#19723,.F.);
#79019=ADVANCED_FACE('',(#23589),#19724,.F.);
#79020=ADVANCED_FACE('',(#23590),#19725,.F.);
#79021=ADVANCED_FACE('',(#23591),#19726,.F.);
#79022=ADVANCED_FACE('',(#23592),#19727,.F.);
#79023=ADVANCED_FACE('',(#23593),#19728,.F.);
#79024=ADVANCED_FACE('',(#23594),#19729,.F.);
#79025=ADVANCED_FACE('',(#23595),#19730,.F.);
#79026=ADVANCED_FACE('',(#23596),#19731,.F.);
#79027=ADVANCED_FACE('',(#23597),#19732,.F.);
#79028=ADVANCED_FACE('',(#23598),#19733,.F.);
#79029=ADVANCED_FACE('',(#23599),#19734,.F.);
#79030=ADVANCED_FACE('',(#23600),#19735,.F.);
#79031=ADVANCED_FACE('',(#23601),#19736,.F.);
#79032=ADVANCED_FACE('',(#23602),#19737,.F.);
#79033=ADVANCED_FACE('',(#23603),#19738,.F.);
#79034=ADVANCED_FACE('',(#23604),#19739,.F.);
#79035=ADVANCED_FACE('',(#23605),#19740,.F.);
#79036=ADVANCED_FACE('',(#23606),#19741,.F.);
#79037=ADVANCED_FACE('',(#23607),#19742,.F.);
#79038=ADVANCED_FACE('',(#23608),#19743,.F.);
#79039=ADVANCED_FACE('',(#23609),#19744,.F.);
#79040=ADVANCED_FACE('',(#23610),#19745,.F.);
#79041=ADVANCED_FACE('',(#23611),#19746,.F.);
#79042=ADVANCED_FACE('',(#23612),#19747,.F.);
#79043=ADVANCED_FACE('',(#23613),#19748,.F.);
#79044=ADVANCED_FACE('',(#23614),#19749,.F.);
#79045=ADVANCED_FACE('',(#23615),#19750,.F.);
#79046=ADVANCED_FACE('',(#23616),#19751,.F.);
#79047=ADVANCED_FACE('',(#23617),#19752,.F.);
#79048=ADVANCED_FACE('',(#23618),#19753,.F.);
#79049=ADVANCED_FACE('',(#23619),#19754,.F.);
#79050=ADVANCED_FACE('',(#23620),#19755,.F.);
#79051=ADVANCED_FACE('',(#23621),#19756,.F.);
#79052=ADVANCED_FACE('',(#23622),#19757,.F.);
#79053=ADVANCED_FACE('',(#23623),#19758,.F.);
#79054=ADVANCED_FACE('',(#23624),#19759,.F.);
#79055=ADVANCED_FACE('',(#23625),#19760,.F.);
#79056=ADVANCED_FACE('',(#23626),#19761,.F.);
#79057=ADVANCED_FACE('',(#23627),#19762,.F.);
#79058=ADVANCED_FACE('',(#23628),#19763,.F.);
#79059=ADVANCED_FACE('',(#23629),#19764,.F.);
#79060=ADVANCED_FACE('',(#23630),#19765,.F.);
#79061=ADVANCED_FACE('',(#23631),#19766,.F.);
#79062=ADVANCED_FACE('',(#23632),#19767,.F.);
#79063=ADVANCED_FACE('',(#23633),#19768,.F.);
#79064=ADVANCED_FACE('',(#23634),#19769,.F.);
#79065=ADVANCED_FACE('',(#23635),#19770,.F.);
#79066=ADVANCED_FACE('',(#23636),#19771,.F.);
#79067=ADVANCED_FACE('',(#23637),#19772,.F.);
#79068=ADVANCED_FACE('',(#23638),#19773,.F.);
#79069=ADVANCED_FACE('',(#23639),#19774,.F.);
#79070=ADVANCED_FACE('',(#23640),#19775,.F.);
#79071=ADVANCED_FACE('',(#23641),#19776,.F.);
#79072=ADVANCED_FACE('',(#23642),#19777,.F.);
#79073=ADVANCED_FACE('',(#23643),#19778,.F.);
#79074=ADVANCED_FACE('',(#23644),#19779,.F.);
#79075=ADVANCED_FACE('',(#23645),#19780,.F.);
#79076=ADVANCED_FACE('',(#23646),#19781,.F.);
#79077=ADVANCED_FACE('',(#23647),#19782,.F.);
#79078=ADVANCED_FACE('',(#23648),#19783,.F.);
#79079=ADVANCED_FACE('',(#23649),#19784,.F.);
#79080=ADVANCED_FACE('',(#23650),#19785,.F.);
#79081=ADVANCED_FACE('',(#23651),#19786,.F.);
#79082=ADVANCED_FACE('',(#23652),#19787,.F.);
#79083=ADVANCED_FACE('',(#23653),#19788,.F.);
#79084=ADVANCED_FACE('',(#23654),#19789,.F.);
#79085=ADVANCED_FACE('',(#23655),#19790,.F.);
#79086=ADVANCED_FACE('',(#23656),#19791,.F.);
#79087=ADVANCED_FACE('',(#23657),#19792,.F.);
#79088=ADVANCED_FACE('',(#23658),#19793,.F.);
#79089=ADVANCED_FACE('',(#23659),#19794,.F.);
#79090=ADVANCED_FACE('',(#23660),#19795,.F.);
#79091=ADVANCED_FACE('',(#23661),#19796,.F.);
#79092=ADVANCED_FACE('',(#23662),#19797,.F.);
#79093=ADVANCED_FACE('',(#23663),#19798,.F.);
#79094=ADVANCED_FACE('',(#23664),#19799,.F.);
#79095=ADVANCED_FACE('',(#23665),#19800,.F.);
#79096=ADVANCED_FACE('',(#23666),#19801,.F.);
#79097=ADVANCED_FACE('',(#23667),#19802,.F.);
#79098=ADVANCED_FACE('',(#23668),#19803,.F.);
#79099=ADVANCED_FACE('',(#23669),#19804,.F.);
#79100=ADVANCED_FACE('',(#23670),#19805,.F.);
#79101=ADVANCED_FACE('',(#23671),#19806,.F.);
#79102=ADVANCED_FACE('',(#23672),#19807,.F.);
#79103=ADVANCED_FACE('',(#23673),#19808,.F.);
#79104=ADVANCED_FACE('',(#23674),#19809,.F.);
#79105=ADVANCED_FACE('',(#23675),#19810,.F.);
#79106=ADVANCED_FACE('',(#23676),#19811,.F.);
#79107=ADVANCED_FACE('',(#23677),#19812,.F.);
#79108=ADVANCED_FACE('',(#23678),#19813,.F.);
#79109=ADVANCED_FACE('',(#23679),#19814,.F.);
#79110=ADVANCED_FACE('',(#23680),#19815,.F.);
#79111=ADVANCED_FACE('',(#23681),#19816,.F.);
#79112=ADVANCED_FACE('',(#23682),#19817,.F.);
#79113=ADVANCED_FACE('',(#23683),#19818,.F.);
#79114=ADVANCED_FACE('',(#23684),#19819,.F.);
#79115=ADVANCED_FACE('',(#23685),#19820,.F.);
#79116=ADVANCED_FACE('',(#23686),#19821,.F.);
#79117=ADVANCED_FACE('',(#23687),#19822,.F.);
#79118=ADVANCED_FACE('',(#23688),#19823,.F.);
#79119=ADVANCED_FACE('',(#23689),#19824,.F.);
#79120=ADVANCED_FACE('',(#23690),#19825,.F.);
#79121=ADVANCED_FACE('',(#23691),#19826,.F.);
#79122=ADVANCED_FACE('',(#23692),#19827,.F.);
#79123=ADVANCED_FACE('',(#23693),#19828,.F.);
#79124=ADVANCED_FACE('',(#23694),#19829,.F.);
#79125=ADVANCED_FACE('',(#23695),#19830,.F.);
#79126=ADVANCED_FACE('',(#23696),#19831,.F.);
#79127=ADVANCED_FACE('',(#23697),#19832,.F.);
#79128=ADVANCED_FACE('',(#23698),#19833,.F.);
#79129=ADVANCED_FACE('',(#23699),#19834,.F.);
#79130=ADVANCED_FACE('',(#23700,#331),#19835,.F.);
#79131=ADVANCED_FACE('',(#23701,#332,#333,#334,#335,#336,#337,#338,#339,
#340,#341,#342,#343,#344,#345,#346,#347,#348,#349,#350,#351,#352,#353,#354,
#355,#356,#357,#358,#359,#360,#361,#362,#363,#364,#365,#366,#367,#368,#369,
#370,#371,#372,#373,#374,#375,#376,#377,#378,#379,#380,#381,#382,#383,#384,
#385,#386,#387,#388,#389,#390,#391,#392,#393,#394,#395,#396,#397,#398,#399,
#400,#401,#402,#403,#404,#405,#406,#407,#408,#409,#410,#411,#412,#413,#414,
#415,#416,#417,#418,#419,#420,#421,#422,#423,#424,#425,#426,#427,#428,#429,
#430,#431,#432,#433,#434,#435,#436,#437,#438,#439,#440,#441,#442,#443,#444,
#445,#446,#447,#448,#449,#450,#451,#452,#453,#454,#455,#456,#457,#458,#459,
#460,#461,#462,#463,#464,#465,#466,#467,#468,#469,#470,#471,#472,#473,#474,
#475,#476,#477,#478,#479,#480,#481,#482,#483,#484,#485,#486,#487,#488,#489,
#490,#491,#492,#493,#494,#495,#496,#497,#498,#499,#500,#501,#502,#503,#504,
#505,#506,#507,#508,#509,#510,#511,#512,#513,#514,#515,#516,#517,#518,#519,
#520,#521,#522,#523,#524,#525,#526,#527,#528,#529,#530,#531,#532,#533,#534,
#535,#536,#537,#538,#539,#540,#541,#542,#543,#544,#545,#546,#547,#548,#549,
#550,#551,#552,#553,#554,#555,#556,#557,#558,#559,#560,#561,#562,#563,#564,
#565,#566,#567,#568,#569,#570,#571,#572,#573,#574,#575,#576,#577,#578,#579,
#580,#581,#582,#583,#584,#585,#586,#587,#588,#589,#590,#591,#592,#593,#594,
#595,#596,#597,#598,#599,#600,#601,#602,#603,#604,#605,#606,#607,#608,#609,
#610,#611,#612,#613,#614,#615,#616,#617,#618,#619,#620,#621,#622,#623,#624,
#625,#626,#627,#628,#629,#630,#631,#632,#633,#634,#635,#636,#637,#638,#639,
#640,#641,#642,#643,#644,#645,#646,#647,#648,#649,#650,#651,#652,#653,#654,
#655,#656,#657,#658,#659,#660,#661,#662,#663,#664,#665,#666,#667,#668,#669,
#670,#671,#672,#673,#674,#675,#676,#677,#678,#679,#680,#681,#682,#683,#684,
#685,#686,#687,#688,#689,#690,#691,#692,#693,#694,#695,#696,#697,#698,#699,
#700,#701,#702,#703,#704,#705,#706,#707,#708,#709,#710,#711,#712,#713,#714,
#715,#716,#717,#718,#719,#720,#721,#722,#723,#724,#725,#726,#727,#728,#729,
#730,#731,#732,#733,#734,#735,#736,#737,#738,#739,#740,#741,#742,#743,#744,
#745,#746,#747,#748,#749,#750,#751,#752,#753,#754,#755,#756,#757,#758,#759,
#760,#761,#762,#763,#764,#765,#766,#767,#768),#19836,.F.);
#79132=ADVANCED_FACE('',(#23702),#19837,.F.);
#79133=ADVANCED_FACE('',(#23703),#19838,.F.);
#79134=ADVANCED_FACE('',(#23704),#19839,.F.);
#79135=ADVANCED_FACE('',(#23705),#19840,.F.);
#79136=ADVANCED_FACE('',(#23706,#769,#770,#771,#772,#773,#774,#775,#776,
#777,#778,#779,#780,#781,#782,#783,#784,#785,#786,#787,#788,#789,#790,#791,
#792,#793,#794,#795,#796,#797,#798,#799,#800,#801,#802,#803,#804,#805,#806,
#807,#808,#809,#810,#811,#812,#813,#814,#815,#816,#817,#818,#819,#820,#821,
#822,#823,#824,#825,#826,#827,#828,#829,#830,#831,#832,#833,#834,#835,#836,
#837,#838,#839,#840,#841,#842,#843,#844,#845,#846,#847,#848,#849,#850,#851,
#852,#853,#854,#855,#856,#857,#858,#859,#860,#861,#862,#863,#864,#865,#866,
#867,#868,#869,#870,#871,#872,#873,#874,#875,#876,#877,#878,#879,#880,#881,
#882,#883,#884,#885,#886,#887,#888,#889,#890,#891,#892,#893,#894,#895,#896,
#897,#898,#899,#900,#901,#902,#903,#904,#905,#906,#907,#908,#909,#910,#911,
#912,#913,#914,#915,#916,#917,#918,#919,#920,#921,#922,#923,#924,#925,#926,
#927,#928,#929,#930,#931,#932,#933,#934,#935,#936,#937,#938,#939,#940,#941,
#942,#943,#944,#945,#946,#947,#948,#949,#950,#951,#952,#953,#954,#955,#956,
#957,#958,#959,#960,#961,#962,#963,#964,#965,#966,#967,#968,#969,#970,#971,
#972,#973,#974,#975,#976,#977,#978,#979,#980,#981,#982,#983,#984,#985,#986,
#987,#988,#989,#990,#991,#992,#993,#994,#995,#996,#997,#998,#999,#1000,
#1001,#1002,#1003,#1004,#1005,#1006,#1007,#1008,#1009,#1010,#1011,#1012,
#1013,#1014,#1015,#1016,#1017,#1018,#1019,#1020,#1021,#1022,#1023,#1024,
#1025,#1026,#1027,#1028,#1029,#1030,#1031,#1032,#1033,#1034,#1035,#1036,
#1037,#1038,#1039,#1040,#1041,#1042,#1043,#1044,#1045,#1046,#1047,#1048,
#1049,#1050,#1051,#1052,#1053,#1054,#1055,#1056,#1057,#1058,#1059,#1060,
#1061,#1062,#1063,#1064,#1065,#1066,#1067,#1068,#1069,#1070,#1071,#1072,
#1073,#1074,#1075,#1076,#1077,#1078,#1079,#1080,#1081,#1082,#1083,#1084,
#1085,#1086,#1087,#1088,#1089,#1090,#1091,#1092,#1093,#1094,#1095,#1096,
#1097,#1098,#1099,#1100,#1101,#1102,#1103,#1104,#1105,#1106,#1107,#1108,
#1109,#1110,#1111,#1112,#1113,#1114,#1115,#1116,#1117,#1118,#1119,#1120,
#1121,#1122,#1123,#1124,#1125,#1126,#1127,#1128,#1129,#1130,#1131,#1132,
#1133,#1134,#1135,#1136,#1137,#1138,#1139,#1140,#1141,#1142,#1143,#1144,
#1145,#1146,#1147,#1148,#1149,#1150,#1151,#1152,#1153,#1154,#1155,#1156,
#1157,#1158,#1159,#1160,#1161,#1162,#1163,#1164,#1165,#1166,#1167,#1168,
#1169,#1170,#1171,#1172,#1173,#1174,#1175,#1176,#1177,#1178,#1179,#1180,
#1181,#1182,#1183,#1184,#1185,#1186,#1187,#1188,#1189,#1190,#1191,#1192,
#1193,#1194,#1195,#1196,#1197,#1198,#1199,#1200,#1201,#1202,#1203,#1204,
#1205),#19841,.T.);
#79137=ADVANCED_FACE('',(#23707,#1206),#19842,.T.);
#79138=ADVANCED_FACE('',(#23708),#19843,.F.);
#79139=ADVANCED_FACE('',(#23709),#19844,.F.);
#79140=ADVANCED_FACE('',(#23710),#19845,.F.);
#79141=ADVANCED_FACE('',(#23711),#19846,.F.);
#79142=ADVANCED_FACE('',(#23712),#2295,.F.);
#79143=ADVANCED_FACE('',(#23713),#2296,.F.);
#79144=ADVANCED_FACE('',(#23714),#19847,.F.);
#79145=ADVANCED_FACE('',(#23715),#19848,.F.);
#79146=ADVANCED_FACE('',(#23716),#19849,.F.);
#79147=ADVANCED_FACE('',(#23717),#19850,.F.);
#79148=ADVANCED_FACE('',(#23718),#2297,.F.);
#79149=ADVANCED_FACE('',(#23719),#2298,.F.);
#79150=ADVANCED_FACE('',(#23720,#1207),#19851,.T.);
#79151=ADVANCED_FACE('',(#23721,#1208,#1209,#1210,#1211,#1212,#1213,#1214,
#1215,#1216,#1217,#1218,#1219,#1220,#1221,#1222,#1223,#1224,#1225,#1226,
#1227,#1228,#1229,#1230,#1231,#1232,#1233,#1234,#1235,#1236,#1237,#1238,
#1239,#1240,#1241,#1242,#1243,#1244,#1245,#1246,#1247,#1248,#1249,#1250,
#1251,#1252,#1253,#1254,#1255,#1256,#1257,#1258,#1259,#1260,#1261,#1262,
#1263,#1264,#1265,#1266,#1267,#1268,#1269,#1270,#1271,#1272,#1273,#1274,
#1275,#1276,#1277,#1278,#1279,#1280,#1281,#1282,#1283,#1284,#1285,#1286,
#1287,#1288,#1289,#1290,#1291,#1292,#1293,#1294,#1295,#1296,#1297,#1298,
#1299,#1300,#1301,#1302,#1303,#1304,#1305,#1306,#1307,#1308,#1309,#1310,
#1311,#1312,#1313,#1314,#1315,#1316,#1317,#1318,#1319,#1320,#1321,#1322,
#1323,#1324,#1325,#1326,#1327,#1328,#1329,#1330,#1331,#1332,#1333,#1334,
#1335,#1336,#1337,#1338,#1339,#1340,#1341,#1342,#1343,#1344,#1345,#1346,
#1347,#1348,#1349,#1350,#1351,#1352,#1353,#1354,#1355,#1356,#1357,#1358,
#1359,#1360,#1361,#1362,#1363,#1364,#1365,#1366,#1367,#1368,#1369,#1370,
#1371,#1372,#1373,#1374,#1375,#1376,#1377,#1378,#1379,#1380,#1381,#1382,
#1383,#1384,#1385,#1386,#1387,#1388,#1389,#1390,#1391,#1392,#1393,#1394,
#1395,#1396,#1397,#1398,#1399,#1400,#1401,#1402,#1403,#1404,#1405,#1406,
#1407,#1408,#1409,#1410,#1411,#1412,#1413,#1414,#1415,#1416,#1417,#1418,
#1419,#1420,#1421,#1422,#1423,#1424,#1425,#1426,#1427,#1428,#1429,#1430,
#1431,#1432,#1433,#1434,#1435,#1436,#1437,#1438,#1439,#1440,#1441,#1442,
#1443,#1444,#1445,#1446,#1447,#1448,#1449,#1450,#1451,#1452,#1453,#1454,
#1455,#1456,#1457,#1458,#1459,#1460,#1461,#1462,#1463),#75297,.F.);
#79152=ADVANCED_FACE('',(#23722),#19852,.F.);
#79153=ADVANCED_FACE('',(#23723),#19853,.F.);
#79154=ADVANCED_FACE('',(#23724),#19854,.F.);
#79155=ADVANCED_FACE('',(#23725),#19855,.F.);
#79156=ADVANCED_FACE('',(#23726,#1464,#1465,#1466,#1467,#1468,#1469,#1470,
#1471,#1472,#1473,#1474,#1475,#1476,#1477,#1478,#1479,#1480,#1481,#1482,
#1483,#1484,#1485,#1486,#1487,#1488,#1489,#1490,#1491,#1492,#1493,#1494,
#1495,#1496,#1497,#1498,#1499,#1500,#1501,#1502,#1503,#1504,#1505,#1506,
#1507,#1508,#1509,#1510,#1511,#1512,#1513,#1514,#1515,#1516,#1517,#1518,
#1519,#1520,#1521,#1522,#1523,#1524,#1525,#1526,#1527,#1528,#1529,#1530,
#1531,#1532,#1533,#1534,#1535,#1536,#1537,#1538,#1539,#1540,#1541,#1542,
#1543,#1544,#1545,#1546,#1547,#1548,#1549,#1550,#1551,#1552,#1553,#1554,
#1555,#1556,#1557,#1558,#1559,#1560,#1561,#1562,#1563,#1564,#1565,#1566,
#1567,#1568,#1569,#1570,#1571,#1572,#1573,#1574,#1575,#1576,#1577,#1578,
#1579,#1580,#1581,#1582,#1583,#1584,#1585,#1586,#1587,#1588,#1589,#1590,
#1591,#1592,#1593,#1594,#1595,#1596,#1597,#1598,#1599,#1600,#1601,#1602,
#1603,#1604,#1605,#1606,#1607,#1608,#1609,#1610,#1611,#1612,#1613,#1614,
#1615,#1616,#1617,#1618,#1619,#1620,#1621,#1622,#1623,#1624,#1625,#1626,
#1627,#1628,#1629,#1630,#1631,#1632,#1633,#1634,#1635,#1636,#1637,#1638,
#1639,#1640,#1641,#1642,#1643,#1644,#1645,#1646,#1647,#1648,#1649,#1650,
#1651,#1652,#1653,#1654,#1655,#1656,#1657,#1658,#1659,#1660,#1661,#1662,
#1663,#1664,#1665,#1666,#1667,#1668,#1669,#1670,#1671,#1672,#1673,#1674,
#1675,#1676,#1677,#1678,#1679,#1680,#1681,#1682,#1683,#1684,#1685,#1686,
#1687,#1688,#1689,#1690,#1691,#1692,#1693,#1694,#1695,#1696,#1697,#1698,
#1699,#1700,#1701,#1702,#1703,#1704,#1705,#1706,#1707,#1708,#1709,#1710,
#1711,#1712,#1713,#1714,#1715,#1716,#1717,#1718,#1719),#75298,.T.);
#79157=ADVANCED_FACE('',(#23727,#1720),#19856,.F.);
#79158=ADVANCED_FACE('',(#23728),#2299,.T.);
#79159=ADVANCED_FACE('',(#23729),#2300,.T.);
#79160=ADVANCED_FACE('',(#23730),#2301,.T.);
#79161=ADVANCED_FACE('',(#23731),#2302,.T.);
#79162=ADVANCED_FACE('',(#23732),#2303,.T.);
#79163=ADVANCED_FACE('',(#23733),#2304,.T.);
#79164=ADVANCED_FACE('',(#23734),#2305,.T.);
#79165=ADVANCED_FACE('',(#23735),#2306,.T.);
#79166=ADVANCED_FACE('',(#23736),#2307,.T.);
#79167=ADVANCED_FACE('',(#23737),#2308,.T.);
#79168=ADVANCED_FACE('',(#23738),#2309,.T.);
#79169=ADVANCED_FACE('',(#23739),#2310,.T.);
#79170=ADVANCED_FACE('',(#23740),#2311,.T.);
#79171=ADVANCED_FACE('',(#23741),#2312,.T.);
#79172=ADVANCED_FACE('',(#23742),#2313,.T.);
#79173=ADVANCED_FACE('',(#23743),#2314,.T.);
#79174=ADVANCED_FACE('',(#23744),#2315,.T.);
#79175=ADVANCED_FACE('',(#23745),#1963,.T.);
#79176=ADVANCED_FACE('',(#23746),#2316,.T.);
#79177=ADVANCED_FACE('',(#23747),#2317,.T.);
#79178=ADVANCED_FACE('',(#23748),#2318,.T.);
#79179=ADVANCED_FACE('',(#23749),#2319,.T.);
#79180=ADVANCED_FACE('',(#23750),#2320,.T.);
#79181=ADVANCED_FACE('',(#23751),#2321,.T.);
#79182=ADVANCED_FACE('',(#23752),#2322,.T.);
#79183=ADVANCED_FACE('',(#23753),#2323,.T.);
#79184=ADVANCED_FACE('',(#23754),#2324,.T.);
#79185=ADVANCED_FACE('',(#23755),#2325,.T.);
#79186=ADVANCED_FACE('',(#23756),#2326,.T.);
#79187=ADVANCED_FACE('',(#23757),#2327,.T.);
#79188=ADVANCED_FACE('',(#23758),#2328,.T.);
#79189=ADVANCED_FACE('',(#23759),#2329,.T.);
#79190=ADVANCED_FACE('',(#23760),#2330,.T.);
#79191=ADVANCED_FACE('',(#23761),#2331,.T.);
#79192=ADVANCED_FACE('',(#23762),#1964,.T.);
#79193=ADVANCED_FACE('',(#23763),#1965,.T.);
#79194=ADVANCED_FACE('',(#23764),#2332,.F.);
#79195=ADVANCED_FACE('',(#23765),#2333,.T.);
#79196=ADVANCED_FACE('',(#23766),#2334,.T.);
#79197=ADVANCED_FACE('',(#23767),#2335,.T.);
#79198=ADVANCED_FACE('',(#23768),#2336,.T.);
#79199=ADVANCED_FACE('',(#23769),#2337,.T.);
#79200=ADVANCED_FACE('',(#23770),#2338,.T.);
#79201=ADVANCED_FACE('',(#23771),#207,.F.);
#79202=ADVANCED_FACE('',(#23772),#208,.F.);
#79203=ADVANCED_FACE('',(#23773),#209,.F.);
#79204=ADVANCED_FACE('',(#23774),#210,.F.);
#79205=ADVANCED_FACE('',(#23775),#19857,.F.);
#79206=ADVANCED_FACE('',(#23776),#211,.F.);
#79207=ADVANCED_FACE('',(#23777),#212,.F.);
#79208=ADVANCED_FACE('',(#23778),#213,.F.);
#79209=ADVANCED_FACE('',(#23779),#214,.F.);
#79210=ADVANCED_FACE('',(#23780),#19858,.T.);
#79211=ADVANCED_FACE('',(#23781),#75299,.T.);
#79212=ADVANCED_FACE('',(#23782),#1966,.T.);
#79213=ADVANCED_FACE('',(#23783),#215,.F.);
#79214=ADVANCED_FACE('',(#23784),#216,.F.);
#79215=ADVANCED_FACE('',(#23785),#217,.F.);
#79216=ADVANCED_FACE('',(#23786),#218,.F.);
#79217=ADVANCED_FACE('',(#23787),#19859,.F.);
#79218=ADVANCED_FACE('',(#23788),#219,.F.);
#79219=ADVANCED_FACE('',(#23789),#220,.F.);
#79220=ADVANCED_FACE('',(#23790),#221,.F.);
#79221=ADVANCED_FACE('',(#23791),#222,.F.);
#79222=ADVANCED_FACE('',(#23792),#2339,.T.);
#79223=ADVANCED_FACE('',(#23793),#223,.F.);
#79224=ADVANCED_FACE('',(#23794),#224,.F.);
#79225=ADVANCED_FACE('',(#23795),#2340,.F.);
#79226=ADVANCED_FACE('',(#23796),#1967,.F.);
#79227=ADVANCED_FACE('',(#23797,#1721),#19860,.F.);
#79228=ADVANCED_FACE('',(#23798,#1722),#19861,.F.);
#79229=ADVANCED_FACE('',(#23799,#1723),#19862,.T.);
#79230=ADVANCED_FACE('',(#23800),#2341,.F.);
#79231=ADVANCED_FACE('',(#23801),#1968,.F.);
#79232=ADVANCED_FACE('',(#23802,#1724),#19863,.T.);
#79233=ADVANCED_FACE('',(#23803),#2342,.T.);
#79234=ADVANCED_FACE('',(#23804),#225,.F.);
#79235=ADVANCED_FACE('',(#23805),#75300,.T.);
#79236=ADVANCED_FACE('',(#23806),#19864,.T.);
#79237=ADVANCED_FACE('',(#23807),#2343,.T.);
#79238=ADVANCED_FACE('',(#23808),#2344,.T.);
#79239=ADVANCED_FACE('',(#23809),#2345,.T.);
#79240=ADVANCED_FACE('',(#23810),#2346,.T.);
#79241=ADVANCED_FACE('',(#23811),#2347,.T.);
#79242=ADVANCED_FACE('',(#23812),#2348,.T.);
#79243=ADVANCED_FACE('',(#23813),#2349,.T.);
#79244=ADVANCED_FACE('',(#23814),#2350,.T.);
#79245=ADVANCED_FACE('',(#23815),#2351,.T.);
#79246=ADVANCED_FACE('',(#23816),#2352,.T.);
#79247=ADVANCED_FACE('',(#23817),#2353,.T.);
#79248=ADVANCED_FACE('',(#23818),#2354,.T.);
#79249=ADVANCED_FACE('',(#23819),#2355,.T.);
#79250=ADVANCED_FACE('',(#23820),#2356,.T.);
#79251=ADVANCED_FACE('',(#23821),#2357,.T.);
#79252=ADVANCED_FACE('',(#23822),#2358,.T.);
#79253=ADVANCED_FACE('',(#23823),#2359,.T.);
#79254=ADVANCED_FACE('',(#23824),#2360,.T.);
#79255=ADVANCED_FACE('',(#23825),#1969,.T.);
#79256=ADVANCED_FACE('',(#23826),#2361,.T.);
#79257=ADVANCED_FACE('',(#23827),#2362,.T.);
#79258=ADVANCED_FACE('',(#23828),#2363,.T.);
#79259=ADVANCED_FACE('',(#23829),#2364,.T.);
#79260=ADVANCED_FACE('',(#23830),#2365,.T.);
#79261=ADVANCED_FACE('',(#23831),#2366,.T.);
#79262=ADVANCED_FACE('',(#23832),#2367,.T.);
#79263=ADVANCED_FACE('',(#23833),#2368,.T.);
#79264=ADVANCED_FACE('',(#23834),#2369,.T.);
#79265=ADVANCED_FACE('',(#23835),#2370,.T.);
#79266=ADVANCED_FACE('',(#23836),#2371,.T.);
#79267=ADVANCED_FACE('',(#23837),#2372,.T.);
#79268=ADVANCED_FACE('',(#23838),#2373,.T.);
#79269=ADVANCED_FACE('',(#23839),#2374,.T.);
#79270=ADVANCED_FACE('',(#23840),#2375,.T.);
#79271=ADVANCED_FACE('',(#23841),#2376,.T.);
#79272=ADVANCED_FACE('',(#23842),#1970,.T.);
#79273=ADVANCED_FACE('',(#23843),#1971,.T.);
#79274=ADVANCED_FACE('',(#23844),#2377,.F.);
#79275=ADVANCED_FACE('',(#23845),#2378,.T.);
#79276=ADVANCED_FACE('',(#23846),#2379,.T.);
#79277=ADVANCED_FACE('',(#23847),#2380,.T.);
#79278=ADVANCED_FACE('',(#23848),#2381,.T.);
#79279=ADVANCED_FACE('',(#23849),#2382,.T.);
#79280=ADVANCED_FACE('',(#23850),#2383,.T.);
#79281=ADVANCED_FACE('',(#23851),#226,.F.);
#79282=ADVANCED_FACE('',(#23852),#227,.F.);
#79283=ADVANCED_FACE('',(#23853),#228,.F.);
#79284=ADVANCED_FACE('',(#23854),#229,.F.);
#79285=ADVANCED_FACE('',(#23855),#19865,.F.);
#79286=ADVANCED_FACE('',(#23856),#230,.F.);
#79287=ADVANCED_FACE('',(#23857),#231,.F.);
#79288=ADVANCED_FACE('',(#23858),#232,.F.);
#79289=ADVANCED_FACE('',(#23859),#233,.F.);
#79290=ADVANCED_FACE('',(#23860),#19866,.T.);
#79291=ADVANCED_FACE('',(#23861),#75301,.T.);
#79292=ADVANCED_FACE('',(#23862),#1972,.T.);
#79293=ADVANCED_FACE('',(#23863),#234,.F.);
#79294=ADVANCED_FACE('',(#23864),#235,.F.);
#79295=ADVANCED_FACE('',(#23865),#236,.F.);
#79296=ADVANCED_FACE('',(#23866),#237,.F.);
#79297=ADVANCED_FACE('',(#23867),#19867,.F.);
#79298=ADVANCED_FACE('',(#23868),#238,.F.);
#79299=ADVANCED_FACE('',(#23869),#239,.F.);
#79300=ADVANCED_FACE('',(#23870),#240,.F.);
#79301=ADVANCED_FACE('',(#23871),#241,.F.);
#79302=ADVANCED_FACE('',(#23872),#2384,.T.);
#79303=ADVANCED_FACE('',(#23873),#242,.F.);
#79304=ADVANCED_FACE('',(#23874),#243,.F.);
#79305=ADVANCED_FACE('',(#23875),#2385,.F.);
#79306=ADVANCED_FACE('',(#23876),#1973,.F.);
#79307=ADVANCED_FACE('',(#23877,#1725),#19868,.F.);
#79308=ADVANCED_FACE('',(#23878,#1726),#19869,.F.);
#79309=ADVANCED_FACE('',(#23879,#1727),#19870,.T.);
#79310=ADVANCED_FACE('',(#23880),#2386,.F.);
#79311=ADVANCED_FACE('',(#23881),#1974,.F.);
#79312=ADVANCED_FACE('',(#23882,#1728),#19871,.T.);
#79313=ADVANCED_FACE('',(#23883),#2387,.T.);
#79314=ADVANCED_FACE('',(#23884),#244,.F.);
#79315=ADVANCED_FACE('',(#23885),#75302,.T.);
#79316=ADVANCED_FACE('',(#23886),#19872,.T.);
#79317=ADVANCED_FACE('',(#23887),#2388,.T.);
#79318=CLOSED_SHELL('',(#75303,#75304,#75305,#75306,#75307,#75308,#75309));
#79319=CLOSED_SHELL('',(#75310,#75311,#75312,#75313,#75314,#75315,#75316));
#79320=CLOSED_SHELL('',(#75317,#75318,#75319,#75320,#75321,#75322,#75323,
#75324,#75325,#75326));
#79321=CLOSED_SHELL('',(#75327,#75328,#75329,#75330,#75331,#75332,#75333,
#75334,#75335,#75336));
#79322=CLOSED_SHELL('',(#75337,#75338,#75339,#75340,#75341,#75342,#75343,
#75344,#75345,#75346,#75347,#75348,#75349,#75350,#75351,#75352,#75353,#75354,
#75355,#75356,#75357,#75358,#75359,#75360,#75361,#75362,#75363,#75364,#75365,
#75366,#75367,#75368,#75369,#75370,#75371,#75372,#75373,#75374,#75375,#75376,
#75377,#75378,#75379,#75380,#75381,#75382,#75383,#75384,#75385,#75386,#75387,
#75388,#75389,#75390,#75391,#75392,#75393,#75394,#75395,#75396,#75397,#75398,
#75399,#75400,#75401,#75402,#75403,#75404,#75405,#75406,#75407,#75408,#75409,
#75410,#75411,#75412,#75413,#75414,#75415,#75416,#75417,#75418,#75419,#75420,
#75421,#75422,#75423,#75424,#75425,#75426,#75427,#75428,#75429,#75430,#75431,
#75432,#75433,#75434,#75435,#75436,#75437,#75438,#75439,#75440,#75441,#75442,
#75443,#75444,#75445,#75446,#75447,#75448,#75449,#75450,#75451,#75452,#75453,
#75454,#75455,#75456,#75457,#75458,#75459,#75460,#75461,#75462,#75463,#75464,
#75465,#75466,#75467,#75468,#75469,#75470,#75471,#75472,#75473,#75474,#75475,
#75476,#75477,#75478,#75479,#75480,#75481,#75482,#75483,#75484,#75485,#75486,
#75487,#75488,#75489,#75490,#75491,#75492,#75493,#75494,#75495,#75496,#75497,
#75498,#75499,#75500,#75501,#75502,#75503,#75504,#75505,#75506,#75507,#75508,
#75509,#75510,#75511,#75512,#75513,#75514,#75515,#75516,#75517,#75518,#75519,
#75520,#75521,#75522,#75523,#75524,#75525,#75526,#75527,#75528,#75529,#75530,
#75531,#75532,#75533,#75534,#75535,#75536,#75537,#75538,#75539,#75540,#75541,
#75542,#75543,#75544,#75545,#75546,#75547,#75548,#75549,#75550,#75551,#75552,
#75553,#75554,#75555,#75556,#75557,#75558,#75559,#75560,#75561,#75562,#75563,
#75564,#75565,#75566,#75567,#75568,#75569,#75570,#75571,#75572,#75573,#75574,
#75575,#75576,#75577,#75578,#75579,#75580,#75581,#75582,#75583,#75584,#75585,
#75586,#75587,#75588,#75589,#75590,#75591,#75592,#75593,#75594,#75595,#75596,
#75597,#75598,#75599,#75600,#75601,#75602,#75603,#75604,#75605,#75606,#75607,
#75608,#75609,#75610,#75611,#75612,#75613,#75614,#75615,#75616,#75617,#75618,
#75619,#75620,#75621,#75622,#75623,#75624,#75625,#75626,#75627,#75628,#75629,
#75630,#75631,#75632,#75633,#75634,#75635,#75636,#75637,#75638,#75639,#75640,
#75641,#75642,#75643,#75644,#75645,#75646,#75647,#75648,#75649,#75650,#75651,
#75652,#75653,#75654,#75655,#75656,#75657,#75658,#75659,#75660,#75661,#75662,
#75663,#75664,#75665,#75666,#75667,#75668,#75669,#75670,#75671,#75672,#75673,
#75674,#75675,#75676,#75677,#75678,#75679,#75680,#75681,#75682,#75683,#75684,
#75685,#75686,#75687,#75688,#75689,#75690,#75691,#75692,#75693,#75694,#75695,
#75696,#75697,#75698,#75699,#75700,#75701,#75702,#75703,#75704,#75705,#75706,
#75707,#75708,#75709,#75710,#75711,#75712,#75713,#75714,#75715,#75716,#75717,
#75718,#75719,#75720,#75721,#75722,#75723,#75724,#75725,#75726,#75727,#75728,
#75729,#75730,#75731,#75732,#75733,#75734,#75735,#75736,#75737,#75738,#75739,
#75740,#75741,#75742,#75743,#75744,#75745,#75746,#75747,#75748,#75749,#75750,
#75751,#75752,#75753,#75754,#75755,#75756,#75757,#75758,#75759,#75760,#75761,
#75762,#75763,#75764,#75765,#75766,#75767,#75768,#75769,#75770,#75771,#75772,
#75773,#75774,#75775,#75776,#75777,#75778,#75779,#75780,#75781,#75782,#75783,
#75784,#75785,#75786,#75787,#75788,#75789,#75790,#75791,#75792,#75793,#75794,
#75795,#75796,#75797,#75798,#75799,#75800,#75801,#75802,#75803,#75804,#75805,
#75806,#75807,#75808,#75809,#75810,#75811,#75812,#75813,#75814,#75815,#75816,
#75817,#75818,#75819,#75820,#75821,#75822,#75823,#75824,#75825,#75826,#75827,
#75828,#75829,#75830,#75831,#75832,#75833,#75834,#75835,#75836,#75837,#75838,
#75839,#75840,#75841,#75842,#75843,#75844,#75845,#75846,#75847,#75848,#75849,
#75850,#75851,#75852,#75853,#75854,#75855,#75856,#75857,#75858,#75859,#75860,
#75861,#75862,#75863,#75864,#75865,#75866,#75867,#75868,#75869,#75870,#75871,
#75872,#75873,#75874,#75875,#75876,#75877,#75878,#75879,#75880,#75881,#75882,
#75883,#75884,#75885,#75886,#75887,#75888,#75889,#75890,#75891,#75892,#75893,
#75894,#75895,#75896,#75897,#75898,#75899,#75900,#75901,#75902,#75903,#75904,
#75905,#75906,#75907,#75908,#75909,#75910,#75911,#75912,#75913,#75914,#75915,
#75916,#75917,#75918,#75919,#75920,#75921,#75922,#75923,#75924,#75925,#75926,
#75927,#75928,#75929,#75930,#75931,#75932,#75933,#75934,#75935,#75936,#75937,
#75938,#75939,#75940,#75941,#75942,#75943,#75944));
#79323=CLOSED_SHELL('',(#75945,#75946,#75947,#75948,#75949,#75950,#75951,
#75952,#75953,#75954,#75955,#75956,#75957,#75958,#75959,#75960,#75961,#75962,
#75963,#75964,#75965,#75966,#75967,#75968,#75969,#75970,#75971,#75972,#75973,
#75974,#75975,#75976,#75977,#75978,#75979,#75980,#75981,#75982,#75983,#75984,
#75985,#75986,#75987,#75988,#75989,#75990,#75991,#75992,#75993,#75994,#75995,
#75996,#75997,#75998,#75999,#76000,#76001,#76002,#76003,#76004,#76005,#76006,
#76007,#76008,#76009,#76010,#76011,#76012,#76013,#76014,#76015,#76016,#76017,
#76018,#76019,#76020,#76021,#76022,#76023,#76024,#76025,#76026,#76027,#76028,
#76029,#76030));
#79324=CLOSED_SHELL('',(#76031,#76032,#76033,#76034,#76035,#76036,#76037,
#76038,#76039,#76040,#76041,#76042,#76043,#76044,#76045,#76046,#76047,#76048,
#76049,#76050,#76051,#76052,#76053,#76054,#76055,#76056,#76057,#76058,#76059,
#76060,#76061,#76062,#76063,#76064,#76065,#76066,#76067,#76068,#76069,#76070,
#76071,#76072,#76073,#76074,#76075,#76076,#76077,#76078,#76079,#76080,#76081,
#76082,#76083,#76084,#76085,#76086,#76087,#76088,#76089,#76090,#76091,#76092,
#76093,#76094,#76095,#76096,#76097));
#79325=CLOSED_SHELL('',(#76098,#76099,#76100,#76101,#76102,#76103,#76104,
#76105,#76106,#76107,#76108,#76109,#76110,#76111,#76112,#76113,#76114,#76115));
#79326=CLOSED_SHELL('',(#76116,#76117,#76118,#76119,#76120,#76121,#76122,
#76123,#76124,#76125,#76126,#76127,#76128,#76129,#76130,#76131,#76132,#76133,
#76134,#76135,#76136,#76137,#76138,#76139,#76140,#76141,#76142,#76143,#76144,
#76145,#76146,#76147,#76148,#76149,#76150,#76151,#76152));
#79327=CLOSED_SHELL('',(#76153,#76154,#76155,#76156,#76157,#76158,#76159,
#76160,#76161,#76162,#76163,#76164,#76165,#76166,#76167,#76168,#76169,#76170));
#79328=CLOSED_SHELL('',(#76171,#76172,#76173,#76174,#76175,#76176,#76177,
#76178,#76179,#76180,#76181,#76182,#76183));
#79329=CLOSED_SHELL('',(#76184,#76185,#76186,#76187,#76188,#76189,#76190,
#76191,#76192,#76193,#76194,#76195,#76196,#76197,#76198,#76199,#76200,#76201,
#76202,#76203,#76204,#76205,#76206,#76207,#76208,#76209,#76210,#76211,#76212,
#76213,#76214,#76215,#76216,#76217,#76218,#76219,#76220));
#79330=CLOSED_SHELL('',(#76221,#76222,#76223));
#79331=CLOSED_SHELL('',(#76224,#76225,#76226,#76227,#76228,#76229,#76230,
#76231,#76232,#76233,#76234,#76235,#76236,#76237,#76238,#76239,#76240,#76241,
#76242,#76243,#76244,#76245,#76246,#76247,#76248,#76249,#76250,#76251,#76252,
#76253,#76254,#76255,#76256,#76257,#76258,#76259,#76260,#76261,#76262,#76263,
#76264,#76265,#76266,#76267,#76268,#76269,#76270));
#79332=CLOSED_SHELL('',(#76271,#76272,#76273,#76274,#76275,#76276,#76277,
#76278,#76279,#76280,#76281,#76282,#76283));
#79333=CLOSED_SHELL('',(#76284,#76285,#76286,#76287,#76288,#76289,#76290,
#76291,#76292,#76293,#76294,#76295,#76296,#76297,#76298,#76299,#76300,#76301,
#76302,#76303,#76304,#76305,#76306,#76307,#76308,#76309,#76310,#76311,#76312,
#76313,#76314,#76315,#76316,#76317,#76318,#76319,#76320,#76321,#76322,#76323,
#76324,#76325,#76326,#76327,#76328,#76329,#76330,#76331,#76332,#76333,#76334,
#76335,#76336,#76337,#76338,#76339,#76340,#76341,#76342,#76343,#76344,#76345,
#76346,#76347,#76348,#76349,#76350,#76351,#76352,#76353,#76354,#76355,#76356,
#76357,#76358,#76359,#76360,#76361,#76362,#76363,#76364,#76365,#76366,#76367,
#76368,#76369,#76370,#76371,#76372,#76373,#76374,#76375,#76376,#76377,#76378,
#76379,#76380,#76381,#76382,#76383,#76384,#76385,#76386,#76387,#76388,#76389,
#76390,#76391,#76392,#76393,#76394,#76395,#76396,#76397,#76398,#76399,#76400,
#76401,#76402,#76403,#76404,#76405,#76406,#76407,#76408,#76409,#76410,#76411,
#76412,#76413,#76414,#76415,#76416,#76417,#76418,#76419,#76420,#76421,#76422,
#76423,#76424,#76425,#76426,#76427,#76428,#76429,#76430,#76431,#76432,#76433,
#76434,#76435,#76436,#76437,#76438,#76439,#76440,#76441,#76442,#76443,#76444,
#76445,#76446,#76447,#76448,#76449,#76450,#76451,#76452,#76453,#76454,#76455,
#76456,#76457,#76458,#76459,#76460,#76461,#76462,#76463,#76464,#76465,#76466,
#76467,#76468,#76469,#76470,#76471,#76472,#76473,#76474,#76475,#76476,#76477,
#76478,#76479,#76480,#76481,#76482,#76483,#76484,#76485,#76486,#76487,#76488,
#76489,#76490,#76491,#76492,#76493,#76494,#76495,#76496,#76497,#76498,#76499,
#76500,#76501,#76502,#76503,#76504,#76505,#76506,#76507,#76508,#76509,#76510,
#76511,#76512,#76513,#76514,#76515,#76516,#76517,#76518,#76519,#76520,#76521,
#76522,#76523,#76524,#76525,#76526,#76527,#76528,#76529,#76530,#76531,#76532,
#76533,#76534,#76535,#76536,#76537,#76538,#76539,#76540,#76541,#76542,#76543,
#76544,#76545,#76546,#76547,#76548,#76549,#76550,#76551,#76552,#76553,#76554,
#76555,#76556,#76557,#76558,#76559,#76560,#76561,#76562,#76563,#76564,#76565,
#76566,#76567,#76568,#76569,#76570,#76571,#76572,#76573,#76574,#76575,#76576,
#76577,#76578,#76579,#76580,#76581,#76582,#76583,#76584,#76585,#76586,#76587,
#76588,#76589,#76590,#76591,#76592,#76593,#76594,#76595,#76596,#76597,#76598,
#76599,#76600,#76601,#76602,#76603,#76604,#76605,#76606,#76607,#76608,#76609,
#76610,#76611,#76612,#76613,#76614,#76615,#76616,#76617,#76618,#76619,#76620,
#76621,#76622,#76623,#76624,#76625,#76626,#76627,#76628,#76629,#76630,#76631,
#76632,#76633,#76634,#76635,#76636,#76637,#76638,#76639,#76640,#76641,#76642,
#76643,#76644,#76645,#76646,#76647,#76648,#76649,#76650,#76651,#76652,#76653,
#76654,#76655,#76656,#76657,#76658,#76659,#76660,#76661,#76662,#76663,#76664,
#76665,#76666,#76667,#76668,#76669,#76670,#76671,#76672,#76673,#76674,#76675,
#76676,#76677,#76678,#76679,#76680,#76681,#76682,#76683,#76684,#76685,#76686,
#76687,#76688,#76689,#76690,#76691,#76692,#76693,#76694,#76695,#76696,#76697,
#76698,#76699,#76700,#76701,#76702,#76703,#76704,#76705,#76706,#76707,#76708,
#76709,#76710,#76711,#76712,#76713,#76714,#76715,#76716,#76717,#76718,#76719,
#76720,#76721,#76722,#76723,#76724,#76725,#76726,#76727,#76728,#76729,#76730,
#76731,#76732,#76733,#76734,#76735,#76736,#76737,#76738,#76739,#76740,#76741,
#76742,#76743,#76744,#76745,#76746,#76747,#76748,#76749,#76750,#76751,#76752,
#76753,#76754,#76755,#76756,#76757,#76758,#76759,#76760,#76761,#76762,#76763,
#76764,#76765,#76766,#76767,#76768,#76769,#76770,#76771,#76772,#76773,#76774,
#76775,#76776,#76777,#76778,#76779,#76780,#76781,#76782,#76783,#76784,#76785,
#76786,#76787,#76788,#76789,#76790,#76791,#76792,#76793,#76794,#76795,#76796,
#76797,#76798,#76799,#76800,#76801,#76802,#76803,#76804,#76805,#76806,#76807,
#76808,#76809,#76810,#76811,#76812,#76813,#76814,#76815,#76816,#76817,#76818,
#76819,#76820,#76821,#76822,#76823,#76824,#76825,#76826,#76827,#76828,#76829,
#76830,#76831,#76832,#76833,#76834,#76835,#76836,#76837,#76838,#76839,#76840,
#76841,#76842,#76843,#76844,#76845,#76846,#76847,#76848,#76849,#76850,#76851,
#76852,#76853,#76854,#76855,#76856,#76857,#76858,#76859,#76860,#76861,#76862,
#76863,#76864,#76865,#76866,#76867,#76868,#76869,#76870,#76871,#76872,#76873,
#76874,#76875,#76876,#76877,#76878,#76879,#76880,#76881,#76882,#76883,#76884,
#76885,#76886,#76887,#76888,#76889,#76890,#76891,#76892,#76893,#76894,#76895,
#76896,#76897,#76898,#76899,#76900,#76901,#76902,#76903,#76904,#76905,#76906,
#76907,#76908,#76909,#76910,#76911,#76912,#76913,#76914,#76915,#76916,#76917,
#76918,#76919,#76920,#76921,#76922,#76923,#76924,#76925,#76926,#76927,#76928,
#76929,#76930,#76931,#76932,#76933,#76934,#76935,#76936,#76937,#76938,#76939,
#76940,#76941,#76942,#76943,#76944,#76945,#76946,#76947,#76948,#76949,#76950,
#76951,#76952,#76953,#76954,#76955,#76956,#76957,#76958,#76959,#76960,#76961,
#76962,#76963,#76964,#76965,#76966,#76967,#76968,#76969,#76970,#76971,#76972,
#76973,#76974,#76975,#76976,#76977,#76978,#76979,#76980,#76981,#76982,#76983,
#76984,#76985,#76986,#76987,#76988,#76989,#76990,#76991,#76992,#76993,#76994,
#76995,#76996,#76997,#76998,#76999,#77000,#77001,#77002,#77003,#77004,#77005,
#77006,#77007,#77008,#77009,#77010,#77011,#77012,#77013,#77014,#77015,#77016,
#77017,#77018,#77019,#77020,#77021,#77022,#77023,#77024,#77025,#77026,#77027,
#77028,#77029,#77030,#77031,#77032,#77033,#77034,#77035,#77036,#77037,#77038,
#77039,#77040,#77041,#77042,#77043,#77044,#77045,#77046,#77047,#77048,#77049,
#77050,#77051,#77052,#77053,#77054,#77055,#77056,#77057,#77058,#77059,#77060,
#77061,#77062,#77063,#77064,#77065,#77066,#77067,#77068,#77069,#77070,#77071,
#77072,#77073,#77074,#77075,#77076,#77077,#77078,#77079,#77080,#77081,#77082,
#77083,#77084,#77085,#77086,#77087,#77088,#77089,#77090,#77091,#77092,#77093,
#77094,#77095,#77096,#77097,#77098,#77099,#77100,#77101,#77102,#77103,#77104,
#77105,#77106,#77107,#77108,#77109,#77110,#77111,#77112,#77113,#77114,#77115,
#77116,#77117,#77118,#77119,#77120,#77121,#77122,#77123,#77124,#77125,#77126,
#77127,#77128,#77129,#77130,#77131,#77132,#77133,#77134,#77135,#77136,#77137,
#77138,#77139,#77140,#77141,#77142,#77143,#77144,#77145,#77146,#77147,#77148,
#77149,#77150,#77151,#77152,#77153,#77154,#77155,#77156,#77157,#77158,#77159,
#77160,#77161,#77162,#77163,#77164,#77165,#77166,#77167,#77168,#77169,#77170,
#77171,#77172,#77173,#77174,#77175,#77176,#77177,#77178,#77179,#77180,#77181,
#77182,#77183,#77184,#77185,#77186,#77187,#77188,#77189,#77190,#77191,#77192,
#77193,#77194,#77195,#77196,#77197,#77198,#77199,#77200,#77201,#77202,#77203,
#77204,#77205,#77206,#77207,#77208,#77209,#77210,#77211,#77212,#77213,#77214,
#77215,#77216,#77217,#77218,#77219,#77220,#77221,#77222,#77223,#77224,#77225,
#77226,#77227,#77228,#77229,#77230,#77231,#77232,#77233,#77234,#77235,#77236,
#77237,#77238,#77239,#77240,#77241,#77242,#77243,#77244,#77245,#77246,#77247,
#77248,#77249,#77250,#77251,#77252,#77253,#77254,#77255,#77256,#77257,#77258,
#77259,#77260,#77261,#77262,#77263,#77264,#77265,#77266,#77267,#77268,#77269,
#77270,#77271,#77272,#77273,#77274,#77275,#77276,#77277,#77278,#77279,#77280,
#77281,#77282,#77283,#77284,#77285,#77286,#77287,#77288,#77289,#77290,#77291,
#77292,#77293,#77294,#77295,#77296,#77297,#77298,#77299,#77300,#77301,#77302,
#77303,#77304,#77305,#77306,#77307,#77308,#77309,#77310,#77311,#77312,#77313,
#77314,#77315,#77316,#77317,#77318,#77319,#77320,#77321,#77322,#77323,#77324,
#77325,#77326,#77327,#77328,#77329,#77330,#77331,#77332,#77333,#77334,#77335,
#77336,#77337,#77338,#77339,#77340,#77341,#77342,#77343,#77344,#77345,#77346,
#77347,#77348,#77349,#77350,#77351,#77352,#77353,#77354,#77355,#77356,#77357,
#77358,#77359,#77360,#77361,#77362,#77363,#77364,#77365,#77366,#77367,#77368,
#77369,#77370,#77371,#77372,#77373,#77374,#77375,#77376,#77377,#77378,#77379,
#77380,#77381,#77382,#77383,#77384,#77385,#77386,#77387,#77388,#77389,#77390,
#77391,#77392,#77393,#77394,#77395,#77396,#77397,#77398,#77399,#77400,#77401,
#77402,#77403,#77404,#77405,#77406,#77407,#77408,#77409,#77410,#77411,#77412,
#77413,#77414,#77415,#77416,#77417,#77418,#77419,#77420,#77421,#77422,#77423,
#77424,#77425,#77426,#77427,#77428,#77429,#77430,#77431,#77432,#77433,#77434,
#77435,#77436,#77437,#77438,#77439,#77440,#77441,#77442,#77443,#77444,#77445,
#77446,#77447,#77448,#77449,#77450,#77451,#77452,#77453,#77454,#77455,#77456,
#77457,#77458,#77459,#77460,#77461,#77462,#77463,#77464,#77465,#77466,#77467,
#77468,#77469,#77470,#77471,#77472,#77473,#77474,#77475,#77476,#77477,#77478,
#77479,#77480,#77481,#77482,#77483,#77484,#77485,#77486,#77487,#77488,#77489,
#77490,#77491,#77492,#77493,#77494,#77495,#77496,#77497,#77498,#77499,#77500,
#77501,#77502,#77503,#77504,#77505,#77506,#77507,#77508,#77509,#77510,#77511,
#77512,#77513,#77514,#77515,#77516,#77517,#77518,#77519,#77520,#77521,#77522,
#77523,#77524,#77525,#77526,#77527,#77528,#77529,#77530,#77531,#77532,#77533,
#77534,#77535,#77536,#77537,#77538,#77539,#77540,#77541,#77542,#77543,#77544,
#77545,#77546,#77547,#77548,#77549,#77550,#77551,#77552,#77553,#77554,#77555,
#77556,#77557,#77558,#77559,#77560,#77561,#77562,#77563,#77564,#77565,#77566,
#77567,#77568,#77569,#77570,#77571,#77572,#77573,#77574,#77575,#77576,#77577,
#77578,#77579,#77580,#77581,#77582,#77583,#77584,#77585,#77586,#77587,#77588,
#77589,#77590,#77591,#77592,#77593,#77594,#77595,#77596,#77597,#77598,#77599,
#77600,#77601,#77602,#77603,#77604,#77605,#77606,#77607,#77608,#77609,#77610,
#77611,#77612,#77613,#77614,#77615,#77616,#77617,#77618,#77619,#77620,#77621,
#77622,#77623,#77624,#77625,#77626,#77627,#77628,#77629,#77630,#77631,#77632,
#77633,#77634,#77635,#77636,#77637,#77638,#77639,#77640,#77641,#77642,#77643,
#77644,#77645,#77646,#77647,#77648,#77649,#77650,#77651,#77652,#77653,#77654,
#77655,#77656,#77657,#77658,#77659,#77660,#77661,#77662,#77663,#77664,#77665,
#77666,#77667,#77668,#77669,#77670,#77671,#77672,#77673,#77674,#77675,#77676,
#77677,#77678,#77679,#77680,#77681,#77682,#77683,#77684,#77685,#77686,#77687,
#77688,#77689,#77690,#77691,#77692,#77693,#77694,#77695,#77696,#77697,#77698,
#77699,#77700,#77701,#77702,#77703,#77704,#77705,#77706,#77707,#77708,#77709,
#77710,#77711,#77712,#77713,#77714,#77715,#77716,#77717,#77718,#77719,#77720,
#77721,#77722,#77723,#77724,#77725,#77726,#77727,#77728,#77729,#77730,#77731,
#77732,#77733,#77734,#77735,#77736,#77737,#77738,#77739,#77740,#77741,#77742,
#77743,#77744,#77745,#77746,#77747,#77748,#77749,#77750,#77751,#77752,#77753,
#77754,#77755,#77756,#77757,#77758,#77759,#77760,#77761,#77762,#77763,#77764,
#77765,#77766,#77767,#77768,#77769,#77770,#77771,#77772,#77773,#77774,#77775,
#77776,#77777,#77778,#77779,#77780,#77781,#77782,#77783,#77784,#77785,#77786,
#77787,#77788,#77789,#77790,#77791,#77792,#77793,#77794,#77795,#77796,#77797,
#77798,#77799,#77800,#77801,#77802,#77803,#77804,#77805,#77806,#77807,#77808,
#77809,#77810,#77811,#77812,#77813,#77814,#77815,#77816,#77817,#77818,#77819,
#77820,#77821,#77822,#77823,#77824,#77825,#77826,#77827,#77828,#77829,#77830,
#77831,#77832,#77833,#77834,#77835,#77836,#77837,#77838,#77839,#77840,#77841,
#77842,#77843,#77844,#77845,#77846,#77847,#77848,#77849,#77850,#77851,#77852,
#77853,#77854,#77855,#77856,#77857,#77858,#77859,#77860,#77861,#77862,#77863,
#77864,#77865,#77866,#77867,#77868,#77869,#77870,#77871,#77872,#77873,#77874,
#77875,#77876,#77877,#77878,#77879,#77880,#77881,#77882,#77883,#77884,#77885,
#77886,#77887,#77888,#77889,#77890,#77891,#77892,#77893,#77894,#77895,#77896,
#77897,#77898,#77899,#77900,#77901,#77902,#77903,#77904,#77905,#77906,#77907,
#77908,#77909,#77910,#77911,#77912,#77913,#77914,#77915,#77916,#77917,#77918,
#77919,#77920,#77921,#77922,#77923,#77924,#77925,#77926,#77927,#77928,#77929,
#77930,#77931,#77932,#77933,#77934,#77935,#77936,#77937,#77938,#77939,#77940,
#77941,#77942,#77943,#77944,#77945,#77946,#77947,#77948,#77949,#77950,#77951,
#77952,#77953,#77954,#77955,#77956,#77957,#77958,#77959,#77960,#77961,#77962,
#77963,#77964,#77965,#77966,#77967,#77968,#77969,#77970,#77971,#77972,#77973,
#77974,#77975,#77976,#77977,#77978,#77979,#77980,#77981,#77982,#77983,#77984,
#77985,#77986,#77987,#77988,#77989,#77990,#77991,#77992,#77993,#77994,#77995,
#77996,#77997,#77998,#77999,#78000,#78001,#78002,#78003,#78004,#78005,#78006,
#78007,#78008,#78009,#78010,#78011,#78012,#78013,#78014,#78015,#78016,#78017,
#78018,#78019,#78020,#78021,#78022,#78023,#78024,#78025,#78026,#78027,#78028,
#78029,#78030,#78031,#78032,#78033,#78034,#78035,#78036,#78037,#78038,#78039,
#78040,#78041,#78042,#78043,#78044,#78045,#78046,#78047,#78048,#78049,#78050,
#78051,#78052,#78053,#78054,#78055,#78056,#78057,#78058,#78059,#78060,#78061,
#78062,#78063,#78064,#78065,#78066,#78067,#78068,#78069,#78070,#78071,#78072,
#78073,#78074,#78075,#78076,#78077,#78078,#78079,#78080,#78081,#78082,#78083,
#78084,#78085,#78086,#78087,#78088,#78089,#78090,#78091,#78092,#78093,#78094,
#78095,#78096,#78097,#78098,#78099,#78100,#78101,#78102,#78103,#78104,#78105,
#78106,#78107,#78108,#78109,#78110,#78111,#78112,#78113,#78114,#78115,#78116,
#78117,#78118,#78119,#78120,#78121,#78122,#78123,#78124,#78125,#78126,#78127,
#78128,#78129,#78130,#78131,#78132,#78133,#78134,#78135,#78136,#78137,#78138,
#78139,#78140,#78141,#78142,#78143,#78144,#78145,#78146,#78147,#78148,#78149,
#78150,#78151,#78152,#78153,#78154,#78155,#78156,#78157,#78158,#78159,#78160,
#78161,#78162,#78163,#78164,#78165,#78166,#78167,#78168,#78169,#78170,#78171,
#78172,#78173,#78174,#78175,#78176,#78177,#78178,#78179,#78180,#78181,#78182,
#78183,#78184,#78185,#78186,#78187,#78188,#78189,#78190,#78191,#78192,#78193,
#78194,#78195,#78196,#78197,#78198,#78199,#78200,#78201,#78202,#78203,#78204,
#78205,#78206,#78207,#78208,#78209,#78210,#78211,#78212,#78213,#78214,#78215,
#78216,#78217,#78218,#78219,#78220,#78221,#78222,#78223,#78224,#78225,#78226,
#78227,#78228,#78229,#78230,#78231,#78232,#78233,#78234,#78235,#78236,#78237,
#78238,#78239,#78240,#78241,#78242,#78243,#78244,#78245,#78246,#78247,#78248,
#78249,#78250,#78251,#78252,#78253,#78254,#78255,#78256,#78257,#78258,#78259,
#78260,#78261,#78262,#78263,#78264,#78265,#78266,#78267,#78268,#78269,#78270,
#78271,#78272,#78273,#78274,#78275,#78276,#78277,#78278,#78279,#78280,#78281,
#78282,#78283,#78284,#78285,#78286,#78287,#78288,#78289,#78290,#78291,#78292,
#78293,#78294,#78295,#78296,#78297,#78298,#78299,#78300,#78301,#78302,#78303,
#78304,#78305,#78306,#78307,#78308,#78309,#78310,#78311,#78312,#78313,#78314,
#78315,#78316,#78317,#78318,#78319,#78320,#78321,#78322,#78323,#78324,#78325,
#78326,#78327,#78328,#78329,#78330,#78331,#78332,#78333,#78334,#78335,#78336,
#78337,#78338,#78339,#78340,#78341,#78342,#78343,#78344,#78345,#78346,#78347,
#78348,#78349,#78350,#78351,#78352,#78353,#78354,#78355,#78356,#78357,#78358,
#78359,#78360,#78361,#78362,#78363,#78364,#78365,#78366,#78367,#78368,#78369,
#78370,#78371,#78372,#78373,#78374,#78375,#78376,#78377,#78378,#78379,#78380,
#78381,#78382,#78383,#78384,#78385,#78386,#78387,#78388,#78389,#78390,#78391,
#78392,#78393,#78394,#78395,#78396,#78397,#78398,#78399,#78400,#78401,#78402,
#78403,#78404,#78405,#78406,#78407,#78408,#78409,#78410,#78411,#78412,#78413,
#78414,#78415,#78416,#78417,#78418,#78419,#78420,#78421,#78422,#78423,#78424,
#78425,#78426,#78427,#78428,#78429,#78430,#78431,#78432,#78433,#78434,#78435,
#78436,#78437,#78438,#78439,#78440,#78441,#78442,#78443,#78444,#78445,#78446,
#78447,#78448,#78449,#78450,#78451,#78452,#78453,#78454,#78455,#78456,#78457,
#78458,#78459,#78460,#78461,#78462,#78463,#78464,#78465,#78466,#78467,#78468,
#78469,#78470,#78471,#78472,#78473,#78474,#78475,#78476,#78477,#78478,#78479,
#78480,#78481,#78482,#78483,#78484,#78485,#78486,#78487,#78488,#78489,#78490,
#78491,#78492,#78493,#78494,#78495,#78496,#78497,#78498,#78499,#78500,#78501,
#78502,#78503,#78504,#78505,#78506,#78507,#78508,#78509,#78510,#78511,#78512,
#78513,#78514,#78515,#78516,#78517,#78518,#78519,#78520,#78521,#78522,#78523,
#78524,#78525,#78526,#78527,#78528,#78529,#78530,#78531,#78532,#78533,#78534,
#78535,#78536,#78537,#78538,#78539,#78540,#78541,#78542,#78543,#78544,#78545,
#78546,#78547,#78548,#78549,#78550,#78551,#78552,#78553,#78554,#78555,#78556,
#78557,#78558,#78559,#78560,#78561,#78562,#78563,#78564,#78565,#78566,#78567,
#78568,#78569,#78570,#78571,#78572,#78573,#78574,#78575,#78576,#78577,#78578,
#78579,#78580,#78581,#78582,#78583,#78584,#78585,#78586,#78587,#78588,#78589,
#78590,#78591,#78592,#78593,#78594,#78595,#78596,#78597,#78598,#78599,#78600,
#78601,#78602,#78603,#78604,#78605,#78606,#78607,#78608,#78609,#78610,#78611,
#78612,#78613,#78614,#78615,#78616,#78617,#78618,#78619,#78620,#78621,#78622,
#78623,#78624,#78625,#78626,#78627,#78628,#78629,#78630,#78631,#78632,#78633,
#78634,#78635,#78636,#78637,#78638,#78639,#78640,#78641,#78642,#78643,#78644,
#78645,#78646,#78647,#78648,#78649,#78650,#78651,#78652,#78653,#78654,#78655,
#78656,#78657,#78658,#78659,#78660,#78661,#78662,#78663,#78664,#78665,#78666,
#78667,#78668,#78669,#78670,#78671,#78672,#78673,#78674,#78675,#78676,#78677,
#78678,#78679,#78680,#78681,#78682,#78683,#78684,#78685,#78686,#78687,#78688,
#78689,#78690,#78691,#78692,#78693,#78694,#78695,#78696,#78697,#78698,#78699,
#78700,#78701,#78702,#78703,#78704,#78705,#78706,#78707,#78708,#78709,#78710,
#78711,#78712,#78713,#78714,#78715,#78716,#78717,#78718,#78719,#78720,#78721,
#78722,#78723,#78724,#78725,#78726,#78727,#78728,#78729,#78730,#78731,#78732,
#78733,#78734,#78735,#78736,#78737,#78738,#78739,#78740,#78741,#78742,#78743,
#78744,#78745,#78746,#78747,#78748,#78749,#78750,#78751,#78752,#78753,#78754,
#78755,#78756,#78757,#78758,#78759,#78760,#78761,#78762,#78763,#78764,#78765,
#78766,#78767,#78768,#78769,#78770,#78771,#78772,#78773,#78774,#78775,#78776,
#78777,#78778,#78779,#78780,#78781,#78782,#78783,#78784,#78785,#78786,#78787,
#78788,#78789,#78790,#78791,#78792,#78793,#78794,#78795,#78796,#78797,#78798,
#78799,#78800,#78801,#78802,#78803,#78804,#78805,#78806,#78807,#78808,#78809,
#78810,#78811,#78812,#78813,#78814,#78815,#78816,#78817,#78818,#78819,#78820,
#78821,#78822,#78823,#78824,#78825,#78826,#78827,#78828,#78829,#78830,#78831,
#78832,#78833,#78834,#78835,#78836,#78837,#78838,#78839,#78840,#78841,#78842,
#78843,#78844,#78845,#78846,#78847,#78848,#78849,#78850,#78851,#78852,#78853,
#78854,#78855,#78856,#78857,#78858,#78859,#78860,#78861,#78862,#78863,#78864,
#78865,#78866,#78867,#78868,#78869,#78870,#78871,#78872,#78873,#78874,#78875,
#78876,#78877,#78878,#78879,#78880,#78881,#78882,#78883,#78884,#78885,#78886,
#78887,#78888,#78889,#78890,#78891,#78892,#78893,#78894,#78895,#78896,#78897,
#78898,#78899,#78900,#78901,#78902,#78903,#78904,#78905,#78906,#78907,#78908,
#78909,#78910,#78911,#78912,#78913,#78914,#78915,#78916,#78917,#78918,#78919,
#78920,#78921,#78922,#78923,#78924,#78925,#78926,#78927,#78928,#78929,#78930,
#78931,#78932,#78933,#78934,#78935,#78936,#78937,#78938,#78939,#78940,#78941,
#78942,#78943,#78944,#78945,#78946,#78947,#78948,#78949,#78950,#78951,#78952,
#78953,#78954,#78955,#78956,#78957,#78958,#78959,#78960,#78961,#78962,#78963,
#78964,#78965,#78966,#78967,#78968,#78969,#78970,#78971,#78972,#78973,#78974,
#78975,#78976,#78977,#78978,#78979,#78980,#78981,#78982,#78983,#78984,#78985,
#78986,#78987,#78988,#78989,#78990,#78991,#78992,#78993,#78994,#78995,#78996,
#78997,#78998,#78999,#79000,#79001,#79002,#79003,#79004,#79005,#79006,#79007,
#79008,#79009,#79010,#79011,#79012,#79013,#79014,#79015,#79016,#79017,#79018,
#79019,#79020,#79021,#79022,#79023,#79024,#79025,#79026,#79027,#79028,#79029,
#79030,#79031,#79032,#79033,#79034,#79035,#79036,#79037,#79038,#79039,#79040,
#79041,#79042,#79043,#79044,#79045,#79046,#79047,#79048,#79049,#79050,#79051,
#79052,#79053,#79054,#79055,#79056,#79057,#79058,#79059,#79060,#79061,#79062,
#79063,#79064,#79065,#79066,#79067,#79068,#79069,#79070,#79071,#79072,#79073,
#79074,#79075,#79076,#79077,#79078,#79079,#79080,#79081,#79082,#79083,#79084,
#79085,#79086,#79087,#79088,#79089,#79090,#79091,#79092,#79093,#79094,#79095,
#79096,#79097,#79098,#79099,#79100,#79101,#79102,#79103,#79104,#79105,#79106,
#79107,#79108,#79109,#79110,#79111,#79112,#79113,#79114,#79115,#79116,#79117,
#79118,#79119,#79120,#79121,#79122,#79123,#79124,#79125,#79126,#79127,#79128,
#79129,#79130,#79131,#79132,#79133,#79134,#79135,#79136,#79137,#79138,#79139,
#79140,#79141,#79142,#79143,#79144,#79145,#79146,#79147,#79148,#79149,#79150,
#79151,#79152,#79153,#79154,#79155,#79156,#79157));
#79334=CLOSED_SHELL('',(#79158,#79159,#79160,#79161,#79162,#79163,#79164,
#79165,#79166,#79167,#79168,#79169,#79170,#79171,#79172,#79173,#79174,#79175,
#79176,#79177,#79178,#79179,#79180,#79181,#79182,#79183,#79184,#79185,#79186,
#79187,#79188,#79189,#79190,#79191,#79192,#79193,#79194,#79195,#79196,#79197,
#79198,#79199,#79200,#79201,#79202,#79203,#79204,#79205,#79206,#79207,#79208,
#79209,#79210,#79211,#79212,#79213,#79214,#79215,#79216,#79217,#79218,#79219,
#79220,#79221,#79222,#79223,#79224,#79225,#79226,#79227,#79228,#79229,#79230,
#79231,#79232,#79233,#79234,#79235,#79236,#79237));
#79335=CLOSED_SHELL('',(#79238,#79239,#79240,#79241,#79242,#79243,#79244,
#79245,#79246,#79247,#79248,#79249,#79250,#79251,#79252,#79253,#79254,#79255,
#79256,#79257,#79258,#79259,#79260,#79261,#79262,#79263,#79264,#79265,#79266,
#79267,#79268,#79269,#79270,#79271,#79272,#79273,#79274,#79275,#79276,#79277,
#79278,#79279,#79280,#79281,#79282,#79283,#79284,#79285,#79286,#79287,#79288,
#79289,#79290,#79291,#79292,#79293,#79294,#79295,#79296,#79297,#79298,#79299,
#79300,#79301,#79302,#79303,#79304,#79305,#79306,#79307,#79308,#79309,#79310,
#79311,#79312,#79313,#79314,#79315,#79316,#79317));
#79336=BREP_WITH_VOIDS('Body1',#79322,(#1975,#1976,#1977,#1978));
#79337=BREP_WITH_VOIDS('Body1',#79331,(#1979));
#79338=DERIVED_UNIT_ELEMENT(#79364,1.);
#79339=DERIVED_UNIT_ELEMENT(#221664,-3.);
#79340=DERIVED_UNIT_ELEMENT(#79364,1.);
#79341=DERIVED_UNIT_ELEMENT(#221664,-3.);
#79342=DERIVED_UNIT_ELEMENT(#79364,1.);
#79343=DERIVED_UNIT_ELEMENT(#221664,-3.);
#79344=DERIVED_UNIT_ELEMENT(#79364,1.);
#79345=DERIVED_UNIT_ELEMENT(#221664,-3.);
#79346=DERIVED_UNIT_ELEMENT(#79364,1.);
#79347=DERIVED_UNIT_ELEMENT(#221664,-3.);
#79348=DERIVED_UNIT_ELEMENT(#79364,1.);
#79349=DERIVED_UNIT_ELEMENT(#221664,-3.);
#79350=DERIVED_UNIT_ELEMENT(#79364,1.);
#79351=DERIVED_UNIT_ELEMENT(#221664,-3.);
#79352=DERIVED_UNIT_ELEMENT(#79364,1.);
#79353=DERIVED_UNIT_ELEMENT(#221664,-3.);
#79354=DERIVED_UNIT_ELEMENT(#79364,1.);
#79355=DERIVED_UNIT_ELEMENT(#221664,-3.);
#79356=DERIVED_UNIT_ELEMENT(#79364,1.);
#79357=DERIVED_UNIT_ELEMENT(#221664,-3.);
#79358=DERIVED_UNIT_ELEMENT(#79364,1.);
#79359=DERIVED_UNIT_ELEMENT(#221664,-3.);
#79360=DERIVED_UNIT_ELEMENT(#79364,1.);
#79361=DERIVED_UNIT_ELEMENT(#221664,-3.);
#79362=DERIVED_UNIT_ELEMENT(#79364,1.);
#79363=DERIVED_UNIT_ELEMENT(#221664,-3.);
#79364=(
MASS_UNIT()
NAMED_UNIT(*)
SI_UNIT(.KILO.,.GRAM.)
);
#79365=DERIVED_UNIT((#79338,#79339));
#79366=DERIVED_UNIT((#79340,#79341));
#79367=DERIVED_UNIT((#79342,#79343));
#79368=DERIVED_UNIT((#79344,#79345));
#79369=DERIVED_UNIT((#79346,#79347));
#79370=DERIVED_UNIT((#79348,#79349));
#79371=DERIVED_UNIT((#79350,#79351));
#79372=DERIVED_UNIT((#79352,#79353));
#79373=DERIVED_UNIT((#79354,#79355));
#79374=DERIVED_UNIT((#79356,#79357));
#79375=DERIVED_UNIT((#79358,#79359));
#79376=DERIVED_UNIT((#79360,#79361));
#79377=DERIVED_UNIT((#79362,#79363));
#79378=MEASURE_REPRESENTATION_ITEM('density measure',
POSITIVE_RATIO_MEASURE(7850.),#79365);
#79379=MEASURE_REPRESENTATION_ITEM('density measure',
POSITIVE_RATIO_MEASURE(7850.),#79366);
#79380=MEASURE_REPRESENTATION_ITEM('density measure',
POSITIVE_RATIO_MEASURE(7850.),#79367);
#79381=MEASURE_REPRESENTATION_ITEM('density measure',
POSITIVE_RATIO_MEASURE(7850.),#79368);
#79382=MEASURE_REPRESENTATION_ITEM('density measure',
POSITIVE_RATIO_MEASURE(7850.),#79369);
#79383=MEASURE_REPRESENTATION_ITEM('density measure',
POSITIVE_RATIO_MEASURE(7850.),#79370);
#79384=MEASURE_REPRESENTATION_ITEM('density measure',
POSITIVE_RATIO_MEASURE(7850.),#79371);
#79385=MEASURE_REPRESENTATION_ITEM('density measure',
POSITIVE_RATIO_MEASURE(7850.),#79372);
#79386=MEASURE_REPRESENTATION_ITEM('density measure',
POSITIVE_RATIO_MEASURE(7850.),#79373);
#79387=MEASURE_REPRESENTATION_ITEM('density measure',
POSITIVE_RATIO_MEASURE(7850.),#79374);
#79388=MEASURE_REPRESENTATION_ITEM('density measure',
POSITIVE_RATIO_MEASURE(7850.),#79375);
#79389=MEASURE_REPRESENTATION_ITEM('density measure',
POSITIVE_RATIO_MEASURE(7850.),#79376);
#79390=MEASURE_REPRESENTATION_ITEM('density measure',
POSITIVE_RATIO_MEASURE(7850.),#79377);
#79391=PROPERTY_DEFINITION_REPRESENTATION(#79456,#79417);
#79392=PROPERTY_DEFINITION_REPRESENTATION(#79457,#79418);
#79393=PROPERTY_DEFINITION_REPRESENTATION(#79458,#79419);
#79394=PROPERTY_DEFINITION_REPRESENTATION(#79459,#79420);
#79395=PROPERTY_DEFINITION_REPRESENTATION(#79460,#79421);
#79396=PROPERTY_DEFINITION_REPRESENTATION(#79461,#79422);
#79397=PROPERTY_DEFINITION_REPRESENTATION(#79462,#79423);
#79398=PROPERTY_DEFINITION_REPRESENTATION(#79463,#79424);
#79399=PROPERTY_DEFINITION_REPRESENTATION(#79464,#79425);
#79400=PROPERTY_DEFINITION_REPRESENTATION(#79465,#79426);
#79401=PROPERTY_DEFINITION_REPRESENTATION(#79466,#79427);
#79402=PROPERTY_DEFINITION_REPRESENTATION(#79467,#79428);
#79403=PROPERTY_DEFINITION_REPRESENTATION(#79468,#79429);
#79404=PROPERTY_DEFINITION_REPRESENTATION(#79469,#79430);
#79405=PROPERTY_DEFINITION_REPRESENTATION(#79470,#79431);
#79406=PROPERTY_DEFINITION_REPRESENTATION(#79471,#79432);
#79407=PROPERTY_DEFINITION_REPRESENTATION(#79472,#79433);
#79408=PROPERTY_DEFINITION_REPRESENTATION(#79473,#79434);
#79409=PROPERTY_DEFINITION_REPRESENTATION(#79474,#79435);
#79410=PROPERTY_DEFINITION_REPRESENTATION(#79475,#79436);
#79411=PROPERTY_DEFINITION_REPRESENTATION(#79476,#79437);
#79412=PROPERTY_DEFINITION_REPRESENTATION(#79477,#79438);
#79413=PROPERTY_DEFINITION_REPRESENTATION(#79478,#79439);
#79414=PROPERTY_DEFINITION_REPRESENTATION(#79479,#79440);
#79415=PROPERTY_DEFINITION_REPRESENTATION(#79480,#79441);
#79416=PROPERTY_DEFINITION_REPRESENTATION(#79481,#79442);
#79417=REPRESENTATION('material name',(#79443),#221649);
#79418=REPRESENTATION('density',(#79378),#221649);
#79419=REPRESENTATION('material name',(#79444),#221650);
#79420=REPRESENTATION('density',(#79379),#221650);
#79421=REPRESENTATION('material name',(#79445),#221651);
#79422=REPRESENTATION('density',(#79380),#221651);
#79423=REPRESENTATION('material name',(#79446),#221652);
#79424=REPRESENTATION('density',(#79381),#221652);
#79425=REPRESENTATION('material name',(#79447),#221653);
#79426=REPRESENTATION('density',(#79382),#221653);
#79427=REPRESENTATION('material name',(#79448),#221654);
#79428=REPRESENTATION('density',(#79383),#221654);
#79429=REPRESENTATION('material name',(#79449),#221655);
#79430=REPRESENTATION('density',(#79384),#221655);
#79431=REPRESENTATION('material name',(#79450),#221656);
#79432=REPRESENTATION('density',(#79385),#221656);
#79433=REPRESENTATION('material name',(#79451),#221657);
#79434=REPRESENTATION('density',(#79386),#221657);
#79435=REPRESENTATION('material name',(#79452),#221658);
#79436=REPRESENTATION('density',(#79387),#221658);
#79437=REPRESENTATION('material name',(#79453),#221659);
#79438=REPRESENTATION('density',(#79388),#221659);
#79439=REPRESENTATION('material name',(#79454),#221660);
#79440=REPRESENTATION('density',(#79389),#221660);
#79441=REPRESENTATION('material name',(#79455),#221661);
#79442=REPRESENTATION('density',(#79390),#221661);
#79443=DESCRIPTIVE_REPRESENTATION_ITEM('Steel','Steel');
#79444=DESCRIPTIVE_REPRESENTATION_ITEM('Steel','Steel');
#79445=DESCRIPTIVE_REPRESENTATION_ITEM('Steel','Steel');
#79446=DESCRIPTIVE_REPRESENTATION_ITEM('Steel','Steel');
#79447=DESCRIPTIVE_REPRESENTATION_ITEM('Steel','Steel');
#79448=DESCRIPTIVE_REPRESENTATION_ITEM('Steel','Steel');
#79449=DESCRIPTIVE_REPRESENTATION_ITEM('Steel','Steel');
#79450=DESCRIPTIVE_REPRESENTATION_ITEM('Steel','Steel');
#79451=DESCRIPTIVE_REPRESENTATION_ITEM('Steel','Steel');
#79452=DESCRIPTIVE_REPRESENTATION_ITEM('Steel','Steel');
#79453=DESCRIPTIVE_REPRESENTATION_ITEM('Steel','Steel');
#79454=DESCRIPTIVE_REPRESENTATION_ITEM('Steel','Steel');
#79455=DESCRIPTIVE_REPRESENTATION_ITEM('Steel','Steel');
#79456=PROPERTY_DEFINITION('material property','material name',#221724);
#79457=PROPERTY_DEFINITION('material property','density of part',#221724);
#79458=PROPERTY_DEFINITION('material property','material name',#221725);
#79459=PROPERTY_DEFINITION('material property','density of part',#221725);
#79460=PROPERTY_DEFINITION('material property','material name',#221726);
#79461=PROPERTY_DEFINITION('material property','density of part',#221726);
#79462=PROPERTY_DEFINITION('material property','material name',#221727);
#79463=PROPERTY_DEFINITION('material property','density of part',#221727);
#79464=PROPERTY_DEFINITION('material property','material name',#221728);
#79465=PROPERTY_DEFINITION('material property','density of part',#221728);
#79466=PROPERTY_DEFINITION('material property','material name',#221729);
#79467=PROPERTY_DEFINITION('material property','density of part',#221729);
#79468=PROPERTY_DEFINITION('material property','material name',#221730);
#79469=PROPERTY_DEFINITION('material property','density of part',#221730);
#79470=PROPERTY_DEFINITION('material property','material name',#221731);
#79471=PROPERTY_DEFINITION('material property','density of part',#221731);
#79472=PROPERTY_DEFINITION('material property','material name',#221732);
#79473=PROPERTY_DEFINITION('material property','density of part',#221732);
#79474=PROPERTY_DEFINITION('material property','material name',#221733);
#79475=PROPERTY_DEFINITION('material property','density of part',#221733);
#79476=PROPERTY_DEFINITION('material property','material name',#221734);
#79477=PROPERTY_DEFINITION('material property','density of part',#221734);
#79478=PROPERTY_DEFINITION('material property','material name',#221735);
#79479=PROPERTY_DEFINITION('material property','density of part',#221735);
#79480=PROPERTY_DEFINITION('material property','material name',#221736);
#79481=PROPERTY_DEFINITION('material property','density of part',#221736);
#79482=AXIS2_PLACEMENT_3D('',#106595,#86164,#86165);
#79483=AXIS2_PLACEMENT_3D('',#106596,#86166,#86167);
#79484=AXIS2_PLACEMENT_3D('',#106597,#86168,#86169);
#79485=AXIS2_PLACEMENT_3D('',#106600,#86170,#86171);
#79486=AXIS2_PLACEMENT_3D('',#106602,#86172,#86173);
#79487=AXIS2_PLACEMENT_3D('',#106604,#86174,#86175);
#79488=AXIS2_PLACEMENT_3D('',#106611,#86176,#86177);
#79489=AXIS2_PLACEMENT_3D('',#106616,#86180,#86181);
#79490=AXIS2_PLACEMENT_3D('',#106865,#86182,#86183);
#79491=AXIS2_PLACEMENT_3D('',#106876,#86184,#86185);
#79492=AXIS2_PLACEMENT_3D('',#106877,#86186,#86187);
#79493=AXIS2_PLACEMENT_3D('',#106880,#86188,#86189);
#79494=AXIS2_PLACEMENT_3D('',#106882,#86190,#86191);
#79495=AXIS2_PLACEMENT_3D('',#106884,#86192,#86193);
#79496=AXIS2_PLACEMENT_3D('',#106946,#86194,#86195);
#79497=AXIS2_PLACEMENT_3D('',#106948,#86196,#86197);
#79498=AXIS2_PLACEMENT_3D('',#107141,#86200,#86201);
#79499=AXIS2_PLACEMENT_3D('',#107152,#86202,#86203);
#79500=AXIS2_PLACEMENT_3D('',#107153,#86204,#86205);
#79501=AXIS2_PLACEMENT_3D('',#107192,#86206,#86207);
#79502=AXIS2_PLACEMENT_3D('',#107576,#86209,#86210);
#79503=AXIS2_PLACEMENT_3D('',#107757,#86211,#86212);
#79504=AXIS2_PLACEMENT_3D('',#107760,#86215,#86216);
#79505=AXIS2_PLACEMENT_3D('',#107983,#86217,#86218);
#79506=AXIS2_PLACEMENT_3D('',#108205,#86219,#86220);
#79507=AXIS2_PLACEMENT_3D('',#108206,#86221,#86222);
#79508=AXIS2_PLACEMENT_3D('',#108209,#86223,#86224);
#79509=AXIS2_PLACEMENT_3D('',#108280,#86226,#86227);
#79510=AXIS2_PLACEMENT_3D('',#108283,#86228,#86229);
#79511=AXIS2_PLACEMENT_3D('',#108824,#86230,#86231);
#79512=AXIS2_PLACEMENT_3D('',#108826,#86233,#86234);
#79513=AXIS2_PLACEMENT_3D('',#108896,#86236,#86237);
#79514=AXIS2_PLACEMENT_3D('',#109121,#86238,#86239);
#79515=AXIS2_PLACEMENT_3D('',#109122,#86240,#86241);
#79516=AXIS2_PLACEMENT_3D('',#109172,#86243,#86244);
#79517=AXIS2_PLACEMENT_3D('',#109197,#86245,#86246);
#79518=AXIS2_PLACEMENT_3D('',#109323,#86248,#86249);
#79519=AXIS2_PLACEMENT_3D('',#109438,#86251,#86252);
#79520=AXIS2_PLACEMENT_3D('',#109456,#86254,#86255);
#79521=AXIS2_PLACEMENT_3D('',#109488,#86256,#86257);
#79522=AXIS2_PLACEMENT_3D('',#109601,#86259,#86260);
#79523=AXIS2_PLACEMENT_3D('',#109631,#86262,#86263);
#79524=AXIS2_PLACEMENT_3D('',#109678,#86264,#86265);
#79525=AXIS2_PLACEMENT_3D('',#109765,#86268,#86269);
#79526=AXIS2_PLACEMENT_3D('',#109993,#86271,#86272);
#79527=AXIS2_PLACEMENT_3D('',#110219,#86274,#86275);
#79528=AXIS2_PLACEMENT_3D('',#110451,#86277,#86278);
#79529=AXIS2_PLACEMENT_3D('',#110456,#86280,#86281);
#79530=AXIS2_PLACEMENT_3D('',#110483,#86282,#86283);
#79531=AXIS2_PLACEMENT_3D('',#110650,#86287,#86288);
#79532=AXIS2_PLACEMENT_3D('',#110651,#86289,#86290);
#79533=AXIS2_PLACEMENT_3D('',#110784,#86291,#86292);
#79534=AXIS2_PLACEMENT_3D('',#111044,#86294,#86295);
#79535=AXIS2_PLACEMENT_3D('',#111152,#86297,#86298);
#79536=AXIS2_PLACEMENT_3D('',#111299,#86299,#86300);
#79537=AXIS2_PLACEMENT_3D('',#111301,#86301,#86302);
#79538=AXIS2_PLACEMENT_3D('',#111302,#86303,#86304);
#79539=AXIS2_PLACEMENT_3D('',#111303,#86305,#86306);
#79540=AXIS2_PLACEMENT_3D('',#111306,#86307,#86308);
#79541=AXIS2_PLACEMENT_3D('',#111366,#86309,#86310);
#79542=AXIS2_PLACEMENT_3D('',#111388,#86311,#86312);
#79543=AXIS2_PLACEMENT_3D('',#111447,#86313,#86314);
#79544=AXIS2_PLACEMENT_3D('',#111450,#86315,#86316);
#79545=AXIS2_PLACEMENT_3D('',#111452,#86317,#86318);
#79546=AXIS2_PLACEMENT_3D('',#111454,#86319,#86320);
#79547=AXIS2_PLACEMENT_3D('',#111456,#86321,#86322);
#79548=AXIS2_PLACEMENT_3D('',#111457,#86323,#86324);
#79549=AXIS2_PLACEMENT_3D('',#111458,#86325,#86326);
#79550=AXIS2_PLACEMENT_3D('',#111461,#86327,#86328);
#79551=AXIS2_PLACEMENT_3D('',#111493,#86331,#86332);
#79552=AXIS2_PLACEMENT_3D('',#111496,#86333,#86334);
#79553=AXIS2_PLACEMENT_3D('',#111571,#86335,#86336);
#79554=AXIS2_PLACEMENT_3D('',#111572,#86337,#86338);
#79555=AXIS2_PLACEMENT_3D('',#111573,#86339,#86340);
#79556=AXIS2_PLACEMENT_3D('',#111576,#86341,#86342);
#79557=AXIS2_PLACEMENT_3D('',#111580,#86344,#86345);
#79558=AXIS2_PLACEMENT_3D('',#111582,#86347,#86348);
#79559=AXIS2_PLACEMENT_3D('',#111585,#86349,#86350);
#79560=AXIS2_PLACEMENT_3D('',#111588,#86352,#86353);
#79561=AXIS2_PLACEMENT_3D('',#111589,#86354,#86355);
#79562=AXIS2_PLACEMENT_3D('',#111590,#86356,#86357);
#79563=AXIS2_PLACEMENT_3D('',#111592,#86358,#86359);
#79564=AXIS2_PLACEMENT_3D('',#111593,#86360,#86361);
#79565=AXIS2_PLACEMENT_3D('',#111594,#86362,#86363);
#79566=AXIS2_PLACEMENT_3D('',#111597,#86364,#86365);
#79567=AXIS2_PLACEMENT_3D('',#111600,#86367,#86368);
#79568=AXIS2_PLACEMENT_3D('',#111601,#86369,#86370);
#79569=AXIS2_PLACEMENT_3D('',#111602,#86371,#86372);
#79570=AXIS2_PLACEMENT_3D('',#111604,#86373,#86374);
#79571=AXIS2_PLACEMENT_3D('',#111605,#86375,#86376);
#79572=AXIS2_PLACEMENT_3D('',#111606,#86377,#86378);
#79573=AXIS2_PLACEMENT_3D('',#111609,#86379,#86380);
#79574=AXIS2_PLACEMENT_3D('',#111611,#86381,#86382);
#79575=AXIS2_PLACEMENT_3D('',#111613,#86383,#86384);
#79576=AXIS2_PLACEMENT_3D('',#111614,#86385,#86386);
#79577=AXIS2_PLACEMENT_3D('',#111615,#86387,#86388);
#79578=AXIS2_PLACEMENT_3D('',#111652,#86391,#86392);
#79579=AXIS2_PLACEMENT_3D('',#112254,#86393,#86394);
#79580=AXIS2_PLACEMENT_3D('',#112257,#86396,#86397);
#79581=AXIS2_PLACEMENT_3D('',#112259,#86398,#86399);
#79582=AXIS2_PLACEMENT_3D('',#112933,#86400,#86401);
#79583=AXIS2_PLACEMENT_3D('',#112936,#86402,#86403);
#79584=AXIS2_PLACEMENT_3D('',#112937,#86404,#86405);
#79585=AXIS2_PLACEMENT_3D('',#112938,#86406,#86407);
#79586=AXIS2_PLACEMENT_3D('',#112939,#86408,#86409);
#79587=AXIS2_PLACEMENT_3D('',#113348,#86412,#86413);
#79588=AXIS2_PLACEMENT_3D('',#113351,#86414,#86415);
#79589=AXIS2_PLACEMENT_3D('',#113353,#86416,#86417);
#79590=AXIS2_PLACEMENT_3D('',#113355,#86418,#86419);
#79591=AXIS2_PLACEMENT_3D('',#113357,#86420,#86421);
#79592=AXIS2_PLACEMENT_3D('',#113358,#86422,#86423);
#79593=AXIS2_PLACEMENT_3D('',#113359,#86424,#86425);
#79594=AXIS2_PLACEMENT_3D('',#113360,#86426,#86427);
#79595=AXIS2_PLACEMENT_3D('',#113371,#86429,#86430);
#79596=AXIS2_PLACEMENT_3D('',#113378,#86431,#86432);
#79597=AXIS2_PLACEMENT_3D('',#113380,#86433,#86434);
#79598=AXIS2_PLACEMENT_3D('',#113382,#86435,#86436);
#79599=AXIS2_PLACEMENT_3D('',#113384,#86437,#86438);
#79600=AXIS2_PLACEMENT_3D('',#113385,#86439,#86440);
#79601=AXIS2_PLACEMENT_3D('',#113386,#86441,#86442);
#79602=AXIS2_PLACEMENT_3D('',#113389,#86444,#86445);
#79603=AXIS2_PLACEMENT_3D('',#113390,#86446,#86447);
#79604=AXIS2_PLACEMENT_3D('',#113392,#86448,#86449);
#79605=AXIS2_PLACEMENT_3D('',#113396,#86451,#86452);
#79606=AXIS2_PLACEMENT_3D('',#113408,#86453,#86454);
#79607=AXIS2_PLACEMENT_3D('',#113409,#86455,#86456);
#79608=AXIS2_PLACEMENT_3D('',#113412,#86457,#86458);
#79609=AXIS2_PLACEMENT_3D('',#113429,#86459,#86460);
#79610=AXIS2_PLACEMENT_3D('',#113432,#86462,#86463);
#79611=AXIS2_PLACEMENT_3D('',#113434,#86464,#86465);
#79612=AXIS2_PLACEMENT_3D('',#113449,#86466,#86467);
#79613=AXIS2_PLACEMENT_3D('',#113451,#86468,#86469);
#79614=AXIS2_PLACEMENT_3D('',#113455,#86471,#86472);
#79615=AXIS2_PLACEMENT_3D('',#113456,#86473,#86474);
#79616=AXIS2_PLACEMENT_3D('',#113457,#86475,#86476);
#79617=AXIS2_PLACEMENT_3D('',#113460,#86478,#86479);
#79618=AXIS2_PLACEMENT_3D('',#113461,#86480,#86481);
#79619=AXIS2_PLACEMENT_3D('',#113463,#86482,#86483);
#79620=AXIS2_PLACEMENT_3D('',#113466,#86485,#86486);
#79621=AXIS2_PLACEMENT_3D('',#113467,#86487,#86488);
#79622=AXIS2_PLACEMENT_3D('',#113469,#86489,#86490);
#79623=AXIS2_PLACEMENT_3D('',#113473,#86492,#86493);
#79624=AXIS2_PLACEMENT_3D('',#113492,#86494,#86495);
#79625=AXIS2_PLACEMENT_3D('',#113494,#86496,#86497);
#79626=AXIS2_PLACEMENT_3D('',#113512,#86498,#86499);
#79627=AXIS2_PLACEMENT_3D('',#113513,#86500,#86501);
#79628=AXIS2_PLACEMENT_3D('',#113516,#86502,#86503);
#79629=AXIS2_PLACEMENT_3D('',#113517,#86504,#86505);
#79630=AXIS2_PLACEMENT_3D('',#113519,#86506,#86507);
#79631=AXIS2_PLACEMENT_3D('',#113520,#86508,#86509);
#79632=AXIS2_PLACEMENT_3D('',#113521,#86510,#86511);
#79633=AXIS2_PLACEMENT_3D('',#113523,#86512,#86513);
#79634=AXIS2_PLACEMENT_3D('',#113525,#86515,#86516);
#79635=AXIS2_PLACEMENT_3D('',#113528,#86517,#86518);
#79636=AXIS2_PLACEMENT_3D('',#113531,#86520,#86521);
#79637=AXIS2_PLACEMENT_3D('',#113532,#86522,#86523);
#79638=AXIS2_PLACEMENT_3D('',#113533,#86524,#86525);
#79639=AXIS2_PLACEMENT_3D('',#113536,#86526,#86527);
#79640=AXIS2_PLACEMENT_3D('',#113537,#86528,#86529);
#79641=AXIS2_PLACEMENT_3D('',#113539,#86531,#86532);
#79642=AXIS2_PLACEMENT_3D('',#113542,#86533,#86534);
#79643=AXIS2_PLACEMENT_3D('',#113600,#86535,#86536);
#79644=AXIS2_PLACEMENT_3D('',#113659,#86537,#86538);
#79645=AXIS2_PLACEMENT_3D('',#113662,#86539,#86540);
#79646=AXIS2_PLACEMENT_3D('',#113666,#86542,#86543);
#79647=AXIS2_PLACEMENT_3D('',#113668,#86545,#86546);
#79648=AXIS2_PLACEMENT_3D('',#113925,#86547,#86548);
#79649=AXIS2_PLACEMENT_3D('',#113928,#86549,#86550);
#79650=AXIS2_PLACEMENT_3D('',#113931,#86552,#86553);
#79651=AXIS2_PLACEMENT_3D('',#113932,#86554,#86555);
#79652=AXIS2_PLACEMENT_3D('',#113933,#86556,#86557);
#79653=AXIS2_PLACEMENT_3D('',#113935,#86559,#86560);
#79654=AXIS2_PLACEMENT_3D('',#113937,#86561,#86562);
#79655=AXIS2_PLACEMENT_3D('',#113961,#86564,#86565);
#79656=AXIS2_PLACEMENT_3D('',#113998,#86566,#86567);
#79657=AXIS2_PLACEMENT_3D('',#114225,#86568,#86569);
#79658=AXIS2_PLACEMENT_3D('',#114227,#86570,#86571);
#79659=AXIS2_PLACEMENT_3D('',#114229,#86572,#86573);
#79660=AXIS2_PLACEMENT_3D('',#114231,#86574,#86575);
#79661=AXIS2_PLACEMENT_3D('',#114232,#86576,#86577);
#79662=AXIS2_PLACEMENT_3D('',#114233,#86578,#86579);
#79663=AXIS2_PLACEMENT_3D('',#114236,#86581,#86582);
#79664=AXIS2_PLACEMENT_3D('',#114237,#86583,#86584);
#79665=AXIS2_PLACEMENT_3D('',#114288,#86585,#86586);
#79666=AXIS2_PLACEMENT_3D('',#114289,#86587,#86588);
#79667=AXIS2_PLACEMENT_3D('',#114412,#86589,#86590);
#79668=AXIS2_PLACEMENT_3D('',#114915,#86592,#86593);
#79669=AXIS2_PLACEMENT_3D('',#115275,#86594,#86595);
#79670=AXIS2_PLACEMENT_3D('',#115278,#86596,#86597);
#79671=AXIS2_PLACEMENT_3D('',#115282,#86599,#86600);
#79672=AXIS2_PLACEMENT_3D('',#115456,#86603,#86604);
#79673=AXIS2_PLACEMENT_3D('',#115459,#86605,#86606);
#79674=AXIS2_PLACEMENT_3D('',#115605,#86609,#86610);
#79675=AXIS2_PLACEMENT_3D('',#115607,#86611,#86612);
#79676=AXIS2_PLACEMENT_3D('',#115610,#86614,#86615);
#79677=AXIS2_PLACEMENT_3D('',#115611,#86616,#86617);
#79678=AXIS2_PLACEMENT_3D('',#115614,#86618,#86619);
#79679=AXIS2_PLACEMENT_3D('',#115617,#86621,#86622);
#79680=AXIS2_PLACEMENT_3D('',#115618,#86623,#86624);
#79681=AXIS2_PLACEMENT_3D('',#115619,#86625,#86626);
#79682=AXIS2_PLACEMENT_3D('',#115622,#86628,#86629);
#79683=AXIS2_PLACEMENT_3D('',#115623,#86630,#86631);
#79684=AXIS2_PLACEMENT_3D('',#115626,#86632,#86633);
#79685=AXIS2_PLACEMENT_3D('',#115630,#86635,#86636);
#79686=AXIS2_PLACEMENT_3D('',#115631,#86637,#86638);
#79687=AXIS2_PLACEMENT_3D('',#115632,#86639,#86640);
#79688=AXIS2_PLACEMENT_3D('',#115633,#86641,#86642);
#79689=AXIS2_PLACEMENT_3D('',#115663,#86644,#86645);
#79690=AXIS2_PLACEMENT_3D('',#115666,#86647,#86648);
#79691=AXIS2_PLACEMENT_3D('',#115667,#86649,#86650);
#79692=AXIS2_PLACEMENT_3D('',#115670,#86651,#86652);
#79693=AXIS2_PLACEMENT_3D('',#115671,#86653,#86654);
#79694=AXIS2_PLACEMENT_3D('',#115673,#86655,#86656);
#79695=AXIS2_PLACEMENT_3D('',#115674,#86657,#86658);
#79696=AXIS2_PLACEMENT_3D('',#115675,#86659,#86660);
#79697=AXIS2_PLACEMENT_3D('',#115677,#86661,#86662);
#79698=AXIS2_PLACEMENT_3D('',#115679,#86664,#86665);
#79699=AXIS2_PLACEMENT_3D('',#115717,#86666,#86667);
#79700=AXIS2_PLACEMENT_3D('',#115731,#86668,#86669);
#79701=AXIS2_PLACEMENT_3D('',#115765,#86670,#86671);
#79702=AXIS2_PLACEMENT_3D('',#115778,#86672,#86673);
#79703=AXIS2_PLACEMENT_3D('',#116094,#86675,#86676);
#79704=AXIS2_PLACEMENT_3D('',#116638,#86677,#86678);
#79705=AXIS2_PLACEMENT_3D('',#116709,#86680,#86681);
#79706=AXIS2_PLACEMENT_3D('',#116713,#86683,#86684);
#79707=AXIS2_PLACEMENT_3D('',#116715,#86686,#86687);
#79708=AXIS2_PLACEMENT_3D('',#116750,#86689,#86690);
#79709=AXIS2_PLACEMENT_3D('',#116752,#86692,#86693);
#79710=AXIS2_PLACEMENT_3D('',#116754,#86694,#86695);
#79711=AXIS2_PLACEMENT_3D('',#116757,#86697,#86698);
#79712=AXIS2_PLACEMENT_3D('',#116758,#86699,#86700);
#79713=AXIS2_PLACEMENT_3D('',#116761,#86701,#86702);
#79714=AXIS2_PLACEMENT_3D('',#116764,#86704,#86705);
#79715=AXIS2_PLACEMENT_3D('',#116765,#86706,#86707);
#79716=AXIS2_PLACEMENT_3D('',#116766,#86708,#86709);
#79717=AXIS2_PLACEMENT_3D('',#116769,#86711,#86712);
#79718=AXIS2_PLACEMENT_3D('',#116770,#86713,#86714);
#79719=AXIS2_PLACEMENT_3D('',#116773,#86715,#86716);
#79720=AXIS2_PLACEMENT_3D('',#116777,#86718,#86719);
#79721=AXIS2_PLACEMENT_3D('',#116778,#86720,#86721);
#79722=AXIS2_PLACEMENT_3D('',#116779,#86722,#86723);
#79723=AXIS2_PLACEMENT_3D('',#116780,#86724,#86725);
#79724=AXIS2_PLACEMENT_3D('',#116810,#86727,#86728);
#79725=AXIS2_PLACEMENT_3D('',#116813,#86730,#86731);
#79726=AXIS2_PLACEMENT_3D('',#116814,#86732,#86733);
#79727=AXIS2_PLACEMENT_3D('',#116827,#86740,#86741);
#79728=AXIS2_PLACEMENT_3D('',#116830,#86744,#86745);
#79729=AXIS2_PLACEMENT_3D('',#116832,#86747,#86748);
#79730=AXIS2_PLACEMENT_3D('',#116834,#86750,#86751);
#79731=AXIS2_PLACEMENT_3D('',#116836,#86753,#86754);
#79732=AXIS2_PLACEMENT_3D('',#116838,#86756,#86757);
#79733=AXIS2_PLACEMENT_3D('',#116839,#86758,#86759);
#79734=AXIS2_PLACEMENT_3D('',#116840,#86760,#86761);
#79735=AXIS2_PLACEMENT_3D('',#116841,#86762,#86763);
#79736=AXIS2_PLACEMENT_3D('',#116846,#86765,#86766);
#79737=AXIS2_PLACEMENT_3D('',#116849,#86768,#86769);
#79738=AXIS2_PLACEMENT_3D('',#117050,#86770,#86771);
#79739=AXIS2_PLACEMENT_3D('',#117058,#86772,#86773);
#79740=AXIS2_PLACEMENT_3D('',#117059,#86774,#86775);
#79741=AXIS2_PLACEMENT_3D('',#117061,#86776,#86777);
#79742=AXIS2_PLACEMENT_3D('',#117107,#86778,#86779);
#79743=AXIS2_PLACEMENT_3D('',#117109,#86780,#86781);
#79744=AXIS2_PLACEMENT_3D('',#117110,#86782,#86783);
#79745=AXIS2_PLACEMENT_3D('',#117111,#86784,#86785);
#79746=AXIS2_PLACEMENT_3D('',#117117,#86788,#86789);
#79747=AXIS2_PLACEMENT_3D('',#117274,#86791,#86792);
#79748=AXIS2_PLACEMENT_3D('',#117355,#86793,#86794);
#79749=AXIS2_PLACEMENT_3D('',#117358,#86796,#86797);
#79750=AXIS2_PLACEMENT_3D('',#117359,#86798,#86799);
#79751=AXIS2_PLACEMENT_3D('',#117362,#86800,#86801);
#79752=AXIS2_PLACEMENT_3D('',#117408,#86803,#86804);
#79753=AXIS2_PLACEMENT_3D('',#117488,#86805,#86806);
#79754=AXIS2_PLACEMENT_3D('',#117506,#86808,#86809);
#79755=AXIS2_PLACEMENT_3D('',#117508,#86811,#86812);
#79756=AXIS2_PLACEMENT_3D('',#117511,#86814,#86815);
#79757=AXIS2_PLACEMENT_3D('',#117614,#86816,#86817);
#79758=AXIS2_PLACEMENT_3D('',#117617,#86818,#86819);
#79759=AXIS2_PLACEMENT_3D('',#117776,#86822,#86823);
#79760=AXIS2_PLACEMENT_3D('',#117923,#86824,#86825);
#79761=AXIS2_PLACEMENT_3D('',#118018,#86826,#86827);
#79762=AXIS2_PLACEMENT_3D('',#118197,#86828,#86829);
#79763=AXIS2_PLACEMENT_3D('',#118199,#86830,#86831);
#79764=AXIS2_PLACEMENT_3D('',#118201,#86832,#86833);
#79765=AXIS2_PLACEMENT_3D('',#118203,#86834,#86835);
#79766=AXIS2_PLACEMENT_3D('',#118204,#86836,#86837);
#79767=AXIS2_PLACEMENT_3D('',#118205,#86838,#86839);
#79768=AXIS2_PLACEMENT_3D('',#118207,#86840,#86841);
#79769=AXIS2_PLACEMENT_3D('',#118208,#86842,#86843);
#79770=AXIS2_PLACEMENT_3D('',#118209,#86844,#86845);
#79771=AXIS2_PLACEMENT_3D('',#118212,#86846,#86847);
#79772=AXIS2_PLACEMENT_3D('',#118213,#86848,#86849);
#79773=AXIS2_PLACEMENT_3D('',#118214,#86850,#86851);
#79774=AXIS2_PLACEMENT_3D('',#118310,#86852,#86853);
#79775=AXIS2_PLACEMENT_3D('',#118954,#86854,#86855);
#79776=AXIS2_PLACEMENT_3D('',#118956,#86857,#86858);
#79777=AXIS2_PLACEMENT_3D('',#118958,#86859,#86860);
#79778=AXIS2_PLACEMENT_3D('',#118960,#86861,#86862);
#79779=AXIS2_PLACEMENT_3D('',#118961,#86863,#86864);
#79780=AXIS2_PLACEMENT_3D('',#118962,#86865,#86866);
#79781=AXIS2_PLACEMENT_3D('',#118964,#86867,#86868);
#79782=AXIS2_PLACEMENT_3D('',#118965,#86869,#86870);
#79783=AXIS2_PLACEMENT_3D('',#118966,#86871,#86872);
#79784=AXIS2_PLACEMENT_3D('',#118967,#86873,#86874);
#79785=AXIS2_PLACEMENT_3D('',#118968,#86875,#86876);
#79786=AXIS2_PLACEMENT_3D('',#118969,#86877,#86878);
#79787=AXIS2_PLACEMENT_3D('',#118997,#86880,#86881);
#79788=AXIS2_PLACEMENT_3D('',#118998,#86882,#86883);
#79789=AXIS2_PLACEMENT_3D('',#118999,#86884,#86885);
#79790=AXIS2_PLACEMENT_3D('',#119001,#86886,#86887);
#79791=AXIS2_PLACEMENT_3D('',#119002,#86888,#86889);
#79792=AXIS2_PLACEMENT_3D('',#119269,#86890,#86891);
#79793=AXIS2_PLACEMENT_3D('',#119270,#86892,#86893);
#79794=AXIS2_PLACEMENT_3D('',#119271,#86894,#86895);
#79795=AXIS2_PLACEMENT_3D('',#119356,#86896,#86897);
#79796=AXIS2_PLACEMENT_3D('',#119358,#86899,#86900);
#79797=AXIS2_PLACEMENT_3D('',#119360,#86901,#86902);
#79798=AXIS2_PLACEMENT_3D('',#119362,#86903,#86904);
#79799=AXIS2_PLACEMENT_3D('',#119363,#86905,#86906);
#79800=AXIS2_PLACEMENT_3D('',#119364,#86907,#86908);
#79801=AXIS2_PLACEMENT_3D('',#119366,#86909,#86910);
#79802=AXIS2_PLACEMENT_3D('',#119367,#86911,#86912);
#79803=AXIS2_PLACEMENT_3D('',#119368,#86913,#86914);
#79804=AXIS2_PLACEMENT_3D('',#119370,#86915,#86916);
#79805=AXIS2_PLACEMENT_3D('',#119371,#86917,#86918);
#79806=AXIS2_PLACEMENT_3D('',#119372,#86919,#86920);
#79807=AXIS2_PLACEMENT_3D('',#119489,#86922,#86923);
#79808=AXIS2_PLACEMENT_3D('',#119491,#86925,#86926);
#79809=AXIS2_PLACEMENT_3D('',#119492,#86927,#86928);
#79810=AXIS2_PLACEMENT_3D('',#119493,#86929,#86930);
#79811=AXIS2_PLACEMENT_3D('',#119494,#86931,#86932);
#79812=AXIS2_PLACEMENT_3D('',#119495,#86933,#86934);
#79813=AXIS2_PLACEMENT_3D('',#119496,#86935,#86936);
#79814=AXIS2_PLACEMENT_3D('',#119497,#86937,#86938);
#79815=AXIS2_PLACEMENT_3D('',#119624,#86940,#86941);
#79816=AXIS2_PLACEMENT_3D('',#119648,#86942,#86943);
#79817=AXIS2_PLACEMENT_3D('',#119649,#86944,#86945);
#79818=AXIS2_PLACEMENT_3D('',#119769,#86946,#86947);
#79819=AXIS2_PLACEMENT_3D('',#119770,#86948,#86949);
#79820=AXIS2_PLACEMENT_3D('',#119804,#86951,#86952);
#79821=AXIS2_PLACEMENT_3D('',#119871,#86953,#86954);
#79822=AXIS2_PLACEMENT_3D('',#119974,#86955,#86956);
#79823=AXIS2_PLACEMENT_3D('',#120091,#86957,#86958);
#79824=AXIS2_PLACEMENT_3D('',#120453,#86959,#86960);
#79825=AXIS2_PLACEMENT_3D('',#120537,#86961,#86962);
#79826=AXIS2_PLACEMENT_3D('',#120636,#86963,#86964);
#79827=AXIS2_PLACEMENT_3D('',#120949,#86965,#86966);
#79828=AXIS2_PLACEMENT_3D('',#121105,#86967,#86968);
#79829=AXIS2_PLACEMENT_3D('',#121190,#86969,#86970);
#79830=AXIS2_PLACEMENT_3D('',#121429,#86971,#86972);
#79831=AXIS2_PLACEMENT_3D('',#121514,#86973,#86974);
#79832=AXIS2_PLACEMENT_3D('',#121680,#86975,#86976);
#79833=AXIS2_PLACEMENT_3D('',#121904,#86977,#86978);
#79834=AXIS2_PLACEMENT_3D('',#123591,#86982,#86983);
#79835=AXIS2_PLACEMENT_3D('',#123592,#86984,#86985);
#79836=AXIS2_PLACEMENT_3D('',#123605,#86992,#86993);
#79837=AXIS2_PLACEMENT_3D('',#123608,#86996,#86997);
#79838=AXIS2_PLACEMENT_3D('',#123610,#86999,#87000);
#79839=AXIS2_PLACEMENT_3D('',#123612,#87002,#87003);
#79840=AXIS2_PLACEMENT_3D('',#123614,#87005,#87006);
#79841=AXIS2_PLACEMENT_3D('',#123616,#87008,#87009);
#79842=AXIS2_PLACEMENT_3D('',#123617,#87010,#87011);
#79843=AXIS2_PLACEMENT_3D('',#123618,#87012,#87013);
#79844=AXIS2_PLACEMENT_3D('',#123740,#87014,#87015);
#79845=AXIS2_PLACEMENT_3D('',#123745,#87017,#87018);
#79846=AXIS2_PLACEMENT_3D('',#123748,#87020,#87021);
#79847=AXIS2_PLACEMENT_3D('',#123911,#87022,#87023);
#79848=AXIS2_PLACEMENT_3D('',#124095,#87024,#87025);
#79849=AXIS2_PLACEMENT_3D('',#124098,#87026,#87027);
#79850=AXIS2_PLACEMENT_3D('',#124101,#87029,#87030);
#79851=AXIS2_PLACEMENT_3D('',#124359,#87032,#87033);
#79852=AXIS2_PLACEMENT_3D('',#124364,#87035,#87036);
#79853=AXIS2_PLACEMENT_3D('',#124419,#87037,#87038);
#79854=AXIS2_PLACEMENT_3D('',#124435,#87040,#87041);
#79855=AXIS2_PLACEMENT_3D('',#124469,#87043,#87044);
#79856=AXIS2_PLACEMENT_3D('',#124470,#87045,#87046);
#79857=AXIS2_PLACEMENT_3D('',#124471,#87047,#87048);
#79858=AXIS2_PLACEMENT_3D('',#124654,#87051,#87052);
#79859=AXIS2_PLACEMENT_3D('',#124656,#87053,#87054);
#79860=AXIS2_PLACEMENT_3D('',#124657,#87055,#87056);
#79861=AXIS2_PLACEMENT_3D('',#124658,#87057,#87058);
#79862=AXIS2_PLACEMENT_3D('',#124686,#87059,#87060);
#79863=AXIS2_PLACEMENT_3D('',#124706,#87061,#87062);
#79864=AXIS2_PLACEMENT_3D('',#124715,#87063,#87064);
#79865=AXIS2_PLACEMENT_3D('',#124717,#87066,#87067);
#79866=AXIS2_PLACEMENT_3D('',#124738,#87068,#87069);
#79867=AXIS2_PLACEMENT_3D('',#124772,#87071,#87072);
#79868=AXIS2_PLACEMENT_3D('',#124773,#87073,#87074);
#79869=AXIS2_PLACEMENT_3D('',#125006,#87075,#87076);
#79870=AXIS2_PLACEMENT_3D('',#125049,#87077,#87078);
#79871=AXIS2_PLACEMENT_3D('',#125111,#87079,#87080);
#79872=AXIS2_PLACEMENT_3D('',#125112,#87081,#87082);
#79873=AXIS2_PLACEMENT_3D('',#125113,#87083,#87084);
#79874=AXIS2_PLACEMENT_3D('',#125114,#87085,#87086);
#79875=AXIS2_PLACEMENT_3D('',#125116,#87087,#87088);
#79876=AXIS2_PLACEMENT_3D('',#125117,#87089,#87090);
#79877=AXIS2_PLACEMENT_3D('',#125404,#87091,#87092);
#79878=AXIS2_PLACEMENT_3D('',#125406,#87094,#87095);
#79879=AXIS2_PLACEMENT_3D('',#125407,#87096,#87097);
#79880=AXIS2_PLACEMENT_3D('',#125408,#87098,#87099);
#79881=AXIS2_PLACEMENT_3D('',#125409,#87100,#87101);
#79882=AXIS2_PLACEMENT_3D('',#125411,#87102,#87103);
#79883=AXIS2_PLACEMENT_3D('',#125413,#87104,#87105);
#79884=AXIS2_PLACEMENT_3D('',#125414,#87106,#87107);
#79885=AXIS2_PLACEMENT_3D('',#125415,#87108,#87109);
#79886=AXIS2_PLACEMENT_3D('',#125417,#87110,#87111);
#79887=AXIS2_PLACEMENT_3D('',#125418,#87112,#87113);
#79888=AXIS2_PLACEMENT_3D('',#125419,#87114,#87115);
#79889=AXIS2_PLACEMENT_3D('',#125931,#87117,#87118);
#79890=AXIS2_PLACEMENT_3D('',#125962,#87119,#87120);
#79891=AXIS2_PLACEMENT_3D('',#125964,#87121,#87122);
#79892=AXIS2_PLACEMENT_3D('',#125966,#87123,#87124);
#79893=AXIS2_PLACEMENT_3D('',#125968,#87125,#87126);
#79894=AXIS2_PLACEMENT_3D('',#125969,#87127,#87128);
#79895=AXIS2_PLACEMENT_3D('',#125970,#87129,#87130);
#79896=AXIS2_PLACEMENT_3D('',#125972,#87131,#87132);
#79897=AXIS2_PLACEMENT_3D('',#125973,#87133,#87134);
#79898=AXIS2_PLACEMENT_3D('',#125974,#87135,#87136);
#79899=AXIS2_PLACEMENT_3D('',#125977,#87137,#87138);
#79900=AXIS2_PLACEMENT_3D('',#125978,#87139,#87140);
#79901=AXIS2_PLACEMENT_3D('',#125979,#87141,#87142);
#79902=AXIS2_PLACEMENT_3D('',#125980,#87143,#87144);
#79903=AXIS2_PLACEMENT_3D('',#126066,#87146,#87147);
#79904=AXIS2_PLACEMENT_3D('',#126067,#87148,#87149);
#79905=AXIS2_PLACEMENT_3D('',#126068,#87150,#87151);
#79906=AXIS2_PLACEMENT_3D('',#126069,#87152,#87153);
#79907=AXIS2_PLACEMENT_3D('',#126070,#87154,#87155);
#79908=AXIS2_PLACEMENT_3D('',#126071,#87156,#87157);
#79909=AXIS2_PLACEMENT_3D('',#126072,#87158,#87159);
#79910=AXIS2_PLACEMENT_3D('',#126073,#87160,#87161);
#79911=AXIS2_PLACEMENT_3D('',#126074,#87162,#87163);
#79912=AXIS2_PLACEMENT_3D('',#126075,#87164,#87165);
#79913=AXIS2_PLACEMENT_3D('',#126213,#87167,#87168);
#79914=AXIS2_PLACEMENT_3D('',#126215,#87170,#87171);
#79915=AXIS2_PLACEMENT_3D('',#126217,#87172,#87173);
#79916=AXIS2_PLACEMENT_3D('',#126219,#87174,#87175);
#79917=AXIS2_PLACEMENT_3D('',#126220,#87176,#87177);
#79918=AXIS2_PLACEMENT_3D('',#126221,#87178,#87179);
#79919=AXIS2_PLACEMENT_3D('',#126223,#87180,#87181);
#79920=AXIS2_PLACEMENT_3D('',#126224,#87182,#87183);
#79921=AXIS2_PLACEMENT_3D('',#126225,#87184,#87185);
#79922=AXIS2_PLACEMENT_3D('',#126227,#87186,#87187);
#79923=AXIS2_PLACEMENT_3D('',#126228,#87188,#87189);
#79924=AXIS2_PLACEMENT_3D('',#126229,#87190,#87191);
#79925=AXIS2_PLACEMENT_3D('',#126356,#87193,#87194);
#79926=AXIS2_PLACEMENT_3D('',#126388,#87196,#87197);
#79927=AXIS2_PLACEMENT_3D('',#126409,#87198,#87199);
#79928=AXIS2_PLACEMENT_3D('',#126410,#87200,#87201);
#79929=AXIS2_PLACEMENT_3D('',#126554,#87202,#87203);
#79930=AXIS2_PLACEMENT_3D('',#126555,#87204,#87205);
#79931=AXIS2_PLACEMENT_3D('',#126612,#87206,#87207);
#79932=AXIS2_PLACEMENT_3D('',#126974,#87208,#87209);
#79933=AXIS2_PLACEMENT_3D('',#127058,#87210,#87211);
#79934=AXIS2_PLACEMENT_3D('',#127145,#87212,#87213);
#79935=AXIS2_PLACEMENT_3D('',#127206,#87214,#87215);
#79936=AXIS2_PLACEMENT_3D('',#127391,#87216,#87217);
#79937=AXIS2_PLACEMENT_3D('',#127559,#87218,#87219);
#79938=AXIS2_PLACEMENT_3D('',#127715,#87220,#87221);
#79939=AXIS2_PLACEMENT_3D('',#127898,#87222,#87223);
#79940=AXIS2_PLACEMENT_3D('',#128064,#87224,#87225);
#79941=AXIS2_PLACEMENT_3D('',#128149,#87226,#87227);
#79942=AXIS2_PLACEMENT_3D('',#128607,#87228,#87229);
#79943=AXIS2_PLACEMENT_3D('',#129974,#87233,#87234);
#79944=AXIS2_PLACEMENT_3D('',#130317,#87237,#87238);
#79945=AXIS2_PLACEMENT_3D('',#130318,#87239,#87240);
#79946=AXIS2_PLACEMENT_3D('',#130319,#87241,#87242);
#79947=AXIS2_PLACEMENT_3D('',#130320,#87243,#87244);
#79948=AXIS2_PLACEMENT_3D('',#130331,#87249,#87250);
#79949=AXIS2_PLACEMENT_3D('',#130333,#87251,#87252);
#79950=AXIS2_PLACEMENT_3D('',#130335,#87253,#87254);
#79951=AXIS2_PLACEMENT_3D('',#130337,#87255,#87256);
#79952=AXIS2_PLACEMENT_3D('',#130338,#87257,#87258);
#79953=AXIS2_PLACEMENT_3D('',#130339,#87259,#87260);
#79954=AXIS2_PLACEMENT_3D('',#130348,#87264,#87265);
#79955=AXIS2_PLACEMENT_3D('',#130350,#87266,#87267);
#79956=AXIS2_PLACEMENT_3D('',#130352,#87268,#87269);
#79957=AXIS2_PLACEMENT_3D('',#130354,#87270,#87271);
#79958=AXIS2_PLACEMENT_3D('',#130356,#87272,#87273);
#79959=AXIS2_PLACEMENT_3D('',#130358,#87275,#87276);
#79960=AXIS2_PLACEMENT_3D('',#130363,#87279,#87280);
#79961=AXIS2_PLACEMENT_3D('',#130364,#87281,#87282);
#79962=AXIS2_PLACEMENT_3D('',#130369,#87285,#87286);
#79963=AXIS2_PLACEMENT_3D('',#130370,#87287,#87288);
#79964=AXIS2_PLACEMENT_3D('',#130372,#87289,#87290);
#79965=AXIS2_PLACEMENT_3D('',#130374,#87291,#87292);
#79966=AXIS2_PLACEMENT_3D('',#130377,#87294,#87295);
#79967=AXIS2_PLACEMENT_3D('',#130402,#87296,#87297);
#79968=AXIS2_PLACEMENT_3D('',#130576,#87302,#87303);
#79969=AXIS2_PLACEMENT_3D('',#130597,#87304,#87305);
#79970=AXIS2_PLACEMENT_3D('',#130614,#87307,#87308);
#79971=AXIS2_PLACEMENT_3D('',#130810,#87310,#87311);
#79972=AXIS2_PLACEMENT_3D('',#131016,#87312,#87313);
#79973=AXIS2_PLACEMENT_3D('',#131033,#87315,#87316);
#79974=AXIS2_PLACEMENT_3D('',#131052,#87317,#87318);
#79975=AXIS2_PLACEMENT_3D('',#131160,#87320,#87321);
#79976=AXIS2_PLACEMENT_3D('',#131257,#87323,#87324);
#79977=AXIS2_PLACEMENT_3D('',#131349,#87326,#87327);
#79978=AXIS2_PLACEMENT_3D('',#131583,#87329,#87330);
#79979=AXIS2_PLACEMENT_3D('',#131864,#87331,#87332);
#79980=AXIS2_PLACEMENT_3D('',#131877,#87333,#87334);
#79981=AXIS2_PLACEMENT_3D('',#131879,#87336,#87337);
#79982=AXIS2_PLACEMENT_3D('',#131893,#87339,#87340);
#79983=AXIS2_PLACEMENT_3D('',#131950,#87341,#87342);
#79984=AXIS2_PLACEMENT_3D('',#132331,#87343,#87344);
#79985=AXIS2_PLACEMENT_3D('',#132332,#87345,#87346);
#79986=AXIS2_PLACEMENT_3D('',#132382,#87347,#87348);
#79987=AXIS2_PLACEMENT_3D('',#132384,#87349,#87350);
#79988=AXIS2_PLACEMENT_3D('',#132488,#87352,#87353);
#79989=AXIS2_PLACEMENT_3D('',#132587,#87354,#87355);
#79990=AXIS2_PLACEMENT_3D('',#132589,#87356,#87357);
#79991=AXIS2_PLACEMENT_3D('',#132642,#87358,#87359);
#79992=AXIS2_PLACEMENT_3D('',#132849,#87360,#87361);
#79993=AXIS2_PLACEMENT_3D('',#132917,#87362,#87363);
#79994=AXIS2_PLACEMENT_3D('',#132932,#87364,#87365);
#79995=AXIS2_PLACEMENT_3D('',#132995,#87366,#87367);
#79996=AXIS2_PLACEMENT_3D('',#133155,#87368,#87369);
#79997=AXIS2_PLACEMENT_3D('',#133212,#87370,#87371);
#79998=AXIS2_PLACEMENT_3D('',#133214,#87372,#87373);
#79999=AXIS2_PLACEMENT_3D('',#133215,#87374,#87375);
#80000=AXIS2_PLACEMENT_3D('',#133253,#87376,#87377);
#80001=AXIS2_PLACEMENT_3D('',#133378,#87378,#87379);
#80002=AXIS2_PLACEMENT_3D('',#133410,#87380,#87381);
#80003=AXIS2_PLACEMENT_3D('',#133411,#87382,#87383);
#80004=AXIS2_PLACEMENT_3D('',#133412,#87384,#87385);
#80005=AXIS2_PLACEMENT_3D('',#133413,#87386,#87387);
#80006=AXIS2_PLACEMENT_3D('',#133453,#87388,#87389);
#80007=AXIS2_PLACEMENT_3D('',#133454,#87390,#87391);
#80008=AXIS2_PLACEMENT_3D('',#133455,#87392,#87393);
#80009=AXIS2_PLACEMENT_3D('',#133456,#87394,#87395);
#80010=AXIS2_PLACEMENT_3D('',#133457,#87396,#87397);
#80011=AXIS2_PLACEMENT_3D('',#133460,#87399,#87400);
#80012=AXIS2_PLACEMENT_3D('',#133461,#87401,#87402);
#80013=AXIS2_PLACEMENT_3D('',#133462,#87403,#87404);
#80014=AXIS2_PLACEMENT_3D('',#133463,#87405,#87406);
#80015=AXIS2_PLACEMENT_3D('',#133464,#87407,#87408);
#80016=AXIS2_PLACEMENT_3D('',#133465,#87409,#87410);
#80017=AXIS2_PLACEMENT_3D('',#133467,#87412,#87413);
#80018=AXIS2_PLACEMENT_3D('',#133525,#87418,#87419);
#80019=AXIS2_PLACEMENT_3D('',#133526,#87420,#87421);
#80020=AXIS2_PLACEMENT_3D('',#133527,#87422,#87423);
#80021=AXIS2_PLACEMENT_3D('',#133609,#87424,#87425);
#80022=AXIS2_PLACEMENT_3D('',#133977,#87426,#87427);
#80023=AXIS2_PLACEMENT_3D('',#133978,#87428,#87429);
#80024=AXIS2_PLACEMENT_3D('',#134346,#87430,#87431);
#80025=AXIS2_PLACEMENT_3D('',#134411,#87432,#87433);
#80026=AXIS2_PLACEMENT_3D('',#134563,#87435,#87436);
#80027=AXIS2_PLACEMENT_3D('',#134695,#87439,#87440);
#80028=AXIS2_PLACEMENT_3D('',#134697,#87441,#87442);
#80029=AXIS2_PLACEMENT_3D('',#134699,#87443,#87444);
#80030=AXIS2_PLACEMENT_3D('',#134700,#87445,#87446);
#80031=AXIS2_PLACEMENT_3D('',#134701,#87447,#87448);
#80032=AXIS2_PLACEMENT_3D('',#134703,#87449,#87450);
#80033=AXIS2_PLACEMENT_3D('',#134704,#87451,#87452);
#80034=AXIS2_PLACEMENT_3D('',#134705,#87453,#87454);
#80035=AXIS2_PLACEMENT_3D('',#134706,#87455,#87456);
#80036=AXIS2_PLACEMENT_3D('',#134708,#87457,#87458);
#80037=AXIS2_PLACEMENT_3D('',#134710,#87459,#87460);
#80038=AXIS2_PLACEMENT_3D('',#134713,#87462,#87463);
#80039=AXIS2_PLACEMENT_3D('',#134714,#87464,#87465);
#80040=AXIS2_PLACEMENT_3D('',#134716,#87466,#87467);
#80041=AXIS2_PLACEMENT_3D('',#134717,#87468,#87469);
#80042=AXIS2_PLACEMENT_3D('',#135394,#87470,#87471);
#80043=AXIS2_PLACEMENT_3D('',#135575,#87474,#87475);
#80044=AXIS2_PLACEMENT_3D('',#135579,#87478,#87479);
#80045=AXIS2_PLACEMENT_3D('',#135580,#87480,#87481);
#80046=AXIS2_PLACEMENT_3D('',#135606,#87482,#87483);
#80047=AXIS2_PLACEMENT_3D('',#135608,#87484,#87485);
#80048=AXIS2_PLACEMENT_3D('',#135609,#87486,#87487);
#80049=AXIS2_PLACEMENT_3D('',#135610,#87488,#87489);
#80050=AXIS2_PLACEMENT_3D('',#135612,#87490,#87491);
#80051=AXIS2_PLACEMENT_3D('',#135616,#87493,#87494);
#80052=AXIS2_PLACEMENT_3D('',#135618,#87495,#87496);
#80053=AXIS2_PLACEMENT_3D('',#135620,#87498,#87499);
#80054=AXIS2_PLACEMENT_3D('',#135623,#87500,#87501);
#80055=AXIS2_PLACEMENT_3D('',#135627,#87503,#87504);
#80056=AXIS2_PLACEMENT_3D('',#135630,#87506,#87507);
#80057=AXIS2_PLACEMENT_3D('',#135631,#87508,#87509);
#80058=AXIS2_PLACEMENT_3D('',#135951,#87511,#87512);
#80059=AXIS2_PLACEMENT_3D('',#135976,#87513,#87514);
#80060=AXIS2_PLACEMENT_3D('',#136019,#87515,#87516);
#80061=AXIS2_PLACEMENT_3D('',#136044,#87517,#87518);
#80062=AXIS2_PLACEMENT_3D('',#136404,#87519,#87520);
#80063=AXIS2_PLACEMENT_3D('',#137882,#87523,#87524);
#80064=AXIS2_PLACEMENT_3D('',#137893,#87525,#87526);
#80065=AXIS2_PLACEMENT_3D('',#138650,#87529,#87530);
#80066=AXIS2_PLACEMENT_3D('',#138664,#87531,#87532);
#80067=AXIS2_PLACEMENT_3D('',#138941,#87535,#87536);
#80068=AXIS2_PLACEMENT_3D('',#138982,#87537,#87538);
#80069=AXIS2_PLACEMENT_3D('',#138983,#87539,#87540);
#80070=AXIS2_PLACEMENT_3D('',#138984,#87541,#87542);
#80071=AXIS2_PLACEMENT_3D('',#138985,#87543,#87544);
#80072=AXIS2_PLACEMENT_3D('',#139141,#87546,#87547);
#80073=AXIS2_PLACEMENT_3D('',#139467,#87548,#87549);
#80074=AXIS2_PLACEMENT_3D('',#140135,#87550,#87551);
#80075=AXIS2_PLACEMENT_3D('',#140500,#87552,#87553);
#80076=AXIS2_PLACEMENT_3D('',#140501,#87554,#87555);
#80077=AXIS2_PLACEMENT_3D('',#140594,#87556,#87557);
#80078=AXIS2_PLACEMENT_3D('',#140647,#87558,#87559);
#80079=AXIS2_PLACEMENT_3D('',#141027,#87561,#87562);
#80080=AXIS2_PLACEMENT_3D('',#141029,#87563,#87564);
#80081=AXIS2_PLACEMENT_3D('',#141095,#87565,#87566);
#80082=AXIS2_PLACEMENT_3D('',#142788,#87567,#87568);
#80083=AXIS2_PLACEMENT_3D('',#142795,#87569,#87570);
#80084=AXIS2_PLACEMENT_3D('',#142965,#87572,#87573);
#80085=AXIS2_PLACEMENT_3D('',#143054,#87575,#87576);
#80086=AXIS2_PLACEMENT_3D('',#143069,#87577,#87578);
#80087=AXIS2_PLACEMENT_3D('',#143239,#87579,#87580);
#80088=AXIS2_PLACEMENT_3D('',#143261,#87581,#87582);
#80089=AXIS2_PLACEMENT_3D('',#143262,#87583,#87584);
#80090=AXIS2_PLACEMENT_3D('',#143302,#87585,#87586);
#80091=AXIS2_PLACEMENT_3D('',#143309,#87587,#87588);
#80092=AXIS2_PLACEMENT_3D('',#143311,#87589,#87590);
#80093=AXIS2_PLACEMENT_3D('',#143312,#87591,#87592);
#80094=AXIS2_PLACEMENT_3D('',#143479,#87593,#87594);
#80095=AXIS2_PLACEMENT_3D('',#143482,#87596,#87597);
#80096=AXIS2_PLACEMENT_3D('',#143582,#87598,#87599);
#80097=AXIS2_PLACEMENT_3D('',#143583,#87600,#87601);
#80098=AXIS2_PLACEMENT_3D('',#143585,#87602,#87603);
#80099=AXIS2_PLACEMENT_3D('',#143586,#87604,#87605);
#80100=AXIS2_PLACEMENT_3D('',#143648,#87606,#87607);
#80101=AXIS2_PLACEMENT_3D('',#143687,#87608,#87609);
#80102=AXIS2_PLACEMENT_3D('',#143745,#87611,#87612);
#80103=AXIS2_PLACEMENT_3D('',#143746,#87613,#87614);
#80104=AXIS2_PLACEMENT_3D('',#143747,#87615,#87616);
#80105=AXIS2_PLACEMENT_3D('',#143749,#87617,#87618);
#80106=AXIS2_PLACEMENT_3D('',#143750,#87619,#87620);
#80107=AXIS2_PLACEMENT_3D('',#143850,#87621,#87622);
#80108=AXIS2_PLACEMENT_3D('',#143851,#87623,#87624);
#80109=AXIS2_PLACEMENT_3D('',#143854,#87626,#87627);
#80110=AXIS2_PLACEMENT_3D('',#143969,#87628,#87629);
#80111=AXIS2_PLACEMENT_3D('',#143970,#87630,#87631);
#80112=AXIS2_PLACEMENT_3D('',#143972,#87632,#87633);
#80113=AXIS2_PLACEMENT_3D('',#143973,#87634,#87635);
#80114=AXIS2_PLACEMENT_3D('',#143974,#87636,#87637);
#80115=AXIS2_PLACEMENT_3D('',#143991,#87638,#87639);
#80116=AXIS2_PLACEMENT_3D('',#143992,#87640,#87641);
#80117=AXIS2_PLACEMENT_3D('',#144002,#87642,#87643);
#80118=AXIS2_PLACEMENT_3D('',#144021,#87644,#87645);
#80119=AXIS2_PLACEMENT_3D('',#144079,#87646,#87647);
#80120=AXIS2_PLACEMENT_3D('',#144142,#87648,#87649);
#80121=AXIS2_PLACEMENT_3D('',#144193,#87650,#87651);
#80122=AXIS2_PLACEMENT_3D('',#144324,#87652,#87653);
#80123=AXIS2_PLACEMENT_3D('',#144325,#87654,#87655);
#80124=AXIS2_PLACEMENT_3D('',#144479,#87657,#87658);
#80125=AXIS2_PLACEMENT_3D('',#144480,#87659,#87660);
#80126=AXIS2_PLACEMENT_3D('',#144546,#87661,#87662);
#80127=AXIS2_PLACEMENT_3D('',#144725,#87663,#87664);
#80128=AXIS2_PLACEMENT_3D('',#144893,#87665,#87666);
#80129=AXIS2_PLACEMENT_3D('',#145131,#87667,#87668);
#80130=AXIS2_PLACEMENT_3D('',#145222,#87669,#87670);
#80131=AXIS2_PLACEMENT_3D('',#145255,#87671,#87672);
#80132=AXIS2_PLACEMENT_3D('',#145294,#87673,#87674);
#80133=AXIS2_PLACEMENT_3D('',#145295,#87675,#87676);
#80134=AXIS2_PLACEMENT_3D('',#145396,#87677,#87678);
#80135=AXIS2_PLACEMENT_3D('',#145398,#87680,#87681);
#80136=AXIS2_PLACEMENT_3D('',#145400,#87683,#87684);
#80137=AXIS2_PLACEMENT_3D('',#145403,#87687,#87688);
#80138=AXIS2_PLACEMENT_3D('',#145405,#87690,#87691);
#80139=AXIS2_PLACEMENT_3D('',#145406,#87692,#87693);
#80140=AXIS2_PLACEMENT_3D('',#145407,#87694,#87695);
#80141=AXIS2_PLACEMENT_3D('',#145410,#87696,#87697);
#80142=AXIS2_PLACEMENT_3D('',#145412,#87699,#87700);
#80143=AXIS2_PLACEMENT_3D('',#145589,#87704,#87705);
#80144=AXIS2_PLACEMENT_3D('',#145591,#87706,#87707);
#80145=AXIS2_PLACEMENT_3D('',#145592,#87708,#87709);
#80146=AXIS2_PLACEMENT_3D('',#145593,#87710,#87711);
#80147=AXIS2_PLACEMENT_3D('',#145597,#87713,#87714);
#80148=AXIS2_PLACEMENT_3D('',#145599,#87715,#87716);
#80149=AXIS2_PLACEMENT_3D('',#145617,#87717,#87718);
#80150=AXIS2_PLACEMENT_3D('',#145618,#87719,#87720);
#80151=AXIS2_PLACEMENT_3D('',#145620,#87721,#87722);
#80152=AXIS2_PLACEMENT_3D('',#145628,#87723,#87724);
#80153=AXIS2_PLACEMENT_3D('',#145630,#87725,#87726);
#80154=AXIS2_PLACEMENT_3D('',#145632,#87728,#87729);
#80155=AXIS2_PLACEMENT_3D('',#145634,#87730,#87731);
#80156=AXIS2_PLACEMENT_3D('',#145636,#87732,#87733);
#80157=AXIS2_PLACEMENT_3D('',#145637,#87734,#87735);
#80158=AXIS2_PLACEMENT_3D('',#145703,#87736,#87737);
#80159=AXIS2_PLACEMENT_3D('',#145798,#87738,#87739);
#80160=AXIS2_PLACEMENT_3D('',#145832,#87741,#87742);
#80161=AXIS2_PLACEMENT_3D('',#145856,#87744,#87745);
#80162=AXIS2_PLACEMENT_3D('',#145870,#87746,#87747);
#80163=AXIS2_PLACEMENT_3D('',#145882,#87749,#87750);
#80164=AXIS2_PLACEMENT_3D('',#145884,#87752,#87753);
#80165=AXIS2_PLACEMENT_3D('',#145949,#87756,#87757);
#80166=AXIS2_PLACEMENT_3D('',#145950,#87758,#87759);
#80167=AXIS2_PLACEMENT_3D('',#145951,#87760,#87761);
#80168=AXIS2_PLACEMENT_3D('',#146004,#87762,#87763);
#80169=AXIS2_PLACEMENT_3D('',#146005,#87764,#87765);
#80170=AXIS2_PLACEMENT_3D('',#146078,#87766,#87767);
#80171=AXIS2_PLACEMENT_3D('',#146079,#87768,#87769);
#80172=AXIS2_PLACEMENT_3D('',#146080,#87770,#87771);
#80173=AXIS2_PLACEMENT_3D('',#146081,#87772,#87773);
#80174=AXIS2_PLACEMENT_3D('',#146295,#87774,#87775);
#80175=AXIS2_PLACEMENT_3D('',#146297,#87777,#87778);
#80176=AXIS2_PLACEMENT_3D('',#146368,#87784,#87785);
#80177=AXIS2_PLACEMENT_3D('',#146607,#87786,#87787);
#80178=AXIS2_PLACEMENT_3D('',#146608,#87788,#87789);
#80179=AXIS2_PLACEMENT_3D('',#146610,#87790,#87791);
#80180=AXIS2_PLACEMENT_3D('',#146612,#87792,#87793);
#80181=AXIS2_PLACEMENT_3D('',#146613,#87794,#87795);
#80182=AXIS2_PLACEMENT_3D('',#146614,#87796,#87797);
#80183=AXIS2_PLACEMENT_3D('',#146615,#87798,#87799);
#80184=AXIS2_PLACEMENT_3D('',#146616,#87800,#87801);
#80185=AXIS2_PLACEMENT_3D('',#146655,#87802,#87803);
#80186=AXIS2_PLACEMENT_3D('',#146656,#87804,#87805);
#80187=AXIS2_PLACEMENT_3D('',#146658,#87806,#87807);
#80188=AXIS2_PLACEMENT_3D('',#146905,#87808,#87809);
#80189=AXIS2_PLACEMENT_3D('',#146907,#87811,#87812);
#80190=AXIS2_PLACEMENT_3D('',#146911,#87815,#87816);
#80191=AXIS2_PLACEMENT_3D('',#146918,#87820,#87821);
#80192=AXIS2_PLACEMENT_3D('',#146919,#87822,#87823);
#80193=AXIS2_PLACEMENT_3D('',#146920,#87824,#87825);
#80194=AXIS2_PLACEMENT_3D('',#146921,#87826,#87827);
#80195=AXIS2_PLACEMENT_3D('',#146922,#87828,#87829);
#80196=AXIS2_PLACEMENT_3D('',#146923,#87830,#87831);
#80197=AXIS2_PLACEMENT_3D('',#146924,#87832,#87833);
#80198=AXIS2_PLACEMENT_3D('',#147115,#87834,#87835);
#80199=AXIS2_PLACEMENT_3D('',#147264,#87836,#87837);
#80200=AXIS2_PLACEMENT_3D('',#147375,#87838,#87839);
#80201=AXIS2_PLACEMENT_3D('',#147444,#87840,#87841);
#80202=AXIS2_PLACEMENT_3D('',#147449,#87842,#87843);
#80203=AXIS2_PLACEMENT_3D('',#147575,#87845,#87846);
#80204=AXIS2_PLACEMENT_3D('',#147577,#87847,#87848);
#80205=AXIS2_PLACEMENT_3D('',#147610,#87849,#87850);
#80206=AXIS2_PLACEMENT_3D('',#147707,#87851,#87852);
#80207=AXIS2_PLACEMENT_3D('',#147712,#87853,#87854);
#80208=AXIS2_PLACEMENT_3D('',#148080,#87857,#87858);
#80209=AXIS2_PLACEMENT_3D('',#148457,#87859,#87860);
#80210=AXIS2_PLACEMENT_3D('',#148458,#87861,#87862);
#80211=AXIS2_PLACEMENT_3D('',#148483,#87863,#87864);
#80212=AXIS2_PLACEMENT_3D('',#148484,#87865,#87866);
#80213=AXIS2_PLACEMENT_3D('',#148487,#87867,#87868);
#80214=AXIS2_PLACEMENT_3D('',#148500,#87869,#87870);
#80215=AXIS2_PLACEMENT_3D('',#148559,#87871,#87872);
#80216=AXIS2_PLACEMENT_3D('',#148565,#87873,#87874);
#80217=AXIS2_PLACEMENT_3D('',#148667,#87875,#87876);
#80218=AXIS2_PLACEMENT_3D('',#148766,#87877,#87878);
#80219=AXIS2_PLACEMENT_3D('',#148957,#87879,#87880);
#80220=AXIS2_PLACEMENT_3D('',#149011,#87881,#87882);
#80221=AXIS2_PLACEMENT_3D('',#149117,#87883,#87884);
#80222=AXIS2_PLACEMENT_3D('',#149135,#87885,#87886);
#80223=AXIS2_PLACEMENT_3D('',#149206,#87887,#87888);
#80224=AXIS2_PLACEMENT_3D('',#149563,#87889,#87890);
#80225=AXIS2_PLACEMENT_3D('',#149606,#87891,#87892);
#80226=AXIS2_PLACEMENT_3D('',#149634,#87893,#87894);
#80227=AXIS2_PLACEMENT_3D('',#149816,#87895,#87896);
#80228=AXIS2_PLACEMENT_3D('',#149818,#87897,#87898);
#80229=AXIS2_PLACEMENT_3D('',#149820,#87899,#87900);
#80230=AXIS2_PLACEMENT_3D('',#149822,#87901,#87902);
#80231=AXIS2_PLACEMENT_3D('',#149824,#87903,#87904);
#80232=AXIS2_PLACEMENT_3D('',#149825,#87905,#87906);
#80233=AXIS2_PLACEMENT_3D('',#149826,#87907,#87908);
#80234=AXIS2_PLACEMENT_3D('',#149828,#87910,#87911);
#80235=AXIS2_PLACEMENT_3D('',#149865,#87912,#87913);
#80236=AXIS2_PLACEMENT_3D('',#149956,#87916,#87917);
#80237=AXIS2_PLACEMENT_3D('',#149958,#87919,#87920);
#80238=AXIS2_PLACEMENT_3D('',#149982,#87921,#87922);
#80239=AXIS2_PLACEMENT_3D('',#149983,#87923,#87924);
#80240=AXIS2_PLACEMENT_3D('',#150076,#87925,#87926);
#80241=AXIS2_PLACEMENT_3D('',#150078,#87927,#87928);
#80242=AXIS2_PLACEMENT_3D('',#150080,#87929,#87930);
#80243=AXIS2_PLACEMENT_3D('',#150081,#87931,#87932);
#80244=AXIS2_PLACEMENT_3D('',#150082,#87933,#87934);
#80245=AXIS2_PLACEMENT_3D('',#150112,#87936,#87937);
#80246=AXIS2_PLACEMENT_3D('',#150148,#87938,#87939);
#80247=AXIS2_PLACEMENT_3D('',#150258,#87943,#87944);
#80248=AXIS2_PLACEMENT_3D('',#150277,#87946,#87947);
#80249=AXIS2_PLACEMENT_3D('',#150343,#87948,#87949);
#80250=AXIS2_PLACEMENT_3D('',#150601,#87950,#87951);
#80251=AXIS2_PLACEMENT_3D('',#150689,#87952,#87953);
#80252=AXIS2_PLACEMENT_3D('',#150711,#87954,#87955);
#80253=AXIS2_PLACEMENT_3D('',#150814,#87956,#87957);
#80254=AXIS2_PLACEMENT_3D('',#150836,#87958,#87959);
#80255=AXIS2_PLACEMENT_3D('',#150891,#87960,#87961);
#80256=AXIS2_PLACEMENT_3D('',#151146,#87962,#87963);
#80257=AXIS2_PLACEMENT_3D('',#151225,#87964,#87965);
#80258=AXIS2_PLACEMENT_3D('',#151346,#87966,#87967);
#80259=AXIS2_PLACEMENT_3D('',#151347,#87968,#87969);
#80260=AXIS2_PLACEMENT_3D('',#151348,#87970,#87971);
#80261=AXIS2_PLACEMENT_3D('',#151349,#87972,#87973);
#80262=AXIS2_PLACEMENT_3D('',#151350,#87974,#87975);
#80263=AXIS2_PLACEMENT_3D('',#151351,#87976,#87977);
#80264=AXIS2_PLACEMENT_3D('',#151352,#87978,#87979);
#80265=AXIS2_PLACEMENT_3D('',#151354,#87980,#87981);
#80266=AXIS2_PLACEMENT_3D('',#151355,#87982,#87983);
#80267=AXIS2_PLACEMENT_3D('',#151356,#87984,#87985);
#80268=AXIS2_PLACEMENT_3D('',#151357,#87986,#87987);
#80269=AXIS2_PLACEMENT_3D('',#151358,#87988,#87989);
#80270=AXIS2_PLACEMENT_3D('',#151359,#87990,#87991);
#80271=AXIS2_PLACEMENT_3D('',#151360,#87992,#87993);
#80272=AXIS2_PLACEMENT_3D('',#151362,#87994,#87995);
#80273=AXIS2_PLACEMENT_3D('',#151363,#87996,#87997);
#80274=AXIS2_PLACEMENT_3D('',#151364,#87998,#87999);
#80275=AXIS2_PLACEMENT_3D('',#151365,#88000,#88001);
#80276=AXIS2_PLACEMENT_3D('',#151366,#88002,#88003);
#80277=AXIS2_PLACEMENT_3D('',#151367,#88004,#88005);
#80278=AXIS2_PLACEMENT_3D('',#151685,#88006,#88007);
#80279=AXIS2_PLACEMENT_3D('',#152883,#88008,#88009);
#80280=AXIS2_PLACEMENT_3D('',#152884,#88010,#88011);
#80281=AXIS2_PLACEMENT_3D('',#152885,#88012,#88013);
#80282=AXIS2_PLACEMENT_3D('',#152886,#88014,#88015);
#80283=AXIS2_PLACEMENT_3D('',#153185,#88016,#88017);
#80284=AXIS2_PLACEMENT_3D('',#153251,#88018,#88019);
#80285=AXIS2_PLACEMENT_3D('',#153253,#88020,#88021);
#80286=AXIS2_PLACEMENT_3D('',#153254,#88022,#88023);
#80287=AXIS2_PLACEMENT_3D('',#153255,#88024,#88025);
#80288=AXIS2_PLACEMENT_3D('',#153257,#88026,#88027);
#80289=AXIS2_PLACEMENT_3D('',#153258,#88028,#88029);
#80290=AXIS2_PLACEMENT_3D('',#153259,#88030,#88031);
#80291=AXIS2_PLACEMENT_3D('',#153260,#88032,#88033);
#80292=AXIS2_PLACEMENT_3D('',#153261,#88034,#88035);
#80293=AXIS2_PLACEMENT_3D('',#153262,#88036,#88037);
#80294=AXIS2_PLACEMENT_3D('',#153263,#88038,#88039);
#80295=AXIS2_PLACEMENT_3D('',#153264,#88040,#88041);
#80296=AXIS2_PLACEMENT_3D('',#153652,#88042,#88043);
#80297=AXIS2_PLACEMENT_3D('',#153673,#88044,#88045);
#80298=AXIS2_PLACEMENT_3D('',#153885,#88046,#88047);
#80299=AXIS2_PLACEMENT_3D('',#154081,#88048,#88049);
#80300=AXIS2_PLACEMENT_3D('',#154117,#88050,#88051);
#80301=AXIS2_PLACEMENT_3D('',#154128,#88052,#88053);
#80302=AXIS2_PLACEMENT_3D('',#154201,#88054,#88055);
#80303=AXIS2_PLACEMENT_3D('',#154339,#88056,#88057);
#80304=AXIS2_PLACEMENT_3D('',#154377,#88058,#88059);
#80305=AXIS2_PLACEMENT_3D('',#154415,#88060,#88061);
#80306=AXIS2_PLACEMENT_3D('',#154611,#88062,#88063);
#80307=AXIS2_PLACEMENT_3D('',#154817,#88064,#88065);
#80308=AXIS2_PLACEMENT_3D('',#154818,#88066,#88067);
#80309=AXIS2_PLACEMENT_3D('',#154819,#88068,#88069);
#80310=AXIS2_PLACEMENT_3D('',#154820,#88070,#88071);
#80311=AXIS2_PLACEMENT_3D('',#154821,#88072,#88073);
#80312=AXIS2_PLACEMENT_3D('',#154822,#88074,#88075);
#80313=AXIS2_PLACEMENT_3D('',#154823,#88076,#88077);
#80314=AXIS2_PLACEMENT_3D('',#154824,#88078,#88079);
#80315=AXIS2_PLACEMENT_3D('',#154825,#88080,#88081);
#80316=AXIS2_PLACEMENT_3D('',#154826,#88082,#88083);
#80317=AXIS2_PLACEMENT_3D('',#154829,#88085,#88086);
#80318=AXIS2_PLACEMENT_3D('',#154831,#88087,#88088);
#80319=AXIS2_PLACEMENT_3D('',#154833,#88090,#88091);
#80320=AXIS2_PLACEMENT_3D('',#155004,#88093,#88094);
#80321=AXIS2_PLACEMENT_3D('',#155005,#88095,#88096);
#80322=AXIS2_PLACEMENT_3D('',#155053,#88097,#88098);
#80323=AXIS2_PLACEMENT_3D('',#155054,#88099,#88100);
#80324=AXIS2_PLACEMENT_3D('',#155484,#88101,#88102);
#80325=AXIS2_PLACEMENT_3D('',#155722,#88103,#88104);
#80326=AXIS2_PLACEMENT_3D('',#155864,#88105,#88106);
#80327=AXIS2_PLACEMENT_3D('',#155865,#88107,#88108);
#80328=AXIS2_PLACEMENT_3D('',#155866,#88109,#88110);
#80329=AXIS2_PLACEMENT_3D('',#155867,#88111,#88112);
#80330=AXIS2_PLACEMENT_3D('',#155868,#88113,#88114);
#80331=AXIS2_PLACEMENT_3D('',#155869,#88115,#88116);
#80332=AXIS2_PLACEMENT_3D('',#156062,#88117,#88118);
#80333=AXIS2_PLACEMENT_3D('',#156224,#88119,#88120);
#80334=AXIS2_PLACEMENT_3D('',#156225,#88121,#88122);
#80335=AXIS2_PLACEMENT_3D('',#156251,#88123,#88124);
#80336=AXIS2_PLACEMENT_3D('',#156275,#88125,#88126);
#80337=AXIS2_PLACEMENT_3D('',#156300,#88127,#88128);
#80338=AXIS2_PLACEMENT_3D('',#156301,#88129,#88130);
#80339=AXIS2_PLACEMENT_3D('',#156302,#88131,#88132);
#80340=AXIS2_PLACEMENT_3D('',#156681,#88133,#88134);
#80341=AXIS2_PLACEMENT_3D('',#156682,#88135,#88136);
#80342=AXIS2_PLACEMENT_3D('',#156683,#88137,#88138);
#80343=AXIS2_PLACEMENT_3D('',#156806,#88139,#88140);
#80344=AXIS2_PLACEMENT_3D('',#156809,#88142,#88143);
#80345=AXIS2_PLACEMENT_3D('',#156810,#88144,#88145);
#80346=AXIS2_PLACEMENT_3D('',#156866,#88146,#88147);
#80347=AXIS2_PLACEMENT_3D('',#156997,#88148,#88149);
#80348=AXIS2_PLACEMENT_3D('',#157000,#88151,#88152);
#80349=AXIS2_PLACEMENT_3D('',#157028,#88153,#88154);
#80350=AXIS2_PLACEMENT_3D('',#157029,#88155,#88156);
#80351=AXIS2_PLACEMENT_3D('',#157030,#88157,#88158);
#80352=AXIS2_PLACEMENT_3D('',#157046,#88159,#88160);
#80353=AXIS2_PLACEMENT_3D('',#157047,#88161,#88162);
#80354=AXIS2_PLACEMENT_3D('',#157048,#88163,#88164);
#80355=AXIS2_PLACEMENT_3D('',#157049,#88165,#88166);
#80356=AXIS2_PLACEMENT_3D('',#157050,#88167,#88168);
#80357=AXIS2_PLACEMENT_3D('',#157105,#88169,#88170);
#80358=AXIS2_PLACEMENT_3D('',#157121,#88171,#88172);
#80359=AXIS2_PLACEMENT_3D('',#157122,#88173,#88174);
#80360=AXIS2_PLACEMENT_3D('',#157123,#88175,#88176);
#80361=AXIS2_PLACEMENT_3D('',#157124,#88177,#88178);
#80362=AXIS2_PLACEMENT_3D('',#157125,#88179,#88180);
#80363=AXIS2_PLACEMENT_3D('',#157369,#88181,#88182);
#80364=AXIS2_PLACEMENT_3D('',#157416,#88183,#88184);
#80365=AXIS2_PLACEMENT_3D('',#157454,#88185,#88186);
#80366=AXIS2_PLACEMENT_3D('',#157455,#88187,#88188);
#80367=AXIS2_PLACEMENT_3D('',#157705,#88189,#88190);
#80368=AXIS2_PLACEMENT_3D('',#157706,#88191,#88192);
#80369=AXIS2_PLACEMENT_3D('',#157747,#88193,#88194);
#80370=AXIS2_PLACEMENT_3D('',#157797,#88195,#88196);
#80371=AXIS2_PLACEMENT_3D('',#157798,#88197,#88198);
#80372=AXIS2_PLACEMENT_3D('',#157932,#88199,#88200);
#80373=AXIS2_PLACEMENT_3D('',#158052,#88201,#88202);
#80374=AXIS2_PLACEMENT_3D('',#158091,#88203,#88204);
#80375=AXIS2_PLACEMENT_3D('',#158201,#88205,#88206);
#80376=AXIS2_PLACEMENT_3D('',#158202,#88207,#88208);
#80377=AXIS2_PLACEMENT_3D('',#158203,#88209,#88210);
#80378=AXIS2_PLACEMENT_3D('',#158204,#88211,#88212);
#80379=AXIS2_PLACEMENT_3D('',#158205,#88213,#88214);
#80380=AXIS2_PLACEMENT_3D('',#158206,#88215,#88216);
#80381=AXIS2_PLACEMENT_3D('',#158209,#88217,#88218);
#80382=AXIS2_PLACEMENT_3D('',#158252,#88219,#88220);
#80383=AXIS2_PLACEMENT_3D('',#158294,#88221,#88222);
#80384=AXIS2_PLACEMENT_3D('',#158295,#88223,#88224);
#80385=AXIS2_PLACEMENT_3D('',#158465,#88227,#88228);
#80386=AXIS2_PLACEMENT_3D('',#158467,#88229,#88230);
#80387=AXIS2_PLACEMENT_3D('',#158468,#88231,#88232);
#80388=AXIS2_PLACEMENT_3D('',#158628,#88233,#88234);
#80389=AXIS2_PLACEMENT_3D('',#158711,#88237,#88238);
#80390=AXIS2_PLACEMENT_3D('',#158714,#88239,#88240);
#80391=AXIS2_PLACEMENT_3D('',#158716,#88241,#88242);
#80392=AXIS2_PLACEMENT_3D('',#158741,#88245,#88246);
#80393=AXIS2_PLACEMENT_3D('',#158742,#88247,#88248);
#80394=AXIS2_PLACEMENT_3D('',#158762,#88249,#88250);
#80395=AXIS2_PLACEMENT_3D('',#158763,#88251,#88252);
#80396=AXIS2_PLACEMENT_3D('',#158765,#88254,#88255);
#80397=AXIS2_PLACEMENT_3D('',#158767,#88256,#88257);
#80398=AXIS2_PLACEMENT_3D('',#158769,#88258,#88259);
#80399=AXIS2_PLACEMENT_3D('',#158770,#88260,#88261);
#80400=AXIS2_PLACEMENT_3D('',#158771,#88262,#88263);
#80401=AXIS2_PLACEMENT_3D('',#158773,#88264,#88265);
#80402=AXIS2_PLACEMENT_3D('',#158774,#88266,#88267);
#80403=AXIS2_PLACEMENT_3D('',#158775,#88268,#88269);
#80404=AXIS2_PLACEMENT_3D('',#158863,#88270,#88271);
#80405=AXIS2_PLACEMENT_3D('',#158864,#88272,#88273);
#80406=AXIS2_PLACEMENT_3D('',#158865,#88274,#88275);
#80407=AXIS2_PLACEMENT_3D('',#158903,#88276,#88277);
#80408=AXIS2_PLACEMENT_3D('',#158905,#88278,#88279);
#80409=AXIS2_PLACEMENT_3D('',#158994,#88280,#88281);
#80410=AXIS2_PLACEMENT_3D('',#159027,#88283,#88284);
#80411=AXIS2_PLACEMENT_3D('',#159056,#88285,#88286);
#80412=AXIS2_PLACEMENT_3D('',#159065,#88291,#88292);
#80413=AXIS2_PLACEMENT_3D('',#159067,#88293,#88294);
#80414=AXIS2_PLACEMENT_3D('',#159069,#88295,#88296);
#80415=AXIS2_PLACEMENT_3D('',#159071,#88298,#88299);
#80416=AXIS2_PLACEMENT_3D('',#159073,#88300,#88301);
#80417=AXIS2_PLACEMENT_3D('',#159075,#88303,#88304);
#80418=AXIS2_PLACEMENT_3D('',#159077,#88305,#88306);
#80419=AXIS2_PLACEMENT_3D('',#159079,#88308,#88309);
#80420=AXIS2_PLACEMENT_3D('',#159081,#88311,#88312);
#80421=AXIS2_PLACEMENT_3D('',#159084,#88313,#88314);
#80422=AXIS2_PLACEMENT_3D('',#159088,#88316,#88317);
#80423=AXIS2_PLACEMENT_3D('',#159090,#88319,#88320);
#80424=AXIS2_PLACEMENT_3D('',#159095,#88323,#88324);
#80425=AXIS2_PLACEMENT_3D('',#159096,#88325,#88326);
#80426=AXIS2_PLACEMENT_3D('',#159100,#88329,#88330);
#80427=AXIS2_PLACEMENT_3D('',#159103,#88332,#88333);
#80428=AXIS2_PLACEMENT_3D('',#159104,#88334,#88335);
#80429=AXIS2_PLACEMENT_3D('',#159106,#88337,#88338);
#80430=AXIS2_PLACEMENT_3D('',#159115,#88343,#88344);
#80431=AXIS2_PLACEMENT_3D('',#159117,#88345,#88346);
#80432=AXIS2_PLACEMENT_3D('',#159120,#88348,#88349);
#80433=AXIS2_PLACEMENT_3D('',#159121,#88350,#88351);
#80434=AXIS2_PLACEMENT_3D('',#159127,#88355,#88356);
#80435=AXIS2_PLACEMENT_3D('',#159129,#88357,#88358);
#80436=AXIS2_PLACEMENT_3D('',#159132,#88360,#88361);
#80437=AXIS2_PLACEMENT_3D('',#159133,#88362,#88363);
#80438=AXIS2_PLACEMENT_3D('',#159139,#88367,#88368);
#80439=AXIS2_PLACEMENT_3D('',#159141,#88369,#88370);
#80440=AXIS2_PLACEMENT_3D('',#159143,#88371,#88372);
#80441=AXIS2_PLACEMENT_3D('',#159145,#88374,#88375);
#80442=AXIS2_PLACEMENT_3D('',#159147,#88376,#88377);
#80443=AXIS2_PLACEMENT_3D('',#159148,#88378,#88379);
#80444=AXIS2_PLACEMENT_3D('',#159149,#88380,#88381);
#80445=AXIS2_PLACEMENT_3D('',#159151,#88382,#88383);
#80446=AXIS2_PLACEMENT_3D('',#159153,#88385,#88386);
#80447=AXIS2_PLACEMENT_3D('',#159155,#88387,#88388);
#80448=AXIS2_PLACEMENT_3D('',#159156,#88389,#88390);
#80449=AXIS2_PLACEMENT_3D('',#159157,#88391,#88392);
#80450=AXIS2_PLACEMENT_3D('',#159159,#88393,#88394);
#80451=AXIS2_PLACEMENT_3D('',#159161,#88396,#88397);
#80452=AXIS2_PLACEMENT_3D('',#159164,#88398,#88399);
#80453=AXIS2_PLACEMENT_3D('',#159165,#88400,#88401);
#80454=AXIS2_PLACEMENT_3D('',#159166,#88402,#88403);
#80455=AXIS2_PLACEMENT_3D('',#159167,#88404,#88405);
#80456=AXIS2_PLACEMENT_3D('',#159170,#88407,#88408);
#80457=AXIS2_PLACEMENT_3D('',#159171,#88409,#88410);
#80458=AXIS2_PLACEMENT_3D('',#159177,#88414,#88415);
#80459=AXIS2_PLACEMENT_3D('',#159331,#88416,#88417);
#80460=AXIS2_PLACEMENT_3D('',#159332,#88418,#88419);
#80461=AXIS2_PLACEMENT_3D('',#159335,#88421,#88422);
#80462=AXIS2_PLACEMENT_3D('',#159401,#88423,#88424);
#80463=AXIS2_PLACEMENT_3D('',#159403,#88425,#88426);
#80464=AXIS2_PLACEMENT_3D('',#159508,#88427,#88428);
#80465=AXIS2_PLACEMENT_3D('',#159513,#88431,#88432);
#80466=AXIS2_PLACEMENT_3D('',#159514,#88433,#88434);
#80467=AXIS2_PLACEMENT_3D('',#159519,#88438,#88439);
#80468=AXIS2_PLACEMENT_3D('',#159520,#88440,#88441);
#80469=AXIS2_PLACEMENT_3D('',#159521,#88442,#88443);
#80470=AXIS2_PLACEMENT_3D('',#159676,#88445,#88446);
#80471=AXIS2_PLACEMENT_3D('',#159677,#88447,#88448);
#80472=AXIS2_PLACEMENT_3D('',#159684,#88449,#88450);
#80473=AXIS2_PLACEMENT_3D('',#159686,#88452,#88453);
#80474=AXIS2_PLACEMENT_3D('',#159687,#88454,#88455);
#80475=AXIS2_PLACEMENT_3D('',#159688,#88456,#88457);
#80476=AXIS2_PLACEMENT_3D('',#159689,#88458,#88459);
#80477=AXIS2_PLACEMENT_3D('',#159691,#88460,#88461);
#80478=AXIS2_PLACEMENT_3D('',#159693,#88463,#88464);
#80479=AXIS2_PLACEMENT_3D('',#159697,#88467,#88468);
#80480=AXIS2_PLACEMENT_3D('',#159698,#88469,#88470);
#80481=AXIS2_PLACEMENT_3D('',#159699,#88471,#88472);
#80482=AXIS2_PLACEMENT_3D('',#159701,#88474,#88475);
#80483=AXIS2_PLACEMENT_3D('',#159718,#88484,#88485);
#80484=AXIS2_PLACEMENT_3D('',#159724,#88489,#88490);
#80485=AXIS2_PLACEMENT_3D('',#159728,#88493,#88494);
#80486=AXIS2_PLACEMENT_3D('',#159732,#88497,#88498);
#80487=AXIS2_PLACEMENT_3D('',#159736,#88501,#88502);
#80488=AXIS2_PLACEMENT_3D('',#159740,#88505,#88506);
#80489=AXIS2_PLACEMENT_3D('',#159744,#88509,#88510);
#80490=AXIS2_PLACEMENT_3D('',#159748,#88513,#88514);
#80491=AXIS2_PLACEMENT_3D('',#159750,#88516,#88517);
#80492=AXIS2_PLACEMENT_3D('',#159751,#88518,#88519);
#80493=AXIS2_PLACEMENT_3D('',#159752,#88520,#88521);
#80494=AXIS2_PLACEMENT_3D('',#159755,#88524,#88525);
#80495=AXIS2_PLACEMENT_3D('',#159801,#88526,#88527);
#80496=AXIS2_PLACEMENT_3D('',#159814,#88528,#88529);
#80497=AXIS2_PLACEMENT_3D('',#159936,#88530,#88531);
#80498=AXIS2_PLACEMENT_3D('',#160081,#88532,#88533);
#80499=AXIS2_PLACEMENT_3D('',#160177,#88534,#88535);
#80500=AXIS2_PLACEMENT_3D('',#160178,#88536,#88537);
#80501=AXIS2_PLACEMENT_3D('',#160225,#88539,#88540);
#80502=AXIS2_PLACEMENT_3D('',#160329,#88541,#88542);
#80503=AXIS2_PLACEMENT_3D('',#160330,#88543,#88544);
#80504=AXIS2_PLACEMENT_3D('',#160470,#88546,#88547);
#80505=AXIS2_PLACEMENT_3D('',#160500,#88548,#88549);
#80506=AXIS2_PLACEMENT_3D('',#160557,#88550,#88551);
#80507=AXIS2_PLACEMENT_3D('',#160662,#88552,#88553);
#80508=AXIS2_PLACEMENT_3D('',#160677,#88555,#88556);
#80509=AXIS2_PLACEMENT_3D('',#160790,#88557,#88558);
#80510=AXIS2_PLACEMENT_3D('',#160815,#88559,#88560);
#80511=AXIS2_PLACEMENT_3D('',#160865,#88561,#88562);
#80512=AXIS2_PLACEMENT_3D('',#160882,#88563,#88564);
#80513=AXIS2_PLACEMENT_3D('',#160979,#88565,#88566);
#80514=AXIS2_PLACEMENT_3D('',#160981,#88568,#88569);
#80515=AXIS2_PLACEMENT_3D('',#161429,#88570,#88571);
#80516=AXIS2_PLACEMENT_3D('',#161431,#88572,#88573);
#80517=AXIS2_PLACEMENT_3D('',#161796,#88574,#88575);
#80518=AXIS2_PLACEMENT_3D('',#161797,#88576,#88577);
#80519=AXIS2_PLACEMENT_3D('',#161910,#88578,#88579);
#80520=AXIS2_PLACEMENT_3D('',#161935,#88580,#88581);
#80521=AXIS2_PLACEMENT_3D('',#161936,#88582,#88583);
#80522=AXIS2_PLACEMENT_3D('',#161937,#88584,#88585);
#80523=AXIS2_PLACEMENT_3D('',#161938,#88586,#88587);
#80524=AXIS2_PLACEMENT_3D('',#162146,#88589,#88590);
#80525=AXIS2_PLACEMENT_3D('',#162327,#88591,#88592);
#80526=AXIS2_PLACEMENT_3D('',#162745,#88594,#88595);
#80527=AXIS2_PLACEMENT_3D('',#163163,#88597,#88598);
#80528=AXIS2_PLACEMENT_3D('',#163569,#88600,#88601);
#80529=AXIS2_PLACEMENT_3D('',#163990,#88603,#88604);
#80530=AXIS2_PLACEMENT_3D('',#164418,#88606,#88607);
#80531=AXIS2_PLACEMENT_3D('',#164423,#88609,#88610);
#80532=AXIS2_PLACEMENT_3D('',#164830,#88611,#88612);
#80533=AXIS2_PLACEMENT_3D('',#164974,#88614,#88615);
#80534=AXIS2_PLACEMENT_3D('',#165103,#88616,#88617);
#80535=AXIS2_PLACEMENT_3D('',#165633,#88619,#88620);
#80536=AXIS2_PLACEMENT_3D('',#166147,#88622,#88623);
#80537=AXIS2_PLACEMENT_3D('',#166683,#88625,#88626);
#80538=AXIS2_PLACEMENT_3D('',#167207,#88628,#88629);
#80539=AXIS2_PLACEMENT_3D('',#167727,#88631,#88632);
#80540=AXIS2_PLACEMENT_3D('',#168253,#88634,#88635);
#80541=AXIS2_PLACEMENT_3D('',#168279,#88637,#88638);
#80542=AXIS2_PLACEMENT_3D('',#168280,#88639,#88640);
#80543=AXIS2_PLACEMENT_3D('',#168456,#88642,#88643);
#80544=AXIS2_PLACEMENT_3D('',#168627,#88644,#88645);
#80545=AXIS2_PLACEMENT_3D('',#169155,#88647,#88648);
#80546=AXIS2_PLACEMENT_3D('',#169671,#88650,#88651);
#80547=AXIS2_PLACEMENT_3D('',#170189,#88653,#88654);
#80548=AXIS2_PLACEMENT_3D('',#170715,#88656,#88657);
#80549=AXIS2_PLACEMENT_3D('',#170875,#88659,#88660);
#80550=AXIS2_PLACEMENT_3D('',#171014,#88661,#88662);
#80551=AXIS2_PLACEMENT_3D('',#171444,#88664,#88665);
#80552=AXIS2_PLACEMENT_3D('',#171888,#88667,#88668);
#80553=AXIS2_PLACEMENT_3D('',#172332,#88670,#88671);
#80554=AXIS2_PLACEMENT_3D('',#172766,#88673,#88674);
#80555=AXIS2_PLACEMENT_3D('',#173202,#88676,#88677);
#80556=AXIS2_PLACEMENT_3D('',#173218,#88679,#88680);
#80557=AXIS2_PLACEMENT_3D('',#173230,#88681,#88682);
#80558=AXIS2_PLACEMENT_3D('',#173273,#88683,#88684);
#80559=AXIS2_PLACEMENT_3D('',#173292,#88685,#88686);
#80560=AXIS2_PLACEMENT_3D('',#173294,#88687,#88688);
#80561=AXIS2_PLACEMENT_3D('',#173298,#88690,#88691);
#80562=AXIS2_PLACEMENT_3D('',#173299,#88692,#88693);
#80563=AXIS2_PLACEMENT_3D('',#173300,#88694,#88695);
#80564=AXIS2_PLACEMENT_3D('',#173302,#88696,#88697);
#80565=AXIS2_PLACEMENT_3D('',#173305,#88699,#88700);
#80566=AXIS2_PLACEMENT_3D('',#173306,#88701,#88702);
#80567=AXIS2_PLACEMENT_3D('',#173308,#88703,#88704);
#80568=AXIS2_PLACEMENT_3D('',#173311,#88706,#88707);
#80569=AXIS2_PLACEMENT_3D('',#173312,#88708,#88709);
#80570=AXIS2_PLACEMENT_3D('',#173513,#88710,#88711);
#80571=AXIS2_PLACEMENT_3D('',#173700,#88712,#88713);
#80572=AXIS2_PLACEMENT_3D('',#173702,#88714,#88715);
#80573=AXIS2_PLACEMENT_3D('',#173749,#88717,#88718);
#80574=AXIS2_PLACEMENT_3D('',#173777,#88719,#88720);
#80575=AXIS2_PLACEMENT_3D('',#173778,#88721,#88722);
#80576=AXIS2_PLACEMENT_3D('',#173794,#88724,#88725);
#80577=AXIS2_PLACEMENT_3D('',#173797,#88726,#88727);
#80578=AXIS2_PLACEMENT_3D('',#173800,#88729,#88730);
#80579=AXIS2_PLACEMENT_3D('',#173801,#88731,#88732);
#80580=AXIS2_PLACEMENT_3D('',#173802,#88733,#88734);
#80581=AXIS2_PLACEMENT_3D('',#173804,#88735,#88736);
#80582=AXIS2_PLACEMENT_3D('',#173807,#88738,#88739);
#80583=AXIS2_PLACEMENT_3D('',#173808,#88740,#88741);
#80584=AXIS2_PLACEMENT_3D('',#173810,#88742,#88743);
#80585=AXIS2_PLACEMENT_3D('',#173811,#88744,#88745);
#80586=AXIS2_PLACEMENT_3D('',#173812,#88746,#88747);
#80587=AXIS2_PLACEMENT_3D('',#173814,#88748,#88749);
#80588=AXIS2_PLACEMENT_3D('',#173815,#88750,#88751);
#80589=AXIS2_PLACEMENT_3D('',#173816,#88752,#88753);
#80590=AXIS2_PLACEMENT_3D('',#173819,#88754,#88755);
#80591=AXIS2_PLACEMENT_3D('',#173823,#88757,#88758);
#80592=AXIS2_PLACEMENT_3D('',#173825,#88760,#88761);
#80593=AXIS2_PLACEMENT_3D('',#173826,#88762,#88763);
#80594=AXIS2_PLACEMENT_3D('',#173879,#88764,#88765);
#80595=AXIS2_PLACEMENT_3D('',#173949,#88767,#88768);
#80596=AXIS2_PLACEMENT_3D('',#173950,#88769,#88770);
#80597=AXIS2_PLACEMENT_3D('',#174019,#88771,#88772);
#80598=AXIS2_PLACEMENT_3D('',#174616,#88773,#88774);
#80599=AXIS2_PLACEMENT_3D('',#174622,#88778,#88779);
#80600=AXIS2_PLACEMENT_3D('',#174628,#88783,#88784);
#80601=AXIS2_PLACEMENT_3D('',#174634,#88788,#88789);
#80602=AXIS2_PLACEMENT_3D('',#174636,#88790,#88791);
#80603=AXIS2_PLACEMENT_3D('',#174639,#88793,#88794);
#80604=AXIS2_PLACEMENT_3D('',#174640,#88795,#88796);
#80605=AXIS2_PLACEMENT_3D('',#174646,#88800,#88801);
#80606=AXIS2_PLACEMENT_3D('',#174652,#88805,#88806);
#80607=AXIS2_PLACEMENT_3D('',#174655,#88809,#88810);
#80608=AXIS2_PLACEMENT_3D('',#174656,#88811,#88812);
#80609=AXIS2_PLACEMENT_3D('',#174657,#88813,#88814);
#80610=AXIS2_PLACEMENT_3D('',#174670,#88821,#88822);
#80611=AXIS2_PLACEMENT_3D('',#174673,#88825,#88826);
#80612=AXIS2_PLACEMENT_3D('',#174675,#88828,#88829);
#80613=AXIS2_PLACEMENT_3D('',#174677,#88831,#88832);
#80614=AXIS2_PLACEMENT_3D('',#174679,#88834,#88835);
#80615=AXIS2_PLACEMENT_3D('',#174681,#88837,#88838);
#80616=AXIS2_PLACEMENT_3D('',#174682,#88839,#88840);
#80617=AXIS2_PLACEMENT_3D('',#174683,#88841,#88842);
#80618=AXIS2_PLACEMENT_3D('',#174684,#88843,#88844);
#80619=AXIS2_PLACEMENT_3D('',#174685,#88845,#88846);
#80620=AXIS2_PLACEMENT_3D('',#174686,#88847,#88848);
#80621=AXIS2_PLACEMENT_3D('',#174687,#88849,#88850);
#80622=AXIS2_PLACEMENT_3D('',#174689,#88851,#88852);
#80623=AXIS2_PLACEMENT_3D('',#174691,#88853,#88854);
#80624=AXIS2_PLACEMENT_3D('',#174692,#88855,#88856);
#80625=AXIS2_PLACEMENT_3D('',#174693,#88857,#88858);
#80626=AXIS2_PLACEMENT_3D('',#174695,#88859,#88860);
#80627=AXIS2_PLACEMENT_3D('',#174697,#88861,#88862);
#80628=AXIS2_PLACEMENT_3D('',#174698,#88863,#88864);
#80629=AXIS2_PLACEMENT_3D('',#174699,#88865,#88866);
#80630=AXIS2_PLACEMENT_3D('',#174701,#88867,#88868);
#80631=AXIS2_PLACEMENT_3D('',#174705,#88870,#88871);
#80632=AXIS2_PLACEMENT_3D('',#174709,#88873,#88874);
#80633=AXIS2_PLACEMENT_3D('',#174713,#88876,#88877);
#80634=AXIS2_PLACEMENT_3D('',#174717,#88879,#88880);
#80635=AXIS2_PLACEMENT_3D('',#174721,#88882,#88883);
#80636=AXIS2_PLACEMENT_3D('',#174725,#88885,#88886);
#80637=AXIS2_PLACEMENT_3D('',#174728,#88888,#88889);
#80638=AXIS2_PLACEMENT_3D('',#174729,#88890,#88891);
#80639=AXIS2_PLACEMENT_3D('',#174731,#88892,#88893);
#80640=AXIS2_PLACEMENT_3D('',#174733,#88894,#88895);
#80641=AXIS2_PLACEMENT_3D('',#174734,#88896,#88897);
#80642=AXIS2_PLACEMENT_3D('',#174735,#88898,#88899);
#80643=AXIS2_PLACEMENT_3D('',#174737,#88900,#88901);
#80644=AXIS2_PLACEMENT_3D('',#174739,#88902,#88903);
#80645=AXIS2_PLACEMENT_3D('',#174740,#88904,#88905);
#80646=AXIS2_PLACEMENT_3D('',#174741,#88906,#88907);
#80647=AXIS2_PLACEMENT_3D('',#174743,#88908,#88909);
#80648=AXIS2_PLACEMENT_3D('',#174746,#88911,#88912);
#80649=AXIS2_PLACEMENT_3D('',#174747,#88913,#88914);
#80650=AXIS2_PLACEMENT_3D('',#174748,#88915,#88916);
#80651=AXIS2_PLACEMENT_3D('',#174749,#88917,#88918);
#80652=AXIS2_PLACEMENT_3D('',#174750,#88919,#88920);
#80653=AXIS2_PLACEMENT_3D('',#174751,#88921,#88922);
#80654=AXIS2_PLACEMENT_3D('',#174752,#88923,#88924);
#80655=AXIS2_PLACEMENT_3D('',#174753,#88925,#88926);
#80656=AXIS2_PLACEMENT_3D('',#174754,#88927,#88928);
#80657=AXIS2_PLACEMENT_3D('',#174755,#88929,#88930);
#80658=AXIS2_PLACEMENT_3D('',#174756,#88931,#88932);
#80659=AXIS2_PLACEMENT_3D('',#174757,#88933,#88934);
#80660=AXIS2_PLACEMENT_3D('',#174758,#88935,#88936);
#80661=AXIS2_PLACEMENT_3D('',#174759,#88937,#88938);
#80662=AXIS2_PLACEMENT_3D('',#174760,#88939,#88940);
#80663=AXIS2_PLACEMENT_3D('',#174761,#88941,#88942);
#80664=AXIS2_PLACEMENT_3D('',#174762,#88943,#88944);
#80665=AXIS2_PLACEMENT_3D('',#174763,#88945,#88946);
#80666=AXIS2_PLACEMENT_3D('',#174764,#88947,#88948);
#80667=AXIS2_PLACEMENT_3D('',#174765,#88949,#88950);
#80668=AXIS2_PLACEMENT_3D('',#174766,#88951,#88952);
#80669=AXIS2_PLACEMENT_3D('',#174924,#88955,#88956);
#80670=AXIS2_PLACEMENT_3D('',#175090,#88958,#88959);
#80671=AXIS2_PLACEMENT_3D('',#175120,#88961,#88962);
#80672=AXIS2_PLACEMENT_3D('',#175254,#88966,#88967);
#80673=AXIS2_PLACEMENT_3D('',#175331,#88968,#88969);
#80674=AXIS2_PLACEMENT_3D('',#175491,#88971,#88972);
#80675=AXIS2_PLACEMENT_3D('',#175656,#88974,#88975);
#80676=AXIS2_PLACEMENT_3D('',#175813,#88977,#88978);
#80677=AXIS2_PLACEMENT_3D('',#175818,#88980,#88981);
#80678=AXIS2_PLACEMENT_3D('',#175827,#88982,#88983);
#80679=AXIS2_PLACEMENT_3D('',#175829,#88984,#88985);
#80680=AXIS2_PLACEMENT_3D('',#175832,#88987,#88988);
#80681=AXIS2_PLACEMENT_3D('',#175833,#88989,#88990);
#80682=AXIS2_PLACEMENT_3D('',#175962,#88991,#88992);
#80683=AXIS2_PLACEMENT_3D('',#175963,#88993,#88994);
#80684=AXIS2_PLACEMENT_3D('',#176130,#88995,#88996);
#80685=AXIS2_PLACEMENT_3D('',#176151,#88998,#88999);
#80686=AXIS2_PLACEMENT_3D('',#176257,#89000,#89001);
#80687=AXIS2_PLACEMENT_3D('',#176264,#89002,#89003);
#80688=AXIS2_PLACEMENT_3D('',#176270,#89004,#89005);
#80689=AXIS2_PLACEMENT_3D('',#176276,#89006,#89007);
#80690=AXIS2_PLACEMENT_3D('',#176282,#89008,#89009);
#80691=AXIS2_PLACEMENT_3D('',#176288,#89010,#89011);
#80692=AXIS2_PLACEMENT_3D('',#176291,#89013,#89014);
#80693=AXIS2_PLACEMENT_3D('',#176293,#89015,#89016);
#80694=AXIS2_PLACEMENT_3D('',#176298,#89017,#89018);
#80695=AXIS2_PLACEMENT_3D('',#176299,#89019,#89020);
#80696=AXIS2_PLACEMENT_3D('',#176306,#89021,#89022);
#80697=AXIS2_PLACEMENT_3D('',#176312,#89023,#89024);
#80698=AXIS2_PLACEMENT_3D('',#176318,#89025,#89026);
#80699=AXIS2_PLACEMENT_3D('',#176324,#89027,#89028);
#80700=AXIS2_PLACEMENT_3D('',#176330,#89029,#89030);
#80701=AXIS2_PLACEMENT_3D('',#176333,#89032,#89033);
#80702=AXIS2_PLACEMENT_3D('',#176335,#89034,#89035);
#80703=AXIS2_PLACEMENT_3D('',#176340,#89036,#89037);
#80704=AXIS2_PLACEMENT_3D('',#176341,#89038,#89039);
#80705=AXIS2_PLACEMENT_3D('',#176344,#89042,#89043);
#80706=AXIS2_PLACEMENT_3D('',#176347,#89046,#89047);
#80707=AXIS2_PLACEMENT_3D('',#176349,#89049,#89050);
#80708=AXIS2_PLACEMENT_3D('',#176351,#89052,#89053);
#80709=AXIS2_PLACEMENT_3D('',#176353,#89055,#89056);
#80710=AXIS2_PLACEMENT_3D('',#176355,#89058,#89059);
#80711=AXIS2_PLACEMENT_3D('',#176357,#89061,#89062);
#80712=AXIS2_PLACEMENT_3D('',#176360,#89065,#89066);
#80713=AXIS2_PLACEMENT_3D('',#176361,#89067,#89068);
#80714=AXIS2_PLACEMENT_3D('',#176363,#89070,#89071);
#80715=AXIS2_PLACEMENT_3D('',#176364,#89072,#89073);
#80716=AXIS2_PLACEMENT_3D('',#176365,#89074,#89075);
#80717=AXIS2_PLACEMENT_3D('',#177864,#89078,#89079);
#80718=AXIS2_PLACEMENT_3D('',#177865,#89080,#89081);
#80719=AXIS2_PLACEMENT_3D('',#177866,#89082,#89083);
#80720=AXIS2_PLACEMENT_3D('',#177867,#89084,#89085);
#80721=AXIS2_PLACEMENT_3D('',#177869,#89086,#89087);
#80722=AXIS2_PLACEMENT_3D('',#177871,#89088,#89089);
#80723=AXIS2_PLACEMENT_3D('',#177872,#89090,#89091);
#80724=AXIS2_PLACEMENT_3D('',#177873,#89092,#89093);
#80725=AXIS2_PLACEMENT_3D('',#177875,#89094,#89095);
#80726=AXIS2_PLACEMENT_3D('',#177877,#89096,#89097);
#80727=AXIS2_PLACEMENT_3D('',#177878,#89098,#89099);
#80728=AXIS2_PLACEMENT_3D('',#177879,#89100,#89101);
#80729=AXIS2_PLACEMENT_3D('',#177881,#89102,#89103);
#80730=AXIS2_PLACEMENT_3D('',#177885,#89105,#89106);
#80731=AXIS2_PLACEMENT_3D('',#177889,#89108,#89109);
#80732=AXIS2_PLACEMENT_3D('',#177893,#89111,#89112);
#80733=AXIS2_PLACEMENT_3D('',#177897,#89114,#89115);
#80734=AXIS2_PLACEMENT_3D('',#177901,#89117,#89118);
#80735=AXIS2_PLACEMENT_3D('',#177905,#89120,#89121);
#80736=AXIS2_PLACEMENT_3D('',#177908,#89123,#89124);
#80737=AXIS2_PLACEMENT_3D('',#177909,#89125,#89126);
#80738=AXIS2_PLACEMENT_3D('',#177911,#89127,#89128);
#80739=AXIS2_PLACEMENT_3D('',#177913,#89129,#89130);
#80740=AXIS2_PLACEMENT_3D('',#177914,#89131,#89132);
#80741=AXIS2_PLACEMENT_3D('',#177915,#89133,#89134);
#80742=AXIS2_PLACEMENT_3D('',#177917,#89135,#89136);
#80743=AXIS2_PLACEMENT_3D('',#177919,#89137,#89138);
#80744=AXIS2_PLACEMENT_3D('',#177920,#89139,#89140);
#80745=AXIS2_PLACEMENT_3D('',#177921,#89141,#89142);
#80746=AXIS2_PLACEMENT_3D('',#177923,#89143,#89144);
#80747=AXIS2_PLACEMENT_3D('',#177926,#89146,#89147);
#80748=AXIS2_PLACEMENT_3D('',#177927,#89148,#89149);
#80749=AXIS2_PLACEMENT_3D('',#177928,#89150,#89151);
#80750=AXIS2_PLACEMENT_3D('',#177929,#89152,#89153);
#80751=AXIS2_PLACEMENT_3D('',#177930,#89154,#89155);
#80752=AXIS2_PLACEMENT_3D('',#177931,#89156,#89157);
#80753=AXIS2_PLACEMENT_3D('',#177932,#89158,#89159);
#80754=AXIS2_PLACEMENT_3D('',#177933,#89160,#89161);
#80755=AXIS2_PLACEMENT_3D('',#177934,#89162,#89163);
#80756=AXIS2_PLACEMENT_3D('',#177935,#89164,#89165);
#80757=AXIS2_PLACEMENT_3D('',#177936,#89166,#89167);
#80758=AXIS2_PLACEMENT_3D('',#177937,#89168,#89169);
#80759=AXIS2_PLACEMENT_3D('',#177938,#89170,#89171);
#80760=AXIS2_PLACEMENT_3D('',#177939,#89172,#89173);
#80761=AXIS2_PLACEMENT_3D('',#177940,#89174,#89175);
#80762=AXIS2_PLACEMENT_3D('',#177941,#89176,#89177);
#80763=AXIS2_PLACEMENT_3D('',#177942,#89178,#89179);
#80764=AXIS2_PLACEMENT_3D('',#177943,#89180,#89181);
#80765=AXIS2_PLACEMENT_3D('',#177944,#89182,#89183);
#80766=AXIS2_PLACEMENT_3D('',#177945,#89184,#89185);
#80767=AXIS2_PLACEMENT_3D('',#177946,#89186,#89187);
#80768=AXIS2_PLACEMENT_3D('',#177948,#89188,#89189);
#80769=AXIS2_PLACEMENT_3D('',#177950,#89190,#89191);
#80770=AXIS2_PLACEMENT_3D('',#177951,#89192,#89193);
#80771=AXIS2_PLACEMENT_3D('',#177952,#89194,#89195);
#80772=AXIS2_PLACEMENT_3D('',#177955,#89197,#89198);
#80773=AXIS2_PLACEMENT_3D('',#177956,#89199,#89200);
#80774=AXIS2_PLACEMENT_3D('',#177959,#89201,#89202);
#80775=AXIS2_PLACEMENT_3D('',#177963,#89204,#89205);
#80776=AXIS2_PLACEMENT_3D('',#177965,#89207,#89208);
#80777=AXIS2_PLACEMENT_3D('',#177966,#89209,#89210);
#80778=AXIS2_PLACEMENT_3D('',#177967,#89211,#89212);
#80779=AXIS2_PLACEMENT_3D('',#177968,#89213,#89214);
#80780=AXIS2_PLACEMENT_3D('',#177970,#89215,#89216);
#80781=AXIS2_PLACEMENT_3D('',#177972,#89217,#89218);
#80782=AXIS2_PLACEMENT_3D('',#177973,#89219,#89220);
#80783=AXIS2_PLACEMENT_3D('',#177974,#89221,#89222);
#80784=AXIS2_PLACEMENT_3D('',#177976,#89223,#89224);
#80785=AXIS2_PLACEMENT_3D('',#177978,#89226,#89227);
#80786=AXIS2_PLACEMENT_3D('',#177980,#89228,#89229);
#80787=AXIS2_PLACEMENT_3D('',#177983,#89231,#89232);
#80788=AXIS2_PLACEMENT_3D('',#177984,#89233,#89234);
#80789=AXIS2_PLACEMENT_3D('',#177985,#89235,#89236);
#80790=AXIS2_PLACEMENT_3D('',#177986,#89237,#89238);
#80791=AXIS2_PLACEMENT_3D('',#177988,#89239,#89240);
#80792=AXIS2_PLACEMENT_3D('',#177989,#89241,#89242);
#80793=AXIS2_PLACEMENT_3D('',#177992,#89244,#89245);
#80794=AXIS2_PLACEMENT_3D('',#177993,#89246,#89247);
#80795=AXIS2_PLACEMENT_3D('',#177994,#89248,#89249);
#80796=AXIS2_PLACEMENT_3D('',#177995,#89250,#89251);
#80797=AXIS2_PLACEMENT_3D('',#177996,#89252,#89253);
#80798=AXIS2_PLACEMENT_3D('',#178152,#89256,#89257);
#80799=AXIS2_PLACEMENT_3D('',#178318,#89259,#89260);
#80800=AXIS2_PLACEMENT_3D('',#178348,#89262,#89263);
#80801=AXIS2_PLACEMENT_3D('',#178488,#89267,#89268);
#80802=AXIS2_PLACEMENT_3D('',#178567,#89269,#89270);
#80803=AXIS2_PLACEMENT_3D('',#178733,#89272,#89273);
#80804=AXIS2_PLACEMENT_3D('',#178902,#89275,#89276);
#80805=AXIS2_PLACEMENT_3D('',#179061,#89278,#89279);
#80806=AXIS2_PLACEMENT_3D('',#179066,#89281,#89282);
#80807=AXIS2_PLACEMENT_3D('',#179075,#89283,#89284);
#80808=AXIS2_PLACEMENT_3D('',#179077,#89285,#89286);
#80809=AXIS2_PLACEMENT_3D('',#179080,#89288,#89289);
#80810=AXIS2_PLACEMENT_3D('',#179081,#89290,#89291);
#80811=AXIS2_PLACEMENT_3D('',#179210,#89292,#89293);
#80812=AXIS2_PLACEMENT_3D('',#179211,#89294,#89295);
#80813=AXIS2_PLACEMENT_3D('',#179374,#89296,#89297);
#80814=AXIS2_PLACEMENT_3D('',#179395,#89299,#89300);
#80815=AXIS2_PLACEMENT_3D('',#179501,#89301,#89302);
#80816=AXIS2_PLACEMENT_3D('',#179508,#89303,#89304);
#80817=AXIS2_PLACEMENT_3D('',#179514,#89305,#89306);
#80818=AXIS2_PLACEMENT_3D('',#179520,#89307,#89308);
#80819=AXIS2_PLACEMENT_3D('',#179526,#89309,#89310);
#80820=AXIS2_PLACEMENT_3D('',#179532,#89311,#89312);
#80821=AXIS2_PLACEMENT_3D('',#179535,#89314,#89315);
#80822=AXIS2_PLACEMENT_3D('',#179537,#89316,#89317);
#80823=AXIS2_PLACEMENT_3D('',#179542,#89318,#89319);
#80824=AXIS2_PLACEMENT_3D('',#179543,#89320,#89321);
#80825=AXIS2_PLACEMENT_3D('',#179550,#89322,#89323);
#80826=AXIS2_PLACEMENT_3D('',#179556,#89324,#89325);
#80827=AXIS2_PLACEMENT_3D('',#179562,#89326,#89327);
#80828=AXIS2_PLACEMENT_3D('',#179568,#89328,#89329);
#80829=AXIS2_PLACEMENT_3D('',#179574,#89330,#89331);
#80830=AXIS2_PLACEMENT_3D('',#179577,#89333,#89334);
#80831=AXIS2_PLACEMENT_3D('',#179579,#89335,#89336);
#80832=AXIS2_PLACEMENT_3D('',#179584,#89337,#89338);
#80833=AXIS2_PLACEMENT_3D('',#179585,#89339,#89340);
#80834=AXIS2_PLACEMENT_3D('',#179588,#89343,#89344);
#80835=AXIS2_PLACEMENT_3D('',#179591,#89347,#89348);
#80836=AXIS2_PLACEMENT_3D('',#179593,#89350,#89351);
#80837=AXIS2_PLACEMENT_3D('',#179595,#89353,#89354);
#80838=AXIS2_PLACEMENT_3D('',#179597,#89356,#89357);
#80839=AXIS2_PLACEMENT_3D('',#179599,#89359,#89360);
#80840=AXIS2_PLACEMENT_3D('',#179601,#89362,#89363);
#80841=AXIS2_PLACEMENT_3D('',#179604,#89366,#89367);
#80842=AXIS2_PLACEMENT_3D('',#179605,#89368,#89369);
#80843=AXIS2_PLACEMENT_3D('',#179607,#89371,#89372);
#80844=AXIS2_PLACEMENT_3D('',#179608,#89373,#89374);
#80845=AXIS2_PLACEMENT_3D('',#179609,#89375,#89376);
#80846=AXIS2_PLACEMENT_3D('',#181108,#89379,#89380);
#80847=AXIS2_PLACEMENT_3D('',#181109,#89381,#89382);
#80848=AXIS2_PLACEMENT_3D('',#181110,#89383,#89384);
#80849=AXIS2_PLACEMENT_3D('',#181111,#89385,#89386);
#80850=AXIS2_PLACEMENT_3D('',#181113,#89387,#89388);
#80851=AXIS2_PLACEMENT_3D('',#181117,#89390,#89391);
#80852=AXIS2_PLACEMENT_3D('',#181118,#89392,#89393);
#80853=AXIS2_PLACEMENT_3D('',#181119,#89394,#89395);
#80854=AXIS2_PLACEMENT_3D('',#181122,#89397,#89398);
#80855=AXIS2_PLACEMENT_3D('',#181123,#89399,#89400);
#80856=AXIS2_PLACEMENT_3D('',#181239,#89402,#89403);
#80857=AXIS2_PLACEMENT_3D('',#181316,#89404,#89405);
#80858=AXIS2_PLACEMENT_3D('',#181680,#89407,#89408);
#80859=AXIS2_PLACEMENT_3D('',#182042,#89410,#89411);
#80860=AXIS2_PLACEMENT_3D('',#182064,#89413,#89414);
#80861=AXIS2_PLACEMENT_3D('',#182065,#89415,#89416);
#80862=AXIS2_PLACEMENT_3D('',#182149,#89418,#89419);
#80863=AXIS2_PLACEMENT_3D('',#182206,#89420,#89421);
#80864=AXIS2_PLACEMENT_3D('',#182588,#89423,#89424);
#80865=AXIS2_PLACEMENT_3D('',#182590,#89425,#89426);
#80866=AXIS2_PLACEMENT_3D('',#182594,#89428,#89429);
#80867=AXIS2_PLACEMENT_3D('',#182598,#89431,#89432);
#80868=AXIS2_PLACEMENT_3D('',#182602,#89434,#89435);
#80869=AXIS2_PLACEMENT_3D('',#182606,#89437,#89438);
#80870=AXIS2_PLACEMENT_3D('',#182609,#89440,#89441);
#80871=AXIS2_PLACEMENT_3D('',#182610,#89442,#89443);
#80872=AXIS2_PLACEMENT_3D('',#182613,#89444,#89445);
#80873=AXIS2_PLACEMENT_3D('',#182627,#89446,#89447);
#80874=AXIS2_PLACEMENT_3D('',#182629,#89448,#89449);
#80875=AXIS2_PLACEMENT_3D('',#182632,#89451,#89452);
#80876=AXIS2_PLACEMENT_3D('',#182633,#89453,#89454);
#80877=AXIS2_PLACEMENT_3D('',#182812,#89455,#89456);
#80878=AXIS2_PLACEMENT_3D('',#182973,#89457,#89458);
#80879=AXIS2_PLACEMENT_3D('',#182983,#89459,#89460);
#80880=AXIS2_PLACEMENT_3D('',#182984,#89461,#89462);
#80881=AXIS2_PLACEMENT_3D('',#183012,#89464,#89465);
#80882=AXIS2_PLACEMENT_3D('',#183015,#89466,#89467);
#80883=AXIS2_PLACEMENT_3D('',#183018,#89469,#89470);
#80884=AXIS2_PLACEMENT_3D('',#183019,#89471,#89472);
#80885=AXIS2_PLACEMENT_3D('',#183020,#89473,#89474);
#80886=AXIS2_PLACEMENT_3D('',#183023,#89475,#89476);
#80887=AXIS2_PLACEMENT_3D('',#183025,#89477,#89478);
#80888=AXIS2_PLACEMENT_3D('',#183029,#89480,#89481);
#80889=AXIS2_PLACEMENT_3D('',#183031,#89482,#89483);
#80890=AXIS2_PLACEMENT_3D('',#183033,#89485,#89486);
#80891=AXIS2_PLACEMENT_3D('',#183044,#89488,#89489);
#80892=AXIS2_PLACEMENT_3D('',#183045,#89490,#89491);
#80893=AXIS2_PLACEMENT_3D('',#183055,#89493,#89494);
#80894=AXIS2_PLACEMENT_3D('',#183056,#89495,#89496);
#80895=AXIS2_PLACEMENT_3D('',#183057,#89497,#89498);
#80896=AXIS2_PLACEMENT_3D('',#183185,#89499,#89500);
#80897=AXIS2_PLACEMENT_3D('',#183188,#89502,#89503);
#80898=AXIS2_PLACEMENT_3D('',#183189,#89504,#89505);
#80899=AXIS2_PLACEMENT_3D('',#183444,#89506,#89507);
#80900=AXIS2_PLACEMENT_3D('',#183446,#89508,#89509);
#80901=AXIS2_PLACEMENT_3D('',#183449,#89511,#89512);
#80902=AXIS2_PLACEMENT_3D('',#183450,#89513,#89514);
#80903=AXIS2_PLACEMENT_3D('',#183452,#89515,#89516);
#80904=AXIS2_PLACEMENT_3D('',#183453,#89517,#89518);
#80905=AXIS2_PLACEMENT_3D('',#183454,#89519,#89520);
#80906=AXIS2_PLACEMENT_3D('',#183457,#89522,#89523);
#80907=AXIS2_PLACEMENT_3D('',#183458,#89524,#89525);
#80908=AXIS2_PLACEMENT_3D('',#183461,#89526,#89527);
#80909=AXIS2_PLACEMENT_3D('',#183464,#89529,#89530);
#80910=AXIS2_PLACEMENT_3D('',#183465,#89531,#89532);
#80911=AXIS2_PLACEMENT_3D('',#183466,#89533,#89534);
#80912=AXIS2_PLACEMENT_3D('',#183468,#89535,#89536);
#80913=AXIS2_PLACEMENT_3D('',#183472,#89538,#89539);
#80914=AXIS2_PLACEMENT_3D('',#183473,#89540,#89541);
#80915=AXIS2_PLACEMENT_3D('',#183474,#89542,#89543);
#80916=AXIS2_PLACEMENT_3D('',#183476,#89544,#89545);
#80917=AXIS2_PLACEMENT_3D('',#183477,#89546,#89547);
#80918=AXIS2_PLACEMENT_3D('',#183478,#89548,#89549);
#80919=AXIS2_PLACEMENT_3D('',#183480,#89550,#89551);
#80920=AXIS2_PLACEMENT_3D('',#183481,#89552,#89553);
#80921=AXIS2_PLACEMENT_3D('',#183482,#89554,#89555);
#80922=AXIS2_PLACEMENT_3D('',#183483,#89556,#89557);
#80923=AXIS2_PLACEMENT_3D('',#183484,#89558,#89559);
#80924=AXIS2_PLACEMENT_3D('',#183486,#89560,#89561);
#80925=AXIS2_PLACEMENT_3D('',#183489,#89563,#89564);
#80926=AXIS2_PLACEMENT_3D('',#183490,#89565,#89566);
#80927=AXIS2_PLACEMENT_3D('',#183492,#89567,#89568);
#80928=AXIS2_PLACEMENT_3D('',#183493,#89569,#89570);
#80929=AXIS2_PLACEMENT_3D('',#183494,#89571,#89572);
#80930=AXIS2_PLACEMENT_3D('',#183496,#89573,#89574);
#80931=AXIS2_PLACEMENT_3D('',#183499,#89576,#89577);
#80932=AXIS2_PLACEMENT_3D('',#183500,#89578,#89579);
#80933=AXIS2_PLACEMENT_3D('',#183502,#89580,#89581);
#80934=AXIS2_PLACEMENT_3D('',#183505,#89583,#89584);
#80935=AXIS2_PLACEMENT_3D('',#183506,#89585,#89586);
#80936=AXIS2_PLACEMENT_3D('',#183507,#89587,#89588);
#80937=AXIS2_PLACEMENT_3D('',#183508,#89589,#89590);
#80938=AXIS2_PLACEMENT_3D('',#183509,#89591,#89592);
#80939=AXIS2_PLACEMENT_3D('',#183510,#89593,#89594);
#80940=AXIS2_PLACEMENT_3D('',#183511,#89595,#89596);
#80941=AXIS2_PLACEMENT_3D('',#183728,#89597,#89598);
#80942=AXIS2_PLACEMENT_3D('',#183730,#89600,#89601);
#80943=AXIS2_PLACEMENT_3D('',#183743,#89603,#89604);
#80944=AXIS2_PLACEMENT_3D('',#183745,#89606,#89607);
#80945=AXIS2_PLACEMENT_3D('',#183751,#89609,#89610);
#80946=AXIS2_PLACEMENT_3D('',#183752,#89611,#89612);
#80947=AXIS2_PLACEMENT_3D('',#183753,#89613,#89614);
#80948=AXIS2_PLACEMENT_3D('',#183754,#89615,#89616);
#80949=AXIS2_PLACEMENT_3D('',#183755,#89617,#89618);
#80950=AXIS2_PLACEMENT_3D('',#183756,#89619,#89620);
#80951=AXIS2_PLACEMENT_3D('',#183757,#89621,#89622);
#80952=AXIS2_PLACEMENT_3D('',#183758,#89623,#89624);
#80953=AXIS2_PLACEMENT_3D('',#183760,#89625,#89626);
#80954=AXIS2_PLACEMENT_3D('',#183762,#89627,#89628);
#80955=AXIS2_PLACEMENT_3D('',#183763,#89629,#89630);
#80956=AXIS2_PLACEMENT_3D('',#183764,#89631,#89632);
#80957=AXIS2_PLACEMENT_3D('',#183767,#89634,#89635);
#80958=AXIS2_PLACEMENT_3D('',#183768,#89636,#89637);
#80959=AXIS2_PLACEMENT_3D('',#183771,#89638,#89639);
#80960=AXIS2_PLACEMENT_3D('',#183775,#89641,#89642);
#80961=AXIS2_PLACEMENT_3D('',#183777,#89644,#89645);
#80962=AXIS2_PLACEMENT_3D('',#183778,#89646,#89647);
#80963=AXIS2_PLACEMENT_3D('',#183779,#89648,#89649);
#80964=AXIS2_PLACEMENT_3D('',#183780,#89650,#89651);
#80965=AXIS2_PLACEMENT_3D('',#183782,#89652,#89653);
#80966=AXIS2_PLACEMENT_3D('',#183784,#89654,#89655);
#80967=AXIS2_PLACEMENT_3D('',#183785,#89656,#89657);
#80968=AXIS2_PLACEMENT_3D('',#183786,#89658,#89659);
#80969=AXIS2_PLACEMENT_3D('',#183788,#89660,#89661);
#80970=AXIS2_PLACEMENT_3D('',#183790,#89663,#89664);
#80971=AXIS2_PLACEMENT_3D('',#183792,#89665,#89666);
#80972=AXIS2_PLACEMENT_3D('',#183795,#89668,#89669);
#80973=AXIS2_PLACEMENT_3D('',#183796,#89670,#89671);
#80974=AXIS2_PLACEMENT_3D('',#183797,#89672,#89673);
#80975=AXIS2_PLACEMENT_3D('',#183798,#89674,#89675);
#80976=AXIS2_PLACEMENT_3D('',#183800,#89676,#89677);
#80977=AXIS2_PLACEMENT_3D('',#183801,#89678,#89679);
#80978=AXIS2_PLACEMENT_3D('',#183804,#89681,#89682);
#80979=AXIS2_PLACEMENT_3D('',#183805,#89683,#89684);
#80980=AXIS2_PLACEMENT_3D('',#183806,#89685,#89686);
#80981=AXIS2_PLACEMENT_3D('',#183807,#89687,#89688);
#80982=AXIS2_PLACEMENT_3D('',#183808,#89689,#89690);
#80983=AXIS2_PLACEMENT_3D('',#183821,#89692,#89693);
#80984=AXIS2_PLACEMENT_3D('',#183822,#89694,#89695);
#80985=AXIS2_PLACEMENT_3D('',#183909,#89697,#89698);
#80986=AXIS2_PLACEMENT_3D('',#183964,#89699,#89700);
#80987=AXIS2_PLACEMENT_3D('',#184162,#89702,#89703);
#80988=AXIS2_PLACEMENT_3D('',#184167,#89705,#89706);
#80989=AXIS2_PLACEMENT_3D('',#184348,#89707,#89708);
#80990=AXIS2_PLACEMENT_3D('',#184351,#89709,#89710);
#80991=AXIS2_PLACEMENT_3D('',#184354,#89712,#89713);
#80992=AXIS2_PLACEMENT_3D('',#184355,#89714,#89715);
#80993=AXIS2_PLACEMENT_3D('',#184356,#89716,#89717);
#80994=AXIS2_PLACEMENT_3D('',#184358,#89718,#89719);
#80995=AXIS2_PLACEMENT_3D('',#184359,#89720,#89721);
#80996=AXIS2_PLACEMENT_3D('',#184360,#89722,#89723);
#80997=AXIS2_PLACEMENT_3D('',#184362,#89724,#89725);
#80998=AXIS2_PLACEMENT_3D('',#184363,#89726,#89727);
#80999=AXIS2_PLACEMENT_3D('',#184364,#89728,#89729);
#81000=AXIS2_PLACEMENT_3D('',#184407,#89732,#89733);
#81001=AXIS2_PLACEMENT_3D('',#184450,#89736,#89737);
#81002=AXIS2_PLACEMENT_3D('',#184454,#89739,#89740);
#81003=AXIS2_PLACEMENT_3D('',#184476,#89741,#89742);
#81004=AXIS2_PLACEMENT_3D('',#184479,#89744,#89745);
#81005=AXIS2_PLACEMENT_3D('',#184480,#89746,#89747);
#81006=AXIS2_PLACEMENT_3D('',#184481,#89748,#89749);
#81007=AXIS2_PLACEMENT_3D('',#184484,#89750,#89751);
#81008=AXIS2_PLACEMENT_3D('',#184505,#89752,#89753);
#81009=AXIS2_PLACEMENT_3D('',#184527,#89754,#89755);
#81010=AXIS2_PLACEMENT_3D('',#184548,#89756,#89757);
#81011=AXIS2_PLACEMENT_3D('',#184569,#89758,#89759);
#81012=AXIS2_PLACEMENT_3D('',#184590,#89760,#89761);
#81013=AXIS2_PLACEMENT_3D('',#184591,#89762,#89763);
#81014=AXIS2_PLACEMENT_3D('',#184614,#89766,#89767);
#81015=AXIS2_PLACEMENT_3D('',#184637,#89770,#89771);
#81016=AXIS2_PLACEMENT_3D('',#184639,#89772,#89773);
#81017=AXIS2_PLACEMENT_3D('',#184643,#89775,#89776);
#81018=AXIS2_PLACEMENT_3D('',#184665,#89777,#89778);
#81019=AXIS2_PLACEMENT_3D('',#184668,#89780,#89781);
#81020=AXIS2_PLACEMENT_3D('',#184669,#89782,#89783);
#81021=AXIS2_PLACEMENT_3D('',#184670,#89784,#89785);
#81022=AXIS2_PLACEMENT_3D('',#184672,#89786,#89787);
#81023=AXIS2_PLACEMENT_3D('',#184674,#89788,#89789);
#81024=AXIS2_PLACEMENT_3D('',#184695,#89790,#89791);
#81025=AXIS2_PLACEMENT_3D('',#184697,#89792,#89793);
#81026=AXIS2_PLACEMENT_3D('',#184718,#89794,#89795);
#81027=AXIS2_PLACEMENT_3D('',#184720,#89796,#89797);
#81028=AXIS2_PLACEMENT_3D('',#184740,#89798,#89799);
#81029=AXIS2_PLACEMENT_3D('',#184742,#89800,#89801);
#81030=AXIS2_PLACEMENT_3D('',#184743,#89802,#89803);
#81031=AXIS2_PLACEMENT_3D('',#184744,#89804,#89805);
#81032=AXIS2_PLACEMENT_3D('',#184746,#89806,#89807);
#81033=AXIS2_PLACEMENT_3D('',#184749,#89809,#89810);
#81034=AXIS2_PLACEMENT_3D('',#184750,#89811,#89812);
#81035=AXIS2_PLACEMENT_3D('',#184752,#89813,#89814);
#81036=AXIS2_PLACEMENT_3D('',#184755,#89816,#89817);
#81037=AXIS2_PLACEMENT_3D('',#184756,#89818,#89819);
#81038=AXIS2_PLACEMENT_3D('',#184758,#89820,#89821);
#81039=AXIS2_PLACEMENT_3D('',#184759,#89822,#89823);
#81040=AXIS2_PLACEMENT_3D('',#184760,#89824,#89825);
#81041=AXIS2_PLACEMENT_3D('',#184762,#89826,#89827);
#81042=AXIS2_PLACEMENT_3D('',#184764,#89828,#89829);
#81043=AXIS2_PLACEMENT_3D('',#184765,#89830,#89831);
#81044=AXIS2_PLACEMENT_3D('',#184766,#89832,#89833);
#81045=AXIS2_PLACEMENT_3D('',#184768,#89834,#89835);
#81046=AXIS2_PLACEMENT_3D('',#184770,#89837,#89838);
#81047=AXIS2_PLACEMENT_3D('',#184772,#89839,#89840);
#81048=AXIS2_PLACEMENT_3D('',#184775,#89842,#89843);
#81049=AXIS2_PLACEMENT_3D('',#184776,#89844,#89845);
#81050=AXIS2_PLACEMENT_3D('',#184778,#89846,#89847);
#81051=AXIS2_PLACEMENT_3D('',#184781,#89849,#89850);
#81052=AXIS2_PLACEMENT_3D('',#184782,#89851,#89852);
#81053=AXIS2_PLACEMENT_3D('',#184784,#89853,#89854);
#81054=AXIS2_PLACEMENT_3D('',#184787,#89856,#89857);
#81055=AXIS2_PLACEMENT_3D('',#184788,#89858,#89859);
#81056=AXIS2_PLACEMENT_3D('',#184791,#89860,#89861);
#81057=AXIS2_PLACEMENT_3D('',#184795,#89863,#89864);
#81058=AXIS2_PLACEMENT_3D('',#184799,#89866,#89867);
#81059=AXIS2_PLACEMENT_3D('',#184803,#89869,#89870);
#81060=AXIS2_PLACEMENT_3D('',#184806,#89872,#89873);
#81061=AXIS2_PLACEMENT_3D('',#184808,#89874,#89875);
#81062=AXIS2_PLACEMENT_3D('',#184810,#89877,#89878);
#81063=AXIS2_PLACEMENT_3D('',#184869,#89879,#89880);
#81064=AXIS2_PLACEMENT_3D('',#184908,#89881,#89882);
#81065=AXIS2_PLACEMENT_3D('',#184910,#89883,#89884);
#81066=AXIS2_PLACEMENT_3D('',#184913,#89886,#89887);
#81067=AXIS2_PLACEMENT_3D('',#186585,#89890,#89891);
#81068=AXIS2_PLACEMENT_3D('',#186596,#89894,#89895);
#81069=AXIS2_PLACEMENT_3D('',#186601,#89896,#89897);
#81070=AXIS2_PLACEMENT_3D('',#186602,#89898,#89899);
#81071=AXIS2_PLACEMENT_3D('',#186607,#89900,#89901);
#81072=AXIS2_PLACEMENT_3D('',#186608,#89902,#89903);
#81073=AXIS2_PLACEMENT_3D('',#186611,#89906,#89907);
#81074=AXIS2_PLACEMENT_3D('',#186612,#89908,#89909);
#81075=AXIS2_PLACEMENT_3D('',#186613,#89910,#89911);
#81076=AXIS2_PLACEMENT_3D('',#186614,#89912,#89913);
#81077=AXIS2_PLACEMENT_3D('',#186634,#89914,#89915);
#81078=AXIS2_PLACEMENT_3D('',#186904,#89917,#89918);
#81079=AXIS2_PLACEMENT_3D('',#187074,#89919,#89920);
#81080=AXIS2_PLACEMENT_3D('',#187075,#89921,#89922);
#81081=AXIS2_PLACEMENT_3D('',#187076,#89923,#89924);
#81082=AXIS2_PLACEMENT_3D('',#187077,#89925,#89926);
#81083=AXIS2_PLACEMENT_3D('',#187080,#89927,#89928);
#81084=AXIS2_PLACEMENT_3D('',#187086,#89932,#89933);
#81085=AXIS2_PLACEMENT_3D('',#187090,#89935,#89936);
#81086=AXIS2_PLACEMENT_3D('',#187093,#89938,#89939);
#81087=AXIS2_PLACEMENT_3D('',#187094,#89940,#89941);
#81088=AXIS2_PLACEMENT_3D('',#187096,#89942,#89943);
#81089=AXIS2_PLACEMENT_3D('',#187098,#89944,#89945);
#81090=AXIS2_PLACEMENT_3D('',#187100,#89947,#89948);
#81091=AXIS2_PLACEMENT_3D('',#187101,#89949,#89950);
#81092=AXIS2_PLACEMENT_3D('',#187103,#89951,#89952);
#81093=AXIS2_PLACEMENT_3D('',#187105,#89954,#89955);
#81094=AXIS2_PLACEMENT_3D('',#187106,#89956,#89957);
#81095=AXIS2_PLACEMENT_3D('',#187107,#89958,#89959);
#81096=AXIS2_PLACEMENT_3D('',#187110,#89960,#89961);
#81097=AXIS2_PLACEMENT_3D('',#187116,#89965,#89966);
#81098=AXIS2_PLACEMENT_3D('',#187119,#89967,#89968);
#81099=AXIS2_PLACEMENT_3D('',#187122,#89970,#89971);
#81100=AXIS2_PLACEMENT_3D('',#187124,#89973,#89974);
#81101=AXIS2_PLACEMENT_3D('',#187126,#89975,#89976);
#81102=AXIS2_PLACEMENT_3D('',#187128,#89977,#89978);
#81103=AXIS2_PLACEMENT_3D('',#187130,#89980,#89981);
#81104=AXIS2_PLACEMENT_3D('',#187131,#89982,#89983);
#81105=AXIS2_PLACEMENT_3D('',#187133,#89984,#89985);
#81106=AXIS2_PLACEMENT_3D('',#187135,#89987,#89988);
#81107=AXIS2_PLACEMENT_3D('',#187136,#89989,#89990);
#81108=AXIS2_PLACEMENT_3D('',#187137,#89991,#89992);
#81109=AXIS2_PLACEMENT_3D('',#187142,#89994,#89995);
#81110=AXIS2_PLACEMENT_3D('',#187145,#89997,#89998);
#81111=AXIS2_PLACEMENT_3D('',#187146,#89999,#90000);
#81112=AXIS2_PLACEMENT_3D('',#187151,#90003,#90004);
#81113=AXIS2_PLACEMENT_3D('',#187152,#90005,#90006);
#81114=AXIS2_PLACEMENT_3D('',#187157,#90009,#90010);
#81115=AXIS2_PLACEMENT_3D('',#187158,#90011,#90012);
#81116=AXIS2_PLACEMENT_3D('',#187160,#90013,#90014);
#81117=AXIS2_PLACEMENT_3D('',#187162,#90016,#90017);
#81118=AXIS2_PLACEMENT_3D('',#187163,#90018,#90019);
#81119=AXIS2_PLACEMENT_3D('',#187164,#90020,#90021);
#81120=AXIS2_PLACEMENT_3D('',#187165,#90022,#90023);
#81121=AXIS2_PLACEMENT_3D('',#187170,#90025,#90026);
#81122=AXIS2_PLACEMENT_3D('',#187173,#90028,#90029);
#81123=AXIS2_PLACEMENT_3D('',#187174,#90030,#90031);
#81124=AXIS2_PLACEMENT_3D('',#187178,#90033,#90034);
#81125=AXIS2_PLACEMENT_3D('',#187179,#90035,#90036);
#81126=AXIS2_PLACEMENT_3D('',#187180,#90037,#90038);
#81127=AXIS2_PLACEMENT_3D('',#187184,#90040,#90041);
#81128=AXIS2_PLACEMENT_3D('',#187185,#90042,#90043);
#81129=AXIS2_PLACEMENT_3D('',#187186,#90044,#90045);
#81130=AXIS2_PLACEMENT_3D('',#187187,#90046,#90047);
#81131=AXIS2_PLACEMENT_3D('',#187188,#90048,#90049);
#81132=AXIS2_PLACEMENT_3D('',#187189,#90050,#90051);
#81133=AXIS2_PLACEMENT_3D('',#187194,#90053,#90054);
#81134=AXIS2_PLACEMENT_3D('',#187197,#90056,#90057);
#81135=AXIS2_PLACEMENT_3D('',#187198,#90058,#90059);
#81136=AXIS2_PLACEMENT_3D('',#187202,#90061,#90062);
#81137=AXIS2_PLACEMENT_3D('',#187203,#90063,#90064);
#81138=AXIS2_PLACEMENT_3D('',#187204,#90065,#90066);
#81139=AXIS2_PLACEMENT_3D('',#187208,#90068,#90069);
#81140=AXIS2_PLACEMENT_3D('',#187209,#90070,#90071);
#81141=AXIS2_PLACEMENT_3D('',#187210,#90072,#90073);
#81142=AXIS2_PLACEMENT_3D('',#187211,#90074,#90075);
#81143=AXIS2_PLACEMENT_3D('',#187212,#90076,#90077);
#81144=AXIS2_PLACEMENT_3D('',#187213,#90078,#90079);
#81145=AXIS2_PLACEMENT_3D('',#187218,#90081,#90082);
#81146=AXIS2_PLACEMENT_3D('',#187221,#90084,#90085);
#81147=AXIS2_PLACEMENT_3D('',#187222,#90086,#90087);
#81148=AXIS2_PLACEMENT_3D('',#187226,#90089,#90090);
#81149=AXIS2_PLACEMENT_3D('',#187227,#90091,#90092);
#81150=AXIS2_PLACEMENT_3D('',#187228,#90093,#90094);
#81151=AXIS2_PLACEMENT_3D('',#187232,#90096,#90097);
#81152=AXIS2_PLACEMENT_3D('',#187233,#90098,#90099);
#81153=AXIS2_PLACEMENT_3D('',#187234,#90100,#90101);
#81154=AXIS2_PLACEMENT_3D('',#187235,#90102,#90103);
#81155=AXIS2_PLACEMENT_3D('',#187236,#90104,#90105);
#81156=AXIS2_PLACEMENT_3D('',#187237,#90106,#90107);
#81157=AXIS2_PLACEMENT_3D('',#187242,#90109,#90110);
#81158=AXIS2_PLACEMENT_3D('',#187245,#90112,#90113);
#81159=AXIS2_PLACEMENT_3D('',#187246,#90114,#90115);
#81160=AXIS2_PLACEMENT_3D('',#187250,#90117,#90118);
#81161=AXIS2_PLACEMENT_3D('',#187251,#90119,#90120);
#81162=AXIS2_PLACEMENT_3D('',#187252,#90121,#90122);
#81163=AXIS2_PLACEMENT_3D('',#187256,#90124,#90125);
#81164=AXIS2_PLACEMENT_3D('',#187257,#90126,#90127);
#81165=AXIS2_PLACEMENT_3D('',#187258,#90128,#90129);
#81166=AXIS2_PLACEMENT_3D('',#187259,#90130,#90131);
#81167=AXIS2_PLACEMENT_3D('',#187260,#90132,#90133);
#81168=AXIS2_PLACEMENT_3D('',#187261,#90134,#90135);
#81169=AXIS2_PLACEMENT_3D('',#187264,#90136,#90137);
#81170=AXIS2_PLACEMENT_3D('',#187270,#90141,#90142);
#81171=AXIS2_PLACEMENT_3D('',#187273,#90143,#90144);
#81172=AXIS2_PLACEMENT_3D('',#187276,#90146,#90147);
#81173=AXIS2_PLACEMENT_3D('',#187278,#90149,#90150);
#81174=AXIS2_PLACEMENT_3D('',#187280,#90151,#90152);
#81175=AXIS2_PLACEMENT_3D('',#187282,#90153,#90154);
#81176=AXIS2_PLACEMENT_3D('',#187284,#90156,#90157);
#81177=AXIS2_PLACEMENT_3D('',#187285,#90158,#90159);
#81178=AXIS2_PLACEMENT_3D('',#187287,#90160,#90161);
#81179=AXIS2_PLACEMENT_3D('',#187289,#90163,#90164);
#81180=AXIS2_PLACEMENT_3D('',#187290,#90165,#90166);
#81181=AXIS2_PLACEMENT_3D('',#187291,#90167,#90168);
#81182=AXIS2_PLACEMENT_3D('',#187296,#90170,#90171);
#81183=AXIS2_PLACEMENT_3D('',#187299,#90173,#90174);
#81184=AXIS2_PLACEMENT_3D('',#187300,#90175,#90176);
#81185=AXIS2_PLACEMENT_3D('',#187306,#90179,#90180);
#81186=AXIS2_PLACEMENT_3D('',#187307,#90181,#90182);
#81187=AXIS2_PLACEMENT_3D('',#187308,#90183,#90184);
#81188=AXIS2_PLACEMENT_3D('',#187313,#90187,#90188);
#81189=AXIS2_PLACEMENT_3D('',#187314,#90189,#90190);
#81190=AXIS2_PLACEMENT_3D('',#187316,#90191,#90192);
#81191=AXIS2_PLACEMENT_3D('',#187318,#90194,#90195);
#81192=AXIS2_PLACEMENT_3D('',#187319,#90196,#90197);
#81193=AXIS2_PLACEMENT_3D('',#187320,#90198,#90199);
#81194=AXIS2_PLACEMENT_3D('',#187321,#90200,#90201);
#81195=AXIS2_PLACEMENT_3D('',#187326,#90203,#90204);
#81196=AXIS2_PLACEMENT_3D('',#187329,#90206,#90207);
#81197=AXIS2_PLACEMENT_3D('',#187330,#90208,#90209);
#81198=AXIS2_PLACEMENT_3D('',#187336,#90212,#90213);
#81199=AXIS2_PLACEMENT_3D('',#187337,#90214,#90215);
#81200=AXIS2_PLACEMENT_3D('',#187338,#90216,#90217);
#81201=AXIS2_PLACEMENT_3D('',#187343,#90220,#90221);
#81202=AXIS2_PLACEMENT_3D('',#187344,#90222,#90223);
#81203=AXIS2_PLACEMENT_3D('',#187346,#90224,#90225);
#81204=AXIS2_PLACEMENT_3D('',#187348,#90227,#90228);
#81205=AXIS2_PLACEMENT_3D('',#187349,#90229,#90230);
#81206=AXIS2_PLACEMENT_3D('',#187350,#90231,#90232);
#81207=AXIS2_PLACEMENT_3D('',#187351,#90233,#90234);
#81208=AXIS2_PLACEMENT_3D('',#187356,#90236,#90237);
#81209=AXIS2_PLACEMENT_3D('',#187359,#90239,#90240);
#81210=AXIS2_PLACEMENT_3D('',#187360,#90241,#90242);
#81211=AXIS2_PLACEMENT_3D('',#187364,#90244,#90245);
#81212=AXIS2_PLACEMENT_3D('',#187365,#90246,#90247);
#81213=AXIS2_PLACEMENT_3D('',#187366,#90248,#90249);
#81214=AXIS2_PLACEMENT_3D('',#187372,#90252,#90253);
#81215=AXIS2_PLACEMENT_3D('',#187373,#90254,#90255);
#81216=AXIS2_PLACEMENT_3D('',#187374,#90256,#90257);
#81217=AXIS2_PLACEMENT_3D('',#187376,#90258,#90259);
#81218=AXIS2_PLACEMENT_3D('',#187378,#90261,#90262);
#81219=AXIS2_PLACEMENT_3D('',#187379,#90263,#90264);
#81220=AXIS2_PLACEMENT_3D('',#187380,#90265,#90266);
#81221=AXIS2_PLACEMENT_3D('',#187381,#90267,#90268);
#81222=AXIS2_PLACEMENT_3D('',#187386,#90270,#90271);
#81223=AXIS2_PLACEMENT_3D('',#187389,#90273,#90274);
#81224=AXIS2_PLACEMENT_3D('',#187390,#90275,#90276);
#81225=AXIS2_PLACEMENT_3D('',#187394,#90278,#90279);
#81226=AXIS2_PLACEMENT_3D('',#187395,#90280,#90281);
#81227=AXIS2_PLACEMENT_3D('',#187396,#90282,#90283);
#81228=AXIS2_PLACEMENT_3D('',#187400,#90285,#90286);
#81229=AXIS2_PLACEMENT_3D('',#187401,#90287,#90288);
#81230=AXIS2_PLACEMENT_3D('',#187402,#90289,#90290);
#81231=AXIS2_PLACEMENT_3D('',#187403,#90291,#90292);
#81232=AXIS2_PLACEMENT_3D('',#187404,#90293,#90294);
#81233=AXIS2_PLACEMENT_3D('',#187405,#90295,#90296);
#81234=AXIS2_PLACEMENT_3D('',#187410,#90298,#90299);
#81235=AXIS2_PLACEMENT_3D('',#187413,#90301,#90302);
#81236=AXIS2_PLACEMENT_3D('',#187414,#90303,#90304);
#81237=AXIS2_PLACEMENT_3D('',#187420,#90307,#90308);
#81238=AXIS2_PLACEMENT_3D('',#187421,#90309,#90310);
#81239=AXIS2_PLACEMENT_3D('',#187422,#90311,#90312);
#81240=AXIS2_PLACEMENT_3D('',#187427,#90315,#90316);
#81241=AXIS2_PLACEMENT_3D('',#187428,#90317,#90318);
#81242=AXIS2_PLACEMENT_3D('',#187430,#90319,#90320);
#81243=AXIS2_PLACEMENT_3D('',#187432,#90322,#90323);
#81244=AXIS2_PLACEMENT_3D('',#187433,#90324,#90325);
#81245=AXIS2_PLACEMENT_3D('',#187434,#90326,#90327);
#81246=AXIS2_PLACEMENT_3D('',#187435,#90328,#90329);
#81247=AXIS2_PLACEMENT_3D('',#187440,#90331,#90332);
#81248=AXIS2_PLACEMENT_3D('',#187443,#90334,#90335);
#81249=AXIS2_PLACEMENT_3D('',#187444,#90336,#90337);
#81250=AXIS2_PLACEMENT_3D('',#187450,#90340,#90341);
#81251=AXIS2_PLACEMENT_3D('',#187451,#90342,#90343);
#81252=AXIS2_PLACEMENT_3D('',#187452,#90344,#90345);
#81253=AXIS2_PLACEMENT_3D('',#187457,#90348,#90349);
#81254=AXIS2_PLACEMENT_3D('',#187458,#90350,#90351);
#81255=AXIS2_PLACEMENT_3D('',#187460,#90352,#90353);
#81256=AXIS2_PLACEMENT_3D('',#187462,#90355,#90356);
#81257=AXIS2_PLACEMENT_3D('',#187463,#90357,#90358);
#81258=AXIS2_PLACEMENT_3D('',#187464,#90359,#90360);
#81259=AXIS2_PLACEMENT_3D('',#187465,#90361,#90362);
#81260=AXIS2_PLACEMENT_3D('',#187470,#90364,#90365);
#81261=AXIS2_PLACEMENT_3D('',#187473,#90367,#90368);
#81262=AXIS2_PLACEMENT_3D('',#187474,#90369,#90370);
#81263=AXIS2_PLACEMENT_3D('',#187480,#90373,#90374);
#81264=AXIS2_PLACEMENT_3D('',#187481,#90375,#90376);
#81265=AXIS2_PLACEMENT_3D('',#187482,#90377,#90378);
#81266=AXIS2_PLACEMENT_3D('',#187487,#90381,#90382);
#81267=AXIS2_PLACEMENT_3D('',#187488,#90383,#90384);
#81268=AXIS2_PLACEMENT_3D('',#187490,#90385,#90386);
#81269=AXIS2_PLACEMENT_3D('',#187492,#90388,#90389);
#81270=AXIS2_PLACEMENT_3D('',#187493,#90390,#90391);
#81271=AXIS2_PLACEMENT_3D('',#187494,#90392,#90393);
#81272=AXIS2_PLACEMENT_3D('',#187495,#90394,#90395);
#81273=AXIS2_PLACEMENT_3D('',#187500,#90397,#90398);
#81274=AXIS2_PLACEMENT_3D('',#187503,#90400,#90401);
#81275=AXIS2_PLACEMENT_3D('',#187504,#90402,#90403);
#81276=AXIS2_PLACEMENT_3D('',#187510,#90406,#90407);
#81277=AXIS2_PLACEMENT_3D('',#187511,#90408,#90409);
#81278=AXIS2_PLACEMENT_3D('',#187512,#90410,#90411);
#81279=AXIS2_PLACEMENT_3D('',#187517,#90414,#90415);
#81280=AXIS2_PLACEMENT_3D('',#187518,#90416,#90417);
#81281=AXIS2_PLACEMENT_3D('',#187520,#90418,#90419);
#81282=AXIS2_PLACEMENT_3D('',#187522,#90421,#90422);
#81283=AXIS2_PLACEMENT_3D('',#187523,#90423,#90424);
#81284=AXIS2_PLACEMENT_3D('',#187524,#90425,#90426);
#81285=AXIS2_PLACEMENT_3D('',#187525,#90427,#90428);
#81286=AXIS2_PLACEMENT_3D('',#187530,#90430,#90431);
#81287=AXIS2_PLACEMENT_3D('',#187533,#90433,#90434);
#81288=AXIS2_PLACEMENT_3D('',#187534,#90435,#90436);
#81289=AXIS2_PLACEMENT_3D('',#187538,#90438,#90439);
#81290=AXIS2_PLACEMENT_3D('',#187539,#90440,#90441);
#81291=AXIS2_PLACEMENT_3D('',#187540,#90442,#90443);
#81292=AXIS2_PLACEMENT_3D('',#187544,#90445,#90446);
#81293=AXIS2_PLACEMENT_3D('',#187545,#90447,#90448);
#81294=AXIS2_PLACEMENT_3D('',#187546,#90449,#90450);
#81295=AXIS2_PLACEMENT_3D('',#187547,#90451,#90452);
#81296=AXIS2_PLACEMENT_3D('',#187548,#90453,#90454);
#81297=AXIS2_PLACEMENT_3D('',#187549,#90455,#90456);
#81298=AXIS2_PLACEMENT_3D('',#187554,#90458,#90459);
#81299=AXIS2_PLACEMENT_3D('',#187557,#90461,#90462);
#81300=AXIS2_PLACEMENT_3D('',#187558,#90463,#90464);
#81301=AXIS2_PLACEMENT_3D('',#187562,#90466,#90467);
#81302=AXIS2_PLACEMENT_3D('',#187563,#90468,#90469);
#81303=AXIS2_PLACEMENT_3D('',#187564,#90470,#90471);
#81304=AXIS2_PLACEMENT_3D('',#187568,#90473,#90474);
#81305=AXIS2_PLACEMENT_3D('',#187569,#90475,#90476);
#81306=AXIS2_PLACEMENT_3D('',#187570,#90477,#90478);
#81307=AXIS2_PLACEMENT_3D('',#187571,#90479,#90480);
#81308=AXIS2_PLACEMENT_3D('',#187572,#90481,#90482);
#81309=AXIS2_PLACEMENT_3D('',#187573,#90483,#90484);
#81310=AXIS2_PLACEMENT_3D('',#187578,#90486,#90487);
#81311=AXIS2_PLACEMENT_3D('',#187581,#90489,#90490);
#81312=AXIS2_PLACEMENT_3D('',#187582,#90491,#90492);
#81313=AXIS2_PLACEMENT_3D('',#187586,#90494,#90495);
#81314=AXIS2_PLACEMENT_3D('',#187587,#90496,#90497);
#81315=AXIS2_PLACEMENT_3D('',#187588,#90498,#90499);
#81316=AXIS2_PLACEMENT_3D('',#187592,#90501,#90502);
#81317=AXIS2_PLACEMENT_3D('',#187593,#90503,#90504);
#81318=AXIS2_PLACEMENT_3D('',#187594,#90505,#90506);
#81319=AXIS2_PLACEMENT_3D('',#187595,#90507,#90508);
#81320=AXIS2_PLACEMENT_3D('',#187596,#90509,#90510);
#81321=AXIS2_PLACEMENT_3D('',#187597,#90511,#90512);
#81322=AXIS2_PLACEMENT_3D('',#187602,#90514,#90515);
#81323=AXIS2_PLACEMENT_3D('',#187605,#90517,#90518);
#81324=AXIS2_PLACEMENT_3D('',#187606,#90519,#90520);
#81325=AXIS2_PLACEMENT_3D('',#187610,#90522,#90523);
#81326=AXIS2_PLACEMENT_3D('',#187611,#90524,#90525);
#81327=AXIS2_PLACEMENT_3D('',#187612,#90526,#90527);
#81328=AXIS2_PLACEMENT_3D('',#187616,#90529,#90530);
#81329=AXIS2_PLACEMENT_3D('',#187617,#90531,#90532);
#81330=AXIS2_PLACEMENT_3D('',#187618,#90533,#90534);
#81331=AXIS2_PLACEMENT_3D('',#187619,#90535,#90536);
#81332=AXIS2_PLACEMENT_3D('',#187620,#90537,#90538);
#81333=AXIS2_PLACEMENT_3D('',#187621,#90539,#90540);
#81334=AXIS2_PLACEMENT_3D('',#187626,#90542,#90543);
#81335=AXIS2_PLACEMENT_3D('',#187629,#90545,#90546);
#81336=AXIS2_PLACEMENT_3D('',#187630,#90547,#90548);
#81337=AXIS2_PLACEMENT_3D('',#187634,#90550,#90551);
#81338=AXIS2_PLACEMENT_3D('',#187635,#90552,#90553);
#81339=AXIS2_PLACEMENT_3D('',#187636,#90554,#90555);
#81340=AXIS2_PLACEMENT_3D('',#187640,#90557,#90558);
#81341=AXIS2_PLACEMENT_3D('',#187641,#90559,#90560);
#81342=AXIS2_PLACEMENT_3D('',#187642,#90561,#90562);
#81343=AXIS2_PLACEMENT_3D('',#187643,#90563,#90564);
#81344=AXIS2_PLACEMENT_3D('',#187644,#90565,#90566);
#81345=AXIS2_PLACEMENT_3D('',#187645,#90567,#90568);
#81346=AXIS2_PLACEMENT_3D('',#187650,#90570,#90571);
#81347=AXIS2_PLACEMENT_3D('',#187653,#90573,#90574);
#81348=AXIS2_PLACEMENT_3D('',#187654,#90575,#90576);
#81349=AXIS2_PLACEMENT_3D('',#187658,#90578,#90579);
#81350=AXIS2_PLACEMENT_3D('',#187659,#90580,#90581);
#81351=AXIS2_PLACEMENT_3D('',#187660,#90582,#90583);
#81352=AXIS2_PLACEMENT_3D('',#187664,#90585,#90586);
#81353=AXIS2_PLACEMENT_3D('',#187665,#90587,#90588);
#81354=AXIS2_PLACEMENT_3D('',#187666,#90589,#90590);
#81355=AXIS2_PLACEMENT_3D('',#187667,#90591,#90592);
#81356=AXIS2_PLACEMENT_3D('',#187668,#90593,#90594);
#81357=AXIS2_PLACEMENT_3D('',#187669,#90595,#90596);
#81358=AXIS2_PLACEMENT_3D('',#187672,#90597,#90598);
#81359=AXIS2_PLACEMENT_3D('',#187676,#90600,#90601);
#81360=AXIS2_PLACEMENT_3D('',#187678,#90603,#90604);
#81361=AXIS2_PLACEMENT_3D('',#187680,#90605,#90606);
#81362=AXIS2_PLACEMENT_3D('',#187683,#90608,#90609);
#81363=AXIS2_PLACEMENT_3D('',#187684,#90610,#90611);
#81364=AXIS2_PLACEMENT_3D('',#187688,#90613,#90614);
#81365=AXIS2_PLACEMENT_3D('',#187690,#90615,#90616);
#81366=AXIS2_PLACEMENT_3D('',#187692,#90618,#90619);
#81367=AXIS2_PLACEMENT_3D('',#187693,#90620,#90621);
#81368=AXIS2_PLACEMENT_3D('',#187695,#90622,#90623);
#81369=AXIS2_PLACEMENT_3D('',#187697,#90625,#90626);
#81370=AXIS2_PLACEMENT_3D('',#187698,#90627,#90628);
#81371=AXIS2_PLACEMENT_3D('',#187699,#90629,#90630);
#81372=AXIS2_PLACEMENT_3D('',#187704,#90632,#90633);
#81373=AXIS2_PLACEMENT_3D('',#187707,#90635,#90636);
#81374=AXIS2_PLACEMENT_3D('',#187708,#90637,#90638);
#81375=AXIS2_PLACEMENT_3D('',#187714,#90641,#90642);
#81376=AXIS2_PLACEMENT_3D('',#187715,#90643,#90644);
#81377=AXIS2_PLACEMENT_3D('',#187716,#90645,#90646);
#81378=AXIS2_PLACEMENT_3D('',#187721,#90649,#90650);
#81379=AXIS2_PLACEMENT_3D('',#187722,#90651,#90652);
#81380=AXIS2_PLACEMENT_3D('',#187724,#90653,#90654);
#81381=AXIS2_PLACEMENT_3D('',#187726,#90656,#90657);
#81382=AXIS2_PLACEMENT_3D('',#187727,#90658,#90659);
#81383=AXIS2_PLACEMENT_3D('',#187728,#90660,#90661);
#81384=AXIS2_PLACEMENT_3D('',#187729,#90662,#90663);
#81385=AXIS2_PLACEMENT_3D('',#187734,#90665,#90666);
#81386=AXIS2_PLACEMENT_3D('',#187737,#90668,#90669);
#81387=AXIS2_PLACEMENT_3D('',#187738,#90670,#90671);
#81388=AXIS2_PLACEMENT_3D('',#187742,#90673,#90674);
#81389=AXIS2_PLACEMENT_3D('',#187743,#90675,#90676);
#81390=AXIS2_PLACEMENT_3D('',#187744,#90677,#90678);
#81391=AXIS2_PLACEMENT_3D('',#187748,#90680,#90681);
#81392=AXIS2_PLACEMENT_3D('',#187749,#90682,#90683);
#81393=AXIS2_PLACEMENT_3D('',#187750,#90684,#90685);
#81394=AXIS2_PLACEMENT_3D('',#187751,#90686,#90687);
#81395=AXIS2_PLACEMENT_3D('',#187752,#90688,#90689);
#81396=AXIS2_PLACEMENT_3D('',#187753,#90690,#90691);
#81397=AXIS2_PLACEMENT_3D('',#187758,#90693,#90694);
#81398=AXIS2_PLACEMENT_3D('',#187761,#90696,#90697);
#81399=AXIS2_PLACEMENT_3D('',#187762,#90698,#90699);
#81400=AXIS2_PLACEMENT_3D('',#187766,#90701,#90702);
#81401=AXIS2_PLACEMENT_3D('',#187767,#90703,#90704);
#81402=AXIS2_PLACEMENT_3D('',#187768,#90705,#90706);
#81403=AXIS2_PLACEMENT_3D('',#187772,#90708,#90709);
#81404=AXIS2_PLACEMENT_3D('',#187773,#90710,#90711);
#81405=AXIS2_PLACEMENT_3D('',#187774,#90712,#90713);
#81406=AXIS2_PLACEMENT_3D('',#187775,#90714,#90715);
#81407=AXIS2_PLACEMENT_3D('',#187776,#90716,#90717);
#81408=AXIS2_PLACEMENT_3D('',#187777,#90718,#90719);
#81409=AXIS2_PLACEMENT_3D('',#187782,#90721,#90722);
#81410=AXIS2_PLACEMENT_3D('',#187785,#90724,#90725);
#81411=AXIS2_PLACEMENT_3D('',#187786,#90726,#90727);
#81412=AXIS2_PLACEMENT_3D('',#187790,#90729,#90730);
#81413=AXIS2_PLACEMENT_3D('',#187791,#90731,#90732);
#81414=AXIS2_PLACEMENT_3D('',#187792,#90733,#90734);
#81415=AXIS2_PLACEMENT_3D('',#187796,#90736,#90737);
#81416=AXIS2_PLACEMENT_3D('',#187797,#90738,#90739);
#81417=AXIS2_PLACEMENT_3D('',#187798,#90740,#90741);
#81418=AXIS2_PLACEMENT_3D('',#187799,#90742,#90743);
#81419=AXIS2_PLACEMENT_3D('',#187800,#90744,#90745);
#81420=AXIS2_PLACEMENT_3D('',#187801,#90746,#90747);
#81421=AXIS2_PLACEMENT_3D('',#187806,#90749,#90750);
#81422=AXIS2_PLACEMENT_3D('',#187809,#90752,#90753);
#81423=AXIS2_PLACEMENT_3D('',#187810,#90754,#90755);
#81424=AXIS2_PLACEMENT_3D('',#187814,#90757,#90758);
#81425=AXIS2_PLACEMENT_3D('',#187815,#90759,#90760);
#81426=AXIS2_PLACEMENT_3D('',#187816,#90761,#90762);
#81427=AXIS2_PLACEMENT_3D('',#187820,#90764,#90765);
#81428=AXIS2_PLACEMENT_3D('',#187821,#90766,#90767);
#81429=AXIS2_PLACEMENT_3D('',#187822,#90768,#90769);
#81430=AXIS2_PLACEMENT_3D('',#187823,#90770,#90771);
#81431=AXIS2_PLACEMENT_3D('',#187824,#90772,#90773);
#81432=AXIS2_PLACEMENT_3D('',#187825,#90774,#90775);
#81433=AXIS2_PLACEMENT_3D('',#187830,#90777,#90778);
#81434=AXIS2_PLACEMENT_3D('',#187833,#90780,#90781);
#81435=AXIS2_PLACEMENT_3D('',#187834,#90782,#90783);
#81436=AXIS2_PLACEMENT_3D('',#187838,#90785,#90786);
#81437=AXIS2_PLACEMENT_3D('',#187839,#90787,#90788);
#81438=AXIS2_PLACEMENT_3D('',#187840,#90789,#90790);
#81439=AXIS2_PLACEMENT_3D('',#187844,#90792,#90793);
#81440=AXIS2_PLACEMENT_3D('',#187845,#90794,#90795);
#81441=AXIS2_PLACEMENT_3D('',#187846,#90796,#90797);
#81442=AXIS2_PLACEMENT_3D('',#187847,#90798,#90799);
#81443=AXIS2_PLACEMENT_3D('',#187848,#90800,#90801);
#81444=AXIS2_PLACEMENT_3D('',#187849,#90802,#90803);
#81445=AXIS2_PLACEMENT_3D('',#187854,#90805,#90806);
#81446=AXIS2_PLACEMENT_3D('',#187857,#90808,#90809);
#81447=AXIS2_PLACEMENT_3D('',#187858,#90810,#90811);
#81448=AXIS2_PLACEMENT_3D('',#187862,#90813,#90814);
#81449=AXIS2_PLACEMENT_3D('',#187863,#90815,#90816);
#81450=AXIS2_PLACEMENT_3D('',#187864,#90817,#90818);
#81451=AXIS2_PLACEMENT_3D('',#187868,#90820,#90821);
#81452=AXIS2_PLACEMENT_3D('',#187869,#90822,#90823);
#81453=AXIS2_PLACEMENT_3D('',#187870,#90824,#90825);
#81454=AXIS2_PLACEMENT_3D('',#187871,#90826,#90827);
#81455=AXIS2_PLACEMENT_3D('',#187872,#90828,#90829);
#81456=AXIS2_PLACEMENT_3D('',#187873,#90830,#90831);
#81457=AXIS2_PLACEMENT_3D('',#187878,#90833,#90834);
#81458=AXIS2_PLACEMENT_3D('',#187881,#90836,#90837);
#81459=AXIS2_PLACEMENT_3D('',#187882,#90838,#90839);
#81460=AXIS2_PLACEMENT_3D('',#187886,#90841,#90842);
#81461=AXIS2_PLACEMENT_3D('',#187887,#90843,#90844);
#81462=AXIS2_PLACEMENT_3D('',#187888,#90845,#90846);
#81463=AXIS2_PLACEMENT_3D('',#187892,#90848,#90849);
#81464=AXIS2_PLACEMENT_3D('',#187893,#90850,#90851);
#81465=AXIS2_PLACEMENT_3D('',#187894,#90852,#90853);
#81466=AXIS2_PLACEMENT_3D('',#187895,#90854,#90855);
#81467=AXIS2_PLACEMENT_3D('',#187896,#90856,#90857);
#81468=AXIS2_PLACEMENT_3D('',#187897,#90858,#90859);
#81469=AXIS2_PLACEMENT_3D('',#187902,#90861,#90862);
#81470=AXIS2_PLACEMENT_3D('',#187905,#90864,#90865);
#81471=AXIS2_PLACEMENT_3D('',#187906,#90866,#90867);
#81472=AXIS2_PLACEMENT_3D('',#187910,#90869,#90870);
#81473=AXIS2_PLACEMENT_3D('',#187911,#90871,#90872);
#81474=AXIS2_PLACEMENT_3D('',#187912,#90873,#90874);
#81475=AXIS2_PLACEMENT_3D('',#187916,#90876,#90877);
#81476=AXIS2_PLACEMENT_3D('',#187917,#90878,#90879);
#81477=AXIS2_PLACEMENT_3D('',#187918,#90880,#90881);
#81478=AXIS2_PLACEMENT_3D('',#187919,#90882,#90883);
#81479=AXIS2_PLACEMENT_3D('',#187920,#90884,#90885);
#81480=AXIS2_PLACEMENT_3D('',#187921,#90886,#90887);
#81481=AXIS2_PLACEMENT_3D('',#187926,#90889,#90890);
#81482=AXIS2_PLACEMENT_3D('',#187929,#90892,#90893);
#81483=AXIS2_PLACEMENT_3D('',#187930,#90894,#90895);
#81484=AXIS2_PLACEMENT_3D('',#187936,#90898,#90899);
#81485=AXIS2_PLACEMENT_3D('',#187937,#90900,#90901);
#81486=AXIS2_PLACEMENT_3D('',#187938,#90902,#90903);
#81487=AXIS2_PLACEMENT_3D('',#187943,#90906,#90907);
#81488=AXIS2_PLACEMENT_3D('',#187944,#90908,#90909);
#81489=AXIS2_PLACEMENT_3D('',#187946,#90910,#90911);
#81490=AXIS2_PLACEMENT_3D('',#187948,#90913,#90914);
#81491=AXIS2_PLACEMENT_3D('',#187949,#90915,#90916);
#81492=AXIS2_PLACEMENT_3D('',#187950,#90917,#90918);
#81493=AXIS2_PLACEMENT_3D('',#187951,#90919,#90920);
#81494=AXIS2_PLACEMENT_3D('',#187956,#90922,#90923);
#81495=AXIS2_PLACEMENT_3D('',#187959,#90925,#90926);
#81496=AXIS2_PLACEMENT_3D('',#187960,#90927,#90928);
#81497=AXIS2_PLACEMENT_3D('',#187966,#90931,#90932);
#81498=AXIS2_PLACEMENT_3D('',#187967,#90933,#90934);
#81499=AXIS2_PLACEMENT_3D('',#187968,#90935,#90936);
#81500=AXIS2_PLACEMENT_3D('',#187973,#90939,#90940);
#81501=AXIS2_PLACEMENT_3D('',#187974,#90941,#90942);
#81502=AXIS2_PLACEMENT_3D('',#187976,#90943,#90944);
#81503=AXIS2_PLACEMENT_3D('',#187978,#90946,#90947);
#81504=AXIS2_PLACEMENT_3D('',#187979,#90948,#90949);
#81505=AXIS2_PLACEMENT_3D('',#187980,#90950,#90951);
#81506=AXIS2_PLACEMENT_3D('',#187981,#90952,#90953);
#81507=AXIS2_PLACEMENT_3D('',#187986,#90955,#90956);
#81508=AXIS2_PLACEMENT_3D('',#187989,#90958,#90959);
#81509=AXIS2_PLACEMENT_3D('',#187990,#90960,#90961);
#81510=AXIS2_PLACEMENT_3D('',#187994,#90963,#90964);
#81511=AXIS2_PLACEMENT_3D('',#187995,#90965,#90966);
#81512=AXIS2_PLACEMENT_3D('',#187996,#90967,#90968);
#81513=AXIS2_PLACEMENT_3D('',#188000,#90970,#90971);
#81514=AXIS2_PLACEMENT_3D('',#188001,#90972,#90973);
#81515=AXIS2_PLACEMENT_3D('',#188002,#90974,#90975);
#81516=AXIS2_PLACEMENT_3D('',#188003,#90976,#90977);
#81517=AXIS2_PLACEMENT_3D('',#188004,#90978,#90979);
#81518=AXIS2_PLACEMENT_3D('',#188005,#90980,#90981);
#81519=AXIS2_PLACEMENT_3D('',#188010,#90983,#90984);
#81520=AXIS2_PLACEMENT_3D('',#188013,#90986,#90987);
#81521=AXIS2_PLACEMENT_3D('',#188014,#90988,#90989);
#81522=AXIS2_PLACEMENT_3D('',#188018,#90991,#90992);
#81523=AXIS2_PLACEMENT_3D('',#188019,#90993,#90994);
#81524=AXIS2_PLACEMENT_3D('',#188020,#90995,#90996);
#81525=AXIS2_PLACEMENT_3D('',#188024,#90998,#90999);
#81526=AXIS2_PLACEMENT_3D('',#188025,#91000,#91001);
#81527=AXIS2_PLACEMENT_3D('',#188026,#91002,#91003);
#81528=AXIS2_PLACEMENT_3D('',#188027,#91004,#91005);
#81529=AXIS2_PLACEMENT_3D('',#188028,#91006,#91007);
#81530=AXIS2_PLACEMENT_3D('',#188029,#91008,#91009);
#81531=AXIS2_PLACEMENT_3D('',#188034,#91011,#91012);
#81532=AXIS2_PLACEMENT_3D('',#188037,#91014,#91015);
#81533=AXIS2_PLACEMENT_3D('',#188038,#91016,#91017);
#81534=AXIS2_PLACEMENT_3D('',#188042,#91019,#91020);
#81535=AXIS2_PLACEMENT_3D('',#188043,#91021,#91022);
#81536=AXIS2_PLACEMENT_3D('',#188044,#91023,#91024);
#81537=AXIS2_PLACEMENT_3D('',#188048,#91026,#91027);
#81538=AXIS2_PLACEMENT_3D('',#188049,#91028,#91029);
#81539=AXIS2_PLACEMENT_3D('',#188050,#91030,#91031);
#81540=AXIS2_PLACEMENT_3D('',#188051,#91032,#91033);
#81541=AXIS2_PLACEMENT_3D('',#188052,#91034,#91035);
#81542=AXIS2_PLACEMENT_3D('',#188053,#91036,#91037);
#81543=AXIS2_PLACEMENT_3D('',#188058,#91039,#91040);
#81544=AXIS2_PLACEMENT_3D('',#188061,#91042,#91043);
#81545=AXIS2_PLACEMENT_3D('',#188062,#91044,#91045);
#81546=AXIS2_PLACEMENT_3D('',#188066,#91047,#91048);
#81547=AXIS2_PLACEMENT_3D('',#188067,#91049,#91050);
#81548=AXIS2_PLACEMENT_3D('',#188068,#91051,#91052);
#81549=AXIS2_PLACEMENT_3D('',#188072,#91054,#91055);
#81550=AXIS2_PLACEMENT_3D('',#188073,#91056,#91057);
#81551=AXIS2_PLACEMENT_3D('',#188074,#91058,#91059);
#81552=AXIS2_PLACEMENT_3D('',#188075,#91060,#91061);
#81553=AXIS2_PLACEMENT_3D('',#188076,#91062,#91063);
#81554=AXIS2_PLACEMENT_3D('',#188077,#91064,#91065);
#81555=AXIS2_PLACEMENT_3D('',#188082,#91067,#91068);
#81556=AXIS2_PLACEMENT_3D('',#188085,#91070,#91071);
#81557=AXIS2_PLACEMENT_3D('',#188086,#91072,#91073);
#81558=AXIS2_PLACEMENT_3D('',#188090,#91075,#91076);
#81559=AXIS2_PLACEMENT_3D('',#188091,#91077,#91078);
#81560=AXIS2_PLACEMENT_3D('',#188092,#91079,#91080);
#81561=AXIS2_PLACEMENT_3D('',#188096,#91082,#91083);
#81562=AXIS2_PLACEMENT_3D('',#188097,#91084,#91085);
#81563=AXIS2_PLACEMENT_3D('',#188098,#91086,#91087);
#81564=AXIS2_PLACEMENT_3D('',#188099,#91088,#91089);
#81565=AXIS2_PLACEMENT_3D('',#188100,#91090,#91091);
#81566=AXIS2_PLACEMENT_3D('',#188101,#91092,#91093);
#81567=AXIS2_PLACEMENT_3D('',#188106,#91095,#91096);
#81568=AXIS2_PLACEMENT_3D('',#188109,#91098,#91099);
#81569=AXIS2_PLACEMENT_3D('',#188110,#91100,#91101);
#81570=AXIS2_PLACEMENT_3D('',#188114,#91103,#91104);
#81571=AXIS2_PLACEMENT_3D('',#188115,#91105,#91106);
#81572=AXIS2_PLACEMENT_3D('',#188116,#91107,#91108);
#81573=AXIS2_PLACEMENT_3D('',#188120,#91110,#91111);
#81574=AXIS2_PLACEMENT_3D('',#188121,#91112,#91113);
#81575=AXIS2_PLACEMENT_3D('',#188122,#91114,#91115);
#81576=AXIS2_PLACEMENT_3D('',#188123,#91116,#91117);
#81577=AXIS2_PLACEMENT_3D('',#188124,#91118,#91119);
#81578=AXIS2_PLACEMENT_3D('',#188125,#91120,#91121);
#81579=AXIS2_PLACEMENT_3D('',#188130,#91123,#91124);
#81580=AXIS2_PLACEMENT_3D('',#188133,#91126,#91127);
#81581=AXIS2_PLACEMENT_3D('',#188134,#91128,#91129);
#81582=AXIS2_PLACEMENT_3D('',#188138,#91131,#91132);
#81583=AXIS2_PLACEMENT_3D('',#188139,#91133,#91134);
#81584=AXIS2_PLACEMENT_3D('',#188140,#91135,#91136);
#81585=AXIS2_PLACEMENT_3D('',#188144,#91138,#91139);
#81586=AXIS2_PLACEMENT_3D('',#188145,#91140,#91141);
#81587=AXIS2_PLACEMENT_3D('',#188146,#91142,#91143);
#81588=AXIS2_PLACEMENT_3D('',#188147,#91144,#91145);
#81589=AXIS2_PLACEMENT_3D('',#188148,#91146,#91147);
#81590=AXIS2_PLACEMENT_3D('',#188149,#91148,#91149);
#81591=AXIS2_PLACEMENT_3D('',#188154,#91151,#91152);
#81592=AXIS2_PLACEMENT_3D('',#188157,#91154,#91155);
#81593=AXIS2_PLACEMENT_3D('',#188158,#91156,#91157);
#81594=AXIS2_PLACEMENT_3D('',#188162,#91159,#91160);
#81595=AXIS2_PLACEMENT_3D('',#188163,#91161,#91162);
#81596=AXIS2_PLACEMENT_3D('',#188164,#91163,#91164);
#81597=AXIS2_PLACEMENT_3D('',#188168,#91166,#91167);
#81598=AXIS2_PLACEMENT_3D('',#188169,#91168,#91169);
#81599=AXIS2_PLACEMENT_3D('',#188170,#91170,#91171);
#81600=AXIS2_PLACEMENT_3D('',#188171,#91172,#91173);
#81601=AXIS2_PLACEMENT_3D('',#188172,#91174,#91175);
#81602=AXIS2_PLACEMENT_3D('',#188173,#91176,#91177);
#81603=AXIS2_PLACEMENT_3D('',#188178,#91179,#91180);
#81604=AXIS2_PLACEMENT_3D('',#188181,#91182,#91183);
#81605=AXIS2_PLACEMENT_3D('',#188182,#91184,#91185);
#81606=AXIS2_PLACEMENT_3D('',#188186,#91187,#91188);
#81607=AXIS2_PLACEMENT_3D('',#188187,#91189,#91190);
#81608=AXIS2_PLACEMENT_3D('',#188188,#91191,#91192);
#81609=AXIS2_PLACEMENT_3D('',#188192,#91194,#91195);
#81610=AXIS2_PLACEMENT_3D('',#188193,#91196,#91197);
#81611=AXIS2_PLACEMENT_3D('',#188194,#91198,#91199);
#81612=AXIS2_PLACEMENT_3D('',#188195,#91200,#91201);
#81613=AXIS2_PLACEMENT_3D('',#188196,#91202,#91203);
#81614=AXIS2_PLACEMENT_3D('',#188197,#91204,#91205);
#81615=AXIS2_PLACEMENT_3D('',#188202,#91207,#91208);
#81616=AXIS2_PLACEMENT_3D('',#188205,#91210,#91211);
#81617=AXIS2_PLACEMENT_3D('',#188206,#91212,#91213);
#81618=AXIS2_PLACEMENT_3D('',#188210,#91215,#91216);
#81619=AXIS2_PLACEMENT_3D('',#188211,#91217,#91218);
#81620=AXIS2_PLACEMENT_3D('',#188212,#91219,#91220);
#81621=AXIS2_PLACEMENT_3D('',#188216,#91222,#91223);
#81622=AXIS2_PLACEMENT_3D('',#188217,#91224,#91225);
#81623=AXIS2_PLACEMENT_3D('',#188218,#91226,#91227);
#81624=AXIS2_PLACEMENT_3D('',#188219,#91228,#91229);
#81625=AXIS2_PLACEMENT_3D('',#188220,#91230,#91231);
#81626=AXIS2_PLACEMENT_3D('',#188221,#91232,#91233);
#81627=AXIS2_PLACEMENT_3D('',#188227,#91236,#91237);
#81628=AXIS2_PLACEMENT_3D('',#188228,#91238,#91239);
#81629=AXIS2_PLACEMENT_3D('',#188233,#91241,#91242);
#81630=AXIS2_PLACEMENT_3D('',#188236,#91244,#91245);
#81631=AXIS2_PLACEMENT_3D('',#188237,#91246,#91247);
#81632=AXIS2_PLACEMENT_3D('',#188241,#91249,#91250);
#81633=AXIS2_PLACEMENT_3D('',#188242,#91251,#91252);
#81634=AXIS2_PLACEMENT_3D('',#188243,#91253,#91254);
#81635=AXIS2_PLACEMENT_3D('',#188246,#91256,#91257);
#81636=AXIS2_PLACEMENT_3D('',#188247,#91258,#91259);
#81637=AXIS2_PLACEMENT_3D('',#188248,#91260,#91261);
#81638=AXIS2_PLACEMENT_3D('',#188249,#91262,#91263);
#81639=AXIS2_PLACEMENT_3D('',#188250,#91264,#91265);
#81640=AXIS2_PLACEMENT_3D('',#188251,#91266,#91267);
#81641=AXIS2_PLACEMENT_3D('',#188256,#91269,#91270);
#81642=AXIS2_PLACEMENT_3D('',#188259,#91272,#91273);
#81643=AXIS2_PLACEMENT_3D('',#188260,#91274,#91275);
#81644=AXIS2_PLACEMENT_3D('',#188264,#91277,#91278);
#81645=AXIS2_PLACEMENT_3D('',#188265,#91279,#91280);
#81646=AXIS2_PLACEMENT_3D('',#188266,#91281,#91282);
#81647=AXIS2_PLACEMENT_3D('',#188270,#91284,#91285);
#81648=AXIS2_PLACEMENT_3D('',#188271,#91286,#91287);
#81649=AXIS2_PLACEMENT_3D('',#188272,#91288,#91289);
#81650=AXIS2_PLACEMENT_3D('',#188273,#91290,#91291);
#81651=AXIS2_PLACEMENT_3D('',#188274,#91292,#91293);
#81652=AXIS2_PLACEMENT_3D('',#188275,#91294,#91295);
#81653=AXIS2_PLACEMENT_3D('',#188280,#91297,#91298);
#81654=AXIS2_PLACEMENT_3D('',#188283,#91300,#91301);
#81655=AXIS2_PLACEMENT_3D('',#188284,#91302,#91303);
#81656=AXIS2_PLACEMENT_3D('',#188288,#91305,#91306);
#81657=AXIS2_PLACEMENT_3D('',#188289,#91307,#91308);
#81658=AXIS2_PLACEMENT_3D('',#188290,#91309,#91310);
#81659=AXIS2_PLACEMENT_3D('',#188294,#91312,#91313);
#81660=AXIS2_PLACEMENT_3D('',#188295,#91314,#91315);
#81661=AXIS2_PLACEMENT_3D('',#188296,#91316,#91317);
#81662=AXIS2_PLACEMENT_3D('',#188297,#91318,#91319);
#81663=AXIS2_PLACEMENT_3D('',#188298,#91320,#91321);
#81664=AXIS2_PLACEMENT_3D('',#188299,#91322,#91323);
#81665=AXIS2_PLACEMENT_3D('',#188304,#91325,#91326);
#81666=AXIS2_PLACEMENT_3D('',#188307,#91328,#91329);
#81667=AXIS2_PLACEMENT_3D('',#188308,#91330,#91331);
#81668=AXIS2_PLACEMENT_3D('',#188312,#91333,#91334);
#81669=AXIS2_PLACEMENT_3D('',#188313,#91335,#91336);
#81670=AXIS2_PLACEMENT_3D('',#188314,#91337,#91338);
#81671=AXIS2_PLACEMENT_3D('',#188318,#91340,#91341);
#81672=AXIS2_PLACEMENT_3D('',#188319,#91342,#91343);
#81673=AXIS2_PLACEMENT_3D('',#188320,#91344,#91345);
#81674=AXIS2_PLACEMENT_3D('',#188321,#91346,#91347);
#81675=AXIS2_PLACEMENT_3D('',#188322,#91348,#91349);
#81676=AXIS2_PLACEMENT_3D('',#188323,#91350,#91351);
#81677=AXIS2_PLACEMENT_3D('',#188328,#91353,#91354);
#81678=AXIS2_PLACEMENT_3D('',#188331,#91356,#91357);
#81679=AXIS2_PLACEMENT_3D('',#188332,#91358,#91359);
#81680=AXIS2_PLACEMENT_3D('',#188336,#91361,#91362);
#81681=AXIS2_PLACEMENT_3D('',#188337,#91363,#91364);
#81682=AXIS2_PLACEMENT_3D('',#188338,#91365,#91366);
#81683=AXIS2_PLACEMENT_3D('',#188342,#91368,#91369);
#81684=AXIS2_PLACEMENT_3D('',#188343,#91370,#91371);
#81685=AXIS2_PLACEMENT_3D('',#188344,#91372,#91373);
#81686=AXIS2_PLACEMENT_3D('',#188345,#91374,#91375);
#81687=AXIS2_PLACEMENT_3D('',#188346,#91376,#91377);
#81688=AXIS2_PLACEMENT_3D('',#188347,#91378,#91379);
#81689=AXIS2_PLACEMENT_3D('',#188352,#91381,#91382);
#81690=AXIS2_PLACEMENT_3D('',#188355,#91384,#91385);
#81691=AXIS2_PLACEMENT_3D('',#188356,#91386,#91387);
#81692=AXIS2_PLACEMENT_3D('',#188360,#91389,#91390);
#81693=AXIS2_PLACEMENT_3D('',#188361,#91391,#91392);
#81694=AXIS2_PLACEMENT_3D('',#188362,#91393,#91394);
#81695=AXIS2_PLACEMENT_3D('',#188366,#91396,#91397);
#81696=AXIS2_PLACEMENT_3D('',#188367,#91398,#91399);
#81697=AXIS2_PLACEMENT_3D('',#188368,#91400,#91401);
#81698=AXIS2_PLACEMENT_3D('',#188369,#91402,#91403);
#81699=AXIS2_PLACEMENT_3D('',#188370,#91404,#91405);
#81700=AXIS2_PLACEMENT_3D('',#188371,#91406,#91407);
#81701=AXIS2_PLACEMENT_3D('',#188376,#91409,#91410);
#81702=AXIS2_PLACEMENT_3D('',#188379,#91412,#91413);
#81703=AXIS2_PLACEMENT_3D('',#188380,#91414,#91415);
#81704=AXIS2_PLACEMENT_3D('',#188384,#91417,#91418);
#81705=AXIS2_PLACEMENT_3D('',#188385,#91419,#91420);
#81706=AXIS2_PLACEMENT_3D('',#188386,#91421,#91422);
#81707=AXIS2_PLACEMENT_3D('',#188390,#91424,#91425);
#81708=AXIS2_PLACEMENT_3D('',#188391,#91426,#91427);
#81709=AXIS2_PLACEMENT_3D('',#188392,#91428,#91429);
#81710=AXIS2_PLACEMENT_3D('',#188393,#91430,#91431);
#81711=AXIS2_PLACEMENT_3D('',#188394,#91432,#91433);
#81712=AXIS2_PLACEMENT_3D('',#188395,#91434,#91435);
#81713=AXIS2_PLACEMENT_3D('',#188400,#91437,#91438);
#81714=AXIS2_PLACEMENT_3D('',#188403,#91440,#91441);
#81715=AXIS2_PLACEMENT_3D('',#188404,#91442,#91443);
#81716=AXIS2_PLACEMENT_3D('',#188408,#91445,#91446);
#81717=AXIS2_PLACEMENT_3D('',#188409,#91447,#91448);
#81718=AXIS2_PLACEMENT_3D('',#188410,#91449,#91450);
#81719=AXIS2_PLACEMENT_3D('',#188414,#91452,#91453);
#81720=AXIS2_PLACEMENT_3D('',#188415,#91454,#91455);
#81721=AXIS2_PLACEMENT_3D('',#188416,#91456,#91457);
#81722=AXIS2_PLACEMENT_3D('',#188417,#91458,#91459);
#81723=AXIS2_PLACEMENT_3D('',#188418,#91460,#91461);
#81724=AXIS2_PLACEMENT_3D('',#188419,#91462,#91463);
#81725=AXIS2_PLACEMENT_3D('',#188424,#91465,#91466);
#81726=AXIS2_PLACEMENT_3D('',#188427,#91468,#91469);
#81727=AXIS2_PLACEMENT_3D('',#188428,#91470,#91471);
#81728=AXIS2_PLACEMENT_3D('',#188432,#91473,#91474);
#81729=AXIS2_PLACEMENT_3D('',#188433,#91475,#91476);
#81730=AXIS2_PLACEMENT_3D('',#188434,#91477,#91478);
#81731=AXIS2_PLACEMENT_3D('',#188438,#91480,#91481);
#81732=AXIS2_PLACEMENT_3D('',#188439,#91482,#91483);
#81733=AXIS2_PLACEMENT_3D('',#188440,#91484,#91485);
#81734=AXIS2_PLACEMENT_3D('',#188441,#91486,#91487);
#81735=AXIS2_PLACEMENT_3D('',#188442,#91488,#91489);
#81736=AXIS2_PLACEMENT_3D('',#188443,#91490,#91491);
#81737=AXIS2_PLACEMENT_3D('',#188448,#91493,#91494);
#81738=AXIS2_PLACEMENT_3D('',#188451,#91496,#91497);
#81739=AXIS2_PLACEMENT_3D('',#188452,#91498,#91499);
#81740=AXIS2_PLACEMENT_3D('',#188456,#91501,#91502);
#81741=AXIS2_PLACEMENT_3D('',#188457,#91503,#91504);
#81742=AXIS2_PLACEMENT_3D('',#188458,#91505,#91506);
#81743=AXIS2_PLACEMENT_3D('',#188462,#91508,#91509);
#81744=AXIS2_PLACEMENT_3D('',#188463,#91510,#91511);
#81745=AXIS2_PLACEMENT_3D('',#188464,#91512,#91513);
#81746=AXIS2_PLACEMENT_3D('',#188465,#91514,#91515);
#81747=AXIS2_PLACEMENT_3D('',#188466,#91516,#91517);
#81748=AXIS2_PLACEMENT_3D('',#188467,#91518,#91519);
#81749=AXIS2_PLACEMENT_3D('',#188472,#91521,#91522);
#81750=AXIS2_PLACEMENT_3D('',#188475,#91524,#91525);
#81751=AXIS2_PLACEMENT_3D('',#188476,#91526,#91527);
#81752=AXIS2_PLACEMENT_3D('',#188480,#91529,#91530);
#81753=AXIS2_PLACEMENT_3D('',#188481,#91531,#91532);
#81754=AXIS2_PLACEMENT_3D('',#188482,#91533,#91534);
#81755=AXIS2_PLACEMENT_3D('',#188486,#91536,#91537);
#81756=AXIS2_PLACEMENT_3D('',#188487,#91538,#91539);
#81757=AXIS2_PLACEMENT_3D('',#188488,#91540,#91541);
#81758=AXIS2_PLACEMENT_3D('',#188489,#91542,#91543);
#81759=AXIS2_PLACEMENT_3D('',#188490,#91544,#91545);
#81760=AXIS2_PLACEMENT_3D('',#188491,#91546,#91547);
#81761=AXIS2_PLACEMENT_3D('',#188496,#91549,#91550);
#81762=AXIS2_PLACEMENT_3D('',#188499,#91552,#91553);
#81763=AXIS2_PLACEMENT_3D('',#188500,#91554,#91555);
#81764=AXIS2_PLACEMENT_3D('',#188504,#91557,#91558);
#81765=AXIS2_PLACEMENT_3D('',#188505,#91559,#91560);
#81766=AXIS2_PLACEMENT_3D('',#188506,#91561,#91562);
#81767=AXIS2_PLACEMENT_3D('',#188512,#91565,#91566);
#81768=AXIS2_PLACEMENT_3D('',#188513,#91567,#91568);
#81769=AXIS2_PLACEMENT_3D('',#188514,#91569,#91570);
#81770=AXIS2_PLACEMENT_3D('',#188516,#91571,#91572);
#81771=AXIS2_PLACEMENT_3D('',#188518,#91574,#91575);
#81772=AXIS2_PLACEMENT_3D('',#188519,#91576,#91577);
#81773=AXIS2_PLACEMENT_3D('',#188520,#91578,#91579);
#81774=AXIS2_PLACEMENT_3D('',#188521,#91580,#91581);
#81775=AXIS2_PLACEMENT_3D('',#188526,#91583,#91584);
#81776=AXIS2_PLACEMENT_3D('',#188529,#91586,#91587);
#81777=AXIS2_PLACEMENT_3D('',#188530,#91588,#91589);
#81778=AXIS2_PLACEMENT_3D('',#188534,#91591,#91592);
#81779=AXIS2_PLACEMENT_3D('',#188535,#91593,#91594);
#81780=AXIS2_PLACEMENT_3D('',#188536,#91595,#91596);
#81781=AXIS2_PLACEMENT_3D('',#188542,#91599,#91600);
#81782=AXIS2_PLACEMENT_3D('',#188543,#91601,#91602);
#81783=AXIS2_PLACEMENT_3D('',#188544,#91603,#91604);
#81784=AXIS2_PLACEMENT_3D('',#188546,#91605,#91606);
#81785=AXIS2_PLACEMENT_3D('',#188548,#91608,#91609);
#81786=AXIS2_PLACEMENT_3D('',#188549,#91610,#91611);
#81787=AXIS2_PLACEMENT_3D('',#188550,#91612,#91613);
#81788=AXIS2_PLACEMENT_3D('',#188551,#91614,#91615);
#81789=AXIS2_PLACEMENT_3D('',#188556,#91617,#91618);
#81790=AXIS2_PLACEMENT_3D('',#188559,#91620,#91621);
#81791=AXIS2_PLACEMENT_3D('',#188560,#91622,#91623);
#81792=AXIS2_PLACEMENT_3D('',#188564,#91625,#91626);
#81793=AXIS2_PLACEMENT_3D('',#188565,#91627,#91628);
#81794=AXIS2_PLACEMENT_3D('',#188566,#91629,#91630);
#81795=AXIS2_PLACEMENT_3D('',#188570,#91632,#91633);
#81796=AXIS2_PLACEMENT_3D('',#188571,#91634,#91635);
#81797=AXIS2_PLACEMENT_3D('',#188572,#91636,#91637);
#81798=AXIS2_PLACEMENT_3D('',#188573,#91638,#91639);
#81799=AXIS2_PLACEMENT_3D('',#188574,#91640,#91641);
#81800=AXIS2_PLACEMENT_3D('',#188575,#91642,#91643);
#81801=AXIS2_PLACEMENT_3D('',#188580,#91645,#91646);
#81802=AXIS2_PLACEMENT_3D('',#188583,#91648,#91649);
#81803=AXIS2_PLACEMENT_3D('',#188584,#91650,#91651);
#81804=AXIS2_PLACEMENT_3D('',#188588,#91653,#91654);
#81805=AXIS2_PLACEMENT_3D('',#188589,#91655,#91656);
#81806=AXIS2_PLACEMENT_3D('',#188590,#91657,#91658);
#81807=AXIS2_PLACEMENT_3D('',#188594,#91660,#91661);
#81808=AXIS2_PLACEMENT_3D('',#188595,#91662,#91663);
#81809=AXIS2_PLACEMENT_3D('',#188596,#91664,#91665);
#81810=AXIS2_PLACEMENT_3D('',#188597,#91666,#91667);
#81811=AXIS2_PLACEMENT_3D('',#188598,#91668,#91669);
#81812=AXIS2_PLACEMENT_3D('',#188599,#91670,#91671);
#81813=AXIS2_PLACEMENT_3D('',#188604,#91673,#91674);
#81814=AXIS2_PLACEMENT_3D('',#188607,#91676,#91677);
#81815=AXIS2_PLACEMENT_3D('',#188608,#91678,#91679);
#81816=AXIS2_PLACEMENT_3D('',#188612,#91681,#91682);
#81817=AXIS2_PLACEMENT_3D('',#188613,#91683,#91684);
#81818=AXIS2_PLACEMENT_3D('',#188614,#91685,#91686);
#81819=AXIS2_PLACEMENT_3D('',#188618,#91688,#91689);
#81820=AXIS2_PLACEMENT_3D('',#188619,#91690,#91691);
#81821=AXIS2_PLACEMENT_3D('',#188620,#91692,#91693);
#81822=AXIS2_PLACEMENT_3D('',#188621,#91694,#91695);
#81823=AXIS2_PLACEMENT_3D('',#188622,#91696,#91697);
#81824=AXIS2_PLACEMENT_3D('',#188623,#91698,#91699);
#81825=AXIS2_PLACEMENT_3D('',#188628,#91701,#91702);
#81826=AXIS2_PLACEMENT_3D('',#188631,#91704,#91705);
#81827=AXIS2_PLACEMENT_3D('',#188632,#91706,#91707);
#81828=AXIS2_PLACEMENT_3D('',#188636,#91709,#91710);
#81829=AXIS2_PLACEMENT_3D('',#188637,#91711,#91712);
#81830=AXIS2_PLACEMENT_3D('',#188638,#91713,#91714);
#81831=AXIS2_PLACEMENT_3D('',#188642,#91716,#91717);
#81832=AXIS2_PLACEMENT_3D('',#188643,#91718,#91719);
#81833=AXIS2_PLACEMENT_3D('',#188644,#91720,#91721);
#81834=AXIS2_PLACEMENT_3D('',#188645,#91722,#91723);
#81835=AXIS2_PLACEMENT_3D('',#188646,#91724,#91725);
#81836=AXIS2_PLACEMENT_3D('',#188647,#91726,#91727);
#81837=AXIS2_PLACEMENT_3D('',#188652,#91729,#91730);
#81838=AXIS2_PLACEMENT_3D('',#188655,#91732,#91733);
#81839=AXIS2_PLACEMENT_3D('',#188656,#91734,#91735);
#81840=AXIS2_PLACEMENT_3D('',#188660,#91737,#91738);
#81841=AXIS2_PLACEMENT_3D('',#188661,#91739,#91740);
#81842=AXIS2_PLACEMENT_3D('',#188662,#91741,#91742);
#81843=AXIS2_PLACEMENT_3D('',#188666,#91744,#91745);
#81844=AXIS2_PLACEMENT_3D('',#188667,#91746,#91747);
#81845=AXIS2_PLACEMENT_3D('',#188668,#91748,#91749);
#81846=AXIS2_PLACEMENT_3D('',#188669,#91750,#91751);
#81847=AXIS2_PLACEMENT_3D('',#188670,#91752,#91753);
#81848=AXIS2_PLACEMENT_3D('',#188671,#91754,#91755);
#81849=AXIS2_PLACEMENT_3D('',#188676,#91757,#91758);
#81850=AXIS2_PLACEMENT_3D('',#188679,#91760,#91761);
#81851=AXIS2_PLACEMENT_3D('',#188680,#91762,#91763);
#81852=AXIS2_PLACEMENT_3D('',#188684,#91765,#91766);
#81853=AXIS2_PLACEMENT_3D('',#188685,#91767,#91768);
#81854=AXIS2_PLACEMENT_3D('',#188686,#91769,#91770);
#81855=AXIS2_PLACEMENT_3D('',#188690,#91772,#91773);
#81856=AXIS2_PLACEMENT_3D('',#188691,#91774,#91775);
#81857=AXIS2_PLACEMENT_3D('',#188692,#91776,#91777);
#81858=AXIS2_PLACEMENT_3D('',#188693,#91778,#91779);
#81859=AXIS2_PLACEMENT_3D('',#188694,#91780,#91781);
#81860=AXIS2_PLACEMENT_3D('',#188695,#91782,#91783);
#81861=AXIS2_PLACEMENT_3D('',#188700,#91785,#91786);
#81862=AXIS2_PLACEMENT_3D('',#188703,#91788,#91789);
#81863=AXIS2_PLACEMENT_3D('',#188704,#91790,#91791);
#81864=AXIS2_PLACEMENT_3D('',#188708,#91793,#91794);
#81865=AXIS2_PLACEMENT_3D('',#188709,#91795,#91796);
#81866=AXIS2_PLACEMENT_3D('',#188710,#91797,#91798);
#81867=AXIS2_PLACEMENT_3D('',#188714,#91800,#91801);
#81868=AXIS2_PLACEMENT_3D('',#188715,#91802,#91803);
#81869=AXIS2_PLACEMENT_3D('',#188716,#91804,#91805);
#81870=AXIS2_PLACEMENT_3D('',#188717,#91806,#91807);
#81871=AXIS2_PLACEMENT_3D('',#188718,#91808,#91809);
#81872=AXIS2_PLACEMENT_3D('',#188719,#91810,#91811);
#81873=AXIS2_PLACEMENT_3D('',#188724,#91813,#91814);
#81874=AXIS2_PLACEMENT_3D('',#188727,#91816,#91817);
#81875=AXIS2_PLACEMENT_3D('',#188728,#91818,#91819);
#81876=AXIS2_PLACEMENT_3D('',#188732,#91821,#91822);
#81877=AXIS2_PLACEMENT_3D('',#188733,#91823,#91824);
#81878=AXIS2_PLACEMENT_3D('',#188734,#91825,#91826);
#81879=AXIS2_PLACEMENT_3D('',#188738,#91828,#91829);
#81880=AXIS2_PLACEMENT_3D('',#188739,#91830,#91831);
#81881=AXIS2_PLACEMENT_3D('',#188740,#91832,#91833);
#81882=AXIS2_PLACEMENT_3D('',#188741,#91834,#91835);
#81883=AXIS2_PLACEMENT_3D('',#188742,#91836,#91837);
#81884=AXIS2_PLACEMENT_3D('',#188743,#91838,#91839);
#81885=AXIS2_PLACEMENT_3D('',#188748,#91841,#91842);
#81886=AXIS2_PLACEMENT_3D('',#188751,#91844,#91845);
#81887=AXIS2_PLACEMENT_3D('',#188752,#91846,#91847);
#81888=AXIS2_PLACEMENT_3D('',#188756,#91849,#91850);
#81889=AXIS2_PLACEMENT_3D('',#188757,#91851,#91852);
#81890=AXIS2_PLACEMENT_3D('',#188758,#91853,#91854);
#81891=AXIS2_PLACEMENT_3D('',#188762,#91856,#91857);
#81892=AXIS2_PLACEMENT_3D('',#188763,#91858,#91859);
#81893=AXIS2_PLACEMENT_3D('',#188764,#91860,#91861);
#81894=AXIS2_PLACEMENT_3D('',#188765,#91862,#91863);
#81895=AXIS2_PLACEMENT_3D('',#188766,#91864,#91865);
#81896=AXIS2_PLACEMENT_3D('',#188767,#91866,#91867);
#81897=AXIS2_PLACEMENT_3D('',#188772,#91869,#91870);
#81898=AXIS2_PLACEMENT_3D('',#188775,#91872,#91873);
#81899=AXIS2_PLACEMENT_3D('',#188776,#91874,#91875);
#81900=AXIS2_PLACEMENT_3D('',#188780,#91877,#91878);
#81901=AXIS2_PLACEMENT_3D('',#188781,#91879,#91880);
#81902=AXIS2_PLACEMENT_3D('',#188782,#91881,#91882);
#81903=AXIS2_PLACEMENT_3D('',#188786,#91884,#91885);
#81904=AXIS2_PLACEMENT_3D('',#188787,#91886,#91887);
#81905=AXIS2_PLACEMENT_3D('',#188788,#91888,#91889);
#81906=AXIS2_PLACEMENT_3D('',#188789,#91890,#91891);
#81907=AXIS2_PLACEMENT_3D('',#188790,#91892,#91893);
#81908=AXIS2_PLACEMENT_3D('',#188791,#91894,#91895);
#81909=AXIS2_PLACEMENT_3D('',#188796,#91897,#91898);
#81910=AXIS2_PLACEMENT_3D('',#188799,#91900,#91901);
#81911=AXIS2_PLACEMENT_3D('',#188800,#91902,#91903);
#81912=AXIS2_PLACEMENT_3D('',#188804,#91905,#91906);
#81913=AXIS2_PLACEMENT_3D('',#188805,#91907,#91908);
#81914=AXIS2_PLACEMENT_3D('',#188806,#91909,#91910);
#81915=AXIS2_PLACEMENT_3D('',#188810,#91912,#91913);
#81916=AXIS2_PLACEMENT_3D('',#188811,#91914,#91915);
#81917=AXIS2_PLACEMENT_3D('',#188812,#91916,#91917);
#81918=AXIS2_PLACEMENT_3D('',#188813,#91918,#91919);
#81919=AXIS2_PLACEMENT_3D('',#188814,#91920,#91921);
#81920=AXIS2_PLACEMENT_3D('',#188815,#91922,#91923);
#81921=AXIS2_PLACEMENT_3D('',#188820,#91925,#91926);
#81922=AXIS2_PLACEMENT_3D('',#188823,#91928,#91929);
#81923=AXIS2_PLACEMENT_3D('',#188824,#91930,#91931);
#81924=AXIS2_PLACEMENT_3D('',#188828,#91933,#91934);
#81925=AXIS2_PLACEMENT_3D('',#188829,#91935,#91936);
#81926=AXIS2_PLACEMENT_3D('',#188830,#91937,#91938);
#81927=AXIS2_PLACEMENT_3D('',#188834,#91940,#91941);
#81928=AXIS2_PLACEMENT_3D('',#188835,#91942,#91943);
#81929=AXIS2_PLACEMENT_3D('',#188836,#91944,#91945);
#81930=AXIS2_PLACEMENT_3D('',#188837,#91946,#91947);
#81931=AXIS2_PLACEMENT_3D('',#188838,#91948,#91949);
#81932=AXIS2_PLACEMENT_3D('',#188839,#91950,#91951);
#81933=AXIS2_PLACEMENT_3D('',#188844,#91953,#91954);
#81934=AXIS2_PLACEMENT_3D('',#188847,#91956,#91957);
#81935=AXIS2_PLACEMENT_3D('',#188848,#91958,#91959);
#81936=AXIS2_PLACEMENT_3D('',#188852,#91961,#91962);
#81937=AXIS2_PLACEMENT_3D('',#188853,#91963,#91964);
#81938=AXIS2_PLACEMENT_3D('',#188854,#91965,#91966);
#81939=AXIS2_PLACEMENT_3D('',#188858,#91968,#91969);
#81940=AXIS2_PLACEMENT_3D('',#188859,#91970,#91971);
#81941=AXIS2_PLACEMENT_3D('',#188860,#91972,#91973);
#81942=AXIS2_PLACEMENT_3D('',#188861,#91974,#91975);
#81943=AXIS2_PLACEMENT_3D('',#188862,#91976,#91977);
#81944=AXIS2_PLACEMENT_3D('',#188863,#91978,#91979);
#81945=AXIS2_PLACEMENT_3D('',#188868,#91981,#91982);
#81946=AXIS2_PLACEMENT_3D('',#188871,#91984,#91985);
#81947=AXIS2_PLACEMENT_3D('',#188872,#91986,#91987);
#81948=AXIS2_PLACEMENT_3D('',#188876,#91989,#91990);
#81949=AXIS2_PLACEMENT_3D('',#188877,#91991,#91992);
#81950=AXIS2_PLACEMENT_3D('',#188878,#91993,#91994);
#81951=AXIS2_PLACEMENT_3D('',#188882,#91996,#91997);
#81952=AXIS2_PLACEMENT_3D('',#188883,#91998,#91999);
#81953=AXIS2_PLACEMENT_3D('',#188884,#92000,#92001);
#81954=AXIS2_PLACEMENT_3D('',#188885,#92002,#92003);
#81955=AXIS2_PLACEMENT_3D('',#188886,#92004,#92005);
#81956=AXIS2_PLACEMENT_3D('',#188887,#92006,#92007);
#81957=AXIS2_PLACEMENT_3D('',#188892,#92009,#92010);
#81958=AXIS2_PLACEMENT_3D('',#188895,#92012,#92013);
#81959=AXIS2_PLACEMENT_3D('',#188896,#92014,#92015);
#81960=AXIS2_PLACEMENT_3D('',#188900,#92017,#92018);
#81961=AXIS2_PLACEMENT_3D('',#188901,#92019,#92020);
#81962=AXIS2_PLACEMENT_3D('',#188902,#92021,#92022);
#81963=AXIS2_PLACEMENT_3D('',#188906,#92024,#92025);
#81964=AXIS2_PLACEMENT_3D('',#188907,#92026,#92027);
#81965=AXIS2_PLACEMENT_3D('',#188908,#92028,#92029);
#81966=AXIS2_PLACEMENT_3D('',#188909,#92030,#92031);
#81967=AXIS2_PLACEMENT_3D('',#188910,#92032,#92033);
#81968=AXIS2_PLACEMENT_3D('',#188911,#92034,#92035);
#81969=AXIS2_PLACEMENT_3D('',#188916,#92037,#92038);
#81970=AXIS2_PLACEMENT_3D('',#188919,#92040,#92041);
#81971=AXIS2_PLACEMENT_3D('',#188920,#92042,#92043);
#81972=AXIS2_PLACEMENT_3D('',#188924,#92045,#92046);
#81973=AXIS2_PLACEMENT_3D('',#188925,#92047,#92048);
#81974=AXIS2_PLACEMENT_3D('',#188926,#92049,#92050);
#81975=AXIS2_PLACEMENT_3D('',#188930,#92052,#92053);
#81976=AXIS2_PLACEMENT_3D('',#188931,#92054,#92055);
#81977=AXIS2_PLACEMENT_3D('',#188932,#92056,#92057);
#81978=AXIS2_PLACEMENT_3D('',#188933,#92058,#92059);
#81979=AXIS2_PLACEMENT_3D('',#188934,#92060,#92061);
#81980=AXIS2_PLACEMENT_3D('',#188935,#92062,#92063);
#81981=AXIS2_PLACEMENT_3D('',#188940,#92065,#92066);
#81982=AXIS2_PLACEMENT_3D('',#188943,#92068,#92069);
#81983=AXIS2_PLACEMENT_3D('',#188944,#92070,#92071);
#81984=AXIS2_PLACEMENT_3D('',#188948,#92073,#92074);
#81985=AXIS2_PLACEMENT_3D('',#188949,#92075,#92076);
#81986=AXIS2_PLACEMENT_3D('',#188950,#92077,#92078);
#81987=AXIS2_PLACEMENT_3D('',#188954,#92080,#92081);
#81988=AXIS2_PLACEMENT_3D('',#188955,#92082,#92083);
#81989=AXIS2_PLACEMENT_3D('',#188956,#92084,#92085);
#81990=AXIS2_PLACEMENT_3D('',#188957,#92086,#92087);
#81991=AXIS2_PLACEMENT_3D('',#188958,#92088,#92089);
#81992=AXIS2_PLACEMENT_3D('',#188959,#92090,#92091);
#81993=AXIS2_PLACEMENT_3D('',#188964,#92093,#92094);
#81994=AXIS2_PLACEMENT_3D('',#188967,#92096,#92097);
#81995=AXIS2_PLACEMENT_3D('',#188968,#92098,#92099);
#81996=AXIS2_PLACEMENT_3D('',#188972,#92101,#92102);
#81997=AXIS2_PLACEMENT_3D('',#188973,#92103,#92104);
#81998=AXIS2_PLACEMENT_3D('',#188974,#92105,#92106);
#81999=AXIS2_PLACEMENT_3D('',#188978,#92108,#92109);
#82000=AXIS2_PLACEMENT_3D('',#188979,#92110,#92111);
#82001=AXIS2_PLACEMENT_3D('',#188980,#92112,#92113);
#82002=AXIS2_PLACEMENT_3D('',#188981,#92114,#92115);
#82003=AXIS2_PLACEMENT_3D('',#188982,#92116,#92117);
#82004=AXIS2_PLACEMENT_3D('',#188983,#92118,#92119);
#82005=AXIS2_PLACEMENT_3D('',#188988,#92121,#92122);
#82006=AXIS2_PLACEMENT_3D('',#188991,#92124,#92125);
#82007=AXIS2_PLACEMENT_3D('',#188992,#92126,#92127);
#82008=AXIS2_PLACEMENT_3D('',#188996,#92129,#92130);
#82009=AXIS2_PLACEMENT_3D('',#188997,#92131,#92132);
#82010=AXIS2_PLACEMENT_3D('',#188998,#92133,#92134);
#82011=AXIS2_PLACEMENT_3D('',#189002,#92136,#92137);
#82012=AXIS2_PLACEMENT_3D('',#189003,#92138,#92139);
#82013=AXIS2_PLACEMENT_3D('',#189004,#92140,#92141);
#82014=AXIS2_PLACEMENT_3D('',#189005,#92142,#92143);
#82015=AXIS2_PLACEMENT_3D('',#189006,#92144,#92145);
#82016=AXIS2_PLACEMENT_3D('',#189007,#92146,#92147);
#82017=AXIS2_PLACEMENT_3D('',#189012,#92149,#92150);
#82018=AXIS2_PLACEMENT_3D('',#189015,#92152,#92153);
#82019=AXIS2_PLACEMENT_3D('',#189016,#92154,#92155);
#82020=AXIS2_PLACEMENT_3D('',#189020,#92157,#92158);
#82021=AXIS2_PLACEMENT_3D('',#189021,#92159,#92160);
#82022=AXIS2_PLACEMENT_3D('',#189022,#92161,#92162);
#82023=AXIS2_PLACEMENT_3D('',#189026,#92164,#92165);
#82024=AXIS2_PLACEMENT_3D('',#189027,#92166,#92167);
#82025=AXIS2_PLACEMENT_3D('',#189028,#92168,#92169);
#82026=AXIS2_PLACEMENT_3D('',#189029,#92170,#92171);
#82027=AXIS2_PLACEMENT_3D('',#189030,#92172,#92173);
#82028=AXIS2_PLACEMENT_3D('',#189031,#92174,#92175);
#82029=AXIS2_PLACEMENT_3D('',#189036,#92177,#92178);
#82030=AXIS2_PLACEMENT_3D('',#189039,#92180,#92181);
#82031=AXIS2_PLACEMENT_3D('',#189040,#92182,#92183);
#82032=AXIS2_PLACEMENT_3D('',#189044,#92185,#92186);
#82033=AXIS2_PLACEMENT_3D('',#189045,#92187,#92188);
#82034=AXIS2_PLACEMENT_3D('',#189046,#92189,#92190);
#82035=AXIS2_PLACEMENT_3D('',#189050,#92192,#92193);
#82036=AXIS2_PLACEMENT_3D('',#189051,#92194,#92195);
#82037=AXIS2_PLACEMENT_3D('',#189052,#92196,#92197);
#82038=AXIS2_PLACEMENT_3D('',#189053,#92198,#92199);
#82039=AXIS2_PLACEMENT_3D('',#189054,#92200,#92201);
#82040=AXIS2_PLACEMENT_3D('',#189055,#92202,#92203);
#82041=AXIS2_PLACEMENT_3D('',#189060,#92205,#92206);
#82042=AXIS2_PLACEMENT_3D('',#189063,#92208,#92209);
#82043=AXIS2_PLACEMENT_3D('',#189064,#92210,#92211);
#82044=AXIS2_PLACEMENT_3D('',#189068,#92213,#92214);
#82045=AXIS2_PLACEMENT_3D('',#189069,#92215,#92216);
#82046=AXIS2_PLACEMENT_3D('',#189070,#92217,#92218);
#82047=AXIS2_PLACEMENT_3D('',#189074,#92220,#92221);
#82048=AXIS2_PLACEMENT_3D('',#189075,#92222,#92223);
#82049=AXIS2_PLACEMENT_3D('',#189076,#92224,#92225);
#82050=AXIS2_PLACEMENT_3D('',#189077,#92226,#92227);
#82051=AXIS2_PLACEMENT_3D('',#189078,#92228,#92229);
#82052=AXIS2_PLACEMENT_3D('',#189079,#92230,#92231);
#82053=AXIS2_PLACEMENT_3D('',#189084,#92233,#92234);
#82054=AXIS2_PLACEMENT_3D('',#189087,#92236,#92237);
#82055=AXIS2_PLACEMENT_3D('',#189088,#92238,#92239);
#82056=AXIS2_PLACEMENT_3D('',#189092,#92241,#92242);
#82057=AXIS2_PLACEMENT_3D('',#189093,#92243,#92244);
#82058=AXIS2_PLACEMENT_3D('',#189094,#92245,#92246);
#82059=AXIS2_PLACEMENT_3D('',#189098,#92248,#92249);
#82060=AXIS2_PLACEMENT_3D('',#189099,#92250,#92251);
#82061=AXIS2_PLACEMENT_3D('',#189100,#92252,#92253);
#82062=AXIS2_PLACEMENT_3D('',#189101,#92254,#92255);
#82063=AXIS2_PLACEMENT_3D('',#189102,#92256,#92257);
#82064=AXIS2_PLACEMENT_3D('',#189103,#92258,#92259);
#82065=AXIS2_PLACEMENT_3D('',#189108,#92261,#92262);
#82066=AXIS2_PLACEMENT_3D('',#189111,#92264,#92265);
#82067=AXIS2_PLACEMENT_3D('',#189112,#92266,#92267);
#82068=AXIS2_PLACEMENT_3D('',#189116,#92269,#92270);
#82069=AXIS2_PLACEMENT_3D('',#189117,#92271,#92272);
#82070=AXIS2_PLACEMENT_3D('',#189118,#92273,#92274);
#82071=AXIS2_PLACEMENT_3D('',#189122,#92276,#92277);
#82072=AXIS2_PLACEMENT_3D('',#189123,#92278,#92279);
#82073=AXIS2_PLACEMENT_3D('',#189124,#92280,#92281);
#82074=AXIS2_PLACEMENT_3D('',#189125,#92282,#92283);
#82075=AXIS2_PLACEMENT_3D('',#189126,#92284,#92285);
#82076=AXIS2_PLACEMENT_3D('',#189127,#92286,#92287);
#82077=AXIS2_PLACEMENT_3D('',#189132,#92289,#92290);
#82078=AXIS2_PLACEMENT_3D('',#189135,#92292,#92293);
#82079=AXIS2_PLACEMENT_3D('',#189136,#92294,#92295);
#82080=AXIS2_PLACEMENT_3D('',#189140,#92297,#92298);
#82081=AXIS2_PLACEMENT_3D('',#189141,#92299,#92300);
#82082=AXIS2_PLACEMENT_3D('',#189142,#92301,#92302);
#82083=AXIS2_PLACEMENT_3D('',#189146,#92304,#92305);
#82084=AXIS2_PLACEMENT_3D('',#189147,#92306,#92307);
#82085=AXIS2_PLACEMENT_3D('',#189148,#92308,#92309);
#82086=AXIS2_PLACEMENT_3D('',#189149,#92310,#92311);
#82087=AXIS2_PLACEMENT_3D('',#189150,#92312,#92313);
#82088=AXIS2_PLACEMENT_3D('',#189151,#92314,#92315);
#82089=AXIS2_PLACEMENT_3D('',#189156,#92317,#92318);
#82090=AXIS2_PLACEMENT_3D('',#189159,#92320,#92321);
#82091=AXIS2_PLACEMENT_3D('',#189160,#92322,#92323);
#82092=AXIS2_PLACEMENT_3D('',#189164,#92325,#92326);
#82093=AXIS2_PLACEMENT_3D('',#189165,#92327,#92328);
#82094=AXIS2_PLACEMENT_3D('',#189166,#92329,#92330);
#82095=AXIS2_PLACEMENT_3D('',#189170,#92332,#92333);
#82096=AXIS2_PLACEMENT_3D('',#189171,#92334,#92335);
#82097=AXIS2_PLACEMENT_3D('',#189172,#92336,#92337);
#82098=AXIS2_PLACEMENT_3D('',#189173,#92338,#92339);
#82099=AXIS2_PLACEMENT_3D('',#189174,#92340,#92341);
#82100=AXIS2_PLACEMENT_3D('',#189175,#92342,#92343);
#82101=AXIS2_PLACEMENT_3D('',#189180,#92345,#92346);
#82102=AXIS2_PLACEMENT_3D('',#189183,#92348,#92349);
#82103=AXIS2_PLACEMENT_3D('',#189184,#92350,#92351);
#82104=AXIS2_PLACEMENT_3D('',#189188,#92353,#92354);
#82105=AXIS2_PLACEMENT_3D('',#189189,#92355,#92356);
#82106=AXIS2_PLACEMENT_3D('',#189190,#92357,#92358);
#82107=AXIS2_PLACEMENT_3D('',#189194,#92360,#92361);
#82108=AXIS2_PLACEMENT_3D('',#189195,#92362,#92363);
#82109=AXIS2_PLACEMENT_3D('',#189196,#92364,#92365);
#82110=AXIS2_PLACEMENT_3D('',#189197,#92366,#92367);
#82111=AXIS2_PLACEMENT_3D('',#189198,#92368,#92369);
#82112=AXIS2_PLACEMENT_3D('',#189199,#92370,#92371);
#82113=AXIS2_PLACEMENT_3D('',#189204,#92373,#92374);
#82114=AXIS2_PLACEMENT_3D('',#189207,#92376,#92377);
#82115=AXIS2_PLACEMENT_3D('',#189208,#92378,#92379);
#82116=AXIS2_PLACEMENT_3D('',#189212,#92381,#92382);
#82117=AXIS2_PLACEMENT_3D('',#189213,#92383,#92384);
#82118=AXIS2_PLACEMENT_3D('',#189214,#92385,#92386);
#82119=AXIS2_PLACEMENT_3D('',#189218,#92388,#92389);
#82120=AXIS2_PLACEMENT_3D('',#189219,#92390,#92391);
#82121=AXIS2_PLACEMENT_3D('',#189220,#92392,#92393);
#82122=AXIS2_PLACEMENT_3D('',#189221,#92394,#92395);
#82123=AXIS2_PLACEMENT_3D('',#189222,#92396,#92397);
#82124=AXIS2_PLACEMENT_3D('',#189223,#92398,#92399);
#82125=AXIS2_PLACEMENT_3D('',#189228,#92401,#92402);
#82126=AXIS2_PLACEMENT_3D('',#189231,#92404,#92405);
#82127=AXIS2_PLACEMENT_3D('',#189232,#92406,#92407);
#82128=AXIS2_PLACEMENT_3D('',#189236,#92409,#92410);
#82129=AXIS2_PLACEMENT_3D('',#189237,#92411,#92412);
#82130=AXIS2_PLACEMENT_3D('',#189238,#92413,#92414);
#82131=AXIS2_PLACEMENT_3D('',#189242,#92416,#92417);
#82132=AXIS2_PLACEMENT_3D('',#189243,#92418,#92419);
#82133=AXIS2_PLACEMENT_3D('',#189244,#92420,#92421);
#82134=AXIS2_PLACEMENT_3D('',#189245,#92422,#92423);
#82135=AXIS2_PLACEMENT_3D('',#189246,#92424,#92425);
#82136=AXIS2_PLACEMENT_3D('',#189247,#92426,#92427);
#82137=AXIS2_PLACEMENT_3D('',#189252,#92429,#92430);
#82138=AXIS2_PLACEMENT_3D('',#189255,#92432,#92433);
#82139=AXIS2_PLACEMENT_3D('',#189256,#92434,#92435);
#82140=AXIS2_PLACEMENT_3D('',#189260,#92437,#92438);
#82141=AXIS2_PLACEMENT_3D('',#189261,#92439,#92440);
#82142=AXIS2_PLACEMENT_3D('',#189262,#92441,#92442);
#82143=AXIS2_PLACEMENT_3D('',#189266,#92444,#92445);
#82144=AXIS2_PLACEMENT_3D('',#189267,#92446,#92447);
#82145=AXIS2_PLACEMENT_3D('',#189268,#92448,#92449);
#82146=AXIS2_PLACEMENT_3D('',#189269,#92450,#92451);
#82147=AXIS2_PLACEMENT_3D('',#189270,#92452,#92453);
#82148=AXIS2_PLACEMENT_3D('',#189271,#92454,#92455);
#82149=AXIS2_PLACEMENT_3D('',#189276,#92457,#92458);
#82150=AXIS2_PLACEMENT_3D('',#189279,#92460,#92461);
#82151=AXIS2_PLACEMENT_3D('',#189280,#92462,#92463);
#82152=AXIS2_PLACEMENT_3D('',#189284,#92465,#92466);
#82153=AXIS2_PLACEMENT_3D('',#189285,#92467,#92468);
#82154=AXIS2_PLACEMENT_3D('',#189286,#92469,#92470);
#82155=AXIS2_PLACEMENT_3D('',#189290,#92472,#92473);
#82156=AXIS2_PLACEMENT_3D('',#189291,#92474,#92475);
#82157=AXIS2_PLACEMENT_3D('',#189292,#92476,#92477);
#82158=AXIS2_PLACEMENT_3D('',#189293,#92478,#92479);
#82159=AXIS2_PLACEMENT_3D('',#189294,#92480,#92481);
#82160=AXIS2_PLACEMENT_3D('',#189295,#92482,#92483);
#82161=AXIS2_PLACEMENT_3D('',#189300,#92485,#92486);
#82162=AXIS2_PLACEMENT_3D('',#189303,#92488,#92489);
#82163=AXIS2_PLACEMENT_3D('',#189304,#92490,#92491);
#82164=AXIS2_PLACEMENT_3D('',#189308,#92493,#92494);
#82165=AXIS2_PLACEMENT_3D('',#189309,#92495,#92496);
#82166=AXIS2_PLACEMENT_3D('',#189310,#92497,#92498);
#82167=AXIS2_PLACEMENT_3D('',#189314,#92500,#92501);
#82168=AXIS2_PLACEMENT_3D('',#189315,#92502,#92503);
#82169=AXIS2_PLACEMENT_3D('',#189316,#92504,#92505);
#82170=AXIS2_PLACEMENT_3D('',#189317,#92506,#92507);
#82171=AXIS2_PLACEMENT_3D('',#189318,#92508,#92509);
#82172=AXIS2_PLACEMENT_3D('',#189319,#92510,#92511);
#82173=AXIS2_PLACEMENT_3D('',#189324,#92513,#92514);
#82174=AXIS2_PLACEMENT_3D('',#189327,#92516,#92517);
#82175=AXIS2_PLACEMENT_3D('',#189328,#92518,#92519);
#82176=AXIS2_PLACEMENT_3D('',#189332,#92521,#92522);
#82177=AXIS2_PLACEMENT_3D('',#189333,#92523,#92524);
#82178=AXIS2_PLACEMENT_3D('',#189334,#92525,#92526);
#82179=AXIS2_PLACEMENT_3D('',#189338,#92528,#92529);
#82180=AXIS2_PLACEMENT_3D('',#189339,#92530,#92531);
#82181=AXIS2_PLACEMENT_3D('',#189340,#92532,#92533);
#82182=AXIS2_PLACEMENT_3D('',#189341,#92534,#92535);
#82183=AXIS2_PLACEMENT_3D('',#189342,#92536,#92537);
#82184=AXIS2_PLACEMENT_3D('',#189343,#92538,#92539);
#82185=AXIS2_PLACEMENT_3D('',#189348,#92541,#92542);
#82186=AXIS2_PLACEMENT_3D('',#189351,#92544,#92545);
#82187=AXIS2_PLACEMENT_3D('',#189352,#92546,#92547);
#82188=AXIS2_PLACEMENT_3D('',#189356,#92549,#92550);
#82189=AXIS2_PLACEMENT_3D('',#189357,#92551,#92552);
#82190=AXIS2_PLACEMENT_3D('',#189358,#92553,#92554);
#82191=AXIS2_PLACEMENT_3D('',#189362,#92556,#92557);
#82192=AXIS2_PLACEMENT_3D('',#189363,#92558,#92559);
#82193=AXIS2_PLACEMENT_3D('',#189364,#92560,#92561);
#82194=AXIS2_PLACEMENT_3D('',#189365,#92562,#92563);
#82195=AXIS2_PLACEMENT_3D('',#189366,#92564,#92565);
#82196=AXIS2_PLACEMENT_3D('',#189367,#92566,#92567);
#82197=AXIS2_PLACEMENT_3D('',#189372,#92569,#92570);
#82198=AXIS2_PLACEMENT_3D('',#189375,#92572,#92573);
#82199=AXIS2_PLACEMENT_3D('',#189376,#92574,#92575);
#82200=AXIS2_PLACEMENT_3D('',#189380,#92577,#92578);
#82201=AXIS2_PLACEMENT_3D('',#189381,#92579,#92580);
#82202=AXIS2_PLACEMENT_3D('',#189382,#92581,#92582);
#82203=AXIS2_PLACEMENT_3D('',#189386,#92584,#92585);
#82204=AXIS2_PLACEMENT_3D('',#189387,#92586,#92587);
#82205=AXIS2_PLACEMENT_3D('',#189388,#92588,#92589);
#82206=AXIS2_PLACEMENT_3D('',#189389,#92590,#92591);
#82207=AXIS2_PLACEMENT_3D('',#189390,#92592,#92593);
#82208=AXIS2_PLACEMENT_3D('',#189391,#92594,#92595);
#82209=AXIS2_PLACEMENT_3D('',#189396,#92597,#92598);
#82210=AXIS2_PLACEMENT_3D('',#189399,#92600,#92601);
#82211=AXIS2_PLACEMENT_3D('',#189400,#92602,#92603);
#82212=AXIS2_PLACEMENT_3D('',#189404,#92605,#92606);
#82213=AXIS2_PLACEMENT_3D('',#189405,#92607,#92608);
#82214=AXIS2_PLACEMENT_3D('',#189406,#92609,#92610);
#82215=AXIS2_PLACEMENT_3D('',#189410,#92612,#92613);
#82216=AXIS2_PLACEMENT_3D('',#189411,#92614,#92615);
#82217=AXIS2_PLACEMENT_3D('',#189412,#92616,#92617);
#82218=AXIS2_PLACEMENT_3D('',#189413,#92618,#92619);
#82219=AXIS2_PLACEMENT_3D('',#189414,#92620,#92621);
#82220=AXIS2_PLACEMENT_3D('',#189415,#92622,#92623);
#82221=AXIS2_PLACEMENT_3D('',#189420,#92625,#92626);
#82222=AXIS2_PLACEMENT_3D('',#189423,#92628,#92629);
#82223=AXIS2_PLACEMENT_3D('',#189424,#92630,#92631);
#82224=AXIS2_PLACEMENT_3D('',#189428,#92633,#92634);
#82225=AXIS2_PLACEMENT_3D('',#189429,#92635,#92636);
#82226=AXIS2_PLACEMENT_3D('',#189430,#92637,#92638);
#82227=AXIS2_PLACEMENT_3D('',#189434,#92640,#92641);
#82228=AXIS2_PLACEMENT_3D('',#189435,#92642,#92643);
#82229=AXIS2_PLACEMENT_3D('',#189436,#92644,#92645);
#82230=AXIS2_PLACEMENT_3D('',#189437,#92646,#92647);
#82231=AXIS2_PLACEMENT_3D('',#189438,#92648,#92649);
#82232=AXIS2_PLACEMENT_3D('',#189439,#92650,#92651);
#82233=AXIS2_PLACEMENT_3D('',#189444,#92653,#92654);
#82234=AXIS2_PLACEMENT_3D('',#189447,#92656,#92657);
#82235=AXIS2_PLACEMENT_3D('',#189448,#92658,#92659);
#82236=AXIS2_PLACEMENT_3D('',#189452,#92661,#92662);
#82237=AXIS2_PLACEMENT_3D('',#189453,#92663,#92664);
#82238=AXIS2_PLACEMENT_3D('',#189454,#92665,#92666);
#82239=AXIS2_PLACEMENT_3D('',#189458,#92668,#92669);
#82240=AXIS2_PLACEMENT_3D('',#189459,#92670,#92671);
#82241=AXIS2_PLACEMENT_3D('',#189460,#92672,#92673);
#82242=AXIS2_PLACEMENT_3D('',#189461,#92674,#92675);
#82243=AXIS2_PLACEMENT_3D('',#189462,#92676,#92677);
#82244=AXIS2_PLACEMENT_3D('',#189463,#92678,#92679);
#82245=AXIS2_PLACEMENT_3D('',#189468,#92681,#92682);
#82246=AXIS2_PLACEMENT_3D('',#189471,#92684,#92685);
#82247=AXIS2_PLACEMENT_3D('',#189472,#92686,#92687);
#82248=AXIS2_PLACEMENT_3D('',#189476,#92689,#92690);
#82249=AXIS2_PLACEMENT_3D('',#189477,#92691,#92692);
#82250=AXIS2_PLACEMENT_3D('',#189478,#92693,#92694);
#82251=AXIS2_PLACEMENT_3D('',#189482,#92696,#92697);
#82252=AXIS2_PLACEMENT_3D('',#189483,#92698,#92699);
#82253=AXIS2_PLACEMENT_3D('',#189484,#92700,#92701);
#82254=AXIS2_PLACEMENT_3D('',#189485,#92702,#92703);
#82255=AXIS2_PLACEMENT_3D('',#189486,#92704,#92705);
#82256=AXIS2_PLACEMENT_3D('',#189487,#92706,#92707);
#82257=AXIS2_PLACEMENT_3D('',#189492,#92709,#92710);
#82258=AXIS2_PLACEMENT_3D('',#189495,#92712,#92713);
#82259=AXIS2_PLACEMENT_3D('',#189496,#92714,#92715);
#82260=AXIS2_PLACEMENT_3D('',#189500,#92717,#92718);
#82261=AXIS2_PLACEMENT_3D('',#189501,#92719,#92720);
#82262=AXIS2_PLACEMENT_3D('',#189502,#92721,#92722);
#82263=AXIS2_PLACEMENT_3D('',#189506,#92724,#92725);
#82264=AXIS2_PLACEMENT_3D('',#189507,#92726,#92727);
#82265=AXIS2_PLACEMENT_3D('',#189508,#92728,#92729);
#82266=AXIS2_PLACEMENT_3D('',#189509,#92730,#92731);
#82267=AXIS2_PLACEMENT_3D('',#189510,#92732,#92733);
#82268=AXIS2_PLACEMENT_3D('',#189511,#92734,#92735);
#82269=AXIS2_PLACEMENT_3D('',#189516,#92737,#92738);
#82270=AXIS2_PLACEMENT_3D('',#189519,#92740,#92741);
#82271=AXIS2_PLACEMENT_3D('',#189520,#92742,#92743);
#82272=AXIS2_PLACEMENT_3D('',#189524,#92745,#92746);
#82273=AXIS2_PLACEMENT_3D('',#189525,#92747,#92748);
#82274=AXIS2_PLACEMENT_3D('',#189526,#92749,#92750);
#82275=AXIS2_PLACEMENT_3D('',#189530,#92752,#92753);
#82276=AXIS2_PLACEMENT_3D('',#189531,#92754,#92755);
#82277=AXIS2_PLACEMENT_3D('',#189532,#92756,#92757);
#82278=AXIS2_PLACEMENT_3D('',#189533,#92758,#92759);
#82279=AXIS2_PLACEMENT_3D('',#189534,#92760,#92761);
#82280=AXIS2_PLACEMENT_3D('',#189535,#92762,#92763);
#82281=AXIS2_PLACEMENT_3D('',#189540,#92765,#92766);
#82282=AXIS2_PLACEMENT_3D('',#189543,#92768,#92769);
#82283=AXIS2_PLACEMENT_3D('',#189544,#92770,#92771);
#82284=AXIS2_PLACEMENT_3D('',#189548,#92773,#92774);
#82285=AXIS2_PLACEMENT_3D('',#189549,#92775,#92776);
#82286=AXIS2_PLACEMENT_3D('',#189550,#92777,#92778);
#82287=AXIS2_PLACEMENT_3D('',#189554,#92780,#92781);
#82288=AXIS2_PLACEMENT_3D('',#189555,#92782,#92783);
#82289=AXIS2_PLACEMENT_3D('',#189556,#92784,#92785);
#82290=AXIS2_PLACEMENT_3D('',#189557,#92786,#92787);
#82291=AXIS2_PLACEMENT_3D('',#189558,#92788,#92789);
#82292=AXIS2_PLACEMENT_3D('',#189559,#92790,#92791);
#82293=AXIS2_PLACEMENT_3D('',#189564,#92793,#92794);
#82294=AXIS2_PLACEMENT_3D('',#189567,#92796,#92797);
#82295=AXIS2_PLACEMENT_3D('',#189568,#92798,#92799);
#82296=AXIS2_PLACEMENT_3D('',#189572,#92801,#92802);
#82297=AXIS2_PLACEMENT_3D('',#189573,#92803,#92804);
#82298=AXIS2_PLACEMENT_3D('',#189574,#92805,#92806);
#82299=AXIS2_PLACEMENT_3D('',#189578,#92808,#92809);
#82300=AXIS2_PLACEMENT_3D('',#189579,#92810,#92811);
#82301=AXIS2_PLACEMENT_3D('',#189580,#92812,#92813);
#82302=AXIS2_PLACEMENT_3D('',#189581,#92814,#92815);
#82303=AXIS2_PLACEMENT_3D('',#189582,#92816,#92817);
#82304=AXIS2_PLACEMENT_3D('',#189583,#92818,#92819);
#82305=AXIS2_PLACEMENT_3D('',#189588,#92821,#92822);
#82306=AXIS2_PLACEMENT_3D('',#189591,#92824,#92825);
#82307=AXIS2_PLACEMENT_3D('',#189592,#92826,#92827);
#82308=AXIS2_PLACEMENT_3D('',#189596,#92829,#92830);
#82309=AXIS2_PLACEMENT_3D('',#189597,#92831,#92832);
#82310=AXIS2_PLACEMENT_3D('',#189598,#92833,#92834);
#82311=AXIS2_PLACEMENT_3D('',#189602,#92836,#92837);
#82312=AXIS2_PLACEMENT_3D('',#189603,#92838,#92839);
#82313=AXIS2_PLACEMENT_3D('',#189604,#92840,#92841);
#82314=AXIS2_PLACEMENT_3D('',#189605,#92842,#92843);
#82315=AXIS2_PLACEMENT_3D('',#189606,#92844,#92845);
#82316=AXIS2_PLACEMENT_3D('',#189607,#92846,#92847);
#82317=AXIS2_PLACEMENT_3D('',#189612,#92849,#92850);
#82318=AXIS2_PLACEMENT_3D('',#189615,#92852,#92853);
#82319=AXIS2_PLACEMENT_3D('',#189616,#92854,#92855);
#82320=AXIS2_PLACEMENT_3D('',#189620,#92857,#92858);
#82321=AXIS2_PLACEMENT_3D('',#189621,#92859,#92860);
#82322=AXIS2_PLACEMENT_3D('',#189622,#92861,#92862);
#82323=AXIS2_PLACEMENT_3D('',#189626,#92864,#92865);
#82324=AXIS2_PLACEMENT_3D('',#189627,#92866,#92867);
#82325=AXIS2_PLACEMENT_3D('',#189628,#92868,#92869);
#82326=AXIS2_PLACEMENT_3D('',#189629,#92870,#92871);
#82327=AXIS2_PLACEMENT_3D('',#189630,#92872,#92873);
#82328=AXIS2_PLACEMENT_3D('',#189631,#92874,#92875);
#82329=AXIS2_PLACEMENT_3D('',#189636,#92877,#92878);
#82330=AXIS2_PLACEMENT_3D('',#189639,#92880,#92881);
#82331=AXIS2_PLACEMENT_3D('',#189640,#92882,#92883);
#82332=AXIS2_PLACEMENT_3D('',#189644,#92885,#92886);
#82333=AXIS2_PLACEMENT_3D('',#189645,#92887,#92888);
#82334=AXIS2_PLACEMENT_3D('',#189646,#92889,#92890);
#82335=AXIS2_PLACEMENT_3D('',#189650,#92892,#92893);
#82336=AXIS2_PLACEMENT_3D('',#189651,#92894,#92895);
#82337=AXIS2_PLACEMENT_3D('',#189652,#92896,#92897);
#82338=AXIS2_PLACEMENT_3D('',#189653,#92898,#92899);
#82339=AXIS2_PLACEMENT_3D('',#189654,#92900,#92901);
#82340=AXIS2_PLACEMENT_3D('',#189655,#92902,#92903);
#82341=AXIS2_PLACEMENT_3D('',#189660,#92905,#92906);
#82342=AXIS2_PLACEMENT_3D('',#189663,#92908,#92909);
#82343=AXIS2_PLACEMENT_3D('',#189664,#92910,#92911);
#82344=AXIS2_PLACEMENT_3D('',#189668,#92913,#92914);
#82345=AXIS2_PLACEMENT_3D('',#189669,#92915,#92916);
#82346=AXIS2_PLACEMENT_3D('',#189670,#92917,#92918);
#82347=AXIS2_PLACEMENT_3D('',#189674,#92920,#92921);
#82348=AXIS2_PLACEMENT_3D('',#189675,#92922,#92923);
#82349=AXIS2_PLACEMENT_3D('',#189676,#92924,#92925);
#82350=AXIS2_PLACEMENT_3D('',#189677,#92926,#92927);
#82351=AXIS2_PLACEMENT_3D('',#189678,#92928,#92929);
#82352=AXIS2_PLACEMENT_3D('',#189679,#92930,#92931);
#82353=AXIS2_PLACEMENT_3D('',#189684,#92933,#92934);
#82354=AXIS2_PLACEMENT_3D('',#189687,#92936,#92937);
#82355=AXIS2_PLACEMENT_3D('',#189688,#92938,#92939);
#82356=AXIS2_PLACEMENT_3D('',#189692,#92941,#92942);
#82357=AXIS2_PLACEMENT_3D('',#189693,#92943,#92944);
#82358=AXIS2_PLACEMENT_3D('',#189694,#92945,#92946);
#82359=AXIS2_PLACEMENT_3D('',#189698,#92948,#92949);
#82360=AXIS2_PLACEMENT_3D('',#189699,#92950,#92951);
#82361=AXIS2_PLACEMENT_3D('',#189700,#92952,#92953);
#82362=AXIS2_PLACEMENT_3D('',#189701,#92954,#92955);
#82363=AXIS2_PLACEMENT_3D('',#189702,#92956,#92957);
#82364=AXIS2_PLACEMENT_3D('',#189703,#92958,#92959);
#82365=AXIS2_PLACEMENT_3D('',#189708,#92961,#92962);
#82366=AXIS2_PLACEMENT_3D('',#189711,#92964,#92965);
#82367=AXIS2_PLACEMENT_3D('',#189712,#92966,#92967);
#82368=AXIS2_PLACEMENT_3D('',#189716,#92969,#92970);
#82369=AXIS2_PLACEMENT_3D('',#189717,#92971,#92972);
#82370=AXIS2_PLACEMENT_3D('',#189718,#92973,#92974);
#82371=AXIS2_PLACEMENT_3D('',#189722,#92976,#92977);
#82372=AXIS2_PLACEMENT_3D('',#189723,#92978,#92979);
#82373=AXIS2_PLACEMENT_3D('',#189724,#92980,#92981);
#82374=AXIS2_PLACEMENT_3D('',#189725,#92982,#92983);
#82375=AXIS2_PLACEMENT_3D('',#189726,#92984,#92985);
#82376=AXIS2_PLACEMENT_3D('',#189727,#92986,#92987);
#82377=AXIS2_PLACEMENT_3D('',#189732,#92989,#92990);
#82378=AXIS2_PLACEMENT_3D('',#189735,#92992,#92993);
#82379=AXIS2_PLACEMENT_3D('',#189736,#92994,#92995);
#82380=AXIS2_PLACEMENT_3D('',#189740,#92997,#92998);
#82381=AXIS2_PLACEMENT_3D('',#189741,#92999,#93000);
#82382=AXIS2_PLACEMENT_3D('',#189742,#93001,#93002);
#82383=AXIS2_PLACEMENT_3D('',#189746,#93004,#93005);
#82384=AXIS2_PLACEMENT_3D('',#189747,#93006,#93007);
#82385=AXIS2_PLACEMENT_3D('',#189748,#93008,#93009);
#82386=AXIS2_PLACEMENT_3D('',#189749,#93010,#93011);
#82387=AXIS2_PLACEMENT_3D('',#189750,#93012,#93013);
#82388=AXIS2_PLACEMENT_3D('',#189751,#93014,#93015);
#82389=AXIS2_PLACEMENT_3D('',#189756,#93017,#93018);
#82390=AXIS2_PLACEMENT_3D('',#189759,#93020,#93021);
#82391=AXIS2_PLACEMENT_3D('',#189760,#93022,#93023);
#82392=AXIS2_PLACEMENT_3D('',#189764,#93025,#93026);
#82393=AXIS2_PLACEMENT_3D('',#189765,#93027,#93028);
#82394=AXIS2_PLACEMENT_3D('',#189766,#93029,#93030);
#82395=AXIS2_PLACEMENT_3D('',#189770,#93032,#93033);
#82396=AXIS2_PLACEMENT_3D('',#189771,#93034,#93035);
#82397=AXIS2_PLACEMENT_3D('',#189772,#93036,#93037);
#82398=AXIS2_PLACEMENT_3D('',#189773,#93038,#93039);
#82399=AXIS2_PLACEMENT_3D('',#189774,#93040,#93041);
#82400=AXIS2_PLACEMENT_3D('',#189775,#93042,#93043);
#82401=AXIS2_PLACEMENT_3D('',#189780,#93045,#93046);
#82402=AXIS2_PLACEMENT_3D('',#189783,#93048,#93049);
#82403=AXIS2_PLACEMENT_3D('',#189784,#93050,#93051);
#82404=AXIS2_PLACEMENT_3D('',#189788,#93053,#93054);
#82405=AXIS2_PLACEMENT_3D('',#189789,#93055,#93056);
#82406=AXIS2_PLACEMENT_3D('',#189790,#93057,#93058);
#82407=AXIS2_PLACEMENT_3D('',#189794,#93060,#93061);
#82408=AXIS2_PLACEMENT_3D('',#189795,#93062,#93063);
#82409=AXIS2_PLACEMENT_3D('',#189796,#93064,#93065);
#82410=AXIS2_PLACEMENT_3D('',#189797,#93066,#93067);
#82411=AXIS2_PLACEMENT_3D('',#189798,#93068,#93069);
#82412=AXIS2_PLACEMENT_3D('',#189799,#93070,#93071);
#82413=AXIS2_PLACEMENT_3D('',#189804,#93073,#93074);
#82414=AXIS2_PLACEMENT_3D('',#189807,#93076,#93077);
#82415=AXIS2_PLACEMENT_3D('',#189808,#93078,#93079);
#82416=AXIS2_PLACEMENT_3D('',#189812,#93081,#93082);
#82417=AXIS2_PLACEMENT_3D('',#189813,#93083,#93084);
#82418=AXIS2_PLACEMENT_3D('',#189814,#93085,#93086);
#82419=AXIS2_PLACEMENT_3D('',#189818,#93088,#93089);
#82420=AXIS2_PLACEMENT_3D('',#189819,#93090,#93091);
#82421=AXIS2_PLACEMENT_3D('',#189820,#93092,#93093);
#82422=AXIS2_PLACEMENT_3D('',#189821,#93094,#93095);
#82423=AXIS2_PLACEMENT_3D('',#189822,#93096,#93097);
#82424=AXIS2_PLACEMENT_3D('',#189823,#93098,#93099);
#82425=AXIS2_PLACEMENT_3D('',#189828,#93101,#93102);
#82426=AXIS2_PLACEMENT_3D('',#189831,#93104,#93105);
#82427=AXIS2_PLACEMENT_3D('',#189832,#93106,#93107);
#82428=AXIS2_PLACEMENT_3D('',#189836,#93109,#93110);
#82429=AXIS2_PLACEMENT_3D('',#189837,#93111,#93112);
#82430=AXIS2_PLACEMENT_3D('',#189838,#93113,#93114);
#82431=AXIS2_PLACEMENT_3D('',#189842,#93116,#93117);
#82432=AXIS2_PLACEMENT_3D('',#189843,#93118,#93119);
#82433=AXIS2_PLACEMENT_3D('',#189844,#93120,#93121);
#82434=AXIS2_PLACEMENT_3D('',#189845,#93122,#93123);
#82435=AXIS2_PLACEMENT_3D('',#189846,#93124,#93125);
#82436=AXIS2_PLACEMENT_3D('',#189847,#93126,#93127);
#82437=AXIS2_PLACEMENT_3D('',#189852,#93129,#93130);
#82438=AXIS2_PLACEMENT_3D('',#189855,#93132,#93133);
#82439=AXIS2_PLACEMENT_3D('',#189856,#93134,#93135);
#82440=AXIS2_PLACEMENT_3D('',#189860,#93137,#93138);
#82441=AXIS2_PLACEMENT_3D('',#189861,#93139,#93140);
#82442=AXIS2_PLACEMENT_3D('',#189862,#93141,#93142);
#82443=AXIS2_PLACEMENT_3D('',#189866,#93144,#93145);
#82444=AXIS2_PLACEMENT_3D('',#189867,#93146,#93147);
#82445=AXIS2_PLACEMENT_3D('',#189868,#93148,#93149);
#82446=AXIS2_PLACEMENT_3D('',#189869,#93150,#93151);
#82447=AXIS2_PLACEMENT_3D('',#189870,#93152,#93153);
#82448=AXIS2_PLACEMENT_3D('',#189871,#93154,#93155);
#82449=AXIS2_PLACEMENT_3D('',#189876,#93157,#93158);
#82450=AXIS2_PLACEMENT_3D('',#189879,#93160,#93161);
#82451=AXIS2_PLACEMENT_3D('',#189880,#93162,#93163);
#82452=AXIS2_PLACEMENT_3D('',#189884,#93165,#93166);
#82453=AXIS2_PLACEMENT_3D('',#189885,#93167,#93168);
#82454=AXIS2_PLACEMENT_3D('',#189886,#93169,#93170);
#82455=AXIS2_PLACEMENT_3D('',#189890,#93172,#93173);
#82456=AXIS2_PLACEMENT_3D('',#189891,#93174,#93175);
#82457=AXIS2_PLACEMENT_3D('',#189892,#93176,#93177);
#82458=AXIS2_PLACEMENT_3D('',#189893,#93178,#93179);
#82459=AXIS2_PLACEMENT_3D('',#189894,#93180,#93181);
#82460=AXIS2_PLACEMENT_3D('',#189895,#93182,#93183);
#82461=AXIS2_PLACEMENT_3D('',#189900,#93185,#93186);
#82462=AXIS2_PLACEMENT_3D('',#189903,#93188,#93189);
#82463=AXIS2_PLACEMENT_3D('',#189904,#93190,#93191);
#82464=AXIS2_PLACEMENT_3D('',#189908,#93193,#93194);
#82465=AXIS2_PLACEMENT_3D('',#189909,#93195,#93196);
#82466=AXIS2_PLACEMENT_3D('',#189910,#93197,#93198);
#82467=AXIS2_PLACEMENT_3D('',#189914,#93200,#93201);
#82468=AXIS2_PLACEMENT_3D('',#189915,#93202,#93203);
#82469=AXIS2_PLACEMENT_3D('',#189916,#93204,#93205);
#82470=AXIS2_PLACEMENT_3D('',#189917,#93206,#93207);
#82471=AXIS2_PLACEMENT_3D('',#189918,#93208,#93209);
#82472=AXIS2_PLACEMENT_3D('',#189919,#93210,#93211);
#82473=AXIS2_PLACEMENT_3D('',#189924,#93213,#93214);
#82474=AXIS2_PLACEMENT_3D('',#189927,#93216,#93217);
#82475=AXIS2_PLACEMENT_3D('',#189928,#93218,#93219);
#82476=AXIS2_PLACEMENT_3D('',#189932,#93221,#93222);
#82477=AXIS2_PLACEMENT_3D('',#189933,#93223,#93224);
#82478=AXIS2_PLACEMENT_3D('',#189934,#93225,#93226);
#82479=AXIS2_PLACEMENT_3D('',#189938,#93228,#93229);
#82480=AXIS2_PLACEMENT_3D('',#189939,#93230,#93231);
#82481=AXIS2_PLACEMENT_3D('',#189940,#93232,#93233);
#82482=AXIS2_PLACEMENT_3D('',#189941,#93234,#93235);
#82483=AXIS2_PLACEMENT_3D('',#189942,#93236,#93237);
#82484=AXIS2_PLACEMENT_3D('',#189943,#93238,#93239);
#82485=AXIS2_PLACEMENT_3D('',#189948,#93241,#93242);
#82486=AXIS2_PLACEMENT_3D('',#189951,#93244,#93245);
#82487=AXIS2_PLACEMENT_3D('',#189952,#93246,#93247);
#82488=AXIS2_PLACEMENT_3D('',#189956,#93249,#93250);
#82489=AXIS2_PLACEMENT_3D('',#189957,#93251,#93252);
#82490=AXIS2_PLACEMENT_3D('',#189958,#93253,#93254);
#82491=AXIS2_PLACEMENT_3D('',#189962,#93256,#93257);
#82492=AXIS2_PLACEMENT_3D('',#189963,#93258,#93259);
#82493=AXIS2_PLACEMENT_3D('',#189964,#93260,#93261);
#82494=AXIS2_PLACEMENT_3D('',#189965,#93262,#93263);
#82495=AXIS2_PLACEMENT_3D('',#189966,#93264,#93265);
#82496=AXIS2_PLACEMENT_3D('',#189967,#93266,#93267);
#82497=AXIS2_PLACEMENT_3D('',#189972,#93269,#93270);
#82498=AXIS2_PLACEMENT_3D('',#189975,#93272,#93273);
#82499=AXIS2_PLACEMENT_3D('',#189976,#93274,#93275);
#82500=AXIS2_PLACEMENT_3D('',#189980,#93277,#93278);
#82501=AXIS2_PLACEMENT_3D('',#189981,#93279,#93280);
#82502=AXIS2_PLACEMENT_3D('',#189982,#93281,#93282);
#82503=AXIS2_PLACEMENT_3D('',#189986,#93284,#93285);
#82504=AXIS2_PLACEMENT_3D('',#189987,#93286,#93287);
#82505=AXIS2_PLACEMENT_3D('',#189988,#93288,#93289);
#82506=AXIS2_PLACEMENT_3D('',#189989,#93290,#93291);
#82507=AXIS2_PLACEMENT_3D('',#189990,#93292,#93293);
#82508=AXIS2_PLACEMENT_3D('',#189991,#93294,#93295);
#82509=AXIS2_PLACEMENT_3D('',#189996,#93297,#93298);
#82510=AXIS2_PLACEMENT_3D('',#189999,#93300,#93301);
#82511=AXIS2_PLACEMENT_3D('',#190000,#93302,#93303);
#82512=AXIS2_PLACEMENT_3D('',#190004,#93305,#93306);
#82513=AXIS2_PLACEMENT_3D('',#190005,#93307,#93308);
#82514=AXIS2_PLACEMENT_3D('',#190006,#93309,#93310);
#82515=AXIS2_PLACEMENT_3D('',#190010,#93312,#93313);
#82516=AXIS2_PLACEMENT_3D('',#190011,#93314,#93315);
#82517=AXIS2_PLACEMENT_3D('',#190012,#93316,#93317);
#82518=AXIS2_PLACEMENT_3D('',#190013,#93318,#93319);
#82519=AXIS2_PLACEMENT_3D('',#190014,#93320,#93321);
#82520=AXIS2_PLACEMENT_3D('',#190015,#93322,#93323);
#82521=AXIS2_PLACEMENT_3D('',#190020,#93325,#93326);
#82522=AXIS2_PLACEMENT_3D('',#190023,#93328,#93329);
#82523=AXIS2_PLACEMENT_3D('',#190024,#93330,#93331);
#82524=AXIS2_PLACEMENT_3D('',#190028,#93333,#93334);
#82525=AXIS2_PLACEMENT_3D('',#190029,#93335,#93336);
#82526=AXIS2_PLACEMENT_3D('',#190030,#93337,#93338);
#82527=AXIS2_PLACEMENT_3D('',#190034,#93340,#93341);
#82528=AXIS2_PLACEMENT_3D('',#190035,#93342,#93343);
#82529=AXIS2_PLACEMENT_3D('',#190036,#93344,#93345);
#82530=AXIS2_PLACEMENT_3D('',#190037,#93346,#93347);
#82531=AXIS2_PLACEMENT_3D('',#190038,#93348,#93349);
#82532=AXIS2_PLACEMENT_3D('',#190039,#93350,#93351);
#82533=AXIS2_PLACEMENT_3D('',#190044,#93353,#93354);
#82534=AXIS2_PLACEMENT_3D('',#190047,#93356,#93357);
#82535=AXIS2_PLACEMENT_3D('',#190048,#93358,#93359);
#82536=AXIS2_PLACEMENT_3D('',#190052,#93361,#93362);
#82537=AXIS2_PLACEMENT_3D('',#190053,#93363,#93364);
#82538=AXIS2_PLACEMENT_3D('',#190054,#93365,#93366);
#82539=AXIS2_PLACEMENT_3D('',#190058,#93368,#93369);
#82540=AXIS2_PLACEMENT_3D('',#190059,#93370,#93371);
#82541=AXIS2_PLACEMENT_3D('',#190060,#93372,#93373);
#82542=AXIS2_PLACEMENT_3D('',#190061,#93374,#93375);
#82543=AXIS2_PLACEMENT_3D('',#190062,#93376,#93377);
#82544=AXIS2_PLACEMENT_3D('',#190063,#93378,#93379);
#82545=AXIS2_PLACEMENT_3D('',#190068,#93381,#93382);
#82546=AXIS2_PLACEMENT_3D('',#190071,#93384,#93385);
#82547=AXIS2_PLACEMENT_3D('',#190072,#93386,#93387);
#82548=AXIS2_PLACEMENT_3D('',#190076,#93389,#93390);
#82549=AXIS2_PLACEMENT_3D('',#190077,#93391,#93392);
#82550=AXIS2_PLACEMENT_3D('',#190078,#93393,#93394);
#82551=AXIS2_PLACEMENT_3D('',#190082,#93396,#93397);
#82552=AXIS2_PLACEMENT_3D('',#190083,#93398,#93399);
#82553=AXIS2_PLACEMENT_3D('',#190084,#93400,#93401);
#82554=AXIS2_PLACEMENT_3D('',#190085,#93402,#93403);
#82555=AXIS2_PLACEMENT_3D('',#190086,#93404,#93405);
#82556=AXIS2_PLACEMENT_3D('',#190087,#93406,#93407);
#82557=AXIS2_PLACEMENT_3D('',#190092,#93409,#93410);
#82558=AXIS2_PLACEMENT_3D('',#190095,#93412,#93413);
#82559=AXIS2_PLACEMENT_3D('',#190096,#93414,#93415);
#82560=AXIS2_PLACEMENT_3D('',#190100,#93417,#93418);
#82561=AXIS2_PLACEMENT_3D('',#190101,#93419,#93420);
#82562=AXIS2_PLACEMENT_3D('',#190102,#93421,#93422);
#82563=AXIS2_PLACEMENT_3D('',#190106,#93424,#93425);
#82564=AXIS2_PLACEMENT_3D('',#190107,#93426,#93427);
#82565=AXIS2_PLACEMENT_3D('',#190108,#93428,#93429);
#82566=AXIS2_PLACEMENT_3D('',#190109,#93430,#93431);
#82567=AXIS2_PLACEMENT_3D('',#190110,#93432,#93433);
#82568=AXIS2_PLACEMENT_3D('',#190111,#93434,#93435);
#82569=AXIS2_PLACEMENT_3D('',#190116,#93437,#93438);
#82570=AXIS2_PLACEMENT_3D('',#190119,#93440,#93441);
#82571=AXIS2_PLACEMENT_3D('',#190120,#93442,#93443);
#82572=AXIS2_PLACEMENT_3D('',#190124,#93445,#93446);
#82573=AXIS2_PLACEMENT_3D('',#190125,#93447,#93448);
#82574=AXIS2_PLACEMENT_3D('',#190126,#93449,#93450);
#82575=AXIS2_PLACEMENT_3D('',#190130,#93452,#93453);
#82576=AXIS2_PLACEMENT_3D('',#190131,#93454,#93455);
#82577=AXIS2_PLACEMENT_3D('',#190132,#93456,#93457);
#82578=AXIS2_PLACEMENT_3D('',#190133,#93458,#93459);
#82579=AXIS2_PLACEMENT_3D('',#190134,#93460,#93461);
#82580=AXIS2_PLACEMENT_3D('',#190135,#93462,#93463);
#82581=AXIS2_PLACEMENT_3D('',#190140,#93465,#93466);
#82582=AXIS2_PLACEMENT_3D('',#190143,#93468,#93469);
#82583=AXIS2_PLACEMENT_3D('',#190144,#93470,#93471);
#82584=AXIS2_PLACEMENT_3D('',#190148,#93473,#93474);
#82585=AXIS2_PLACEMENT_3D('',#190149,#93475,#93476);
#82586=AXIS2_PLACEMENT_3D('',#190150,#93477,#93478);
#82587=AXIS2_PLACEMENT_3D('',#190154,#93480,#93481);
#82588=AXIS2_PLACEMENT_3D('',#190155,#93482,#93483);
#82589=AXIS2_PLACEMENT_3D('',#190156,#93484,#93485);
#82590=AXIS2_PLACEMENT_3D('',#190157,#93486,#93487);
#82591=AXIS2_PLACEMENT_3D('',#190158,#93488,#93489);
#82592=AXIS2_PLACEMENT_3D('',#190159,#93490,#93491);
#82593=AXIS2_PLACEMENT_3D('',#190164,#93493,#93494);
#82594=AXIS2_PLACEMENT_3D('',#190167,#93496,#93497);
#82595=AXIS2_PLACEMENT_3D('',#190168,#93498,#93499);
#82596=AXIS2_PLACEMENT_3D('',#190172,#93501,#93502);
#82597=AXIS2_PLACEMENT_3D('',#190173,#93503,#93504);
#82598=AXIS2_PLACEMENT_3D('',#190174,#93505,#93506);
#82599=AXIS2_PLACEMENT_3D('',#190178,#93508,#93509);
#82600=AXIS2_PLACEMENT_3D('',#190179,#93510,#93511);
#82601=AXIS2_PLACEMENT_3D('',#190180,#93512,#93513);
#82602=AXIS2_PLACEMENT_3D('',#190181,#93514,#93515);
#82603=AXIS2_PLACEMENT_3D('',#190182,#93516,#93517);
#82604=AXIS2_PLACEMENT_3D('',#190183,#93518,#93519);
#82605=AXIS2_PLACEMENT_3D('',#190188,#93521,#93522);
#82606=AXIS2_PLACEMENT_3D('',#190191,#93524,#93525);
#82607=AXIS2_PLACEMENT_3D('',#190192,#93526,#93527);
#82608=AXIS2_PLACEMENT_3D('',#190196,#93529,#93530);
#82609=AXIS2_PLACEMENT_3D('',#190197,#93531,#93532);
#82610=AXIS2_PLACEMENT_3D('',#190198,#93533,#93534);
#82611=AXIS2_PLACEMENT_3D('',#190202,#93536,#93537);
#82612=AXIS2_PLACEMENT_3D('',#190203,#93538,#93539);
#82613=AXIS2_PLACEMENT_3D('',#190204,#93540,#93541);
#82614=AXIS2_PLACEMENT_3D('',#190205,#93542,#93543);
#82615=AXIS2_PLACEMENT_3D('',#190206,#93544,#93545);
#82616=AXIS2_PLACEMENT_3D('',#190207,#93546,#93547);
#82617=AXIS2_PLACEMENT_3D('',#190212,#93549,#93550);
#82618=AXIS2_PLACEMENT_3D('',#190215,#93552,#93553);
#82619=AXIS2_PLACEMENT_3D('',#190216,#93554,#93555);
#82620=AXIS2_PLACEMENT_3D('',#190220,#93557,#93558);
#82621=AXIS2_PLACEMENT_3D('',#190221,#93559,#93560);
#82622=AXIS2_PLACEMENT_3D('',#190222,#93561,#93562);
#82623=AXIS2_PLACEMENT_3D('',#190226,#93564,#93565);
#82624=AXIS2_PLACEMENT_3D('',#190227,#93566,#93567);
#82625=AXIS2_PLACEMENT_3D('',#190228,#93568,#93569);
#82626=AXIS2_PLACEMENT_3D('',#190229,#93570,#93571);
#82627=AXIS2_PLACEMENT_3D('',#190230,#93572,#93573);
#82628=AXIS2_PLACEMENT_3D('',#190231,#93574,#93575);
#82629=AXIS2_PLACEMENT_3D('',#190236,#93577,#93578);
#82630=AXIS2_PLACEMENT_3D('',#190239,#93580,#93581);
#82631=AXIS2_PLACEMENT_3D('',#190240,#93582,#93583);
#82632=AXIS2_PLACEMENT_3D('',#190246,#93586,#93587);
#82633=AXIS2_PLACEMENT_3D('',#190247,#93588,#93589);
#82634=AXIS2_PLACEMENT_3D('',#190248,#93590,#93591);
#82635=AXIS2_PLACEMENT_3D('',#190253,#93594,#93595);
#82636=AXIS2_PLACEMENT_3D('',#190254,#93596,#93597);
#82637=AXIS2_PLACEMENT_3D('',#190256,#93599,#93600);
#82638=AXIS2_PLACEMENT_3D('',#190257,#93601,#93602);
#82639=AXIS2_PLACEMENT_3D('',#190258,#93603,#93604);
#82640=AXIS2_PLACEMENT_3D('',#190259,#93605,#93606);
#82641=AXIS2_PLACEMENT_3D('',#190264,#93608,#93609);
#82642=AXIS2_PLACEMENT_3D('',#190267,#93611,#93612);
#82643=AXIS2_PLACEMENT_3D('',#190268,#93613,#93614);
#82644=AXIS2_PLACEMENT_3D('',#190274,#93617,#93618);
#82645=AXIS2_PLACEMENT_3D('',#190275,#93619,#93620);
#82646=AXIS2_PLACEMENT_3D('',#190276,#93621,#93622);
#82647=AXIS2_PLACEMENT_3D('',#190281,#93625,#93626);
#82648=AXIS2_PLACEMENT_3D('',#190282,#93627,#93628);
#82649=AXIS2_PLACEMENT_3D('',#190284,#93629,#93630);
#82650=AXIS2_PLACEMENT_3D('',#190286,#93632,#93633);
#82651=AXIS2_PLACEMENT_3D('',#190287,#93634,#93635);
#82652=AXIS2_PLACEMENT_3D('',#190288,#93636,#93637);
#82653=AXIS2_PLACEMENT_3D('',#190289,#93638,#93639);
#82654=AXIS2_PLACEMENT_3D('',#190294,#93641,#93642);
#82655=AXIS2_PLACEMENT_3D('',#190297,#93644,#93645);
#82656=AXIS2_PLACEMENT_3D('',#190298,#93646,#93647);
#82657=AXIS2_PLACEMENT_3D('',#190304,#93650,#93651);
#82658=AXIS2_PLACEMENT_3D('',#190305,#93652,#93653);
#82659=AXIS2_PLACEMENT_3D('',#190306,#93654,#93655);
#82660=AXIS2_PLACEMENT_3D('',#190311,#93658,#93659);
#82661=AXIS2_PLACEMENT_3D('',#190312,#93660,#93661);
#82662=AXIS2_PLACEMENT_3D('',#190314,#93662,#93663);
#82663=AXIS2_PLACEMENT_3D('',#190316,#93665,#93666);
#82664=AXIS2_PLACEMENT_3D('',#190317,#93667,#93668);
#82665=AXIS2_PLACEMENT_3D('',#190318,#93669,#93670);
#82666=AXIS2_PLACEMENT_3D('',#190319,#93671,#93672);
#82667=AXIS2_PLACEMENT_3D('',#190324,#93674,#93675);
#82668=AXIS2_PLACEMENT_3D('',#190327,#93677,#93678);
#82669=AXIS2_PLACEMENT_3D('',#190328,#93679,#93680);
#82670=AXIS2_PLACEMENT_3D('',#190334,#93683,#93684);
#82671=AXIS2_PLACEMENT_3D('',#190335,#93685,#93686);
#82672=AXIS2_PLACEMENT_3D('',#190336,#93687,#93688);
#82673=AXIS2_PLACEMENT_3D('',#190341,#93691,#93692);
#82674=AXIS2_PLACEMENT_3D('',#190342,#93693,#93694);
#82675=AXIS2_PLACEMENT_3D('',#190344,#93695,#93696);
#82676=AXIS2_PLACEMENT_3D('',#190346,#93698,#93699);
#82677=AXIS2_PLACEMENT_3D('',#190347,#93700,#93701);
#82678=AXIS2_PLACEMENT_3D('',#190348,#93702,#93703);
#82679=AXIS2_PLACEMENT_3D('',#190349,#93704,#93705);
#82680=AXIS2_PLACEMENT_3D('',#190354,#93707,#93708);
#82681=AXIS2_PLACEMENT_3D('',#190357,#93710,#93711);
#82682=AXIS2_PLACEMENT_3D('',#190358,#93712,#93713);
#82683=AXIS2_PLACEMENT_3D('',#190364,#93716,#93717);
#82684=AXIS2_PLACEMENT_3D('',#190365,#93718,#93719);
#82685=AXIS2_PLACEMENT_3D('',#190366,#93720,#93721);
#82686=AXIS2_PLACEMENT_3D('',#190371,#93724,#93725);
#82687=AXIS2_PLACEMENT_3D('',#190372,#93726,#93727);
#82688=AXIS2_PLACEMENT_3D('',#190374,#93728,#93729);
#82689=AXIS2_PLACEMENT_3D('',#190376,#93731,#93732);
#82690=AXIS2_PLACEMENT_3D('',#190377,#93733,#93734);
#82691=AXIS2_PLACEMENT_3D('',#190378,#93735,#93736);
#82692=AXIS2_PLACEMENT_3D('',#190379,#93737,#93738);
#82693=AXIS2_PLACEMENT_3D('',#190386,#93741,#93742);
#82694=AXIS2_PLACEMENT_3D('',#190389,#93744,#93745);
#82695=AXIS2_PLACEMENT_3D('',#190390,#93746,#93747);
#82696=AXIS2_PLACEMENT_3D('',#190395,#93750,#93751);
#82697=AXIS2_PLACEMENT_3D('',#190396,#93752,#93753);
#82698=AXIS2_PLACEMENT_3D('',#190401,#93756,#93757);
#82699=AXIS2_PLACEMENT_3D('',#190402,#93758,#93759);
#82700=AXIS2_PLACEMENT_3D('',#190404,#93760,#93761);
#82701=AXIS2_PLACEMENT_3D('',#190406,#93763,#93764);
#82702=AXIS2_PLACEMENT_3D('',#190407,#93765,#93766);
#82703=AXIS2_PLACEMENT_3D('',#190408,#93767,#93768);
#82704=AXIS2_PLACEMENT_3D('',#190409,#93769,#93770);
#82705=AXIS2_PLACEMENT_3D('',#190416,#93773,#93774);
#82706=AXIS2_PLACEMENT_3D('',#190419,#93776,#93777);
#82707=AXIS2_PLACEMENT_3D('',#190420,#93778,#93779);
#82708=AXIS2_PLACEMENT_3D('',#190425,#93782,#93783);
#82709=AXIS2_PLACEMENT_3D('',#190426,#93784,#93785);
#82710=AXIS2_PLACEMENT_3D('',#190431,#93788,#93789);
#82711=AXIS2_PLACEMENT_3D('',#190432,#93790,#93791);
#82712=AXIS2_PLACEMENT_3D('',#190434,#93792,#93793);
#82713=AXIS2_PLACEMENT_3D('',#190436,#93795,#93796);
#82714=AXIS2_PLACEMENT_3D('',#190437,#93797,#93798);
#82715=AXIS2_PLACEMENT_3D('',#190438,#93799,#93800);
#82716=AXIS2_PLACEMENT_3D('',#190439,#93801,#93802);
#82717=AXIS2_PLACEMENT_3D('',#190444,#93804,#93805);
#82718=AXIS2_PLACEMENT_3D('',#190447,#93807,#93808);
#82719=AXIS2_PLACEMENT_3D('',#190448,#93809,#93810);
#82720=AXIS2_PLACEMENT_3D('',#190454,#93813,#93814);
#82721=AXIS2_PLACEMENT_3D('',#190455,#93815,#93816);
#82722=AXIS2_PLACEMENT_3D('',#190456,#93817,#93818);
#82723=AXIS2_PLACEMENT_3D('',#190461,#93821,#93822);
#82724=AXIS2_PLACEMENT_3D('',#190462,#93823,#93824);
#82725=AXIS2_PLACEMENT_3D('',#190464,#93825,#93826);
#82726=AXIS2_PLACEMENT_3D('',#190466,#93828,#93829);
#82727=AXIS2_PLACEMENT_3D('',#190467,#93830,#93831);
#82728=AXIS2_PLACEMENT_3D('',#190468,#93832,#93833);
#82729=AXIS2_PLACEMENT_3D('',#190469,#93834,#93835);
#82730=AXIS2_PLACEMENT_3D('',#190474,#93837,#93838);
#82731=AXIS2_PLACEMENT_3D('',#190477,#93840,#93841);
#82732=AXIS2_PLACEMENT_3D('',#190478,#93842,#93843);
#82733=AXIS2_PLACEMENT_3D('',#190484,#93846,#93847);
#82734=AXIS2_PLACEMENT_3D('',#190485,#93848,#93849);
#82735=AXIS2_PLACEMENT_3D('',#190486,#93850,#93851);
#82736=AXIS2_PLACEMENT_3D('',#190491,#93854,#93855);
#82737=AXIS2_PLACEMENT_3D('',#190492,#93856,#93857);
#82738=AXIS2_PLACEMENT_3D('',#190494,#93858,#93859);
#82739=AXIS2_PLACEMENT_3D('',#190496,#93861,#93862);
#82740=AXIS2_PLACEMENT_3D('',#190497,#93863,#93864);
#82741=AXIS2_PLACEMENT_3D('',#190498,#93865,#93866);
#82742=AXIS2_PLACEMENT_3D('',#190499,#93867,#93868);
#82743=AXIS2_PLACEMENT_3D('',#190504,#93870,#93871);
#82744=AXIS2_PLACEMENT_3D('',#190507,#93873,#93874);
#82745=AXIS2_PLACEMENT_3D('',#190508,#93875,#93876);
#82746=AXIS2_PLACEMENT_3D('',#190514,#93879,#93880);
#82747=AXIS2_PLACEMENT_3D('',#190515,#93881,#93882);
#82748=AXIS2_PLACEMENT_3D('',#190516,#93883,#93884);
#82749=AXIS2_PLACEMENT_3D('',#190521,#93887,#93888);
#82750=AXIS2_PLACEMENT_3D('',#190522,#93889,#93890);
#82751=AXIS2_PLACEMENT_3D('',#190524,#93891,#93892);
#82752=AXIS2_PLACEMENT_3D('',#190526,#93894,#93895);
#82753=AXIS2_PLACEMENT_3D('',#190527,#93896,#93897);
#82754=AXIS2_PLACEMENT_3D('',#190528,#93898,#93899);
#82755=AXIS2_PLACEMENT_3D('',#190529,#93900,#93901);
#82756=AXIS2_PLACEMENT_3D('',#190534,#93903,#93904);
#82757=AXIS2_PLACEMENT_3D('',#190537,#93906,#93907);
#82758=AXIS2_PLACEMENT_3D('',#190538,#93908,#93909);
#82759=AXIS2_PLACEMENT_3D('',#190542,#93911,#93912);
#82760=AXIS2_PLACEMENT_3D('',#190543,#93913,#93914);
#82761=AXIS2_PLACEMENT_3D('',#190544,#93915,#93916);
#82762=AXIS2_PLACEMENT_3D('',#190548,#93918,#93919);
#82763=AXIS2_PLACEMENT_3D('',#190549,#93920,#93921);
#82764=AXIS2_PLACEMENT_3D('',#190550,#93922,#93923);
#82765=AXIS2_PLACEMENT_3D('',#190551,#93924,#93925);
#82766=AXIS2_PLACEMENT_3D('',#190552,#93926,#93927);
#82767=AXIS2_PLACEMENT_3D('',#190553,#93928,#93929);
#82768=AXIS2_PLACEMENT_3D('',#190558,#93931,#93932);
#82769=AXIS2_PLACEMENT_3D('',#190561,#93934,#93935);
#82770=AXIS2_PLACEMENT_3D('',#190562,#93936,#93937);
#82771=AXIS2_PLACEMENT_3D('',#190566,#93939,#93940);
#82772=AXIS2_PLACEMENT_3D('',#190567,#93941,#93942);
#82773=AXIS2_PLACEMENT_3D('',#190568,#93943,#93944);
#82774=AXIS2_PLACEMENT_3D('',#190572,#93946,#93947);
#82775=AXIS2_PLACEMENT_3D('',#190573,#93948,#93949);
#82776=AXIS2_PLACEMENT_3D('',#190574,#93950,#93951);
#82777=AXIS2_PLACEMENT_3D('',#190575,#93952,#93953);
#82778=AXIS2_PLACEMENT_3D('',#190576,#93954,#93955);
#82779=AXIS2_PLACEMENT_3D('',#190577,#93956,#93957);
#82780=AXIS2_PLACEMENT_3D('',#190582,#93959,#93960);
#82781=AXIS2_PLACEMENT_3D('',#190585,#93962,#93963);
#82782=AXIS2_PLACEMENT_3D('',#190586,#93964,#93965);
#82783=AXIS2_PLACEMENT_3D('',#190590,#93967,#93968);
#82784=AXIS2_PLACEMENT_3D('',#190591,#93969,#93970);
#82785=AXIS2_PLACEMENT_3D('',#190592,#93971,#93972);
#82786=AXIS2_PLACEMENT_3D('',#190596,#93974,#93975);
#82787=AXIS2_PLACEMENT_3D('',#190597,#93976,#93977);
#82788=AXIS2_PLACEMENT_3D('',#190598,#93978,#93979);
#82789=AXIS2_PLACEMENT_3D('',#190599,#93980,#93981);
#82790=AXIS2_PLACEMENT_3D('',#190600,#93982,#93983);
#82791=AXIS2_PLACEMENT_3D('',#190601,#93984,#93985);
#82792=AXIS2_PLACEMENT_3D('',#190606,#93987,#93988);
#82793=AXIS2_PLACEMENT_3D('',#190609,#93990,#93991);
#82794=AXIS2_PLACEMENT_3D('',#190610,#93992,#93993);
#82795=AXIS2_PLACEMENT_3D('',#190614,#93995,#93996);
#82796=AXIS2_PLACEMENT_3D('',#190615,#93997,#93998);
#82797=AXIS2_PLACEMENT_3D('',#190616,#93999,#94000);
#82798=AXIS2_PLACEMENT_3D('',#190620,#94002,#94003);
#82799=AXIS2_PLACEMENT_3D('',#190621,#94004,#94005);
#82800=AXIS2_PLACEMENT_3D('',#190622,#94006,#94007);
#82801=AXIS2_PLACEMENT_3D('',#190623,#94008,#94009);
#82802=AXIS2_PLACEMENT_3D('',#190624,#94010,#94011);
#82803=AXIS2_PLACEMENT_3D('',#190625,#94012,#94013);
#82804=AXIS2_PLACEMENT_3D('',#190630,#94015,#94016);
#82805=AXIS2_PLACEMENT_3D('',#190633,#94018,#94019);
#82806=AXIS2_PLACEMENT_3D('',#190634,#94020,#94021);
#82807=AXIS2_PLACEMENT_3D('',#190638,#94023,#94024);
#82808=AXIS2_PLACEMENT_3D('',#190639,#94025,#94026);
#82809=AXIS2_PLACEMENT_3D('',#190640,#94027,#94028);
#82810=AXIS2_PLACEMENT_3D('',#190644,#94030,#94031);
#82811=AXIS2_PLACEMENT_3D('',#190645,#94032,#94033);
#82812=AXIS2_PLACEMENT_3D('',#190646,#94034,#94035);
#82813=AXIS2_PLACEMENT_3D('',#190647,#94036,#94037);
#82814=AXIS2_PLACEMENT_3D('',#190648,#94038,#94039);
#82815=AXIS2_PLACEMENT_3D('',#190649,#94040,#94041);
#82816=AXIS2_PLACEMENT_3D('',#190654,#94043,#94044);
#82817=AXIS2_PLACEMENT_3D('',#190657,#94046,#94047);
#82818=AXIS2_PLACEMENT_3D('',#190658,#94048,#94049);
#82819=AXIS2_PLACEMENT_3D('',#190662,#94051,#94052);
#82820=AXIS2_PLACEMENT_3D('',#190663,#94053,#94054);
#82821=AXIS2_PLACEMENT_3D('',#190664,#94055,#94056);
#82822=AXIS2_PLACEMENT_3D('',#190668,#94058,#94059);
#82823=AXIS2_PLACEMENT_3D('',#190669,#94060,#94061);
#82824=AXIS2_PLACEMENT_3D('',#190670,#94062,#94063);
#82825=AXIS2_PLACEMENT_3D('',#190671,#94064,#94065);
#82826=AXIS2_PLACEMENT_3D('',#190672,#94066,#94067);
#82827=AXIS2_PLACEMENT_3D('',#190673,#94068,#94069);
#82828=AXIS2_PLACEMENT_3D('',#190678,#94071,#94072);
#82829=AXIS2_PLACEMENT_3D('',#190681,#94074,#94075);
#82830=AXIS2_PLACEMENT_3D('',#190682,#94076,#94077);
#82831=AXIS2_PLACEMENT_3D('',#190686,#94079,#94080);
#82832=AXIS2_PLACEMENT_3D('',#190687,#94081,#94082);
#82833=AXIS2_PLACEMENT_3D('',#190688,#94083,#94084);
#82834=AXIS2_PLACEMENT_3D('',#190692,#94086,#94087);
#82835=AXIS2_PLACEMENT_3D('',#190693,#94088,#94089);
#82836=AXIS2_PLACEMENT_3D('',#190694,#94090,#94091);
#82837=AXIS2_PLACEMENT_3D('',#190695,#94092,#94093);
#82838=AXIS2_PLACEMENT_3D('',#190696,#94094,#94095);
#82839=AXIS2_PLACEMENT_3D('',#190697,#94096,#94097);
#82840=AXIS2_PLACEMENT_3D('',#190702,#94099,#94100);
#82841=AXIS2_PLACEMENT_3D('',#190705,#94102,#94103);
#82842=AXIS2_PLACEMENT_3D('',#190706,#94104,#94105);
#82843=AXIS2_PLACEMENT_3D('',#190710,#94107,#94108);
#82844=AXIS2_PLACEMENT_3D('',#190711,#94109,#94110);
#82845=AXIS2_PLACEMENT_3D('',#190712,#94111,#94112);
#82846=AXIS2_PLACEMENT_3D('',#190716,#94114,#94115);
#82847=AXIS2_PLACEMENT_3D('',#190717,#94116,#94117);
#82848=AXIS2_PLACEMENT_3D('',#190718,#94118,#94119);
#82849=AXIS2_PLACEMENT_3D('',#190719,#94120,#94121);
#82850=AXIS2_PLACEMENT_3D('',#190720,#94122,#94123);
#82851=AXIS2_PLACEMENT_3D('',#190721,#94124,#94125);
#82852=AXIS2_PLACEMENT_3D('',#190728,#94128,#94129);
#82853=AXIS2_PLACEMENT_3D('',#190731,#94131,#94132);
#82854=AXIS2_PLACEMENT_3D('',#190732,#94133,#94134);
#82855=AXIS2_PLACEMENT_3D('',#190737,#94137,#94138);
#82856=AXIS2_PLACEMENT_3D('',#190738,#94139,#94140);
#82857=AXIS2_PLACEMENT_3D('',#190743,#94143,#94144);
#82858=AXIS2_PLACEMENT_3D('',#190744,#94145,#94146);
#82859=AXIS2_PLACEMENT_3D('',#190746,#94147,#94148);
#82860=AXIS2_PLACEMENT_3D('',#190748,#94150,#94151);
#82861=AXIS2_PLACEMENT_3D('',#190749,#94152,#94153);
#82862=AXIS2_PLACEMENT_3D('',#190750,#94154,#94155);
#82863=AXIS2_PLACEMENT_3D('',#190751,#94156,#94157);
#82864=AXIS2_PLACEMENT_3D('',#190758,#94160,#94161);
#82865=AXIS2_PLACEMENT_3D('',#190761,#94163,#94164);
#82866=AXIS2_PLACEMENT_3D('',#190762,#94165,#94166);
#82867=AXIS2_PLACEMENT_3D('',#190767,#94169,#94170);
#82868=AXIS2_PLACEMENT_3D('',#190768,#94171,#94172);
#82869=AXIS2_PLACEMENT_3D('',#190773,#94175,#94176);
#82870=AXIS2_PLACEMENT_3D('',#190774,#94177,#94178);
#82871=AXIS2_PLACEMENT_3D('',#190776,#94179,#94180);
#82872=AXIS2_PLACEMENT_3D('',#190778,#94182,#94183);
#82873=AXIS2_PLACEMENT_3D('',#190779,#94184,#94185);
#82874=AXIS2_PLACEMENT_3D('',#190780,#94186,#94187);
#82875=AXIS2_PLACEMENT_3D('',#190781,#94188,#94189);
#82876=AXIS2_PLACEMENT_3D('',#190786,#94191,#94192);
#82877=AXIS2_PLACEMENT_3D('',#190789,#94194,#94195);
#82878=AXIS2_PLACEMENT_3D('',#190790,#94196,#94197);
#82879=AXIS2_PLACEMENT_3D('',#190794,#94199,#94200);
#82880=AXIS2_PLACEMENT_3D('',#190795,#94201,#94202);
#82881=AXIS2_PLACEMENT_3D('',#190796,#94203,#94204);
#82882=AXIS2_PLACEMENT_3D('',#190800,#94206,#94207);
#82883=AXIS2_PLACEMENT_3D('',#190801,#94208,#94209);
#82884=AXIS2_PLACEMENT_3D('',#190802,#94210,#94211);
#82885=AXIS2_PLACEMENT_3D('',#190803,#94212,#94213);
#82886=AXIS2_PLACEMENT_3D('',#190804,#94214,#94215);
#82887=AXIS2_PLACEMENT_3D('',#190805,#94216,#94217);
#82888=AXIS2_PLACEMENT_3D('',#190810,#94219,#94220);
#82889=AXIS2_PLACEMENT_3D('',#190813,#94222,#94223);
#82890=AXIS2_PLACEMENT_3D('',#190814,#94224,#94225);
#82891=AXIS2_PLACEMENT_3D('',#190818,#94227,#94228);
#82892=AXIS2_PLACEMENT_3D('',#190819,#94229,#94230);
#82893=AXIS2_PLACEMENT_3D('',#190820,#94231,#94232);
#82894=AXIS2_PLACEMENT_3D('',#190824,#94234,#94235);
#82895=AXIS2_PLACEMENT_3D('',#190825,#94236,#94237);
#82896=AXIS2_PLACEMENT_3D('',#190826,#94238,#94239);
#82897=AXIS2_PLACEMENT_3D('',#190827,#94240,#94241);
#82898=AXIS2_PLACEMENT_3D('',#190828,#94242,#94243);
#82899=AXIS2_PLACEMENT_3D('',#190829,#94244,#94245);
#82900=AXIS2_PLACEMENT_3D('',#190834,#94247,#94248);
#82901=AXIS2_PLACEMENT_3D('',#190837,#94250,#94251);
#82902=AXIS2_PLACEMENT_3D('',#190838,#94252,#94253);
#82903=AXIS2_PLACEMENT_3D('',#190842,#94255,#94256);
#82904=AXIS2_PLACEMENT_3D('',#190843,#94257,#94258);
#82905=AXIS2_PLACEMENT_3D('',#190844,#94259,#94260);
#82906=AXIS2_PLACEMENT_3D('',#190848,#94262,#94263);
#82907=AXIS2_PLACEMENT_3D('',#190849,#94264,#94265);
#82908=AXIS2_PLACEMENT_3D('',#190850,#94266,#94267);
#82909=AXIS2_PLACEMENT_3D('',#190851,#94268,#94269);
#82910=AXIS2_PLACEMENT_3D('',#190852,#94270,#94271);
#82911=AXIS2_PLACEMENT_3D('',#190853,#94272,#94273);
#82912=AXIS2_PLACEMENT_3D('',#190858,#94275,#94276);
#82913=AXIS2_PLACEMENT_3D('',#190861,#94278,#94279);
#82914=AXIS2_PLACEMENT_3D('',#190862,#94280,#94281);
#82915=AXIS2_PLACEMENT_3D('',#190866,#94283,#94284);
#82916=AXIS2_PLACEMENT_3D('',#190867,#94285,#94286);
#82917=AXIS2_PLACEMENT_3D('',#190868,#94287,#94288);
#82918=AXIS2_PLACEMENT_3D('',#190872,#94290,#94291);
#82919=AXIS2_PLACEMENT_3D('',#190873,#94292,#94293);
#82920=AXIS2_PLACEMENT_3D('',#190874,#94294,#94295);
#82921=AXIS2_PLACEMENT_3D('',#190875,#94296,#94297);
#82922=AXIS2_PLACEMENT_3D('',#190876,#94298,#94299);
#82923=AXIS2_PLACEMENT_3D('',#190877,#94300,#94301);
#82924=AXIS2_PLACEMENT_3D('',#190882,#94303,#94304);
#82925=AXIS2_PLACEMENT_3D('',#190885,#94306,#94307);
#82926=AXIS2_PLACEMENT_3D('',#190886,#94308,#94309);
#82927=AXIS2_PLACEMENT_3D('',#190890,#94311,#94312);
#82928=AXIS2_PLACEMENT_3D('',#190891,#94313,#94314);
#82929=AXIS2_PLACEMENT_3D('',#190892,#94315,#94316);
#82930=AXIS2_PLACEMENT_3D('',#190898,#94319,#94320);
#82931=AXIS2_PLACEMENT_3D('',#190899,#94321,#94322);
#82932=AXIS2_PLACEMENT_3D('',#190900,#94323,#94324);
#82933=AXIS2_PLACEMENT_3D('',#190902,#94325,#94326);
#82934=AXIS2_PLACEMENT_3D('',#190904,#94328,#94329);
#82935=AXIS2_PLACEMENT_3D('',#190905,#94330,#94331);
#82936=AXIS2_PLACEMENT_3D('',#190906,#94332,#94333);
#82937=AXIS2_PLACEMENT_3D('',#190907,#94334,#94335);
#82938=AXIS2_PLACEMENT_3D('',#190912,#94337,#94338);
#82939=AXIS2_PLACEMENT_3D('',#190915,#94340,#94341);
#82940=AXIS2_PLACEMENT_3D('',#190916,#94342,#94343);
#82941=AXIS2_PLACEMENT_3D('',#190922,#94346,#94347);
#82942=AXIS2_PLACEMENT_3D('',#190923,#94348,#94349);
#82943=AXIS2_PLACEMENT_3D('',#190924,#94350,#94351);
#82944=AXIS2_PLACEMENT_3D('',#190929,#94354,#94355);
#82945=AXIS2_PLACEMENT_3D('',#190930,#94356,#94357);
#82946=AXIS2_PLACEMENT_3D('',#190932,#94358,#94359);
#82947=AXIS2_PLACEMENT_3D('',#190934,#94361,#94362);
#82948=AXIS2_PLACEMENT_3D('',#190935,#94363,#94364);
#82949=AXIS2_PLACEMENT_3D('',#190936,#94365,#94366);
#82950=AXIS2_PLACEMENT_3D('',#190937,#94367,#94368);
#82951=AXIS2_PLACEMENT_3D('',#190942,#94370,#94371);
#82952=AXIS2_PLACEMENT_3D('',#190945,#94373,#94374);
#82953=AXIS2_PLACEMENT_3D('',#190946,#94375,#94376);
#82954=AXIS2_PLACEMENT_3D('',#190952,#94379,#94380);
#82955=AXIS2_PLACEMENT_3D('',#190953,#94381,#94382);
#82956=AXIS2_PLACEMENT_3D('',#190954,#94383,#94384);
#82957=AXIS2_PLACEMENT_3D('',#190959,#94387,#94388);
#82958=AXIS2_PLACEMENT_3D('',#190960,#94389,#94390);
#82959=AXIS2_PLACEMENT_3D('',#190962,#94391,#94392);
#82960=AXIS2_PLACEMENT_3D('',#190964,#94394,#94395);
#82961=AXIS2_PLACEMENT_3D('',#190965,#94396,#94397);
#82962=AXIS2_PLACEMENT_3D('',#190966,#94398,#94399);
#82963=AXIS2_PLACEMENT_3D('',#190967,#94400,#94401);
#82964=AXIS2_PLACEMENT_3D('',#190972,#94403,#94404);
#82965=AXIS2_PLACEMENT_3D('',#190975,#94406,#94407);
#82966=AXIS2_PLACEMENT_3D('',#190976,#94408,#94409);
#82967=AXIS2_PLACEMENT_3D('',#190980,#94411,#94412);
#82968=AXIS2_PLACEMENT_3D('',#190981,#94413,#94414);
#82969=AXIS2_PLACEMENT_3D('',#190982,#94415,#94416);
#82970=AXIS2_PLACEMENT_3D('',#190988,#94419,#94420);
#82971=AXIS2_PLACEMENT_3D('',#190989,#94421,#94422);
#82972=AXIS2_PLACEMENT_3D('',#190990,#94423,#94424);
#82973=AXIS2_PLACEMENT_3D('',#190992,#94425,#94426);
#82974=AXIS2_PLACEMENT_3D('',#190994,#94428,#94429);
#82975=AXIS2_PLACEMENT_3D('',#190995,#94430,#94431);
#82976=AXIS2_PLACEMENT_3D('',#190996,#94432,#94433);
#82977=AXIS2_PLACEMENT_3D('',#190997,#94434,#94435);
#82978=AXIS2_PLACEMENT_3D('',#191002,#94437,#94438);
#82979=AXIS2_PLACEMENT_3D('',#191005,#94440,#94441);
#82980=AXIS2_PLACEMENT_3D('',#191006,#94442,#94443);
#82981=AXIS2_PLACEMENT_3D('',#191010,#94445,#94446);
#82982=AXIS2_PLACEMENT_3D('',#191011,#94447,#94448);
#82983=AXIS2_PLACEMENT_3D('',#191012,#94449,#94450);
#82984=AXIS2_PLACEMENT_3D('',#191016,#94452,#94453);
#82985=AXIS2_PLACEMENT_3D('',#191017,#94454,#94455);
#82986=AXIS2_PLACEMENT_3D('',#191018,#94456,#94457);
#82987=AXIS2_PLACEMENT_3D('',#191019,#94458,#94459);
#82988=AXIS2_PLACEMENT_3D('',#191020,#94460,#94461);
#82989=AXIS2_PLACEMENT_3D('',#191021,#94462,#94463);
#82990=AXIS2_PLACEMENT_3D('',#191026,#94465,#94466);
#82991=AXIS2_PLACEMENT_3D('',#191029,#94468,#94469);
#82992=AXIS2_PLACEMENT_3D('',#191030,#94470,#94471);
#82993=AXIS2_PLACEMENT_3D('',#191034,#94473,#94474);
#82994=AXIS2_PLACEMENT_3D('',#191035,#94475,#94476);
#82995=AXIS2_PLACEMENT_3D('',#191036,#94477,#94478);
#82996=AXIS2_PLACEMENT_3D('',#191040,#94480,#94481);
#82997=AXIS2_PLACEMENT_3D('',#191041,#94482,#94483);
#82998=AXIS2_PLACEMENT_3D('',#191042,#94484,#94485);
#82999=AXIS2_PLACEMENT_3D('',#191043,#94486,#94487);
#83000=AXIS2_PLACEMENT_3D('',#191044,#94488,#94489);
#83001=AXIS2_PLACEMENT_3D('',#191045,#94490,#94491);
#83002=AXIS2_PLACEMENT_3D('',#191050,#94493,#94494);
#83003=AXIS2_PLACEMENT_3D('',#191053,#94496,#94497);
#83004=AXIS2_PLACEMENT_3D('',#191054,#94498,#94499);
#83005=AXIS2_PLACEMENT_3D('',#191058,#94501,#94502);
#83006=AXIS2_PLACEMENT_3D('',#191059,#94503,#94504);
#83007=AXIS2_PLACEMENT_3D('',#191060,#94505,#94506);
#83008=AXIS2_PLACEMENT_3D('',#191064,#94508,#94509);
#83009=AXIS2_PLACEMENT_3D('',#191065,#94510,#94511);
#83010=AXIS2_PLACEMENT_3D('',#191066,#94512,#94513);
#83011=AXIS2_PLACEMENT_3D('',#191067,#94514,#94515);
#83012=AXIS2_PLACEMENT_3D('',#191068,#94516,#94517);
#83013=AXIS2_PLACEMENT_3D('',#191069,#94518,#94519);
#83014=AXIS2_PLACEMENT_3D('',#191074,#94521,#94522);
#83015=AXIS2_PLACEMENT_3D('',#191077,#94524,#94525);
#83016=AXIS2_PLACEMENT_3D('',#191078,#94526,#94527);
#83017=AXIS2_PLACEMENT_3D('',#191082,#94529,#94530);
#83018=AXIS2_PLACEMENT_3D('',#191083,#94531,#94532);
#83019=AXIS2_PLACEMENT_3D('',#191084,#94533,#94534);
#83020=AXIS2_PLACEMENT_3D('',#191088,#94536,#94537);
#83021=AXIS2_PLACEMENT_3D('',#191089,#94538,#94539);
#83022=AXIS2_PLACEMENT_3D('',#191090,#94540,#94541);
#83023=AXIS2_PLACEMENT_3D('',#191091,#94542,#94543);
#83024=AXIS2_PLACEMENT_3D('',#191092,#94544,#94545);
#83025=AXIS2_PLACEMENT_3D('',#191093,#94546,#94547);
#83026=AXIS2_PLACEMENT_3D('',#191098,#94549,#94550);
#83027=AXIS2_PLACEMENT_3D('',#191101,#94552,#94553);
#83028=AXIS2_PLACEMENT_3D('',#191102,#94554,#94555);
#83029=AXIS2_PLACEMENT_3D('',#191106,#94557,#94558);
#83030=AXIS2_PLACEMENT_3D('',#191107,#94559,#94560);
#83031=AXIS2_PLACEMENT_3D('',#191108,#94561,#94562);
#83032=AXIS2_PLACEMENT_3D('',#191112,#94564,#94565);
#83033=AXIS2_PLACEMENT_3D('',#191113,#94566,#94567);
#83034=AXIS2_PLACEMENT_3D('',#191114,#94568,#94569);
#83035=AXIS2_PLACEMENT_3D('',#191115,#94570,#94571);
#83036=AXIS2_PLACEMENT_3D('',#191116,#94572,#94573);
#83037=AXIS2_PLACEMENT_3D('',#191117,#94574,#94575);
#83038=AXIS2_PLACEMENT_3D('',#191122,#94577,#94578);
#83039=AXIS2_PLACEMENT_3D('',#191125,#94580,#94581);
#83040=AXIS2_PLACEMENT_3D('',#191126,#94582,#94583);
#83041=AXIS2_PLACEMENT_3D('',#191130,#94585,#94586);
#83042=AXIS2_PLACEMENT_3D('',#191131,#94587,#94588);
#83043=AXIS2_PLACEMENT_3D('',#191132,#94589,#94590);
#83044=AXIS2_PLACEMENT_3D('',#191136,#94592,#94593);
#83045=AXIS2_PLACEMENT_3D('',#191137,#94594,#94595);
#83046=AXIS2_PLACEMENT_3D('',#191138,#94596,#94597);
#83047=AXIS2_PLACEMENT_3D('',#191139,#94598,#94599);
#83048=AXIS2_PLACEMENT_3D('',#191140,#94600,#94601);
#83049=AXIS2_PLACEMENT_3D('',#191141,#94602,#94603);
#83050=AXIS2_PLACEMENT_3D('',#191146,#94605,#94606);
#83051=AXIS2_PLACEMENT_3D('',#191149,#94608,#94609);
#83052=AXIS2_PLACEMENT_3D('',#191150,#94610,#94611);
#83053=AXIS2_PLACEMENT_3D('',#191154,#94613,#94614);
#83054=AXIS2_PLACEMENT_3D('',#191155,#94615,#94616);
#83055=AXIS2_PLACEMENT_3D('',#191156,#94617,#94618);
#83056=AXIS2_PLACEMENT_3D('',#191160,#94620,#94621);
#83057=AXIS2_PLACEMENT_3D('',#191161,#94622,#94623);
#83058=AXIS2_PLACEMENT_3D('',#191162,#94624,#94625);
#83059=AXIS2_PLACEMENT_3D('',#191163,#94626,#94627);
#83060=AXIS2_PLACEMENT_3D('',#191164,#94628,#94629);
#83061=AXIS2_PLACEMENT_3D('',#191165,#94630,#94631);
#83062=AXIS2_PLACEMENT_3D('',#191170,#94633,#94634);
#83063=AXIS2_PLACEMENT_3D('',#191173,#94636,#94637);
#83064=AXIS2_PLACEMENT_3D('',#191174,#94638,#94639);
#83065=AXIS2_PLACEMENT_3D('',#191178,#94641,#94642);
#83066=AXIS2_PLACEMENT_3D('',#191179,#94643,#94644);
#83067=AXIS2_PLACEMENT_3D('',#191180,#94645,#94646);
#83068=AXIS2_PLACEMENT_3D('',#191184,#94648,#94649);
#83069=AXIS2_PLACEMENT_3D('',#191185,#94650,#94651);
#83070=AXIS2_PLACEMENT_3D('',#191186,#94652,#94653);
#83071=AXIS2_PLACEMENT_3D('',#191187,#94654,#94655);
#83072=AXIS2_PLACEMENT_3D('',#191188,#94656,#94657);
#83073=AXIS2_PLACEMENT_3D('',#191189,#94658,#94659);
#83074=AXIS2_PLACEMENT_3D('',#191194,#94661,#94662);
#83075=AXIS2_PLACEMENT_3D('',#191197,#94664,#94665);
#83076=AXIS2_PLACEMENT_3D('',#191198,#94666,#94667);
#83077=AXIS2_PLACEMENT_3D('',#191202,#94669,#94670);
#83078=AXIS2_PLACEMENT_3D('',#191203,#94671,#94672);
#83079=AXIS2_PLACEMENT_3D('',#191204,#94673,#94674);
#83080=AXIS2_PLACEMENT_3D('',#191208,#94676,#94677);
#83081=AXIS2_PLACEMENT_3D('',#191209,#94678,#94679);
#83082=AXIS2_PLACEMENT_3D('',#191210,#94680,#94681);
#83083=AXIS2_PLACEMENT_3D('',#191211,#94682,#94683);
#83084=AXIS2_PLACEMENT_3D('',#191212,#94684,#94685);
#83085=AXIS2_PLACEMENT_3D('',#191213,#94686,#94687);
#83086=AXIS2_PLACEMENT_3D('',#191218,#94689,#94690);
#83087=AXIS2_PLACEMENT_3D('',#191221,#94692,#94693);
#83088=AXIS2_PLACEMENT_3D('',#191222,#94694,#94695);
#83089=AXIS2_PLACEMENT_3D('',#191226,#94697,#94698);
#83090=AXIS2_PLACEMENT_3D('',#191227,#94699,#94700);
#83091=AXIS2_PLACEMENT_3D('',#191228,#94701,#94702);
#83092=AXIS2_PLACEMENT_3D('',#191232,#94704,#94705);
#83093=AXIS2_PLACEMENT_3D('',#191233,#94706,#94707);
#83094=AXIS2_PLACEMENT_3D('',#191234,#94708,#94709);
#83095=AXIS2_PLACEMENT_3D('',#191235,#94710,#94711);
#83096=AXIS2_PLACEMENT_3D('',#191236,#94712,#94713);
#83097=AXIS2_PLACEMENT_3D('',#191237,#94714,#94715);
#83098=AXIS2_PLACEMENT_3D('',#191242,#94717,#94718);
#83099=AXIS2_PLACEMENT_3D('',#191245,#94720,#94721);
#83100=AXIS2_PLACEMENT_3D('',#191246,#94722,#94723);
#83101=AXIS2_PLACEMENT_3D('',#191250,#94725,#94726);
#83102=AXIS2_PLACEMENT_3D('',#191251,#94727,#94728);
#83103=AXIS2_PLACEMENT_3D('',#191252,#94729,#94730);
#83104=AXIS2_PLACEMENT_3D('',#191258,#94733,#94734);
#83105=AXIS2_PLACEMENT_3D('',#191259,#94735,#94736);
#83106=AXIS2_PLACEMENT_3D('',#191260,#94737,#94738);
#83107=AXIS2_PLACEMENT_3D('',#191262,#94739,#94740);
#83108=AXIS2_PLACEMENT_3D('',#191264,#94742,#94743);
#83109=AXIS2_PLACEMENT_3D('',#191265,#94744,#94745);
#83110=AXIS2_PLACEMENT_3D('',#191266,#94746,#94747);
#83111=AXIS2_PLACEMENT_3D('',#191267,#94748,#94749);
#83112=AXIS2_PLACEMENT_3D('',#191272,#94751,#94752);
#83113=AXIS2_PLACEMENT_3D('',#191275,#94754,#94755);
#83114=AXIS2_PLACEMENT_3D('',#191276,#94756,#94757);
#83115=AXIS2_PLACEMENT_3D('',#191280,#94759,#94760);
#83116=AXIS2_PLACEMENT_3D('',#191281,#94761,#94762);
#83117=AXIS2_PLACEMENT_3D('',#191282,#94763,#94764);
#83118=AXIS2_PLACEMENT_3D('',#191288,#94767,#94768);
#83119=AXIS2_PLACEMENT_3D('',#191289,#94769,#94770);
#83120=AXIS2_PLACEMENT_3D('',#191290,#94771,#94772);
#83121=AXIS2_PLACEMENT_3D('',#191292,#94773,#94774);
#83122=AXIS2_PLACEMENT_3D('',#191294,#94776,#94777);
#83123=AXIS2_PLACEMENT_3D('',#191295,#94778,#94779);
#83124=AXIS2_PLACEMENT_3D('',#191296,#94780,#94781);
#83125=AXIS2_PLACEMENT_3D('',#191297,#94782,#94783);
#83126=AXIS2_PLACEMENT_3D('',#191302,#94785,#94786);
#83127=AXIS2_PLACEMENT_3D('',#191305,#94788,#94789);
#83128=AXIS2_PLACEMENT_3D('',#191306,#94790,#94791);
#83129=AXIS2_PLACEMENT_3D('',#191310,#94793,#94794);
#83130=AXIS2_PLACEMENT_3D('',#191311,#94795,#94796);
#83131=AXIS2_PLACEMENT_3D('',#191312,#94797,#94798);
#83132=AXIS2_PLACEMENT_3D('',#191316,#94800,#94801);
#83133=AXIS2_PLACEMENT_3D('',#191317,#94802,#94803);
#83134=AXIS2_PLACEMENT_3D('',#191318,#94804,#94805);
#83135=AXIS2_PLACEMENT_3D('',#191319,#94806,#94807);
#83136=AXIS2_PLACEMENT_3D('',#191320,#94808,#94809);
#83137=AXIS2_PLACEMENT_3D('',#191321,#94810,#94811);
#83138=AXIS2_PLACEMENT_3D('',#191326,#94813,#94814);
#83139=AXIS2_PLACEMENT_3D('',#191329,#94816,#94817);
#83140=AXIS2_PLACEMENT_3D('',#191330,#94818,#94819);
#83141=AXIS2_PLACEMENT_3D('',#191334,#94821,#94822);
#83142=AXIS2_PLACEMENT_3D('',#191335,#94823,#94824);
#83143=AXIS2_PLACEMENT_3D('',#191336,#94825,#94826);
#83144=AXIS2_PLACEMENT_3D('',#191340,#94828,#94829);
#83145=AXIS2_PLACEMENT_3D('',#191341,#94830,#94831);
#83146=AXIS2_PLACEMENT_3D('',#191342,#94832,#94833);
#83147=AXIS2_PLACEMENT_3D('',#191343,#94834,#94835);
#83148=AXIS2_PLACEMENT_3D('',#191344,#94836,#94837);
#83149=AXIS2_PLACEMENT_3D('',#191345,#94838,#94839);
#83150=AXIS2_PLACEMENT_3D('',#191350,#94841,#94842);
#83151=AXIS2_PLACEMENT_3D('',#191353,#94844,#94845);
#83152=AXIS2_PLACEMENT_3D('',#191354,#94846,#94847);
#83153=AXIS2_PLACEMENT_3D('',#191358,#94849,#94850);
#83154=AXIS2_PLACEMENT_3D('',#191359,#94851,#94852);
#83155=AXIS2_PLACEMENT_3D('',#191360,#94853,#94854);
#83156=AXIS2_PLACEMENT_3D('',#191364,#94856,#94857);
#83157=AXIS2_PLACEMENT_3D('',#191365,#94858,#94859);
#83158=AXIS2_PLACEMENT_3D('',#191366,#94860,#94861);
#83159=AXIS2_PLACEMENT_3D('',#191367,#94862,#94863);
#83160=AXIS2_PLACEMENT_3D('',#191368,#94864,#94865);
#83161=AXIS2_PLACEMENT_3D('',#191369,#94866,#94867);
#83162=AXIS2_PLACEMENT_3D('',#191374,#94869,#94870);
#83163=AXIS2_PLACEMENT_3D('',#191377,#94872,#94873);
#83164=AXIS2_PLACEMENT_3D('',#191378,#94874,#94875);
#83165=AXIS2_PLACEMENT_3D('',#191382,#94877,#94878);
#83166=AXIS2_PLACEMENT_3D('',#191383,#94879,#94880);
#83167=AXIS2_PLACEMENT_3D('',#191384,#94881,#94882);
#83168=AXIS2_PLACEMENT_3D('',#191388,#94884,#94885);
#83169=AXIS2_PLACEMENT_3D('',#191389,#94886,#94887);
#83170=AXIS2_PLACEMENT_3D('',#191390,#94888,#94889);
#83171=AXIS2_PLACEMENT_3D('',#191391,#94890,#94891);
#83172=AXIS2_PLACEMENT_3D('',#191392,#94892,#94893);
#83173=AXIS2_PLACEMENT_3D('',#191393,#94894,#94895);
#83174=AXIS2_PLACEMENT_3D('',#191398,#94897,#94898);
#83175=AXIS2_PLACEMENT_3D('',#191401,#94900,#94901);
#83176=AXIS2_PLACEMENT_3D('',#191402,#94902,#94903);
#83177=AXIS2_PLACEMENT_3D('',#191406,#94905,#94906);
#83178=AXIS2_PLACEMENT_3D('',#191407,#94907,#94908);
#83179=AXIS2_PLACEMENT_3D('',#191408,#94909,#94910);
#83180=AXIS2_PLACEMENT_3D('',#191412,#94912,#94913);
#83181=AXIS2_PLACEMENT_3D('',#191413,#94914,#94915);
#83182=AXIS2_PLACEMENT_3D('',#191414,#94916,#94917);
#83183=AXIS2_PLACEMENT_3D('',#191415,#94918,#94919);
#83184=AXIS2_PLACEMENT_3D('',#191416,#94920,#94921);
#83185=AXIS2_PLACEMENT_3D('',#191417,#94922,#94923);
#83186=AXIS2_PLACEMENT_3D('',#191422,#94925,#94926);
#83187=AXIS2_PLACEMENT_3D('',#191425,#94928,#94929);
#83188=AXIS2_PLACEMENT_3D('',#191426,#94930,#94931);
#83189=AXIS2_PLACEMENT_3D('',#191430,#94933,#94934);
#83190=AXIS2_PLACEMENT_3D('',#191431,#94935,#94936);
#83191=AXIS2_PLACEMENT_3D('',#191432,#94937,#94938);
#83192=AXIS2_PLACEMENT_3D('',#191436,#94940,#94941);
#83193=AXIS2_PLACEMENT_3D('',#191437,#94942,#94943);
#83194=AXIS2_PLACEMENT_3D('',#191438,#94944,#94945);
#83195=AXIS2_PLACEMENT_3D('',#191439,#94946,#94947);
#83196=AXIS2_PLACEMENT_3D('',#191440,#94948,#94949);
#83197=AXIS2_PLACEMENT_3D('',#191441,#94950,#94951);
#83198=AXIS2_PLACEMENT_3D('',#191446,#94953,#94954);
#83199=AXIS2_PLACEMENT_3D('',#191449,#94956,#94957);
#83200=AXIS2_PLACEMENT_3D('',#191450,#94958,#94959);
#83201=AXIS2_PLACEMENT_3D('',#191454,#94961,#94962);
#83202=AXIS2_PLACEMENT_3D('',#191455,#94963,#94964);
#83203=AXIS2_PLACEMENT_3D('',#191456,#94965,#94966);
#83204=AXIS2_PLACEMENT_3D('',#191460,#94968,#94969);
#83205=AXIS2_PLACEMENT_3D('',#191461,#94970,#94971);
#83206=AXIS2_PLACEMENT_3D('',#191462,#94972,#94973);
#83207=AXIS2_PLACEMENT_3D('',#191463,#94974,#94975);
#83208=AXIS2_PLACEMENT_3D('',#191464,#94976,#94977);
#83209=AXIS2_PLACEMENT_3D('',#191465,#94978,#94979);
#83210=AXIS2_PLACEMENT_3D('',#191470,#94981,#94982);
#83211=AXIS2_PLACEMENT_3D('',#191473,#94984,#94985);
#83212=AXIS2_PLACEMENT_3D('',#191474,#94986,#94987);
#83213=AXIS2_PLACEMENT_3D('',#191478,#94989,#94990);
#83214=AXIS2_PLACEMENT_3D('',#191479,#94991,#94992);
#83215=AXIS2_PLACEMENT_3D('',#191480,#94993,#94994);
#83216=AXIS2_PLACEMENT_3D('',#191484,#94996,#94997);
#83217=AXIS2_PLACEMENT_3D('',#191485,#94998,#94999);
#83218=AXIS2_PLACEMENT_3D('',#191486,#95000,#95001);
#83219=AXIS2_PLACEMENT_3D('',#191487,#95002,#95003);
#83220=AXIS2_PLACEMENT_3D('',#191488,#95004,#95005);
#83221=AXIS2_PLACEMENT_3D('',#191489,#95006,#95007);
#83222=AXIS2_PLACEMENT_3D('',#191494,#95009,#95010);
#83223=AXIS2_PLACEMENT_3D('',#191497,#95012,#95013);
#83224=AXIS2_PLACEMENT_3D('',#191498,#95014,#95015);
#83225=AXIS2_PLACEMENT_3D('',#191502,#95017,#95018);
#83226=AXIS2_PLACEMENT_3D('',#191503,#95019,#95020);
#83227=AXIS2_PLACEMENT_3D('',#191504,#95021,#95022);
#83228=AXIS2_PLACEMENT_3D('',#191508,#95024,#95025);
#83229=AXIS2_PLACEMENT_3D('',#191509,#95026,#95027);
#83230=AXIS2_PLACEMENT_3D('',#191510,#95028,#95029);
#83231=AXIS2_PLACEMENT_3D('',#191511,#95030,#95031);
#83232=AXIS2_PLACEMENT_3D('',#191512,#95032,#95033);
#83233=AXIS2_PLACEMENT_3D('',#191513,#95034,#95035);
#83234=AXIS2_PLACEMENT_3D('',#191518,#95037,#95038);
#83235=AXIS2_PLACEMENT_3D('',#191521,#95040,#95041);
#83236=AXIS2_PLACEMENT_3D('',#191522,#95042,#95043);
#83237=AXIS2_PLACEMENT_3D('',#191528,#95046,#95047);
#83238=AXIS2_PLACEMENT_3D('',#191529,#95048,#95049);
#83239=AXIS2_PLACEMENT_3D('',#191530,#95050,#95051);
#83240=AXIS2_PLACEMENT_3D('',#191535,#95054,#95055);
#83241=AXIS2_PLACEMENT_3D('',#191536,#95056,#95057);
#83242=AXIS2_PLACEMENT_3D('',#191538,#95058,#95059);
#83243=AXIS2_PLACEMENT_3D('',#191540,#95061,#95062);
#83244=AXIS2_PLACEMENT_3D('',#191541,#95063,#95064);
#83245=AXIS2_PLACEMENT_3D('',#191542,#95065,#95066);
#83246=AXIS2_PLACEMENT_3D('',#191543,#95067,#95068);
#83247=AXIS2_PLACEMENT_3D('',#191548,#95070,#95071);
#83248=AXIS2_PLACEMENT_3D('',#191551,#95073,#95074);
#83249=AXIS2_PLACEMENT_3D('',#191552,#95075,#95076);
#83250=AXIS2_PLACEMENT_3D('',#191556,#95078,#95079);
#83251=AXIS2_PLACEMENT_3D('',#191557,#95080,#95081);
#83252=AXIS2_PLACEMENT_3D('',#191558,#95082,#95083);
#83253=AXIS2_PLACEMENT_3D('',#191564,#95086,#95087);
#83254=AXIS2_PLACEMENT_3D('',#191565,#95088,#95089);
#83255=AXIS2_PLACEMENT_3D('',#191566,#95090,#95091);
#83256=AXIS2_PLACEMENT_3D('',#191568,#95092,#95093);
#83257=AXIS2_PLACEMENT_3D('',#191570,#95095,#95096);
#83258=AXIS2_PLACEMENT_3D('',#191571,#95097,#95098);
#83259=AXIS2_PLACEMENT_3D('',#191572,#95099,#95100);
#83260=AXIS2_PLACEMENT_3D('',#191573,#95101,#95102);
#83261=AXIS2_PLACEMENT_3D('',#191578,#95104,#95105);
#83262=AXIS2_PLACEMENT_3D('',#191581,#95107,#95108);
#83263=AXIS2_PLACEMENT_3D('',#191582,#95109,#95110);
#83264=AXIS2_PLACEMENT_3D('',#191586,#95112,#95113);
#83265=AXIS2_PLACEMENT_3D('',#191587,#95114,#95115);
#83266=AXIS2_PLACEMENT_3D('',#191588,#95116,#95117);
#83267=AXIS2_PLACEMENT_3D('',#191592,#95119,#95120);
#83268=AXIS2_PLACEMENT_3D('',#191593,#95121,#95122);
#83269=AXIS2_PLACEMENT_3D('',#191594,#95123,#95124);
#83270=AXIS2_PLACEMENT_3D('',#191595,#95125,#95126);
#83271=AXIS2_PLACEMENT_3D('',#191596,#95127,#95128);
#83272=AXIS2_PLACEMENT_3D('',#191597,#95129,#95130);
#83273=AXIS2_PLACEMENT_3D('',#191602,#95132,#95133);
#83274=AXIS2_PLACEMENT_3D('',#191605,#95135,#95136);
#83275=AXIS2_PLACEMENT_3D('',#191606,#95137,#95138);
#83276=AXIS2_PLACEMENT_3D('',#191610,#95140,#95141);
#83277=AXIS2_PLACEMENT_3D('',#191611,#95142,#95143);
#83278=AXIS2_PLACEMENT_3D('',#191612,#95144,#95145);
#83279=AXIS2_PLACEMENT_3D('',#191616,#95147,#95148);
#83280=AXIS2_PLACEMENT_3D('',#191617,#95149,#95150);
#83281=AXIS2_PLACEMENT_3D('',#191618,#95151,#95152);
#83282=AXIS2_PLACEMENT_3D('',#191619,#95153,#95154);
#83283=AXIS2_PLACEMENT_3D('',#191620,#95155,#95156);
#83284=AXIS2_PLACEMENT_3D('',#191621,#95157,#95158);
#83285=AXIS2_PLACEMENT_3D('',#191626,#95160,#95161);
#83286=AXIS2_PLACEMENT_3D('',#191629,#95163,#95164);
#83287=AXIS2_PLACEMENT_3D('',#191630,#95165,#95166);
#83288=AXIS2_PLACEMENT_3D('',#191634,#95168,#95169);
#83289=AXIS2_PLACEMENT_3D('',#191635,#95170,#95171);
#83290=AXIS2_PLACEMENT_3D('',#191636,#95172,#95173);
#83291=AXIS2_PLACEMENT_3D('',#191640,#95175,#95176);
#83292=AXIS2_PLACEMENT_3D('',#191641,#95177,#95178);
#83293=AXIS2_PLACEMENT_3D('',#191642,#95179,#95180);
#83294=AXIS2_PLACEMENT_3D('',#191643,#95181,#95182);
#83295=AXIS2_PLACEMENT_3D('',#191644,#95183,#95184);
#83296=AXIS2_PLACEMENT_3D('',#191645,#95185,#95186);
#83297=AXIS2_PLACEMENT_3D('',#191650,#95188,#95189);
#83298=AXIS2_PLACEMENT_3D('',#191653,#95191,#95192);
#83299=AXIS2_PLACEMENT_3D('',#191654,#95193,#95194);
#83300=AXIS2_PLACEMENT_3D('',#191658,#95196,#95197);
#83301=AXIS2_PLACEMENT_3D('',#191659,#95198,#95199);
#83302=AXIS2_PLACEMENT_3D('',#191660,#95200,#95201);
#83303=AXIS2_PLACEMENT_3D('',#191664,#95203,#95204);
#83304=AXIS2_PLACEMENT_3D('',#191665,#95205,#95206);
#83305=AXIS2_PLACEMENT_3D('',#191666,#95207,#95208);
#83306=AXIS2_PLACEMENT_3D('',#191667,#95209,#95210);
#83307=AXIS2_PLACEMENT_3D('',#191668,#95211,#95212);
#83308=AXIS2_PLACEMENT_3D('',#191669,#95213,#95214);
#83309=AXIS2_PLACEMENT_3D('',#191674,#95216,#95217);
#83310=AXIS2_PLACEMENT_3D('',#191677,#95219,#95220);
#83311=AXIS2_PLACEMENT_3D('',#191678,#95221,#95222);
#83312=AXIS2_PLACEMENT_3D('',#191682,#95224,#95225);
#83313=AXIS2_PLACEMENT_3D('',#191683,#95226,#95227);
#83314=AXIS2_PLACEMENT_3D('',#191684,#95228,#95229);
#83315=AXIS2_PLACEMENT_3D('',#191688,#95231,#95232);
#83316=AXIS2_PLACEMENT_3D('',#191689,#95233,#95234);
#83317=AXIS2_PLACEMENT_3D('',#191690,#95235,#95236);
#83318=AXIS2_PLACEMENT_3D('',#191691,#95237,#95238);
#83319=AXIS2_PLACEMENT_3D('',#191692,#95239,#95240);
#83320=AXIS2_PLACEMENT_3D('',#191693,#95241,#95242);
#83321=AXIS2_PLACEMENT_3D('',#191698,#95244,#95245);
#83322=AXIS2_PLACEMENT_3D('',#191701,#95247,#95248);
#83323=AXIS2_PLACEMENT_3D('',#191702,#95249,#95250);
#83324=AXIS2_PLACEMENT_3D('',#191706,#95252,#95253);
#83325=AXIS2_PLACEMENT_3D('',#191707,#95254,#95255);
#83326=AXIS2_PLACEMENT_3D('',#191708,#95256,#95257);
#83327=AXIS2_PLACEMENT_3D('',#191712,#95259,#95260);
#83328=AXIS2_PLACEMENT_3D('',#191713,#95261,#95262);
#83329=AXIS2_PLACEMENT_3D('',#191714,#95263,#95264);
#83330=AXIS2_PLACEMENT_3D('',#191715,#95265,#95266);
#83331=AXIS2_PLACEMENT_3D('',#191716,#95267,#95268);
#83332=AXIS2_PLACEMENT_3D('',#191717,#95269,#95270);
#83333=AXIS2_PLACEMENT_3D('',#191722,#95272,#95273);
#83334=AXIS2_PLACEMENT_3D('',#191725,#95275,#95276);
#83335=AXIS2_PLACEMENT_3D('',#191726,#95277,#95278);
#83336=AXIS2_PLACEMENT_3D('',#191730,#95280,#95281);
#83337=AXIS2_PLACEMENT_3D('',#191731,#95282,#95283);
#83338=AXIS2_PLACEMENT_3D('',#191732,#95284,#95285);
#83339=AXIS2_PLACEMENT_3D('',#191736,#95287,#95288);
#83340=AXIS2_PLACEMENT_3D('',#191737,#95289,#95290);
#83341=AXIS2_PLACEMENT_3D('',#191738,#95291,#95292);
#83342=AXIS2_PLACEMENT_3D('',#191739,#95293,#95294);
#83343=AXIS2_PLACEMENT_3D('',#191740,#95295,#95296);
#83344=AXIS2_PLACEMENT_3D('',#191741,#95297,#95298);
#83345=AXIS2_PLACEMENT_3D('',#191746,#95300,#95301);
#83346=AXIS2_PLACEMENT_3D('',#191749,#95303,#95304);
#83347=AXIS2_PLACEMENT_3D('',#191750,#95305,#95306);
#83348=AXIS2_PLACEMENT_3D('',#191754,#95308,#95309);
#83349=AXIS2_PLACEMENT_3D('',#191755,#95310,#95311);
#83350=AXIS2_PLACEMENT_3D('',#191756,#95312,#95313);
#83351=AXIS2_PLACEMENT_3D('',#191760,#95315,#95316);
#83352=AXIS2_PLACEMENT_3D('',#191761,#95317,#95318);
#83353=AXIS2_PLACEMENT_3D('',#191762,#95319,#95320);
#83354=AXIS2_PLACEMENT_3D('',#191763,#95321,#95322);
#83355=AXIS2_PLACEMENT_3D('',#191764,#95323,#95324);
#83356=AXIS2_PLACEMENT_3D('',#191765,#95325,#95326);
#83357=AXIS2_PLACEMENT_3D('',#191770,#95328,#95329);
#83358=AXIS2_PLACEMENT_3D('',#191773,#95331,#95332);
#83359=AXIS2_PLACEMENT_3D('',#191774,#95333,#95334);
#83360=AXIS2_PLACEMENT_3D('',#191778,#95336,#95337);
#83361=AXIS2_PLACEMENT_3D('',#191779,#95338,#95339);
#83362=AXIS2_PLACEMENT_3D('',#191780,#95340,#95341);
#83363=AXIS2_PLACEMENT_3D('',#191784,#95343,#95344);
#83364=AXIS2_PLACEMENT_3D('',#191785,#95345,#95346);
#83365=AXIS2_PLACEMENT_3D('',#191786,#95347,#95348);
#83366=AXIS2_PLACEMENT_3D('',#191787,#95349,#95350);
#83367=AXIS2_PLACEMENT_3D('',#191788,#95351,#95352);
#83368=AXIS2_PLACEMENT_3D('',#191789,#95353,#95354);
#83369=AXIS2_PLACEMENT_3D('',#191794,#95356,#95357);
#83370=AXIS2_PLACEMENT_3D('',#191797,#95359,#95360);
#83371=AXIS2_PLACEMENT_3D('',#191798,#95361,#95362);
#83372=AXIS2_PLACEMENT_3D('',#191802,#95364,#95365);
#83373=AXIS2_PLACEMENT_3D('',#191803,#95366,#95367);
#83374=AXIS2_PLACEMENT_3D('',#191804,#95368,#95369);
#83375=AXIS2_PLACEMENT_3D('',#191808,#95371,#95372);
#83376=AXIS2_PLACEMENT_3D('',#191809,#95373,#95374);
#83377=AXIS2_PLACEMENT_3D('',#191810,#95375,#95376);
#83378=AXIS2_PLACEMENT_3D('',#191811,#95377,#95378);
#83379=AXIS2_PLACEMENT_3D('',#191812,#95379,#95380);
#83380=AXIS2_PLACEMENT_3D('',#191813,#95381,#95382);
#83381=AXIS2_PLACEMENT_3D('',#191818,#95384,#95385);
#83382=AXIS2_PLACEMENT_3D('',#191821,#95387,#95388);
#83383=AXIS2_PLACEMENT_3D('',#191822,#95389,#95390);
#83384=AXIS2_PLACEMENT_3D('',#191826,#95392,#95393);
#83385=AXIS2_PLACEMENT_3D('',#191827,#95394,#95395);
#83386=AXIS2_PLACEMENT_3D('',#191828,#95396,#95397);
#83387=AXIS2_PLACEMENT_3D('',#191832,#95399,#95400);
#83388=AXIS2_PLACEMENT_3D('',#191833,#95401,#95402);
#83389=AXIS2_PLACEMENT_3D('',#191834,#95403,#95404);
#83390=AXIS2_PLACEMENT_3D('',#191835,#95405,#95406);
#83391=AXIS2_PLACEMENT_3D('',#191836,#95407,#95408);
#83392=AXIS2_PLACEMENT_3D('',#191837,#95409,#95410);
#83393=AXIS2_PLACEMENT_3D('',#191842,#95412,#95413);
#83394=AXIS2_PLACEMENT_3D('',#191845,#95415,#95416);
#83395=AXIS2_PLACEMENT_3D('',#191846,#95417,#95418);
#83396=AXIS2_PLACEMENT_3D('',#191850,#95420,#95421);
#83397=AXIS2_PLACEMENT_3D('',#191851,#95422,#95423);
#83398=AXIS2_PLACEMENT_3D('',#191852,#95424,#95425);
#83399=AXIS2_PLACEMENT_3D('',#191856,#95427,#95428);
#83400=AXIS2_PLACEMENT_3D('',#191857,#95429,#95430);
#83401=AXIS2_PLACEMENT_3D('',#191858,#95431,#95432);
#83402=AXIS2_PLACEMENT_3D('',#191859,#95433,#95434);
#83403=AXIS2_PLACEMENT_3D('',#191860,#95435,#95436);
#83404=AXIS2_PLACEMENT_3D('',#191861,#95437,#95438);
#83405=AXIS2_PLACEMENT_3D('',#191866,#95440,#95441);
#83406=AXIS2_PLACEMENT_3D('',#191869,#95443,#95444);
#83407=AXIS2_PLACEMENT_3D('',#191870,#95445,#95446);
#83408=AXIS2_PLACEMENT_3D('',#191874,#95448,#95449);
#83409=AXIS2_PLACEMENT_3D('',#191875,#95450,#95451);
#83410=AXIS2_PLACEMENT_3D('',#191876,#95452,#95453);
#83411=AXIS2_PLACEMENT_3D('',#191880,#95455,#95456);
#83412=AXIS2_PLACEMENT_3D('',#191881,#95457,#95458);
#83413=AXIS2_PLACEMENT_3D('',#191882,#95459,#95460);
#83414=AXIS2_PLACEMENT_3D('',#191883,#95461,#95462);
#83415=AXIS2_PLACEMENT_3D('',#191884,#95463,#95464);
#83416=AXIS2_PLACEMENT_3D('',#191885,#95465,#95466);
#83417=AXIS2_PLACEMENT_3D('',#191890,#95468,#95469);
#83418=AXIS2_PLACEMENT_3D('',#191893,#95471,#95472);
#83419=AXIS2_PLACEMENT_3D('',#191894,#95473,#95474);
#83420=AXIS2_PLACEMENT_3D('',#191898,#95476,#95477);
#83421=AXIS2_PLACEMENT_3D('',#191899,#95478,#95479);
#83422=AXIS2_PLACEMENT_3D('',#191900,#95480,#95481);
#83423=AXIS2_PLACEMENT_3D('',#191904,#95483,#95484);
#83424=AXIS2_PLACEMENT_3D('',#191905,#95485,#95486);
#83425=AXIS2_PLACEMENT_3D('',#191906,#95487,#95488);
#83426=AXIS2_PLACEMENT_3D('',#191907,#95489,#95490);
#83427=AXIS2_PLACEMENT_3D('',#191908,#95491,#95492);
#83428=AXIS2_PLACEMENT_3D('',#191909,#95493,#95494);
#83429=AXIS2_PLACEMENT_3D('',#191914,#95496,#95497);
#83430=AXIS2_PLACEMENT_3D('',#191917,#95499,#95500);
#83431=AXIS2_PLACEMENT_3D('',#191918,#95501,#95502);
#83432=AXIS2_PLACEMENT_3D('',#191922,#95504,#95505);
#83433=AXIS2_PLACEMENT_3D('',#191923,#95506,#95507);
#83434=AXIS2_PLACEMENT_3D('',#191924,#95508,#95509);
#83435=AXIS2_PLACEMENT_3D('',#191928,#95511,#95512);
#83436=AXIS2_PLACEMENT_3D('',#191929,#95513,#95514);
#83437=AXIS2_PLACEMENT_3D('',#191930,#95515,#95516);
#83438=AXIS2_PLACEMENT_3D('',#191931,#95517,#95518);
#83439=AXIS2_PLACEMENT_3D('',#191932,#95519,#95520);
#83440=AXIS2_PLACEMENT_3D('',#191933,#95521,#95522);
#83441=AXIS2_PLACEMENT_3D('',#191938,#95524,#95525);
#83442=AXIS2_PLACEMENT_3D('',#191941,#95527,#95528);
#83443=AXIS2_PLACEMENT_3D('',#191942,#95529,#95530);
#83444=AXIS2_PLACEMENT_3D('',#191946,#95532,#95533);
#83445=AXIS2_PLACEMENT_3D('',#191947,#95534,#95535);
#83446=AXIS2_PLACEMENT_3D('',#191948,#95536,#95537);
#83447=AXIS2_PLACEMENT_3D('',#191952,#95539,#95540);
#83448=AXIS2_PLACEMENT_3D('',#191953,#95541,#95542);
#83449=AXIS2_PLACEMENT_3D('',#191954,#95543,#95544);
#83450=AXIS2_PLACEMENT_3D('',#191955,#95545,#95546);
#83451=AXIS2_PLACEMENT_3D('',#191956,#95547,#95548);
#83452=AXIS2_PLACEMENT_3D('',#191957,#95549,#95550);
#83453=AXIS2_PLACEMENT_3D('',#191962,#95552,#95553);
#83454=AXIS2_PLACEMENT_3D('',#191965,#95555,#95556);
#83455=AXIS2_PLACEMENT_3D('',#191966,#95557,#95558);
#83456=AXIS2_PLACEMENT_3D('',#191970,#95560,#95561);
#83457=AXIS2_PLACEMENT_3D('',#191971,#95562,#95563);
#83458=AXIS2_PLACEMENT_3D('',#191972,#95564,#95565);
#83459=AXIS2_PLACEMENT_3D('',#191976,#95567,#95568);
#83460=AXIS2_PLACEMENT_3D('',#191977,#95569,#95570);
#83461=AXIS2_PLACEMENT_3D('',#191978,#95571,#95572);
#83462=AXIS2_PLACEMENT_3D('',#191979,#95573,#95574);
#83463=AXIS2_PLACEMENT_3D('',#191980,#95575,#95576);
#83464=AXIS2_PLACEMENT_3D('',#191981,#95577,#95578);
#83465=AXIS2_PLACEMENT_3D('',#191986,#95580,#95581);
#83466=AXIS2_PLACEMENT_3D('',#191989,#95583,#95584);
#83467=AXIS2_PLACEMENT_3D('',#191990,#95585,#95586);
#83468=AXIS2_PLACEMENT_3D('',#191994,#95588,#95589);
#83469=AXIS2_PLACEMENT_3D('',#191995,#95590,#95591);
#83470=AXIS2_PLACEMENT_3D('',#191996,#95592,#95593);
#83471=AXIS2_PLACEMENT_3D('',#192000,#95595,#95596);
#83472=AXIS2_PLACEMENT_3D('',#192001,#95597,#95598);
#83473=AXIS2_PLACEMENT_3D('',#192002,#95599,#95600);
#83474=AXIS2_PLACEMENT_3D('',#192003,#95601,#95602);
#83475=AXIS2_PLACEMENT_3D('',#192004,#95603,#95604);
#83476=AXIS2_PLACEMENT_3D('',#192005,#95605,#95606);
#83477=AXIS2_PLACEMENT_3D('',#192010,#95608,#95609);
#83478=AXIS2_PLACEMENT_3D('',#192013,#95611,#95612);
#83479=AXIS2_PLACEMENT_3D('',#192014,#95613,#95614);
#83480=AXIS2_PLACEMENT_3D('',#192018,#95616,#95617);
#83481=AXIS2_PLACEMENT_3D('',#192019,#95618,#95619);
#83482=AXIS2_PLACEMENT_3D('',#192020,#95620,#95621);
#83483=AXIS2_PLACEMENT_3D('',#192024,#95623,#95624);
#83484=AXIS2_PLACEMENT_3D('',#192025,#95625,#95626);
#83485=AXIS2_PLACEMENT_3D('',#192026,#95627,#95628);
#83486=AXIS2_PLACEMENT_3D('',#192027,#95629,#95630);
#83487=AXIS2_PLACEMENT_3D('',#192028,#95631,#95632);
#83488=AXIS2_PLACEMENT_3D('',#192029,#95633,#95634);
#83489=AXIS2_PLACEMENT_3D('',#192034,#95636,#95637);
#83490=AXIS2_PLACEMENT_3D('',#192037,#95639,#95640);
#83491=AXIS2_PLACEMENT_3D('',#192038,#95641,#95642);
#83492=AXIS2_PLACEMENT_3D('',#192042,#95644,#95645);
#83493=AXIS2_PLACEMENT_3D('',#192043,#95646,#95647);
#83494=AXIS2_PLACEMENT_3D('',#192044,#95648,#95649);
#83495=AXIS2_PLACEMENT_3D('',#192048,#95651,#95652);
#83496=AXIS2_PLACEMENT_3D('',#192049,#95653,#95654);
#83497=AXIS2_PLACEMENT_3D('',#192050,#95655,#95656);
#83498=AXIS2_PLACEMENT_3D('',#192051,#95657,#95658);
#83499=AXIS2_PLACEMENT_3D('',#192052,#95659,#95660);
#83500=AXIS2_PLACEMENT_3D('',#192053,#95661,#95662);
#83501=AXIS2_PLACEMENT_3D('',#192058,#95664,#95665);
#83502=AXIS2_PLACEMENT_3D('',#192061,#95667,#95668);
#83503=AXIS2_PLACEMENT_3D('',#192062,#95669,#95670);
#83504=AXIS2_PLACEMENT_3D('',#192066,#95672,#95673);
#83505=AXIS2_PLACEMENT_3D('',#192067,#95674,#95675);
#83506=AXIS2_PLACEMENT_3D('',#192068,#95676,#95677);
#83507=AXIS2_PLACEMENT_3D('',#192072,#95679,#95680);
#83508=AXIS2_PLACEMENT_3D('',#192073,#95681,#95682);
#83509=AXIS2_PLACEMENT_3D('',#192074,#95683,#95684);
#83510=AXIS2_PLACEMENT_3D('',#192075,#95685,#95686);
#83511=AXIS2_PLACEMENT_3D('',#192076,#95687,#95688);
#83512=AXIS2_PLACEMENT_3D('',#192077,#95689,#95690);
#83513=AXIS2_PLACEMENT_3D('',#192082,#95692,#95693);
#83514=AXIS2_PLACEMENT_3D('',#192085,#95695,#95696);
#83515=AXIS2_PLACEMENT_3D('',#192086,#95697,#95698);
#83516=AXIS2_PLACEMENT_3D('',#192090,#95700,#95701);
#83517=AXIS2_PLACEMENT_3D('',#192091,#95702,#95703);
#83518=AXIS2_PLACEMENT_3D('',#192092,#95704,#95705);
#83519=AXIS2_PLACEMENT_3D('',#192096,#95707,#95708);
#83520=AXIS2_PLACEMENT_3D('',#192097,#95709,#95710);
#83521=AXIS2_PLACEMENT_3D('',#192098,#95711,#95712);
#83522=AXIS2_PLACEMENT_3D('',#192099,#95713,#95714);
#83523=AXIS2_PLACEMENT_3D('',#192100,#95715,#95716);
#83524=AXIS2_PLACEMENT_3D('',#192101,#95717,#95718);
#83525=AXIS2_PLACEMENT_3D('',#192106,#95720,#95721);
#83526=AXIS2_PLACEMENT_3D('',#192109,#95723,#95724);
#83527=AXIS2_PLACEMENT_3D('',#192110,#95725,#95726);
#83528=AXIS2_PLACEMENT_3D('',#192114,#95728,#95729);
#83529=AXIS2_PLACEMENT_3D('',#192115,#95730,#95731);
#83530=AXIS2_PLACEMENT_3D('',#192116,#95732,#95733);
#83531=AXIS2_PLACEMENT_3D('',#192120,#95735,#95736);
#83532=AXIS2_PLACEMENT_3D('',#192121,#95737,#95738);
#83533=AXIS2_PLACEMENT_3D('',#192122,#95739,#95740);
#83534=AXIS2_PLACEMENT_3D('',#192123,#95741,#95742);
#83535=AXIS2_PLACEMENT_3D('',#192124,#95743,#95744);
#83536=AXIS2_PLACEMENT_3D('',#192125,#95745,#95746);
#83537=AXIS2_PLACEMENT_3D('',#192130,#95748,#95749);
#83538=AXIS2_PLACEMENT_3D('',#192133,#95751,#95752);
#83539=AXIS2_PLACEMENT_3D('',#192134,#95753,#95754);
#83540=AXIS2_PLACEMENT_3D('',#192138,#95756,#95757);
#83541=AXIS2_PLACEMENT_3D('',#192139,#95758,#95759);
#83542=AXIS2_PLACEMENT_3D('',#192140,#95760,#95761);
#83543=AXIS2_PLACEMENT_3D('',#192144,#95763,#95764);
#83544=AXIS2_PLACEMENT_3D('',#192145,#95765,#95766);
#83545=AXIS2_PLACEMENT_3D('',#192146,#95767,#95768);
#83546=AXIS2_PLACEMENT_3D('',#192147,#95769,#95770);
#83547=AXIS2_PLACEMENT_3D('',#192148,#95771,#95772);
#83548=AXIS2_PLACEMENT_3D('',#192149,#95773,#95774);
#83549=AXIS2_PLACEMENT_3D('',#192154,#95776,#95777);
#83550=AXIS2_PLACEMENT_3D('',#192157,#95779,#95780);
#83551=AXIS2_PLACEMENT_3D('',#192158,#95781,#95782);
#83552=AXIS2_PLACEMENT_3D('',#192162,#95784,#95785);
#83553=AXIS2_PLACEMENT_3D('',#192163,#95786,#95787);
#83554=AXIS2_PLACEMENT_3D('',#192164,#95788,#95789);
#83555=AXIS2_PLACEMENT_3D('',#192168,#95791,#95792);
#83556=AXIS2_PLACEMENT_3D('',#192169,#95793,#95794);
#83557=AXIS2_PLACEMENT_3D('',#192170,#95795,#95796);
#83558=AXIS2_PLACEMENT_3D('',#192171,#95797,#95798);
#83559=AXIS2_PLACEMENT_3D('',#192172,#95799,#95800);
#83560=AXIS2_PLACEMENT_3D('',#192173,#95801,#95802);
#83561=AXIS2_PLACEMENT_3D('',#192178,#95804,#95805);
#83562=AXIS2_PLACEMENT_3D('',#192181,#95807,#95808);
#83563=AXIS2_PLACEMENT_3D('',#192182,#95809,#95810);
#83564=AXIS2_PLACEMENT_3D('',#192186,#95812,#95813);
#83565=AXIS2_PLACEMENT_3D('',#192187,#95814,#95815);
#83566=AXIS2_PLACEMENT_3D('',#192188,#95816,#95817);
#83567=AXIS2_PLACEMENT_3D('',#192192,#95819,#95820);
#83568=AXIS2_PLACEMENT_3D('',#192193,#95821,#95822);
#83569=AXIS2_PLACEMENT_3D('',#192194,#95823,#95824);
#83570=AXIS2_PLACEMENT_3D('',#192195,#95825,#95826);
#83571=AXIS2_PLACEMENT_3D('',#192196,#95827,#95828);
#83572=AXIS2_PLACEMENT_3D('',#192197,#95829,#95830);
#83573=AXIS2_PLACEMENT_3D('',#192202,#95832,#95833);
#83574=AXIS2_PLACEMENT_3D('',#192205,#95835,#95836);
#83575=AXIS2_PLACEMENT_3D('',#192206,#95837,#95838);
#83576=AXIS2_PLACEMENT_3D('',#192210,#95840,#95841);
#83577=AXIS2_PLACEMENT_3D('',#192211,#95842,#95843);
#83578=AXIS2_PLACEMENT_3D('',#192212,#95844,#95845);
#83579=AXIS2_PLACEMENT_3D('',#192216,#95847,#95848);
#83580=AXIS2_PLACEMENT_3D('',#192217,#95849,#95850);
#83581=AXIS2_PLACEMENT_3D('',#192218,#95851,#95852);
#83582=AXIS2_PLACEMENT_3D('',#192219,#95853,#95854);
#83583=AXIS2_PLACEMENT_3D('',#192220,#95855,#95856);
#83584=AXIS2_PLACEMENT_3D('',#192221,#95857,#95858);
#83585=AXIS2_PLACEMENT_3D('',#192226,#95860,#95861);
#83586=AXIS2_PLACEMENT_3D('',#192229,#95863,#95864);
#83587=AXIS2_PLACEMENT_3D('',#192230,#95865,#95866);
#83588=AXIS2_PLACEMENT_3D('',#192234,#95868,#95869);
#83589=AXIS2_PLACEMENT_3D('',#192235,#95870,#95871);
#83590=AXIS2_PLACEMENT_3D('',#192236,#95872,#95873);
#83591=AXIS2_PLACEMENT_3D('',#192240,#95875,#95876);
#83592=AXIS2_PLACEMENT_3D('',#192241,#95877,#95878);
#83593=AXIS2_PLACEMENT_3D('',#192242,#95879,#95880);
#83594=AXIS2_PLACEMENT_3D('',#192243,#95881,#95882);
#83595=AXIS2_PLACEMENT_3D('',#192244,#95883,#95884);
#83596=AXIS2_PLACEMENT_3D('',#192245,#95885,#95886);
#83597=AXIS2_PLACEMENT_3D('',#192250,#95888,#95889);
#83598=AXIS2_PLACEMENT_3D('',#192253,#95891,#95892);
#83599=AXIS2_PLACEMENT_3D('',#192254,#95893,#95894);
#83600=AXIS2_PLACEMENT_3D('',#192258,#95896,#95897);
#83601=AXIS2_PLACEMENT_3D('',#192259,#95898,#95899);
#83602=AXIS2_PLACEMENT_3D('',#192260,#95900,#95901);
#83603=AXIS2_PLACEMENT_3D('',#192264,#95903,#95904);
#83604=AXIS2_PLACEMENT_3D('',#192265,#95905,#95906);
#83605=AXIS2_PLACEMENT_3D('',#192266,#95907,#95908);
#83606=AXIS2_PLACEMENT_3D('',#192267,#95909,#95910);
#83607=AXIS2_PLACEMENT_3D('',#192268,#95911,#95912);
#83608=AXIS2_PLACEMENT_3D('',#192269,#95913,#95914);
#83609=AXIS2_PLACEMENT_3D('',#192274,#95916,#95917);
#83610=AXIS2_PLACEMENT_3D('',#192277,#95919,#95920);
#83611=AXIS2_PLACEMENT_3D('',#192278,#95921,#95922);
#83612=AXIS2_PLACEMENT_3D('',#192282,#95924,#95925);
#83613=AXIS2_PLACEMENT_3D('',#192283,#95926,#95927);
#83614=AXIS2_PLACEMENT_3D('',#192284,#95928,#95929);
#83615=AXIS2_PLACEMENT_3D('',#192288,#95931,#95932);
#83616=AXIS2_PLACEMENT_3D('',#192289,#95933,#95934);
#83617=AXIS2_PLACEMENT_3D('',#192290,#95935,#95936);
#83618=AXIS2_PLACEMENT_3D('',#192291,#95937,#95938);
#83619=AXIS2_PLACEMENT_3D('',#192292,#95939,#95940);
#83620=AXIS2_PLACEMENT_3D('',#192293,#95941,#95942);
#83621=AXIS2_PLACEMENT_3D('',#192298,#95944,#95945);
#83622=AXIS2_PLACEMENT_3D('',#192301,#95947,#95948);
#83623=AXIS2_PLACEMENT_3D('',#192302,#95949,#95950);
#83624=AXIS2_PLACEMENT_3D('',#192306,#95952,#95953);
#83625=AXIS2_PLACEMENT_3D('',#192307,#95954,#95955);
#83626=AXIS2_PLACEMENT_3D('',#192308,#95956,#95957);
#83627=AXIS2_PLACEMENT_3D('',#192312,#95959,#95960);
#83628=AXIS2_PLACEMENT_3D('',#192313,#95961,#95962);
#83629=AXIS2_PLACEMENT_3D('',#192314,#95963,#95964);
#83630=AXIS2_PLACEMENT_3D('',#192315,#95965,#95966);
#83631=AXIS2_PLACEMENT_3D('',#192316,#95967,#95968);
#83632=AXIS2_PLACEMENT_3D('',#192317,#95969,#95970);
#83633=AXIS2_PLACEMENT_3D('',#192322,#95972,#95973);
#83634=AXIS2_PLACEMENT_3D('',#192325,#95975,#95976);
#83635=AXIS2_PLACEMENT_3D('',#192326,#95977,#95978);
#83636=AXIS2_PLACEMENT_3D('',#192330,#95980,#95981);
#83637=AXIS2_PLACEMENT_3D('',#192331,#95982,#95983);
#83638=AXIS2_PLACEMENT_3D('',#192332,#95984,#95985);
#83639=AXIS2_PLACEMENT_3D('',#192336,#95987,#95988);
#83640=AXIS2_PLACEMENT_3D('',#192337,#95989,#95990);
#83641=AXIS2_PLACEMENT_3D('',#192338,#95991,#95992);
#83642=AXIS2_PLACEMENT_3D('',#192339,#95993,#95994);
#83643=AXIS2_PLACEMENT_3D('',#192340,#95995,#95996);
#83644=AXIS2_PLACEMENT_3D('',#192341,#95997,#95998);
#83645=AXIS2_PLACEMENT_3D('',#192346,#96000,#96001);
#83646=AXIS2_PLACEMENT_3D('',#192349,#96003,#96004);
#83647=AXIS2_PLACEMENT_3D('',#192350,#96005,#96006);
#83648=AXIS2_PLACEMENT_3D('',#192354,#96008,#96009);
#83649=AXIS2_PLACEMENT_3D('',#192355,#96010,#96011);
#83650=AXIS2_PLACEMENT_3D('',#192356,#96012,#96013);
#83651=AXIS2_PLACEMENT_3D('',#192360,#96015,#96016);
#83652=AXIS2_PLACEMENT_3D('',#192361,#96017,#96018);
#83653=AXIS2_PLACEMENT_3D('',#192362,#96019,#96020);
#83654=AXIS2_PLACEMENT_3D('',#192363,#96021,#96022);
#83655=AXIS2_PLACEMENT_3D('',#192364,#96023,#96024);
#83656=AXIS2_PLACEMENT_3D('',#192365,#96025,#96026);
#83657=AXIS2_PLACEMENT_3D('',#192370,#96028,#96029);
#83658=AXIS2_PLACEMENT_3D('',#192373,#96031,#96032);
#83659=AXIS2_PLACEMENT_3D('',#192374,#96033,#96034);
#83660=AXIS2_PLACEMENT_3D('',#192378,#96036,#96037);
#83661=AXIS2_PLACEMENT_3D('',#192379,#96038,#96039);
#83662=AXIS2_PLACEMENT_3D('',#192380,#96040,#96041);
#83663=AXIS2_PLACEMENT_3D('',#192384,#96043,#96044);
#83664=AXIS2_PLACEMENT_3D('',#192385,#96045,#96046);
#83665=AXIS2_PLACEMENT_3D('',#192386,#96047,#96048);
#83666=AXIS2_PLACEMENT_3D('',#192387,#96049,#96050);
#83667=AXIS2_PLACEMENT_3D('',#192388,#96051,#96052);
#83668=AXIS2_PLACEMENT_3D('',#192389,#96053,#96054);
#83669=AXIS2_PLACEMENT_3D('',#192394,#96056,#96057);
#83670=AXIS2_PLACEMENT_3D('',#192397,#96059,#96060);
#83671=AXIS2_PLACEMENT_3D('',#192398,#96061,#96062);
#83672=AXIS2_PLACEMENT_3D('',#192402,#96064,#96065);
#83673=AXIS2_PLACEMENT_3D('',#192403,#96066,#96067);
#83674=AXIS2_PLACEMENT_3D('',#192404,#96068,#96069);
#83675=AXIS2_PLACEMENT_3D('',#192408,#96071,#96072);
#83676=AXIS2_PLACEMENT_3D('',#192409,#96073,#96074);
#83677=AXIS2_PLACEMENT_3D('',#192410,#96075,#96076);
#83678=AXIS2_PLACEMENT_3D('',#192411,#96077,#96078);
#83679=AXIS2_PLACEMENT_3D('',#192412,#96079,#96080);
#83680=AXIS2_PLACEMENT_3D('',#192413,#96081,#96082);
#83681=AXIS2_PLACEMENT_3D('',#192418,#96084,#96085);
#83682=AXIS2_PLACEMENT_3D('',#192421,#96087,#96088);
#83683=AXIS2_PLACEMENT_3D('',#192422,#96089,#96090);
#83684=AXIS2_PLACEMENT_3D('',#192426,#96092,#96093);
#83685=AXIS2_PLACEMENT_3D('',#192427,#96094,#96095);
#83686=AXIS2_PLACEMENT_3D('',#192428,#96096,#96097);
#83687=AXIS2_PLACEMENT_3D('',#192432,#96099,#96100);
#83688=AXIS2_PLACEMENT_3D('',#192433,#96101,#96102);
#83689=AXIS2_PLACEMENT_3D('',#192434,#96103,#96104);
#83690=AXIS2_PLACEMENT_3D('',#192435,#96105,#96106);
#83691=AXIS2_PLACEMENT_3D('',#192436,#96107,#96108);
#83692=AXIS2_PLACEMENT_3D('',#192437,#96109,#96110);
#83693=AXIS2_PLACEMENT_3D('',#192442,#96112,#96113);
#83694=AXIS2_PLACEMENT_3D('',#192445,#96115,#96116);
#83695=AXIS2_PLACEMENT_3D('',#192446,#96117,#96118);
#83696=AXIS2_PLACEMENT_3D('',#192450,#96120,#96121);
#83697=AXIS2_PLACEMENT_3D('',#192451,#96122,#96123);
#83698=AXIS2_PLACEMENT_3D('',#192452,#96124,#96125);
#83699=AXIS2_PLACEMENT_3D('',#192456,#96127,#96128);
#83700=AXIS2_PLACEMENT_3D('',#192457,#96129,#96130);
#83701=AXIS2_PLACEMENT_3D('',#192458,#96131,#96132);
#83702=AXIS2_PLACEMENT_3D('',#192459,#96133,#96134);
#83703=AXIS2_PLACEMENT_3D('',#192460,#96135,#96136);
#83704=AXIS2_PLACEMENT_3D('',#192461,#96137,#96138);
#83705=AXIS2_PLACEMENT_3D('',#192466,#96140,#96141);
#83706=AXIS2_PLACEMENT_3D('',#192469,#96143,#96144);
#83707=AXIS2_PLACEMENT_3D('',#192470,#96145,#96146);
#83708=AXIS2_PLACEMENT_3D('',#192474,#96148,#96149);
#83709=AXIS2_PLACEMENT_3D('',#192475,#96150,#96151);
#83710=AXIS2_PLACEMENT_3D('',#192476,#96152,#96153);
#83711=AXIS2_PLACEMENT_3D('',#192480,#96155,#96156);
#83712=AXIS2_PLACEMENT_3D('',#192481,#96157,#96158);
#83713=AXIS2_PLACEMENT_3D('',#192482,#96159,#96160);
#83714=AXIS2_PLACEMENT_3D('',#192483,#96161,#96162);
#83715=AXIS2_PLACEMENT_3D('',#192484,#96163,#96164);
#83716=AXIS2_PLACEMENT_3D('',#192485,#96165,#96166);
#83717=AXIS2_PLACEMENT_3D('',#192490,#96168,#96169);
#83718=AXIS2_PLACEMENT_3D('',#192493,#96171,#96172);
#83719=AXIS2_PLACEMENT_3D('',#192494,#96173,#96174);
#83720=AXIS2_PLACEMENT_3D('',#192498,#96176,#96177);
#83721=AXIS2_PLACEMENT_3D('',#192499,#96178,#96179);
#83722=AXIS2_PLACEMENT_3D('',#192500,#96180,#96181);
#83723=AXIS2_PLACEMENT_3D('',#192504,#96183,#96184);
#83724=AXIS2_PLACEMENT_3D('',#192505,#96185,#96186);
#83725=AXIS2_PLACEMENT_3D('',#192506,#96187,#96188);
#83726=AXIS2_PLACEMENT_3D('',#192507,#96189,#96190);
#83727=AXIS2_PLACEMENT_3D('',#192508,#96191,#96192);
#83728=AXIS2_PLACEMENT_3D('',#192509,#96193,#96194);
#83729=AXIS2_PLACEMENT_3D('',#192514,#96196,#96197);
#83730=AXIS2_PLACEMENT_3D('',#192517,#96199,#96200);
#83731=AXIS2_PLACEMENT_3D('',#192518,#96201,#96202);
#83732=AXIS2_PLACEMENT_3D('',#192522,#96204,#96205);
#83733=AXIS2_PLACEMENT_3D('',#192523,#96206,#96207);
#83734=AXIS2_PLACEMENT_3D('',#192524,#96208,#96209);
#83735=AXIS2_PLACEMENT_3D('',#192528,#96211,#96212);
#83736=AXIS2_PLACEMENT_3D('',#192529,#96213,#96214);
#83737=AXIS2_PLACEMENT_3D('',#192530,#96215,#96216);
#83738=AXIS2_PLACEMENT_3D('',#192531,#96217,#96218);
#83739=AXIS2_PLACEMENT_3D('',#192532,#96219,#96220);
#83740=AXIS2_PLACEMENT_3D('',#192533,#96221,#96222);
#83741=AXIS2_PLACEMENT_3D('',#192538,#96224,#96225);
#83742=AXIS2_PLACEMENT_3D('',#192541,#96227,#96228);
#83743=AXIS2_PLACEMENT_3D('',#192542,#96229,#96230);
#83744=AXIS2_PLACEMENT_3D('',#192546,#96232,#96233);
#83745=AXIS2_PLACEMENT_3D('',#192547,#96234,#96235);
#83746=AXIS2_PLACEMENT_3D('',#192548,#96236,#96237);
#83747=AXIS2_PLACEMENT_3D('',#192552,#96239,#96240);
#83748=AXIS2_PLACEMENT_3D('',#192553,#96241,#96242);
#83749=AXIS2_PLACEMENT_3D('',#192554,#96243,#96244);
#83750=AXIS2_PLACEMENT_3D('',#192555,#96245,#96246);
#83751=AXIS2_PLACEMENT_3D('',#192556,#96247,#96248);
#83752=AXIS2_PLACEMENT_3D('',#192557,#96249,#96250);
#83753=AXIS2_PLACEMENT_3D('',#192562,#96252,#96253);
#83754=AXIS2_PLACEMENT_3D('',#192565,#96255,#96256);
#83755=AXIS2_PLACEMENT_3D('',#192566,#96257,#96258);
#83756=AXIS2_PLACEMENT_3D('',#192570,#96260,#96261);
#83757=AXIS2_PLACEMENT_3D('',#192571,#96262,#96263);
#83758=AXIS2_PLACEMENT_3D('',#192572,#96264,#96265);
#83759=AXIS2_PLACEMENT_3D('',#192576,#96267,#96268);
#83760=AXIS2_PLACEMENT_3D('',#192577,#96269,#96270);
#83761=AXIS2_PLACEMENT_3D('',#192578,#96271,#96272);
#83762=AXIS2_PLACEMENT_3D('',#192579,#96273,#96274);
#83763=AXIS2_PLACEMENT_3D('',#192580,#96275,#96276);
#83764=AXIS2_PLACEMENT_3D('',#192581,#96277,#96278);
#83765=AXIS2_PLACEMENT_3D('',#192586,#96280,#96281);
#83766=AXIS2_PLACEMENT_3D('',#192589,#96283,#96284);
#83767=AXIS2_PLACEMENT_3D('',#192590,#96285,#96286);
#83768=AXIS2_PLACEMENT_3D('',#192594,#96288,#96289);
#83769=AXIS2_PLACEMENT_3D('',#192595,#96290,#96291);
#83770=AXIS2_PLACEMENT_3D('',#192596,#96292,#96293);
#83771=AXIS2_PLACEMENT_3D('',#192600,#96295,#96296);
#83772=AXIS2_PLACEMENT_3D('',#192601,#96297,#96298);
#83773=AXIS2_PLACEMENT_3D('',#192602,#96299,#96300);
#83774=AXIS2_PLACEMENT_3D('',#192603,#96301,#96302);
#83775=AXIS2_PLACEMENT_3D('',#192604,#96303,#96304);
#83776=AXIS2_PLACEMENT_3D('',#192605,#96305,#96306);
#83777=AXIS2_PLACEMENT_3D('',#192610,#96308,#96309);
#83778=AXIS2_PLACEMENT_3D('',#192613,#96311,#96312);
#83779=AXIS2_PLACEMENT_3D('',#192614,#96313,#96314);
#83780=AXIS2_PLACEMENT_3D('',#192618,#96316,#96317);
#83781=AXIS2_PLACEMENT_3D('',#192619,#96318,#96319);
#83782=AXIS2_PLACEMENT_3D('',#192620,#96320,#96321);
#83783=AXIS2_PLACEMENT_3D('',#192624,#96323,#96324);
#83784=AXIS2_PLACEMENT_3D('',#192625,#96325,#96326);
#83785=AXIS2_PLACEMENT_3D('',#192626,#96327,#96328);
#83786=AXIS2_PLACEMENT_3D('',#192627,#96329,#96330);
#83787=AXIS2_PLACEMENT_3D('',#192628,#96331,#96332);
#83788=AXIS2_PLACEMENT_3D('',#192629,#96333,#96334);
#83789=AXIS2_PLACEMENT_3D('',#192634,#96336,#96337);
#83790=AXIS2_PLACEMENT_3D('',#192637,#96339,#96340);
#83791=AXIS2_PLACEMENT_3D('',#192638,#96341,#96342);
#83792=AXIS2_PLACEMENT_3D('',#192642,#96344,#96345);
#83793=AXIS2_PLACEMENT_3D('',#192643,#96346,#96347);
#83794=AXIS2_PLACEMENT_3D('',#192644,#96348,#96349);
#83795=AXIS2_PLACEMENT_3D('',#192648,#96351,#96352);
#83796=AXIS2_PLACEMENT_3D('',#192649,#96353,#96354);
#83797=AXIS2_PLACEMENT_3D('',#192650,#96355,#96356);
#83798=AXIS2_PLACEMENT_3D('',#192651,#96357,#96358);
#83799=AXIS2_PLACEMENT_3D('',#192652,#96359,#96360);
#83800=AXIS2_PLACEMENT_3D('',#192653,#96361,#96362);
#83801=AXIS2_PLACEMENT_3D('',#192658,#96364,#96365);
#83802=AXIS2_PLACEMENT_3D('',#192661,#96367,#96368);
#83803=AXIS2_PLACEMENT_3D('',#192662,#96369,#96370);
#83804=AXIS2_PLACEMENT_3D('',#192666,#96372,#96373);
#83805=AXIS2_PLACEMENT_3D('',#192667,#96374,#96375);
#83806=AXIS2_PLACEMENT_3D('',#192668,#96376,#96377);
#83807=AXIS2_PLACEMENT_3D('',#192672,#96379,#96380);
#83808=AXIS2_PLACEMENT_3D('',#192673,#96381,#96382);
#83809=AXIS2_PLACEMENT_3D('',#192674,#96383,#96384);
#83810=AXIS2_PLACEMENT_3D('',#192675,#96385,#96386);
#83811=AXIS2_PLACEMENT_3D('',#192676,#96387,#96388);
#83812=AXIS2_PLACEMENT_3D('',#192677,#96389,#96390);
#83813=AXIS2_PLACEMENT_3D('',#192682,#96392,#96393);
#83814=AXIS2_PLACEMENT_3D('',#192685,#96395,#96396);
#83815=AXIS2_PLACEMENT_3D('',#192686,#96397,#96398);
#83816=AXIS2_PLACEMENT_3D('',#192690,#96400,#96401);
#83817=AXIS2_PLACEMENT_3D('',#192691,#96402,#96403);
#83818=AXIS2_PLACEMENT_3D('',#192692,#96404,#96405);
#83819=AXIS2_PLACEMENT_3D('',#192696,#96407,#96408);
#83820=AXIS2_PLACEMENT_3D('',#192697,#96409,#96410);
#83821=AXIS2_PLACEMENT_3D('',#192698,#96411,#96412);
#83822=AXIS2_PLACEMENT_3D('',#192699,#96413,#96414);
#83823=AXIS2_PLACEMENT_3D('',#192700,#96415,#96416);
#83824=AXIS2_PLACEMENT_3D('',#192701,#96417,#96418);
#83825=AXIS2_PLACEMENT_3D('',#192706,#96420,#96421);
#83826=AXIS2_PLACEMENT_3D('',#192709,#96423,#96424);
#83827=AXIS2_PLACEMENT_3D('',#192710,#96425,#96426);
#83828=AXIS2_PLACEMENT_3D('',#192714,#96428,#96429);
#83829=AXIS2_PLACEMENT_3D('',#192715,#96430,#96431);
#83830=AXIS2_PLACEMENT_3D('',#192716,#96432,#96433);
#83831=AXIS2_PLACEMENT_3D('',#192720,#96435,#96436);
#83832=AXIS2_PLACEMENT_3D('',#192721,#96437,#96438);
#83833=AXIS2_PLACEMENT_3D('',#192722,#96439,#96440);
#83834=AXIS2_PLACEMENT_3D('',#192723,#96441,#96442);
#83835=AXIS2_PLACEMENT_3D('',#192724,#96443,#96444);
#83836=AXIS2_PLACEMENT_3D('',#192725,#96445,#96446);
#83837=AXIS2_PLACEMENT_3D('',#192730,#96448,#96449);
#83838=AXIS2_PLACEMENT_3D('',#192733,#96451,#96452);
#83839=AXIS2_PLACEMENT_3D('',#192734,#96453,#96454);
#83840=AXIS2_PLACEMENT_3D('',#192738,#96456,#96457);
#83841=AXIS2_PLACEMENT_3D('',#192739,#96458,#96459);
#83842=AXIS2_PLACEMENT_3D('',#192740,#96460,#96461);
#83843=AXIS2_PLACEMENT_3D('',#192744,#96463,#96464);
#83844=AXIS2_PLACEMENT_3D('',#192745,#96465,#96466);
#83845=AXIS2_PLACEMENT_3D('',#192746,#96467,#96468);
#83846=AXIS2_PLACEMENT_3D('',#192747,#96469,#96470);
#83847=AXIS2_PLACEMENT_3D('',#192748,#96471,#96472);
#83848=AXIS2_PLACEMENT_3D('',#192749,#96473,#96474);
#83849=AXIS2_PLACEMENT_3D('',#192754,#96476,#96477);
#83850=AXIS2_PLACEMENT_3D('',#192757,#96479,#96480);
#83851=AXIS2_PLACEMENT_3D('',#192758,#96481,#96482);
#83852=AXIS2_PLACEMENT_3D('',#192762,#96484,#96485);
#83853=AXIS2_PLACEMENT_3D('',#192763,#96486,#96487);
#83854=AXIS2_PLACEMENT_3D('',#192764,#96488,#96489);
#83855=AXIS2_PLACEMENT_3D('',#192768,#96491,#96492);
#83856=AXIS2_PLACEMENT_3D('',#192769,#96493,#96494);
#83857=AXIS2_PLACEMENT_3D('',#192770,#96495,#96496);
#83858=AXIS2_PLACEMENT_3D('',#192771,#96497,#96498);
#83859=AXIS2_PLACEMENT_3D('',#192772,#96499,#96500);
#83860=AXIS2_PLACEMENT_3D('',#192773,#96501,#96502);
#83861=AXIS2_PLACEMENT_3D('',#192778,#96504,#96505);
#83862=AXIS2_PLACEMENT_3D('',#192781,#96507,#96508);
#83863=AXIS2_PLACEMENT_3D('',#192782,#96509,#96510);
#83864=AXIS2_PLACEMENT_3D('',#192786,#96512,#96513);
#83865=AXIS2_PLACEMENT_3D('',#192787,#96514,#96515);
#83866=AXIS2_PLACEMENT_3D('',#192788,#96516,#96517);
#83867=AXIS2_PLACEMENT_3D('',#192792,#96519,#96520);
#83868=AXIS2_PLACEMENT_3D('',#192793,#96521,#96522);
#83869=AXIS2_PLACEMENT_3D('',#192794,#96523,#96524);
#83870=AXIS2_PLACEMENT_3D('',#192795,#96525,#96526);
#83871=AXIS2_PLACEMENT_3D('',#192796,#96527,#96528);
#83872=AXIS2_PLACEMENT_3D('',#192797,#96529,#96530);
#83873=AXIS2_PLACEMENT_3D('',#192802,#96532,#96533);
#83874=AXIS2_PLACEMENT_3D('',#192805,#96535,#96536);
#83875=AXIS2_PLACEMENT_3D('',#192806,#96537,#96538);
#83876=AXIS2_PLACEMENT_3D('',#192810,#96540,#96541);
#83877=AXIS2_PLACEMENT_3D('',#192811,#96542,#96543);
#83878=AXIS2_PLACEMENT_3D('',#192812,#96544,#96545);
#83879=AXIS2_PLACEMENT_3D('',#192816,#96547,#96548);
#83880=AXIS2_PLACEMENT_3D('',#192817,#96549,#96550);
#83881=AXIS2_PLACEMENT_3D('',#192818,#96551,#96552);
#83882=AXIS2_PLACEMENT_3D('',#192819,#96553,#96554);
#83883=AXIS2_PLACEMENT_3D('',#192820,#96555,#96556);
#83884=AXIS2_PLACEMENT_3D('',#192821,#96557,#96558);
#83885=AXIS2_PLACEMENT_3D('',#192826,#96560,#96561);
#83886=AXIS2_PLACEMENT_3D('',#192829,#96563,#96564);
#83887=AXIS2_PLACEMENT_3D('',#192830,#96565,#96566);
#83888=AXIS2_PLACEMENT_3D('',#192834,#96568,#96569);
#83889=AXIS2_PLACEMENT_3D('',#192835,#96570,#96571);
#83890=AXIS2_PLACEMENT_3D('',#192836,#96572,#96573);
#83891=AXIS2_PLACEMENT_3D('',#192840,#96575,#96576);
#83892=AXIS2_PLACEMENT_3D('',#192841,#96577,#96578);
#83893=AXIS2_PLACEMENT_3D('',#192842,#96579,#96580);
#83894=AXIS2_PLACEMENT_3D('',#192843,#96581,#96582);
#83895=AXIS2_PLACEMENT_3D('',#192844,#96583,#96584);
#83896=AXIS2_PLACEMENT_3D('',#192845,#96585,#96586);
#83897=AXIS2_PLACEMENT_3D('',#192850,#96588,#96589);
#83898=AXIS2_PLACEMENT_3D('',#192853,#96591,#96592);
#83899=AXIS2_PLACEMENT_3D('',#192854,#96593,#96594);
#83900=AXIS2_PLACEMENT_3D('',#192858,#96596,#96597);
#83901=AXIS2_PLACEMENT_3D('',#192859,#96598,#96599);
#83902=AXIS2_PLACEMENT_3D('',#192860,#96600,#96601);
#83903=AXIS2_PLACEMENT_3D('',#192864,#96603,#96604);
#83904=AXIS2_PLACEMENT_3D('',#192865,#96605,#96606);
#83905=AXIS2_PLACEMENT_3D('',#192866,#96607,#96608);
#83906=AXIS2_PLACEMENT_3D('',#192867,#96609,#96610);
#83907=AXIS2_PLACEMENT_3D('',#192868,#96611,#96612);
#83908=AXIS2_PLACEMENT_3D('',#192869,#96613,#96614);
#83909=AXIS2_PLACEMENT_3D('',#192874,#96616,#96617);
#83910=AXIS2_PLACEMENT_3D('',#192877,#96619,#96620);
#83911=AXIS2_PLACEMENT_3D('',#192878,#96621,#96622);
#83912=AXIS2_PLACEMENT_3D('',#192882,#96624,#96625);
#83913=AXIS2_PLACEMENT_3D('',#192883,#96626,#96627);
#83914=AXIS2_PLACEMENT_3D('',#192884,#96628,#96629);
#83915=AXIS2_PLACEMENT_3D('',#192888,#96631,#96632);
#83916=AXIS2_PLACEMENT_3D('',#192889,#96633,#96634);
#83917=AXIS2_PLACEMENT_3D('',#192890,#96635,#96636);
#83918=AXIS2_PLACEMENT_3D('',#192891,#96637,#96638);
#83919=AXIS2_PLACEMENT_3D('',#192892,#96639,#96640);
#83920=AXIS2_PLACEMENT_3D('',#192893,#96641,#96642);
#83921=AXIS2_PLACEMENT_3D('',#192898,#96644,#96645);
#83922=AXIS2_PLACEMENT_3D('',#192901,#96647,#96648);
#83923=AXIS2_PLACEMENT_3D('',#192902,#96649,#96650);
#83924=AXIS2_PLACEMENT_3D('',#192906,#96652,#96653);
#83925=AXIS2_PLACEMENT_3D('',#192907,#96654,#96655);
#83926=AXIS2_PLACEMENT_3D('',#192908,#96656,#96657);
#83927=AXIS2_PLACEMENT_3D('',#192912,#96659,#96660);
#83928=AXIS2_PLACEMENT_3D('',#192913,#96661,#96662);
#83929=AXIS2_PLACEMENT_3D('',#192914,#96663,#96664);
#83930=AXIS2_PLACEMENT_3D('',#192915,#96665,#96666);
#83931=AXIS2_PLACEMENT_3D('',#192916,#96667,#96668);
#83932=AXIS2_PLACEMENT_3D('',#192917,#96669,#96670);
#83933=AXIS2_PLACEMENT_3D('',#192922,#96672,#96673);
#83934=AXIS2_PLACEMENT_3D('',#192925,#96675,#96676);
#83935=AXIS2_PLACEMENT_3D('',#192926,#96677,#96678);
#83936=AXIS2_PLACEMENT_3D('',#192930,#96680,#96681);
#83937=AXIS2_PLACEMENT_3D('',#192931,#96682,#96683);
#83938=AXIS2_PLACEMENT_3D('',#192932,#96684,#96685);
#83939=AXIS2_PLACEMENT_3D('',#192936,#96687,#96688);
#83940=AXIS2_PLACEMENT_3D('',#192937,#96689,#96690);
#83941=AXIS2_PLACEMENT_3D('',#192938,#96691,#96692);
#83942=AXIS2_PLACEMENT_3D('',#192939,#96693,#96694);
#83943=AXIS2_PLACEMENT_3D('',#192940,#96695,#96696);
#83944=AXIS2_PLACEMENT_3D('',#192941,#96697,#96698);
#83945=AXIS2_PLACEMENT_3D('',#192946,#96700,#96701);
#83946=AXIS2_PLACEMENT_3D('',#192949,#96703,#96704);
#83947=AXIS2_PLACEMENT_3D('',#192950,#96705,#96706);
#83948=AXIS2_PLACEMENT_3D('',#192954,#96708,#96709);
#83949=AXIS2_PLACEMENT_3D('',#192955,#96710,#96711);
#83950=AXIS2_PLACEMENT_3D('',#192956,#96712,#96713);
#83951=AXIS2_PLACEMENT_3D('',#192960,#96715,#96716);
#83952=AXIS2_PLACEMENT_3D('',#192961,#96717,#96718);
#83953=AXIS2_PLACEMENT_3D('',#192962,#96719,#96720);
#83954=AXIS2_PLACEMENT_3D('',#192963,#96721,#96722);
#83955=AXIS2_PLACEMENT_3D('',#192964,#96723,#96724);
#83956=AXIS2_PLACEMENT_3D('',#192965,#96725,#96726);
#83957=AXIS2_PLACEMENT_3D('',#192970,#96728,#96729);
#83958=AXIS2_PLACEMENT_3D('',#192973,#96731,#96732);
#83959=AXIS2_PLACEMENT_3D('',#192974,#96733,#96734);
#83960=AXIS2_PLACEMENT_3D('',#192978,#96736,#96737);
#83961=AXIS2_PLACEMENT_3D('',#192979,#96738,#96739);
#83962=AXIS2_PLACEMENT_3D('',#192980,#96740,#96741);
#83963=AXIS2_PLACEMENT_3D('',#192984,#96743,#96744);
#83964=AXIS2_PLACEMENT_3D('',#192985,#96745,#96746);
#83965=AXIS2_PLACEMENT_3D('',#192986,#96747,#96748);
#83966=AXIS2_PLACEMENT_3D('',#192987,#96749,#96750);
#83967=AXIS2_PLACEMENT_3D('',#192988,#96751,#96752);
#83968=AXIS2_PLACEMENT_3D('',#192989,#96753,#96754);
#83969=AXIS2_PLACEMENT_3D('',#192994,#96756,#96757);
#83970=AXIS2_PLACEMENT_3D('',#192997,#96759,#96760);
#83971=AXIS2_PLACEMENT_3D('',#192998,#96761,#96762);
#83972=AXIS2_PLACEMENT_3D('',#193002,#96764,#96765);
#83973=AXIS2_PLACEMENT_3D('',#193003,#96766,#96767);
#83974=AXIS2_PLACEMENT_3D('',#193004,#96768,#96769);
#83975=AXIS2_PLACEMENT_3D('',#193008,#96771,#96772);
#83976=AXIS2_PLACEMENT_3D('',#193009,#96773,#96774);
#83977=AXIS2_PLACEMENT_3D('',#193010,#96775,#96776);
#83978=AXIS2_PLACEMENT_3D('',#193011,#96777,#96778);
#83979=AXIS2_PLACEMENT_3D('',#193012,#96779,#96780);
#83980=AXIS2_PLACEMENT_3D('',#193013,#96781,#96782);
#83981=AXIS2_PLACEMENT_3D('',#193018,#96784,#96785);
#83982=AXIS2_PLACEMENT_3D('',#193021,#96787,#96788);
#83983=AXIS2_PLACEMENT_3D('',#193022,#96789,#96790);
#83984=AXIS2_PLACEMENT_3D('',#193026,#96792,#96793);
#83985=AXIS2_PLACEMENT_3D('',#193027,#96794,#96795);
#83986=AXIS2_PLACEMENT_3D('',#193028,#96796,#96797);
#83987=AXIS2_PLACEMENT_3D('',#193032,#96799,#96800);
#83988=AXIS2_PLACEMENT_3D('',#193033,#96801,#96802);
#83989=AXIS2_PLACEMENT_3D('',#193034,#96803,#96804);
#83990=AXIS2_PLACEMENT_3D('',#193035,#96805,#96806);
#83991=AXIS2_PLACEMENT_3D('',#193036,#96807,#96808);
#83992=AXIS2_PLACEMENT_3D('',#193037,#96809,#96810);
#83993=AXIS2_PLACEMENT_3D('',#193042,#96812,#96813);
#83994=AXIS2_PLACEMENT_3D('',#193045,#96815,#96816);
#83995=AXIS2_PLACEMENT_3D('',#193046,#96817,#96818);
#83996=AXIS2_PLACEMENT_3D('',#193050,#96820,#96821);
#83997=AXIS2_PLACEMENT_3D('',#193051,#96822,#96823);
#83998=AXIS2_PLACEMENT_3D('',#193052,#96824,#96825);
#83999=AXIS2_PLACEMENT_3D('',#193056,#96827,#96828);
#84000=AXIS2_PLACEMENT_3D('',#193057,#96829,#96830);
#84001=AXIS2_PLACEMENT_3D('',#193058,#96831,#96832);
#84002=AXIS2_PLACEMENT_3D('',#193059,#96833,#96834);
#84003=AXIS2_PLACEMENT_3D('',#193060,#96835,#96836);
#84004=AXIS2_PLACEMENT_3D('',#193061,#96837,#96838);
#84005=AXIS2_PLACEMENT_3D('',#193066,#96840,#96841);
#84006=AXIS2_PLACEMENT_3D('',#193069,#96843,#96844);
#84007=AXIS2_PLACEMENT_3D('',#193070,#96845,#96846);
#84008=AXIS2_PLACEMENT_3D('',#193074,#96848,#96849);
#84009=AXIS2_PLACEMENT_3D('',#193075,#96850,#96851);
#84010=AXIS2_PLACEMENT_3D('',#193076,#96852,#96853);
#84011=AXIS2_PLACEMENT_3D('',#193080,#96855,#96856);
#84012=AXIS2_PLACEMENT_3D('',#193081,#96857,#96858);
#84013=AXIS2_PLACEMENT_3D('',#193082,#96859,#96860);
#84014=AXIS2_PLACEMENT_3D('',#193083,#96861,#96862);
#84015=AXIS2_PLACEMENT_3D('',#193084,#96863,#96864);
#84016=AXIS2_PLACEMENT_3D('',#193085,#96865,#96866);
#84017=AXIS2_PLACEMENT_3D('',#193090,#96868,#96869);
#84018=AXIS2_PLACEMENT_3D('',#193093,#96871,#96872);
#84019=AXIS2_PLACEMENT_3D('',#193094,#96873,#96874);
#84020=AXIS2_PLACEMENT_3D('',#193098,#96876,#96877);
#84021=AXIS2_PLACEMENT_3D('',#193099,#96878,#96879);
#84022=AXIS2_PLACEMENT_3D('',#193100,#96880,#96881);
#84023=AXIS2_PLACEMENT_3D('',#193104,#96883,#96884);
#84024=AXIS2_PLACEMENT_3D('',#193105,#96885,#96886);
#84025=AXIS2_PLACEMENT_3D('',#193106,#96887,#96888);
#84026=AXIS2_PLACEMENT_3D('',#193107,#96889,#96890);
#84027=AXIS2_PLACEMENT_3D('',#193108,#96891,#96892);
#84028=AXIS2_PLACEMENT_3D('',#193109,#96893,#96894);
#84029=AXIS2_PLACEMENT_3D('',#193114,#96896,#96897);
#84030=AXIS2_PLACEMENT_3D('',#193117,#96899,#96900);
#84031=AXIS2_PLACEMENT_3D('',#193118,#96901,#96902);
#84032=AXIS2_PLACEMENT_3D('',#193122,#96904,#96905);
#84033=AXIS2_PLACEMENT_3D('',#193123,#96906,#96907);
#84034=AXIS2_PLACEMENT_3D('',#193124,#96908,#96909);
#84035=AXIS2_PLACEMENT_3D('',#193128,#96911,#96912);
#84036=AXIS2_PLACEMENT_3D('',#193129,#96913,#96914);
#84037=AXIS2_PLACEMENT_3D('',#193130,#96915,#96916);
#84038=AXIS2_PLACEMENT_3D('',#193131,#96917,#96918);
#84039=AXIS2_PLACEMENT_3D('',#193132,#96919,#96920);
#84040=AXIS2_PLACEMENT_3D('',#193133,#96921,#96922);
#84041=AXIS2_PLACEMENT_3D('',#193138,#96924,#96925);
#84042=AXIS2_PLACEMENT_3D('',#193141,#96927,#96928);
#84043=AXIS2_PLACEMENT_3D('',#193142,#96929,#96930);
#84044=AXIS2_PLACEMENT_3D('',#193146,#96932,#96933);
#84045=AXIS2_PLACEMENT_3D('',#193147,#96934,#96935);
#84046=AXIS2_PLACEMENT_3D('',#193148,#96936,#96937);
#84047=AXIS2_PLACEMENT_3D('',#193152,#96939,#96940);
#84048=AXIS2_PLACEMENT_3D('',#193153,#96941,#96942);
#84049=AXIS2_PLACEMENT_3D('',#193154,#96943,#96944);
#84050=AXIS2_PLACEMENT_3D('',#193155,#96945,#96946);
#84051=AXIS2_PLACEMENT_3D('',#193156,#96947,#96948);
#84052=AXIS2_PLACEMENT_3D('',#193157,#96949,#96950);
#84053=AXIS2_PLACEMENT_3D('',#193162,#96952,#96953);
#84054=AXIS2_PLACEMENT_3D('',#193165,#96955,#96956);
#84055=AXIS2_PLACEMENT_3D('',#193166,#96957,#96958);
#84056=AXIS2_PLACEMENT_3D('',#193170,#96960,#96961);
#84057=AXIS2_PLACEMENT_3D('',#193171,#96962,#96963);
#84058=AXIS2_PLACEMENT_3D('',#193172,#96964,#96965);
#84059=AXIS2_PLACEMENT_3D('',#193176,#96967,#96968);
#84060=AXIS2_PLACEMENT_3D('',#193177,#96969,#96970);
#84061=AXIS2_PLACEMENT_3D('',#193178,#96971,#96972);
#84062=AXIS2_PLACEMENT_3D('',#193179,#96973,#96974);
#84063=AXIS2_PLACEMENT_3D('',#193180,#96975,#96976);
#84064=AXIS2_PLACEMENT_3D('',#193181,#96977,#96978);
#84065=AXIS2_PLACEMENT_3D('',#193186,#96980,#96981);
#84066=AXIS2_PLACEMENT_3D('',#193189,#96983,#96984);
#84067=AXIS2_PLACEMENT_3D('',#193190,#96985,#96986);
#84068=AXIS2_PLACEMENT_3D('',#193194,#96988,#96989);
#84069=AXIS2_PLACEMENT_3D('',#193195,#96990,#96991);
#84070=AXIS2_PLACEMENT_3D('',#193196,#96992,#96993);
#84071=AXIS2_PLACEMENT_3D('',#193200,#96995,#96996);
#84072=AXIS2_PLACEMENT_3D('',#193201,#96997,#96998);
#84073=AXIS2_PLACEMENT_3D('',#193202,#96999,#97000);
#84074=AXIS2_PLACEMENT_3D('',#193203,#97001,#97002);
#84075=AXIS2_PLACEMENT_3D('',#193204,#97003,#97004);
#84076=AXIS2_PLACEMENT_3D('',#193205,#97005,#97006);
#84077=AXIS2_PLACEMENT_3D('',#193210,#97008,#97009);
#84078=AXIS2_PLACEMENT_3D('',#193213,#97011,#97012);
#84079=AXIS2_PLACEMENT_3D('',#193214,#97013,#97014);
#84080=AXIS2_PLACEMENT_3D('',#193218,#97016,#97017);
#84081=AXIS2_PLACEMENT_3D('',#193219,#97018,#97019);
#84082=AXIS2_PLACEMENT_3D('',#193220,#97020,#97021);
#84083=AXIS2_PLACEMENT_3D('',#193224,#97023,#97024);
#84084=AXIS2_PLACEMENT_3D('',#193225,#97025,#97026);
#84085=AXIS2_PLACEMENT_3D('',#193226,#97027,#97028);
#84086=AXIS2_PLACEMENT_3D('',#193227,#97029,#97030);
#84087=AXIS2_PLACEMENT_3D('',#193228,#97031,#97032);
#84088=AXIS2_PLACEMENT_3D('',#193229,#97033,#97034);
#84089=AXIS2_PLACEMENT_3D('',#193234,#97036,#97037);
#84090=AXIS2_PLACEMENT_3D('',#193237,#97039,#97040);
#84091=AXIS2_PLACEMENT_3D('',#193238,#97041,#97042);
#84092=AXIS2_PLACEMENT_3D('',#193242,#97044,#97045);
#84093=AXIS2_PLACEMENT_3D('',#193243,#97046,#97047);
#84094=AXIS2_PLACEMENT_3D('',#193244,#97048,#97049);
#84095=AXIS2_PLACEMENT_3D('',#193248,#97051,#97052);
#84096=AXIS2_PLACEMENT_3D('',#193249,#97053,#97054);
#84097=AXIS2_PLACEMENT_3D('',#193250,#97055,#97056);
#84098=AXIS2_PLACEMENT_3D('',#193251,#97057,#97058);
#84099=AXIS2_PLACEMENT_3D('',#193252,#97059,#97060);
#84100=AXIS2_PLACEMENT_3D('',#193253,#97061,#97062);
#84101=AXIS2_PLACEMENT_3D('',#193258,#97064,#97065);
#84102=AXIS2_PLACEMENT_3D('',#193261,#97067,#97068);
#84103=AXIS2_PLACEMENT_3D('',#193262,#97069,#97070);
#84104=AXIS2_PLACEMENT_3D('',#193266,#97072,#97073);
#84105=AXIS2_PLACEMENT_3D('',#193267,#97074,#97075);
#84106=AXIS2_PLACEMENT_3D('',#193268,#97076,#97077);
#84107=AXIS2_PLACEMENT_3D('',#193272,#97079,#97080);
#84108=AXIS2_PLACEMENT_3D('',#193273,#97081,#97082);
#84109=AXIS2_PLACEMENT_3D('',#193274,#97083,#97084);
#84110=AXIS2_PLACEMENT_3D('',#193275,#97085,#97086);
#84111=AXIS2_PLACEMENT_3D('',#193276,#97087,#97088);
#84112=AXIS2_PLACEMENT_3D('',#193277,#97089,#97090);
#84113=AXIS2_PLACEMENT_3D('',#193282,#97092,#97093);
#84114=AXIS2_PLACEMENT_3D('',#193285,#97095,#97096);
#84115=AXIS2_PLACEMENT_3D('',#193286,#97097,#97098);
#84116=AXIS2_PLACEMENT_3D('',#193290,#97100,#97101);
#84117=AXIS2_PLACEMENT_3D('',#193291,#97102,#97103);
#84118=AXIS2_PLACEMENT_3D('',#193292,#97104,#97105);
#84119=AXIS2_PLACEMENT_3D('',#193296,#97107,#97108);
#84120=AXIS2_PLACEMENT_3D('',#193297,#97109,#97110);
#84121=AXIS2_PLACEMENT_3D('',#193298,#97111,#97112);
#84122=AXIS2_PLACEMENT_3D('',#193299,#97113,#97114);
#84123=AXIS2_PLACEMENT_3D('',#193300,#97115,#97116);
#84124=AXIS2_PLACEMENT_3D('',#193301,#97117,#97118);
#84125=AXIS2_PLACEMENT_3D('',#193306,#97120,#97121);
#84126=AXIS2_PLACEMENT_3D('',#193309,#97123,#97124);
#84127=AXIS2_PLACEMENT_3D('',#193310,#97125,#97126);
#84128=AXIS2_PLACEMENT_3D('',#193314,#97128,#97129);
#84129=AXIS2_PLACEMENT_3D('',#193315,#97130,#97131);
#84130=AXIS2_PLACEMENT_3D('',#193316,#97132,#97133);
#84131=AXIS2_PLACEMENT_3D('',#193320,#97135,#97136);
#84132=AXIS2_PLACEMENT_3D('',#193321,#97137,#97138);
#84133=AXIS2_PLACEMENT_3D('',#193322,#97139,#97140);
#84134=AXIS2_PLACEMENT_3D('',#193323,#97141,#97142);
#84135=AXIS2_PLACEMENT_3D('',#193324,#97143,#97144);
#84136=AXIS2_PLACEMENT_3D('',#193325,#97145,#97146);
#84137=AXIS2_PLACEMENT_3D('',#193330,#97148,#97149);
#84138=AXIS2_PLACEMENT_3D('',#193333,#97151,#97152);
#84139=AXIS2_PLACEMENT_3D('',#193334,#97153,#97154);
#84140=AXIS2_PLACEMENT_3D('',#193338,#97156,#97157);
#84141=AXIS2_PLACEMENT_3D('',#193339,#97158,#97159);
#84142=AXIS2_PLACEMENT_3D('',#193340,#97160,#97161);
#84143=AXIS2_PLACEMENT_3D('',#193344,#97163,#97164);
#84144=AXIS2_PLACEMENT_3D('',#193345,#97165,#97166);
#84145=AXIS2_PLACEMENT_3D('',#193346,#97167,#97168);
#84146=AXIS2_PLACEMENT_3D('',#193347,#97169,#97170);
#84147=AXIS2_PLACEMENT_3D('',#193348,#97171,#97172);
#84148=AXIS2_PLACEMENT_3D('',#193349,#97173,#97174);
#84149=AXIS2_PLACEMENT_3D('',#193354,#97176,#97177);
#84150=AXIS2_PLACEMENT_3D('',#193357,#97179,#97180);
#84151=AXIS2_PLACEMENT_3D('',#193358,#97181,#97182);
#84152=AXIS2_PLACEMENT_3D('',#193362,#97184,#97185);
#84153=AXIS2_PLACEMENT_3D('',#193363,#97186,#97187);
#84154=AXIS2_PLACEMENT_3D('',#193364,#97188,#97189);
#84155=AXIS2_PLACEMENT_3D('',#193368,#97191,#97192);
#84156=AXIS2_PLACEMENT_3D('',#193369,#97193,#97194);
#84157=AXIS2_PLACEMENT_3D('',#193370,#97195,#97196);
#84158=AXIS2_PLACEMENT_3D('',#193371,#97197,#97198);
#84159=AXIS2_PLACEMENT_3D('',#193372,#97199,#97200);
#84160=AXIS2_PLACEMENT_3D('',#193373,#97201,#97202);
#84161=AXIS2_PLACEMENT_3D('',#193378,#97204,#97205);
#84162=AXIS2_PLACEMENT_3D('',#193381,#97207,#97208);
#84163=AXIS2_PLACEMENT_3D('',#193382,#97209,#97210);
#84164=AXIS2_PLACEMENT_3D('',#193386,#97212,#97213);
#84165=AXIS2_PLACEMENT_3D('',#193387,#97214,#97215);
#84166=AXIS2_PLACEMENT_3D('',#193388,#97216,#97217);
#84167=AXIS2_PLACEMENT_3D('',#193392,#97219,#97220);
#84168=AXIS2_PLACEMENT_3D('',#193393,#97221,#97222);
#84169=AXIS2_PLACEMENT_3D('',#193394,#97223,#97224);
#84170=AXIS2_PLACEMENT_3D('',#193395,#97225,#97226);
#84171=AXIS2_PLACEMENT_3D('',#193396,#97227,#97228);
#84172=AXIS2_PLACEMENT_3D('',#193397,#97229,#97230);
#84173=AXIS2_PLACEMENT_3D('',#193402,#97232,#97233);
#84174=AXIS2_PLACEMENT_3D('',#193405,#97235,#97236);
#84175=AXIS2_PLACEMENT_3D('',#193406,#97237,#97238);
#84176=AXIS2_PLACEMENT_3D('',#193410,#97240,#97241);
#84177=AXIS2_PLACEMENT_3D('',#193411,#97242,#97243);
#84178=AXIS2_PLACEMENT_3D('',#193412,#97244,#97245);
#84179=AXIS2_PLACEMENT_3D('',#193416,#97247,#97248);
#84180=AXIS2_PLACEMENT_3D('',#193417,#97249,#97250);
#84181=AXIS2_PLACEMENT_3D('',#193418,#97251,#97252);
#84182=AXIS2_PLACEMENT_3D('',#193419,#97253,#97254);
#84183=AXIS2_PLACEMENT_3D('',#193420,#97255,#97256);
#84184=AXIS2_PLACEMENT_3D('',#193421,#97257,#97258);
#84185=AXIS2_PLACEMENT_3D('',#193422,#97259,#97260);
#84186=AXIS2_PLACEMENT_3D('',#193431,#97265,#97266);
#84187=AXIS2_PLACEMENT_3D('',#193437,#97270,#97271);
#84188=AXIS2_PLACEMENT_3D('',#193443,#97275,#97276);
#84189=AXIS2_PLACEMENT_3D('',#193446,#97279,#97280);
#84190=AXIS2_PLACEMENT_3D('',#193455,#97285,#97286);
#84191=AXIS2_PLACEMENT_3D('',#193461,#97290,#97291);
#84192=AXIS2_PLACEMENT_3D('',#193467,#97295,#97296);
#84193=AXIS2_PLACEMENT_3D('',#193470,#97299,#97300);
#84194=AXIS2_PLACEMENT_3D('',#193479,#97305,#97306);
#84195=AXIS2_PLACEMENT_3D('',#193485,#97310,#97311);
#84196=AXIS2_PLACEMENT_3D('',#193491,#97315,#97316);
#84197=AXIS2_PLACEMENT_3D('',#193494,#97319,#97320);
#84198=AXIS2_PLACEMENT_3D('',#193503,#97325,#97326);
#84199=AXIS2_PLACEMENT_3D('',#193509,#97330,#97331);
#84200=AXIS2_PLACEMENT_3D('',#193515,#97335,#97336);
#84201=AXIS2_PLACEMENT_3D('',#193518,#97339,#97340);
#84202=AXIS2_PLACEMENT_3D('',#193527,#97345,#97346);
#84203=AXIS2_PLACEMENT_3D('',#193533,#97350,#97351);
#84204=AXIS2_PLACEMENT_3D('',#193539,#97355,#97356);
#84205=AXIS2_PLACEMENT_3D('',#193542,#97359,#97360);
#84206=AXIS2_PLACEMENT_3D('',#193551,#97365,#97366);
#84207=AXIS2_PLACEMENT_3D('',#193557,#97370,#97371);
#84208=AXIS2_PLACEMENT_3D('',#193563,#97375,#97376);
#84209=AXIS2_PLACEMENT_3D('',#193566,#97379,#97380);
#84210=AXIS2_PLACEMENT_3D('',#193575,#97385,#97386);
#84211=AXIS2_PLACEMENT_3D('',#193581,#97390,#97391);
#84212=AXIS2_PLACEMENT_3D('',#193587,#97395,#97396);
#84213=AXIS2_PLACEMENT_3D('',#193590,#97399,#97400);
#84214=AXIS2_PLACEMENT_3D('',#193599,#97405,#97406);
#84215=AXIS2_PLACEMENT_3D('',#193605,#97410,#97411);
#84216=AXIS2_PLACEMENT_3D('',#193611,#97415,#97416);
#84217=AXIS2_PLACEMENT_3D('',#193614,#97419,#97420);
#84218=AXIS2_PLACEMENT_3D('',#193623,#97425,#97426);
#84219=AXIS2_PLACEMENT_3D('',#193629,#97430,#97431);
#84220=AXIS2_PLACEMENT_3D('',#193635,#97435,#97436);
#84221=AXIS2_PLACEMENT_3D('',#193638,#97439,#97440);
#84222=AXIS2_PLACEMENT_3D('',#193647,#97445,#97446);
#84223=AXIS2_PLACEMENT_3D('',#193653,#97450,#97451);
#84224=AXIS2_PLACEMENT_3D('',#193659,#97455,#97456);
#84225=AXIS2_PLACEMENT_3D('',#193662,#97459,#97460);
#84226=AXIS2_PLACEMENT_3D('',#193671,#97465,#97466);
#84227=AXIS2_PLACEMENT_3D('',#193677,#97470,#97471);
#84228=AXIS2_PLACEMENT_3D('',#193683,#97475,#97476);
#84229=AXIS2_PLACEMENT_3D('',#193686,#97479,#97480);
#84230=AXIS2_PLACEMENT_3D('',#193695,#97485,#97486);
#84231=AXIS2_PLACEMENT_3D('',#193701,#97490,#97491);
#84232=AXIS2_PLACEMENT_3D('',#193707,#97495,#97496);
#84233=AXIS2_PLACEMENT_3D('',#193710,#97499,#97500);
#84234=AXIS2_PLACEMENT_3D('',#193719,#97505,#97506);
#84235=AXIS2_PLACEMENT_3D('',#193725,#97510,#97511);
#84236=AXIS2_PLACEMENT_3D('',#193731,#97515,#97516);
#84237=AXIS2_PLACEMENT_3D('',#193734,#97519,#97520);
#84238=AXIS2_PLACEMENT_3D('',#193743,#97525,#97526);
#84239=AXIS2_PLACEMENT_3D('',#193749,#97530,#97531);
#84240=AXIS2_PLACEMENT_3D('',#193755,#97535,#97536);
#84241=AXIS2_PLACEMENT_3D('',#193758,#97539,#97540);
#84242=AXIS2_PLACEMENT_3D('',#193767,#97545,#97546);
#84243=AXIS2_PLACEMENT_3D('',#193773,#97550,#97551);
#84244=AXIS2_PLACEMENT_3D('',#193779,#97555,#97556);
#84245=AXIS2_PLACEMENT_3D('',#193782,#97559,#97560);
#84246=AXIS2_PLACEMENT_3D('',#193791,#97565,#97566);
#84247=AXIS2_PLACEMENT_3D('',#193797,#97570,#97571);
#84248=AXIS2_PLACEMENT_3D('',#193803,#97575,#97576);
#84249=AXIS2_PLACEMENT_3D('',#193806,#97579,#97580);
#84250=AXIS2_PLACEMENT_3D('',#193815,#97585,#97586);
#84251=AXIS2_PLACEMENT_3D('',#193821,#97590,#97591);
#84252=AXIS2_PLACEMENT_3D('',#193827,#97595,#97596);
#84253=AXIS2_PLACEMENT_3D('',#193830,#97599,#97600);
#84254=AXIS2_PLACEMENT_3D('',#193839,#97605,#97606);
#84255=AXIS2_PLACEMENT_3D('',#193845,#97610,#97611);
#84256=AXIS2_PLACEMENT_3D('',#193851,#97615,#97616);
#84257=AXIS2_PLACEMENT_3D('',#193854,#97619,#97620);
#84258=AXIS2_PLACEMENT_3D('',#193863,#97625,#97626);
#84259=AXIS2_PLACEMENT_3D('',#193869,#97630,#97631);
#84260=AXIS2_PLACEMENT_3D('',#193875,#97635,#97636);
#84261=AXIS2_PLACEMENT_3D('',#193878,#97639,#97640);
#84262=AXIS2_PLACEMENT_3D('',#193887,#97645,#97646);
#84263=AXIS2_PLACEMENT_3D('',#193893,#97650,#97651);
#84264=AXIS2_PLACEMENT_3D('',#193899,#97655,#97656);
#84265=AXIS2_PLACEMENT_3D('',#193902,#97659,#97660);
#84266=AXIS2_PLACEMENT_3D('',#193911,#97665,#97666);
#84267=AXIS2_PLACEMENT_3D('',#193917,#97670,#97671);
#84268=AXIS2_PLACEMENT_3D('',#193923,#97675,#97676);
#84269=AXIS2_PLACEMENT_3D('',#193926,#97679,#97680);
#84270=AXIS2_PLACEMENT_3D('',#193935,#97685,#97686);
#84271=AXIS2_PLACEMENT_3D('',#193941,#97690,#97691);
#84272=AXIS2_PLACEMENT_3D('',#193947,#97695,#97696);
#84273=AXIS2_PLACEMENT_3D('',#193950,#97699,#97700);
#84274=AXIS2_PLACEMENT_3D('',#193959,#97705,#97706);
#84275=AXIS2_PLACEMENT_3D('',#193965,#97710,#97711);
#84276=AXIS2_PLACEMENT_3D('',#193971,#97715,#97716);
#84277=AXIS2_PLACEMENT_3D('',#193974,#97719,#97720);
#84278=AXIS2_PLACEMENT_3D('',#193983,#97725,#97726);
#84279=AXIS2_PLACEMENT_3D('',#193989,#97730,#97731);
#84280=AXIS2_PLACEMENT_3D('',#193995,#97735,#97736);
#84281=AXIS2_PLACEMENT_3D('',#193998,#97739,#97740);
#84282=AXIS2_PLACEMENT_3D('',#194007,#97745,#97746);
#84283=AXIS2_PLACEMENT_3D('',#194013,#97750,#97751);
#84284=AXIS2_PLACEMENT_3D('',#194019,#97755,#97756);
#84285=AXIS2_PLACEMENT_3D('',#194022,#97759,#97760);
#84286=AXIS2_PLACEMENT_3D('',#194031,#97765,#97766);
#84287=AXIS2_PLACEMENT_3D('',#194037,#97770,#97771);
#84288=AXIS2_PLACEMENT_3D('',#194043,#97775,#97776);
#84289=AXIS2_PLACEMENT_3D('',#194046,#97779,#97780);
#84290=AXIS2_PLACEMENT_3D('',#194055,#97785,#97786);
#84291=AXIS2_PLACEMENT_3D('',#194061,#97790,#97791);
#84292=AXIS2_PLACEMENT_3D('',#194067,#97795,#97796);
#84293=AXIS2_PLACEMENT_3D('',#194070,#97799,#97800);
#84294=AXIS2_PLACEMENT_3D('',#194079,#97805,#97806);
#84295=AXIS2_PLACEMENT_3D('',#194085,#97810,#97811);
#84296=AXIS2_PLACEMENT_3D('',#194091,#97815,#97816);
#84297=AXIS2_PLACEMENT_3D('',#194094,#97819,#97820);
#84298=AXIS2_PLACEMENT_3D('',#194103,#97825,#97826);
#84299=AXIS2_PLACEMENT_3D('',#194109,#97830,#97831);
#84300=AXIS2_PLACEMENT_3D('',#194115,#97835,#97836);
#84301=AXIS2_PLACEMENT_3D('',#194118,#97839,#97840);
#84302=AXIS2_PLACEMENT_3D('',#194127,#97845,#97846);
#84303=AXIS2_PLACEMENT_3D('',#194133,#97850,#97851);
#84304=AXIS2_PLACEMENT_3D('',#194139,#97855,#97856);
#84305=AXIS2_PLACEMENT_3D('',#194142,#97859,#97860);
#84306=AXIS2_PLACEMENT_3D('',#194151,#97865,#97866);
#84307=AXIS2_PLACEMENT_3D('',#194157,#97870,#97871);
#84308=AXIS2_PLACEMENT_3D('',#194163,#97875,#97876);
#84309=AXIS2_PLACEMENT_3D('',#194166,#97879,#97880);
#84310=AXIS2_PLACEMENT_3D('',#194175,#97885,#97886);
#84311=AXIS2_PLACEMENT_3D('',#194181,#97890,#97891);
#84312=AXIS2_PLACEMENT_3D('',#194187,#97895,#97896);
#84313=AXIS2_PLACEMENT_3D('',#194190,#97899,#97900);
#84314=AXIS2_PLACEMENT_3D('',#194199,#97905,#97906);
#84315=AXIS2_PLACEMENT_3D('',#194205,#97910,#97911);
#84316=AXIS2_PLACEMENT_3D('',#194211,#97915,#97916);
#84317=AXIS2_PLACEMENT_3D('',#194214,#97919,#97920);
#84318=AXIS2_PLACEMENT_3D('',#194223,#97925,#97926);
#84319=AXIS2_PLACEMENT_3D('',#194229,#97930,#97931);
#84320=AXIS2_PLACEMENT_3D('',#194235,#97935,#97936);
#84321=AXIS2_PLACEMENT_3D('',#194238,#97939,#97940);
#84322=AXIS2_PLACEMENT_3D('',#194247,#97945,#97946);
#84323=AXIS2_PLACEMENT_3D('',#194253,#97950,#97951);
#84324=AXIS2_PLACEMENT_3D('',#194259,#97955,#97956);
#84325=AXIS2_PLACEMENT_3D('',#194262,#97959,#97960);
#84326=AXIS2_PLACEMENT_3D('',#194271,#97965,#97966);
#84327=AXIS2_PLACEMENT_3D('',#194277,#97970,#97971);
#84328=AXIS2_PLACEMENT_3D('',#194283,#97975,#97976);
#84329=AXIS2_PLACEMENT_3D('',#194286,#97979,#97980);
#84330=AXIS2_PLACEMENT_3D('',#194295,#97985,#97986);
#84331=AXIS2_PLACEMENT_3D('',#194301,#97990,#97991);
#84332=AXIS2_PLACEMENT_3D('',#194307,#97995,#97996);
#84333=AXIS2_PLACEMENT_3D('',#194310,#97999,#98000);
#84334=AXIS2_PLACEMENT_3D('',#194319,#98005,#98006);
#84335=AXIS2_PLACEMENT_3D('',#194325,#98010,#98011);
#84336=AXIS2_PLACEMENT_3D('',#194331,#98015,#98016);
#84337=AXIS2_PLACEMENT_3D('',#194334,#98019,#98020);
#84338=AXIS2_PLACEMENT_3D('',#194343,#98025,#98026);
#84339=AXIS2_PLACEMENT_3D('',#194349,#98030,#98031);
#84340=AXIS2_PLACEMENT_3D('',#194355,#98035,#98036);
#84341=AXIS2_PLACEMENT_3D('',#194358,#98039,#98040);
#84342=AXIS2_PLACEMENT_3D('',#194367,#98045,#98046);
#84343=AXIS2_PLACEMENT_3D('',#194373,#98050,#98051);
#84344=AXIS2_PLACEMENT_3D('',#194379,#98055,#98056);
#84345=AXIS2_PLACEMENT_3D('',#194382,#98059,#98060);
#84346=AXIS2_PLACEMENT_3D('',#194391,#98065,#98066);
#84347=AXIS2_PLACEMENT_3D('',#194397,#98070,#98071);
#84348=AXIS2_PLACEMENT_3D('',#194403,#98075,#98076);
#84349=AXIS2_PLACEMENT_3D('',#194406,#98079,#98080);
#84350=AXIS2_PLACEMENT_3D('',#194415,#98085,#98086);
#84351=AXIS2_PLACEMENT_3D('',#194421,#98090,#98091);
#84352=AXIS2_PLACEMENT_3D('',#194427,#98095,#98096);
#84353=AXIS2_PLACEMENT_3D('',#194430,#98099,#98100);
#84354=AXIS2_PLACEMENT_3D('',#194439,#98105,#98106);
#84355=AXIS2_PLACEMENT_3D('',#194445,#98110,#98111);
#84356=AXIS2_PLACEMENT_3D('',#194451,#98115,#98116);
#84357=AXIS2_PLACEMENT_3D('',#194454,#98119,#98120);
#84358=AXIS2_PLACEMENT_3D('',#194463,#98125,#98126);
#84359=AXIS2_PLACEMENT_3D('',#194469,#98130,#98131);
#84360=AXIS2_PLACEMENT_3D('',#194475,#98135,#98136);
#84361=AXIS2_PLACEMENT_3D('',#194478,#98139,#98140);
#84362=AXIS2_PLACEMENT_3D('',#194487,#98145,#98146);
#84363=AXIS2_PLACEMENT_3D('',#194493,#98150,#98151);
#84364=AXIS2_PLACEMENT_3D('',#194499,#98155,#98156);
#84365=AXIS2_PLACEMENT_3D('',#194502,#98159,#98160);
#84366=AXIS2_PLACEMENT_3D('',#194511,#98165,#98166);
#84367=AXIS2_PLACEMENT_3D('',#194517,#98170,#98171);
#84368=AXIS2_PLACEMENT_3D('',#194523,#98175,#98176);
#84369=AXIS2_PLACEMENT_3D('',#194526,#98179,#98180);
#84370=AXIS2_PLACEMENT_3D('',#194535,#98185,#98186);
#84371=AXIS2_PLACEMENT_3D('',#194541,#98190,#98191);
#84372=AXIS2_PLACEMENT_3D('',#194547,#98195,#98196);
#84373=AXIS2_PLACEMENT_3D('',#194550,#98199,#98200);
#84374=AXIS2_PLACEMENT_3D('',#194559,#98205,#98206);
#84375=AXIS2_PLACEMENT_3D('',#194565,#98210,#98211);
#84376=AXIS2_PLACEMENT_3D('',#194571,#98215,#98216);
#84377=AXIS2_PLACEMENT_3D('',#194574,#98219,#98220);
#84378=AXIS2_PLACEMENT_3D('',#194583,#98225,#98226);
#84379=AXIS2_PLACEMENT_3D('',#194589,#98230,#98231);
#84380=AXIS2_PLACEMENT_3D('',#194595,#98235,#98236);
#84381=AXIS2_PLACEMENT_3D('',#194598,#98239,#98240);
#84382=AXIS2_PLACEMENT_3D('',#194607,#98245,#98246);
#84383=AXIS2_PLACEMENT_3D('',#194613,#98250,#98251);
#84384=AXIS2_PLACEMENT_3D('',#194619,#98255,#98256);
#84385=AXIS2_PLACEMENT_3D('',#194622,#98259,#98260);
#84386=AXIS2_PLACEMENT_3D('',#194631,#98265,#98266);
#84387=AXIS2_PLACEMENT_3D('',#194637,#98270,#98271);
#84388=AXIS2_PLACEMENT_3D('',#194643,#98275,#98276);
#84389=AXIS2_PLACEMENT_3D('',#194646,#98279,#98280);
#84390=AXIS2_PLACEMENT_3D('',#194655,#98285,#98286);
#84391=AXIS2_PLACEMENT_3D('',#194661,#98290,#98291);
#84392=AXIS2_PLACEMENT_3D('',#194667,#98295,#98296);
#84393=AXIS2_PLACEMENT_3D('',#194670,#98299,#98300);
#84394=AXIS2_PLACEMENT_3D('',#194679,#98305,#98306);
#84395=AXIS2_PLACEMENT_3D('',#194685,#98310,#98311);
#84396=AXIS2_PLACEMENT_3D('',#194691,#98315,#98316);
#84397=AXIS2_PLACEMENT_3D('',#194694,#98319,#98320);
#84398=AXIS2_PLACEMENT_3D('',#194703,#98325,#98326);
#84399=AXIS2_PLACEMENT_3D('',#194709,#98330,#98331);
#84400=AXIS2_PLACEMENT_3D('',#194715,#98335,#98336);
#84401=AXIS2_PLACEMENT_3D('',#194718,#98339,#98340);
#84402=AXIS2_PLACEMENT_3D('',#194727,#98345,#98346);
#84403=AXIS2_PLACEMENT_3D('',#194733,#98350,#98351);
#84404=AXIS2_PLACEMENT_3D('',#194739,#98355,#98356);
#84405=AXIS2_PLACEMENT_3D('',#194742,#98359,#98360);
#84406=AXIS2_PLACEMENT_3D('',#194751,#98365,#98366);
#84407=AXIS2_PLACEMENT_3D('',#194757,#98370,#98371);
#84408=AXIS2_PLACEMENT_3D('',#194763,#98375,#98376);
#84409=AXIS2_PLACEMENT_3D('',#194766,#98379,#98380);
#84410=AXIS2_PLACEMENT_3D('',#194775,#98385,#98386);
#84411=AXIS2_PLACEMENT_3D('',#194781,#98390,#98391);
#84412=AXIS2_PLACEMENT_3D('',#194787,#98395,#98396);
#84413=AXIS2_PLACEMENT_3D('',#194790,#98399,#98400);
#84414=AXIS2_PLACEMENT_3D('',#194799,#98405,#98406);
#84415=AXIS2_PLACEMENT_3D('',#194805,#98410,#98411);
#84416=AXIS2_PLACEMENT_3D('',#194811,#98415,#98416);
#84417=AXIS2_PLACEMENT_3D('',#194814,#98419,#98420);
#84418=AXIS2_PLACEMENT_3D('',#194823,#98425,#98426);
#84419=AXIS2_PLACEMENT_3D('',#194829,#98430,#98431);
#84420=AXIS2_PLACEMENT_3D('',#194835,#98435,#98436);
#84421=AXIS2_PLACEMENT_3D('',#194838,#98439,#98440);
#84422=AXIS2_PLACEMENT_3D('',#194847,#98445,#98446);
#84423=AXIS2_PLACEMENT_3D('',#194853,#98450,#98451);
#84424=AXIS2_PLACEMENT_3D('',#194859,#98455,#98456);
#84425=AXIS2_PLACEMENT_3D('',#194862,#98459,#98460);
#84426=AXIS2_PLACEMENT_3D('',#194871,#98465,#98466);
#84427=AXIS2_PLACEMENT_3D('',#194877,#98470,#98471);
#84428=AXIS2_PLACEMENT_3D('',#194883,#98475,#98476);
#84429=AXIS2_PLACEMENT_3D('',#194886,#98479,#98480);
#84430=AXIS2_PLACEMENT_3D('',#194895,#98485,#98486);
#84431=AXIS2_PLACEMENT_3D('',#194901,#98490,#98491);
#84432=AXIS2_PLACEMENT_3D('',#194907,#98495,#98496);
#84433=AXIS2_PLACEMENT_3D('',#194910,#98499,#98500);
#84434=AXIS2_PLACEMENT_3D('',#194919,#98505,#98506);
#84435=AXIS2_PLACEMENT_3D('',#194925,#98510,#98511);
#84436=AXIS2_PLACEMENT_3D('',#194931,#98515,#98516);
#84437=AXIS2_PLACEMENT_3D('',#194934,#98519,#98520);
#84438=AXIS2_PLACEMENT_3D('',#194943,#98525,#98526);
#84439=AXIS2_PLACEMENT_3D('',#194949,#98530,#98531);
#84440=AXIS2_PLACEMENT_3D('',#194955,#98535,#98536);
#84441=AXIS2_PLACEMENT_3D('',#194958,#98539,#98540);
#84442=AXIS2_PLACEMENT_3D('',#194967,#98545,#98546);
#84443=AXIS2_PLACEMENT_3D('',#194973,#98550,#98551);
#84444=AXIS2_PLACEMENT_3D('',#194979,#98555,#98556);
#84445=AXIS2_PLACEMENT_3D('',#194982,#98559,#98560);
#84446=AXIS2_PLACEMENT_3D('',#194991,#98565,#98566);
#84447=AXIS2_PLACEMENT_3D('',#194997,#98570,#98571);
#84448=AXIS2_PLACEMENT_3D('',#195003,#98575,#98576);
#84449=AXIS2_PLACEMENT_3D('',#195006,#98579,#98580);
#84450=AXIS2_PLACEMENT_3D('',#195015,#98585,#98586);
#84451=AXIS2_PLACEMENT_3D('',#195021,#98590,#98591);
#84452=AXIS2_PLACEMENT_3D('',#195027,#98595,#98596);
#84453=AXIS2_PLACEMENT_3D('',#195030,#98599,#98600);
#84454=AXIS2_PLACEMENT_3D('',#195039,#98605,#98606);
#84455=AXIS2_PLACEMENT_3D('',#195045,#98610,#98611);
#84456=AXIS2_PLACEMENT_3D('',#195051,#98615,#98616);
#84457=AXIS2_PLACEMENT_3D('',#195054,#98619,#98620);
#84458=AXIS2_PLACEMENT_3D('',#195063,#98625,#98626);
#84459=AXIS2_PLACEMENT_3D('',#195069,#98630,#98631);
#84460=AXIS2_PLACEMENT_3D('',#195075,#98635,#98636);
#84461=AXIS2_PLACEMENT_3D('',#195078,#98639,#98640);
#84462=AXIS2_PLACEMENT_3D('',#195087,#98645,#98646);
#84463=AXIS2_PLACEMENT_3D('',#195093,#98650,#98651);
#84464=AXIS2_PLACEMENT_3D('',#195099,#98655,#98656);
#84465=AXIS2_PLACEMENT_3D('',#195102,#98659,#98660);
#84466=AXIS2_PLACEMENT_3D('',#195111,#98665,#98666);
#84467=AXIS2_PLACEMENT_3D('',#195117,#98670,#98671);
#84468=AXIS2_PLACEMENT_3D('',#195123,#98675,#98676);
#84469=AXIS2_PLACEMENT_3D('',#195126,#98679,#98680);
#84470=AXIS2_PLACEMENT_3D('',#195135,#98685,#98686);
#84471=AXIS2_PLACEMENT_3D('',#195141,#98690,#98691);
#84472=AXIS2_PLACEMENT_3D('',#195147,#98695,#98696);
#84473=AXIS2_PLACEMENT_3D('',#195150,#98699,#98700);
#84474=AXIS2_PLACEMENT_3D('',#195159,#98705,#98706);
#84475=AXIS2_PLACEMENT_3D('',#195165,#98710,#98711);
#84476=AXIS2_PLACEMENT_3D('',#195171,#98715,#98716);
#84477=AXIS2_PLACEMENT_3D('',#195174,#98719,#98720);
#84478=AXIS2_PLACEMENT_3D('',#195183,#98725,#98726);
#84479=AXIS2_PLACEMENT_3D('',#195189,#98730,#98731);
#84480=AXIS2_PLACEMENT_3D('',#195195,#98735,#98736);
#84481=AXIS2_PLACEMENT_3D('',#195198,#98739,#98740);
#84482=AXIS2_PLACEMENT_3D('',#195207,#98745,#98746);
#84483=AXIS2_PLACEMENT_3D('',#195213,#98750,#98751);
#84484=AXIS2_PLACEMENT_3D('',#195219,#98755,#98756);
#84485=AXIS2_PLACEMENT_3D('',#195222,#98759,#98760);
#84486=AXIS2_PLACEMENT_3D('',#195231,#98765,#98766);
#84487=AXIS2_PLACEMENT_3D('',#195237,#98770,#98771);
#84488=AXIS2_PLACEMENT_3D('',#195243,#98775,#98776);
#84489=AXIS2_PLACEMENT_3D('',#195246,#98779,#98780);
#84490=AXIS2_PLACEMENT_3D('',#195255,#98785,#98786);
#84491=AXIS2_PLACEMENT_3D('',#195261,#98790,#98791);
#84492=AXIS2_PLACEMENT_3D('',#195267,#98795,#98796);
#84493=AXIS2_PLACEMENT_3D('',#195270,#98799,#98800);
#84494=AXIS2_PLACEMENT_3D('',#195279,#98805,#98806);
#84495=AXIS2_PLACEMENT_3D('',#195285,#98810,#98811);
#84496=AXIS2_PLACEMENT_3D('',#195291,#98815,#98816);
#84497=AXIS2_PLACEMENT_3D('',#195294,#98819,#98820);
#84498=AXIS2_PLACEMENT_3D('',#195303,#98825,#98826);
#84499=AXIS2_PLACEMENT_3D('',#195309,#98830,#98831);
#84500=AXIS2_PLACEMENT_3D('',#195315,#98835,#98836);
#84501=AXIS2_PLACEMENT_3D('',#195318,#98839,#98840);
#84502=AXIS2_PLACEMENT_3D('',#195327,#98845,#98846);
#84503=AXIS2_PLACEMENT_3D('',#195333,#98850,#98851);
#84504=AXIS2_PLACEMENT_3D('',#195339,#98855,#98856);
#84505=AXIS2_PLACEMENT_3D('',#195342,#98859,#98860);
#84506=AXIS2_PLACEMENT_3D('',#195351,#98865,#98866);
#84507=AXIS2_PLACEMENT_3D('',#195357,#98870,#98871);
#84508=AXIS2_PLACEMENT_3D('',#195363,#98875,#98876);
#84509=AXIS2_PLACEMENT_3D('',#195366,#98879,#98880);
#84510=AXIS2_PLACEMENT_3D('',#195375,#98885,#98886);
#84511=AXIS2_PLACEMENT_3D('',#195381,#98890,#98891);
#84512=AXIS2_PLACEMENT_3D('',#195387,#98895,#98896);
#84513=AXIS2_PLACEMENT_3D('',#195390,#98899,#98900);
#84514=AXIS2_PLACEMENT_3D('',#195399,#98905,#98906);
#84515=AXIS2_PLACEMENT_3D('',#195405,#98910,#98911);
#84516=AXIS2_PLACEMENT_3D('',#195411,#98915,#98916);
#84517=AXIS2_PLACEMENT_3D('',#195414,#98919,#98920);
#84518=AXIS2_PLACEMENT_3D('',#195423,#98925,#98926);
#84519=AXIS2_PLACEMENT_3D('',#195429,#98930,#98931);
#84520=AXIS2_PLACEMENT_3D('',#195435,#98935,#98936);
#84521=AXIS2_PLACEMENT_3D('',#195438,#98939,#98940);
#84522=AXIS2_PLACEMENT_3D('',#195447,#98945,#98946);
#84523=AXIS2_PLACEMENT_3D('',#195453,#98950,#98951);
#84524=AXIS2_PLACEMENT_3D('',#195459,#98955,#98956);
#84525=AXIS2_PLACEMENT_3D('',#195462,#98959,#98960);
#84526=AXIS2_PLACEMENT_3D('',#195471,#98965,#98966);
#84527=AXIS2_PLACEMENT_3D('',#195477,#98970,#98971);
#84528=AXIS2_PLACEMENT_3D('',#195483,#98975,#98976);
#84529=AXIS2_PLACEMENT_3D('',#195486,#98979,#98980);
#84530=AXIS2_PLACEMENT_3D('',#195495,#98985,#98986);
#84531=AXIS2_PLACEMENT_3D('',#195501,#98990,#98991);
#84532=AXIS2_PLACEMENT_3D('',#195507,#98995,#98996);
#84533=AXIS2_PLACEMENT_3D('',#195510,#98999,#99000);
#84534=AXIS2_PLACEMENT_3D('',#195519,#99005,#99006);
#84535=AXIS2_PLACEMENT_3D('',#195525,#99010,#99011);
#84536=AXIS2_PLACEMENT_3D('',#195531,#99015,#99016);
#84537=AXIS2_PLACEMENT_3D('',#195534,#99019,#99020);
#84538=AXIS2_PLACEMENT_3D('',#195543,#99025,#99026);
#84539=AXIS2_PLACEMENT_3D('',#195549,#99030,#99031);
#84540=AXIS2_PLACEMENT_3D('',#195555,#99035,#99036);
#84541=AXIS2_PLACEMENT_3D('',#195558,#99039,#99040);
#84542=AXIS2_PLACEMENT_3D('',#195567,#99045,#99046);
#84543=AXIS2_PLACEMENT_3D('',#195573,#99050,#99051);
#84544=AXIS2_PLACEMENT_3D('',#195579,#99055,#99056);
#84545=AXIS2_PLACEMENT_3D('',#195582,#99059,#99060);
#84546=AXIS2_PLACEMENT_3D('',#195591,#99065,#99066);
#84547=AXIS2_PLACEMENT_3D('',#195597,#99070,#99071);
#84548=AXIS2_PLACEMENT_3D('',#195603,#99075,#99076);
#84549=AXIS2_PLACEMENT_3D('',#195606,#99079,#99080);
#84550=AXIS2_PLACEMENT_3D('',#195615,#99085,#99086);
#84551=AXIS2_PLACEMENT_3D('',#195621,#99090,#99091);
#84552=AXIS2_PLACEMENT_3D('',#195627,#99095,#99096);
#84553=AXIS2_PLACEMENT_3D('',#195630,#99099,#99100);
#84554=AXIS2_PLACEMENT_3D('',#195639,#99105,#99106);
#84555=AXIS2_PLACEMENT_3D('',#195645,#99110,#99111);
#84556=AXIS2_PLACEMENT_3D('',#195651,#99115,#99116);
#84557=AXIS2_PLACEMENT_3D('',#195654,#99119,#99120);
#84558=AXIS2_PLACEMENT_3D('',#195663,#99125,#99126);
#84559=AXIS2_PLACEMENT_3D('',#195669,#99130,#99131);
#84560=AXIS2_PLACEMENT_3D('',#195675,#99135,#99136);
#84561=AXIS2_PLACEMENT_3D('',#195678,#99139,#99140);
#84562=AXIS2_PLACEMENT_3D('',#195687,#99145,#99146);
#84563=AXIS2_PLACEMENT_3D('',#195693,#99150,#99151);
#84564=AXIS2_PLACEMENT_3D('',#195699,#99155,#99156);
#84565=AXIS2_PLACEMENT_3D('',#195702,#99159,#99160);
#84566=AXIS2_PLACEMENT_3D('',#195711,#99165,#99166);
#84567=AXIS2_PLACEMENT_3D('',#195717,#99170,#99171);
#84568=AXIS2_PLACEMENT_3D('',#195723,#99175,#99176);
#84569=AXIS2_PLACEMENT_3D('',#195726,#99179,#99180);
#84570=AXIS2_PLACEMENT_3D('',#195735,#99185,#99186);
#84571=AXIS2_PLACEMENT_3D('',#195741,#99190,#99191);
#84572=AXIS2_PLACEMENT_3D('',#195747,#99195,#99196);
#84573=AXIS2_PLACEMENT_3D('',#195750,#99199,#99200);
#84574=AXIS2_PLACEMENT_3D('',#195759,#99205,#99206);
#84575=AXIS2_PLACEMENT_3D('',#195765,#99210,#99211);
#84576=AXIS2_PLACEMENT_3D('',#195771,#99215,#99216);
#84577=AXIS2_PLACEMENT_3D('',#195774,#99219,#99220);
#84578=AXIS2_PLACEMENT_3D('',#195783,#99225,#99226);
#84579=AXIS2_PLACEMENT_3D('',#195789,#99230,#99231);
#84580=AXIS2_PLACEMENT_3D('',#195795,#99235,#99236);
#84581=AXIS2_PLACEMENT_3D('',#195798,#99239,#99240);
#84582=AXIS2_PLACEMENT_3D('',#195807,#99245,#99246);
#84583=AXIS2_PLACEMENT_3D('',#195813,#99250,#99251);
#84584=AXIS2_PLACEMENT_3D('',#195819,#99255,#99256);
#84585=AXIS2_PLACEMENT_3D('',#195822,#99259,#99260);
#84586=AXIS2_PLACEMENT_3D('',#195831,#99265,#99266);
#84587=AXIS2_PLACEMENT_3D('',#195837,#99270,#99271);
#84588=AXIS2_PLACEMENT_3D('',#195843,#99275,#99276);
#84589=AXIS2_PLACEMENT_3D('',#195846,#99279,#99280);
#84590=AXIS2_PLACEMENT_3D('',#195855,#99285,#99286);
#84591=AXIS2_PLACEMENT_3D('',#195861,#99290,#99291);
#84592=AXIS2_PLACEMENT_3D('',#195867,#99295,#99296);
#84593=AXIS2_PLACEMENT_3D('',#195870,#99299,#99300);
#84594=AXIS2_PLACEMENT_3D('',#195879,#99305,#99306);
#84595=AXIS2_PLACEMENT_3D('',#195885,#99310,#99311);
#84596=AXIS2_PLACEMENT_3D('',#195891,#99315,#99316);
#84597=AXIS2_PLACEMENT_3D('',#195894,#99319,#99320);
#84598=AXIS2_PLACEMENT_3D('',#195903,#99325,#99326);
#84599=AXIS2_PLACEMENT_3D('',#195909,#99330,#99331);
#84600=AXIS2_PLACEMENT_3D('',#195915,#99335,#99336);
#84601=AXIS2_PLACEMENT_3D('',#195918,#99339,#99340);
#84602=AXIS2_PLACEMENT_3D('',#195927,#99345,#99346);
#84603=AXIS2_PLACEMENT_3D('',#195933,#99350,#99351);
#84604=AXIS2_PLACEMENT_3D('',#195939,#99355,#99356);
#84605=AXIS2_PLACEMENT_3D('',#195942,#99359,#99360);
#84606=AXIS2_PLACEMENT_3D('',#195951,#99365,#99366);
#84607=AXIS2_PLACEMENT_3D('',#195957,#99370,#99371);
#84608=AXIS2_PLACEMENT_3D('',#195963,#99375,#99376);
#84609=AXIS2_PLACEMENT_3D('',#195966,#99379,#99380);
#84610=AXIS2_PLACEMENT_3D('',#195975,#99385,#99386);
#84611=AXIS2_PLACEMENT_3D('',#195981,#99390,#99391);
#84612=AXIS2_PLACEMENT_3D('',#195987,#99395,#99396);
#84613=AXIS2_PLACEMENT_3D('',#195990,#99399,#99400);
#84614=AXIS2_PLACEMENT_3D('',#195999,#99405,#99406);
#84615=AXIS2_PLACEMENT_3D('',#196005,#99410,#99411);
#84616=AXIS2_PLACEMENT_3D('',#196011,#99415,#99416);
#84617=AXIS2_PLACEMENT_3D('',#196014,#99419,#99420);
#84618=AXIS2_PLACEMENT_3D('',#196023,#99425,#99426);
#84619=AXIS2_PLACEMENT_3D('',#196029,#99430,#99431);
#84620=AXIS2_PLACEMENT_3D('',#196035,#99435,#99436);
#84621=AXIS2_PLACEMENT_3D('',#196038,#99439,#99440);
#84622=AXIS2_PLACEMENT_3D('',#196047,#99445,#99446);
#84623=AXIS2_PLACEMENT_3D('',#196053,#99450,#99451);
#84624=AXIS2_PLACEMENT_3D('',#196059,#99455,#99456);
#84625=AXIS2_PLACEMENT_3D('',#196062,#99459,#99460);
#84626=AXIS2_PLACEMENT_3D('',#196071,#99465,#99466);
#84627=AXIS2_PLACEMENT_3D('',#196077,#99470,#99471);
#84628=AXIS2_PLACEMENT_3D('',#196083,#99475,#99476);
#84629=AXIS2_PLACEMENT_3D('',#196086,#99479,#99480);
#84630=AXIS2_PLACEMENT_3D('',#196095,#99485,#99486);
#84631=AXIS2_PLACEMENT_3D('',#196101,#99490,#99491);
#84632=AXIS2_PLACEMENT_3D('',#196107,#99495,#99496);
#84633=AXIS2_PLACEMENT_3D('',#196110,#99499,#99500);
#84634=AXIS2_PLACEMENT_3D('',#196119,#99505,#99506);
#84635=AXIS2_PLACEMENT_3D('',#196125,#99510,#99511);
#84636=AXIS2_PLACEMENT_3D('',#196131,#99515,#99516);
#84637=AXIS2_PLACEMENT_3D('',#196134,#99519,#99520);
#84638=AXIS2_PLACEMENT_3D('',#196143,#99525,#99526);
#84639=AXIS2_PLACEMENT_3D('',#196149,#99530,#99531);
#84640=AXIS2_PLACEMENT_3D('',#196155,#99535,#99536);
#84641=AXIS2_PLACEMENT_3D('',#196158,#99539,#99540);
#84642=AXIS2_PLACEMENT_3D('',#196167,#99545,#99546);
#84643=AXIS2_PLACEMENT_3D('',#196173,#99550,#99551);
#84644=AXIS2_PLACEMENT_3D('',#196179,#99555,#99556);
#84645=AXIS2_PLACEMENT_3D('',#196182,#99559,#99560);
#84646=AXIS2_PLACEMENT_3D('',#196191,#99565,#99566);
#84647=AXIS2_PLACEMENT_3D('',#196197,#99570,#99571);
#84648=AXIS2_PLACEMENT_3D('',#196203,#99575,#99576);
#84649=AXIS2_PLACEMENT_3D('',#196206,#99579,#99580);
#84650=AXIS2_PLACEMENT_3D('',#196215,#99585,#99586);
#84651=AXIS2_PLACEMENT_3D('',#196221,#99590,#99591);
#84652=AXIS2_PLACEMENT_3D('',#196227,#99595,#99596);
#84653=AXIS2_PLACEMENT_3D('',#196230,#99599,#99600);
#84654=AXIS2_PLACEMENT_3D('',#196239,#99605,#99606);
#84655=AXIS2_PLACEMENT_3D('',#196245,#99610,#99611);
#84656=AXIS2_PLACEMENT_3D('',#196251,#99615,#99616);
#84657=AXIS2_PLACEMENT_3D('',#196254,#99619,#99620);
#84658=AXIS2_PLACEMENT_3D('',#196263,#99625,#99626);
#84659=AXIS2_PLACEMENT_3D('',#196269,#99630,#99631);
#84660=AXIS2_PLACEMENT_3D('',#196275,#99635,#99636);
#84661=AXIS2_PLACEMENT_3D('',#196278,#99639,#99640);
#84662=AXIS2_PLACEMENT_3D('',#196287,#99645,#99646);
#84663=AXIS2_PLACEMENT_3D('',#196293,#99650,#99651);
#84664=AXIS2_PLACEMENT_3D('',#196299,#99655,#99656);
#84665=AXIS2_PLACEMENT_3D('',#196302,#99659,#99660);
#84666=AXIS2_PLACEMENT_3D('',#196311,#99665,#99666);
#84667=AXIS2_PLACEMENT_3D('',#196317,#99670,#99671);
#84668=AXIS2_PLACEMENT_3D('',#196323,#99675,#99676);
#84669=AXIS2_PLACEMENT_3D('',#196326,#99679,#99680);
#84670=AXIS2_PLACEMENT_3D('',#196335,#99685,#99686);
#84671=AXIS2_PLACEMENT_3D('',#196341,#99690,#99691);
#84672=AXIS2_PLACEMENT_3D('',#196347,#99695,#99696);
#84673=AXIS2_PLACEMENT_3D('',#196350,#99699,#99700);
#84674=AXIS2_PLACEMENT_3D('',#196359,#99705,#99706);
#84675=AXIS2_PLACEMENT_3D('',#196365,#99710,#99711);
#84676=AXIS2_PLACEMENT_3D('',#196371,#99715,#99716);
#84677=AXIS2_PLACEMENT_3D('',#196374,#99719,#99720);
#84678=AXIS2_PLACEMENT_3D('',#196383,#99725,#99726);
#84679=AXIS2_PLACEMENT_3D('',#196389,#99730,#99731);
#84680=AXIS2_PLACEMENT_3D('',#196395,#99735,#99736);
#84681=AXIS2_PLACEMENT_3D('',#196398,#99739,#99740);
#84682=AXIS2_PLACEMENT_3D('',#196407,#99745,#99746);
#84683=AXIS2_PLACEMENT_3D('',#196413,#99750,#99751);
#84684=AXIS2_PLACEMENT_3D('',#196419,#99755,#99756);
#84685=AXIS2_PLACEMENT_3D('',#196422,#99759,#99760);
#84686=AXIS2_PLACEMENT_3D('',#196431,#99765,#99766);
#84687=AXIS2_PLACEMENT_3D('',#196437,#99770,#99771);
#84688=AXIS2_PLACEMENT_3D('',#196443,#99775,#99776);
#84689=AXIS2_PLACEMENT_3D('',#196446,#99779,#99780);
#84690=AXIS2_PLACEMENT_3D('',#196455,#99785,#99786);
#84691=AXIS2_PLACEMENT_3D('',#196461,#99790,#99791);
#84692=AXIS2_PLACEMENT_3D('',#196467,#99795,#99796);
#84693=AXIS2_PLACEMENT_3D('',#196470,#99799,#99800);
#84694=AXIS2_PLACEMENT_3D('',#196479,#99805,#99806);
#84695=AXIS2_PLACEMENT_3D('',#196485,#99810,#99811);
#84696=AXIS2_PLACEMENT_3D('',#196491,#99815,#99816);
#84697=AXIS2_PLACEMENT_3D('',#196494,#99819,#99820);
#84698=AXIS2_PLACEMENT_3D('',#196503,#99825,#99826);
#84699=AXIS2_PLACEMENT_3D('',#196509,#99830,#99831);
#84700=AXIS2_PLACEMENT_3D('',#196515,#99835,#99836);
#84701=AXIS2_PLACEMENT_3D('',#196518,#99839,#99840);
#84702=AXIS2_PLACEMENT_3D('',#196527,#99845,#99846);
#84703=AXIS2_PLACEMENT_3D('',#196533,#99850,#99851);
#84704=AXIS2_PLACEMENT_3D('',#196539,#99855,#99856);
#84705=AXIS2_PLACEMENT_3D('',#196542,#99859,#99860);
#84706=AXIS2_PLACEMENT_3D('',#196551,#99865,#99866);
#84707=AXIS2_PLACEMENT_3D('',#196557,#99870,#99871);
#84708=AXIS2_PLACEMENT_3D('',#196563,#99875,#99876);
#84709=AXIS2_PLACEMENT_3D('',#196566,#99879,#99880);
#84710=AXIS2_PLACEMENT_3D('',#196575,#99885,#99886);
#84711=AXIS2_PLACEMENT_3D('',#196581,#99890,#99891);
#84712=AXIS2_PLACEMENT_3D('',#196587,#99895,#99896);
#84713=AXIS2_PLACEMENT_3D('',#196590,#99899,#99900);
#84714=AXIS2_PLACEMENT_3D('',#196599,#99905,#99906);
#84715=AXIS2_PLACEMENT_3D('',#196605,#99910,#99911);
#84716=AXIS2_PLACEMENT_3D('',#196611,#99915,#99916);
#84717=AXIS2_PLACEMENT_3D('',#196614,#99919,#99920);
#84718=AXIS2_PLACEMENT_3D('',#196623,#99925,#99926);
#84719=AXIS2_PLACEMENT_3D('',#196629,#99930,#99931);
#84720=AXIS2_PLACEMENT_3D('',#196635,#99935,#99936);
#84721=AXIS2_PLACEMENT_3D('',#196638,#99939,#99940);
#84722=AXIS2_PLACEMENT_3D('',#196647,#99945,#99946);
#84723=AXIS2_PLACEMENT_3D('',#196653,#99950,#99951);
#84724=AXIS2_PLACEMENT_3D('',#196659,#99955,#99956);
#84725=AXIS2_PLACEMENT_3D('',#196662,#99959,#99960);
#84726=AXIS2_PLACEMENT_3D('',#196671,#99965,#99966);
#84727=AXIS2_PLACEMENT_3D('',#196677,#99970,#99971);
#84728=AXIS2_PLACEMENT_3D('',#196683,#99975,#99976);
#84729=AXIS2_PLACEMENT_3D('',#196686,#99979,#99980);
#84730=AXIS2_PLACEMENT_3D('',#196695,#99985,#99986);
#84731=AXIS2_PLACEMENT_3D('',#196701,#99990,#99991);
#84732=AXIS2_PLACEMENT_3D('',#196707,#99995,#99996);
#84733=AXIS2_PLACEMENT_3D('',#196710,#99999,#100000);
#84734=AXIS2_PLACEMENT_3D('',#196719,#100005,#100006);
#84735=AXIS2_PLACEMENT_3D('',#196725,#100010,#100011);
#84736=AXIS2_PLACEMENT_3D('',#196731,#100015,#100016);
#84737=AXIS2_PLACEMENT_3D('',#196734,#100019,#100020);
#84738=AXIS2_PLACEMENT_3D('',#196743,#100025,#100026);
#84739=AXIS2_PLACEMENT_3D('',#196749,#100030,#100031);
#84740=AXIS2_PLACEMENT_3D('',#196755,#100035,#100036);
#84741=AXIS2_PLACEMENT_3D('',#196758,#100039,#100040);
#84742=AXIS2_PLACEMENT_3D('',#196767,#100045,#100046);
#84743=AXIS2_PLACEMENT_3D('',#196773,#100050,#100051);
#84744=AXIS2_PLACEMENT_3D('',#196779,#100055,#100056);
#84745=AXIS2_PLACEMENT_3D('',#196782,#100059,#100060);
#84746=AXIS2_PLACEMENT_3D('',#196791,#100065,#100066);
#84747=AXIS2_PLACEMENT_3D('',#196797,#100070,#100071);
#84748=AXIS2_PLACEMENT_3D('',#196803,#100075,#100076);
#84749=AXIS2_PLACEMENT_3D('',#196806,#100079,#100080);
#84750=AXIS2_PLACEMENT_3D('',#196815,#100085,#100086);
#84751=AXIS2_PLACEMENT_3D('',#196821,#100090,#100091);
#84752=AXIS2_PLACEMENT_3D('',#196827,#100095,#100096);
#84753=AXIS2_PLACEMENT_3D('',#196830,#100099,#100100);
#84754=AXIS2_PLACEMENT_3D('',#196839,#100105,#100106);
#84755=AXIS2_PLACEMENT_3D('',#196845,#100110,#100111);
#84756=AXIS2_PLACEMENT_3D('',#196851,#100115,#100116);
#84757=AXIS2_PLACEMENT_3D('',#196854,#100119,#100120);
#84758=AXIS2_PLACEMENT_3D('',#196863,#100125,#100126);
#84759=AXIS2_PLACEMENT_3D('',#196869,#100130,#100131);
#84760=AXIS2_PLACEMENT_3D('',#196875,#100135,#100136);
#84761=AXIS2_PLACEMENT_3D('',#196878,#100139,#100140);
#84762=AXIS2_PLACEMENT_3D('',#196887,#100145,#100146);
#84763=AXIS2_PLACEMENT_3D('',#196893,#100150,#100151);
#84764=AXIS2_PLACEMENT_3D('',#196899,#100155,#100156);
#84765=AXIS2_PLACEMENT_3D('',#196902,#100159,#100160);
#84766=AXIS2_PLACEMENT_3D('',#196911,#100165,#100166);
#84767=AXIS2_PLACEMENT_3D('',#196917,#100170,#100171);
#84768=AXIS2_PLACEMENT_3D('',#196923,#100175,#100176);
#84769=AXIS2_PLACEMENT_3D('',#196926,#100179,#100180);
#84770=AXIS2_PLACEMENT_3D('',#196935,#100185,#100186);
#84771=AXIS2_PLACEMENT_3D('',#196941,#100190,#100191);
#84772=AXIS2_PLACEMENT_3D('',#196947,#100195,#100196);
#84773=AXIS2_PLACEMENT_3D('',#196950,#100199,#100200);
#84774=AXIS2_PLACEMENT_3D('',#196959,#100205,#100206);
#84775=AXIS2_PLACEMENT_3D('',#196965,#100210,#100211);
#84776=AXIS2_PLACEMENT_3D('',#196971,#100215,#100216);
#84777=AXIS2_PLACEMENT_3D('',#196974,#100219,#100220);
#84778=AXIS2_PLACEMENT_3D('',#196983,#100225,#100226);
#84779=AXIS2_PLACEMENT_3D('',#196989,#100230,#100231);
#84780=AXIS2_PLACEMENT_3D('',#196995,#100235,#100236);
#84781=AXIS2_PLACEMENT_3D('',#196998,#100239,#100240);
#84782=AXIS2_PLACEMENT_3D('',#197007,#100245,#100246);
#84783=AXIS2_PLACEMENT_3D('',#197013,#100250,#100251);
#84784=AXIS2_PLACEMENT_3D('',#197019,#100255,#100256);
#84785=AXIS2_PLACEMENT_3D('',#197022,#100259,#100260);
#84786=AXIS2_PLACEMENT_3D('',#197031,#100265,#100266);
#84787=AXIS2_PLACEMENT_3D('',#197037,#100270,#100271);
#84788=AXIS2_PLACEMENT_3D('',#197043,#100275,#100276);
#84789=AXIS2_PLACEMENT_3D('',#197046,#100279,#100280);
#84790=AXIS2_PLACEMENT_3D('',#197055,#100285,#100286);
#84791=AXIS2_PLACEMENT_3D('',#197061,#100290,#100291);
#84792=AXIS2_PLACEMENT_3D('',#197067,#100295,#100296);
#84793=AXIS2_PLACEMENT_3D('',#197070,#100299,#100300);
#84794=AXIS2_PLACEMENT_3D('',#197079,#100305,#100306);
#84795=AXIS2_PLACEMENT_3D('',#197085,#100310,#100311);
#84796=AXIS2_PLACEMENT_3D('',#197091,#100315,#100316);
#84797=AXIS2_PLACEMENT_3D('',#197094,#100319,#100320);
#84798=AXIS2_PLACEMENT_3D('',#197103,#100325,#100326);
#84799=AXIS2_PLACEMENT_3D('',#197109,#100330,#100331);
#84800=AXIS2_PLACEMENT_3D('',#197115,#100335,#100336);
#84801=AXIS2_PLACEMENT_3D('',#197118,#100339,#100340);
#84802=AXIS2_PLACEMENT_3D('',#197127,#100345,#100346);
#84803=AXIS2_PLACEMENT_3D('',#197133,#100350,#100351);
#84804=AXIS2_PLACEMENT_3D('',#197139,#100355,#100356);
#84805=AXIS2_PLACEMENT_3D('',#197142,#100359,#100360);
#84806=AXIS2_PLACEMENT_3D('',#197151,#100365,#100366);
#84807=AXIS2_PLACEMENT_3D('',#197157,#100370,#100371);
#84808=AXIS2_PLACEMENT_3D('',#197163,#100375,#100376);
#84809=AXIS2_PLACEMENT_3D('',#197166,#100379,#100380);
#84810=AXIS2_PLACEMENT_3D('',#197175,#100385,#100386);
#84811=AXIS2_PLACEMENT_3D('',#197181,#100390,#100391);
#84812=AXIS2_PLACEMENT_3D('',#197187,#100395,#100396);
#84813=AXIS2_PLACEMENT_3D('',#197190,#100399,#100400);
#84814=AXIS2_PLACEMENT_3D('',#197199,#100405,#100406);
#84815=AXIS2_PLACEMENT_3D('',#197205,#100410,#100411);
#84816=AXIS2_PLACEMENT_3D('',#197211,#100415,#100416);
#84817=AXIS2_PLACEMENT_3D('',#197214,#100419,#100420);
#84818=AXIS2_PLACEMENT_3D('',#197223,#100425,#100426);
#84819=AXIS2_PLACEMENT_3D('',#197229,#100430,#100431);
#84820=AXIS2_PLACEMENT_3D('',#197235,#100435,#100436);
#84821=AXIS2_PLACEMENT_3D('',#197238,#100439,#100440);
#84822=AXIS2_PLACEMENT_3D('',#197247,#100445,#100446);
#84823=AXIS2_PLACEMENT_3D('',#197253,#100450,#100451);
#84824=AXIS2_PLACEMENT_3D('',#197259,#100455,#100456);
#84825=AXIS2_PLACEMENT_3D('',#197262,#100459,#100460);
#84826=AXIS2_PLACEMENT_3D('',#197271,#100465,#100466);
#84827=AXIS2_PLACEMENT_3D('',#197277,#100470,#100471);
#84828=AXIS2_PLACEMENT_3D('',#197283,#100475,#100476);
#84829=AXIS2_PLACEMENT_3D('',#197286,#100479,#100480);
#84830=AXIS2_PLACEMENT_3D('',#197295,#100485,#100486);
#84831=AXIS2_PLACEMENT_3D('',#197301,#100490,#100491);
#84832=AXIS2_PLACEMENT_3D('',#197307,#100495,#100496);
#84833=AXIS2_PLACEMENT_3D('',#197310,#100499,#100500);
#84834=AXIS2_PLACEMENT_3D('',#197319,#100505,#100506);
#84835=AXIS2_PLACEMENT_3D('',#197325,#100510,#100511);
#84836=AXIS2_PLACEMENT_3D('',#197331,#100515,#100516);
#84837=AXIS2_PLACEMENT_3D('',#197334,#100519,#100520);
#84838=AXIS2_PLACEMENT_3D('',#197343,#100525,#100526);
#84839=AXIS2_PLACEMENT_3D('',#197349,#100530,#100531);
#84840=AXIS2_PLACEMENT_3D('',#197355,#100535,#100536);
#84841=AXIS2_PLACEMENT_3D('',#197358,#100539,#100540);
#84842=AXIS2_PLACEMENT_3D('',#197367,#100545,#100546);
#84843=AXIS2_PLACEMENT_3D('',#197373,#100550,#100551);
#84844=AXIS2_PLACEMENT_3D('',#197379,#100555,#100556);
#84845=AXIS2_PLACEMENT_3D('',#197382,#100559,#100560);
#84846=AXIS2_PLACEMENT_3D('',#197391,#100565,#100566);
#84847=AXIS2_PLACEMENT_3D('',#197397,#100570,#100571);
#84848=AXIS2_PLACEMENT_3D('',#197403,#100575,#100576);
#84849=AXIS2_PLACEMENT_3D('',#197406,#100579,#100580);
#84850=AXIS2_PLACEMENT_3D('',#197415,#100585,#100586);
#84851=AXIS2_PLACEMENT_3D('',#197421,#100590,#100591);
#84852=AXIS2_PLACEMENT_3D('',#197427,#100595,#100596);
#84853=AXIS2_PLACEMENT_3D('',#197430,#100599,#100600);
#84854=AXIS2_PLACEMENT_3D('',#197439,#100605,#100606);
#84855=AXIS2_PLACEMENT_3D('',#197445,#100610,#100611);
#84856=AXIS2_PLACEMENT_3D('',#197451,#100615,#100616);
#84857=AXIS2_PLACEMENT_3D('',#197454,#100619,#100620);
#84858=AXIS2_PLACEMENT_3D('',#197463,#100625,#100626);
#84859=AXIS2_PLACEMENT_3D('',#197469,#100630,#100631);
#84860=AXIS2_PLACEMENT_3D('',#197475,#100635,#100636);
#84861=AXIS2_PLACEMENT_3D('',#197478,#100639,#100640);
#84862=AXIS2_PLACEMENT_3D('',#197487,#100645,#100646);
#84863=AXIS2_PLACEMENT_3D('',#197493,#100650,#100651);
#84864=AXIS2_PLACEMENT_3D('',#197499,#100655,#100656);
#84865=AXIS2_PLACEMENT_3D('',#197502,#100659,#100660);
#84866=AXIS2_PLACEMENT_3D('',#197511,#100665,#100666);
#84867=AXIS2_PLACEMENT_3D('',#197517,#100670,#100671);
#84868=AXIS2_PLACEMENT_3D('',#197523,#100675,#100676);
#84869=AXIS2_PLACEMENT_3D('',#197526,#100679,#100680);
#84870=AXIS2_PLACEMENT_3D('',#197535,#100685,#100686);
#84871=AXIS2_PLACEMENT_3D('',#197541,#100690,#100691);
#84872=AXIS2_PLACEMENT_3D('',#197547,#100695,#100696);
#84873=AXIS2_PLACEMENT_3D('',#197550,#100699,#100700);
#84874=AXIS2_PLACEMENT_3D('',#197559,#100705,#100706);
#84875=AXIS2_PLACEMENT_3D('',#197565,#100710,#100711);
#84876=AXIS2_PLACEMENT_3D('',#197571,#100715,#100716);
#84877=AXIS2_PLACEMENT_3D('',#197574,#100719,#100720);
#84878=AXIS2_PLACEMENT_3D('',#197583,#100725,#100726);
#84879=AXIS2_PLACEMENT_3D('',#197589,#100730,#100731);
#84880=AXIS2_PLACEMENT_3D('',#197595,#100735,#100736);
#84881=AXIS2_PLACEMENT_3D('',#197598,#100739,#100740);
#84882=AXIS2_PLACEMENT_3D('',#197607,#100745,#100746);
#84883=AXIS2_PLACEMENT_3D('',#197613,#100750,#100751);
#84884=AXIS2_PLACEMENT_3D('',#197619,#100755,#100756);
#84885=AXIS2_PLACEMENT_3D('',#197622,#100759,#100760);
#84886=AXIS2_PLACEMENT_3D('',#197631,#100765,#100766);
#84887=AXIS2_PLACEMENT_3D('',#197637,#100770,#100771);
#84888=AXIS2_PLACEMENT_3D('',#197643,#100775,#100776);
#84889=AXIS2_PLACEMENT_3D('',#197646,#100779,#100780);
#84890=AXIS2_PLACEMENT_3D('',#197655,#100785,#100786);
#84891=AXIS2_PLACEMENT_3D('',#197661,#100790,#100791);
#84892=AXIS2_PLACEMENT_3D('',#197667,#100795,#100796);
#84893=AXIS2_PLACEMENT_3D('',#197670,#100799,#100800);
#84894=AXIS2_PLACEMENT_3D('',#197679,#100805,#100806);
#84895=AXIS2_PLACEMENT_3D('',#197685,#100810,#100811);
#84896=AXIS2_PLACEMENT_3D('',#197691,#100815,#100816);
#84897=AXIS2_PLACEMENT_3D('',#197694,#100819,#100820);
#84898=AXIS2_PLACEMENT_3D('',#197703,#100825,#100826);
#84899=AXIS2_PLACEMENT_3D('',#197709,#100830,#100831);
#84900=AXIS2_PLACEMENT_3D('',#197715,#100835,#100836);
#84901=AXIS2_PLACEMENT_3D('',#197718,#100839,#100840);
#84902=AXIS2_PLACEMENT_3D('',#197727,#100845,#100846);
#84903=AXIS2_PLACEMENT_3D('',#197733,#100850,#100851);
#84904=AXIS2_PLACEMENT_3D('',#197739,#100855,#100856);
#84905=AXIS2_PLACEMENT_3D('',#197742,#100859,#100860);
#84906=AXIS2_PLACEMENT_3D('',#197751,#100865,#100866);
#84907=AXIS2_PLACEMENT_3D('',#197757,#100870,#100871);
#84908=AXIS2_PLACEMENT_3D('',#197763,#100875,#100876);
#84909=AXIS2_PLACEMENT_3D('',#197766,#100879,#100880);
#84910=AXIS2_PLACEMENT_3D('',#197775,#100885,#100886);
#84911=AXIS2_PLACEMENT_3D('',#197781,#100890,#100891);
#84912=AXIS2_PLACEMENT_3D('',#197787,#100895,#100896);
#84913=AXIS2_PLACEMENT_3D('',#197790,#100899,#100900);
#84914=AXIS2_PLACEMENT_3D('',#197799,#100905,#100906);
#84915=AXIS2_PLACEMENT_3D('',#197805,#100910,#100911);
#84916=AXIS2_PLACEMENT_3D('',#197811,#100915,#100916);
#84917=AXIS2_PLACEMENT_3D('',#197814,#100919,#100920);
#84918=AXIS2_PLACEMENT_3D('',#197823,#100925,#100926);
#84919=AXIS2_PLACEMENT_3D('',#197829,#100930,#100931);
#84920=AXIS2_PLACEMENT_3D('',#197835,#100935,#100936);
#84921=AXIS2_PLACEMENT_3D('',#197838,#100939,#100940);
#84922=AXIS2_PLACEMENT_3D('',#197847,#100945,#100946);
#84923=AXIS2_PLACEMENT_3D('',#197853,#100950,#100951);
#84924=AXIS2_PLACEMENT_3D('',#197859,#100955,#100956);
#84925=AXIS2_PLACEMENT_3D('',#197862,#100959,#100960);
#84926=AXIS2_PLACEMENT_3D('',#197871,#100965,#100966);
#84927=AXIS2_PLACEMENT_3D('',#197877,#100970,#100971);
#84928=AXIS2_PLACEMENT_3D('',#197883,#100975,#100976);
#84929=AXIS2_PLACEMENT_3D('',#197886,#100979,#100980);
#84930=AXIS2_PLACEMENT_3D('',#197895,#100985,#100986);
#84931=AXIS2_PLACEMENT_3D('',#197901,#100990,#100991);
#84932=AXIS2_PLACEMENT_3D('',#197907,#100995,#100996);
#84933=AXIS2_PLACEMENT_3D('',#197910,#100999,#101000);
#84934=AXIS2_PLACEMENT_3D('',#197919,#101005,#101006);
#84935=AXIS2_PLACEMENT_3D('',#197925,#101010,#101011);
#84936=AXIS2_PLACEMENT_3D('',#197931,#101015,#101016);
#84937=AXIS2_PLACEMENT_3D('',#197934,#101019,#101020);
#84938=AXIS2_PLACEMENT_3D('',#197943,#101025,#101026);
#84939=AXIS2_PLACEMENT_3D('',#197949,#101030,#101031);
#84940=AXIS2_PLACEMENT_3D('',#197955,#101035,#101036);
#84941=AXIS2_PLACEMENT_3D('',#197958,#101039,#101040);
#84942=AXIS2_PLACEMENT_3D('',#197967,#101045,#101046);
#84943=AXIS2_PLACEMENT_3D('',#197973,#101050,#101051);
#84944=AXIS2_PLACEMENT_3D('',#197979,#101055,#101056);
#84945=AXIS2_PLACEMENT_3D('',#197982,#101059,#101060);
#84946=AXIS2_PLACEMENT_3D('',#197991,#101065,#101066);
#84947=AXIS2_PLACEMENT_3D('',#197997,#101070,#101071);
#84948=AXIS2_PLACEMENT_3D('',#198003,#101075,#101076);
#84949=AXIS2_PLACEMENT_3D('',#198006,#101079,#101080);
#84950=AXIS2_PLACEMENT_3D('',#198015,#101085,#101086);
#84951=AXIS2_PLACEMENT_3D('',#198021,#101090,#101091);
#84952=AXIS2_PLACEMENT_3D('',#198027,#101095,#101096);
#84953=AXIS2_PLACEMENT_3D('',#198030,#101099,#101100);
#84954=AXIS2_PLACEMENT_3D('',#198039,#101105,#101106);
#84955=AXIS2_PLACEMENT_3D('',#198045,#101110,#101111);
#84956=AXIS2_PLACEMENT_3D('',#198051,#101115,#101116);
#84957=AXIS2_PLACEMENT_3D('',#198054,#101119,#101120);
#84958=AXIS2_PLACEMENT_3D('',#198063,#101125,#101126);
#84959=AXIS2_PLACEMENT_3D('',#198069,#101130,#101131);
#84960=AXIS2_PLACEMENT_3D('',#198075,#101135,#101136);
#84961=AXIS2_PLACEMENT_3D('',#198078,#101139,#101140);
#84962=AXIS2_PLACEMENT_3D('',#198087,#101145,#101146);
#84963=AXIS2_PLACEMENT_3D('',#198093,#101150,#101151);
#84964=AXIS2_PLACEMENT_3D('',#198099,#101155,#101156);
#84965=AXIS2_PLACEMENT_3D('',#198102,#101159,#101160);
#84966=AXIS2_PLACEMENT_3D('',#198111,#101165,#101166);
#84967=AXIS2_PLACEMENT_3D('',#198117,#101170,#101171);
#84968=AXIS2_PLACEMENT_3D('',#198123,#101175,#101176);
#84969=AXIS2_PLACEMENT_3D('',#198126,#101179,#101180);
#84970=AXIS2_PLACEMENT_3D('',#198135,#101185,#101186);
#84971=AXIS2_PLACEMENT_3D('',#198141,#101190,#101191);
#84972=AXIS2_PLACEMENT_3D('',#198147,#101195,#101196);
#84973=AXIS2_PLACEMENT_3D('',#198150,#101199,#101200);
#84974=AXIS2_PLACEMENT_3D('',#198159,#101205,#101206);
#84975=AXIS2_PLACEMENT_3D('',#198165,#101210,#101211);
#84976=AXIS2_PLACEMENT_3D('',#198171,#101215,#101216);
#84977=AXIS2_PLACEMENT_3D('',#198174,#101219,#101220);
#84978=AXIS2_PLACEMENT_3D('',#198183,#101225,#101226);
#84979=AXIS2_PLACEMENT_3D('',#198189,#101230,#101231);
#84980=AXIS2_PLACEMENT_3D('',#198195,#101235,#101236);
#84981=AXIS2_PLACEMENT_3D('',#198198,#101239,#101240);
#84982=AXIS2_PLACEMENT_3D('',#198207,#101245,#101246);
#84983=AXIS2_PLACEMENT_3D('',#198213,#101250,#101251);
#84984=AXIS2_PLACEMENT_3D('',#198219,#101255,#101256);
#84985=AXIS2_PLACEMENT_3D('',#198222,#101259,#101260);
#84986=AXIS2_PLACEMENT_3D('',#198231,#101265,#101266);
#84987=AXIS2_PLACEMENT_3D('',#198237,#101270,#101271);
#84988=AXIS2_PLACEMENT_3D('',#198243,#101275,#101276);
#84989=AXIS2_PLACEMENT_3D('',#198246,#101279,#101280);
#84990=AXIS2_PLACEMENT_3D('',#198255,#101285,#101286);
#84991=AXIS2_PLACEMENT_3D('',#198261,#101290,#101291);
#84992=AXIS2_PLACEMENT_3D('',#198267,#101295,#101296);
#84993=AXIS2_PLACEMENT_3D('',#198270,#101299,#101300);
#84994=AXIS2_PLACEMENT_3D('',#198279,#101305,#101306);
#84995=AXIS2_PLACEMENT_3D('',#198285,#101310,#101311);
#84996=AXIS2_PLACEMENT_3D('',#198291,#101315,#101316);
#84997=AXIS2_PLACEMENT_3D('',#198294,#101319,#101320);
#84998=AXIS2_PLACEMENT_3D('',#198303,#101325,#101326);
#84999=AXIS2_PLACEMENT_3D('',#198309,#101330,#101331);
#85000=AXIS2_PLACEMENT_3D('',#198315,#101335,#101336);
#85001=AXIS2_PLACEMENT_3D('',#198318,#101339,#101340);
#85002=AXIS2_PLACEMENT_3D('',#198327,#101345,#101346);
#85003=AXIS2_PLACEMENT_3D('',#198333,#101350,#101351);
#85004=AXIS2_PLACEMENT_3D('',#198339,#101355,#101356);
#85005=AXIS2_PLACEMENT_3D('',#198342,#101359,#101360);
#85006=AXIS2_PLACEMENT_3D('',#198351,#101365,#101366);
#85007=AXIS2_PLACEMENT_3D('',#198357,#101370,#101371);
#85008=AXIS2_PLACEMENT_3D('',#198363,#101375,#101376);
#85009=AXIS2_PLACEMENT_3D('',#198366,#101379,#101380);
#85010=AXIS2_PLACEMENT_3D('',#198375,#101385,#101386);
#85011=AXIS2_PLACEMENT_3D('',#198381,#101390,#101391);
#85012=AXIS2_PLACEMENT_3D('',#198387,#101395,#101396);
#85013=AXIS2_PLACEMENT_3D('',#198390,#101399,#101400);
#85014=AXIS2_PLACEMENT_3D('',#198399,#101405,#101406);
#85015=AXIS2_PLACEMENT_3D('',#198405,#101410,#101411);
#85016=AXIS2_PLACEMENT_3D('',#198411,#101415,#101416);
#85017=AXIS2_PLACEMENT_3D('',#198414,#101419,#101420);
#85018=AXIS2_PLACEMENT_3D('',#198423,#101425,#101426);
#85019=AXIS2_PLACEMENT_3D('',#198429,#101430,#101431);
#85020=AXIS2_PLACEMENT_3D('',#198435,#101435,#101436);
#85021=AXIS2_PLACEMENT_3D('',#198438,#101439,#101440);
#85022=AXIS2_PLACEMENT_3D('',#198447,#101445,#101446);
#85023=AXIS2_PLACEMENT_3D('',#198453,#101450,#101451);
#85024=AXIS2_PLACEMENT_3D('',#198459,#101455,#101456);
#85025=AXIS2_PLACEMENT_3D('',#198462,#101459,#101460);
#85026=AXIS2_PLACEMENT_3D('',#198471,#101465,#101466);
#85027=AXIS2_PLACEMENT_3D('',#198477,#101470,#101471);
#85028=AXIS2_PLACEMENT_3D('',#198483,#101475,#101476);
#85029=AXIS2_PLACEMENT_3D('',#198486,#101479,#101480);
#85030=AXIS2_PLACEMENT_3D('',#198495,#101485,#101486);
#85031=AXIS2_PLACEMENT_3D('',#198501,#101490,#101491);
#85032=AXIS2_PLACEMENT_3D('',#198507,#101495,#101496);
#85033=AXIS2_PLACEMENT_3D('',#198510,#101499,#101500);
#85034=AXIS2_PLACEMENT_3D('',#198519,#101505,#101506);
#85035=AXIS2_PLACEMENT_3D('',#198525,#101510,#101511);
#85036=AXIS2_PLACEMENT_3D('',#198531,#101515,#101516);
#85037=AXIS2_PLACEMENT_3D('',#198534,#101519,#101520);
#85038=AXIS2_PLACEMENT_3D('',#198543,#101525,#101526);
#85039=AXIS2_PLACEMENT_3D('',#198549,#101530,#101531);
#85040=AXIS2_PLACEMENT_3D('',#198555,#101535,#101536);
#85041=AXIS2_PLACEMENT_3D('',#198558,#101539,#101540);
#85042=AXIS2_PLACEMENT_3D('',#198567,#101545,#101546);
#85043=AXIS2_PLACEMENT_3D('',#198573,#101550,#101551);
#85044=AXIS2_PLACEMENT_3D('',#198579,#101555,#101556);
#85045=AXIS2_PLACEMENT_3D('',#198582,#101559,#101560);
#85046=AXIS2_PLACEMENT_3D('',#198591,#101565,#101566);
#85047=AXIS2_PLACEMENT_3D('',#198597,#101570,#101571);
#85048=AXIS2_PLACEMENT_3D('',#198603,#101575,#101576);
#85049=AXIS2_PLACEMENT_3D('',#198606,#101579,#101580);
#85050=AXIS2_PLACEMENT_3D('',#198615,#101585,#101586);
#85051=AXIS2_PLACEMENT_3D('',#198621,#101590,#101591);
#85052=AXIS2_PLACEMENT_3D('',#198627,#101595,#101596);
#85053=AXIS2_PLACEMENT_3D('',#198630,#101599,#101600);
#85054=AXIS2_PLACEMENT_3D('',#198639,#101605,#101606);
#85055=AXIS2_PLACEMENT_3D('',#198645,#101610,#101611);
#85056=AXIS2_PLACEMENT_3D('',#198651,#101615,#101616);
#85057=AXIS2_PLACEMENT_3D('',#198654,#101619,#101620);
#85058=AXIS2_PLACEMENT_3D('',#198663,#101625,#101626);
#85059=AXIS2_PLACEMENT_3D('',#198669,#101630,#101631);
#85060=AXIS2_PLACEMENT_3D('',#198675,#101635,#101636);
#85061=AXIS2_PLACEMENT_3D('',#198678,#101639,#101640);
#85062=AXIS2_PLACEMENT_3D('',#198687,#101645,#101646);
#85063=AXIS2_PLACEMENT_3D('',#198693,#101650,#101651);
#85064=AXIS2_PLACEMENT_3D('',#198699,#101655,#101656);
#85065=AXIS2_PLACEMENT_3D('',#198702,#101659,#101660);
#85066=AXIS2_PLACEMENT_3D('',#198711,#101665,#101666);
#85067=AXIS2_PLACEMENT_3D('',#198717,#101670,#101671);
#85068=AXIS2_PLACEMENT_3D('',#198723,#101675,#101676);
#85069=AXIS2_PLACEMENT_3D('',#198726,#101679,#101680);
#85070=AXIS2_PLACEMENT_3D('',#198735,#101685,#101686);
#85071=AXIS2_PLACEMENT_3D('',#198741,#101690,#101691);
#85072=AXIS2_PLACEMENT_3D('',#198747,#101695,#101696);
#85073=AXIS2_PLACEMENT_3D('',#198750,#101699,#101700);
#85074=AXIS2_PLACEMENT_3D('',#198759,#101705,#101706);
#85075=AXIS2_PLACEMENT_3D('',#198765,#101710,#101711);
#85076=AXIS2_PLACEMENT_3D('',#198771,#101715,#101716);
#85077=AXIS2_PLACEMENT_3D('',#198774,#101719,#101720);
#85078=AXIS2_PLACEMENT_3D('',#198783,#101725,#101726);
#85079=AXIS2_PLACEMENT_3D('',#198789,#101730,#101731);
#85080=AXIS2_PLACEMENT_3D('',#198795,#101735,#101736);
#85081=AXIS2_PLACEMENT_3D('',#198798,#101739,#101740);
#85082=AXIS2_PLACEMENT_3D('',#198807,#101745,#101746);
#85083=AXIS2_PLACEMENT_3D('',#198813,#101750,#101751);
#85084=AXIS2_PLACEMENT_3D('',#198819,#101755,#101756);
#85085=AXIS2_PLACEMENT_3D('',#198822,#101759,#101760);
#85086=AXIS2_PLACEMENT_3D('',#198831,#101765,#101766);
#85087=AXIS2_PLACEMENT_3D('',#198837,#101770,#101771);
#85088=AXIS2_PLACEMENT_3D('',#198843,#101775,#101776);
#85089=AXIS2_PLACEMENT_3D('',#198846,#101779,#101780);
#85090=AXIS2_PLACEMENT_3D('',#198855,#101785,#101786);
#85091=AXIS2_PLACEMENT_3D('',#198861,#101790,#101791);
#85092=AXIS2_PLACEMENT_3D('',#198867,#101795,#101796);
#85093=AXIS2_PLACEMENT_3D('',#198870,#101799,#101800);
#85094=AXIS2_PLACEMENT_3D('',#198879,#101805,#101806);
#85095=AXIS2_PLACEMENT_3D('',#198885,#101810,#101811);
#85096=AXIS2_PLACEMENT_3D('',#198891,#101815,#101816);
#85097=AXIS2_PLACEMENT_3D('',#198894,#101819,#101820);
#85098=AXIS2_PLACEMENT_3D('',#198903,#101825,#101826);
#85099=AXIS2_PLACEMENT_3D('',#198909,#101830,#101831);
#85100=AXIS2_PLACEMENT_3D('',#198915,#101835,#101836);
#85101=AXIS2_PLACEMENT_3D('',#198918,#101839,#101840);
#85102=AXIS2_PLACEMENT_3D('',#198927,#101845,#101846);
#85103=AXIS2_PLACEMENT_3D('',#198933,#101850,#101851);
#85104=AXIS2_PLACEMENT_3D('',#198939,#101855,#101856);
#85105=AXIS2_PLACEMENT_3D('',#198942,#101859,#101860);
#85106=AXIS2_PLACEMENT_3D('',#198951,#101865,#101866);
#85107=AXIS2_PLACEMENT_3D('',#198957,#101870,#101871);
#85108=AXIS2_PLACEMENT_3D('',#198963,#101875,#101876);
#85109=AXIS2_PLACEMENT_3D('',#198966,#101879,#101880);
#85110=AXIS2_PLACEMENT_3D('',#198975,#101885,#101886);
#85111=AXIS2_PLACEMENT_3D('',#198981,#101890,#101891);
#85112=AXIS2_PLACEMENT_3D('',#198987,#101895,#101896);
#85113=AXIS2_PLACEMENT_3D('',#198990,#101899,#101900);
#85114=AXIS2_PLACEMENT_3D('',#198999,#101905,#101906);
#85115=AXIS2_PLACEMENT_3D('',#199005,#101910,#101911);
#85116=AXIS2_PLACEMENT_3D('',#199011,#101915,#101916);
#85117=AXIS2_PLACEMENT_3D('',#199014,#101919,#101920);
#85118=AXIS2_PLACEMENT_3D('',#199023,#101925,#101926);
#85119=AXIS2_PLACEMENT_3D('',#199029,#101930,#101931);
#85120=AXIS2_PLACEMENT_3D('',#199035,#101935,#101936);
#85121=AXIS2_PLACEMENT_3D('',#199038,#101939,#101940);
#85122=AXIS2_PLACEMENT_3D('',#199047,#101945,#101946);
#85123=AXIS2_PLACEMENT_3D('',#199053,#101950,#101951);
#85124=AXIS2_PLACEMENT_3D('',#199059,#101955,#101956);
#85125=AXIS2_PLACEMENT_3D('',#199062,#101959,#101960);
#85126=AXIS2_PLACEMENT_3D('',#199071,#101965,#101966);
#85127=AXIS2_PLACEMENT_3D('',#199077,#101970,#101971);
#85128=AXIS2_PLACEMENT_3D('',#199083,#101975,#101976);
#85129=AXIS2_PLACEMENT_3D('',#199086,#101979,#101980);
#85130=AXIS2_PLACEMENT_3D('',#199095,#101985,#101986);
#85131=AXIS2_PLACEMENT_3D('',#199101,#101990,#101991);
#85132=AXIS2_PLACEMENT_3D('',#199107,#101995,#101996);
#85133=AXIS2_PLACEMENT_3D('',#199110,#101999,#102000);
#85134=AXIS2_PLACEMENT_3D('',#199119,#102005,#102006);
#85135=AXIS2_PLACEMENT_3D('',#199125,#102010,#102011);
#85136=AXIS2_PLACEMENT_3D('',#199131,#102015,#102016);
#85137=AXIS2_PLACEMENT_3D('',#199134,#102019,#102020);
#85138=AXIS2_PLACEMENT_3D('',#199143,#102025,#102026);
#85139=AXIS2_PLACEMENT_3D('',#199149,#102030,#102031);
#85140=AXIS2_PLACEMENT_3D('',#199155,#102035,#102036);
#85141=AXIS2_PLACEMENT_3D('',#199158,#102039,#102040);
#85142=AXIS2_PLACEMENT_3D('',#199167,#102045,#102046);
#85143=AXIS2_PLACEMENT_3D('',#199173,#102050,#102051);
#85144=AXIS2_PLACEMENT_3D('',#199179,#102055,#102056);
#85145=AXIS2_PLACEMENT_3D('',#199182,#102059,#102060);
#85146=AXIS2_PLACEMENT_3D('',#199191,#102065,#102066);
#85147=AXIS2_PLACEMENT_3D('',#199197,#102070,#102071);
#85148=AXIS2_PLACEMENT_3D('',#199203,#102075,#102076);
#85149=AXIS2_PLACEMENT_3D('',#199206,#102079,#102080);
#85150=AXIS2_PLACEMENT_3D('',#199215,#102085,#102086);
#85151=AXIS2_PLACEMENT_3D('',#199221,#102090,#102091);
#85152=AXIS2_PLACEMENT_3D('',#199227,#102095,#102096);
#85153=AXIS2_PLACEMENT_3D('',#199230,#102099,#102100);
#85154=AXIS2_PLACEMENT_3D('',#199239,#102105,#102106);
#85155=AXIS2_PLACEMENT_3D('',#199245,#102110,#102111);
#85156=AXIS2_PLACEMENT_3D('',#199251,#102115,#102116);
#85157=AXIS2_PLACEMENT_3D('',#199254,#102119,#102120);
#85158=AXIS2_PLACEMENT_3D('',#199263,#102125,#102126);
#85159=AXIS2_PLACEMENT_3D('',#199269,#102130,#102131);
#85160=AXIS2_PLACEMENT_3D('',#199275,#102135,#102136);
#85161=AXIS2_PLACEMENT_3D('',#199278,#102139,#102140);
#85162=AXIS2_PLACEMENT_3D('',#199287,#102145,#102146);
#85163=AXIS2_PLACEMENT_3D('',#199293,#102150,#102151);
#85164=AXIS2_PLACEMENT_3D('',#199299,#102155,#102156);
#85165=AXIS2_PLACEMENT_3D('',#199302,#102159,#102160);
#85166=AXIS2_PLACEMENT_3D('',#199311,#102165,#102166);
#85167=AXIS2_PLACEMENT_3D('',#199317,#102170,#102171);
#85168=AXIS2_PLACEMENT_3D('',#199323,#102175,#102176);
#85169=AXIS2_PLACEMENT_3D('',#199326,#102179,#102180);
#85170=AXIS2_PLACEMENT_3D('',#199335,#102185,#102186);
#85171=AXIS2_PLACEMENT_3D('',#199341,#102190,#102191);
#85172=AXIS2_PLACEMENT_3D('',#199347,#102195,#102196);
#85173=AXIS2_PLACEMENT_3D('',#199350,#102199,#102200);
#85174=AXIS2_PLACEMENT_3D('',#199359,#102205,#102206);
#85175=AXIS2_PLACEMENT_3D('',#199365,#102210,#102211);
#85176=AXIS2_PLACEMENT_3D('',#199371,#102215,#102216);
#85177=AXIS2_PLACEMENT_3D('',#199374,#102219,#102220);
#85178=AXIS2_PLACEMENT_3D('',#199383,#102225,#102226);
#85179=AXIS2_PLACEMENT_3D('',#199389,#102230,#102231);
#85180=AXIS2_PLACEMENT_3D('',#199395,#102235,#102236);
#85181=AXIS2_PLACEMENT_3D('',#199398,#102239,#102240);
#85182=AXIS2_PLACEMENT_3D('',#199407,#102245,#102246);
#85183=AXIS2_PLACEMENT_3D('',#199413,#102250,#102251);
#85184=AXIS2_PLACEMENT_3D('',#199419,#102255,#102256);
#85185=AXIS2_PLACEMENT_3D('',#199422,#102259,#102260);
#85186=AXIS2_PLACEMENT_3D('',#199431,#102265,#102266);
#85187=AXIS2_PLACEMENT_3D('',#199437,#102270,#102271);
#85188=AXIS2_PLACEMENT_3D('',#199443,#102275,#102276);
#85189=AXIS2_PLACEMENT_3D('',#199446,#102279,#102280);
#85190=AXIS2_PLACEMENT_3D('',#199455,#102285,#102286);
#85191=AXIS2_PLACEMENT_3D('',#199461,#102290,#102291);
#85192=AXIS2_PLACEMENT_3D('',#199467,#102295,#102296);
#85193=AXIS2_PLACEMENT_3D('',#199470,#102299,#102300);
#85194=AXIS2_PLACEMENT_3D('',#199479,#102305,#102306);
#85195=AXIS2_PLACEMENT_3D('',#199485,#102310,#102311);
#85196=AXIS2_PLACEMENT_3D('',#199491,#102315,#102316);
#85197=AXIS2_PLACEMENT_3D('',#199494,#102319,#102320);
#85198=AXIS2_PLACEMENT_3D('',#199503,#102325,#102326);
#85199=AXIS2_PLACEMENT_3D('',#199509,#102330,#102331);
#85200=AXIS2_PLACEMENT_3D('',#199515,#102335,#102336);
#85201=AXIS2_PLACEMENT_3D('',#199518,#102339,#102340);
#85202=AXIS2_PLACEMENT_3D('',#199527,#102345,#102346);
#85203=AXIS2_PLACEMENT_3D('',#199533,#102350,#102351);
#85204=AXIS2_PLACEMENT_3D('',#199539,#102355,#102356);
#85205=AXIS2_PLACEMENT_3D('',#199542,#102359,#102360);
#85206=AXIS2_PLACEMENT_3D('',#199551,#102365,#102366);
#85207=AXIS2_PLACEMENT_3D('',#199557,#102370,#102371);
#85208=AXIS2_PLACEMENT_3D('',#199563,#102375,#102376);
#85209=AXIS2_PLACEMENT_3D('',#199566,#102379,#102380);
#85210=AXIS2_PLACEMENT_3D('',#199575,#102385,#102386);
#85211=AXIS2_PLACEMENT_3D('',#199581,#102390,#102391);
#85212=AXIS2_PLACEMENT_3D('',#199587,#102395,#102396);
#85213=AXIS2_PLACEMENT_3D('',#199590,#102399,#102400);
#85214=AXIS2_PLACEMENT_3D('',#199599,#102405,#102406);
#85215=AXIS2_PLACEMENT_3D('',#199605,#102410,#102411);
#85216=AXIS2_PLACEMENT_3D('',#199611,#102415,#102416);
#85217=AXIS2_PLACEMENT_3D('',#199614,#102419,#102420);
#85218=AXIS2_PLACEMENT_3D('',#199623,#102425,#102426);
#85219=AXIS2_PLACEMENT_3D('',#199629,#102430,#102431);
#85220=AXIS2_PLACEMENT_3D('',#199635,#102435,#102436);
#85221=AXIS2_PLACEMENT_3D('',#199638,#102439,#102440);
#85222=AXIS2_PLACEMENT_3D('',#199647,#102445,#102446);
#85223=AXIS2_PLACEMENT_3D('',#199653,#102450,#102451);
#85224=AXIS2_PLACEMENT_3D('',#199659,#102455,#102456);
#85225=AXIS2_PLACEMENT_3D('',#199662,#102459,#102460);
#85226=AXIS2_PLACEMENT_3D('',#199671,#102465,#102466);
#85227=AXIS2_PLACEMENT_3D('',#199677,#102470,#102471);
#85228=AXIS2_PLACEMENT_3D('',#199683,#102475,#102476);
#85229=AXIS2_PLACEMENT_3D('',#199686,#102479,#102480);
#85230=AXIS2_PLACEMENT_3D('',#199695,#102485,#102486);
#85231=AXIS2_PLACEMENT_3D('',#199701,#102490,#102491);
#85232=AXIS2_PLACEMENT_3D('',#199707,#102495,#102496);
#85233=AXIS2_PLACEMENT_3D('',#199710,#102499,#102500);
#85234=AXIS2_PLACEMENT_3D('',#199719,#102505,#102506);
#85235=AXIS2_PLACEMENT_3D('',#199725,#102510,#102511);
#85236=AXIS2_PLACEMENT_3D('',#199731,#102515,#102516);
#85237=AXIS2_PLACEMENT_3D('',#199734,#102519,#102520);
#85238=AXIS2_PLACEMENT_3D('',#199743,#102525,#102526);
#85239=AXIS2_PLACEMENT_3D('',#199749,#102530,#102531);
#85240=AXIS2_PLACEMENT_3D('',#199755,#102535,#102536);
#85241=AXIS2_PLACEMENT_3D('',#199758,#102539,#102540);
#85242=AXIS2_PLACEMENT_3D('',#199767,#102545,#102546);
#85243=AXIS2_PLACEMENT_3D('',#199773,#102550,#102551);
#85244=AXIS2_PLACEMENT_3D('',#199779,#102555,#102556);
#85245=AXIS2_PLACEMENT_3D('',#199782,#102559,#102560);
#85246=AXIS2_PLACEMENT_3D('',#199791,#102565,#102566);
#85247=AXIS2_PLACEMENT_3D('',#199797,#102570,#102571);
#85248=AXIS2_PLACEMENT_3D('',#199803,#102575,#102576);
#85249=AXIS2_PLACEMENT_3D('',#199806,#102579,#102580);
#85250=AXIS2_PLACEMENT_3D('',#199815,#102585,#102586);
#85251=AXIS2_PLACEMENT_3D('',#199821,#102590,#102591);
#85252=AXIS2_PLACEMENT_3D('',#199827,#102595,#102596);
#85253=AXIS2_PLACEMENT_3D('',#199830,#102599,#102600);
#85254=AXIS2_PLACEMENT_3D('',#199839,#102605,#102606);
#85255=AXIS2_PLACEMENT_3D('',#199845,#102610,#102611);
#85256=AXIS2_PLACEMENT_3D('',#199851,#102615,#102616);
#85257=AXIS2_PLACEMENT_3D('',#199854,#102619,#102620);
#85258=AXIS2_PLACEMENT_3D('',#199863,#102625,#102626);
#85259=AXIS2_PLACEMENT_3D('',#199869,#102630,#102631);
#85260=AXIS2_PLACEMENT_3D('',#199875,#102635,#102636);
#85261=AXIS2_PLACEMENT_3D('',#199878,#102639,#102640);
#85262=AXIS2_PLACEMENT_3D('',#199887,#102645,#102646);
#85263=AXIS2_PLACEMENT_3D('',#199893,#102650,#102651);
#85264=AXIS2_PLACEMENT_3D('',#199899,#102655,#102656);
#85265=AXIS2_PLACEMENT_3D('',#199902,#102659,#102660);
#85266=AXIS2_PLACEMENT_3D('',#199911,#102665,#102666);
#85267=AXIS2_PLACEMENT_3D('',#199917,#102670,#102671);
#85268=AXIS2_PLACEMENT_3D('',#199923,#102675,#102676);
#85269=AXIS2_PLACEMENT_3D('',#199926,#102679,#102680);
#85270=AXIS2_PLACEMENT_3D('',#199935,#102685,#102686);
#85271=AXIS2_PLACEMENT_3D('',#199941,#102690,#102691);
#85272=AXIS2_PLACEMENT_3D('',#199947,#102695,#102696);
#85273=AXIS2_PLACEMENT_3D('',#199950,#102699,#102700);
#85274=AXIS2_PLACEMENT_3D('',#199959,#102705,#102706);
#85275=AXIS2_PLACEMENT_3D('',#199965,#102710,#102711);
#85276=AXIS2_PLACEMENT_3D('',#199971,#102715,#102716);
#85277=AXIS2_PLACEMENT_3D('',#199974,#102719,#102720);
#85278=AXIS2_PLACEMENT_3D('',#199983,#102725,#102726);
#85279=AXIS2_PLACEMENT_3D('',#199989,#102730,#102731);
#85280=AXIS2_PLACEMENT_3D('',#199995,#102735,#102736);
#85281=AXIS2_PLACEMENT_3D('',#199998,#102739,#102740);
#85282=AXIS2_PLACEMENT_3D('',#200007,#102745,#102746);
#85283=AXIS2_PLACEMENT_3D('',#200013,#102750,#102751);
#85284=AXIS2_PLACEMENT_3D('',#200019,#102755,#102756);
#85285=AXIS2_PLACEMENT_3D('',#200022,#102759,#102760);
#85286=AXIS2_PLACEMENT_3D('',#200031,#102765,#102766);
#85287=AXIS2_PLACEMENT_3D('',#200037,#102770,#102771);
#85288=AXIS2_PLACEMENT_3D('',#200043,#102775,#102776);
#85289=AXIS2_PLACEMENT_3D('',#200046,#102779,#102780);
#85290=AXIS2_PLACEMENT_3D('',#200055,#102785,#102786);
#85291=AXIS2_PLACEMENT_3D('',#200061,#102790,#102791);
#85292=AXIS2_PLACEMENT_3D('',#200067,#102795,#102796);
#85293=AXIS2_PLACEMENT_3D('',#200070,#102799,#102800);
#85294=AXIS2_PLACEMENT_3D('',#200079,#102805,#102806);
#85295=AXIS2_PLACEMENT_3D('',#200085,#102810,#102811);
#85296=AXIS2_PLACEMENT_3D('',#200091,#102815,#102816);
#85297=AXIS2_PLACEMENT_3D('',#200094,#102819,#102820);
#85298=AXIS2_PLACEMENT_3D('',#200103,#102825,#102826);
#85299=AXIS2_PLACEMENT_3D('',#200109,#102830,#102831);
#85300=AXIS2_PLACEMENT_3D('',#200115,#102835,#102836);
#85301=AXIS2_PLACEMENT_3D('',#200118,#102839,#102840);
#85302=AXIS2_PLACEMENT_3D('',#200127,#102845,#102846);
#85303=AXIS2_PLACEMENT_3D('',#200133,#102850,#102851);
#85304=AXIS2_PLACEMENT_3D('',#200139,#102855,#102856);
#85305=AXIS2_PLACEMENT_3D('',#200142,#102859,#102860);
#85306=AXIS2_PLACEMENT_3D('',#200151,#102865,#102866);
#85307=AXIS2_PLACEMENT_3D('',#200157,#102870,#102871);
#85308=AXIS2_PLACEMENT_3D('',#200163,#102875,#102876);
#85309=AXIS2_PLACEMENT_3D('',#200166,#102879,#102880);
#85310=AXIS2_PLACEMENT_3D('',#200175,#102885,#102886);
#85311=AXIS2_PLACEMENT_3D('',#200181,#102890,#102891);
#85312=AXIS2_PLACEMENT_3D('',#200187,#102895,#102896);
#85313=AXIS2_PLACEMENT_3D('',#200190,#102899,#102900);
#85314=AXIS2_PLACEMENT_3D('',#200199,#102905,#102906);
#85315=AXIS2_PLACEMENT_3D('',#200205,#102910,#102911);
#85316=AXIS2_PLACEMENT_3D('',#200211,#102915,#102916);
#85317=AXIS2_PLACEMENT_3D('',#200214,#102919,#102920);
#85318=AXIS2_PLACEMENT_3D('',#200223,#102925,#102926);
#85319=AXIS2_PLACEMENT_3D('',#200229,#102930,#102931);
#85320=AXIS2_PLACEMENT_3D('',#200235,#102935,#102936);
#85321=AXIS2_PLACEMENT_3D('',#200238,#102939,#102940);
#85322=AXIS2_PLACEMENT_3D('',#200247,#102945,#102946);
#85323=AXIS2_PLACEMENT_3D('',#200253,#102950,#102951);
#85324=AXIS2_PLACEMENT_3D('',#200259,#102955,#102956);
#85325=AXIS2_PLACEMENT_3D('',#200262,#102959,#102960);
#85326=AXIS2_PLACEMENT_3D('',#200271,#102965,#102966);
#85327=AXIS2_PLACEMENT_3D('',#200277,#102970,#102971);
#85328=AXIS2_PLACEMENT_3D('',#200283,#102975,#102976);
#85329=AXIS2_PLACEMENT_3D('',#200286,#102979,#102980);
#85330=AXIS2_PLACEMENT_3D('',#200295,#102985,#102986);
#85331=AXIS2_PLACEMENT_3D('',#200301,#102990,#102991);
#85332=AXIS2_PLACEMENT_3D('',#200307,#102995,#102996);
#85333=AXIS2_PLACEMENT_3D('',#200310,#102999,#103000);
#85334=AXIS2_PLACEMENT_3D('',#200319,#103005,#103006);
#85335=AXIS2_PLACEMENT_3D('',#200325,#103010,#103011);
#85336=AXIS2_PLACEMENT_3D('',#200331,#103015,#103016);
#85337=AXIS2_PLACEMENT_3D('',#200334,#103019,#103020);
#85338=AXIS2_PLACEMENT_3D('',#200343,#103025,#103026);
#85339=AXIS2_PLACEMENT_3D('',#200349,#103030,#103031);
#85340=AXIS2_PLACEMENT_3D('',#200355,#103035,#103036);
#85341=AXIS2_PLACEMENT_3D('',#200358,#103039,#103040);
#85342=AXIS2_PLACEMENT_3D('',#200367,#103045,#103046);
#85343=AXIS2_PLACEMENT_3D('',#200373,#103050,#103051);
#85344=AXIS2_PLACEMENT_3D('',#200379,#103055,#103056);
#85345=AXIS2_PLACEMENT_3D('',#200382,#103059,#103060);
#85346=AXIS2_PLACEMENT_3D('',#200391,#103065,#103066);
#85347=AXIS2_PLACEMENT_3D('',#200397,#103070,#103071);
#85348=AXIS2_PLACEMENT_3D('',#200403,#103075,#103076);
#85349=AXIS2_PLACEMENT_3D('',#200406,#103079,#103080);
#85350=AXIS2_PLACEMENT_3D('',#200415,#103085,#103086);
#85351=AXIS2_PLACEMENT_3D('',#200421,#103090,#103091);
#85352=AXIS2_PLACEMENT_3D('',#200427,#103095,#103096);
#85353=AXIS2_PLACEMENT_3D('',#200430,#103099,#103100);
#85354=AXIS2_PLACEMENT_3D('',#200439,#103105,#103106);
#85355=AXIS2_PLACEMENT_3D('',#200445,#103110,#103111);
#85356=AXIS2_PLACEMENT_3D('',#200451,#103115,#103116);
#85357=AXIS2_PLACEMENT_3D('',#200454,#103119,#103120);
#85358=AXIS2_PLACEMENT_3D('',#200463,#103125,#103126);
#85359=AXIS2_PLACEMENT_3D('',#200469,#103130,#103131);
#85360=AXIS2_PLACEMENT_3D('',#200475,#103135,#103136);
#85361=AXIS2_PLACEMENT_3D('',#200478,#103139,#103140);
#85362=AXIS2_PLACEMENT_3D('',#200487,#103145,#103146);
#85363=AXIS2_PLACEMENT_3D('',#200493,#103150,#103151);
#85364=AXIS2_PLACEMENT_3D('',#200499,#103155,#103156);
#85365=AXIS2_PLACEMENT_3D('',#200502,#103159,#103160);
#85366=AXIS2_PLACEMENT_3D('',#200511,#103165,#103166);
#85367=AXIS2_PLACEMENT_3D('',#200517,#103170,#103171);
#85368=AXIS2_PLACEMENT_3D('',#200523,#103175,#103176);
#85369=AXIS2_PLACEMENT_3D('',#200526,#103179,#103180);
#85370=AXIS2_PLACEMENT_3D('',#200535,#103185,#103186);
#85371=AXIS2_PLACEMENT_3D('',#200541,#103190,#103191);
#85372=AXIS2_PLACEMENT_3D('',#200547,#103195,#103196);
#85373=AXIS2_PLACEMENT_3D('',#200550,#103199,#103200);
#85374=AXIS2_PLACEMENT_3D('',#200559,#103205,#103206);
#85375=AXIS2_PLACEMENT_3D('',#200565,#103210,#103211);
#85376=AXIS2_PLACEMENT_3D('',#200571,#103215,#103216);
#85377=AXIS2_PLACEMENT_3D('',#200574,#103219,#103220);
#85378=AXIS2_PLACEMENT_3D('',#200583,#103225,#103226);
#85379=AXIS2_PLACEMENT_3D('',#200589,#103230,#103231);
#85380=AXIS2_PLACEMENT_3D('',#200595,#103235,#103236);
#85381=AXIS2_PLACEMENT_3D('',#200598,#103239,#103240);
#85382=AXIS2_PLACEMENT_3D('',#200607,#103245,#103246);
#85383=AXIS2_PLACEMENT_3D('',#200613,#103250,#103251);
#85384=AXIS2_PLACEMENT_3D('',#200619,#103255,#103256);
#85385=AXIS2_PLACEMENT_3D('',#200622,#103259,#103260);
#85386=AXIS2_PLACEMENT_3D('',#200631,#103265,#103266);
#85387=AXIS2_PLACEMENT_3D('',#200637,#103270,#103271);
#85388=AXIS2_PLACEMENT_3D('',#200643,#103275,#103276);
#85389=AXIS2_PLACEMENT_3D('',#200646,#103279,#103280);
#85390=AXIS2_PLACEMENT_3D('',#200655,#103285,#103286);
#85391=AXIS2_PLACEMENT_3D('',#200661,#103290,#103291);
#85392=AXIS2_PLACEMENT_3D('',#200667,#103295,#103296);
#85393=AXIS2_PLACEMENT_3D('',#200670,#103299,#103300);
#85394=AXIS2_PLACEMENT_3D('',#200679,#103305,#103306);
#85395=AXIS2_PLACEMENT_3D('',#200685,#103310,#103311);
#85396=AXIS2_PLACEMENT_3D('',#200691,#103315,#103316);
#85397=AXIS2_PLACEMENT_3D('',#200694,#103319,#103320);
#85398=AXIS2_PLACEMENT_3D('',#200703,#103325,#103326);
#85399=AXIS2_PLACEMENT_3D('',#200709,#103330,#103331);
#85400=AXIS2_PLACEMENT_3D('',#200715,#103335,#103336);
#85401=AXIS2_PLACEMENT_3D('',#200718,#103339,#103340);
#85402=AXIS2_PLACEMENT_3D('',#200727,#103345,#103346);
#85403=AXIS2_PLACEMENT_3D('',#200733,#103350,#103351);
#85404=AXIS2_PLACEMENT_3D('',#200739,#103355,#103356);
#85405=AXIS2_PLACEMENT_3D('',#200742,#103359,#103360);
#85406=AXIS2_PLACEMENT_3D('',#200751,#103365,#103366);
#85407=AXIS2_PLACEMENT_3D('',#200757,#103370,#103371);
#85408=AXIS2_PLACEMENT_3D('',#200763,#103375,#103376);
#85409=AXIS2_PLACEMENT_3D('',#200766,#103379,#103380);
#85410=AXIS2_PLACEMENT_3D('',#200775,#103385,#103386);
#85411=AXIS2_PLACEMENT_3D('',#200781,#103390,#103391);
#85412=AXIS2_PLACEMENT_3D('',#200787,#103395,#103396);
#85413=AXIS2_PLACEMENT_3D('',#200790,#103399,#103400);
#85414=AXIS2_PLACEMENT_3D('',#200799,#103405,#103406);
#85415=AXIS2_PLACEMENT_3D('',#200805,#103410,#103411);
#85416=AXIS2_PLACEMENT_3D('',#200811,#103415,#103416);
#85417=AXIS2_PLACEMENT_3D('',#200814,#103419,#103420);
#85418=AXIS2_PLACEMENT_3D('',#200823,#103425,#103426);
#85419=AXIS2_PLACEMENT_3D('',#200829,#103430,#103431);
#85420=AXIS2_PLACEMENT_3D('',#200835,#103435,#103436);
#85421=AXIS2_PLACEMENT_3D('',#200838,#103439,#103440);
#85422=AXIS2_PLACEMENT_3D('',#200847,#103445,#103446);
#85423=AXIS2_PLACEMENT_3D('',#200853,#103450,#103451);
#85424=AXIS2_PLACEMENT_3D('',#200859,#103455,#103456);
#85425=AXIS2_PLACEMENT_3D('',#200862,#103459,#103460);
#85426=AXIS2_PLACEMENT_3D('',#200871,#103465,#103466);
#85427=AXIS2_PLACEMENT_3D('',#200877,#103470,#103471);
#85428=AXIS2_PLACEMENT_3D('',#200883,#103475,#103476);
#85429=AXIS2_PLACEMENT_3D('',#200886,#103479,#103480);
#85430=AXIS2_PLACEMENT_3D('',#200895,#103485,#103486);
#85431=AXIS2_PLACEMENT_3D('',#200901,#103490,#103491);
#85432=AXIS2_PLACEMENT_3D('',#200907,#103495,#103496);
#85433=AXIS2_PLACEMENT_3D('',#200910,#103499,#103500);
#85434=AXIS2_PLACEMENT_3D('',#200919,#103505,#103506);
#85435=AXIS2_PLACEMENT_3D('',#200925,#103510,#103511);
#85436=AXIS2_PLACEMENT_3D('',#200931,#103515,#103516);
#85437=AXIS2_PLACEMENT_3D('',#200934,#103519,#103520);
#85438=AXIS2_PLACEMENT_3D('',#200943,#103525,#103526);
#85439=AXIS2_PLACEMENT_3D('',#200949,#103530,#103531);
#85440=AXIS2_PLACEMENT_3D('',#200955,#103535,#103536);
#85441=AXIS2_PLACEMENT_3D('',#200958,#103539,#103540);
#85442=AXIS2_PLACEMENT_3D('',#200967,#103545,#103546);
#85443=AXIS2_PLACEMENT_3D('',#200973,#103550,#103551);
#85444=AXIS2_PLACEMENT_3D('',#200979,#103555,#103556);
#85445=AXIS2_PLACEMENT_3D('',#200982,#103559,#103560);
#85446=AXIS2_PLACEMENT_3D('',#200991,#103565,#103566);
#85447=AXIS2_PLACEMENT_3D('',#200997,#103570,#103571);
#85448=AXIS2_PLACEMENT_3D('',#201003,#103575,#103576);
#85449=AXIS2_PLACEMENT_3D('',#201006,#103579,#103580);
#85450=AXIS2_PLACEMENT_3D('',#201015,#103585,#103586);
#85451=AXIS2_PLACEMENT_3D('',#201021,#103590,#103591);
#85452=AXIS2_PLACEMENT_3D('',#201027,#103595,#103596);
#85453=AXIS2_PLACEMENT_3D('',#201030,#103599,#103600);
#85454=AXIS2_PLACEMENT_3D('',#201039,#103605,#103606);
#85455=AXIS2_PLACEMENT_3D('',#201045,#103610,#103611);
#85456=AXIS2_PLACEMENT_3D('',#201051,#103615,#103616);
#85457=AXIS2_PLACEMENT_3D('',#201054,#103619,#103620);
#85458=AXIS2_PLACEMENT_3D('',#201063,#103625,#103626);
#85459=AXIS2_PLACEMENT_3D('',#201069,#103630,#103631);
#85460=AXIS2_PLACEMENT_3D('',#201075,#103635,#103636);
#85461=AXIS2_PLACEMENT_3D('',#201078,#103639,#103640);
#85462=AXIS2_PLACEMENT_3D('',#201087,#103645,#103646);
#85463=AXIS2_PLACEMENT_3D('',#201093,#103650,#103651);
#85464=AXIS2_PLACEMENT_3D('',#201099,#103655,#103656);
#85465=AXIS2_PLACEMENT_3D('',#201102,#103659,#103660);
#85466=AXIS2_PLACEMENT_3D('',#201111,#103665,#103666);
#85467=AXIS2_PLACEMENT_3D('',#201117,#103670,#103671);
#85468=AXIS2_PLACEMENT_3D('',#201123,#103675,#103676);
#85469=AXIS2_PLACEMENT_3D('',#201126,#103679,#103680);
#85470=AXIS2_PLACEMENT_3D('',#201135,#103685,#103686);
#85471=AXIS2_PLACEMENT_3D('',#201141,#103690,#103691);
#85472=AXIS2_PLACEMENT_3D('',#201147,#103695,#103696);
#85473=AXIS2_PLACEMENT_3D('',#201150,#103699,#103700);
#85474=AXIS2_PLACEMENT_3D('',#201159,#103705,#103706);
#85475=AXIS2_PLACEMENT_3D('',#201165,#103710,#103711);
#85476=AXIS2_PLACEMENT_3D('',#201171,#103715,#103716);
#85477=AXIS2_PLACEMENT_3D('',#201174,#103719,#103720);
#85478=AXIS2_PLACEMENT_3D('',#201183,#103725,#103726);
#85479=AXIS2_PLACEMENT_3D('',#201189,#103730,#103731);
#85480=AXIS2_PLACEMENT_3D('',#201195,#103735,#103736);
#85481=AXIS2_PLACEMENT_3D('',#201198,#103739,#103740);
#85482=AXIS2_PLACEMENT_3D('',#201207,#103745,#103746);
#85483=AXIS2_PLACEMENT_3D('',#201213,#103750,#103751);
#85484=AXIS2_PLACEMENT_3D('',#201219,#103755,#103756);
#85485=AXIS2_PLACEMENT_3D('',#201222,#103759,#103760);
#85486=AXIS2_PLACEMENT_3D('',#201231,#103765,#103766);
#85487=AXIS2_PLACEMENT_3D('',#201237,#103770,#103771);
#85488=AXIS2_PLACEMENT_3D('',#201243,#103775,#103776);
#85489=AXIS2_PLACEMENT_3D('',#201246,#103779,#103780);
#85490=AXIS2_PLACEMENT_3D('',#201255,#103785,#103786);
#85491=AXIS2_PLACEMENT_3D('',#201261,#103790,#103791);
#85492=AXIS2_PLACEMENT_3D('',#201267,#103795,#103796);
#85493=AXIS2_PLACEMENT_3D('',#201270,#103799,#103800);
#85494=AXIS2_PLACEMENT_3D('',#201279,#103805,#103806);
#85495=AXIS2_PLACEMENT_3D('',#201285,#103810,#103811);
#85496=AXIS2_PLACEMENT_3D('',#201291,#103815,#103816);
#85497=AXIS2_PLACEMENT_3D('',#201294,#103819,#103820);
#85498=AXIS2_PLACEMENT_3D('',#201303,#103825,#103826);
#85499=AXIS2_PLACEMENT_3D('',#201309,#103830,#103831);
#85500=AXIS2_PLACEMENT_3D('',#201315,#103835,#103836);
#85501=AXIS2_PLACEMENT_3D('',#201318,#103839,#103840);
#85502=AXIS2_PLACEMENT_3D('',#201327,#103845,#103846);
#85503=AXIS2_PLACEMENT_3D('',#201333,#103850,#103851);
#85504=AXIS2_PLACEMENT_3D('',#201339,#103855,#103856);
#85505=AXIS2_PLACEMENT_3D('',#201342,#103859,#103860);
#85506=AXIS2_PLACEMENT_3D('',#201351,#103865,#103866);
#85507=AXIS2_PLACEMENT_3D('',#201357,#103870,#103871);
#85508=AXIS2_PLACEMENT_3D('',#201363,#103875,#103876);
#85509=AXIS2_PLACEMENT_3D('',#201366,#103879,#103880);
#85510=AXIS2_PLACEMENT_3D('',#201375,#103885,#103886);
#85511=AXIS2_PLACEMENT_3D('',#201381,#103890,#103891);
#85512=AXIS2_PLACEMENT_3D('',#201387,#103895,#103896);
#85513=AXIS2_PLACEMENT_3D('',#201390,#103899,#103900);
#85514=AXIS2_PLACEMENT_3D('',#201399,#103905,#103906);
#85515=AXIS2_PLACEMENT_3D('',#201405,#103910,#103911);
#85516=AXIS2_PLACEMENT_3D('',#201411,#103915,#103916);
#85517=AXIS2_PLACEMENT_3D('',#201414,#103919,#103920);
#85518=AXIS2_PLACEMENT_3D('',#201423,#103925,#103926);
#85519=AXIS2_PLACEMENT_3D('',#201429,#103930,#103931);
#85520=AXIS2_PLACEMENT_3D('',#201435,#103935,#103936);
#85521=AXIS2_PLACEMENT_3D('',#201438,#103939,#103940);
#85522=AXIS2_PLACEMENT_3D('',#201447,#103945,#103946);
#85523=AXIS2_PLACEMENT_3D('',#201453,#103950,#103951);
#85524=AXIS2_PLACEMENT_3D('',#201459,#103955,#103956);
#85525=AXIS2_PLACEMENT_3D('',#201462,#103959,#103960);
#85526=AXIS2_PLACEMENT_3D('',#201471,#103965,#103966);
#85527=AXIS2_PLACEMENT_3D('',#201477,#103970,#103971);
#85528=AXIS2_PLACEMENT_3D('',#201483,#103975,#103976);
#85529=AXIS2_PLACEMENT_3D('',#201486,#103979,#103980);
#85530=AXIS2_PLACEMENT_3D('',#201495,#103985,#103986);
#85531=AXIS2_PLACEMENT_3D('',#201501,#103990,#103991);
#85532=AXIS2_PLACEMENT_3D('',#201507,#103995,#103996);
#85533=AXIS2_PLACEMENT_3D('',#201510,#103999,#104000);
#85534=AXIS2_PLACEMENT_3D('',#201519,#104005,#104006);
#85535=AXIS2_PLACEMENT_3D('',#201525,#104010,#104011);
#85536=AXIS2_PLACEMENT_3D('',#201531,#104015,#104016);
#85537=AXIS2_PLACEMENT_3D('',#201534,#104019,#104020);
#85538=AXIS2_PLACEMENT_3D('',#201543,#104025,#104026);
#85539=AXIS2_PLACEMENT_3D('',#201549,#104030,#104031);
#85540=AXIS2_PLACEMENT_3D('',#201555,#104035,#104036);
#85541=AXIS2_PLACEMENT_3D('',#201558,#104039,#104040);
#85542=AXIS2_PLACEMENT_3D('',#201567,#104045,#104046);
#85543=AXIS2_PLACEMENT_3D('',#201573,#104050,#104051);
#85544=AXIS2_PLACEMENT_3D('',#201579,#104055,#104056);
#85545=AXIS2_PLACEMENT_3D('',#201582,#104059,#104060);
#85546=AXIS2_PLACEMENT_3D('',#201591,#104065,#104066);
#85547=AXIS2_PLACEMENT_3D('',#201597,#104070,#104071);
#85548=AXIS2_PLACEMENT_3D('',#201603,#104075,#104076);
#85549=AXIS2_PLACEMENT_3D('',#201606,#104079,#104080);
#85550=AXIS2_PLACEMENT_3D('',#201615,#104085,#104086);
#85551=AXIS2_PLACEMENT_3D('',#201621,#104090,#104091);
#85552=AXIS2_PLACEMENT_3D('',#201627,#104095,#104096);
#85553=AXIS2_PLACEMENT_3D('',#201630,#104099,#104100);
#85554=AXIS2_PLACEMENT_3D('',#201639,#104105,#104106);
#85555=AXIS2_PLACEMENT_3D('',#201645,#104110,#104111);
#85556=AXIS2_PLACEMENT_3D('',#201651,#104115,#104116);
#85557=AXIS2_PLACEMENT_3D('',#201654,#104119,#104120);
#85558=AXIS2_PLACEMENT_3D('',#201663,#104125,#104126);
#85559=AXIS2_PLACEMENT_3D('',#201669,#104130,#104131);
#85560=AXIS2_PLACEMENT_3D('',#201675,#104135,#104136);
#85561=AXIS2_PLACEMENT_3D('',#201678,#104139,#104140);
#85562=AXIS2_PLACEMENT_3D('',#201687,#104145,#104146);
#85563=AXIS2_PLACEMENT_3D('',#201693,#104150,#104151);
#85564=AXIS2_PLACEMENT_3D('',#201699,#104155,#104156);
#85565=AXIS2_PLACEMENT_3D('',#201702,#104159,#104160);
#85566=AXIS2_PLACEMENT_3D('',#201711,#104165,#104166);
#85567=AXIS2_PLACEMENT_3D('',#201717,#104170,#104171);
#85568=AXIS2_PLACEMENT_3D('',#201723,#104175,#104176);
#85569=AXIS2_PLACEMENT_3D('',#201726,#104179,#104180);
#85570=AXIS2_PLACEMENT_3D('',#201735,#104185,#104186);
#85571=AXIS2_PLACEMENT_3D('',#201741,#104190,#104191);
#85572=AXIS2_PLACEMENT_3D('',#201747,#104195,#104196);
#85573=AXIS2_PLACEMENT_3D('',#201750,#104199,#104200);
#85574=AXIS2_PLACEMENT_3D('',#201759,#104205,#104206);
#85575=AXIS2_PLACEMENT_3D('',#201765,#104210,#104211);
#85576=AXIS2_PLACEMENT_3D('',#201771,#104215,#104216);
#85577=AXIS2_PLACEMENT_3D('',#201774,#104219,#104220);
#85578=AXIS2_PLACEMENT_3D('',#201783,#104225,#104226);
#85579=AXIS2_PLACEMENT_3D('',#201789,#104230,#104231);
#85580=AXIS2_PLACEMENT_3D('',#201795,#104235,#104236);
#85581=AXIS2_PLACEMENT_3D('',#201798,#104239,#104240);
#85582=AXIS2_PLACEMENT_3D('',#201807,#104245,#104246);
#85583=AXIS2_PLACEMENT_3D('',#201813,#104250,#104251);
#85584=AXIS2_PLACEMENT_3D('',#201819,#104255,#104256);
#85585=AXIS2_PLACEMENT_3D('',#201822,#104259,#104260);
#85586=AXIS2_PLACEMENT_3D('',#201831,#104265,#104266);
#85587=AXIS2_PLACEMENT_3D('',#201837,#104270,#104271);
#85588=AXIS2_PLACEMENT_3D('',#201843,#104275,#104276);
#85589=AXIS2_PLACEMENT_3D('',#201846,#104279,#104280);
#85590=AXIS2_PLACEMENT_3D('',#201855,#104285,#104286);
#85591=AXIS2_PLACEMENT_3D('',#201861,#104290,#104291);
#85592=AXIS2_PLACEMENT_3D('',#201867,#104295,#104296);
#85593=AXIS2_PLACEMENT_3D('',#201870,#104299,#104300);
#85594=AXIS2_PLACEMENT_3D('',#201879,#104305,#104306);
#85595=AXIS2_PLACEMENT_3D('',#201885,#104310,#104311);
#85596=AXIS2_PLACEMENT_3D('',#201891,#104315,#104316);
#85597=AXIS2_PLACEMENT_3D('',#201894,#104319,#104320);
#85598=AXIS2_PLACEMENT_3D('',#201903,#104325,#104326);
#85599=AXIS2_PLACEMENT_3D('',#201909,#104330,#104331);
#85600=AXIS2_PLACEMENT_3D('',#201915,#104335,#104336);
#85601=AXIS2_PLACEMENT_3D('',#201918,#104339,#104340);
#85602=AXIS2_PLACEMENT_3D('',#201927,#104345,#104346);
#85603=AXIS2_PLACEMENT_3D('',#201933,#104350,#104351);
#85604=AXIS2_PLACEMENT_3D('',#201939,#104355,#104356);
#85605=AXIS2_PLACEMENT_3D('',#201942,#104359,#104360);
#85606=AXIS2_PLACEMENT_3D('',#201951,#104365,#104366);
#85607=AXIS2_PLACEMENT_3D('',#201957,#104370,#104371);
#85608=AXIS2_PLACEMENT_3D('',#201963,#104375,#104376);
#85609=AXIS2_PLACEMENT_3D('',#201966,#104379,#104380);
#85610=AXIS2_PLACEMENT_3D('',#201975,#104385,#104386);
#85611=AXIS2_PLACEMENT_3D('',#201981,#104390,#104391);
#85612=AXIS2_PLACEMENT_3D('',#201987,#104395,#104396);
#85613=AXIS2_PLACEMENT_3D('',#201990,#104399,#104400);
#85614=AXIS2_PLACEMENT_3D('',#201999,#104405,#104406);
#85615=AXIS2_PLACEMENT_3D('',#202005,#104410,#104411);
#85616=AXIS2_PLACEMENT_3D('',#202011,#104415,#104416);
#85617=AXIS2_PLACEMENT_3D('',#202014,#104419,#104420);
#85618=AXIS2_PLACEMENT_3D('',#202023,#104425,#104426);
#85619=AXIS2_PLACEMENT_3D('',#202029,#104430,#104431);
#85620=AXIS2_PLACEMENT_3D('',#202035,#104435,#104436);
#85621=AXIS2_PLACEMENT_3D('',#202038,#104439,#104440);
#85622=AXIS2_PLACEMENT_3D('',#202047,#104445,#104446);
#85623=AXIS2_PLACEMENT_3D('',#202053,#104450,#104451);
#85624=AXIS2_PLACEMENT_3D('',#202059,#104455,#104456);
#85625=AXIS2_PLACEMENT_3D('',#202062,#104459,#104460);
#85626=AXIS2_PLACEMENT_3D('',#202071,#104465,#104466);
#85627=AXIS2_PLACEMENT_3D('',#202077,#104470,#104471);
#85628=AXIS2_PLACEMENT_3D('',#202083,#104475,#104476);
#85629=AXIS2_PLACEMENT_3D('',#202086,#104479,#104480);
#85630=AXIS2_PLACEMENT_3D('',#202095,#104485,#104486);
#85631=AXIS2_PLACEMENT_3D('',#202101,#104490,#104491);
#85632=AXIS2_PLACEMENT_3D('',#202107,#104495,#104496);
#85633=AXIS2_PLACEMENT_3D('',#202110,#104499,#104500);
#85634=AXIS2_PLACEMENT_3D('',#202119,#104505,#104506);
#85635=AXIS2_PLACEMENT_3D('',#202125,#104510,#104511);
#85636=AXIS2_PLACEMENT_3D('',#202131,#104515,#104516);
#85637=AXIS2_PLACEMENT_3D('',#202134,#104519,#104520);
#85638=AXIS2_PLACEMENT_3D('',#202143,#104525,#104526);
#85639=AXIS2_PLACEMENT_3D('',#202149,#104530,#104531);
#85640=AXIS2_PLACEMENT_3D('',#202155,#104535,#104536);
#85641=AXIS2_PLACEMENT_3D('',#202158,#104539,#104540);
#85642=AXIS2_PLACEMENT_3D('',#202167,#104545,#104546);
#85643=AXIS2_PLACEMENT_3D('',#202173,#104550,#104551);
#85644=AXIS2_PLACEMENT_3D('',#202179,#104555,#104556);
#85645=AXIS2_PLACEMENT_3D('',#202182,#104559,#104560);
#85646=AXIS2_PLACEMENT_3D('',#202191,#104565,#104566);
#85647=AXIS2_PLACEMENT_3D('',#202197,#104570,#104571);
#85648=AXIS2_PLACEMENT_3D('',#202203,#104575,#104576);
#85649=AXIS2_PLACEMENT_3D('',#202206,#104579,#104580);
#85650=AXIS2_PLACEMENT_3D('',#202215,#104585,#104586);
#85651=AXIS2_PLACEMENT_3D('',#202221,#104590,#104591);
#85652=AXIS2_PLACEMENT_3D('',#202227,#104595,#104596);
#85653=AXIS2_PLACEMENT_3D('',#202230,#104599,#104600);
#85654=AXIS2_PLACEMENT_3D('',#202239,#104605,#104606);
#85655=AXIS2_PLACEMENT_3D('',#202245,#104610,#104611);
#85656=AXIS2_PLACEMENT_3D('',#202251,#104615,#104616);
#85657=AXIS2_PLACEMENT_3D('',#202254,#104619,#104620);
#85658=AXIS2_PLACEMENT_3D('',#202263,#104625,#104626);
#85659=AXIS2_PLACEMENT_3D('',#202269,#104630,#104631);
#85660=AXIS2_PLACEMENT_3D('',#202275,#104635,#104636);
#85661=AXIS2_PLACEMENT_3D('',#202278,#104639,#104640);
#85662=AXIS2_PLACEMENT_3D('',#202287,#104645,#104646);
#85663=AXIS2_PLACEMENT_3D('',#202293,#104650,#104651);
#85664=AXIS2_PLACEMENT_3D('',#202299,#104655,#104656);
#85665=AXIS2_PLACEMENT_3D('',#202302,#104659,#104660);
#85666=AXIS2_PLACEMENT_3D('',#202311,#104665,#104666);
#85667=AXIS2_PLACEMENT_3D('',#202317,#104670,#104671);
#85668=AXIS2_PLACEMENT_3D('',#202323,#104675,#104676);
#85669=AXIS2_PLACEMENT_3D('',#202326,#104679,#104680);
#85670=AXIS2_PLACEMENT_3D('',#202335,#104685,#104686);
#85671=AXIS2_PLACEMENT_3D('',#202341,#104690,#104691);
#85672=AXIS2_PLACEMENT_3D('',#202347,#104695,#104696);
#85673=AXIS2_PLACEMENT_3D('',#202350,#104699,#104700);
#85674=AXIS2_PLACEMENT_3D('',#202359,#104705,#104706);
#85675=AXIS2_PLACEMENT_3D('',#202365,#104710,#104711);
#85676=AXIS2_PLACEMENT_3D('',#202371,#104715,#104716);
#85677=AXIS2_PLACEMENT_3D('',#202374,#104719,#104720);
#85678=AXIS2_PLACEMENT_3D('',#202383,#104725,#104726);
#85679=AXIS2_PLACEMENT_3D('',#202389,#104730,#104731);
#85680=AXIS2_PLACEMENT_3D('',#202395,#104735,#104736);
#85681=AXIS2_PLACEMENT_3D('',#202398,#104739,#104740);
#85682=AXIS2_PLACEMENT_3D('',#202407,#104745,#104746);
#85683=AXIS2_PLACEMENT_3D('',#202413,#104750,#104751);
#85684=AXIS2_PLACEMENT_3D('',#202419,#104755,#104756);
#85685=AXIS2_PLACEMENT_3D('',#202422,#104759,#104760);
#85686=AXIS2_PLACEMENT_3D('',#202431,#104765,#104766);
#85687=AXIS2_PLACEMENT_3D('',#202437,#104770,#104771);
#85688=AXIS2_PLACEMENT_3D('',#202443,#104775,#104776);
#85689=AXIS2_PLACEMENT_3D('',#202446,#104779,#104780);
#85690=AXIS2_PLACEMENT_3D('',#202455,#104785,#104786);
#85691=AXIS2_PLACEMENT_3D('',#202461,#104790,#104791);
#85692=AXIS2_PLACEMENT_3D('',#202467,#104795,#104796);
#85693=AXIS2_PLACEMENT_3D('',#202470,#104799,#104800);
#85694=AXIS2_PLACEMENT_3D('',#202479,#104805,#104806);
#85695=AXIS2_PLACEMENT_3D('',#202485,#104810,#104811);
#85696=AXIS2_PLACEMENT_3D('',#202491,#104815,#104816);
#85697=AXIS2_PLACEMENT_3D('',#202494,#104819,#104820);
#85698=AXIS2_PLACEMENT_3D('',#202503,#104825,#104826);
#85699=AXIS2_PLACEMENT_3D('',#202509,#104830,#104831);
#85700=AXIS2_PLACEMENT_3D('',#202515,#104835,#104836);
#85701=AXIS2_PLACEMENT_3D('',#202518,#104839,#104840);
#85702=AXIS2_PLACEMENT_3D('',#202527,#104845,#104846);
#85703=AXIS2_PLACEMENT_3D('',#202533,#104850,#104851);
#85704=AXIS2_PLACEMENT_3D('',#202539,#104855,#104856);
#85705=AXIS2_PLACEMENT_3D('',#202542,#104859,#104860);
#85706=AXIS2_PLACEMENT_3D('',#202551,#104865,#104866);
#85707=AXIS2_PLACEMENT_3D('',#202557,#104870,#104871);
#85708=AXIS2_PLACEMENT_3D('',#202563,#104875,#104876);
#85709=AXIS2_PLACEMENT_3D('',#202566,#104879,#104880);
#85710=AXIS2_PLACEMENT_3D('',#202575,#104885,#104886);
#85711=AXIS2_PLACEMENT_3D('',#202581,#104890,#104891);
#85712=AXIS2_PLACEMENT_3D('',#202587,#104895,#104896);
#85713=AXIS2_PLACEMENT_3D('',#202590,#104899,#104900);
#85714=AXIS2_PLACEMENT_3D('',#202599,#104905,#104906);
#85715=AXIS2_PLACEMENT_3D('',#202605,#104910,#104911);
#85716=AXIS2_PLACEMENT_3D('',#202611,#104915,#104916);
#85717=AXIS2_PLACEMENT_3D('',#202614,#104919,#104920);
#85718=AXIS2_PLACEMENT_3D('',#202623,#104925,#104926);
#85719=AXIS2_PLACEMENT_3D('',#202629,#104930,#104931);
#85720=AXIS2_PLACEMENT_3D('',#202635,#104935,#104936);
#85721=AXIS2_PLACEMENT_3D('',#202638,#104939,#104940);
#85722=AXIS2_PLACEMENT_3D('',#202647,#104945,#104946);
#85723=AXIS2_PLACEMENT_3D('',#202653,#104950,#104951);
#85724=AXIS2_PLACEMENT_3D('',#202659,#104955,#104956);
#85725=AXIS2_PLACEMENT_3D('',#202662,#104959,#104960);
#85726=AXIS2_PLACEMENT_3D('',#202671,#104965,#104966);
#85727=AXIS2_PLACEMENT_3D('',#202677,#104970,#104971);
#85728=AXIS2_PLACEMENT_3D('',#202683,#104975,#104976);
#85729=AXIS2_PLACEMENT_3D('',#202686,#104979,#104980);
#85730=AXIS2_PLACEMENT_3D('',#202695,#104985,#104986);
#85731=AXIS2_PLACEMENT_3D('',#202701,#104990,#104991);
#85732=AXIS2_PLACEMENT_3D('',#202707,#104995,#104996);
#85733=AXIS2_PLACEMENT_3D('',#202710,#104999,#105000);
#85734=AXIS2_PLACEMENT_3D('',#202719,#105005,#105006);
#85735=AXIS2_PLACEMENT_3D('',#202725,#105010,#105011);
#85736=AXIS2_PLACEMENT_3D('',#202731,#105015,#105016);
#85737=AXIS2_PLACEMENT_3D('',#202734,#105019,#105020);
#85738=AXIS2_PLACEMENT_3D('',#202743,#105025,#105026);
#85739=AXIS2_PLACEMENT_3D('',#202749,#105030,#105031);
#85740=AXIS2_PLACEMENT_3D('',#202755,#105035,#105036);
#85741=AXIS2_PLACEMENT_3D('',#202758,#105039,#105040);
#85742=AXIS2_PLACEMENT_3D('',#202767,#105045,#105046);
#85743=AXIS2_PLACEMENT_3D('',#202773,#105050,#105051);
#85744=AXIS2_PLACEMENT_3D('',#202779,#105055,#105056);
#85745=AXIS2_PLACEMENT_3D('',#202782,#105059,#105060);
#85746=AXIS2_PLACEMENT_3D('',#202791,#105065,#105066);
#85747=AXIS2_PLACEMENT_3D('',#202797,#105070,#105071);
#85748=AXIS2_PLACEMENT_3D('',#202803,#105075,#105076);
#85749=AXIS2_PLACEMENT_3D('',#202806,#105079,#105080);
#85750=AXIS2_PLACEMENT_3D('',#202815,#105085,#105086);
#85751=AXIS2_PLACEMENT_3D('',#202821,#105090,#105091);
#85752=AXIS2_PLACEMENT_3D('',#202827,#105095,#105096);
#85753=AXIS2_PLACEMENT_3D('',#202830,#105099,#105100);
#85754=AXIS2_PLACEMENT_3D('',#202839,#105105,#105106);
#85755=AXIS2_PLACEMENT_3D('',#202845,#105110,#105111);
#85756=AXIS2_PLACEMENT_3D('',#202851,#105115,#105116);
#85757=AXIS2_PLACEMENT_3D('',#202854,#105119,#105120);
#85758=AXIS2_PLACEMENT_3D('',#202863,#105125,#105126);
#85759=AXIS2_PLACEMENT_3D('',#202869,#105130,#105131);
#85760=AXIS2_PLACEMENT_3D('',#202875,#105135,#105136);
#85761=AXIS2_PLACEMENT_3D('',#202878,#105139,#105140);
#85762=AXIS2_PLACEMENT_3D('',#202887,#105145,#105146);
#85763=AXIS2_PLACEMENT_3D('',#202893,#105150,#105151);
#85764=AXIS2_PLACEMENT_3D('',#202899,#105155,#105156);
#85765=AXIS2_PLACEMENT_3D('',#202902,#105159,#105160);
#85766=AXIS2_PLACEMENT_3D('',#202911,#105165,#105166);
#85767=AXIS2_PLACEMENT_3D('',#202917,#105170,#105171);
#85768=AXIS2_PLACEMENT_3D('',#202923,#105175,#105176);
#85769=AXIS2_PLACEMENT_3D('',#202926,#105179,#105180);
#85770=AXIS2_PLACEMENT_3D('',#202935,#105185,#105186);
#85771=AXIS2_PLACEMENT_3D('',#202941,#105190,#105191);
#85772=AXIS2_PLACEMENT_3D('',#202947,#105195,#105196);
#85773=AXIS2_PLACEMENT_3D('',#202950,#105199,#105200);
#85774=AXIS2_PLACEMENT_3D('',#202959,#105205,#105206);
#85775=AXIS2_PLACEMENT_3D('',#202965,#105210,#105211);
#85776=AXIS2_PLACEMENT_3D('',#202971,#105215,#105216);
#85777=AXIS2_PLACEMENT_3D('',#202974,#105219,#105220);
#85778=AXIS2_PLACEMENT_3D('',#202983,#105225,#105226);
#85779=AXIS2_PLACEMENT_3D('',#202989,#105230,#105231);
#85780=AXIS2_PLACEMENT_3D('',#202995,#105235,#105236);
#85781=AXIS2_PLACEMENT_3D('',#202998,#105239,#105240);
#85782=AXIS2_PLACEMENT_3D('',#203007,#105245,#105246);
#85783=AXIS2_PLACEMENT_3D('',#203013,#105250,#105251);
#85784=AXIS2_PLACEMENT_3D('',#203019,#105255,#105256);
#85785=AXIS2_PLACEMENT_3D('',#203022,#105259,#105260);
#85786=AXIS2_PLACEMENT_3D('',#203031,#105265,#105266);
#85787=AXIS2_PLACEMENT_3D('',#203037,#105270,#105271);
#85788=AXIS2_PLACEMENT_3D('',#203043,#105275,#105276);
#85789=AXIS2_PLACEMENT_3D('',#203046,#105279,#105280);
#85790=AXIS2_PLACEMENT_3D('',#203055,#105285,#105286);
#85791=AXIS2_PLACEMENT_3D('',#203061,#105290,#105291);
#85792=AXIS2_PLACEMENT_3D('',#203067,#105295,#105296);
#85793=AXIS2_PLACEMENT_3D('',#203070,#105299,#105300);
#85794=AXIS2_PLACEMENT_3D('',#203079,#105305,#105306);
#85795=AXIS2_PLACEMENT_3D('',#203085,#105310,#105311);
#85796=AXIS2_PLACEMENT_3D('',#203091,#105315,#105316);
#85797=AXIS2_PLACEMENT_3D('',#203094,#105319,#105320);
#85798=AXIS2_PLACEMENT_3D('',#203103,#105325,#105326);
#85799=AXIS2_PLACEMENT_3D('',#203109,#105330,#105331);
#85800=AXIS2_PLACEMENT_3D('',#203115,#105335,#105336);
#85801=AXIS2_PLACEMENT_3D('',#203118,#105339,#105340);
#85802=AXIS2_PLACEMENT_3D('',#203127,#105345,#105346);
#85803=AXIS2_PLACEMENT_3D('',#203133,#105350,#105351);
#85804=AXIS2_PLACEMENT_3D('',#203139,#105355,#105356);
#85805=AXIS2_PLACEMENT_3D('',#203142,#105359,#105360);
#85806=AXIS2_PLACEMENT_3D('',#203151,#105365,#105366);
#85807=AXIS2_PLACEMENT_3D('',#203157,#105370,#105371);
#85808=AXIS2_PLACEMENT_3D('',#203163,#105375,#105376);
#85809=AXIS2_PLACEMENT_3D('',#203166,#105379,#105380);
#85810=AXIS2_PLACEMENT_3D('',#203175,#105385,#105386);
#85811=AXIS2_PLACEMENT_3D('',#203181,#105390,#105391);
#85812=AXIS2_PLACEMENT_3D('',#203187,#105395,#105396);
#85813=AXIS2_PLACEMENT_3D('',#203190,#105399,#105400);
#85814=AXIS2_PLACEMENT_3D('',#203199,#105405,#105406);
#85815=AXIS2_PLACEMENT_3D('',#203205,#105410,#105411);
#85816=AXIS2_PLACEMENT_3D('',#203211,#105415,#105416);
#85817=AXIS2_PLACEMENT_3D('',#203214,#105419,#105420);
#85818=AXIS2_PLACEMENT_3D('',#203223,#105425,#105426);
#85819=AXIS2_PLACEMENT_3D('',#203229,#105430,#105431);
#85820=AXIS2_PLACEMENT_3D('',#203235,#105435,#105436);
#85821=AXIS2_PLACEMENT_3D('',#203238,#105439,#105440);
#85822=AXIS2_PLACEMENT_3D('',#203247,#105445,#105446);
#85823=AXIS2_PLACEMENT_3D('',#203253,#105450,#105451);
#85824=AXIS2_PLACEMENT_3D('',#203259,#105455,#105456);
#85825=AXIS2_PLACEMENT_3D('',#203262,#105459,#105460);
#85826=AXIS2_PLACEMENT_3D('',#203271,#105465,#105466);
#85827=AXIS2_PLACEMENT_3D('',#203277,#105470,#105471);
#85828=AXIS2_PLACEMENT_3D('',#203283,#105475,#105476);
#85829=AXIS2_PLACEMENT_3D('',#203286,#105479,#105480);
#85830=AXIS2_PLACEMENT_3D('',#203295,#105485,#105486);
#85831=AXIS2_PLACEMENT_3D('',#203301,#105490,#105491);
#85832=AXIS2_PLACEMENT_3D('',#203307,#105495,#105496);
#85833=AXIS2_PLACEMENT_3D('',#203310,#105499,#105500);
#85834=AXIS2_PLACEMENT_3D('',#203319,#105505,#105506);
#85835=AXIS2_PLACEMENT_3D('',#203325,#105510,#105511);
#85836=AXIS2_PLACEMENT_3D('',#203331,#105515,#105516);
#85837=AXIS2_PLACEMENT_3D('',#203334,#105519,#105520);
#85838=AXIS2_PLACEMENT_3D('',#203343,#105525,#105526);
#85839=AXIS2_PLACEMENT_3D('',#203349,#105530,#105531);
#85840=AXIS2_PLACEMENT_3D('',#203355,#105535,#105536);
#85841=AXIS2_PLACEMENT_3D('',#203358,#105539,#105540);
#85842=AXIS2_PLACEMENT_3D('',#203367,#105545,#105546);
#85843=AXIS2_PLACEMENT_3D('',#203373,#105550,#105551);
#85844=AXIS2_PLACEMENT_3D('',#203379,#105555,#105556);
#85845=AXIS2_PLACEMENT_3D('',#203382,#105559,#105560);
#85846=AXIS2_PLACEMENT_3D('',#203391,#105565,#105566);
#85847=AXIS2_PLACEMENT_3D('',#203397,#105570,#105571);
#85848=AXIS2_PLACEMENT_3D('',#203403,#105575,#105576);
#85849=AXIS2_PLACEMENT_3D('',#203406,#105579,#105580);
#85850=AXIS2_PLACEMENT_3D('',#203415,#105585,#105586);
#85851=AXIS2_PLACEMENT_3D('',#203421,#105590,#105591);
#85852=AXIS2_PLACEMENT_3D('',#203427,#105595,#105596);
#85853=AXIS2_PLACEMENT_3D('',#203430,#105599,#105600);
#85854=AXIS2_PLACEMENT_3D('',#203439,#105605,#105606);
#85855=AXIS2_PLACEMENT_3D('',#203445,#105610,#105611);
#85856=AXIS2_PLACEMENT_3D('',#203451,#105615,#105616);
#85857=AXIS2_PLACEMENT_3D('',#203454,#105619,#105620);
#85858=AXIS2_PLACEMENT_3D('',#203463,#105625,#105626);
#85859=AXIS2_PLACEMENT_3D('',#203469,#105630,#105631);
#85860=AXIS2_PLACEMENT_3D('',#203475,#105635,#105636);
#85861=AXIS2_PLACEMENT_3D('',#203478,#105639,#105640);
#85862=AXIS2_PLACEMENT_3D('',#203487,#105645,#105646);
#85863=AXIS2_PLACEMENT_3D('',#203493,#105650,#105651);
#85864=AXIS2_PLACEMENT_3D('',#203499,#105655,#105656);
#85865=AXIS2_PLACEMENT_3D('',#203502,#105659,#105660);
#85866=AXIS2_PLACEMENT_3D('',#203511,#105665,#105666);
#85867=AXIS2_PLACEMENT_3D('',#203517,#105670,#105671);
#85868=AXIS2_PLACEMENT_3D('',#203523,#105675,#105676);
#85869=AXIS2_PLACEMENT_3D('',#203526,#105679,#105680);
#85870=AXIS2_PLACEMENT_3D('',#203535,#105685,#105686);
#85871=AXIS2_PLACEMENT_3D('',#203541,#105690,#105691);
#85872=AXIS2_PLACEMENT_3D('',#203547,#105695,#105696);
#85873=AXIS2_PLACEMENT_3D('',#203550,#105699,#105700);
#85874=AXIS2_PLACEMENT_3D('',#203559,#105705,#105706);
#85875=AXIS2_PLACEMENT_3D('',#203565,#105710,#105711);
#85876=AXIS2_PLACEMENT_3D('',#203571,#105715,#105716);
#85877=AXIS2_PLACEMENT_3D('',#203574,#105719,#105720);
#85878=AXIS2_PLACEMENT_3D('',#203583,#105725,#105726);
#85879=AXIS2_PLACEMENT_3D('',#203589,#105730,#105731);
#85880=AXIS2_PLACEMENT_3D('',#203595,#105735,#105736);
#85881=AXIS2_PLACEMENT_3D('',#203598,#105739,#105740);
#85882=AXIS2_PLACEMENT_3D('',#203607,#105745,#105746);
#85883=AXIS2_PLACEMENT_3D('',#203613,#105750,#105751);
#85884=AXIS2_PLACEMENT_3D('',#203619,#105755,#105756);
#85885=AXIS2_PLACEMENT_3D('',#203622,#105759,#105760);
#85886=AXIS2_PLACEMENT_3D('',#203631,#105765,#105766);
#85887=AXIS2_PLACEMENT_3D('',#203637,#105770,#105771);
#85888=AXIS2_PLACEMENT_3D('',#203643,#105775,#105776);
#85889=AXIS2_PLACEMENT_3D('',#203646,#105779,#105780);
#85890=AXIS2_PLACEMENT_3D('',#203655,#105785,#105786);
#85891=AXIS2_PLACEMENT_3D('',#203661,#105790,#105791);
#85892=AXIS2_PLACEMENT_3D('',#203667,#105795,#105796);
#85893=AXIS2_PLACEMENT_3D('',#203670,#105799,#105800);
#85894=AXIS2_PLACEMENT_3D('',#203679,#105805,#105806);
#85895=AXIS2_PLACEMENT_3D('',#203685,#105810,#105811);
#85896=AXIS2_PLACEMENT_3D('',#203691,#105815,#105816);
#85897=AXIS2_PLACEMENT_3D('',#203694,#105819,#105820);
#85898=AXIS2_PLACEMENT_3D('',#203703,#105825,#105826);
#85899=AXIS2_PLACEMENT_3D('',#203709,#105830,#105831);
#85900=AXIS2_PLACEMENT_3D('',#203715,#105835,#105836);
#85901=AXIS2_PLACEMENT_3D('',#203718,#105839,#105840);
#85902=AXIS2_PLACEMENT_3D('',#203727,#105845,#105846);
#85903=AXIS2_PLACEMENT_3D('',#203733,#105850,#105851);
#85904=AXIS2_PLACEMENT_3D('',#203739,#105855,#105856);
#85905=AXIS2_PLACEMENT_3D('',#203742,#105859,#105860);
#85906=AXIS2_PLACEMENT_3D('',#203751,#105865,#105866);
#85907=AXIS2_PLACEMENT_3D('',#203757,#105870,#105871);
#85908=AXIS2_PLACEMENT_3D('',#203763,#105875,#105876);
#85909=AXIS2_PLACEMENT_3D('',#203766,#105879,#105880);
#85910=AXIS2_PLACEMENT_3D('',#203775,#105885,#105886);
#85911=AXIS2_PLACEMENT_3D('',#203781,#105890,#105891);
#85912=AXIS2_PLACEMENT_3D('',#203787,#105895,#105896);
#85913=AXIS2_PLACEMENT_3D('',#203790,#105899,#105900);
#85914=AXIS2_PLACEMENT_3D('',#203799,#105905,#105906);
#85915=AXIS2_PLACEMENT_3D('',#203805,#105910,#105911);
#85916=AXIS2_PLACEMENT_3D('',#203811,#105915,#105916);
#85917=AXIS2_PLACEMENT_3D('',#203814,#105919,#105920);
#85918=AXIS2_PLACEMENT_3D('',#203823,#105925,#105926);
#85919=AXIS2_PLACEMENT_3D('',#203829,#105930,#105931);
#85920=AXIS2_PLACEMENT_3D('',#203835,#105935,#105936);
#85921=AXIS2_PLACEMENT_3D('',#203838,#105939,#105940);
#85922=AXIS2_PLACEMENT_3D('',#203847,#105945,#105946);
#85923=AXIS2_PLACEMENT_3D('',#203853,#105950,#105951);
#85924=AXIS2_PLACEMENT_3D('',#203859,#105955,#105956);
#85925=AXIS2_PLACEMENT_3D('',#203862,#105959,#105960);
#85926=AXIS2_PLACEMENT_3D('',#203871,#105965,#105966);
#85927=AXIS2_PLACEMENT_3D('',#203877,#105970,#105971);
#85928=AXIS2_PLACEMENT_3D('',#203883,#105975,#105976);
#85929=AXIS2_PLACEMENT_3D('',#203886,#105979,#105980);
#85930=AXIS2_PLACEMENT_3D('',#203887,#105981,#105982);
#85931=AXIS2_PLACEMENT_3D('',#203896,#105987,#105988);
#85932=AXIS2_PLACEMENT_3D('',#203902,#105992,#105993);
#85933=AXIS2_PLACEMENT_3D('',#203906,#105996,#105997);
#85934=AXIS2_PLACEMENT_3D('',#203910,#106000,#106001);
#85935=AXIS2_PLACEMENT_3D('',#203912,#106003,#106004);
#85936=AXIS2_PLACEMENT_3D('',#203913,#106005,#106006);
#85937=AXIS2_PLACEMENT_3D('',#203914,#106007,#106008);
#85938=AXIS2_PLACEMENT_3D('',#203916,#106010,#106011);
#85939=AXIS2_PLACEMENT_3D('',#203918,#106013,#106014);
#85940=AXIS2_PLACEMENT_3D('',#203920,#106016,#106017);
#85941=AXIS2_PLACEMENT_3D('',#203922,#106019,#106020);
#85942=AXIS2_PLACEMENT_3D('',#203923,#106021,#106022);
#85943=AXIS2_PLACEMENT_3D('',#203924,#106023,#106024);
#85944=AXIS2_PLACEMENT_3D('',#203926,#106026,#106027);
#85945=AXIS2_PLACEMENT_3D('',#203928,#106029,#106030);
#85946=AXIS2_PLACEMENT_3D('',#203930,#106032,#106033);
#85947=AXIS2_PLACEMENT_3D('',#203932,#106035,#106036);
#85948=AXIS2_PLACEMENT_3D('',#203933,#106037,#106038);
#85949=AXIS2_PLACEMENT_3D('',#203934,#106039,#106040);
#85950=AXIS2_PLACEMENT_3D('',#203936,#106041,#106042);
#85951=AXIS2_PLACEMENT_3D('',#203937,#106043,#106044);
#85952=AXIS2_PLACEMENT_3D('',#203940,#106045,#106046);
#85953=AXIS2_PLACEMENT_3D('',#203942,#106047,#106048);
#85954=AXIS2_PLACEMENT_3D('',#203944,#106049,#106050);
#85955=AXIS2_PLACEMENT_3D('',#203945,#106051,#106052);
#85956=AXIS2_PLACEMENT_3D('',#203946,#106053,#106054);
#85957=AXIS2_PLACEMENT_3D('',#203951,#106057,#106058);
#85958=AXIS2_PLACEMENT_3D('',#203952,#106059,#106060);
#85959=AXIS2_PLACEMENT_3D('',#203955,#106062,#106063);
#85960=AXIS2_PLACEMENT_3D('',#203956,#106064,#106065);
#85961=AXIS2_PLACEMENT_3D('',#203959,#106067,#106068);
#85962=AXIS2_PLACEMENT_3D('',#203960,#106069,#106070);
#85963=AXIS2_PLACEMENT_3D('',#203961,#106071,#106072);
#85964=AXIS2_PLACEMENT_3D('',#203962,#106073,#106074);
#85965=AXIS2_PLACEMENT_3D('',#203964,#106075,#106076);
#85966=AXIS2_PLACEMENT_3D('',#203965,#106077,#106078);
#85967=AXIS2_PLACEMENT_3D('',#203966,#106079,#106080);
#85968=AXIS2_PLACEMENT_3D('',#203967,#106081,#106082);
#85969=AXIS2_PLACEMENT_3D('',#204039,#106085,#106086);
#85970=AXIS2_PLACEMENT_3D('',#204040,#106087,#106088);
#85971=AXIS2_PLACEMENT_3D('',#204138,#106090,#106091);
#85972=AXIS2_PLACEMENT_3D('',#204280,#106093,#106094);
#85973=AXIS2_PLACEMENT_3D('',#204414,#106096,#106097);
#85974=AXIS2_PLACEMENT_3D('',#204551,#106099,#106100);
#85975=AXIS2_PLACEMENT_3D('',#204690,#106102,#106103);
#85976=AXIS2_PLACEMENT_3D('',#204828,#106105,#106106);
#85977=AXIS2_PLACEMENT_3D('',#204964,#106108,#106109);
#85978=AXIS2_PLACEMENT_3D('',#205093,#106111,#106112);
#85979=AXIS2_PLACEMENT_3D('',#205106,#106114,#106115);
#85980=AXIS2_PLACEMENT_3D('',#205107,#106116,#106117);
#85981=AXIS2_PLACEMENT_3D('',#205176,#106119,#106120);
#85982=AXIS2_PLACEMENT_3D('',#205241,#106121,#106122);
#85983=AXIS2_PLACEMENT_3D('',#205384,#106124,#106125);
#85984=AXIS2_PLACEMENT_3D('',#205549,#106127,#106128);
#85985=AXIS2_PLACEMENT_3D('',#205709,#106130,#106131);
#85986=AXIS2_PLACEMENT_3D('',#205876,#106133,#106134);
#85987=AXIS2_PLACEMENT_3D('',#206041,#106136,#106137);
#85988=AXIS2_PLACEMENT_3D('',#206201,#106139,#106140);
#85989=AXIS2_PLACEMENT_3D('',#206204,#106141,#106142);
#85990=AXIS2_PLACEMENT_3D('',#206205,#106143,#106144);
#85991=AXIS2_PLACEMENT_3D('',#206301,#106148,#106149);
#85992=AXIS2_PLACEMENT_3D('',#206357,#106151,#106152);
#85993=AXIS2_PLACEMENT_3D('',#206416,#106153,#106154);
#85994=AXIS2_PLACEMENT_3D('',#206452,#106157,#106158);
#85995=AXIS2_PLACEMENT_3D('',#206586,#106160,#106161);
#85996=AXIS2_PLACEMENT_3D('',#206734,#106163,#106164);
#85997=AXIS2_PLACEMENT_3D('',#206878,#106166,#106167);
#85998=AXIS2_PLACEMENT_3D('',#206906,#106170,#106171);
#85999=AXIS2_PLACEMENT_3D('',#207040,#106173,#106174);
#86000=AXIS2_PLACEMENT_3D('',#207168,#106176,#106177);
#86001=AXIS2_PLACEMENT_3D('',#207314,#106179,#106180);
#86002=AXIS2_PLACEMENT_3D('',#207330,#106182,#106183);
#86003=AXIS2_PLACEMENT_3D('',#207331,#106184,#106185);
#86004=AXIS2_PLACEMENT_3D('',#207411,#106187,#106188);
#86005=AXIS2_PLACEMENT_3D('',#207484,#106189,#106190);
#86006=AXIS2_PLACEMENT_3D('',#207642,#106192,#106193);
#86007=AXIS2_PLACEMENT_3D('',#207800,#106195,#106196);
#86008=AXIS2_PLACEMENT_3D('',#207858,#106199,#106200);
#86009=AXIS2_PLACEMENT_3D('',#208016,#106202,#106203);
#86010=AXIS2_PLACEMENT_3D('',#208178,#106205,#106206);
#86011=AXIS2_PLACEMENT_3D('',#208336,#106208,#106209);
#86012=AXIS2_PLACEMENT_3D('',#208341,#106211,#106212);
#86013=AXIS2_PLACEMENT_3D('',#208414,#106213,#106214);
#86014=AXIS2_PLACEMENT_3D('',#208452,#106215,#106216);
#86015=AXIS2_PLACEMENT_3D('',#208466,#106217,#106218);
#86016=AXIS2_PLACEMENT_3D('',#208467,#106219,#106220);
#86017=AXIS2_PLACEMENT_3D('',#208469,#106221,#106222);
#86018=AXIS2_PLACEMENT_3D('',#208472,#106224,#106225);
#86019=AXIS2_PLACEMENT_3D('',#208473,#106226,#106227);
#86020=AXIS2_PLACEMENT_3D('',#208490,#106228,#106229);
#86021=AXIS2_PLACEMENT_3D('',#208525,#106230,#106231);
#86022=AXIS2_PLACEMENT_3D('',#208558,#106232,#106233);
#86023=AXIS2_PLACEMENT_3D('',#208592,#106236,#106237);
#86024=AXIS2_PLACEMENT_3D('',#208594,#106238,#106239);
#86025=AXIS2_PLACEMENT_3D('',#208725,#106240,#106241);
#86026=AXIS2_PLACEMENT_3D('',#208846,#106242,#106243);
#86027=AXIS2_PLACEMENT_3D('',#209644,#106247,#106248);
#86028=AXIS2_PLACEMENT_3D('',#210311,#106251,#106252);
#86029=AXIS2_PLACEMENT_3D('',#210316,#106254,#106255);
#86030=AXIS2_PLACEMENT_3D('',#210317,#106256,#106257);
#86031=AXIS2_PLACEMENT_3D('',#210318,#106258,#106259);
#86032=AXIS2_PLACEMENT_3D('',#210319,#106260,#106261);
#86033=AXIS2_PLACEMENT_3D('',#210320,#106262,#106263);
#86034=AXIS2_PLACEMENT_3D('',#210322,#106264,#106265);
#86035=AXIS2_PLACEMENT_3D('',#210333,#106266,#106267);
#86036=AXIS2_PLACEMENT_3D('',#211402,#106270,#106271);
#86037=AXIS2_PLACEMENT_3D('',#212210,#106274,#106275);
#86038=AXIS2_PLACEMENT_3D('',#212631,#106277,#106278);
#86039=AXIS2_PLACEMENT_3D('',#212634,#106279,#106280);
#86040=AXIS2_PLACEMENT_3D('',#212637,#106282,#106283);
#86041=AXIS2_PLACEMENT_3D('',#212638,#106284,#106285);
#86042=AXIS2_PLACEMENT_3D('',#212639,#106286,#106287);
#86043=AXIS2_PLACEMENT_3D('',#212642,#106289,#106290);
#86044=AXIS2_PLACEMENT_3D('',#212643,#106291,#106292);
#86045=AXIS2_PLACEMENT_3D('',#212644,#106293,#106294);
#86046=AXIS2_PLACEMENT_3D('',#212645,#106295,#106296);
#86047=AXIS2_PLACEMENT_3D('',#212647,#106297,#106298);
#86048=AXIS2_PLACEMENT_3D('',#212648,#106299,#106300);
#86049=AXIS2_PLACEMENT_3D('',#212651,#106302,#106303);
#86050=AXIS2_PLACEMENT_3D('',#212652,#106304,#106305);
#86051=AXIS2_PLACEMENT_3D('',#212655,#106307,#106308);
#86052=AXIS2_PLACEMENT_3D('',#212656,#106309,#106310);
#86053=AXIS2_PLACEMENT_3D('',#212663,#106311,#106312);
#86054=AXIS2_PLACEMENT_3D('',#212772,#106313,#106314);
#86055=AXIS2_PLACEMENT_3D('',#212784,#106315,#106316);
#86056=AXIS2_PLACEMENT_3D('',#212785,#106317,#106318);
#86057=AXIS2_PLACEMENT_3D('',#212786,#106319,#106320);
#86058=AXIS2_PLACEMENT_3D('',#212788,#106322,#106323);
#86059=AXIS2_PLACEMENT_3D('',#212789,#106324,#106325);
#86060=AXIS2_PLACEMENT_3D('',#212790,#106326,#106327);
#86061=AXIS2_PLACEMENT_3D('',#212862,#106330,#106331);
#86062=AXIS2_PLACEMENT_3D('',#212863,#106332,#106333);
#86063=AXIS2_PLACEMENT_3D('',#212959,#106335,#106336);
#86064=AXIS2_PLACEMENT_3D('',#213099,#106338,#106339);
#86065=AXIS2_PLACEMENT_3D('',#213235,#106341,#106342);
#86066=AXIS2_PLACEMENT_3D('',#213378,#106344,#106345);
#86067=AXIS2_PLACEMENT_3D('',#213515,#106347,#106348);
#86068=AXIS2_PLACEMENT_3D('',#213651,#106350,#106351);
#86069=AXIS2_PLACEMENT_3D('',#213787,#106353,#106354);
#86070=AXIS2_PLACEMENT_3D('',#213914,#106356,#106357);
#86071=AXIS2_PLACEMENT_3D('',#213927,#106359,#106360);
#86072=AXIS2_PLACEMENT_3D('',#213928,#106361,#106362);
#86073=AXIS2_PLACEMENT_3D('',#213997,#106364,#106365);
#86074=AXIS2_PLACEMENT_3D('',#214062,#106366,#106367);
#86075=AXIS2_PLACEMENT_3D('',#214203,#106369,#106370);
#86076=AXIS2_PLACEMENT_3D('',#214368,#106372,#106373);
#86077=AXIS2_PLACEMENT_3D('',#214526,#106375,#106376);
#86078=AXIS2_PLACEMENT_3D('',#214693,#106378,#106379);
#86079=AXIS2_PLACEMENT_3D('',#214858,#106381,#106382);
#86080=AXIS2_PLACEMENT_3D('',#215018,#106384,#106385);
#86081=AXIS2_PLACEMENT_3D('',#215021,#106386,#106387);
#86082=AXIS2_PLACEMENT_3D('',#215022,#106388,#106389);
#86083=AXIS2_PLACEMENT_3D('',#215118,#106393,#106394);
#86084=AXIS2_PLACEMENT_3D('',#215174,#106396,#106397);
#86085=AXIS2_PLACEMENT_3D('',#215233,#106398,#106399);
#86086=AXIS2_PLACEMENT_3D('',#215269,#106402,#106403);
#86087=AXIS2_PLACEMENT_3D('',#215411,#106405,#106406);
#86088=AXIS2_PLACEMENT_3D('',#215561,#106408,#106409);
#86089=AXIS2_PLACEMENT_3D('',#215707,#106411,#106412);
#86090=AXIS2_PLACEMENT_3D('',#215735,#106415,#106416);
#86091=AXIS2_PLACEMENT_3D('',#215875,#106418,#106419);
#86092=AXIS2_PLACEMENT_3D('',#216011,#106421,#106422);
#86093=AXIS2_PLACEMENT_3D('',#216149,#106424,#106425);
#86094=AXIS2_PLACEMENT_3D('',#216165,#106427,#106428);
#86095=AXIS2_PLACEMENT_3D('',#216166,#106429,#106430);
#86096=AXIS2_PLACEMENT_3D('',#216246,#106432,#106433);
#86097=AXIS2_PLACEMENT_3D('',#216319,#106434,#106435);
#86098=AXIS2_PLACEMENT_3D('',#216477,#106437,#106438);
#86099=AXIS2_PLACEMENT_3D('',#216635,#106440,#106441);
#86100=AXIS2_PLACEMENT_3D('',#216693,#106444,#106445);
#86101=AXIS2_PLACEMENT_3D('',#216853,#106447,#106448);
#86102=AXIS2_PLACEMENT_3D('',#217013,#106450,#106451);
#86103=AXIS2_PLACEMENT_3D('',#217173,#106453,#106454);
#86104=AXIS2_PLACEMENT_3D('',#217178,#106456,#106457);
#86105=AXIS2_PLACEMENT_3D('',#217251,#106458,#106459);
#86106=AXIS2_PLACEMENT_3D('',#217289,#106460,#106461);
#86107=AXIS2_PLACEMENT_3D('',#217303,#106462,#106463);
#86108=AXIS2_PLACEMENT_3D('',#217304,#106464,#106465);
#86109=AXIS2_PLACEMENT_3D('',#217306,#106466,#106467);
#86110=AXIS2_PLACEMENT_3D('',#217309,#106469,#106470);
#86111=AXIS2_PLACEMENT_3D('',#217310,#106471,#106472);
#86112=AXIS2_PLACEMENT_3D('',#217327,#106473,#106474);
#86113=AXIS2_PLACEMENT_3D('',#217362,#106475,#106476);
#86114=AXIS2_PLACEMENT_3D('',#217395,#106477,#106478);
#86115=AXIS2_PLACEMENT_3D('',#217429,#106481,#106482);
#86116=AXIS2_PLACEMENT_3D('',#217431,#106483,#106484);
#86117=AXIS2_PLACEMENT_3D('',#217560,#106485,#106486);
#86118=AXIS2_PLACEMENT_3D('',#217673,#106487,#106488);
#86119=AXIS2_PLACEMENT_3D('',#218475,#106492,#106493);
#86120=AXIS2_PLACEMENT_3D('',#219142,#106496,#106497);
#86121=AXIS2_PLACEMENT_3D('',#219147,#106499,#106500);
#86122=AXIS2_PLACEMENT_3D('',#219148,#106501,#106502);
#86123=AXIS2_PLACEMENT_3D('',#219149,#106503,#106504);
#86124=AXIS2_PLACEMENT_3D('',#219150,#106505,#106506);
#86125=AXIS2_PLACEMENT_3D('',#219151,#106507,#106508);
#86126=AXIS2_PLACEMENT_3D('',#219153,#106509,#106510);
#86127=AXIS2_PLACEMENT_3D('',#219164,#106511,#106512);
#86128=AXIS2_PLACEMENT_3D('',#220233,#106515,#106516);
#86129=AXIS2_PLACEMENT_3D('',#221041,#106519,#106520);
#86130=AXIS2_PLACEMENT_3D('',#221462,#106522,#106523);
#86131=AXIS2_PLACEMENT_3D('',#221465,#106524,#106525);
#86132=AXIS2_PLACEMENT_3D('',#221468,#106527,#106528);
#86133=AXIS2_PLACEMENT_3D('',#221469,#106529,#106530);
#86134=AXIS2_PLACEMENT_3D('',#221470,#106531,#106532);
#86135=AXIS2_PLACEMENT_3D('',#221473,#106534,#106535);
#86136=AXIS2_PLACEMENT_3D('',#221474,#106536,#106537);
#86137=AXIS2_PLACEMENT_3D('',#221475,#106538,#106539);
#86138=AXIS2_PLACEMENT_3D('',#221476,#106540,#106541);
#86139=AXIS2_PLACEMENT_3D('',#221478,#106542,#106543);
#86140=AXIS2_PLACEMENT_3D('',#221479,#106544,#106545);
#86141=AXIS2_PLACEMENT_3D('',#221482,#106547,#106548);
#86142=AXIS2_PLACEMENT_3D('',#221483,#106549,#106550);
#86143=AXIS2_PLACEMENT_3D('',#221486,#106552,#106553);
#86144=AXIS2_PLACEMENT_3D('',#221487,#106554,#106555);
#86145=AXIS2_PLACEMENT_3D('',#221494,#106556,#106557);
#86146=AXIS2_PLACEMENT_3D('',#221603,#106558,#106559);
#86147=AXIS2_PLACEMENT_3D('',#221615,#106560,#106561);
#86148=AXIS2_PLACEMENT_3D('',#221616,#106562,#106563);
#86149=AXIS2_PLACEMENT_3D('',#221617,#106564,#106565);
#86150=AXIS2_PLACEMENT_3D('',#221619,#106567,#106568);
#86151=AXIS2_PLACEMENT_3D('',#221620,#106569,#106570);
#86152=AXIS2_PLACEMENT_3D('',#221621,#106571,#106572);
#86153=AXIS2_PLACEMENT_3D('',#221622,#106573,#106574);
#86154=AXIS2_PLACEMENT_3D('',#221623,#106575,#106576);
#86155=AXIS2_PLACEMENT_3D('',#221624,#106577,#106578);
#86156=AXIS2_PLACEMENT_3D('',#221625,#106579,#106580);
#86157=AXIS2_PLACEMENT_3D('',#221626,#106581,#106582);
#86158=AXIS2_PLACEMENT_3D('',#221627,#106583,#106584);
#86159=AXIS2_PLACEMENT_3D('',#221628,#106585,#106586);
#86160=AXIS2_PLACEMENT_3D('',#221629,#106587,#106588);
#86161=AXIS2_PLACEMENT_3D('',#221630,#106589,#106590);
#86162=AXIS2_PLACEMENT_3D('',#221631,#106591,#106592);
#86163=AXIS2_PLACEMENT_3D('',#221632,#106593,#106594);
#86164=DIRECTION('axis',(0.,0.,1.));
#86165=DIRECTION('refdir',(1.,0.,0.));
#86166=DIRECTION('axis',(0.,0.,1.));
#86167=DIRECTION('refdir',(1.,0.,0.));
#86168=DIRECTION('center_axis',(0.156610083413696,-0.431983230632625,0.888180032552723));
#86169=DIRECTION('ref_axis',(0.961785334650907,0.271198694721067,-0.037686045587615));
#86170=DIRECTION('center_axis',(0.,-1.,0.));
#86171=DIRECTION('ref_axis',(-0.173648177666903,0.,-0.984807753012213));
#86172=DIRECTION('center_axis',(-0.156610100625892,0.431983257504582,-0.888180016448061));
#86173=DIRECTION('ref_axis',(0.338848737580694,0.868195889116037,0.362515421964341));
#86174=DIRECTION('center_axis',(0.940152247861526,-0.297712383088708,-0.165774207271705));
#86175=DIRECTION('ref_axis',(-0.173647839019125,1.10267237741349E-6,-0.984807812724276));
#86176=DIRECTION('center_axis',(-0.984807753012213,0.,0.173648177666902));
#86177=DIRECTION('ref_axis',(0.,1.,0.));
#86178=DIRECTION('',(-2.025323837648E-10,-1.,-2.189203733894E-10));
#86179=DIRECTION('',(0.173648177666902,0.,0.984807753012213));
#86180=DIRECTION('center_axis',(-0.984807753040743,-3.31556822456762E-10,
0.173648177505103));
#86181=DIRECTION('ref_axis',(0.155995631336126,-0.439294647618469,0.884695187947696));
#86182=DIRECTION('center_axis',(0.,-1.,0.));
#86183=DIRECTION('ref_axis',(0.173648177666903,0.,0.984807753012213));
#86184=DIRECTION('center_axis',(0.173648177666902,0.,0.984807753012213));
#86185=DIRECTION('ref_axis',(0.984807753012213,0.,-0.173648177666902));
#86186=DIRECTION('center_axis',(0.156610200040416,0.431982195134571,0.888180515621694));
#86187=DIRECTION('ref_axis',(0.961785732595754,-0.271197107788908,-0.0376873095641012));
#86188=DIRECTION('center_axis',(-0.940152146377266,-0.297712713531889,0.165774189377293));
#86189=DIRECTION('ref_axis',(-0.173647969304453,-6.78449113130987E-7,-0.984807789751878));
#86190=DIRECTION('center_axis',(-0.156610083777503,-0.4319834600727,-0.888179920895998));
#86191=DIRECTION('ref_axis',(0.98480775277219,2.88567290812795E-9,-0.173648179028143));
#86192=DIRECTION('center_axis',(0.,-1.,0.));
#86193=DIRECTION('ref_axis',(-0.173648177666903,0.,-0.984807753012213));
#86194=DIRECTION('center_axis',(-0.984807753012213,0.,0.173648177666902));
#86195=DIRECTION('ref_axis',(0.,1.,0.));
#86196=DIRECTION('center_axis',(-0.984807752957808,-6.43089184032011E-10,
0.173648177975449));
#86197=DIRECTION('ref_axis',(0.156008598329541,0.439141908993185,0.884768727415856));
#86198=DIRECTION('',(-0.173648177666902,0.,-0.984807753012213));
#86199=DIRECTION('',(-2.025323837648E-10,-1.,-2.189203733894E-10));
#86200=DIRECTION('center_axis',(0.,-1.,0.));
#86201=DIRECTION('ref_axis',(0.173648177666903,0.,0.984807753012213));
#86202=DIRECTION('center_axis',(0.173648177666902,0.,0.984807753012213));
#86203=DIRECTION('ref_axis',(0.984807753012213,0.,-0.173648177666902));
#86204=DIRECTION('center_axis',(0.173648177666902,0.,0.984807753012213));
#86205=DIRECTION('ref_axis',(0.984807753012213,0.,-0.173648177666902));
#86206=DIRECTION('center_axis',(-0.173648177666902,0.,-0.984807753012213));
#86207=DIRECTION('ref_axis',(0.984807753012213,0.,-0.173648177666902));
#86208=DIRECTION('',(-0.173648177666902,0.,-0.984807753012213));
#86209=DIRECTION('center_axis',(0.0391216869526731,-0.999210589338024,-0.00690592243911207));
#86210=DIRECTION('ref_axis',(-0.99913461352629,-0.0390191476249176,-0.0144059075484885));
#86211=DIRECTION('center_axis',(-0.984807753012213,0.,0.173648177666903));
#86212=DIRECTION('ref_axis',(0.173648177666903,0.,0.984807753012213));
#86213=DIRECTION('',(-0.984807631231399,0.,0.1736488683188));
#86214=DIRECTION('',(-0.984809724314531,4.00369164637112E-9,0.173636997484805));
#86215=DIRECTION('center_axis',(0.,1.,0.));
#86216=DIRECTION('ref_axis',(1.,0.,0.));
#86217=DIRECTION('center_axis',(-0.810842955514487,0.459818666371144,0.362078024117999));
#86218=DIRECTION('ref_axis',(0.0796317671110352,0.699582071269321,-0.710101195059761));
#86219=DIRECTION('center_axis',(0.173648177666902,0.,0.984807753012213));
#86220=DIRECTION('ref_axis',(0.,-1.,0.));
#86221=DIRECTION('center_axis',(0.173648177666902,0.,0.984807753012213));
#86222=DIRECTION('ref_axis',(0.984807753012213,0.,-0.173648177666902));
#86223=DIRECTION('center_axis',(-0.173648177666902,0.,-0.984807753012213));
#86224=DIRECTION('ref_axis',(0.984807753012213,0.,-0.173648177666902));
#86225=DIRECTION('',(0.173648177666902,0.,0.984807753012213));
#86226=DIRECTION('center_axis',(0.0387475933097257,0.999225688321113,-0.00682992034369552));
#86227=DIRECTION('ref_axis',(-0.999147598170087,0.0386453691656854,-0.0145124950643757));
#86228=DIRECTION('center_axis',(0.984807753012213,0.,-0.173648177666902));
#86229=DIRECTION('ref_axis',(-0.173648177666902,0.,-0.984807753012213));
#86230=DIRECTION('center_axis',(0.,-1.,0.));
#86231=DIRECTION('ref_axis',(0.,0.,-1.));
#86232=DIRECTION('',(0.984811647878971,1.54338751793195E-8,-0.173626087331095));
#86233=DIRECTION('center_axis',(0.984807753012213,0.,-0.173648177666902));
#86234=DIRECTION('ref_axis',(0.173648177666902,0.,0.984807753012213));
#86235=DIRECTION('',(0.984807759252478,-3.52789443014592E-8,-0.173648142276596));
#86236=DIRECTION('center_axis',(0.810782065545516,0.460194129063917,-0.361737205392049));
#86237=DIRECTION('ref_axis',(0.0802095373079066,-0.699502947700354,-0.710114114972634));
#86238=DIRECTION('center_axis',(0.173648177666902,0.,0.984807753012213));
#86239=DIRECTION('ref_axis',(0.,-1.,0.));
#86240=DIRECTION('center_axis',(-1.,0.,0.));
#86241=DIRECTION('ref_axis',(0.,1.,0.));
#86242=DIRECTION('',(-1.,0.,0.));
#86243=DIRECTION('center_axis',(-1.,0.,0.));
#86244=DIRECTION('ref_axis',(0.,0.139931005087302,0.990161256470509));
#86245=DIRECTION('center_axis',(-1.,0.,0.));
#86246=DIRECTION('ref_axis',(0.,1.,0.));
#86247=DIRECTION('',(-1.,0.,0.));
#86248=DIRECTION('center_axis',(-1.,0.,0.));
#86249=DIRECTION('ref_axis',(0.,1.,0.));
#86250=DIRECTION('',(-1.,0.,0.));
#86251=DIRECTION('center_axis',(1.,0.,0.));
#86252=DIRECTION('ref_axis',(0.,-1.,0.));
#86253=DIRECTION('',(1.,0.,0.));
#86254=DIRECTION('center_axis',(-1.,0.,0.));
#86255=DIRECTION('ref_axis',(0.,-0.992397367379901,-0.1230750389699));
#86256=DIRECTION('center_axis',(1.,0.,0.));
#86257=DIRECTION('ref_axis',(0.,-1.,0.));
#86258=DIRECTION('',(1.,0.,0.));
#86259=DIRECTION('center_axis',(1.,0.,0.));
#86260=DIRECTION('ref_axis',(0.,-1.,0.));
#86261=DIRECTION('',(1.,0.,0.));
#86262=DIRECTION('center_axis',(-1.,0.,0.));
#86263=DIRECTION('ref_axis',(0.,-0.857325768567308,-0.514774248142304));
#86264=DIRECTION('center_axis',(0.173648177666903,0.,0.984807753012213));
#86265=DIRECTION('ref_axis',(0.984807753012213,0.,-0.173648177666903));
#86266=DIRECTION('',(0.173648177666903,0.,0.984807753012213));
#86267=DIRECTION('',(0.173648177666903,0.,0.984807753012213));
#86268=DIRECTION('center_axis',(0.173648177666903,0.,0.984807753012213));
#86269=DIRECTION('ref_axis',(0.984807753012213,0.,-0.173648177666903));
#86270=DIRECTION('',(0.173648177666903,0.,0.984807753012213));
#86271=DIRECTION('center_axis',(0.173648177666903,0.,0.984807753012213));
#86272=DIRECTION('ref_axis',(0.984807753012213,0.,-0.173648177666903));
#86273=DIRECTION('',(0.173648177666903,0.,0.984807753012213));
#86274=DIRECTION('center_axis',(0.173648177666903,0.,0.984807753012213));
#86275=DIRECTION('ref_axis',(0.984807753012213,0.,-0.173648177666903));
#86276=DIRECTION('',(0.173648177666903,0.,0.984807753012213));
#86277=DIRECTION('center_axis',(0.173648177666903,0.,0.984807753012213));
#86278=DIRECTION('ref_axis',(0.984807753012213,0.,-0.173648177666903));
#86279=DIRECTION('',(0.173648177666903,0.,0.984807753012213));
#86280=DIRECTION('center_axis',(-0.173648177666903,0.,-0.984807753012213));
#86281=DIRECTION('ref_axis',(-0.984807753012213,0.,0.173648177666903));
#86282=DIRECTION('center_axis',(0.173648177666903,0.,0.984807753012213));
#86283=DIRECTION('ref_axis',(0.,-1.,0.));
#86284=DIRECTION('',(0.173648177666903,0.,0.984807753012213));
#86285=DIRECTION('',(-0.173648177666903,0.,-0.984807753012213));
#86286=DIRECTION('',(0.173648177666903,0.,0.984807753012213));
#86287=DIRECTION('center_axis',(0.173648177666903,0.,0.984807753012213));
#86288=DIRECTION('ref_axis',(0.,-1.,0.));
#86289=DIRECTION('center_axis',(0.173648177666903,0.,0.984807753012213));
#86290=DIRECTION('ref_axis',(0.,-1.,0.));
#86291=DIRECTION('center_axis',(0.173648177666903,0.,0.984807753012213));
#86292=DIRECTION('ref_axis',(0.,-1.,0.));
#86293=DIRECTION('',(0.173648177666903,0.,0.984807753012213));
#86294=DIRECTION('center_axis',(0.173648177666903,0.,0.984807753012213));
#86295=DIRECTION('ref_axis',(0.,-1.,0.));
#86296=DIRECTION('',(0.173648177666903,0.,0.984807753012213));
#86297=DIRECTION('center_axis',(-0.173648177666903,0.,-0.984807753012213));
#86298=DIRECTION('ref_axis',(0.984807753012213,0.,-0.173648177666903));
#86299=DIRECTION('center_axis',(0.173648177666902,0.,0.984807753012213));
#86300=DIRECTION('ref_axis',(0.984807753012213,0.,-0.173648177666902));
#86301=DIRECTION('center_axis',(-3.77535033790721E-16,-1.,-2.84635355732631E-15));
#86302=DIRECTION('ref_axis',(-0.984807753012204,-1.22464679914735E-16,0.173648177666953));
#86303=DIRECTION('center_axis',(0.173648177666902,0.,0.984807753012213));
#86304=DIRECTION('ref_axis',(0.984807753012213,0.,-0.173648177666902));
#86305=DIRECTION('center_axis',(0.173648177666902,0.,0.984807753012213));
#86306=DIRECTION('ref_axis',(0.984807753012213,0.,-0.173648177666902));
#86307=DIRECTION('center_axis',(-0.173648177666902,0.,-0.984807753012213));
#86308=DIRECTION('ref_axis',(-0.984807753012213,0.,0.173648177666902));
#86309=DIRECTION('center_axis',(0.173648177666902,0.,0.984807753012213));
#86310=DIRECTION('ref_axis',(-0.984807753012213,0.,0.173648177666902));
#86311=DIRECTION('center_axis',(0.173648177666902,0.,0.984807753012213));
#86312=DIRECTION('ref_axis',(-0.984807753012213,0.,0.173648177666902));
#86313=DIRECTION('center_axis',(-0.62194003125718,0.74694017202758,-0.235097802905997));
#86314=DIRECTION('ref_axis',(-0.677339878007115,-0.362498100233908,0.640160774327914));
#86315=DIRECTION('center_axis',(0.621933305629086,-0.746947822272283,0.235091288975095));
#86316=DIRECTION('ref_axis',(0.353583401256323,2.62174188094628E-7,-0.935403003178813));
#86317=DIRECTION('center_axis',(0.39293929197921,0.557382729135213,0.73138444478992));
#86318=DIRECTION('ref_axis',(0.677339878007116,0.362498100233908,-0.640160774327913));
#86319=DIRECTION('center_axis',(0.621933305629086,-0.746947822272283,0.235091288975095));
#86320=DIRECTION('ref_axis',(0.353583401256323,2.62174188094628E-7,-0.935403003178813));
#86321=DIRECTION('center_axis',(0.173648177666902,0.,0.984807753012213));
#86322=DIRECTION('ref_axis',(0.782050857825719,0.607767196495907,-0.137896666520851));
#86323=DIRECTION('center_axis',(0.,1.,0.));
#86324=DIRECTION('ref_axis',(0.353585017730993,0.,-0.935402392147985));
#86325=DIRECTION('center_axis',(0.,1.,0.));
#86326=DIRECTION('ref_axis',(1.,0.,0.));
#86327=DIRECTION('center_axis',(0.,-1.,0.));
#86328=DIRECTION('ref_axis',(0.916673510305537,0.,-0.399636929605017));
#86329=DIRECTION('',(1.794251608235E-8,-0.999999999999999,4.127905851638E-8));
#86330=DIRECTION('',(-5.50004478946E-11,-1.,-3.753192811798E-11));
#86331=DIRECTION('center_axis',(3.02975422528107E-10,-1.,-4.69337161727405E-11));
#86332=DIRECTION('ref_axis',(0.312852999424802,5.02069497088088E-11,0.949801558616801));
#86333=DIRECTION('center_axis',(0.,1.,0.));
#86334=DIRECTION('ref_axis',(0.173648177666898,0.,0.984807753012214));
#86335=DIRECTION('center_axis',(0.173648177666904,2.09451819877512E-15,
0.984807753012213));
#86336=DIRECTION('ref_axis',(-0.681789982854609,-0.721602424588219,0.120217969154012));
#86337=DIRECTION('center_axis',(0.710639662326888,-0.692307692307688,-0.125304946029797));
#86338=DIRECTION('ref_axis',(0.173648177666926,-2.4450854095363E-14,0.984807753012209));
#86339=DIRECTION('center_axis',(-0.173648177666902,-1.35349239628917E-17,
-0.984807753012213));
#86340=DIRECTION('ref_axis',(2.35031488101622E-18,-1.,1.33292980550865E-17));
#86341=DIRECTION('center_axis',(0.173648177666902,0.,0.984807753012213));
#86342=DIRECTION('ref_axis',(0.984807753012213,0.,-0.173648177666902));
#86343=DIRECTION('',(0.573567618895493,-3.99540154301384E-14,-0.819158218267115));
#86344=DIRECTION('center_axis',(0.173648177666902,0.,0.984807753012213));
#86345=DIRECTION('ref_axis',(-0.984807753012213,0.,0.173648177666902));
#86346=DIRECTION('',(-0.819139113627864,-3.7946361193661E-14,-0.573594902805942));
#86347=DIRECTION('center_axis',(0.173648177666902,0.,0.984807753012213));
#86348=DIRECTION('ref_axis',(-0.984807753012213,0.,0.173648177666902));
#86349=DIRECTION('center_axis',(0.173648177666902,0.,0.984807753012213));
#86350=DIRECTION('ref_axis',(0.984807753012213,0.,-0.173648177666902));
#86351=DIRECTION('',(0.173648177666902,0.,0.984807753012213));
#86352=DIRECTION('center_axis',(0.173648177666902,0.,0.984807753012213));
#86353=DIRECTION('ref_axis',(-0.984807753012213,0.,0.173648177666902));
#86354=DIRECTION('center_axis',(0.173648177666902,0.,0.984807753012213));
#86355=DIRECTION('ref_axis',(0.984807753012213,0.,-0.173648177666902));
#86356=DIRECTION('center_axis',(0.173648177666903,-1.10104762772743E-17,
0.984807753012213));
#86357=DIRECTION('ref_axis',(-0.984138869602196,0.0368502742755397,0.173530235474769));
#86358=DIRECTION('center_axis',(0.173648177666902,0.,0.984807753012213));
#86359=DIRECTION('ref_axis',(-0.984807753012213,0.,0.173648177666902));
#86360=DIRECTION('center_axis',(0.0362904358071779,0.99932079798522,-0.00639898297447297));
#86361=DIRECTION('ref_axis',(0.984138869602196,-0.0368502742755396,-0.173530235474768));
#86362=DIRECTION('center_axis',(0.173648177666902,0.,0.984807753012213));
#86363=DIRECTION('ref_axis',(-0.984807753012213,0.,0.173648177666902));
#86364=DIRECTION('center_axis',(0.173648177666902,0.,0.984807753012213));
#86365=DIRECTION('ref_axis',(0.984807753012213,0.,-0.173648177666902));
#86366=DIRECTION('',(0.173648177666902,0.,0.984807753012213));
#86367=DIRECTION('center_axis',(0.173648177666902,0.,0.984807753012213));
#86368=DIRECTION('ref_axis',(-0.984807753012213,0.,0.173648177666902));
#86369=DIRECTION('center_axis',(0.173648177666902,0.,0.984807753012213));
#86370=DIRECTION('ref_axis',(0.984807753012213,0.,-0.173648177666902));
#86371=DIRECTION('center_axis',(0.173648177666902,-8.04145241919534E-18,
0.984807753012213));
#86372=DIRECTION('ref_axis',(-0.984225072739169,0.0343945931603786,0.173545435413638));
#86373=DIRECTION('center_axis',(0.173648177666902,0.,0.984807753012213));
#86374=DIRECTION('ref_axis',(-0.984807753012213,0.,0.173648177666902));
#86375=DIRECTION('center_axis',(0.0338720620060416,0.99940833094453,-0.00597255842389421));
#86376=DIRECTION('ref_axis',(0.984225072739169,-0.0343945931603785,-0.173545435413638));
#86377=DIRECTION('center_axis',(0.,1.,0.));
#86378=DIRECTION('ref_axis',(1.,0.,0.));
#86379=DIRECTION('center_axis',(0.,1.,0.));
#86380=DIRECTION('ref_axis',(1.,0.,0.));
#86381=DIRECTION('center_axis',(0.399636929605014,0.,0.916673510305538));
#86382=DIRECTION('ref_axis',(0.916673510305538,0.,-0.399636929605014));
#86383=DIRECTION('center_axis',(0.,1.,0.));
#86384=DIRECTION('ref_axis',(1.,0.,0.));
#86385=DIRECTION('center_axis',(0.399636929605016,0.,-0.916673510305537));
#86386=DIRECTION('ref_axis',(0.,1.,0.));
#86387=DIRECTION('center_axis',(0.,1.,0.));
#86388=DIRECTION('ref_axis',(1.,0.,0.));
#86389=DIRECTION('',(3.93130974098696E-8,-0.999999999999995,9.01091822956491E-8));
#86390=DIRECTION('',(1.026064694511E-11,-1.,6.99782860462E-12));
#86391=DIRECTION('center_axis',(-0.173648177666902,0.,-0.984807753012213));
#86392=DIRECTION('ref_axis',(-0.984807753012213,0.,0.173648177666902));
#86393=DIRECTION('center_axis',(-0.803670499663718,1.75978326149641E-7,
0.595074556648357));
#86394=DIRECTION('ref_axis',(0.595074539966384,-0.000236546883935123,0.80367047720404));
#86395=DIRECTION('',(0.173648177666902,0.,0.984807753012213));
#86396=DIRECTION('center_axis',(0.173648177666902,0.,0.984807753012213));
#86397=DIRECTION('ref_axis',(0.984807753012213,0.,-0.173648177666902));
#86398=DIRECTION('center_axis',(-0.803670499663718,1.75978326149641E-7,
0.595074556648357));
#86399=DIRECTION('ref_axis',(0.595074539966384,-0.000236546883935123,0.80367047720404));
#86400=DIRECTION('center_axis',(0.,1.,0.));
#86401=DIRECTION('ref_axis',(1.,0.,0.));
#86402=DIRECTION('center_axis',(0.,-1.,0.));
#86403=DIRECTION('ref_axis',(1.,0.,0.));
#86404=DIRECTION('center_axis',(0.399636929605016,0.,0.916673510305537));
#86405=DIRECTION('ref_axis',(0.,-1.,0.));
#86406=DIRECTION('center_axis',(0.399636929605014,0.,-0.916673510305538));
#86407=DIRECTION('ref_axis',(0.916673510305538,0.,0.399636929605014));
#86408=DIRECTION('center_axis',(0.,-1.,0.));
#86409=DIRECTION('ref_axis',(-1.,0.,0.));
#86410=DIRECTION('',(1.548136098957E-14,1.,-3.664781422684E-14));
#86411=DIRECTION('',(0.,-1.,0.));
#86412=DIRECTION('center_axis',(-0.62193825517579,-0.746941405650846,-0.235098582031521));
#86413=DIRECTION('ref_axis',(-0.677340854507514,0.362495984395913,0.640160939226901));
#86414=DIRECTION('center_axis',(0.621933330370316,0.746947780441719,0.235091356429106));
#86415=DIRECTION('ref_axis',(0.782054095085269,-0.607763215737225,-0.137895851848809));
#86416=DIRECTION('center_axis',(-0.392940419865306,0.55738245202121,-0.731384050014013));
#86417=DIRECTION('ref_axis',(0.677340854507515,-0.362495984395913,-0.640160939226901));
#86418=DIRECTION('center_axis',(0.621933330370316,0.746947780441719,0.235091356429106));
#86419=DIRECTION('ref_axis',(0.782054095085269,-0.607763215737225,-0.137895851848809));
#86420=DIRECTION('center_axis',(0.,1.,0.));
#86421=DIRECTION('ref_axis',(0.353584869536014,0.,-0.935402448166135));
#86422=DIRECTION('center_axis',(-0.173648177666903,7.27812871698714E-16,
-0.984807753012213));
#86423=DIRECTION('ref_axis',(0.782051073965749,-0.607766909728233,-0.137896704632171));
#86424=DIRECTION('center_axis',(0.173648177666902,0.,0.984807753012213));
#86425=DIRECTION('ref_axis',(-0.984807753012213,0.,0.173648177666902));
#86426=DIRECTION('center_axis',(0.173648177666902,0.,0.984807753012213));
#86427=DIRECTION('ref_axis',(0.984807753012213,0.,-0.173648177666902));
#86428=DIRECTION('',(0.173648177666902,0.,0.984807753012213));
#86429=DIRECTION('center_axis',(0.173648177666903,1.2793705768531E-16,0.984807753012213));
#86430=DIRECTION('ref_axis',(0.9329757660115,0.320145396331696,-0.164508799894948));
#86431=DIRECTION('center_axis',(0.173648177666902,4.8935450121219E-18,0.984807753012213));
#86432=DIRECTION('ref_axis',(-0.983580074845734,0.0499167317439819,0.173431704882525));
#86433=DIRECTION('center_axis',(0.173648177666903,0.,0.984807753012213));
#86434=DIRECTION('ref_axis',(0.984807753012213,0.,-0.173648177666903));
#86435=DIRECTION('center_axis',(0.0491583844265041,0.998753382918926,-0.00866794950243004));
#86436=DIRECTION('ref_axis',(0.983580074845734,-0.0499167317439817,-0.173431704882525));
#86437=DIRECTION('center_axis',(0.173648177666902,0.,0.984807753012213));
#86438=DIRECTION('ref_axis',(0.984807753012213,0.,-0.173648177666902));
#86439=DIRECTION('center_axis',(0.173648177666902,0.,0.984807753012213));
#86440=DIRECTION('ref_axis',(0.984807753012213,0.,-0.173648177666902));
#86441=DIRECTION('center_axis',(0.173648177666902,0.,0.984807753012213));
#86442=DIRECTION('ref_axis',(-0.984807753012213,0.,0.173648177666902));
#86443=DIRECTION('',(0.173648177666902,0.,0.984807753012213));
#86444=DIRECTION('center_axis',(0.173648177666902,0.,0.984807753012213));
#86445=DIRECTION('ref_axis',(-0.984807753012213,0.,0.173648177666902));
#86446=DIRECTION('center_axis',(0.173648177666902,0.,0.984807753012213));
#86447=DIRECTION('ref_axis',(-0.984807753012213,0.,0.173648177666902));
#86448=DIRECTION('center_axis',(0.173648177666903,0.,0.984807753012213));
#86449=DIRECTION('ref_axis',(-0.984807753012213,0.,0.173648177666903));
#86450=DIRECTION('',(0.173648177666902,0.,0.984807753012213));
#86451=DIRECTION('center_axis',(0.173648177666903,0.,0.984807753012213));
#86452=DIRECTION('ref_axis',(0.984807753012213,0.,-0.173648177666903));
#86453=DIRECTION('center_axis',(0.173648177666903,0.,0.984807753012213));
#86454=DIRECTION('ref_axis',(0.984807753012213,0.,-0.173648177666903));
#86455=DIRECTION('center_axis',(0.190809912898503,0.,-0.981627005099017));
#86456=DIRECTION('ref_axis',(0.981627005099017,0.,0.190809912898503));
#86457=DIRECTION('center_axis',(-0.190809912898503,0.,0.981627005099017));
#86458=DIRECTION('ref_axis',(0.981627005099017,0.,0.190809912898503));
#86459=DIRECTION('center_axis',(0.190809912898503,0.,-0.981627005099017));
#86460=DIRECTION('ref_axis',(-0.981627005099017,0.,-0.190809912898503));
#86461=DIRECTION('',(0.190809912898503,0.,-0.981627005099017));
#86462=DIRECTION('center_axis',(0.190809912898503,0.,-0.981627005099017));
#86463=DIRECTION('ref_axis',(0.981627005099017,0.,0.190809912898503));
#86464=DIRECTION('center_axis',(0.190809912898503,0.,-0.981627005099017));
#86465=DIRECTION('ref_axis',(-0.981627005099017,0.,-0.190809912898503));
#86466=DIRECTION('center_axis',(0.190809912898503,0.,-0.981627005099017));
#86467=DIRECTION('ref_axis',(0.981627005099017,0.,0.190809912898503));
#86468=DIRECTION('center_axis',(0.190809912898503,0.,-0.981627005099017));
#86469=DIRECTION('ref_axis',(0.981627005099017,0.,0.190809912898503));
#86470=DIRECTION('',(0.190809912898503,0.,-0.981627005099017));
#86471=DIRECTION('center_axis',(0.190809912898503,0.,-0.981627005099017));
#86472=DIRECTION('ref_axis',(0.981627005099017,0.,0.190809912898503));
#86473=DIRECTION('center_axis',(0.190809912898503,0.,-0.981627005099017));
#86474=DIRECTION('ref_axis',(0.981627005099017,0.,0.190809912898503));
#86475=DIRECTION('center_axis',(0.190809912898503,2.42635641189931E-17,
-0.981627005099017));
#86476=DIRECTION('ref_axis',(4.62972855615232E-18,-1.,-2.38177697791552E-17));
#86477=DIRECTION('',(0.134925187626816,0.707095228669965,-0.69412645197834));
#86478=DIRECTION('center_axis',(0.190809912898503,0.,-0.981627005099017));
#86479=DIRECTION('ref_axis',(0.981627005099017,0.,0.190809912898503));
#86480=DIRECTION('center_axis',(0.190809912898504,0.,-0.981627005099017));
#86481=DIRECTION('ref_axis',(0.981627005099017,0.,0.190809912898504));
#86482=DIRECTION('center_axis',(0.190809912898503,0.,-0.981627005099017));
#86483=DIRECTION('ref_axis',(0.981627005099017,0.,0.190809912898503));
#86484=DIRECTION('',(0.190809912898504,0.,-0.981627005099017));
#86485=DIRECTION('center_axis',(0.190809912898504,0.,-0.981627005099017));
#86486=DIRECTION('ref_axis',(-0.981627005099017,0.,-0.190809912898504));
#86487=DIRECTION('center_axis',(0.173648177666903,0.,0.984807753012213));
#86488=DIRECTION('ref_axis',(-0.984807753012213,0.,0.173648177666903));
#86489=DIRECTION('center_axis',(0.173648177666902,0.,0.984807753012213));
#86490=DIRECTION('ref_axis',(-0.984807753012213,0.,0.173648177666902));
#86491=DIRECTION('',(0.173648177666903,0.,0.984807753012213));
#86492=DIRECTION('center_axis',(0.403404352147799,-6.13683761632244E-5,
-0.915021816626324));
#86493=DIRECTION('ref_axis',(0.914262104708908,-0.0407141998164361,0.403072149653813));
#86494=DIRECTION('center_axis',(-0.691975445312705,-6.74709518344435E-5,
-0.721921033446148));
#86495=DIRECTION('ref_axis',(0.721885115931311,0.00991088319453953,-0.691941943945547));
#86496=DIRECTION('center_axis',(-0.692027149057367,6.1891542016879E-5,-0.721871471341657));
#86497=DIRECTION('ref_axis',(0.721167827159643,-0.0440831886297046,-0.691356375214749));
#86498=DIRECTION('center_axis',(0.403333139961256,6.74332542398484E-5,-0.915053208104179));
#86499=DIRECTION('ref_axis',(0.914881149946327,0.0193618170927673,0.403258727756452));
#86500=DIRECTION('center_axis',(0.173648177666903,-3.1720657846433E-17,
0.984807753012213));
#86501=DIRECTION('ref_axis',(-0.982890310181394,0.0623719011882791,0.173310080761864));
#86502=DIRECTION('center_axis',(0.173648177666903,0.,0.984807753012213));
#86503=DIRECTION('ref_axis',(0.984807753012213,0.,-0.173648177666903));
#86504=DIRECTION('center_axis',(0.173648177666903,0.,0.984807753012213));
#86505=DIRECTION('ref_axis',(0.984807753012213,0.,-0.173648177666903));
#86506=DIRECTION('center_axis',(0.0614243318603288,0.998052977522816,-0.0108307669789647));
#86507=DIRECTION('ref_axis',(0.982890310181394,-0.062371901188279,-0.173310080761863));
#86508=DIRECTION('center_axis',(0.173648177666903,0.,0.984807753012213));
#86509=DIRECTION('ref_axis',(0.984807753012213,0.,-0.173648177666903));
#86510=DIRECTION('center_axis',(0.173648177666902,0.,0.984807753012213));
#86511=DIRECTION('ref_axis',(-0.984807753012213,0.,0.173648177666902));
#86512=DIRECTION('center_axis',(0.173648177666903,0.,0.984807753012213));
#86513=DIRECTION('ref_axis',(-0.984807753012213,0.,0.173648177666903));
#86514=DIRECTION('',(0.173648177666902,0.,0.984807753012213));
#86515=DIRECTION('center_axis',(0.173648177666902,-5.19592868310163E-17,
0.984807753012213));
#86516=DIRECTION('ref_axis',(-9.02263547107784E-18,-1.,-5.11699085121702E-17));
#86517=DIRECTION('center_axis',(0.173648177666902,0.,0.984807753012213));
#86518=DIRECTION('ref_axis',(-0.984807753012213,0.,0.173648177666902));
#86519=DIRECTION('',(0.12279097479207,0.707088520672423,0.696382222951518));
#86520=DIRECTION('center_axis',(0.173648177666902,0.,0.984807753012213));
#86521=DIRECTION('ref_axis',(-0.984807753012213,0.,0.173648177666902));
#86522=DIRECTION('center_axis',(0.173648177666902,0.,0.984807753012213));
#86523=DIRECTION('ref_axis',(-0.984807753012213,0.,0.173648177666902));
#86524=DIRECTION('center_axis',(0.173648177666902,0.,0.984807753012213));
#86525=DIRECTION('ref_axis',(-0.984807753012213,0.,0.173648177666902));
#86526=DIRECTION('center_axis',(0.173648177666902,0.,0.984807753012213));
#86527=DIRECTION('ref_axis',(0.984807753012213,0.,-0.173648177666902));
#86528=DIRECTION('center_axis',(0.173648177666902,0.,0.984807753012213));
#86529=DIRECTION('ref_axis',(0.984807753012213,0.,-0.173648177666902));
#86530=DIRECTION('',(0.173648177666902,0.,0.984807753012213));
#86531=DIRECTION('center_axis',(-0.173648177666902,0.,-0.984807753012213));
#86532=DIRECTION('ref_axis',(0.984807753012213,0.,-0.173648177666902));
#86533=DIRECTION('center_axis',(0.768062672188182,-3.57030663143955E-6,
-0.640374680619403));
#86534=DIRECTION('ref_axis',(0.640373969760258,-0.00148573958139851,0.768061827870247));
#86535=DIRECTION('center_axis',(-0.173648177666902,-1.37778369814978E-16,
-0.984807753012213));
#86536=DIRECTION('ref_axis',(0.791088680366871,0.59558472277628,-0.139490278481711));
#86537=DIRECTION('center_axis',(0.,-1.,0.));
#86538=DIRECTION('ref_axis',(-1.,0.,0.));
#86539=DIRECTION('center_axis',(0.,1.,0.));
#86540=DIRECTION('ref_axis',(-0.92054989510347,0.,-0.390624999999987));
#86541=DIRECTION('',(2.085442929456E-13,-1.,6.417977260753E-13));
#86542=DIRECTION('center_axis',(0.,-1.,0.));
#86543=DIRECTION('ref_axis',(-0.951104406813915,0.,0.308869563633505));
#86544=DIRECTION('',(2.04281036531E-14,1.,-4.831690603169E-14));
#86545=DIRECTION('center_axis',(0.173648177666903,0.,0.984807753012213));
#86546=DIRECTION('ref_axis',(0.,-1.,0.));
#86547=DIRECTION('center_axis',(0.173648177666903,0.,0.984807753012213));
#86548=DIRECTION('ref_axis',(0.,-1.,0.));
#86549=DIRECTION('center_axis',(-0.173648177666902,0.,-0.984807753012213));
#86550=DIRECTION('ref_axis',(0.984807753012213,0.,-0.173648177666902));
#86551=DIRECTION('',(0.173648177666903,0.,0.984807753012213));
#86552=DIRECTION('center_axis',(0.173648177666902,0.,0.984807753012213));
#86553=DIRECTION('ref_axis',(0.984807753012213,0.,-0.173648177666902));
#86554=DIRECTION('center_axis',(-0.173648177666902,0.,-0.984807753012213));
#86555=DIRECTION('ref_axis',(0.984807753012213,0.,-0.173648177666902));
#86556=DIRECTION('center_axis',(-0.173648177666903,0.,-0.984807753012213));
#86557=DIRECTION('ref_axis',(-0.984807753012213,0.,0.173648177666903));
#86558=DIRECTION('',(0.0425655252567249,-2.63800745320352E-17,-0.999093677319409));
#86559=DIRECTION('center_axis',(-0.173648177666903,0.,-0.984807753012213));
#86560=DIRECTION('ref_axis',(-0.984807753012213,0.,0.173648177666903));
#86561=DIRECTION('center_axis',(-0.173648177666903,0.,-0.984807753012213));
#86562=DIRECTION('ref_axis',(-0.984807753012213,0.,0.173648177666903));
#86563=DIRECTION('',(0.573576435615923,-8.65956055458343E-17,-0.819152044803731));
#86564=DIRECTION('center_axis',(0.173648177666903,0.,0.984807753012213));
#86565=DIRECTION('ref_axis',(0.984807753012213,0.,-0.173648177666903));
#86566=DIRECTION('center_axis',(0.173648177666903,0.,0.984807753012213));
#86567=DIRECTION('ref_axis',(0.984807753012213,0.,-0.173648177666903));
#86568=DIRECTION('center_axis',(1.,0.,0.));
#86569=DIRECTION('ref_axis',(0.,0.999170306594043,-0.040727121439721));
#86570=DIRECTION('center_axis',(1.,0.,0.));
#86571=DIRECTION('ref_axis',(0.,-1.,0.));
#86572=DIRECTION('center_axis',(0.,-0.0407271214397213,-0.999170306594043));
#86573=DIRECTION('ref_axis',(0.,-0.999170306594043,0.0407271214397213));
#86574=DIRECTION('center_axis',(1.,0.,0.));
#86575=DIRECTION('ref_axis',(0.,-1.,0.));
#86576=DIRECTION('center_axis',(1.,0.,0.));
#86577=DIRECTION('ref_axis',(0.,-1.,0.));
#86578=DIRECTION('center_axis',(1.,0.,0.));
#86579=DIRECTION('ref_axis',(0.,-1.,0.));
#86580=DIRECTION('',(1.,0.,0.));
#86581=DIRECTION('center_axis',(-1.,0.,0.));
#86582=DIRECTION('ref_axis',(0.,-1.,0.));
#86583=DIRECTION('center_axis',(-1.,-1.04909975265626E-16,0.));
#86584=DIRECTION('ref_axis',(-7.91782854057881E-17,0.754725994409142,0.656040146151995));
#86585=DIRECTION('center_axis',(1.,0.,0.));
#86586=DIRECTION('ref_axis',(0.,-0.628687890661713,-0.777657724281915));
#86587=DIRECTION('center_axis',(1.,0.,0.));
#86588=DIRECTION('ref_axis',(0.,-1.,0.));
#86589=DIRECTION('center_axis',(-1.,0.,0.));
#86590=DIRECTION('ref_axis',(0.,0.,1.));
#86591=DIRECTION('',(1.,0.,0.));
#86592=DIRECTION('center_axis',(-1.,0.,0.));
#86593=DIRECTION('ref_axis',(0.,0.,1.));
#86594=DIRECTION('center_axis',(0.,-1.,0.));
#86595=DIRECTION('ref_axis',(-1.,0.,0.));
#86596=DIRECTION('center_axis',(0.,-1.,0.));
#86597=DIRECTION('ref_axis',(-0.951104406813915,0.,0.308869563633505));
#86598=DIRECTION('',(-1.424093909463E-10,-1.,-4.385222496239E-10));
#86599=DIRECTION('center_axis',(0.,-1.,0.));
#86600=DIRECTION('ref_axis',(-0.92054989510347,0.,0.390624999999987));
#86601=DIRECTION('',(0.,-1.,0.));
#86602=DIRECTION('',(0.,1.,0.));
#86603=DIRECTION('center_axis',(0.,1.,0.));
#86604=DIRECTION('ref_axis',(1.,0.,0.));
#86605=DIRECTION('center_axis',(0.,-1.,0.));
#86606=DIRECTION('ref_axis',(0.916673510305537,0.,-0.399636929605016));
#86607=DIRECTION('',(1.15953143331196E-6,-0.999999999996469,-2.39123208817793E-6));
#86608=DIRECTION('',(9.96499151473735E-7,-0.999999999997636,1.93274404172707E-6));
#86609=DIRECTION('center_axis',(-1.,0.,0.));
#86610=DIRECTION('ref_axis',(0.,0.,1.));
#86611=DIRECTION('center_axis',(-1.,0.,0.));
#86612=DIRECTION('ref_axis',(0.,0.,1.));
#86613=DIRECTION('',(1.,0.,0.));
#86614=DIRECTION('center_axis',(1.,0.,0.));
#86615=DIRECTION('ref_axis',(0.,0.,1.));
#86616=DIRECTION('center_axis',(-1.,0.,0.));
#86617=DIRECTION('ref_axis',(0.,0.,1.));
#86618=DIRECTION('center_axis',(1.,0.,0.));
#86619=DIRECTION('ref_axis',(0.,0.,1.));
#86620=DIRECTION('',(1.,0.,0.));
#86621=DIRECTION('center_axis',(-1.,0.,0.));
#86622=DIRECTION('ref_axis',(0.,0.,1.));
#86623=DIRECTION('center_axis',(1.,0.,0.));
#86624=DIRECTION('ref_axis',(0.,0.,1.));
#86625=DIRECTION('center_axis',(1.,0.,6.86169978136685E-18));
#86626=DIRECTION('ref_axis',(6.86169978136685E-18,0.,-1.));
#86627=DIRECTION('',(-0.707106781821139,8.65956055458343E-17,-0.707106780551956));
#86628=DIRECTION('center_axis',(-1.,0.,0.));
#86629=DIRECTION('ref_axis',(0.,0.,1.));
#86630=DIRECTION('center_axis',(1.,0.,0.));
#86631=DIRECTION('ref_axis',(0.,0.,-1.));
#86632=DIRECTION('center_axis',(-1.,0.,0.));
#86633=DIRECTION('ref_axis',(0.,0.,1.));
#86634=DIRECTION('',(1.,0.,0.));
#86635=DIRECTION('center_axis',(-1.,0.,0.));
#86636=DIRECTION('ref_axis',(0.,0.,-1.));
#86637=DIRECTION('center_axis',(-1.,0.,0.));
#86638=DIRECTION('ref_axis',(0.,0.,-1.));
#86639=DIRECTION('center_axis',(-1.,0.,0.));
#86640=DIRECTION('ref_axis',(0.,0.,1.));
#86641=DIRECTION('center_axis',(-1.,0.,-2.79182864590248E-17));
#86642=DIRECTION('ref_axis',(-2.79182864590248E-17,0.,1.));
#86643=DIRECTION('',(-0.500000001036284,-1.0605752379922E-16,-0.86602540318614));
#86644=DIRECTION('center_axis',(-1.,0.,6.88416479379655E-18));
#86645=DIRECTION('ref_axis',(6.88416479379655E-18,0.,1.));
#86646=DIRECTION('',(-0.707106781821139,-8.65956055458343E-17,-0.707106780551956));
#86647=DIRECTION('center_axis',(1.,0.,0.));
#86648=DIRECTION('ref_axis',(0.,0.,1.));
#86649=DIRECTION('center_axis',(-1.,0.,0.));
#86650=DIRECTION('ref_axis',(0.,-0.998325932398639,0.057838851133022));
#86651=DIRECTION('center_axis',(1.,0.,0.));
#86652=DIRECTION('ref_axis',(0.,1.,0.));
#86653=DIRECTION('center_axis',(1.,0.,0.));
#86654=DIRECTION('ref_axis',(0.,1.,0.));
#86655=DIRECTION('center_axis',(0.,-0.0578388511330215,-0.998325932398639));
#86656=DIRECTION('ref_axis',(0.,0.998325932398639,-0.0578388511330215));
#86657=DIRECTION('center_axis',(-1.,0.,0.));
#86658=DIRECTION('ref_axis',(0.,0.,1.));
#86659=DIRECTION('center_axis',(-1.,0.,0.));
#86660=DIRECTION('ref_axis',(0.,1.,0.));
#86661=DIRECTION('center_axis',(-1.,0.,0.));
#86662=DIRECTION('ref_axis',(0.,1.,0.));
#86663=DIRECTION('',(-1.,0.,0.));
#86664=DIRECTION('center_axis',(-1.,1.71983566009223E-17,0.));
#86665=DIRECTION('ref_axis',(-1.29799163280414E-17,-0.754718408812697,0.656048872721561));
#86666=DIRECTION('center_axis',(1.,0.,0.));
#86667=DIRECTION('ref_axis',(0.,0.867366884881976,0.497669254636186));
#86668=DIRECTION('center_axis',(-1.,0.,0.));
#86669=DIRECTION('ref_axis',(0.,1.,0.));
#86670=DIRECTION('center_axis',(-1.,0.,0.));
#86671=DIRECTION('ref_axis',(0.,-0.27343727392181,0.961889836327534));
#86672=DIRECTION('center_axis',(-1.,0.,0.));
#86673=DIRECTION('ref_axis',(0.,0.,1.));
#86674=DIRECTION('',(1.,0.,0.));
#86675=DIRECTION('center_axis',(-1.,0.,0.));
#86676=DIRECTION('ref_axis',(0.,0.,-1.));
#86677=DIRECTION('center_axis',(0.,-1.,0.));
#86678=DIRECTION('ref_axis',(-1.,0.,0.));
#86679=DIRECTION('',(0.,-1.,0.));
#86680=DIRECTION('center_axis',(0.,1.,0.));
#86681=DIRECTION('ref_axis',(-0.951104406813915,0.,0.308869563633505));
#86682=DIRECTION('',(1.424328388566E-10,-1.,4.385942986573E-10));
#86683=DIRECTION('center_axis',(0.,1.,0.));
#86684=DIRECTION('ref_axis',(-0.92054989510347,0.,-0.390624999999987));
#86685=DIRECTION('',(0.,1.,0.));
#86686=DIRECTION('center_axis',(0.,1.,0.));
#86687=DIRECTION('ref_axis',(1.,0.,0.));
#86688=DIRECTION('',(-6.02495790651922E-7,-0.999999999999037,1.25033281170505E-6));
#86689=DIRECTION('center_axis',(0.,1.,0.));
#86690=DIRECTION('ref_axis',(0.916673510305537,0.,0.399636929605016));
#86691=DIRECTION('',(1.22060867629305E-7,-0.999999999999941,3.20447341735213E-7));
#86692=DIRECTION('center_axis',(-1.,0.,0.));
#86693=DIRECTION('ref_axis',(0.,0.,1.));
#86694=DIRECTION('center_axis',(-1.,0.,0.));
#86695=DIRECTION('ref_axis',(0.,0.,1.));
#86696=DIRECTION('',(1.,0.,0.));
#86697=DIRECTION('center_axis',(1.,0.,0.));
#86698=DIRECTION('ref_axis',(0.,0.,1.));
#86699=DIRECTION('center_axis',(-1.,0.,0.));
#86700=DIRECTION('ref_axis',(0.,0.,1.));
#86701=DIRECTION('center_axis',(1.,0.,0.));
#86702=DIRECTION('ref_axis',(0.,0.,1.));
#86703=DIRECTION('',(1.,0.,0.));
#86704=DIRECTION('center_axis',(-1.,0.,0.));
#86705=DIRECTION('ref_axis',(0.,0.,1.));
#86706=DIRECTION('center_axis',(1.,0.,0.));
#86707=DIRECTION('ref_axis',(0.,0.,1.));
#86708=DIRECTION('center_axis',(1.,0.,6.86169978136685E-18));
#86709=DIRECTION('ref_axis',(6.86169978136685E-18,0.,-1.));
#86710=DIRECTION('',(-0.707106781821139,8.65956055458343E-17,-0.707106780551956));
#86711=DIRECTION('center_axis',(-1.,0.,0.));
#86712=DIRECTION('ref_axis',(0.,0.,1.));
#86713=DIRECTION('center_axis',(1.,0.,0.));
#86714=DIRECTION('ref_axis',(0.,0.,-1.));
#86715=DIRECTION('center_axis',(-1.,0.,0.));
#86716=DIRECTION('ref_axis',(0.,0.,1.));
#86717=DIRECTION('',(1.,0.,0.));
#86718=DIRECTION('center_axis',(-1.,0.,0.));
#86719=DIRECTION('ref_axis',(0.,0.,-1.));
#86720=DIRECTION('center_axis',(-1.,0.,0.));
#86721=DIRECTION('ref_axis',(0.,0.,-1.));
#86722=DIRECTION('center_axis',(-1.,0.,0.));
#86723=DIRECTION('ref_axis',(0.,0.,1.));
#86724=DIRECTION('center_axis',(-1.,0.,-2.79182864590248E-17));
#86725=DIRECTION('ref_axis',(-2.79182864590248E-17,0.,1.));
#86726=DIRECTION('',(-0.500000001036284,-1.0605752379922E-16,-0.86602540318614));
#86727=DIRECTION('center_axis',(-1.,0.,6.88416479379655E-18));
#86728=DIRECTION('ref_axis',(6.88416479379655E-18,0.,1.));
#86729=DIRECTION('',(-0.707106781821139,-8.65956055458343E-17,-0.707106780551956));
#86730=DIRECTION('center_axis',(1.,0.,0.));
#86731=DIRECTION('ref_axis',(0.,0.,1.));
#86732=DIRECTION('center_axis',(1.,0.,0.));
#86733=DIRECTION('ref_axis',(0.,1.,0.));
#86734=DIRECTION('',(0.,0.5,0.866025403784439));
#86735=DIRECTION('',(0.,1.,-1.14462064665688E-15));
#86736=DIRECTION('',(0.,0.5,-0.866025403784439));
#86737=DIRECTION('',(0.,-0.5,-0.866025403784438));
#86738=DIRECTION('',(0.,-1.,3.29078435913854E-15));
#86739=DIRECTION('',(0.,-0.5,0.866025403784439));
#86740=DIRECTION('center_axis',(0.,-0.866025403784439,0.5));
#86741=DIRECTION('ref_axis',(-1.,0.,0.));
#86742=DIRECTION('',(-1.,0.,0.));
#86743=DIRECTION('',(-1.,0.,0.));
#86744=DIRECTION('center_axis',(0.,1.14462064665688E-15,1.));
#86745=DIRECTION('ref_axis',(0.,-1.,1.14462064665688E-15));
#86746=DIRECTION('',(-1.,0.,0.));
#86747=DIRECTION('center_axis',(0.,0.866025403784439,0.5));
#86748=DIRECTION('ref_axis',(1.,0.,0.));
#86749=DIRECTION('',(-1.,0.,0.));
#86750=DIRECTION('center_axis',(0.,0.866025403784438,-0.5));
#86751=DIRECTION('ref_axis',(-1.,0.,0.));
#86752=DIRECTION('',(-1.,0.,0.));
#86753=DIRECTION('center_axis',(0.,-3.29078435913854E-15,-1.));
#86754=DIRECTION('ref_axis',(0.,-1.,3.29078435913854E-15));
#86755=DIRECTION('',(-1.,0.,0.));
#86756=DIRECTION('center_axis',(0.,-0.866025403784439,-0.5));
#86757=DIRECTION('ref_axis',(0.,0.5,-0.866025403784439));
#86758=DIRECTION('center_axis',(1.,0.,0.));
#86759=DIRECTION('ref_axis',(0.,1.,0.));
#86760=DIRECTION('center_axis',(-1.,0.,0.));
#86761=DIRECTION('ref_axis',(0.,0.,1.));
#86762=DIRECTION('center_axis',(-0.173648177666902,6.04454757851474E-16,
-0.984807753012213));
#86763=DIRECTION('ref_axis',(-0.463438942593986,-0.882352941176469,0.0817167894903066));
#86764=DIRECTION('',(-0.173648177666902,2.77440767547504E-8,-0.984807753012213));
#86765=DIRECTION('center_axis',(0.173648177666898,0.,0.984807753012214));
#86766=DIRECTION('ref_axis',(-0.984807753012214,0.,0.173648177666898));
#86767=DIRECTION('',(-0.173648117922493,-3.57010191110886E-9,-0.984807763546762));
#86768=DIRECTION('center_axis',(-0.173648177666903,-9.86864910777917E-16,
-0.984807753012213));
#86769=DIRECTION('ref_axis',(0.463439330841621,0.882352730916633,-0.0817168579488417));
#86770=DIRECTION('center_axis',(-0.397579755272508,0.101323258775101,-0.911956103893519));
#86771=DIRECTION('ref_axis',(-0.392477586383088,-0.917154287992033,0.0692051746962059));
#86772=DIRECTION('center_axis',(0.393372356615379,-0.17691820058078,-0.902196286488767));
#86773=DIRECTION('ref_axis',(-0.916656540587377,-7.20245669423595E-6,-0.3996758518431));
#86774=DIRECTION('center_axis',(-0.173648177666902,0.,-0.984807753012213));
#86775=DIRECTION('ref_axis',(-0.984807753012213,0.,0.173648177666902));
#86776=DIRECTION('center_axis',(0.173648177666902,0.,0.984807753012213));
#86777=DIRECTION('ref_axis',(-0.984807753012213,0.,0.173648177666902));
#86778=DIRECTION('center_axis',(0.868839692726475,-0.434335125464283,0.237635407990666));
#86779=DIRECTION('ref_axis',(0.469231632397537,0.569298297750996,-0.675071198715632));
#86780=DIRECTION('center_axis',(0.,-1.,0.));
#86781=DIRECTION('ref_axis',(0.263820822858805,0.,-0.964571704657618));
#86782=DIRECTION('center_axis',(-0.868840214246772,0.434332901506587,-0.237637566004393));
#86783=DIRECTION('ref_axis',(0.463438490098785,0.882353178018822,-0.081716798365105));
#86784=DIRECTION('center_axis',(-0.984807753012213,0.,0.173648177666902));
#86785=DIRECTION('ref_axis',(0.,1.,0.));
#86786=DIRECTION('',(0.,-1.,0.));
#86787=DIRECTION('',(1.76688803752592E-7,-0.999999999999454,1.02989646555295E-6));
#86788=DIRECTION('center_axis',(-0.984807753012216,-2.97655366217181E-14,
0.173648177666884));
#86789=DIRECTION('ref_axis',(0.171669242031833,-0.150541017827785,0.97358465132293));
#86790=DIRECTION('',(0.173648177666902,0.,0.984807753012213));
#86791=DIRECTION('center_axis',(0.159542862636401,-0.394791526125702,0.904812536319608));
#86792=DIRECTION('ref_axis',(0.116378695458399,-0.902639656840687,-0.414364150406293));
#86793=DIRECTION('center_axis',(0.173648177666902,0.,0.984807753012213));
#86794=DIRECTION('ref_axis',(0.,1.,0.));
#86795=DIRECTION('',(0.173648177666902,0.,0.984807753012213));
#86796=DIRECTION('center_axis',(0.173648177666907,0.,0.984807753012212));
#86797=DIRECTION('ref_axis',(-0.984807753012212,0.,0.173648177666907));
#86798=DIRECTION('center_axis',(-0.173648177666902,0.,-0.984807753012213));
#86799=DIRECTION('ref_axis',(-0.984807753012213,0.,0.173648177666902));
#86800=DIRECTION('center_axis',(-0.173648177666902,0.,-0.984807753012213));
#86801=DIRECTION('ref_axis',(-0.984807753012213,0.,0.173648177666902));
#86802=DIRECTION('',(-0.984807753012213,0.,0.173648177666902));
#86803=DIRECTION('center_axis',(0.984805369615038,-5.94830521183634E-6,
-0.173661693939703));
#86804=DIRECTION('ref_axis',(5.14708112789013E-6,0.999999999973931,-5.06405332903727E-6));
#86805=DIRECTION('center_axis',(0.984807753012213,0.,-0.173648177666902));
#86806=DIRECTION('ref_axis',(-0.173648177666902,0.,-0.984807753012213));
#86807=DIRECTION('',(0.984791886359845,5.81942005172826E-8,-0.173738137896708));
#86808=DIRECTION('center_axis',(0.984807753012213,0.,-0.173648177666902));
#86809=DIRECTION('ref_axis',(0.173648177666902,0.,0.984807753012213));
#86810=DIRECTION('',(0.984807753012213,0.,-0.173648177666902));
#86811=DIRECTION('center_axis',(0.173648177666902,0.,0.984807753012213));
#86812=DIRECTION('ref_axis',(0.984807753012213,0.,-0.173648177666902));
#86813=DIRECTION('',(-0.173648177666902,0.,-0.984807753012213));
#86814=DIRECTION('center_axis',(0.173648177666902,0.,0.984807753012213));
#86815=DIRECTION('ref_axis',(-0.984807753012213,0.,0.173648177666902));
#86816=DIRECTION('center_axis',(0.984807753012213,0.,-0.173648177666902));
#86817=DIRECTION('ref_axis',(0.173648177666902,0.,0.984807753012213));
#86818=DIRECTION('center_axis',(0.984807753016654,-6.51848275878855E-11,
-0.173648177641717));
#86819=DIRECTION('ref_axis',(6.55053788989343E-11,1.,-3.8902214782866E-12));
#86820=DIRECTION('',(0.984807727666866,-1.33909143097295E-7,-0.173648321407394));
#86821=DIRECTION('',(0.984807753012213,0.,-0.173648177666902));
#86822=DIRECTION('center_axis',(0.951179035368867,7.0777324670319E-6,-0.308639664697617));
#86823=DIRECTION('ref_axis',(1.4524932914303E-5,-0.999999999656205,2.18315400864325E-5));
#86824=DIRECTION('center_axis',(0.982743786584323,1.24231498930631E-20,
-0.184972024722405));
#86825=DIRECTION('ref_axis',(0.184972024692575,-1.79592168335814E-5,0.98274378642584));
#86826=DIRECTION('center_axis',(0.810538528342403,0.460364015539678,-0.362066661360467));
#86827=DIRECTION('ref_axis',(-0.407745277886695,-0.000235138511653656,-0.913095686700459));
#86828=DIRECTION('center_axis',(0.,1.,0.));
#86829=DIRECTION('ref_axis',(-0.394380038568694,0.,-0.918947433305385));
#86830=DIRECTION('center_axis',(0.399636929605016,-2.01051104928073E-15,
-0.916673510305537));
#86831=DIRECTION('ref_axis',(-1.61907524424502E-14,1.,-9.25185853854296E-15));
#86832=DIRECTION('center_axis',(0.,1.,0.));
#86833=DIRECTION('ref_axis',(0.407236366022499,0.,0.913322802840698));
#86834=DIRECTION('center_axis',(0.913322802840698,0.,-0.407236366022499));
#86835=DIRECTION('ref_axis',(0.,1.,0.));
#86836=DIRECTION('center_axis',(0.,1.,0.));
#86837=DIRECTION('ref_axis',(0.407236366022499,0.,0.913322802840698));
#86838=DIRECTION('center_axis',(0.,1.,0.));
#86839=DIRECTION('ref_axis',(-0.897582332306211,0.,-0.440846863130206));
#86840=DIRECTION('center_axis',(-0.399636929605016,0.,-0.916673510305537));
#86841=DIRECTION('ref_axis',(0.,1.,0.));
#86842=DIRECTION('center_axis',(0.,1.,0.));
#86843=DIRECTION('ref_axis',(0.916673510305537,0.,0.399636929605016));
#86844=DIRECTION('center_axis',(0.,1.,0.));
#86845=DIRECTION('ref_axis',(-0.922191781452919,0.,0.386732877087908));
#86846=DIRECTION('center_axis',(-0.913322802840698,2.13360716298275E-16,
-0.407236366022499));
#86847=DIRECTION('ref_axis',(-4.10189821923682E-14,1.,9.25185853854296E-14));
#86848=DIRECTION('center_axis',(0.,1.,0.));
#86849=DIRECTION('ref_axis',(0.916673510305537,0.,-0.399636929605016));
#86850=DIRECTION('center_axis',(0.,1.,0.));
#86851=DIRECTION('ref_axis',(0.916673510305537,0.,-0.399636929605016));
#86852=DIRECTION('center_axis',(-0.622024016430491,0.134731225190498,-0.77131940202639));
#86853=DIRECTION('ref_axis',(-0.266840017955903,-0.962591712338371,0.0470489123654965));
#86854=DIRECTION('center_axis',(0.,-1.,0.));
#86855=DIRECTION('ref_axis',(0.738951779496096,0.,-0.67375831540661));
#86856=DIRECTION('',(-6.43993943992487E-5,-0.999999997767879,-1.78033415409196E-5));
#86857=DIRECTION('center_axis',(0.,-1.,0.));
#86858=DIRECTION('ref_axis',(-0.278163242525689,0.,0.960533815389961));
#86859=DIRECTION('center_axis',(0.,1.,0.));
#86860=DIRECTION('ref_axis',(0.263821366478493,0.,-0.964571555971573));
#86861=DIRECTION('center_axis',(-0.998752834435612,0.,0.0499277048023606));
#86862=DIRECTION('ref_axis',(-0.0499277048023606,0.,-0.998752834435612));
#86863=DIRECTION('center_axis',(0.,1.,0.));
#86864=DIRECTION('ref_axis',(0.271911425253992,0.,-0.962322283237972));
#86865=DIRECTION('center_axis',(0.,1.,0.));
#86866=DIRECTION('ref_axis',(1.,0.,0.));
#86867=DIRECTION('center_axis',(0.,1.,0.));
#86868=DIRECTION('ref_axis',(-0.0499277048023506,0.,-0.998752834435612));
#86869=DIRECTION('center_axis',(0.,1.,0.));
#86870=DIRECTION('ref_axis',(-0.92054989510347,0.,-0.390624999999987));
#86871=DIRECTION('center_axis',(0.,-1.,0.));
#86872=DIRECTION('ref_axis',(-0.515104509808459,0.,0.857127379083755));
#86873=DIRECTION('center_axis',(0.308869563633509,0.,0.951104406813913));
#86874=DIRECTION('ref_axis',(-0.951104406813913,0.,0.308869563633509));
#86875=DIRECTION('center_axis',(0.,1.,0.));
#86876=DIRECTION('ref_axis',(-0.951104406813913,0.,0.308869563633509));
#86877=DIRECTION('center_axis',(-0.173648177666902,0.,-0.984807753012213));
#86878=DIRECTION('ref_axis',(-0.984807753012213,0.,0.173648177666902));
#86879=DIRECTION('',(-6.30405482876974E-6,-0.999999999979658,9.7046148712086E-7));
#86880=DIRECTION('center_axis',(0.970634532808316,-0.169018497876731,-0.171176374232767));
#86881=DIRECTION('ref_axis',(0.160171782561879,0.98499010992977,-0.0643388172994282));
#86882=DIRECTION('center_axis',(0.0431678122391723,-0.0175769693413298,
0.998913204505405));
#86883=DIRECTION('ref_axis',(-0.000608192349912218,-0.999845501768985,-0.0175670912330945));
#86884=DIRECTION('center_axis',(0.,1.,0.));
#86885=DIRECTION('ref_axis',(1.,0.,0.));
#86886=DIRECTION('center_axis',(0.,1.,0.));
#86887=DIRECTION('ref_axis',(-0.926972158432388,0.,0.375130134075095));
#86888=DIRECTION('center_axis',(0.,1.,0.));
#86889=DIRECTION('ref_axis',(-0.92054989510347,0.,0.390624999999989));
#86890=DIRECTION('center_axis',(0.,1.,0.));
#86891=DIRECTION('ref_axis',(0.946765333984011,0.,-0.321924528991104));
#86892=DIRECTION('center_axis',(0.390624999999987,0.,0.92054989510347));
#86893=DIRECTION('ref_axis',(-0.92054989510347,0.,0.390624999999987));
#86894=DIRECTION('center_axis',(0.,1.,0.));
#86895=DIRECTION('ref_axis',(-0.92054989510347,0.,0.390624999999988));
#86896=DIRECTION('center_axis',(0.,1.,0.));
#86897=DIRECTION('ref_axis',(1.,0.,0.));
#86898=DIRECTION('',(1.04371427654077E-6,-0.999999999999347,-4.65377558618838E-7));
#86899=DIRECTION('center_axis',(0.,1.,0.));
#86900=DIRECTION('ref_axis',(0.945670538570915,0.,-0.325126486892404));
#86901=DIRECTION('center_axis',(0.,1.,0.));
#86902=DIRECTION('ref_axis',(-0.92054989510347,0.,0.390624999999988));
#86903=DIRECTION('center_axis',(0.390624999999987,-8.10565941154282E-16,
0.92054989510347));
#86904=DIRECTION('ref_axis',(4.56810515340559E-14,1.,-1.85037170770859E-14));
#86905=DIRECTION('center_axis',(0.,1.,0.));
#86906=DIRECTION('ref_axis',(-0.92054989510347,0.,0.390624999999988));
#86907=DIRECTION('center_axis',(0.,1.,0.));
#86908=DIRECTION('ref_axis',(1.,0.,0.));
#86909=DIRECTION('center_axis',(0.,1.,0.));
#86910=DIRECTION('ref_axis',(-0.92054989510347,0.,-0.390624999999987));
#86911=DIRECTION('center_axis',(0.,1.,0.));
#86912=DIRECTION('ref_axis',(0.407236366022499,0.,-0.913322802840698));
#86913=DIRECTION('center_axis',(0.,-1.,0.));
#86914=DIRECTION('ref_axis',(-0.4961343040974,0.,0.868245790256301));
#86915=DIRECTION('center_axis',(-0.390624999999987,0.,0.92054989510347));
#86916=DIRECTION('ref_axis',(0.,1.,0.));
#86917=DIRECTION('center_axis',(0.,1.,0.));
#86918=DIRECTION('ref_axis',(0.407236366022499,0.,-0.913322802840698));
#86919=DIRECTION('center_axis',(0.,1.,0.));
#86920=DIRECTION('ref_axis',(1.,0.,0.));
#86921=DIRECTION('',(-1.53786555571077E-6,0.999999999998582,-6.8571404094823E-7));
#86922=DIRECTION('center_axis',(0.,-1.,0.));
#86923=DIRECTION('ref_axis',(-1.,0.,0.));
#86924=DIRECTION('',(4.22571058986286E-5,0.999999999107167,5.65750982326781E-8));
#86925=DIRECTION('center_axis',(0.,-1.,0.));
#86926=DIRECTION('ref_axis',(-0.467917575539515,0.,0.88377211004943));
#86927=DIRECTION('center_axis',(-0.390624999999987,0.,0.92054989510347));
#86928=DIRECTION('ref_axis',(-0.92054989510347,0.,-0.390624999999987));
#86929=DIRECTION('center_axis',(0.,1.,0.));
#86930=DIRECTION('ref_axis',(-0.0499277048023506,0.,-0.998752834435612));
#86931=DIRECTION('center_axis',(0.,-1.,0.));
#86932=DIRECTION('ref_axis',(0.916639684291378,0.,0.399714509596791));
#86933=DIRECTION('center_axis',(0.,-1.,0.));
#86934=DIRECTION('ref_axis',(-0.515086222159914,0.,0.857138369075278));
#86935=DIRECTION('center_axis',(0.,-1.,0.));
#86936=DIRECTION('ref_axis',(0.91633435450131,0.,0.400413974232504));
#86937=DIRECTION('center_axis',(0.,1.,0.));
#86938=DIRECTION('ref_axis',(1.,0.,0.));
#86939=DIRECTION('',(0.,-1.,0.));
#86940=DIRECTION('center_axis',(0.,-1.,0.));
#86941=DIRECTION('ref_axis',(-1.,0.,0.));
#86942=DIRECTION('center_axis',(0.,1.,0.));
#86943=DIRECTION('ref_axis',(-0.948871785268399,0.,0.3156617416184));
#86944=DIRECTION('center_axis',(0.,-1.,0.));
#86945=DIRECTION('ref_axis',(0.91474129068957,0.,0.404040061265687));
#86946=DIRECTION('center_axis',(0.,1.,0.));
#86947=DIRECTION('ref_axis',(-0.92054989510347,0.,-0.390624999999987));
#86948=DIRECTION('center_axis',(0.,-1.,0.));
#86949=DIRECTION('ref_axis',(-1.,0.,0.));
#86950=DIRECTION('',(0.,1.,0.));
#86951=DIRECTION('center_axis',(0.,-1.,0.));
#86952=DIRECTION('ref_axis',(-1.,0.,0.));
#86953=DIRECTION('center_axis',(-0.224095358856088,0.819067467960532,-0.528119070918561));
#86954=DIRECTION('ref_axis',(0.463977785912221,-0.386881508811817,-0.796898558362032));
#86955=DIRECTION('center_axis',(-0.246837407809856,0.623230767295425,-0.742061119317046));
#86956=DIRECTION('ref_axis',(0.539791218156059,-0.547528396775396,-0.63940448506885));
#86957=DIRECTION('center_axis',(0.246857274377899,-0.623239151827494,-0.742047468640693));
#86958=DIRECTION('ref_axis',(0.948871848468687,1.0093306299581E-7,0.315661551639739));
#86959=DIRECTION('center_axis',(0.000234595565147093,-0.999999938412346,
0.000261036827030693));
#86960=DIRECTION('ref_axis',(0.426145025547988,0.000336119971929968,0.90465479837564));
#86961=DIRECTION('center_axis',(-0.224070766742793,-0.819060243879251,0.528140708890878));
#86962=DIRECTION('ref_axis',(0.463992687595474,0.386903384656539,0.796879261117545));
#86963=DIRECTION('center_axis',(-2.61370721960272E-5,-2.03256955069848E-6,
0.999999999656361));
#86964=DIRECTION('ref_axis',(0.724569107033424,0.689202153739462,2.03389663803666E-5));
#86965=DIRECTION('center_axis',(-0.213402506147939,-0.824296876250407,-0.524398732048048));
#86966=DIRECTION('ref_axis',(8.7042714726054E-6,0.536761814042771,-0.843733817569113));
#86967=DIRECTION('center_axis',(0.213403354295598,-0.824295992344205,0.524399776297312));
#86968=DIRECTION('ref_axis',(-0.463992645966795,0.386850387757512,0.796905014402968));
#86969=DIRECTION('center_axis',(0.166308270996678,-0.675248184444775,0.718596860835149));
#86970=DIRECTION('ref_axis',(1.12997034448066E-5,-0.728744204079672,-0.684786013943481));
#86971=DIRECTION('center_axis',(-0.166317165768798,0.675241121871308,0.718601438702019));
#86972=DIRECTION('ref_axis',(-0.539788588710075,0.547519703716366,-0.639414148686693));
#86973=DIRECTION('center_axis',(-0.213391375091325,0.824299649237854,0.52439890284304));
#86974=DIRECTION('ref_axis',(1.03309119588017E-5,-0.53676035334655,0.843734746806459));
#86975=DIRECTION('center_axis',(0.21337795284944,0.824302204958805,-0.524400347194617));
#86976=DIRECTION('ref_axis',(-4.47031203145252E-5,0.536770362230098,0.843728378231407));
#86977=DIRECTION('center_axis',(-1.,0.,0.));
#86978=DIRECTION('ref_axis',(0.,0.,1.));
#86979=DIRECTION('',(-0.500066124153989,-0.76271838947367,-0.410115264081084));
#86980=DIRECTION('',(-1.,0.,-3.55271367880069E-14));
#86981=DIRECTION('',(-0.500661336716138,0.762431358709554,0.409922735614791));
#86982=DIRECTION('center_axis',(-1.,0.,0.));
#86983=DIRECTION('ref_axis',(0.,0.,1.));
#86984=DIRECTION('center_axis',(1.,0.,0.));
#86985=DIRECTION('ref_axis',(0.,1.,0.));
#86986=DIRECTION('',(0.,0.5,0.866025403784439));
#86987=DIRECTION('',(0.,1.,-1.14462064665688E-15));
#86988=DIRECTION('',(0.,0.5,-0.866025403784439));
#86989=DIRECTION('',(0.,-0.5,-0.866025403784438));
#86990=DIRECTION('',(0.,-1.,3.29078435913854E-15));
#86991=DIRECTION('',(0.,-0.5,0.866025403784439));
#86992=DIRECTION('center_axis',(0.,-0.866025403784439,0.5));
#86993=DIRECTION('ref_axis',(-1.,0.,0.));
#86994=DIRECTION('',(-1.,0.,0.));
#86995=DIRECTION('',(-1.,0.,0.));
#86996=DIRECTION('center_axis',(0.,1.14462064665688E-15,1.));
#86997=DIRECTION('ref_axis',(0.,-1.,1.14462064665688E-15));
#86998=DIRECTION('',(-1.,0.,0.));
#86999=DIRECTION('center_axis',(0.,0.866025403784439,0.5));
#87000=DIRECTION('ref_axis',(1.,0.,0.));
#87001=DIRECTION('',(-1.,0.,0.));
#87002=DIRECTION('center_axis',(0.,0.866025403784438,-0.5));
#87003=DIRECTION('ref_axis',(-1.,0.,0.));
#87004=DIRECTION('',(-1.,0.,0.));
#87005=DIRECTION('center_axis',(0.,-3.29078435913854E-15,-1.));
#87006=DIRECTION('ref_axis',(0.,-1.,3.29078435913854E-15));
#87007=DIRECTION('',(-1.,0.,0.));
#87008=DIRECTION('center_axis',(0.,-0.866025403784439,-0.5));
#87009=DIRECTION('ref_axis',(0.,0.5,-0.866025403784439));
#87010=DIRECTION('center_axis',(1.,0.,0.));
#87011=DIRECTION('ref_axis',(0.,1.,0.));
#87012=DIRECTION('center_axis',(-1.,0.,0.));
#87013=DIRECTION('ref_axis',(0.,0.,1.));
#87014=DIRECTION('center_axis',(0.173648177666902,6.04454757851474E-16,
0.984807753012213));
#87015=DIRECTION('ref_axis',(-0.463438942593986,0.882352941176469,0.0817167894903066));
#87016=DIRECTION('',(0.173648126084303,-1.16611032631002E-8,0.984807762107616));
#87017=DIRECTION('center_axis',(0.173648177666898,0.,0.984807753012214));
#87018=DIRECTION('ref_axis',(-0.984807753012214,0.,0.173648177666898));
#87019=DIRECTION('',(0.173648177666902,2.95597971572804E-8,0.984807753012213));
#87020=DIRECTION('center_axis',(0.173648177666903,-2.0600805012489E-15,
0.984807753012213));
#87021=DIRECTION('ref_axis',(0.4634392991042,-0.882352748104395,-0.0817168523526793));
#87022=DIRECTION('center_axis',(-0.95118330404232,-5.76953425511624E-6,
0.308626509032921));
#87023=DIRECTION('ref_axis',(5.44496996660637E-6,0.999999999355918,3.54755617336676E-5));
#87024=DIRECTION('center_axis',(0.984807753012213,0.,-0.173648177666902));
#87025=DIRECTION('ref_axis',(0.,1.,0.));
#87026=DIRECTION('center_axis',(0.984807753012213,0.,-0.173648177666902));
#87027=DIRECTION('ref_axis',(0.,-1.,0.));
#87028=DIRECTION('',(0.984807768899111,5.32100394428906E-13,-0.173648087567802));
#87029=DIRECTION('center_axis',(0.984807753012207,1.14048525880399E-7,-0.173648177666901));
#87030=DIRECTION('ref_axis',(1.12315871800155E-7,-0.999999999999994,-1.98043226913534E-8));
#87031=DIRECTION('',(0.984807714044911,-4.85499100747805E-8,-0.173648398661302));
#87032=DIRECTION('center_axis',(-0.173648177666902,0.,-0.984807753012213));
#87033=DIRECTION('ref_axis',(0.,-1.,0.));
#87034=DIRECTION('',(-0.173648177666902,0.,-0.984807753012213));
#87035=DIRECTION('center_axis',(0.173648177666907,0.,0.984807753012212));
#87036=DIRECTION('ref_axis',(-0.984807753012212,0.,0.173648177666907));
#87037=DIRECTION('center_axis',(-0.984807753012213,0.,0.173648177666903));
#87038=DIRECTION('ref_axis',(-0.173648177666903,0.,-0.984807753012213));
#87039=DIRECTION('',(-0.984807752772238,-4.00549727818515E-7,0.173648179027407));
#87040=DIRECTION('center_axis',(-0.984807753012213,0.,0.173648177666902));
#87041=DIRECTION('ref_axis',(0.173648177666902,0.,0.984807753012213));
#87042=DIRECTION('',(-0.984807753012213,0.,0.173648177666902));
#87043=DIRECTION('center_axis',(0.159552933030562,0.394801167068611,0.90480655393438));
#87044=DIRECTION('ref_axis',(0.116380632029358,0.902634096597889,-0.414375718578394));
#87045=DIRECTION('center_axis',(0.984807755014784,-3.72227084958571E-8,
-0.173648166309755));
#87046=DIRECTION('ref_axis',(0.173219343573378,0.0702347132572566,0.982375765206817));
#87047=DIRECTION('center_axis',(-0.984807753012213,0.,0.173648177666902));
#87048=DIRECTION('ref_axis',(0.,1.,0.));
#87049=DIRECTION('',(0.,-1.,0.));
#87050=DIRECTION('',(-9.4026263796054E-8,-0.999999999999844,-5.51330525790224E-7));
#87051=DIRECTION('center_axis',(0.868839919953252,0.434334769816394,0.237635227237391));
#87052=DIRECTION('ref_axis',(0.469231347474836,-0.569298881243943,-0.675070904691755));
#87053=DIRECTION('center_axis',(0.,-1.,0.));
#87054=DIRECTION('ref_axis',(0.263820905625295,0.,-0.964571682020081));
#87055=DIRECTION('center_axis',(-0.868839778608605,-0.434333710023902,-0.237637681027702));
#87056=DIRECTION('ref_axis',(0.263821400093756,4.3081659164672E-8,-0.964571546777412));
#87057=DIRECTION('center_axis',(-0.173648177666902,0.,-0.984807753012213));
#87058=DIRECTION('ref_axis',(-0.984807753012213,0.,0.173648177666902));
#87059=DIRECTION('center_axis',(0.173648177666902,0.,0.984807753012213));
#87060=DIRECTION('ref_axis',(-0.984807753012213,0.,0.173648177666902));
#87061=DIRECTION('center_axis',(-0.173648177666902,0.,-0.984807753012213));
#87062=DIRECTION('ref_axis',(-0.984807753012213,0.,0.173648177666902));
#87063=DIRECTION('center_axis',(-0.173648177666902,0.,-0.984807753012213));
#87064=DIRECTION('ref_axis',(-0.984807753012213,0.,0.173648177666902));
#87065=DIRECTION('',(0.984807753012213,0.,-0.173648177666902));
#87066=DIRECTION('center_axis',(0.173648177666902,0.,0.984807753012213));
#87067=DIRECTION('ref_axis',(0.984807753012213,0.,-0.173648177666902));
#87068=DIRECTION('center_axis',(0.173648177666902,0.,0.984807753012213));
#87069=DIRECTION('ref_axis',(-0.984807753012213,0.,0.173648177666902));
#87070=DIRECTION('',(0.173648177666902,0.,0.984807753012213));
#87071=DIRECTION('center_axis',(-0.393409542444277,-0.176889802087537,0.90218564044836));
#87072=DIRECTION('ref_axis',(-0.916641374847507,1.2837746409996E-5,-0.39971063252416));
#87073=DIRECTION('center_axis',(0.39758819974252,0.101304962457168,0.911954455006967));
#87074=DIRECTION('ref_axis',(-0.916670483337923,3.52527253137775E-6,0.399643872672397));
#87075=DIRECTION('center_axis',(-0.810495180234583,0.460325137160707,0.362213101522415));
#87076=DIRECTION('ref_axis',(-0.407809813917888,0.000427669905792924,-0.913066795349995));
#87077=DIRECTION('center_axis',(-0.982739063229984,0.,0.184997117820396));
#87078=DIRECTION('ref_axis',(0.184997117820396,0.,0.982739063229984));
#87079=DIRECTION('center_axis',(0.970623774538595,0.169109840258299,-0.171147159568199));
#87080=DIRECTION('ref_axis',(0.160257422681418,-0.984973277091295,-0.0643832423192878));
#87081=DIRECTION('center_axis',(-0.173654718138959,-9.74544300691725E-6,
-0.984806599679909));
#87082=DIRECTION('ref_axis',(8.88767218123285E-5,0.999999995723609,-2.55677663475359E-5));
#87083=DIRECTION('center_axis',(-0.0432132455015585,-0.0171107728542251,
-0.99891933451383));
#87084=DIRECTION('ref_axis',(-0.000613241581050437,0.999853592022779,-0.0171002471885266));
#87085=DIRECTION('center_axis',(0.,-1.,0.));
#87086=DIRECTION('ref_axis',(0.,0.,-1.));
#87087=DIRECTION('center_axis',(0.,-1.,0.));
#87088=DIRECTION('ref_axis',(0.184998949610495,0.,0.982738718400274));
#87089=DIRECTION('center_axis',(0.,-1.,0.));
#87090=DIRECTION('ref_axis',(-0.92054989510347,0.,0.390624999999987));
#87091=DIRECTION('center_axis',(-0.173648177666902,0.,-0.984807753012213));
#87092=DIRECTION('ref_axis',(-0.984807753012213,0.,0.173648177666902));
#87093=DIRECTION('',(3.02443292467696E-8,-0.999999999999985,1.68898496137498E-7));
#87094=DIRECTION('center_axis',(0.,1.,0.));
#87095=DIRECTION('ref_axis',(-0.515104509808457,0.,0.857127379083756));
#87096=DIRECTION('center_axis',(-0.308869563633509,0.,-0.951104406813913));
#87097=DIRECTION('ref_axis',(-0.951104406813913,0.,0.308869563633509));
#87098=DIRECTION('center_axis',(0.,-1.,0.));
#87099=DIRECTION('ref_axis',(0.173648177666902,0.,0.984807753012213));
#87100=DIRECTION('center_axis',(0.,-1.,0.));
#87101=DIRECTION('ref_axis',(0.,0.,-1.));
#87102=DIRECTION('center_axis',(0.,-1.,0.));
#87103=DIRECTION('ref_axis',(-0.951104406813915,0.,0.308869563633505));
#87104=DIRECTION('center_axis',(0.,-1.,0.));
#87105=DIRECTION('ref_axis',(-0.92054989510347,0.,-0.390624999999987));
#87106=DIRECTION('center_axis',(0.,-1.,0.));
#87107=DIRECTION('ref_axis',(-0.0499277048023606,0.,-0.998752834435612));
#87108=DIRECTION('center_axis',(0.,-1.,0.));
#87109=DIRECTION('ref_axis',(0.0559121723748785,0.,0.998435690958773));
#87110=DIRECTION('center_axis',(0.998752834435612,0.,-0.0499277048023606));
#87111=DIRECTION('ref_axis',(-0.0499277048023606,0.,-0.998752834435612));
#87112=DIRECTION('center_axis',(0.,-1.,0.));
#87113=DIRECTION('ref_axis',(-0.0499277048023606,0.,-0.998752834435612));
#87114=DIRECTION('center_axis',(0.,-1.,0.));
#87115=DIRECTION('ref_axis',(0.738977760494908,0.,-0.673729819359312));
#87116=DIRECTION('',(4.15986094482921E-5,-0.999999999067449,1.16041817154406E-5));
#87117=DIRECTION('center_axis',(0.622026863566978,0.134727224711234,0.771317804748883));
#87118=DIRECTION('ref_axis',(-0.778414735295653,-1.07091660949363E-6,0.627750348365854));
#87119=DIRECTION('center_axis',(0.,1.,0.));
#87120=DIRECTION('ref_axis',(-0.38894989240481,0.,0.921258911055023));
#87121=DIRECTION('center_axis',(0.399636929605016,3.72066793566512E-15,
0.916673510305537));
#87122=DIRECTION('ref_axis',(-5.43546689139399E-14,-1.,2.77555756156289E-14));
#87123=DIRECTION('center_axis',(0.,-1.,0.));
#87124=DIRECTION('ref_axis',(0.407236366022499,0.,-0.913322802840698));
#87125=DIRECTION('center_axis',(0.913322802840698,0.,0.407236366022499));
#87126=DIRECTION('ref_axis',(0.,-1.,0.));
#87127=DIRECTION('center_axis',(0.,-1.,0.));
#87128=DIRECTION('ref_axis',(0.407236366022499,0.,-0.913322802840698));
#87129=DIRECTION('center_axis',(0.,1.,0.));
#87130=DIRECTION('ref_axis',(-0.888996404394544,0.,0.457914176427824));
#87131=DIRECTION('center_axis',(-0.399636929605016,0.,0.916673510305537));
#87132=DIRECTION('ref_axis',(0.,-1.,0.));
#87133=DIRECTION('center_axis',(0.,-1.,0.));
#87134=DIRECTION('ref_axis',(0.916673510305537,0.,-0.399636929605016));
#87135=DIRECTION('center_axis',(0.,1.,0.));
#87136=DIRECTION('ref_axis',(-0.924457470735394,0.,-0.381285175166198));
#87137=DIRECTION('center_axis',(-0.913322802840698,7.76865850722253E-16,
0.407236366022499));
#87138=DIRECTION('ref_axis',(-4.21031843648538E-14,-1.,-9.25185853854296E-14));
#87139=DIRECTION('center_axis',(0.,-1.,0.));
#87140=DIRECTION('ref_axis',(0.916673510305537,0.,0.399636929605016));
#87141=DIRECTION('center_axis',(0.,-1.,0.));
#87142=DIRECTION('ref_axis',(0.916673510305537,0.,0.399636929605016));
#87143=DIRECTION('center_axis',(0.,1.,0.));
#87144=DIRECTION('ref_axis',(1.,0.,0.));
#87145=DIRECTION('',(-1.08852304226319E-6,-0.99999999999929,4.85357233595664E-7));
#87146=DIRECTION('center_axis',(0.,1.,0.));
#87147=DIRECTION('ref_axis',(-0.467905576874307,0.,-0.883778462698612));
#87148=DIRECTION('center_axis',(-0.390624999999987,0.,-0.92054989510347));
#87149=DIRECTION('ref_axis',(-0.92054989510347,0.,0.390624999999987));
#87150=DIRECTION('center_axis',(0.,-1.,0.));
#87151=DIRECTION('ref_axis',(0.184972798800006,0.,0.98274364088713));
#87152=DIRECTION('center_axis',(0.,-1.,0.));
#87153=DIRECTION('ref_axis',(0.915933776184509,0.,-0.401329437799404));
#87154=DIRECTION('center_axis',(0.,-1.,0.));
#87155=DIRECTION('ref_axis',(-0.515104509731028,0.,0.857127379130289));
#87156=DIRECTION('center_axis',(0.,-1.,0.));
#87157=DIRECTION('ref_axis',(0.931383237830313,0.,-0.364040195979405));
#87158=DIRECTION('center_axis',(0.390624999999987,0.,-0.92054989510347));
#87159=DIRECTION('ref_axis',(-0.92054989510347,0.,-0.390624999999987));
#87160=DIRECTION('center_axis',(0.,-1.,0.));
#87161=DIRECTION('ref_axis',(0.946765333984011,0.,0.321924528991104));
#87162=DIRECTION('center_axis',(0.,-1.,0.));
#87163=DIRECTION('ref_axis',(-0.92054989510347,0.,-0.390624999999988));
#87164=DIRECTION('center_axis',(0.,-1.,0.));
#87165=DIRECTION('ref_axis',(-1.,0.,0.));
#87166=DIRECTION('',(3.339300040861E-5,0.999999999434799,-3.912721493535E-6));
#87167=DIRECTION('center_axis',(0.,1.,0.));
#87168=DIRECTION('ref_axis',(1.,0.,0.));
#87169=DIRECTION('',(-1.5281607930716E-6,-0.9999999999986,-6.81386790616307E-7));
#87170=DIRECTION('center_axis',(0.,-1.,0.));
#87171=DIRECTION('ref_axis',(0.945670538570914,0.,0.325126486892405));
#87172=DIRECTION('center_axis',(0.,-1.,0.));
#87173=DIRECTION('ref_axis',(-0.92054989510347,0.,-0.390624999999988));
#87174=DIRECTION('center_axis',(0.390624999999987,5.84690488553155E-16,
-0.92054989510347));
#87175=DIRECTION('ref_axis',(4.5102810375397E-14,-1.,1.85037170770859E-14));
#87176=DIRECTION('center_axis',(0.,-1.,0.));
#87177=DIRECTION('ref_axis',(-0.92054989510347,0.,-0.390624999999988));
#87178=DIRECTION('center_axis',(0.,1.,0.));
#87179=DIRECTION('ref_axis',(1.,0.,0.));
#87180=DIRECTION('center_axis',(0.,-1.,0.));
#87181=DIRECTION('ref_axis',(-0.92054989510347,0.,0.390624999999988));
#87182=DIRECTION('center_axis',(0.,-1.,0.));
#87183=DIRECTION('ref_axis',(0.407236366022499,0.,0.913322802840698));
#87184=DIRECTION('center_axis',(0.,1.,0.));
#87185=DIRECTION('ref_axis',(-0.496122516224214,0.,-0.868252525994226));
#87186=DIRECTION('center_axis',(-0.390624999999987,0.,-0.92054989510347));
#87187=DIRECTION('ref_axis',(0.,-1.,0.));
#87188=DIRECTION('center_axis',(0.,-1.,0.));
#87189=DIRECTION('ref_axis',(0.4072363660225,0.,0.913322802840698));
#87190=DIRECTION('center_axis',(0.,1.,0.));
#87191=DIRECTION('ref_axis',(1.,0.,0.));
#87192=DIRECTION('',(0.,-1.,0.));
#87193=DIRECTION('center_axis',(0.,-1.,0.));
#87194=DIRECTION('ref_axis',(-1.,0.,0.));
#87195=DIRECTION('',(0.,1.,0.));
#87196=DIRECTION('center_axis',(0.,-1.,0.));
#87197=DIRECTION('ref_axis',(-1.,0.,0.));
#87198=DIRECTION('center_axis',(0.,-1.,0.));
#87199=DIRECTION('ref_axis',(-0.948871785268399,0.,-0.3156617416184));
#87200=DIRECTION('center_axis',(0.,-1.,0.));
#87201=DIRECTION('ref_axis',(0.916481355130724,0.,-0.400077399633811));
#87202=DIRECTION('center_axis',(0.,-1.,0.));
#87203=DIRECTION('ref_axis',(-0.92054989510347,0.,0.390624999999987));
#87204=DIRECTION('center_axis',(0.,-1.,0.));
#87205=DIRECTION('ref_axis',(-1.,0.,0.));
#87206=DIRECTION('center_axis',(-0.224058386535214,0.819056424696978,-0.528151884012393));
#87207=DIRECTION('ref_axis',(0.464012190567123,-0.386908739989834,-0.796865304756443));
#87208=DIRECTION('center_axis',(0.000234595565451377,-0.999999938412346,
0.000261036827419178));
#87209=DIRECTION('ref_axis',(0.426145025549655,0.000336119972411781,0.904654798374854));
#87210=DIRECTION('center_axis',(-0.224095509272251,-0.819067663979687,0.528118703083757));
#87211=DIRECTION('ref_axis',(0.463970536020739,0.386884684319262,0.796901237760247));
#87212=DIRECTION('center_axis',(-0.246850867614741,-0.623236588607253,0.742051752763272));
#87213=DIRECTION('ref_axis',(0.539787633059408,0.547517821159986,0.639416567433424));
#87214=DIRECTION('center_axis',(0.0015456208083213,0.00171768113197915,
0.999997330310359));
#87215=DIRECTION('ref_axis',(0.550747471894769,0.834668797317559,-0.00228494769739675));
#87216=DIRECTION('center_axis',(0.246871071069859,0.623239366842138,0.742042698156266));
#87217=DIRECTION('ref_axis',(0.539806900209745,0.547489979087855,-0.639424141931102));
#87218=DIRECTION('center_axis',(-0.213357641816103,-0.824307171415416,-0.524400804568212));
#87219=DIRECTION('ref_axis',(-0.463983424918666,-0.386871231470338,0.796900264563495));
#87220=DIRECTION('center_axis',(0.213374617987456,-0.82430473740624,0.524397723382107));
#87221=DIRECTION('ref_axis',(-1.00295012044401E-5,-0.536760887317295,-0.843734407112664));
#87222=DIRECTION('center_axis',(-0.213391699957863,0.824299991802442,0.524398232170541));
#87223=DIRECTION('ref_axis',(1.69583914793472E-5,-0.536758484410448,0.843735935661041));
#87224=DIRECTION('center_axis',(0.213360527418366,0.824307096359649,-0.52439974850383));
#87225=DIRECTION('ref_axis',(-2.00487952037749E-5,0.53676311541999,0.843732989471594));
#87226=DIRECTION('center_axis',(0.1663438053302,0.675238304245454,-0.718597920194591));
#87227=DIRECTION('ref_axis',(8.19782755311054E-6,0.728750066126856,0.68477977558694));
#87228=DIRECTION('center_axis',(-1.,0.,0.));
#87229=DIRECTION('ref_axis',(0.,0.,1.));
#87230=DIRECTION('',(-0.500066124153987,0.762718389473674,-0.410115264081081));
#87231=DIRECTION('',(-0.500660779556073,-0.762417033624258,0.409950058731417));
#87232=DIRECTION('',(-1.,0.,-3.55271367880069E-14));
#87233=DIRECTION('center_axis',(1.,0.,0.));
#87234=DIRECTION('ref_axis',(0.,1.,0.));
#87235=DIRECTION('',(0.532111185932234,-0.738603577927986,0.413911150463199));
#87236=DIRECTION('',(-0.358455003852291,0.738603577927671,0.570941997829637));
#87237=DIRECTION('center_axis',(-0.839921904894139,-0.522108531837321,0.148100893520862));
#87238=DIRECTION('ref_axis',(-0.527930412690934,0.849287630521003,-5.13852122356239E-18));
#87239=DIRECTION('center_axis',(0.173648177666903,0.,0.984807753012213));
#87240=DIRECTION('ref_axis',(0.,-1.,0.));
#87241=DIRECTION('center_axis',(-0.173648177666902,0.,-0.984807753012213));
#87242=DIRECTION('ref_axis',(-0.984807753012213,0.,0.173648177666902));
#87243=DIRECTION('center_axis',(0.,1.,0.));
#87244=DIRECTION('ref_axis',(1.,0.,0.));
#87245=DIRECTION('',(-0.984807753012213,0.,0.173648177666902));
#87246=DIRECTION('',(-0.173648177666902,0.,-0.984807753012213));
#87247=DIRECTION('',(-0.984807753012213,0.,0.173648177666902));
#87248=DIRECTION('',(-0.173651710791594,1.14934020021696E-8,-0.984807130020469));
#87249=DIRECTION('center_axis',(0.,-1.,0.));
#87250=DIRECTION('ref_axis',(-0.984807753012213,0.,0.173648177666903));
#87251=DIRECTION('center_axis',(0.,-1.,0.));
#87252=DIRECTION('ref_axis',(-0.0499277048023606,0.,-0.998752834435612));
#87253=DIRECTION('center_axis',(0.,-1.,0.));
#87254=DIRECTION('ref_axis',(-0.92054989510347,0.,-0.390624999999987));
#87255=DIRECTION('center_axis',(0.,-1.,0.));
#87256=DIRECTION('ref_axis',(-0.951104406813915,0.,0.308869563633505));
#87257=DIRECTION('center_axis',(0.,-1.,0.));
#87258=DIRECTION('ref_axis',(0.173648177666904,0.,0.984807753012213));
#87259=DIRECTION('center_axis',(0.,-1.,0.));
#87260=DIRECTION('ref_axis',(0.,0.,-1.));
#87261=DIRECTION('',(0.984807753012213,0.,-0.173648177666902));
#87262=DIRECTION('',(0.173648177666902,0.,0.984807753012213));
#87263=DIRECTION('',(0.984807753012213,0.,-0.173648177666902));
#87264=DIRECTION('center_axis',(0.,1.,0.));
#87265=DIRECTION('ref_axis',(-0.951104406813942,0.,0.30886956363342));
#87266=DIRECTION('center_axis',(0.,1.,0.));
#87267=DIRECTION('ref_axis',(-0.92054989510347,0.,-0.390624999999987));
#87268=DIRECTION('center_axis',(0.,1.,0.));
#87269=DIRECTION('ref_axis',(-0.0499277048023606,0.,-0.998752834435612));
#87270=DIRECTION('center_axis',(0.,1.,0.));
#87271=DIRECTION('ref_axis',(0.3114756963496,0.,-0.9502541189511));
#87272=DIRECTION('center_axis',(0.,1.,0.));
#87273=DIRECTION('ref_axis',(-0.874458269240608,0.,-0.485100747635705));
#87274=DIRECTION('',(0.173722816438492,-3.55490858096083E-8,0.984794589266552));
#87275=DIRECTION('center_axis',(-0.173648177666902,0.,-0.984807753012213));
#87276=DIRECTION('ref_axis',(-0.984807753012213,0.,0.173648177666902));
#87277=DIRECTION('',(0.98480779821852,2.86780361313506E-5,-0.173647918920904));
#87278=DIRECTION('',(-2.619623158332E-9,1.,-1.484149674398E-8));
#87279=DIRECTION('center_axis',(-0.173738860884696,-3.29476084001257E-5,
-0.984791758258031));
#87280=DIRECTION('ref_axis',(0.227733791624276,0.972892847856778,-0.0402097841520986));
#87281=DIRECTION('center_axis',(-0.173648177666902,0.,-0.984807753012213));
#87282=DIRECTION('ref_axis',(-0.984807753012213,0.,0.173648177666902));
#87283=DIRECTION('',(-2.619623158332E-9,1.,-1.484149674398E-8));
#87284=DIRECTION('',(-0.984808118285514,2.85919679452004E-5,0.173646103732403));
#87285=DIRECTION('center_axis',(-0.173798222257865,3.70611714430505E-5,
-0.984781283619097));
#87286=DIRECTION('ref_axis',(-0.226415421385525,0.973209345122142,0.0399953438008206));
#87287=DIRECTION('center_axis',(0.984807753012213,0.,-0.173648177666903));
#87288=DIRECTION('ref_axis',(0.13914925430432,-0.598224410459968,0.789154636149579));
#87289=DIRECTION('center_axis',(0.984701214027571,0.00034783784991401,-0.174250962985741));
#87290=DIRECTION('ref_axis',(0.147000879085088,-0.538606975966355,0.829634417673586));
#87291=DIRECTION('center_axis',(0.984796609140205,0.000132133476650577,
-0.173711315597746));
#87292=DIRECTION('ref_axis',(0.0494872421690545,-0.95877571584193,0.279821620991475));
#87293=DIRECTION('',(0.98480819903795,7.61270752104513E-7,-0.173645648108583));
#87294=DIRECTION('center_axis',(0.984804385279843,1.83453921068791E-5,-0.173667274974411));
#87295=DIRECTION('ref_axis',(0.0493756213064273,-0.958761501507835,0.279890034204587));
#87296=DIRECTION('center_axis',(0.984807753012213,0.,-0.173648177666902));
#87297=DIRECTION('ref_axis',(0.,-1.,0.));
#87298=DIRECTION('',(0.,1.,0.));
#87299=DIRECTION('',(-0.173647957746888,-0.00166011264183791,-0.984806392544419));
#87300=DIRECTION('',(-5.36954384231574E-8,0.999999999999952,-3.04520965216585E-7));
#87301=DIRECTION('',(-0.173648177666902,0.,-0.984807753012213));
#87302=DIRECTION('center_axis',(-0.984807753012213,1.47875699429781E-16,
0.173648177666902));
#87303=DIRECTION('ref_axis',(0.118437015122884,0.731304063260744,0.671689690636314));
#87304=DIRECTION('center_axis',(-0.984807753012213,1.10906774572336E-17,
0.173648177666902));
#87305=DIRECTION('ref_axis',(0.173046420789886,0.0831790275611967,0.981395020175762));
#87306=DIRECTION('',(0.984807866755134,-7.84910877958438E-6,-0.173647532420113));
#87307=DIRECTION('center_axis',(0.984807753012213,-5.91502797719126E-17,
-0.173648177666902));
#87308=DIRECTION('ref_axis',(0.0712749837854421,0.911880281676684,0.404220519735993));
#87309=DIRECTION('',(-0.984807701359279,7.21578091369084E-7,0.173648470603496));
#87310=DIRECTION('center_axis',(-0.984807753012213,-2.95751398859563E-17,
0.173648177666903));
#87311=DIRECTION('ref_axis',(0.118437565749294,-0.731301105875289,0.671692813393862));
#87312=DIRECTION('center_axis',(0.984807753012213,2.66176258973607E-16,
-0.173648177666903));
#87313=DIRECTION('ref_axis',(0.119975660912596,-0.722938587260738,0.680415784530337));
#87314=DIRECTION('',(0.984807662516202,-6.24263663490926E-6,-0.173648690782289));
#87315=DIRECTION('center_axis',(-0.984807753012213,2.95751398859563E-16,
0.173648177666902));
#87316=DIRECTION('ref_axis',(0.0174472473523288,-0.994939614274932,0.0989482567116538));
#87317=DIRECTION('center_axis',(-0.984807753012213,-1.51942396384287E-16,
0.173648177666902));
#87318=DIRECTION('ref_axis',(-0.0915532115266896,-0.849720177918111,-0.519224064059017));
#87319=DIRECTION('',(-0.984807753012213,0.,0.173648177666902));
#87320=DIRECTION('center_axis',(-0.984807753012213,-3.08475197493174E-16,
0.173648177666902));
#87321=DIRECTION('ref_axis',(-0.148632496508293,-0.517074437493711,-0.84293677525202));
#87322=DIRECTION('',(0.984807705057875,5.76825355638144E-7,-0.173648449628293));
#87323=DIRECTION('center_axis',(-0.984807753012213,-2.93785902374558E-17,
0.173648177666902));
#87324=DIRECTION('ref_axis',(-0.091553228988867,0.84972011552227,-0.519224163091946));
#87325=DIRECTION('',(0.984807701171163,-6.23576923384803E-7,-0.173648471670733));
#87326=DIRECTION('center_axis',(-0.984807753012213,2.20339426780919E-16,
0.173648177666902));
#87327=DIRECTION('ref_axis',(-0.0751084169313667,0.901618518365397,-0.4259609994432));
#87328=DIRECTION('',(0.984807753012213,0.,-0.173648177666902));
#87329=DIRECTION('center_axis',(-4.5541240007271E-5,0.999999998908222,1.04666705814102E-5));
#87330=DIRECTION('ref_axis',(-0.729107486866968,-4.0367840113073E-5,0.684399204386571));
#87331=DIRECTION('center_axis',(-0.984807753012213,0.,0.173648177666902));
#87332=DIRECTION('ref_axis',(0.122787513031607,-0.707108456623977,0.696362590332343));
#87333=DIRECTION('center_axis',(-0.984807753012213,0.,0.173648177666902));
#87334=DIRECTION('ref_axis',(0.,-1.,0.));
#87335=DIRECTION('',(-0.984807753012213,0.,0.173648177666902));
#87336=DIRECTION('center_axis',(0.984807753012213,0.,-0.173648177666902));
#87337=DIRECTION('ref_axis',(0.122787512666764,0.707108458725017,0.696362588263213));
#87338=DIRECTION('',(0.984807753012213,0.,-0.173648177666902));
#87339=DIRECTION('center_axis',(0.984807753012213,0.,-0.173648177666902));
#87340=DIRECTION('ref_axis',(0.,1.,0.));
#87341=DIRECTION('center_axis',(-0.468047248986744,0.720808604941997,0.511240381579461));
#87342=DIRECTION('ref_axis',(0.149821931102216,-0.505420385471279,0.849766805018216));
#87343=DIRECTION('center_axis',(-0.984807752980486,8.02724707364289E-6,
0.173648177661298));
#87344=DIRECTION('ref_axis',(0.173648177647197,-2.42677927780413E-6,0.984807753012698));
#87345=DIRECTION('center_axis',(-0.984807753012213,0.,0.173648177666903));
#87346=DIRECTION('ref_axis',(0.1391482160283,0.598232419576064,0.789148747793665));
#87347=DIRECTION('center_axis',(0.,1.,0.));
#87348=DIRECTION('ref_axis',(-0.984807753012214,0.,0.173648177666898));
#87349=DIRECTION('center_axis',(5.99767279256134E-6,0.999999998756089,-4.95161662595558E-5));
#87350=DIRECTION('ref_axis',(-0.173665667877379,-4.77221618665076E-5,-0.984804667699793));
#87351=DIRECTION('',(3.128857622442E-9,1.,-1.424668953682E-8));
#87352=DIRECTION('center_axis',(0.325178856357606,0.402282522364151,0.85581977283672));
#87353=DIRECTION('ref_axis',(0.0712965070296305,-0.912858053252779,0.402003709804923));
#87354=DIRECTION('center_axis',(0.00953570295887386,-0.900814846469353,
0.434098701621504));
#87355=DIRECTION('ref_axis',(-0.495353769654611,-0.381364780402071,-0.780503393431346));
#87356=DIRECTION('center_axis',(0.540815948209504,0.356362088464686,0.76192136869059));
#87357=DIRECTION('ref_axis',(-0.235026539236875,-0.805720097908675,0.543670534129239));
#87358=DIRECTION('center_axis',(0.540853504125162,0.356471320596299,0.761843609061508));
#87359=DIRECTION('ref_axis',(0.0676210056074329,-0.921248442444026,0.383051833170259));
#87360=DIRECTION('center_axis',(-0.0822813569473299,-0.880495422945283,
-0.466859281230773));
#87361=DIRECTION('ref_axis',(0.988016782566545,-0.0106874206885076,-0.153976025425647));
#87362=DIRECTION('center_axis',(0.984806655704334,5.35809355578126E-6,-0.173654400611492));
#87363=DIRECTION('ref_axis',(0.140766524539594,0.585557533745896,0.798315201059373));
#87364=DIRECTION('center_axis',(-0.118543194053381,-0.732033583437037,-0.670875803605968));
#87365=DIRECTION('ref_axis',(0.979768502675954,-0.195953546642656,0.0406926126254334));
#87366=DIRECTION('center_axis',(-0.118296406893678,-0.732058422007768,-0.670892261755598));
#87367=DIRECTION('ref_axis',(-0.992860141709842,0.0767780069429456,0.0912900687576806));
#87368=DIRECTION('center_axis',(-0.0825005446561861,0.87918155882871,-0.46929036506938));
#87369=DIRECTION('ref_axis',(0.988854899622876,0.0136564674857691,-0.148254808986559));
#87370=DIRECTION('center_axis',(-0.984807753012326,-4.76834328723365E-13,
0.173648177666263));
#87371=DIRECTION('ref_axis',(0.119869363396271,-0.723523116755521,0.679812941359128));
#87372=DIRECTION('center_axis',(-0.118924556957068,0.728675399195287,-0.674454677765789));
#87373=DIRECTION('ref_axis',(-0.984804485455633,1.76838323664053E-5,0.173666706981354));
#87374=DIRECTION('center_axis',(-0.984806653083073,5.45304870040947E-6,
0.173654415473897));
#87375=DIRECTION('ref_axis',(0.14033160238962,-0.589008723332889,0.79584908444285));
#87376=DIRECTION('center_axis',(-0.119158532281579,0.728650964800672,-0.674439779134912));
#87377=DIRECTION('ref_axis',(0.977813440898981,0.203990901934536,0.0476296832367139));
#87378=DIRECTION('center_axis',(-0.172166082870035,0.000366553130519414,
-0.985067868498405));
#87379=DIRECTION('ref_axis',(-0.985067935878727,-2.329605698763E-5,0.172166085977808));
#87380=DIRECTION('center_axis',(0.,-1.,0.));
#87381=DIRECTION('ref_axis',(0.934249900475282,0.,-0.356619017246593));
#87382=DIRECTION('center_axis',(0.390624999999987,-2.7899036639383E-15,
-0.92054989510347));
#87383=DIRECTION('ref_axis',(1.89084858881472E-13,-1.,8.32667268468867E-14));
#87384=DIRECTION('center_axis',(-0.308869563633505,0.,-0.951104406813915));
#87385=DIRECTION('ref_axis',(0.,-1.,0.));
#87386=DIRECTION('center_axis',(0.,-1.,0.));
#87387=DIRECTION('ref_axis',(0.0556368722626882,0.,0.998451069629767));
#87388=DIRECTION('center_axis',(0.,-1.,0.));
#87389=DIRECTION('ref_axis',(-0.0499277048023606,0.,-0.998752834435612));
#87390=DIRECTION('center_axis',(0.998752834435612,-1.73393901318555E-16,
-0.0499277048023606));
#87391=DIRECTION('ref_axis',(-8.67361737988402E-16,-1.,-1.38777878078145E-14));
#87392=DIRECTION('center_axis',(0.,-1.,0.));
#87393=DIRECTION('ref_axis',(0.945670538570914,0.,0.325126486892406));
#87394=DIRECTION('center_axis',(0.,-1.,0.));
#87395=DIRECTION('ref_axis',(-0.92054989510347,0.,-0.390624999999988));
#87396=DIRECTION('center_axis',(0.,-1.,0.));
#87397=DIRECTION('ref_axis',(-1.,0.,0.));
#87398=DIRECTION('',(-2.877698079828E-14,1.,0.));
#87399=DIRECTION('center_axis',(0.,1.,0.));
#87400=DIRECTION('ref_axis',(-0.0499277048023506,0.,-0.998752834435612));
#87401=DIRECTION('center_axis',(0.,-1.,0.));
#87402=DIRECTION('ref_axis',(-0.496134304097401,0.,0.868245790256301));
#87403=DIRECTION('center_axis',(-0.390624999999987,1.64421355075197E-15,
0.92054989510347));
#87404=DIRECTION('ref_axis',(-1.21430643318377E-14,1.,-6.93889390390721E-15));
#87405=DIRECTION('center_axis',(-0.998752834435612,-8.63521945113378E-17,
0.0499277048023606));
#87406=DIRECTION('ref_axis',(1.30104260698261E-15,1.,2.77555756156289E-14));
#87407=DIRECTION('center_axis',(-0.173648177666902,0.,-0.984807753012213));
#87408=DIRECTION('ref_axis',(-0.984807753012213,0.,0.173648177666902));
#87409=DIRECTION('center_axis',(0.173648177666902,0.,0.984807753012213));
#87410=DIRECTION('ref_axis',(-0.984807753012213,0.,0.173648177666902));
#87411=DIRECTION('',(1.450155551197E-11,-1.,-2.556888034633E-12));
#87412=DIRECTION('center_axis',(0.984807753012213,0.,-0.173648177666902));
#87413=DIRECTION('ref_axis',(0.,-1.,0.));
#87414=DIRECTION('',(0.,1.,0.));
#87415=DIRECTION('',(0.173648177666902,0.,0.984807753012213));
#87416=DIRECTION('',(6.51332343039219E-8,0.99999999999993,3.69388507198911E-7));
#87417=DIRECTION('',(0.173648177370708,-5.92206446015928E-5,0.984807751283846));
#87418=DIRECTION('center_axis',(0.173648177666902,0.,0.984807753012213));
#87419=DIRECTION('ref_axis',(0.,1.,0.));
#87420=DIRECTION('center_axis',(0.173648177666898,0.,0.984807753012214));
#87421=DIRECTION('ref_axis',(-0.984807753012214,0.,0.173648177666898));
#87422=DIRECTION('center_axis',(0.173648177666902,0.,0.984807753012213));
#87423=DIRECTION('ref_axis',(0.,-1.,0.));
#87424=DIRECTION('center_axis',(0.0705615471450538,-0.994935989107725,0.0715782483910466));
#87425=DIRECTION('ref_axis',(-0.173073282542036,-0.0828800320757138,-0.981415579228928));
#87426=DIRECTION('center_axis',(-0.984807753012213,-3.59689602365803E-17,
0.173648177666902));
#87427=DIRECTION('ref_axis',(0.00203933837147199,-0.999931035895442,0.0115656626301812));
#87428=DIRECTION('center_axis',(0.984807753012213,-5.43782705938852E-17,
-0.173648177666902));
#87429=DIRECTION('ref_axis',(0.0865532966445691,0.866923871076506,0.490868137688406));
#87430=DIRECTION('center_axis',(-0.984807753012213,1.47875699429781E-16,
0.173648177666902));
#87431=DIRECTION('ref_axis',(-0.0023628809126313,-0.999907416559164,-0.013400563561729));
#87432=DIRECTION('center_axis',(0.984807753012213,-5.91502797719126E-17,
-0.173648177666902));
#87433=DIRECTION('ref_axis',(0.0467849591103274,0.963021699437997,0.265330688034002));
#87434=DIRECTION('',(-0.984807734026167,4.52289952656485E-7,0.173648285341494));
#87435=DIRECTION('center_axis',(0.984807753012213,3.99726500021128E-16,
-0.173648177666902));
#87436=DIRECTION('ref_axis',(0.00236288091262727,0.999907416559164,0.0134005635617093));
#87437=DIRECTION('',(0.984807753012213,0.,-0.173648177666902));
#87438=DIRECTION('',(0.984809659012493,-8.77532653136194E-6,-0.173637367633499));
#87439=DIRECTION('center_axis',(-0.984807753012213,3.51192997585509E-17,
0.173648177666903));
#87440=DIRECTION('ref_axis',(-0.173365149690665,-0.0570712691222515,-0.983202621596133));
#87441=DIRECTION('center_axis',(-0.172758048290314,0.100499036796366,-0.979823759843537));
#87442=DIRECTION('ref_axis',(0.984808733743122,-5.48978072977703E-5,-0.173642606895596));
#87443=DIRECTION('center_axis',(-0.984807753012213,7.02386062257915E-17,
0.173648177666903));
#87444=DIRECTION('ref_axis',(0.173046305904731,0.0831869535125862,0.981394368629666));
#87445=DIRECTION('center_axis',(-0.0143784831960099,0.996544562420649,-0.0818058331099832));
#87446=DIRECTION('ref_axis',(0.984809079270561,-4.49124382155832E-5,-0.173640650105737));
#87447=DIRECTION('center_axis',(-0.984807753012107,-8.63808404924054E-17,
0.173648177667502));
#87448=DIRECTION('ref_axis',(-0.172276800540999,0.125429352942195,-0.977030286846758));
#87449=DIRECTION('center_axis',(-0.984807753012108,6.73770473281316E-17,
0.1736481776675));
#87450=DIRECTION('ref_axis',(0.173048689248285,-0.0830223701171357,0.981407885239151));
#87451=DIRECTION('center_axis',(0.0144827209458809,0.996537080801731,0.0818785526323483));
#87452=DIRECTION('ref_axis',(0.984806418859583,-4.41489308059733E-5,-0.173655738240447));
#87453=DIRECTION('center_axis',(-0.984807753012107,-2.45183611171223E-18,
0.173648177667501));
#87454=DIRECTION('ref_axis',(0.173048500696551,-0.0830354026532529,0.981406815909125));
#87455=DIRECTION('center_axis',(-0.984807753012107,3.1873869452259E-17,
0.173648177667502));
#87456=DIRECTION('ref_axis',(0.173648177667502,9.94558247889318E-15,0.984807753012107));
#87457=DIRECTION('center_axis',(-0.984787402847089,4.77665004704958E-6,
0.173763549603677));
#87458=DIRECTION('ref_axis',(0.0460456062353661,-0.964243981143723,0.260985338619855));
#87459=DIRECTION('center_axis',(-0.984787403020211,-4.77668398007977E-6,
0.173763548622521));
#87460=DIRECTION('ref_axis',(-0.0460456142525782,-0.964243968000674,-0.260985385764066));
#87461=DIRECTION('',(0.984807753012107,0.,-0.173648177667501));
#87462=DIRECTION('center_axis',(0.778348606443954,9.80121874209452E-8,-0.62783233975859));
#87463=DIRECTION('ref_axis',(0.625005248891585,-0.0947925361689985,0.774843735178015));
#87464=DIRECTION('center_axis',(-0.984807753012107,3.1873869452259E-17,
0.173648177667502));
#87465=DIRECTION('ref_axis',(0.173648177660458,9.0068198248696E-6,0.984807752972162));
#87466=DIRECTION('center_axis',(0.416627933083572,-8.76783794334763E-5,
-0.909077091168297));
#87467=DIRECTION('ref_axis',(0.904296443220308,0.102460377442959,0.414427091094858));
#87468=DIRECTION('center_axis',(0.416694788203033,9.03336795019935E-5,-0.90904644838658));
#87469=DIRECTION('ref_axis',(0.903932694694705,-0.105961771702308,0.414340181975725));
#87470=DIRECTION('center_axis',(-0.173648177666902,0.,-0.984807753012213));
#87471=DIRECTION('ref_axis',(-0.984807753012213,0.,0.173648177666902));
#87472=DIRECTION('',(0.,-1.,0.));
#87473=DIRECTION('',(0.984807752993594,6.14919168343789E-6,-0.173648177663619));
#87474=DIRECTION('center_axis',(-0.173648177666902,3.60825379108868E-16,
-0.984807753012213));
#87475=DIRECTION('ref_axis',(0.791113853674831,0.595550245061522,-0.139494717215097));
#87476=DIRECTION('',(-0.98480775279897,2.08102296353245E-5,0.173648177629302));
#87477=DIRECTION('',(0.,-1.,0.));
#87478=DIRECTION('center_axis',(0.173648177666902,0.,0.984807753012213));
#87479=DIRECTION('ref_axis',(0.,-1.,0.));
#87480=DIRECTION('center_axis',(0.173648177666902,0.,0.984807753012213));
#87481=DIRECTION('ref_axis',(0.,-1.,0.));
#87482=DIRECTION('center_axis',(0.140833149244339,-0.988277940715504,0.0589299242239757));
#87483=DIRECTION('ref_axis',(-0.976574519445544,-0.128890957877333,0.172305916750323));
#87484=DIRECTION('center_axis',(-1.45716096092398E-7,-0.999999999999986,
-8.54998680566197E-8));
#87485=DIRECTION('ref_axis',(0.173652309740699,-1.0950480730089E-7,0.984807024407172));
#87486=DIRECTION('center_axis',(0.397005631927029,-5.6725704996324E-5,-0.91781617168168));
#87487=DIRECTION('ref_axis',(-0.618040008182569,0.739279070835237,-0.26738175650309));
#87488=DIRECTION('center_axis',(-0.984807753012213,2.46716227694479E-17,
0.173648177666903));
#87489=DIRECTION('ref_axis',(0.173648177666902,7.45831290246043E-11,0.984807753012213));
#87490=DIRECTION('center_axis',(0.396684871120988,8.29230411004112E-5,-0.917954849732542));
#87491=DIRECTION('ref_axis',(0.917617038505464,-0.0271629495190743,0.396536435675066));
#87492=DIRECTION('',(0.984807753012213,0.,-0.173648177666902));
#87493=DIRECTION('center_axis',(-0.984807752591731,-1.68263835837692E-10,
0.173648180051576));
#87494=DIRECTION('ref_axis',(0.173648180048437,-6.01398766220049E-6,0.984807752573921));
#87495=DIRECTION('center_axis',(-0.984807753398451,-2.54577945895623E-11,
0.173648175476438));
#87496=DIRECTION('ref_axis',(0.173046505047202,0.0831730633887027,0.981395510799539));
#87497=DIRECTION('',(0.984807753012213,0.,-0.173648177666902));
#87498=DIRECTION('center_axis',(-0.984807753012213,2.46716227694479E-17,
0.173648177666903));
#87499=DIRECTION('ref_axis',(0.173648177666902,1.30076688193796E-8,0.984807753012213));
#87500=DIRECTION('center_axis',(-0.686735486868187,-8.14046591486839E-5,
-0.726907397437388));
#87501=DIRECTION('ref_axis',(0.726646064054819,-0.0268893988940089,-0.686485584568794));
#87502=DIRECTION('',(0.984807753012213,0.,-0.173648177666902));
#87503=DIRECTION('center_axis',(0.516198321513486,-3.61900781727334E-6,
-0.856469084587157));
#87504=DIRECTION('ref_axis',(0.856468926804281,0.00060919642574273,0.516198223842778));
#87505=DIRECTION('',(0.984807753012213,0.,-0.173648177666902));
#87506=DIRECTION('center_axis',(-0.686740422865691,8.08918317377472E-5,
-0.726902734249063));
#87507=DIRECTION('ref_axis',(0.72661180009037,0.0283664668836154,-0.686462406491407));
#87508=DIRECTION('center_axis',(-0.984807753012213,1.09651656753102E-17,
0.173648177666902));
#87509=DIRECTION('ref_axis',(0.118437018843228,0.731304043279059,0.671689711735432));
#87510=DIRECTION('',(-0.984807851409346,7.72996941407336E-9,0.173647619628108));
#87511=DIRECTION('center_axis',(0.112178949404874,0.988278168362575,-0.103547792097819));
#87512=DIRECTION('ref_axis',(0.95746136560598,-0.0796203342802649,0.277359578419478));
#87513=DIRECTION('center_axis',(8.73464525969481E-8,0.999999999999991,-1.05573893634399E-7));
#87514=DIRECTION('ref_axis',(0.17364493317501,8.88027804399136E-8,0.984808325098158));
#87515=DIRECTION('center_axis',(-0.112184478285304,0.988277949487833,0.10354389111859));
#87516=DIRECTION('ref_axis',(0.976611185680797,0.128891163139917,-0.172097821216851));
#87517=DIRECTION('center_axis',(-0.140829727433864,-0.98827813488146,-0.0589348452625973));
#87518=DIRECTION('ref_axis',(0.805607533053029,-0.0797909770181293,-0.587051873921466));
#87519=DIRECTION('center_axis',(-0.984807753012213,-3.0154205607103E-17,
0.173648177666903));
#87520=DIRECTION('ref_axis',(-0.173046420789344,0.083179027598608,-0.981395020172686));
#87521=DIRECTION('',(0.984807681305532,-5.61027557369018E-9,-0.173648584335206));
#87522=DIRECTION('',(0.984807945990428,-1.26003174213104E-13,-0.173647083229505));
#87523=DIRECTION('center_axis',(-0.984807753031958,3.17862934597828E-11,
0.173648177554921));
#87524=DIRECTION('ref_axis',(-0.0511404417972143,-0.955649609771606,-0.290031857829726));
#87525=DIRECTION('center_axis',(-0.984807753012213,-9.71445146547012E-17,
0.173648177666902));
#87526=DIRECTION('ref_axis',(-0.0915527669893199,0.849721766333212,-0.519221542962313));
#87527=DIRECTION('',(0.984807753012213,0.,-0.173648177666902));
#87528=DIRECTION('',(0.984807789518797,4.35503035001299E-7,-0.1736479706271));
#87529=DIRECTION('center_axis',(-0.454554571362216,-0.76693110554782,0.452986557192275));
#87530=DIRECTION('ref_axis',(-0.81199513940023,0.565830688971329,0.143176551881345));
#87531=DIRECTION('center_axis',(-0.984807753012213,-3.5605199344424E-16,
0.173648177666902));
#87532=DIRECTION('ref_axis',(-0.00236288091263331,0.999907416559164,-0.0134005635617392));
#87533=DIRECTION('',(0.984807787586651,-4.14936868640622E-7,-0.173647981584909));
#87534=DIRECTION('',(0.984807753012213,0.,-0.173648177666902));
#87535=DIRECTION('center_axis',(-0.984815825350885,-1.94466018545213E-5,
0.173602389846124));
#87536=DIRECTION('ref_axis',(0.0511700711168919,-0.955605550622165,0.290171768857692));
#87537=DIRECTION('center_axis',(-0.190809912898502,-9.49751800403212E-8,
0.981627005099013));
#87538=DIRECTION('ref_axis',(-4.97747620118824E-7,0.999999999999876,4.04178578453096E-24));
#87539=DIRECTION('center_axis',(0.190809912898503,0.,-0.981627005099017));
#87540=DIRECTION('ref_axis',(0.,-1.,0.));
#87541=DIRECTION('center_axis',(0.190809912898503,0.,-0.981627005099017));
#87542=DIRECTION('ref_axis',(0.,-1.,0.));
#87543=DIRECTION('center_axis',(-0.190809912898503,0.,0.981627005099017));
#87544=DIRECTION('ref_axis',(0.,1.,0.));
#87545=DIRECTION('',(-3.635245538593E-8,0.999999999999999,-1.866361044514E-8));
#87546=DIRECTION('center_axis',(0.190809912898503,0.,-0.981627005099017));
#87547=DIRECTION('ref_axis',(0.,-1.,0.));
#87548=DIRECTION('center_axis',(-8.80448426118404E-5,0.999999995977604,
-1.71142691292802E-5));
#87549=DIRECTION('ref_axis',(0.473468177754614,5.6760866602408E-5,0.880810922634324));
#87550=DIRECTION('center_axis',(-0.976953213978548,0.0974838992373601,-0.189892883190669));
#87551=DIRECTION('ref_axis',(0.190801607119635,-4.66549814768457E-7,-0.981628619550361));
#87552=DIRECTION('center_axis',(-0.800108939388847,-0.588097435439644,-0.118182450217318));
#87553=DIRECTION('ref_axis',(0.596174896320331,-0.757825141935888,-0.265097241115962));
#87554=DIRECTION('center_axis',(-0.675651786267923,-0.735965325320194,-0.0430081810741494));
#87555=DIRECTION('ref_axis',(-0.730667597463077,0.676266554259198,-0.0937465178442656));
#87556=DIRECTION('center_axis',(0.107073044687985,-0.827666229220606,-0.550911949506441));
#87557=DIRECTION('ref_axis',(0.98163660235276,1.75954457808426E-5,0.190760532112199));
#87558=DIRECTION('center_axis',(-0.981627005099017,0.,-0.190809912898503));
#87559=DIRECTION('ref_axis',(-0.190809912898503,0.,0.981627005099017));
#87560=DIRECTION('',(-6.598096137308E-10,1.,-1.279942325608E-10));
#87561=DIRECTION('center_axis',(0.,1.,0.));
#87562=DIRECTION('ref_axis',(0.981627005099017,0.,0.190809912898502));
#87563=DIRECTION('center_axis',(-0.799675205911076,0.588765746219848,-0.117789902492802));
#87564=DIRECTION('ref_axis',(0.596998789463264,0.800603041435647,-0.0512563695884574));
#87565=DIRECTION('center_axis',(0.976958619535709,0.0974612280175059,0.189876709335828));
#87566=DIRECTION('ref_axis',(0.190786976255942,-2.08181573059927E-5,-0.981631463054093));
#87567=DIRECTION('center_axis',(-0.984807753012213,-2.95751398859563E-17,
0.173648177666903));
#87568=DIRECTION('ref_axis',(-0.173046420789344,0.0831790275986082,-0.981395020172686));
#87569=DIRECTION('center_axis',(0.984807753012213,3.03145183831052E-16,
-0.173648177666902));
#87570=DIRECTION('ref_axis',(0.0108577499378729,-0.998043254585349,0.0615773598246225));
#87571=DIRECTION('',(0.984807753012213,0.,-0.173648177666902));
#87572=DIRECTION('center_axis',(0.984807753012213,9.16829336464645E-16,
-0.173648177666903));
#87573=DIRECTION('ref_axis',(0.103441898062484,-0.803208388241305,0.586648155868606));
#87574=DIRECTION('',(-0.984807766253658,9.3962545399306E-8,0.173648102570893));
#87575=DIRECTION('center_axis',(0.172766604332646,0.100486419652285,0.979823545283962));
#87576=DIRECTION('ref_axis',(0.98480822440525,-1.91663112048265E-7,-0.173645504242816));
#87577=DIRECTION('center_axis',(-0.240517466226023,0.0124905486229052,0.970564441258442));
#87578=DIRECTION('ref_axis',(0.957551275334907,0.166737877871554,0.235146837502408));
#87579=DIRECTION('center_axis',(-0.984807753012213,-1.51942396384287E-16,
0.173648177666902));
#87580=DIRECTION('ref_axis',(-0.0915531241012405,-0.849720490306423,-0.519223568244658));
#87581=DIRECTION('center_axis',(0.984807753012213,1.51942396384287E-16,
-0.173648177666902));
#87582=DIRECTION('ref_axis',(0.00236288091262946,-0.999907416559164,0.0134005635617186));
#87583=DIRECTION('center_axis',(-0.984807753012213,-7.51655445223487E-16,
0.173648177666902));
#87584=DIRECTION('ref_axis',(-0.0140997774057779,0.996698041116542,-0.0799638112620634));
#87585=DIRECTION('center_axis',(0.984807753012213,-1.47930621883394E-15,
-0.173648177666902));
#87586=DIRECTION('ref_axis',(0.00236288091262263,-0.999907416559164,0.0134005635616892));
#87587=DIRECTION('center_axis',(-0.984807753012213,-3.50624536671156E-16,
0.173648177666902));
#87588=DIRECTION('ref_axis',(-0.0174417350637655,0.994942819454527,-0.0989169949697339));
#87589=DIRECTION('center_axis',(0.984807753012213,4.05541630188082E-16,
-0.173648177666902));
#87590=DIRECTION('ref_axis',(0.0108576734130155,-0.99804328219437,0.0615769258305894));
#87591=DIRECTION('center_axis',(-0.173295783426445,-0.062517609495443,-0.98288357395451));
#87592=DIRECTION('ref_axis',(-0.984810412796333,3.80932965607098E-5,0.173633088427341));
#87593=DIRECTION('center_axis',(0.984807753012213,-5.38458166943201E-15,
-0.173648177666901));
#87594=DIRECTION('ref_axis',(-0.0407970909149098,0.972009612883567,-0.231371799999089));
#87595=DIRECTION('',(0.984807687628933,-2.59140590676409E-7,-0.173648548473306));
#87596=DIRECTION('center_axis',(0.984807753012213,-5.38458166943201E-15,
-0.173648177666901));
#87597=DIRECTION('ref_axis',(0.0407970909149098,-0.972009612883567,0.231371799999089));
#87598=DIRECTION('center_axis',(-0.167224647446209,-0.269421488102054,-0.948392312830174));
#87599=DIRECTION('ref_axis',(-0.984808093511156,-2.14966491856184E-6,0.173646246577062));
#87600=DIRECTION('center_axis',(-0.984807753012213,-2.02770816388138E-16,
0.173648177666902));
#87601=DIRECTION('ref_axis',(-0.110025883188373,0.7736494953753,-0.623987791013705));
#87602=DIRECTION('center_axis',(0.984807753012213,1.52078009876091E-16,
-0.173648177666902));
#87603=DIRECTION('ref_axis',(0.103441898062483,-0.803208388241305,0.586648155868606));
#87604=DIRECTION('center_axis',(-0.139475672938697,-0.595698149020197,-0.791005848216187));
#87605=DIRECTION('ref_axis',(0.103441898016906,-0.803208388435972,0.586648155610114));
#87606=DIRECTION('center_axis',(-0.984807753012214,3.20576898360514E-15,
0.173648177666899));
#87607=DIRECTION('ref_axis',(-0.109429766257885,0.776448339114792,-0.620607043903488));
#87608=DIRECTION('center_axis',(0.,-1.,0.));
#87609=DIRECTION('ref_axis',(-0.173648177666898,0.,-0.984807753012214));
#87610=DIRECTION('',(-8.565880838752E-11,-1.,1.505910719479E-11));
#87611=DIRECTION('center_axis',(0.984901889102444,0.000257016284667763,
-0.173113265768588));
#87612=DIRECTION('ref_axis',(0.173113399729199,-0.000651956645208656,0.984901683309929));
#87613=DIRECTION('center_axis',(0.139473992434594,-0.595698140751181,0.791006150759866));
#87614=DIRECTION('ref_axis',(0.103440598648708,0.803208394568672,0.586648376325728));
#87615=DIRECTION('center_axis',(-0.984807753012213,3.46400144663069E-16,
0.173648177666902));
#87616=DIRECTION('ref_axis',(-0.0421501634500986,-0.97009310576118,-0.239045455668495));
#87617=DIRECTION('center_axis',(0.984807753012213,-4.22438916266538E-17,
-0.173648177666902));
#87618=DIRECTION('ref_axis',(0.0467849591103272,0.963021699437997,0.265330688034001));
#87619=DIRECTION('center_axis',(0.167232170899728,-0.269429194209485,0.948388797025667));
#87620=DIRECTION('ref_axis',(-0.984803328168082,7.04152060432668E-5,0.17367325606082));
#87621=DIRECTION('center_axis',(-0.9848077750298,-7.05368960287473E-8,0.1736480527989));
#87622=DIRECTION('ref_axis',(0.0407970401597095,0.972009548712139,0.231372078537215));
#87623=DIRECTION('center_axis',(-0.984807753012213,-5.38458166943201E-15,
0.173648177666901));
#87624=DIRECTION('ref_axis',(-0.0407970909149098,-0.972009612883567,-0.231371799999089));
#87625=DIRECTION('',(-0.984807701505426,-2.26153704840706E-7,0.173648469776005));
#87626=DIRECTION('center_axis',(-0.984803957534525,-0.000225618307817559,
0.173669554962053));
#87627=DIRECTION('ref_axis',(0.172048805725959,-0.13757327250827,0.975434673947793));
#87628=DIRECTION('center_axis',(0.173311955176598,-0.0625216763371239,0.982880463831111));
#87629=DIRECTION('ref_axis',(-0.984807591131402,-4.20708473535737E-5,0.173649090639741));
#87630=DIRECTION('center_axis',(-0.984807753012213,3.73594668215124E-16,
0.173648177666902));
#87631=DIRECTION('ref_axis',(0.00180597749651713,-0.999945916354496,0.0102422073426411));
#87632=DIRECTION('center_axis',(0.984807753012213,-2.14387893151549E-16,
-0.173648177666902));
#87633=DIRECTION('ref_axis',(0.00236288091262434,0.999907416559164,0.0134005635616892));
#87634=DIRECTION('center_axis',(0.173632090960341,-0.0136072847582164,0.984716577899575));
#87635=DIRECTION('ref_axis',(-0.984807754634243,4.27085877774405E-8,0.173648168467909));
#87636=DIRECTION('center_axis',(-0.984807753012213,-4.38922887721939E-17,
0.173648177666902));
#87637=DIRECTION('ref_axis',(0.161562458752702,-0.366542983040298,0.916266235057094));
#87638=DIRECTION('center_axis',(0.984807753012213,4.55368148680565E-16,
-0.173648177666903));
#87639=DIRECTION('ref_axis',(-0.156740864913815,0.43040754996901,-0.888921617577019));
#87640=DIRECTION('center_axis',(-0.984807753012213,-2.93785902374558E-17,
0.173648177666902));
#87641=DIRECTION('ref_axis',(-0.0917700003358048,0.848944277013721,-0.520453534490849));
#87642=DIRECTION('center_axis',(-0.984807753012145,-1.27114520028174E-13,
0.17364817766729));
#87643=DIRECTION('ref_axis',(-0.166072447287528,0.29214804337792,-0.941843651038953));
#87644=DIRECTION('center_axis',(0.984807753012145,1.27328329737158E-13,
-0.173648177667291));
#87645=DIRECTION('ref_axis',(-0.162244947343955,0.356405400048795,-0.920136820194375));
#87646=DIRECTION('center_axis',(-0.201501638275048,0.96280516344127,0.180009185941446));
#87647=DIRECTION('ref_axis',(0.976016676961642,0.181908483442498,0.119585743064987));
#87648=DIRECTION('center_axis',(1.21185977076882E-11,1.,-3.61798710391132E-11));
#87649=DIRECTION('ref_axis',(0.996578836186276,-9.08695904165718E-12,0.0826475847536266));
#87650=DIRECTION('center_axis',(0.201484553848451,0.962823392583096,-0.179930790181304));
#87651=DIRECTION('ref_axis',(0.976087907632447,-0.182066474456054,0.118761085599849));
#87652=DIRECTION('center_axis',(-0.984807753012213,-1.44182084052305E-14,
0.173648177666903));
#87653=DIRECTION('ref_axis',(-0.166064612600648,-0.292295700970649,-0.941799218324094));
#87654=DIRECTION('center_axis',(0.984807753012213,1.47249787968311E-14,
-0.173648177666902));
#87655=DIRECTION('ref_axis',(-0.156683846646441,-0.431095489042511,-0.888598250913917));
#87656=DIRECTION('',(0.984807776058194,5.24229513912697E-14,-0.173648046966599));
#87657=DIRECTION('center_axis',(-0.0771912637911887,-0.914517936634286,
0.397112644432895));
#87658=DIRECTION('ref_axis',(-0.141744409590102,-0.384189181042076,-0.912308717222505));
#87659=DIRECTION('center_axis',(-3.05340545697296E-8,-0.999999999999987,
1.57083313648698E-7));
#87660=DIRECTION('ref_axis',(-0.173648189854594,-1.49394681507557E-7,-0.984807750863183));
#87661=DIRECTION('center_axis',(0.0771819226456397,-0.914539590865797,-0.3970645886449));
#87662=DIRECTION('ref_axis',(-0.141611064558104,0.384159300577726,-0.912342007239803));
#87663=DIRECTION('center_axis',(0.084142908898196,-0.897541669062807,-0.432826666436));
#87664=DIRECTION('ref_axis',(0.981622833089212,-3.42192540777386E-7,0.190831374668297));
#87665=DIRECTION('center_axis',(-0.0841377180325195,-0.897531445507195,
0.432848875163198));
#87666=DIRECTION('ref_axis',(-0.135188302065196,-0.420091172265935,-0.89735585470256));
#87667=DIRECTION('center_axis',(-0.677112882379002,0.734636173451785,-0.0427532124233805));
#87668=DIRECTION('ref_axis',(-0.733973201133508,-0.678397144997567,-0.0325676784094527));
#87669=DIRECTION('center_axis',(-0.190686705650736,-0.0313546077358391,
0.98115007458686));
#87670=DIRECTION('ref_axis',(0.981632739712338,-3.22581837650991E-6,0.19078040862322));
#87671=DIRECTION('center_axis',(-0.984807753012213,-1.44799683600039E-14,
0.173648177666903));
#87672=DIRECTION('ref_axis',(0.155662080843755,0.443201134484021,0.882803529093234));
#87673=DIRECTION('center_axis',(0.984807753012213,1.44399655486805E-14,
-0.173648177666903));
#87674=DIRECTION('ref_axis',(-0.15668505394005,-0.431080936724009,-0.888605097816209));
#87675=DIRECTION('center_axis',(0.984807753012213,0.,-0.173648177666902));
#87676=DIRECTION('ref_axis',(0.,-1.,0.));
#87677=DIRECTION('center_axis',(0.984807753012145,1.27057714228674E-13,
-0.17364817766729));
#87678=DIRECTION('ref_axis',(-0.162245431570886,0.356398089659788,-0.920139566381769));
#87679=DIRECTION('',(8.81218894669602E-8,0.999999999999902,4.32820325270801E-7));
#87680=DIRECTION('center_axis',(0.,1.,0.));
#87681=DIRECTION('ref_axis',(-0.173648177666898,0.,-0.984807753012214));
#87682=DIRECTION('',(-7.10683480609823E-7,0.999999999999732,1.76068375849406E-7));
#87683=DIRECTION('center_axis',(0.173648177666902,0.,0.984807753012213));
#87684=DIRECTION('ref_axis',(0.,-1.,0.));
#87685=DIRECTION('',(2.81021024324399E-5,-0.999999999592795,-4.96817573254497E-6));
#87686=DIRECTION('',(-2.79857101008889E-5,-0.999999999596161,4.94759277264081E-6));
#87687=DIRECTION('center_axis',(0.,-1.,0.));
#87688=DIRECTION('ref_axis',(0.984807753012214,0.,-0.173648177666898));
#87689=DIRECTION('',(0.,-1.,0.));
#87690=DIRECTION('center_axis',(0.984807753012213,0.,-0.173648177666902));
#87691=DIRECTION('ref_axis',(0.,-1.,0.));
#87692=DIRECTION('center_axis',(0.173648177666902,0.,0.984807753012213));
#87693=DIRECTION('ref_axis',(0.,-1.,0.));
#87694=DIRECTION('center_axis',(0.173648177666902,0.,0.984807753012213));
#87695=DIRECTION('ref_axis',(0.,-1.,0.));
#87696=DIRECTION('center_axis',(-0.173648177666903,8.36511531019332E-17,
-0.984807753012213));
#87697=DIRECTION('ref_axis',(-0.975914789972338,0.134084894844204,0.17208010834453));
#87698=DIRECTION('',(0.,1.,0.));
#87699=DIRECTION('center_axis',(0.,1.,0.));
#87700=DIRECTION('ref_axis',(-0.819141634169878,0.,-0.573591303254767));
#87701=DIRECTION('',(1.39364876480604E-5,0.999999999901329,-1.76500621154505E-6));
#87702=DIRECTION('',(-7.60889122223396E-8,0.999999999999997,1.313139806872E-8));
#87703=DIRECTION('',(-3.71082567177192E-8,0.999999999999977,-2.10540427148495E-7));
#87704=DIRECTION('center_axis',(0.173648177666902,0.,0.984807753012213));
#87705=DIRECTION('ref_axis',(0.984807753012213,-1.22464679914735E-16,-0.173648177666902));
#87706=DIRECTION('center_axis',(0.173648177666902,8.44686595599678E-23,
0.984807753012213));
#87707=DIRECTION('ref_axis',(0.984807753012137,3.91820935308914E-7,-0.173648177666889));
#87708=DIRECTION('center_axis',(0.173648177666902,-2.4603280324098E-16,
0.984807753012213));
#87709=DIRECTION('ref_axis',(-0.829311792010217,-0.539313198208507,0.146230044351063));
#87710=DIRECTION('center_axis',(-0.173648177666902,0.,-0.984807753012213));
#87711=DIRECTION('ref_axis',(-0.984807753012213,0.,0.173648177666902));
#87712=DIRECTION('',(-1.090258469048E-7,0.999999999999801,-6.20717966282101E-7));
#87713=DIRECTION('center_axis',(-0.173648177666903,6.47634049830965E-16,
-0.984807753012213));
#87714=DIRECTION('ref_axis',(-0.681789982854665,0.721602424588165,0.12021796915402));
#87715=DIRECTION('center_axis',(0.173648177666902,-2.87247579347555E-16,
0.984807753012213));
#87716=DIRECTION('ref_axis',(-0.606044361063923,-0.788219989143623,0.106861972361774));
#87717=DIRECTION('center_axis',(0.173648177666903,2.73912803682029E-16,
0.984807753012213));
#87718=DIRECTION('ref_axis',(-0.750334089213524,-0.647683848740426,0.132304144473635));
#87719=DIRECTION('center_axis',(-0.173648177666902,0.,-0.984807753012213));
#87720=DIRECTION('ref_axis',(-0.984807753012213,0.,0.173648177666902));
#87721=DIRECTION('center_axis',(-0.173648177666902,-1.61124207346389E-16,
-0.984807753012213));
#87722=DIRECTION('ref_axis',(-0.750329716580782,0.647689071844487,0.132303373460505));
#87723=DIRECTION('center_axis',(-0.173648177666902,-2.87247456824783E-16,
-0.984807753012213));
#87724=DIRECTION('ref_axis',(-0.606044921708883,0.788219544673781,0.106862071218607));
#87725=DIRECTION('center_axis',(0.173648177666903,6.10624530269016E-16,
0.984807753012213));
#87726=DIRECTION('ref_axis',(-0.681789982854614,-0.721602424588215,0.120217969154011));
#87727=DIRECTION('',(8.2153927947679E-8,0.999999999999888,4.67122875809294E-7));
#87728=DIRECTION('center_axis',(-0.173648177666902,1.77232881935626E-16,
-0.984807753012213));
#87729=DIRECTION('ref_axis',(0.801893974638295,0.580494060044092,-0.141395543396257));
#87730=DIRECTION('center_axis',(0.659077833040731,-0.743026690968582,-0.116308841033747));
#87731=DIRECTION('ref_axis',(-0.173639109027328,0.000135049773334708,-0.984809342755111));
#87732=DIRECTION('center_axis',(0.173648177666902,-1.20886287747465E-16,
0.984807753012213));
#87733=DIRECTION('ref_axis',(-0.750329716580742,-0.647689071844535,0.132303373460498));
#87734=DIRECTION('center_axis',(0.637849218735937,-0.761904762558937,-0.112470026887006));
#87735=DIRECTION('ref_axis',(-0.750329717224971,-0.64768907107501,0.132303373574089));
#87736=DIRECTION('center_axis',(-0.173668324352799,-6.63106817671438E-6,
-0.98480420037311));
#87737=DIRECTION('ref_axis',(-0.984804200395333,1.62419221665202E-6,0.17366832434578));
#87738=DIRECTION('center_axis',(-0.173648177666903,0.,-0.984807753012213));
#87739=DIRECTION('ref_axis',(0.984807753012213,0.,-0.173648177666903));
#87740=DIRECTION('',(-0.173878181060975,0.000322054883223046,-0.984767116851278));
#87741=DIRECTION('center_axis',(-0.173648177666903,0.,-0.984807753012213));
#87742=DIRECTION('ref_axis',(0.984807753012213,0.,-0.173648177666903));
#87743=DIRECTION('',(-0.173877367546055,-0.00032091573288183,-0.984767260863371));
#87744=DIRECTION('center_axis',(-0.173648177666902,-1.20886287747465E-16,
-0.984807753012213));
#87745=DIRECTION('ref_axis',(-0.750329716580742,0.647689071844535,0.132303373460498));
#87746=DIRECTION('center_axis',(-0.173648177666897,3.28903571045203E-15,
-0.984807753012214));
#87747=DIRECTION('ref_axis',(-0.936719925941306,-0.308666459146836,0.165168996310654));
#87748=DIRECTION('',(-0.173636642897303,-6.51718399708411E-5,-0.984809784677217));
#87749=DIRECTION('center_axis',(-0.984807753012213,0.,0.173648177666902));
#87750=DIRECTION('ref_axis',(0.,1.,0.));
#87751=DIRECTION('',(2.35372139113308E-6,0.999999999974235,6.78157916925224E-6));
#87752=DIRECTION('center_axis',(-0.984807753012213,-2.26576147468896E-16,
0.173648177666902));
#87753=DIRECTION('ref_axis',(0.0174469104577598,-0.994939810195265,0.0989463460876066));
#87754=DIRECTION('',(-1.35344856793906E-6,0.999999999998245,-1.29536058899606E-6));
#87755=DIRECTION('',(-0.173639122016199,6.67188537162898E-5,-0.984809347464796));
#87756=DIRECTION('center_axis',(-0.173648177666907,-1.19615497498102E-14,
-0.984807753012212));
#87757=DIRECTION('ref_axis',(-0.936720096114287,0.308665926660553,0.165169026316749));
#87758=DIRECTION('center_axis',(-0.172153314886262,-0.000369434897238181,
-0.985070098871917));
#87759=DIRECTION('ref_axis',(-0.938950108420514,0.302462075571974,0.163979836375689));
#87760=DIRECTION('center_axis',(-0.173642877220662,-1.74636676018426E-6,
-0.984808687607639));
#87761=DIRECTION('ref_axis',(-0.797231544682396,0.587079646333193,0.140567965855004));
#87762=DIRECTION('center_axis',(0.637849235778954,0.761904751719864,-0.112470003658296));
#87763=DIRECTION('ref_axis',(-0.750329430917128,0.647689083824637,0.132304934881434));
#87764=DIRECTION('center_axis',(-0.173648177666902,-3.38353683695286E-16,
-0.984807753012213));
#87765=DIRECTION('ref_axis',(0.785231832909193,-0.603523382437399,-0.138457558253028));
#87766=DIRECTION('center_axis',(-0.173648177666902,1.43623595195129E-16,
-0.984807753012213));
#87767=DIRECTION('ref_axis',(0.630875084425314,-0.767868624027015,-0.111240298840895));
#87768=DIRECTION('center_axis',(-0.173648177666902,-2.93948484863116E-16,
-0.984807753012213));
#87769=DIRECTION('ref_axis',(-0.606035537815208,0.788226983978802,0.106860416584968));
#87770=DIRECTION('center_axis',(0.710639662326888,-0.692307692307688,-0.125304946029797));
#87771=DIRECTION('ref_axis',(-0.173648177665894,1.11610884899936E-12,-0.984807753012391));
#87772=DIRECTION('center_axis',(-0.173648177666902,3.88578058618862E-16,
-0.984807753012213));
#87773=DIRECTION('ref_axis',(0.889587405855847,0.428986868317277,-0.156858261350812));
#87774=DIRECTION('center_axis',(-0.173648177666898,0.,-0.984807753012214));
#87775=DIRECTION('ref_axis',(0.915664591049666,-0.36808992979761,-0.161456372681408));
#87776=DIRECTION('',(0.173648177666902,7.6637955192051E-11,0.984807753012213));
#87777=DIRECTION('center_axis',(-0.984807753012213,0.,0.173648177666902));
#87778=DIRECTION('ref_axis',(0.,1.,0.));
#87779=DIRECTION('',(4.437051728155E-11,-1.,2.516170452507E-10));
#87780=DIRECTION('',(-1.351043146217E-10,-1.,-1.097321493067E-11));
#87781=DIRECTION('',(1.996062744186E-11,-1.,1.132315338918E-10));
#87782=DIRECTION('',(-0.173648177666902,1.00328634318001E-11,-0.984807753012213));
#87783=DIRECTION('',(0.,1.,0.));
#87784=DIRECTION('center_axis',(0.,1.,0.));
#87785=DIRECTION('ref_axis',(0.819151987079672,0.,0.573576518054414));
#87786=DIRECTION('center_axis',(-4.06837822689946E-10,1.,-2.53848971472811E-9));
#87787=DIRECTION('ref_axis',(0.312566484770769,2.53846366149446E-9,0.949895885135863));
#87788=DIRECTION('center_axis',(0.173648177666903,-1.19205647900064E-29,
0.984807753012213));
#87789=DIRECTION('ref_axis',(0.984807753012213,-1.04083408558608E-14,-0.173648177666903));
#87790=DIRECTION('center_axis',(4.41761171680438E-10,-1.,2.56294060048864E-9));
#87791=DIRECTION('ref_axis',(-3.11479720759106E-33,2.56294060048864E-9,
1.));
#87792=DIRECTION('center_axis',(-0.710639662326888,-0.692307692307688,0.125304946029795));
#87793=DIRECTION('ref_axis',(0.173648177387696,2.95556609701271E-10,0.984807753061445));
#87794=DIRECTION('center_axis',(-0.173648177666899,-3.16105230837517E-15,
-0.984807753012214));
#87795=DIRECTION('ref_axis',(-0.681789982854612,0.721602424588218,0.120217969154005));
#87796=DIRECTION('center_axis',(-0.173648177666901,-4.0708177569595E-16,
-0.984807753012213));
#87797=DIRECTION('ref_axis',(0.893467078353688,-0.420591235207693,-0.157542352288493));
#87798=DIRECTION('center_axis',(0.71063966232689,0.692307692307686,-0.125304946029799));
#87799=DIRECTION('ref_axis',(0.633285392360227,-0.707023094958418,-0.314750623539612));
#87800=DIRECTION('center_axis',(-0.173648177666903,-3.98954431097579E-16,
-0.984807753012213));
#87801=DIRECTION('ref_axis',(0.629931807325388,0.768666696624785,-0.111073973637894));
#87802=DIRECTION('center_axis',(0.173648177666902,-1.87058128807964E-16,
0.984807753012213));
#87803=DIRECTION('ref_axis',(-0.606035677048363,-0.78822687359976,0.10686044113553));
#87804=DIRECTION('center_axis',(-0.173648177666902,1.05109872153861E-16,
-0.984807753012213));
#87805=DIRECTION('ref_axis',(-0.709980153735304,0.693005037133797,0.125188656871057));
#87806=DIRECTION('center_axis',(-0.173648177666902,4.20439473358018E-17,
-0.984807753012213));
#87807=DIRECTION('ref_axis',(0.681789982854614,-0.721602424588215,-0.12021796915401));
#87808=DIRECTION('center_axis',(0.,1.,0.));
#87809=DIRECTION('ref_axis',(-0.819128681345575,0.,-0.573609800645926));
#87810=DIRECTION('',(-0.000104732033721804,0.999999994335537,1.89770173025207E-5));
#87811=DIRECTION('center_axis',(-0.173648177666902,0.,-0.984807753012213));
#87812=DIRECTION('ref_axis',(-0.984807753012213,0.,0.173648177666902));
#87813=DIRECTION('',(-2.965055618919E-10,-1.,5.228312595822E-11));
#87814=DIRECTION('',(-0.984807721882561,4.36142738440383E-7,0.173648354211293));
#87815=DIRECTION('center_axis',(-0.173648177666902,0.,-0.984807753012213));
#87816=DIRECTION('ref_axis',(-0.984807753012213,0.,0.173648177666902));
#87817=DIRECTION('',(0.000104623869886698,0.999999994344178,-1.91177692657596E-5));
#87818=DIRECTION('',(0.984807722792198,4.31673701686499E-7,-0.1736483490525));
#87819=DIRECTION('',(-9.024447313596E-12,-1.,1.598357449676E-12));
#87820=DIRECTION('center_axis',(-0.173648177666902,6.30659209509215E-17,
-0.984807753012213));
#87821=DIRECTION('ref_axis',(-0.606056619441591,0.788210270758188,0.106864133844497));
#87822=DIRECTION('center_axis',(-0.984807753012213,1.8503717077086E-15,
0.173648177666903));
#87823=DIRECTION('ref_axis',(0.0751084169313687,0.901618518365398,0.425960999443198));
#87824=DIRECTION('center_axis',(-0.984807753012213,1.2335811384724E-15,
0.173648177666903));
#87825=DIRECTION('ref_axis',(-0.0751084169313687,-0.901618518365396,-0.425960999443203));
#87826=DIRECTION('center_axis',(0.,0.,1.));
#87827=DIRECTION('ref_axis',(1.,0.,0.));
#87828=DIRECTION('center_axis',(0.,-1.,0.));
#87829=DIRECTION('ref_axis',(0.984807753012213,0.,-0.173648177666903));
#87830=DIRECTION('center_axis',(0.156564412664908,-0.432532134460022,0.887920907145648));
#87831=DIRECTION('ref_axis',(-0.075108416931378,-0.901618518365421,-0.425960999443147));
#87832=DIRECTION('center_axis',(-0.984807753012213,2.98614490958382E-16,
0.173648177666903));
#87833=DIRECTION('ref_axis',(0.161725191946745,0.364155244606999,0.917189140861908));
#87834=DIRECTION('center_axis',(-0.730811865748475,-0.554283463095025,0.398351427034748));
#87835=DIRECTION('ref_axis',(0.656406878005312,-0.410641643559799,0.632853419902134));
#87836=DIRECTION('center_axis',(0.926024209527167,0.340292288158955,-0.163341121549745));
#87837=DIRECTION('ref_axis',(-0.180419693350444,0.779131598163688,0.600335478706889));
#87838=DIRECTION('center_axis',(0.925983753120755,-0.340399802521857,-0.163346452056609));
#87839=DIRECTION('ref_axis',(-0.173594778761283,0.000353804681334812,-0.984817103633496));
#87840=DIRECTION('center_axis',(-0.695347255811973,0.70213706029504,-0.153283209762188));
#87841=DIRECTION('ref_axis',(0.620272016580331,0.478605536989138,-0.621449406959817));
#87842=DIRECTION('center_axis',(-0.984807753012196,2.8194560172209E-16,
0.173648177666999));
#87843=DIRECTION('ref_axis',(0.156623827406739,0.43181818181821,0.888257864890415));
#87844=DIRECTION('',(0.622150730667944,0.75432770888201,0.209566638428358));
#87845=DIRECTION('center_axis',(0.224487892977242,-0.241948423367666,0.943963000512488));
#87846=DIRECTION('ref_axis',(-0.18733184772302,-0.961334023585974,-0.201850622799835));
#87847=DIRECTION('center_axis',(1.55730139623408E-6,0.999999999997948,1.29560869156906E-6));
#87848=DIRECTION('ref_axis',(0.729105700774769,-2.48721301333868E-7,-0.684401108340475));
#87849=DIRECTION('center_axis',(-0.173648177666901,-9.49857476623745E-16,
-0.984807753012213));
#87850=DIRECTION('ref_axis',(-0.315917116162589,-0.947150125830322,0.0557047112470661));
#87851=DIRECTION('center_axis',(-0.173648177666902,0.,-0.984807753012213));
#87852=DIRECTION('ref_axis',(-0.984807753012213,0.,0.173648177666902));
#87853=DIRECTION('center_axis',(-0.173648177666902,0.,-0.984807753012213));
#87854=DIRECTION('ref_axis',(-0.984807753012213,0.,0.173648177666902));
#87855=DIRECTION('',(-0.622131158824598,0.754172855889872,-0.210181171036981));
#87856=DIRECTION('',(0.174534476450797,-0.00122572414799798,0.984650300426684));
#87857=DIRECTION('center_axis',(-0.0707686828235114,-0.994894683248916,
-0.0719469441634933));
#87858=DIRECTION('ref_axis',(-0.173001180656409,0.0832765703625063,-0.981394724012793));
#87859=DIRECTION('center_axis',(-6.73423872643482E-7,-0.99999999999248,
-3.81917657283092E-6));
#87860=DIRECTION('ref_axis',(0.679405139203387,-3.25989944411653E-6,0.733763352051191));
#87861=DIRECTION('center_axis',(0.938200139829041,-9.39842509682406E-5,
-0.346093179348754));
#87862=DIRECTION('ref_axis',(0.342337059059529,0.147180963465246,0.927977964171518));
#87863=DIRECTION('center_axis',(-2.61574989044999E-8,-1.,-1.99490763817199E-8));
#87864=DIRECTION('ref_axis',(-0.679404928955814,3.24094387247223E-8,-0.733763546730515));
#87865=DIRECTION('center_axis',(-1.,0.,0.));
#87866=DIRECTION('ref_axis',(0.,0.,1.));
#87867=DIRECTION('center_axis',(-1.,0.,0.));
#87868=DIRECTION('ref_axis',(0.,-0.748331477354783,0.663324958071086));
#87869=DIRECTION('center_axis',(-1.,0.,0.));
#87870=DIRECTION('ref_axis',(0.,0.748331477354783,-0.663324958071086));
#87871=DIRECTION('center_axis',(-0.20258578429475,-0.48430305448073,-0.851122524330261));
#87872=DIRECTION('ref_axis',(0.972820028468568,1.76583649998364E-5,-0.231562501063097));
#87873=DIRECTION('center_axis',(-0.224959803675515,-0.646322642471482,-0.729150278446738));
#87874=DIRECTION('ref_axis',(0.955555444304602,4.45507300384497E-7,-0.29481145306727));
#87875=DIRECTION('center_axis',(0.198384291592322,0.861437385015848,0.467513961873302));
#87876=DIRECTION('ref_axis',(-3.79004033482016E-6,0.476995229637716,-0.878905882838714));
#87877=DIRECTION('center_axis',(-0.198384293344405,0.861437385923514,-0.467513959457367));
#87878=DIRECTION('ref_axis',(3.70182108121826E-6,-0.476993894565724,-0.878906607401105));
#87879=DIRECTION('center_axis',(1.,0.,0.));
#87880=DIRECTION('ref_axis',(0.,-1.,0.));
#87881=DIRECTION('center_axis',(-0.224959803616002,0.646322642426279,-0.729150278505167));
#87882=DIRECTION('ref_axis',(7.58238768779224E-7,-0.748331361275018,-0.663325089026266));
#87883=DIRECTION('center_axis',(0.224959803662862,-0.646322642460983,-0.729150278459948));
#87884=DIRECTION('ref_axis',(2.66897615120205E-13,-0.748331477359025,0.663324958066301));
#87885=DIRECTION('center_axis',(0.198384291071427,-0.861437384747512,-0.467513962588771));
#87886=DIRECTION('ref_axis',(5.22391162033877E-6,-0.476993626757997,0.878906752736013));
#87887=DIRECTION('center_axis',(1.,0.,0.));
#87888=DIRECTION('ref_axis',(0.,-1.,0.));
#87889=DIRECTION('center_axis',(0.198384291487557,0.861437384962546,-0.46751396201597));
#87890=DIRECTION('ref_axis',(0.920549900482293,-4.9913569769151E-9,0.390624987324212));
#87891=DIRECTION('center_axis',(0.224959803665131,0.646322642464532,-0.729150278456101));
#87892=DIRECTION('ref_axis',(0.955555562815279,-2.90698700666896E-8,0.294811068945476));
#87893=DIRECTION('center_axis',(0.202585776058526,0.484303048332413,-0.851122529789159));
#87894=DIRECTION('ref_axis',(0.972822293955169,4.34825508932484E-9,0.231552983966525));
#87895=DIRECTION('center_axis',(0.,1.,0.));
#87896=DIRECTION('ref_axis',(-1.,0.,0.));
#87897=DIRECTION('center_axis',(0.,-1.,0.));
#87898=DIRECTION('ref_axis',(-0.972822292136262,0.,-0.231552991608291));
#87899=DIRECTION('center_axis',(0.390624999999987,0.,-0.92054989510347));
#87900=DIRECTION('ref_axis',(0.,-1.,0.));
#87901=DIRECTION('center_axis',(0.,-1.,0.));
#87902=DIRECTION('ref_axis',(-1.,0.,0.));
#87903=DIRECTION('center_axis',(0.390624999999979,0.,0.920549895103474));
#87904=DIRECTION('ref_axis',(-0.920549895103474,0.,0.390624999999979));
#87905=DIRECTION('center_axis',(0.,-1.,0.));
#87906=DIRECTION('ref_axis',(-0.92054989510347,0.,0.390624999999988));
#87907=DIRECTION('center_axis',(0.,-1.,0.));
#87908=DIRECTION('ref_axis',(-1.,0.,0.));
#87909=DIRECTION('',(0.,-1.,0.));
#87910=DIRECTION('center_axis',(0.,1.,0.));
#87911=DIRECTION('ref_axis',(1.,0.,0.));
#87912=DIRECTION('center_axis',(0.,-1.,0.));
#87913=DIRECTION('ref_axis',(0.407236366022499,0.,0.913322802840698));
#87914=DIRECTION('',(0.,-1.,0.));
#87915=DIRECTION('',(0.,-1.,0.));
#87916=DIRECTION('center_axis',(0.,1.,0.));
#87917=DIRECTION('ref_axis',(-0.920549895103471,0.,0.390624999999986));
#87918=DIRECTION('',(0.,-1.,0.));
#87919=DIRECTION('center_axis',(0.,-1.,0.));
#87920=DIRECTION('ref_axis',(-1.,0.,0.));
#87921=DIRECTION('center_axis',(0.,1.,0.));
#87922=DIRECTION('ref_axis',(-0.972822292136262,0.,0.231552991608291));
#87923=DIRECTION('center_axis',(0.,1.,0.));
#87924=DIRECTION('ref_axis',(-1.,0.,0.));
#87925=DIRECTION('center_axis',(0.390624999999987,0.,0.92054989510347));
#87926=DIRECTION('ref_axis',(0.,1.,0.));
#87927=DIRECTION('center_axis',(0.,1.,0.));
#87928=DIRECTION('ref_axis',(-0.92054989510347,0.,-0.390624999999987));
#87929=DIRECTION('center_axis',(0.390624999999991,0.,-0.920549895103469));
#87930=DIRECTION('ref_axis',(-0.920549895103469,0.,-0.390624999999991));
#87931=DIRECTION('center_axis',(0.,1.,0.));
#87932=DIRECTION('ref_axis',(-0.92054989510347,0.,-0.390624999999987));
#87933=DIRECTION('center_axis',(0.,-1.,0.));
#87934=DIRECTION('ref_axis',(-1.,0.,0.));
#87935=DIRECTION('',(2.849630032705E-13,1.,-6.731484522631E-13));
#87936=DIRECTION('center_axis',(0.,-1.,0.));
#87937=DIRECTION('ref_axis',(-1.,0.,0.));
#87938=DIRECTION('center_axis',(0.,1.,0.));
#87939=DIRECTION('ref_axis',(0.407236366022499,0.,-0.913322802840698));
#87940=DIRECTION('',(2.490857672745E-11,-1.,-3.242137599245E-11));
#87941=DIRECTION('',(5.04906701331786E-7,0.999999999999872,-2.70515465025393E-8));
#87942=DIRECTION('',(0.,-1.,0.));
#87943=DIRECTION('center_axis',(0.,-1.,0.));
#87944=DIRECTION('ref_axis',(-0.92054989510347,0.,-0.390624999999987));
#87945=DIRECTION('',(0.,1.,0.));
#87946=DIRECTION('center_axis',(-0.224959803790892,-0.646322642561247,0.729150278331572));
#87947=DIRECTION('ref_axis',(-3.99311694827824E-11,0.748331477256131,0.66332495818238));
#87948=DIRECTION('center_axis',(-0.198384293281608,-0.86143738589211,0.467513959541878));
#87949=DIRECTION('ref_axis',(-8.58600511532262E-6,0.476996080598531,0.878905420975386));
#87950=DIRECTION('center_axis',(0.198384288808409,-0.861437383575475,-0.467513965708642));
#87951=DIRECTION('ref_axis',(5.22459482121113E-6,-0.476993629596688,0.878906751195416));
#87952=DIRECTION('center_axis',(-0.224959800409593,0.646322639913861,0.729150281721439));
#87953=DIRECTION('ref_axis',(0.955555445223718,-4.48148750110284E-7,0.294811450088189));
#87954=DIRECTION('center_axis',(-0.202585784297521,0.484303054482622,0.851122524328525));
#87955=DIRECTION('ref_axis',(0.972820028467264,-1.76583687795184E-5,0.231562501068576));
#87956=DIRECTION('center_axis',(0.202585775073753,-0.48430304759702,0.851122530442007));
#87957=DIRECTION('ref_axis',(0.972822294179919,-4.88508078433452E-9,-0.231552983022287));
#87958=DIRECTION('center_axis',(0.224959803667178,-0.646322642467156,0.729150278453144));
#87959=DIRECTION('ref_axis',(0.955555562814303,2.90703354721545E-8,-0.294811068948639));
#87960=DIRECTION('center_axis',(0.198384289460816,-0.861437383911164,0.467513964813263));
#87961=DIRECTION('ref_axis',(0.920549901087734,2.47085567722425E-9,-0.390624985897424));
#87962=DIRECTION('center_axis',(0.198384289851298,0.861437384113648,0.467513964274471));
#87963=DIRECTION('ref_axis',(-3.78951340993614E-6,0.476995231822333,-0.878905881653092));
#87964=DIRECTION('center_axis',(0.224959803669713,0.646322642466345,0.729150278453081));
#87965=DIRECTION('ref_axis',(-7.87814258274064E-13,0.748331477353354,-0.663324958072698));
#87966=DIRECTION('center_axis',(-1.,0.,0.));
#87967=DIRECTION('ref_axis',(0.,0.,1.));
#87968=DIRECTION('center_axis',(-1.,0.,0.));
#87969=DIRECTION('ref_axis',(0.,0.748331477354783,-0.663324958071086));
#87970=DIRECTION('center_axis',(-1.,0.,0.));
#87971=DIRECTION('ref_axis',(0.,-0.748331477354783,0.663324958071086));
#87972=DIRECTION('center_axis',(1.,0.,0.));
#87973=DIRECTION('ref_axis',(0.,-1.,0.));
#87974=DIRECTION('center_axis',(1.,0.,0.));
#87975=DIRECTION('ref_axis',(0.,-1.,0.));
#87976=DIRECTION('center_axis',(0.,-1.,0.));
#87977=DIRECTION('ref_axis',(-1.,0.,0.));
#87978=DIRECTION('center_axis',(0.,1.,0.));
#87979=DIRECTION('ref_axis',(1.,0.,0.));
#87980=DIRECTION('center_axis',(0.,-1.,0.));
#87981=DIRECTION('ref_axis',(-0.92054989510347,0.,-0.390624999999987));
#87982=DIRECTION('center_axis',(0.913322802840698,0.,0.407236366022499));
#87983=DIRECTION('ref_axis',(0.,-1.,0.));
#87984=DIRECTION('center_axis',(0.,1.,0.));
#87985=DIRECTION('ref_axis',(1.,0.,0.));
#87986=DIRECTION('center_axis',(0.,-1.,0.));
#87987=DIRECTION('ref_axis',(0.407236366022499,0.,-0.913322802840698));
#87988=DIRECTION('center_axis',(0.,-1.,0.));
#87989=DIRECTION('ref_axis',(0.407236366022499,0.,-0.913322802840698));
#87990=DIRECTION('center_axis',(0.,1.,0.));
#87991=DIRECTION('ref_axis',(1.,0.,0.));
#87992=DIRECTION('center_axis',(0.,-1.,0.));
#87993=DIRECTION('ref_axis',(0.916673510305537,0.,0.399636929605016));
#87994=DIRECTION('center_axis',(0.9133228028407,0.,-0.407236366022496));
#87995=DIRECTION('ref_axis',(0.407236366022496,0.,0.9133228028407));
#87996=DIRECTION('center_axis',(0.,-1.,0.));
#87997=DIRECTION('ref_axis',(0.916673510305537,0.,0.399636929605016));
#87998=DIRECTION('center_axis',(0.,1.,0.));
#87999=DIRECTION('ref_axis',(1.,0.,0.));
#88000=DIRECTION('center_axis',(0.,-1.,0.));
#88001=DIRECTION('ref_axis',(0.4072363660225,0.,0.913322802840698));
#88002=DIRECTION('center_axis',(0.,1.,0.));
#88003=DIRECTION('ref_axis',(1.,0.,0.));
#88004=DIRECTION('center_axis',(0.,1.,0.));
#88005=DIRECTION('ref_axis',(1.,0.,0.));
#88006=DIRECTION('center_axis',(0.397580169372953,0.101324582793625,0.91195577625402));
#88007=DIRECTION('ref_axis',(-0.916673679426937,4.1861421552281E-6,0.399636541657988));
#88008=DIRECTION('center_axis',(0.,1.,0.));
#88009=DIRECTION('ref_axis',(1.,0.,0.));
#88010=DIRECTION('center_axis',(0.,1.,0.));
#88011=DIRECTION('ref_axis',(0.407236366022499,0.,0.913322802840698));
#88012=DIRECTION('center_axis',(0.,1.,0.));
#88013=DIRECTION('ref_axis',(1.,0.,0.));
#88014=DIRECTION('center_axis',(0.,1.,0.));
#88015=DIRECTION('ref_axis',(0.916673510305537,0.,-0.399636929605016));
#88016=DIRECTION('center_axis',(-0.397580166491966,0.101324584811521,-0.911955777285825));
#88017=DIRECTION('ref_axis',(-0.916673138003703,9.14519632467006E-6,0.399637783472497));
#88018=DIRECTION('center_axis',(0.,1.,0.));
#88019=DIRECTION('ref_axis',(1.,0.,0.));
#88020=DIRECTION('center_axis',(0.9133228028407,0.,0.407236366022496));
#88021=DIRECTION('ref_axis',(0.407236366022496,0.,-0.9133228028407));
#88022=DIRECTION('center_axis',(0.,1.,0.));
#88023=DIRECTION('ref_axis',(0.916673510305537,0.,-0.399636929605016));
#88024=DIRECTION('center_axis',(0.,1.,0.));
#88025=DIRECTION('ref_axis',(1.,0.,0.));
#88026=DIRECTION('center_axis',(0.,1.,0.));
#88027=DIRECTION('ref_axis',(0.407236366022499,0.,0.913322802840698));
#88028=DIRECTION('center_axis',(0.913322802840698,0.,-0.407236366022499));
#88029=DIRECTION('ref_axis',(0.,1.,0.));
#88030=DIRECTION('center_axis',(0.,1.,0.));
#88031=DIRECTION('ref_axis',(1.,0.,0.));
#88032=DIRECTION('center_axis',(0.,1.,0.));
#88033=DIRECTION('ref_axis',(-0.92054989510347,0.,0.390624999999987));
#88034=DIRECTION('center_axis',(0.,1.,0.));
#88035=DIRECTION('ref_axis',(1.,0.,0.));
#88036=DIRECTION('center_axis',(0.,1.,0.));
#88037=DIRECTION('ref_axis',(0.407236366022499,0.,-0.913322802840698));
#88038=DIRECTION('center_axis',(0.,1.,0.));
#88039=DIRECTION('ref_axis',(1.,0.,0.));
#88040=DIRECTION('center_axis',(-0.173648177666902,0.,-0.984807753012213));
#88041=DIRECTION('ref_axis',(-0.984807753012213,0.,0.173648177666902));
#88042=DIRECTION('center_axis',(0.404936583198885,-0.815730022456604,-0.413050716075109));
#88043=DIRECTION('ref_axis',(-0.853071505689579,-0.499641512218464,0.15042395237648));
#88044=DIRECTION('center_axis',(-0.984807753012213,2.368475785867E-17,0.173648177666902));
#88045=DIRECTION('ref_axis',(0.156623827406651,0.43181818181821,0.888257864890431));
#88046=DIRECTION('center_axis',(-0.822942767980762,0.55434158079449,-0.124380916665012));
#88047=DIRECTION('ref_axis',(0.566224638055893,0.818181846626126,-0.0998404983457853));
#88048=DIRECTION('center_axis',(-0.730772467313229,-0.554341581231179,0.398342832664342));
#88049=DIRECTION('ref_axis',(-0.566224585875474,0.818181842406769,0.0998408288527907));
#88050=DIRECTION('center_axis',(0.601034283802093,0.702059042596753,-0.381930478493975));
#88051=DIRECTION('ref_axis',(0.161931824632277,0.360993841660879,0.918401617188353));
#88052=DIRECTION('center_axis',(-0.984807753012213,2.368475785867E-17,0.173648177666902));
#88053=DIRECTION('ref_axis',(-0.166064467486216,-0.292298435122346,-0.941798395339229));
#88054=DIRECTION('center_axis',(0.201526976551162,0.962806257988152,-0.179974962983743));
#88055=DIRECTION('ref_axis',(0.171766241992109,0.146158578916091,0.974235098896122));
#88056=DIRECTION('center_axis',(-0.601034543449881,0.702058555044682,0.381930966103257));
#88057=DIRECTION('ref_axis',(0.161932171293584,-0.360994252463314,0.918401394592037));
#88058=DIRECTION('center_axis',(-0.984807753012213,2.368475785867E-17,0.173648177666902));
#88059=DIRECTION('ref_axis',(0.156623827406651,0.43181818181821,0.888257864890431));
#88060=DIRECTION('center_axis',(-0.73077246730534,0.554341581255442,0.39834283264505));
#88061=DIRECTION('ref_axis',(0.156623827039417,-0.431818181546998,0.888257865087031));
#88062=DIRECTION('center_axis',(0.822942767728722,0.554341581230101,0.124380916391147));
#88063=DIRECTION('ref_axis',(0.566224639647915,-0.818181842407621,-0.0998405238871412));
#88064=DIRECTION('center_axis',(-0.173648177666902,0.,-0.984807753012213));
#88065=DIRECTION('ref_axis',(-0.984807753012213,0.,0.173648177666902));
#88066=DIRECTION('center_axis',(-0.173648177666902,1.05109872153861E-17,
-0.984807753012213));
#88067=DIRECTION('ref_axis',(0.71842372566634,-0.68397380420233,-0.126677486416051));
#88068=DIRECTION('center_axis',(-0.173648177666903,4.8350541190776E-16,
-0.984807753012213));
#88069=DIRECTION('ref_axis',(-0.718423725666291,0.683973804202383,0.126677486416043));
#88070=DIRECTION('center_axis',(0.173648177666902,0.,0.984807753012213));
#88071=DIRECTION('ref_axis',(0.984807753012213,0.,-0.173648177666902));
#88072=DIRECTION('center_axis',(0.173648177666902,0.,0.984807753012213));
#88073=DIRECTION('ref_axis',(0.984807753012213,0.,-0.173648177666902));
#88074=DIRECTION('center_axis',(0.173648177666902,0.,0.984807753012213));
#88075=DIRECTION('ref_axis',(0.,-1.,0.));
#88076=DIRECTION('center_axis',(0.173648177666902,0.,0.984807753012213));
#88077=DIRECTION('ref_axis',(0.,-1.,0.));
#88078=DIRECTION('center_axis',(0.173648177666902,0.,0.984807753012213));
#88079=DIRECTION('ref_axis',(0.984807753012213,0.,-0.173648177666902));
#88080=DIRECTION('center_axis',(-0.173648177666902,-4.06038199430382E-17,
-0.984807753012213));
#88081=DIRECTION('ref_axis',(1.13553386910767E-16,1.,-6.12527251775702E-17));
#88082=DIRECTION('center_axis',(0.,-1.,0.));
#88083=DIRECTION('ref_axis',(0.173648177666898,0.,0.984807753012214));
#88084=DIRECTION('',(-1.726015970809E-11,-1.,3.043153626436E-12));
#88085=DIRECTION('center_axis',(0.,-1.,0.));
#88086=DIRECTION('ref_axis',(-0.173648177666898,0.,-0.984807753012214));
#88087=DIRECTION('center_axis',(0.,1.,0.));
#88088=DIRECTION('ref_axis',(0.984807678492017,0.,-0.173648600291403));
#88089=DIRECTION('',(2.443314655013E-11,-1.,-4.308252333139E-12));
#88090=DIRECTION('center_axis',(0.173648177666902,0.,0.984807753012213));
#88091=DIRECTION('ref_axis',(0.,-1.,0.));
#88092=DIRECTION('',(3.24463096977915E-7,0.999999999999946,-5.82194489842227E-8));
#88093=DIRECTION('center_axis',(0.920222040575711,0.356178462119004,-0.162259973996103));
#88094=DIRECTION('ref_axis',(0.12376266272234,-0.658093616333623,-0.742694819866687));
#88095=DIRECTION('center_axis',(0.241714278350237,-0.0321281187450775,0.969815442044272));
#88096=DIRECTION('ref_axis',(0.384280518492239,-0.914567435308961,-0.126074935572958));
#88097=DIRECTION('center_axis',(0.118051334199801,-0.733369237422903,0.669502385429205));
#88098=DIRECTION('ref_axis',(0.123762664959406,-0.658093610311519,-0.742694824830021));
#88099=DIRECTION('center_axis',(-1.92083386233814E-10,1.,-2.71332586028924E-11));
#88100=DIRECTION('ref_axis',(0.573562007104527,8.79450586429204E-11,-0.819162147566785));
#88101=DIRECTION('center_axis',(-0.926044070670311,-0.340292292317125,0.163228474739905));
#88102=DIRECTION('ref_axis',(0.374865784447703,-0.779130469521357,0.502425472198452));
#88103=DIRECTION('center_axis',(-0.730732981967633,0.554399311899593,0.398334924441667));
#88104=DIRECTION('ref_axis',(0.656438883269888,0.410464961352669,0.632934837114481));
#88105=DIRECTION('center_axis',(-0.984807753012213,-1.18056891774303E-16,
0.173648177666902));
#88106=DIRECTION('ref_axis',(0.0583004691281475,-0.941955046662688,0.330638390641696));
#88107=DIRECTION('center_axis',(-0.156564412664908,-0.432532134460024,-0.887920907145647));
#88108=DIRECTION('ref_axis',(-0.0751084169313595,0.901618518365421,-0.425960999443152));
#88109=DIRECTION('center_axis',(0.,0.,1.));
#88110=DIRECTION('ref_axis',(1.,0.,0.));
#88111=DIRECTION('center_axis',(0.,1.,0.));
#88112=DIRECTION('ref_axis',(0.173648177666898,0.,0.984807753012214));
#88113=DIRECTION('center_axis',(0.984807753012213,-2.19577442648087E-15,
-0.173648177666901));
#88114=DIRECTION('ref_axis',(-0.0751084169313502,0.901618518365437,-0.425960999443119));
#88115=DIRECTION('center_axis',(0.984807753012213,-2.96059473233375E-15,
-0.173648177666901));
#88116=DIRECTION('ref_axis',(0.0924969807172837,0.846323733445026,0.524576445111539));
#88117=DIRECTION('center_axis',(0.,1.,0.));
#88118=DIRECTION('ref_axis',(-0.81912263281209,0.,-0.573618438001247));
#88119=DIRECTION('center_axis',(-0.173648177666903,3.36351590892355E-16,
-0.984807753012213));
#88120=DIRECTION('ref_axis',(0.636767654207682,-0.762837013608687,-0.112279317879234));
#88121=DIRECTION('center_axis',(0.,-1.,0.));
#88122=DIRECTION('ref_axis',(-0.984807753012214,0.,0.173648177666898));
#88123=DIRECTION('center_axis',(-0.118051264626697,-0.733369608829381,-0.669501990859981));
#88124=DIRECTION('ref_axis',(0.123762305293398,0.65809327391301,-0.742695182843486));
#88125=DIRECTION('center_axis',(0.241762412222673,0.0322470771212345,0.969799495799731));
#88126=DIRECTION('ref_axis',(0.367434395505702,0.921979202041583,-0.122255126690558));
#88127=DIRECTION('center_axis',(-0.926007889327754,0.340399724817355,0.163209730858875));
#88128=DIRECTION('ref_axis',(-0.17347623837402,0.000278443640092277,-0.984838015710573));
#88129=DIRECTION('center_axis',(-0.920222117579503,0.356178256986601,0.162259987573902));
#88130=DIRECTION('ref_axis',(0.123762302773065,0.65809328252365,-0.742695175633689));
#88131=DIRECTION('center_axis',(-5.77150179500071E-11,-1.,-1.59649478822151E-10));
#88132=DIRECTION('ref_axis',(0.573570749823452,9.76712044575835E-11,-0.819156026009065));
#88133=DIRECTION('center_axis',(0.,1.,0.));
#88134=DIRECTION('ref_axis',(0.984807753012213,0.,-0.173648177666903));
#88135=DIRECTION('center_axis',(0.,-1.,0.));
#88136=DIRECTION('ref_axis',(-1.,0.,0.));
#88137=DIRECTION('center_axis',(0.,1.,0.));
#88138=DIRECTION('ref_axis',(1.,0.,0.));
#88139=DIRECTION('center_axis',(0.,1.,0.));
#88140=DIRECTION('ref_axis',(-0.638049918300179,0.,-0.76999500112477));
#88141=DIRECTION('',(1.42678478092006E-6,0.999999999998742,6.93297741290229E-7));
#88142=DIRECTION('center_axis',(0.,1.,0.));
#88143=DIRECTION('ref_axis',(0.353583464998389,0.,-0.935402979084273));
#88144=DIRECTION('center_axis',(0.,1.,0.));
#88145=DIRECTION('ref_axis',(-0.581942537871004,0.,0.813229907600707));
#88146=DIRECTION('center_axis',(-0.950253372983717,2.30324546582274E-6,
-0.311477972138905));
#88147=DIRECTION('ref_axis',(0.311477972127205,-4.36632101694612E-6,-0.950253372980312));
#88148=DIRECTION('center_axis',(0.,-1.,0.));
#88149=DIRECTION('ref_axis',(-1.,0.,0.));
#88150=DIRECTION('',(-1.37512520730395E-6,0.999999999998864,-6.16668900731678E-7));
#88151=DIRECTION('center_axis',(0.,1.,0.));
#88152=DIRECTION('ref_axis',(0.31147569764019,0.,-0.950254118528069));
#88153=DIRECTION('center_axis',(0.,-1.,0.));
#88154=DIRECTION('ref_axis',(-0.173648177666902,0.,-0.984807753012213));
#88155=DIRECTION('center_axis',(0.,1.,0.));
#88156=DIRECTION('ref_axis',(-0.951104406813913,0.,0.308869563633509));
#88157=DIRECTION('center_axis',(0.,-1.,0.));
#88158=DIRECTION('ref_axis',(0.173648177905701,0.,0.984807752970106));
#88159=DIRECTION('center_axis',(-0.173648177666902,0.,-0.984807753012213));
#88160=DIRECTION('ref_axis',(0.,-1.,0.));
#88161=DIRECTION('center_axis',(0.173648177666898,0.,0.984807753012214));
#88162=DIRECTION('ref_axis',(-0.984807753012214,0.,0.173648177666898));
#88163=DIRECTION('center_axis',(-0.173648177666902,0.,-0.984807753012213));
#88164=DIRECTION('ref_axis',(0.,1.,0.));
#88165=DIRECTION('center_axis',(0.,1.,0.));
#88166=DIRECTION('ref_axis',(0.855993839943912,0.,-0.516986021066407));
#88167=DIRECTION('center_axis',(0.,-1.,0.));
#88168=DIRECTION('ref_axis',(-0.984807753012213,0.,0.173648177666903));
#88169=DIRECTION('center_axis',(0.,1.,0.));
#88170=DIRECTION('ref_axis',(-0.638049654090004,0.,-0.769995220060246));
#88171=DIRECTION('center_axis',(0.308869563633505,0.,0.951104406813915));
#88172=DIRECTION('ref_axis',(0.,1.,0.));
#88173=DIRECTION('center_axis',(0.,-1.,0.));
#88174=DIRECTION('ref_axis',(0.91474129068957,0.,0.404040061265687));
#88175=DIRECTION('center_axis',(0.,-1.,0.));
#88176=DIRECTION('ref_axis',(-0.330689828029415,0.,0.943739496703341));
#88177=DIRECTION('center_axis',(0.173648177666901,-9.49857476623745E-16,
0.984807753012213));
#88178=DIRECTION('ref_axis',(-0.315957255971813,0.947136320160717,0.0557117889784327));
#88179=DIRECTION('center_axis',(0.173648177330704,6.22302969527983E-5,0.984807751105318));
#88180=DIRECTION('ref_axis',(0.782059007286606,0.607747668930201,-0.137936507248064));
#88181=DIRECTION('center_axis',(-0.468012284071803,0.720824709793966,0.511249684311236));
#88182=DIRECTION('ref_axis',(-0.526462193329491,-0.69207313268382,0.493834322432033));
#88183=DIRECTION('center_axis',(0.938122107850457,9.54847915278239E-5,-0.346304637053663));
#88184=DIRECTION('ref_axis',(0.342789334776549,-0.142378604065038,0.928560070791299));
#88185=DIRECTION('center_axis',(0.984807753012213,0.,-0.173648177666902));
#88186=DIRECTION('ref_axis',(0.,-1.,0.));
#88187=DIRECTION('center_axis',(0.984807753012213,4.71278345147005E-16,
-0.173648177666903));
#88188=DIRECTION('ref_axis',(0.119983582797752,-0.72289498517529,0.680460711773598));
#88189=DIRECTION('center_axis',(-0.984807753012213,-1.35945676484713E-17,
0.173648177666902));
#88190=DIRECTION('ref_axis',(-0.173356956027276,0.0578907986824709,-0.983156153021921));
#88191=DIRECTION('center_axis',(0.,-1.,0.));
#88192=DIRECTION('ref_axis',(0.819152071792271,0.,0.573576397072291));
#88193=DIRECTION('center_axis',(0.173648177666903,0.,0.984807753012213));
#88194=DIRECTION('ref_axis',(-0.984807753012213,0.,0.173648177666903));
#88195=DIRECTION('center_axis',(-0.984807753012213,-4.67879703234887E-16,
0.173648177666902));
#88196=DIRECTION('ref_axis',(0.00218187333490138,0.999921058430618,0.0123740185769414));
#88197=DIRECTION('center_axis',(-0.984807753012145,-1.27187584978315E-13,
0.17364817766729));
#88198=DIRECTION('ref_axis',(0.172089384615116,-0.133689495210303,0.975967398314721));
#88199=DIRECTION('center_axis',(4.0599214194867E-7,0.999999999999808,4.68423390877839E-7));
#88200=DIRECTION('ref_axis',(-0.984810514839275,3.18491799434328E-7,0.173632513838568));
#88201=DIRECTION('center_axis',(0.984807753012213,-2.13717932240342E-15,
-0.173648177666903));
#88202=DIRECTION('ref_axis',(-0.109429766257892,-0.776448339114791,-0.620607043903487));
#88203=DIRECTION('center_axis',(-0.442012531356003,-0.893567484242663,0.078498874058781));
#88204=DIRECTION('ref_axis',(0.273297331194067,-0.217505218314496,-0.937016568032905));
#88205=DIRECTION('center_axis',(-0.173648177666902,2.91433543964104E-16,
-0.984807753012213));
#88206=DIRECTION('ref_axis',(-0.595306851389017,-0.796612410881215,0.10496865970047));
#88207=DIRECTION('center_axis',(-0.173648177666902,0.,-0.984807753012213));
#88208=DIRECTION('ref_axis',(-0.984807753012213,0.,0.173648177666902));
#88209=DIRECTION('center_axis',(-0.173648177666902,0.,-0.984807753012213));
#88210=DIRECTION('ref_axis',(-0.984807753012213,0.,0.173648177666902));
#88211=DIRECTION('center_axis',(0.173648177666902,0.,0.984807753012213));
#88212=DIRECTION('ref_axis',(-0.984807753012213,-1.01064309961486E-15,0.173648177666902));
#88213=DIRECTION('axis',(0.,0.,1.));
#88214=DIRECTION('refdir',(1.,0.,0.));
#88215=DIRECTION('center_axis',(0.173648177666903,-6.04203006598724E-18,
0.984807753012213));
#88216=DIRECTION('ref_axis',(-0.984756463038268,-0.0102058657879588,0.173639133860657));
#88217=DIRECTION('center_axis',(-0.173648177666902,-4.61141851223429E-16,
-0.984807753012213));
#88218=DIRECTION('ref_axis',(0.927511157342012,-0.336119036715289,-0.163545241947503));
#88219=DIRECTION('center_axis',(0.173648177666903,-1.85288922023609E-16,
0.984807753012213));
#88220=DIRECTION('ref_axis',(0.942703464213078,0.289274509623319,-0.166224055548075));
#88221=DIRECTION('center_axis',(-0.173648177666902,-4.61141851223429E-16,
-0.984807753012213));
#88222=DIRECTION('ref_axis',(0.927511157342012,-0.336119036715289,-0.163545241947503));
#88223=DIRECTION('center_axis',(0.173648177666902,-1.50111279695127E-18,
0.984807753012213));
#88224=DIRECTION('ref_axis',(0.984806496090504,0.00159769267247521,-0.173647956037692));
#88225=DIRECTION('',(-0.173648177666902,1.50111279695126E-18,-0.984807753012213));
#88226=DIRECTION('',(-0.173648177666902,1.50111279695126E-18,-0.984807753012213));
#88227=DIRECTION('center_axis',(0.529918793382048,0.000598506209364813,
0.848048179180187));
#88228=DIRECTION('ref_axis',(0.848046930758909,0.00148135485041045,-0.529919058742183));
#88229=DIRECTION('center_axis',(0.173648177666902,-1.50111279695127E-18,
0.984807753012213));
#88230=DIRECTION('ref_axis',(0.984806496090504,0.00159769267247521,-0.173647956037692));
#88231=DIRECTION('center_axis',(0.529918793382048,0.000598506209364813,
0.848048179180187));
#88232=DIRECTION('ref_axis',(0.848046930758909,0.00148135485041045,-0.529919058742183));
#88233=DIRECTION('center_axis',(0.999998762173495,0.00157342029648582,2.18262210013749E-7));
#88234=DIRECTION('ref_axis',(-2.18262210388419E-7,0.000277436450264717,
-0.999999961514483));
#88235=DIRECTION('',(0.999998760211623,0.00157466659798374,5.66973100805864E-7));
#88236=DIRECTION('',(0.999998761676006,0.00157373645740291,1.29989624092794E-7));
#88237=DIRECTION('center_axis',(0.173648177666902,-1.49186218934005E-18,
0.984807753012213));
#88238=DIRECTION('ref_axis',(0.984806496090504,0.00159769267247521,-0.173647956037692));
#88239=DIRECTION('center_axis',(0.173648177666902,-1.49186218934005E-18,
0.984807753012213));
#88240=DIRECTION('ref_axis',(0.984806496090504,0.00159769267247533,-0.173647956037692));
#88241=DIRECTION('center_axis',(0.529918793382083,0.000598506209369939,
0.848048179180166));
#88242=DIRECTION('ref_axis',(0.848046930758885,0.00148135485220636,-0.529919058742217));
#88243=DIRECTION('',(0.173648177666902,-1.49186218934005E-18,0.984807753012213));
#88244=DIRECTION('',(0.173648177666902,-1.49186218934005E-18,0.984807753012213));
#88245=DIRECTION('center_axis',(-0.173648177666902,1.49186218934005E-18,
-0.984807753012213));
#88246=DIRECTION('ref_axis',(-0.984806496090504,-0.00159769267247533,0.173647956037692));
#88247=DIRECTION('center_axis',(-0.173648177666902,1.49186218934005E-18,
-0.984807753012213));
#88248=DIRECTION('ref_axis',(-0.984806496090504,-0.00159769267247533,0.173647956037692));
#88249=DIRECTION('center_axis',(0.529918793382083,0.000598506209369939,
0.848048179180166));
#88250=DIRECTION('ref_axis',(0.848046930758885,0.00148135485220636,-0.529919058742217));
#88251=DIRECTION('center_axis',(0.984806496090504,0.00159769267247521,-0.173647956037692));
#88252=DIRECTION('ref_axis',(-0.173648177666902,-7.3602384881327E-19,-0.984807753012213));
#88253=DIRECTION('',(0.984806496090504,0.00159769267247521,-0.173647956037692));
#88254=DIRECTION('center_axis',(-0.173648177666903,4.70361612381465E-17,
-0.984807753012213));
#88255=DIRECTION('ref_axis',(0.984806496090504,0.00159769267247229,-0.173647956037693));
#88256=DIRECTION('center_axis',(-0.529918793382001,-0.000598506209405786,
-0.848048179180217));
#88257=DIRECTION('ref_axis',(0.848046930758947,0.00148135484529274,-0.529919058742137));
#88258=DIRECTION('center_axis',(0.173648177666903,1.59201841970382E-16,
0.984807753012213));
#88259=DIRECTION('ref_axis',(0.00157342013078983,-0.999998723688248,-0.000277436421047882));
#88260=DIRECTION('center_axis',(-0.529918793384811,-0.000598506215654095,
-0.848048179178457));
#88261=DIRECTION('ref_axis',(0.848046930757165,0.00148135485777394,-0.529919058744953));
#88262=DIRECTION('center_axis',(0.173648177666903,-6.48778977136688E-18,
0.984807753012213));
#88263=DIRECTION('ref_axis',(-0.984749768728927,-0.0108514562123488,0.173637953473302));
#88264=DIRECTION('center_axis',(0.0106865982093938,-0.99994112121568,-0.00188433559630659));
#88265=DIRECTION('ref_axis',(0.984749768728927,0.0108514562123489,-0.173637953473302));
#88266=DIRECTION('center_axis',(-0.173648177666903,-8.10973730173238E-20,
-0.984807753012213));
#88267=DIRECTION('ref_axis',(0.984806496090504,0.00159769267248121,-0.173647956037693));
#88268=DIRECTION('center_axis',(0.173648177666902,7.29480667023956E-16,
0.984807753012213));
#88269=DIRECTION('ref_axis',(-0.80947494239616,0.569541759667294,0.14273227255185));
#88270=DIRECTION('center_axis',(-0.173648177666909,-8.8187772501904E-18,
-0.984807753012212));
#88271=DIRECTION('ref_axis',(-0.984806496090238,-0.00159769284073281,0.173647956037652));
#88272=DIRECTION('center_axis',(-0.00157342029648582,0.999998723687979,
0.000277436450264715));
#88273=DIRECTION('ref_axis',(0.173648177666899,-3.61333496938023E-18,0.984807753012214));
#88274=DIRECTION('center_axis',(0.173648177666903,2.70178024823687E-16,
0.984807753012213));
#88275=DIRECTION('ref_axis',(-0.808728963551724,-0.570633414289505,0.142600736354538));
#88276=DIRECTION('center_axis',(-0.00157342029648582,0.999998723687979,
0.000277436450264715));
#88277=DIRECTION('ref_axis',(0.173648177666899,-3.61333496938023E-18,0.984807753012214));
#88278=DIRECTION('center_axis',(-0.173648177666904,-2.99281451101198E-15,
-0.984807753012213));
#88279=DIRECTION('ref_axis',(-0.343208372641265,-0.93730769666911,0.0605168961016933));
#88280=DIRECTION('center_axis',(0.984806496090504,0.00159769267247521,-0.173647956037693));
#88281=DIRECTION('ref_axis',(-0.173648177666903,-5.3530757125254E-20,-0.984807753012213));
#88282=DIRECTION('',(0.984806496090504,0.00159769267247521,-0.173647956037693));
#88283=DIRECTION('center_axis',(0.984806496090504,0.00159769267247521,-0.173647956037693));
#88284=DIRECTION('ref_axis',(-0.173648177666903,-3.73849559887003E-19,-0.984807753012213));
#88285=DIRECTION('center_axis',(0.89187284005045,0.424065723658381,-0.157261245061962));
#88286=DIRECTION('ref_axis',(7.57847339502874E-18,-0.347702922065335,-0.937604755740513));
#88287=DIRECTION('',(-0.417623212445505,0.905631416205343,0.0736382401242789));
#88288=DIRECTION('',(0.173648177666903,1.77379537806039E-19,0.984807753012213));
#88289=DIRECTION('',(-0.417623212445505,0.905631416205343,0.0736382401242789));
#88290=DIRECTION('',(0.173648177666806,-1.57202615380602E-16,0.98480775301223));
#88291=DIRECTION('center_axis',(-0.173648177666903,1.42314599624734E-16,
-0.984807753012213));
#88292=DIRECTION('ref_axis',(-0.00157342013078447,0.999998723688248,0.000277436421047244));
#88293=DIRECTION('center_axis',(-0.173648177666903,3.93652485185651E-17,
-0.984807753012213));
#88294=DIRECTION('ref_axis',(0.893202752211758,-0.421169721037697,-0.157495744457965));
#88295=DIRECTION('center_axis',(-0.173648177666903,-2.95239363889238E-17,
-0.984807753012213));
#88296=DIRECTION('ref_axis',(0.893202752211758,-0.421169721037697,-0.157495744457965));
#88297=DIRECTION('',(0.173648177666709,1.74490518016149E-14,0.984807753012247));
#88298=DIRECTION('center_axis',(-0.173648177666903,-1.77379537806039E-19,
-0.984807753012213));
#88299=DIRECTION('ref_axis',(-0.984807753012213,3.83929687396358E-37,0.173648177666903));
#88300=DIRECTION('center_axis',(0.173648177666903,0.,0.984807753012213));
#88301=DIRECTION('ref_axis',(0.417623212445507,-0.905631416205343,-0.0736382401242741));
#88302=DIRECTION('',(0.893202752211756,-0.421169721037697,-0.157495744457976));
#88303=DIRECTION('center_axis',(-0.173648177666903,7.16660291201912E-16,
-0.984807753012213));
#88304=DIRECTION('ref_axis',(-0.00157342013078448,0.999998723688248,0.000277436421047828));
#88305=DIRECTION('center_axis',(-0.173648177666903,-3.48020931800866E-17,
-0.984807753012213));
#88306=DIRECTION('ref_axis',(0.893202752211759,-0.421169721037697,-0.157495744457965));
#88307=DIRECTION('',(0.173648177666903,1.77379537806039E-19,0.984807753012213));
#88308=DIRECTION('center_axis',(-0.414771206611954,-0.906981844405385,0.0731353545466874));
#88309=DIRECTION('ref_axis',(-0.909417241788805,0.415884936415402,2.11769803727567E-18));
#88310=DIRECTION('',(0.893202752211756,-0.421169721037697,-0.157495744457976));
#88311=DIRECTION('center_axis',(0.173648177666903,1.77379537806039E-19,
0.984807753012213));
#88312=DIRECTION('ref_axis',(1.02148804663124E-18,-1.,1.45468743896681E-36));
#88313=DIRECTION('center_axis',(0.173648177666903,-6.88891849074889E-17,
0.984807753012213));
#88314=DIRECTION('ref_axis',(0.891872840050451,0.424065723658381,-0.157261245061954));
#88315=DIRECTION('',(-0.414771206611954,-0.906981844405386,0.0731353545466775));
#88316=DIRECTION('center_axis',(-0.173648177666903,-2.43614652260606E-16,
-0.984807753012213));
#88317=DIRECTION('ref_axis',(0.414771206611955,0.906981844405385,-0.0731353545466813));
#88318=DIRECTION('',(0.89187284005045,0.424065723658381,-0.157261245061962));
#88319=DIRECTION('center_axis',(0.173648177666903,-1.42314599624734E-16,
0.984807753012213));
#88320=DIRECTION('ref_axis',(0.00157342013078447,-0.999998723688248,-0.000277436421047244));
#88321=DIRECTION('',(0.173648177666806,-1.57202615380602E-16,0.98480775301223));
#88322=DIRECTION('',(0.173648177666902,5.32908145459909E-14,0.984807753012213));
#88323=DIRECTION('center_axis',(0.173648177666903,-6.88891849074889E-17,
0.984807753012213));
#88324=DIRECTION('ref_axis',(0.891872840050451,0.424065723658381,-0.157261245061954));
#88325=DIRECTION('center_axis',(-0.893202752211757,0.421169721037697,0.157495744457976));
#88326=DIRECTION('ref_axis',(0.173648177666915,8.8205638096327E-18,0.984807753012211));
#88327=DIRECTION('',(0.173648177666903,1.77379537806039E-19,0.984807753012213));
#88328=DIRECTION('',(-0.414771206611954,-0.906981844405384,0.0731353545466974));
#88329=DIRECTION('center_axis',(0.173648177666903,-7.16660291201912E-16,
0.984807753012213));
#88330=DIRECTION('ref_axis',(0.00157342013078448,-0.999998723688248,-0.000277436421047828));
#88331=DIRECTION('',(0.173648177667,1.57513029571763E-16,0.984807753012196));
#88332=DIRECTION('center_axis',(0.173648177666903,-8.12048840868686E-17,
0.984807753012213));
#88333=DIRECTION('ref_axis',(0.891872840050451,0.424065723658381,-0.157261245061954));
#88334=DIRECTION('center_axis',(0.417623212445504,-0.905631416205343,-0.0736382401242889));
#88335=DIRECTION('ref_axis',(4.02781508425194E-18,0.081044018053505,-0.996710523240195));
#88336=DIRECTION('',(0.89187284005045,0.424065723658381,-0.157261245061962));
#88337=DIRECTION('center_axis',(-0.00145739791678334,-0.999846419038759,
-0.0174646593635094));
#88338=DIRECTION('ref_axis',(-2.53744808518323E-21,0.0174646779110831,-0.99984748088169));
#88339=DIRECTION('',(0.173649190170913,-0.0174523841625769,0.984652920089119));
#88340=DIRECTION('',(0.984806496090239,0.00159769284073286,-0.173647956037646));
#88341=DIRECTION('',(0.173649190225314,-0.0174523841624888,0.984652920079526));
#88342=DIRECTION('',(-0.984806496090294,-0.00159769284073286,0.173647956037338));
#88343=DIRECTION('center_axis',(0.173648177666903,-9.44812840053846E-15,
0.984807753012213));
#88344=DIRECTION('ref_axis',(-0.00157342029648291,0.999998723687979,0.000277436450273798));
#88345=DIRECTION('center_axis',(0.173648177666903,6.91086727774848E-15,
0.984807753012213));
#88346=DIRECTION('ref_axis',(0.00157342029648635,-0.999998723687979,-0.000277436450257794));
#88347=DIRECTION('',(0.190808973440195,2.78835766832232E-5,0.981627187315635));
#88348=DIRECTION('center_axis',(-0.173648177666897,1.00951792985966E-17,
-0.984807753012214));
#88349=DIRECTION('ref_axis',(0.98480649609024,0.00159769284073303,-0.17364795603764));
#88350=DIRECTION('center_axis',(0.981625926717135,0.00159744950437461,-0.190808773780994));
#88351=DIRECTION('ref_axis',(-1.58138488522882E-19,-0.99996495671813,-0.00837169849608073));
#88352=DIRECTION('',(-0.00157342029648582,0.999998723687979,0.000277436450264717));
#88353=DIRECTION('',(0.190808973440108,2.7883631917396E-5,0.981627187315651));
#88354=DIRECTION('',(0.0015734202964251,-0.999998723687979,-0.000277436450577356));
#88355=DIRECTION('center_axis',(0.173648177666903,-6.57942269886179E-19,
0.984807753012213));
#88356=DIRECTION('ref_axis',(-0.984806496090239,-0.00159769284073276,0.173647956037646));
#88357=DIRECTION('center_axis',(0.173648177666894,-1.47993596544271E-17,
0.984807753012215));
#88358=DIRECTION('ref_axis',(0.984806496090241,0.00159769284073259,-0.173647956037637));
#88359=DIRECTION('',(0.173594270245887,0.0174523841625767,0.984662603953679));
#88360=DIRECTION('center_axis',(-0.173648177666903,-3.35757540913268E-15,
-0.984807753012213));
#88361=DIRECTION('ref_axis',(-0.00157342029648637,0.999998723687979,0.000277436450261404));
#88362=DIRECTION('center_axis',(-0.00460375923069061,0.999846419038759,
-0.0169098709728103));
#88363=DIRECTION('ref_axis',(-0.964879947320468,-1.01243743119455E-18,0.262691239402557));
#88364=DIRECTION('',(-0.984806496090239,-0.00159769284073286,0.173647956037646));
#88365=DIRECTION('',(0.173594270191486,0.0174523841624883,0.984662603963271));
#88366=DIRECTION('',(0.984806496090188,0.00159769284073286,-0.173647956037937));
#88367=DIRECTION('center_axis',(0.98480649609024,0.00159769284073286,-0.173647956037645));
#88368=DIRECTION('ref_axis',(-0.173648177666902,-4.25482427716051E-18,-0.984807753012213));
#88369=DIRECTION('center_axis',(0.98480649609024,0.00159769284073286,-0.173647956037645));
#88370=DIRECTION('ref_axis',(0.173648177666902,5.15300653782458E-19,0.984807753012213));
#88371=DIRECTION('center_axis',(0.98480649609024,0.00159769284073286,-0.173647956037645));
#88372=DIRECTION('ref_axis',(0.173648177666902,4.25482427716051E-18,0.984807753012213));
#88373=DIRECTION('',(0.984806496090163,0.00159769288929177,-0.173647956037633));
#88374=DIRECTION('center_axis',(0.173648177666903,-1.63457705018331E-15,
0.984807753012213));
#88375=DIRECTION('ref_axis',(0.224660098927353,-0.973631655051934,-0.039613636929517));
#88376=DIRECTION('center_axis',(0.00157342029648582,-0.999998723687979,
-0.000277436450264715));
#88377=DIRECTION('ref_axis',(0.173648177666901,7.61225010390707E-20,0.984807753012213));
#88378=DIRECTION('center_axis',(-0.173648177666903,4.34089614276706E-15,
-0.984807753012213));
#88379=DIRECTION('ref_axis',(-0.00157342029648684,0.999998723687979,0.000277436450269305));
#88380=DIRECTION('center_axis',(0.00157342029648582,-0.999998723687979,
-0.000277436450264715));
#88381=DIRECTION('ref_axis',(-0.173648177666901,4.11768476579406E-19,-0.984807753012213));
#88382=DIRECTION('center_axis',(0.00157342029648582,-0.999998723687979,
-0.000277436450264715));
#88383=DIRECTION('ref_axis',(0.173648177666901,7.61225010390707E-20,0.984807753012213));
#88384=DIRECTION('',(0.0015734203443027,-0.999998723687901,-0.000277436458698203));
#88385=DIRECTION('center_axis',(0.173648177666904,4.18775938476715E-16,
0.984807753012213));
#88386=DIRECTION('ref_axis',(-0.958840002473252,-0.228125843079737,0.169069362618583));
#88387=DIRECTION('center_axis',(-0.98480649609024,-0.00159769284073286,
0.173647956037645));
#88388=DIRECTION('ref_axis',(0.173648177666902,5.15300653782458E-19,0.984807753012213));
#88389=DIRECTION('center_axis',(-0.173648177666903,5.80467749850325E-19,
-0.984807753012213));
#88390=DIRECTION('ref_axis',(0.984806496090239,0.00159769284073277,-0.173647956037646));
#88391=DIRECTION('center_axis',(-0.98480649609024,-0.00159769284073286,
0.173647956037645));
#88392=DIRECTION('ref_axis',(-0.173648177666902,-4.25482427716051E-18,-0.984807753012213));
#88393=DIRECTION('center_axis',(-0.98480649609024,-0.00159769284073286,
0.173647956037645));
#88394=DIRECTION('ref_axis',(0.173648177666902,4.25482427716051E-18,0.984807753012213));
#88395=DIRECTION('',(-0.984806496090163,-0.00159769288928886,0.173647956037633));
#88396=DIRECTION('center_axis',(0.173648177666903,-1.63457705018331E-15,
0.984807753012213));
#88397=DIRECTION('ref_axis',(-0.224660098927352,0.973631655051934,0.039613636929517));
#88398=DIRECTION('center_axis',(-0.00157342029648582,0.999998723687979,
0.000277436450264715));
#88399=DIRECTION('ref_axis',(0.173648177666899,-3.61333496938023E-18,0.984807753012214));
#88400=DIRECTION('center_axis',(-0.173648177666903,-3.35757540913268E-15,
-0.984807753012213));
#88401=DIRECTION('ref_axis',(0.00157342029648637,-0.999998723687979,-0.000277436450261404));
#88402=DIRECTION('center_axis',(-0.173648177666903,4.55102546821287E-15,
-0.984807753012213));
#88403=DIRECTION('ref_axis',(0.00157342029648563,-0.999998723687979,-0.000277436450269305));
#88404=DIRECTION('center_axis',(0.173648177666899,-5.37964561848111E-18,
0.984807753012214));
#88405=DIRECTION('ref_axis',(0.98480649609024,0.00159769284073276,-0.173647956037643));
#88406=DIRECTION('',(0.156434486976668,-2.78836790155617E-5,0.987688336727152));
#88407=DIRECTION('center_axis',(0.173648177666894,-1.47993596544271E-17,
0.984807753012215));
#88408=DIRECTION('ref_axis',(-0.984806496090241,-0.00159769284073259,0.173647956037637));
#88409=DIRECTION('center_axis',(-0.987687083864603,-0.00159744950437461,
0.156434243444705));
#88410=DIRECTION('ref_axis',(-0.00161736185591408,0.999998692069458,-1.3098294468559E-20));
#88411=DIRECTION('',(-0.0015672529834684,0.999998721807879,0.000316386936718628));
#88412=DIRECTION('',(-0.156434487048126,2.79785493473008E-5,-0.987688336713151));
#88413=DIRECTION('',(0.00157343755135569,-0.999998723691179,-0.000277327037485099));
#88414=DIRECTION('center_axis',(-0.00157342029648582,0.999998723687979,
0.000277436450264715));
#88415=DIRECTION('ref_axis',(0.813978516242862,0.00111957060601937,0.580893898794544));
#88416=DIRECTION('center_axis',(-0.173648177666903,1.67985947297096E-15,
-0.984807753012213));
#88417=DIRECTION('ref_axis',(0.343208372641262,0.937307696669111,-0.0605168961016879));
#88418=DIRECTION('center_axis',(-0.173648177666903,7.07772878971226E-16,
-0.984807753012213));
#88419=DIRECTION('ref_axis',(-0.343208372641267,-0.937307696669109,0.0605168961016898));
#88420=DIRECTION('',(-0.167631936046611,0.016358281640073,-0.985713924340652));
#88421=DIRECTION('center_axis',(-0.819151155511157,-0.00112973932296881,
-0.573576593066522));
#88422=DIRECTION('ref_axis',(0.573575547587063,0.00112973047439091,-0.819151887575959));
#88423=DIRECTION('center_axis',(-0.00111431000077956,0.999999196217831,
0.000604877603267272));
#88424=DIRECTION('ref_axis',(-0.814897680756574,-0.0005574592593905,-0.579604571355964));
#88425=DIRECTION('center_axis',(0.0019082391455338,-0.999997900468177,-0.000746781495225125));
#88426=DIRECTION('ref_axis',(-0.581802269400352,-0.00171760010831627,0.81332845097812));
#88427=DIRECTION('center_axis',(0.173648177666903,-3.30780989858582E-15,
0.984807753012213));
#88428=DIRECTION('ref_axis',(0.0015734202964841,-0.999998723687979,-0.000277436450267774));
#88429=DIRECTION('',(0.156434486976398,-2.78835073328855E-5,0.987688336727199));
#88430=DIRECTION('',(-0.16758048981795,-0.0163387632005932,-0.985722995698817));
#88431=DIRECTION('center_axis',(0.819151155513041,0.00112973931574178,0.573576593063845));
#88432=DIRECTION('ref_axis',(0.573575547570477,0.00112973931585084,-0.819151887575378));
#88433=DIRECTION('center_axis',(-0.987687083864603,-0.00159744950437461,
0.156434243444705));
#88434=DIRECTION('ref_axis',(-0.00161736185591408,0.999998692069458,-1.3098294468559E-20));
#88435=DIRECTION('',(0.156434486976551,-2.78836043610342E-5,0.987688336727172));
#88436=DIRECTION('',(-0.00157342029645223,0.999998723687979,0.000277436450476588));
#88437=DIRECTION('',(0.00157342026969061,-0.999998723687974,-0.000277436619430731));
#88438=DIRECTION('center_axis',(0.1736481776669,-5.09813795295912E-18,0.984807753012213));
#88439=DIRECTION('ref_axis',(0.98480649609024,0.00159769284073301,-0.173647956037644));
#88440=DIRECTION('center_axis',(0.819151155513551,0.00112973933284856,0.573576593063084));
#88441=DIRECTION('ref_axis',(0.573575547569693,0.00112973932749382,-0.819151887575911));
#88442=DIRECTION('center_axis',(-0.00157342029648582,0.999998723687979,
0.000277436450264715));
#88443=DIRECTION('ref_axis',(-0.173648177666899,4.10122594699871E-18,-0.984807753012214));
#88444=DIRECTION('',(-0.00157342029692248,0.999998723687978,0.000277436450337063));
#88445=DIRECTION('center_axis',(-0.173648177666916,-2.23918124064188E-17,
-0.984807753012211));
#88446=DIRECTION('ref_axis',(0.984806496049417,0.00159771878360705,-0.173647956030462));
#88447=DIRECTION('center_axis',(-0.00157342029648582,0.999998723687979,
0.000277436450264715));
#88448=DIRECTION('ref_axis',(0.813978512696035,0.00111957059905984,0.580893903764556));
#88449=DIRECTION('center_axis',(-0.00157342029648582,0.999998723687979,
0.000277436450264715));
#88450=DIRECTION('ref_axis',(0.173648177666899,-3.61333496938023E-18,0.984807753012214));
#88451=DIRECTION('',(-0.00157958616680064,0.999998724013009,0.00023849506217036));
#88452=DIRECTION('center_axis',(0.173648177666904,4.18775938476715E-16,
0.984807753012213));
#88453=DIRECTION('ref_axis',(0.958840002473252,0.228125843079737,-0.169069362618583));
#88454=DIRECTION('center_axis',(-0.173648177666897,1.00951792985966E-17,
-0.984807753012214));
#88455=DIRECTION('ref_axis',(-0.98480649609024,-0.00159769284073303,0.17364795603764));
#88456=DIRECTION('center_axis',(-0.173648177666903,6.33237545291264E-19,
-0.984807753012213));
#88457=DIRECTION('ref_axis',(-0.984806496090239,-0.00159769284070554,0.173647956037646));
#88458=DIRECTION('center_axis',(0.173648177666903,-4.92055672404642E-15,
0.984807753012213));
#88459=DIRECTION('ref_axis',(0.00157342029648369,-0.999998723687979,-0.000277436450269339));
#88460=DIRECTION('center_axis',(0.173648177666903,6.91086727774848E-15,
0.984807753012213));
#88461=DIRECTION('ref_axis',(-0.00157342029648636,0.999998723687979,0.000277436450257794));
#88462=DIRECTION('',(0.156434486976507,-2.78835766825765E-5,0.98768833672718));
#88463=DIRECTION('center_axis',(-0.987687083864603,-0.00159744950437461,
0.156434243444705));
#88464=DIRECTION('ref_axis',(-0.00161736185591408,0.999998692069458,-1.3098294468559E-20));
#88465=DIRECTION('',(-0.156434486979456,2.79313446666122E-5,-0.987688336725363));
#88466=DIRECTION('',(0.00157342022766082,-0.999998723688078,-0.000277436481588655));
#88467=DIRECTION('center_axis',(-0.173648177666904,-2.48013246669082E-18,
-0.984807753012213));
#88468=DIRECTION('ref_axis',(0.809998687527633,-0.568773463940462,-0.142824622949545));
#88469=DIRECTION('center_axis',(-0.819151155512569,-0.0011297393161222,
-0.573576593064518));
#88470=DIRECTION('ref_axis',(0.573575547571143,0.00112973932052989,-0.819151887574906));
#88471=DIRECTION('center_axis',(0.819151155511153,0.00112973932295936,0.573576593066528));
#88472=DIRECTION('ref_axis',(4.42381266920449E-20,-0.999998060265046,0.0019696360437663));
#88473=DIRECTION('',(0.00157341843450662,-0.999998723688043,-0.000277446777199153));
#88474=DIRECTION('center_axis',(-0.173648177666903,-1.77379537806039E-19,
-0.984807753012213));
#88475=DIRECTION('ref_axis',(-0.984807753012213,3.83929687396358E-37,0.173648177666903));
#88476=DIRECTION('',(0.00157342029648582,-0.999998723687979,-0.000277436450264717));
#88477=DIRECTION('',(0.984806496090239,0.00159769284073286,-0.173647956037646));
#88478=DIRECTION('',(-0.00157342029648582,0.999998723687979,0.000277436450264717));
#88479=DIRECTION('',(0.984806496090239,0.00159769284073286,-0.173647956037646));
#88480=DIRECTION('',(-0.00157342029648582,0.999998723687979,0.000277436450264717));
#88481=DIRECTION('',(-0.984806496090239,-0.00159769284073286,0.173647956037646));
#88482=DIRECTION('',(-0.00157342029648582,0.999998723687979,0.000277436450264717));
#88483=DIRECTION('',(-0.984806496090239,-0.00159769284073286,0.173647956037646));
#88484=DIRECTION('center_axis',(-0.984806496090239,-0.00159769284073286,
0.173647956037646));
#88485=DIRECTION('ref_axis',(-0.0016223397637217,0.99999868400598,2.63557796693769E-20));
#88486=DIRECTION('',(0.173648177666903,1.77379537806039E-19,0.984807753012213));
#88487=DIRECTION('',(0.173648177666903,1.77379537806039E-19,0.984807753012213));
#88488=DIRECTION('',(-0.00157342029648582,0.999998723687979,0.000277436450264717));
#88489=DIRECTION('center_axis',(0.00157342029648582,-0.999998723687979,
-0.000277436450264717));
#88490=DIRECTION('ref_axis',(-2.2370400977484E-23,0.000277436793683327,
-0.999999961514412));
#88491=DIRECTION('',(0.173648177666903,1.77379537806039E-19,0.984807753012213));
#88492=DIRECTION('',(-0.984806496090239,-0.00159769284073286,0.173647956037646));
#88493=DIRECTION('center_axis',(0.984806496090239,0.00159769284073286,-0.173647956037646));
#88494=DIRECTION('ref_axis',(-1.16826950231067E-19,-0.999957675712221,-0.00920036869984769));
#88495=DIRECTION('',(0.173648177666903,1.77379537806039E-19,0.984807753012213));
#88496=DIRECTION('',(0.00157342029648582,-0.999998723687979,-0.00027743645028658));
#88497=DIRECTION('center_axis',(0.00157342029648582,-0.999998723687979,
-0.000277436450264717));
#88498=DIRECTION('ref_axis',(-2.2370400977484E-23,0.000277436793683327,
-0.999999961514412));
#88499=DIRECTION('',(0.173648177666903,1.77379537806039E-19,0.984807753012213));
#88500=DIRECTION('',(-0.984806496090222,-0.00159769284073286,0.173647956037743));
#88501=DIRECTION('center_axis',(0.984806496090239,0.00159769284073286,-0.173647956037646));
#88502=DIRECTION('ref_axis',(-1.16826950231067E-19,-0.999957675712221,-0.00920036869984769));
#88503=DIRECTION('',(0.173648177666903,1.77379537806039E-19,0.984807753012213));
#88504=DIRECTION('',(0.00157342029648582,-0.999998723687979,-0.000277436450264717));
#88505=DIRECTION('center_axis',(-0.00157342029648582,0.999998723687979,
0.000277436450264717));
#88506=DIRECTION('ref_axis',(0.173648177666903,-3.52094571672426E-20,0.984807753012213));
#88507=DIRECTION('',(0.173648177666903,1.77379537806039E-19,0.984807753012213));
#88508=DIRECTION('',(0.984806496090222,0.00159769284073286,-0.173647956037743));
#88509=DIRECTION('center_axis',(0.984806496090239,0.00159769284073286,-0.173647956037646));
#88510=DIRECTION('ref_axis',(-1.16826950231067E-19,-0.999957675712221,-0.00920036869984769));
#88511=DIRECTION('',(0.173648177666903,1.77379537806039E-19,0.984807753012213));
#88512=DIRECTION('',(0.00157342029648582,-0.999998723687979,-0.000277436450264717));
#88513=DIRECTION('center_axis',(-0.00157342029648582,0.999998723687979,
0.000277436450264717));
#88514=DIRECTION('ref_axis',(0.173648177666903,-3.52094571672426E-20,0.984807753012213));
#88515=DIRECTION('',(0.984806496090239,0.00159769284073286,-0.173647956037646));
#88516=DIRECTION('center_axis',(0.173648177666903,1.77379537806039E-19,
0.984807753012213));
#88517=DIRECTION('ref_axis',(1.02148804663124E-18,-1.,1.45468743896681E-36));
#88518=DIRECTION('center_axis',(0.173648177666903,1.77379537806039E-19,
0.984807753012213));
#88519=DIRECTION('ref_axis',(1.02148804663124E-18,-1.,1.45468743896681E-36));
#88520=DIRECTION('center_axis',(0.529918793382054,0.000598506209361558,
0.848048179180184));
#88521=DIRECTION('ref_axis',(0.0011294293297492,-0.999999362194491,-4.78634101357847E-20));
#88522=DIRECTION('',(0.00157342013088156,-0.999998723688247,-0.000277436420824379));
#88523=DIRECTION('',(0.00157342013076796,-0.999998723688248,-0.000277436421032639));
#88524=DIRECTION('center_axis',(0.173648177666903,1.77379537806039E-19,
0.984807753012213));
#88525=DIRECTION('ref_axis',(1.02148804663124E-18,-1.,1.45468743896681E-36));
#88526=DIRECTION('center_axis',(-0.314055242383514,-0.91431658158538,-0.255723470509566));
#88527=DIRECTION('ref_axis',(0.629237412598948,0.00124254729691768,-0.777212155503242));
#88528=DIRECTION('center_axis',(0.316965079769398,-0.913473350106414,0.255146187218511));
#88529=DIRECTION('ref_axis',(0.629162965906753,0.00120921019910097,-0.777272474838851));
#88530=DIRECTION('center_axis',(0.662632777829612,0.144272974524305,0.734917077341194));
#88531=DIRECTION('ref_axis',(0.742560405946752,0.00129143749156779,-0.669777855493447));
#88532=DIRECTION('center_axis',(0.146692737802188,0.952760334528529,-0.265949216252245));
#88533=DIRECTION('ref_axis',(-0.000412525464939198,0.268916590385109,0.963163380345406));
#88534=DIRECTION('center_axis',(-0.239999751079929,-0.186076176852954,-0.952772677971698));
#88535=DIRECTION('ref_axis',(-0.00155278376594829,0.9815301219139,-0.191301355557826));
#88536=DIRECTION('center_axis',(0.999998762173495,0.00157342029648582,2.18262210013629E-7));
#88537=DIRECTION('ref_axis',(-2.18262210388565E-7,0.000277436450264733,
-0.999999961514484));
#88538=DIRECTION('',(0.999998762247466,0.00157337326398415,3.28322100784373E-7));
#88539=DIRECTION('center_axis',(0.240601503772138,-0.185862702176551,0.95266257002268));
#88540=DIRECTION('ref_axis',(0.00153245606422671,-0.981421019486281,-0.191860454729264));
#88541=DIRECTION('center_axis',(-0.149644118021572,0.952159144810393,0.266457502982158));
#88542=DIRECTION('ref_axis',(0.000424375672975945,-0.269430126258093,0.963019847651042));
#88543=DIRECTION('center_axis',(0.999998762173495,0.00157342029648582,2.18262210013629E-7));
#88544=DIRECTION('ref_axis',(-2.18262210388565E-7,0.000277436450264733,
-0.999999961514484));
#88545=DIRECTION('',(0.999998762516763,0.00157320126714693,1.64818022882485E-6));
#88546=DIRECTION('center_axis',(-0.663074807330075,0.142596683678673,-0.734845552267978));
#88547=DIRECTION('ref_axis',(0.742562201227128,0.00135037093647457,-0.669775748894401));
#88548=DIRECTION('center_axis',(-0.252940505516454,0.721654216431443,-0.644388308844753));
#88549=DIRECTION('ref_axis',(0.931456534788202,0.00158377533602745,-0.363849165803687));
#88550=DIRECTION('center_axis',(0.250670969471596,0.722091646399503,0.644785017865819));
#88551=DIRECTION('ref_axis',(0.00105715928539588,-0.666254233378766,0.745723929426378));
#88552=DIRECTION('center_axis',(0.999998762173495,0.00157342029648582,2.1826221001363E-7));
#88553=DIRECTION('ref_axis',(-2.18262210388565E-7,0.000277436450264734,
-0.999999961514484));
#88554=DIRECTION('',(0.999998762173495,0.00157342029648582,2.18262209944475E-7));
#88555=DIRECTION('center_axis',(0.134465664742365,0.000413144039032103,
0.990918167316251));
#88556=DIRECTION('ref_axis',(0.990647603194621,-0.0234266874123494,-0.134419182416933));
#88557=DIRECTION('center_axis',(-0.275261853306783,-0.318164219754394,-0.907194819970988));
#88558=DIRECTION('ref_axis',(-0.927511143457601,0.336119090075094,0.16354521102455));
#88559=DIRECTION('center_axis',(-0.00157337729948021,0.999998723772464,
0.000277375768317332));
#88560=DIRECTION('ref_axis',(-0.98480671474633,-0.00159763995970335,0.173646716459311));
#88561=DIRECTION('center_axis',(0.276268688411157,-0.317806043628553,0.907014294505189));
#88562=DIRECTION('ref_axis',(-0.926448783505642,-0.33912381130528,0.163363680623008));
#88563=DIRECTION('center_axis',(0.999998762173495,0.00157342029648582,2.1826221001363E-7));
#88564=DIRECTION('ref_axis',(-2.18262210388565E-7,0.000277436450264734,
-0.999999961514484));
#88565=DIRECTION('center_axis',(0.134373628028009,0.000182201052963753,
0.990930721540798));
#88566=DIRECTION('ref_axis',(0.990818423918398,0.0150309177067826,-0.134361163796515));
#88567=DIRECTION('',(0.999998762173495,0.00157342029648582,2.18262209944475E-7));
#88568=DIRECTION('center_axis',(0.999998762173495,0.00157342029648582,2.18262210013657E-7));
#88569=DIRECTION('ref_axis',(2.18261402645051E-7,-0.000277435936897481,
0.999999961514626));
#88570=DIRECTION('center_axis',(0.966997552472099,-0.18932204760366,-0.170507758779852));
#88571=DIRECTION('ref_axis',(-0.17364740989288,4.04346645584571E-6,-0.984807888382879));
#88572=DIRECTION('center_axis',(-0.966395599704911,-0.192457245450031,0.170410544112656));
#88573=DIRECTION('ref_axis',(0.00103847482039741,-0.66584029656634,-0.74609357391583));
#88574=DIRECTION('center_axis',(0.975127266349125,-0.139841305698193,-0.171962855416822));
#88575=DIRECTION('ref_axis',(-0.00123501906440318,0.772405548492563,-0.635128446367987));
#88576=DIRECTION('center_axis',(0.173651504889683,2.11958655523597E-5,0.984807166099173));
#88577=DIRECTION('ref_axis',(0.984521190641717,-0.0241012604084658,-0.173600559976454));
#88578=DIRECTION('center_axis',(-0.974685226395651,-0.143017999760238,0.171856222437942));
#88579=DIRECTION('ref_axis',(0.00122150236050521,-0.772045967302346,-0.635565521645226));
#88580=DIRECTION('center_axis',(0.173652216761134,-2.53504643415288E-5,
0.984807040476102));
#88581=DIRECTION('ref_axis',(0.984520060172094,0.0241442914896521,-0.173600991665369));
#88582=DIRECTION('center_axis',(0.173648177666903,1.77379537806039E-19,
0.984807753012213));
#88583=DIRECTION('ref_axis',(1.02148804663124E-18,-1.,1.45468743896681E-36));
#88584=DIRECTION('axis',(0.,0.,1.));
#88585=DIRECTION('refdir',(1.,0.,0.));
#88586=DIRECTION('center_axis',(0.173648177666903,0.,0.984807753012213));
#88587=DIRECTION('ref_axis',(0.984807753012213,0.,-0.173648177666903));
#88588=DIRECTION('',(-0.173648177666903,0.,-0.984807753012213));
#88589=DIRECTION('center_axis',(-0.173648177666903,0.,-0.984807753012213));
#88590=DIRECTION('ref_axis',(0.984807753012213,0.,-0.173648177666903));
#88591=DIRECTION('center_axis',(0.173648177666903,0.,0.984807753012213));
#88592=DIRECTION('ref_axis',(0.984807753012213,0.,-0.173648177666903));
#88593=DIRECTION('',(-0.173648177666903,0.,-0.984807753012213));
#88594=DIRECTION('center_axis',(0.173648177666903,0.,0.984807753012213));
#88595=DIRECTION('ref_axis',(0.984807753012213,0.,-0.173648177666903));
#88596=DIRECTION('',(-0.173648177666903,0.,-0.984807753012213));
#88597=DIRECTION('center_axis',(0.173648177666903,0.,0.984807753012213));
#88598=DIRECTION('ref_axis',(0.984807753012213,0.,-0.173648177666903));
#88599=DIRECTION('',(-0.173648177666903,0.,-0.984807753012213));
#88600=DIRECTION('center_axis',(0.173648177666903,0.,0.984807753012213));
#88601=DIRECTION('ref_axis',(0.984807753012213,0.,-0.173648177666903));
#88602=DIRECTION('',(-0.173648177666903,0.,-0.984807753012213));
#88603=DIRECTION('center_axis',(0.173648177666903,0.,0.984807753012213));
#88604=DIRECTION('ref_axis',(0.984807753012213,0.,-0.173648177666903));
#88605=DIRECTION('',(-0.173648177666903,0.,-0.984807753012213));
#88606=DIRECTION('center_axis',(0.173648177666903,0.,0.984807753012213));
#88607=DIRECTION('ref_axis',(0.984807753012213,0.,-0.173648177666903));
#88608=DIRECTION('',(-0.173648177666903,0.,-0.984807753012213));
#88609=DIRECTION('center_axis',(0.173648177666903,0.,0.984807753012213));
#88610=DIRECTION('ref_axis',(-0.984807753012213,0.,0.173648177666903));
#88611=DIRECTION('center_axis',(-0.173648177666902,0.,-0.984807753012213));
#88612=DIRECTION('ref_axis',(-0.984807753012213,0.,0.173648177666902));
#88613=DIRECTION('',(0.173648177666902,0.,0.984807753012213));
#88614=DIRECTION('center_axis',(0.173648177666902,0.,0.984807753012213));
#88615=DIRECTION('ref_axis',(0.984807753012213,0.,-0.173648177666902));
#88616=DIRECTION('center_axis',(-0.173648177666902,0.,-0.984807753012213));
#88617=DIRECTION('ref_axis',(-0.984807753012213,0.,0.173648177666902));
#88618=DIRECTION('',(0.173648177666902,0.,0.984807753012213));
#88619=DIRECTION('center_axis',(-0.173648177666902,0.,-0.984807753012213));
#88620=DIRECTION('ref_axis',(-0.984807753012213,0.,0.173648177666902));
#88621=DIRECTION('',(0.173648177666902,0.,0.984807753012213));
#88622=DIRECTION('center_axis',(-0.173648177666902,0.,-0.984807753012213));
#88623=DIRECTION('ref_axis',(-0.984807753012213,0.,0.173648177666902));
#88624=DIRECTION('',(0.173648177666902,0.,0.984807753012213));
#88625=DIRECTION('center_axis',(-0.173648177666902,0.,-0.984807753012213));
#88626=DIRECTION('ref_axis',(-0.984807753012213,0.,0.173648177666902));
#88627=DIRECTION('',(0.173648177666902,0.,0.984807753012213));
#88628=DIRECTION('center_axis',(-0.173648177666902,0.,-0.984807753012213));
#88629=DIRECTION('ref_axis',(-0.984807753012213,0.,0.173648177666902));
#88630=DIRECTION('',(0.173648177666902,0.,0.984807753012213));
#88631=DIRECTION('center_axis',(-0.173648177666902,0.,-0.984807753012213));
#88632=DIRECTION('ref_axis',(-0.984807753012213,0.,0.173648177666902));
#88633=DIRECTION('',(0.173648177666902,0.,0.984807753012213));
#88634=DIRECTION('center_axis',(-0.173648177666902,0.,-0.984807753012213));
#88635=DIRECTION('ref_axis',(-0.984807753012213,0.,0.173648177666902));
#88636=DIRECTION('',(-0.573576435615923,8.65956055458343E-17,0.81915204480373));
#88637=DIRECTION('center_axis',(0.173648177666902,0.,0.984807753012213));
#88638=DIRECTION('ref_axis',(0.984807753012213,0.,-0.173648177666902));
#88639=DIRECTION('center_axis',(0.173648177666903,0.,0.984807753012213));
#88640=DIRECTION('ref_axis',(0.984807753012213,0.,-0.173648177666903));
#88641=DIRECTION('',(-0.173648177666903,0.,-0.984807753012213));
#88642=DIRECTION('center_axis',(0.173648177666903,0.,0.984807753012213));
#88643=DIRECTION('ref_axis',(-0.984807753012213,0.,0.173648177666903));
#88644=DIRECTION('center_axis',(0.173648177666903,0.,0.984807753012213));
#88645=DIRECTION('ref_axis',(0.984807753012213,0.,-0.173648177666903));
#88646=DIRECTION('',(-0.173648177666903,0.,-0.984807753012213));
#88647=DIRECTION('center_axis',(0.173648177666903,0.,0.984807753012213));
#88648=DIRECTION('ref_axis',(0.984807753012213,0.,-0.173648177666903));
#88649=DIRECTION('',(-0.173648177666903,0.,-0.984807753012213));
#88650=DIRECTION('center_axis',(0.173648177666903,0.,0.984807753012213));
#88651=DIRECTION('ref_axis',(0.984807753012213,0.,-0.173648177666903));
#88652=DIRECTION('',(-0.173648177666903,0.,-0.984807753012213));
#88653=DIRECTION('center_axis',(0.173648177666903,0.,0.984807753012213));
#88654=DIRECTION('ref_axis',(0.984807753012213,0.,-0.173648177666903));
#88655=DIRECTION('',(-0.173648177666903,0.,-0.984807753012213));
#88656=DIRECTION('center_axis',(0.173648177666902,0.,0.984807753012213));
#88657=DIRECTION('ref_axis',(0.984807753012213,0.,-0.173648177666902));
#88658=DIRECTION('',(-0.173648177666902,0.,-0.984807753012213));
#88659=DIRECTION('center_axis',(0.173648177666902,0.,0.984807753012213));
#88660=DIRECTION('ref_axis',(-0.984807753012213,0.,0.173648177666902));
#88661=DIRECTION('center_axis',(0.173648177666902,0.,0.984807753012213));
#88662=DIRECTION('ref_axis',(0.984807753012213,0.,-0.173648177666902));
#88663=DIRECTION('',(-0.173648177666902,0.,-0.984807753012213));
#88664=DIRECTION('center_axis',(0.173648177666902,0.,0.984807753012213));
#88665=DIRECTION('ref_axis',(0.984807753012213,0.,-0.173648177666902));
#88666=DIRECTION('',(-0.173648177666902,0.,-0.984807753012213));
#88667=DIRECTION('center_axis',(0.173648177666902,0.,0.984807753012213));
#88668=DIRECTION('ref_axis',(0.984807753012213,0.,-0.173648177666902));
#88669=DIRECTION('',(-0.173648177666902,0.,-0.984807753012213));
#88670=DIRECTION('center_axis',(0.173648177666902,0.,0.984807753012213));
#88671=DIRECTION('ref_axis',(0.984807753012213,0.,-0.173648177666902));
#88672=DIRECTION('',(-0.173648177666902,0.,-0.984807753012213));
#88673=DIRECTION('center_axis',(0.173648177666902,0.,0.984807753012213));
#88674=DIRECTION('ref_axis',(0.984807753012213,0.,-0.173648177666902));
#88675=DIRECTION('',(-0.173648177666902,0.,-0.984807753012213));
#88676=DIRECTION('center_axis',(-0.173648177666902,0.,-0.984807753012213));
#88677=DIRECTION('ref_axis',(-0.984807753012213,0.,0.173648177666902));
#88678=DIRECTION('',(0.766044442349839,-1.0605752379922E-16,-0.642787610603163));
#88679=DIRECTION('center_axis',(0.173648177666903,0.,0.984807753012213));
#88680=DIRECTION('ref_axis',(-0.984807753012213,0.,0.173648177666903));
#88681=DIRECTION('center_axis',(0.173648177666902,0.,0.984807753012213));
#88682=DIRECTION('ref_axis',(0.984807753012213,0.,-0.173648177666902));
#88683=DIRECTION('center_axis',(-0.173648177666902,0.,-0.984807753012213));
#88684=DIRECTION('ref_axis',(0.984807753012213,0.,-0.173648177666902));
#88685=DIRECTION('center_axis',(0.173648177666902,0.,0.984807753012213));
#88686=DIRECTION('ref_axis',(0.984807753012213,0.,-0.173648177666902));
#88687=DIRECTION('center_axis',(0.173648177666902,0.,0.984807753012213));
#88688=DIRECTION('ref_axis',(0.984807753012213,0.,-0.173648177666902));
#88689=DIRECTION('',(-0.173648177666902,0.,-0.984807753012213));
#88690=DIRECTION('center_axis',(0.173648177666902,0.,0.984807753012213));
#88691=DIRECTION('ref_axis',(0.984807753012213,0.,-0.173648177666902));
#88692=DIRECTION('center_axis',(0.173648177666902,0.,0.984807753012213));
#88693=DIRECTION('ref_axis',(0.984807753012213,0.,-0.173648177666902));
#88694=DIRECTION('center_axis',(0.173648177666902,0.,0.984807753012213));
#88695=DIRECTION('ref_axis',(0.984807753012213,0.,-0.173648177666902));
#88696=DIRECTION('center_axis',(0.173648177666902,0.,0.984807753012213));
#88697=DIRECTION('ref_axis',(0.984807753012213,0.,-0.173648177666902));
#88698=DIRECTION('',(-0.173648177666902,0.,-0.984807753012213));
#88699=DIRECTION('center_axis',(0.173648177666902,0.,0.984807753012213));
#88700=DIRECTION('ref_axis',(0.984807753012213,0.,-0.173648177666902));
#88701=DIRECTION('center_axis',(0.173648177666903,0.,0.984807753012213));
#88702=DIRECTION('ref_axis',(0.984807753012213,0.,-0.173648177666903));
#88703=DIRECTION('center_axis',(0.173648177666903,0.,0.984807753012213));
#88704=DIRECTION('ref_axis',(0.984807753012213,0.,-0.173648177666903));
#88705=DIRECTION('',(-0.173648177666903,0.,-0.984807753012213));
#88706=DIRECTION('center_axis',(0.173648177666903,0.,0.984807753012213));
#88707=DIRECTION('ref_axis',(0.984807753012213,0.,-0.173648177666903));
#88708=DIRECTION('center_axis',(0.173648177666903,0.,0.984807753012213));
#88709=DIRECTION('ref_axis',(0.984807753012213,0.,-0.173648177666903));
#88710=DIRECTION('center_axis',(-0.173648177666903,0.,-0.984807753012213));
#88711=DIRECTION('ref_axis',(0.984807753012213,0.,-0.173648177666903));
#88712=DIRECTION('center_axis',(-0.173648177666902,0.,-0.984807753012213));
#88713=DIRECTION('ref_axis',(-0.984807753012213,0.,0.173648177666902));
#88714=DIRECTION('center_axis',(0.173648177666903,0.,0.984807753012213));
#88715=DIRECTION('ref_axis',(-0.984807753012213,0.,0.173648177666903));
#88716=DIRECTION('',(-0.766044442349838,1.0605752379922E-16,0.642787610603164));
#88717=DIRECTION('center_axis',(0.173648177666902,0.,0.984807753012213));
#88718=DIRECTION('ref_axis',(0.984807753012213,0.,-0.173648177666902));
#88719=DIRECTION('center_axis',(-0.173648177666902,0.,-0.984807753012213));
#88720=DIRECTION('ref_axis',(0.984807753012213,0.,-0.173648177666902));
#88721=DIRECTION('center_axis',(-0.119891710860469,0.417487739272624,0.900738566524152));
#88722=DIRECTION('ref_axis',(0.837183562575301,0.530176150202612,-0.1343016467139));
#88723=DIRECTION('',(0.766044442349838,1.0605752379922E-16,-0.642787610603164));
#88724=DIRECTION('center_axis',(-0.173648177666902,0.,-0.984807753012213));
#88725=DIRECTION('ref_axis',(-0.984807753012213,0.,0.173648177666902));
#88726=DIRECTION('center_axis',(0.173648177666902,0.,0.984807753012213));
#88727=DIRECTION('ref_axis',(0.984807753012213,0.,-0.173648177666902));
#88728=DIRECTION('',(-0.173648177666902,0.,-0.984807753012213));
#88729=DIRECTION('center_axis',(-0.173648177666902,0.,-0.984807753012213));
#88730=DIRECTION('ref_axis',(-0.984807753012213,0.,0.173648177666902));
#88731=DIRECTION('center_axis',(0.173648177666902,0.,0.984807753012213));
#88732=DIRECTION('ref_axis',(0.984807753012213,0.,-0.173648177666902));
#88733=DIRECTION('center_axis',(-0.173648177666902,0.,-0.984807753012213));
#88734=DIRECTION('ref_axis',(-0.984807753012213,0.,0.173648177666902));
#88735=DIRECTION('center_axis',(0.173648177666902,0.,0.984807753012213));
#88736=DIRECTION('ref_axis',(-0.984807753012213,0.,0.173648177666902));
#88737=DIRECTION('',(-0.173648177666902,0.,-0.984807753012213));
#88738=DIRECTION('center_axis',(-0.173648177666902,0.,-0.984807753012213));
#88739=DIRECTION('ref_axis',(-0.984807753012213,0.,0.173648177666902));
#88740=DIRECTION('center_axis',(-0.173648177666902,0.,-0.984807753012213));
#88741=DIRECTION('ref_axis',(-0.984807753012213,0.,0.173648177666902));
#88742=DIRECTION('center_axis',(-0.173648177666902,0.,-0.984807753012213));
#88743=DIRECTION('ref_axis',(-0.984807753012213,0.,0.173648177666902));
#88744=DIRECTION('center_axis',(-1.2060416625019E-16,-1.,2.12657684957543E-17));
#88745=DIRECTION('ref_axis',(0.984807753012213,-1.22464679914735E-16,-0.173648177666903));
#88746=DIRECTION('center_axis',(0.173648177666903,0.,0.984807753012213));
#88747=DIRECTION('ref_axis',(0.984807753012213,0.,-0.173648177666903));
#88748=DIRECTION('center_axis',(1.2060416625019E-16,-1.,-2.12657684957544E-17));
#88749=DIRECTION('ref_axis',(-0.984807753012213,-1.22464679914735E-16,0.173648177666903));
#88750=DIRECTION('center_axis',(-0.173648177666902,0.,-0.984807753012213));
#88751=DIRECTION('ref_axis',(0.984807753012213,0.,-0.173648177666902));
#88752=DIRECTION('center_axis',(-0.173648177666904,0.,-0.984807753012213));
#88753=DIRECTION('ref_axis',(-0.984807753012213,0.,0.173648177666904));
#88754=DIRECTION('center_axis',(-0.173648177666902,0.,-0.984807753012213));
#88755=DIRECTION('ref_axis',(-0.984807753012213,0.,0.173648177666902));
#88756=DIRECTION('',(-0.173648177666902,0.,-0.984807753012213));
#88757=DIRECTION('center_axis',(0.173648177666902,0.,0.984807753012213));
#88758=DIRECTION('ref_axis',(0.984807753012213,0.,-0.173648177666902));
#88759=DIRECTION('',(-0.173648177666902,0.,-0.984807753012213));
#88760=DIRECTION('center_axis',(-0.173648177666902,0.,-0.984807753012213));
#88761=DIRECTION('ref_axis',(-0.984807753012213,0.,0.173648177666902));
#88762=DIRECTION('center_axis',(0.173648177666902,0.,0.984807753012213));
#88763=DIRECTION('ref_axis',(0.984807753012213,0.,-0.173648177666902));
#88764=DIRECTION('center_axis',(0.173648177666902,0.,0.984807753012213));
#88765=DIRECTION('ref_axis',(0.984807753012213,0.,-0.173648177666902));
#88766=DIRECTION('',(0.573576435615923,8.65956055458343E-17,-0.81915204480373));
#88767=DIRECTION('center_axis',(-0.173648177666902,0.,-0.984807753012213));
#88768=DIRECTION('ref_axis',(-0.984807753012213,0.,0.173648177666902));
#88769=DIRECTION('center_axis',(-0.173648177666902,0.,-0.984807753012213));
#88770=DIRECTION('ref_axis',(-0.984807753012213,0.,0.173648177666902));
#88771=DIRECTION('center_axis',(0.173648177666903,0.,0.984807753012213));
#88772=DIRECTION('ref_axis',(0.984807753012213,0.,-0.173648177666903));
#88773=DIRECTION('center_axis',(-0.984807753012213,-1.65054501924843E-16,
0.173648177666902));
#88774=DIRECTION('ref_axis',(-1.67600733666031E-16,1.,-4.61841862597087E-33));
#88775=DIRECTION('',(-1.62546953165154E-16,1.,2.86614134749672E-17));
#88776=DIRECTION('',(-0.173648177666902,0.,-0.984807753012213));
#88777=DIRECTION('',(1.62546953165154E-16,-1.,-2.86614134749672E-17));
#88778=DIRECTION('center_axis',(3.41673825694851E-16,-1.,-6.02463140718734E-17));
#88779=DIRECTION('ref_axis',(-1.26946471329372E-48,6.02463140718734E-17,
-1.));
#88780=DIRECTION('',(-0.984807753012213,-3.46944695195361E-16,0.173648177666902));
#88781=DIRECTION('',(-0.173648177666902,0.,-0.984807753012213));
#88782=DIRECTION('',(0.984807753012213,3.46944695195361E-16,-0.173648177666902));
#88783=DIRECTION('center_axis',(0.984807753012213,4.95163505774528E-16,
-0.173648177666902));
#88784=DIRECTION('ref_axis',(2.57199264728249E-34,-1.,-2.85153298138474E-15));
#88785=DIRECTION('',(4.87640859495463E-16,-1.,-8.59842404249014E-17));
#88786=DIRECTION('',(-0.173648177666902,0.,-0.984807753012213));
#88787=DIRECTION('',(-4.87640859495463E-16,1.,8.59842404249014E-17));
#88788=DIRECTION('center_axis',(-0.173648177666904,0.,-0.984807753012213));
#88789=DIRECTION('ref_axis',(0.984807753012213,-1.22464679914735E-16,-0.173648177666904));
#88790=DIRECTION('center_axis',(-0.173648177666902,0.,-0.984807753012213));
#88791=DIRECTION('ref_axis',(-0.984807753012213,0.,0.173648177666902));
#88792=DIRECTION('',(-0.173648177666902,0.,-0.984807753012213));
#88793=DIRECTION('center_axis',(0.173648177666902,0.,0.984807753012213));
#88794=DIRECTION('ref_axis',(0.984807753012213,0.,-0.173648177666902));
#88795=DIRECTION('center_axis',(0.984807753012213,4.95163505774529E-16,
-0.173648177666902));
#88796=DIRECTION('ref_axis',(-2.6719634195278E-33,-1.,-2.85153298138475E-15));
#88797=DIRECTION('',(4.87640859495464E-16,-1.,-8.59842404249016E-17));
#88798=DIRECTION('',(-0.173648177666902,0.,-0.984807753012213));
#88799=DIRECTION('',(-4.87640859495464E-16,1.,8.59842404249016E-17));
#88800=DIRECTION('center_axis',(0.,1.,0.));
#88801=DIRECTION('ref_axis',(1.,0.,0.));
#88802=DIRECTION('',(0.984807753012213,0.,-0.173648177666902));
#88803=DIRECTION('',(-0.173648177666902,0.,-0.984807753012213));
#88804=DIRECTION('',(-0.984807753012213,0.,0.173648177666902));
#88805=DIRECTION('center_axis',(-0.984807753012213,-1.65054501924843E-16,
0.173648177666902));
#88806=DIRECTION('ref_axis',(-1.67600733666031E-16,1.,-4.61841862597087E-33));
#88807=DIRECTION('',(-1.62546953165154E-16,1.,2.86614134749672E-17));
#88808=DIRECTION('',(1.62546953165154E-16,-1.,-2.86614134749672E-17));
#88809=DIRECTION('center_axis',(-0.173648177666902,0.,-0.984807753012213));
#88810=DIRECTION('ref_axis',(-0.984807753012213,0.,0.173648177666902));
#88811=DIRECTION('center_axis',(-0.173648177666902,0.,-0.984807753012213));
#88812=DIRECTION('ref_axis',(-0.984807753012213,0.,0.173648177666902));
#88813=DIRECTION('center_axis',(0.173648177666902,0.,0.984807753012213));
#88814=DIRECTION('ref_axis',(0.,-1.,0.));
#88815=DIRECTION('',(-0.492403876506108,-0.866025403784438,0.0868240888334514));
#88816=DIRECTION('',(-0.984807753012213,1.12673594905287E-15,0.173648177666902));
#88817=DIRECTION('',(-0.492403876506106,0.866025403784439,0.0868240888334511));
#88818=DIRECTION('',(0.492403876506108,0.866025403784438,-0.0868240888334516));
#88819=DIRECTION('',(0.984807753012213,-3.63059361361481E-15,-0.173648177666902));
#88820=DIRECTION('',(0.492403876506104,-0.86602540378444,-0.0868240888334507));
#88821=DIRECTION('center_axis',(-0.852868531952447,0.5,0.150383733180411));
#88822=DIRECTION('ref_axis',(0.173648177666903,1.44229019851021E-17,0.984807753012213));
#88823=DIRECTION('',(-0.173648177666902,0.,-0.984807753012213));
#88824=DIRECTION('',(-0.173648177666902,0.,-0.984807753012213));
#88825=DIRECTION('center_axis',(3.57543673872449E-15,1.,-6.30445964853305E-16));
#88826=DIRECTION('ref_axis',(1.,-3.57543673872449E-15,0.));
#88827=DIRECTION('',(-0.173648177666902,0.,-0.984807753012213));
#88828=DIRECTION('center_axis',(0.852868531952448,0.499999999999999,-0.150383733180411));
#88829=DIRECTION('ref_axis',(-2.28442492313379E-17,-0.288022074947211,-0.957623769725409));
#88830=DIRECTION('',(-0.173648177666902,0.,-0.984807753012213));
#88831=DIRECTION('center_axis',(0.852868531952447,-0.5,-0.150383733180411));
#88832=DIRECTION('ref_axis',(3.00594623393023E-17,0.28802207494721,-0.95762376972541));
#88833=DIRECTION('',(-0.173648177666902,0.,-0.984807753012213));
#88834=DIRECTION('center_axis',(-1.10961829822484E-15,-1.,1.95655644264819E-16));
#88835=DIRECTION('ref_axis',(-1.,1.10961829822484E-15,0.));
#88836=DIRECTION('',(-0.173648177666902,0.,-0.984807753012213));
#88837=DIRECTION('center_axis',(-0.852868531952448,-0.5,0.150383733180411));
#88838=DIRECTION('ref_axis',(-0.505751557519974,0.862679176789449,-2.10183654596508E-18));
#88839=DIRECTION('center_axis',(0.173648177666902,0.,0.984807753012213));
#88840=DIRECTION('ref_axis',(0.,-1.,0.));
#88841=DIRECTION('center_axis',(-0.173648177666902,0.,-0.984807753012213));
#88842=DIRECTION('ref_axis',(-0.984807753012213,0.,0.173648177666902));
#88843=DIRECTION('center_axis',(0.173648177666902,0.,0.984807753012213));
#88844=DIRECTION('ref_axis',(0.,-1.,0.));
#88845=DIRECTION('center_axis',(-0.173648177666902,0.,-0.984807753012213));
#88846=DIRECTION('ref_axis',(-0.984807753012213,0.,0.173648177666902));
#88847=DIRECTION('axis',(0.,0.,1.));
#88848=DIRECTION('refdir',(1.,0.,0.));
#88849=DIRECTION('center_axis',(1.,0.,0.));
#88850=DIRECTION('ref_axis',(0.,0.,-1.));
#88851=DIRECTION('center_axis',(1.,0.,0.));
#88852=DIRECTION('ref_axis',(0.,0.,-1.));
#88853=DIRECTION('center_axis',(0.,-1.,0.));
#88854=DIRECTION('ref_axis',(0.,0.,1.));
#88855=DIRECTION('center_axis',(1.,0.,0.));
#88856=DIRECTION('ref_axis',(0.,0.,-1.));
#88857=DIRECTION('center_axis',(1.,0.,0.));
#88858=DIRECTION('ref_axis',(0.,0.,-1.));
#88859=DIRECTION('center_axis',(1.,0.,0.));
#88860=DIRECTION('ref_axis',(0.,0.,-1.));
#88861=DIRECTION('center_axis',(0.,-1.,0.));
#88862=DIRECTION('ref_axis',(0.,0.,1.));
#88863=DIRECTION('center_axis',(1.,0.,0.));
#88864=DIRECTION('ref_axis',(0.,0.,-1.));
#88865=DIRECTION('center_axis',(1.,0.,0.));
#88866=DIRECTION('ref_axis',(0.,0.,-1.));
#88867=DIRECTION('center_axis',(1.,0.,0.));
#88868=DIRECTION('ref_axis',(0.,0.,-1.));
#88869=DIRECTION('',(-1.,0.,0.));
#88870=DIRECTION('center_axis',(1.,0.,0.));
#88871=DIRECTION('ref_axis',(0.,0.,-1.));
#88872=DIRECTION('',(-1.,0.,0.));
#88873=DIRECTION('center_axis',(1.,0.,0.));
#88874=DIRECTION('ref_axis',(0.,0.,1.));
#88875=DIRECTION('',(1.,0.,0.));
#88876=DIRECTION('center_axis',(1.,0.,0.));
#88877=DIRECTION('ref_axis',(0.,0.,-1.));
#88878=DIRECTION('',(-1.,0.,0.));
#88879=DIRECTION('center_axis',(1.,0.,0.));
#88880=DIRECTION('ref_axis',(0.,0.,1.));
#88881=DIRECTION('',(1.,0.,0.));
#88882=DIRECTION('center_axis',(1.,0.,0.));
#88883=DIRECTION('ref_axis',(0.,0.,-1.));
#88884=DIRECTION('',(-1.,0.,0.));
#88885=DIRECTION('center_axis',(1.,0.,0.));
#88886=DIRECTION('ref_axis',(0.,0.,1.));
#88887=DIRECTION('',(1.,0.,0.));
#88888=DIRECTION('center_axis',(1.,0.,0.));
#88889=DIRECTION('ref_axis',(0.,0.,-1.));
#88890=DIRECTION('center_axis',(1.,0.,0.));
#88891=DIRECTION('ref_axis',(0.,0.,-1.));
#88892=DIRECTION('center_axis',(1.,0.,0.));
#88893=DIRECTION('ref_axis',(0.,0.,-1.));
#88894=DIRECTION('center_axis',(0.,-1.,0.));
#88895=DIRECTION('ref_axis',(0.,0.,1.));
#88896=DIRECTION('center_axis',(1.,0.,0.));
#88897=DIRECTION('ref_axis',(0.,0.,-1.));
#88898=DIRECTION('center_axis',(1.,0.,0.));
#88899=DIRECTION('ref_axis',(0.,0.,-1.));
#88900=DIRECTION('center_axis',(1.,0.,0.));
#88901=DIRECTION('ref_axis',(0.,0.,-1.));
#88902=DIRECTION('center_axis',(0.,-1.,0.));
#88903=DIRECTION('ref_axis',(0.,0.,1.));
#88904=DIRECTION('center_axis',(1.,0.,0.));
#88905=DIRECTION('ref_axis',(0.,0.,-1.));
#88906=DIRECTION('center_axis',(1.,0.,0.));
#88907=DIRECTION('ref_axis',(0.,0.,-1.));
#88908=DIRECTION('center_axis',(1.,0.,0.));
#88909=DIRECTION('ref_axis',(0.,0.,-1.));
#88910=DIRECTION('',(1.,0.,0.));
#88911=DIRECTION('center_axis',(1.,0.,0.));
#88912=DIRECTION('ref_axis',(0.,0.,-1.));
#88913=DIRECTION('center_axis',(-1.,0.,0.));
#88914=DIRECTION('ref_axis',(0.,1.,-2.82534752406804E-15));
#88915=DIRECTION('center_axis',(-1.,0.,0.));
#88916=DIRECTION('ref_axis',(0.,1.,0.));
#88917=DIRECTION('center_axis',(-1.,0.,0.));
#88918=DIRECTION('ref_axis',(0.,1.,0.));
#88919=DIRECTION('center_axis',(-1.,0.,0.));
#88920=DIRECTION('ref_axis',(0.,0.,1.));
#88921=DIRECTION('center_axis',(-1.,0.,0.));
#88922=DIRECTION('ref_axis',(0.,-0.500000000000002,0.866025403784437));
#88923=DIRECTION('center_axis',(-1.,0.,0.));
#88924=DIRECTION('ref_axis',(0.,-0.500000000000002,0.866025403784437));
#88925=DIRECTION('center_axis',(-1.,0.,0.));
#88926=DIRECTION('ref_axis',(0.,0.,1.));
#88927=DIRECTION('center_axis',(-1.,0.,0.));
#88928=DIRECTION('ref_axis',(0.,0.,1.));
#88929=DIRECTION('center_axis',(-1.,0.,0.));
#88930=DIRECTION('ref_axis',(0.,-0.500000000000001,-0.866025403784438));
#88931=DIRECTION('center_axis',(-1.,0.,0.));
#88932=DIRECTION('ref_axis',(0.,-0.500000000000002,-0.866025403784437));
#88933=DIRECTION('center_axis',(-1.,0.,0.));
#88934=DIRECTION('ref_axis',(0.,-0.500000000000001,-0.866025403784438));
#88935=DIRECTION('center_axis',(-1.,0.,0.));
#88936=DIRECTION('ref_axis',(0.,0.,1.));
#88937=DIRECTION('center_axis',(1.,0.,0.));
#88938=DIRECTION('ref_axis',(0.,1.,0.));
#88939=DIRECTION('center_axis',(-1.,0.,0.));
#88940=DIRECTION('ref_axis',(0.,0.,1.));
#88941=DIRECTION('center_axis',(-1.,0.,0.));
#88942=DIRECTION('ref_axis',(0.,0.,1.));
#88943=DIRECTION('center_axis',(-1.,0.,0.));
#88944=DIRECTION('ref_axis',(0.,0.,1.));
#88945=DIRECTION('center_axis',(1.,0.,0.));
#88946=DIRECTION('ref_axis',(0.,1.,0.));
#88947=DIRECTION('center_axis',(1.,0.,0.));
#88948=DIRECTION('ref_axis',(0.,1.,0.));
#88949=DIRECTION('axis',(0.,0.,1.));
#88950=DIRECTION('refdir',(1.,0.,0.));
#88951=DIRECTION('center_axis',(-1.,0.,0.));
#88952=DIRECTION('ref_axis',(0.,0.,1.));
#88953=DIRECTION('',(-1.,0.,0.));
#88954=DIRECTION('',(-0.999999999965599,-7.79366993348666E-6,-2.83899568731E-6));
#88955=DIRECTION('center_axis',(-1.,0.,0.));
#88956=DIRECTION('ref_axis',(0.,0.,1.));
#88957=DIRECTION('',(-1.,0.,0.));
#88958=DIRECTION('center_axis',(-1.,0.,0.));
#88959=DIRECTION('ref_axis',(0.,0.,1.));
#88960=DIRECTION('',(-1.,0.,0.));
#88961=DIRECTION('center_axis',(1.,0.,0.));
#88962=DIRECTION('ref_axis',(0.,0.,-1.));
#88963=DIRECTION('',(1.,0.,0.));
#88964=DIRECTION('',(0.999999999992329,-8.06779582213464E-7,3.83300064466167E-6));
#88965=DIRECTION('',(1.,0.,0.));
#88966=DIRECTION('center_axis',(-1.,0.,0.));
#88967=DIRECTION('ref_axis',(0.,1.,0.));
#88968=DIRECTION('center_axis',(1.,0.,0.));
#88969=DIRECTION('ref_axis',(0.,0.,-1.));
#88970=DIRECTION('',(1.,0.,0.));
#88971=DIRECTION('center_axis',(1.,0.,0.));
#88972=DIRECTION('ref_axis',(0.,0.,-1.));
#88973=DIRECTION('',(1.,0.,0.));
#88974=DIRECTION('center_axis',(1.,0.,0.));
#88975=DIRECTION('ref_axis',(0.,0.,-1.));
#88976=DIRECTION('',(1.,0.,0.));
#88977=DIRECTION('center_axis',(1.,0.,0.));
#88978=DIRECTION('ref_axis',(0.,0.,-1.));
#88979=DIRECTION('',(1.,0.,0.));
#88980=DIRECTION('center_axis',(-1.,0.,0.));
#88981=DIRECTION('ref_axis',(0.,-0.957773424896036,-0.287524027801011));
#88982=DIRECTION('center_axis',(1.,0.,0.));
#88983=DIRECTION('ref_axis',(0.,0.,-1.));
#88984=DIRECTION('center_axis',(-1.,0.,0.));
#88985=DIRECTION('ref_axis',(0.,1.,0.));
#88986=DIRECTION('',(1.,0.,0.));
#88987=DIRECTION('center_axis',(1.,0.,0.));
#88988=DIRECTION('ref_axis',(0.,-1.,0.));
#88989=DIRECTION('center_axis',(1.,0.,0.));
#88990=DIRECTION('ref_axis',(0.,0.,-1.));
#88991=DIRECTION('center_axis',(-1.,0.,0.));
#88992=DIRECTION('ref_axis',(0.,-0.957773424896036,-0.287524027801011));
#88993=DIRECTION('center_axis',(-1.,0.,0.));
#88994=DIRECTION('ref_axis',(0.,0.,1.));
#88995=DIRECTION('center_axis',(-1.,0.,8.90699599727784E-17));
#88996=DIRECTION('ref_axis',(8.90699599727784E-17,0.,1.));
#88997=DIRECTION('',(-0.707106708341652,-8.65956145444752E-17,-0.707106854031435));
#88998=DIRECTION('center_axis',(1.,0.,0.));
#88999=DIRECTION('ref_axis',(0.,1.,0.));
#89000=DIRECTION('center_axis',(1.,0.,-6.83634867380023E-18));
#89001=DIRECTION('ref_axis',(-6.83634867380023E-18,0.,-1.));
#89002=DIRECTION('center_axis',(-1.,0.,0.));
#89003=DIRECTION('ref_axis',(0.,0.906250000000018,-0.422742164327108));
#89004=DIRECTION('center_axis',(-1.,0.,0.));
#89005=DIRECTION('ref_axis',(0.,0.087019546441882,-0.99620660434322));
#89006=DIRECTION('center_axis',(-1.,0.,0.));
#89007=DIRECTION('ref_axis',(0.,-0.819230453558104,-0.573464440016103));
#89008=DIRECTION('center_axis',(1.,0.,0.));
#89009=DIRECTION('ref_axis',(0.,-0.819230453558104,0.573464440016103));
#89010=DIRECTION('center_axis',(1.,0.,0.));
#89011=DIRECTION('ref_axis',(0.,0.087019546441882,0.99620660434322));
#89012=DIRECTION('',(-0.707106781821139,8.65956055458343E-17,-0.707106780551956));
#89013=DIRECTION('center_axis',(1.,0.,0.));
#89014=DIRECTION('ref_axis',(0.,-1.,0.));
#89015=DIRECTION('center_axis',(1.,0.,0.));
#89016=DIRECTION('ref_axis',(0.,0.087019546441882,0.99620660434322));
#89017=DIRECTION('center_axis',(1.,0.,0.));
#89018=DIRECTION('ref_axis',(0.,0.906250000000018,0.422742164327108));
#89019=DIRECTION('center_axis',(-1.,0.,-1.02545230107003E-16));
#89020=DIRECTION('ref_axis',(-1.02545230107003E-16,0.,1.));
#89021=DIRECTION('center_axis',(1.,0.,0.));
#89022=DIRECTION('ref_axis',(0.,0.906250000000018,0.422742164327108));
#89023=DIRECTION('center_axis',(1.,0.,0.));
#89024=DIRECTION('ref_axis',(0.,0.087019546441882,0.99620660434322));
#89025=DIRECTION('center_axis',(1.,0.,0.));
#89026=DIRECTION('ref_axis',(0.,-0.819230453558104,0.573464440016103));
#89027=DIRECTION('center_axis',(-1.,0.,0.));
#89028=DIRECTION('ref_axis',(0.,-0.819230453558104,-0.573464440016103));
#89029=DIRECTION('center_axis',(-1.,0.,0.));
#89030=DIRECTION('ref_axis',(0.,0.087019546441882,-0.99620660434322));
#89031=DIRECTION('',(0.707106781821139,8.65956055458343E-17,0.707106780551956));
#89032=DIRECTION('center_axis',(1.,0.,0.));
#89033=DIRECTION('ref_axis',(0.,1.,0.));
#89034=DIRECTION('center_axis',(-1.,0.,0.));
#89035=DIRECTION('ref_axis',(0.,0.087019546441882,-0.99620660434322));
#89036=DIRECTION('center_axis',(-1.,0.,0.));
#89037=DIRECTION('ref_axis',(0.,0.906250000000018,-0.422742164327108));
#89038=DIRECTION('center_axis',(1.,0.,0.));
#89039=DIRECTION('ref_axis',(0.,0.,-1.));
#89040=DIRECTION('',(1.,0.,0.));
#89041=DIRECTION('',(1.,0.,0.));
#89042=DIRECTION('center_axis',(0.,0.500000000000017,0.866025403784429));
#89043=DIRECTION('ref_axis',(1.,0.,0.));
#89044=DIRECTION('',(1.,0.,0.));
#89045=DIRECTION('',(1.,0.,0.));
#89046=DIRECTION('center_axis',(0.,-0.500000000000017,-0.866025403784429));
#89047=DIRECTION('ref_axis',(0.,-0.866025403784429,0.500000000000017));
#89048=DIRECTION('',(1.,0.,0.));
#89049=DIRECTION('center_axis',(0.,0.500000000000017,-0.866025403784429));
#89050=DIRECTION('ref_axis',(-1.,0.,0.));
#89051=DIRECTION('',(1.,0.,0.));
#89052=DIRECTION('center_axis',(1.,0.,0.));
#89053=DIRECTION('ref_axis',(0.,0.,-1.));
#89054=DIRECTION('',(1.,0.,0.));
#89055=DIRECTION('center_axis',(1.,0.,0.));
#89056=DIRECTION('ref_axis',(0.,0.,-1.));
#89057=DIRECTION('',(1.,0.,0.));
#89058=DIRECTION('center_axis',(0.,1.,0.));
#89059=DIRECTION('ref_axis',(1.,0.,0.));
#89060=DIRECTION('',(1.,0.,0.));
#89061=DIRECTION('center_axis',(0.,-0.500000000000017,0.866025403784429));
#89062=DIRECTION('ref_axis',(-1.,0.,0.));
#89063=DIRECTION('',(1.,0.,0.));
#89064=DIRECTION('',(1.,0.,0.));
#89065=DIRECTION('center_axis',(1.,0.,0.));
#89066=DIRECTION('ref_axis',(0.,0.,-1.));
#89067=DIRECTION('center_axis',(1.,0.,0.));
#89068=DIRECTION('ref_axis',(0.,0.,-1.));
#89069=DIRECTION('',(1.,0.,0.));
#89070=DIRECTION('center_axis',(1.,0.,0.));
#89071=DIRECTION('ref_axis',(0.,-5.35449122399261E-13,1.));
#89072=DIRECTION('center_axis',(0.,-1.,0.));
#89073=DIRECTION('ref_axis',(0.,0.,-1.));
#89074=DIRECTION('center_axis',(-1.,0.,0.));
#89075=DIRECTION('ref_axis',(0.,0.,1.));
#89076=DIRECTION('',(-0.461790830635515,-0.303368053954474,0.833496882166236));
#89077=DIRECTION('',(-0.461753481727668,0.303366050431034,-0.833518303073334));
#89078=DIRECTION('center_axis',(1.,0.,0.));
#89079=DIRECTION('ref_axis',(0.,1.,0.));
#89080=DIRECTION('center_axis',(-1.,0.,0.));
#89081=DIRECTION('ref_axis',(0.,0.,1.));
#89082=DIRECTION('axis',(0.,0.,1.));
#89083=DIRECTION('refdir',(1.,0.,0.));
#89084=DIRECTION('center_axis',(1.,0.,0.));
#89085=DIRECTION('ref_axis',(0.,0.,-1.));
#89086=DIRECTION('center_axis',(1.,0.,0.));
#89087=DIRECTION('ref_axis',(0.,0.,-1.));
#89088=DIRECTION('center_axis',(0.,-1.,0.));
#89089=DIRECTION('ref_axis',(0.,0.,1.));
#89090=DIRECTION('center_axis',(1.,0.,0.));
#89091=DIRECTION('ref_axis',(0.,0.,-1.));
#89092=DIRECTION('center_axis',(1.,0.,0.));
#89093=DIRECTION('ref_axis',(0.,0.,-1.));
#89094=DIRECTION('center_axis',(1.,0.,0.));
#89095=DIRECTION('ref_axis',(0.,0.,-1.));
#89096=DIRECTION('center_axis',(0.,-1.,0.));
#89097=DIRECTION('ref_axis',(0.,0.,1.));
#89098=DIRECTION('center_axis',(1.,0.,0.));
#89099=DIRECTION('ref_axis',(0.,0.,-1.));
#89100=DIRECTION('center_axis',(1.,0.,0.));
#89101=DIRECTION('ref_axis',(0.,0.,-1.));
#89102=DIRECTION('center_axis',(1.,0.,0.));
#89103=DIRECTION('ref_axis',(0.,0.,-1.));
#89104=DIRECTION('',(-1.,0.,0.));
#89105=DIRECTION('center_axis',(1.,0.,0.));
#89106=DIRECTION('ref_axis',(0.,0.,-1.));
#89107=DIRECTION('',(-1.,0.,0.));
#89108=DIRECTION('center_axis',(1.,0.,0.));
#89109=DIRECTION('ref_axis',(0.,0.,1.));
#89110=DIRECTION('',(1.,0.,0.));
#89111=DIRECTION('center_axis',(1.,0.,0.));
#89112=DIRECTION('ref_axis',(0.,0.,-1.));
#89113=DIRECTION('',(-1.,0.,0.));
#89114=DIRECTION('center_axis',(1.,0.,0.));
#89115=DIRECTION('ref_axis',(0.,0.,1.));
#89116=DIRECTION('',(1.,0.,0.));
#89117=DIRECTION('center_axis',(1.,0.,0.));
#89118=DIRECTION('ref_axis',(0.,0.,-1.));
#89119=DIRECTION('',(-1.,0.,0.));
#89120=DIRECTION('center_axis',(1.,0.,0.));
#89121=DIRECTION('ref_axis',(0.,0.,1.));
#89122=DIRECTION('',(1.,0.,0.));
#89123=DIRECTION('center_axis',(1.,0.,0.));
#89124=DIRECTION('ref_axis',(0.,0.,-1.));
#89125=DIRECTION('center_axis',(1.,0.,0.));
#89126=DIRECTION('ref_axis',(0.,0.,-1.));
#89127=DIRECTION('center_axis',(1.,0.,0.));
#89128=DIRECTION('ref_axis',(0.,0.,-1.));
#89129=DIRECTION('center_axis',(0.,-1.,0.));
#89130=DIRECTION('ref_axis',(0.,0.,1.));
#89131=DIRECTION('center_axis',(1.,0.,0.));
#89132=DIRECTION('ref_axis',(0.,0.,-1.));
#89133=DIRECTION('center_axis',(1.,0.,0.));
#89134=DIRECTION('ref_axis',(0.,0.,-1.));
#89135=DIRECTION('center_axis',(1.,0.,0.));
#89136=DIRECTION('ref_axis',(0.,0.,-1.));
#89137=DIRECTION('center_axis',(0.,-1.,0.));
#89138=DIRECTION('ref_axis',(0.,0.,1.));
#89139=DIRECTION('center_axis',(1.,0.,0.));
#89140=DIRECTION('ref_axis',(0.,0.,-1.));
#89141=DIRECTION('center_axis',(1.,0.,0.));
#89142=DIRECTION('ref_axis',(0.,0.,-1.));
#89143=DIRECTION('center_axis',(1.,0.,0.));
#89144=DIRECTION('ref_axis',(0.,0.,-1.));
#89145=DIRECTION('',(1.,0.,0.));
#89146=DIRECTION('center_axis',(1.,0.,0.));
#89147=DIRECTION('ref_axis',(0.,0.,-1.));
#89148=DIRECTION('center_axis',(-1.,0.,0.));
#89149=DIRECTION('ref_axis',(0.,1.,-1.71512449944288E-15));
#89150=DIRECTION('center_axis',(-1.,0.,0.));
#89151=DIRECTION('ref_axis',(0.,1.,0.));
#89152=DIRECTION('center_axis',(-1.,0.,0.));
#89153=DIRECTION('ref_axis',(0.,1.,0.));
#89154=DIRECTION('center_axis',(-1.,0.,0.));
#89155=DIRECTION('ref_axis',(0.,0.,1.));
#89156=DIRECTION('center_axis',(-1.,0.,0.));
#89157=DIRECTION('ref_axis',(0.,-0.500000000000002,0.866025403784437));
#89158=DIRECTION('center_axis',(-1.,0.,0.));
#89159=DIRECTION('ref_axis',(0.,-0.500000000000002,0.866025403784437));
#89160=DIRECTION('center_axis',(-1.,0.,0.));
#89161=DIRECTION('ref_axis',(0.,0.,1.));
#89162=DIRECTION('center_axis',(-1.,0.,0.));
#89163=DIRECTION('ref_axis',(0.,0.,1.));
#89164=DIRECTION('center_axis',(-1.,0.,0.));
#89165=DIRECTION('ref_axis',(0.,-0.500000000000001,-0.866025403784438));
#89166=DIRECTION('center_axis',(-1.,0.,0.));
#89167=DIRECTION('ref_axis',(0.,-0.499999999999999,-0.866025403784439));
#89168=DIRECTION('center_axis',(-1.,0.,0.));
#89169=DIRECTION('ref_axis',(0.,-0.500000000000001,-0.866025403784438));
#89170=DIRECTION('center_axis',(-1.,0.,0.));
#89171=DIRECTION('ref_axis',(0.,0.,1.));
#89172=DIRECTION('center_axis',(1.,0.,0.));
#89173=DIRECTION('ref_axis',(0.,1.,0.));
#89174=DIRECTION('center_axis',(-1.,0.,0.));
#89175=DIRECTION('ref_axis',(0.,0.,1.));
#89176=DIRECTION('center_axis',(-1.,0.,0.));
#89177=DIRECTION('ref_axis',(0.,0.,1.));
#89178=DIRECTION('center_axis',(-1.,0.,0.));
#89179=DIRECTION('ref_axis',(0.,0.,1.));
#89180=DIRECTION('center_axis',(1.,0.,0.));
#89181=DIRECTION('ref_axis',(0.,1.,0.));
#89182=DIRECTION('center_axis',(1.,0.,0.));
#89183=DIRECTION('ref_axis',(0.,1.,0.));
#89184=DIRECTION('axis',(0.,0.,1.));
#89185=DIRECTION('refdir',(1.,0.,0.));
#89186=DIRECTION('center_axis',(1.,0.,0.));
#89187=DIRECTION('ref_axis',(0.,0.924224592736303,0.381849318686593));
#89188=DIRECTION('center_axis',(1.,0.,0.));
#89189=DIRECTION('ref_axis',(0.,0.381849318686592,-0.924224592736303));
#89190=DIRECTION('center_axis',(0.,0.381849318686593,-0.924224592736303));
#89191=DIRECTION('ref_axis',(0.,-0.924224592736303,-0.381849318686593));
#89192=DIRECTION('center_axis',(1.,0.,0.));
#89193=DIRECTION('ref_axis',(0.,0.381849318686593,-0.924224592736303));
#89194=DIRECTION('center_axis',(1.,0.,0.));
#89195=DIRECTION('ref_axis',(0.,0.924224592736303,0.381849318686593));
#89196=DIRECTION('',(-1.,0.,0.));
#89197=DIRECTION('center_axis',(1.,0.,0.));
#89198=DIRECTION('ref_axis',(0.,0.381849318686593,-0.924224592736303));
#89199=DIRECTION('center_axis',(-1.,0.,0.));
#89200=DIRECTION('ref_axis',(0.,0.381849318686589,-0.924224592736304));
#89201=DIRECTION('center_axis',(-1.,0.,0.));
#89202=DIRECTION('ref_axis',(0.,-0.228299548172813,0.973590938897897));
#89203=DIRECTION('',(1.,0.,0.));
#89204=DIRECTION('center_axis',(-1.,0.,0.));
#89205=DIRECTION('ref_axis',(0.,-0.228299548172813,0.973590938897897));
#89206=DIRECTION('',(1.,0.,0.));
#89207=DIRECTION('center_axis',(-1.,0.,0.));
#89208=DIRECTION('ref_axis',(0.,-0.381849318686606,0.924224592736298));
#89209=DIRECTION('center_axis',(-1.,0.,0.));
#89210=DIRECTION('ref_axis',(0.,-0.890419977397047,-0.455139828901232));
#89211=DIRECTION('center_axis',(-1.,0.,0.));
#89212=DIRECTION('ref_axis',(0.,-0.890419977397047,-0.455139828901232));
#89213=DIRECTION('center_axis',(1.,0.,0.));
#89214=DIRECTION('ref_axis',(0.,0.924224592736303,0.381849318686593));
#89215=DIRECTION('center_axis',(1.,0.,0.));
#89216=DIRECTION('ref_axis',(0.,0.381849318686593,-0.924224592736303));
#89217=DIRECTION('center_axis',(0.,-0.381849318686593,0.924224592736303));
#89218=DIRECTION('ref_axis',(0.,-0.924224592736303,-0.381849318686593));
#89219=DIRECTION('center_axis',(1.,0.,0.));
#89220=DIRECTION('ref_axis',(0.,0.381849318686592,-0.924224592736303));
#89221=DIRECTION('center_axis',(1.,0.,0.));
#89222=DIRECTION('ref_axis',(0.,0.924224592736303,0.381849318686593));
#89223=DIRECTION('center_axis',(1.,0.,0.));
#89224=DIRECTION('ref_axis',(0.,0.381849318686593,-0.924224592736303));
#89225=DIRECTION('',(1.,0.,0.));
#89226=DIRECTION('center_axis',(1.,2.78424187714042E-18,1.15032739033389E-18));
#89227=DIRECTION('ref_axis',(-3.01251654524499E-18,0.924224592736303,0.381849318686592));
#89228=DIRECTION('center_axis',(1.,0.,0.));
#89229=DIRECTION('ref_axis',(0.,-0.924224592736303,-0.381849318686593));
#89230=DIRECTION('',(-0.660627895620383,0.693827893847185,0.286659444721021));
#89231=DIRECTION('center_axis',(1.,0.,0.));
#89232=DIRECTION('ref_axis',(0.,0.924224592736303,0.381849318686593));
#89233=DIRECTION('center_axis',(1.,0.,0.));
#89234=DIRECTION('ref_axis',(0.,1.,0.));
#89235=DIRECTION('center_axis',(1.,0.,0.));
#89236=DIRECTION('ref_axis',(0.,1.,0.));
#89237=DIRECTION('center_axis',(1.,0.,0.));
#89238=DIRECTION('ref_axis',(0.,1.,0.));
#89239=DIRECTION('center_axis',(1.,0.,0.));
#89240=DIRECTION('ref_axis',(0.,0.924224592736303,0.381849318686593));
#89241=DIRECTION('center_axis',(1.,-4.17704712177877E-17,-1.72577381094218E-17));
#89242=DIRECTION('ref_axis',(4.51951522888177E-17,0.924224592736303,0.381849318686593));
#89243=DIRECTION('',(0.660627895620383,-0.693827893847184,-0.286659444721022));
#89244=DIRECTION('center_axis',(1.,0.,0.));
#89245=DIRECTION('ref_axis',(0.,0.924224592736303,0.381849318686592));
#89246=DIRECTION('center_axis',(1.,0.,0.));
#89247=DIRECTION('ref_axis',(0.,1.,0.));
#89248=DIRECTION('center_axis',(1.,0.,0.));
#89249=DIRECTION('ref_axis',(0.,1.,0.));
#89250=DIRECTION('axis',(0.,0.,1.));
#89251=DIRECTION('refdir',(1.,0.,0.));
#89252=DIRECTION('center_axis',(-1.,0.,0.));
#89253=DIRECTION('ref_axis',(0.,0.,1.));
#89254=DIRECTION('',(-1.,0.,0.));
#89255=DIRECTION('',(-0.999999999965599,-7.79366990386846E-6,-2.8389956576918E-6));
#89256=DIRECTION('center_axis',(-1.,0.,0.));
#89257=DIRECTION('ref_axis',(0.,0.,1.));
#89258=DIRECTION('',(-1.,0.,0.));
#89259=DIRECTION('center_axis',(-1.,0.,0.));
#89260=DIRECTION('ref_axis',(0.,0.,1.));
#89261=DIRECTION('',(-1.,0.,0.));
#89262=DIRECTION('center_axis',(1.,0.,0.));
#89263=DIRECTION('ref_axis',(0.,0.,-1.));
#89264=DIRECTION('',(1.,0.,0.));
#89265=DIRECTION('',(0.999999999992329,-8.06779552607498E-7,3.8330006150557E-6));
#89266=DIRECTION('',(1.,0.,0.));
#89267=DIRECTION('center_axis',(-1.,0.,0.));
#89268=DIRECTION('ref_axis',(0.,1.,0.));
#89269=DIRECTION('center_axis',(1.,0.,0.));
#89270=DIRECTION('ref_axis',(0.,0.,-1.));
#89271=DIRECTION('',(1.,0.,0.));
#89272=DIRECTION('center_axis',(1.,0.,0.));
#89273=DIRECTION('ref_axis',(0.,0.,-1.));
#89274=DIRECTION('',(1.,0.,0.));
#89275=DIRECTION('center_axis',(1.,0.,0.));
#89276=DIRECTION('ref_axis',(0.,0.,-1.));
#89277=DIRECTION('',(1.,0.,0.));
#89278=DIRECTION('center_axis',(1.,0.,0.));
#89279=DIRECTION('ref_axis',(0.,0.,-1.));
#89280=DIRECTION('',(1.,0.,0.));
#89281=DIRECTION('center_axis',(-1.,0.,0.));
#89282=DIRECTION('ref_axis',(0.,-0.957773424896036,-0.287524027801011));
#89283=DIRECTION('center_axis',(1.,0.,0.));
#89284=DIRECTION('ref_axis',(0.,0.,-1.));
#89285=DIRECTION('center_axis',(-1.,0.,0.));
#89286=DIRECTION('ref_axis',(0.,1.,0.));
#89287=DIRECTION('',(1.,0.,0.));
#89288=DIRECTION('center_axis',(1.,0.,0.));
#89289=DIRECTION('ref_axis',(0.,-1.,0.));
#89290=DIRECTION('center_axis',(1.,0.,0.));
#89291=DIRECTION('ref_axis',(0.,0.,-1.));
#89292=DIRECTION('center_axis',(-1.,0.,0.));
#89293=DIRECTION('ref_axis',(0.,-0.957773424896036,-0.287524027801011));
#89294=DIRECTION('center_axis',(-1.,0.,0.));
#89295=DIRECTION('ref_axis',(0.,0.,1.));
#89296=DIRECTION('center_axis',(-1.,0.,8.90699599727784E-17));
#89297=DIRECTION('ref_axis',(8.90699599727784E-17,0.,1.));
#89298=DIRECTION('',(-0.707106708341652,-8.65956145444752E-17,-0.707106854031435));
#89299=DIRECTION('center_axis',(1.,0.,0.));
#89300=DIRECTION('ref_axis',(0.,1.,0.));
#89301=DIRECTION('center_axis',(1.,0.,-6.83634867380023E-18));
#89302=DIRECTION('ref_axis',(-6.83634867380023E-18,0.,-1.));
#89303=DIRECTION('center_axis',(-1.,0.,0.));
#89304=DIRECTION('ref_axis',(0.,0.906250000000018,-0.422742164327108));
#89305=DIRECTION('center_axis',(-1.,0.,0.));
#89306=DIRECTION('ref_axis',(0.,0.087019546441882,-0.99620660434322));
#89307=DIRECTION('center_axis',(-1.,0.,0.));
#89308=DIRECTION('ref_axis',(0.,-0.819230453558104,-0.573464440016103));
#89309=DIRECTION('center_axis',(1.,0.,0.));
#89310=DIRECTION('ref_axis',(0.,-0.819230453558104,0.573464440016103));
#89311=DIRECTION('center_axis',(1.,0.,0.));
#89312=DIRECTION('ref_axis',(0.,0.087019546441882,0.99620660434322));
#89313=DIRECTION('',(-0.707106781821139,8.65956055458343E-17,-0.707106780551956));
#89314=DIRECTION('center_axis',(1.,0.,0.));
#89315=DIRECTION('ref_axis',(0.,-1.,0.));
#89316=DIRECTION('center_axis',(1.,0.,0.));
#89317=DIRECTION('ref_axis',(0.,0.087019546441882,0.99620660434322));
#89318=DIRECTION('center_axis',(1.,0.,0.));
#89319=DIRECTION('ref_axis',(0.,0.906250000000018,0.422742164327108));
#89320=DIRECTION('center_axis',(-1.,0.,-1.02545230107003E-16));
#89321=DIRECTION('ref_axis',(-1.02545230107003E-16,0.,1.));
#89322=DIRECTION('center_axis',(1.,0.,0.));
#89323=DIRECTION('ref_axis',(0.,0.906250000000018,0.422742164327108));
#89324=DIRECTION('center_axis',(1.,0.,0.));
#89325=DIRECTION('ref_axis',(0.,0.087019546441882,0.99620660434322));
#89326=DIRECTION('center_axis',(1.,0.,0.));
#89327=DIRECTION('ref_axis',(0.,-0.819230453558104,0.573464440016103));
#89328=DIRECTION('center_axis',(-1.,0.,0.));
#89329=DIRECTION('ref_axis',(0.,-0.819230453558104,-0.573464440016103));
#89330=DIRECTION('center_axis',(-1.,0.,0.));
#89331=DIRECTION('ref_axis',(0.,0.087019546441882,-0.99620660434322));
#89332=DIRECTION('',(0.707106781821139,8.65956055458343E-17,0.707106780551956));
#89333=DIRECTION('center_axis',(1.,0.,0.));
#89334=DIRECTION('ref_axis',(0.,1.,0.));
#89335=DIRECTION('center_axis',(-1.,0.,0.));
#89336=DIRECTION('ref_axis',(0.,0.087019546441882,-0.99620660434322));
#89337=DIRECTION('center_axis',(-1.,0.,0.));
#89338=DIRECTION('ref_axis',(0.,0.906250000000018,-0.422742164327108));
#89339=DIRECTION('center_axis',(1.,0.,0.));
#89340=DIRECTION('ref_axis',(0.,0.,-1.));
#89341=DIRECTION('',(1.,0.,0.));
#89342=DIRECTION('',(1.,0.,0.));
#89343=DIRECTION('center_axis',(0.,0.500000000000017,0.866025403784429));
#89344=DIRECTION('ref_axis',(1.,0.,0.));
#89345=DIRECTION('',(1.,0.,0.));
#89346=DIRECTION('',(1.,0.,0.));
#89347=DIRECTION('center_axis',(0.,-0.500000000000017,-0.866025403784429));
#89348=DIRECTION('ref_axis',(0.,-0.866025403784429,0.500000000000017));
#89349=DIRECTION('',(1.,0.,0.));
#89350=DIRECTION('center_axis',(0.,0.500000000000017,-0.866025403784429));
#89351=DIRECTION('ref_axis',(-1.,0.,0.));
#89352=DIRECTION('',(1.,0.,0.));
#89353=DIRECTION('center_axis',(1.,0.,0.));
#89354=DIRECTION('ref_axis',(0.,0.,-1.));
#89355=DIRECTION('',(1.,0.,0.));
#89356=DIRECTION('center_axis',(1.,0.,0.));
#89357=DIRECTION('ref_axis',(0.,0.,-1.));
#89358=DIRECTION('',(1.,0.,0.));
#89359=DIRECTION('center_axis',(0.,1.,0.));
#89360=DIRECTION('ref_axis',(1.,0.,0.));
#89361=DIRECTION('',(1.,0.,0.));
#89362=DIRECTION('center_axis',(0.,-0.500000000000017,0.866025403784429));
#89363=DIRECTION('ref_axis',(-1.,0.,0.));
#89364=DIRECTION('',(1.,0.,0.));
#89365=DIRECTION('',(1.,0.,0.));
#89366=DIRECTION('center_axis',(1.,0.,0.));
#89367=DIRECTION('ref_axis',(0.,0.,-1.));
#89368=DIRECTION('center_axis',(1.,0.,0.));
#89369=DIRECTION('ref_axis',(0.,0.,-1.));
#89370=DIRECTION('',(1.,0.,0.));
#89371=DIRECTION('center_axis',(1.,0.,0.));
#89372=DIRECTION('ref_axis',(0.,-5.35449122399261E-13,1.));
#89373=DIRECTION('center_axis',(0.,-1.,0.));
#89374=DIRECTION('ref_axis',(0.,0.,-1.));
#89375=DIRECTION('center_axis',(-1.,0.,0.));
#89376=DIRECTION('ref_axis',(0.,0.,1.));
#89377=DIRECTION('',(-0.461790830635516,-0.303368053954436,0.833496882166249));
#89378=DIRECTION('',(-0.461753481727666,0.303366050430997,-0.833518303073349));
#89379=DIRECTION('center_axis',(1.,0.,0.));
#89380=DIRECTION('ref_axis',(0.,1.,0.));
#89381=DIRECTION('center_axis',(-1.,0.,0.));
#89382=DIRECTION('ref_axis',(0.,0.,1.));
#89383=DIRECTION('axis',(0.,0.,1.));
#89384=DIRECTION('refdir',(1.,0.,0.));
#89385=DIRECTION('center_axis',(0.173648177666905,0.,0.984807753012213));
#89386=DIRECTION('ref_axis',(0.984807753012213,0.,-0.173648177666905));
#89387=DIRECTION('center_axis',(-0.173648177666884,0.,-0.984807753012216));
#89388=DIRECTION('ref_axis',(0.984807753012216,0.,-0.173648177666884));
#89389=DIRECTION('',(0.173648177666905,0.,0.984807753012213));
#89390=DIRECTION('center_axis',(0.173648177666905,0.,0.984807753012213));
#89391=DIRECTION('ref_axis',(0.984807753012213,0.,-0.173648177666905));
#89392=DIRECTION('center_axis',(0.173648177666905,0.,0.984807753012213));
#89393=DIRECTION('ref_axis',(0.984807753012213,0.,-0.173648177666905));
#89394=DIRECTION('center_axis',(-0.173648177666902,0.,-0.984807753012213));
#89395=DIRECTION('ref_axis',(-0.984807753012213,0.,0.173648177666902));
#89396=DIRECTION('',(0.754709579450836,-1.04972719039646E-16,-0.656059029878518));
#89397=DIRECTION('center_axis',(0.173648177666884,0.,0.984807753012216));
#89398=DIRECTION('ref_axis',(0.984807753012216,0.,-0.173648177666884));
#89399=DIRECTION('center_axis',(0.173648177666902,6.42277782841E-16,0.984807753012213));
#89400=DIRECTION('ref_axis',(0.171010071662809,-0.984807753012213,-0.0301536896070356));
#89401=DIRECTION('',(-0.173648177666902,-6.42277782841E-16,-0.984807753012213));
#89402=DIRECTION('center_axis',(-0.173648177666902,-6.42277782841E-16,-0.984807753012213));
#89403=DIRECTION('ref_axis',(-0.171010071662809,0.984807753012213,0.0301536896070356));
#89404=DIRECTION('center_axis',(0.173648177666902,6.42277782841E-16,0.984807753012213));
#89405=DIRECTION('ref_axis',(0.171010071662809,-0.984807753012213,-0.0301536896070356));
#89406=DIRECTION('',(-0.173648177666902,-6.42277782841E-16,-0.984807753012213));
#89407=DIRECTION('center_axis',(0.173648177666902,6.42277782841E-16,0.984807753012213));
#89408=DIRECTION('ref_axis',(0.171010071662809,-0.984807753012213,-0.0301536896070356));
#89409=DIRECTION('',(-0.173648177666902,-6.42277782841E-16,-0.984807753012213));
#89410=DIRECTION('center_axis',(0.173648177666902,-1.13774921531834E-16,
0.984807753012213));
#89411=DIRECTION('ref_axis',(0.171010071662809,-0.984807753012213,-0.0301536896070363));
#89412=DIRECTION('',(-0.00186542286370051,-0.696364239695072,-0.717686119324768));
#89413=DIRECTION('center_axis',(-0.173648177666902,-6.42277782841E-16,-0.984807753012213));
#89414=DIRECTION('ref_axis',(-0.171010071662809,0.984807753012213,0.0301536896070356));
#89415=DIRECTION('center_axis',(-0.173648177666902,2.83723661848651E-16,
-0.984807753012213));
#89416=DIRECTION('ref_axis',(-0.171010071662807,0.984807753012213,0.0301536896070362));
#89417=DIRECTION('',(0.173648177666902,-2.83723661848651E-16,0.984807753012213));
#89418=DIRECTION('center_axis',(-0.173648177666902,2.83723661848651E-16,
-0.984807753012213));
#89419=DIRECTION('ref_axis',(0.171010071662807,-0.984807753012213,-0.0301536896070362));
#89420=DIRECTION('center_axis',(-0.173648177666902,2.83723661848651E-16,
-0.984807753012213));
#89421=DIRECTION('ref_axis',(-0.171010071662807,0.984807753012213,0.0301536896070362));
#89422=DIRECTION('',(0.173648177666902,-2.83723661848651E-16,0.984807753012213));
#89423=DIRECTION('center_axis',(-0.173648177666902,-8.51926239304202E-16,
-0.984807753012213));
#89424=DIRECTION('ref_axis',(-0.171010071662808,0.984807753012213,0.0301536896070352));
#89425=DIRECTION('center_axis',(0.173648177666902,8.51926239304202E-16,
0.984807753012213));
#89426=DIRECTION('ref_axis',(0.171010071662808,-0.984807753012213,-0.0301536896070352));
#89427=DIRECTION('',(0.173648177666902,8.51926239304202E-16,0.984807753012213));
#89428=DIRECTION('center_axis',(-0.173648177666902,-8.51926239304202E-16,
-0.984807753012213));
#89429=DIRECTION('ref_axis',(0.171010071662808,-0.984807753012213,-0.0301536896070352));
#89430=DIRECTION('',(-0.173648177666902,0.,-0.984807753012213));
#89431=DIRECTION('center_axis',(0.173648177666902,8.51926239304202E-16,
0.984807753012213));
#89432=DIRECTION('ref_axis',(-0.171010071662808,0.984807753012213,0.0301536896070352));
#89433=DIRECTION('',(0.173648177666902,0.,0.984807753012213));
#89434=DIRECTION('center_axis',(-0.173648177666902,-8.51926239304202E-16,
-0.984807753012213));
#89435=DIRECTION('ref_axis',(0.171010071662808,-0.984807753012213,-0.0301536896070352));
#89436=DIRECTION('',(-0.173648177666902,0.,-0.984807753012213));
#89437=DIRECTION('center_axis',(0.173648177666902,8.51926239304202E-16,
0.984807753012213));
#89438=DIRECTION('ref_axis',(-0.171010071662808,0.984807753012213,0.0301536896070352));
#89439=DIRECTION('',(0.173648177666902,0.,0.984807753012213));
#89440=DIRECTION('center_axis',(-0.173648177666902,-8.51926239304202E-16,
-0.984807753012213));
#89441=DIRECTION('ref_axis',(0.171010071662808,-0.984807753012213,-0.0301536896070352));
#89442=DIRECTION('center_axis',(-0.173648177666902,2.26576127474522E-17,
-0.984807753012213));
#89443=DIRECTION('ref_axis',(-0.171010071662808,0.984807753012213,0.0301536896070361));
#89444=DIRECTION('center_axis',(0.173648177666902,-7.67302066723185E-16,
0.984807753012213));
#89445=DIRECTION('ref_axis',(0.171010071662807,-0.984807753012213,-0.0301536896070368));
#89446=DIRECTION('center_axis',(-0.173648177666902,4.06830024443141E-16,
-0.984807753012213));
#89447=DIRECTION('ref_axis',(-0.171010071662808,0.984807753012213,0.0301536896070366));
#89448=DIRECTION('center_axis',(-0.173648177666902,4.06830024443141E-16,
-0.984807753012213));
#89449=DIRECTION('ref_axis',(-0.171010071662808,0.984807753012213,0.0301536896070366));
#89450=DIRECTION('',(0.173648177666902,-4.06830024443141E-16,0.984807753012213));
#89451=DIRECTION('center_axis',(-0.173648177666902,4.06830024443141E-16,
-0.984807753012213));
#89452=DIRECTION('ref_axis',(-0.171010071662808,0.984807753012213,0.0301536896070366));
#89453=DIRECTION('center_axis',(-0.173648177666902,2.83723661848651E-16,
-0.984807753012213));
#89454=DIRECTION('ref_axis',(-0.171010071662807,0.984807753012213,0.0301536896070362));
#89455=DIRECTION('center_axis',(0.173648177666902,-2.83723661848651E-16,
0.984807753012213));
#89456=DIRECTION('ref_axis',(-0.171010071662807,0.984807753012213,0.0301536896070362));
#89457=DIRECTION('center_axis',(-0.173648177666902,1.8503717077086E-17,
-0.984807753012213));
#89458=DIRECTION('ref_axis',(-0.171010071662807,0.984807753012213,0.0301536896070359));
#89459=DIRECTION('center_axis',(0.173648177666902,6.42277782841E-16,0.984807753012213));
#89460=DIRECTION('ref_axis',(-0.171010071662809,0.984807753012213,0.0301536896070356));
#89461=DIRECTION('center_axis',(-0.605579649361399,-0.190525192352794,-0.772640562848117));
#89462=DIRECTION('ref_axis',(0.381374075544339,-0.921640193904515,-0.0716461267784125));
#89463=DIRECTION('',(-0.0612749772472734,0.852868531363239,0.518517738726129));
#89464=DIRECTION('center_axis',(0.173648177666902,-1.04370139711662E-15,
0.984807753012213));
#89465=DIRECTION('ref_axis',(0.171010071662806,-0.984807753012213,-0.0301536896070368));
#89466=DIRECTION('center_axis',(-0.173648177666902,1.04370139711662E-15,
-0.984807753012213));
#89467=DIRECTION('ref_axis',(-0.171010071662806,0.984807753012213,0.0301536896070368));
#89468=DIRECTION('',(0.173648177666902,-1.04370139711662E-15,0.984807753012213));
#89469=DIRECTION('center_axis',(0.173648177666902,-1.04370139711662E-15,
0.984807753012213));
#89470=DIRECTION('ref_axis',(0.171010071662806,-0.984807753012213,-0.0301536896070368));
#89471=DIRECTION('center_axis',(-0.173648177666902,1.04370139711662E-15,
-0.984807753012213));
#89472=DIRECTION('ref_axis',(-0.171010071662806,0.984807753012213,0.0301536896070368));
#89473=DIRECTION('center_axis',(0.173648177666902,1.22504424478055E-15,
0.984807753012213));
#89474=DIRECTION('ref_axis',(-0.984807753012213,6.95411525205428E-14,0.173648177666902));
#89475=DIRECTION('center_axis',(-0.173648177666902,-1.22504424478055E-15,
-0.984807753012213));
#89476=DIRECTION('ref_axis',(0.171010071662809,-0.984807753012213,-0.0301536896070351));
#89477=DIRECTION('center_axis',(-0.173648177666902,-1.22504424478055E-15,
-0.984807753012213));
#89478=DIRECTION('ref_axis',(0.171010071662809,-0.984807753012213,-0.0301536896070351));
#89479=DIRECTION('',(-0.173648177666902,-1.22504424478055E-15,-0.984807753012213));
#89480=DIRECTION('center_axis',(0.173648177666902,1.22504424478055E-15,
0.984807753012213));
#89481=DIRECTION('ref_axis',(0.171010071662809,-0.984807753012213,-0.0301536896070351));
#89482=DIRECTION('center_axis',(0.173648177666902,1.22504424478055E-15,
0.984807753012213));
#89483=DIRECTION('ref_axis',(0.171010071662809,-0.984807753012213,-0.0301536896070351));
#89484=DIRECTION('',(0.173648177666902,1.22504424478055E-15,0.984807753012213));
#89485=DIRECTION('center_axis',(0.173648177666902,-1.7073787383701E-17,
0.984807753012213));
#89486=DIRECTION('ref_axis',(0.171010071662809,-0.984807753012213,-0.0301536896070363));
#89487=DIRECTION('',(0.00186542286370016,0.696364239695072,0.717686119324768));
#89488=DIRECTION('center_axis',(-0.173648177666902,5.60929665760627E-16,
-0.984807753012213));
#89489=DIRECTION('ref_axis',(0.171010071662806,-0.984807753012213,-0.0301536896070362));
#89490=DIRECTION('center_axis',(-0.173648177666902,1.79020106093818E-17,
-0.984807753012213));
#89491=DIRECTION('ref_axis',(-0.17101007166281,0.984807753012213,0.0301536896070365));
#89492=DIRECTION('',(-0.00186542286369971,-0.696364239695071,-0.717686119324768));
#89493=DIRECTION('center_axis',(0.173648177666902,-5.60929665760627E-16,
0.984807753012213));
#89494=DIRECTION('ref_axis',(0.171010071662806,-0.984807753012213,-0.0301536896070362));
#89495=DIRECTION('center_axis',(0.173648177666902,-1.13774921531834E-16,
0.984807753012213));
#89496=DIRECTION('ref_axis',(0.171010071662809,-0.984807753012213,-0.0301536896070363));
#89497=DIRECTION('center_axis',(-0.173648177666902,-6.42277782841E-16,-0.984807753012213));
#89498=DIRECTION('ref_axis',(-0.171010071662809,0.984807753012213,0.0301536896070356));
#89499=DIRECTION('center_axis',(-0.173648177666902,-8.32320468273753E-17,
-0.984807753012213));
#89500=DIRECTION('ref_axis',(-0.171010071662807,0.984807753012213,0.0301536896070358));
#89501=DIRECTION('',(-0.00186542286370196,-0.696364239695072,-0.717686119324767));
#89502=DIRECTION('center_axis',(0.173648177666903,-1.55366487411101E-15,
0.984807753012213));
#89503=DIRECTION('ref_axis',(-0.171010071662807,0.984807753012213,0.0301536896070375));
#89504=DIRECTION('center_axis',(0.173648177666902,6.42277782841E-16,0.984807753012213));
#89505=DIRECTION('ref_axis',(0.171010071662809,-0.984807753012213,-0.0301536896070356));
#89506=DIRECTION('center_axis',(0.173648177666884,0.,0.984807753012216));
#89507=DIRECTION('ref_axis',(0.984807753012216,0.,-0.173648177666884));
#89508=DIRECTION('center_axis',(0.173648177666884,0.,0.984807753012216));
#89509=DIRECTION('ref_axis',(0.984807753012216,0.,-0.173648177666884));
#89510=DIRECTION('',(-0.173648177666884,0.,-0.984807753012216));
#89511=DIRECTION('center_axis',(0.173648177666884,0.,0.984807753012216));
#89512=DIRECTION('ref_axis',(0.984807753012216,0.,-0.173648177666884));
#89513=DIRECTION('center_axis',(0.173648177666884,0.,0.984807753012216));
#89514=DIRECTION('ref_axis',(0.984807753012216,0.,-0.173648177666883));
#89515=DIRECTION('center_axis',(1.20604166250191E-16,-1.,-2.1265768495752E-17));
#89516=DIRECTION('ref_axis',(-0.984807753012216,-1.22464679914735E-16,0.173648177666884));
#89517=DIRECTION('center_axis',(0.173648177666884,0.,0.984807753012216));
#89518=DIRECTION('ref_axis',(0.984807753012216,0.,-0.173648177666884));
#89519=DIRECTION('center_axis',(0.173648177666884,0.,0.984807753012216));
#89520=DIRECTION('ref_axis',(0.984807753012216,0.,-0.173648177666884));
#89521=DIRECTION('',(-0.173648177666884,0.,-0.984807753012216));
#89522=DIRECTION('center_axis',(0.173648177666884,0.,0.984807753012216));
#89523=DIRECTION('ref_axis',(0.984807753012216,0.,-0.173648177666884));
#89524=DIRECTION('center_axis',(0.173648177666903,0.,0.984807753012213));
#89525=DIRECTION('ref_axis',(0.984807753012213,0.,-0.173648177666903));
#89526=DIRECTION('center_axis',(-0.173648177666903,0.,-0.984807753012213));
#89527=DIRECTION('ref_axis',(-0.984807753012213,0.,0.173648177666903));
#89528=DIRECTION('',(-0.173648177666903,0.,-0.984807753012213));
#89529=DIRECTION('center_axis',(0.173648177666903,0.,0.984807753012213));
#89530=DIRECTION('ref_axis',(0.984807753012213,0.,-0.173648177666903));
#89531=DIRECTION('center_axis',(-0.173648177666903,0.,-0.984807753012213));
#89532=DIRECTION('ref_axis',(-0.984807753012213,0.,0.173648177666903));
#89533=DIRECTION('center_axis',(0.173648177666902,0.,0.984807753012213));
#89534=DIRECTION('ref_axis',(0.984807753012213,0.,-0.173648177666902));
#89535=DIRECTION('center_axis',(-0.173648177666902,0.,-0.984807753012213));
#89536=DIRECTION('ref_axis',(0.984807753012213,0.,-0.173648177666902));
#89537=DIRECTION('',(-0.173648177666902,0.,-0.984807753012213));
#89538=DIRECTION('center_axis',(0.173648177666902,0.,0.984807753012213));
#89539=DIRECTION('ref_axis',(-0.984807753012213,0.,0.173648177666902));
#89540=DIRECTION('center_axis',(0.173648177666902,0.,0.984807753012213));
#89541=DIRECTION('ref_axis',(-0.984807753012213,0.,0.173648177666902));
#89542=DIRECTION('center_axis',(0.173648177666902,0.,0.984807753012213));
#89543=DIRECTION('ref_axis',(0.984807753012213,0.,-0.173648177666902));
#89544=DIRECTION('center_axis',(0.173648177666902,0.,0.984807753012213));
#89545=DIRECTION('ref_axis',(0.984807753012213,0.,-0.173648177666902));
#89546=DIRECTION('center_axis',(1.2060416625019E-16,-1.,-2.12657684957542E-17));
#89547=DIRECTION('ref_axis',(-0.984807753012213,-1.22464679914735E-16,0.173648177666902));
#89548=DIRECTION('center_axis',(-0.173648177666902,0.,-0.984807753012213));
#89549=DIRECTION('ref_axis',(-0.984807753012213,0.,0.173648177666902));
#89550=DIRECTION('center_axis',(-0.173648177666902,0.,-0.984807753012213));
#89551=DIRECTION('ref_axis',(-0.984807753012213,0.,0.173648177666902));
#89552=DIRECTION('center_axis',(-1.2060416625019E-16,-1.,2.12657684957543E-17));
#89553=DIRECTION('ref_axis',(0.984807753012213,-1.22464679914735E-16,-0.173648177666902));
#89554=DIRECTION('center_axis',(-0.173648177666902,0.,-0.984807753012213));
#89555=DIRECTION('ref_axis',(-0.984807753012213,0.,0.173648177666902));
#89556=DIRECTION('center_axis',(1.2060416625019E-16,1.,-2.12657684957543E-17));
#89557=DIRECTION('ref_axis',(0.984807753012213,-1.22464679914735E-16,-0.173648177666902));
#89558=DIRECTION('center_axis',(0.173648177666902,0.,0.984807753012213));
#89559=DIRECTION('ref_axis',(0.984807753012213,0.,-0.173648177666902));
#89560=DIRECTION('center_axis',(0.173648177666902,0.,0.984807753012213));
#89561=DIRECTION('ref_axis',(0.984807753012213,0.,-0.173648177666902));
#89562=DIRECTION('',(0.173648177666902,0.,0.984807753012213));
#89563=DIRECTION('center_axis',(0.173648177666902,0.,0.984807753012213));
#89564=DIRECTION('ref_axis',(0.984807753012213,0.,-0.173648177666902));
#89565=DIRECTION('center_axis',(0.173648177666902,0.,0.984807753012213));
#89566=DIRECTION('ref_axis',(0.984807753012213,0.,-0.173648177666902));
#89567=DIRECTION('center_axis',(-1.2060416625019E-16,1.,2.12657684957542E-17));
#89568=DIRECTION('ref_axis',(-0.984807753012213,-1.22464679914735E-16,0.173648177666903));
#89569=DIRECTION('center_axis',(-0.173648177666902,0.,-0.984807753012213));
#89570=DIRECTION('ref_axis',(0.984807753012213,0.,-0.173648177666902));
#89571=DIRECTION('center_axis',(-0.173648177666904,0.,-0.984807753012213));
#89572=DIRECTION('ref_axis',(-0.984807753012213,0.,0.173648177666904));
#89573=DIRECTION('center_axis',(-0.173648177666904,0.,-0.984807753012213));
#89574=DIRECTION('ref_axis',(-0.984807753012213,0.,0.173648177666904));
#89575=DIRECTION('',(0.173648177666904,0.,0.984807753012213));
#89576=DIRECTION('center_axis',(-0.173648177666904,0.,-0.984807753012213));
#89577=DIRECTION('ref_axis',(-0.984807753012213,0.,0.173648177666904));
#89578=DIRECTION('center_axis',(0.173648177666884,0.,0.984807753012216));
#89579=DIRECTION('ref_axis',(0.984807753012216,0.,-0.173648177666884));
#89580=DIRECTION('center_axis',(-0.173648177666902,0.,-0.984807753012213));
#89581=DIRECTION('ref_axis',(-0.984807753012213,0.,0.173648177666902));
#89582=DIRECTION('',(-0.173648177666884,0.,-0.984807753012216));
#89583=DIRECTION('center_axis',(0.173648177666884,0.,0.984807753012216));
#89584=DIRECTION('ref_axis',(0.984807753012216,0.,-0.173648177666884));
#89585=DIRECTION('center_axis',(-0.173648177666902,0.,-0.984807753012213));
#89586=DIRECTION('ref_axis',(-0.984807753012213,0.,0.173648177666902));
#89587=DIRECTION('center_axis',(0.173648177666902,0.,0.984807753012213));
#89588=DIRECTION('ref_axis',(0.,-1.,0.));
#89589=DIRECTION('center_axis',(0.173648177666902,0.,0.984807753012213));
#89590=DIRECTION('ref_axis',(0.,-1.,0.));
#89591=DIRECTION('center_axis',(-0.173648177666902,0.,-0.984807753012213));
#89592=DIRECTION('ref_axis',(-0.984807753012213,0.,0.173648177666902));
#89593=DIRECTION('center_axis',(-0.173648177666884,0.,-0.984807753012216));
#89594=DIRECTION('ref_axis',(-0.984807753012216,0.,0.173648177666884));
#89595=DIRECTION('center_axis',(0.173648177666884,0.,0.984807753012216));
#89596=DIRECTION('ref_axis',(0.984807753012216,0.,-0.173648177666884));
#89597=DIRECTION('center_axis',(-0.173648177666902,0.,-0.984807753012213));
#89598=DIRECTION('ref_axis',(-0.984807753012213,0.,0.173648177666902));
#89599=DIRECTION('',(0.171010071662808,-0.984807753012213,-0.0301536896070361));
#89600=DIRECTION('center_axis',(-0.969846310392964,-0.173648177666903,0.171010071662808));
#89601=DIRECTION('ref_axis',(-0.176244384228223,0.984346441568219,-1.7290608322831E-18));
#89602=DIRECTION('',(0.171010071662808,-0.984807753012213,-0.0301536896070361));
#89603=DIRECTION('center_axis',(-0.173648177666902,0.,-0.984807753012213));
#89604=DIRECTION('ref_axis',(-0.984807753012213,0.,0.173648177666902));
#89605=DIRECTION('',(-0.171010071662808,0.984807753012213,0.0301536896070361));
#89606=DIRECTION('center_axis',(0.969846310392964,0.173648177666903,-0.171010071662808));
#89607=DIRECTION('ref_axis',(2.6217127112405E-18,-0.701673843159865,-0.712498293208669));
#89608=DIRECTION('',(-0.171010071662808,0.984807753012213,0.0301536896070361));
#89609=DIRECTION('center_axis',(0.173648177666902,0.,0.984807753012213));
#89610=DIRECTION('ref_axis',(0.,-1.,0.));
#89611=DIRECTION('center_axis',(-0.173648177666902,0.,-0.984807753012213));
#89612=DIRECTION('ref_axis',(-0.984807753012213,0.,0.173648177666902));
#89613=DIRECTION('center_axis',(-0.173648177666902,0.,-0.984807753012213));
#89614=DIRECTION('ref_axis',(-0.984807753012213,0.,0.173648177666902));
#89615=DIRECTION('center_axis',(-0.173648177666902,2.26576127474522E-17,
-0.984807753012213));
#89616=DIRECTION('ref_axis',(0.17101007166281,-0.984807753012213,-0.0301536896070364));
#89617=DIRECTION('center_axis',(0.173648177666902,-7.67302066723185E-16,
0.984807753012213));
#89618=DIRECTION('ref_axis',(0.171010071662807,-0.984807753012213,-0.0301536896070368));
#89619=DIRECTION('center_axis',(0.173648177666902,0.,0.984807753012213));
#89620=DIRECTION('ref_axis',(0.,-1.,0.));
#89621=DIRECTION('axis',(0.,0.,1.));
#89622=DIRECTION('refdir',(1.,0.,0.));
#89623=DIRECTION('center_axis',(1.,0.,0.));
#89624=DIRECTION('ref_axis',(0.,0.924224592736303,0.381849318686593));
#89625=DIRECTION('center_axis',(1.,0.,0.));
#89626=DIRECTION('ref_axis',(0.,0.381849318686592,-0.924224592736303));
#89627=DIRECTION('center_axis',(0.,0.381849318686593,-0.924224592736303));
#89628=DIRECTION('ref_axis',(0.,-0.924224592736303,-0.381849318686593));
#89629=DIRECTION('center_axis',(1.,0.,0.));
#89630=DIRECTION('ref_axis',(0.,0.381849318686593,-0.924224592736303));
#89631=DIRECTION('center_axis',(1.,0.,0.));
#89632=DIRECTION('ref_axis',(0.,0.924224592736303,0.381849318686593));
#89633=DIRECTION('',(-1.,0.,0.));
#89634=DIRECTION('center_axis',(1.,0.,0.));
#89635=DIRECTION('ref_axis',(0.,0.381849318686593,-0.924224592736303));
#89636=DIRECTION('center_axis',(-1.,0.,0.));
#89637=DIRECTION('ref_axis',(0.,0.381849318686586,-0.924224592736306));
#89638=DIRECTION('center_axis',(-1.,0.,0.));
#89639=DIRECTION('ref_axis',(0.,-0.228299548172813,0.973590938897897));
#89640=DIRECTION('',(1.,0.,0.));
#89641=DIRECTION('center_axis',(-1.,0.,0.));
#89642=DIRECTION('ref_axis',(0.,-0.228299548172813,0.973590938897897));
#89643=DIRECTION('',(1.,0.,0.));
#89644=DIRECTION('center_axis',(-1.,0.,0.));
#89645=DIRECTION('ref_axis',(0.,-0.381849318686584,0.924224592736306));
#89646=DIRECTION('center_axis',(-1.,0.,0.));
#89647=DIRECTION('ref_axis',(0.,-0.890419977397047,-0.455139828901232));
#89648=DIRECTION('center_axis',(-1.,0.,0.));
#89649=DIRECTION('ref_axis',(0.,-0.890419977397047,-0.455139828901232));
#89650=DIRECTION('center_axis',(1.,0.,0.));
#89651=DIRECTION('ref_axis',(0.,0.924224592736303,0.381849318686593));
#89652=DIRECTION('center_axis',(1.,0.,0.));
#89653=DIRECTION('ref_axis',(0.,0.381849318686593,-0.924224592736303));
#89654=DIRECTION('center_axis',(0.,-0.381849318686593,0.924224592736303));
#89655=DIRECTION('ref_axis',(0.,-0.924224592736303,-0.381849318686593));
#89656=DIRECTION('center_axis',(1.,0.,0.));
#89657=DIRECTION('ref_axis',(0.,0.381849318686592,-0.924224592736303));
#89658=DIRECTION('center_axis',(1.,0.,0.));
#89659=DIRECTION('ref_axis',(0.,0.924224592736303,0.381849318686593));
#89660=DIRECTION('center_axis',(1.,0.,0.));
#89661=DIRECTION('ref_axis',(0.,0.381849318686593,-0.924224592736303));
#89662=DIRECTION('',(1.,0.,0.));
#89663=DIRECTION('center_axis',(1.,-4.17636281571063E-17,-1.72549108550083E-17));
#89664=DIRECTION('ref_axis',(4.51877481786748E-17,0.924224592736303,0.381849318686593));
#89665=DIRECTION('center_axis',(1.,0.,0.));
#89666=DIRECTION('ref_axis',(0.,-0.924224592736303,-0.381849318686593));
#89667=DIRECTION('',(-0.660627895620383,0.693827893847184,0.286659444721022));
#89668=DIRECTION('center_axis',(1.,0.,0.));
#89669=DIRECTION('ref_axis',(0.,0.924224592736303,0.381849318686593));
#89670=DIRECTION('center_axis',(1.,0.,0.));
#89671=DIRECTION('ref_axis',(0.,1.,0.));
#89672=DIRECTION('center_axis',(1.,0.,0.));
#89673=DIRECTION('ref_axis',(0.,1.,0.));
#89674=DIRECTION('center_axis',(1.,0.,0.));
#89675=DIRECTION('ref_axis',(0.,1.,0.));
#89676=DIRECTION('center_axis',(1.,0.,0.));
#89677=DIRECTION('ref_axis',(0.,0.924224592736303,0.381849318686593));
#89678=DIRECTION('center_axis',(1.,2.78469808118585E-18,1.15051587396146E-18));
#89679=DIRECTION('ref_axis',(-3.01301015258785E-18,0.924224592736303,0.381849318686593));
#89680=DIRECTION('',(0.660627895620383,-0.693827893847184,-0.286659444721022));
#89681=DIRECTION('center_axis',(1.,0.,0.));
#89682=DIRECTION('ref_axis',(0.,0.924224592736303,0.381849318686592));
#89683=DIRECTION('center_axis',(1.,0.,0.));
#89684=DIRECTION('ref_axis',(0.,1.,0.));
#89685=DIRECTION('center_axis',(1.,0.,0.));
#89686=DIRECTION('ref_axis',(0.,1.,0.));
#89687=DIRECTION('axis',(0.,0.,1.));
#89688=DIRECTION('refdir',(1.,0.,0.));
#89689=DIRECTION('center_axis',(0.190809912898503,0.,-0.981627005099017));
#89690=DIRECTION('ref_axis',(0.,1.,0.));
#89691=DIRECTION('',(-0.190809912898503,0.,0.981627005099017));
#89692=DIRECTION('center_axis',(0.190809912898504,-3.49368872714712E-16,
-0.981627005099017));
#89693=DIRECTION('ref_axis',(0.574140136795491,-0.811115328353722,0.11160209420118));
#89694=DIRECTION('center_axis',(0.190809912898503,0.,-0.981627005099017));
#89695=DIRECTION('ref_axis',(0.,1.,0.));
#89696=DIRECTION('',(-0.190809912898503,0.,0.981627005099017));
#89697=DIRECTION('center_axis',(0.190809912898504,-3.49368872714712E-16,
-0.981627005099017));
#89698=DIRECTION('ref_axis',(0.574140136795491,-0.811115328353722,0.11160209420118));
#89699=DIRECTION('center_axis',(0.190809912898503,0.,-0.981627005099017));
#89700=DIRECTION('ref_axis',(0.,1.,0.));
#89701=DIRECTION('',(-0.190809912898503,0.,0.981627005099017));
#89702=DIRECTION('center_axis',(0.190809912898503,0.,-0.981627005099017));
#89703=DIRECTION('ref_axis',(0.,1.,0.));
#89704=DIRECTION('',(-0.190809912898503,0.,0.981627005099017));
#89705=DIRECTION('center_axis',(0.190809912898504,-6.43574239211312E-16,
-0.981627005099017));
#89706=DIRECTION('ref_axis',(0.574140136791955,-0.811115328356319,0.111602094200493));
#89707=DIRECTION('center_axis',(-0.190809912898503,1.46277694072906E-15,
0.981627005099017));
#89708=DIRECTION('ref_axis',(5.57389751783728E-17,-1.,1.50099017455135E-15));
#89709=DIRECTION('center_axis',(0.190809912898503,0.,-0.981627005099017));
#89710=DIRECTION('ref_axis',(0.981627005099017,0.,0.190809912898503));
#89711=DIRECTION('',(-0.190693676655342,0.0348994966626399,0.981029024451551));
#89712=DIRECTION('center_axis',(-0.190809912898503,0.,0.981627005099017));
#89713=DIRECTION('ref_axis',(-0.981627005099017,0.,-0.190809912898503));
#89714=DIRECTION('center_axis',(0.190809912898503,0.,-0.981627005099017));
#89715=DIRECTION('ref_axis',(0.981627005099017,0.,0.190809912898503));
#89716=DIRECTION('center_axis',(0.190809912898503,0.,-0.981627005099017));
#89717=DIRECTION('ref_axis',(0.,1.,0.));
#89718=DIRECTION('center_axis',(0.981627005099017,0.,0.190809912898503));
#89719=DIRECTION('ref_axis',(0.,-1.,0.));
#89720=DIRECTION('center_axis',(-0.190809912898504,0.,0.981627005099017));
#89721=DIRECTION('ref_axis',(0.981627005099017,0.,0.190809912898504));
#89722=DIRECTION('center_axis',(0.190809912898503,0.,-0.981627005099017));
#89723=DIRECTION('ref_axis',(0.,1.,0.));
#89724=DIRECTION('center_axis',(-0.981627005099017,0.,-0.190809912898503));
#89725=DIRECTION('ref_axis',(0.,-1.,0.));
#89726=DIRECTION('center_axis',(-0.190809912898504,0.,0.981627005099017));
#89727=DIRECTION('ref_axis',(0.981627005099017,0.,0.190809912898504));
#89728=DIRECTION('center_axis',(0.,-1.,0.));
#89729=DIRECTION('ref_axis',(0.981627005099017,0.,0.190809912898502));
#89730=DIRECTION('',(0.,-1.,0.));
#89731=DIRECTION('',(0.,-1.,0.));
#89732=DIRECTION('center_axis',(0.,-1.,0.));
#89733=DIRECTION('ref_axis',(0.981627005099017,0.,0.190809912898502));
#89734=DIRECTION('',(0.,-1.,0.));
#89735=DIRECTION('',(0.,-1.,0.));
#89736=DIRECTION('center_axis',(0.190809912898503,0.,-0.981627005099017));
#89737=DIRECTION('ref_axis',(0.,1.,0.));
#89738=DIRECTION('',(0.190809912898503,0.,-0.981627005099017));
#89739=DIRECTION('center_axis',(0.190809912898503,-2.47317346244379E-16,
-0.981627005099017));
#89740=DIRECTION('ref_axis',(0.421966359657993,-0.902893528415321,0.0820223607482341));
#89741=DIRECTION('center_axis',(0.190809912898503,-2.47317346244379E-16,
-0.981627005099017));
#89742=DIRECTION('ref_axis',(0.421966359657993,-0.902893528415321,0.0820223607482341));
#89743=DIRECTION('',(0.190809912898503,0.,-0.981627005099017));
#89744=DIRECTION('center_axis',(-0.190809912898504,0.,0.981627005099017));
#89745=DIRECTION('ref_axis',(0.981627005099017,0.,0.190809912898504));
#89746=DIRECTION('center_axis',(0.190809912898503,-2.47317346244379E-16,
-0.981627005099017));
#89747=DIRECTION('ref_axis',(0.421966359657993,-0.902893528415321,0.0820223607482341));
#89748=DIRECTION('center_axis',(0.190809912898503,-2.47317346244379E-16,
-0.981627005099017));
#89749=DIRECTION('ref_axis',(0.421966359657993,-0.902893528415321,0.0820223607482341));
#89750=DIRECTION('center_axis',(0.190809912898504,2.18221187862687E-16,
-0.981627005099017));
#89751=DIRECTION('ref_axis',(-0.886304670221616,-0.42986425339371,-0.17228103551355));
#89752=DIRECTION('center_axis',(0.190809912898504,0.,-0.981627005099017));
#89753=DIRECTION('ref_axis',(-0.981627005099017,0.,-0.190809912898504));
#89754=DIRECTION('center_axis',(0.190809912898504,1.30932712717612E-16,
-0.981627005099017));
#89755=DIRECTION('ref_axis',(0.886304670221616,0.429864253393709,0.17228103551355));
#89756=DIRECTION('center_axis',(0.190809912898504,1.30932712717612E-16,
-0.981627005099017));
#89757=DIRECTION('ref_axis',(0.886304670221616,0.429864253393709,0.17228103551355));
#89758=DIRECTION('center_axis',(0.190809912898503,-2.47317346244379E-16,
-0.981627005099017));
#89759=DIRECTION('ref_axis',(-0.421966359657993,0.902893528415321,-0.0820223607482341));
#89760=DIRECTION('center_axis',(0.190809912898503,-2.47317346244379E-16,
-0.981627005099017));
#89761=DIRECTION('ref_axis',(-0.421966359657993,0.902893528415321,-0.0820223607482341));
#89762=DIRECTION('center_axis',(-0.981627005099017,0.,-0.190809912898503));
#89763=DIRECTION('ref_axis',(0.,-1.,0.));
#89764=DIRECTION('',(-0.981627005099017,0.,-0.190809912898503));
#89765=DIRECTION('',(-0.981627005099017,-1.072434343069E-14,-0.190809912898503));
#89766=DIRECTION('center_axis',(-0.981627005099017,0.,-0.190809912898503));
#89767=DIRECTION('ref_axis',(0.,-1.,0.));
#89768=DIRECTION('',(-0.981627005099017,0.,-0.190809912898503));
#89769=DIRECTION('',(-0.981627005099017,0.,-0.190809912898503));
#89770=DIRECTION('center_axis',(0.190809912898503,0.,-0.981627005099017));
#89771=DIRECTION('ref_axis',(0.,1.,0.));
#89772=DIRECTION('center_axis',(-0.190809912898503,0.,0.981627005099017));
#89773=DIRECTION('ref_axis',(0.981627005099017,0.,0.190809912898503));
#89774=DIRECTION('',(-0.190809912898503,0.,0.981627005099017));
#89775=DIRECTION('center_axis',(0.190809912898503,5.5156726174395E-17,-0.981627005099017));
#89776=DIRECTION('ref_axis',(0.410813063807969,-0.908215781839759,0.0798543688341771));
#89777=DIRECTION('center_axis',(0.190809912898503,5.5156726174395E-17,-0.981627005099017));
#89778=DIRECTION('ref_axis',(0.410813063807969,-0.908215781839759,0.0798543688341771));
#89779=DIRECTION('',(-0.190809912898503,0.,0.981627005099017));
#89780=DIRECTION('center_axis',(-0.190809912898503,0.,0.981627005099017));
#89781=DIRECTION('ref_axis',(0.981627005099017,0.,0.190809912898503));
#89782=DIRECTION('center_axis',(0.190809912898503,5.5156726174395E-17,-0.981627005099017));
#89783=DIRECTION('ref_axis',(0.410813063807969,-0.908215781839759,0.0798543688341771));
#89784=DIRECTION('center_axis',(0.190809912898503,5.5156726174395E-17,-0.981627005099017));
#89785=DIRECTION('ref_axis',(0.410813063807969,-0.908215781839759,0.0798543688341771));
#89786=DIRECTION('center_axis',(0.190809912898503,-9.65242708051913E-17,
-0.981627005099017));
#89787=DIRECTION('ref_axis',(0.891529137911025,0.418502202643181,0.17329657422589));
#89788=DIRECTION('center_axis',(0.190809912898503,-9.65242708051913E-17,
-0.981627005099017));
#89789=DIRECTION('ref_axis',(0.891529137911025,0.418502202643181,0.17329657422589));
#89790=DIRECTION('center_axis',(0.190809912898503,0.,-0.981627005099017));
#89791=DIRECTION('ref_axis',(-0.981627005099017,0.,-0.190809912898503));
#89792=DIRECTION('center_axis',(0.190809912898503,0.,-0.981627005099017));
#89793=DIRECTION('ref_axis',(-0.981627005099017,0.,-0.190809912898503));
#89794=DIRECTION('center_axis',(0.190809912898503,5.5156726174395E-17,-0.981627005099017));
#89795=DIRECTION('ref_axis',(-0.410813063807969,0.908215781839759,-0.0798543688341771));
#89796=DIRECTION('center_axis',(0.190809912898503,5.5156726174395E-17,-0.981627005099017));
#89797=DIRECTION('ref_axis',(-0.410813063807969,0.908215781839759,-0.0798543688341771));
#89798=DIRECTION('center_axis',(0.190809912898503,0.,-0.981627005099017));
#89799=DIRECTION('ref_axis',(0.,1.,0.));
#89800=DIRECTION('center_axis',(-0.190809912898503,0.,0.981627005099017));
#89801=DIRECTION('ref_axis',(0.981627005099017,0.,0.190809912898503));
#89802=DIRECTION('center_axis',(-0.981627005099017,0.,-0.190809912898503));
#89803=DIRECTION('ref_axis',(0.,-1.,0.));
#89804=DIRECTION('center_axis',(0.190809912898503,0.,-0.981627005099017));
#89805=DIRECTION('ref_axis',(0.,1.,0.));
#89806=DIRECTION('center_axis',(-0.190809912898503,0.,0.981627005099017));
#89807=DIRECTION('ref_axis',(0.981627005099017,0.,0.190809912898503));
#89808=DIRECTION('',(0.190809912898503,0.,-0.981627005099017));
#89809=DIRECTION('center_axis',(-0.190809912898503,0.,0.981627005099017));
#89810=DIRECTION('ref_axis',(0.981627005099017,0.,0.190809912898503));
#89811=DIRECTION('center_axis',(0.190809912898503,0.,-0.981627005099017));
#89812=DIRECTION('ref_axis',(0.,1.,0.));
#89813=DIRECTION('center_axis',(-0.190809912898504,0.,0.981627005099017));
#89814=DIRECTION('ref_axis',(0.981627005099017,0.,0.190809912898504));
#89815=DIRECTION('',(-0.190809912898503,0.,0.981627005099017));
#89816=DIRECTION('center_axis',(-0.190809912898504,0.,0.981627005099017));
#89817=DIRECTION('ref_axis',(0.981627005099017,0.,0.190809912898504));
#89818=DIRECTION('center_axis',(0.190809912898503,0.,-0.981627005099017));
#89819=DIRECTION('ref_axis',(0.,1.,0.));
#89820=DIRECTION('center_axis',(0.981627005099017,0.,0.190809912898503));
#89821=DIRECTION('ref_axis',(0.,-1.,0.));
#89822=DIRECTION('center_axis',(-0.190809912898503,0.,0.981627005099017));
#89823=DIRECTION('ref_axis',(0.981627005099017,0.,0.190809912898503));
#89824=DIRECTION('center_axis',(0.190809912898503,0.,-0.981627005099017));
#89825=DIRECTION('ref_axis',(0.,1.,0.));
#89826=DIRECTION('center_axis',(-0.981627005099017,0.,-0.190809912898503));
#89827=DIRECTION('ref_axis',(0.,-1.,0.));
#89828=DIRECTION('center_axis',(-0.190809912898503,0.,0.981627005099017));
#89829=DIRECTION('ref_axis',(0.981627005099017,0.,0.190809912898503));
#89830=DIRECTION('center_axis',(-0.190809912898503,0.,0.981627005099017));
#89831=DIRECTION('ref_axis',(0.981627005099017,0.,0.190809912898503));
#89832=DIRECTION('center_axis',(-0.190809912898503,1.16273051859071E-15,
0.981627005099017));
#89833=DIRECTION('ref_axis',(-4.2332613184886E-18,-1.,1.18367033947895E-15));
#89834=DIRECTION('center_axis',(0.190809912898503,0.,-0.981627005099017));
#89835=DIRECTION('ref_axis',(0.981627005099017,0.,0.190809912898503));
#89836=DIRECTION('',(0.190693676655342,-0.0348994966626396,-0.981029024451551));
#89837=DIRECTION('center_axis',(0.190809912898503,0.,-0.981627005099017));
#89838=DIRECTION('ref_axis',(0.,1.,0.));
#89839=DIRECTION('center_axis',(-0.190809912898503,0.,0.981627005099017));
#89840=DIRECTION('ref_axis',(0.,1.,0.));
#89841=DIRECTION('',(0.190809912898503,0.,-0.981627005099017));
#89842=DIRECTION('center_axis',(-0.190809912898503,0.,0.981627005099017));
#89843=DIRECTION('ref_axis',(0.981627005099017,0.,0.190809912898503));
#89844=DIRECTION('center_axis',(0.190809912898503,0.,-0.981627005099017));
#89845=DIRECTION('ref_axis',(0.,1.,0.));
#89846=DIRECTION('center_axis',(-0.190809912898503,0.,0.981627005099017));
#89847=DIRECTION('ref_axis',(0.981627005099017,0.,0.190809912898503));
#89848=DIRECTION('',(0.190809912898503,0.,-0.981627005099017));
#89849=DIRECTION('center_axis',(-0.190809912898503,0.,0.981627005099017));
#89850=DIRECTION('ref_axis',(0.,1.,0.));
#89851=DIRECTION('center_axis',(0.190809912898503,0.,-0.981627005099017));
#89852=DIRECTION('ref_axis',(0.,1.,0.));
#89853=DIRECTION('center_axis',(-0.190809912898503,0.,0.981627005099017));
#89854=DIRECTION('ref_axis',(0.981627005099017,0.,0.190809912898503));
#89855=DIRECTION('',(-0.190809912898503,0.,0.981627005099017));
#89856=DIRECTION('center_axis',(-0.190809912898503,0.,0.981627005099017));
#89857=DIRECTION('ref_axis',(0.981627005099017,0.,0.190809912898503));
#89858=DIRECTION('center_axis',(0.190809912898503,0.,-0.981627005099017));
#89859=DIRECTION('ref_axis',(0.,1.,0.));
#89860=DIRECTION('center_axis',(-0.190809912898503,0.,0.981627005099017));
#89861=DIRECTION('ref_axis',(0.981627005099017,0.,0.190809912898503));
#89862=DIRECTION('',(0.190809912898503,0.,-0.981627005099017));
#89863=DIRECTION('center_axis',(0.190809912898503,-2.65000753919799E-16,
-0.981627005099017));
#89864=DIRECTION('ref_axis',(-0.309763741346266,0.948905109489044,-0.0602122722769161));
#89865=DIRECTION('',(0.190809912898503,0.,-0.981627005099017));
#89866=DIRECTION('center_axis',(-0.190809912898503,2.65000753919799E-16,
0.981627005099017));
#89867=DIRECTION('ref_axis',(-0.309763741346266,0.948905109489044,-0.0602122722769161));
#89868=DIRECTION('',(-0.190809912898503,0.,0.981627005099017));
#89869=DIRECTION('center_axis',(0.190809912898503,-2.65000753919799E-16,
-0.981627005099017));
#89870=DIRECTION('ref_axis',(0.309763741346266,-0.948905109489044,0.0602122722769161));
#89871=DIRECTION('',(-0.190809912898503,0.,0.981627005099017));
#89872=DIRECTION('center_axis',(-0.190809912898503,0.,0.981627005099017));
#89873=DIRECTION('ref_axis',(0.981627005099017,0.,0.190809912898503));
#89874=DIRECTION('center_axis',(0.190809912898503,-2.65000753919799E-16,
-0.981627005099017));
#89875=DIRECTION('ref_axis',(0.309763741346266,-0.948905109489044,0.0602122722769161));
#89876=DIRECTION('',(-0.190809912898503,0.,0.981627005099017));
#89877=DIRECTION('center_axis',(0.190809912898503,2.42663671716433E-17,
-0.981627005099017));
#89878=DIRECTION('ref_axis',(0.549709825015208,0.828493500750504,0.106853298947315));
#89879=DIRECTION('center_axis',(-0.190809912898503,-1.38499642189817E-16,
0.981627005099017));
#89880=DIRECTION('ref_axis',(0.733440712215292,-0.664634735150065,0.142567143820477));
#89881=DIRECTION('center_axis',(0.190809912898503,0.,-0.981627005099017));
#89882=DIRECTION('ref_axis',(0.,1.,0.));
#89883=DIRECTION('center_axis',(-0.190809912898503,0.,0.981627005099017));
#89884=DIRECTION('ref_axis',(0.981627005099017,0.,0.190809912898503));
#89885=DIRECTION('',(0.190809912898503,0.,-0.981627005099017));
#89886=DIRECTION('center_axis',(-0.190809912898503,0.,0.981627005099017));
#89887=DIRECTION('ref_axis',(0.981627005099017,0.,0.190809912898503));
#89888=DIRECTION('',(0.0954145326459342,-0.865996387817356,-0.490862835471632));
#89889=DIRECTION('',(0.190809912899824,0.,-0.98162700509876));
#89890=DIRECTION('center_axis',(0.,-1.,0.));
#89891=DIRECTION('ref_axis',(0.,0.,-1.));
#89892=DIRECTION('',(-0.981627005099017,0.,-0.190809912898503));
#89893=DIRECTION('',(-0.981627005099017,0.,-0.190809912898503));
#89894=DIRECTION('center_axis',(-0.190809912898503,-2.68840323315103E-17,
0.981627005099017));
#89895=DIRECTION('ref_axis',(5.12973986753602E-18,-1.,-2.63900921425656E-17));
#89896=DIRECTION('center_axis',(0.190809912898503,2.80359349652818E-16,
-0.981627005099017));
#89897=DIRECTION('ref_axis',(-0.170230827332271,-0.984848484848479,-0.0330896859674664));
#89898=DIRECTION('center_axis',(-0.190809912898503,-2.68840323315103E-17,
0.981627005099017));
#89899=DIRECTION('ref_axis',(5.12973986753602E-18,-1.,-2.63900921425656E-17));
#89900=DIRECTION('center_axis',(0.190809912898503,2.80359349652818E-16,
-0.981627005099017));
#89901=DIRECTION('ref_axis',(0.170230827332271,0.984848484848479,0.0330896859674664));
#89902=DIRECTION('center_axis',(0.,1.,0.));
#89903=DIRECTION('ref_axis',(1.,0.,0.));
#89904=DIRECTION('',(0.981627005099017,0.,0.190809912898503));
#89905=DIRECTION('',(0.981627005099017,0.,0.190809912898503));
#89906=DIRECTION('center_axis',(0.190809912898503,0.,-0.981627005099017));
#89907=DIRECTION('ref_axis',(0.,-1.,0.));
#89908=DIRECTION('center_axis',(0.190809912898503,0.,-0.981627005099017));
#89909=DIRECTION('ref_axis',(0.,-1.,0.));
#89910=DIRECTION('center_axis',(0.190809912898503,0.,-0.981627005099017));
#89911=DIRECTION('ref_axis',(0.,-1.,0.));
#89912=DIRECTION('center_axis',(0.190809912898503,0.,-0.981627005099017));
#89913=DIRECTION('ref_axis',(0.,-1.,0.));
#89914=DIRECTION('center_axis',(0.190809912898504,-6.43574239211312E-16,
-0.981627005099017));
#89915=DIRECTION('ref_axis',(0.574140136791955,-0.811115328356319,0.111602094200493));
#89916=DIRECTION('',(0.0954057063114802,0.866023134057401,-0.49081736163323));
#89917=DIRECTION('center_axis',(0.190809912898503,0.,-0.981627005099017));
#89918=DIRECTION('ref_axis',(0.,1.,0.));
#89919=DIRECTION('center_axis',(0.190809912898503,0.,-0.981627005099017));
#89920=DIRECTION('ref_axis',(0.,-1.,0.));
#89921=DIRECTION('center_axis',(0.190809912898503,0.,-0.981627005099017));
#89922=DIRECTION('ref_axis',(0.,-1.,0.));
#89923=DIRECTION('center_axis',(0.190809912898503,0.,-0.981627005099017));
#89924=DIRECTION('ref_axis',(0.,-1.,0.));
#89925=DIRECTION('center_axis',(-0.981627005099017,0.,-0.190809912898503));
#89926=DIRECTION('ref_axis',(-0.190809912898503,0.,0.981627005099017));
#89927=DIRECTION('center_axis',(-0.981627005099017,4.22136220887777E-18,
-0.190809912898503));
#89928=DIRECTION('ref_axis',(-0.190787588212088,0.0152965859522907,0.981512155117001));
#89929=DIRECTION('',(-0.190809912898503,0.,0.981627005099017));
#89930=DIRECTION('',(0.,-1.,0.));
#89931=DIRECTION('',(-0.190809912898503,0.,0.981627005099017));
#89932=DIRECTION('center_axis',(0.,1.,0.));
#89933=DIRECTION('ref_axis',(1.,0.,0.));
#89934=DIRECTION('',(-0.981627005099017,0.,-0.190809912898503));
#89935=DIRECTION('center_axis',(0.,1.,0.));
#89936=DIRECTION('ref_axis',(-0.710663462661499,0.,0.703532119265331));
#89937=DIRECTION('',(-0.190809912898503,0.,0.981627005099017));
#89938=DIRECTION('center_axis',(0.,1.,0.));
#89939=DIRECTION('ref_axis',(-0.706868204155822,0.,0.707345277748797));
#89940=DIRECTION('center_axis',(0.981627005099017,0.,0.190809912898503));
#89941=DIRECTION('ref_axis',(0.,-1.,0.));
#89942=DIRECTION('center_axis',(0.981627005099017,1.36071346699076E-17,
0.190809912898504));
#89943=DIRECTION('ref_axis',(-0.190549299057218,0.0522474292087793,0.980286269805854));
#89944=DIRECTION('center_axis',(0.981627005099017,3.13226948961353E-17,
0.190809912898504));
#89945=DIRECTION('ref_axis',(-0.190534941381885,0.0536663262517514,0.980212406338158));
#89946=DIRECTION('',(-0.190809912898503,0.,0.981627005099017));
#89947=DIRECTION('center_axis',(0.,-1.,0.));
#89948=DIRECTION('ref_axis',(0.,0.,-1.));
#89949=DIRECTION('center_axis',(0.,-1.,0.));
#89950=DIRECTION('ref_axis',(-0.679202351867065,0.,0.733951064593715));
#89951=DIRECTION('center_axis',(0.,-1.,0.));
#89952=DIRECTION('ref_axis',(-0.688011363844931,0.,0.725699912650014));
#89953=DIRECTION('',(0.981627005099012,0.,0.190809912898527));
#89954=DIRECTION('center_axis',(-0.190809912898503,0.,0.981627005099017));
#89955=DIRECTION('ref_axis',(0.,1.,0.));
#89956=DIRECTION('center_axis',(0.190809912898503,7.28528651098404E-18,
-0.981627005099017));
#89957=DIRECTION('ref_axis',(-0.98136931371192,0.0229120103408305,-0.190759822517053));
#89958=DIRECTION('center_axis',(-0.981627005099017,0.,-0.190809912898503));
#89959=DIRECTION('ref_axis',(-0.190809912898503,0.,0.981627005099017));
#89960=DIRECTION('center_axis',(-0.981627005099017,3.63686590303316E-17,
-0.190809912898503));
#89961=DIRECTION('ref_axis',(-0.190004571672825,0.0917795157137274,0.977483904337447));
#89962=DIRECTION('',(-0.190809912898503,0.,0.981627005099017));
#89963=DIRECTION('',(0.,-1.,0.));
#89964=DIRECTION('',(-0.190809912898503,0.,0.981627005099017));
#89965=DIRECTION('center_axis',(0.,1.,0.));
#89966=DIRECTION('ref_axis',(1.,0.,0.));
#89967=DIRECTION('center_axis',(0.,1.,0.));
#89968=DIRECTION('ref_axis',(-0.705384737821605,0.,0.708824640971479));
#89969=DIRECTION('',(-0.190809912898503,0.,0.981627005099017));
#89970=DIRECTION('center_axis',(0.,1.,0.));
#89971=DIRECTION('ref_axis',(-0.709191690509886,0.,0.705015706287264));
#89972=DIRECTION('',(-0.981627005099017,0.,-0.190809912898503));
#89973=DIRECTION('center_axis',(0.981627005099017,0.,0.190809912898503));
#89974=DIRECTION('ref_axis',(0.,-1.,0.));
#89975=DIRECTION('center_axis',(0.981627005099017,-3.95843917670041E-17,
0.190809912898503));
#89976=DIRECTION('ref_axis',(-0.189267639880765,0.126886613792695,0.973692737846077));
#89977=DIRECTION('center_axis',(0.981627005099017,7.30862880909824E-17,
0.190809912898504));
#89978=DIRECTION('ref_axis',(-0.189182369469026,0.130332506611401,0.973254061796032));
#89979=DIRECTION('',(-0.190809912898503,0.,0.981627005099017));
#89980=DIRECTION('center_axis',(0.,-1.,0.));
#89981=DIRECTION('ref_axis',(0.,0.,-1.));
#89982=DIRECTION('center_axis',(0.,-1.,0.));
#89983=DIRECTION('ref_axis',(-0.680489170594158,0.,0.732758137930979));
#89984=DIRECTION('center_axis',(0.,-1.,0.));
#89985=DIRECTION('ref_axis',(-0.689369692174638,0.,0.724409709702351));
#89986=DIRECTION('',(0.981627005099017,0.,0.190809912898503));
#89987=DIRECTION('center_axis',(-0.190809912898503,0.,0.981627005099017));
#89988=DIRECTION('ref_axis',(0.,1.,0.));
#89989=DIRECTION('center_axis',(0.190809912898504,-6.41105212966596E-17,
-0.981627005099017));
#89990=DIRECTION('ref_axis',(-0.972307089527912,0.137472062045006,-0.18899829578823));
#89991=DIRECTION('center_axis',(0.981627005099017,0.,0.190809912898503));
#89992=DIRECTION('ref_axis',(0.,-1.,0.));
#89993=DIRECTION('',(-0.190809912898503,0.,0.981627005099017));
#89994=DIRECTION('center_axis',(0.981627005099017,6.26453897922707E-17,
0.190809912898504));
#89995=DIRECTION('ref_axis',(-0.186677203055246,0.206998686971002,0.960366162175527));
#89996=DIRECTION('',(-0.190809912898503,0.,0.981627005099017));
#89997=DIRECTION('center_axis',(0.981627005099017,-1.03909028388386E-16,
0.190809912898503));
#89998=DIRECTION('ref_axis',(-0.186895105393115,0.201525798376691,0.961487166928781));
#89999=DIRECTION('center_axis',(0.,1.,0.));
#90000=DIRECTION('ref_axis',(1.,0.,0.));
#90001=DIRECTION('',(-0.190809912898503,0.,0.981627005099017));
#90002=DIRECTION('',(-0.981627005099017,0.,-0.190809912898503));
#90003=DIRECTION('center_axis',(0.,1.,0.));
#90004=DIRECTION('ref_axis',(-0.713534436527226,0.,0.700620159494268));
#90005=DIRECTION('center_axis',(-0.981627005099017,0.,-0.190809912898503));
#90006=DIRECTION('ref_axis',(-0.190809912898503,0.,0.981627005099017));
#90007=DIRECTION('',(-0.190809912898503,0.,0.981627005099017));
#90008=DIRECTION('',(0.,-1.,0.));
#90009=DIRECTION('center_axis',(-0.981627005099017,-4.15641817489504E-17,
-0.190809912898504));
#90010=DIRECTION('ref_axis',(-0.188089389572928,0.168262445475198,0.967631195741843));
#90011=DIRECTION('center_axis',(0.,-1.,0.));
#90012=DIRECTION('ref_axis',(0.,0.,-1.));
#90013=DIRECTION('center_axis',(0.,-1.,0.));
#90014=DIRECTION('ref_axis',(-0.692715647339658,0.,0.721210809632522));
#90015=DIRECTION('',(0.981627005099017,0.,0.190809912898503));
#90016=DIRECTION('center_axis',(0.,-1.,0.));
#90017=DIRECTION('ref_axis',(-0.683657405158267,0.,0.729803091506377));
#90018=DIRECTION('center_axis',(-0.190809912898503,0.,0.981627005099017));
#90019=DIRECTION('ref_axis',(0.,1.,0.));
#90020=DIRECTION('center_axis',(0.190809912898503,5.24540628790851E-17,
-0.981627005099017));
#90021=DIRECTION('ref_axis',(-0.94993897729484,0.252032113749207,-0.184650353520213));
#90022=DIRECTION('center_axis',(0.,-1.,0.));
#90023=DIRECTION('ref_axis',(0.,0.,-1.));
#90024=DIRECTION('',(-0.190809912898503,0.,0.981627005099017));
#90025=DIRECTION('center_axis',(0.,-1.,0.));
#90026=DIRECTION('ref_axis',(-0.631733075007243,0.,0.775185991838019));
#90027=DIRECTION('',(-0.190809912898503,0.,0.981627005099017));
#90028=DIRECTION('center_axis',(0.,-1.,0.));
#90029=DIRECTION('ref_axis',(-0.623815939113541,0.,0.781571285365507));
#90030=DIRECTION('center_axis',(0.981627005099017,0.,0.190809912898503));
#90031=DIRECTION('ref_axis',(0.,-1.,0.));
#90032=DIRECTION('',(-0.190809912898503,0.,0.981627005099017));
#90033=DIRECTION('center_axis',(0.981627005099017,8.36846343838454E-18,
0.190809912898503));
#90034=DIRECTION('ref_axis',(-0.190558051740874,0.0513631640146422,0.980331298235003));
#90035=DIRECTION('center_axis',(0.981627005099017,-1.02429212253849E-17,
0.190809912898503));
#90036=DIRECTION('ref_axis',(-0.190570150509215,0.0501150985729195,0.980393540691656));
#90037=DIRECTION('center_axis',(0.,1.,0.));
#90038=DIRECTION('ref_axis',(1.,0.,0.));
#90039=DIRECTION('',(-0.190809912898503,0.,0.981627005099017));
#90040=DIRECTION('center_axis',(0.,1.,0.));
#90041=DIRECTION('ref_axis',(-0.660441325182145,0.,0.750877657139732));
#90042=DIRECTION('center_axis',(0.,1.,0.));
#90043=DIRECTION('ref_axis',(-0.652047602561264,0.,0.758178029221441));
#90044=DIRECTION('center_axis',(-0.981627005099017,0.,-0.190809912898503));
#90045=DIRECTION('ref_axis',(-0.190809912898503,0.,0.981627005099017));
#90046=DIRECTION('center_axis',(-0.981627005099017,-1.43307256972171E-17,
-0.190809912898504));
#90047=DIRECTION('ref_axis',(-0.19078849457757,0.0149828714853907,0.981516817939905));
#90048=DIRECTION('center_axis',(-0.981627005099017,3.55175265017129E-18,
-0.190809912898503));
#90049=DIRECTION('ref_axis',(-0.190789564261716,0.0146039592402605,0.98152232096032));
#90050=DIRECTION('center_axis',(0.,-1.,0.));
#90051=DIRECTION('ref_axis',(0.,0.,-1.));
#90052=DIRECTION('',(-0.190809912898503,0.,0.981627005099017));
#90053=DIRECTION('center_axis',(0.,-1.,0.));
#90054=DIRECTION('ref_axis',(-0.632954523642759,0.,0.774188976284323));
#90055=DIRECTION('',(-0.190809912898503,0.,0.981627005099017));
#90056=DIRECTION('center_axis',(0.,-1.,0.));
#90057=DIRECTION('ref_axis',(-0.624972028608451,0.,0.780647144013887));
#90058=DIRECTION('center_axis',(0.981627005099017,0.,0.190809912898503));
#90059=DIRECTION('ref_axis',(0.,-1.,0.));
#90060=DIRECTION('',(-0.190809912898503,0.,0.981627005099017));
#90061=DIRECTION('center_axis',(0.981627005099017,7.65116657223729E-17,
0.190809912898504));
#90062=DIRECTION('ref_axis',(-0.189319606485261,0.124739112606999,0.97396008151581));
#90063=DIRECTION('center_axis',(0.981627005099017,5.00765037685485E-17,
0.190809912898504));
#90064=DIRECTION('ref_axis',(-0.189391419979737,0.121708096534195,0.974329528073578));
#90065=DIRECTION('center_axis',(0.,1.,0.));
#90066=DIRECTION('ref_axis',(1.,0.,0.));
#90067=DIRECTION('',(-0.190809912898503,0.,0.981627005099017));
#90068=DIRECTION('center_axis',(0.,1.,0.));
#90069=DIRECTION('ref_axis',(-0.662667500259754,0.,0.7489137360868));
#90070=DIRECTION('center_axis',(0.,1.,0.));
#90071=DIRECTION('ref_axis',(-0.654155114939017,0.,0.756360420434016));
#90072=DIRECTION('center_axis',(-0.981627005099017,0.,-0.190809912898503));
#90073=DIRECTION('ref_axis',(-0.190809912898503,0.,0.981627005099017));
#90074=DIRECTION('center_axis',(-0.981627005099017,-1.74461008487861E-17,
-0.190809912898503));
#90075=DIRECTION('ref_axis',(-0.190037332549694,0.0898972289123082,0.977652443597051));
#90076=DIRECTION('center_axis',(-0.981627005099017,-7.57707232036542E-17,
-0.190809912898504));
#90077=DIRECTION('ref_axis',(-0.190075989568967,0.0876237554415419,0.977851315728367));
#90078=DIRECTION('center_axis',(0.,-1.,0.));
#90079=DIRECTION('ref_axis',(0.,0.,-1.));
#90080=DIRECTION('',(-0.190809912898503,0.,0.981627005099017));
#90081=DIRECTION('center_axis',(0.,-1.,0.));
#90082=DIRECTION('ref_axis',(-0.635964061167762,0.,0.771718674714437));
#90083=DIRECTION('',(-0.190809912898503,0.,0.981627005099017));
#90084=DIRECTION('center_axis',(0.,-1.,0.));
#90085=DIRECTION('ref_axis',(-0.627819040820256,0.,0.778359333459511));
#90086=DIRECTION('center_axis',(0.981627005099017,0.,0.190809912898503));
#90087=DIRECTION('ref_axis',(0.,-1.,0.));
#90088=DIRECTION('',(-0.190809912898503,0.,0.981627005099017));
#90089=DIRECTION('center_axis',(0.981627005099017,5.73837492917797E-17,
0.190809912898504));
#90090=DIRECTION('ref_axis',(-0.187027825861746,0.198115061199294,0.962169951141392));
#90091=DIRECTION('center_axis',(0.981627005099017,6.37337320690617E-17,
0.190809912898504));
#90092=DIRECTION('ref_axis',(-0.187211139464168,0.193301094495603,0.963113013164774));
#90093=DIRECTION('center_axis',(0.,1.,0.));
#90094=DIRECTION('ref_axis',(1.,0.,0.));
#90095=DIRECTION('',(-0.190809912898513,0.,0.981627005099015));
#90096=DIRECTION('center_axis',(0.,1.,0.));
#90097=DIRECTION('ref_axis',(-0.666833013553189,0.,0.74520717390238));
#90098=DIRECTION('center_axis',(0.,1.,0.));
#90099=DIRECTION('ref_axis',(-0.658095710086924,0.,0.752934284227506));
#90100=DIRECTION('center_axis',(-0.981627005099017,0.,-0.190809912898503));
#90101=DIRECTION('ref_axis',(-0.190809912898503,0.,0.981627005099017));
#90102=DIRECTION('center_axis',(-0.981627005099017,-9.96920048502059E-17,
-0.190809912898504));
#90103=DIRECTION('ref_axis',(-0.188200600434938,0.164811586339199,0.96820332317354));
#90104=DIRECTION('center_axis',(-0.981627005099017,-3.78853616018271E-17,
-0.190809912898503));
#90105=DIRECTION('ref_axis',(-0.188331766656967,0.160643551642793,0.968878111520461));
#90106=DIRECTION('center_axis',(0.981627005099017,0.,0.190809912898503));
#90107=DIRECTION('ref_axis',(0.,-1.,0.));
#90108=DIRECTION('',(-0.190809912898493,0.,0.981627005099019));
#90109=DIRECTION('center_axis',(0.981627005099017,-3.82558328611865E-17,
0.190809912898503));
#90110=DIRECTION('ref_axis',(-0.183643278732954,0.271491009791614,0.944758052507911));
#90111=DIRECTION('',(-0.190809912898503,0.,0.981627005099017));
#90112=DIRECTION('center_axis',(0.981627005099017,2.45830109409238E-16,
0.190809912898504));
#90113=DIRECTION('ref_axis',(-0.183993708038349,0.264894092456889,0.946560846001851));
#90114=DIRECTION('center_axis',(0.,1.,0.));
#90115=DIRECTION('ref_axis',(1.,0.,0.));
#90116=DIRECTION('',(-0.190809912898503,0.,0.981627005099017));
#90117=DIRECTION('center_axis',(0.,1.,0.));
#90118=DIRECTION('ref_axis',(-0.673095267236959,0.,0.739555786417229));
#90119=DIRECTION('center_axis',(0.,1.,0.));
#90120=DIRECTION('ref_axis',(-0.664012722407567,0.,0.747721274594278));
#90121=DIRECTION('center_axis',(-0.981627005099017,0.,-0.190809912898503));
#90122=DIRECTION('ref_axis',(-0.190809912898503,0.,0.981627005099017));
#90123=DIRECTION('',(-0.190809912898503,0.,0.981627005099017));
#90124=DIRECTION('center_axis',(-0.981627005099017,-1.99384009700412E-16,
-0.190809912898504));
#90125=DIRECTION('ref_axis',(-0.185246010449827,0.2397259437662,0.953003351252149));
#90126=DIRECTION('center_axis',(-0.981627005099017,-1.65748457007993E-16,
-0.190809912898504));
#90127=DIRECTION('ref_axis',(-0.185527829167789,0.233663347844097,0.954453175634392));
#90128=DIRECTION('center_axis',(0.,-1.,0.));
#90129=DIRECTION('ref_axis',(0.,0.,-1.));
#90130=DIRECTION('center_axis',(0.,-1.,0.));
#90131=DIRECTION('ref_axis',(-0.640873994377488,0.,0.767646092500081));
#90132=DIRECTION('center_axis',(0.,-1.,0.));
#90133=DIRECTION('ref_axis',(-0.632459259128942,0.,0.774593626065997));
#90134=DIRECTION('center_axis',(-0.981627005099017,0.,-0.190809912898503));
#90135=DIRECTION('ref_axis',(-0.190809912898503,0.,0.981627005099017));
#90136=DIRECTION('center_axis',(-0.981627005099017,-1.70484127208222E-16,
-0.190809912898504));
#90137=DIRECTION('ref_axis',(-0.181615101248095,0.306683144045398,0.9343240359517));
#90138=DIRECTION('',(-0.190809912898503,0.,0.981627005099017));
#90139=DIRECTION('',(0.,-1.,0.));
#90140=DIRECTION('',(-0.190809912898503,0.,0.981627005099017));
#90141=DIRECTION('center_axis',(0.,1.,0.));
#90142=DIRECTION('ref_axis',(1.,0.,0.));
#90143=DIRECTION('center_axis',(0.,1.,0.));
#90144=DIRECTION('ref_axis',(-0.655547712408208,0.,0.755153757029895));
#90145=DIRECTION('',(-0.190809912898503,0.,0.981627005099017));
#90146=DIRECTION('center_axis',(0.,1.,0.));
#90147=DIRECTION('ref_axis',(-0.672133847791218,0.,0.74042966624344));
#90148=DIRECTION('',(-0.981627005099017,0.,-0.190809912898503));
#90149=DIRECTION('center_axis',(0.981627005099017,0.,0.190809912898503));
#90150=DIRECTION('ref_axis',(0.,-1.,0.));
#90151=DIRECTION('center_axis',(0.981627005099017,-1.82096377340177E-17,
0.190809912898503));
#90152=DIRECTION('ref_axis',(-0.179683420316472,0.336487090418195,0.924386448648654));
#90153=DIRECTION('center_axis',(0.981627005099017,2.10407080736525E-16,
0.190809912898504));
#90154=DIRECTION('ref_axis',(-0.179104025447188,0.344866958383991,0.921405735321627));
#90155=DIRECTION('',(-0.190809912898503,0.,0.981627005099017));
#90156=DIRECTION('center_axis',(0.,-1.,0.));
#90157=DIRECTION('ref_axis',(0.,0.,-1.));
#90158=DIRECTION('center_axis',(0.,-1.,0.));
#90159=DIRECTION('ref_axis',(-0.63906727483693,0.,0.769150842314107));
#90160=DIRECTION('center_axis',(0.,-1.,0.));
#90161=DIRECTION('ref_axis',(-0.647876541765181,0.,0.761745355502999));
#90162=DIRECTION('',(0.981627005099017,-1.201910499755E-14,0.190809912898503));
#90163=DIRECTION('center_axis',(-0.190809912898503,0.,0.981627005099017));
#90164=DIRECTION('ref_axis',(0.,1.,0.));
#90165=DIRECTION('center_axis',(0.190809912898504,-2.79755002021787E-16,
-0.981627005099017));
#90166=DIRECTION('ref_axis',(-0.860530616782567,0.481152217157524,-0.167271042037209));
#90167=DIRECTION('center_axis',(0.,-1.,0.));
#90168=DIRECTION('ref_axis',(0.,0.,-1.));
#90169=DIRECTION('',(-0.190809912898503,0.,0.981627005099017));
#90170=DIRECTION('center_axis',(0.,-1.,0.));
#90171=DIRECTION('ref_axis',(-0.36010817800382,0.,0.932910553126488));
#90172=DIRECTION('',(-0.190809912898503,0.,0.981627005099017));
#90173=DIRECTION('center_axis',(0.,-1.,0.));
#90174=DIRECTION('ref_axis',(-0.355750051979793,0.,0.934581136400888));
#90175=DIRECTION('center_axis',(0.981627005099017,0.,0.190809912898503));
#90176=DIRECTION('ref_axis',(0.,-1.,0.));
#90177=DIRECTION('',(-0.190809912898503,0.,0.981627005099017));
#90178=DIRECTION('',(0.,1.,0.));
#90179=DIRECTION('center_axis',(0.981627005099017,1.36798056621695E-16,
0.190809912898504));
#90180=DIRECTION('ref_axis',(-0.159259150209648,0.550783426949693,0.819313212191805));
#90181=DIRECTION('center_axis',(0.981627005099017,5.99180671853892E-16,
0.190809912898504));
#90182=DIRECTION('ref_axis',(-0.158343211241182,0.557989617362613,0.814601138207746));
#90183=DIRECTION('center_axis',(0.,1.,0.));
#90184=DIRECTION('ref_axis',(1.,0.,0.));
#90185=DIRECTION('',(-0.190809912898481,-2.237399193409E-14,0.981627005099021));
#90186=DIRECTION('',(-0.981627005099017,0.,-0.190809912898503));
#90187=DIRECTION('center_axis',(0.,1.,0.));
#90188=DIRECTION('ref_axis',(-0.39557835715531,0.,0.918432231223571));
#90189=DIRECTION('center_axis',(-0.981627005099017,0.,-0.190809912898503));
#90190=DIRECTION('ref_axis',(-0.190809912898503,0.,0.981627005099017));
#90191=DIRECTION('center_axis',(-0.981627005099017,-1.9977671997632E-16,
-0.190809912898504));
#90192=DIRECTION('ref_axis',(-0.160683023926675,0.539305080265381,0.826638370886405));
#90193=DIRECTION('',(0.,-1.,0.));
#90194=DIRECTION('center_axis',(-0.981627005099017,-4.57841563969441E-16,
-0.190809912898504));
#90195=DIRECTION('ref_axis',(-0.161960951934984,0.528701459898722,0.833212707745912));
#90196=DIRECTION('center_axis',(-0.190809912898503,0.,0.981627005099017));
#90197=DIRECTION('ref_axis',(0.,1.,0.));
#90198=DIRECTION('center_axis',(0.190809912898503,-3.03067918856936E-16,
-0.981627005099017));
#90199=DIRECTION('ref_axis',(-0.314874673283405,0.94715774678758,-0.0612057417645015));
#90200=DIRECTION('center_axis',(0.,-1.,0.));
#90201=DIRECTION('ref_axis',(0.,0.,-1.));
#90202=DIRECTION('',(-0.190809912898503,0.,0.981627005099017));
#90203=DIRECTION('center_axis',(0.,-1.,0.));
#90204=DIRECTION('ref_axis',(-0.287232890231326,0.,0.957860776297557));
#90205=DIRECTION('',(-0.190809912898503,0.,0.981627005099017));
#90206=DIRECTION('center_axis',(0.,-1.,0.));
#90207=DIRECTION('ref_axis',(-0.284731188473297,0.,0.95860740155216));
#90208=DIRECTION('center_axis',(0.981627005099017,0.,0.190809912898503));
#90209=DIRECTION('ref_axis',(0.,-1.,0.));
#90210=DIRECTION('',(-0.190809912898503,0.,0.981627005099017));
#90211=DIRECTION('',(0.,1.,0.));
#90212=DIRECTION('center_axis',(0.981627005099017,-2.99384533280007E-17,
0.190809912898503));
#90213=DIRECTION('ref_axis',(-0.158046676310463,0.560293947206128,0.813075605851874));
#90214=DIRECTION('center_axis',(0.981627005099017,-3.45621705615262E-16,
0.190809912898503));
#90215=DIRECTION('ref_axis',(-0.158864696644741,0.553903401621509,0.817283934647009));
#90216=DIRECTION('center_axis',(0.,1.,0.));
#90217=DIRECTION('ref_axis',(1.,0.,0.));
#90218=DIRECTION('',(-0.190809912898503,0.,0.981627005099017));
#90219=DIRECTION('',(-0.981627005099017,0.,-0.190809912898503));
#90220=DIRECTION('center_axis',(0.,1.,0.));
#90221=DIRECTION('ref_axis',(-0.323465005201917,0.,0.946240133586461));
#90222=DIRECTION('center_axis',(-0.981627005099017,0.,-0.190809912898503));
#90223=DIRECTION('ref_axis',(-0.190809912898503,0.,0.981627005099017));
#90224=DIRECTION('center_axis',(-0.981627005099017,-1.35608682274755E-16,
-0.190809912898503));
#90225=DIRECTION('ref_axis',(-0.161324598799703,0.534018424990321,0.829938971005081));
#90226=DIRECTION('',(1.2372117882059E-14,-1.,2.40490809969879E-15));
#90227=DIRECTION('center_axis',(-0.981627005099017,-2.17379342169057E-16,
-0.190809912898504));
#90228=DIRECTION('ref_axis',(-0.162549414642268,0.52371770234561,0.836240070822543));
#90229=DIRECTION('center_axis',(-0.190809912898503,0.,0.981627005099017));
#90230=DIRECTION('ref_axis',(0.,1.,0.));
#90231=DIRECTION('center_axis',(0.190809912898503,-2.21472709933915E-16,
-0.981627005099017));
#90232=DIRECTION('ref_axis',(-0.202419432825034,0.978508161618217,-0.0393465482771771));
#90233=DIRECTION('center_axis',(0.,-1.,0.));
#90234=DIRECTION('ref_axis',(0.,0.,-1.));
#90235=DIRECTION('',(-0.190809912898503,0.,0.981627005099017));
#90236=DIRECTION('center_axis',(0.,-1.,0.));
#90237=DIRECTION('ref_axis',(-0.213228510768614,0.,0.977002355266045));
#90238=DIRECTION('',(-0.190809912898503,0.,0.981627005099017));
#90239=DIRECTION('center_axis',(0.,-1.,0.));
#90240=DIRECTION('ref_axis',(-0.212642527010119,0.,0.977130060793726));
#90241=DIRECTION('center_axis',(0.981627005099017,0.,0.190809912898503));
#90242=DIRECTION('ref_axis',(0.,-1.,0.));
#90243=DIRECTION('',(-0.190809912898503,0.,0.981627005099017));
#90244=DIRECTION('center_axis',(0.981627005099017,1.78427841472896E-16,
0.190809912898504));
#90245=DIRECTION('ref_axis',(-0.157717823102993,0.562833367160933,0.811383811205239));
#90246=DIRECTION('center_axis',(0.981627005099017,5.43708098996233E-16,
0.190809912898504));
#90247=DIRECTION('ref_axis',(-0.159091080364181,0.552115896314094,0.818448572108133));
#90248=DIRECTION('center_axis',(0.,1.,0.));
#90249=DIRECTION('ref_axis',(1.,0.,0.));
#90250=DIRECTION('',(-0.190809912898503,0.,0.981627005099017));
#90251=DIRECTION('',(-0.981627005099017,2.00746580949E-14,-0.190809912898503));
#90252=DIRECTION('center_axis',(0.,1.,0.));
#90253=DIRECTION('ref_axis',(-0.245163967178927,0.,0.969481629117896));
#90254=DIRECTION('center_axis',(0.,1.,0.));
#90255=DIRECTION('ref_axis',(-0.250213113485533,0.,0.968190785868093));
#90256=DIRECTION('center_axis',(-0.981627005099017,0.,-0.190809912898503));
#90257=DIRECTION('ref_axis',(-0.190809912898503,0.,0.981627005099017));
#90258=DIRECTION('center_axis',(-0.981627005099017,1.19226339786349E-16,
-0.190809912898503));
#90259=DIRECTION('ref_axis',(-0.161675195212823,0.531098237955401,0.831742624189457));
#90260=DIRECTION('',(0.,-1.,0.));
#90261=DIRECTION('center_axis',(-0.981627005099017,-2.00758200789695E-16,
-0.190809912898504));
#90262=DIRECTION('ref_axis',(-0.162871454312254,0.52096239795233,0.83789681303247));
#90263=DIRECTION('center_axis',(-0.190809912898503,0.,0.981627005099017));
#90264=DIRECTION('ref_axis',(0.,1.,0.));
#90265=DIRECTION('center_axis',(0.190809912898503,-2.68098543604213E-16,
-0.981627005099017));
#90266=DIRECTION('ref_axis',(-0.0899641923666874,0.995791462362609,-0.0174873547898578));
#90267=DIRECTION('center_axis',(0.,-1.,0.));
#90268=DIRECTION('ref_axis',(0.,0.,-1.));
#90269=DIRECTION('',(-0.190809912898503,0.,0.981627005099017));
#90270=DIRECTION('center_axis',(0.,-1.,0.));
#90271=DIRECTION('ref_axis',(-0.138110878477997,0.,0.99041677350802));
#90272=DIRECTION('',(-0.190809912898503,0.,0.981627005099017));
#90273=DIRECTION('center_axis',(0.,-1.,0.));
#90274=DIRECTION('ref_axis',(-0.139498295720707,0.,0.990222311145845));
#90275=DIRECTION('center_axis',(0.981627005099017,0.,0.190809912898503));
#90276=DIRECTION('ref_axis',(0.,-1.,0.));
#90277=DIRECTION('',(-0.190809912898503,0.,0.981627005099017));
#90278=DIRECTION('center_axis',(0.981627005099017,-1.04257444818754E-16,
0.190809912898503));
#90279=DIRECTION('ref_axis',(-0.15765649718869,0.563305078924996,0.811068318300929));
#90280=DIRECTION('center_axis',(0.981627005099017,2.86623894051664E-16,
0.190809912898504));
#90281=DIRECTION('ref_axis',(-0.159034788508833,0.552561149824621,0.818158977062798));
#90282=DIRECTION('center_axis',(0.,1.,0.));
#90283=DIRECTION('ref_axis',(1.,0.,0.));
#90284=DIRECTION('',(-0.190809912898503,0.,0.981627005099017));
#90285=DIRECTION('center_axis',(0.,1.,0.));
#90286=DIRECTION('ref_axis',(-0.175424908276315,0.,0.984492814375121));
#90287=DIRECTION('center_axis',(0.,1.,0.));
#90288=DIRECTION('ref_axis',(-0.17584854355869,0.,0.984417233559169));
#90289=DIRECTION('center_axis',(-0.981627005099017,0.,-0.190809912898503));
#90290=DIRECTION('ref_axis',(-0.190809912898503,0.,0.981627005099017));
#90291=DIRECTION('center_axis',(-0.981627005099017,-3.27049270256878E-16,
-0.190809912898504));
#90292=DIRECTION('ref_axis',(-0.161754912532506,0.5304311251837,0.832152732200018));
#90293=DIRECTION('center_axis',(-0.981627005099017,-2.14578408646104E-16,
-0.190809912898504));
#90294=DIRECTION('ref_axis',(-0.162944724580192,0.520332710947401,0.838273754002602));
#90295=DIRECTION('center_axis',(0.,-1.,0.));
#90296=DIRECTION('ref_axis',(0.,0.,-1.));
#90297=DIRECTION('',(-0.190809912898503,0.,0.981627005099017));
#90298=DIRECTION('center_axis',(0.,-1.,0.));
#90299=DIRECTION('ref_axis',(-0.0618760686472822,0.,0.998083840230247));
#90300=DIRECTION('',(-0.190809912898503,0.,0.981627005099017));
#90301=DIRECTION('center_axis',(0.,-1.,0.));
#90302=DIRECTION('ref_axis',(-0.0652949673712366,0.,0.997866006654195));
#90303=DIRECTION('center_axis',(0.981627005099017,0.,0.190809912898503));
#90304=DIRECTION('ref_axis',(0.,-1.,0.));
#90305=DIRECTION('',(-0.190809912898503,0.,0.981627005099017));
#90306=DIRECTION('',(0.,1.,0.));
#90307=DIRECTION('center_axis',(0.981627005099017,1.50452980269455E-16,
0.190809912898503));
#90308=DIRECTION('ref_axis',(-0.158447752147023,0.557173939626296,0.815138951860889));
#90309=DIRECTION('center_axis',(0.981627005099017,2.31540729222364E-16,
0.190809912898504));
#90310=DIRECTION('ref_axis',(-0.158692756981343,0.555255482759283,0.816399386175306));
#90311=DIRECTION('center_axis',(0.,1.,0.));
#90312=DIRECTION('ref_axis',(1.,0.,0.));
#90313=DIRECTION('',(-0.190809912898503,0.,0.981627005099017));
#90314=DIRECTION('',(-0.981627005099017,0.,-0.190809912898503));
#90315=DIRECTION('center_axis',(0.,1.,0.));
#90316=DIRECTION('ref_axis',(-0.100377124109986,0.,0.994949462513252));
#90317=DIRECTION('center_axis',(-0.981627005099017,0.,-0.190809912898503));
#90318=DIRECTION('ref_axis',(-0.190809912898503,0.,0.981627005099017));
#90319=DIRECTION('center_axis',(-0.981627005099017,1.04674326304966E-16,
-0.190809912898503));
#90320=DIRECTION('ref_axis',(-0.161568217374531,0.531991649679407,0.831192273668253));
#90321=DIRECTION('',(-1.21473334453955E-14,-1.,-2.36121421336731E-15));
#90322=DIRECTION('center_axis',(-0.981627005099017,5.75453027144371E-17,
-0.190809912898503));
#90323=DIRECTION('ref_axis',(-0.162773155018957,0.521805547768498,0.837391109531975));
#90324=DIRECTION('center_axis',(-0.190809912898503,0.,0.981627005099017));
#90325=DIRECTION('ref_axis',(0.,1.,0.));
#90326=DIRECTION('center_axis',(0.190809912898503,5.8865115008751E-16,-0.981627005099017));
#90327=DIRECTION('ref_axis',(0.134946288550026,0.990505644687143,0.0262310321847858));
#90328=DIRECTION('center_axis',(0.,-1.,0.));
#90329=DIRECTION('ref_axis',(0.,0.,-1.));
#90330=DIRECTION('',(-0.190809912898503,0.,0.981627005099017));
#90331=DIRECTION('center_axis',(0.,-1.,0.));
#90332=DIRECTION('ref_axis',(0.0154999611699387,0.,0.999879868386063));
#90333=DIRECTION('',(-0.190809912898503,0.,0.981627005099017));
#90334=DIRECTION('center_axis',(0.,-1.,0.));
#90335=DIRECTION('ref_axis',(0.00998904194942923,0.,0.999950108275874));
#90336=DIRECTION('center_axis',(0.981627005099017,0.,0.190809912898503));
#90337=DIRECTION('ref_axis',(0.,-1.,0.));
#90338=DIRECTION('',(-0.19080991289849,0.,0.98162700509902));
#90339=DIRECTION('',(0.,1.,0.));
#90340=DIRECTION('center_axis',(0.981627005099017,-4.59929004743199E-17,
0.190809912898503));
#90341=DIRECTION('ref_axis',(-0.159944922126264,0.545298088879797,0.822841185253913));
#90342=DIRECTION('center_axis',(0.981627005099017,3.8312017680401E-16,0.190809912898504));
#90343=DIRECTION('ref_axis',(-0.158046000911432,0.560299179896621,0.813072131242412));
#90344=DIRECTION('center_axis',(0.,1.,0.));
#90345=DIRECTION('ref_axis',(1.,0.,0.));
#90346=DIRECTION('',(-0.190809912898503,0.,0.981627005099017));
#90347=DIRECTION('',(-0.981627005099017,0.,-0.190809912898503));
#90348=DIRECTION('center_axis',(0.,1.,0.));
#90349=DIRECTION('ref_axis',(-0.0237851745823533,0.,0.999717092716778));
#90350=DIRECTION('center_axis',(-0.981627005099017,0.,-0.190809912898503));
#90351=DIRECTION('ref_axis',(-0.190809912898503,0.,0.981627005099017));
#90352=DIRECTION('center_axis',(-0.981627005099017,4.55117302256744E-17,
-0.190809912898503));
#90353=DIRECTION('ref_axis',(-0.1611045890806,0.535839585425286,0.828807124769345));
#90354=DIRECTION('',(0.,-1.,0.));
#90355=DIRECTION('center_axis',(-0.981627005099017,-2.33394570578009E-16,
-0.190809912898504));
#90356=DIRECTION('ref_axis',(-0.162347493712948,0.525435160950585,0.835201282878539));
#90357=DIRECTION('center_axis',(-0.190809912898503,0.,0.981627005099017));
#90358=DIRECTION('ref_axis',(0.,1.,0.));
#90359=DIRECTION('center_axis',(0.190809912898503,6.99387505054468E-17,
-0.981627005099017));
#90360=DIRECTION('ref_axis',(0.247401529008408,0.967718871180627,0.0480902256721118));
#90361=DIRECTION('center_axis',(-0.981627005099017,0.,-0.190809912898503));
#90362=DIRECTION('ref_axis',(-0.190809912898503,0.,0.981627005099017));
#90363=DIRECTION('',(-0.190809912898503,0.,0.981627005099017));
#90364=DIRECTION('center_axis',(-0.981627005099017,1.08576435036114E-16,
-0.190809912898503));
#90365=DIRECTION('ref_axis',(-0.188102688558877,0.167853620862203,0.967699612752));
#90366=DIRECTION('',(-0.190809912898503,0.,0.981627005099017));
#90367=DIRECTION('center_axis',(-0.981627005099017,-8.82536396353935E-17,
-0.190809912898504));
#90368=DIRECTION('ref_axis',(-0.188243617855828,0.163456664470504,0.968424627514566));
#90369=DIRECTION('center_axis',(0.,-1.,0.));
#90370=DIRECTION('ref_axis',(0.,0.,-1.));
#90371=DIRECTION('',(-0.190809912898503,0.,0.981627005099017));
#90372=DIRECTION('',(0.981627005099017,0.,0.190809912898503));
#90373=DIRECTION('center_axis',(0.,-1.,0.));
#90374=DIRECTION('ref_axis',(0.382749389888478,0.,0.923852209252107));
#90375=DIRECTION('center_axis',(0.,-1.,0.));
#90376=DIRECTION('ref_axis',(0.388822090405444,0.,0.921312857835351));
#90377=DIRECTION('center_axis',(0.981627005099017,0.,0.190809912898503));
#90378=DIRECTION('ref_axis',(0.,-1.,0.));
#90379=DIRECTION('',(-0.190809912898469,0.,0.981627005099024));
#90380=DIRECTION('',(0.,1.,0.));
#90381=DIRECTION('center_axis',(0.981627005099017,5.14287578091947E-17,
0.190809912898504));
#90382=DIRECTION('ref_axis',(-0.18673928257389,0.205454980260091,0.960685532018732));
#90383=DIRECTION('center_axis',(0.,1.,0.));
#90384=DIRECTION('ref_axis',(1.,0.,0.));
#90385=DIRECTION('center_axis',(0.,1.,0.));
#90386=DIRECTION('ref_axis',(0.36800660983366,0.,0.929823174113625));
#90387=DIRECTION('',(-0.981627005099017,0.,-0.190809912898503));
#90388=DIRECTION('center_axis',(0.,1.,0.));
#90389=DIRECTION('ref_axis',(0.356362726694326,0.,0.934347690649998));
#90390=DIRECTION('center_axis',(-0.190809912898503,0.,0.981627005099017));
#90391=DIRECTION('ref_axis',(0.,1.,0.));
#90392=DIRECTION('center_axis',(0.190809912898503,2.33129168351489E-17,
-0.981627005099017));
#90393=DIRECTION('ref_axis',(0.933488573509569,0.309312139601285,0.181452702989912));
#90394=DIRECTION('center_axis',(-0.981627005099017,0.,-0.190809912898503));
#90395=DIRECTION('ref_axis',(-0.190809912898503,0.,0.981627005099017));
#90396=DIRECTION('',(-0.190809912898503,0.,0.981627005099017));
#90397=DIRECTION('center_axis',(-0.981627005099017,-9.56506689603866E-17,
-0.190809912898504));
#90398=DIRECTION('ref_axis',(-0.19000848861158,0.0915565204702765,0.977504055139885));
#90399=DIRECTION('',(-0.190809912898503,0.,0.981627005099017));
#90400=DIRECTION('center_axis',(-0.981627005099017,-2.69663898885924E-17,
-0.190809912898504));
#90401=DIRECTION('ref_axis',(-0.190050008447378,0.0891581806202793,0.977717655111962));
#90402=DIRECTION('center_axis',(0.,-1.,0.));
#90403=DIRECTION('ref_axis',(0.,0.,-1.));
#90404=DIRECTION('',(-0.190809912898503,0.,0.981627005099017));
#90405=DIRECTION('',(0.981627005099017,0.,0.190809912898503));
#90406=DIRECTION('center_axis',(0.,-1.,0.));
#90407=DIRECTION('ref_axis',(0.392668203964276,0.,0.919680206156178));
#90408=DIRECTION('center_axis',(0.,-1.,0.));
#90409=DIRECTION('ref_axis',(0.384550963585417,0.,0.923103762534596));
#90410=DIRECTION('center_axis',(0.981627005099017,0.,0.190809912898503));
#90411=DIRECTION('ref_axis',(0.,-1.,0.));
#90412=DIRECTION('',(-0.190809912898503,0.,0.981627005099017));
#90413=DIRECTION('',(0.,1.,0.));
#90414=DIRECTION('center_axis',(0.981627005099017,4.11430062473557E-17,
0.190809912898504));
#90415=DIRECTION('ref_axis',(-0.189206656454335,0.129360543126695,0.97337900688033));
#90416=DIRECTION('center_axis',(0.,1.,0.));
#90417=DIRECTION('ref_axis',(1.,0.,0.));
#90418=DIRECTION('center_axis',(0.,1.,0.));
#90419=DIRECTION('ref_axis',(0.36244598286257,0.,0.932004779766062));
#90420=DIRECTION('',(-0.981627005099017,0.,-0.190809912898503));
#90421=DIRECTION('center_axis',(0.,1.,0.));
#90422=DIRECTION('ref_axis',(0.351135646025879,0.,0.936324600814263));
#90423=DIRECTION('center_axis',(-0.190809912898503,0.,0.981627005099017));
#90424=DIRECTION('ref_axis',(0.,1.,0.));
#90425=DIRECTION('center_axis',(0.190809912898504,1.57362188637255E-16,
-0.981627005099017));
#90426=DIRECTION('ref_axis',(0.962831300769634,0.194752087897094,0.187156379848449));
#90427=DIRECTION('center_axis',(0.,-1.,0.));
#90428=DIRECTION('ref_axis',(0.,0.,-1.));
#90429=DIRECTION('',(-0.190809912898503,0.,0.981627005099017));
#90430=DIRECTION('center_axis',(0.,-1.,0.));
#90431=DIRECTION('ref_axis',(0.394709160970064,0.,0.918806115699231));
#90432=DIRECTION('',(-0.190809912898493,0.,0.981627005099019));
#90433=DIRECTION('center_axis',(0.,-1.,0.));
#90434=DIRECTION('ref_axis',(0.382819211217212,0.,0.92382327937925));
#90435=DIRECTION('center_axis',(0.981627005099017,0.,0.190809912898503));
#90436=DIRECTION('ref_axis',(0.,-1.,0.));
#90437=DIRECTION('',(-0.190809912898503,0.,0.981627005099017));
#90438=DIRECTION('center_axis',(0.981627005099017,6.7972359589236E-18,0.190809912898503));
#90439=DIRECTION('ref_axis',(-0.190523485063913,0.0547720629017275,0.980153468985643));
#90440=DIRECTION('center_axis',(0.981627005099017,1.02857515618389E-17,
0.190809912898503));
#90441=DIRECTION('ref_axis',(-0.190539030231083,0.0532661059933524,0.980233441538751));
#90442=DIRECTION('center_axis',(0.,1.,0.));
#90443=DIRECTION('ref_axis',(1.,0.,0.));
#90444=DIRECTION('',(-0.190809912898503,0.,0.981627005099017));
#90445=DIRECTION('center_axis',(0.,1.,0.));
#90446=DIRECTION('ref_axis',(0.359481261317514,0.,0.933152304161314));
#90447=DIRECTION('center_axis',(0.,1.,0.));
#90448=DIRECTION('ref_axis',(0.34834621044521,0.,0.937365946505665));
#90449=DIRECTION('center_axis',(-0.981627005099017,0.,-0.190809912898503));
#90450=DIRECTION('ref_axis',(-0.190809912898503,0.,0.981627005099017));
#90451=DIRECTION('center_axis',(-0.981627005099017,-3.23144151893198E-18,
-0.190809912898503));
#90452=DIRECTION('ref_axis',(-0.190787696570484,0.0152594200783794,0.981512712569838));
#90453=DIRECTION('center_axis',(-0.981627005099017,2.45148998987204E-18,
-0.190809912898503));
#90454=DIRECTION('ref_axis',(-0.190788845310911,0.0148596967700502,0.981518622297525));
#90455=DIRECTION('center_axis',(0.,-1.,0.));
#90456=DIRECTION('ref_axis',(0.,0.,-1.));
#90457=DIRECTION('',(-0.190809912898503,0.,0.981627005099017));
#90458=DIRECTION('center_axis',(0.,-1.,0.));
#90459=DIRECTION('ref_axis',(-0.574285234822728,0.,0.81865528097277));
#90460=DIRECTION('',(-0.190809912898503,0.,0.981627005099017));
#90461=DIRECTION('center_axis',(0.,-1.,0.));
#90462=DIRECTION('ref_axis',(-0.567322385194415,0.,0.823495787030705));
#90463=DIRECTION('center_axis',(0.981627005099017,0.,0.190809912898503));
#90464=DIRECTION('ref_axis',(0.,-1.,0.));
#90465=DIRECTION('',(-0.190809912898503,0.,0.981627005099017));
#90466=DIRECTION('center_axis',(0.981627005099017,2.11646646347863E-17,
0.190809912898504));
#90467=DIRECTION('ref_axis',(-0.190575246060068,0.049580034247521,0.980419754897441));
#90468=DIRECTION('center_axis',(0.981627005099017,1.06393782711632E-17,
0.190809912898504));
#90469=DIRECTION('ref_axis',(-0.190585783831876,0.0484547159815876,0.980473966763184));
#90470=DIRECTION('center_axis',(0.,1.,0.));
#90471=DIRECTION('ref_axis',(1.,0.,0.));
#90472=DIRECTION('',(-0.190809912898503,0.,0.981627005099017));
#90473=DIRECTION('center_axis',(0.,1.,0.));
#90474=DIRECTION('ref_axis',(-0.603515359960136,0.,0.797351371913404));
#90475=DIRECTION('center_axis',(0.,1.,0.));
#90476=DIRECTION('ref_axis',(-0.59604858216218,0.,0.802948371754035));
#90477=DIRECTION('center_axis',(-0.981627005099017,0.,-0.190809912898503));
#90478=DIRECTION('ref_axis',(-0.190809912898503,0.,0.981627005099017));
#90479=DIRECTION('center_axis',(-0.981627005099017,6.33476981587151E-18,
-0.190809912898503));
#90480=DIRECTION('ref_axis',(-0.190790116719056,0.0144043596890905,0.981525163092764));
#90481=DIRECTION('center_axis',(-0.981627005099017,-4.39364430834196E-18,
-0.190809912898504));
#90482=DIRECTION('ref_axis',(-0.190791033980825,0.0140667035476899,0.981529881971929));
#90483=DIRECTION('center_axis',(0.,-1.,0.));
#90484=DIRECTION('ref_axis',(0.,0.,-1.));
#90485=DIRECTION('',(-0.190809912898503,0.,0.981627005099017));
#90486=DIRECTION('center_axis',(0.,-1.,0.));
#90487=DIRECTION('ref_axis',(-0.575359874209948,0.,0.817900369940687));
#90488=DIRECTION('',(-0.190809912898503,0.,0.981627005099017));
#90489=DIRECTION('center_axis',(0.,-1.,0.));
#90490=DIRECTION('ref_axis',(-0.568338838106609,0.,0.822794606873204));
#90491=DIRECTION('center_axis',(0.981627005099017,0.,0.190809912898503));
#90492=DIRECTION('ref_axis',(0.,-1.,0.));
#90493=DIRECTION('',(-0.190809912898503,0.,0.981627005099017));
#90494=DIRECTION('center_axis',(0.981627005099017,2.22785943524066E-17,
0.190809912898503));
#90495=DIRECTION('ref_axis',(-0.189421658366475,0.120408654601104,0.97448509031121));
#90496=DIRECTION('center_axis',(0.981627005099017,4.25575130846527E-17,
0.190809912898504));
#90497=DIRECTION('ref_axis',(-0.189484179630181,0.1176757388124,0.974806732724407));
#90498=DIRECTION('center_axis',(0.,1.,0.));
#90499=DIRECTION('ref_axis',(1.,0.,0.));
#90500=DIRECTION('',(-0.190809912898503,0.,0.981627005099017));
#90501=DIRECTION('center_axis',(0.,1.,0.));
#90502=DIRECTION('ref_axis',(-0.605496675700037,0.,0.795847834523789));
#90503=DIRECTION('center_axis',(0.,1.,0.));
#90504=DIRECTION('ref_axis',(-0.597922812738481,0.,0.801553685043555));
#90505=DIRECTION('center_axis',(-0.981627005099017,0.,-0.190809912898503));
#90506=DIRECTION('ref_axis',(-0.190809912898503,0.,0.981627005099017));
#90507=DIRECTION('center_axis',(-0.981627005099017,-2.30355266031692E-18,
-0.190809912898503));
#90508=DIRECTION('ref_axis',(-0.190095951678253,0.0864261581345065,0.977954011365386));
#90509=DIRECTION('center_axis',(-0.981627005099017,-3.51491544667356E-17,
-0.190809912898504));
#90510=DIRECTION('ref_axis',(-0.190129090875907,0.0844002212861198,0.978124496906991));
#90511=DIRECTION('center_axis',(0.,-1.,0.));
#90512=DIRECTION('ref_axis',(0.,0.,-1.));
#90513=DIRECTION('',(-0.190809912898503,0.,0.981627005099017));
#90514=DIRECTION('center_axis',(0.,-1.,0.));
#90515=DIRECTION('ref_axis',(-0.578008173140809,0.,0.816030974768988));
#90516=DIRECTION('',(-0.190809912898503,0.,0.981627005099017));
#90517=DIRECTION('center_axis',(0.,-1.,0.));
#90518=DIRECTION('ref_axis',(-0.570842395473156,0.,0.82105965649913));
#90519=DIRECTION('center_axis',(0.981627005099017,0.,0.190809912898503));
#90520=DIRECTION('ref_axis',(0.,-1.,0.));
#90521=DIRECTION('',(-0.190809912898503,0.,0.981627005099017));
#90522=DIRECTION('center_axis',(0.981627005099017,7.12915019277012E-17,
0.190809912898504));
#90523=DIRECTION('ref_axis',(-0.187288294113551,0.191237274954706,0.963509937445346));
#90524=DIRECTION('center_axis',(0.981627005099017,-4.25575130846527E-18,
0.190809912898503));
#90525=DIRECTION('ref_axis',(-0.187447758333338,0.186896761643308,0.964330305643793));
#90526=DIRECTION('center_axis',(0.,1.,0.));
#90527=DIRECTION('ref_axis',(1.,0.,0.));
#90528=DIRECTION('',(-0.190809912898503,0.,0.981627005099017));
#90529=DIRECTION('center_axis',(0.,1.,0.));
#90530=DIRECTION('ref_axis',(-0.609205159578384,0.,0.793012656609638));
#90531=DIRECTION('center_axis',(0.,1.,0.));
#90532=DIRECTION('ref_axis',(-0.601428192999473,0.,0.798926860648325));
#90533=DIRECTION('center_axis',(-0.981627005099017,0.,-0.190809912898503));
#90534=DIRECTION('ref_axis',(-0.190809912898503,0.,0.981627005099017));
#90535=DIRECTION('center_axis',(-0.981627005099017,-7.37136851301412E-17,
-0.190809912898504));
#90536=DIRECTION('ref_axis',(-0.188399474304184,0.158447956579895,0.969226435430629));
#90537=DIRECTION('center_axis',(-0.981627005099017,-1.31809329250259E-17,
-0.190809912898503));
#90538=DIRECTION('ref_axis',(-0.188511838100476,0.154733739024593,0.969804494165421));
#90539=DIRECTION('center_axis',(0.,-1.,0.));
#90540=DIRECTION('ref_axis',(0.,0.,-1.));
#90541=DIRECTION('',(-0.190809912898514,0.,0.981627005099015));
#90542=DIRECTION('center_axis',(0.,-1.,0.));
#90543=DIRECTION('ref_axis',(-0.58233026870445,0.,0.812952309886996));
#90544=DIRECTION('',(-0.190809912898503,0.,0.981627005099017));
#90545=DIRECTION('center_axis',(0.,-1.,0.));
#90546=DIRECTION('ref_axis',(-0.574924123248839,0.,0.818206729687891));
#90547=DIRECTION('center_axis',(0.981627005099017,0.,0.190809912898503));
#90548=DIRECTION('ref_axis',(0.,-1.,0.));
#90549=DIRECTION('',(-0.190809912898503,0.,0.981627005099017));
#90550=DIRECTION('center_axis',(0.981627005099017,3.56457509638507E-17,
0.190809912898503));
#90551=DIRECTION('ref_axis',(-0.184141102885343,0.26206589530831,0.94731912296988));
#90552=DIRECTION('center_axis',(0.981627005099017,1.70230052338611E-16,
0.190809912898504));
#90553=DIRECTION('ref_axis',(-0.184445559233683,0.256117784474097,0.948885407283226));
#90554=DIRECTION('center_axis',(0.,1.,0.));
#90555=DIRECTION('ref_axis',(1.,0.,0.));
#90556=DIRECTION('',(-0.190809912898503,0.,0.981627005099017));
#90557=DIRECTION('center_axis',(0.,1.,0.));
#90558=DIRECTION('ref_axis',(-0.614783199716477,0.,0.788696150203847));
#90559=DIRECTION('center_axis',(0.,1.,0.));
#90560=DIRECTION('ref_axis',(-0.606694140002808,0.,0.794935356168194));
#90561=DIRECTION('center_axis',(-0.981627005099017,0.,-0.190809912898503));
#90562=DIRECTION('ref_axis',(-0.190809912898503,0.,0.981627005099017));
#90563=DIRECTION('center_axis',(-0.981627005099017,-6.44994744888736E-17,
-0.190809912898504));
#90564=DIRECTION('ref_axis',(-0.185673212549806,0.230469755025396,0.955201104563834));
#90565=DIRECTION('center_axis',(-0.981627005099017,-6.15110203167874E-17,
-0.190809912898503));
#90566=DIRECTION('ref_axis',(-0.185914346858001,0.225067256763002,0.956441626846897));
#90567=DIRECTION('center_axis',(0.,-1.,0.));
#90568=DIRECTION('ref_axis',(0.,0.,-1.));
#90569=DIRECTION('',(-0.190809912898503,0.,0.981627005099017));
#90570=DIRECTION('center_axis',(0.,-1.,0.));
#90571=DIRECTION('ref_axis',(-0.588497763347602,0.,0.808498845104228));
#90572=DIRECTION('',(-0.190809912898503,0.,0.981627005099017));
#90573=DIRECTION('center_axis',(0.,-1.,0.));
#90574=DIRECTION('ref_axis',(-0.580739637394756,0.,0.814089352318655));
#90575=DIRECTION('center_axis',(0.981627005099017,0.,0.190809912898503));
#90576=DIRECTION('ref_axis',(0.,-1.,0.));
#90577=DIRECTION('',(-0.190809912898503,0.,0.981627005099017));
#90578=DIRECTION('center_axis',(0.981627005099017,1.3367156611444E-16,0.190809912898504));
#90579=DIRECTION('ref_axis',(-0.179926892481102,0.332894515661892,0.925638998100409));
#90580=DIRECTION('center_axis',(0.981627005099017,-1.36184041870889E-16,
0.190809912898503));
#90581=DIRECTION('ref_axis',(-0.180429379482987,0.325338807305,0.928224056723776));
#90582=DIRECTION('center_axis',(0.,1.,0.));
#90583=DIRECTION('ref_axis',(1.,0.,0.));
#90584=DIRECTION('',(-0.190809912898503,0.,0.981627005099017));
#90585=DIRECTION('center_axis',(0.,1.,0.));
#90586=DIRECTION('ref_axis',(-0.622458164940441,0.,0.782653073142232));
#90587=DIRECTION('center_axis',(0.,1.,0.));
#90588=DIRECTION('ref_axis',(-0.613926597176052,0.,0.789363118773504));
#90589=DIRECTION('center_axis',(-0.981627005099017,0.,-0.190809912898503));
#90590=DIRECTION('ref_axis',(-0.190809912898503,0.,0.981627005099017));
#90591=DIRECTION('center_axis',(-0.981627005099017,-2.11926844749156E-16,
-0.190809912898504));
#90592=DIRECTION('ref_axis',(-0.181870862608285,0.302491553470801,0.935639807518331));
#90593=DIRECTION('center_axis',(-0.981627005099017,-3.33916967433989E-16,
-0.190809912898504));
#90594=DIRECTION('ref_axis',(-0.182294720132399,0.295400774501413,0.937820354564677));
#90595=DIRECTION('center_axis',(0.,-1.,0.));
#90596=DIRECTION('ref_axis',(0.,0.,-1.));
#90597=DIRECTION('center_axis',(0.,-1.,0.));
#90598=DIRECTION('ref_axis',(-0.588526570035615,0.,0.808477876235407));
#90599=DIRECTION('',(-0.190809912898503,0.,0.981627005099017));
#90600=DIRECTION('center_axis',(0.,-1.,0.));
#90601=DIRECTION('ref_axis',(-0.596773820946327,0.,0.802409500587525));
#90602=DIRECTION('',(-0.190809912898503,0.,0.981627005099017));
#90603=DIRECTION('center_axis',(0.981627005099017,0.,0.190809912898503));
#90604=DIRECTION('ref_axis',(0.,-1.,0.));
#90605=DIRECTION('center_axis',(0.981627005099017,1.70230052338611E-16,
0.190809912898504));
#90606=DIRECTION('ref_axis',(-0.175329552794068,0.394559830135812,0.901987853776442));
#90607=DIRECTION('',(-0.190809912898503,0.,0.981627005099017));
#90608=DIRECTION('center_axis',(0.981627005099017,3.0298888319273E-16,0.190809912898504));
#90609=DIRECTION('ref_axis',(-0.174568404100475,0.403723136015587,0.898072102748745));
#90610=DIRECTION('center_axis',(0.,1.,0.));
#90611=DIRECTION('ref_axis',(1.,0.,0.));
#90612=DIRECTION('',(-0.981627005099017,0.,-0.190809912898503));
#90613=DIRECTION('center_axis',(0.,1.,0.));
#90614=DIRECTION('ref_axis',(-0.620988661056824,0.,0.783819547369707));
#90615=DIRECTION('center_axis',(0.,1.,0.));
#90616=DIRECTION('ref_axis',(-0.623432047557978,0.,0.781877536496392));
#90617=DIRECTION('',(-0.190809912898503,0.,0.981627005099017));
#90618=DIRECTION('center_axis',(-0.981627005099017,0.,-0.190809912898503));
#90619=DIRECTION('ref_axis',(-0.190809912898503,0.,0.981627005099017));
#90620=DIRECTION('center_axis',(-0.981627005099017,-2.81193235733885E-16,
-0.190809912898504));
#90621=DIRECTION('ref_axis',(-0.177590469804984,0.365734292239907,0.913619205421066));
#90622=DIRECTION('center_axis',(-0.981627005099017,-9.21421064126765E-17,
-0.190809912898504));
#90623=DIRECTION('ref_axis',(-0.176923057683389,0.374513351916211,0.910185684844826));
#90624=DIRECTION('',(0.,-1.,0.));
#90625=DIRECTION('center_axis',(-0.190809912898503,0.,0.981627005099017));
#90626=DIRECTION('ref_axis',(0.,1.,0.));
#90627=DIRECTION('center_axis',(0.190809912898504,-5.12884170373276E-16,
-0.981627005099017));
#90628=DIRECTION('ref_axis',(-0.764695635116802,0.627013547027167,-0.148642515713782));
#90629=DIRECTION('center_axis',(0.,-1.,0.));
#90630=DIRECTION('ref_axis',(0.,0.,-1.));
#90631=DIRECTION('',(-0.190809912898503,0.,0.981627005099017));
#90632=DIRECTION('center_axis',(0.,-1.,0.));
#90633=DIRECTION('ref_axis',(-0.489658531934886,0.,0.87191428598422));
#90634=DIRECTION('',(-0.190809912898503,0.,0.981627005099017));
#90635=DIRECTION('center_axis',(0.,-1.,0.));
#90636=DIRECTION('ref_axis',(-0.482690338571901,0.,0.875791092127194));
#90637=DIRECTION('center_axis',(0.981627005099017,0.,0.190809912898503));
#90638=DIRECTION('ref_axis',(0.,-1.,0.));
#90639=DIRECTION('',(-0.190809912898503,0.,0.981627005099017));
#90640=DIRECTION('',(0.,1.,0.));
#90641=DIRECTION('center_axis',(0.981627005099017,1.44986047536651E-16,
0.190809912898504));
#90642=DIRECTION('ref_axis',(-0.163956083486876,0.511532430965294,0.843476718563341));
#90643=DIRECTION('center_axis',(0.981627005099017,2.00892259541186E-16,
0.190809912898504));
#90644=DIRECTION('ref_axis',(-0.164374305125881,0.507832564945586,0.845628271639005));
#90645=DIRECTION('center_axis',(0.,1.,0.));
#90646=DIRECTION('ref_axis',(1.,0.,0.));
#90647=DIRECTION('',(-0.190809912898503,0.,0.981627005099017));
#90648=DIRECTION('',(-0.981627005099017,0.,-0.190809912898503));
#90649=DIRECTION('center_axis',(0.,1.,0.));
#90650=DIRECTION('ref_axis',(-0.521450772443428,0.,0.853281367380158));
#90651=DIRECTION('center_axis',(-0.981627005099017,0.,-0.190809912898503));
#90652=DIRECTION('ref_axis',(-0.190809912898503,0.,0.981627005099017));
#90653=DIRECTION('center_axis',(-0.981627005099017,4.93467903960143E-17,
-0.190809912898503));
#90654=DIRECTION('ref_axis',(-0.166342338650152,0.489915545565209,0.855752875885288));
#90655=DIRECTION('',(0.,-1.,0.));
#90656=DIRECTION('center_axis',(-0.981627005099017,-4.72957903022569E-17,
-0.190809912898503));
#90657=DIRECTION('ref_axis',(-0.167430516953427,0.479626321074999,0.861351040009107));
#90658=DIRECTION('center_axis',(-0.190809912898503,0.,0.981627005099017));
#90659=DIRECTION('ref_axis',(0.,1.,0.));
#90660=DIRECTION('center_axis',(0.190809912898503,-8.15952089230212E-17,
-0.981627005099017));
#90661=DIRECTION('ref_axis',(-0.539785154200082,0.835238238177304,-0.104924128739137));
#90662=DIRECTION('center_axis',(0.,-1.,0.));
#90663=DIRECTION('ref_axis',(0.,0.,-1.));
#90664=DIRECTION('',(-0.190809912898503,0.,0.981627005099017));
#90665=DIRECTION('center_axis',(0.,-1.,0.));
#90666=DIRECTION('ref_axis',(-0.42194565501119,0.,0.906621124956383));
#90667=DIRECTION('',(-0.190809912898503,0.,0.981627005099017));
#90668=DIRECTION('center_axis',(0.,-1.,0.));
#90669=DIRECTION('ref_axis',(-0.416507743824211,0.,0.909132168243136));
#90670=DIRECTION('center_axis',(0.981627005099017,0.,0.190809912898503));
#90671=DIRECTION('ref_axis',(0.,-1.,0.));
#90672=DIRECTION('',(-0.190809912898503,0.,0.981627005099017));
#90673=DIRECTION('center_axis',(0.981627005099017,-7.78644601242735E-17,
0.190809912898503));
#90674=DIRECTION('ref_axis',(-0.1641530299532,0.509794631015901,0.84448991524147));
#90675=DIRECTION('center_axis',(0.981627005099017,1.4958748237708E-16,0.190809912898503));
#90676=DIRECTION('ref_axis',(-0.165285739249462,0.499641205524799,0.850317170320866));
#90677=DIRECTION('center_axis',(0.,1.,0.));
#90678=DIRECTION('ref_axis',(1.,0.,0.));
#90679=DIRECTION('',(-0.190809912898503,0.,0.981627005099017));
#90680=DIRECTION('center_axis',(0.,1.,0.));
#90681=DIRECTION('ref_axis',(-0.461221229340861,0.,0.887285172650431));
#90682=DIRECTION('center_axis',(0.,1.,0.));
#90683=DIRECTION('ref_axis',(-0.45463858135335,0.,0.890676013118695));
#90684=DIRECTION('center_axis',(-0.981627005099017,0.,-0.190809912898503));
#90685=DIRECTION('ref_axis',(-0.190809912898503,0.,0.981627005099017));
#90686=DIRECTION('center_axis',(-0.981627005099017,3.1638104497012E-17,
-0.190809912898503));
#90687=DIRECTION('ref_axis',(-0.167345158855712,0.480443832419612,0.860911912856079));
#90688=DIRECTION('center_axis',(-0.981627005099017,1.21485874416176E-16,
-0.190809912898503));
#90689=DIRECTION('ref_axis',(-0.16834743337274,0.470728280640113,0.86606814251675));
#90690=DIRECTION('center_axis',(0.,-1.,0.));
#90691=DIRECTION('ref_axis',(0.,0.,-1.));
#90692=DIRECTION('',(-0.190809912898503,0.,0.981627005099017));
#90693=DIRECTION('center_axis',(0.,-1.,0.));
#90694=DIRECTION('ref_axis',(-0.353115435082057,0.,0.935579761167806));
#90695=DIRECTION('',(-0.190809912898503,0.,0.981627005099017));
#90696=DIRECTION('center_axis',(0.,-1.,0.));
#90697=DIRECTION('ref_axis',(-0.349265854344674,0.,0.937023672587243));
#90698=DIRECTION('center_axis',(0.981627005099017,0.,0.190809912898503));
#90699=DIRECTION('ref_axis',(0.,-1.,0.));
#90700=DIRECTION('',(-0.190809912898503,0.,0.981627005099017));
#90701=DIRECTION('center_axis',(0.981627005099017,2.7359611324339E-16,0.190809912898504));
#90702=DIRECTION('ref_axis',(-0.164842107563918,0.503650570550101,0.848034894540575));
#90703=DIRECTION('center_axis',(0.981627005099017,8.76849763688622E-17,
0.190809912898503));
#90704=DIRECTION('ref_axis',(-0.165917896355328,0.493852879734794,0.853569320469447));
#90705=DIRECTION('center_axis',(0.,1.,0.));
#90706=DIRECTION('ref_axis',(1.,0.,0.));
#90707=DIRECTION('',(-0.190809912898503,0.,0.981627005099017));
#90708=DIRECTION('center_axis',(0.,1.,0.));
#90709=DIRECTION('ref_axis',(-0.391618463739157,0.,0.920127697039157));
#90710=DIRECTION('center_axis',(0.,1.,0.));
#90711=DIRECTION('ref_axis',(-0.386687356930034,0.,0.922210869590282));
#90712=DIRECTION('center_axis',(-0.981627005099017,0.,-0.190809912898503));
#90713=DIRECTION('ref_axis',(-0.190809912898503,0.,0.981627005099017));
#90714=DIRECTION('center_axis',(-0.981627005099017,-4.76390639943534E-16,
-0.190809912898504));
#90715=DIRECTION('ref_axis',(-0.168060481549877,0.473536168037885,0.864591910730848));
#90716=DIRECTION('center_axis',(-0.981627005099017,-8.86144962521498E-17,
-0.190809912898503));
#90717=DIRECTION('ref_axis',(-0.169003575142171,0.464225672106184,0.869443682446843));
#90718=DIRECTION('center_axis',(0.,-1.,0.));
#90719=DIRECTION('ref_axis',(0.,0.,-1.));
#90720=DIRECTION('',(-0.190809912898503,0.,0.981627005099017));
#90721=DIRECTION('center_axis',(0.,-1.,0.));
#90722=DIRECTION('ref_axis',(-0.283219375007823,0.,0.95905515254347));
#90723=DIRECTION('',(-0.190809912898503,0.,0.981627005099017));
#90724=DIRECTION('center_axis',(0.,-1.,0.));
#90725=DIRECTION('ref_axis',(-0.281011109742765,0.,0.959704515046761));
#90726=DIRECTION('center_axis',(0.981627005099017,0.,0.190809912898503));
#90727=DIRECTION('ref_axis',(0.,-1.,0.));
#90728=DIRECTION('',(-0.190809912898503,0.,0.981627005099017));
#90729=DIRECTION('center_axis',(0.981627005099017,1.64661493304004E-16,
0.190809912898504));
#90730=DIRECTION('ref_axis',(-0.165266478237664,0.499816171268802,0.85021808149975));
#90731=DIRECTION('center_axis',(0.981627005099017,2.88018088012718E-16,
0.190809912898504));
#90732=DIRECTION('ref_axis',(-0.166307924300349,0.490236343963907,0.855575830287305));
#90733=DIRECTION('center_axis',(0.,1.,0.));
#90734=DIRECTION('ref_axis',(1.,0.,0.));
#90735=DIRECTION('',(-0.190809912898503,0.,0.981627005099017));
#90736=DIRECTION('center_axis',(0.,1.,0.));
#90737=DIRECTION('ref_axis',(-0.320878589892636,0.,0.947120335833052));
#90738=DIRECTION('center_axis',(0.,1.,0.));
#90739=DIRECTION('ref_axis',(-0.317659115433943,0.,0.948204981204868));
#90740=DIRECTION('center_axis',(-0.981627005099017,0.,-0.190809912898503));
#90741=DIRECTION('ref_axis',(-0.190809912898503,0.,0.981627005099017));
#90742=DIRECTION('center_axis',(-0.981627005099017,-4.97231835007436E-16,
-0.190809912898504));
#90743=DIRECTION('ref_axis',(-0.168533680974174,0.468894226820799,0.867026298581202));
#90744=DIRECTION('center_axis',(-0.981627005099017,-5.79678245784151E-17,
-0.190809912898503));
#90745=DIRECTION('ref_axis',(-0.169438586252028,0.459849689864406,0.871681609431175));
#90746=DIRECTION('center_axis',(0.,-1.,0.));
#90747=DIRECTION('ref_axis',(0.,0.,-1.));
#90748=DIRECTION('',(-0.190809912898503,0.,0.981627005099017));
#90749=DIRECTION('center_axis',(0.,-1.,0.));
#90750=DIRECTION('ref_axis',(-0.212288523804663,0.,0.977207031626787));
#90751=DIRECTION('',(-0.190809912898503,0.,0.981627005099017));
#90752=DIRECTION('center_axis',(0.,-1.,0.));
#90753=DIRECTION('ref_axis',(-0.211771596214555,0.,0.977319185853189));
#90754=DIRECTION('center_axis',(0.981627005099017,0.,0.190809912898503));
#90755=DIRECTION('ref_axis',(0.,-1.,0.));
#90756=DIRECTION('',(-0.190809912898503,0.,0.981627005099017));
#90757=DIRECTION('center_axis',(0.981627005099017,5.94759471576322E-17,
0.190809912898503));
#90758=DIRECTION('ref_axis',(-0.165450643172752,0.498139876682696,0.851165523228162));
#90759=DIRECTION('center_axis',(0.981627005099017,7.15405393416096E-17,
0.190809912898503));
#90760=DIRECTION('ref_axis',(-0.166477354471641,0.488654299036596,0.856447468605738));
#90761=DIRECTION('center_axis',(0.,1.,0.));
#90762=DIRECTION('ref_axis',(1.,0.,0.));
#90763=DIRECTION('',(-0.190809912898503,0.,0.981627005099017));
#90764=DIRECTION('center_axis',(0.,1.,0.));
#90765=DIRECTION('ref_axis',(-0.249046035387048,0.,0.968491648006318));
#90766=DIRECTION('center_axis',(0.,1.,0.));
#90767=DIRECTION('ref_axis',(-0.247593816860215,0.,0.968863923289845));
#90768=DIRECTION('center_axis',(-0.981627005099017,0.,-0.190809912898503));
#90769=DIRECTION('ref_axis',(-0.190809912898503,0.,0.981627005099017));
#90770=DIRECTION('center_axis',(-0.981627005099017,-1.19226339786349E-16,
-0.190809912898503));
#90771=DIRECTION('ref_axis',(-0.168792500449209,0.466330160156009,0.868357802706335));
#90772=DIRECTION('center_axis',(-0.981627005099017,4.30196144549347E-17,
-0.190809912898503));
#90773=DIRECTION('ref_axis',(-0.169676842617203,0.457430398202074,0.872907326054805));
#90774=DIRECTION('center_axis',(0.,-1.,0.));
#90775=DIRECTION('ref_axis',(0.,0.,-1.));
#90776=DIRECTION('',(-0.190809912898503,0.,0.981627005099017));
#90777=DIRECTION('center_axis',(0.,-1.,0.));
#90778=DIRECTION('ref_axis',(-0.140336198717109,0.,0.990103909359837));
#90779=DIRECTION('',(-0.190809912898503,0.,0.981627005099017));
#90780=DIRECTION('center_axis',(0.,-1.,0.));
#90781=DIRECTION('ref_axis',(-0.141559381142733,0.,0.989929765998824));
#90782=DIRECTION('center_axis',(0.981627005099017,0.,0.190809912898503));
#90783=DIRECTION('ref_axis',(0.,-1.,0.));
#90784=DIRECTION('',(-0.190809912898503,0.,0.981627005099017));
#90785=DIRECTION('center_axis',(0.981627005099017,3.12772334456263E-16,
0.190809912898504));
#90786=DIRECTION('ref_axis',(-0.165404852718561,0.498557368703801,0.850929952938721));
#90787=DIRECTION('center_axis',(0.981627005099017,3.1528628345683E-16,0.190809912898504));
#90788=DIRECTION('ref_axis',(-0.166435218084341,0.48904837398272,0.856230696766984));
#90789=DIRECTION('center_axis',(0.,1.,0.));
#90790=DIRECTION('ref_axis',(1.,0.,0.));
#90791=DIRECTION('',(-0.190809912898503,0.,0.981627005099017));
#90792=DIRECTION('center_axis',(0.,1.,0.));
#90793=DIRECTION('ref_axis',(-0.176144643249429,0.,0.984364294686947));
#90794=DIRECTION('center_axis',(0.,1.,0.));
#90795=DIRECTION('ref_axis',(-0.176512963578363,0.,0.984298315394669));
#90796=DIRECTION('center_axis',(-0.981627005099017,0.,-0.190809912898503));
#90797=DIRECTION('ref_axis',(-0.190809912898503,0.,0.981627005099017));
#90798=DIRECTION('center_axis',(-0.981627005099017,-2.0812226289074E-16,
-0.190809912898504));
#90799=DIRECTION('ref_axis',(-0.168851372823095,0.465744402600315,0.868660673302431));
#90800=DIRECTION('center_axis',(-0.981627005099017,-3.5763068107684E-16,
-0.190809912898504));
#90801=DIRECTION('ref_axis',(-0.169731069638787,0.456877502295317,0.873186298504314));
#90802=DIRECTION('center_axis',(0.,-1.,0.));
#90803=DIRECTION('ref_axis',(0.,0.,-1.));
#90804=DIRECTION('',(-0.190809912898503,0.,0.981627005099017));
#90805=DIRECTION('center_axis',(0.,-1.,0.));
#90806=DIRECTION('ref_axis',(-0.0673590974157918,0.,0.997728796815713));
#90807=DIRECTION('',(-0.190809912898503,0.,0.981627005099017));
#90808=DIRECTION('center_axis',(0.,-1.,0.));
#90809=DIRECTION('ref_axis',(-0.0703714709533455,0.,0.997520854957861));
#90810=DIRECTION('center_axis',(0.981627005099017,0.,0.190809912898503));
#90811=DIRECTION('ref_axis',(0.,-1.,0.));
#90812=DIRECTION('',(-0.190809912898503,0.,0.981627005099017));
#90813=DIRECTION('center_axis',(0.981627005099017,1.654982782964E-16,0.190809912898504));
#90814=DIRECTION('ref_axis',(-0.165126579629839,0.501084557252584,0.849498369146599));
#90815=DIRECTION('center_axis',(0.981627005099017,1.73655546916773E-16,
0.190809912898504));
#90816=DIRECTION('ref_axis',(-0.166179287158349,0.491433013476625,0.854914052864279));
#90817=DIRECTION('center_axis',(0.,1.,0.));
#90818=DIRECTION('ref_axis',(1.,0.,0.));
#90819=DIRECTION('',(-0.190809912898503,0.,0.981627005099017));
#90820=DIRECTION('center_axis',(0.,1.,0.));
#90821=DIRECTION('ref_axis',(-0.102179792300205,0.,0.994765947369273));
#90822=DIRECTION('center_axis',(0.,1.,0.));
#90823=DIRECTION('ref_axis',(-0.104421411927276,0.,0.994533141092399));
#90824=DIRECTION('center_axis',(-0.981627005099017,0.,-0.190809912898503));
#90825=DIRECTION('ref_axis',(-0.190809912898503,0.,0.981627005099017));
#90826=DIRECTION('center_axis',(-0.981627005099017,-7.47673759321185E-17,
-0.190809912898503));
#90827=DIRECTION('ref_axis',(-0.16871350914603,0.467114619230688,0.867951429708254));
#90828=DIRECTION('center_axis',(-0.981627005099017,8.63179540716556E-17,
-0.190809912898503));
#90829=DIRECTION('ref_axis',(-0.169604102816414,0.458170724869904,0.872533114087956));
#90830=DIRECTION('center_axis',(0.,-1.,0.));
#90831=DIRECTION('ref_axis',(0.,0.,-1.));
#90832=DIRECTION('',(-0.190809912898503,0.,0.981627005099017));
#90833=DIRECTION('center_axis',(0.,-1.,0.));
#90834=DIRECTION('ref_axis',(0.00666297473127236,0.,0.999977802137493));
#90835=DIRECTION('',(-0.190809912898503,0.,0.981627005099017));
#90836=DIRECTION('center_axis',(0.,-1.,0.));
#90837=DIRECTION('ref_axis',(0.00181042398919864,0.,0.999998361181147));
#90838=DIRECTION('center_axis',(0.981627005099017,0.,0.190809912898503));
#90839=DIRECTION('ref_axis',(0.,-1.,0.));
#90840=DIRECTION('',(-0.190809912898503,0.,0.981627005099017));
#90841=DIRECTION('center_axis',(0.981627005099017,-3.37281270145013E-16,
0.190809912898503));
#90842=DIRECTION('ref_axis',(-0.164600160397928,0.505819296281817,0.846790190487552));
#90843=DIRECTION('center_axis',(0.981627005099017,2.65237045479699E-16,
0.190809912898504));
#90844=DIRECTION('ref_axis',(-0.165695772046853,0.495896975310785,0.852426595668748));
#90845=DIRECTION('center_axis',(0.,1.,0.));
#90846=DIRECTION('ref_axis',(1.,0.,0.));
#90847=DIRECTION('',(-0.190809912898503,0.,0.981627005099017));
#90848=DIRECTION('center_axis',(0.,1.,0.));
#90849=DIRECTION('ref_axis',(-0.027138860824711,0.,0.999631673284284));
#90850=DIRECTION('center_axis',(0.,1.,0.));
#90851=DIRECTION('ref_axis',(-0.0313077694633037,0.,0.999509791633495));
#90852=DIRECTION('center_axis',(-0.981627005099017,0.,-0.190809912898503));
#90853=DIRECTION('ref_axis',(-0.190809912898503,0.,0.981627005099017));
#90854=DIRECTION('center_axis',(-0.981627005099017,4.55117302256744E-17,
-0.190809912898503));
#90855=DIRECTION('ref_axis',(-0.168371348274985,0.470493294519803,0.866191173409177));
#90856=DIRECTION('center_axis',(-0.981627005099017,-2.77156052561386E-16,
-0.190809912898504));
#90857=DIRECTION('ref_axis',(-0.169289267864162,0.461357702298085,0.870913436752613));
#90858=DIRECTION('center_axis',(0.,-1.,0.));
#90859=DIRECTION('ref_axis',(0.,0.,-1.));
#90860=DIRECTION('',(-0.190809912898503,0.,0.981627005099017));
#90861=DIRECTION('center_axis',(0.,-1.,0.));
#90862=DIRECTION('ref_axis',(0.081768816582179,0.,0.996651323500225));
#90863=DIRECTION('',(-0.190809912898503,0.,0.981627005099017));
#90864=DIRECTION('center_axis',(0.,-1.,0.));
#90865=DIRECTION('ref_axis',(0.0750213618657929,0.,0.9971819268638));
#90866=DIRECTION('center_axis',(0.981627005099017,0.,0.190809912898503));
#90867=DIRECTION('ref_axis',(0.,-1.,0.));
#90868=DIRECTION('',(-0.190809912898503,0.,0.981627005099017));
#90869=DIRECTION('center_axis',(0.981627005099017,-9.45984020779368E-17,
0.190809912898503));
#90870=DIRECTION('ref_axis',(-0.163794505829796,0.512952199260781,0.842645477726844));
#90871=DIRECTION('center_axis',(0.981627005099017,4.54116221843461E-17,
0.190809912898503));
#90872=DIRECTION('ref_axis',(-0.164957395957987,0.502612750449379,0.848627998951525));
#90873=DIRECTION('center_axis',(0.,1.,0.));
#90874=DIRECTION('ref_axis',(1.,0.,0.));
#90875=DIRECTION('',(-0.190809912898503,0.,0.981627005099017));
#90876=DIRECTION('center_axis',(0.,1.,0.));
#90877=DIRECTION('ref_axis',(0.0490098699559957,0.,0.998798294275124));
#90878=DIRECTION('center_axis',(0.,1.,0.));
#90879=DIRECTION('ref_axis',(0.0428565438402263,0.,0.999081236261632));
#90880=DIRECTION('center_axis',(-0.981627005099017,0.,-0.190809912898503));
#90881=DIRECTION('ref_axis',(-0.190809912898503,0.,0.981627005099017));
#90882=DIRECTION('center_axis',(-0.981627005099017,1.08700534976828E-16,
-0.190809912898503));
#90883=DIRECTION('ref_axis',(-0.167805489378009,0.476013437950482,0.863280096275345));
#90884=DIRECTION('center_axis',(-0.981627005099017,-3.87865929651451E-16,
-0.190809912898504));
#90885=DIRECTION('ref_axis',(-0.168769478873421,0.466558960501992,0.868239367557182));
#90886=DIRECTION('center_axis',(0.,-1.,0.));
#90887=DIRECTION('ref_axis',(0.,0.,-1.));
#90888=DIRECTION('',(-0.190809912898503,0.,0.981627005099017));
#90889=DIRECTION('center_axis',(0.,-1.,0.));
#90890=DIRECTION('ref_axis',(0.158019336155245,0.,0.987436017877136));
#90891=DIRECTION('',(-0.190809912898503,0.,0.981627005099017));
#90892=DIRECTION('center_axis',(0.,-1.,0.));
#90893=DIRECTION('ref_axis',(0.149316167640555,0.,0.988789503423827));
#90894=DIRECTION('center_axis',(0.981627005099017,0.,0.190809912898503));
#90895=DIRECTION('ref_axis',(0.,-1.,0.));
#90896=DIRECTION('',(-0.190809912898493,0.,0.981627005099019));
#90897=DIRECTION('',(0.,1.,0.));
#90898=DIRECTION('center_axis',(0.981627005099017,2.45653454077401E-16,
0.190809912898504));
#90899=DIRECTION('ref_axis',(-0.165310900973356,0.499412515026929,0.850446615522606));
#90900=DIRECTION('center_axis',(0.981627005099017,1.72689897470369E-16,
0.190809912898504));
#90901=DIRECTION('ref_axis',(-0.163919320156954,0.511855936218513,0.843287588570561));
#90902=DIRECTION('center_axis',(0.,1.,0.));
#90903=DIRECTION('ref_axis',(1.,0.,0.));
#90904=DIRECTION('',(-0.190809912898503,0.,0.981627005099017));
#90905=DIRECTION('',(-0.981627005099017,0.,-0.190809912898503));
#90906=DIRECTION('center_axis',(0.,1.,0.));
#90907=DIRECTION('ref_axis',(0.118119757483604,0.,0.992999356944411));
#90908=DIRECTION('center_axis',(-0.981627005099017,0.,-0.190809912898503));
#90909=DIRECTION('ref_axis',(-0.190809912898503,0.,0.981627005099017));
#90910=DIRECTION('center_axis',(-0.981627005099017,3.04906463307191E-16,
-0.190809912898503));
#90911=DIRECTION('ref_axis',(-0.166981814435774,0.483903660262205,0.85904267718931));
#90912=DIRECTION('',(1.82418708658322E-14,-1.,3.54587819297421E-15));
#90913=DIRECTION('center_axis',(-0.981627005099017,-7.69816334883557E-17,
-0.190809912898503));
#90914=DIRECTION('ref_axis',(-0.168014818177704,0.473981020103497,0.864356994218455));
#90915=DIRECTION('center_axis',(-0.190809912898503,0.,0.981627005099017));
#90916=DIRECTION('ref_axis',(0.,1.,0.));
#90917=DIRECTION('center_axis',(0.190809912898503,3.96319586197532E-16,
-0.981627005099017));
#90918=DIRECTION('ref_axis',(0.472312009925091,0.876637065109843,0.091808612646749));
#90919=DIRECTION('center_axis',(-0.981627005099017,0.,-0.190809912898503));
#90920=DIRECTION('ref_axis',(-0.190809912898503,0.,0.981627005099017));
#90921=DIRECTION('',(-0.190809912898503,0.,0.981627005099017));
#90922=DIRECTION('center_axis',(-0.981627005099017,-1.8030757312937E-16,
-0.190809912898504));
#90923=DIRECTION('ref_axis',(-0.181596654085648,0.306983029510506,0.934229134001637));
#90924=DIRECTION('',(-0.190809912898503,0.,0.981627005099017));
#90925=DIRECTION('center_axis',(-0.981627005099017,9.94141557488341E-17,
-0.190809912898503));
#90926=DIRECTION('ref_axis',(-0.182046275027808,0.299579406426393,0.936542221682349));
#90927=DIRECTION('center_axis',(0.,-1.,0.));
#90928=DIRECTION('ref_axis',(0.,0.,-1.));
#90929=DIRECTION('',(-0.190809912898493,0.,0.981627005099019));
#90930=DIRECTION('',(0.981627005099017,-1.858330177458E-14,0.190809912898503));
#90931=DIRECTION('center_axis',(0.,-1.,0.));
#90932=DIRECTION('ref_axis',(0.341205688802883,0.,0.939988658404212));
#90933=DIRECTION('center_axis',(0.,-1.,0.));
#90934=DIRECTION('ref_axis',(0.33310368336774,0.,0.942890203643481));
#90935=DIRECTION('center_axis',(0.981627005099017,0.,0.190809912898503));
#90936=DIRECTION('ref_axis',(0.,-1.,0.));
#90937=DIRECTION('',(-0.190809912898487,0.,0.98162700509902));
#90938=DIRECTION('',(0.,1.,0.));
#90939=DIRECTION('center_axis',(0.981627005099017,-1.87874135277778E-16,
0.190809912898503));
#90940=DIRECTION('ref_axis',(-0.179319086707495,0.341783624658495,0.922512124070839));
#90941=DIRECTION('center_axis',(0.,1.,0.));
#90942=DIRECTION('ref_axis',(1.,0.,0.));
#90943=DIRECTION('center_axis',(0.,1.,0.));
#90944=DIRECTION('ref_axis',(0.313402836107741,0.,0.949620272698316));
#90945=DIRECTION('',(-0.981627005099017,0.,-0.190809912898503));
#90946=DIRECTION('center_axis',(0.,1.,0.));
#90947=DIRECTION('ref_axis',(0.302289399785084,0.,0.953216197290821));
#90948=DIRECTION('center_axis',(-0.190809912898503,0.,0.981627005099017));
#90949=DIRECTION('ref_axis',(0.,1.,0.));
#90950=DIRECTION('center_axis',(0.190809912898503,0.,-0.981627005099017));
#90951=DIRECTION('ref_axis',(0.827186458119361,0.538432243009611,0.160789561824102));
#90952=DIRECTION('center_axis',(0.,-1.,0.));
#90953=DIRECTION('ref_axis',(0.,0.,-1.));
#90954=DIRECTION('',(-0.190809912898493,0.,0.981627005099019));
#90955=DIRECTION('center_axis',(0.,-1.,0.));
#90956=DIRECTION('ref_axis',(0.335481893758792,0.,0.942046654343624));
#90957=DIRECTION('',(-0.190809912898503,0.,0.981627005099017));
#90958=DIRECTION('center_axis',(0.,-1.,0.));
#90959=DIRECTION('ref_axis',(0.324430753252009,0.,0.945909449336634));
#90960=DIRECTION('center_axis',(0.981627005099017,0.,0.190809912898503));
#90961=DIRECTION('ref_axis',(0.,-1.,0.));
#90962=DIRECTION('',(-0.190809912898503,0.,0.981627005099017));
#90963=DIRECTION('center_axis',(0.981627005099017,1.97664555486468E-16,
0.190809912898504));
#90964=DIRECTION('ref_axis',(-0.183399207679054,0.275985344180091,0.943502422053326));
#90965=DIRECTION('center_axis',(0.981627005099017,1.87874135277778E-17,
0.190809912898503));
#90966=DIRECTION('ref_axis',(-0.183773297839977,0.2690637045184,0.945426939489168));
#90967=DIRECTION('center_axis',(0.,1.,0.));
#90968=DIRECTION('ref_axis',(1.,0.,0.));
#90969=DIRECTION('',(-0.190809912898503,0.,0.981627005099017));
#90970=DIRECTION('center_axis',(0.,1.,0.));
#90971=DIRECTION('ref_axis',(0.303402411978182,0.,0.952862517053652));
#90972=DIRECTION('center_axis',(0.,1.,0.));
#90973=DIRECTION('ref_axis',(0.292916715383648,0.,0.956137959631796));
#90974=DIRECTION('center_axis',(-0.981627005099017,0.,-0.190809912898503));
#90975=DIRECTION('ref_axis',(-0.190809912898503,0.,0.981627005099017));
#90976=DIRECTION('center_axis',(-0.981627005099017,-1.56582892454453E-16,
-0.190809912898504));
#90977=DIRECTION('ref_axis',(-0.185517346687496,0.233891832008005,0.954399248217417));
#90978=DIRECTION('center_axis',(-0.981627005099017,7.23012041809702E-17,
-0.190809912898503));
#90979=DIRECTION('ref_axis',(-0.185772975278006,0.228250976324805,0.955714336746672));
#90980=DIRECTION('center_axis',(0.,-1.,0.));
#90981=DIRECTION('ref_axis',(0.,0.,-1.));
#90982=DIRECTION('',(-0.190809912898503,0.,0.981627005099017));
#90983=DIRECTION('center_axis',(0.,-1.,0.));
#90984=DIRECTION('ref_axis',(0.329025837701854,0.,0.944320919033669));
#90985=DIRECTION('',(-0.190809912898503,0.,0.981627005099017));
#90986=DIRECTION('center_axis',(0.,-1.,0.));
#90987=DIRECTION('ref_axis',(0.318363930413136,0.,0.947968568999996));
#90988=DIRECTION('center_axis',(0.981627005099017,0.,0.190809912898503));
#90989=DIRECTION('ref_axis',(0.,-1.,0.));
#90990=DIRECTION('',(-0.190809912898503,0.,0.981627005099017));
#90991=DIRECTION('center_axis',(0.981627005099017,1.23540347179043E-16,
0.190809912898504));
#90992=DIRECTION('ref_axis',(-0.186900249967823,0.201394710617895,0.961513633339174));
#90993=DIRECTION('center_axis',(0.981627005099017,1.17421334548611E-16,
0.190809912898504));
#90994=DIRECTION('ref_axis',(-0.187095820528074,0.196343784378293,0.962519751629512));
#90995=DIRECTION('center_axis',(0.,1.,0.));
#90996=DIRECTION('ref_axis',(1.,0.,0.));
#90997=DIRECTION('',(-0.190809912898503,0.,0.981627005099017));
#90998=DIRECTION('center_axis',(0.,1.,0.));
#90999=DIRECTION('ref_axis',(0.296165820896561,0.,0.955136538162302));
#91000=DIRECTION('center_axis',(0.,1.,0.));
#91001=DIRECTION('ref_axis',(0.286119870298458,0.,0.958193832071775));
#91002=DIRECTION('center_axis',(-0.981627005099017,0.,-0.190809912898503));
#91003=DIRECTION('ref_axis',(-0.190809912898503,0.,0.981627005099017));
#91004=DIRECTION('center_axis',(-0.981627005099017,4.27044252148508E-17,
-0.190809912898503));
#91005=DIRECTION('ref_axis',(-0.188326885887437,0.160800634505503,0.968853002263278));
#91006=DIRECTION('center_axis',(-0.981627005099017,3.16317768291745E-17,
-0.190809912898503));
#91007=DIRECTION('ref_axis',(-0.188445952191515,0.156922546223307,0.969465542239345));
#91008=DIRECTION('center_axis',(0.,-1.,0.));
#91009=DIRECTION('ref_axis',(0.,0.,-1.));
#91010=DIRECTION('',(-0.190809912898503,0.,0.981627005099017));
#91011=DIRECTION('center_axis',(0.,-1.,0.));
#91012=DIRECTION('ref_axis',(0.325079416156572,0.,0.945686720426644));
#91013=DIRECTION('',(-0.190809912898503,0.,0.981627005099017));
#91014=DIRECTION('center_axis',(0.,-1.,0.));
#91015=DIRECTION('ref_axis',(0.314651032875617,0.,0.949207420699136));
#91016=DIRECTION('center_axis',(0.981627005099017,0.,0.190809912898503));
#91017=DIRECTION('ref_axis',(0.,-1.,0.));
#91018=DIRECTION('',(-0.190809912898513,0.,0.981627005099015));
#91019=DIRECTION('center_axis',(0.981627005099017,5.43577527587787E-17,
0.190809912898504));
#91020=DIRECTION('ref_axis',(-0.189269653813775,0.126804077055707,0.973703098581525));
#91021=DIRECTION('center_axis',(0.981627005099017,7.98465074930554E-17,
0.190809912898504));
#91022=DIRECTION('ref_axis',(-0.189346238510002,0.123623864238198,0.974097090721931));
#91023=DIRECTION('center_axis',(0.,1.,0.));
#91024=DIRECTION('ref_axis',(1.,0.,0.));
#91025=DIRECTION('',(-0.190809912898503,0.,0.981627005099017));
#91026=DIRECTION('center_axis',(0.,1.,0.));
#91027=DIRECTION('ref_axis',(0.291369117343108,0.,0.956610703190539));
#91028=DIRECTION('center_axis',(0.,1.,0.));
#91029=DIRECTION('ref_axis',(0.281608014703448,0.,0.95952953370638));
#91030=DIRECTION('center_axis',(-0.981627005099017,0.,-0.190809912898503));
#91031=DIRECTION('ref_axis',(-0.190809912898503,0.,0.981627005099017));
#91032=DIRECTION('center_axis',(-0.981627005099017,-5.45667655523093E-17,
-0.190809912898504));
#91033=DIRECTION('ref_axis',(-0.190074550777785,0.0877094370030095,0.977843913826352));
#91034=DIRECTION('center_axis',(-0.981627005099017,-7.68200294422809E-17,
-0.190809912898504));
#91035=DIRECTION('ref_axis',(-0.190109657599699,0.0855941161218201,0.978024521866732));
#91036=DIRECTION('center_axis',(0.,-1.,0.));
#91037=DIRECTION('ref_axis',(0.,0.,-1.));
#91038=DIRECTION('',(-0.190809912898503,0.,0.981627005099017));
#91039=DIRECTION('center_axis',(0.,-1.,0.));
#91040=DIRECTION('ref_axis',(0.323480044633156,0.,0.946234992337597));
#91041=DIRECTION('',(-0.190809912898503,0.,0.981627005099017));
#91042=DIRECTION('center_axis',(0.,-1.,0.));
#91043=DIRECTION('ref_axis',(0.313145356260713,0.,0.949705209974312));
#91044=DIRECTION('center_axis',(0.981627005099017,0.,0.190809912898503));
#91045=DIRECTION('ref_axis',(0.,-1.,0.));
#91046=DIRECTION('',(-0.190809912898503,0.,0.981627005099017));
#91047=DIRECTION('center_axis',(0.981627005099017,2.96496833229702E-17,
0.190809912898504));
#91048=DIRECTION('ref_axis',(-0.190549638224689,0.0522134434935414,0.980288014662521));
#91049=DIRECTION('center_axis',(0.981627005099017,4.22716804374999E-17,
0.190809912898504));
#91050=DIRECTION('ref_axis',(-0.190562538121797,0.0509039440980811,0.980354378548817));
#91051=DIRECTION('center_axis',(0.,1.,0.));
#91052=DIRECTION('ref_axis',(1.,0.,0.));
#91053=DIRECTION('',(-0.190809912898503,0.,0.981627005099017));
#91054=DIRECTION('center_axis',(0.,1.,0.));
#91055=DIRECTION('ref_axis',(0.288811078038997,0.,0.957386108736675));
#91056=DIRECTION('center_axis',(0.,1.,0.));
#91057=DIRECTION('ref_axis',(0.27919973712564,0.,0.960233048165378));
#91058=DIRECTION('center_axis',(-0.981627005099017,0.,-0.190809912898503));
#91059=DIRECTION('ref_axis',(-0.190809912898503,0.,0.981627005099017));
#91060=DIRECTION('center_axis',(-0.981627005099017,-8.89675525309391E-18,
-0.190809912898504));
#91061=DIRECTION('ref_axis',(-0.190789524444921,0.0146182395004994,0.981522116121683));
#91062=DIRECTION('center_axis',(-0.981627005099017,-1.35564757839319E-17,
-0.190809912898504));
#91063=DIRECTION('ref_axis',(-0.190790496067195,0.0142656860203004,0.98152711466001));
#91064=DIRECTION('center_axis',(0.,-1.,0.));
#91065=DIRECTION('ref_axis',(0.,0.,-1.));
#91066=DIRECTION('',(-0.190809912898503,0.,0.981627005099017));
#91067=DIRECTION('center_axis',(0.,-1.,0.));
#91068=DIRECTION('ref_axis',(-0.51578631619443,0.,0.856717267262998));
#91069=DIRECTION('',(-0.190809912898503,0.,0.981627005099017));
#91070=DIRECTION('center_axis',(0.,-1.,0.));
#91071=DIRECTION('ref_axis',(-0.509828849403992,0.,0.860275853616386));
#91072=DIRECTION('center_axis',(0.981627005099017,0.,0.190809912898503));
#91073=DIRECTION('ref_axis',(0.,-1.,0.));
#91074=DIRECTION('',(-0.190809912898503,0.,0.981627005099017));
#91075=DIRECTION('center_axis',(0.981627005099017,4.73701931306098E-17,
0.190809912898504));
#91076=DIRECTION('ref_axis',(-0.190588158690433,0.0481974707091998,0.980486184290338));
#91077=DIRECTION('center_axis',(0.981627005099017,1.61266538800991E-17,
0.190809912898504));
#91078=DIRECTION('ref_axis',(-0.19059759198742,0.047161767008978,0.980534714154062));
#91079=DIRECTION('center_axis',(0.,1.,0.));
#91080=DIRECTION('ref_axis',(1.,0.,0.));
#91081=DIRECTION('',(-0.190809912898503,0.,0.981627005099017));
#91082=DIRECTION('center_axis',(0.,1.,0.));
#91083=DIRECTION('ref_axis',(-0.54548104653432,0.,0.838123157937915));
#91084=DIRECTION('center_axis',(0.,1.,0.));
#91085=DIRECTION('ref_axis',(-0.538997674779873,0.,0.842307251887273));
#91086=DIRECTION('center_axis',(-0.981627005099017,0.,-0.190809912898503));
#91087=DIRECTION('ref_axis',(-0.190809912898503,0.,0.981627005099017));
#91088=DIRECTION('center_axis',(-0.981627005099017,-1.45950760997372E-17,
-0.190809912898504));
#91089=DIRECTION('ref_axis',(-0.190791331241222,0.0139555250478298,0.981531411236463));
#91090=DIRECTION('center_axis',(-0.981627005099017,-5.16982180453677E-18,
-0.190809912898504));
#91091=DIRECTION('ref_axis',(-0.190792141709014,0.0136478005707896,0.981535580710994));
#91092=DIRECTION('center_axis',(0.,-1.,0.));
#91093=DIRECTION('ref_axis',(0.,0.,-1.));
#91094=DIRECTION('',(-0.190809912898503,0.,0.981627005099017));
#91095=DIRECTION('center_axis',(0.,-1.,0.));
#91096=DIRECTION('ref_axis',(-0.516706060412873,0.,0.856162862504914));
#91097=DIRECTION('',(-0.190809912898503,0.,0.981627005099017));
#91098=DIRECTION('center_axis',(0.,-1.,0.));
#91099=DIRECTION('ref_axis',(-0.510698343921526,0.,0.85975996738381));
#91100=DIRECTION('center_axis',(0.981627005099017,0.,0.190809912898503));
#91101=DIRECTION('ref_axis',(0.,-1.,0.));
#91102=DIRECTION('',(-0.190809912898503,0.,0.981627005099017));
#91103=DIRECTION('center_axis',(0.981627005099017,8.84243605104716E-17,
0.190809912898504));
#91104=DIRECTION('ref_axis',(-0.18949826744453,0.117051000293799,0.974879207884619));
#91105=DIRECTION('center_axis',(0.981627005099017,5.24116251103221E-17,
0.190809912898504));
#91106=DIRECTION('ref_axis',(-0.189554217765144,0.114535719878902,0.975167045894838));
#91107=DIRECTION('center_axis',(0.,1.,0.));
#91108=DIRECTION('ref_axis',(1.,0.,0.));
#91109=DIRECTION('',(-0.190809912898503,0.,0.981627005099017));
#91110=DIRECTION('center_axis',(0.,1.,0.));
#91111=DIRECTION('ref_axis',(-0.547202057128739,0.,0.837000542815879));
#91112=DIRECTION('center_axis',(0.,1.,0.));
#91113=DIRECTION('ref_axis',(-0.540624705795703,0.,0.841263886948269));
#91114=DIRECTION('center_axis',(-0.981627005099017,0.,-0.190809912898503));
#91115=DIRECTION('ref_axis',(-0.190809912898503,0.,0.981627005099017));
#91116=DIRECTION('center_axis',(-0.981627005099017,-3.67579694363753E-17,
-0.190809912898504));
#91117=DIRECTION('ref_axis',(-0.190139829212612,0.0837331502869717,0.97817974058453));
#91118=DIRECTION('center_axis',(-0.981627005099017,-2.06792872181471E-18,
-0.190809912898503));
#91119=DIRECTION('ref_axis',(-0.190169103834306,0.081886803424733,0.978330344705578));
#91120=DIRECTION('center_axis',(0.,-1.,0.));
#91121=DIRECTION('ref_axis',(0.,0.,-1.));
#91122=DIRECTION('',(-0.190809912898503,0.,0.981627005099017));
#91123=DIRECTION('center_axis',(0.,-1.,0.));
#91124=DIRECTION('ref_axis',(-0.518972960090495,0.,0.854790656649281));
#91125=DIRECTION('',(-0.190809912898503,0.,0.981627005099017));
#91126=DIRECTION('center_axis',(0.,-1.,0.));
#91127=DIRECTION('ref_axis',(-0.512840213950635,0.,0.858484079616545));
#91128=DIRECTION('center_axis',(0.981627005099017,0.,0.190809912898503));
#91129=DIRECTION('ref_axis',(0.,-1.,0.));
#91130=DIRECTION('',(-0.190809912898493,0.,0.981627005099019));
#91131=DIRECTION('center_axis',(0.981627005099017,1.34741882682623E-16,
0.190809912898504));
#91132=DIRECTION('ref_axis',(-0.187483678682097,0.185904529878394,0.964515098896083));
#91133=DIRECTION('center_axis',(0.981627005099017,4.03166347002478E-17,
0.190809912898503));
#91134=DIRECTION('ref_axis',(-0.187626296241583,0.181909672748906,0.965248798973121));
#91135=DIRECTION('center_axis',(0.,1.,0.));
#91136=DIRECTION('ref_axis',(1.,0.,0.));
#91137=DIRECTION('',(-0.190809912898503,0.,0.981627005099017));
#91138=DIRECTION('center_axis',(0.,1.,0.));
#91139=DIRECTION('ref_axis',(-0.550424059915763,0.,0.834885234188417));
#91140=DIRECTION('center_axis',(0.,1.,0.));
#91141=DIRECTION('ref_axis',(-0.543668385334357,0.,0.839300117233361));
#91142=DIRECTION('center_axis',(-0.981627005099017,0.,-0.190809912898503));
#91143=DIRECTION('ref_axis',(-0.190809912898503,0.,0.981627005099017));
#91144=DIRECTION('center_axis',(-0.981627005099017,-5.18936039101769E-17,
-0.190809912898504));
#91145=DIRECTION('ref_axis',(-0.188548237998538,0.153510775526106,0.969991754472696));
#91146=DIRECTION('center_axis',(-0.981627005099017,-1.61298440301547E-16,
-0.190809912898504));
#91147=DIRECTION('ref_axis',(-0.188647445377018,0.150125806278706,0.970502129643152));
#91148=DIRECTION('center_axis',(0.,-1.,0.));
#91149=DIRECTION('ref_axis',(0.,0.,-1.));
#91150=DIRECTION('',(-0.190809912898503,0.,0.981627005099017));
#91151=DIRECTION('center_axis',(0.,-1.,0.));
#91152=DIRECTION('ref_axis',(-0.522673585683894,0.,0.85253288665502));
#91153=DIRECTION('',(-0.190809912898503,0.,0.981627005099017));
#91154=DIRECTION('center_axis',(0.,-1.,0.));
#91155=DIRECTION('ref_axis',(-0.516333108288111,0.,0.856387833452541));
#91156=DIRECTION('center_axis',(0.981627005099017,0.,0.190809912898503));
#91157=DIRECTION('ref_axis',(0.,-1.,0.));
#91158=DIRECTION('',(-0.190809912898503,0.,0.981627005099017));
#91159=DIRECTION('center_axis',(0.981627005099017,2.18955559359263E-16,
0.190809912898504));
#91160=DIRECTION('ref_axis',(-0.184514106387807,0.254758059462899,0.949238050060472));
#91161=DIRECTION('center_axis',(0.981627005099017,1.20949904100743E-16,
0.190809912898504));
#91162=DIRECTION('ref_axis',(-0.184786143359668,0.249283625618896,0.950637551972653));
#91163=DIRECTION('center_axis',(0.,1.,0.));
#91164=DIRECTION('ref_axis',(1.,0.,0.));
#91165=DIRECTION('',(-0.190809912898514,0.,0.981627005099015));
#91166=DIRECTION('center_axis',(0.,1.,0.));
#91167=DIRECTION('ref_axis',(-0.555272217382648,0.,0.831668662751553));
#91168=DIRECTION('center_axis',(0.,1.,0.));
#91169=DIRECTION('ref_axis',(-0.548242331478566,0.,0.836319523851348));
#91170=DIRECTION('center_axis',(-0.981627005099017,0.,-0.190809912898503));
#91171=DIRECTION('ref_axis',(-0.190809912898503,0.,0.981627005099017));
#91172=DIRECTION('center_axis',(-0.981627005099017,-5.18936039101769E-17,
-0.190809912898504));
#91173=DIRECTION('ref_axis',(-0.185992425315799,0.223288400765293,0.956843303686045));
#91174=DIRECTION('center_axis',(-0.981627005099017,-8.27171488725884E-17,
-0.190809912898504));
#91175=DIRECTION('ref_axis',(-0.186205137201712,0.218364809132596,0.957937606012091));
#91176=DIRECTION('center_axis',(0.,-1.,0.));
#91177=DIRECTION('ref_axis',(0.,0.,-1.));
#91178=DIRECTION('',(-0.190809912898503,0.,0.981627005099017));
#91179=DIRECTION('center_axis',(0.,-1.,0.));
#91180=DIRECTION('ref_axis',(-0.527956416002256,0.,0.849271465905957));
#91181=DIRECTION('',(-0.190809912898503,0.,0.981627005099017));
#91182=DIRECTION('center_axis',(0.,-1.,0.));
#91183=DIRECTION('ref_axis',(-0.521311526714744,0.,0.853366446559942));
#91184=DIRECTION('center_axis',(0.981627005099017,0.,0.190809912898503));
#91185=DIRECTION('ref_axis',(0.,-1.,0.));
#91186=DIRECTION('',(-0.190809912898503,0.,0.981627005099017));
#91187=DIRECTION('center_axis',(0.981627005099017,7.57923090089757E-17,
0.190809912898503));
#91188=DIRECTION('ref_axis',(-0.180542433838233,0.323611589047495,0.928805668058675));
#91189=DIRECTION('center_axis',(0.981627005099017,1.93519846561189E-16,
0.190809912898504));
#91190=DIRECTION('ref_axis',(-0.180990819330081,0.316657578488792,0.931112399930234));
#91191=DIRECTION('center_axis',(0.,1.,0.));
#91192=DIRECTION('ref_axis',(1.,0.,0.));
#91193=DIRECTION('',(-0.190809912898503,0.,0.981627005099017));
#91194=DIRECTION('center_axis',(0.,1.,0.));
#91195=DIRECTION('ref_axis',(-0.561946648451831,0.,0.827173478959374));
#91196=DIRECTION('center_axis',(0.,1.,0.));
#91197=DIRECTION('ref_axis',(-0.554527554446219,0.,0.83216536298977));
#91198=DIRECTION('center_axis',(-0.981627005099017,0.,-0.190809912898503));
#91199=DIRECTION('ref_axis',(-0.190809912898503,0.,0.981627005099017));
#91200=DIRECTION('center_axis',(-0.981627005099017,1.29734009775442E-16,
-0.190809912898503));
#91201=DIRECTION('ref_axis',(-0.182431870353022,0.293066026004411,0.938525927761977));
#91202=DIRECTION('center_axis',(-0.981627005099017,-4.13585744362942E-17,
-0.190809912898503));
#91203=DIRECTION('ref_axis',(-0.18280528294402,0.286603811986498,0.940446959420128));
#91204=DIRECTION('center_axis',(0.,-1.,0.));
#91205=DIRECTION('ref_axis',(0.,0.,-1.));
#91206=DIRECTION('',(-0.190809912898503,0.,0.981627005099017));
#91207=DIRECTION('center_axis',(0.,-1.,0.));
#91208=DIRECTION('ref_axis',(-0.53504944924277,0.,0.844820742444815));
#91209=DIRECTION('',(-0.190809912898503,0.,0.981627005099017));
#91210=DIRECTION('center_axis',(0.,-1.,0.));
#91211=DIRECTION('ref_axis',(-0.52798109669905,0.,0.849256122455687));
#91212=DIRECTION('center_axis',(0.981627005099017,0.,0.190809912898503));
#91213=DIRECTION('ref_axis',(0.,-1.,0.));
#91214=DIRECTION('',(-0.190809912898503,0.,0.981627005099017));
#91215=DIRECTION('center_axis',(0.981627005099017,1.26320515014959E-16,
0.190809912898504));
#91216=DIRECTION('ref_axis',(-0.175500640034728,0.392465118632079,0.902868016935205));
#91217=DIRECTION('center_axis',(0.981627005099017,-8.06332694004955E-17,
0.190809912898503));
#91218=DIRECTION('ref_axis',(-0.176178604698278,0.38403153135881,0.906355825362631));
#91219=DIRECTION('center_axis',(0.,1.,0.));
#91220=DIRECTION('ref_axis',(1.,0.,0.));
#91221=DIRECTION('',(-0.190809912898503,0.,0.981627005099017));
#91222=DIRECTION('center_axis',(0.,1.,0.));
#91223=DIRECTION('ref_axis',(-0.570747207818219,0.,0.821125827609695));
#91224=DIRECTION('center_axis',(0.,1.,0.));
#91225=DIRECTION('ref_axis',(-0.562793888599892,0.,0.826597265271676));
#91226=DIRECTION('center_axis',(-0.981627005099017,0.,-0.190809912898503));
#91227=DIRECTION('ref_axis',(-0.190809912898503,0.,0.981627005099017));
#91228=DIRECTION('center_axis',(-0.981627005099017,-1.5568081173053E-16,
-0.190809912898504));
#91229=DIRECTION('ref_axis',(-0.177806223707996,0.362843651243595,0.914729157490302));
#91230=DIRECTION('center_axis',(-0.981627005099017,3.30868595490354E-17,
-0.190809912898503));
#91231=DIRECTION('ref_axis',(-0.178393143654898,0.3548428148405,0.917748583792421));
#91232=DIRECTION('center_axis',(-0.190809912898503,0.,0.981627005099017));
#91233=DIRECTION('ref_axis',(0.,1.,0.));
#91234=DIRECTION('',(-0.981627005099017,0.,-0.190809912898503));
#91235=DIRECTION('',(0.,-1.,0.));
#91236=DIRECTION('center_axis',(0.190809912898504,-4.66258336702978E-16,
-0.981627005099017));
#91237=DIRECTION('ref_axis',(-0.652240394658444,0.747334233647181,-0.12678332222646));
#91238=DIRECTION('center_axis',(0.,-1.,0.));
#91239=DIRECTION('ref_axis',(0.,0.,-1.));
#91240=DIRECTION('',(-0.190809912898503,0.,0.981627005099017));
#91241=DIRECTION('center_axis',(0.,-1.,0.));
#91242=DIRECTION('ref_axis',(-0.544290275892155,0.,0.838896951698623));
#91243=DIRECTION('',(-0.190809912898503,0.,0.981627005099017));
#91244=DIRECTION('center_axis',(0.,-1.,0.));
#91245=DIRECTION('ref_axis',(-0.536644442339821,0.,0.843808475014196));
#91246=DIRECTION('center_axis',(0.981627005099017,0.,0.190809912898503));
#91247=DIRECTION('ref_axis',(0.,-1.,0.));
#91248=DIRECTION('',(-0.190809912898503,0.,0.981627005099017));
#91249=DIRECTION('center_axis',(0.981627005099017,3.36854706706558E-17,
0.190809912898503));
#91250=DIRECTION('ref_axis',(-0.169293142699848,0.461318648216628,0.870933370954628));
#91251=DIRECTION('center_axis',(0.981627005099017,1.61266538800991E-16,
0.190809912898504));
#91252=DIRECTION('ref_axis',(-0.17026329901866,0.451405484228805,0.875924367634238));
#91253=DIRECTION('center_axis',(0.,1.,0.));
#91254=DIRECTION('ref_axis',(1.,0.,0.));
#91255=DIRECTION('',(-0.190809912898503,0.,0.981627005099017));
#91256=DIRECTION('center_axis',(0.,1.,0.));
#91257=DIRECTION('ref_axis',(-0.568943506648922,0.,0.822376608520712));
#91258=DIRECTION('center_axis',(0.,1.,0.));
#91259=DIRECTION('ref_axis',(-0.573435895591197,0.,0.819250434023395));
#91260=DIRECTION('center_axis',(-0.981627005099017,0.,-0.190809912898503));
#91261=DIRECTION('ref_axis',(-0.190809912898503,0.,0.981627005099017));
#91262=DIRECTION('center_axis',(-0.981627005099017,-7.78404058652653E-17,
-0.190809912898503));
#91263=DIRECTION('ref_axis',(-0.172029590132755,0.432621276482712,0.885011102333313));
#91264=DIRECTION('center_axis',(-0.981627005099017,-2.8951002105406E-16,
-0.190809912898504));
#91265=DIRECTION('ref_axis',(-0.172891236946279,0.423081817694416,0.889443868787443));
#91266=DIRECTION('center_axis',(0.,-1.,0.));
#91267=DIRECTION('ref_axis',(0.,0.,-1.));
#91268=DIRECTION('',(-0.190809912898503,1.036699112927E-14,0.981627005099017));
#91269=DIRECTION('center_axis',(0.,-1.,0.));
#91270=DIRECTION('ref_axis',(-0.479837164377971,0.,0.877357564326944));
#91271=DIRECTION('',(-0.190809912898503,0.,0.981627005099017));
#91272=DIRECTION('center_axis',(0.,-1.,0.));
#91273=DIRECTION('ref_axis',(-0.473524725918971,0.,0.880780525411049));
#91274=DIRECTION('center_axis',(0.981627005099017,0.,0.190809912898503));
#91275=DIRECTION('ref_axis',(0.,-1.,0.));
#91276=DIRECTION('',(-0.190809912898503,0.,0.981627005099017));
#91277=DIRECTION('center_axis',(0.981627005099017,3.86629460097736E-16,
0.190809912898504));
#91278=DIRECTION('ref_axis',(-0.170286389349438,0.451166192838008,0.87604315649538));
#91279=DIRECTION('center_axis',(0.981627005099017,-2.31798761009061E-16,
0.190809912898503));
#91280=DIRECTION('ref_axis',(-0.17117061747492,0.44188028378381,0.880592093148919));
#91281=DIRECTION('center_axis',(0.,1.,0.));
#91282=DIRECTION('ref_axis',(1.,0.,0.));
#91283=DIRECTION('',(-0.190809912898503,0.,0.981627005099017));
#91284=DIRECTION('center_axis',(0.,1.,0.));
#91285=DIRECTION('ref_axis',(-0.517300722376421,0.,0.855803693979427));
#91286=DIRECTION('center_axis',(0.,1.,0.));
#91287=DIRECTION('ref_axis',(-0.509981045434312,0.,0.860185638858105));
#91288=DIRECTION('center_axis',(-0.981627005099017,0.,-0.190809912898503));
#91289=DIRECTION('ref_axis',(-0.190809912898503,0.,0.981627005099017));
#91290=DIRECTION('center_axis',(-0.981627005099017,1.64489301320048E-17,
-0.190809912898503));
#91291=DIRECTION('ref_axis',(-0.172998862914491,0.421871719792196,0.889997553631395));
#91292=DIRECTION('center_axis',(-0.981627005099017,0.,-0.190809912898503));
#91293=DIRECTION('ref_axis',(-0.173775507771522,0.413011554259003,0.893993025111109));
#91294=DIRECTION('center_axis',(0.,-1.,0.));
#91295=DIRECTION('ref_axis',(0.,0.,-1.));
#91296=DIRECTION('',(-0.190809912898503,0.,0.981627005099017));
#91297=DIRECTION('center_axis',(0.,-1.,0.));
#91298=DIRECTION('ref_axis',(-0.414281988925668,0.,0.910148577789249));
#91299=DIRECTION('',(-0.190809912898503,0.,0.981627005099017));
#91300=DIRECTION('center_axis',(0.,-1.,0.));
#91301=DIRECTION('ref_axis',(-0.409359365296299,0.,0.912373229574504));
#91302=DIRECTION('center_axis',(0.981627005099017,0.,0.190809912898503));
#91303=DIRECTION('ref_axis',(0.,-1.,0.));
#91304=DIRECTION('',(-0.190809912898503,0.,0.981627005099017));
#91305=DIRECTION('center_axis',(0.981627005099017,-9.34373521491282E-17,
0.190809912898503));
#91306=DIRECTION('ref_axis',(-0.171009768890973,0.443587536078797,0.879764603049814));
#91307=DIRECTION('center_axis',(0.981627005099017,1.94463727090204E-16,
0.190809912898504));
#91308=DIRECTION('ref_axis',(-0.171833841098054,0.434752737274877,0.884004065876108));
#91309=DIRECTION('center_axis',(0.,1.,0.));
#91310=DIRECTION('ref_axis',(1.,0.,0.));
#91311=DIRECTION('',(-0.190809912898503,0.,0.981627005099017));
#91312=DIRECTION('center_axis',(0.,1.,0.));
#91313=DIRECTION('ref_axis',(-0.451295175740691,0.,0.892374733143638));
#91314=DIRECTION('center_axis',(0.,1.,0.));
#91315=DIRECTION('ref_axis',(-0.445400813995018,0.,0.895331287788255));
#91316=DIRECTION('center_axis',(-0.981627005099017,0.,-0.190809912898503));
#91317=DIRECTION('ref_axis',(-0.190809912898503,0.,0.981627005099017));
#91318=DIRECTION('center_axis',(-0.981627005099017,-3.32200097218626E-16,
-0.190809912898504));
#91319=DIRECTION('ref_axis',(-0.173714529564319,0.413715522361311,0.893679320995823));
#91320=DIRECTION('center_axis',(-0.981627005099017,-1.67043077322241E-16,
-0.190809912898504));
#91321=DIRECTION('ref_axis',(-0.174431144456715,0.405349352773424,0.897365966621025));
#91322=DIRECTION('center_axis',(0.,-1.,0.));
#91323=DIRECTION('ref_axis',(0.,0.,-1.));
#91324=DIRECTION('',(-0.190809912898503,0.,0.981627005099017));
#91325=DIRECTION('center_axis',(0.,-1.,0.));
#91326=DIRECTION('ref_axis',(-0.347690702172142,0.,0.937609287295643));
#91327=DIRECTION('',(-0.190809912898503,0.,0.981627005099017));
#91328=DIRECTION('center_axis',(0.,-1.,0.));
#91329=DIRECTION('ref_axis',(-0.344208002633843,0.,0.938893418297743));
#91330=DIRECTION('center_axis',(0.981627005099017,0.,0.190809912898503));
#91331=DIRECTION('ref_axis',(0.,-1.,0.));
#91332=DIRECTION('',(-0.190809912898503,0.,0.981627005099017));
#91333=DIRECTION('center_axis',(0.981627005099017,-7.5998920345386E-17,
0.190809912898503));
#91334=DIRECTION('ref_axis',(-0.171510885743259,0.43824140554361,0.882342612899731));
#91335=DIRECTION('center_axis',(0.981627005099017,2.77669091834731E-16,
0.190809912898504));
#91336=DIRECTION('ref_axis',(-0.172294487675883,0.429716142106888,0.886373875252017));
#91337=DIRECTION('center_axis',(0.,1.,0.));
#91338=DIRECTION('ref_axis',(1.,0.,0.));
#91339=DIRECTION('',(-0.190809912898503,0.,0.981627005099017));
#91340=DIRECTION('center_axis',(0.,1.,0.));
#91341=DIRECTION('ref_axis',(-0.384183769154313,0.,0.923256644448544));
#91342=DIRECTION('center_axis',(0.,1.,0.));
#91343=DIRECTION('ref_axis',(-0.379771576195477,0.,0.9250802937659));
#91344=DIRECTION('center_axis',(-0.981627005099017,0.,-0.190809912898503));
#91345=DIRECTION('ref_axis',(-0.190809912898503,0.,0.981627005099017));
#91346=DIRECTION('center_axis',(-0.981627005099017,-3.53451119958106E-16,
-0.190809912898504));
#91347=DIRECTION('ref_axis',(-0.174225841498191,0.40776725581042,0.896309779731922));
#91348=DIRECTION('center_axis',(-0.981627005099017,-2.95381654173833E-17,
-0.190809912898503));
#91349=DIRECTION('ref_axis',(-0.174900994791868,0.399749884313687,0.899783124987354));
#91350=DIRECTION('center_axis',(0.,-1.,0.));
#91351=DIRECTION('ref_axis',(0.,0.,-1.));
#91352=DIRECTION('',(-0.190809912898503,0.,0.981627005099017));
#91353=DIRECTION('center_axis',(0.,-1.,0.));
#91354=DIRECTION('ref_axis',(-0.280107790543359,0.,0.959968554525052));
#91355=DIRECTION('',(-0.190809912898503,0.,0.981627005099017));
#91356=DIRECTION('center_axis',(0.,-1.,0.));
#91357=DIRECTION('ref_axis',(-0.278111038185117,0.,0.960548931829918));
#91358=DIRECTION('center_axis',(0.981627005099017,0.,0.190809912898503));
#91359=DIRECTION('ref_axis',(0.,-1.,0.));
#91360=DIRECTION('',(-0.190809912898503,0.,0.981627005099017));
#91361=DIRECTION('center_axis',(0.981627005099017,4.1913834659201E-16,0.190809912898504));
#91362=DIRECTION('ref_axis',(-0.171819814047587,0.434904980194897,0.883931903317404));
#91363=DIRECTION('center_axis',(0.981627005099017,7.20045220031795E-17,
0.190809912898503));
#91364=DIRECTION('ref_axis',(-0.172578958352769,0.426569286306185,0.887837342712113));
#91365=DIRECTION('center_axis',(0.,1.,0.));
#91366=DIRECTION('ref_axis',(1.,0.,0.));
#91367=DIRECTION('',(-0.190809912898503,0.,0.981627005099017));
#91368=DIRECTION('center_axis',(0.,1.,0.));
#91369=DIRECTION('ref_axis',(-0.31602509005927,0.,0.948750832649453));
#91370=DIRECTION('center_axis',(0.,1.,0.));
#91371=DIRECTION('ref_axis',(-0.313146253749265,0.,0.949704914045832));
#91372=DIRECTION('center_axis',(-0.981627005099017,0.,-0.190809912898503));
#91373=DIRECTION('ref_axis',(-0.190809912898503,0.,0.981627005099017));
#91374=DIRECTION('center_axis',(-0.981627005099017,-1.20541050910893E-16,
-0.190809912898504));
#91375=DIRECTION('ref_axis',(-0.174564455395936,0.403770028651194,0.898051788526327));
#91376=DIRECTION('center_axis',(-0.981627005099017,-5.79678245784151E-17,
-0.190809912898503));
#91377=DIRECTION('ref_axis',(-0.175212807608716,0.395981677383196,0.90138725486145));
#91378=DIRECTION('center_axis',(0.,-1.,0.));
#91379=DIRECTION('ref_axis',(0.,0.,-1.));
#91380=DIRECTION('',(-0.190809912898503,1.086578613169E-14,0.981627005099017));
#91381=DIRECTION('center_axis',(0.,-1.,0.));
#91382=DIRECTION('ref_axis',(-0.211560193439188,0.,0.977364969984076));
#91383=DIRECTION('',(-0.190809912898503,0.,0.981627005099017));
#91384=DIRECTION('center_axis',(0.,-1.,0.));
#91385=DIRECTION('ref_axis',(-0.211093004899912,0.,0.977465980626603));
#91386=DIRECTION('center_axis',(0.981627005099017,0.,0.190809912898503));
#91387=DIRECTION('ref_axis',(0.,-1.,0.));
#91388=DIRECTION('',(-0.190809912898503,0.,0.981627005099017));
#91389=DIRECTION('center_axis',(0.981627005099017,-1.4868986789408E-17,
0.190809912898503));
#91390=DIRECTION('ref_axis',(-0.171953954276685,0.433446386204417,0.884621991527988));
#91391=DIRECTION('center_axis',(0.981627005099017,0.,0.190809912898503));
#91392=DIRECTION('ref_axis',(-0.172702595687313,0.425192701759105,0.888473398483971));
#91393=DIRECTION('center_axis',(0.,1.,0.));
#91394=DIRECTION('ref_axis',(1.,0.,0.));
#91395=DIRECTION('',(-0.190809912898503,0.,0.981627005099017));
#91396=DIRECTION('center_axis',(0.,1.,0.));
#91397=DIRECTION('ref_axis',(-0.24685697062186,0.,0.969051926397857));
#91398=DIRECTION('center_axis',(0.,1.,0.));
#91399=DIRECTION('ref_axis',(-0.245559147376533,0.,0.969381609656233));
#91400=DIRECTION('center_axis',(-0.981627005099017,0.,-0.190809912898503));
#91401=DIRECTION('ref_axis',(-0.190809912898503,0.,0.981627005099017));
#91402=DIRECTION('center_axis',(-0.981627005099017,-1.04323047313055E-16,
-0.190809912898503));
#91403=DIRECTION('ref_axis',(-0.174749786833802,0.401562082356488,0.899005231361343));
#91404=DIRECTION('center_axis',(-0.981627005099017,-1.5773858633476E-16,
-0.190809912898504));
#91405=DIRECTION('ref_axis',(-0.175383692187236,0.393898398451778,0.902266375419087));
#91406=DIRECTION('center_axis',(0.,-1.,0.));
#91407=DIRECTION('ref_axis',(0.,0.,-1.));
#91408=DIRECTION('',(-0.190809912898503,0.,0.981627005099017));
#91409=DIRECTION('center_axis',(0.,-1.,0.));
#91410=DIRECTION('ref_axis',(-0.142059493577032,0.,0.989858121290439));
#91411=DIRECTION('',(-0.190809912898503,0.,0.981627005099017));
#91412=DIRECTION('center_axis',(0.,-1.,0.));
#91413=DIRECTION('ref_axis',(-0.14316446678366,0.,0.989698911513269));
#91414=DIRECTION('center_axis',(0.981627005099017,0.,0.190809912898503));
#91415=DIRECTION('ref_axis',(0.,-1.,0.));
#91416=DIRECTION('',(-0.190809912898503,0.,0.981627005099017));
#91417=DIRECTION('center_axis',(0.981627005099017,-8.93635241303609E-17,
0.190809912898503));
#91418=DIRECTION('ref_axis',(-0.171920597703966,0.433809658482487,0.884450387694199));
#91419=DIRECTION('center_axis',(0.981627005099017,2.86623894051663E-16,
0.190809912898504));
#91420=DIRECTION('ref_axis',(-0.172671844247454,0.425535598140786,0.888315196830014));
#91421=DIRECTION('center_axis',(0.,1.,0.));
#91422=DIRECTION('ref_axis',(1.,0.,0.));
#91423=DIRECTION('',(-0.190809912898503,0.,0.981627005099017));
#91424=DIRECTION('center_axis',(0.,1.,0.));
#91425=DIRECTION('ref_axis',(-0.176699795052451,0.,0.984264792842059));
#91426=DIRECTION('center_axis',(0.,1.,0.));
#91427=DIRECTION('ref_axis',(-0.177028780540981,0.,0.984205675080251));
#91428=DIRECTION('center_axis',(-0.981627005099017,0.,-0.190809912898503));
#91429=DIRECTION('ref_axis',(-0.190809912898503,0.,0.981627005099017));
#91430=DIRECTION('center_axis',(-0.981627005099017,0.,-0.190809912898503));
#91431=DIRECTION('ref_axis',(-0.174791955489963,0.401057680016923,0.899222169208165));
#91432=DIRECTION('center_axis',(-0.981627005099017,-8.58313634584417E-17,
-0.190809912898503));
#91433=DIRECTION('ref_axis',(-0.175422595692249,0.393422293643184,0.902466515603283));
#91434=DIRECTION('center_axis',(0.,-1.,0.));
#91435=DIRECTION('ref_axis',(0.,0.,-1.));
#91436=DIRECTION('',(-0.190809912898503,0.,0.981627005099017));
#91437=DIRECTION('center_axis',(0.,-1.,0.));
#91438=DIRECTION('ref_axis',(-0.0716028171606353,0.,0.997433224118116));
#91439=DIRECTION('',(-0.190809912898503,0.,0.981627005099017));
#91440=DIRECTION('center_axis',(0.,-1.,0.));
#91441=DIRECTION('ref_axis',(-0.0743228018941379,0.,0.99723423583359));
#91442=DIRECTION('center_axis',(0.981627005099017,0.,0.190809912898503));
#91443=DIRECTION('ref_axis',(0.,-1.,0.));
#91444=DIRECTION('',(-0.190809912898503,0.,0.981627005099017));
#91445=DIRECTION('center_axis',(0.981627005099017,3.00905960538911E-17,
0.190809912898503));
#91446=DIRECTION('ref_axis',(-0.171717946000204,0.436008640726291,0.883407840260365));
#91447=DIRECTION('center_axis',(0.981627005099017,2.6048332037516E-16,0.190809912898504));
#91448=DIRECTION('ref_axis',(-0.172485113654947,0.427610544193976,0.887354556004291));
#91449=DIRECTION('center_axis',(0.,1.,0.));
#91450=DIRECTION('ref_axis',(1.,0.,0.));
#91451=DIRECTION('',(-0.190809912898503,0.,0.981627005099017));
#91452=DIRECTION('center_axis',(0.,1.,0.));
#91453=DIRECTION('ref_axis',(-0.105558169770634,0.,0.994413129838235));
#91454=DIRECTION('center_axis',(0.,1.,0.));
#91455=DIRECTION('ref_axis',(-0.107559343282833,0.,0.994198666098766));
#91456=DIRECTION('center_axis',(-0.981627005099017,0.,-0.190809912898503));
#91457=DIRECTION('ref_axis',(-0.190809912898503,0.,0.981627005099017));
#91458=DIRECTION('center_axis',(-0.981627005099017,-2.09348652609932E-16,
-0.190809912898504));
#91459=DIRECTION('ref_axis',(-0.174693214665051,0.402237588782009,0.898714194235757));
#91460=DIRECTION('center_axis',(-0.981627005099017,-1.00704279750265E-16,
-0.190809912898503));
#91461=DIRECTION('ref_axis',(-0.17533151323336,0.394535901971296,0.901997939311946));
#91462=DIRECTION('center_axis',(0.,-1.,0.));
#91463=DIRECTION('ref_axis',(0.,0.,-1.));
#91464=DIRECTION('',(-0.190809912898503,0.,0.981627005099017));
#91465=DIRECTION('center_axis',(0.,-1.,0.));
#91466=DIRECTION('ref_axis',(-0.000172612850318695,0.,0.999999985102402));
#91467=DIRECTION('',(-0.190809912898503,-1.073924094398E-14,0.981627005099017));
#91468=DIRECTION('center_axis',(0.,-1.,0.));
#91469=DIRECTION('ref_axis',(-0.00455200992318091,0.,0.99998963954916));
#91470=DIRECTION('center_axis',(0.981627005099017,0.,0.190809912898503));
#91471=DIRECTION('ref_axis',(0.,-1.,0.));
#91472=DIRECTION('',(-0.190809912898503,0.,0.981627005099017));
#91473=DIRECTION('center_axis',(0.981627005099017,-7.66548341238665E-17,
0.190809912898503));
#91474=DIRECTION('ref_axis',(-0.171334862813509,0.440128478582875,0.881437057948552));
#91475=DIRECTION('center_axis',(0.981627005099017,1.76824696986466E-16,
0.190809912898504));
#91476=DIRECTION('ref_axis',(-0.172132568081392,0.431494770724981,0.885540875308814));
#91477=DIRECTION('center_axis',(0.,1.,0.));
#91478=DIRECTION('ref_axis',(1.,0.,0.));
#91479=DIRECTION('',(-0.190809912898503,0.,0.981627005099017));
#91480=DIRECTION('center_axis',(0.,1.,0.));
#91481=DIRECTION('ref_axis',(-0.0334212901421124,0.,0.999441352639182));
#91482=DIRECTION('center_axis',(0.,1.,0.));
#91483=DIRECTION('ref_axis',(-0.0371410100073943,0.,0.999310034661731));
#91484=DIRECTION('center_axis',(-0.981627005099017,0.,-0.190809912898503));
#91485=DIRECTION('ref_axis',(-0.190809912898503,0.,0.981627005099017));
#91486=DIRECTION('center_axis',(-0.981627005099017,-1.66876344160806E-16,
-0.190809912898504));
#91487=DIRECTION('ref_axis',(-0.174448259539567,0.405147003614198,0.897454015649856));
#91488=DIRECTION('center_axis',(-0.981627005099017,5.83486426445023E-17,
-0.190809912898503));
#91489=DIRECTION('ref_axis',(-0.175105749529825,0.397280243645616,0.900836491540212));
#91490=DIRECTION('center_axis',(0.,-1.,0.));
#91491=DIRECTION('ref_axis',(0.,0.,-1.));
#91492=DIRECTION('',(-0.190809912898503,-1.312424708425E-14,0.981627005099017));
#91493=DIRECTION('center_axis',(0.,-1.,0.));
#91494=DIRECTION('ref_axis',(0.0722647313333386,0.,0.99738548646214));
#91495=DIRECTION('',(-0.190809912898503,0.,0.981627005099017));
#91496=DIRECTION('center_axis',(0.,-1.,0.));
#91497=DIRECTION('ref_axis',(0.0661784895354501,0.,0.997807800892941));
#91498=DIRECTION('center_axis',(0.981627005099017,0.,0.190809912898503));
#91499=DIRECTION('ref_axis',(0.,-1.,0.));
#91500=DIRECTION('',(-0.190809912898503,0.,0.981627005099017));
#91501=DIRECTION('center_axis',(0.981627005099017,-1.57664003463228E-17,
0.190809912898503));
#91502=DIRECTION('ref_axis',(-0.170749290996154,0.446335030525624,0.8784245671371));
#91503=DIRECTION('center_axis',(0.981627005099017,1.21097659158256E-16,
0.190809912898504));
#91504=DIRECTION('ref_axis',(-0.171594788424947,0.437338367274091,0.882774252623755));
#91505=DIRECTION('center_axis',(0.,1.,0.));
#91506=DIRECTION('ref_axis',(1.,0.,0.));
#91507=DIRECTION('',(-0.190809912898503,0.,0.981627005099017));
#91508=DIRECTION('center_axis',(0.,1.,0.));
#91509=DIRECTION('ref_axis',(0.0397379259201496,0.,0.99921013667975));
#91510=DIRECTION('center_axis',(0.,1.,0.));
#91511=DIRECTION('ref_axis',(0.034250810833452,0.,0.999413268851905));
#91512=DIRECTION('center_axis',(-0.981627005099017,0.,-0.190809912898503));
#91513=DIRECTION('ref_axis',(-0.190809912898503,0.,0.981627005099017));
#91514=DIRECTION('center_axis',(-0.981627005099017,-3.26101604930485E-16,
-0.190809912898504));
#91515=DIRECTION('ref_axis',(-0.17404349559963,0.409900460457291,0.895371696088481));
#91516=DIRECTION('center_axis',(-0.981627005099017,-1.34261283340887E-16,
-0.190809912898504));
#91517=DIRECTION('ref_axis',(-0.174733298347147,0.401759104876689,0.898920405874407));
#91518=DIRECTION('center_axis',(0.,-1.,0.));
#91519=DIRECTION('ref_axis',(0.,0.,-1.));
#91520=DIRECTION('',(-0.190809912898503,0.,0.981627005099017));
#91521=DIRECTION('center_axis',(0.,-1.,0.));
#91522=DIRECTION('ref_axis',(0.14576169806305,0.,0.98931972960099));
#91523=DIRECTION('',(-0.190809912898503,0.,0.981627005099017));
#91524=DIRECTION('center_axis',(0.,-1.,0.));
#91525=DIRECTION('ref_axis',(0.137916286966303,0.,0.990443889268558));
#91526=DIRECTION('center_axis',(0.981627005099017,0.,0.190809912898503));
#91527=DIRECTION('ref_axis',(0.,-1.,0.));
#91528=DIRECTION('',(-0.190809912898503,0.,0.981627005099017));
#91529=DIRECTION('center_axis',(0.981627005099017,1.63768969384934E-17,
0.190809912898503));
#91530=DIRECTION('ref_axis',(-0.169924896128147,0.454894312187821,0.874183444372523));
#91531=DIRECTION('center_axis',(0.981627005099017,4.70972447646461E-17,
0.190809912898503));
#91532=DIRECTION('ref_axis',(-0.170839952553044,0.445381139307003,0.878890978086173));
#91533=DIRECTION('center_axis',(0.,1.,0.));
#91534=DIRECTION('ref_axis',(1.,0.,0.));
#91535=DIRECTION('',(-0.190809912898503,0.,0.981627005099017));
#91536=DIRECTION('center_axis',(0.,1.,0.));
#91537=DIRECTION('ref_axis',(0.113965105299485,0.,0.993484753166387));
#91538=DIRECTION('center_axis',(0.,1.,0.));
#91539=DIRECTION('ref_axis',(0.10665743332964,0.,0.994295827163895));
#91540=DIRECTION('center_axis',(-0.981627005099017,0.,-0.190809912898503));
#91541=DIRECTION('ref_axis',(-0.190809912898503,0.,0.981627005099017));
#91542=DIRECTION('center_axis',(-0.981627005099017,-1.52453231653595E-16,
-0.190809912898504));
#91543=DIRECTION('ref_axis',(-0.173455071838668,0.416694818559092,0.892344533372311));
#91544=DIRECTION('center_axis',(-0.981627005099017,-2.6173755386041E-16,
-0.190809912898504));
#91545=DIRECTION('ref_axis',(-0.174193181128001,0.408150322866915,0.896141757531776));
#91546=DIRECTION('center_axis',(-0.981627005099017,0.,-0.190809912898503));
#91547=DIRECTION('ref_axis',(-0.190809912898503,0.,0.981627005099017));
#91548=DIRECTION('',(-0.190809912898503,0.,0.981627005099017));
#91549=DIRECTION('center_axis',(-0.981627005099017,6.70372400852628E-17,
-0.190809912898503));
#91550=DIRECTION('ref_axis',(-0.172645118482797,0.425833332110878,0.888177705376243));
#91551=DIRECTION('',(-0.190809912898503,0.,0.981627005099017));
#91552=DIRECTION('center_axis',(-0.981627005099017,-3.37053264169227E-16,
-0.190809912898504));
#91553=DIRECTION('ref_axis',(-0.173452293294153,0.416726584693078,0.892330239071299));
#91554=DIRECTION('center_axis',(0.,-1.,0.));
#91555=DIRECTION('ref_axis',(0.,0.,-1.));
#91556=DIRECTION('',(-0.190809912898503,0.,0.981627005099017));
#91557=DIRECTION('center_axis',(0.,-1.,0.));
#91558=DIRECTION('ref_axis',(0.22039446301111,0.,0.975410826613097));
#91559=DIRECTION('center_axis',(0.,-1.,0.));
#91560=DIRECTION('ref_axis',(0.210730120697371,0.,0.977544278399128));
#91561=DIRECTION('center_axis',(0.981627005099017,0.,0.190809912898503));
#91562=DIRECTION('ref_axis',(0.,-1.,0.));
#91563=DIRECTION('',(-0.190809912898503,0.,0.981627005099017));
#91564=DIRECTION('',(0.,1.,0.));
#91565=DIRECTION('center_axis',(0.981627005099017,4.38639578588372E-16,
0.190809912898504));
#91566=DIRECTION('ref_axis',(-0.169421882294232,0.460018699991902,0.871595675446844));
#91567=DIRECTION('center_axis',(0.981627005099017,2.79740284150959E-16,
0.190809912898504));
#91568=DIRECTION('ref_axis',(-0.169818718509315,0.455982046898394,0.873637210603008));
#91569=DIRECTION('center_axis',(0.,1.,0.));
#91570=DIRECTION('ref_axis',(1.,0.,0.));
#91571=DIRECTION('center_axis',(0.,1.,0.));
#91572=DIRECTION('ref_axis',(0.189328555217771,0.,0.981913793659684));
#91573=DIRECTION('',(-0.981627005099017,0.,-0.190809912898503));
#91574=DIRECTION('center_axis',(0.,1.,0.));
#91575=DIRECTION('ref_axis',(0.180140439134743,0.,0.983640901034693));
#91576=DIRECTION('center_axis',(-0.190809912898503,0.,0.981627005099017));
#91577=DIRECTION('ref_axis',(0.,1.,0.));
#91578=DIRECTION('center_axis',(0.190809912898503,-1.0490812575817E-16,
-0.981627005099017));
#91579=DIRECTION('ref_axis',(0.629209430370232,0.767552346417929,0.122306533928078));
#91580=DIRECTION('center_axis',(-0.981627005099017,0.,-0.190809912898503));
#91581=DIRECTION('ref_axis',(-0.190809912898503,0.,0.981627005099017));
#91582=DIRECTION('',(-0.190809912898503,0.,0.981627005099017));
#91583=DIRECTION('center_axis',(-0.981627005099017,1.77118070983608E-17,
-0.190809912898503));
#91584=DIRECTION('ref_axis',(-0.17748337255926,0.367159421047011,0.913068240604948));
#91585=DIRECTION('',(-0.190809912898503,0.,0.981627005099017));
#91586=DIRECTION('center_axis',(-0.981627005099017,-5.92257891558324E-17,
-0.190809912898503));
#91587=DIRECTION('ref_axis',(-0.178099143471772,0.358876189925692,0.916236091517377));
#91588=DIRECTION('center_axis',(0.,-1.,0.));
#91589=DIRECTION('ref_axis',(0.,0.,-1.));
#91590=DIRECTION('',(-0.190809912898503,0.,0.981627005099017));
#91591=DIRECTION('center_axis',(0.,-1.,0.));
#91592=DIRECTION('ref_axis',(0.282313487580406,0.,0.959322205898617));
#91593=DIRECTION('center_axis',(0.,-1.,0.));
#91594=DIRECTION('ref_axis',(0.27169297752195,0.,0.962383980521942));
#91595=DIRECTION('center_axis',(0.981627005099017,0.,0.190809912898503));
#91596=DIRECTION('ref_axis',(0.,-1.,0.));
#91597=DIRECTION('',(-0.190809912898503,0.,0.981627005099017));
#91598=DIRECTION('',(0.,1.,0.));
#91599=DIRECTION('center_axis',(0.981627005099017,2.74504066559155E-17,
0.190809912898503));
#91600=DIRECTION('ref_axis',(-0.174748898384523,0.40157270146071,0.899000660708847));
#91601=DIRECTION('center_axis',(0.981627005099017,5.23739686473236E-17,
0.190809912898503));
#91602=DIRECTION('ref_axis',(-0.174916036819089,0.399569073108612,0.899860509122735));
#91603=DIRECTION('center_axis',(0.,1.,0.));
#91604=DIRECTION('ref_axis',(1.,0.,0.));
#91605=DIRECTION('center_axis',(0.,1.,0.));
#91606=DIRECTION('ref_axis',(0.251348939241017,0.,0.967896539275978));
#91607=DIRECTION('',(-0.981627005099017,0.,-0.190809912898503));
#91608=DIRECTION('center_axis',(0.,1.,0.));
#91609=DIRECTION('ref_axis',(0.241209387750856,0.,0.970473096618787));
#91610=DIRECTION('center_axis',(-0.190809912898503,0.,0.981627005099017));
#91611=DIRECTION('ref_axis',(0.,1.,0.));
#91612=DIRECTION('center_axis',(0.190809912898504,2.21472709933915E-16,
-0.981627005099017));
#91613=DIRECTION('ref_axis',(0.743449495922876,0.652992294713776,0.144512664000285));
#91614=DIRECTION('center_axis',(0.,-1.,0.));
#91615=DIRECTION('ref_axis',(0.,0.,-1.));
#91616=DIRECTION('',(-0.190809912898503,0.,0.981627005099017));
#91617=DIRECTION('center_axis',(0.,-1.,0.));
#91618=DIRECTION('ref_axis',(0.271655976778535,0.,0.962394425524431));
#91619=DIRECTION('',(-0.190809912898503,0.,0.981627005099017));
#91620=DIRECTION('center_axis',(0.,-1.,0.));
#91621=DIRECTION('ref_axis',(0.261714879697109,0.,0.965145233498631));
#91622=DIRECTION('center_axis',(0.981627005099017,0.,0.190809912898503));
#91623=DIRECTION('ref_axis',(0.,-1.,0.));
#91624=DIRECTION('',(-0.190809912898513,0.,0.981627005099015));
#91625=DIRECTION('center_axis',(0.981627005099017,3.56855286526902E-16,
0.190809912898504));
#91626=DIRECTION('ref_axis',(-0.179626317633374,0.337323436149387,0.92409268227697));
#91627=DIRECTION('center_axis',(0.981627005099017,-1.39663916392863E-16,
0.190809912898503));
#91628=DIRECTION('ref_axis',(-0.180156291552091,0.32946923572111,0.926819148123055));
#91629=DIRECTION('center_axis',(0.,1.,0.));
#91630=DIRECTION('ref_axis',(1.,0.,0.));
#91631=DIRECTION('',(-0.190809912898503,0.,0.981627005099017));
#91632=DIRECTION('center_axis',(0.,1.,0.));
#91633=DIRECTION('ref_axis',(0.24013206200696,0.,0.970740229307659));
#91634=DIRECTION('center_axis',(0.,1.,0.));
#91635=DIRECTION('ref_axis',(0.2307209198917,0.,0.973019967484906));
#91636=DIRECTION('center_axis',(-0.981627005099017,0.,-0.190809912898503));
#91637=DIRECTION('ref_axis',(-0.190809912898503,0.,0.981627005099017));
#91638=DIRECTION('center_axis',(-0.981627005099017,-3.01100720672133E-16,
-0.190809912898504));
#91639=DIRECTION('ref_axis',(-0.182226664219433,0.296551840076391,0.937470238991492));
#91640=DIRECTION('center_axis',(-0.981627005099017,-8.46082702226177E-18,
-0.190809912898503));
#91641=DIRECTION('ref_axis',(-0.182618174576295,0.289861538016888,0.939484375119089));
#91642=DIRECTION('center_axis',(0.,-1.,0.));
#91643=DIRECTION('ref_axis',(0.,0.,-1.));
#91644=DIRECTION('',(-0.190809912898503,0.,0.981627005099017));
#91645=DIRECTION('center_axis',(0.,-1.,0.));
#91646=DIRECTION('ref_axis',(0.263749234009829,0.,0.964591282128979));
#91647=DIRECTION('',(-0.190809912898503,0.,0.981627005099017));
#91648=DIRECTION('center_axis',(0.,-1.,0.));
#91649=DIRECTION('ref_axis',(0.254293746183647,0.,0.96712702922206));
#91650=DIRECTION('center_axis',(0.981627005099017,0.,0.190809912898503));
#91651=DIRECTION('ref_axis',(0.,-1.,0.));
#91652=DIRECTION('',(-0.190809912898503,0.,0.981627005099017));
#91653=DIRECTION('center_axis',(0.981627005099017,1.0065149107169E-16,0.190809912898504));
#91654=DIRECTION('ref_axis',(-0.183959150638866,0.265552492287812,0.946383064480741));
#91655=DIRECTION('center_axis',(0.981627005099017,-8.72899477455393E-18,
0.190809912898503));
#91656=DIRECTION('ref_axis',(-0.184280052602452,0.259369398333688,0.948033953727849));
#91657=DIRECTION('center_axis',(0.,1.,0.));
#91658=DIRECTION('ref_axis',(1.,0.,0.));
#91659=DIRECTION('',(-0.190809912898514,0.,0.981627005099015));
#91660=DIRECTION('center_axis',(0.,1.,0.));
#91661=DIRECTION('ref_axis',(0.231663694247404,0.,0.972795935830144));
#91662=DIRECTION('center_axis',(0.,1.,0.));
#91663=DIRECTION('ref_axis',(0.222779670595217,0.,0.974868821108505));
#91664=DIRECTION('center_axis',(-0.981627005099017,0.,-0.190809912898503));
#91665=DIRECTION('ref_axis',(-0.190809912898503,0.,0.981627005099017));
#91666=DIRECTION('center_axis',(-0.981627005099017,-2.21397588729509E-16,
-0.190809912898504));
#91667=DIRECTION('ref_axis',(-0.185875612836097,0.225944259105799,0.956242358573357));
#91668=DIRECTION('center_axis',(-0.981627005099017,-1.69216540445236E-17,
-0.190809912898503));
#91669=DIRECTION('ref_axis',(-0.186098528244237,0.220846886108093,0.957389153208709));
#91670=DIRECTION('center_axis',(0.,-1.,0.));
#91671=DIRECTION('ref_axis',(0.,0.,-1.));
#91672=DIRECTION('',(-0.190809912898503,0.,0.981627005099017));
#91673=DIRECTION('center_axis',(0.,-1.,0.));
#91674=DIRECTION('ref_axis',(0.258226029723844,0.,0.966084529206974));
#91675=DIRECTION('',(-0.190809912898503,0.,0.981627005099017));
#91676=DIRECTION('center_axis',(0.,-1.,0.));
#91677=DIRECTION('ref_axis',(0.249100565290067,0.,0.968477624094728));
#91678=DIRECTION('center_axis',(0.981627005099017,0.,0.190809912898503));
#91679=DIRECTION('ref_axis',(0.,-1.,0.));
#91680=DIRECTION('',(-0.190809912898503,0.,0.981627005099017));
#91681=DIRECTION('center_axis',(0.981627005099017,1.28101897727606E-16,
0.190809912898504));
#91682=DIRECTION('ref_axis',(-0.187193054543419,0.193781548426199,0.963019974777392));
#91683=DIRECTION('center_axis',(0.981627005099017,9.60189425200933E-17,
0.190809912898504));
#91684=DIRECTION('ref_axis',(-0.187361055560064,0.189269560946194,0.963884260769235));
#91685=DIRECTION('center_axis',(0.,1.,0.));
#91686=DIRECTION('ref_axis',(1.,0.,0.));
#91687=DIRECTION('',(-0.190809912898503,0.,0.981627005099017));
#91688=DIRECTION('center_axis',(0.,1.,0.));
#91689=DIRECTION('ref_axis',(0.22553298929724,0.,0.97423553144948));
#91690=DIRECTION('center_axis',(0.,1.,0.));
#91691=DIRECTION('ref_axis',(0.217018515201224,0.,0.976167487708875));
#91692=DIRECTION('center_axis',(-0.981627005099017,0.,-0.190809912898503));
#91693=DIRECTION('ref_axis',(-0.190809912898503,0.,0.981627005099017));
#91694=DIRECTION('center_axis',(-0.981627005099017,-2.21397588729509E-17,
-0.190809912898503));
#91695=DIRECTION('ref_axis',(-0.18849378350218,0.155336678135299,0.96971161177276));
#91696=DIRECTION('center_axis',(-0.981627005099017,-5.92257891558324E-17,
-0.190809912898504));
#91697=DIRECTION('ref_axis',(-0.188597716032453,0.151832234199303,0.970246295620545));
#91698=DIRECTION('center_axis',(0.,-1.,0.));
#91699=DIRECTION('ref_axis',(0.,0.,-1.));
#91700=DIRECTION('',(-0.190809912898503,0.,0.981627005099017));
#91701=DIRECTION('center_axis',(0.,-1.,0.));
#91702=DIRECTION('ref_axis',(0.254848902675841,0.,0.966980887507566));
#91703=DIRECTION('',(-0.190809912898503,0.,0.981627005099017));
#91704=DIRECTION('center_axis',(0.,-1.,0.));
#91705=DIRECTION('ref_axis',(0.245921538009721,0.,0.969289738490475));
#91706=DIRECTION('center_axis',(0.981627005099017,0.,0.190809912898503));
#91707=DIRECTION('ref_axis',(0.,-1.,0.));
#91708=DIRECTION('',(-0.190809912898503,0.,0.981627005099017));
#91709=DIRECTION('center_axis',(0.981627005099017,7.77761521917607E-17,
0.190809912898504));
#91710=DIRECTION('ref_axis',(-0.189384333256716,0.122010604564695,0.974293070226134));
#91711=DIRECTION('center_axis',(0.981627005099017,-2.61869843236618E-17,
0.190809912898503));
#91712=DIRECTION('ref_axis',(-0.18945018196364,0.119169723558698,0.974631830765283));
#91713=DIRECTION('center_axis',(0.,1.,0.));
#91714=DIRECTION('ref_axis',(1.,0.,0.));
#91715=DIRECTION('',(-0.190809912898503,0.,0.981627005099017));
#91716=DIRECTION('center_axis',(0.,1.,0.));
#91717=DIRECTION('ref_axis',(0.22146806454091,0.,0.975167624764329));
#91718=DIRECTION('center_axis',(0.,1.,0.));
#91719=DIRECTION('ref_axis',(0.213193096245038,0.,0.977010083731716));
#91720=DIRECTION('center_axis',(-0.981627005099017,0.,-0.190809912898503));
#91721=DIRECTION('ref_axis',(-0.190809912898503,0.,0.981627005099017));
#91722=DIRECTION('center_axis',(-0.981627005099017,-9.29869872663939E-17,
-0.190809912898504));
#91723=DIRECTION('ref_axis',(-0.190123765131721,0.0847290971646923,0.978097098465073));
#91724=DIRECTION('center_axis',(-0.981627005099017,8.46082702226177E-18,
-0.190809912898503));
#91725=DIRECTION('ref_axis',(-0.190154428082908,0.0828175822905362,0.978254844886552));
#91726=DIRECTION('center_axis',(0.,-1.,0.));
#91727=DIRECTION('ref_axis',(0.,0.,-1.));
#91728=DIRECTION('',(-0.190809912898503,0.,0.981627005099017));
#91729=DIRECTION('center_axis',(0.,-1.,0.));
#91730=DIRECTION('ref_axis',(0.253480050643459,0.,0.967340614223237));
#91731=DIRECTION('',(-0.190809912898503,0.,0.981627005099017));
#91732=DIRECTION('center_axis',(0.,-1.,0.));
#91733=DIRECTION('ref_axis',(0.244632188793599,0.,0.969615950882643));
#91734=DIRECTION('center_axis',(0.981627005099017,0.,0.190809912898503));
#91735=DIRECTION('ref_axis',(0.,-1.,0.));
#91736=DIRECTION('',(-0.190809912898503,0.,0.981627005099017));
#91737=DIRECTION('center_axis',(0.981627005099017,1.02939024959683E-17,
0.190809912898504));
#91738=DIRECTION('ref_axis',(-0.190568956404661,0.0502396607031005,0.980387397586931));
#91739=DIRECTION('center_axis',(0.981627005099017,1.30934921618309E-17,
0.190809912898504));
#91740=DIRECTION('ref_axis',(-0.190580053267881,0.0490698861712299,0.980444485714288));
#91741=DIRECTION('center_axis',(0.,1.,0.));
#91742=DIRECTION('ref_axis',(1.,0.,0.));
#91743=DIRECTION('',(-0.190809912898503,0.,0.981627005099017));
#91744=DIRECTION('center_axis',(0.,1.,0.));
#91745=DIRECTION('ref_axis',(0.219299875562532,0.,0.975657503726722));
#91746=DIRECTION('center_axis',(0.,1.,0.));
#91747=DIRECTION('ref_axis',(0.211150870270054,0.,0.977453482261022));
#91748=DIRECTION('center_axis',(-0.981627005099017,0.,-0.190809912898503));
#91749=DIRECTION('ref_axis',(-0.190809912898503,0.,0.981627005099017));
#91750=DIRECTION('center_axis',(-0.981627005099017,-4.42795177459018E-18,
-0.190809912898504));
#91751=DIRECTION('ref_axis',(-0.190790886558758,0.0141215161941199,0.981529123554926));
#91752=DIRECTION('center_axis',(-0.981627005099017,-5.81681857780497E-18,
-0.190809912898504));
#91753=DIRECTION('ref_axis',(-0.190791735395725,0.0138029303817604,0.981533490420762));
#91754=DIRECTION('center_axis',(0.,-1.,0.));
#91755=DIRECTION('ref_axis',(0.,0.,-1.));
#91756=DIRECTION('',(-0.190809912898503,0.,0.981627005099017));
#91757=DIRECTION('center_axis',(0.,-1.,0.));
#91758=DIRECTION('ref_axis',(-0.456322349908717,0.,0.88981453852687));
#91759=DIRECTION('',(-0.190809912898503,0.,0.981627005099017));
#91760=DIRECTION('center_axis',(0.,-1.,0.));
#91761=DIRECTION('ref_axis',(-0.451413722984057,0.,0.892314771087912));
#91762=DIRECTION('center_axis',(0.981627005099017,0.,0.190809912898503));
#91763=DIRECTION('ref_axis',(0.,-1.,0.));
#91764=DIRECTION('',(-0.190809912898503,0.,0.981627005099017));
#91765=DIRECTION('center_axis',(0.981627005099017,-5.03423776168928E-18,
0.190809912898503));
#91766=DIRECTION('ref_axis',(-0.190597817156863,0.0471367664159099,0.980535872544646));
#91767=DIRECTION('center_axis',(0.981627005099017,3.86331268348434E-17,
0.190809912898504));
#91768=DIRECTION('ref_axis',(-0.190606462635872,0.0461665968132409,0.980580349456445));
#91769=DIRECTION('center_axis',(0.,1.,0.));
#91770=DIRECTION('ref_axis',(1.,0.,0.));
#91771=DIRECTION('',(-0.190809912898503,0.,0.981627005099017));
#91772=DIRECTION('center_axis',(0.,1.,0.));
#91773=DIRECTION('ref_axis',(-0.486439685574001,0.,0.873714159378608));
#91774=DIRECTION('center_axis',(0.,1.,0.));
#91775=DIRECTION('ref_axis',(-0.480986849771355,0.,0.87672780858544));
#91776=DIRECTION('center_axis',(-0.981627005099017,0.,-0.190809912898503));
#91777=DIRECTION('ref_axis',(-0.190809912898503,0.,0.981627005099017));
#91778=DIRECTION('center_axis',(-0.981627005099017,-8.22446506600238E-18,
-0.190809912898504));
#91779=DIRECTION('ref_axis',(-0.190792243226586,0.0136087651545897,0.981536102971019));
#91780=DIRECTION('center_axis',(-0.981627005099017,-8.86796068167317E-18,
-0.190809912898504));
#91781=DIRECTION('ref_axis',(-0.190792977663555,0.0133229533631895,0.981539881302821));
#91782=DIRECTION('center_axis',(0.,-1.,0.));
#91783=DIRECTION('ref_axis',(0.,0.,-1.));
#91784=DIRECTION('',(-0.190809912898503,0.,0.981627005099017));
#91785=DIRECTION('center_axis',(0.,-1.,0.));
#91786=DIRECTION('ref_axis',(-0.457080350189202,0.,0.889425406355652));
#91787=DIRECTION('',(-0.190809912898503,0.,0.981627005099017));
#91788=DIRECTION('center_axis',(0.,-1.,0.));
#91789=DIRECTION('ref_axis',(-0.452130012986409,0.,0.891952045435689));
#91790=DIRECTION('center_axis',(0.981627005099017,0.,0.190809912898503));
#91791=DIRECTION('ref_axis',(0.,-1.,0.));
#91792=DIRECTION('',(-0.190809912898503,0.,0.981627005099017));
#91793=DIRECTION('center_axis',(0.981627005099017,4.02739020935142E-18,
0.190809912898503));
#91794=DIRECTION('ref_axis',(-0.189555553111424,0.114475004152895,0.975173915621627));
#91795=DIRECTION('center_axis',(0.981627005099017,3.09065014678748E-17,
0.190809912898504));
#91796=DIRECTION('ref_axis',(-0.189606818394553,0.112118877975005,0.975437651323713));
#91797=DIRECTION('center_axis',(0.,1.,0.));
#91798=DIRECTION('ref_axis',(1.,0.,0.));
#91799=DIRECTION('',(-0.190809912898503,0.,0.981627005099017));
#91800=DIRECTION('center_axis',(0.,1.,0.));
#91801=DIRECTION('ref_axis',(-0.487887564638898,0.,0.872906480827543));
#91802=DIRECTION('center_axis',(0.,1.,0.));
#91803=DIRECTION('ref_axis',(-0.482355027838568,0.,0.87597581423168));
#91804=DIRECTION('center_axis',(-0.981627005099017,0.,-0.190809912898503));
#91805=DIRECTION('ref_axis',(-0.190809912898503,0.,0.981627005099017));
#91806=DIRECTION('center_axis',(-0.981627005099017,-1.23366975990036E-17,
-0.190809912898503));
#91807=DIRECTION('ref_axis',(-0.190172770405938,0.0816525909275333,0.978349207487261));
#91808=DIRECTION('center_axis',(-0.981627005099017,-2.36478951511284E-17,
-0.190809912898504));
#91809=DIRECTION('ref_axis',(-0.190199294463509,0.0799377201791571,0.978485661253215));
#91810=DIRECTION('center_axis',(0.,-1.,0.));
#91811=DIRECTION('ref_axis',(0.,0.,-1.));
#91812=DIRECTION('',(-0.190809912898503,0.,0.981627005099017));
#91813=DIRECTION('center_axis',(0.,-1.,0.));
#91814=DIRECTION('ref_axis',(-0.458948807817462,0.,0.888462712668872));
#91815=DIRECTION('',(-0.190809912898503,0.,0.981627005099017));
#91816=DIRECTION('center_axis',(0.,-1.,0.));
#91817=DIRECTION('ref_axis',(-0.45389466954082,0.,0.891055345622498));
#91818=DIRECTION('center_axis',(0.981627005099017,0.,0.190809912898503));
#91819=DIRECTION('ref_axis',(0.,-1.,0.));
#91820=DIRECTION('',(-0.190809912898503,0.,0.981627005099017));
#91821=DIRECTION('center_axis',(0.981627005099017,3.62465118841628E-17,
0.190809912898503));
#91822=DIRECTION('ref_axis',(-0.187629699233558,0.181813241889893,0.965266305761789));
#91823=DIRECTION('center_axis',(0.981627005099017,1.93165634174218E-17,
0.190809912898503));
#91824=DIRECTION('ref_axis',(-0.187760314987319,0.178071159136799,0.965938262209102));
#91825=DIRECTION('center_axis',(0.,1.,0.));
#91826=DIRECTION('ref_axis',(1.,0.,0.));
#91827=DIRECTION('',(-0.190809912898503,0.,0.981627005099017));
#91828=DIRECTION('center_axis',(0.,1.,0.));
#91829=DIRECTION('ref_axis',(-0.490598707770679,0.,0.871385625273759));
#91830=DIRECTION('center_axis',(0.,1.,0.));
#91831=DIRECTION('ref_axis',(-0.484914894814882,0.,0.874561344210154));
#91832=DIRECTION('center_axis',(-0.981627005099017,0.,-0.190809912898503));
#91833=DIRECTION('ref_axis',(-0.190809912898503,0.,0.981627005099017));
#91834=DIRECTION('center_axis',(-0.981627005099017,-6.5795720528019E-17,
-0.190809912898504));
#91835=DIRECTION('ref_axis',(-0.188659868247639,0.149696416700501,0.970566039453171));
#91836=DIRECTION('center_axis',(-0.981627005099017,-3.94131585852141E-18,
-0.190809912898503));
#91837=DIRECTION('ref_axis',(-0.188749718337979,0.146552486995096,0.971028275789581));
#91838=DIRECTION('center_axis',(0.,-1.,0.));
#91839=DIRECTION('ref_axis',(0.,0.,-1.));
#91840=DIRECTION('',(-0.190809912898514,0.,0.981627005099015));
#91841=DIRECTION('center_axis',(0.,-1.,0.));
#91842=DIRECTION('ref_axis',(-0.461999637342515,0.,0.886880113146858));
#91843=DIRECTION('',(-0.190809912898503,0.,0.981627005099017));
#91844=DIRECTION('center_axis',(0.,-1.,0.));
#91845=DIRECTION('ref_axis',(-0.45677297861006,0.,0.889583299085416));
#91846=DIRECTION('center_axis',(0.981627005099017,0.,0.190809912898503));
#91847=DIRECTION('ref_axis',(0.,-1.,0.));
#91848=DIRECTION('',(-0.190809912898503,0.,0.981627005099017));
#91849=DIRECTION('center_axis',(0.981627005099017,1.04712145443137E-16,
0.190809912898504));
#91850=DIRECTION('ref_axis',(-0.184792632056183,0.249151479626997,0.950670933255786));
#91851=DIRECTION('center_axis',(0.981627005099017,1.54532507339374E-17,
0.190809912898503));
#91852=DIRECTION('ref_axis',(-0.185041602094931,0.244023440298493,0.951951766676773));
#91853=DIRECTION('center_axis',(0.,1.,0.));
#91854=DIRECTION('ref_axis',(1.,0.,0.));
#91855=DIRECTION('',(-0.190809912898503,0.,0.981627005099017));
#91856=DIRECTION('center_axis',(0.,1.,0.));
#91857=DIRECTION('ref_axis',(-0.494679381455157,0.,0.869075548823659));
#91858=DIRECTION('center_axis',(0.,1.,0.));
#91859=DIRECTION('ref_axis',(-0.48876283045677,0.,0.872416698352276));
#91860=DIRECTION('center_axis',(-0.981627005099017,0.,-0.190809912898503));
#91861=DIRECTION('ref_axis',(-0.190809912898503,0.,0.981627005099017));
#91862=DIRECTION('center_axis',(-0.981627005099017,-4.11223253300119E-17,
-0.190809912898503));
#91863=DIRECTION('ref_axis',(-0.186231764007846,0.217740242473403,0.958074588370942));
#91864=DIRECTION('center_axis',(-0.981627005099017,-7.88263171704282E-18,
-0.190809912898503));
#91865=DIRECTION('ref_axis',(-0.186424284899994,0.213167253811106,0.959065017557286));
#91866=DIRECTION('center_axis',(0.,-1.,0.));
#91867=DIRECTION('ref_axis',(0.,0.,-1.));
#91868=DIRECTION('',(-0.190809912898503,0.,0.981627005099017));
#91869=DIRECTION('center_axis',(0.,-1.,0.));
#91870=DIRECTION('ref_axis',(-0.466356255895842,0.,0.884596994448213));
#91871=DIRECTION('',(-0.190809912898503,0.,0.981627005099017));
#91872=DIRECTION('center_axis',(0.,-1.,0.));
#91873=DIRECTION('ref_axis',(-0.46087664993961,0.,0.887464204089631));
#91874=DIRECTION('center_axis',(0.981627005099017,0.,0.190809912898503));
#91875=DIRECTION('ref_axis',(0.,-1.,0.));
#91876=DIRECTION('',(-0.190809912898503,0.,0.981627005099017));
#91877=DIRECTION('center_axis',(0.981627005099017,2.41643412561085E-17,
0.190809912898503));
#91878=DIRECTION('ref_axis',(-0.181001508829926,0.316489717364005,0.931167392365166));
#91879=DIRECTION('center_axis',(0.981627005099017,-4.63597522018122E-17,
0.190809912898503));
#91880=DIRECTION('ref_axis',(-0.181411469998084,0.30997572146031,0.93327644921443));
#91881=DIRECTION('center_axis',(0.,1.,0.));
#91882=DIRECTION('ref_axis',(1.,0.,0.));
#91883=DIRECTION('',(-0.190809912898503,0.,0.981627005099017));
#91884=DIRECTION('center_axis',(0.,1.,0.));
#91885=DIRECTION('ref_axis',(-0.500299644059964,0.,0.865852335074217));
#91886=DIRECTION('center_axis',(0.,1.,0.));
#91887=DIRECTION('ref_axis',(-0.494052506517587,0.,0.869432067963731));
#91888=DIRECTION('center_axis',(-0.981627005099017,0.,-0.190809912898503));
#91889=DIRECTION('ref_axis',(-0.190809912898503,0.,0.981627005099017));
#91890=DIRECTION('center_axis',(-0.981627005099017,-2.30285021848067E-16,
-0.190809912898504));
#91891=DIRECTION('ref_axis',(-0.1828520022276,0.285784068246309,0.940687308098683));
#91892=DIRECTION('center_axis',(-0.981627005099017,-4.72957903022569E-17,
-0.190809912898503));
#91893=DIRECTION('ref_axis',(-0.183189642441488,0.279782020627107,0.942424307748889));
#91894=DIRECTION('center_axis',(0.,-1.,0.));
#91895=DIRECTION('ref_axis',(0.,0.,-1.));
#91896=DIRECTION('',(-0.190809912898503,0.,0.981627005099017));
#91897=DIRECTION('center_axis',(0.,-1.,0.));
#91898=DIRECTION('ref_axis',(-0.472208353495432,0.,0.881486965807852));
#91899=DIRECTION('',(-0.190809912898503,0.,0.981627005099017));
#91900=DIRECTION('center_axis',(0.,-1.,0.));
#91901=DIRECTION('ref_axis',(-0.466376613371833,0.,0.884586261762989));
#91902=DIRECTION('center_axis',(0.981627005099017,0.,0.190809912898503));
#91903=DIRECTION('ref_axis',(0.,-1.,0.));
#91904=DIRECTION('',(-0.190809912898503,0.,0.981627005099017));
#91905=DIRECTION('center_axis',(0.981627005099017,1.20821706280543E-16,
0.190809912898504));
#91906=DIRECTION('ref_axis',(-0.176194756005532,0.383827955100998,0.906438916220579));
#91907=DIRECTION('center_axis',(0.981627005099017,8.49928790366556E-17,
0.190809912898504));
#91908=DIRECTION('ref_axis',(-0.176813791054772,0.375928002622107,0.909623559576923));
#91909=DIRECTION('center_axis',(0.,1.,0.));
#91910=DIRECTION('ref_axis',(1.,0.,0.));
#91911=DIRECTION('',(-0.190809912898503,0.,0.981627005099017));
#91912=DIRECTION('center_axis',(0.,1.,0.));
#91913=DIRECTION('ref_axis',(-0.507714640295235,0.,0.861525300864624));
#91914=DIRECTION('center_axis',(0.,1.,0.));
#91915=DIRECTION('ref_axis',(-0.501013274042692,0.,0.865439598835772));
#91916=DIRECTION('center_axis',(-0.981627005099017,0.,-0.190809912898503));
#91917=DIRECTION('ref_axis',(-0.190809912898503,0.,0.981627005099017));
#91918=DIRECTION('center_axis',(-0.981627005099017,-2.79631812244081E-16,
-0.190809912898504));
#91919=DIRECTION('ref_axis',(-0.178466524218741,0.353827894019299,0.918126092182958));
#91920=DIRECTION('center_axis',(-0.981627005099017,-3.94131585852141E-17,
-0.190809912898503));
#91921=DIRECTION('ref_axis',(-0.178996506850741,0.346396787442996,0.92085260285477));
#91922=DIRECTION('center_axis',(0.,-1.,0.));
#91923=DIRECTION('ref_axis',(0.,0.,-1.));
#91924=DIRECTION('',(-0.190809912898503,0.,0.981627005099017));
#91925=DIRECTION('center_axis',(0.,-1.,0.));
#91926=DIRECTION('ref_axis',(-0.408333110934888,0.,0.912832991578545));
#91927=DIRECTION('',(-0.190809912898503,0.,0.981627005099017));
#91928=DIRECTION('center_axis',(0.,-1.,0.));
#91929=DIRECTION('ref_axis',(-0.403787833181439,0.,0.914852657958995));
#91930=DIRECTION('center_axis',(0.981627005099017,0.,0.190809912898503));
#91931=DIRECTION('ref_axis',(0.,-1.,0.));
#91932=DIRECTION('',(-0.190809912898503,0.,0.981627005099017));
#91933=DIRECTION('center_axis',(0.981627005099017,-7.78644601242735E-17,
0.190809912898503));
#91934=DIRECTION('ref_axis',(-0.176701106409977,0.377380441141686,0.909043850227917));
#91935=DIRECTION('center_axis',(0.981627005099017,1.79504978852495E-16,
0.190809912898504));
#91936=DIRECTION('ref_axis',(-0.177278780443546,0.369864269024907,0.912015710666829));
#91937=DIRECTION('center_axis',(0.,1.,0.));
#91938=DIRECTION('ref_axis',(1.,0.,0.));
#91939=DIRECTION('',(-0.190809912898503,1.064097794141E-14,0.981627005099017));
#91940=DIRECTION('center_axis',(0.,1.,0.));
#91941=DIRECTION('ref_axis',(-0.44357639185695,0.,0.896236567311985));
#91942=DIRECTION('center_axis',(0.,1.,0.));
#91943=DIRECTION('ref_axis',(-0.438183684981793,0.,0.89888545333417));
#91944=DIRECTION('center_axis',(-0.981627005099017,0.,-0.190809912898503));
#91945=DIRECTION('ref_axis',(-0.190809912898503,0.,0.981627005099017));
#91946=DIRECTION('center_axis',(-0.981627005099017,-2.76833414348855E-16,
-0.190809912898504));
#91947=DIRECTION('ref_axis',(-0.178954866317258,0.34698721230299,0.920638381950031));
#91948=DIRECTION('center_axis',(-0.981627005099017,3.03714686040439E-17,
-0.190809912898503));
#91949=DIRECTION('ref_axis',(-0.179444535603438,0.339970424906788,0.923157499471658));
#91950=DIRECTION('center_axis',(0.,-1.,0.));
#91951=DIRECTION('ref_axis',(0.,0.,-1.));
#91952=DIRECTION('',(-0.190809912898503,0.,0.981627005099017));
#91953=DIRECTION('center_axis',(0.,-1.,0.));
#91954=DIRECTION('ref_axis',(-0.343482113457155,0.,0.939159218522081));
#91955=DIRECTION('',(-0.190809912898503,0.,0.981627005099017));
#91956=DIRECTION('center_axis',(0.,-1.,0.));
#91957=DIRECTION('ref_axis',(-0.340267868241483,0.,0.940328547818472));
#91958=DIRECTION('center_axis',(0.981627005099017,0.,0.190809912898503));
#91959=DIRECTION('ref_axis',(0.,-1.,0.));
#91960=DIRECTION('',(-0.190809912898503,0.,0.981627005099017));
#91961=DIRECTION('center_axis',(0.981627005099017,-1.51997840690772E-17,
0.190809912898503));
#91962=DIRECTION('ref_axis',(-0.177052282767594,0.372832240537104,0.910850486953192));
#91963=DIRECTION('center_axis',(0.981627005099017,1.82677034101796E-16,
0.190809912898504));
#91964=DIRECTION('ref_axis',(-0.177602080516299,0.365579404478994,0.913678937054514));
#91965=DIRECTION('center_axis',(0.,1.,0.));
#91966=DIRECTION('ref_axis',(1.,0.,0.));
#91967=DIRECTION('',(-0.190809912898503,0.,0.981627005099017));
#91968=DIRECTION('center_axis',(0.,1.,0.));
#91969=DIRECTION('ref_axis',(-0.378406320814813,0.,0.925639593128663));
#91970=DIRECTION('center_axis',(0.,1.,0.));
#91971=DIRECTION('ref_axis',(-0.374371948525926,0.,0.927278622721834));
#91972=DIRECTION('center_axis',(-0.981627005099017,0.,-0.190809912898503));
#91973=DIRECTION('ref_axis',(-0.190809912898503,0.,0.981627005099017));
#91974=DIRECTION('center_axis',(-0.981627005099017,-1.69041839979963E-16,
-0.190809912898504));
#91975=DIRECTION('ref_axis',(-0.179304181042026,0.34199834358291,0.922435441452351));
#91976=DIRECTION('center_axis',(-0.981627005099017,-1.47690827086916E-17,
-0.190809912898503));
#91977=DIRECTION('ref_axis',(-0.179765955221612,0.335274096521094,0.924811051807463));
#91978=DIRECTION('center_axis',(0.,-1.,0.));
#91979=DIRECTION('ref_axis',(0.,0.,-1.));
#91980=DIRECTION('',(-0.190809912898503,0.,0.981627005099017));
#91981=DIRECTION('center_axis',(0.,-1.,0.));
#91982=DIRECTION('ref_axis',(-0.277694948631048,0.,0.960669306007431));
#91983=DIRECTION('',(-0.190809912898503,0.,0.981627005099017));
#91984=DIRECTION('center_axis',(0.,-1.,0.));
#91985=DIRECTION('ref_axis',(-0.275852862378494,0.,0.961199874280886));
#91986=DIRECTION('center_axis',(0.981627005099017,0.,0.190809912898503));
#91987=DIRECTION('ref_axis',(0.,-1.,0.));
#91988=DIRECTION('',(-0.190809912898503,0.,0.981627005099017));
#91989=DIRECTION('center_axis',(0.981627005099017,8.23307466520019E-17,
0.190809912898503));
#91990=DIRECTION('ref_axis',(-0.17726894004393,0.369993789121012,0.911965086452095));
#91991=DIRECTION('center_axis',(0.981627005099017,2.16013566009539E-17,
0.190809912898503));
#91992=DIRECTION('ref_axis',(-0.177801871146302,0.362902228648605,0.914706765613303));
#91993=DIRECTION('center_axis',(0.,1.,0.));
#91994=DIRECTION('ref_axis',(1.,0.,0.));
#91995=DIRECTION('',(-0.190809912898503,0.,0.981627005099017));
#91996=DIRECTION('center_axis',(0.,1.,0.));
#91997=DIRECTION('ref_axis',(-0.312255689172483,0.,0.949998097145156));
#91998=DIRECTION('center_axis',(0.,1.,0.));
#91999=DIRECTION('ref_axis',(-0.309624667518334,0.,0.950858856647064));
#92000=DIRECTION('center_axis',(-0.981627005099017,0.,-0.190809912898503));
#92001=DIRECTION('ref_axis',(-0.190809912898503,0.,0.981627005099017));
#92002=DIRECTION('center_axis',(-0.981627005099017,7.53381568193085E-17,
-0.190809912898503));
#92003=DIRECTION('ref_axis',(-0.179535702780267,0.338645830481712,0.92362651159684));
#92004=DIRECTION('center_axis',(-0.981627005099017,1.01443693012226E-16,
-0.190809912898503));
#92005=DIRECTION('ref_axis',(-0.179979422483989,0.332113664902088,0.925909240189141));
#92006=DIRECTION('center_axis',(0.,-1.,0.));
#92007=DIRECTION('ref_axis',(0.,0.,-1.));
#92008=DIRECTION('',(-0.190809912898503,0.,0.981627005099017));
#92009=DIRECTION('center_axis',(0.,-1.,0.));
#92010=DIRECTION('ref_axis',(-0.210995669584697,0.,0.977486996034477));
#92011=DIRECTION('',(-0.190809912898503,0.,0.981627005099017));
#92012=DIRECTION('center_axis',(0.,-1.,0.));
#92013=DIRECTION('ref_axis',(-0.21056483084966,0.,0.977579895460854));
#92014=DIRECTION('center_axis',(0.981627005099017,0.,0.190809912898503));
#92015=DIRECTION('ref_axis',(0.,-1.,0.));
#92016=DIRECTION('',(-0.190809912898503,0.,0.981627005099017));
#92017=DIRECTION('center_axis',(0.981627005099017,1.04082907525856E-16,
0.190809912898504));
#92018=DIRECTION('ref_axis',(-0.177363053987237,0.368752895726096,0.912449258300942));
#92019=DIRECTION('center_axis',(0.981627005099017,-5.72324314732877E-17,
0.190809912898503));
#92020=DIRECTION('ref_axis',(-0.177888737325384,0.361731104481622,0.91515365113367));
#92021=DIRECTION('center_axis',(0.,1.,0.));
#92022=DIRECTION('ref_axis',(1.,0.,0.));
#92023=DIRECTION('',(-0.190809912898503,0.,0.981627005099017));
#92024=DIRECTION('center_axis',(0.,1.,0.));
#92025=DIRECTION('ref_axis',(-0.245157759371825,0.,0.969483198936313));
#92026=DIRECTION('center_axis',(0.,1.,0.));
#92027=DIRECTION('ref_axis',(-0.24397218016453,0.,0.969782230867202));
#92028=DIRECTION('center_axis',(-0.981627005099017,0.,-0.190809912898503));
#92029=DIRECTION('ref_axis',(-0.190809912898503,0.,0.981627005099017));
#92030=DIRECTION('center_axis',(-0.981627005099017,-4.47098774198808E-17,
-0.190809912898503));
#92031=DIRECTION('ref_axis',(-0.179662483893508,0.336794004557109,0.924278740627307));
#92032=DIRECTION('center_axis',(-0.981627005099017,-7.16993574248911E-17,
-0.190809912898503));
#92033=DIRECTION('ref_axis',(-0.180096463940407,0.330366398701499,0.926511363279028));
#92034=DIRECTION('center_axis',(0.,-1.,0.));
#92035=DIRECTION('ref_axis',(0.,0.,-1.));
#92036=DIRECTION('',(-0.190809912898503,0.,0.981627005099017));
#92037=DIRECTION('center_axis',(0.,-1.,0.));
#92038=DIRECTION('ref_axis',(-0.143394636922443,0.,0.989665589025849));
#92039=DIRECTION('',(-0.190809912898503,0.,0.981627005099017));
#92040=DIRECTION('center_axis',(0.,-1.,0.));
#92041=DIRECTION('ref_axis',(-0.144413269309557,0.,0.989517462022437));
#92042=DIRECTION('center_axis',(0.981627005099017,0.,0.190809912898503));
#92043=DIRECTION('ref_axis',(0.,-1.,0.));
#92044=DIRECTION('',(-0.190809912898503,0.,0.981627005099017));
#92045=DIRECTION('center_axis',(0.981627005099017,3.79794977554034E-16,
0.190809912898504));
#92046=DIRECTION('ref_axis',(-0.177339648533324,0.369061948261209,0.912328848279894));
#92047=DIRECTION('center_axis',(0.981627005099017,5.73247788103327E-17,
0.190809912898503));
#92048=DIRECTION('ref_axis',(-0.177867129867076,0.36202282229889,0.915042490951975));
#92049=DIRECTION('center_axis',(0.,1.,0.));
#92050=DIRECTION('ref_axis',(1.,0.,0.));
#92051=DIRECTION('',(-0.190809912898503,0.,0.981627005099017));
#92052=DIRECTION('center_axis',(0.,1.,0.));
#92053=DIRECTION('ref_axis',(-0.177130506572721,0.,0.984187372222023));
#92054=DIRECTION('center_axis',(0.,1.,0.));
#92055=DIRECTION('ref_axis',(-0.177430914250361,0.,0.984133258592697));
#92056=DIRECTION('center_axis',(-0.981627005099017,0.,-0.190809912898503));
#92057=DIRECTION('ref_axis',(-0.190809912898503,0.,0.981627005099017));
#92058=DIRECTION('center_axis',(-0.981627005099017,-1.56091697168055E-16,
-0.190809912898504));
#92059=DIRECTION('ref_axis',(-0.179691336818671,0.336370957433608,0.924427175318595));
#92060=DIRECTION('center_axis',(-0.981627005099017,-1.85967954159957E-16,
-0.190809912898504));
#92061=DIRECTION('ref_axis',(-0.180123114853572,0.329967084990994,0.92664846965718));
#92062=DIRECTION('center_axis',(0.,-1.,0.));
#92063=DIRECTION('ref_axis',(0.,0.,-1.));
#92064=DIRECTION('',(-0.190809912898503,0.,0.981627005099017));
#92065=DIRECTION('center_axis',(0.,-1.,0.));
#92066=DIRECTION('ref_axis',(-0.0748892790042022,0.,0.997191855106243));
#92067=DIRECTION('',(-0.190809912898503,0.,0.981627005099017));
#92068=DIRECTION('center_axis',(0.,-1.,0.));
#92069=DIRECTION('ref_axis',(-0.0773958200853973,0.,0.997000444851109));
#92070=DIRECTION('center_axis',(0.981627005099017,0.,0.190809912898503));
#92071=DIRECTION('ref_axis',(0.,-1.,0.));
#92072=DIRECTION('',(-0.190809912898503,0.,0.981627005099017));
#92073=DIRECTION('center_axis',(0.981627005099017,-6.77038411212549E-17,
0.190809912898503));
#92074=DIRECTION('ref_axis',(-0.1771974842477,0.370932724200007,0.911597480083094));
#92075=DIRECTION('center_axis',(0.981627005099017,1.15770364611182E-16,
0.190809912898504));
#92076=DIRECTION('ref_axis',(-0.177735950146979,0.363788074911298,0.914367633163862));
#92077=DIRECTION('center_axis',(0.,1.,0.));
#92078=DIRECTION('ref_axis',(1.,0.,0.));
#92079=DIRECTION('',(-0.190809912898503,0.,0.981627005099017));
#92080=DIRECTION('center_axis',(0.,1.,0.));
#92081=DIRECTION('ref_axis',(-0.108177998002504,0.,0.994131540968382));
#92082=DIRECTION('center_axis',(0.,1.,0.));
#92083=DIRECTION('ref_axis',(-0.110004590107985,0.,0.993931079177613));
#92084=DIRECTION('center_axis',(-0.981627005099017,0.,-0.190809912898503));
#92085=DIRECTION('ref_axis',(-0.190809912898503,0.,0.981627005099017));
#92086=DIRECTION('center_axis',(-0.981627005099017,-3.43929929287745E-16,
-0.190809912898504));
#92087=DIRECTION('ref_axis',(-0.179623779357055,0.337360558333296,0.924079624042504));
#92088=DIRECTION('center_axis',(-0.981627005099017,-2.08601722339834E-16,
-0.190809912898504));
#92089=DIRECTION('ref_axis',(-0.180060721748086,0.330901079072703,0.926327486557578));
#92090=DIRECTION('center_axis',(0.,-1.,0.));
#92091=DIRECTION('ref_axis',(0.,0.,-1.));
#92092=DIRECTION('',(-0.190809912898503,0.,0.981627005099017));
#92093=DIRECTION('center_axis',(0.,-1.,0.));
#92094=DIRECTION('ref_axis',(-0.00546390507844353,0.,0.999985072759236));
#92095=DIRECTION('',(-0.190809912898503,0.,0.981627005099017));
#92096=DIRECTION('center_axis',(0.,-1.,0.));
#92097=DIRECTION('ref_axis',(-0.00949810829374728,0.,0.999954891952052));
#92098=DIRECTION('center_axis',(0.981627005099017,0.,0.190809912898503));
#92099=DIRECTION('ref_axis',(0.,-1.,0.));
#92100=DIRECTION('',(-0.190809912898503,0.,0.981627005099017));
#92101=DIRECTION('center_axis',(0.981627005099017,-1.07316767773413E-16,
0.190809912898503));
#92102=DIRECTION('ref_axis',(-0.176928890497236,0.374437660883914,0.910215691920986));
#92103=DIRECTION('center_axis',(0.981627005099017,1.76824696986466E-16,
0.190809912898504));
#92104=DIRECTION('ref_axis',(-0.177488407408411,0.367092566139198,0.913094142529107));
#92105=DIRECTION('center_axis',(0.,1.,0.));
#92106=DIRECTION('ref_axis',(1.,0.,0.));
#92107=DIRECTION('',(-0.190809912898503,0.,0.981627005099017));
#92108=DIRECTION('center_axis',(0.,1.,0.));
#92109=DIRECTION('ref_axis',(-0.038290696769099,0.,0.999266642363757));
#92110=DIRECTION('center_axis',(0.,1.,0.));
#92111=DIRECTION('ref_axis',(-0.0416844861317351,0.,0.999130824074572));
#92112=DIRECTION('center_axis',(-0.981627005099017,0.,-0.190809912898503));
#92113=DIRECTION('ref_axis',(-0.190809912898503,0.,0.981627005099017));
#92114=DIRECTION('center_axis',(-0.981627005099017,-7.58528837094573E-17,
-0.190809912898503));
#92115=DIRECTION('ref_axis',(-0.179456238766349,0.339800712708702,0.92321770672496));
#92116=DIRECTION('center_axis',(-0.981627005099017,-2.55275311569698E-16,
-0.190809912898504));
#92117=DIRECTION('ref_axis',(-0.179906116149876,0.333202784993083,0.925532113675544));
#92118=DIRECTION('center_axis',(0.,-1.,0.));
#92119=DIRECTION('ref_axis',(0.,0.,-1.));
#92120=DIRECTION('',(-0.190809912898503,0.,0.981627005099017));
#92121=DIRECTION('center_axis',(0.,-1.,0.));
#92122=DIRECTION('ref_axis',(0.0649114613199094,0.,0.997891027211546));
#92123=DIRECTION('',(-0.190809912898503,0.,0.981627005099017));
#92124=DIRECTION('center_axis',(0.,-1.,0.));
#92125=DIRECTION('ref_axis',(0.059307279506297,0.,0.998239774101174));
#92126=DIRECTION('center_axis',(0.981627005099017,0.,0.190809912898503));
#92127=DIRECTION('ref_axis',(0.,-1.,0.));
#92128=DIRECTION('',(-0.190809912898503,-1.06612429401E-14,0.981627005099017));
#92129=DIRECTION('center_axis',(0.981627005099017,2.36496005194842E-17,
0.190809912898503));
#92130=DIRECTION('ref_axis',(-0.17651869753264,0.379717861790502,0.908105442588376));
#92131=DIRECTION('center_axis',(0.981627005099017,-7.56860369739101E-17,
0.190809912898503));
#92132=DIRECTION('ref_axis',(-0.177111112947321,0.372063984098908,0.911153140480243));
#92133=DIRECTION('center_axis',(0.,1.,0.));
#92134=DIRECTION('ref_axis',(1.,0.,0.));
#92135=DIRECTION('',(-0.190809912898503,0.,0.981627005099017));
#92136=DIRECTION('center_axis',(0.,1.,0.));
#92137=DIRECTION('ref_axis',(0.0325552553334085,0.,0.999469937191798));
#92138=DIRECTION('center_axis',(0.,1.,0.));
#92139=DIRECTION('ref_axis',(0.0275511876846893,0.,0.999620393978216));
#92140=DIRECTION('center_axis',(-0.981627005099017,0.,-0.190809912898503));
#92141=DIRECTION('ref_axis',(-0.190809912898503,0.,0.981627005099017));
#92142=DIRECTION('center_axis',(-0.981627005099017,-2.25165393880573E-16,
-0.190809912898504));
#92143=DIRECTION('ref_axis',(-0.179179567547627,0.343787482964193,0.92179436379845));
#92144=DIRECTION('center_axis',(-0.981627005099017,-4.47537611136289E-17,
-0.190809912898503));
#92145=DIRECTION('ref_axis',(-0.179651202662149,0.336959249251399,0.924220704012833));
#92146=DIRECTION('center_axis',(0.,-1.,0.));
#92147=DIRECTION('ref_axis',(0.,0.,-1.));
#92148=DIRECTION('',(-0.190809912898503,0.,0.981627005099017));
#92149=DIRECTION('center_axis',(0.,-1.,0.));
#92150=DIRECTION('ref_axis',(0.136283439011562,0.,0.990669886617728));
#92151=DIRECTION('',(-0.190809912898503,0.,0.981627005099017));
#92152=DIRECTION('center_axis',(0.,-1.,0.));
#92153=DIRECTION('ref_axis',(0.129062849770344,0.,0.991636415632846));
#92154=DIRECTION('center_axis',(0.981627005099017,0.,0.190809912898503));
#92155=DIRECTION('ref_axis',(0.,-1.,0.));
#92156=DIRECTION('',(-0.190809912898503,0.,0.981627005099017));
#92157=DIRECTION('center_axis',(0.981627005099017,-3.27537938769868E-17,
0.190809912898503));
#92158=DIRECTION('ref_axis',(-0.175941978952378,0.386999638726905,0.905138497506081));
#92159=DIRECTION('center_axis',(0.981627005099017,-1.020440303234E-16,0.190809912898503));
#92160=DIRECTION('ref_axis',(-0.176582176327467,0.378906342395489,0.908432011047567));
#92161=DIRECTION('center_axis',(0.,1.,0.));
#92162=DIRECTION('ref_axis',(1.,0.,0.));
#92163=DIRECTION('',(-0.190809912898503,0.,0.981627005099017));
#92164=DIRECTION('center_axis',(0.,1.,0.));
#92165=DIRECTION('ref_axis',(0.104399906013785,0.,0.994535398879453));
#92166=DIRECTION('center_axis',(0.,1.,0.));
#92167=DIRECTION('ref_axis',(0.0977389164793506,0.,0.995212090061934));
#92168=DIRECTION('center_axis',(-0.981627005099017,0.,-0.190809912898503));
#92169=DIRECTION('ref_axis',(-0.190809912898503,0.,0.981627005099017));
#92170=DIRECTION('center_axis',(-0.981627005099017,-2.80834900414518E-16,
-0.190809912898504));
#92171=DIRECTION('ref_axis',(-0.178777744086074,0.349485976856103,0.919727171611467));
#92172=DIRECTION('center_axis',(-0.981627005099017,-4.31097147534792E-16,
-0.190809912898504));
#92173=DIRECTION('ref_axis',(-0.179281858024905,0.342319625630313,0.92232060005806));
#92174=DIRECTION('center_axis',(0.,-1.,0.));
#92175=DIRECTION('ref_axis',(0.,0.,-1.));
#92176=DIRECTION('',(-0.190809912898503,0.,0.981627005099017));
#92177=DIRECTION('center_axis',(0.,-1.,0.));
#92178=DIRECTION('ref_axis',(0.208719295675094,0.,0.977975590499524));
#92179=DIRECTION('',(-0.190809912898503,0.,0.981627005099017));
#92180=DIRECTION('center_axis',(0.,-1.,0.));
#92181=DIRECTION('ref_axis',(0.19982967058625,0.,0.979830650037745));
#92182=DIRECTION('center_axis',(0.981627005099017,0.,0.190809912898503));
#92183=DIRECTION('ref_axis',(0.,-1.,0.));
#92184=DIRECTION('',(-0.190809912898503,0.,0.981627005099017));
#92185=DIRECTION('center_axis',(0.981627005099017,-5.16046563045143E-17,
0.190809912898503));
#92186=DIRECTION('ref_axis',(-0.175159936094969,0.396623615588896,0.901115255860424));
#92187=DIRECTION('center_axis',(0.981627005099017,3.53789182896801E-16,
0.190809912898504));
#92188=DIRECTION('ref_axis',(-0.17586776654416,0.387925024973219,0.90475670966857));
#92189=DIRECTION('center_axis',(0.,1.,0.));
#92190=DIRECTION('ref_axis',(1.,0.,0.));
#92191=DIRECTION('',(-0.190809912898503,0.,0.981627005099017));
#92192=DIRECTION('center_axis',(0.,1.,0.));
#92193=DIRECTION('ref_axis',(0.177302870499554,0.,0.984156335199148));
#92194=DIRECTION('center_axis',(0.,1.,0.));
#92195=DIRECTION('ref_axis',(0.168932804716011,0.,0.985627570378783));
#92196=DIRECTION('center_axis',(-0.981627005099017,0.,-0.190809912898503));
#92197=DIRECTION('ref_axis',(-0.190809912898503,0.,0.981627005099017));
#92198=DIRECTION('center_axis',(-0.981627005099017,1.25694825159868E-16,
-0.190809912898503));
#92199=DIRECTION('ref_axis',(-0.178225395661155,0.357150536609089,0.916885599484071));
#92200=DIRECTION('center_axis',(-0.981627005099017,2.24702176112819E-16,
-0.190809912898503));
#92201=DIRECTION('ref_axis',(-0.178775847759892,0.349512619419995,0.919717415907683));
#92202=DIRECTION('center_axis',(0.,-1.,0.));
#92203=DIRECTION('ref_axis',(0.,0.,-1.));
#92204=DIRECTION('',(-0.190809912898503,0.,0.981627005099017));
#92205=DIRECTION('center_axis',(0.,-1.,0.));
#92206=DIRECTION('ref_axis',(0.199798691632371,0.,0.979836967470606));
#92207=DIRECTION('',(-0.190809912898503,0.,0.981627005099017));
#92208=DIRECTION('center_axis',(0.,-1.,0.));
#92209=DIRECTION('ref_axis',(0.191473403991459,0.,0.981497802118743));
#92210=DIRECTION('center_axis',(0.981627005099017,0.,0.190809912898503));
#92211=DIRECTION('ref_axis',(0.,-1.,0.));
#92212=DIRECTION('',(-0.190809912898503,0.,0.981627005099017));
#92213=DIRECTION('center_axis',(0.981627005099017,1.46213192862791E-16,
0.190809912898504));
#92214=DIRECTION('ref_axis',(-0.180317335839146,0.327040525134698,0.92764764502234));
#92215=DIRECTION('center_axis',(0.981627005099017,2.46829662486141E-17,
0.190809912898503));
#92216=DIRECTION('ref_axis',(-0.180785163765237,0.31986800304809,0.930054399047929));
#92217=DIRECTION('center_axis',(0.,1.,0.));
#92218=DIRECTION('ref_axis',(1.,0.,0.));
#92219=DIRECTION('',(-0.190809912898503,0.,0.981627005099017));
#92220=DIRECTION('center_axis',(0.,1.,0.));
#92221=DIRECTION('ref_axis',(0.168043234904274,0.,0.985779626084302));
#92222=DIRECTION('center_axis',(0.,1.,0.));
#92223=DIRECTION('ref_axis',(0.160270242051786,0.,0.987073173332485));
#92224=DIRECTION('center_axis',(-0.981627005099017,0.,-0.190809912898503));
#92225=DIRECTION('ref_axis',(-0.190809912898503,0.,0.981627005099017));
#92226=DIRECTION('center_axis',(-0.981627005099017,-9.21762051172364E-17,
-0.190809912898504));
#92227=DIRECTION('ref_axis',(-0.182698509990304,0.288467741107384,0.939897662933431));
#92228=DIRECTION('center_axis',(-0.981627005099017,-2.72852642422708E-16,
-0.190809912898504));
#92229=DIRECTION('ref_axis',(-0.183049019457732,0.282298654146891,0.941700868823225));
#92230=DIRECTION('center_axis',(0.,-1.,0.));
#92231=DIRECTION('ref_axis',(0.,0.,-1.));
#92232=DIRECTION('',(-0.190809912898514,0.,0.981627005099015));
#92233=DIRECTION('center_axis',(0.,-1.,0.));
#92234=DIRECTION('ref_axis',(0.193177433003047,0.,0.981163839212572));
#92235=DIRECTION('',(-0.190809912898503,0.,0.981627005099017));
#92236=DIRECTION('center_axis',(0.,-1.,0.));
#92237=DIRECTION('ref_axis',(0.185255825677008,0.,0.982690327139089));
#92238=DIRECTION('center_axis',(0.981627005099017,0.,0.190809912898503));
#92239=DIRECTION('ref_axis',(0.,-1.,0.));
#92240=DIRECTION('',(-0.190809912898503,0.,0.981627005099017));
#92241=DIRECTION('center_axis',(0.981627005099017,1.97817849167305E-16,
0.190809912898504));
#92242=DIRECTION('ref_axis',(-0.184377642137556,0.257457434680497,0.948536005857201));
#92243=DIRECTION('center_axis',(0.981627005099017,2.71512628734755E-16,
0.190809912898504));
#92244=DIRECTION('ref_axis',(-0.184661337429699,0.25181098112299,0.949995484328506));
#92245=DIRECTION('center_axis',(0.,1.,0.));
#92246=DIRECTION('ref_axis',(1.,0.,0.));
#92247=DIRECTION('',(-0.190809912898503,0.,0.981627005099017));
#92248=DIRECTION('center_axis',(0.,1.,0.));
#92249=DIRECTION('ref_axis',(0.161049074723182,0.,0.986946399522693));
#92250=DIRECTION('center_axis',(0.,1.,0.));
#92251=DIRECTION('ref_axis',(0.153708505209598,0.,0.988116235787183));
#92252=DIRECTION('center_axis',(-0.981627005099017,0.,-0.190809912898503));
#92253=DIRECTION('ref_axis',(-0.190809912898503,0.,0.981627005099017));
#92254=DIRECTION('center_axis',(-0.981627005099017,1.00555860127894E-16,
-0.190809912898503));
#92255=DIRECTION('ref_axis',(-0.186144295153646,0.219784945605611,0.957624602371352));
#92256=DIRECTION('center_axis',(-0.981627005099017,0.,-0.190809912898503));
#92257=DIRECTION('ref_axis',(-0.186344083339142,0.215084688873812,0.958652418354301));
#92258=DIRECTION('center_axis',(0.,-1.,0.));
#92259=DIRECTION('ref_axis',(0.,0.,-1.));
#92260=DIRECTION('',(-0.190809912898503,0.,0.981627005099017));
#92261=DIRECTION('center_axis',(0.,-1.,0.));
#92262=DIRECTION('ref_axis',(0.188550653993909,0.,0.982063465809857));
#92263=DIRECTION('',(-0.190809912898503,0.,0.981627005099017));
#92264=DIRECTION('center_axis',(0.,-1.,0.));
#92265=DIRECTION('ref_axis',(0.180903544065996,0.,0.983500842777657));
#92266=DIRECTION('center_axis',(0.981627005099017,0.,0.190809912898503));
#92267=DIRECTION('ref_axis',(0.,-1.,0.));
#92268=DIRECTION('',(-0.190809912898503,0.,0.981627005099017));
#92269=DIRECTION('center_axis',(0.981627005099017,6.45058203806429E-17,
0.190809912898504));
#92270=DIRECTION('ref_axis',(-0.18741217452723,0.187874344226309,0.964147243744704));
#92271=DIRECTION('center_axis',(0.981627005099017,7.81627264539445E-17,
0.190809912898504));
#92272=DIRECTION('ref_axis',(-0.187560853112628,0.183753959197796,0.964912124941333));
#92273=DIRECTION('center_axis',(0.,1.,0.));
#92274=DIRECTION('ref_axis',(1.,0.,0.));
#92275=DIRECTION('',(-0.190809912898503,0.,0.981627005099017));
#92276=DIRECTION('center_axis',(0.,1.,0.));
#92277=DIRECTION('ref_axis',(0.155983816576654,0.,0.987759610920684));
#92278=DIRECTION('center_axis',(0.,1.,0.));
#92279=DIRECTION('ref_axis',(0.148946583935359,0.,0.98884524326812));
#92280=DIRECTION('center_axis',(-0.981627005099017,0.,-0.190809912898503));
#92281=DIRECTION('ref_axis',(-0.190809912898503,0.,0.981627005099017));
#92282=DIRECTION('center_axis',(-0.981627005099017,5.02779300639471E-17,
-0.190809912898503));
#92283=DIRECTION('ref_axis',(-0.1886190628099,0.151102150103899,0.970356114722164));
#92284=DIRECTION('center_axis',(-0.981627005099017,8.02507771831495E-18,
-0.190809912898503));
#92285=DIRECTION('ref_axis',(-0.188712281941248,0.147870723600793,0.970835683185525));
#92286=DIRECTION('center_axis',(0.,-1.,0.));
#92287=DIRECTION('ref_axis',(0.,0.,-1.));
#92288=DIRECTION('',(-0.190809912898503,0.,0.981627005099017));
#92289=DIRECTION('center_axis',(0.,-1.,0.));
#92290=DIRECTION('ref_axis',(0.185721024850239,0.,0.982602514208353));
#92291=DIRECTION('',(-0.190809912898503,0.,0.981627005099017));
#92292=DIRECTION('center_axis',(0.,-1.,0.));
#92293=DIRECTION('ref_axis',(0.178238744550302,0.,0.983987271229223));
#92294=DIRECTION('center_axis',(0.981627005099017,0.,0.190809912898503));
#92295=DIRECTION('ref_axis',(0.,-1.,0.));
#92296=DIRECTION('',(-0.190809912898514,0.,0.981627005099015));
#92297=DIRECTION('center_axis',(0.981627005099017,-4.30038802537619E-18,
0.190809912898503));
#92298=DIRECTION('ref_axis',(-0.189470225435526,0.118291253772098,0.974734944974497));
#92299=DIRECTION('center_axis',(0.981627005099017,5.34797602053305E-17,
0.190809912898504));
#92300=DIRECTION('ref_axis',(-0.189528540527954,0.115696937272697,0.975034948620336));
#92301=DIRECTION('center_axis',(0.,1.,0.));
#92302=DIRECTION('ref_axis',(1.,0.,0.));
#92303=DIRECTION('',(-0.190809912898503,0.,0.981627005099017));
#92304=DIRECTION('center_axis',(0.,1.,0.));
#92305=DIRECTION('ref_axis',(0.152624503283608,0.,0.988284251112721));
#92306=DIRECTION('center_axis',(0.,1.,0.));
#92307=DIRECTION('ref_axis',(0.145783941845035,0.,0.98931645205168));
#92308=DIRECTION('center_axis',(-0.981627005099017,0.,-0.190809912898503));
#92309=DIRECTION('ref_axis',(-0.190809912898503,0.,0.981627005099017));
#92310=DIRECTION('center_axis',(-0.981627005099017,-2.93287925373025E-17,
-0.190809912898504));
#92311=DIRECTION('ref_axis',(-0.190160727448627,0.0824193546021032,0.978287252152036));
#92312=DIRECTION('center_axis',(-0.981627005099017,-2.00626942957873E-17,
-0.190809912898504));
#92313=DIRECTION('ref_axis',(-0.190188242024429,0.0806567583276901,0.978428801667104));
#92314=DIRECTION('center_axis',(0.,-1.,0.));
#92315=DIRECTION('ref_axis',(0.,0.,-1.));
#92316=DIRECTION('',(-0.190809912898503,0.,0.981627005099017));
#92317=DIRECTION('center_axis',(0.,-1.,0.));
#92318=DIRECTION('ref_axis',(0.184573958484037,0.,0.982818627138056));
#92319=DIRECTION('',(-0.190809912898503,0.,0.981627005099017));
#92320=DIRECTION('center_axis',(0.,-1.,0.));
#92321=DIRECTION('ref_axis',(0.177157841455015,0.,0.984182452196238));
#92322=DIRECTION('center_axis',(0.981627005099017,0.,0.190809912898503));
#92323=DIRECTION('ref_axis',(0.,-1.,0.));
#92324=DIRECTION('',(-0.190809912898503,0.,0.981627005099017));
#92325=DIRECTION('center_axis',(0.981627005099017,2.58023281522571E-17,
0.190809912898504));
#92326=DIRECTION('ref_axis',(-0.190583431643196,0.0487081633179298,0.980461865861848));
#92327=DIRECTION('center_axis',(0.981627005099017,4.2166734008049E-17,0.190809912898504));
#92328=DIRECTION('ref_axis',(-0.190593262483975,0.0476399153475881,0.980512440900874));
#92329=DIRECTION('center_axis',(0.,1.,0.));
#92330=DIRECTION('ref_axis',(1.,0.,0.));
#92331=DIRECTION('',(-0.190809912898503,0.,0.981627005099017));
#92332=DIRECTION('center_axis',(0.,1.,0.));
#92333=DIRECTION('ref_axis',(0.150832413364278,0.,0.988559347271932));
#92334=DIRECTION('center_axis',(0.,1.,0.));
#92335=DIRECTION('ref_axis',(0.144095311729787,0.,0.989563813575201));
#92336=DIRECTION('center_axis',(-0.981627005099017,0.,-0.190809912898503));
#92337=DIRECTION('ref_axis',(-0.190809912898503,0.,0.981627005099017));
#92338=DIRECTION('center_axis',(-0.981627005099017,-3.1423706289967E-18,
-0.190809912898504));
#92339=DIRECTION('ref_axis',(-0.190791909796416,0.0137365591003498,0.981534387630061));
#92340=DIRECTION('center_axis',(-0.981627005099017,-6.52037564613089E-18,
-0.190809912898504));
#92341=DIRECTION('ref_axis',(-0.190792671615323,0.0134427930546203,0.981538306829019));
#92342=DIRECTION('center_axis',(0.981627005099017,0.,0.190809912898503));
#92343=DIRECTION('ref_axis',(0.,-1.,0.));
#92344=DIRECTION('',(-0.190809912898503,0.,0.981627005099017));
#92345=DIRECTION('center_axis',(0.981627005099017,1.45995862733013E-17,
0.190809912898504));
#92346=DIRECTION('ref_axis',(-0.190604886647506,0.046344966455992,0.98057224173963));
#92347=DIRECTION('',(-0.190809912898493,0.,0.981627005099019));
#92348=DIRECTION('center_axis',(0.981627005099017,-7.47937411885398E-18,
0.190809912898503));
#92349=DIRECTION('ref_axis',(-0.19061297638741,0.0454219277749919,0.980613859635859));
#92350=DIRECTION('center_axis',(0.,1.,0.));
#92351=DIRECTION('ref_axis',(1.,0.,0.));
#92352=DIRECTION('',(-0.190809912898503,0.,0.981627005099017));
#92353=DIRECTION('center_axis',(0.,1.,0.));
#92354=DIRECTION('ref_axis',(-0.426465074644572,0.,0.904504029901691));
#92355=DIRECTION('center_axis',(0.,1.,0.));
#92356=DIRECTION('ref_axis',(-0.422083537818967,0.,0.906556940904555));
#92357=DIRECTION('center_axis',(-0.981627005099017,0.,-0.190809912898503));
#92358=DIRECTION('ref_axis',(-0.190809912898503,0.,0.981627005099017));
#92359=DIRECTION('',(-0.190809912898503,0.,0.981627005099017));
#92360=DIRECTION('center_axis',(-0.981627005099017,-1.48303614829744E-18,
-0.190809912898503));
#92361=DIRECTION('ref_axis',(-0.190792919880392,0.0133456620116604,0.981539584035705));
#92362=DIRECTION('center_axis',(-0.981627005099017,-9.01652974182553E-18,
-0.190809912898504));
#92363=DIRECTION('ref_axis',(-0.190793600227308,0.01307578557334,0.981543084099696));
#92364=DIRECTION('center_axis',(0.,-1.,0.));
#92365=DIRECTION('ref_axis',(0.,0.,-1.));
#92366=DIRECTION('center_axis',(0.,-1.,0.));
#92367=DIRECTION('ref_axis',(-0.395956002292056,0.,0.918269483457277));
#92368=DIRECTION('center_axis',(0.,-1.,0.));
#92369=DIRECTION('ref_axis',(-0.3921344237022,0.,0.919907926777318));
#92370=DIRECTION('center_axis',(0.,-1.,0.));
#92371=DIRECTION('ref_axis',(0.,0.,-1.));
#92372=DIRECTION('',(-0.190809912898503,0.,0.981627005099017));
#92373=DIRECTION('center_axis',(0.,-1.,0.));
#92374=DIRECTION('ref_axis',(-0.396546255825506,0.,0.918014742251328));
#92375=DIRECTION('',(-0.190809912898503,0.,0.981627005099017));
#92376=DIRECTION('center_axis',(0.,-1.,0.));
#92377=DIRECTION('ref_axis',(-0.39269200471537,0.,0.919670043783434));
#92378=DIRECTION('center_axis',(0.981627005099017,0.,0.190809912898503));
#92379=DIRECTION('ref_axis',(0.,-1.,0.));
#92380=DIRECTION('',(-0.190809912898503,0.,0.981627005099017));
#92381=DIRECTION('center_axis',(0.981627005099017,1.01223798161555E-16,
0.190809912898504));
#92382=DIRECTION('ref_axis',(-0.18959747408221,0.112552061393099,0.975389579244011));
#92383=DIRECTION('center_axis',(0.981627005099017,1.4958748237708E-17,0.190809912898503));
#92384=DIRECTION('ref_axis',(-0.189645435508974,0.110310396025003,0.975636318163392));
#92385=DIRECTION('center_axis',(0.,1.,0.));
#92386=DIRECTION('ref_axis',(1.,0.,0.));
#92387=DIRECTION('',(-0.190809912898503,0.,0.981627005099017));
#92388=DIRECTION('center_axis',(0.,1.,0.));
#92389=DIRECTION('ref_axis',(-0.427628772377974,0.,0.903954441902083));
#92390=DIRECTION('center_axis',(0.,1.,0.));
#92391=DIRECTION('ref_axis',(-0.423182760142292,0.,0.906044343019894));
#92392=DIRECTION('center_axis',(-0.981627005099017,0.,-0.190809912898503));
#92393=DIRECTION('ref_axis',(-0.190809912898503,0.,0.981627005099017));
#92394=DIRECTION('center_axis',(-0.981627005099017,-6.12988274629607E-17,
-0.190809912898504));
#92395=DIRECTION('ref_axis',(-0.190197207765472,0.0800739720699311,0.978474926176017));
#92396=DIRECTION('center_axis',(-0.981627005099017,-3.41679021795494E-17,
-0.190809912898504));
#92397=DIRECTION('ref_axis',(-0.190221775423882,0.0784547134400175,0.978601315191039));
#92398=DIRECTION('center_axis',(0.,-1.,0.));
#92399=DIRECTION('ref_axis',(0.,0.,-1.));
#92400=DIRECTION('',(-0.190809912898503,0.,0.981627005099017));
#92401=DIRECTION('center_axis',(0.,-1.,0.));
#92402=DIRECTION('ref_axis',(-0.398001355800204,0.,0.917384826984401));
#92403=DIRECTION('',(-0.190809912898503,0.,0.981627005099017));
#92404=DIRECTION('center_axis',(0.,-1.,0.));
#92405=DIRECTION('ref_axis',(-0.394065783747253,0.,0.919082236842636));
#92406=DIRECTION('center_axis',(0.981627005099017,0.,0.190809912898503));
#92407=DIRECTION('ref_axis',(0.,-1.,0.));
#92408=DIRECTION('',(-0.190809912898503,0.,0.981627005099017));
#92409=DIRECTION('center_axis',(0.981627005099017,2.33593380372821E-17,
0.190809912898503));
#92410=DIRECTION('ref_axis',(-0.187736511312627,0.178759156330292,0.965815803529972));
#92411=DIRECTION('center_axis',(0.981627005099017,1.60806543555361E-16,
0.190809912898504));
#92412=DIRECTION('ref_axis',(-0.18785866856038,0.1751988642749,0.966444244953379));
#92413=DIRECTION('center_axis',(0.,1.,0.));
#92414=DIRECTION('ref_axis',(1.,0.,0.));
#92415=DIRECTION('',(-0.190809912898503,0.,0.981627005099017));
#92416=DIRECTION('center_axis',(0.,1.,0.));
#92417=DIRECTION('ref_axis',(-0.429808105205998,0.,0.902920258217319));
#92418=DIRECTION('center_axis',(0.,1.,0.));
#92419=DIRECTION('ref_axis',(-0.425239687746592,0.,0.905080774276628));
#92420=DIRECTION('center_axis',(-0.981627005099017,0.,-0.190809912898503));
#92421=DIRECTION('ref_axis',(-0.190809912898503,0.,0.981627005099017));
#92422=DIRECTION('center_axis',(-0.981627005099017,-1.18642891863795E-17,
-0.190809912898503));
#92423=DIRECTION('ref_axis',(-0.188742650756643,0.146802282128194,0.970991916417078));
#92424=DIRECTION('center_axis',(-0.981627005099017,-7.59286715101097E-18,
-0.190809912898503));
#92425=DIRECTION('ref_axis',(-0.188825848790083,0.1438336413067,0.971419931058222));
#92426=DIRECTION('center_axis',(0.,-1.,0.));
#92427=DIRECTION('ref_axis',(0.,0.,-1.));
#92428=DIRECTION('',(-0.190809912898503,0.,0.981627005099017));
#92429=DIRECTION('center_axis',(0.,-1.,0.));
#92430=DIRECTION('ref_axis',(-0.400377667961243,0.,0.916350218528875));
#92431=DIRECTION('',(-0.190809912898503,0.,0.981627005099017));
#92432=DIRECTION('center_axis',(0.,-1.,0.));
#92433=DIRECTION('ref_axis',(-0.396306902290058,0.,0.918118096541648));
#92434=DIRECTION('center_axis',(0.981627005099017,0.,0.190809912898503));
#92435=DIRECTION('ref_axis',(0.,-1.,0.));
#92436=DIRECTION('',(-0.190809912898503,0.,0.981627005099017));
#92437=DIRECTION('center_axis',(0.981627005099017,2.56952718410103E-16,
0.190809912898504));
#92438=DIRECTION('ref_axis',(-0.184996241362783,0.244966251267409,0.951718407104557));
#92439=DIRECTION('center_axis',(0.981627005099017,1.34628734139372E-16,
0.190809912898504));
#92440=DIRECTION('ref_axis',(-0.185228969653602,0.240087332524911,0.952915684392978));
#92441=DIRECTION('center_axis',(0.,1.,0.));
#92442=DIRECTION('ref_axis',(1.,0.,0.));
#92443=DIRECTION('',(-0.190809912898503,0.,0.981627005099017));
#92444=DIRECTION('center_axis',(0.,1.,0.));
#92445=DIRECTION('ref_axis',(-0.4330891117883,0.,0.901351108753088));
#92446=DIRECTION('center_axis',(0.,1.,0.));
#92447=DIRECTION('ref_axis',(-0.428332303170954,0.,0.903621291283171));
#92448=DIRECTION('center_axis',(-0.981627005099017,0.,-0.190809912898503));
#92449=DIRECTION('ref_axis',(-0.190809912898503,0.,0.981627005099017));
#92450=DIRECTION('center_axis',(-0.981627005099017,-3.1638104497012E-17,
-0.190809912898503));
#92451=DIRECTION('ref_axis',(-0.186409145148707,0.213530592186508,0.958987130677679));
#92452=DIRECTION('center_axis',(-0.981627005099017,3.79643357550549E-17,
-0.190809912898503));
#92453=DIRECTION('ref_axis',(-0.186587325039356,0.209212569173405,0.959903782175339));
#92454=DIRECTION('center_axis',(0.,-1.,0.));
#92455=DIRECTION('ref_axis',(0.,0.,-1.));
#92456=DIRECTION('',(-0.190809912898503,0.,0.981627005099017));
#92457=DIRECTION('center_axis',(0.,-1.,0.));
#92458=DIRECTION('ref_axis',(-0.403771969882212,0.,0.914859659367183));
#92459=DIRECTION('',(-0.190809912898503,0.,0.981627005099017));
#92460=DIRECTION('center_axis',(0.,-1.,0.));
#92461=DIRECTION('ref_axis',(-0.399502905152937,0.,0.916731928523472));
#92462=DIRECTION('center_axis',(0.981627005099017,0.,0.190809912898503));
#92463=DIRECTION('ref_axis',(0.,-1.,0.));
#92464=DIRECTION('',(-0.190809912898503,0.,0.981627005099017));
#92465=DIRECTION('center_axis',(0.981627005099017,1.40156028223692E-16,
0.190809912898504));
#92466=DIRECTION('ref_axis',(-0.181336805679145,0.311173346204495,0.932892336509408));
#92467=DIRECTION('center_axis',(0.981627005099017,8.22731153073938E-17,
0.190809912898504));
#92468=DIRECTION('ref_axis',(-0.181719747816134,0.304975800774901,0.934862393187013));
#92469=DIRECTION('center_axis',(0.,1.,0.));
#92470=DIRECTION('ref_axis',(1.,0.,0.));
#92471=DIRECTION('',(-0.190809912898503,0.,0.981627005099017));
#92472=DIRECTION('center_axis',(0.,1.,0.));
#92473=DIRECTION('ref_axis',(-0.437609570560575,0.,0.899165092601903));
#92474=DIRECTION('center_axis',(0.,1.,0.));
#92475=DIRECTION('ref_axis',(-0.432585020225244,0.,0.901593145646486));
#92476=DIRECTION('center_axis',(-0.981627005099017,0.,-0.190809912898503));
#92477=DIRECTION('ref_axis',(-0.190809912898503,0.,0.981627005099017));
#92478=DIRECTION('center_axis',(-0.981627005099017,-2.45195309851843E-16,
-0.190809912898504));
#92479=DIRECTION('ref_axis',(-0.183163100495339,0.280258902244805,0.942287761954633));
#92480=DIRECTION('center_axis',(-0.981627005099017,1.13893007265165E-16,
-0.190809912898503));
#92481=DIRECTION('ref_axis',(-0.183475365996515,0.274591497040088,0.943894220676093));
#92482=DIRECTION('center_axis',(0.,-1.,0.));
#92483=DIRECTION('ref_axis',(0.,0.,-1.));
#92484=DIRECTION('',(-0.190809912898503,0.,0.981627005099017));
#92485=DIRECTION('center_axis',(0.,-1.,0.));
#92486=DIRECTION('ref_axis',(-0.340256652364869,0.,0.940332606326853));
#92487=DIRECTION('',(-0.190809912898503,0.,0.981627005099017));
#92488=DIRECTION('center_axis',(0.,-1.,0.));
#92489=DIRECTION('ref_axis',(-0.337238794243498,0.,0.941419139202721));
#92490=DIRECTION('center_axis',(0.981627005099017,0.,0.190809912898503));
#92491=DIRECTION('ref_axis',(0.,-1.,0.));
#92492=DIRECTION('',(-0.190809912898503,0.,0.981627005099017));
#92493=DIRECTION('center_axis',(0.981627005099017,-7.5998920345386E-18,
0.190809912898503));
#92494=DIRECTION('ref_axis',(-0.181569549045125,0.307423075530589,0.934089691352422));
#92495=DIRECTION('center_axis',(0.981627005099017,7.30708136407185E-17,
0.190809912898503));
#92496=DIRECTION('ref_axis',(-0.181934257059101,0.301442666851091,0.935965942067368));
#92497=DIRECTION('center_axis',(0.,1.,0.));
#92498=DIRECTION('ref_axis',(1.,0.,0.));
#92499=DIRECTION('',(-0.190809912898503,0.,0.981627005099017));
#92500=DIRECTION('center_axis',(0.,1.,0.));
#92501=DIRECTION('ref_axis',(-0.37394254111531,0.,0.927451872575728));
#92502=DIRECTION('center_axis',(0.,1.,0.));
#92503=DIRECTION('ref_axis',(-0.370185230514857,0.,0.928957961970649));
#92504=DIRECTION('center_axis',(-0.981627005099017,0.,-0.190809912898503));
#92505=DIRECTION('ref_axis',(-0.190809912898503,0.,0.981627005099017));
#92506=DIRECTION('center_axis',(-0.981627005099017,-1.45990679982696E-16,
-0.190809912898504));
#92507=DIRECTION('ref_axis',(-0.183385828075594,0.276229431355416,0.943433590304104));
#92508=DIRECTION('center_axis',(-0.981627005099017,-1.03383578960841E-16,
-0.190809912898504));
#92509=DIRECTION('ref_axis',(-0.183680511877257,0.270798308728604,0.944949599474087));
#92510=DIRECTION('center_axis',(0.,-1.,0.));
#92511=DIRECTION('ref_axis',(0.,0.,-1.));
#92512=DIRECTION('',(-0.190809912898503,0.,0.981627005099017));
#92513=DIRECTION('center_axis',(0.,-1.,0.));
#92514=DIRECTION('ref_axis',(-0.275846435585838,0.,0.961201718670222));
#92515=DIRECTION('',(-0.190809912898503,1.132361187045E-14,0.981627005099017));
#92516=DIRECTION('center_axis',(0.,-1.,0.));
#92517=DIRECTION('ref_axis',(-0.274117437734562,0.,0.961696225598208));
#92518=DIRECTION('center_axis',(0.981627005099017,0.,0.190809912898503));
#92519=DIRECTION('ref_axis',(0.,-1.,0.));
#92520=DIRECTION('',(-0.190809912898503,0.,0.981627005099017));
#92521=DIRECTION('center_axis',(0.981627005099017,3.74230666600009E-17,
0.190809912898503));
#92522=DIRECTION('ref_axis',(-0.181713220883714,0.305082598047195,0.934828815198184));
#92523=DIRECTION('center_axis',(0.981627005099017,-9.36058786041334E-17,
0.190809912898503));
#92524=DIRECTION('ref_axis',(-0.182066886709518,0.299235170990892,0.93664825906311));
#92525=DIRECTION('center_axis',(0.,1.,0.));
#92526=DIRECTION('ref_axis',(1.,0.,0.));
#92527=DIRECTION('',(-0.190809912898503,0.,0.981627005099017));
#92528=DIRECTION('center_axis',(0.,1.,0.));
#92529=DIRECTION('ref_axis',(-0.309344683605792,0.,0.950949981189774));
#92530=DIRECTION('center_axis',(0.,1.,0.));
#92531=DIRECTION('ref_axis',(-0.306895274081955,0.,0.951743290360464));
#92532=DIRECTION('center_axis',(-0.981627005099017,0.,-0.190809912898503));
#92533=DIRECTION('ref_axis',(-0.190809912898503,0.,0.981627005099017));
#92534=DIRECTION('center_axis',(-0.981627005099017,-9.04057881831701E-17,
-0.190809912898504));
#92535=DIRECTION('ref_axis',(-0.183533539382005,0.273521632312099,0.944193495306571));
#92536=DIRECTION('center_axis',(-0.981627005099017,-1.95641407952151E-16,
-0.190809912898504));
#92537=DIRECTION('ref_axis',(-0.18381683332523,0.268245652420898,0.945650909026989));
#92538=DIRECTION('center_axis',(0.,-1.,0.));
#92539=DIRECTION('ref_axis',(0.,0.,-1.));
#92540=DIRECTION('',(-0.190809912898503,0.,0.981627005099017));
#92541=DIRECTION('center_axis',(0.,-1.,0.));
#92542=DIRECTION('ref_axis',(-0.210563327934167,0.,0.977580219178605));
#92543=DIRECTION('',(-0.190809912898503,0.,0.981627005099017));
#92544=DIRECTION('center_axis',(0.,-1.,0.));
#92545=DIRECTION('ref_axis',(-0.210159055405375,0.,0.977667208937234));
#92546=DIRECTION('center_axis',(0.981627005099017,0.,0.190809912898503));
#92547=DIRECTION('ref_axis',(0.,-1.,0.));
#92548=DIRECTION('',(-0.190809912898503,0.,0.981627005099017));
#92549=DIRECTION('center_axis',(0.981627005099017,2.60207268814641E-16,
0.190809912898504));
#92550=DIRECTION('ref_axis',(-0.181775649940103,0.304059405247896,0.935149983248222));
#92551=DIRECTION('center_axis',(0.981627005099017,3.43394588839726E-16,
0.190809912898504));
#92552=DIRECTION('ref_axis',(-0.182124568584603,0.298269507204199,0.936945005104375));
#92553=DIRECTION('center_axis',(0.,1.,0.));
#92554=DIRECTION('ref_axis',(1.,0.,0.));
#92555=DIRECTION('',(-0.190809912898503,0.,0.981627005099017));
#92556=DIRECTION('center_axis',(0.,1.,0.));
#92557=DIRECTION('ref_axis',(-0.24384603732277,0.,0.969813956427717));
#92558=DIRECTION('center_axis',(0.,1.,0.));
#92559=DIRECTION('ref_axis',(-0.242742672216863,0.,0.970090714874138));
#92560=DIRECTION('center_axis',(-0.981627005099017,0.,-0.190809912898503));
#92561=DIRECTION('ref_axis',(-0.190809912898503,0.,0.981627005099017));
#92562=DIRECTION('center_axis',(-0.981627005099017,-5.96131698931744E-17,
-0.190809912898504));
#92563=DIRECTION('ref_axis',(-0.183614456317799,0.272025926757612,0.94460977477622));
#92564=DIRECTION('center_axis',(-0.981627005099017,-7.88692931673802E-17,
-0.190809912898504));
#92565=DIRECTION('ref_axis',(-0.183891602408533,0.266834398951196,0.94603556069525));
#92566=DIRECTION('center_axis',(0.,-1.,0.));
#92567=DIRECTION('ref_axis',(0.,0.,-1.));
#92568=DIRECTION('',(-0.190809912898503,0.,0.981627005099017));
#92569=DIRECTION('center_axis',(0.,-1.,0.));
#92570=DIRECTION('ref_axis',(-0.144416822146308,0.,0.98951694350383));
#92571=DIRECTION('',(-0.190809912898503,0.,0.981627005099017));
#92572=DIRECTION('center_axis',(0.,-1.,0.));
#92573=DIRECTION('ref_axis',(-0.14537237934921,0.,0.989377011721189));
#92574=DIRECTION('center_axis',(0.981627005099017,0.,0.190809912898503));
#92575=DIRECTION('ref_axis',(0.,-1.,0.));
#92576=DIRECTION('',(-0.190809912898503,0.,0.981627005099017));
#92577=DIRECTION('center_axis',(0.981627005099017,-1.19151365507148E-16,
0.190809912898503));
#92578=DIRECTION('ref_axis',(-0.181760123195241,0.304314238039989,0.935070105469206));
#92579=DIRECTION('center_axis',(0.981627005099017,7.16559735129159E-18,
0.190809912898503));
#92580=DIRECTION('ref_axis',(-0.182110219627529,0.298510046456984,0.936871186488016));
#92581=DIRECTION('center_axis',(0.,1.,0.));
#92582=DIRECTION('ref_axis',(1.,0.,0.));
#92583=DIRECTION('',(-0.190809912898503,0.,0.981627005099017));
#92584=DIRECTION('center_axis',(0.,1.,0.));
#92585=DIRECTION('ref_axis',(-0.177462871614912,0.,0.984127496414052));
#92586=DIRECTION('center_axis',(0.,1.,0.));
#92587=DIRECTION('ref_axis',(-0.177742357598668,0.,0.984077057102373));
#92588=DIRECTION('center_axis',(-0.981627005099017,0.,-0.190809912898503));
#92589=DIRECTION('ref_axis',(-0.190809912898503,0.,0.981627005099017));
#92590=DIRECTION('center_axis',(-0.981627005099017,-1.0406113144537E-16,
-0.190809912898504));
#92591=DIRECTION('ref_axis',(-0.183632874440486,0.271684234850208,0.944704527330414));
#92592=DIRECTION('center_axis',(-0.981627005099017,-1.43052272430736E-16,
-0.190809912898504));
#92593=DIRECTION('ref_axis',(-0.183908630238396,0.266511876338901,0.946123160848605));
#92594=DIRECTION('center_axis',(0.,-1.,0.));
#92595=DIRECTION('ref_axis',(0.,0.,-1.));
#92596=DIRECTION('',(-0.190809912898503,0.,0.981627005099017));
#92597=DIRECTION('center_axis',(0.,-1.,0.));
#92598=DIRECTION('ref_axis',(-0.0774045612714574,0.,0.996999766245897));
#92599=DIRECTION('',(-0.190809912898503,0.,0.981627005099017));
#92600=DIRECTION('center_axis',(0.,-1.,0.));
#92601=DIRECTION('ref_axis',(-0.0797552408636643,0.,0.996814476998995));
#92602=DIRECTION('center_axis',(0.981627005099017,0.,0.190809912898503));
#92603=DIRECTION('ref_axis',(0.,-1.,0.));
#92604=DIRECTION('',(-0.190809912898503,0.,0.981627005099017));
#92605=DIRECTION('center_axis',(0.981627005099017,0.,0.190809912898503));
#92606=DIRECTION('ref_axis',(-0.181665829576745,0.305856807673619,0.934585009276254));
#92607=DIRECTION('center_axis',(0.981627005099017,5.06495345173922E-17,
0.190809912898503));
#92608=DIRECTION('ref_axis',(-0.182023119703858,0.299965605628596,0.936423098461985));
#92609=DIRECTION('center_axis',(0.,1.,0.));
#92610=DIRECTION('ref_axis',(1.,0.,0.));
#92611=DIRECTION('',(-0.190809912898503,0.,0.981627005099017));
#92612=DIRECTION('center_axis',(0.,1.,0.));
#92613=DIRECTION('ref_axis',(-0.110198871269438,0.,0.993909557641409));
#92614=DIRECTION('center_axis',(0.,1.,0.));
#92615=DIRECTION('ref_axis',(-0.111897714940647,0.,0.99371972979863));
#92616=DIRECTION('center_axis',(-0.981627005099017,0.,-0.190809912898503));
#92617=DIRECTION('ref_axis',(-0.190809912898503,0.,0.981627005099017));
#92618=DIRECTION('center_axis',(-0.981627005099017,-2.0187191501672E-16,
-0.190809912898504));
#92619=DIRECTION('ref_axis',(-0.183589751211426,0.272483527884585,0.944482678656256));
#92620=DIRECTION('center_axis',(-0.981627005099017,-2.87726513572186E-16,
-0.190809912898504));
#92621=DIRECTION('ref_axis',(-0.183868767449469,0.267266256174104,0.945918085601122));
#92622=DIRECTION('center_axis',(0.,-1.,0.));
#92623=DIRECTION('ref_axis',(0.,0.,-1.));
#92624=DIRECTION('',(-0.190809912898503,0.,0.981627005099017));
#92625=DIRECTION('center_axis',(0.,-1.,0.));
#92626=DIRECTION('ref_axis',(-0.00951217486443362,0.,0.999954758241266));
#92627=DIRECTION('',(-0.190809912898503,0.,0.981627005099017));
#92628=DIRECTION('center_axis',(0.,-1.,0.));
#92629=DIRECTION('ref_axis',(-0.0132944259954453,0.,0.999911625213674));
#92630=DIRECTION('center_axis',(0.981627005099017,0.,0.190809912898503));
#92631=DIRECTION('ref_axis',(0.,-1.,0.));
#92632=DIRECTION('',(-0.190809912898503,0.,0.981627005099017));
#92633=DIRECTION('center_axis',(0.981627005099017,1.30313218010573E-16,
0.190809912898504));
#92634=DIRECTION('ref_axis',(-0.181487751748704,0.308746843185004,0.933668882842571));
#92635=DIRECTION('center_axis',(0.981627005099017,3.38914002557394E-16,
0.190809912898504));
#92636=DIRECTION('ref_axis',(-0.181858819374924,0.302690361553391,0.935577850762958));
#92637=DIRECTION('center_axis',(0.,1.,0.));
#92638=DIRECTION('ref_axis',(1.,0.,0.));
#92639=DIRECTION('',(-0.190809912898503,0.,0.981627005099017));
#92640=DIRECTION('center_axis',(0.,1.,0.));
#92641=DIRECTION('ref_axis',(-0.0420453982044825,0.,0.999115701252776));
#92642=DIRECTION('center_axis',(0.,1.,0.));
#92643=DIRECTION('ref_axis',(-0.0452008111636282,0.,0.998977921012347));
#92644=DIRECTION('center_axis',(-0.981627005099017,0.,-0.190809912898503));
#92645=DIRECTION('ref_axis',(-0.190809912898503,0.,0.981627005099017));
#92646=DIRECTION('center_axis',(-0.981627005099017,-6.82675953385116E-17,
-0.190809912898503));
#92647=DIRECTION('ref_axis',(-0.183482833113299,0.274454421803195,0.943932635470027));
#92648=DIRECTION('center_axis',(-0.981627005099017,0.,-0.190809912898503));
#92649=DIRECTION('ref_axis',(-0.183770012633108,0.269125326340587,0.945410038649315));
#92650=DIRECTION('center_axis',(0.,-1.,0.));
#92651=DIRECTION('ref_axis',(0.,0.,-1.));
#92652=DIRECTION('',(-0.190809912898503,0.,0.981627005099017));
#92653=DIRECTION('center_axis',(0.,-1.,0.));
#92654=DIRECTION('ref_axis',(0.0592877418835069,0.,0.99824093467577));
#92655=DIRECTION('',(-0.190809912898503,0.,0.981627005099017));
#92656=DIRECTION('center_axis',(0.,-1.,0.));
#92657=DIRECTION('ref_axis',(0.0540352232974096,0.,0.998539030105083));
#92658=DIRECTION('center_axis',(0.981627005099017,0.,0.190809912898503));
#92659=DIRECTION('ref_axis',(0.,-1.,0.));
#92660=DIRECTION('',(-0.190809912898503,0.,0.981627005099017));
#92661=DIRECTION('center_axis',(0.981627005099017,3.46860807619102E-16,
0.190809912898504));
#92662=DIRECTION('ref_axis',(-0.181215978183,0.313100693055305,0.93227073603083));
#92663=DIRECTION('center_axis',(0.981627005099017,3.55724373777378E-16,
0.190809912898504));
#92664=DIRECTION('ref_axis',(-0.181608554935483,0.306789600923706,0.93429035826092));
#92665=DIRECTION('center_axis',(0.,1.,0.));
#92666=DIRECTION('ref_axis',(1.,0.,0.));
#92667=DIRECTION('',(-0.190809912898503,0.,0.981627005099017));
#92668=DIRECTION('center_axis',(0.,1.,0.));
#92669=DIRECTION('ref_axis',(0.0270191259379464,0.,0.999634916773894));
#92670=DIRECTION('center_axis',(0.,1.,0.));
#92671=DIRECTION('ref_axis',(0.0223681473937496,0.,0.999749801691489));
#92672=DIRECTION('center_axis',(-0.981627005099017,0.,-0.190809912898503));
#92673=DIRECTION('ref_axis',(-0.190809912898503,0.,0.981627005099017));
#92674=DIRECTION('center_axis',(-0.981627005099017,-3.88216196345816E-17,
-0.190809912898503));
#92675=DIRECTION('ref_axis',(-0.183306354127305,0.277674505471101,0.943024734324575));
#92676=DIRECTION('center_axis',(-0.981627005099017,-1.19343362969677E-16,
-0.190809912898504));
#92677=DIRECTION('ref_axis',(-0.183607255301246,0.272159393626116,0.944572728942461));
#92678=DIRECTION('center_axis',(0.,-1.,0.));
#92679=DIRECTION('ref_axis',(0.,0.,-1.));
#92680=DIRECTION('',(-0.190809912898503,0.,0.981627005099017));
#92681=DIRECTION('center_axis',(0.,-1.,0.));
#92682=DIRECTION('ref_axis',(0.129037681608313,0.,0.991639690979114));
#92683=DIRECTION('',(-0.190809912898493,0.,0.981627005099019));
#92684=DIRECTION('center_axis',(0.,-1.,0.));
#92685=DIRECTION('ref_axis',(0.122272610118709,0.,0.992496553553088));
#92686=DIRECTION('center_axis',(0.981627005099017,0.,0.190809912898503));
#92687=DIRECTION('ref_axis',(0.,-1.,0.));
#92688=DIRECTION('',(-0.190809912898503,0.,0.981627005099017));
#92689=DIRECTION('center_axis',(0.981627005099017,-8.1884484692467E-18,
0.190809912898503));
#92690=DIRECTION('ref_axis',(-0.180834252140125,0.319104965266087,0.93030693558387));
#92691=DIRECTION('center_axis',(0.981627005099017,7.84954079410769E-18,
0.190809912898503));
#92692=DIRECTION('ref_axis',(-0.181258021464907,0.312431545483989,0.932487028886254));
#92693=DIRECTION('center_axis',(0.,1.,0.));
#92694=DIRECTION('ref_axis',(1.,0.,0.));
#92695=DIRECTION('',(-0.190809912898503,0.,0.981627005099017));
#92696=DIRECTION('center_axis',(0.,1.,0.));
#92697=DIRECTION('ref_axis',(0.0970308224791404,0.,0.995281377043207));
#92698=DIRECTION('center_axis',(0.,1.,0.));
#92699=DIRECTION('ref_axis',(0.0908422199685957,0.,0.995865297653843));
#92700=DIRECTION('center_axis',(-0.981627005099017,0.,-0.190809912898503));
#92701=DIRECTION('ref_axis',(-0.190809912898503,0.,0.981627005099017));
#92702=DIRECTION('center_axis',(-0.981627005099017,-4.81431257853459E-17,
-0.190809912898503));
#92703=DIRECTION('ref_axis',(-0.183050227681134,0.28227713515299,0.941707084562767));
#92704=DIRECTION('center_axis',(-0.981627005099017,9.23779601860268E-17,
-0.190809912898503));
#92705=DIRECTION('ref_axis',(-0.183371589738963,0.2764889283937,0.943360340777748));
#92706=DIRECTION('center_axis',(0.,-1.,0.));
#92707=DIRECTION('ref_axis',(0.,0.,-1.));
#92708=DIRECTION('',(-0.190809912898503,0.,0.981627005099017));
#92709=DIRECTION('center_axis',(0.,-1.,0.));
#92710=DIRECTION('ref_axis',(0.123657514606589,0.,0.99232495639348));
#92711=DIRECTION('',(-0.190809912898503,0.,0.981627005099017));
#92712=DIRECTION('center_axis',(0.,-1.,0.));
#92713=DIRECTION('ref_axis',(0.117218477629797,0.,0.993106151678738));
#92714=DIRECTION('center_axis',(0.981627005099017,0.,0.190809912898503));
#92715=DIRECTION('ref_axis',(0.,-1.,0.));
#92716=DIRECTION('',(-0.190809912898503,0.,0.981627005099017));
#92717=DIRECTION('center_axis',(0.981627005099017,1.228267270387E-16,0.190809912898504));
#92718=DIRECTION('ref_axis',(-0.184691122397272,0.251210291805195,0.950148713938394));
#92719=DIRECTION('center_axis',(0.981627005099017,1.56990815882154E-16,
0.190809912898504));
#92720=DIRECTION('ref_axis',(-0.184948385867005,0.245956748572503,0.951472213150144));
#92721=DIRECTION('center_axis',(0.,1.,0.));
#92722=DIRECTION('ref_axis',(1.,0.,0.));
#92723=DIRECTION('',(-0.190809912898503,0.,0.981627005099017));
#92724=DIRECTION('center_axis',(0.,1.,0.));
#92725=DIRECTION('ref_axis',(0.0914624082264752,0.,0.995808529729191));
#92726=DIRECTION('center_axis',(0.,1.,0.));
#92727=DIRECTION('ref_axis',(0.0856161376277009,0.,0.996328197421771));
#92728=DIRECTION('center_axis',(-0.981627005099017,0.,-0.190809912898503));
#92729=DIRECTION('ref_axis',(-0.190809912898503,0.,0.981627005099017));
#92730=DIRECTION('center_axis',(-0.981627005099017,-2.32691774629172E-16,
-0.190809912898504));
#92731=DIRECTION('ref_axis',(-0.186344772310312,0.215068293449893,0.958655962786008));
#92732=DIRECTION('center_axis',(-0.981627005099017,-1.00076123534862E-16,
-0.190809912898504));
#92733=DIRECTION('ref_axis',(-0.186528095125347,0.210658231157109,0.959599072203943));
#92734=DIRECTION('center_axis',(0.,-1.,0.));
#92735=DIRECTION('ref_axis',(0.,0.,-1.));
#92736=DIRECTION('',(-0.190809912898503,0.,0.981627005099017));
#92737=DIRECTION('center_axis',(0.,-1.,0.));
#92738=DIRECTION('ref_axis',(0.119896958150858,0.,0.992786341277));
#92739=DIRECTION('',(-0.190809912898503,0.,0.981627005099017));
#92740=DIRECTION('center_axis',(0.,-1.,0.));
#92741=DIRECTION('ref_axis',(0.113679714473517,0.,0.993517449528301));
#92742=DIRECTION('center_axis',(0.981627005099017,0.,0.190809912898503));
#92743=DIRECTION('ref_axis',(0.,-1.,0.));
#92744=DIRECTION('',(-0.190809912898503,0.,0.981627005099017));
#92745=DIRECTION('center_axis',(0.981627005099017,1.51486296681064E-16,
0.190809912898504));
#92746=DIRECTION('ref_axis',(-0.187576469189326,0.183315618344298,0.964992462290516));
#92747=DIRECTION('center_axis',(0.981627005099017,1.33442193499831E-16,
0.190809912898504));
#92748=DIRECTION('ref_axis',(-0.187711401531336,0.179481951661004,0.965686625548422));
#92749=DIRECTION('center_axis',(0.,1.,0.));
#92750=DIRECTION('ref_axis',(1.,0.,0.));
#92751=DIRECTION('',(-0.190809912898503,0.,0.981627005099017));
#92752=DIRECTION('center_axis',(0.,1.,0.));
#92753=DIRECTION('ref_axis',(0.0874284944613751,0.,0.9961707977833));
#92754=DIRECTION('center_axis',(0.,1.,0.));
#92755=DIRECTION('ref_axis',(0.0818224711015746,0.,0.996646920038803));
#92756=DIRECTION('center_axis',(-0.981627005099017,0.,-0.190809912898503));
#92757=DIRECTION('ref_axis',(-0.190809912898503,0.,0.981627005099017));
#92758=DIRECTION('center_axis',(-0.981627005099017,-8.42504701243554E-17,
-0.190809912898504));
#92759=DIRECTION('ref_axis',(-0.188712603501478,0.147859451746807,0.970837337461239));
#92760=DIRECTION('center_axis',(-0.981627005099017,-1.07774286883698E-16,
-0.190809912898504));
#92761=DIRECTION('ref_axis',(-0.188798187650067,0.144827533920497,0.971277627539396));
#92762=DIRECTION('center_axis',(0.,-1.,0.));
#92763=DIRECTION('ref_axis',(0.,0.,-1.));
#92764=DIRECTION('',(-0.190809912898503,0.,0.981627005099017));
#92765=DIRECTION('center_axis',(0.,-1.,0.));
#92766=DIRECTION('ref_axis',(0.117596679694482,0.,0.993061438645582));
#92767=DIRECTION('',(-0.190809912898503,0.,0.981627005099017));
#92768=DIRECTION('center_axis',(0.,-1.,0.));
#92769=DIRECTION('ref_axis',(0.111512654940727,0.,0.993763013896206));
#92770=DIRECTION('center_axis',(0.981627005099017,0.,0.190809912898503));
#92771=DIRECTION('ref_axis',(0.,-1.,0.));
#92772=DIRECTION('',(-0.190809912898492,0.,0.981627005099019));
#92773=DIRECTION('center_axis',(0.981627005099017,3.27537938769868E-17,
0.190809912898504));
#92774=DIRECTION('ref_axis',(-0.189534667147167,0.115420944883498,0.975066467186526));
#92775=DIRECTION('center_axis',(0.981627005099017,3.92477039705384E-17,
0.190809912898504));
#92776=DIRECTION('ref_axis',(-0.189587617832801,0.113007154749503,0.975338873489571));
#92777=DIRECTION('center_axis',(0.,1.,0.));
#92778=DIRECTION('ref_axis',(1.,0.,0.));
#92779=DIRECTION('',(-0.190809912898503,0.,0.981627005099017));
#92780=DIRECTION('center_axis',(0.,1.,0.));
#92781=DIRECTION('ref_axis',(0.0847526256525639,0.,0.996402023505069));
#92782=DIRECTION('center_axis',(0.,1.,0.));
#92783=DIRECTION('ref_axis',(0.0793024169710135,0.,0.996850603983644));
#92784=DIRECTION('center_axis',(-0.981627005099017,0.,-0.190809912898503));
#92785=DIRECTION('ref_axis',(-0.190809912898503,0.,0.981627005099017));
#92786=DIRECTION('center_axis',(-0.981627005099017,2.00596357438942E-17,
-0.190809912898503));
#92787=DIRECTION('ref_axis',(-0.190188336952842,0.0806506100437121,0.978429290029019));
#92788=DIRECTION('center_axis',(-0.981627005099017,-9.62270418604446E-18,
-0.190809912898503));
#92789=DIRECTION('ref_axis',(-0.190213606479589,0.0789968366839196,0.97855928982559));
#92790=DIRECTION('center_axis',(0.,-1.,0.));
#92791=DIRECTION('ref_axis',(0.,0.,-1.));
#92792=DIRECTION('',(-0.190809912898503,0.,0.981627005099017));
#92793=DIRECTION('center_axis',(0.,-1.,0.));
#92794=DIRECTION('ref_axis',(0.116664111632625,0.,0.993171427829542));
#92795=DIRECTION('',(-0.190809912898503,0.,0.981627005099017));
#92796=DIRECTION('center_axis',(0.,-1.,0.));
#92797=DIRECTION('ref_axis',(0.110633569332503,0.,0.993861264632419));
#92798=DIRECTION('center_axis',(0.981627005099017,0.,0.190809912898503));
#92799=DIRECTION('ref_axis',(0.,-1.,0.));
#92800=DIRECTION('',(-0.190809912898503,0.,0.981627005099017));
#92801=DIRECTION('center_axis',(0.981627005099017,1.12591166452142E-17,
0.190809912898504));
#92802=DIRECTION('ref_axis',(-0.190594295464282,0.0475262714226105,0.980517755097346));
#92803=DIRECTION('center_axis',(0.981627005099017,-2.551100758085E-17,0.190809912898503));
#92804=DIRECTION('ref_axis',(-0.190603224387164,0.0465323578380378,0.980563690194191));
#92805=DIRECTION('center_axis',(0.,1.,0.));
#92806=DIRECTION('ref_axis',(1.,0.,0.));
#92807=DIRECTION('',(-0.190809912898503,0.,0.981627005099017));
#92808=DIRECTION('center_axis',(0.,1.,0.));
#92809=DIRECTION('ref_axis',(0.083324953951956,0.,0.99652242927538));
#92810=DIRECTION('center_axis',(0.,1.,0.));
#92811=DIRECTION('ref_axis',(0.0779567276864901,0.,0.996956743599447));
#92812=DIRECTION('center_axis',(-0.981627005099017,0.,-0.190809912898503));
#92813=DIRECTION('ref_axis',(-0.190809912898503,0.,0.981627005099017));
#92814=DIRECTION('center_axis',(-0.981627005099017,-2.50745446798676E-18,
-0.190809912898504));
#92815=DIRECTION('ref_axis',(-0.19079267424387,0.0134417683406195,0.981538320351656));
#92816=DIRECTION('center_axis',(-0.981627005099017,-9.62270418604446E-19,
-0.190809912898503));
#92817=DIRECTION('ref_axis',(-0.190793373996996,0.0131661394473206,0.981541920251446));
#92818=DIRECTION('center_axis',(0.,-1.,0.));
#92819=DIRECTION('ref_axis',(0.,0.,-1.));
#92820=DIRECTION('',(-0.190809912898515,0.,0.981627005099015));
#92821=DIRECTION('center_axis',(0.,-1.,0.));
#92822=DIRECTION('ref_axis',(-0.334732212895843,0.,0.942313294849358));
#92823=DIRECTION('',(-0.190809912898516,0.,0.981627005099015));
#92824=DIRECTION('center_axis',(0.,-1.,0.));
#92825=DIRECTION('ref_axis',(-0.332032295999667,0.,0.943268018334762));
#92826=DIRECTION('center_axis',(0.981627005099017,0.,0.190809912898503));
#92827=DIRECTION('ref_axis',(0.,-1.,0.));
#92828=DIRECTION('',(-0.190809912898503,0.,0.981627005099017));
#92829=DIRECTION('center_axis',(0.981627005099017,1.51997840690772E-17,
0.190809912898504));
#92830=DIRECTION('ref_axis',(-0.190609801410987,0.0457864155045494,0.980597525879659));
#92831=DIRECTION('center_axis',(0.981627005099017,2.74015551152694E-17,
0.190809912898504));
#92832=DIRECTION('ref_axis',(-0.190617515250888,0.0448957163395215,0.980637209947664));
#92833=DIRECTION('center_axis',(0.,1.,0.));
#92834=DIRECTION('ref_axis',(1.,0.,0.));
#92835=DIRECTION('',(-0.190809912898503,0.,0.981627005099017));
#92836=DIRECTION('center_axis',(0.,1.,0.));
#92837=DIRECTION('ref_axis',(-0.365610687831021,0.,0.930767868452563));
#92838=DIRECTION('center_axis',(0.,1.,0.));
#92839=DIRECTION('ref_axis',(-0.362336833871464,0.,0.932047219200832));
#92840=DIRECTION('center_axis',(-0.981627005099017,0.,-0.190809912898503));
#92841=DIRECTION('ref_axis',(-0.190809912898503,0.,0.981627005099017));
#92842=DIRECTION('center_axis',(-0.981627005099017,9.60464999886156E-19,
-0.190809912898503));
#92843=DIRECTION('ref_axis',(-0.190793405028745,0.0131537824454998,0.981542079895159));
#92844=DIRECTION('center_axis',(-0.981627005099017,-6.46147368505259E-18,
-0.190809912898504));
#92845=DIRECTION('ref_axis',(-0.190794047817322,0.0128951575585105,0.981545386739209));
#92846=DIRECTION('center_axis',(0.,-1.,0.));
#92847=DIRECTION('ref_axis',(0.,0.,-1.));
#92848=DIRECTION('',(-0.190809912898503,0.,0.981627005099017));
#92849=DIRECTION('center_axis',(0.,-1.,0.));
#92850=DIRECTION('ref_axis',(-0.335149294303462,0.,0.942165033594376));
#92851=DIRECTION('',(-0.190809912898503,0.,0.981627005099017));
#92852=DIRECTION('center_axis',(0.,-1.,0.));
#92853=DIRECTION('ref_axis',(-0.332426172894225,0.,0.943129280414355));
#92854=DIRECTION('center_axis',(0.981627005099017,0.,0.190809912898503));
#92855=DIRECTION('ref_axis',(0.,-1.,0.));
#92856=DIRECTION('',(-0.190809912898503,0.,0.981627005099017));
#92857=DIRECTION('center_axis',(0.981627005099017,7.5998920345386E-18,0.190809912898503));
#92858=DIRECTION('ref_axis',(-0.189626613313853,0.111195580511101,0.975539486847107));
#92859=DIRECTION('center_axis',(0.981627005099017,1.82677034101797E-17,
0.190809912898503));
#92860=DIRECTION('ref_axis',(-0.189672340528791,0.109032453967399,0.975774731800418));
#92861=DIRECTION('center_axis',(0.,1.,0.));
#92862=DIRECTION('ref_axis',(1.,0.,0.));
#92863=DIRECTION('',(-0.190809912898503,0.,0.981627005099017));
#92864=DIRECTION('center_axis',(0.,1.,0.));
#92865=DIRECTION('ref_axis',(-0.366480370880962,0.,0.930425783047177));
#92866=DIRECTION('center_axis',(0.,1.,0.));
#92867=DIRECTION('ref_axis',(-0.363158067036044,0.,0.931727545126065));
#92868=DIRECTION('center_axis',(-0.981627005099017,0.,-0.190809912898503));
#92869=DIRECTION('ref_axis',(-0.190809912898503,0.,0.981627005099017));
#92870=DIRECTION('center_axis',(-0.981627005099017,-3.45767399959016E-17,
-0.190809912898504));
#92871=DIRECTION('ref_axis',(-0.190214727024376,0.0789226946729824,0.978565054500005));
#92872=DIRECTION('center_axis',(-0.981627005099017,-5.53840601575937E-17,
-0.190809912898504));
#92873=DIRECTION('ref_axis',(-0.19023793643477,0.0773709453510314,0.978684455969608));
#92874=DIRECTION('center_axis',(0.,-1.,0.));
#92875=DIRECTION('ref_axis',(0.,0.,-1.));
#92876=DIRECTION('',(-0.190809912898493,0.,0.981627005099019));
#92877=DIRECTION('center_axis',(0.,-1.,0.));
#92878=DIRECTION('ref_axis',(-0.336177570564712,0.,0.941798620220484));
#92879=DIRECTION('',(-0.190809912898503,0.,0.981627005099017));
#92880=DIRECTION('center_axis',(0.,-1.,0.));
#92881=DIRECTION('ref_axis',(-0.333396687233972,0.,0.942786640200959));
#92882=DIRECTION('center_axis',(0.981627005099017,0.,0.190809912898503));
#92883=DIRECTION('ref_axis',(0.,-1.,0.));
#92884=DIRECTION('',(-0.190809912898503,0.,0.981627005099017));
#92885=DIRECTION('center_axis',(0.981627005099017,4.17994061899623E-17,
0.190809912898504));
#92886=DIRECTION('ref_axis',(-0.187810734417079,0.176604745517606,0.966197646394556));
#92887=DIRECTION('center_axis',(0.981627005099017,1.13259761143114E-16,
0.190809912898504));
#92888=DIRECTION('ref_axis',(-0.187927174114397,0.173169191595305,0.966796673717698));
#92889=DIRECTION('center_axis',(0.,1.,0.));
#92890=DIRECTION('ref_axis',(1.,0.,0.));
#92891=DIRECTION('',(-0.190809912898503,-1.576961924456E-14,0.981627005099017));
#92892=DIRECTION('center_axis',(0.,1.,0.));
#92893=DIRECTION('ref_axis',(-0.36810928335472,0.,0.929782531298623));
#92894=DIRECTION('center_axis',(0.,1.,0.));
#92895=DIRECTION('ref_axis',(-0.364694981855002,0.,0.931127043002071));
#92896=DIRECTION('center_axis',(-0.981627005099017,0.,-0.190809912898503));
#92897=DIRECTION('ref_axis',(-0.190809912898503,0.,0.981627005099017));
#92898=DIRECTION('center_axis',(-0.981627005099017,-3.84185999954462E-17,
-0.190809912898504));
#92899=DIRECTION('ref_axis',(-0.188801982134388,0.144691606900499,0.971297148371536));
#92900=DIRECTION('center_axis',(-0.981627005099017,-3.69227067717291E-18,
-0.190809912898503));
#92901=DIRECTION('ref_axis',(-0.188880563702572,0.141846733143594,0.971701413476325));
#92902=DIRECTION('center_axis',(0.,-1.,0.));
#92903=DIRECTION('ref_axis',(0.,0.,-1.));
#92904=DIRECTION('',(-0.190809912898503,0.,0.981627005099017));
#92905=DIRECTION('center_axis',(0.,-1.,0.));
#92906=DIRECTION('ref_axis',(-0.337857092755181,0.,0.941197420775799));
#92907=DIRECTION('',(-0.190809912898503,-1.139455022803E-14,0.981627005099017));
#92908=DIRECTION('center_axis',(0.,-1.,0.));
#92909=DIRECTION('ref_axis',(-0.334980161426978,0.,0.942225180861961));
#92910=DIRECTION('center_axis',(0.981627005099017,0.,0.190809912898503));
#92911=DIRECTION('ref_axis',(0.,-1.,0.));
#92912=DIRECTION('',(-0.190809912898503,0.,0.981627005099017));
#92913=DIRECTION('center_axis',(0.981627005099017,2.65996221208851E-16,
0.190809912898504));
#92914=DIRECTION('ref_axis',(-0.18513766459081,0.242013910524089,0.95244596290955));
#92915=DIRECTION('center_axis',(0.981627005099017,-5.1149569548503E-17,
0.190809912898503));
#92916=DIRECTION('ref_axis',(-0.185359421522839,0.237305929223209,0.953586797731716));
#92917=DIRECTION('center_axis',(0.,1.,0.));
#92918=DIRECTION('ref_axis',(1.,0.,0.));
#92919=DIRECTION('',(-0.190809912898503,0.,0.981627005099017));
#92920=DIRECTION('center_axis',(0.,1.,0.));
#92921=DIRECTION('ref_axis',(-0.370562121723774,0.,0.928807684046366));
#92922=DIRECTION('center_axis',(0.,1.,0.));
#92923=DIRECTION('ref_axis',(-0.367006186766544,0.,0.930218500608906));
#92924=DIRECTION('center_axis',(-0.981627005099017,0.,-0.190809912898503));
#92925=DIRECTION('ref_axis',(-0.190809912898503,0.,0.981627005099017));
#92926=DIRECTION('center_axis',(-0.981627005099017,-4.61023199945355E-17,
-0.190809912898503));
#92927=DIRECTION('ref_axis',(-0.186536220732626,0.210460519128004,0.959640874620897));
#92928=DIRECTION('center_axis',(-0.981627005099017,-5.16917894804207E-17,
-0.190809912898504));
#92929=DIRECTION('ref_axis',(-0.186704454524913,0.206322520936108,0.960506358133627));
#92930=DIRECTION('center_axis',(0.,-1.,0.));
#92931=DIRECTION('ref_axis',(0.,0.,-1.));
#92932=DIRECTION('',(-0.190809912898503,0.,0.981627005099017));
#92933=DIRECTION('center_axis',(0.,-1.,0.));
#92934=DIRECTION('ref_axis',(-0.274471632436799,0.,0.961595197048882));
#92935=DIRECTION('',(-0.190809912898503,0.,0.981627005099017));
#92936=DIRECTION('center_axis',(0.,-1.,0.));
#92937=DIRECTION('ref_axis',(-0.272823755605811,0.,0.962064030289638));
#92938=DIRECTION('center_axis',(0.981627005099017,0.,0.190809912898503));
#92939=DIRECTION('ref_axis',(0.,-1.,0.));
#92940=DIRECTION('',(-0.190809912898503,0.,0.981627005099017));
#92941=DIRECTION('center_axis',(0.981627005099017,5.23922933240012E-17,
0.190809912898503));
#92942=DIRECTION('ref_axis',(-0.185225001331504,0.240171406973301,0.952895269247471));
#92943=DIRECTION('center_axis',(0.981627005099017,1.44009044006359E-17,
0.190809912898503));
#92944=DIRECTION('ref_axis',(-0.185440110076089,0.235568113333292,0.954001902280892));
#92945=DIRECTION('center_axis',(0.,1.,0.));
#92946=DIRECTION('ref_axis',(1.,0.,0.));
#92947=DIRECTION('',(-0.190809912898503,1.142355795319E-14,0.981627005099017));
#92948=DIRECTION('center_axis',(0.,1.,0.));
#92949=DIRECTION('ref_axis',(-0.307140935229151,0.,0.951664040461004));
#92950=DIRECTION('center_axis',(0.,1.,0.));
#92951=DIRECTION('ref_axis',(-0.304823463240135,0.,0.952408870316888));
#92952=DIRECTION('center_axis',(-0.981627005099017,0.,-0.190809912898503));
#92953=DIRECTION('ref_axis',(-0.190809912898503,0.,0.981627005099017));
#92954=DIRECTION('center_axis',(-0.981627005099017,-7.53381568193084E-17,
-0.190809912898504));
#92955=DIRECTION('ref_axis',(-0.186620533713518,0.208397434142596,0.960074625140809));
#92956=DIRECTION('center_axis',(-0.981627005099017,-2.17379342169057E-17,
-0.190809912898503));
#92957=DIRECTION('ref_axis',(-0.18678231992954,0.204377639939707,0.960906938914698));
#92958=DIRECTION('center_axis',(0.,-1.,0.));
#92959=DIRECTION('ref_axis',(0.,0.,-1.));
#92960=DIRECTION('',(-0.190809912898503,0.,0.981627005099017));
#92961=DIRECTION('center_axis',(0.,-1.,0.));
#92962=DIRECTION('ref_axis',(-0.210241863716573,0.,0.977649404817996));
#92963=DIRECTION('',(-0.190809912898503,0.,0.981627005099017));
#92964=DIRECTION('center_axis',(0.,-1.,0.));
#92965=DIRECTION('ref_axis',(-0.209856641284083,0.,0.977732166858063));
#92966=DIRECTION('center_axis',(0.981627005099017,0.,0.190809912898503));
#92967=DIRECTION('ref_axis',(0.,-1.,0.));
#92968=DIRECTION('',(-0.190809912898503,0.,0.981627005099017));
#92969=DIRECTION('center_axis',(0.981627005099017,1.41255374499376E-16,
0.190809912898504));
#92970=DIRECTION('ref_axis',(-0.185262960048131,0.239365914769592,0.953090548941034));
#92971=DIRECTION('center_axis',(0.981627005099017,-1.21618916880736E-16,
0.190809912898503));
#92972=DIRECTION('ref_axis',(-0.185475209669276,0.234807909926708,0.954182473132885));
#92973=DIRECTION('center_axis',(0.,1.,0.));
#92974=DIRECTION('ref_axis',(1.,0.,0.));
#92975=DIRECTION('',(-0.190809912898503,0.,0.981627005099017));
#92976=DIRECTION('center_axis',(0.,1.,0.));
#92977=DIRECTION('ref_axis',(-0.242853318412819,0.,0.970063021527922));
#92978=DIRECTION('center_axis',(0.,1.,0.));
#92979=DIRECTION('ref_axis',(-0.241809655546285,0.,0.970323703969241));
#92980=DIRECTION('center_axis',(-0.981627005099017,0.,-0.190809912898503));
#92981=DIRECTION('ref_axis',(-0.190809912898503,0.,0.981627005099017));
#92982=DIRECTION('center_axis',(-0.981627005099017,6.70648161298212E-17,
-0.190809912898503));
#92983=DIRECTION('ref_axis',(-0.186666733374594,0.207257848958206,0.96031230060667));
#92984=DIRECTION('center_axis',(-0.981627005099017,3.58496787124456E-17,
-0.190809912898503));
#92985=DIRECTION('ref_axis',(-0.186825037997708,0.203302399200895,0.961126703227163));
#92986=DIRECTION('center_axis',(0.,-1.,0.));
#92987=DIRECTION('ref_axis',(0.,0.,-1.));
#92988=DIRECTION('',(-0.190809912898503,0.,0.981627005099017));
#92989=DIRECTION('center_axis',(0.,-1.,0.));
#92990=DIRECTION('ref_axis',(-0.145176670594025,0.,0.989405748070646));
#92991=DIRECTION('',(-0.190809912898503,0.,0.981627005099017));
#92992=DIRECTION('center_axis',(0.,-1.,0.));
#92993=DIRECTION('ref_axis',(-0.146087012429917,0.,0.989271744668421));
#92994=DIRECTION('center_axis',(0.981627005099017,0.,0.190809912898503));
#92995=DIRECTION('ref_axis',(0.,-1.,0.));
#92996=DIRECTION('',(-0.190809912898503,0.,0.981627005099017));
#92997=DIRECTION('center_axis',(0.981627005099017,-4.46817620651805E-17,
0.190809912898503));
#92998=DIRECTION('ref_axis',(-0.185253518835601,0.239566527818698,0.953041978355581));
#92999=DIRECTION('center_axis',(0.981627005099017,1.14649557620665E-16,
0.190809912898504));
#93000=DIRECTION('ref_axis',(-0.185466477867897,0.234997270615096,0.954137552133199));
#93001=DIRECTION('center_axis',(0.,1.,0.));
#93002=DIRECTION('ref_axis',(1.,0.,0.));
#93003=DIRECTION('',(-0.190809912898503,0.,0.981627005099017));
#93004=DIRECTION('center_axis',(0.,1.,0.));
#93005=DIRECTION('ref_axis',(-0.177714334075482,0.,0.984082118252388));
#93006=DIRECTION('center_axis',(0.,1.,0.));
#93007=DIRECTION('ref_axis',(-0.177978632904428,0.,0.984034352159248));
#93008=DIRECTION('center_axis',(-0.981627005099017,0.,-0.190809912898503));
#93009=DIRECTION('ref_axis',(-0.190809912898503,0.,0.981627005099017));
#93010=DIRECTION('center_axis',(-0.981627005099017,-6.68964416434522E-17,
-0.190809912898504));
#93011=DIRECTION('ref_axis',(-0.186677250480035,0.206997512266798,0.960366406153699));
#93012=DIRECTION('center_axis',(-0.981627005099017,-1.14441817944589E-16,
-0.190809912898504));
#93013=DIRECTION('ref_axis',(-0.186834767627011,0.203056667686805,0.961176757580879));
#93014=DIRECTION('center_axis',(0.,-1.,0.));
#93015=DIRECTION('ref_axis',(0.,0.,-1.));
#93016=DIRECTION('',(-0.190809912898503,0.,0.981627005099017));
#93017=DIRECTION('center_axis',(0.,-1.,0.));
#93018=DIRECTION('ref_axis',(-0.0792738467656748,0.,0.99685287641606));
#93019=DIRECTION('',(-0.190809912898503,0.,0.981627005099017));
#93020=DIRECTION('center_axis',(0.,-1.,0.));
#93021=DIRECTION('ref_axis',(-0.0815128335683136,0.,0.996672292162105));
#93022=DIRECTION('center_axis',(0.981627005099017,0.,0.190809912898503));
#93023=DIRECTION('ref_axis',(0.,-1.,0.));
#93024=DIRECTION('',(-0.190809912898503,0.,0.981627005099017));
#93025=DIRECTION('center_axis',(0.981627005099017,2.25679470404183E-17,
0.190809912898503));
#93026=DIRECTION('ref_axis',(-0.185196189525605,0.240780891147295,0.9527470460954));
#93027=DIRECTION('center_axis',(0.981627005099017,-1.44712955763978E-17,
0.190809912898503));
#93028=DIRECTION('ref_axis',(-0.185413480709429,0.236143136345897,0.953864906749345));
#93029=DIRECTION('center_axis',(0.,1.,0.));
#93030=DIRECTION('ref_axis',(1.,0.,0.));
#93031=DIRECTION('',(-0.190809912898503,0.,0.981627005099017));
#93032=DIRECTION('center_axis',(0.,1.,0.));
#93033=DIRECTION('ref_axis',(-0.111727396157644,0.,0.993738893748168));
#93034=DIRECTION('center_axis',(0.,1.,0.));
#93035=DIRECTION('ref_axis',(-0.113333541028712,0.,0.993556998102219));
#93036=DIRECTION('center_axis',(-0.981627005099017,0.,-0.190809912898503));
#93037=DIRECTION('ref_axis',(-0.190809912898503,0.,0.981627005099017));
#93038=DIRECTION('center_axis',(-0.981627005099017,-1.12151063898178E-16,
-0.190809912898504));
#93039=DIRECTION('ref_axis',(-0.186652627005605,0.207606497435908,0.960239729991579));
#93040=DIRECTION('center_axis',(-0.981627005099017,-1.43863256786093E-16,
-0.190809912898504));
#93041=DIRECTION('ref_axis',(-0.186811990818403,0.203631433275501,0.961059581643423));
#93042=DIRECTION('center_axis',(0.,-1.,0.));
#93043=DIRECTION('ref_axis',(0.,0.,-1.));
#93044=DIRECTION('',(-0.190809912898503,0.,0.981627005099017));
#93045=DIRECTION('center_axis',(0.,-1.,0.));
#93046=DIRECTION('ref_axis',(-0.0125199473708714,0.,0.99992162238739));
#93047=DIRECTION('',(-0.190809912898503,0.,0.981627005099017));
#93048=DIRECTION('center_axis',(0.,-1.,0.));
#93049=DIRECTION('ref_axis',(-0.0161217085140551,0.,0.999870036812079));
#93050=DIRECTION('center_axis',(0.981627005099017,0.,0.190809912898503));
#93051=DIRECTION('ref_axis',(0.,-1.,0.));
#93052=DIRECTION('',(-0.190809912898503,0.,0.981627005099017));
#93053=DIRECTION('center_axis',(0.981627005099017,-4.59929004743199E-17,
0.190809912898503));
#93054=DIRECTION('ref_axis',(-0.185087953259993,0.243056025486103,0.952190221559183));
#93055=DIRECTION('center_axis',(0.981627005099017,0.,0.190809912898503));
#93056=DIRECTION('ref_axis',(-0.18531353769894,0.238288156967503,0.953350747099164));
#93057=DIRECTION('center_axis',(0.,1.,0.));
#93058=DIRECTION('ref_axis',(1.,0.,0.));
#93059=DIRECTION('',(-0.190809912898503,0.,0.981627005099017));
#93060=DIRECTION('center_axis',(0.,1.,0.));
#93061=DIRECTION('ref_axis',(-0.0448845029220051,0.,0.998992182851019));
#93062=DIRECTION('center_axis',(0.,1.,0.));
#93063=DIRECTION('ref_axis',(-0.0478670082003263,0.,0.998853717781513));
#93064=DIRECTION('center_axis',(-0.981627005099017,0.,-0.190809912898503));
#93065=DIRECTION('ref_axis',(-0.190809912898503,0.,0.981627005099017));
#93066=DIRECTION('center_axis',(-0.981627005099017,-8.3438172080403E-17,
-0.190809912898504));
#93067=DIRECTION('ref_axis',(-0.1865915874356,0.209108130897699,0.959925710193624));
#93068=DIRECTION('center_axis',(-0.981627005099017,-1.09403704958442E-16,
-0.190809912898504));
#93069=DIRECTION('ref_axis',(-0.186755573580884,0.205047867688004,0.960769341565955));
#93070=DIRECTION('center_axis',(0.,-1.,0.));
#93071=DIRECTION('ref_axis',(0.,0.,-1.));
#93072=DIRECTION('',(-0.190809912898503,0.,0.981627005099017));
#93073=DIRECTION('center_axis',(0.,-1.,0.));
#93074=DIRECTION('ref_axis',(0.0551106337815708,0.,0.998480254208461));
#93075=DIRECTION('',(-0.190809912898503,0.,0.981627005099017));
#93076=DIRECTION('center_axis',(0.,-1.,0.));
#93077=DIRECTION('ref_axis',(0.0501099354614011,0.,0.998743708049294));
#93078=DIRECTION('center_axis',(0.981627005099017,0.,0.190809912898503));
#93079=DIRECTION('ref_axis',(0.,-1.,0.));
#93080=DIRECTION('',(-0.190809912898503,0.,0.981627005099017));
#93081=DIRECTION('center_axis',(0.981627005099017,1.7343040380955E-16,0.190809912898504));
#93082=DIRECTION('ref_axis',(-0.184922851173921,0.246483524320091,0.951340849197834));
#93083=DIRECTION('center_axis',(0.981627005099017,-6.05488295791281E-17,
0.190809912898503));
#93084=DIRECTION('ref_axis',(-0.185161373141239,0.241515217748391,0.952567932219219));
#93085=DIRECTION('center_axis',(0.,1.,0.));
#93086=DIRECTION('ref_axis',(1.,0.,0.));
#93087=DIRECTION('',(-0.190809912898503,0.,0.981627005099017));
#93088=DIRECTION('center_axis',(0.,1.,0.));
#93089=DIRECTION('ref_axis',(0.0228343129577635,0.,0.999739263084004));
#93090=DIRECTION('center_axis',(0.,1.,0.));
#93091=DIRECTION('ref_axis',(0.018439340499448,0.,0.999829980907727));
#93092=DIRECTION('center_axis',(-0.981627005099017,0.,-0.190809912898503));
#93093=DIRECTION('ref_axis',(-0.190809912898503,0.,0.981627005099017));
#93094=DIRECTION('center_axis',(-0.981627005099017,-6.21145914153305E-17,
-0.190809912898504));
#93095=DIRECTION('ref_axis',(-0.186490869672513,0.211561527977992,0.959407564806744));
#93096=DIRECTION('center_axis',(-0.981627005099017,-1.8647400464012E-16,
-0.190809912898504));
#93097=DIRECTION('ref_axis',(-0.186662621580147,0.207359538000907,0.960291147363589));
#93098=DIRECTION('center_axis',(0.,-1.,0.));
#93099=DIRECTION('ref_axis',(0.,0.,-1.));
#93100=DIRECTION('',(-0.190809912898503,0.,0.981627005099017));
#93101=DIRECTION('center_axis',(0.,-1.,0.));
#93102=DIRECTION('ref_axis',(0.0521902993854495,0.,0.9986371576554));
#93103=DIRECTION('',(-0.190809912898503,0.,0.981627005099017));
#93104=DIRECTION('center_axis',(0.,-1.,0.));
#93105=DIRECTION('ref_axis',(0.047360966192575,0.,0.998877839818917));
#93106=DIRECTION('center_axis',(0.981627005099017,0.,0.190809912898503));
#93107=DIRECTION('ref_axis',(0.,-1.,0.));
#93108=DIRECTION('',(-0.190809912898503,0.,0.981627005099017));
#93109=DIRECTION('center_axis',(0.981627005099017,-3.9416000865807E-18,
0.190809912898503));
#93110=DIRECTION('ref_axis',(-0.187698004760385,0.179866355585003,0.965617705480559));
#93111=DIRECTION('center_axis',(0.981627005099017,8.32546406713011E-17,
0.190809912898504));
#93112=DIRECTION('ref_axis',(-0.187823180046607,0.176240834573197,0.966261673288413));
#93113=DIRECTION('center_axis',(0.,1.,0.));
#93114=DIRECTION('ref_axis',(1.,0.,0.));
#93115=DIRECTION('',(-0.190809912898503,0.,0.981627005099017));
#93116=DIRECTION('center_axis',(0.,1.,0.));
#93117=DIRECTION('ref_axis',(0.0198019381976702,0.,0.999803922398595));
#93118=DIRECTION('center_axis',(0.,1.,0.));
#93119=DIRECTION('ref_axis',(0.015586695628152,0.,0.999878520081012));
#93120=DIRECTION('center_axis',(-0.981627005099017,0.,-0.190809912898503));
#93121=DIRECTION('ref_axis',(-0.190809912898503,0.,0.981627005099017));
#93122=DIRECTION('center_axis',(-0.981627005099017,-1.08700534976828E-16,
-0.190809912898504));
#93123=DIRECTION('ref_axis',(-0.188780805300353,0.145448550484899,0.971188203548618));
#93124=DIRECTION('center_axis',(-0.981627005099017,-7.45896018560482E-17,
-0.190809912898504));
#93125=DIRECTION('ref_axis',(-0.188861020080131,0.142559682375593,0.971600870756744));
#93126=DIRECTION('center_axis',(0.,-1.,0.));
#93127=DIRECTION('ref_axis',(0.,0.,-1.));
#93128=DIRECTION('',(-0.190809912898503,0.,0.981627005099017));
#93129=DIRECTION('center_axis',(0.,-1.,0.));
#93130=DIRECTION('ref_axis',(0.0504037002691461,0.,0.998728925684631));
#93131=DIRECTION('',(-0.190809912898503,0.,0.981627005099017));
#93132=DIRECTION('center_axis',(0.,-1.,0.));
#93133=DIRECTION('ref_axis',(0.0456773194928813,0.,0.998956246531321));
#93134=DIRECTION('center_axis',(0.981627005099017,0.,0.190809912898503));
#93135=DIRECTION('ref_axis',(0.,-1.,0.));
#93136=DIRECTION('',(-0.190809912898503,0.,0.981627005099017));
#93137=DIRECTION('center_axis',(0.981627005099017,2.75912006060649E-17,
0.190809912898504));
#93138=DIRECTION('ref_axis',(-0.189582359577673,0.113249186849803,0.975311822247029));
#93139=DIRECTION('center_axis',(0.981627005099017,3.0274414789564E-17,0.190809912898504));
#93140=DIRECTION('ref_axis',(-0.189631500029847,0.110966451397898,0.975564626696042));
#93141=DIRECTION('center_axis',(0.,1.,0.));
#93142=DIRECTION('ref_axis',(1.,0.,0.));
#93143=DIRECTION('',(-0.190809912898503,0.,0.981627005099017));
#93144=DIRECTION('center_axis',(0.,1.,0.));
#93145=DIRECTION('ref_axis',(0.0177900737106688,0.,0.999841744116222));
#93146=DIRECTION('center_axis',(0.,1.,0.));
#93147=DIRECTION('ref_axis',(0.0136914263007247,0.,0.999906268030085));
#93148=DIRECTION('center_axis',(-0.981627005099017,0.,-0.190809912898503));
#93149=DIRECTION('ref_axis',(-0.190809912898503,0.,0.981627005099017));
#93150=DIRECTION('center_axis',(-0.981627005099017,3.29983766893944E-17,
-0.190809912898503));
#93151=DIRECTION('ref_axis',(-0.190208473521459,0.0793355729917432,0.978532883177008));
#93152=DIRECTION('center_axis',(-0.981627005099017,-3.17005807888205E-17,
-0.190809912898504));
#93153=DIRECTION('ref_axis',(-0.190232163502544,0.077759826750329,0.97865475695615));
#93154=DIRECTION('center_axis',(0.,-1.,0.));
#93155=DIRECTION('ref_axis',(0.,0.,-1.));
#93156=DIRECTION('',(-0.190809912898503,0.,0.981627005099017));
#93157=DIRECTION('center_axis',(0.,-1.,0.));
#93158=DIRECTION('ref_axis',(0.049679326965256,0.,0.998765219895186));
#93159=DIRECTION('',(-0.190809912898503,0.,0.981627005099017));
#93160=DIRECTION('center_axis',(0.,-1.,0.));
#93161=DIRECTION('ref_axis',(0.0449942826424662,0.,0.99898724442782));
#93162=DIRECTION('center_axis',(0.981627005099017,0.,0.190809912898503));
#93163=DIRECTION('ref_axis',(0.,-1.,0.));
#93164=DIRECTION('',(-0.190809912898503,0.,0.981627005099017));
#93165=DIRECTION('center_axis',(0.981627005099017,-9.85400021645174E-19,
0.190809912898503));
#93166=DIRECTION('ref_axis',(-0.190602337609787,0.0466320181146215,0.980559128142838));
#93167=DIRECTION('center_axis',(0.981627005099017,1.70293583191298E-17,
0.190809912898504));
#93168=DIRECTION('ref_axis',(-0.190610625689641,0.0456920682226691,0.980601766404558));
#93169=DIRECTION('center_axis',(0.,1.,0.));
#93170=DIRECTION('ref_axis',(1.,0.,0.));
#93171=DIRECTION('',(-0.190809912898503,0.,0.981627005099017));
#93172=DIRECTION('center_axis',(0.,1.,0.));
#93173=DIRECTION('ref_axis',(0.0167165551221656,0.,0.999860268629996));
#93174=DIRECTION('center_axis',(0.,1.,0.));
#93175=DIRECTION('ref_axis',(0.0126792641246964,0.,0.999919614899746));
#93176=DIRECTION('center_axis',(-0.981627005099017,0.,-0.190809912898503));
#93177=DIRECTION('ref_axis',(-0.190809912898503,0.,0.981627005099017));
#93178=DIRECTION('center_axis',(-0.981627005099017,-1.45581073629681E-18,
-0.190809912898503));
#93179=DIRECTION('ref_axis',(-0.190793231849958,0.0132225954986201,0.98154118897198));
#93180=DIRECTION('center_axis',(-0.981627005099017,3.26329508120211E-18,
-0.190809912898503));
#93181=DIRECTION('ref_axis',(-0.190793887927854,0.0129599711250496,0.981544564183314));
#93182=DIRECTION('center_axis',(0.,-1.,0.));
#93183=DIRECTION('ref_axis',(0.,0.,-1.));
#93184=DIRECTION('',(-0.190809912898503,0.,0.981627005099017));
#93185=DIRECTION('center_axis',(0.,-1.,0.));
#93186=DIRECTION('ref_axis',(-0.272681755189035,0.,0.962104287687685));
#93187=DIRECTION('',(-0.190809912898503,0.,0.981627005099017));
#93188=DIRECTION('center_axis',(0.,-1.,0.));
#93189=DIRECTION('ref_axis',(-0.271135734555198,0.,0.962541122990188));
#93190=DIRECTION('center_axis',(0.981627005099017,0.,0.190809912898503));
#93191=DIRECTION('ref_axis',(0.,-1.,0.));
#93192=DIRECTION('',(-0.190809912898503,0.,0.981627005099017));
#93193=DIRECTION('center_axis',(0.981627005099017,3.36807599940008E-17,
0.190809912898504));
#93194=DIRECTION('ref_axis',(-0.190612838364399,0.0454378337517089,0.980613149572562));
#93195=DIRECTION('center_axis',(0.981627005099017,0.,0.190809912898503));
#93196=DIRECTION('ref_axis',(-0.190620324225006,0.0445669403603487,0.980651660794632));
#93197=DIRECTION('center_axis',(0.,1.,0.));
#93198=DIRECTION('ref_axis',(1.,0.,0.));
#93199=DIRECTION('',(-0.190809912898503,0.,0.981627005099017));
#93200=DIRECTION('center_axis',(0.,1.,0.));
#93201=DIRECTION('ref_axis',(-0.303914183891769,0.,0.952699411582373));
#93202=DIRECTION('center_axis',(0.,1.,0.));
#93203=DIRECTION('ref_axis',(-0.301781433815546,0.,0.95337713744574));
#93204=DIRECTION('center_axis',(-0.981627005099017,0.,-0.190809912898503));
#93205=DIRECTION('ref_axis',(-0.190809912898503,0.,0.981627005099017));
#93206=DIRECTION('center_axis',(-0.981627005099017,-5.17949828132746E-18,
-0.190809912898504));
#93207=DIRECTION('ref_axis',(-0.190793727100074,0.0130248396339095,0.981543736800237));
#93208=DIRECTION('center_axis',(-0.981627005099017,3.17011540663208E-18,
-0.190809912898503));
#93209=DIRECTION('ref_axis',(-0.190794345521308,0.0127736024962302,0.981546918285807));
#93210=DIRECTION('center_axis',(0.,-1.,0.));
#93211=DIRECTION('ref_axis',(0.,0.,-1.));
#93212=DIRECTION('',(-0.190809912898503,0.,0.981627005099017));
#93213=DIRECTION('center_axis',(0.,-1.,0.));
#93214=DIRECTION('ref_axis',(-0.272920620201063,0.,0.962036555994141));
#93215=DIRECTION('',(-0.190809912898515,0.,0.981627005099015));
#93216=DIRECTION('center_axis',(0.,-1.,0.));
#93217=DIRECTION('ref_axis',(-0.271361249859389,0.,0.9624775696476));
#93218=DIRECTION('center_axis',(0.981627005099017,0.,0.190809912898503));
#93219=DIRECTION('ref_axis',(0.,-1.,0.));
#93220=DIRECTION('',(-0.190809912898503,0.,0.981627005099017));
#93221=DIRECTION('center_axis',(0.981627005099017,1.12269199980003E-17,
0.190809912898503));
#93222=DIRECTION('ref_axis',(-0.18964461730024,0.110349024825598,0.975632108865368));
#93223=DIRECTION('center_axis',(0.981627005099017,5.40033915023846E-17,
0.190809912898504));
#93224=DIRECTION('ref_axis',(-0.189688989693149,0.108233998017997,0.975860383898349));
#93225=DIRECTION('center_axis',(0.,1.,0.));
#93226=DIRECTION('ref_axis',(1.,0.,0.));
#93227=DIRECTION('',(-0.190809912898503,0.,0.981627005099017));
#93228=DIRECTION('center_axis',(0.,1.,0.));
#93229=DIRECTION('ref_axis',(-0.304480839231191,0.,0.952518460997512));
#93230=DIRECTION('center_axis',(0.,1.,0.));
#93231=DIRECTION('ref_axis',(-0.302316369370631,0.,0.953207644120923));
#93232=DIRECTION('center_axis',(-0.981627005099017,0.,-0.190809912898503));
#93233=DIRECTION('ref_axis',(-0.190809912898503,0.,0.981627005099017));
#93234=DIRECTION('center_axis',(-0.981627005099017,-4.70863480120678E-17,
-0.190809912898504));
#93235=DIRECTION('ref_axis',(-0.190226356519923,0.0781490378034625,0.978624882769465));
#93236=DIRECTION('center_axis',(-0.981627005099017,9.05747259037737E-18,
-0.190809912898503));
#93237=DIRECTION('ref_axis',(-0.190248684812419,0.0766416149774004,0.978739751303073));
#93238=DIRECTION('center_axis',(0.,-1.,0.));
#93239=DIRECTION('ref_axis',(0.,0.,-1.));
#93240=DIRECTION('',(-0.190809912898503,1.022228972926E-14,0.981627005099017));
#93241=DIRECTION('center_axis',(0.,-1.,0.));
#93242=DIRECTION('ref_axis',(-0.273509562255009,0.,0.961869283923275));
#93243=DIRECTION('',(-0.190809912898503,0.,0.981627005099017));
#93244=DIRECTION('center_axis',(0.,-1.,0.));
#93245=DIRECTION('ref_axis',(-0.271916957880207,0.,0.962320719935497));
#93246=DIRECTION('center_axis',(0.981627005099017,0.,0.190809912898503));
#93247=DIRECTION('ref_axis',(0.,-1.,0.));
#93248=DIRECTION('',(-0.190809912898503,0.,0.981627005099017));
#93249=DIRECTION('center_axis',(0.981627005099017,5.61345999900013E-17,
0.190809912898504));
#93250=DIRECTION('ref_axis',(-0.187856584998405,0.175260215899398,0.966433526009748));
#93251=DIRECTION('center_axis',(0.981627005099017,-1.80011305007949E-17,
0.190809912898503));
#93252=DIRECTION('ref_axis',(-0.187969558572489,0.171901055675604,0.967014721763674));
#93253=DIRECTION('center_axis',(0.,1.,0.));
#93254=DIRECTION('ref_axis',(1.,0.,0.));
#93255=DIRECTION('',(-0.190809912898503,0.,0.981627005099017));
#93256=DIRECTION('center_axis',(0.,1.,0.));
#93257=DIRECTION('ref_axis',(-0.305542296483778,0.,0.95217850482954));
#93258=DIRECTION('center_axis',(0.,1.,0.));
#93259=DIRECTION('ref_axis',(-0.303317587437942,0.,0.952889522007051));
#93260=DIRECTION('center_axis',(-0.981627005099017,0.,-0.190809912898503));
#93261=DIRECTION('ref_axis',(-0.190809912898503,0.,0.981627005099017));
#93262=DIRECTION('center_axis',(-0.981627005099017,-7.53381568193085E-17,
-0.190809912898504));
#93263=DIRECTION('ref_axis',(-0.18884135974173,0.143273235972994,0.971499727588599));
#93264=DIRECTION('center_axis',(-0.981627005099017,-1.44919561446038E-17,
-0.190809912898503));
#93265=DIRECTION('ref_axis',(-0.188916947337466,0.140509627458605,0.971888590117271));
#93266=DIRECTION('center_axis',(0.,-1.,0.));
#93267=DIRECTION('ref_axis',(0.,0.,-1.));
#93268=DIRECTION('',(-0.190809912898503,0.,0.981627005099017));
#93269=DIRECTION('center_axis',(0.,-1.,0.));
#93270=DIRECTION('ref_axis',(-0.210016949218452,0.,0.977697745236724));
#93271=DIRECTION('',(-0.190809912898503,0.,0.981627005099017));
#93272=DIRECTION('center_axis',(0.,-1.,0.));
#93273=DIRECTION('ref_axis',(-0.209644703523565,0.,0.977777632329824));
#93274=DIRECTION('center_axis',(0.981627005099017,0.,0.190809912898503));
#93275=DIRECTION('ref_axis',(0.,-1.,0.));
#93276=DIRECTION('',(-0.190809912898503,0.,0.981627005099017));
#93277=DIRECTION('center_axis',(0.981627005099017,4.08897136708722E-17,
0.190809912898503));
#93278=DIRECTION('ref_axis',(-0.187876516051428,0.1746724242913,0.966536061876937));
#93279=DIRECTION('center_axis',(0.981627005099017,2.11044591057748E-16,
0.190809912898504));
#93280=DIRECTION('ref_axis',(-0.187987998623376,0.1713463126492,0.967109587128108));
#93281=DIRECTION('center_axis',(0.,1.,0.));
#93282=DIRECTION('ref_axis',(1.,0.,0.));
#93283=DIRECTION('',(-0.190809912898503,0.,0.981627005099017));
#93284=DIRECTION('center_axis',(0.,1.,0.));
#93285=DIRECTION('ref_axis',(-0.242133347595446,0.,0.970242980898199));
#93286=DIRECTION('center_axis',(0.,1.,0.));
#93287=DIRECTION('ref_axis',(-0.241131647472688,0.,0.970492415522712));
#93288=DIRECTION('center_axis',(-0.981627005099017,0.,-0.190809912898503));
#93289=DIRECTION('ref_axis',(-0.190809912898503,0.,0.981627005099017));
#93290=DIRECTION('center_axis',(-0.981627005099017,2.60807618282638E-17,
-0.190809912898503));
#93291=DIRECTION('ref_axis',(-0.188862940934346,0.142489771158805,0.971610752645699));
#93292=DIRECTION('center_axis',(-0.981627005099017,-7.88692931673802E-17,
-0.190809912898504));
#93293=DIRECTION('ref_axis',(-0.188936911383774,0.139770399450607,0.971991295719348));
#93294=DIRECTION('center_axis',(0.,-1.,0.));
#93295=DIRECTION('ref_axis',(0.,0.,-1.));
#93296=DIRECTION('',(-0.190809912898503,1.171213937656E-14,0.981627005099017));
#93297=DIRECTION('center_axis',(0.,-1.,0.));
#93298=DIRECTION('ref_axis',(-0.145708207453926,0.,0.989327609177346));
#93299=DIRECTION('',(-0.190809912898503,0.,0.981627005099017));
#93300=DIRECTION('center_axis',(0.,-1.,0.));
#93301=DIRECTION('ref_axis',(-0.146587756234231,0.,0.989197669691055));
#93302=DIRECTION('center_axis',(0.981627005099017,0.,0.190809912898503));
#93303=DIRECTION('ref_axis',(0.,-1.,0.));
#93304=DIRECTION('',(-0.190809912898503,0.,0.981627005099017));
#93305=DIRECTION('center_axis',(0.981627005099017,3.35113215488854E-17,
0.190809912898503));
#93306=DIRECTION('ref_axis',(-0.187871558552619,0.174818817597398,0.966510557883802));
#93307=DIRECTION('center_axis',(0.981627005099017,-3.5827986756458E-18,
0.190809912898503));
#93308=DIRECTION('ref_axis',(-0.187983411095129,0.171484494773204,0.967085986459022));
#93309=DIRECTION('center_axis',(0.,1.,0.));
#93310=DIRECTION('ref_axis',(1.,0.,0.));
#93311=DIRECTION('',(-0.190809912898503,-1.31207553052E-14,0.981627005099017));
#93312=DIRECTION('center_axis',(0.,1.,0.));
#93313=DIRECTION('ref_axis',(-0.177896668082247,0.,0.984049173306515));
#93314=DIRECTION('center_axis',(0.,1.,0.));
#93315=DIRECTION('ref_axis',(-0.178150295368446,0.,0.984003288744573));
#93316=DIRECTION('center_axis',(-0.981627005099017,0.,-0.190809912898503));
#93317=DIRECTION('ref_axis',(-0.190809912898503,0.,0.981627005099017));
#93318=DIRECTION('center_axis',(-0.981627005099017,5.94635036830686E-17,
-0.190809912898503));
#93319=DIRECTION('ref_axis',(-0.188867854179084,0.142310789683404,0.971636028972513));
#93320=DIRECTION('center_axis',(-0.981627005099017,-3.5763068107684E-17,
-0.190809912898504));
#93321=DIRECTION('ref_axis',(-0.18894145881405,0.139601459034696,0.972014690103294));
#93322=DIRECTION('center_axis',(0.,-1.,0.));
#93323=DIRECTION('ref_axis',(0.,0.,-1.));
#93324=DIRECTION('',(-0.190809912898503,0.,0.981627005099017));
#93325=DIRECTION('center_axis',(0.,-1.,0.));
#93326=DIRECTION('ref_axis',(-0.080581231656937,0.,0.99674804494649));
#93327=DIRECTION('',(-0.190809912898503,0.,0.981627005099017));
#93328=DIRECTION('center_axis',(0.,-1.,0.));
#93329=DIRECTION('ref_axis',(-0.0827441701585023,0.,0.996570821519866));
#93330=DIRECTION('center_axis',(0.981627005099017,0.,0.190809912898503));
#93331=DIRECTION('ref_axis',(0.,-1.,0.));
#93332=DIRECTION('',(-0.190809912898503,1.014331218259E-14,0.981627005099017));
#93333=DIRECTION('center_axis',(0.981627005099017,3.38519205606274E-17,
0.190809912898503));
#93334=DIRECTION('ref_axis',(-0.187841458045623,0.175704974621005,0.966355704972412));
#93335=DIRECTION('center_axis',(0.981627005099017,1.01299069034784E-16,
0.190809912898504));
#93336=DIRECTION('ref_axis',(-0.187955569592477,0.172320667063197,0.966942755059503));
#93337=DIRECTION('center_axis',(0.,1.,0.));
#93338=DIRECTION('ref_axis',(1.,0.,0.));
#93339=DIRECTION('',(-0.190809912898503,0.,0.981627005099017));
#93340=DIRECTION('center_axis',(0.,1.,0.));
#93341=DIRECTION('ref_axis',(-0.11283548507849,0.,0.993613684138409));
#93342=DIRECTION('center_axis',(0.,1.,0.));
#93343=DIRECTION('ref_axis',(-0.11437651133568,0.,0.99343747344998));
#93344=DIRECTION('center_axis',(-0.981627005099017,0.,-0.190809912898503));
#93345=DIRECTION('ref_axis',(-0.190809912898503,0.,0.981627005099017));
#93346=DIRECTION('center_axis',(-0.981627005099017,-7.10290071355126E-17,
-0.190809912898504));
#93347=DIRECTION('ref_axis',(-0.188856351138037,0.142729466987203,0.971576851251807));
#93348=DIRECTION('center_axis',(-0.981627005099017,-1.11494024009222E-16,
-0.190809912898504));
#93349=DIRECTION('ref_axis',(-0.188930813598223,0.1399966103769,0.971959925488748));
#93350=DIRECTION('center_axis',(0.,-1.,0.));
#93351=DIRECTION('ref_axis',(0.,0.,-1.));
#93352=DIRECTION('',(-0.190809912898503,0.,0.981627005099017));
#93353=DIRECTION('center_axis',(0.,-1.,0.));
#93354=DIRECTION('ref_axis',(-0.0146231970935999,0.,0.999893075336939));
#93355=DIRECTION('',(-0.190809912898503,0.,0.981627005099017));
#93356=DIRECTION('center_axis',(0.,-1.,0.));
#93357=DIRECTION('ref_axis',(-0.0181020988785695,0.,0.999836143583633));
#93358=DIRECTION('center_axis',(0.981627005099017,0.,0.190809912898503));
#93359=DIRECTION('ref_axis',(0.,-1.,0.));
#93360=DIRECTION('',(-0.190809912898503,0.,0.981627005099017));
#93361=DIRECTION('center_axis',(0.981627005099017,3.83274170619332E-18,
0.190809912898503));
#93362=DIRECTION('ref_axis',(-0.187784641315811,0.177365207787101,0.966063409695518));
#93363=DIRECTION('center_axis',(0.981627005099017,-9.57800442010027E-17,
0.190809912898503));
#93364=DIRECTION('ref_axis',(-0.187903076011377,0.173885952381692,0.966672700343697));
#93365=DIRECTION('center_axis',(0.,1.,0.));
#93366=DIRECTION('ref_axis',(1.,0.,0.));
#93367=DIRECTION('',(-0.190809912898503,0.,0.981627005099017));
#93368=DIRECTION('center_axis',(0.,1.,0.));
#93369=DIRECTION('ref_axis',(-0.0469422356412144,0.,0.998897605619818));
#93370=DIRECTION('center_axis',(0.,1.,0.));
#93371=DIRECTION('ref_axis',(-0.049803312308202,0.,0.998759045056981));
#93372=DIRECTION('center_axis',(-0.981627005099017,0.,-0.190809912898503));
#93373=DIRECTION('ref_axis',(-0.190809912898503,0.,0.981627005099017));
#93374=DIRECTION('center_axis',(-0.981627005099017,-3.79264418547286E-18,
-0.190809912898503));
#93375=DIRECTION('ref_axis',(-0.18882783956697,0.143761839992095,0.971430172666341));
#93376=DIRECTION('center_axis',(-0.981627005099017,4.74082721486581E-17,
-0.190809912898503));
#93377=DIRECTION('ref_axis',(-0.188904448833758,0.140970409035506,0.971824291210698));
#93378=DIRECTION('center_axis',(0.,-1.,0.));
#93379=DIRECTION('ref_axis',(0.,0.,-1.));
#93380=DIRECTION('',(-0.190809912898503,0.,0.981627005099017));
#93381=DIRECTION('center_axis',(0.,-1.,0.));
#93382=DIRECTION('ref_axis',(-0.0159100952935859,0.,0.999873426423439));
#93383=DIRECTION('',(-0.190809912898503,0.,0.981627005099017));
#93384=DIRECTION('center_axis',(0.,-1.,0.));
#93385=DIRECTION('ref_axis',(-0.0193151720218505,0.,0.999813444663436));
#93386=DIRECTION('center_axis',(0.981627005099017,0.,0.190809912898503));
#93387=DIRECTION('ref_axis',(0.,-1.,0.));
#93388=DIRECTION('',(-0.190809912898503,0.,0.981627005099017));
#93389=DIRECTION('center_axis',(0.981627005099017,8.04875758300598E-17,
0.190809912898504));
#93390=DIRECTION('ref_axis',(-0.18961636862676,0.111674390088199,0.975486782763985));
#93391=DIRECTION('center_axis',(0.981627005099017,7.36769570776943E-18,
0.190809912898503));
#93392=DIRECTION('ref_axis',(-0.189662875504316,0.109483747795895,0.975726038713736));
#93393=DIRECTION('center_axis',(0.,1.,0.));
#93394=DIRECTION('ref_axis',(1.,0.,0.));
#93395=DIRECTION('',(-0.190809912898503,0.,0.981627005099017));
#93396=DIRECTION('center_axis',(0.,1.,0.));
#93397=DIRECTION('ref_axis',(-0.0483076832324515,0.,0.998832502344969));
#93398=DIRECTION('center_axis',(0.,1.,0.));
#93399=DIRECTION('ref_axis',(-0.051089968923592,0.,0.998694054791249));
#93400=DIRECTION('center_axis',(-0.981627005099017,0.,-0.190809912898503));
#93401=DIRECTION('ref_axis',(-0.190809912898503,0.,0.981627005099017));
#93402=DIRECTION('center_axis',(-0.981627005099017,-4.93043744111472E-17,
-0.190809912898504));
#93403=DIRECTION('ref_axis',(-0.190222363376804,0.0784155490866333,0.978604339931509));
#93404=DIRECTION('center_axis',(-0.981627005099017,-9.11697541320348E-18,
-0.190809912898503));
#93405=DIRECTION('ref_axis',(-0.190244992365523,0.0768929503830163,0.978720755405359));
#93406=DIRECTION('center_axis',(0.,-1.,0.));
#93407=DIRECTION('ref_axis',(0.,0.,-1.));
#93408=DIRECTION('',(-0.190809912898503,0.,0.981627005099017));
#93409=DIRECTION('center_axis',(0.,-1.,0.));
#93410=DIRECTION('ref_axis',(-0.0164319034129535,0.,0.99986498716088));
#93411=DIRECTION('',(-0.190809912898503,0.,0.981627005099017));
#93412=DIRECTION('center_axis',(0.,-1.,0.));
#93413=DIRECTION('ref_axis',(-0.0198073356643245,0.,0.999803815482758));
#93414=DIRECTION('center_axis',(0.981627005099017,0.,0.190809912898503));
#93415=DIRECTION('ref_axis',(0.,-1.,0.));
#93416=DIRECTION('',(-0.190809912898503,0.,0.981627005099017));
#93417=DIRECTION('center_axis',(0.981627005099017,2.20382648106116E-17,
0.190809912898504));
#93418=DIRECTION('ref_axis',(-0.190608073420958,0.0459835723892488,0.980588636185977));
#93419=DIRECTION('center_axis',(0.981627005099017,2.5786934977193E-17,0.190809912898504));
#93420=DIRECTION('ref_axis',(-0.19061591844487,0.0450815432100714,0.980628995133846));
#93421=DIRECTION('center_axis',(0.,1.,0.));
#93422=DIRECTION('ref_axis',(1.,0.,0.));
#93423=DIRECTION('',(-0.190809912898492,0.,0.981627005099019));
#93424=DIRECTION('center_axis',(0.,1.,0.));
#93425=DIRECTION('ref_axis',(-0.0490363496574017,0.,0.998796994595136));
#93426=DIRECTION('center_axis',(0.,1.,0.));
#93427=DIRECTION('ref_axis',(-0.0517771672578115,0.,0.998658662882747));
#93428=DIRECTION('center_axis',(-0.981627005099017,0.,-0.190809912898503));
#93429=DIRECTION('ref_axis',(-0.190809912898503,0.,0.981627005099017));
#93430=DIRECTION('center_axis',(-0.981627005099017,-1.09038520332345E-17,
-0.190809912898504));
#93431=DIRECTION('ref_axis',(-0.19079361651041,0.0130692581810996,0.981543167868573));
#93432=DIRECTION('center_axis',(-0.981627005099017,-8.20527787188313E-18,
-0.190809912898504));
#93433=DIRECTION('ref_axis',(-0.190794243247643,0.0128154917304995,0.981546392136034));
#93434=DIRECTION('center_axis',(0.,-1.,0.));
#93435=DIRECTION('ref_axis',(0.,0.,-1.));
#93436=DIRECTION('',(-0.190809912898503,0.,0.981627005099017));
#93437=DIRECTION('center_axis',(0.,-1.,0.));
#93438=DIRECTION('ref_axis',(-0.209823450757741,0.,0.977739290154647));
#93439=DIRECTION('',(-0.190809912898503,0.,0.981627005099017));
#93440=DIRECTION('center_axis',(0.,-1.,0.));
#93441=DIRECTION('ref_axis',(-0.209462139823336,0.,0.97781675787472));
#93442=DIRECTION('center_axis',(0.981627005099017,0.,0.190809912898503));
#93443=DIRECTION('ref_axis',(0.,-1.,0.));
#93444=DIRECTION('',(-0.190809912898503,0.,0.981627005099017));
#93445=DIRECTION('center_axis',(0.981627005099017,2.78793502301401E-17,
0.190809912898504));
#93446=DIRECTION('ref_axis',(-0.190614158731227,0.0452854433347916,0.980619942237133));
#93447=DIRECTION('center_axis',(0.981627005099017,1.60966213518621E-17,
0.190809912898504));
#93448=DIRECTION('ref_axis',(-0.190621546499908,0.0444231180942404,0.980657948822508));
#93449=DIRECTION('center_axis',(0.,1.,0.));
#93450=DIRECTION('ref_axis',(1.,0.,0.));
#93451=DIRECTION('',(-0.190809912898503,0.,0.981627005099017));
#93452=DIRECTION('center_axis',(0.,1.,0.));
#93453=DIRECTION('ref_axis',(-0.241400245375673,0.,0.970425639362731));
#93454=DIRECTION('center_axis',(0.,1.,0.));
#93455=DIRECTION('ref_axis',(-0.240440133543875,0.,0.970663969755447));
#93456=DIRECTION('center_axis',(-0.981627005099017,0.,-0.190809912898503));
#93457=DIRECTION('ref_axis',(-0.190809912898503,0.,0.981627005099017));
#93458=DIRECTION('center_axis',(-0.981627005099017,-9.3145577958085E-18,
-0.190809912898504));
#93459=DIRECTION('ref_axis',(-0.19079390364194,0.0129536155598903,0.981544645024869));
#93460=DIRECTION('center_axis',(-0.981627005099017,-2.24060491952785E-18,
-0.190809912898503));
#93461=DIRECTION('ref_axis',(-0.190794508898482,0.0127063999500603,0.981547758784307));
#93462=DIRECTION('center_axis',(0.,-1.,0.));
#93463=DIRECTION('ref_axis',(0.,0.,-1.));
#93464=DIRECTION('',(-0.190809912898503,0.,0.981627005099017));
#93465=DIRECTION('center_axis',(0.,-1.,0.));
#93466=DIRECTION('ref_axis',(-0.209879282403704,0.,0.97772730698171));
#93467=DIRECTION('',(-0.190809912898503,0.,0.981627005099017));
#93468=DIRECTION('center_axis',(0.,-1.,0.));
#93469=DIRECTION('ref_axis',(-0.209514838041807,0.,0.977805467687881));
#93470=DIRECTION('center_axis',(0.981627005099017,0.,0.190809912898503));
#93471=DIRECTION('ref_axis',(0.,-1.,0.));
#93472=DIRECTION('',(-0.190809912898503,0.,0.981627005099017));
#93473=DIRECTION('center_axis',(0.981627005099017,7.80621806443923E-17,
0.190809912898504));
#93474=DIRECTION('ref_axis',(-0.189652444394023,0.109978933813099,0.975672375571178));
#93475=DIRECTION('center_axis',(0.981627005099017,-1.07310809012414E-17,
0.190809912898503));
#93476=DIRECTION('ref_axis',(-0.189696233899903,0.107884715371704,0.975897651925323));
#93477=DIRECTION('center_axis',(0.,1.,0.));
#93478=DIRECTION('ref_axis',(1.,0.,0.));
#93479=DIRECTION('',(-0.190809912898503,0.,0.981627005099017));
#93480=DIRECTION('center_axis',(0.,1.,0.));
#93481=DIRECTION('ref_axis',(-0.241655381132283,0.,0.970362136920959));
#93482=DIRECTION('center_axis',(0.,1.,0.));
#93483=DIRECTION('ref_axis',(-0.240680925308484,0.,0.970604292280151));
#93484=DIRECTION('center_axis',(-0.981627005099017,0.,-0.190809912898503));
#93485=DIRECTION('ref_axis',(-0.190809912898503,0.,0.981627005099017));
#93486=DIRECTION('center_axis',(-0.981627005099017,1.11774693549702E-17,
-0.190809912898503));
#93487=DIRECTION('ref_axis',(-0.190232730879222,0.0777216933593315,0.978657675841554));
#93488=DIRECTION('center_axis',(-0.981627005099017,-4.66045823261792E-17,
-0.190809912898504));
#93489=DIRECTION('ref_axis',(-0.190254583170978,0.0762383997003401,0.978770095575855));
#93490=DIRECTION('center_axis',(0.,-1.,0.));
#93491=DIRECTION('ref_axis',(0.,0.,-1.));
#93492=DIRECTION('',(-0.190809912898503,0.,0.981627005099017));
#93493=DIRECTION('center_axis',(0.,-1.,0.));
#93494=DIRECTION('ref_axis',(-0.146033514275245,0.,0.989279643330652));
#93495=DIRECTION('',(-0.190809912898503,0.,0.981627005099017));
#93496=DIRECTION('center_axis',(0.,-1.,0.));
#93497=DIRECTION('ref_axis',(-0.146894553814633,0.,0.989152157182908));
#93498=DIRECTION('center_axis',(0.981627005099017,0.,0.190809912898503));
#93499=DIRECTION('ref_axis',(0.,-1.,0.));
#93500=DIRECTION('',(-0.190809912898503,0.,0.981627005099017));
#93501=DIRECTION('center_axis',(0.981627005099017,4.46817620651804E-17,
0.190809912898504));
#93502=DIRECTION('ref_axis',(-0.189650497494737,0.110071107376204,0.975662359692622));
#93503=DIRECTION('center_axis',(0.981627005099017,3.94107854321037E-17,
0.190809912898504));
#93504=DIRECTION('ref_axis',(-0.18969443164073,0.107971718931196,0.975888380151922));
#93505=DIRECTION('center_axis',(0.,1.,0.));
#93506=DIRECTION('ref_axis',(1.,0.,0.));
#93507=DIRECTION('',(-0.190809912898503,0.,0.981627005099017));
#93508=DIRECTION('center_axis',(0.,1.,0.));
#93509=DIRECTION('ref_axis',(-0.178017695683024,0.,0.98402728621909));
#93510=DIRECTION('center_axis',(0.,1.,0.));
#93511=DIRECTION('ref_axis',(-0.178264395839964,0.,0.983982624427796));
#93512=DIRECTION('center_axis',(-0.981627005099017,0.,-0.190809912898503));
#93513=DIRECTION('ref_axis',(-0.190809912898503,0.,0.981627005099017));
#93514=DIRECTION('center_axis',(-0.981627005099017,-7.43293796038357E-18,
-0.190809912898503));
#93515=DIRECTION('ref_axis',(-0.190234182158607,0.0776240671000532,0.978665141989482));
#93516=DIRECTION('center_axis',(-0.981627005099017,-1.43052272430736E-17,
-0.190809912898503));
#93517=DIRECTION('ref_axis',(-0.190255926766526,0.0761462503825465,0.978777007741237));
#93518=DIRECTION('center_axis',(0.,-1.,0.));
#93519=DIRECTION('ref_axis',(0.,0.,-1.));
#93520=DIRECTION('',(-0.190809912898503,0.,0.981627005099017));
#93521=DIRECTION('center_axis',(0.,-1.,0.));
#93522=DIRECTION('ref_axis',(-0.081381270585825,0.,0.996683043298037));
#93523=DIRECTION('',(-0.190809912898503,0.,0.981627005099017));
#93524=DIRECTION('center_axis',(0.,-1.,0.));
#93525=DIRECTION('ref_axis',(-0.0834985047492355,0.,0.996507902479776));
#93526=DIRECTION('center_axis',(0.981627005099017,0.,0.190809912898503));
#93527=DIRECTION('ref_axis',(0.,-1.,0.));
#93528=DIRECTION('',(-0.190809912898503,0.,0.981627005099017));
#93529=DIRECTION('center_axis',(0.981627005099017,6.77038411212548E-17,
0.190809912898504));
#93530=DIRECTION('ref_axis',(-0.189638677156094,0.110629058094703,0.975601549625443));
#93531=DIRECTION('center_axis',(0.981627005099017,-7.23564778819888E-18,
0.190809912898503));
#93532=DIRECTION('ref_axis',(-0.189683494387,0.108498197780605,0.975832113140113));
#93533=DIRECTION('center_axis',(0.,1.,0.));
#93534=DIRECTION('ref_axis',(1.,0.,0.));
#93535=DIRECTION('',(-0.190809912898503,0.,0.981627005099017));
#93536=DIRECTION('center_axis',(0.,1.,0.));
#93537=DIRECTION('ref_axis',(-0.113570890342994,0.,0.993529895305974));
#93538=DIRECTION('center_axis',(0.,1.,0.));
#93539=DIRECTION('ref_axis',(-0.115069654854028,0.,0.99335742536701));
#93540=DIRECTION('center_axis',(-0.981627005099017,0.,-0.190809912898503));
#93541=DIRECTION('ref_axis',(-0.190809912898503,0.,0.981627005099017));
#93542=DIRECTION('center_axis',(-0.981627005099017,-4.67296099575741E-17,
-0.190809912898504));
#93543=DIRECTION('ref_axis',(-0.19023078442017,0.0778524365384534,0.978647662227787));
#93544=DIRECTION('center_axis',(-0.981627005099017,-7.19316283930464E-18,
-0.190809912898503));
#93545=DIRECTION('ref_axis',(-0.1902527815393,0.0763617874783217,0.978760827030626));
#93546=DIRECTION('center_axis',(0.,-1.,0.));
#93547=DIRECTION('ref_axis',(0.,0.,-1.));
#93548=DIRECTION('',(-0.190809912898503,0.,0.981627005099017));
#93549=DIRECTION('center_axis',(0.,-1.,0.));
#93550=DIRECTION('ref_axis',(-0.0817056899061984,0.,0.996656500624439));
#93551=DIRECTION('',(-0.190809912898503,0.,0.981627005099017));
#93552=DIRECTION('center_axis',(0.,-1.,0.));
#93553=DIRECTION('ref_axis',(-0.0838045698468043,0.,0.996482209611788));
#93554=DIRECTION('center_axis',(0.981627005099017,0.,0.190809912898503));
#93555=DIRECTION('ref_axis',(0.,-1.,0.));
#93556=DIRECTION('',(-0.190809912898503,0.,0.981627005099017));
#93557=DIRECTION('center_axis',(0.981627005099017,3.38519205606274E-17,
0.190809912898504));
#93558=DIRECTION('ref_axis',(-0.190611836340838,0.0455531415684199,0.980607994633952));
#93559=DIRECTION('center_axis',(0.981627005099017,1.08534716822983E-17,
0.190809912898504));
#93560=DIRECTION('ref_axis',(-0.190619397058329,0.0446757284978794,0.980646890959382));
#93561=DIRECTION('center_axis',(0.,1.,0.));
#93562=DIRECTION('ref_axis',(1.,0.,0.));
#93563=DIRECTION('',(-0.190809912898503,0.,0.981627005099017));
#93564=DIRECTION('center_axis',(0.,1.,0.));
#93565=DIRECTION('ref_axis',(-0.113963373338753,0.,0.993484951842378));
#93566=DIRECTION('center_axis',(0.,1.,0.));
#93567=DIRECTION('ref_axis',(-0.115439892558234,0.,0.993314467430201));
#93568=DIRECTION('center_axis',(-0.981627005099017,0.,-0.190809912898503));
#93569=DIRECTION('ref_axis',(-0.190809912898503,0.,0.981627005099017));
#93570=DIRECTION('center_axis',(-0.981627005099017,-1.86918439830296E-18,
-0.190809912898503));
#93571=DIRECTION('ref_axis',(-0.190793849732929,0.0129754060897403,0.981544367688438));
#93572=DIRECTION('center_axis',(-0.981627005099017,-6.7435901618481E-18,
-0.190809912898504));
#93573=DIRECTION('ref_axis',(-0.19079445899501,0.0127269645797202,0.981547502054479));
#93574=DIRECTION('center_axis',(0.,1.,0.));
#93575=DIRECTION('ref_axis',(1.,0.,0.));
#93576=DIRECTION('',(-0.190809912898503,0.,0.981627005099017));
#93577=DIRECTION('center_axis',(0.,1.,0.));
#93578=DIRECTION('ref_axis',(-0.0225095378912939,0.,0.999746628253339));
#93579=DIRECTION('',(-0.190809912898503,0.,0.981627005099017));
#93580=DIRECTION('center_axis',(0.,1.,0.));
#93581=DIRECTION('ref_axis',(-0.0270306194594231,0.,0.99963460604945));
#93582=DIRECTION('center_axis',(-0.981627005099017,0.,-0.190809912898503));
#93583=DIRECTION('ref_axis',(-0.190809912898503,0.,0.981627005099017));
#93584=DIRECTION('',(-0.190809912898503,1.388010436138E-14,0.981627005099017));
#93585=DIRECTION('',(0.,-1.,0.));
#93586=DIRECTION('center_axis',(-0.981627005099017,-1.66876344160806E-16,
-0.190809912898503));
#93587=DIRECTION('ref_axis',(-0.159106063468809,-0.551997296878187,0.81852565311457));
#93588=DIRECTION('center_axis',(-0.981627005099017,-7.29358033056278E-17,
-0.190809912898503));
#93589=DIRECTION('ref_axis',(-0.157581438380154,-0.563881636142117,0.810682176132997));
#93590=DIRECTION('center_axis',(0.,-1.,0.));
#93591=DIRECTION('ref_axis',(0.,0.,-1.));
#93592=DIRECTION('',(-0.190809912898477,5.452489903615E-14,0.981627005099022));
#93593=DIRECTION('',(0.981627005099017,0.,0.190809912898503));
#93594=DIRECTION('center_axis',(0.,-1.,0.));
#93595=DIRECTION('ref_axis',(0.0160126619219826,0.,0.99987178911007));
#93596=DIRECTION('center_axis',(0.981627005099017,0.,0.190809912898503));
#93597=DIRECTION('ref_axis',(0.,-1.,0.));
#93598=DIRECTION('',(0.,1.,0.));
#93599=DIRECTION('center_axis',(0.981627005099017,-3.09443219726316E-16,
0.190809912898504));
#93600=DIRECTION('ref_axis',(-0.161261901248062,-0.534538298062307,0.829616421673603));
#93601=DIRECTION('center_axis',(-0.190809912898503,0.,0.981627005099017));
#93602=DIRECTION('ref_axis',(0.,1.,0.));
#93603=DIRECTION('center_axis',(0.190809912898503,-6.64418129801744E-16,
-0.981627005099017));
#93604=DIRECTION('ref_axis',(0.303629149237578,-0.950960567161055,0.0590198224157714));
#93605=DIRECTION('center_axis',(0.,1.,0.));
#93606=DIRECTION('ref_axis',(1.,0.,0.));
#93607=DIRECTION('',(-0.190809912898503,0.,0.981627005099017));
#93608=DIRECTION('center_axis',(0.,1.,0.));
#93609=DIRECTION('ref_axis',(-0.0996915880567629,0.,0.995018385393316));
#93610=DIRECTION('',(-0.190809912898503,0.,0.981627005099017));
#93611=DIRECTION('center_axis',(0.,1.,0.));
#93612=DIRECTION('ref_axis',(-0.102121602116587,0.,0.99477192279494));
#93613=DIRECTION('center_axis',(-0.981627005099017,0.,-0.190809912898503));
#93614=DIRECTION('ref_axis',(-0.190809912898503,0.,0.981627005099017));
#93615=DIRECTION('',(-0.190809912898503,0.,0.981627005099017));
#93616=DIRECTION('',(0.,-1.,0.));
#93617=DIRECTION('center_axis',(-0.981627005099017,2.69162553355626E-16,
-0.190809912898504));
#93618=DIRECTION('ref_axis',(-0.157963501542323,-0.5609378130862,0.812647710899723));
#93619=DIRECTION('center_axis',(-0.981627005099017,8.63179540716556E-17,
-0.190809912898503));
#93620=DIRECTION('ref_axis',(-0.158086350850289,-0.559986441507683,0.813279712646517));
#93621=DIRECTION('center_axis',(0.,-1.,0.));
#93622=DIRECTION('ref_axis',(0.,0.,-1.));
#93623=DIRECTION('',(-0.190809912898503,0.,0.981627005099017));
#93624=DIRECTION('',(0.981627005099017,0.,0.190809912898503));
#93625=DIRECTION('center_axis',(0.,-1.,0.));
#93626=DIRECTION('ref_axis',(-0.0615580680962634,0.,0.998103503777166));
#93627=DIRECTION('center_axis',(0.981627005099017,0.,0.190809912898503));
#93628=DIRECTION('ref_axis',(0.,-1.,0.));
#93629=DIRECTION('center_axis',(0.981627005099017,-1.80543576323346E-16,
0.190809912898504));
#93630=DIRECTION('ref_axis',(-0.160582097948044,-0.540130107168397,0.826119154328757));
#93631=DIRECTION('',(0.,1.,0.));
#93632=DIRECTION('center_axis',(0.981627005099017,-4.63081458444729E-16,
0.190809912898504));
#93633=DIRECTION('ref_axis',(-0.161838961663713,-0.529726495046211,0.832585125337745));
#93634=DIRECTION('center_axis',(-0.190809912898503,0.,0.981627005099017));
#93635=DIRECTION('ref_axis',(0.,1.,0.));
#93636=DIRECTION('center_axis',(0.190809912898503,5.18712399582064E-16,
-0.981627005099017));
#93637=DIRECTION('ref_axis',(0.191173908779205,-0.980852498727369,0.0371606289284456));
#93638=DIRECTION('center_axis',(0.,1.,0.));
#93639=DIRECTION('ref_axis',(1.,0.,0.));
#93640=DIRECTION('',(-0.190809912898503,0.,0.981627005099017));
#93641=DIRECTION('center_axis',(0.,1.,0.));
#93642=DIRECTION('ref_axis',(-0.175735962495432,0.,0.984437337511029));
#93643=DIRECTION('',(-0.190809912898503,0.,0.981627005099017));
#93644=DIRECTION('center_axis',(0.,1.,0.));
#93645=DIRECTION('ref_axis',(-0.176135083798187,0.,0.984366005231492));
#93646=DIRECTION('center_axis',(-0.981627005099017,0.,-0.190809912898503));
#93647=DIRECTION('ref_axis',(-0.190809912898503,0.,0.981627005099017));
#93648=DIRECTION('',(-0.190809912898503,0.,0.981627005099017));
#93649=DIRECTION('',(0.,-1.,0.));
#93650=DIRECTION('center_axis',(-0.981627005099017,8.91952555246029E-17,
-0.190809912898503));
#93651=DIRECTION('ref_axis',(-0.157500137288895,-0.564505169249368,0.810263920364668));
#93652=DIRECTION('center_axis',(-0.981627005099017,8.58313634584417E-17,
-0.190809912898503));
#93653=DIRECTION('ref_axis',(-0.158289781209933,-0.558405836138714,0.814326265897604));
#93654=DIRECTION('center_axis',(0.,-1.,0.));
#93655=DIRECTION('ref_axis',(0.,0.,-1.));
#93656=DIRECTION('',(-0.190809912898503,0.,0.981627005099017));
#93657=DIRECTION('',(0.981627005099017,0.,0.190809912898503));
#93658=DIRECTION('center_axis',(0.,-1.,0.));
#93659=DIRECTION('ref_axis',(-0.137981858751738,0.,0.990434756385001));
#93660=DIRECTION('center_axis',(0.981627005099017,0.,0.190809912898503));
#93661=DIRECTION('ref_axis',(0.,-1.,0.));
#93662=DIRECTION('center_axis',(0.981627005099017,-1.04257444818754E-16,
0.190809912898503));
#93663=DIRECTION('ref_axis',(-0.160914514245377,-0.537405994836492,0.827829279392179));
#93664=DIRECTION('',(0.,1.,0.));
#93665=DIRECTION('center_axis',(0.981627005099017,-4.58598230482662E-16,
0.190809912898504));
#93666=DIRECTION('ref_axis',(-0.162144254191831,-0.527156039487894,0.834155711401662));
#93667=DIRECTION('center_axis',(-0.190809912898503,0.,0.981627005099017));
#93668=DIRECTION('ref_axis',(0.,1.,0.));
#93669=DIRECTION('center_axis',(0.190809912898503,-5.91565264691904E-16,
-0.981627005099017));
#93670=DIRECTION('ref_axis',(0.0787186683208446,-0.996779432638552,0.0153014354411246));
#93671=DIRECTION('center_axis',(0.,1.,0.));
#93672=DIRECTION('ref_axis',(1.,0.,0.));
#93673=DIRECTION('',(-0.190809912898503,0.,0.981627005099017));
#93674=DIRECTION('center_axis',(0.,1.,0.));
#93675=DIRECTION('ref_axis',(-0.250656761475531,0.,0.968076023836247));
#93676=DIRECTION('',(-0.190809912898503,0.,0.981627005099017));
#93677=DIRECTION('center_axis',(0.,1.,0.));
#93678=DIRECTION('ref_axis',(-0.249083719402477,0.,0.968481956842061));
#93679=DIRECTION('center_axis',(-0.981627005099017,0.,-0.190809912898503));
#93680=DIRECTION('ref_axis',(-0.190809912898503,0.,0.981627005099017));
#93681=DIRECTION('',(-0.190809912898503,0.,0.981627005099017));
#93682=DIRECTION('',(0.,-1.,0.));
#93683=DIRECTION('center_axis',(-0.981627005099017,-1.6393621720623E-16,
-0.190809912898503));
#93684=DIRECTION('ref_axis',(-0.157698222107343,-0.562984198653009,0.811282973327564));
#93685=DIRECTION('center_axis',(-0.981627005099017,2.72457558214586E-16,
-0.190809912898504));
#93686=DIRECTION('ref_axis',(-0.1582029102982,-0.559081597802509,0.813879356029979));
#93687=DIRECTION('center_axis',(0.,-1.,0.));
#93688=DIRECTION('ref_axis',(0.,0.,-1.));
#93689=DIRECTION('',(-0.190809912898503,0.,0.981627005099017));
#93690=DIRECTION('',(0.981627005099017,0.,0.190809912898503));
#93691=DIRECTION('center_axis',(0.,-1.,0.));
#93692=DIRECTION('ref_axis',(-0.21328299146488,0.,0.976990463388355));
#93693=DIRECTION('center_axis',(0.981627005099017,0.,0.190809912898503));
#93694=DIRECTION('ref_axis',(0.,-1.,0.));
#93695=DIRECTION('center_axis',(0.981627005099017,-1.48689867894081E-16,
0.190809912898503));
#93696=DIRECTION('ref_axis',(-0.160969201866504,-0.536955970969592,0.828110621409098));
#93697=DIRECTION('',(0.,1.,0.));
#93698=DIRECTION('center_axis',(0.981627005099017,4.29243236049658E-17,
0.190809912898503));
#93699=DIRECTION('ref_axis',(-0.162194507351624,-0.526731257403113,0.834414240206565));
#93700=DIRECTION('center_axis',(-0.190809912898503,0.,0.981627005099017));
#93701=DIRECTION('ref_axis',(0.,1.,0.));
#93702=DIRECTION('center_axis',(0.190809912898503,1.62461889194944E-16,
-0.981627005099017));
#93703=DIRECTION('ref_axis',(-0.0337365721375064,-0.999409245259327,-0.00655775804619647));
#93704=DIRECTION('center_axis',(0.,1.,0.));
#93705=DIRECTION('ref_axis',(1.,0.,0.));
#93706=DIRECTION('',(-0.190809912898503,0.,0.981627005099017));
#93707=DIRECTION('center_axis',(0.,1.,0.));
#93708=DIRECTION('ref_axis',(-0.324447978030139,0.,0.945903541357233));
#93709=DIRECTION('',(-0.190809912898503,0.,0.981627005099017));
#93710=DIRECTION('center_axis',(0.,1.,0.));
#93711=DIRECTION('ref_axis',(-0.320962116007901,0.,0.947092033588991));
#93712=DIRECTION('center_axis',(-0.981627005099017,0.,-0.190809912898503));
#93713=DIRECTION('ref_axis',(-0.190809912898503,0.,0.981627005099017));
#93714=DIRECTION('',(-0.190809912898503,0.,0.981627005099017));
#93715=DIRECTION('',(0.,-1.,0.));
#93716=DIRECTION('center_axis',(-0.981627005099017,3.76690784096542E-16,
-0.190809912898504));
#93717=DIRECTION('ref_axis',(-0.158565308967581,-0.556254632219511,0.815743726256201));
#93718=DIRECTION('center_axis',(-0.981627005099017,-3.33314991325887E-16,
-0.190809912898503));
#93719=DIRECTION('ref_axis',(-0.157820990225955,-0.562038509834281,0.811914557393424));
#93720=DIRECTION('center_axis',(0.,-1.,0.));
#93721=DIRECTION('ref_axis',(0.,0.,-1.));
#93722=DIRECTION('',(-0.190809912898503,0.,0.981627005099017));
#93723=DIRECTION('',(0.981627005099017,0.,0.190809912898503));
#93724=DIRECTION('center_axis',(0.,-1.,0.));
#93725=DIRECTION('ref_axis',(-0.287465429548881,0.,0.957791014164508));
#93726=DIRECTION('center_axis',(0.981627005099017,0.,0.190809912898503));
#93727=DIRECTION('ref_axis',(0.,-1.,0.));
#93728=DIRECTION('center_axis',(0.981627005099017,-3.89199893264009E-16,
0.190809912898504));
#93729=DIRECTION('ref_axis',(-0.160749232394967,-0.538762885913093,0.8269789822281));
#93730=DIRECTION('',(0.,1.,0.));
#93731=DIRECTION('center_axis',(0.981627005099017,-4.32027132019077E-17,
0.190809912898503));
#93732=DIRECTION('ref_axis',(-0.161992422346658,-0.528436578558402,0.83337460817075));
#93733=DIRECTION('center_axis',(-0.190809912898503,0.,0.981627005099017));
#93734=DIRECTION('ref_axis',(0.,1.,0.));
#93735=DIRECTION('center_axis',(0.190809912898503,5.2454062879085E-17,-0.981627005099017));
#93736=DIRECTION('ref_axis',(-0.146191812595837,-0.988848032204891,-0.0284169515335126));
#93737=DIRECTION('center_axis',(0.,1.,0.));
#93738=DIRECTION('ref_axis',(1.,0.,0.));
#93739=DIRECTION('',(-0.190809912898503,0.,0.981627005099017));
#93740=DIRECTION('',(-0.981627005099017,0.,-0.190809912898503));
#93741=DIRECTION('center_axis',(0.,1.,0.));
#93742=DIRECTION('ref_axis',(-0.390089733402804,0.,0.920776845871859));
#93743=DIRECTION('',(-0.190809912898503,0.,0.981627005099017));
#93744=DIRECTION('center_axis',(0.,1.,0.));
#93745=DIRECTION('ref_axis',(-0.391746367360933,0.,0.920073249072873));
#93746=DIRECTION('center_axis',(-0.981627005099017,0.,-0.190809912898503));
#93747=DIRECTION('ref_axis',(-0.190809912898503,0.,0.981627005099017));
#93748=DIRECTION('',(-0.190809912898503,1.605442884968E-13,0.981627005099017));
#93749=DIRECTION('',(0.,-1.,0.));
#93750=DIRECTION('center_axis',(-0.981627005099017,-8.86144962521498E-17,
-0.190809912898503));
#93751=DIRECTION('ref_axis',(-0.157122673757211,-0.567386932574192,0.808322048527339));
#93752=DIRECTION('center_axis',(0.,-1.,0.));
#93753=DIRECTION('ref_axis',(0.,0.,-1.));
#93754=DIRECTION('',(-0.190809912898503,-1.607428443784E-14,0.981627005099017));
#93755=DIRECTION('',(0.981627005099017,0.,0.190809912898503));
#93756=DIRECTION('center_axis',(0.,-1.,0.));
#93757=DIRECTION('ref_axis',(-0.360513177655806,0.,0.93275412019273));
#93758=DIRECTION('center_axis',(0.981627005099017,0.,0.190809912898503));
#93759=DIRECTION('ref_axis',(0.,-1.,0.));
#93760=DIRECTION('center_axis',(0.981627005099017,-3.03995681381544E-17,
0.190809912898503));
#93761=DIRECTION('ref_axis',(-0.160242144137859,-0.542896069554004,0.824370252316831));
#93762=DIRECTION('',(0.,1.,0.));
#93763=DIRECTION('center_axis',(0.981627005099017,-4.67653207300599E-16,
0.190809912898504));
#93764=DIRECTION('ref_axis',(-0.161527046948701,-0.532334922311487,0.830980471245657));
#93765=DIRECTION('center_axis',(-0.190809912898503,0.,0.981627005099017));
#93766=DIRECTION('ref_axis',(0.,1.,0.));
#93767=DIRECTION('center_axis',(0.190809912898503,2.0981625151634E-16,-0.981627005099017));
#93768=DIRECTION('ref_axis',(-0.258647053054216,-0.964662641128085,-0.0502761450208387));
#93769=DIRECTION('center_axis',(0.,1.,0.));
#93770=DIRECTION('ref_axis',(1.,0.,0.));
#93771=DIRECTION('',(-0.190809912898488,0.,0.98162700509902));
#93772=DIRECTION('',(-0.981627005099017,0.,-0.190809912898503));
#93773=DIRECTION('center_axis',(0.,1.,0.));
#93774=DIRECTION('ref_axis',(-0.699923036064448,0.,0.714218274469595));
#93775=DIRECTION('',(-0.190809912898503,0.,0.981627005099017));
#93776=DIRECTION('center_axis',(0.,1.,0.));
#93777=DIRECTION('ref_axis',(-0.711546942295925,0.,0.702638562071083));
#93778=DIRECTION('center_axis',(-0.981627005099017,0.,-0.190809912898503));
#93779=DIRECTION('ref_axis',(-0.190809912898503,0.,0.981627005099017));
#93780=DIRECTION('',(-0.190809912898503,4.013607212418E-14,0.981627005099017));
#93781=DIRECTION('',(0.,-1.,0.));
#93782=DIRECTION('center_axis',(-0.981627005099017,2.5977613593094E-17,
-0.190809912898503));
#93783=DIRECTION('ref_axis',(-0.186383180917028,-0.214152203332011,0.958853556951892));
#93784=DIRECTION('center_axis',(0.,-1.,0.));
#93785=DIRECTION('ref_axis',(0.,0.,-1.));
#93786=DIRECTION('',(-0.190809912898503,0.,0.981627005099017));
#93787=DIRECTION('',(0.981627005099017,0.,0.190809912898503));
#93788=DIRECTION('center_axis',(0.,-1.,0.));
#93789=DIRECTION('ref_axis',(-0.686504883900775,0.,0.727125191683236));
#93790=DIRECTION('center_axis',(0.981627005099017,0.,0.190809912898503));
#93791=DIRECTION('ref_axis',(0.,-1.,0.));
#93792=DIRECTION('center_axis',(0.981627005099017,-3.65431440454912E-17,
0.190809912898503));
#93793=DIRECTION('ref_axis',(-0.187820057364573,-0.1763322148272,0.966245608562183));
#93794=DIRECTION('',(0.,1.,0.));
#93795=DIRECTION('center_axis',(0.981627005099017,-4.94804897087551E-17,
0.190809912898504));
#93796=DIRECTION('ref_axis',(-0.187977242348303,-0.171670124543093,0.967054251166131));
#93797=DIRECTION('center_axis',(-0.190809912898503,0.,0.981627005099017));
#93798=DIRECTION('ref_axis',(0.,1.,0.));
#93799=DIRECTION('center_axis',(0.190809912898504,2.44785626769064E-16,
-0.981627005099017));
#93800=DIRECTION('ref_axis',(-0.933378495804326,-0.309656688597602,-0.181431305944762));
#93801=DIRECTION('center_axis',(0.981627005099017,0.,0.190809912898503));
#93802=DIRECTION('ref_axis',(0.,-1.,0.));
#93803=DIRECTION('',(-0.190809912898503,0.,0.981627005099017));
#93804=DIRECTION('center_axis',(0.981627005099017,-6.00351652175927E-17,
0.190809912898504));
#93805=DIRECTION('ref_axis',(-0.189859859903711,-0.0996660344675376,0.976739430539619));
#93806=DIRECTION('',(-0.190809912898503,0.,0.981627005099017));
#93807=DIRECTION('center_axis',(0.981627005099017,-1.23701224271888E-17,
0.190809912898503));
#93808=DIRECTION('ref_axis',(-0.189909550677726,-0.0970309399591574,0.976995066134946));
#93809=DIRECTION('center_axis',(0.,1.,0.));
#93810=DIRECTION('ref_axis',(1.,0.,0.));
#93811=DIRECTION('',(-0.190809912898503,0.,0.981627005099017));
#93812=DIRECTION('',(-0.981627005099017,0.,-0.190809912898503));
#93813=DIRECTION('center_axis',(0.,1.,0.));
#93814=DIRECTION('ref_axis',(-0.708046345681522,0.,0.706165966587914));
#93815=DIRECTION('center_axis',(0.,1.,0.));
#93816=DIRECTION('ref_axis',(-0.708026020831984,0.,0.706186344971939));
#93817=DIRECTION('center_axis',(-0.981627005099017,0.,-0.190809912898503));
#93818=DIRECTION('ref_axis',(-0.190809912898503,0.,0.981627005099017));
#93819=DIRECTION('',(-0.190809912898503,0.,0.981627005099017));
#93820=DIRECTION('',(0.,-1.,0.));
#93821=DIRECTION('center_axis',(-0.981627005099017,2.5977613593094E-17,
-0.190809912898503));
#93822=DIRECTION('ref_axis',(-0.188993069322325,-0.137669273570596,0.97228020182593));
#93823=DIRECTION('center_axis',(0.,-1.,0.));
#93824=DIRECTION('ref_axis',(0.,0.,-1.));
#93825=DIRECTION('center_axis',(0.,-1.,0.));
#93826=DIRECTION('ref_axis',(-0.691132671254374,0.,0.722727909191829));
#93827=DIRECTION('',(0.981627005099017,0.,0.190809912898503));
#93828=DIRECTION('center_axis',(0.,-1.,0.));
#93829=DIRECTION('ref_axis',(-0.682158787921673,0.,0.731204067317212));
#93830=DIRECTION('center_axis',(-0.190809912898503,0.,0.981627005099017));
#93831=DIRECTION('ref_axis',(0.,1.,0.));
#93832=DIRECTION('center_axis',(0.190809912898503,-8.74234381318085E-17,
-0.981627005099017));
#93833=DIRECTION('ref_axis',(-0.960530036154236,-0.206208093067504,-0.186709057088846));
#93834=DIRECTION('center_axis',(0.981627005099017,0.,0.190809912898503));
#93835=DIRECTION('ref_axis',(0.,-1.,0.));
#93836=DIRECTION('',(-0.190809912898503,0.,0.981627005099017));
#93837=DIRECTION('center_axis',(0.981627005099017,5.22044914935589E-18,
0.190809912898503));
#93838=DIRECTION('ref_axis',(-0.190759437640654,-0.0229998541078904,0.981367333704377));
#93839=DIRECTION('',(-0.190809912898503,0.,0.981627005099017));
#93840=DIRECTION('center_axis',(0.981627005099017,-3.71103672815663E-18,
0.190809912898503));
#93841=DIRECTION('ref_axis',(-0.190762071742238,-0.0223917553751911,0.981380884914632));
#93842=DIRECTION('center_axis',(0.,1.,0.));
#93843=DIRECTION('ref_axis',(1.,0.,0.));
#93844=DIRECTION('',(-0.190809912898503,0.,0.981627005099017));
#93845=DIRECTION('',(-0.981627005099013,0.,-0.190809912898526));
#93846=DIRECTION('center_axis',(0.,1.,0.));
#93847=DIRECTION('ref_axis',(-0.711526155446024,0.,0.702659611843601));
#93848=DIRECTION('center_axis',(0.,1.,0.));
#93849=DIRECTION('ref_axis',(-0.706483995353756,0.,0.707729018981837));
#93850=DIRECTION('center_axis',(-0.981627005099017,0.,-0.190809912898503));
#93851=DIRECTION('ref_axis',(-0.190809912898503,0.,0.981627005099017));
#93852=DIRECTION('',(-0.190809912898515,0.,0.981627005099015));
#93853=DIRECTION('',(0.,-1.,0.));
#93854=DIRECTION('center_axis',(-0.981627005099017,3.50697783506769E-17,
-0.190809912898504));
#93855=DIRECTION('ref_axis',(-0.19045240389019,-0.0611863438091478,0.979787789872744));
#93856=DIRECTION('center_axis',(0.,-1.,0.));
#93857=DIRECTION('ref_axis',(0.,0.,-1.));
#93858=DIRECTION('center_axis',(0.,-1.,0.));
#93859=DIRECTION('ref_axis',(-0.688592136426526,0.,0.725148860339415));
#93860=DIRECTION('',(0.981627005099017,0.,0.190809912898503));
#93861=DIRECTION('center_axis',(0.,-1.,0.));
#93862=DIRECTION('ref_axis',(-0.679752594529884,0.,0.733441483848501));
#93863=DIRECTION('center_axis',(-0.190809912898503,0.,0.981627005099017));
#93864=DIRECTION('ref_axis',(0.,1.,0.));
#93865=DIRECTION('center_axis',(0.190809912898504,6.41105212966596E-17,
-0.981627005099017));
#93866=DIRECTION('ref_axis',(-0.977495790902178,-0.0916480413633408,-0.190006882198483));
#93867=DIRECTION('center_axis',(0.,1.,0.));
#93868=DIRECTION('ref_axis',(1.,0.,0.));
#93869=DIRECTION('',(-0.190809912898503,0.,0.981627005099017));
#93870=DIRECTION('center_axis',(0.,1.,0.));
#93871=DIRECTION('ref_axis',(0.120993925133802,0.,0.992653247655351));
#93872=DIRECTION('',(-0.190809912898503,0.,0.981627005099017));
#93873=DIRECTION('center_axis',(0.,1.,0.));
#93874=DIRECTION('ref_axis',(0.113186441507845,0.,0.993573766490839));
#93875=DIRECTION('center_axis',(-0.981627005099017,0.,-0.190809912898503));
#93876=DIRECTION('ref_axis',(-0.190809912898503,0.,0.981627005099017));
#93877=DIRECTION('',(-0.190809912898503,0.,0.981627005099017));
#93878=DIRECTION('',(0.,-1.,0.));
#93879=DIRECTION('center_axis',(-0.981627005099017,5.1352667504369E-16,
-0.190809912898504));
#93880=DIRECTION('ref_axis',(-0.16364102821286,-0.51429587245801,0.841855907776439));
#93881=DIRECTION('center_axis',(-0.981627005099017,-2.15548573767396E-16,
-0.190809912898503));
#93882=DIRECTION('ref_axis',(-0.163734348297844,-0.513479438445504,0.842335995598651));
#93883=DIRECTION('center_axis',(0.,-1.,0.));
#93884=DIRECTION('ref_axis',(0.,0.,-1.));
#93885=DIRECTION('',(-0.190809912898486,-1.729025838123E-14,0.98162700509902));
#93886=DIRECTION('',(0.981627005099017,0.,0.190809912898503));
#93887=DIRECTION('center_axis',(0.,-1.,0.));
#93888=DIRECTION('ref_axis',(0.157666506055977,0.,0.987492416612958));
#93889=DIRECTION('center_axis',(0.981627005099017,0.,0.190809912898503));
#93890=DIRECTION('ref_axis',(0.,-1.,0.));
#93891=DIRECTION('center_axis',(0.981627005099017,1.31015175507947E-16,
0.190809912898503));
#93892=DIRECTION('ref_axis',(-0.165724730740096,-0.495631116264313,0.852575574486927));
#93893=DIRECTION('',(0.,1.,0.));
#93894=DIRECTION('center_axis',(0.981627005099017,-2.040880606468E-16,0.190809912898504));
#93895=DIRECTION('ref_axis',(-0.166837808361562,-0.485266017453878,0.858301833858907));
#93896=DIRECTION('center_axis',(-0.190809912898503,0.,0.981627005099017));
#93897=DIRECTION('ref_axis',(0.,1.,0.));
#93898=DIRECTION('center_axis',(0.190809912898504,-3.73006669362382E-16,
-0.981627005099017));
#93899=DIRECTION('ref_axis',(0.528539630154271,-0.842668807828817,0.10273820939041));
#93900=DIRECTION('center_axis',(0.,-1.,0.));
#93901=DIRECTION('ref_axis',(0.,0.,-1.));
#93902=DIRECTION('',(-0.190809912898503,0.,0.981627005099017));
#93903=DIRECTION('center_axis',(0.,-1.,0.));
#93904=DIRECTION('ref_axis',(0.0887570095372046,0.,0.996053308441879));
#93905=DIRECTION('',(-0.190809912898503,0.,0.981627005099017));
#93906=DIRECTION('center_axis',(0.,-1.,0.));
#93907=DIRECTION('ref_axis',(0.0814953329512814,0.,0.996673723295222));
#93908=DIRECTION('center_axis',(0.981627005099017,0.,0.190809912898503));
#93909=DIRECTION('ref_axis',(0.,-1.,0.));
#93910=DIRECTION('',(-0.190809912898503,0.,0.981627005099017));
#93911=DIRECTION('center_axis',(0.981627005099017,3.15328006926456E-17,
0.190809912898503));
#93912=DIRECTION('ref_axis',(-0.16672759291197,-0.486305331766721,0.857734827354608));
#93913=DIRECTION('center_axis',(0.981627005099017,-1.66509281342602E-16,
0.190809912898504));
#93914=DIRECTION('ref_axis',(-0.16775489422609,-0.476502997179297,0.86301980808226));
#93915=DIRECTION('center_axis',(0.,1.,0.));
#93916=DIRECTION('ref_axis',(1.,0.,0.));
#93917=DIRECTION('',(-0.190809912898503,0.,0.981627005099017));
#93918=DIRECTION('center_axis',(0.,1.,0.));
#93919=DIRECTION('ref_axis',(0.0450135661808758,0.,0.998986375712742));
#93920=DIRECTION('center_axis',(0.,1.,0.));
#93921=DIRECTION('ref_axis',(0.0391533554628644,0.,0.999233213397152));
#93922=DIRECTION('center_axis',(-0.981627005099017,0.,-0.190809912898503));
#93923=DIRECTION('ref_axis',(-0.190809912898503,0.,0.981627005099017));
#93924=DIRECTION('center_axis',(-0.981627005099017,4.50330787761146E-16,
-0.190809912898504));
#93925=DIRECTION('ref_axis',(-0.163482218098267,-0.515681224446299,0.841038904640705));
#93926=DIRECTION('center_axis',(-0.981627005099017,-1.19343362969677E-16,
-0.190809912898503));
#93927=DIRECTION('ref_axis',(-0.164642701979114,-0.505438873877122,0.847009046857732));
#93928=DIRECTION('center_axis',(0.,-1.,0.));
#93929=DIRECTION('ref_axis',(0.,0.,-1.));
#93930=DIRECTION('',(-0.190809912898503,0.,0.981627005099017));
#93931=DIRECTION('center_axis',(0.,-1.,0.));
#93932=DIRECTION('ref_axis',(0.0116866005388723,0.,0.999931709352116));
#93933=DIRECTION('',(-0.190809912898503,1.012116632187E-14,0.981627005099017));
#93934=DIRECTION('center_axis',(0.,-1.,0.));
#93935=DIRECTION('ref_axis',(0.00646633198153377,0.,0.999979093056802));
#93936=DIRECTION('center_axis',(0.981627005099017,0.,0.190809912898503));
#93937=DIRECTION('ref_axis',(0.,-1.,0.));
#93938=DIRECTION('',(-0.190809912898503,0.,0.981627005099017));
#93939=DIRECTION('center_axis',(0.981627005099017,-1.22647734598186E-16,
0.190809912898504));
#93940=DIRECTION('ref_axis',(-0.167439209291461,-0.479542969202221,0.861395757988492));
#93941=DIRECTION('center_axis',(0.981627005099017,-2.35766262648622E-16,
0.190809912898504));
#93942=DIRECTION('ref_axis',(-0.168407671809334,-0.470136093476487,0.866378040861163));
#93943=DIRECTION('center_axis',(0.,1.,0.));
#93944=DIRECTION('ref_axis',(1.,0.,0.));
#93945=DIRECTION('',(-0.190809912898503,0.,0.981627005099017));
#93946=DIRECTION('center_axis',(0.,1.,0.));
#93947=DIRECTION('ref_axis',(-0.0298461846255247,0.,0.999554503398038));
#93948=DIRECTION('center_axis',(0.,1.,0.));
#93949=DIRECTION('ref_axis',(-0.033817507686259,0.,0.999428024508964));
#93950=DIRECTION('center_axis',(-0.981627005099017,0.,-0.190809912898503));
#93951=DIRECTION('ref_axis',(-0.190809912898503,0.,0.981627005099017));
#93952=DIRECTION('center_axis',(-0.981627005099017,3.03411534837829E-17,
-0.190809912898503));
#93953=DIRECTION('ref_axis',(-0.164163607711793,-0.509701069063094,0.84454433282036));
#93954=DIRECTION('center_axis',(-0.981627005099017,2.04220249255758E-16,
-0.190809912898504));
#93955=DIRECTION('ref_axis',(-0.165267798853502,-0.499804177489587,0.850224875445359));
#93956=DIRECTION('center_axis',(0.,-1.,0.));
#93957=DIRECTION('ref_axis',(0.,0.,-1.));
#93958=DIRECTION('',(-0.190809912898503,0.,0.981627005099017));
#93959=DIRECTION('center_axis',(0.,-1.,0.));
#93960=DIRECTION('ref_axis',(-0.0642416745920277,0.,0.99793437020959));
#93961=DIRECTION('',(-0.190809912898503,0.,0.981627005099017));
#93962=DIRECTION('center_axis',(0.,-1.,0.));
#93963=DIRECTION('ref_axis',(-0.0674811483731083,0.,0.997720549359512));
#93964=DIRECTION('center_axis',(0.981627005099017,0.,0.190809912898503));
#93965=DIRECTION('ref_axis',(0.,-1.,0.));
#93966=DIRECTION('',(-0.190809912898503,0.,0.981627005099017));
#93967=DIRECTION('center_axis',(0.981627005099017,-2.40724768431128E-16,
0.190809912898504));
#93968=DIRECTION('ref_axis',(-0.167904431149187,-0.475054190642086,0.86378910502151));
#93969=DIRECTION('center_axis',(0.981627005099017,-1.01299069034784E-16,
0.190809912898503));
#93970=DIRECTION('ref_axis',(-0.168835339045174,-0.465904025763593,0.868578187077467));
#93971=DIRECTION('center_axis',(0.,1.,0.));
#93972=DIRECTION('ref_axis',(1.,0.,0.));
#93973=DIRECTION('',(-0.190809912898503,0.,0.981627005099017));
#93974=DIRECTION('center_axis',(0.,1.,0.));
#93975=DIRECTION('ref_axis',(-0.103635423533207,0.,0.994615352279007));
#93976=DIRECTION('center_axis',(0.,1.,0.));
#93977=DIRECTION('ref_axis',(-0.105771299395389,0.,0.994390482770331));
#93978=DIRECTION('center_axis',(-0.981627005099017,0.,-0.190809912898503));
#93979=DIRECTION('ref_axis',(-0.190809912898503,0.,0.981627005099017));
#93980=DIRECTION('center_axis',(-0.981627005099017,2.99069503728474E-16,
-0.190809912898504));
#93981=DIRECTION('ref_axis',(-0.164575366240622,-0.506040837499906,0.846662636242535));
#93982=DIRECTION('center_axis',(-0.981627005099017,1.72635908143311E-16,
-0.190809912898504));
#93983=DIRECTION('ref_axis',(-0.165646202300485,-0.496351618609119,0.852171582703586));
#93984=DIRECTION('center_axis',(0.,-1.,0.));
#93985=DIRECTION('ref_axis',(0.,0.,-1.));
#93986=DIRECTION('',(-0.190809912898503,0.,0.981627005099017));
#93987=DIRECTION('center_axis',(0.,-1.,0.));
#93988=DIRECTION('ref_axis',(-0.139070803150795,0.,0.990282440372944));
#93989=DIRECTION('',(-0.190809912898503,0.,0.981627005099017));
#93990=DIRECTION('center_axis',(0.,-1.,0.));
#93991=DIRECTION('ref_axis',(-0.14038574967161,0.,0.99009688479923));
#93992=DIRECTION('center_axis',(0.981627005099017,0.,0.190809912898503));
#93993=DIRECTION('ref_axis',(0.,-1.,0.));
#93994=DIRECTION('',(-0.190809912898503,0.,0.981627005099017));
#93995=DIRECTION('center_axis',(0.981627005099017,-2.9787841376787E-16,
0.190809912898504));
#93996=DIRECTION('ref_axis',(-0.168150432820926,-0.472658284615304,0.865054667594282));
#93997=DIRECTION('center_axis',(0.981627005099017,1.43311947025832E-17,
0.190809912898503));
#93998=DIRECTION('ref_axis',(-0.169061774141528,-0.463643263645911,0.869743088848591));
#93999=DIRECTION('center_axis',(0.,1.,0.));
#94000=DIRECTION('ref_axis',(1.,0.,0.));
#94001=DIRECTION('',(-0.190809912898503,0.,0.981627005099017));
#94002=DIRECTION('center_axis',(0.,1.,0.));
#94003=DIRECTION('ref_axis',(-0.176383802734287,0.,0.984321468897734));
#94004=DIRECTION('center_axis',(0.,1.,0.));
#94005=DIRECTION('ref_axis',(-0.176734827717815,0.,0.984258502971427));
#94006=DIRECTION('center_axis',(-0.981627005099017,0.,-0.190809912898503));
#94007=DIRECTION('ref_axis',(-0.190809912898503,0.,0.981627005099017));
#94008=DIRECTION('center_axis',(-0.981627005099017,-8.91952555246029E-17,
-0.190809912898503));
#94009=DIRECTION('ref_axis',(-0.164741217100846,-0.504556436150305,0.847515860693731));
#94010=DIRECTION('center_axis',(-0.981627005099017,2.00273181403031E-16,
-0.190809912898504));
#94011=DIRECTION('ref_axis',(-0.165798759222807,-0.494950627486599,0.852956416114446));
#94012=DIRECTION('center_axis',(0.,-1.,0.));
#94013=DIRECTION('ref_axis',(0.,0.,-1.));
#94014=DIRECTION('',(-0.190809912898503,0.,0.981627005099017));
#94015=DIRECTION('center_axis',(0.,-1.,0.));
#94016=DIRECTION('ref_axis',(-0.212823105190621,0.,0.977090745988837));
#94017=DIRECTION('',(-0.190809912898503,0.,0.981627005099017));
#94018=DIRECTION('center_axis',(0.,-1.,0.));
#94019=DIRECTION('ref_axis',(-0.212267586570765,0.,0.977211579798061));
#94020=DIRECTION('center_axis',(0.981627005099017,0.,0.190809912898503));
#94021=DIRECTION('ref_axis',(0.,-1.,0.));
#94022=DIRECTION('',(-0.190809912898503,0.,0.981627005099017));
#94023=DIRECTION('center_axis',(0.981627005099017,-2.08165815051713E-16,
0.190809912898504));
#94024=DIRECTION('ref_axis',(-0.168190918116109,-0.472262480491401,0.865262945342842));
#94025=DIRECTION('center_axis',(0.981627005099017,-2.14621618024828E-16,
0.190809912898504));
#94026=DIRECTION('ref_axis',(-0.169099058653206,-0.463269660125623,0.869934900075684));
#94027=DIRECTION('center_axis',(0.,1.,0.));
#94028=DIRECTION('ref_axis',(1.,0.,0.));
#94029=DIRECTION('',(-0.190809912898503,0.,0.981627005099017));
#94030=DIRECTION('center_axis',(0.,1.,0.));
#94031=DIRECTION('ref_axis',(-0.248103134940545,0.,0.968733624084905));
#94032=DIRECTION('center_axis',(0.,1.,0.));
#94033=DIRECTION('ref_axis',(-0.246718789670631,0.,0.969087116219929));
#94034=DIRECTION('center_axis',(-0.981627005099017,0.,-0.190809912898503));
#94035=DIRECTION('ref_axis',(-0.190809912898503,0.,0.981627005099017));
#94036=DIRECTION('center_axis',(-0.981627005099017,1.49032924732936E-16,
-0.190809912898503));
#94037=DIRECTION('ref_axis',(-0.164670397132728,-0.505191006835612,0.84715152536047));
#94038=DIRECTION('center_axis',(-0.981627005099017,1.43398714849782E-17,
-0.190809912898503));
#94039=DIRECTION('ref_axis',(-0.165733605986292,-0.495549598052214,0.852621233442535));
#94040=DIRECTION('center_axis',(0.,-1.,0.));
#94041=DIRECTION('ref_axis',(0.,0.,-1.));
#94042=DIRECTION('',(-0.190809912898503,0.,0.981627005099017));
#94043=DIRECTION('center_axis',(0.,-1.,0.));
#94044=DIRECTION('ref_axis',(-0.285502227028518,0.,0.95837804563844));
#94045=DIRECTION('',(-0.190809912898503,0.,0.981627005099017));
#94046=DIRECTION('center_axis',(0.,-1.,0.));
#94047=DIRECTION('ref_axis',(-0.28312994844639,0.,0.959081556642992));
#94048=DIRECTION('center_axis',(0.981627005099017,0.,0.190809912898503));
#94049=DIRECTION('ref_axis',(0.,-1.,0.));
#94050=DIRECTION('',(-0.190809912898503,0.,0.981627005099017));
#94051=DIRECTION('center_axis',(0.981627005099017,-7.48461333200017E-17,
0.190809912898503));
#94052=DIRECTION('ref_axis',(-0.168028098915109,-0.473851694839214,0.864425317348456));
#94053=DIRECTION('center_axis',(0.981627005099017,-2.73617183612082E-16,
0.190809912898504));
#94054=DIRECTION('ref_axis',(-0.168949145239597,-0.46476952090078,0.869163666270323));
#94055=DIRECTION('center_axis',(0.,1.,0.));
#94056=DIRECTION('ref_axis',(1.,0.,0.));
#94057=DIRECTION('',(-0.190809912898503,0.,0.981627005099017));
#94058=DIRECTION('center_axis',(0.,1.,0.));
#94059=DIRECTION('ref_axis',(-0.318788385159717,0.,0.94782591518024));
#94060=DIRECTION('center_axis',(0.,1.,0.));
#94061=DIRECTION('ref_axis',(-0.315718624595745,0.,0.948852860080724));
#94062=DIRECTION('center_axis',(-0.981627005099017,0.,-0.190809912898503));
#94063=DIRECTION('ref_axis',(-0.190809912898503,0.,0.981627005099017));
#94064=DIRECTION('center_axis',(-0.981627005099017,4.52028940915851E-17,
-0.190809912898503));
#94065=DIRECTION('ref_axis',(-0.164358984279519,-0.50796874572249,0.845549453110653));
#94066=DIRECTION('center_axis',(-0.981627005099017,1.30427605301434E-16,
-0.190809912898504));
#94067=DIRECTION('ref_axis',(-0.165447286436924,-0.498170497353102,0.851148254405554));
#94068=DIRECTION('center_axis',(0.,-1.,0.));
#94069=DIRECTION('ref_axis',(0.,0.,-1.));
#94070=DIRECTION('',(-0.190809912898503,0.,0.981627005099017));
#94071=DIRECTION('center_axis',(0.,-1.,0.));
#94072=DIRECTION('ref_axis',(-0.357093458083529,0.,0.934068660321042));
#94073=DIRECTION('',(-0.190809912898503,0.,0.981627005099017));
#94074=DIRECTION('center_axis',(0.,-1.,0.));
#94075=DIRECTION('ref_axis',(-0.352959570505503,0.,0.935638574230761));
#94076=DIRECTION('center_axis',(0.981627005099017,0.,0.190809912898503));
#94077=DIRECTION('ref_axis',(0.,-1.,0.));
#94078=DIRECTION('',(-0.190809912898503,0.,0.981627005099017));
#94079=DIRECTION('center_axis',(0.981627005099017,-4.40793738003239E-16,
0.190809912898504));
#94080=DIRECTION('ref_axis',(-0.167653005397309,-0.477486904547474,0.862495638114722));
#94081=DIRECTION('center_axis',(0.981627005099017,1.46141627281437E-16,
0.190809912898503));
#94082=DIRECTION('ref_axis',(-0.168604119842488,-0.468198184683616,0.867388673335724));
#94083=DIRECTION('center_axis',(0.,1.,0.));
#94084=DIRECTION('ref_axis',(1.,0.,0.));
#94085=DIRECTION('',(-0.190809912898503,0.,0.981627005099017));
#94086=DIRECTION('center_axis',(0.,1.,0.));
#94087=DIRECTION('ref_axis',(-0.388417251131186,0.,0.921483607571884));
#94088=DIRECTION('center_axis',(0.,1.,0.));
#94089=DIRECTION('ref_axis',(-0.38371415291867,0.,0.923451920161471));
#94090=DIRECTION('center_axis',(-0.981627005099017,0.,-0.190809912898503));
#94091=DIRECTION('ref_axis',(-0.190809912898503,0.,0.981627005099017));
#94092=DIRECTION('center_axis',(-0.981627005099017,3.22716239961749E-16,
-0.190809912898504));
#94093=DIRECTION('ref_axis',(-0.163789338595868,-0.512997515374394,0.84261889474544));
#94094=DIRECTION('center_axis',(-0.981627005099017,3.39688902299908E-16,
-0.190809912898504));
#94095=DIRECTION('ref_axis',(-0.164924280814687,-0.502911144781707,0.848457637158221));
#94096=DIRECTION('center_axis',(0.,-1.,0.));
#94097=DIRECTION('ref_axis',(0.,0.,-1.));
#94098=DIRECTION('',(-0.190809912898503,0.,0.981627005099017));
#94099=DIRECTION('center_axis',(0.,-1.,0.));
#94100=DIRECTION('ref_axis',(-0.427562437492918,0.,0.903985819603999));
#94101=DIRECTION('',(-0.190809912898503,0.,0.981627005099017));
#94102=DIRECTION('center_axis',(0.,-1.,0.));
#94103=DIRECTION('ref_axis',(-0.421725528224158,0.,0.906723540470884));
#94104=DIRECTION('center_axis',(0.981627005099017,0.,0.190809912898503));
#94105=DIRECTION('ref_axis',(0.,-1.,0.));
#94106=DIRECTION('',(-0.190809912898503,0.,0.981627005099017));
#94107=DIRECTION('center_axis',(0.981627005099017,-4.20468084671077E-16,
0.190809912898504));
#94108=DIRECTION('ref_axis',(-0.167044212206533,-0.483311793041112,0.859363684289535));
#94109=DIRECTION('center_axis',(0.981627005099017,4.48762447131239E-17,
0.190809912898503));
#94110=DIRECTION('ref_axis',(-0.168045126361751,-0.473685818224829,0.864512915530322));
#94111=DIRECTION('center_axis',(0.,1.,0.));
#94112=DIRECTION('ref_axis',(1.,0.,0.));
#94113=DIRECTION('',(-0.190809912898503,0.,0.981627005099017));
#94114=DIRECTION('center_axis',(0.,1.,0.));
#94115=DIRECTION('ref_axis',(-0.456948248125761,0.,0.889493281894134));
#94116=DIRECTION('center_axis',(0.,1.,0.));
#94117=DIRECTION('ref_axis',(-0.450667931431808,0.,0.892691668819069));
#94118=DIRECTION('center_axis',(-0.981627005099017,0.,-0.190809912898503));
#94119=DIRECTION('ref_axis',(-0.190809912898503,0.,0.981627005099017));
#94120=DIRECTION('center_axis',(-0.981627005099017,1.5819052248506E-17,
-0.190809912898503));
#94121=DIRECTION('ref_axis',(-0.162927501749981,-0.520480818454586,0.838185150664431));
#94122=DIRECTION('center_axis',(-0.981627005099017,1.21485874416176E-16,
-0.190809912898503));
#94123=DIRECTION('ref_axis',(-0.164134821046406,-0.509955637360102,0.844396239004365));
#94124=DIRECTION('center_axis',(0.,1.,0.));
#94125=DIRECTION('ref_axis',(1.,0.,0.));
#94126=DIRECTION('',(-0.190809912898503,0.,0.981627005099017));
#94127=DIRECTION('',(-0.981627005099017,0.,-0.190809912898503));
#94128=DIRECTION('center_axis',(0.,1.,0.));
#94129=DIRECTION('ref_axis',(-0.523385314028976,0.,0.852096129001177));
#94130=DIRECTION('',(-0.190809912898503,0.,0.981627005099017));
#94131=DIRECTION('center_axis',(0.,1.,0.));
#94132=DIRECTION('ref_axis',(-0.516521998262274,0.,0.856273919555622));
#94133=DIRECTION('center_axis',(-0.981627005099017,0.,-0.190809912898503));
#94134=DIRECTION('ref_axis',(-0.190809912898503,0.,0.981627005099017));
#94135=DIRECTION('',(-0.19080991289849,0.,0.98162700509902));
#94136=DIRECTION('',(0.,-1.,0.));
#94137=DIRECTION('center_axis',(-0.981627005099017,2.04948424643113E-16,
-0.190809912898504));
#94138=DIRECTION('ref_axis',(-0.163030388947302,-0.519595181164497,0.838714456767215));
#94139=DIRECTION('center_axis',(0.,-1.,0.));
#94140=DIRECTION('ref_axis',(0.,0.,-1.));
#94141=DIRECTION('',(-0.190809912898503,0.,0.981627005099017));
#94142=DIRECTION('',(0.981627005099017,0.,0.190809912898503));
#94143=DIRECTION('center_axis',(0.,-1.,0.));
#94144=DIRECTION('ref_axis',(-0.489376531975999,0.,0.87207259442729));
#94145=DIRECTION('center_axis',(0.981627005099017,0.,0.190809912898503));
#94146=DIRECTION('ref_axis',(0.,-1.,0.));
#94147=DIRECTION('center_axis',(0.981627005099017,3.22191216748114E-17,
0.190809912898503));
#94148=DIRECTION('ref_axis',(-0.166164628408473,-0.491569135480225,0.854838640510066));
#94149=DIRECTION('',(0.,1.,0.));
#94150=DIRECTION('center_axis',(0.981627005099017,2.00892259541186E-16,
0.190809912898503));
#94151=DIRECTION('ref_axis',(-0.167239670018067,-0.481451652480913,0.860369222540908));
#94152=DIRECTION('center_axis',(-0.190809912898503,0.,0.981627005099017));
#94153=DIRECTION('ref_axis',(0.,1.,0.));
#94154=DIRECTION('center_axis',(0.190809912898503,-3.49693752527234E-17,
-0.981627005099017));
#94155=DIRECTION('ref_axis',(-0.483557533970894,-0.870251193216613,-0.0939945319954744));
#94156=DIRECTION('center_axis',(0.,1.,0.));
#94157=DIRECTION('ref_axis',(1.,0.,0.));
#94158=DIRECTION('',(-0.190809912898503,0.,0.981627005099017));
#94159=DIRECTION('',(-0.981627005099017,0.,-0.190809912898503));
#94160=DIRECTION('center_axis',(0.,1.,0.));
#94161=DIRECTION('ref_axis',(-0.666090131706357,0.,0.745871259966094));
#94162=DIRECTION('',(-0.190809912898503,0.,0.981627005099017));
#94163=DIRECTION('center_axis',(0.,1.,0.));
#94164=DIRECTION('ref_axis',(-0.668602144346241,0.,0.743620314794861));
#94165=DIRECTION('center_axis',(-0.981627005099017,0.,-0.190809912898503));
#94166=DIRECTION('ref_axis',(-0.190809912898503,0.,0.981627005099017));
#94167=DIRECTION('',(-0.19080991289849,0.,0.98162700509902));
#94168=DIRECTION('',(0.,-1.,0.));
#94169=DIRECTION('center_axis',(-0.981627005099017,1.42070106006851E-16,
-0.190809912898504));
#94170=DIRECTION('ref_axis',(-0.178705808705077,-0.350495021766094,0.91935709800504));
#94171=DIRECTION('center_axis',(0.,-1.,0.));
#94172=DIRECTION('ref_axis',(0.,0.,-1.));
#94173=DIRECTION('',(-0.190809912898503,0.,0.981627005099017));
#94174=DIRECTION('',(0.981627005099017,0.,0.190809912898503));
#94175=DIRECTION('center_axis',(0.,-1.,0.));
#94176=DIRECTION('ref_axis',(-0.644082689417421,0.,0.76495587401681));
#94177=DIRECTION('center_axis',(0.981627005099017,0.,0.190809912898503));
#94178=DIRECTION('ref_axis',(0.,-1.,0.));
#94179=DIRECTION('center_axis',(0.981627005099017,-7.65116657223729E-17,
0.190809912898504));
#94180=DIRECTION('ref_axis',(-0.181063354814559,-0.315516578947016,0.931485560786032));
#94181=DIRECTION('',(-2.42927638559096E-14,1.,1.24974812195102E-13));
#94182=DIRECTION('center_axis',(0.981627005099017,-5.46289132020529E-17,
0.190809912898503));
#94183=DIRECTION('ref_axis',(-0.181543217971292,-0.307849891233687,0.933954230396776));
#94184=DIRECTION('center_axis',(-0.190809912898503,0.,0.981627005099017));
#94185=DIRECTION('ref_axis',(0.,1.,0.));
#94186=DIRECTION('center_axis',(0.190809912898504,3.26380835692085E-16,
-0.981627005099017));
#94187=DIRECTION('ref_axis',(-0.820923255345953,-0.548289841013012,-0.159572112457437));
#94188=DIRECTION('center_axis',(0.981627005099017,0.,0.190809912898503));
#94189=DIRECTION('ref_axis',(0.,-1.,0.));
#94190=DIRECTION('',(-0.190809912898503,0.,0.981627005099017));
#94191=DIRECTION('center_axis',(0.981627005099017,-1.24331456798856E-16,
0.190809912898504));
#94192=DIRECTION('ref_axis',(-0.185131631876501,-0.242140630354711,0.952414927439804));
#94193=DIRECTION('',(-0.190809912898503,0.,0.981627005099017));
#94194=DIRECTION('center_axis',(0.981627005099017,-1.18362645271115E-16,
0.190809912898504));
#94195=DIRECTION('ref_axis',(-0.185408204469832,-0.236256893272313,0.953837762985188));
#94196=DIRECTION('center_axis',(0.,1.,0.));
#94197=DIRECTION('ref_axis',(1.,0.,0.));
#94198=DIRECTION('',(-0.190809912898503,0.,0.981627005099017));
#94199=DIRECTION('center_axis',(0.,1.,0.));
#94200=DIRECTION('ref_axis',(-0.670325070726556,0.,0.742067584223591));
#94201=DIRECTION('center_axis',(0.,1.,0.));
#94202=DIRECTION('ref_axis',(-0.661396304967786,0.,0.75003661762274));
#94203=DIRECTION('center_axis',(-0.981627005099017,0.,-0.190809912898503));
#94204=DIRECTION('ref_axis',(-0.190809912898503,0.,0.981627005099017));
#94205=DIRECTION('',(-0.190809912898503,0.,0.981627005099017));
#94206=DIRECTION('center_axis',(-0.981627005099017,1.29599606305268E-16,
-0.190809912898504));
#94207=DIRECTION('ref_axis',(-0.18291500399328,-0.284674558222307,0.941011422467906));
#94208=DIRECTION('center_axis',(-0.981627005099017,3.78853616018271E-17,
-0.190809912898503));
#94209=DIRECTION('ref_axis',(-0.183317340516521,-0.277475225564888,0.943081254115288));
#94210=DIRECTION('center_axis',(0.,-1.,0.));
#94211=DIRECTION('ref_axis',(0.,0.,-1.));
#94212=DIRECTION('center_axis',(0.,-1.,0.));
#94213=DIRECTION('ref_axis',(-0.644808210944829,0.,0.76434440607499));
#94214=DIRECTION('center_axis',(0.,-1.,0.));
#94215=DIRECTION('ref_axis',(-0.636173251407937,0.,0.771546235939917));
#94216=DIRECTION('center_axis',(0.,-1.,0.));
#94217=DIRECTION('ref_axis',(0.,0.,-1.));
#94218=DIRECTION('',(-0.190809912898503,0.,0.981627005099017));
#94219=DIRECTION('center_axis',(0.,-1.,0.));
#94220=DIRECTION('ref_axis',(-0.638671662809062,0.,0.769479374073606));
#94221=DIRECTION('',(-0.190809912898503,0.,0.981627005099017));
#94222=DIRECTION('center_axis',(0.,-1.,0.));
#94223=DIRECTION('ref_axis',(-0.630378608858621,0.,0.776287839331178));
#94224=DIRECTION('center_axis',(0.981627005099017,0.,0.190809912898503));
#94225=DIRECTION('ref_axis',(0.,-1.,0.));
#94226=DIRECTION('',(-0.190809912898503,0.,0.981627005099017));
#94227=DIRECTION('center_axis',(0.981627005099017,-9.56395821529661E-17,
0.190809912898504));
#94228=DIRECTION('ref_axis',(-0.188073006346447,-0.168764681762398,0.967546911768854));
#94229=DIRECTION('center_axis',(0.981627005099017,-2.23068062241716E-16,
0.190809912898504));
#94230=DIRECTION('ref_axis',(-0.18820530720141,-0.164663895310999,0.968227537267057));
#94231=DIRECTION('center_axis',(0.,1.,0.));
#94232=DIRECTION('ref_axis',(1.,0.,0.));
#94233=DIRECTION('',(-0.190809912898503,0.,0.981627005099017));
#94234=DIRECTION('center_axis',(0.,1.,0.));
#94235=DIRECTION('ref_axis',(-0.664925875210949,0.,0.746909352247616));
#94236=DIRECTION('center_axis',(0.,1.,0.));
#94237=DIRECTION('ref_axis',(-0.656292015446062,0.,0.75450698503178));
#94238=DIRECTION('center_axis',(-0.981627005099017,0.,-0.190809912898503));
#94239=DIRECTION('ref_axis',(-0.190809912898503,0.,0.981627005099017));
#94240=DIRECTION('center_axis',(-0.981627005099017,4.48614021825927E-17,
-0.190809912898503));
#94241=DIRECTION('ref_axis',(-0.186564938338183,-0.209760200795403,0.959788613156638));
#94242=DIRECTION('center_axis',(-0.981627005099017,-2.84140212013703E-17,
-0.190809912898503));
#94243=DIRECTION('ref_axis',(-0.186779220325047,-0.204455429363609,0.960890992911532));
#94244=DIRECTION('center_axis',(0.,-1.,0.));
#94245=DIRECTION('ref_axis',(0.,0.,-1.));
#94246=DIRECTION('',(-0.190809912898503,0.,0.981627005099017));
#94247=DIRECTION('center_axis',(0.,-1.,0.));
#94248=DIRECTION('ref_axis',(-0.634540109712014,0.,0.772889933410098));
#94249=DIRECTION('',(-0.190809912898503,0.,0.981627005099017));
#94250=DIRECTION('center_axis',(0.,-1.,0.));
#94251=DIRECTION('ref_axis',(-0.626472251574789,0.,0.779443723437949));
#94252=DIRECTION('center_axis',(0.981627005099017,0.,0.190809912898503));
#94253=DIRECTION('ref_axis',(0.,-1.,0.));
#94254=DIRECTION('',(-0.190809912898503,0.,0.981627005099017));
#94255=DIRECTION('center_axis',(0.981627005099017,2.15189059844174E-17,
0.190809912898503));
#94256=DIRECTION('ref_axis',(-0.189939838479203,-0.0953887331700394,0.977150882588103));
#94257=DIRECTION('center_axis',(0.981627005099017,-2.95906613177786E-17,
0.190809912898504));
#94258=DIRECTION('ref_axis',(-0.189981699417399,-0.0930708973497062,0.977366237371129));
#94259=DIRECTION('center_axis',(0.,1.,0.));
#94260=DIRECTION('ref_axis',(1.,0.,0.));
#94261=DIRECTION('',(-0.190809912898513,0.,0.981627005099015));
#94262=DIRECTION('center_axis',(0.,1.,0.));
#94263=DIRECTION('ref_axis',(-0.661550435497198,0.,0.749900674285246));
#94264=DIRECTION('center_axis',(0.,1.,0.));
#94265=DIRECTION('ref_axis',(-0.653097727316854,0.,0.757273635202996));
#94266=DIRECTION('center_axis',(-0.981627005099017,0.,-0.190809912898503));
#94267=DIRECTION('ref_axis',(-0.190809912898503,0.,0.981627005099017));
#94268=DIRECTION('center_axis',(-0.981627005099017,1.14645805577737E-16,
-0.190809912898504));
#94269=DIRECTION('ref_axis',(-0.189067167669161,-0.1348458433685,0.97266140287142));
#94270=DIRECTION('center_axis',(-0.981627005099017,9.47134040045677E-17,
-0.190809912898504));
#94271=DIRECTION('ref_axis',(-0.189154580960868,-0.131435633162295,0.973111103028192));
#94272=DIRECTION('center_axis',(0.,-1.,0.));
#94273=DIRECTION('ref_axis',(0.,0.,-1.));
#94274=DIRECTION('',(-0.190809912898503,0.,0.981627005099017));
#94275=DIRECTION('center_axis',(0.,-1.,0.));
#94276=DIRECTION('ref_axis',(-0.632255301211611,0.,0.774760113899661));
#94277=DIRECTION('',(-0.190809912898503,0.,0.981627005099017));
#94278=DIRECTION('center_axis',(0.,-1.,0.));
#94279=DIRECTION('ref_axis',(-0.624310263777235,0.,0.781176481047912));
#94280=DIRECTION('center_axis',(0.981627005099017,0.,0.190809912898503));
#94281=DIRECTION('ref_axis',(0.,-1.,0.));
#94282=DIRECTION('',(-0.190809912898503,0.,0.981627005099017));
#94283=DIRECTION('center_axis',(0.981627005099017,-6.57522127301642E-18,
0.190809912898504));
#94284=DIRECTION('ref_axis',(-0.190763677615005,-0.0220127845777007,0.981389146372597));
#94285=DIRECTION('center_axis',(0.981627005099017,1.1381023583761E-18,0.190809912898503));
#94286=DIRECTION('ref_axis',(-0.190765897499961,-0.0214778993883992,0.981400566633674));
#94287=DIRECTION('center_axis',(0.,1.,0.));
#94288=DIRECTION('ref_axis',(1.,0.,0.));
#94289=DIRECTION('',(-0.190809912898503,0.,0.981627005099017));
#94290=DIRECTION('center_axis',(0.,1.,0.));
#94291=DIRECTION('ref_axis',(-0.660073373181361,0.,0.751201132864548));
#94292=DIRECTION('center_axis',(0.,1.,0.));
#94293=DIRECTION('ref_axis',(-0.651699160648413,0.,0.758477556695091));
#94294=DIRECTION('center_axis',(-0.981627005099017,0.,-0.190809912898503));
#94295=DIRECTION('ref_axis',(-0.190809912898503,0.,0.981627005099017));
#94296=DIRECTION('center_axis',(-0.981627005099017,1.99384009700412E-17,
-0.190809912898504));
#94297=DIRECTION('ref_axis',(-0.190466930740712,-0.0599314859415386,0.979862523666995));
#94298=DIRECTION('center_axis',(-0.981627005099017,-3.07818563014845E-17,
-0.190809912898503));
#94299=DIRECTION('ref_axis',(-0.19048407385867,-0.0584158369610204,0.979950716923228));
#94300=DIRECTION('center_axis',(0.,1.,0.));
#94301=DIRECTION('ref_axis',(1.,0.,0.));
#94302=DIRECTION('',(-0.190809912898503,0.,0.981627005099017));
#94303=DIRECTION('center_axis',(0.,1.,0.));
#94304=DIRECTION('ref_axis',(0.358991707710534,0.,0.933340749027425));
#94305=DIRECTION('',(-0.190809912898503,0.,0.981627005099017));
#94306=DIRECTION('center_axis',(0.,1.,0.));
#94307=DIRECTION('ref_axis',(0.347885431423932,0.,0.937537053456014));
#94308=DIRECTION('center_axis',(-0.981627005099017,0.,-0.190809912898503));
#94309=DIRECTION('ref_axis',(-0.190809912898503,0.,0.981627005099017));
#94310=DIRECTION('',(-0.190809912898503,0.,0.981627005099017));
#94311=DIRECTION('center_axis',(-0.981627005099017,2.58515321514558E-18,
-0.190809912898503));
#94312=DIRECTION('ref_axis',(-0.190454140668356,-0.0610376803135203,0.979796724777248));
#94313=DIRECTION('center_axis',(-0.981627005099017,4.65783098075688E-17,
-0.190809912898504));
#94314=DIRECTION('ref_axis',(-0.190472551870653,-0.0594387870801789,0.979891441729296));
#94315=DIRECTION('center_axis',(0.,-1.,0.));
#94316=DIRECTION('ref_axis',(0.,0.,-1.));
#94317=DIRECTION('',(-0.190809912898503,0.,0.981627005099017));
#94318=DIRECTION('',(0.981627005099017,-5.774756729131E-14,0.190809912898503));
#94319=DIRECTION('center_axis',(0.,-1.,0.));
#94320=DIRECTION('ref_axis',(0.394942270734479,0.,0.918705939235778));
#94321=DIRECTION('center_axis',(0.,-1.,0.));
#94322=DIRECTION('ref_axis',(0.383559494744058,0.,0.923516168776531));
#94323=DIRECTION('center_axis',(0.981627005099017,0.,0.190809912898503));
#94324=DIRECTION('ref_axis',(0.,-1.,0.));
#94325=DIRECTION('center_axis',(0.981627005099017,-8.15668315070832E-18,
0.190809912898504));
#94326=DIRECTION('ref_axis',(-0.190757335946959,-0.0234737412435989,0.98135652148159));
#94327=DIRECTION('',(0.,1.,0.));
#94328=DIRECTION('center_axis',(0.981627005099017,1.09286110344539E-17,
0.190809912898503));
#94329=DIRECTION('ref_axis',(-0.190760187776512,-0.0228283311400105,0.98137119279956));
#94330=DIRECTION('center_axis',(-0.190809912898503,0.,0.981627005099017));
#94331=DIRECTION('ref_axis',(0.,1.,0.));
#94332=DIRECTION('center_axis',(0.190809912898504,-6.70246359010532E-17,
-0.981627005099017));
#94333=DIRECTION('ref_axis',(0.978360591987681,-0.0815109057565992,0.190174983339693));
#94334=DIRECTION('center_axis',(-0.981627005099017,0.,-0.190809912898503));
#94335=DIRECTION('ref_axis',(-0.190809912898503,0.,0.981627005099017));
#94336=DIRECTION('',(-0.190809912898503,0.,0.981627005099017));
#94337=DIRECTION('center_axis',(-0.981627005099017,-5.17030643029117E-17,
-0.190809912898503));
#94338=DIRECTION('ref_axis',(-0.189001929486472,-0.137334780705401,0.972325783191514));
#94339=DIRECTION('',(-0.190809912898503,0.,0.981627005099017));
#94340=DIRECTION('center_axis',(-0.981627005099017,1.02962579574626E-16,
-0.190809912898504));
#94341=DIRECTION('ref_axis',(-0.189095833571211,-0.133737270930404,0.972808875417004));
#94342=DIRECTION('center_axis',(0.,-1.,0.));
#94343=DIRECTION('ref_axis',(0.,0.,-1.));
#94344=DIRECTION('',(-0.190809912898503,0.,0.981627005099017));
#94345=DIRECTION('',(0.981627005099017,0.,0.190809912898503));
#94346=DIRECTION('center_axis',(0.,-1.,0.));
#94347=DIRECTION('ref_axis',(0.387469259730511,0.,0.921882624179396));
#94348=DIRECTION('center_axis',(0.,-1.,0.));
#94349=DIRECTION('ref_axis',(0.386800467114359,0.,0.922163433801251));
#94350=DIRECTION('center_axis',(0.981627005099017,0.,0.190809912898503));
#94351=DIRECTION('ref_axis',(0.,-1.,0.));
#94352=DIRECTION('',(-0.190809912898503,0.,0.981627005099017));
#94353=DIRECTION('',(0.,1.,0.));
#94354=DIRECTION('center_axis',(0.981627005099017,1.28571894522987E-17,
0.190809912898503));
#94355=DIRECTION('ref_axis',(-0.189874012029069,-0.0989227682733557,0.976812236549646));
#94356=DIRECTION('center_axis',(0.,1.,0.));
#94357=DIRECTION('ref_axis',(1.,0.,0.));
#94358=DIRECTION('center_axis',(0.,1.,0.));
#94359=DIRECTION('ref_axis',(0.36095771605842,0.,0.932582182554379));
#94360=DIRECTION('',(-0.981627005099017,0.,-0.190809912898503));
#94361=DIRECTION('center_axis',(0.,1.,0.));
#94362=DIRECTION('ref_axis',(0.349735592176022,0.,0.93684844855787));
#94363=DIRECTION('center_axis',(-0.190809912898503,0.,0.981627005099017));
#94364=DIRECTION('ref_axis',(0.,1.,0.));
#94365=DIRECTION('center_axis',(0.190809912898504,-8.15952089230212E-17,
-0.981627005099017));
#94366=DIRECTION('ref_axis',(0.970679932351344,-0.148928067215399,0.188682006894872));
#94367=DIRECTION('center_axis',(-0.981627005099017,0.,-0.190809912898503));
#94368=DIRECTION('ref_axis',(-0.190809912898503,0.,0.981627005099017));
#94369=DIRECTION('',(-0.190809912898503,0.,0.981627005099017));
#94370=DIRECTION('center_axis',(-0.981627005099017,-5.17030643029117E-18,
-0.190809912898503));
#94371=DIRECTION('ref_axis',(-0.186404919780389,-0.213631881097296,0.958965393150607));
#94372=DIRECTION('',(-0.190809912898503,0.,0.981627005099017));
#94373=DIRECTION('center_axis',(-0.981627005099017,2.94178798784645E-17,
-0.190809912898503));
#94374=DIRECTION('ref_axis',(-0.186635225155084,-0.208035754780595,0.960150205678351));
#94375=DIRECTION('center_axis',(0.,-1.,0.));
#94376=DIRECTION('ref_axis',(0.,0.,-1.));
#94377=DIRECTION('',(-0.190809912898503,0.,0.981627005099017));
#94378=DIRECTION('',(0.981627005099017,0.,0.190809912898503));
#94379=DIRECTION('center_axis',(0.,-1.,0.));
#94380=DIRECTION('ref_axis',(0.373637525799342,0.,0.927574794458402));
#94381=DIRECTION('center_axis',(0.,-1.,0.));
#94382=DIRECTION('ref_axis',(0.392669915561929,0.,0.919679475367689));
#94383=DIRECTION('center_axis',(0.981627005099017,0.,0.190809912898503));
#94384=DIRECTION('ref_axis',(0.,-1.,0.));
#94385=DIRECTION('',(-0.190809912898503,0.,0.981627005099017));
#94386=DIRECTION('',(0.,1.,0.));
#94387=DIRECTION('center_axis',(0.981627005099017,4.11430062473558E-17,
0.190809912898503));
#94388=DIRECTION('ref_axis',(-0.187864833462401,-0.175017205406708,0.966475960466566));
#94389=DIRECTION('center_axis',(0.,1.,0.));
#94390=DIRECTION('ref_axis',(1.,0.,0.));
#94391=DIRECTION('center_axis',(0.,1.,0.));
#94392=DIRECTION('ref_axis',(0.365458588656494,0.,0.930827599492626));
#94393=DIRECTION('',(-0.981627005099017,0.,-0.190809912898503));
#94394=DIRECTION('center_axis',(0.,1.,0.));
#94395=DIRECTION('ref_axis',(0.353968321307143,0.,0.935257412433071));
#94396=DIRECTION('center_axis',(-0.190809912898503,0.,0.981627005099017));
#94397=DIRECTION('ref_axis',(0.,1.,0.));
#94398=DIRECTION('center_axis',(0.190809912898502,2.03988022307553E-16,
-0.981627005099017));
#94399=DIRECTION('ref_axis',(0.94693889934147,-0.263488118919596,0.184067194530089));
#94400=DIRECTION('center_axis',(0.,1.,0.));
#94401=DIRECTION('ref_axis',(1.,0.,0.));
#94402=DIRECTION('',(-0.190809912898503,0.,0.981627005099017));
#94403=DIRECTION('center_axis',(0.,1.,0.));
#94404=DIRECTION('ref_axis',(0.184145244684996,0.,0.982899043065921));
#94405=DIRECTION('',(-0.190809912898503,0.,0.981627005099017));
#94406=DIRECTION('center_axis',(0.,1.,0.));
#94407=DIRECTION('ref_axis',(0.175315692747643,0.,0.984512269032953));
#94408=DIRECTION('center_axis',(-0.981627005099017,0.,-0.190809912898503));
#94409=DIRECTION('ref_axis',(-0.190809912898503,0.,0.981627005099017));
#94410=DIRECTION('',(-0.190809912898503,0.,0.981627005099017));
#94411=DIRECTION('center_axis',(-0.981627005099017,-6.70372400852628E-17,
-0.190809912898503));
#94412=DIRECTION('ref_axis',(-0.168720726956303,-0.467043009411895,0.867988561937781));
#94413=DIRECTION('center_axis',(-0.981627005099017,3.04952953295968E-16,
-0.190809912898504));
#94414=DIRECTION('ref_axis',(-0.169713673567315,-0.457054963856906,0.873096803921564));
#94415=DIRECTION('center_axis',(0.,-1.,0.));
#94416=DIRECTION('ref_axis',(0.,0.,-1.));
#94417=DIRECTION('',(-0.190809912898503,0.,0.981627005099017));
#94418=DIRECTION('',(0.981627005099017,0.,0.190809912898503));
#94419=DIRECTION('center_axis',(0.,-1.,0.));
#94420=DIRECTION('ref_axis',(0.211589721837698,0.,0.977358577806859));
#94421=DIRECTION('center_axis',(0.,-1.,0.));
#94422=DIRECTION('ref_axis',(0.218730261134039,0.,0.975785362087501));
#94423=DIRECTION('center_axis',(0.981627005099017,0.,0.190809912898503));
#94424=DIRECTION('ref_axis',(0.,-1.,0.));
#94425=DIRECTION('center_axis',(0.981627005099017,-2.83825609674828E-16,
0.190809912898504));
#94426=DIRECTION('ref_axis',(-0.171498597492433,-0.43837346986139,0.882279395645061));
#94427=DIRECTION('',(0.,1.,0.));
#94428=DIRECTION('center_axis',(0.981627005099017,-3.12650905815778E-16,
0.190809912898504));
#94429=DIRECTION('ref_axis',(-0.172381261221582,-0.428759238128314,0.886820284217318));
#94430=DIRECTION('center_axis',(-0.190809912898503,0.,0.981627005099017));
#94431=DIRECTION('ref_axis',(0.,1.,0.));
#94432=DIRECTION('center_axis',(0.190809912898504,-6.87731046636893E-16,
-0.981627005099017));
#94433=DIRECTION('ref_axis',(0.640994870612618,-0.757364550955772,0.12459740287773));
#94434=DIRECTION('center_axis',(0.,-1.,0.));
#94435=DIRECTION('ref_axis',(0.,0.,-1.));
#94436=DIRECTION('',(-0.190809912898503,1.255691120406E-14,0.981627005099017));
#94437=DIRECTION('center_axis',(0.,-1.,0.));
#94438=DIRECTION('ref_axis',(0.152737602003591,0.,0.988266778220432));
#94439=DIRECTION('',(-0.190809912898503,0.,0.981627005099017));
#94440=DIRECTION('center_axis',(0.,-1.,0.));
#94441=DIRECTION('ref_axis',(0.144410991615934,0.,0.989517794433482));
#94442=DIRECTION('center_axis',(0.981627005099017,0.,0.190809912898503));
#94443=DIRECTION('ref_axis',(0.,-1.,0.));
#94444=DIRECTION('',(-0.190809912898503,0.,0.981627005099017));
#94445=DIRECTION('center_axis',(0.981627005099017,-1.31015175507947E-16,
0.190809912898504));
#94446=DIRECTION('ref_axis',(-0.172473747912141,-0.427736442803512,0.887296084618284));
#94447=DIRECTION('center_axis',(0.981627005099017,-2.82583468587877E-16,
0.190809912898504));
#94448=DIRECTION('ref_axis',(-0.173271151848023,-0.418791220542401,0.891398351767528));
#94449=DIRECTION('center_axis',(0.,1.,0.));
#94450=DIRECTION('ref_axis',(1.,0.,0.));
#94451=DIRECTION('',(-0.190809912898503,0.,0.981627005099017));
#94452=DIRECTION('center_axis',(0.,1.,0.));
#94453=DIRECTION('ref_axis',(0.10984303932686,0.,0.99394894572681));
#94454=DIRECTION('center_axis',(0.,1.,0.));
#94455=DIRECTION('ref_axis',(0.102818743046302,0.,0.994700108614842));
#94456=DIRECTION('center_axis',(-0.981627005099017,0.,-0.190809912898503));
#94457=DIRECTION('ref_axis',(-0.190809912898503,0.,0.981627005099017));
#94458=DIRECTION('center_axis',(-0.981627005099017,1.28381668760922E-16,
-0.190809912898504));
#94459=DIRECTION('ref_axis',(-0.169717089537917,-0.457020123580983,0.873114377479149));
#94460=DIRECTION('center_axis',(-0.981627005099017,3.38719187348766E-16,
-0.190809912898504));
#94461=DIRECTION('ref_axis',(-0.17062403409845,-0.447648741208883,0.877780179476658));
#94462=DIRECTION('center_axis',(0.,-1.,0.));
#94463=DIRECTION('ref_axis',(0.,0.,-1.));
#94464=DIRECTION('',(-0.190809912898503,0.,0.981627005099017));
#94465=DIRECTION('center_axis',(0.,-1.,0.));
#94466=DIRECTION('ref_axis',(0.0776743290905875,0.,0.996978785431429));
#94467=DIRECTION('',(-0.190809912898503,0.,0.981627005099017));
#94468=DIRECTION('center_axis',(0.,-1.,0.));
#94469=DIRECTION('ref_axis',(0.0712170703537014,0.,0.997460840780347));
#94470=DIRECTION('center_axis',(0.981627005099017,0.,0.190809912898503));
#94471=DIRECTION('ref_axis',(0.,-1.,0.));
#94472=DIRECTION('',(-0.190809912898503,0.,0.981627005099017));
#94473=DIRECTION('center_axis',(0.981627005099017,-2.8379520623381E-16,
0.190809912898504));
#94474=DIRECTION('ref_axis',(-0.173192120088612,-0.419688163031609,0.890991770641214));
#94475=DIRECTION('center_axis',(0.981627005099017,1.81646488737385E-16,
0.190809912898503));
#94476=DIRECTION('ref_axis',(-0.173929387576568,-0.411228614003993,0.894784664129641));
#94477=DIRECTION('center_axis',(0.,1.,0.));
#94478=DIRECTION('ref_axis',(1.,0.,0.));
#94479=DIRECTION('',(-0.190809912898503,0.,0.981627005099017));
#94480=DIRECTION('center_axis',(0.,1.,0.));
#94481=DIRECTION('ref_axis',(0.0366430595622812,0.,0.999328417581485));
#94482=DIRECTION('center_axis',(0.,1.,0.));
#94483=DIRECTION('ref_axis',(0.0313675707532251,0.,0.999507916679524));
#94484=DIRECTION('center_axis',(-0.981627005099017,0.,-0.190809912898503));
#94485=DIRECTION('ref_axis',(-0.190809912898503,0.,0.981627005099017));
#94486=DIRECTION('center_axis',(-0.981627005099017,2.3292971780749E-16,
-0.190809912898504));
#94487=DIRECTION('ref_axis',(-0.170440188767048,-0.449568246953191,0.876834381958468));
#94488=DIRECTION('center_axis',(-0.981627005099017,2.53604646310564E-16,
-0.190809912898504));
#94489=DIRECTION('ref_axis',(-0.171287079367587,-0.440639018251895,0.88119123465666));
#94490=DIRECTION('center_axis',(0.,-1.,0.));
#94491=DIRECTION('ref_axis',(0.,0.,-1.));
#94492=DIRECTION('',(-0.190809912898503,0.,0.981627005099017));
#94493=DIRECTION('center_axis',(0.,-1.,0.));
#94494=DIRECTION('ref_axis',(0.00371858367446118,0.,0.999993086043827));
#94495=DIRECTION('',(-0.190809912898503,0.,0.981627005099017));
#94496=DIRECTION('center_axis',(0.,-1.,0.));
#94497=DIRECTION('ref_axis',(-0.000926353014041966,0.,0.999999570934955));
#94498=DIRECTION('center_axis',(0.981627005099017,0.,0.190809912898503));
#94499=DIRECTION('ref_axis',(0.,-1.,0.));
#94500=DIRECTION('',(-0.190809912898503,0.,0.981627005099017));
#94501=DIRECTION('center_axis',(0.981627005099017,-3.2195030332024E-16,
0.190809912898504));
#94502=DIRECTION('ref_axis',(-0.17370268013601,-0.413852151503288,0.893618361276035));
#94503=DIRECTION('center_axis',(0.981627005099017,-1.03147739908772E-16,
0.190809912898504));
#94504=DIRECTION('ref_axis',(-0.174398591463139,-0.405733888890709,0.897198496822913));
#94505=DIRECTION('center_axis',(0.,1.,0.));
#94506=DIRECTION('ref_axis',(1.,0.,0.));
#94507=DIRECTION('',(-0.190809912898503,0.,0.981627005099017));
#94508=DIRECTION('center_axis',(0.,1.,0.));
#94509=DIRECTION('ref_axis',(-0.0355191393229559,0.,0.999368996288036));
#94510=DIRECTION('center_axis',(0.,1.,0.));
#94511=DIRECTION('ref_axis',(-0.0390960923094082,0.,0.999235455518935));
#94512=DIRECTION('center_axis',(-0.981627005099017,0.,-0.190809912898503));
#94513=DIRECTION('ref_axis',(-0.190809912898503,0.,0.981627005099017));
#94514=DIRECTION('center_axis',(-0.981627005099017,-2.27558651128372E-16,
-0.190809912898503));
#94515=DIRECTION('ref_axis',(-0.170937231783471,-0.444354778157526,0.879391433844326));
#94516=DIRECTION('center_axis',(-0.981627005099017,-1.02110124627879E-16,
-0.190809912898503));
#94517=DIRECTION('ref_axis',(-0.171743997738244,-0.435726718837086,0.883541864165107));
#94518=DIRECTION('center_axis',(0.,-1.,0.));
#94519=DIRECTION('ref_axis',(0.,0.,-1.));
#94520=DIRECTION('',(-0.190809912898503,0.,0.981627005099017));
#94521=DIRECTION('center_axis',(0.,-1.,0.));
#94522=DIRECTION('ref_axis',(-0.0691867906738412,0.,0.99760372292622));
#94523=DIRECTION('',(-0.190809912898503,0.,0.981627005099017));
#94524=DIRECTION('center_axis',(0.,-1.,0.));
#94525=DIRECTION('ref_axis',(-0.0720708919844832,0.,0.997399511995349));
#94526=DIRECTION('center_axis',(0.981627005099017,0.,0.190809912898503));
#94527=DIRECTION('ref_axis',(0.,-1.,0.));
#94528=DIRECTION('',(-0.190809912898503,0.,0.981627005099017));
#94529=DIRECTION('center_axis',(0.981627005099017,-1.50452980269455E-17,
0.190809912898503));
#94530=DIRECTION('ref_axis',(-0.174036822496206,-0.409978274115724,0.895337366118781));
#94531=DIRECTION('center_axis',(0.981627005099017,-2.02598138069568E-16,
0.190809912898504));
#94532=DIRECTION('ref_axis',(-0.174706292097902,-0.402081556480905,0.898781471459718));
#94533=DIRECTION('center_axis',(0.,1.,0.));
#94534=DIRECTION('ref_axis',(1.,0.,0.));
#94535=DIRECTION('',(-0.190809912898503,0.,0.981627005099017));
#94536=DIRECTION('center_axis',(0.,1.,0.));
#94537=DIRECTION('ref_axis',(-0.106686710809781,0.,0.994292686152619));
#94538=DIRECTION('center_axis',(0.,1.,0.));
#94539=DIRECTION('ref_axis',(-0.108611424892643,0.,0.99408428132769));
#94540=DIRECTION('center_axis',(-0.981627005099017,0.,-0.190809912898503));
#94541=DIRECTION('ref_axis',(-0.190809912898503,0.,0.981627005099017));
#94542=DIRECTION('center_axis',(-0.981627005099017,2.09348652609932E-16,
-0.190809912898504));
#94543=DIRECTION('ref_axis',(-0.171237890630439,-0.441163807051188,0.880938181804228));
#94544=DIRECTION('center_axis',(-0.981627005099017,-1.58249582464702E-16,
-0.190809912898503));
#94545=DIRECTION('ref_axis',(-0.172020843188232,-0.432716795710511,0.884966103429299));
#94546=DIRECTION('center_axis',(0.,-1.,0.));
#94547=DIRECTION('ref_axis',(0.,0.,-1.));
#94548=DIRECTION('',(-0.190809912898503,0.,0.981627005099017));
#94549=DIRECTION('center_axis',(0.,-1.,0.));
#94550=DIRECTION('ref_axis',(-0.141078288382398,0.,0.989998442699327));
#94551=DIRECTION('',(-0.190809912898503,0.,0.981627005099017));
#94552=DIRECTION('center_axis',(0.,-1.,0.));
#94553=DIRECTION('ref_axis',(-0.142249621027872,0.,0.98983081651231));
#94554=DIRECTION('center_axis',(0.981627005099017,0.,0.190809912898503));
#94555=DIRECTION('ref_axis',(0.,-1.,0.));
#94556=DIRECTION('',(-0.190809912898503,-1.082199615072E-14,0.981627005099017));
#94557=DIRECTION('center_axis',(0.981627005099017,-2.23408810325902E-16,
0.190809912898504));
#94558=DIRECTION('ref_axis',(-0.174213626435771,-0.407910574394006,0.896246938997088));
#94559=DIRECTION('center_axis',(0.981627005099017,2.43630309943914E-16,
0.190809912898503));
#94560=DIRECTION('ref_axis',(-0.174869305192863,-0.400130487804013,0.899620096947088));
#94561=DIRECTION('center_axis',(0.,1.,0.));
#94562=DIRECTION('ref_axis',(1.,0.,0.));
#94563=DIRECTION('',(-0.190809912898503,0.,0.981627005099017));
#94564=DIRECTION('center_axis',(0.,1.,0.));
#94565=DIRECTION('ref_axis',(-0.176885309946529,0.,0.98423147029808));
#94566=DIRECTION('center_axis',(0.,1.,0.));
#94567=DIRECTION('ref_axis',(-0.177201781451223,0.,0.98417454176102));
#94568=DIRECTION('center_axis',(-0.981627005099017,0.,-0.190809912898503));
#94569=DIRECTION('ref_axis',(-0.190809912898503,0.,0.981627005099017));
#94570=DIRECTION('center_axis',(-0.981627005099017,1.33792883286904E-16,
-0.190809912898504));
#94571=DIRECTION('ref_axis',(-0.171359055428295,-0.439869713566988,0.881561517541016));
#94572=DIRECTION('center_axis',(-0.981627005099017,1.85967954159957E-16,
-0.190809912898504));
#94573=DIRECTION('ref_axis',(-0.172132508930255,-0.431495418834412,0.885540571004113));
#94574=DIRECTION('center_axis',(0.,-1.,0.));
#94575=DIRECTION('ref_axis',(0.,0.,-1.));
#94576=DIRECTION('',(-0.190809912898503,0.,0.981627005099017));
#94577=DIRECTION('center_axis',(0.,-1.,0.));
#94578=DIRECTION('ref_axis',(-0.211974931298844,0.,0.9772751037967));
#94579=DIRECTION('',(-0.190809912898503,0.,0.981627005099017));
#94580=DIRECTION('center_axis',(0.,-1.,0.));
#94581=DIRECTION('ref_axis',(-0.211479816819108,0.,0.977382364828707));
#94582=DIRECTION('center_axis',(0.981627005099017,0.,0.190809912898503));
#94583=DIRECTION('ref_axis',(0.,-1.,0.));
#94584=DIRECTION('',(-0.190809912898503,0.,0.981627005099017));
#94585=DIRECTION('center_axis',(0.981627005099017,2.97379735788161E-17,
0.190809912898503));
#94586=DIRECTION('ref_axis',(-0.174242731231815,-0.407568990013114,0.896396669445267));
#94587=DIRECTION('center_axis',(0.981627005099017,0.,0.190809912898503));
#94588=DIRECTION('ref_axis',(-0.174896153086883,-0.399808062848099,0.899758216698831));
#94589=DIRECTION('center_axis',(0.,1.,0.));
#94590=DIRECTION('ref_axis',(1.,0.,0.));
#94591=DIRECTION('',(-0.190809912898503,0.,0.981627005099017));
#94592=DIRECTION('center_axis',(0.,1.,0.));
#94593=DIRECTION('ref_axis',(-0.24612518066157,0.,0.969238048904556));
#94594=DIRECTION('center_axis',(0.,1.,0.));
#94595=DIRECTION('ref_axis',(-0.244876500445944,0.,0.969554278794822));
#94596=DIRECTION('center_axis',(-0.981627005099017,0.,-0.190809912898503));
#94597=DIRECTION('ref_axis',(-0.190809912898503,0.,0.981627005099017));
#94598=DIRECTION('center_axis',(-0.981627005099017,1.04323047313055E-16,
-0.190809912898503));
#94599=DIRECTION('ref_axis',(-0.171307312408284,-0.440422929036202,0.881295324107999));
#94600=DIRECTION('center_axis',(-0.981627005099017,3.87176530094412E-16,
-0.190809912898504));
#94601=DIRECTION('ref_axis',(-0.172084815581002,-0.4320175983019,0.885295211217089));
#94602=DIRECTION('center_axis',(0.,-1.,0.));
#94603=DIRECTION('ref_axis',(0.,0.,-1.));
#94604=DIRECTION('',(-0.190809912898503,0.,0.981627005099017));
#94605=DIRECTION('center_axis',(0.,-1.,0.));
#94606=DIRECTION('ref_axis',(-0.28187983172236,0.,0.959449717529884));
#94607=DIRECTION('',(-0.190809912898503,0.,0.981627005099017));
#94608=DIRECTION('center_axis',(0.,-1.,0.));
#94609=DIRECTION('ref_axis',(-0.279764308576818,0.,0.960068711940211));
#94610=DIRECTION('center_axis',(0.981627005099017,0.,0.190809912898503));
#94611=DIRECTION('ref_axis',(0.,-1.,0.));
#94612=DIRECTION('',(-0.190809912898503,0.,0.981627005099017));
#94613=DIRECTION('center_axis',(0.981627005099017,-1.64661493304004E-16,
0.190809912898504));
#94614=DIRECTION('ref_axis',(-0.174125693879922,-0.408940503765383,0.89579456747122));
#94615=DIRECTION('center_axis',(0.981627005099017,-4.32027132019077E-17,
0.190809912898503));
#94616=DIRECTION('ref_axis',(-0.17478821411242,-0.401102463243196,0.899202921585352));
#94617=DIRECTION('center_axis',(0.,1.,0.));
#94618=DIRECTION('ref_axis',(1.,0.,0.));
#94619=DIRECTION('',(-0.190809912898503,0.,0.981627005099017));
#94620=DIRECTION('center_axis',(0.,1.,0.));
#94621=DIRECTION('ref_axis',(-0.314401954981219,0.,0.949289950807438));
#94622=DIRECTION('center_axis',(0.,1.,0.));
#94623=DIRECTION('ref_axis',(-0.311631599069456,0.,0.950203002763838));
#94624=DIRECTION('center_axis',(-0.981627005099017,0.,-0.190809912898503));
#94625=DIRECTION('ref_axis',(-0.190809912898503,0.,0.981627005099017));
#94626=DIRECTION('center_axis',(-0.981627005099017,2.86284995913372E-16,
-0.190809912898504));
#94627=DIRECTION('ref_axis',(-0.171079864292319,-0.442844547552897,0.880125210828773));
#94628=DIRECTION('center_axis',(-0.981627005099017,2.17379342169057E-16,
-0.190809912898504));
#94629=DIRECTION('ref_axis',(-0.171875290112581,-0.434302484871899,0.884217301506146));
#94630=DIRECTION('center_axis',(0.,-1.,0.));
#94631=DIRECTION('ref_axis',(0.,0.,-1.));
#94632=DIRECTION('',(-0.190809912898503,0.,0.981627005099017));
#94633=DIRECTION('center_axis',(0.,-1.,0.));
#94634=DIRECTION('ref_axis',(-0.350780441750461,0.,0.936457730858874));
#94635=DIRECTION('',(-0.190809912898503,0.,0.981627005099017));
#94636=DIRECTION('center_axis',(0.,-1.,0.));
#94637=DIRECTION('ref_axis',(-0.347091693931338,0.,0.937831198032926));
#94638=DIRECTION('center_axis',(0.981627005099017,0.,0.190809912898503));
#94639=DIRECTION('ref_axis',(0.,-1.,0.));
#94640=DIRECTION('',(-0.190809912898503,0.,0.981627005099017));
#94641=DIRECTION('center_axis',(0.981627005099017,-7.5998920345386E-17,
0.190809912898503));
#94642=DIRECTION('ref_axis',(-0.173856202311149,-0.412077739540977,0.894408160457374));
#94643=DIRECTION('center_axis',(0.981627005099017,-2.338266036503E-16,0.190809912898504));
#94644=DIRECTION('ref_axis',(-0.174539903539162,-0.404061447055713,0.89792548080327));
#94645=DIRECTION('center_axis',(0.,1.,0.));
#94646=DIRECTION('ref_axis',(1.,0.,0.));
#94647=DIRECTION('',(-0.190809912898503,0.,0.981627005099017));
#94648=DIRECTION('center_axis',(0.,1.,0.));
#94649=DIRECTION('ref_axis',(-0.381696314616838,0.,0.924287792523478));
#94650=DIRECTION('center_axis',(0.,1.,0.));
#94651=DIRECTION('ref_axis',(-0.377449478914398,0.,0.926030178162272));
#94652=DIRECTION('center_axis',(-0.981627005099017,0.,-0.190809912898503));
#94653=DIRECTION('ref_axis',(-0.190809912898503,0.,0.981627005099017));
#94654=DIRECTION('center_axis',(-0.981627005099017,1.38306959983606E-16,
-0.190809912898504));
#94655=DIRECTION('ref_axis',(-0.170664142574815,-0.447228603146884,0.877986518670128));
#94656=DIRECTION('center_axis',(-0.981627005099017,1.47690827086916E-16,
-0.190809912898504));
#94657=DIRECTION('ref_axis',(-0.171492837474547,-0.438435356989177,0.882249763069791));
#94658=DIRECTION('center_axis',(0.,-1.,0.));
#94659=DIRECTION('ref_axis',(0.,0.,-1.));
#94660=DIRECTION('',(-0.190809912898503,0.,0.981627005099017));
#94661=DIRECTION('center_axis',(0.,-1.,0.));
#94662=DIRECTION('ref_axis',(-0.418647537023905,0.,0.908148798239483));
#94663=DIRECTION('',(-0.190809912898503,0.,0.981627005099017));
#94664=DIRECTION('center_axis',(0.,-1.,0.));
#94665=DIRECTION('ref_axis',(-0.413435459905699,0.,0.910533426345548));
#94666=DIRECTION('center_axis',(0.981627005099017,0.,0.190809912898503));
#94667=DIRECTION('ref_axis',(0.,-1.,0.));
#94668=DIRECTION('',(-0.190809912898503,0.,0.981627005099017));
#94669=DIRECTION('center_axis',(0.981627005099017,-1.24583136198838E-16,
0.190809912898504));
#94670=DIRECTION('ref_axis',(-0.173419200493624,-0.417104698103898,0.892159992221019));
#94671=DIRECTION('center_axis',(0.981627005099017,-4.03886202418115E-16,
0.190809912898504));
#94672=DIRECTION('ref_axis',(-0.174137931887097,-0.408797349974888,0.895857526245995));
#94673=DIRECTION('center_axis',(0.,1.,0.));
#94674=DIRECTION('ref_axis',(1.,0.,0.));
#94675=DIRECTION('',(-0.190809912898503,1.305554049207E-14,0.981627005099017));
#94676=DIRECTION('center_axis',(0.,1.,0.));
#94677=DIRECTION('ref_axis',(-0.447972451854823,0.,0.894047360255136));
#94678=DIRECTION('center_axis',(0.,1.,0.));
#94679=DIRECTION('ref_axis',(-0.442297590336883,0.,0.896868352425364));
#94680=DIRECTION('center_axis',(-0.981627005099017,0.,-0.190809912898503));
#94681=DIRECTION('ref_axis',(-0.190809912898503,0.,0.981627005099017));
#94682=DIRECTION('center_axis',(-0.981627005099017,-9.49143134910359E-17,
-0.190809912898503));
#94683=DIRECTION('ref_axis',(-0.170036007749122,-0.45375250839628,0.874755061255906));
#94684=DIRECTION('center_axis',(-0.981627005099017,-1.67043077322242E-16,
-0.190809912898503));
#94685=DIRECTION('ref_axis',(-0.170916220682317,-0.444576709493399,0.879283341638914));
#94686=DIRECTION('center_axis',(0.,-1.,0.));
#94687=DIRECTION('ref_axis',(0.,0.,-1.));
#94688=DIRECTION('',(-0.190809912898503,0.,0.981627005099017));
#94689=DIRECTION('center_axis',(0.,-1.,0.));
#94690=DIRECTION('ref_axis',(-0.485432735772008,0.,0.874274018280827));
#94691=DIRECTION('',(-0.190809912898503,0.,0.981627005099017));
#94692=DIRECTION('center_axis',(0.,-1.,0.));
#94693=DIRECTION('ref_axis',(-0.47875184538002,0.,0.877950266555701));
#94694=DIRECTION('center_axis',(0.981627005099017,0.,0.190809912898503));
#94695=DIRECTION('ref_axis',(0.,-1.,0.));
#94696=DIRECTION('',(-0.190809912898503,0.,0.981627005099017));
#94697=DIRECTION('center_axis',(0.981627005099017,0.,0.190809912898503));
#94698=DIRECTION('ref_axis',(-0.172788690240708,-0.424230897743185,0.88891631435412));
#94699=DIRECTION('center_axis',(0.981627005099017,-2.47252011742998E-16,
0.190809912898504));
#94700=DIRECTION('ref_axis',(-0.173559449920186,-0.415499371319114,0.892881509371105));
#94701=DIRECTION('center_axis',(0.,1.,0.));
#94702=DIRECTION('ref_axis',(1.,0.,0.));
#94703=DIRECTION('',(-0.190809912898503,0.,0.981627005099017));
#94704=DIRECTION('center_axis',(0.,1.,0.));
#94705=DIRECTION('ref_axis',(-0.513175031076331,0.,0.85828397834272));
#94706=DIRECTION('center_axis',(0.,1.,0.));
#94707=DIRECTION('ref_axis',(-0.506125809124676,0.,0.862459660122079));
#94708=DIRECTION('center_axis',(-0.981627005099017,0.,-0.190809912898503));
#94709=DIRECTION('ref_axis',(-0.190809912898503,0.,0.981627005099017));
#94710=DIRECTION('center_axis',(-0.981627005099017,0.,-0.190809912898503));
#94711=DIRECTION('ref_axis',(-0.169156033040075,-0.462698015255998,0.870228006423779));
#94712=DIRECTION('center_axis',(-0.981627005099017,1.73417897774942E-16,
-0.190809912898504));
#94713=DIRECTION('ref_axis',(-0.170110942777143,-0.452980414348596,0.875140566631467));
#94714=DIRECTION('center_axis',(0.981627005099017,0.,0.190809912898503));
#94715=DIRECTION('ref_axis',(0.,-1.,0.));
#94716=DIRECTION('',(-0.190809912898503,0.,0.981627005099017));
#94717=DIRECTION('center_axis',(0.981627005099017,-2.69483765365246E-16,
0.190809912898504));
#94718=DIRECTION('ref_axis',(-0.171923576181418,-0.433777236382802,0.884465710555865));
#94719=DIRECTION('',(-0.190809912898503,0.,0.981627005099017));
#94720=DIRECTION('center_axis',(0.981627005099017,-7.2569942460446E-17,
0.190809912898503));
#94721=DIRECTION('ref_axis',(-0.172768570512372,-0.4244559030808,0.888812807841434));
#94722=DIRECTION('center_axis',(0.,1.,0.));
#94723=DIRECTION('ref_axis',(1.,0.,0.));
#94724=DIRECTION('',(-0.190809912898503,0.,0.981627005099017));
#94725=DIRECTION('center_axis',(0.,1.,0.));
#94726=DIRECTION('ref_axis',(-0.577224006242642,0.,0.816585847671385));
#94727=DIRECTION('center_axis',(0.,1.,0.));
#94728=DIRECTION('ref_axis',(-0.568861998611027,0.,0.822432992125357));
#94729=DIRECTION('center_axis',(-0.981627005099017,0.,-0.190809912898503));
#94730=DIRECTION('ref_axis',(-0.190809912898503,0.,0.981627005099017));
#94731=DIRECTION('',(-0.190809912898503,0.,0.981627005099017));
#94732=DIRECTION('',(0.,-1.,0.));
#94733=DIRECTION('center_axis',(-0.981627005099017,6.91914718802358E-17,
-0.190809912898503));
#94734=DIRECTION('ref_axis',(-0.169895538310713,-0.455195395847704,0.874032412248634));
#94735=DIRECTION('center_axis',(-0.981627005099017,1.65434297745177E-17,
-0.190809912898503));
#94736=DIRECTION('ref_axis',(-0.169023616517123,-0.464025219406811,0.869546785868324));
#94737=DIRECTION('center_axis',(0.,-1.,0.));
#94738=DIRECTION('ref_axis',(0.,0.,-1.));
#94739=DIRECTION('center_axis',(0.,-1.,0.));
#94740=DIRECTION('ref_axis',(-0.551064033121797,0.,0.834462959872719));
#94741=DIRECTION('',(0.981627005099017,0.,0.190809912898503));
#94742=DIRECTION('center_axis',(0.,-1.,0.));
#94743=DIRECTION('ref_axis',(-0.542976020742699,0.,0.839748200890257));
#94744=DIRECTION('center_axis',(-0.190809912898503,0.,0.981627005099017));
#94745=DIRECTION('ref_axis',(0.,1.,0.));
#94746=DIRECTION('center_axis',(0.190809912898503,1.16564584175745E-16,
-0.981627005099017));
#94747=DIRECTION('ref_axis',(-0.615493430324788,-0.779008351588359,-0.119640400294435));
#94748=DIRECTION('center_axis',(0.981627005099017,0.,0.190809912898503));
#94749=DIRECTION('ref_axis',(0.,-1.,0.));
#94750=DIRECTION('',(-0.190809912898503,0.,0.981627005099017));
#94751=DIRECTION('center_axis',(0.981627005099017,-1.78228754819253E-17,
0.190809912898503));
#94752=DIRECTION('ref_axis',(-0.176855272063147,-0.375391687874098,0.90983695980022));
#94753=DIRECTION('',(-0.190809912898503,0.,0.981627005099017));
#94754=DIRECTION('center_axis',(0.981627005099017,-3.064140942095E-16,0.190809912898504));
#94755=DIRECTION('ref_axis',(-0.177505054319294,-0.366871421003507,0.913179783033972));
#94756=DIRECTION('center_axis',(0.,1.,0.));
#94757=DIRECTION('ref_axis',(1.,0.,0.));
#94758=DIRECTION('',(-0.190809912898503,0.,0.981627005099017));
#94759=DIRECTION('center_axis',(0.,1.,0.));
#94760=DIRECTION('ref_axis',(-0.628205223222824,0.,0.778047683317393));
#94761=DIRECTION('center_axis',(0.,1.,0.));
#94762=DIRECTION('ref_axis',(-0.619332264144748,0.,0.785128999967101));
#94763=DIRECTION('center_axis',(-0.981627005099017,0.,-0.190809912898503));
#94764=DIRECTION('ref_axis',(-0.190809912898503,0.,0.981627005099017));
#94765=DIRECTION('',(-0.190809912898503,0.,0.981627005099017));
#94766=DIRECTION('',(0.,-1.,0.));
#94767=DIRECTION('center_axis',(-0.981627005099017,1.65855791542818E-16,
-0.190809912898504));
#94768=DIRECTION('ref_axis',(-0.175359682635441,-0.394191890059205,0.902142857599366));
#94769=DIRECTION('center_axis',(-0.981627005099017,2.10894926800414E-16,
-0.190809912898504));
#94770=DIRECTION('ref_axis',(-0.174211595031188,-0.407934402882895,0.896236488378634));
#94771=DIRECTION('center_axis',(0.,-1.,0.));
#94772=DIRECTION('ref_axis',(0.,0.,-1.));
#94773=DIRECTION('center_axis',(0.,-1.,0.));
#94774=DIRECTION('ref_axis',(-0.6029066307257,0.,0.797811753878685));
#94775=DIRECTION('',(0.981627005099017,0.,0.190809912898503));
#94776=DIRECTION('center_axis',(0.,-1.,0.));
#94777=DIRECTION('ref_axis',(-0.594284330901843,0.,0.804255018041261));
#94778=DIRECTION('center_axis',(-0.190809912898503,0.,0.981627005099017));
#94779=DIRECTION('ref_axis',(0.,1.,0.));
#94780=DIRECTION('center_axis',(0.190809912898503,-3.49693752527234E-17,
-0.981627005099017));
#94781=DIRECTION('ref_axis',(-0.733603465583051,-0.664448299884183,-0.142598780028288));
#94782=DIRECTION('center_axis',(0.,-1.,0.));
#94783=DIRECTION('ref_axis',(0.,0.,-1.));
#94784=DIRECTION('',(-0.190809912898503,0.,0.981627005099017));
#94785=DIRECTION('center_axis',(0.,-1.,0.));
#94786=DIRECTION('ref_axis',(-0.593188827435541,0.,0.805063360864005));
#94787=DIRECTION('',(-0.190809912898503,0.,0.981627005099017));
#94788=DIRECTION('center_axis',(0.,-1.,0.));
#94789=DIRECTION('ref_axis',(-0.585155835598189,0.,0.810920864243476));
#94790=DIRECTION('center_axis',(0.981627005099017,0.,0.190809912898503));
#94791=DIRECTION('ref_axis',(0.,-1.,0.));
#94792=DIRECTION('',(-0.190809912898503,0.,0.981627005099017));
#94793=DIRECTION('center_axis',(0.981627005099017,-9.80258151505892E-17,
0.190809912898504));
#94794=DIRECTION('ref_axis',(-0.181744948393978,-0.304563067520509,0.934992038274));
#94795=DIRECTION('center_axis',(0.981627005099017,-7.66035235523749E-17,
0.190809912898504));
#94796=DIRECTION('ref_axis',(-0.182161442088192,-0.297650398172597,0.937134701888712));
#94797=DIRECTION('center_axis',(0.,1.,0.));
#94798=DIRECTION('ref_axis',(1.,0.,0.));
#94799=DIRECTION('',(-0.190809912898503,0.,0.981627005099017));
#94800=DIRECTION('center_axis',(0.,1.,0.));
#94801=DIRECTION('ref_axis',(-0.619117740094101,0.,0.785298175154363));
#94802=DIRECTION('center_axis',(0.,1.,0.));
#94803=DIRECTION('ref_axis',(-0.610780642463143,0.,0.791799852735722));
#94804=DIRECTION('center_axis',(-0.981627005099017,0.,-0.190809912898503));
#94805=DIRECTION('ref_axis',(-0.190809912898503,0.,0.981627005099017));
#94806=DIRECTION('center_axis',(-0.981627005099017,1.28998948977747E-16,
-0.190809912898504));
#94807=DIRECTION('ref_axis',(-0.179045219445688,-0.345704632538082,0.921103206180152));
#94808=DIRECTION('center_axis',(-0.981627005099017,4.48151719450879E-16,
-0.190809912898504));
#94809=DIRECTION('ref_axis',(-0.179607339081024,-0.337600885144495,0.923995046576489));
#94810=DIRECTION('center_axis',(0.,-1.,0.));
#94811=DIRECTION('ref_axis',(0.,0.,-1.));
#94812=DIRECTION('',(-0.190809912898503,0.,0.981627005099017));
#94813=DIRECTION('center_axis',(0.,-1.,0.));
#94814=DIRECTION('ref_axis',(-0.585794842268511,0.,0.810459377619638));
#94815=DIRECTION('',(-0.190809912898503,0.,0.981627005099017));
#94816=DIRECTION('center_axis',(0.,-1.,0.));
#94817=DIRECTION('ref_axis',(-0.578192279907259,0.,0.815900537722366));
#94818=DIRECTION('center_axis',(0.981627005099017,0.,0.190809912898503));
#94819=DIRECTION('ref_axis',(0.,-1.,0.));
#94820=DIRECTION('',(-0.190809912898503,0.,0.981627005099017));
#94821=DIRECTION('center_axis',(0.981627005099017,9.80258151505892E-17,
0.190809912898503));
#94822=DIRECTION('ref_axis',(-0.185524568408441,-0.23373444716689,0.954436400565512));
#94823=DIRECTION('center_axis',(0.981627005099017,6.80920209354444E-17,
0.190809912898503));
#94824=DIRECTION('ref_axis',(-0.185764991591961,-0.228429375341796,0.955673264447528));
#94825=DIRECTION('center_axis',(0.,1.,0.));
#94826=DIRECTION('ref_axis',(1.,0.,0.));
#94827=DIRECTION('',(-0.190809912898493,0.,0.981627005099019));
#94828=DIRECTION('center_axis',(0.,1.,0.));
#94829=DIRECTION('ref_axis',(-0.612315243995724,0.,0.790613712232755));
#94830=DIRECTION('center_axis',(0.,1.,0.));
#94831=DIRECTION('ref_axis',(-0.604365249086077,0.,0.796707377709736));
#94832=DIRECTION('center_axis',(-0.981627005099017,0.,-0.190809912898503));
#94833=DIRECTION('ref_axis',(-0.190809912898503,0.,0.981627005099017));
#94834=DIRECTION('center_axis',(-0.981627005099017,6.44994744888736E-17,
-0.190809912898503));
#94835=DIRECTION('ref_axis',(-0.183524789821252,-0.273682834092602,0.944148482943285));
#94836=DIRECTION('center_axis',(-0.981627005099017,-5.27237317001035E-17,
-0.190809912898503));
#94837=DIRECTION('ref_axis',(-0.183868708640475,-0.267267367406098,0.945917783056592));
#94838=DIRECTION('center_axis',(0.,-1.,0.));
#94839=DIRECTION('ref_axis',(0.,0.,-1.));
#94840=DIRECTION('',(-0.190809912898503,0.,0.981627005099017));
#94841=DIRECTION('center_axis',(0.,-1.,0.));
#94842=DIRECTION('ref_axis',(-0.580391375879782,0.,0.814337676154293));
#94843=DIRECTION('',(-0.190809912898503,0.,0.981627005099017));
#94844=DIRECTION('center_axis',(0.,-1.,0.));
#94845=DIRECTION('ref_axis',(-0.573093697528526,0.,0.819489849755982));
#94846=DIRECTION('center_axis',(0.981627005099017,0.,0.190809912898503));
#94847=DIRECTION('ref_axis',(0.,-1.,0.));
#94848=DIRECTION('',(-0.190809912898503,0.,0.981627005099017));
#94849=DIRECTION('center_axis',(0.981627005099017,-3.56457509638507E-17,
0.190809912898503));
#94850=DIRECTION('ref_axis',(-0.188261002084221,-0.162905826813305,0.968514061170264));
#94851=DIRECTION('center_axis',(0.981627005099017,-6.38362696269791E-17,
0.190809912898504));
#94852=DIRECTION('ref_axis',(-0.188376133470869,-0.159208352510898,0.969106357852084));
#94853=DIRECTION('center_axis',(0.,1.,0.));
#94854=DIRECTION('ref_axis',(1.,0.,0.));
#94855=DIRECTION('',(-0.190809912898503,0.,0.981627005099017));
#94856=DIRECTION('center_axis',(0.,1.,0.));
#94857=DIRECTION('ref_axis',(-0.607507081583685,0.,0.794314261376235));
#94858=DIRECTION('center_axis',(0.,1.,0.));
#94859=DIRECTION('ref_axis',(-0.599823547083943,0.,0.800132309286181));
#94860=DIRECTION('center_axis',(-0.981627005099017,0.,-0.190809912898503));
#94861=DIRECTION('ref_axis',(-0.190809912898503,0.,0.981627005099017));
#94862=DIRECTION('center_axis',(-0.981627005099017,-4.14639478857045E-17,
-0.190809912898503));
#94863=DIRECTION('ref_axis',(-0.186889794312999,-0.201661035647202,0.96145984392659));
#94864=DIRECTION('center_axis',(-0.981627005099017,1.66958483716994E-16,
-0.190809912898504));
#94865=DIRECTION('ref_axis',(-0.187073240040802,-0.196933849667601,0.962403585672734));
#94866=DIRECTION('center_axis',(0.,-1.,0.));
#94867=DIRECTION('ref_axis',(0.,0.,-1.));
#94868=DIRECTION('',(-0.190809912898503,0.,0.981627005099017));
#94869=DIRECTION('center_axis',(0.,-1.,0.));
#94870=DIRECTION('ref_axis',(-0.576755053793433,0.,0.816917136510022));
#94871=DIRECTION('',(-0.190809912898503,0.,0.981627005099017));
#94872=DIRECTION('center_axis',(0.,-1.,0.));
#94873=DIRECTION('ref_axis',(-0.56965800443632,0.,0.821881839428047));
#94874=DIRECTION('center_axis',(0.981627005099017,0.,0.190809912898503));
#94875=DIRECTION('ref_axis',(0.,-1.,0.));
#94876=DIRECTION('',(-0.190809912898503,0.,0.981627005099017));
#94877=DIRECTION('center_axis',(0.981627005099017,2.45064537876473E-17,
0.190809912898503));
#94878=DIRECTION('ref_axis',(-0.18999932772139,-0.0920772064596915,0.977456926680659));
#94879=DIRECTION('center_axis',(0.981627005099017,-7.66035235523749E-17,
0.190809912898504));
#94880=DIRECTION('ref_axis',(-0.190035779958582,-0.0899873296801039,0.977644456248067));
#94881=DIRECTION('center_axis',(0.,1.,0.));
#94882=DIRECTION('ref_axis',(1.,0.,0.));
#94883=DIRECTION('',(-0.190809912898503,0.,0.981627005099017));
#94884=DIRECTION('center_axis',(0.,1.,0.));
#94885=DIRECTION('ref_axis',(-0.604502425562639,0.,0.796603299948529));
#94886=DIRECTION('center_axis',(0.,1.,0.));
#94887=DIRECTION('ref_axis',(-0.596982423120826,0.,0.802254315341954));
#94888=DIRECTION('center_axis',(-0.981627005099017,0.,-0.190809912898503));
#94889=DIRECTION('ref_axis',(-0.190809912898503,0.,0.981627005099017));
#94890=DIRECTION('center_axis',(-0.981627005099017,9.21421064126766E-17,
-0.190809912898504));
#94891=DIRECTION('ref_axis',(-0.18919971148133,-0.129639237201797,0.97334327826986));
#94892=DIRECTION('center_axis',(-0.981627005099017,4.83300873917615E-17,
-0.190809912898504));
#94893=DIRECTION('ref_axis',(-0.189274619583568,-0.126600331929198,0.973728645124971));
#94894=DIRECTION('center_axis',(0.,-1.,0.));
#94895=DIRECTION('ref_axis',(0.,0.,-1.));
#94896=DIRECTION('',(-0.190809912898503,0.,0.981627005099017));
#94897=DIRECTION('center_axis',(0.,-1.,0.));
#94898=DIRECTION('ref_axis',(-0.574744679387081,0.,0.818332788977835));
#94899=DIRECTION('',(-0.190809912898503,0.,0.981627005099017));
#94900=DIRECTION('center_axis',(0.,-1.,0.));
#94901=DIRECTION('ref_axis',(-0.567756991666042,0.,0.823196208940691));
#94902=DIRECTION('center_axis',(0.981627005099017,0.,0.190809912898503));
#94903=DIRECTION('ref_axis',(0.,-1.,0.));
#94904=DIRECTION('',(-0.190809912898503,0.,0.981627005099017));
#94905=DIRECTION('center_axis',(0.981627005099017,-3.89875401167116E-18,
0.190809912898503));
#94906=DIRECTION('ref_axis',(-0.190766832467318,-0.0212485861060798,0.981405376599741));
#94907=DIRECTION('center_axis',(0.981627005099017,4.25575130846528E-18,
0.190809912898503));
#94908=DIRECTION('ref_axis',(-0.190768766076259,-0.0207663068492494,0.981415324105745));
#94909=DIRECTION('center_axis',(0.,1.,0.));
#94910=DIRECTION('ref_axis',(1.,0.,0.));
#94911=DIRECTION('',(-0.190809912898503,0.,0.981627005099017));
#94912=DIRECTION('center_axis',(0.,1.,0.));
#94913=DIRECTION('ref_axis',(-0.60318791972257,0.,0.797599105754739));
#94914=DIRECTION('center_axis',(0.,1.,0.));
#94915=DIRECTION('ref_axis',(-0.595738743977029,0.,0.803178279664404));
#94916=DIRECTION('center_axis',(-0.981627005099017,0.,-0.190809912898503));
#94917=DIRECTION('ref_axis',(-0.190809912898503,0.,0.981627005099017));
#94918=DIRECTION('center_axis',(-0.981627005099017,-2.30355266031692E-18,
-0.190809912898503));
#94919=DIRECTION('ref_axis',(-0.190492927159314,-0.0576174387563383,0.979996262979322));
#94920=DIRECTION('center_axis',(-0.981627005099017,1.75745772333678E-17,
-0.190809912898504));
#94921=DIRECTION('ref_axis',(-0.190507625712308,-0.0562668141907479,0.980071880101803));
#94922=DIRECTION('center_axis',(0.,-1.,0.));
#94923=DIRECTION('ref_axis',(0.,0.,-1.));
#94924=DIRECTION('',(-0.190809912898503,0.,0.981627005099017));
#94925=DIRECTION('center_axis',(0.,-1.,0.));
#94926=DIRECTION('ref_axis',(0.324163687217122,0.,0.946001006283714));
#94927=DIRECTION('',(-0.190809912898493,0.,0.981627005099019));
#94928=DIRECTION('center_axis',(0.,-1.,0.));
#94929=DIRECTION('ref_axis',(0.313789016047043,0.,0.949492734784331));
#94930=DIRECTION('center_axis',(0.981627005099017,0.,0.190809912898503));
#94931=DIRECTION('ref_axis',(0.,-1.,0.));
#94932=DIRECTION('',(-0.190809912898503,0.,0.981627005099017));
#94933=DIRECTION('center_axis',(0.981627005099017,-1.7295648605066E-17,
0.190809912898504));
#94934=DIRECTION('ref_axis',(-0.190762133968866,-0.0223771900686593,0.98138120504128));
#94935=DIRECTION('center_axis',(0.981627005099017,-2.11358402187499E-17,
0.190809912898504));
#94936=DIRECTION('ref_axis',(-0.19076450076384,-0.021815976042031,0.981393381085106));
#94937=DIRECTION('center_axis',(0.,1.,0.));
#94938=DIRECTION('ref_axis',(1.,0.,0.));
#94939=DIRECTION('',(-0.190809912898503,0.,0.981627005099017));
#94940=DIRECTION('center_axis',(0.,1.,0.));
#94941=DIRECTION('ref_axis',(0.288388637747114,0.,0.95751344304838));
#94942=DIRECTION('center_axis',(0.,1.,0.));
#94943=DIRECTION('ref_axis',(0.278801885864545,0.,0.960348639004801));
#94944=DIRECTION('center_axis',(-0.981627005099017,0.,-0.190809912898503));
#94945=DIRECTION('ref_axis',(-0.190809912898503,0.,0.981627005099017));
#94946=DIRECTION('center_axis',(-0.981627005099017,2.13522126074254E-17,
-0.190809912898504));
#94947=DIRECTION('ref_axis',(-0.190483435767225,-0.0584729580020077,0.979947434243699));
#94948=DIRECTION('center_axis',(-0.981627005099017,-1.80753010452426E-17,
-0.190809912898503));
#94949=DIRECTION('ref_axis',(-0.190499006107751,-0.0570627440812116,0.980027536301854));
#94950=DIRECTION('center_axis',(0.,-1.,0.));
#94951=DIRECTION('ref_axis',(0.,0.,-1.));
#94952=DIRECTION('',(-0.190809912898503,0.,0.981627005099017));
#94953=DIRECTION('center_axis',(0.,-1.,0.));
#94954=DIRECTION('ref_axis',(0.327157586265152,0.,0.94496979515176));
#94955=DIRECTION('',(-0.190809912898514,0.,0.981627005099015));
#94956=DIRECTION('center_axis',(0.,-1.,0.));
#94957=DIRECTION('ref_axis',(0.31660664489919,0.,0.948556921015116));
#94958=DIRECTION('center_axis',(0.981627005099017,0.,0.190809912898503));
#94959=DIRECTION('ref_axis',(0.,-1.,0.));
#94960=DIRECTION('',(-0.190809912898503,0.,0.981627005099017));
#94961=DIRECTION('center_axis',(0.981627005099017,-6.17701735895213E-17,
0.190809912898504));
#94962=DIRECTION('ref_axis',(-0.189910724397473,-0.0969678236308587,0.977001104369448));
#94963=DIRECTION('center_axis',(0.981627005099017,2.58326936006944E-17,
0.190809912898503));
#94964=DIRECTION('ref_axis',(-0.189955361826545,-0.0945358961821438,0.977230742888488));
#94965=DIRECTION('center_axis',(0.,1.,0.));
#94966=DIRECTION('ref_axis',(1.,0.,0.));
#94967=DIRECTION('',(-0.190809912898503,0.,0.981627005099017));
#94968=DIRECTION('center_axis',(0.,1.,0.));
#94969=DIRECTION('ref_axis',(0.290085054729223,0.,0.957000867827581));
#94970=DIRECTION('center_axis',(0.,1.,0.));
#94971=DIRECTION('ref_axis',(0.280399314101408,0.,0.959883443263535));
#94972=DIRECTION('center_axis',(-0.981627005099017,0.,-0.190809912898503));
#94973=DIRECTION('ref_axis',(-0.190809912898503,0.,0.981627005099017));
#94974=DIRECTION('center_axis',(-0.981627005099017,-9.48987226996683E-18,
-0.190809912898503));
#94975=DIRECTION('ref_axis',(-0.189151327895628,-0.131564155504506,0.973094367541867));
#94976=DIRECTION('center_axis',(-0.981627005099017,9.94141557488341E-17,
-0.190809912898504));
#94977=DIRECTION('ref_axis',(-0.189230694466041,-0.128391174182701,0.973502671112867));
#94978=DIRECTION('center_axis',(0.,-1.,0.));
#94979=DIRECTION('ref_axis',(0.,0.,-1.));
#94980=DIRECTION('',(-0.190809912898503,0.,0.981627005099017));
#94981=DIRECTION('center_axis',(0.,-1.,0.));
#94982=DIRECTION('ref_axis',(0.332583332787186,0.,0.943073871312406));
#94983=DIRECTION('',(-0.190809912898503,0.,0.981627005099017));
#94984=DIRECTION('center_axis',(0.,-1.,0.));
#94985=DIRECTION('ref_axis',(0.321708056003748,0.,0.946838912752475));
#94986=DIRECTION('center_axis',(0.981627005099017,0.,0.190809912898503));
#94987=DIRECTION('ref_axis',(0.,-1.,0.));
#94988=DIRECTION('',(-0.190809912898503,0.,0.981627005099017));
#94989=DIRECTION('center_axis',(0.981627005099017,-4.44745249844553E-17,
0.190809912898503));
#94990=DIRECTION('ref_axis',(-0.187980954040593,-0.171558457193103,0.967073346072319));
#94991=DIRECTION('center_axis',(0.981627005099017,-7.98465074930554E-17,
0.190809912898504));
#94992=DIRECTION('ref_axis',(-0.18812207510112,-0.167255816322301,0.967799347368043));
#94993=DIRECTION('center_axis',(0.,1.,0.));
#94994=DIRECTION('ref_axis',(1.,0.,0.));
#94995=DIRECTION('',(-0.190809912898503,0.,0.981627005099017));
#94996=DIRECTION('center_axis',(0.,1.,0.));
#94997=DIRECTION('ref_axis',(0.293968036548532,0.,0.955815250708944));
#94998=DIRECTION('center_axis',(0.,1.,0.));
#94999=DIRECTION('ref_axis',(0.284053252507605,0.,0.958808505250058));
#95000=DIRECTION('center_axis',(-0.981627005099017,0.,-0.190809912898503));
#95001=DIRECTION('ref_axis',(-0.190809912898503,0.,0.981627005099017));
#95002=DIRECTION('center_axis',(-0.981627005099017,-9.01537865646849E-17,
-0.190809912898503));
#95003=DIRECTION('ref_axis',(-0.186771248501737,-0.204655353007008,0.960849981640568));
#95004=DIRECTION('center_axis',(-0.981627005099017,9.03765052262128E-18,
-0.190809912898503));
#95005=DIRECTION('ref_axis',(-0.186965682920001,-0.1997196042842,0.961850255016247));
#95006=DIRECTION('center_axis',(0.,-1.,0.));
#95007=DIRECTION('ref_axis',(0.,0.,-1.));
#95008=DIRECTION('',(-0.190809912898503,0.,0.981627005099017));
#95009=DIRECTION('center_axis',(0.,-1.,0.));
#95010=DIRECTION('ref_axis',(0.340670977220966,0.,0.94018258082104));
#95011=DIRECTION('',(-0.190809912898503,0.,0.981627005099017));
#95012=DIRECTION('center_axis',(0.,-1.,0.));
#95013=DIRECTION('ref_axis',(0.329300453690895,0.,0.944225190936448));
#95014=DIRECTION('center_axis',(0.981627005099017,0.,0.190809912898503));
#95015=DIRECTION('ref_axis',(0.,-1.,0.));
#95016=DIRECTION('',(-0.190809912898503,0.,0.981627005099017));
#95017=DIRECTION('center_axis',(0.981627005099017,3.95329110972936E-17,
0.190809912898503));
#95018=DIRECTION('ref_axis',(-0.184939069098101,-0.246149090755304,0.951424282768453));
#95019=DIRECTION('center_axis',(0.981627005099017,5.63622405833332E-17,
0.190809912898503));
#95020=DIRECTION('ref_axis',(-0.185234234721259,-0.239975736462394,0.952942770682773));
#95021=DIRECTION('center_axis',(0.,1.,0.));
#95022=DIRECTION('ref_axis',(1.,0.,0.));
#95023=DIRECTION('',(-0.190809912898503,0.,0.981627005099017));
#95024=DIRECTION('center_axis',(0.,1.,0.));
#95025=DIRECTION('ref_axis',(0.300197402785575,0.,0.953877098666697));
#95026=DIRECTION('center_axis',(0.,1.,0.));
#95027=DIRECTION('ref_axis',(0.289907957000668,0.,0.957054531606062));
#95028=DIRECTION('center_axis',(-0.981627005099017,0.,-0.190809912898503));
#95029=DIRECTION('ref_axis',(-0.190809912898503,0.,0.981627005099017));
#95030=DIRECTION('center_axis',(-0.981627005099017,1.04388594969635E-16,
-0.190809912898504));
#95031=DIRECTION('ref_axis',(-0.183302380149146,-0.277746550509493,0.943004290081299));
#95032=DIRECTION('center_axis',(-0.981627005099017,9.94141557488341E-17,
-0.190809912898504));
#95033=DIRECTION('ref_axis',(-0.183667100790987,-0.271048034385807,0.944880605760656));
#95034=DIRECTION('center_axis',(-0.981627005099017,0.,-0.190809912898503));
#95035=DIRECTION('ref_axis',(-0.190809912898503,0.,0.981627005099017));
#95036=DIRECTION('',(-0.190809912898503,0.,0.981627005099017));
#95037=DIRECTION('center_axis',(-0.981627005099017,2.84696168099005E-17,
-0.190809912898503));
#95038=DIRECTION('ref_axis',(-0.178681321768697,-0.350837748012096,0.919231124266793));
#95039=DIRECTION('',(-0.190809912898503,0.,0.981627005099017));
#95040=DIRECTION('center_axis',(-0.981627005099017,-1.08451806271455E-16,
-0.190809912898503));
#95041=DIRECTION('ref_axis',(-0.179277906329184,-0.342376464487307,0.922300270447427));
#95042=DIRECTION('center_axis',(0.,-1.,0.));
#95043=DIRECTION('ref_axis',(0.,0.,-1.));
#95044=DIRECTION('',(-0.190809912898483,0.,0.981627005099021));
#95045=DIRECTION('',(0.981627005099017,0.,0.190809912898503));
#95046=DIRECTION('center_axis',(0.,-1.,0.));
#95047=DIRECTION('ref_axis',(0.321307357956275,0.,0.946974963620031));
#95048=DIRECTION('center_axis',(0.,-1.,0.));
#95049=DIRECTION('ref_axis',(0.339712961600918,0.,0.940529161547016));
#95050=DIRECTION('center_axis',(0.981627005099017,0.,0.190809912898503));
#95051=DIRECTION('ref_axis',(0.,-1.,0.));
#95052=DIRECTION('',(-0.190809912898503,0.,0.981627005099017));
#95053=DIRECTION('',(0.,1.,0.));
#95054=DIRECTION('center_axis',(0.981627005099017,-1.40905601458333E-16,
0.190809912898504));
#95055=DIRECTION('ref_axis',(-0.181241438981021,-0.3126956566025,0.932401719827897));
#95056=DIRECTION('center_axis',(0.,1.,0.));
#95057=DIRECTION('ref_axis',(1.,0.,0.));
#95058=DIRECTION('center_axis',(0.,1.,0.));
#95059=DIRECTION('ref_axis',(0.30904404227791,0.,0.951047727473511));
#95060=DIRECTION('',(-0.981627005099017,0.,-0.190809912898503));
#95061=DIRECTION('center_axis',(0.,1.,0.));
#95062=DIRECTION('ref_axis',(0.298207091960414,0.,0.954501194501355));
#95063=DIRECTION('center_axis',(-0.190809912898503,0.,0.981627005099017));
#95064=DIRECTION('ref_axis',(0.,1.,0.));
#95065=DIRECTION('center_axis',(0.190809912898504,-3.49693752527234E-16,
-0.981627005099017));
#95066=DIRECTION('ref_axis',(0.85426207248107,-0.492608222327907,0.166052554377481));
#95067=DIRECTION('center_axis',(0.,1.,0.));
#95068=DIRECTION('ref_axis',(1.,0.,0.));
#95069=DIRECTION('',(-0.190809912898503,0.,0.981627005099017));
#95070=DIRECTION('center_axis',(0.,1.,0.));
#95071=DIRECTION('ref_axis',(0.246498687235726,0.,0.969143125235413));
#95072=DIRECTION('',(-0.190809912898503,0.,0.981627005099017));
#95073=DIRECTION('center_axis',(0.,1.,0.));
#95074=DIRECTION('ref_axis',(0.236678365804582,0.,0.971588056307853));
#95075=DIRECTION('center_axis',(-0.981627005099017,0.,-0.190809912898503));
#95076=DIRECTION('ref_axis',(-0.190809912898503,0.,0.981627005099017));
#95077=DIRECTION('',(-0.190809912898503,0.,0.981627005099017));
#95078=DIRECTION('center_axis',(-0.981627005099017,1.77118070983607E-16,
-0.190809912898504));
#95079=DIRECTION('ref_axis',(-0.174075761005115,-0.409523969629305,0.895537686381509));
#95080=DIRECTION('center_axis',(-0.981627005099017,-1.69216540445236E-17,
-0.190809912898503));
#95081=DIRECTION('ref_axis',(-0.174856431613847,-0.40028498107098,0.899553868454957));
#95082=DIRECTION('center_axis',(0.,-1.,0.));
#95083=DIRECTION('ref_axis',(0.,0.,-1.));
#95084=DIRECTION('',(-0.190809912898503,0.,0.981627005099017));
#95085=DIRECTION('',(0.981627005099017,0.,0.190809912898503));
#95086=DIRECTION('center_axis',(0.,-1.,0.));
#95087=DIRECTION('ref_axis',(0.27693655485013,0.,0.960888206082134));
#95088=DIRECTION('center_axis',(0.,-1.,0.));
#95089=DIRECTION('ref_axis',(0.279101841281133,0.,0.960261507191391));
#95090=DIRECTION('center_axis',(0.981627005099017,0.,0.190809912898503));
#95091=DIRECTION('ref_axis',(0.,-1.,0.));
#95092=DIRECTION('center_axis',(0.981627005099017,-1.0065149107169E-16,
0.190809912898504));
#95093=DIRECTION('ref_axis',(-0.176466315004732,-0.38038600246631,0.907835959188856));
#95094=DIRECTION('',(0.,1.,0.));
#95095=DIRECTION('center_axis',(0.981627005099017,0.,0.190809912898503));
#95096=DIRECTION('ref_axis',(-0.177151986277243,-0.371529138153602,0.911363414484513));
#95097=DIRECTION('center_axis',(-0.190809912898503,0.,0.981627005099017));
#95098=DIRECTION('ref_axis',(0.,1.,0.));
#95099=DIRECTION('center_axis',(0.190809912898503,4.4294541986783E-16,-0.981627005099017));
#95100=DIRECTION('ref_axis',(0.753450111070955,-0.640986267800124,0.146456596365046));
#95101=DIRECTION('center_axis',(0.,-1.,0.));
#95102=DIRECTION('ref_axis',(0.,0.,-1.));
#95103=DIRECTION('',(-0.190809912898503,0.,0.981627005099017));
#95104=DIRECTION('center_axis',(0.,-1.,0.));
#95105=DIRECTION('ref_axis',(0.215356558023971,0.,0.976535484719356));
#95106=DIRECTION('',(-0.190809912898503,0.,0.981627005099017));
#95107=DIRECTION('center_axis',(0.,-1.,0.));
#95108=DIRECTION('ref_axis',(0.206031581908636,0.,0.9785453424631));
#95109=DIRECTION('center_axis',(0.981627005099017,0.,0.190809912898503));
#95110=DIRECTION('ref_axis',(0.,-1.,0.));
#95111=DIRECTION('',(-0.190809912898503,0.,0.981627005099017));
#95112=DIRECTION('center_axis',(0.981627005099017,-8.60077605075239E-17,
0.190809912898503));
#95113=DIRECTION('ref_axis',(-0.177360216447652,-0.368790379407218,0.912434660498121));
#95114=DIRECTION('center_axis',(0.981627005099017,-9.05042095782515E-17,
0.190809912898503));
#95115=DIRECTION('ref_axis',(-0.177964786864002,-0.360702216203213,0.915544890140588));
#95116=DIRECTION('center_axis',(0.,1.,0.));
#95117=DIRECTION('ref_axis',(1.,0.,0.));
#95118=DIRECTION('',(-0.190809912898503,0.,0.981627005099017));
#95119=DIRECTION('center_axis',(0.,1.,0.));
#95120=DIRECTION('ref_axis',(0.173299588604038,0.,0.984869155060545));
#95121=DIRECTION('center_axis',(0.,1.,0.));
#95122=DIRECTION('ref_axis',(0.165191125635383,0.,0.986261573828827));
#95123=DIRECTION('center_axis',(-0.981627005099017,0.,-0.190809912898503));
#95124=DIRECTION('ref_axis',(-0.190809912898503,0.,0.981627005099017));
#95125=DIRECTION('center_axis',(-0.981627005099017,4.10603095522234E-16,
-0.190809912898504));
#95126=DIRECTION('ref_axis',(-0.175016396158809,-0.398360213910187,0.90037681059044));
#95127=DIRECTION('center_axis',(-0.981627005099017,4.01253885915747E-17,
-0.190809912898503));
#95128=DIRECTION('ref_axis',(-0.17571344921673,-0.38984099858382,0.90396281980374));
#95129=DIRECTION('center_axis',(0.,-1.,0.));
#95130=DIRECTION('ref_axis',(0.,0.,-1.));
#95131=DIRECTION('',(-0.190809912898503,0.,0.981627005099017));
#95132=DIRECTION('center_axis',(0.,-1.,0.));
#95133=DIRECTION('ref_axis',(0.141672460290673,0.,0.989913589155734));
#95134=DIRECTION('',(-0.190809912898503,0.,0.981627005099017));
#95135=DIRECTION('center_axis',(0.,-1.,0.));
#95136=DIRECTION('ref_axis',(0.134100681649831,0.,0.990967712481618));
#95137=DIRECTION('center_axis',(0.981627005099017,0.,0.190809912898503));
#95138=DIRECTION('ref_axis',(0.,-1.,0.));
#95139=DIRECTION('',(-0.190809912898503,0.,0.981627005099017));
#95140=DIRECTION('center_axis',(0.981627005099017,-1.14638278569454E-16,
0.190809912898504));
#95141=DIRECTION('ref_axis',(-0.178028194999365,-0.359841769342607,0.915871095090161));
#95142=DIRECTION('center_axis',(0.981627005099017,-3.53229335734846E-16,
0.190809912898504));
#95143=DIRECTION('ref_axis',(-0.178575361030583,-0.352316423630891,0.918686006246277));
#95144=DIRECTION('center_axis',(0.,1.,0.));
#95145=DIRECTION('ref_axis',(1.,0.,0.));
#95146=DIRECTION('',(-0.190809912898503,0.,0.981627005099017));
#95147=DIRECTION('center_axis',(0.,1.,0.));
#95148=DIRECTION('ref_axis',(0.101214401296622,0.,0.994864636505975));
#95149=DIRECTION('center_axis',(0.,1.,0.));
#95150=DIRECTION('ref_axis',(0.0947603432797819,0.,0.995500114184573));
#95151=DIRECTION('center_axis',(-0.981627005099017,0.,-0.190809912898503));
#95152=DIRECTION('ref_axis',(-0.190809912898503,0.,0.981627005099017));
#95153=DIRECTION('center_axis',(-0.981627005099017,2.56763337521845E-16,
-0.190809912898504));
#95154=DIRECTION('ref_axis',(-0.175715849516705,-0.389811281877913,0.903975168214991));
#95155=DIRECTION('center_axis',(-0.981627005099017,3.77210004092943E-16,
-0.190809912898504));
#95156=DIRECTION('ref_axis',(-0.176353679441912,-0.381818043972282,0.907256502343455));
#95157=DIRECTION('center_axis',(0.,-1.,0.));
#95158=DIRECTION('ref_axis',(0.,0.,-1.));
#95159=DIRECTION('',(-0.190809912898503,-1.328769267093E-14,0.981627005099017));
#95160=DIRECTION('center_axis',(0.,-1.,0.));
#95161=DIRECTION('ref_axis',(0.0690927304182998,0.,0.997610241829616));
#95162=DIRECTION('',(-0.190809912898503,0.,0.981627005099017));
#95163=DIRECTION('center_axis',(0.,-1.,0.));
#95164=DIRECTION('ref_axis',(0.063217557275382,0.,0.997999769765572));
#95165=DIRECTION('center_axis',(0.981627005099017,0.,0.190809912898503));
#95166=DIRECTION('ref_axis',(0.,-1.,0.));
#95167=DIRECTION('',(-0.190809912898503,0.,0.981627005099017));
#95168=DIRECTION('center_axis',(0.981627005099017,-3.15328006926456E-17,
0.190809912898503));
#95169=DIRECTION('ref_axis',(-0.178521093013203,-0.353070994296397,0.918406822892734));
#95170=DIRECTION('center_axis',(0.981627005099017,-3.33018562685204E-16,
0.190809912898504));
#95171=DIRECTION('ref_axis',(-0.179027665935153,-0.34595423082879,0.921012901647676));
#95172=DIRECTION('center_axis',(0.,1.,0.));
#95173=DIRECTION('ref_axis',(1.,0.,0.));
#95174=DIRECTION('',(-0.190809912898503,0.,0.981627005099017));
#95175=DIRECTION('center_axis',(0.,1.,0.));
#95176=DIRECTION('ref_axis',(0.0301623710479701,0.,0.999545012179424));
#95177=DIRECTION('center_axis',(0.,1.,0.));
#95178=DIRECTION('ref_axis',(0.0253129510981065,0.,0.999679575917556));
#95179=DIRECTION('center_axis',(-0.981627005099017,0.,-0.190809912898503));
#95180=DIRECTION('ref_axis',(-0.190809912898503,0.,0.981627005099017));
#95181=DIRECTION('center_axis',(-0.981627005099017,0.,-0.190809912898503));
#95182=DIRECTION('ref_axis',(-0.176224298070495,-0.383455269460088,0.906590896211104));
#95183=DIRECTION('center_axis',(-0.981627005099017,1.41720243526492E-16,
-0.190809912898504));
#95184=DIRECTION('ref_axis',(-0.176820667107078,-0.375839162626588,0.909658933622901));
#95185=DIRECTION('center_axis',(0.,-1.,0.));
#95186=DIRECTION('ref_axis',(0.,0.,-1.));
#95187=DIRECTION('',(-0.190809912898503,0.,0.981627005099017));
#95188=DIRECTION('center_axis',(0.,-1.,0.));
#95189=DIRECTION('ref_axis',(-0.00245485281101381,0.,0.999996986844299));
#95190=DIRECTION('',(-0.190809912898503,0.,0.981627005099017));
#95191=DIRECTION('center_axis',(0.,-1.,0.));
#95192=DIRECTION('ref_axis',(-0.00668313312353966,0.,0.999977667616459));
#95193=DIRECTION('center_axis',(0.981627005099017,0.,0.190809912898503));
#95194=DIRECTION('ref_axis',(0.,-1.,0.));
#95195=DIRECTION('',(-0.190809912898503,0.,0.981627005099017));
#95196=DIRECTION('center_axis',(0.981627005099017,0.,0.190809912898503));
#95197=DIRECTION('ref_axis',(-0.178871820110591,-0.348161333804301,0.920211148386029));
#95198=DIRECTION('center_axis',(0.981627005099017,-2.43133958356391E-16,
0.190809912898504));
#95199=DIRECTION('ref_axis',(-0.179350425520556,-0.341331684304794,0.922673347482872));
#95200=DIRECTION('center_axis',(0.,1.,0.));
#95201=DIRECTION('ref_axis',(1.,0.,0.));
#95202=DIRECTION('',(-0.190809912898503,0.,0.981627005099017));
#95203=DIRECTION('center_axis',(0.,1.,0.));
#95204=DIRECTION('ref_axis',(-0.0399134285534144,0.,0.999203141618916));
#95205=DIRECTION('center_axis',(0.,1.,0.));
#95206=DIRECTION('ref_axis',(-0.0432028268842918,0.,0.999066321997297));
#95207=DIRECTION('center_axis',(-0.981627005099017,0.,-0.190809912898503));
#95208=DIRECTION('ref_axis',(-0.190809912898503,0.,0.981627005099017));
#95209=DIRECTION('center_axis',(-0.981627005099017,4.55117302256744E-17,
-0.190809912898503));
#95210=DIRECTION('ref_axis',(-0.176574195062516,-0.379008487252018,0.908390951203809));
#95211=DIRECTION('center_axis',(-0.981627005099017,3.20917534544763E-16,
-0.190809912898504));
#95212=DIRECTION('ref_axis',(-0.177142812401908,-0.371649260184588,0.911316219222829));
#95213=DIRECTION('center_axis',(0.,-1.,0.));
#95214=DIRECTION('ref_axis',(0.,0.,-1.));
#95215=DIRECTION('',(-0.190809912898503,0.,0.981627005099017));
#95216=DIRECTION('center_axis',(0.,-1.,0.));
#95217=DIRECTION('ref_axis',(-0.0730201753284488,0.,0.997330463785702));
#95218=DIRECTION('',(-0.190809912898503,0.,0.981627005099017));
#95219=DIRECTION('center_axis',(0.,-1.,0.));
#95220=DIRECTION('ref_axis',(-0.0756467337952682,0.,0.997134680806012));
#95221=DIRECTION('center_axis',(0.981627005099017,0.,0.190809912898503));
#95222=DIRECTION('ref_axis',(0.,-1.,0.));
#95223=DIRECTION('',(-0.190809912898503,0.,0.981627005099017));
#95224=DIRECTION('center_axis',(0.981627005099017,-3.00905960538911E-17,
0.190809912898503));
#95225=DIRECTION('ref_axis',(-0.179101543646402,-0.344902357589395,0.921392967627143));
#95226=DIRECTION('center_axis',(0.981627005099017,-1.01299069034784E-16,
0.190809912898504));
#95227=DIRECTION('ref_axis',(-0.179562245131546,-0.338259087198216,0.92376305947529));
#95228=DIRECTION('center_axis',(0.,1.,0.));
#95229=DIRECTION('ref_axis',(1.,0.,0.));
#95230=DIRECTION('',(-0.190809912898503,0.,0.981627005099017));
#95231=DIRECTION('center_axis',(0.,1.,0.));
#95232=DIRECTION('ref_axis',(-0.109051309513976,0.,0.994036122026401));
#95233=DIRECTION('center_axis',(0.,1.,0.));
#95234=DIRECTION('ref_axis',(-0.110821964250551,0.,0.993840275013872));
#95235=DIRECTION('center_axis',(-0.981627005099017,0.,-0.190809912898503));
#95236=DIRECTION('ref_axis',(-0.190809912898503,0.,0.981627005099017));
#95237=DIRECTION('center_axis',(-0.981627005099017,3.06546241321686E-16,
-0.190809912898504));
#95238=DIRECTION('ref_axis',(-0.176786003350799,-0.376286776602481,0.909480604946233));
#95239=DIRECTION('center_axis',(-0.981627005099017,-2.15794885179139E-17,
-0.190809912898503));
#95240=DIRECTION('ref_axis',(-0.177338131232431,-0.369081972811902,0.91232104248245));
#95241=DIRECTION('center_axis',(0.,-1.,0.));
#95242=DIRECTION('ref_axis',(0.,0.,-1.));
#95243=DIRECTION('',(-0.190809912898503,0.,0.981627005099017));
#95244=DIRECTION('center_axis',(0.,-1.,0.));
#95245=DIRECTION('ref_axis',(-0.142635241858787,0.,0.989775321868496));
#95246=DIRECTION('',(-0.190809912898503,0.,0.981627005099017));
#95247=DIRECTION('center_axis',(0.,-1.,0.));
#95248=DIRECTION('ref_axis',(-0.143702428046443,0.,0.98962094368175));
#95249=DIRECTION('center_axis',(0.981627005099017,0.,0.190809912898503));
#95250=DIRECTION('ref_axis',(0.,-1.,0.));
#95251=DIRECTION('',(-0.190809912898503,0.,0.981627005099017));
#95252=DIRECTION('center_axis',(0.981627005099017,-9.68104844745577E-17,
0.190809912898503));
#95253=DIRECTION('ref_axis',(-0.179223155950715,-0.343162864172706,0.922018605573581));
#95254=DIRECTION('center_axis',(0.981627005099017,-1.71974336430998E-16,
0.190809912898504));
#95255=DIRECTION('ref_axis',(-0.179674512482127,-0.336617711962109,0.924340622042386));
#95256=DIRECTION('center_axis',(0.,1.,0.));
#95257=DIRECTION('ref_axis',(1.,0.,0.));
#95258=DIRECTION('',(-0.190809912898503,0.,0.981627005099017));
#95259=DIRECTION('center_axis',(0.,1.,0.));
#95260=DIRECTION('ref_axis',(-0.177274123368118,0.,0.984161513768988));
#95261=DIRECTION('center_axis',(0.,1.,0.));
#95262=DIRECTION('ref_axis',(-0.1775653711205,0.,0.984109007670817));
#95263=DIRECTION('center_axis',(-0.981627005099017,0.,-0.190809912898503));
#95264=DIRECTION('ref_axis',(-0.190809912898503,0.,0.981627005099017));
#95265=DIRECTION('center_axis',(-0.981627005099017,3.56781022098411E-16,
-0.190809912898504));
#95266=DIRECTION('ref_axis',(-0.176871394992535,-0.375182990983614,0.90991990466743));
#95267=DIRECTION('center_axis',(-0.981627005099017,1.71662726916883E-16,
-0.190809912898504));
#95268=DIRECTION('ref_axis',(-0.177416941265172,-0.368040210182297,0.912726482929624));
#95269=DIRECTION('center_axis',(0.,-1.,0.));
#95270=DIRECTION('ref_axis',(0.,0.,-1.));
#95271=DIRECTION('',(-0.190809912898503,0.,0.981627005099017));
#95272=DIRECTION('center_axis',(0.,-1.,0.));
#95273=DIRECTION('ref_axis',(-0.21131678201032,0.,0.97741762703606));
#95274=DIRECTION('',(-0.190809912898503,1.372221714061E-14,0.981627005099017));
#95275=DIRECTION('center_axis',(0.,-1.,0.));
#95276=DIRECTION('ref_axis',(-0.210865499794873,0.,0.977515084792178));
#95277=DIRECTION('center_axis',(0.981627005099017,0.,0.190809912898503));
#95278=DIRECTION('ref_axis',(0.,-1.,0.));
#95279=DIRECTION('',(-0.190809912898503,0.,0.981627005099017));
#95280=DIRECTION('center_axis',(0.981627005099017,-3.56855682945794E-16,
0.190809912898504));
#95281=DIRECTION('ref_axis',(-0.179243179230579,-0.342875499534802,0.922121615904364));
#95282=DIRECTION('center_axis',(0.981627005099017,-1.43081078683219E-16,
0.190809912898504));
#95283=DIRECTION('ref_axis',(-0.179693005975761,-0.336346465570606,0.924435762344554));
#95284=DIRECTION('center_axis',(0.,1.,0.));
#95285=DIRECTION('ref_axis',(1.,0.,0.));
#95286=DIRECTION('',(-0.190809912898503,0.,0.981627005099017));
#95287=DIRECTION('center_axis',(0.,1.,0.));
#95288=DIRECTION('ref_axis',(-0.244591010378231,0.,0.969626339185439));
#95289=DIRECTION('center_axis',(0.,1.,0.));
#95290=DIRECTION('ref_axis',(-0.243441421751623,0.,0.96991560157343));
#95291=DIRECTION('center_axis',(-0.981627005099017,0.,-0.190809912898503));
#95292=DIRECTION('ref_axis',(-0.190809912898503,0.,0.981627005099017));
#95293=DIRECTION('center_axis',(-0.981627005099017,2.98065849465872E-17,
-0.190809912898503));
#95294=DIRECTION('ref_axis',(-0.176834926434283,-0.375654851236703,0.909732291135866));
#95295=DIRECTION('center_axis',(-0.981627005099017,-5.01895501974238E-17,
-0.190809912898503));
#95296=DIRECTION('ref_axis',(-0.177383278884452,-0.368485598551699,0.912553305857908));
#95297=DIRECTION('center_axis',(0.,-1.,0.));
#95298=DIRECTION('ref_axis',(0.,0.,-1.));
#95299=DIRECTION('',(-0.190809912898503,0.,0.981627005099017));
#95300=DIRECTION('center_axis',(0.,-1.,0.));
#95301=DIRECTION('ref_axis',(-0.279067536185833,0.,0.960271477368337));
#95302=DIRECTION('',(-0.190809912898503,0.,0.981627005099017));
#95303=DIRECTION('center_axis',(0.,-1.,0.));
#95304=DIRECTION('ref_axis',(-0.277138454551981,0.,0.960829993811881));
#95305=DIRECTION('center_axis',(0.981627005099017,0.,0.190809912898503));
#95306=DIRECTION('ref_axis',(0.,-1.,0.));
#95307=DIRECTION('',(-0.190809912898503,0.,0.981627005099017));
#95308=DIRECTION('center_axis',(0.981627005099017,-1.94599946632004E-16,
0.190809912898504));
#95309=DIRECTION('ref_axis',(-0.179162667562163,-0.344029312691491,0.92170742134423));
#95310=DIRECTION('center_axis',(0.981627005099017,-1.94412209408584E-16,
0.190809912898504));
#95311=DIRECTION('ref_axis',(-0.179618660622996,-0.337435405585499,0.924053290570057));
#95312=DIRECTION('center_axis',(0.,1.,0.));
#95313=DIRECTION('ref_axis',(1.,0.,0.));
#95314=DIRECTION('',(-0.190809912898503,0.,0.981627005099017));
#95315=DIRECTION('center_axis',(0.,1.,0.));
#95316=DIRECTION('ref_axis',(-0.310998072064368,0.,0.950410542435345));
#95317=DIRECTION('center_axis',(0.,1.,0.));
#95318=DIRECTION('ref_axis',(-0.308446543639216,0.,0.951241677870046));
#95319=DIRECTION('center_axis',(-0.981627005099017,0.,-0.190809912898503));
#95320=DIRECTION('ref_axis',(-0.190809912898503,0.,0.981627005099017));
#95321=DIRECTION('center_axis',(-0.981627005099017,9.04057881831701E-17,
-0.190809912898503));
#95322=DIRECTION('ref_axis',(-0.176674662131589,-0.377720349383403,0.908907806888228));
#95323=DIRECTION('center_axis',(-0.981627005099017,5.79678245784152E-17,
-0.190809912898503));
#95324=DIRECTION('ref_axis',(-0.177235428855869,-0.370434472390808,0.911792687195297));
#95325=DIRECTION('center_axis',(0.,-1.,0.));
#95326=DIRECTION('ref_axis',(0.,0.,-1.));
#95327=DIRECTION('',(-0.190809912898503,0.,0.981627005099017));
#95328=DIRECTION('center_axis',(0.,-1.,0.));
#95329=DIRECTION('ref_axis',(-0.345876461290101,0.,0.938280061349189));
#95330=DIRECTION('',(-0.190809912898503,0.,0.981627005099017));
#95331=DIRECTION('center_axis',(0.,-1.,0.));
#95332=DIRECTION('ref_axis',(-0.342511199077206,0.,0.939513745778471));
#95333=DIRECTION('center_axis',(0.981627005099017,0.,0.190809912898503));
#95334=DIRECTION('ref_axis',(0.,-1.,0.));
#95335=DIRECTION('',(-0.190809912898503,-1.100134239348E-14,0.981627005099017));
#95336=DIRECTION('center_axis',(0.981627005099017,-1.51997840690772E-17,
0.190809912898503));
#95337=DIRECTION('ref_axis',(-0.178977348700373,-0.346668574534505,0.920754043207196));
#95338=DIRECTION('center_axis',(0.981627005099017,-6.57637322766467E-17,
0.190809912898503));
#95339=DIRECTION('ref_axis',(-0.179447688741777,-0.339924709427799,0.923173720881212));
#95340=DIRECTION('center_axis',(0.,1.,0.));
#95341=DIRECTION('ref_axis',(1.,0.,0.));
#95342=DIRECTION('',(-0.190809912898503,0.,0.981627005099017));
#95343=DIRECTION('center_axis',(0.,1.,0.));
#95344=DIRECTION('ref_axis',(-0.376478086240433,0.,0.926425523493789));
#95345=DIRECTION('center_axis',(0.,1.,0.));
#95346=DIRECTION('ref_axis',(-0.372564967779079,0.,0.928006112471127));
#95347=DIRECTION('center_axis',(-0.981627005099017,0.,-0.190809912898503));
#95348=DIRECTION('ref_axis',(-0.190809912898503,0.,0.981627005099017));
#95349=DIRECTION('center_axis',(-0.981627005099017,-1.07572079987249E-16,
-0.190809912898503));
#95350=DIRECTION('ref_axis',(-0.176381911743642,-0.381459690919397,0.907401744219911));
#95351=DIRECTION('center_axis',(-0.981627005099017,1.25537203023879E-16,
-0.190809912898504));
#95352=DIRECTION('ref_axis',(-0.176965700962373,-0.373959569196591,0.910405064402212));
#95353=DIRECTION('center_axis',(0.,-1.,0.));
#95354=DIRECTION('ref_axis',(0.,0.,-1.));
#95355=DIRECTION('',(-0.190809912898503,0.,0.981627005099017));
#95356=DIRECTION('center_axis',(0.,-1.,0.));
#95357=DIRECTION('ref_axis',(-0.4117178933269,0.,0.911311349822035));
#95358=DIRECTION('',(-0.190809912898503,0.,0.981627005099017));
#95359=DIRECTION('center_axis',(0.,-1.,0.));
#95360=DIRECTION('ref_axis',(-0.406960310608449,0.,0.913445841629089));
#95361=DIRECTION('center_axis',(0.981627005099017,0.,0.190809912898503));
#95362=DIRECTION('ref_axis',(0.,-1.,0.));
#95363=DIRECTION('',(-0.190809912898503,0.,0.981627005099017));
#95364=DIRECTION('center_axis',(0.981627005099017,-2.18020488347966E-16,
0.190809912898504));
#95365=DIRECTION('ref_axis',(-0.178677042467767,-0.350897603166811,0.919209109281865));
#95366=DIRECTION('center_axis',(0.981627005099017,4.48762447131239E-17,
0.190809912898503));
#95367=DIRECTION('ref_axis',(-0.179171085423017,-0.343908881724904,0.921750727267987));
#95368=DIRECTION('center_axis',(0.,1.,0.));
#95369=DIRECTION('ref_axis',(1.,0.,0.));
#95370=DIRECTION('',(-0.190809912898503,-1.075932076554E-14,0.981627005099017));
#95371=DIRECTION('center_axis',(0.,1.,0.));
#95372=DIRECTION('ref_axis',(-0.440999214539524,0.,0.897507488980189));
#95373=DIRECTION('center_axis',(0.,1.,0.));
#95374=DIRECTION('ref_axis',(-0.435767598225736,0.,0.900059220460839));
#95375=DIRECTION('center_axis',(-0.981627005099017,0.,-0.190809912898503));
#95376=DIRECTION('ref_axis',(-0.190809912898503,0.,0.981627005099017));
#95377=DIRECTION('center_axis',(-0.981627005099017,3.9547630621265E-16,
-0.190809912898504));
#95378=DIRECTION('ref_axis',(-0.175940012059776,-0.38702419833801,0.905128378771336));
#95379=DIRECTION('center_axis',(-0.981627005099017,1.67043077322241E-16,
-0.190809912898504));
#95380=DIRECTION('ref_axis',(-0.17655939757736,-0.379197781626803,0.908314825122012));
#95381=DIRECTION('center_axis',(0.,-1.,0.));
#95382=DIRECTION('ref_axis',(0.,0.,-1.));
#95383=DIRECTION('',(-0.190809912898503,0.,0.981627005099017));
#95384=DIRECTION('center_axis',(0.,-1.,0.));
#95385=DIRECTION('ref_axis',(-0.476549513638056,0.,0.879147633251283));
#95386=DIRECTION('',(-0.190809912898503,0.,0.981627005099017));
#95387=DIRECTION('center_axis',(0.,-1.,0.));
#95388=DIRECTION('ref_axis',(-0.470447268182042,0.,0.882428109173803));
#95389=DIRECTION('center_axis',(0.981627005099017,0.,0.190809912898503));
#95390=DIRECTION('ref_axis',(0.,-1.,0.));
#95391=DIRECTION('',(-0.190809912898503,0.,0.981627005099017));
#95392=DIRECTION('center_axis',(0.981627005099017,9.66573650244341E-17,
0.190809912898503));
#95393=DIRECTION('ref_axis',(-0.178244202499692,-0.35689266000621,0.916982351797972));
#95394=DIRECTION('center_axis',(0.981627005099017,-2.16345510275123E-16,
0.190809912898504));
#95395=DIRECTION('ref_axis',(-0.178773394006849,-0.3495470901574,0.919704792505599));
#95396=DIRECTION('center_axis',(0.,1.,0.));
#95397=DIRECTION('ref_axis',(1.,0.,0.));
#95398=DIRECTION('',(-0.190809912898503,0.,0.981627005099017));
#95399=DIRECTION('center_axis',(0.,1.,0.));
#95400=DIRECTION('ref_axis',(-0.504512466774432,0.,0.863404407487695));
#95401=DIRECTION('center_axis',(0.,1.,0.));
#95402=DIRECTION('ref_axis',(-0.498009804424277,0.,0.867171398684997));
#95403=DIRECTION('center_axis',(-0.981627005099017,0.,-0.190809912898503));
#95404=DIRECTION('ref_axis',(-0.190809912898503,0.,0.981627005099017));
#95405=DIRECTION('center_axis',(-0.981627005099017,2.46733951980072E-17,
-0.190809912898503));
#95406=DIRECTION('ref_axis',(-0.175321820541314,-0.394654189483089,0.901948074982992));
#95407=DIRECTION('center_axis',(-0.981627005099017,1.26122107472685E-16,
-0.190809912898504));
#95408=DIRECTION('ref_axis',(-0.175992702275721,-0.386365647532587,0.905399445080686));
#95409=DIRECTION('center_axis',(0.,-1.,0.));
#95410=DIRECTION('ref_axis',(0.,0.,-1.));
#95411=DIRECTION('',(-0.190809912898503,0.,0.981627005099017));
#95412=DIRECTION('center_axis',(0.,-1.,0.));
#95413=DIRECTION('ref_axis',(-0.540308722347473,0.,0.841466864799346));
#95414=DIRECTION('',(-0.190809912898503,0.,0.981627005099017));
#95415=DIRECTION('center_axis',(0.,-1.,0.));
#95416=DIRECTION('ref_axis',(-0.53291531834023,0.,0.84616857864041));
#95417=DIRECTION('center_axis',(0.981627005099017,0.,0.190809912898503));
#95418=DIRECTION('ref_axis',(0.,-1.,0.));
#95419=DIRECTION('',(-0.190809912898503,0.,0.981627005099017));
#95420=DIRECTION('center_axis',(0.981627005099017,-4.29489751050862E-16,
0.190809912898504));
#95421=DIRECTION('ref_axis',(-0.177651170119724,-0.364923706798204,0.913931479910694));
#95422=DIRECTION('center_axis',(0.981627005099017,-8.06332694004955E-18,
0.190809912898503));
#95423=DIRECTION('ref_axis',(-0.178230399159777,-0.35708195021081,0.916911340124546));
#95424=DIRECTION('center_axis',(0.,1.,0.));
#95425=DIRECTION('ref_axis',(1.,0.,0.));
#95426=DIRECTION('',(-0.190809912898503,0.,0.981627005099017));
#95427=DIRECTION('center_axis',(0.,1.,0.));
#95428=DIRECTION('ref_axis',(-0.566947419293269,0.,0.823753982543758));
#95429=DIRECTION('center_axis',(0.,1.,0.));
#95430=DIRECTION('ref_axis',(-0.559227720460236,0.,0.829014087135344));
#95431=DIRECTION('center_axis',(-0.981627005099017,0.,-0.190809912898503));
#95432=DIRECTION('ref_axis',(-0.190809912898503,0.,0.981627005099017));
#95433=DIRECTION('center_axis',(-0.981627005099017,-8.64893398502948E-18,
-0.190809912898503));
#95434=DIRECTION('ref_axis',(-0.174485168153884,-0.404710226387007,0.897643893062326));
#95435=DIRECTION('center_axis',(-0.981627005099017,1.65434297745177E-16,
-0.190809912898504));
#95436=DIRECTION('ref_axis',(-0.175228886041806,-0.395786216552817,0.901469970816197));
#95437=DIRECTION('center_axis',(0.,-1.,0.));
#95438=DIRECTION('ref_axis',(0.,0.,-1.));
#95439=DIRECTION('',(-0.190809912898503,0.,0.981627005099017));
#95440=DIRECTION('center_axis',(0.,-1.,0.));
#95441=DIRECTION('ref_axis',(-0.531976328976784,0.,0.846759225168752));
#95442=DIRECTION('',(-0.190809912898503,0.,0.981627005099017));
#95443=DIRECTION('center_axis',(0.,-1.,0.));
#95444=DIRECTION('ref_axis',(-0.525093536093152,0.,0.8510445219571));
#95445=DIRECTION('center_axis',(0.981627005099017,0.,0.190809912898503));
#95446=DIRECTION('ref_axis',(0.,-1.,0.));
#95447=DIRECTION('',(-0.190809912898503,0.,0.981627005099017));
#95448=DIRECTION('center_axis',(0.981627005099017,-1.68427353353279E-16,
0.190809912898504));
#95449=DIRECTION('ref_axis',(-0.182255177482091,-0.296070177213685,0.937616926279399));
#95450=DIRECTION('center_axis',(0.981627005099017,2.41899808201487E-17,
0.190809912898503));
#95451=DIRECTION('ref_axis',(-0.182627045040003,-0.289707997340905,0.939530009471054));
#95452=DIRECTION('center_axis',(0.,1.,0.));
#95453=DIRECTION('ref_axis',(1.,0.,0.));
#95454=DIRECTION('',(-0.190809912898493,0.,0.981627005099019));
#95455=DIRECTION('center_axis',(0.,1.,0.));
#95456=DIRECTION('ref_axis',(-0.559041153008243,0.,0.829139909329671));
#95457=DIRECTION('center_axis',(0.,1.,0.));
#95458=DIRECTION('ref_axis',(-0.551793165097242,0.,0.833980996757101));
#95459=DIRECTION('center_axis',(-0.981627005099017,0.,-0.190809912898503));
#95460=DIRECTION('ref_axis',(-0.190809912898503,0.,0.981627005099017));
#95461=DIRECTION('center_axis',(-0.981627005099017,2.68116953535914E-16,
-0.190809912898504));
#95462=DIRECTION('ref_axis',(-0.179789130769917,-0.33493260114791,0.924930279072587));
#95463=DIRECTION('center_axis',(-0.981627005099017,7.44454339853295E-17,
-0.190809912898503));
#95464=DIRECTION('ref_axis',(-0.180283848265106,-0.327547213698889,0.927475367248542));
#95465=DIRECTION('center_axis',(0.,-1.,0.));
#95466=DIRECTION('ref_axis',(0.,0.,-1.));
#95467=DIRECTION('',(-0.190809912898517,0.,0.981627005099014));
#95468=DIRECTION('center_axis',(0.,-1.,0.));
#95469=DIRECTION('ref_axis',(-0.525640886100688,0.,0.85070656448583));
#95470=DIRECTION('',(-0.190809912898503,0.,0.981627005099017));
#95471=DIRECTION('center_axis',(0.,-1.,0.));
#95472=DIRECTION('ref_axis',(-0.51913056933854,0.,0.854694946737281));
#95473=DIRECTION('center_axis',(0.981627005099017,0.,0.190809912898503));
#95474=DIRECTION('ref_axis',(0.,-1.,0.));
#95475=DIRECTION('',(-0.190809912898503,0.,0.981627005099017));
#95476=DIRECTION('center_axis',(0.981627005099017,-1.43163250350287E-16,
0.190809912898504));
#95477=DIRECTION('ref_axis',(-0.185819133754778,-0.227216647629105,0.955951800338707));
#95478=DIRECTION('center_axis',(0.981627005099017,-1.12886577160694E-16,
0.190809912898504));
#95479=DIRECTION('ref_axis',(-0.186034045655795,-0.222334044470899,0.957057420704813));
#95480=DIRECTION('center_axis',(0.,1.,0.));
#95481=DIRECTION('ref_axis',(1.,0.,0.));
#95482=DIRECTION('',(-0.190809912898503,0.,0.981627005099017));
#95483=DIRECTION('center_axis',(0.,1.,0.));
#95484=DIRECTION('ref_axis',(-0.553126915130717,0.,0.833097002610126));
#95485=DIRECTION('center_axis',(0.,1.,0.));
#95486=DIRECTION('ref_axis',(-0.546219243843012,0.,0.837642249206407));
#95487=DIRECTION('center_axis',(-0.981627005099017,0.,-0.190809912898503));
#95488=DIRECTION('ref_axis',(-0.190809912898503,0.,0.981627005099017));
#95489=DIRECTION('center_axis',(-0.981627005099017,1.47031877745501E-16,
-0.190809912898504));
#95490=DIRECTION('ref_axis',(-0.183980026099205,-0.265154975908797,0.946490458878134));
#95491=DIRECTION('center_axis',(-0.981627005099017,-8.27171488725884E-18,
-0.190809912898503));
#95492=DIRECTION('ref_axis',(-0.184283187692203,-0.259308210845006,0.948050082285932));
#95493=DIRECTION('center_axis',(0.,-1.,0.));
#95494=DIRECTION('ref_axis',(0.,0.,-1.));
#95495=DIRECTION('',(-0.190809912898503,0.,0.981627005099017));
#95496=DIRECTION('center_axis',(0.,-1.,0.));
#95497=DIRECTION('ref_axis',(-0.521013332380248,0.,0.853548538445254));
#95498=DIRECTION('',(-0.190809912898503,0.,0.981627005099017));
#95499=DIRECTION('center_axis',(0.,-1.,0.));
#95500=DIRECTION('ref_axis',(-0.514766609928991,0.,0.857330354823748));
#95501=DIRECTION('center_axis',(0.981627005099017,0.,0.190809912898503));
#95502=DIRECTION('ref_axis',(0.,-1.,0.));
#95503=DIRECTION('',(-0.190809912898517,0.,0.981627005099014));
#95504=DIRECTION('center_axis',(0.981627005099017,-7.57923090089756E-17,
0.190809912898504));
#95505=DIRECTION('ref_axis',(-0.188402071368518,-0.158363118044504,0.969239796101705));
#95506=DIRECTION('center_axis',(0.981627005099017,-4.03166347002478E-18,
0.190809912898503));
#95507=DIRECTION('ref_axis',(-0.18850506856238,-0.154960091600897,0.969769668084816));
#95508=DIRECTION('center_axis',(0.,1.,0.));
#95509=DIRECTION('ref_axis',(1.,0.,0.));
#95510=DIRECTION('',(-0.190809912898503,0.,0.981627005099017));
#95511=DIRECTION('center_axis',(0.,1.,0.));
#95512=DIRECTION('ref_axis',(-0.548948616419421,0.,0.83585609798051));
#95513=DIRECTION('center_axis',(0.,1.,0.));
#95514=DIRECTION('ref_axis',(-0.542274986861829,0.,0.840201070353998));
#95515=DIRECTION('center_axis',(-0.981627005099017,0.,-0.190809912898503));
#95516=DIRECTION('ref_axis',(-0.190809912898503,0.,0.981627005099017));
#95517=DIRECTION('center_axis',(-0.981627005099017,9.08138068428095E-17,
-0.190809912898504));
#95518=DIRECTION('ref_axis',(-0.187132651579236,-0.195377350669603,0.962709230016131));
#95519=DIRECTION('center_axis',(-0.981627005099017,6.20378616544413E-17,
-0.190809912898504));
#95520=DIRECTION('ref_axis',(-0.187294539337449,-0.191069207991,0.9635420661767));
#95521=DIRECTION('center_axis',(0.,-1.,0.));
#95522=DIRECTION('ref_axis',(0.,0.,-1.));
#95523=DIRECTION('',(-0.190809912898503,0.,0.981627005099017));
#95524=DIRECTION('center_axis',(0.,-1.,0.));
#95525=DIRECTION('ref_axis',(-0.517900254205494,0.,0.855441012983294));
#95526=DIRECTION('',(-0.190809912898503,0.,0.981627005099017));
#95527=DIRECTION('center_axis',(0.,-1.,0.));
#95528=DIRECTION('ref_axis',(-0.511826882023824,0.,0.859088611749551));
#95529=DIRECTION('center_axis',(0.981627005099017,0.,0.190809912898503));
#95530=DIRECTION('ref_axis',(0.,-1.,0.));
#95531=DIRECTION('',(-0.190809912898503,0.,0.981627005099017));
#95532=DIRECTION('center_axis',(0.981627005099017,4.21068383383198E-18,
0.190809912898503));
#95533=DIRECTION('ref_axis',(-0.190043994376944,-0.0895095884599529,0.977686715556157));
#95534=DIRECTION('center_axis',(0.981627005099017,-4.23324664352601E-17,
0.190809912898504));
#95535=DIRECTION('ref_axis',(-0.190076620792719,-0.0875861387309634,0.977854563076852));
#95536=DIRECTION('center_axis',(0.,1.,0.));
#95537=DIRECTION('ref_axis',(1.,0.,0.));
#95538=DIRECTION('',(-0.190809912898503,0.,0.981627005099017));
#95539=DIRECTION('center_axis',(0.,1.,0.));
#95540=DIRECTION('ref_axis',(-0.546338397386211,0.,0.837564538135102));
#95541=DIRECTION('center_axis',(0.,1.,0.));
#95542=DIRECTION('ref_axis',(-0.539808318337868,0.,0.841787965851997));
#95543=DIRECTION('center_axis',(-0.981627005099017,0.,-0.190809912898503));
#95544=DIRECTION('ref_axis',(-0.190809912898503,0.,0.981627005099017));
#95545=DIRECTION('center_axis',(-0.981627005099017,-7.35159388727506E-17,
-0.190809912898503));
#95546=DIRECTION('ref_axis',(-0.18929888904543,-0.125599725430494,0.973853500059403));
#95547=DIRECTION('center_axis',(-0.981627005099017,4.13585744362942E-18,
-0.190809912898503));
#95548=DIRECTION('ref_axis',(-0.189365043089146,-0.122830205137097,0.974193831412325));
#95549=DIRECTION('center_axis',(0.,-1.,0.));
#95550=DIRECTION('ref_axis',(0.,0.,-1.));
#95551=DIRECTION('',(-0.190809912898503,0.,0.981627005099017));
#95552=DIRECTION('center_axis',(0.,-1.,0.));
#95553=DIRECTION('ref_axis',(-0.51617952877047,0.,0.85648041079659));
#95554=DIRECTION('',(-0.190809912898503,0.,0.981627005099017));
#95555=DIRECTION('center_axis',(0.,-1.,0.));
#95556=DIRECTION('ref_axis',(-0.510200612741185,0.,0.860055425399154));
#95557=DIRECTION('center_axis',(0.981627005099017,0.,0.190809912898503));
#95558=DIRECTION('ref_axis',(0.,-1.,0.));
#95559=DIRECTION('',(-0.190809912898503,0.,0.981627005099017));
#95560=DIRECTION('center_axis',(0.981627005099017,-1.0000374105351E-17,
0.190809912898504));
#95561=DIRECTION('ref_axis',(-0.190769201858593,-0.0206560588753701,0.98141756600031));
#95562=DIRECTION('center_axis',(0.981627005099017,1.10870745425681E-17,
0.190809912898503));
#95563=DIRECTION('ref_axis',(-0.190770932895652,-0.020212185860989,0.981426471369528));
#95564=DIRECTION('center_axis',(0.,1.,0.));
#95565=DIRECTION('ref_axis',(1.,0.,0.));
#95566=DIRECTION('',(-0.190809912898503,0.,0.981627005099017));
#95567=DIRECTION('center_axis',(0.,1.,0.));
#95568=DIRECTION('ref_axis',(-0.545196651612185,0.,0.838308183826725));
#95569=DIRECTION('center_axis',(0.,1.,0.));
#95570=DIRECTION('ref_axis',(-0.538728725034813,0.,0.842479294002152));
#95571=DIRECTION('center_axis',(-0.981627005099017,0.,-0.190809912898503));
#95572=DIRECTION('ref_axis',(-0.190809912898503,0.,0.981627005099017));
#95573=DIRECTION('center_axis',(-0.981627005099017,3.89202029326326E-17,
-0.190809912898504));
#95574=DIRECTION('ref_axis',(-0.190512388898313,-0.0558221001913178,0.980096384447207));
#95575=DIRECTION('center_axis',(-0.981627005099017,2.68830733835912E-17,
-0.190809912898504));
#95576=DIRECTION('ref_axis',(-0.190525374954579,-0.0545912022831507,0.980163191581737));
#95577=DIRECTION('center_axis',(0.,-1.,0.));
#95578=DIRECTION('ref_axis',(0.,0.,-1.));
#95579=DIRECTION('',(-0.190809912898503,0.,0.981627005099017));
#95580=DIRECTION('center_axis',(0.,-1.,0.));
#95581=DIRECTION('ref_axis',(0.254065172927508,0.,0.967187100774879));
#95582=DIRECTION('',(-0.190809912898503,0.,0.981627005099017));
#95583=DIRECTION('center_axis',(0.,-1.,0.));
#95584=DIRECTION('ref_axis',(0.245183383065688,0.,0.969476718992501));
#95585=DIRECTION('center_axis',(0.981627005099017,0.,0.190809912898503));
#95586=DIRECTION('ref_axis',(0.,-1.,0.));
#95587=DIRECTION('',(-0.190809912898503,0.,0.981627005099017));
#95588=DIRECTION('center_axis',(0.981627005099017,-9.15013555197185E-18,
0.190809912898504));
#95589=DIRECTION('ref_axis',(-0.190765678400248,-0.0215312831584694,0.981399439468988));
#95590=DIRECTION('center_axis',(0.981627005099017,-8.18343260114431E-18,
0.190809912898504));
#95591=DIRECTION('ref_axis',(-0.190767714546191,-0.02102995121624,0.981409914479503));
#95592=DIRECTION('center_axis',(0.,1.,0.));
#95593=DIRECTION('ref_axis',(1.,0.,0.));
#95594=DIRECTION('',(-0.19080991289849,0.,0.98162700509902));
#95595=DIRECTION('center_axis',(0.,1.,0.));
#95596=DIRECTION('ref_axis',(0.218941789395062,0.,0.975737922219121));
#95597=DIRECTION('center_axis',(0.,1.,0.));
#95598=DIRECTION('ref_axis',(0.210813468337157,0.,0.977526307353239));
#95599=DIRECTION('center_axis',(-0.981627005099017,0.,-0.190809912898503));
#95600=DIRECTION('ref_axis',(-0.190809912898503,0.,0.981627005099017));
#95601=DIRECTION('center_axis',(-0.981627005099017,-1.54978312110657E-17,
-0.190809912898503));
#95602=DIRECTION('ref_axis',(-0.190505263436507,-0.0564860647764627,0.980059727306992));
#95603=DIRECTION('center_axis',(-0.981627005099017,4.86497553780052E-17,
-0.190809912898504));
#95604=DIRECTION('ref_axis',(-0.190518864735177,-0.0552117215270287,0.980129699573501));
#95605=DIRECTION('center_axis',(0.,-1.,0.));
#95606=DIRECTION('ref_axis',(0.,0.,-1.));
#95607=DIRECTION('',(-0.190809912898503,0.,0.981627005099017));
#95608=DIRECTION('center_axis',(0.,-1.,0.));
#95609=DIRECTION('ref_axis',(0.256627372086269,0.,0.966510419962504));
#95610=DIRECTION('',(-0.190809912898503,0.,0.981627005099017));
#95611=DIRECTION('center_axis',(0.,-1.,0.));
#95612=DIRECTION('ref_axis',(0.247596031419092,0.,0.968863357355162));
#95613=DIRECTION('center_axis',(0.981627005099017,0.,0.190809912898503));
#95614=DIRECTION('ref_axis',(0.,-1.,0.));
#95615=DIRECTION('',(-0.190809912898503,0.,0.981627005099017));
#95616=DIRECTION('center_axis',(0.981627005099017,1.37252033279578E-17,
0.190809912898503));
#95617=DIRECTION('ref_axis',(-0.189977568186684,-0.0933022270200431,0.977344984137625));
#95618=DIRECTION('center_axis',(0.981627005099017,2.18224869363849E-17,
0.190809912898503));
#95619=DIRECTION('ref_axis',(-0.190015957421534,-0.0911297886037193,0.977542478644391));
#95620=DIRECTION('center_axis',(0.,1.,0.));
#95621=DIRECTION('ref_axis',(1.,0.,0.));
#95622=DIRECTION('',(-0.190809912898503,0.,0.981627005099017));
#95623=DIRECTION('center_axis',(0.,1.,0.));
#95624=DIRECTION('ref_axis',(0.220379730294923,0.,0.975414155359218));
#95625=DIRECTION('center_axis',(0.,1.,0.));
#95626=DIRECTION('ref_axis',(0.212168144710188,0.,0.977233175025407));
#95627=DIRECTION('center_axis',(-0.981627005099017,0.,-0.190809912898503));
#95628=DIRECTION('ref_axis',(-0.190809912898503,0.,0.981627005099017));
#95629=DIRECTION('center_axis',(-0.981627005099017,-4.42795177459019E-17,
-0.190809912898503));
#95630=DIRECTION('ref_axis',(-0.189262582348626,-0.127093645746998,0.973666719228641));
#95631=DIRECTION('center_axis',(-0.981627005099017,2.53824810667853E-17,
-0.190809912898503));
#95632=DIRECTION('ref_axis',(-0.189331880816577,-0.124226373435802,0.974023227161163));
#95633=DIRECTION('center_axis',(0.,-1.,0.));
#95634=DIRECTION('ref_axis',(0.,0.,-1.));
#95635=DIRECTION('',(-0.190809912898493,0.,0.981627005099019));
#95636=DIRECTION('center_axis',(0.,-1.,0.));
#95637=DIRECTION('ref_axis',(0.261269729827485,0.,0.965265832957882));
#95638=DIRECTION('',(-0.190809912898503,0.,0.981627005099017));
#95639=DIRECTION('center_axis',(0.,-1.,0.));
#95640=DIRECTION('ref_axis',(0.251963327850453,0.,0.967736783127791));
#95641=DIRECTION('center_axis',(0.981627005099017,0.,0.190809912898503));
#95642=DIRECTION('ref_axis',(0.,-1.,0.));
#95643=DIRECTION('',(-0.190809912898503,0.,0.981627005099017));
#95644=DIRECTION('center_axis',(0.981627005099017,-9.60764232957044E-17,
0.190809912898504));
#95645=DIRECTION('ref_axis',(-0.188192253350186,-0.165073170881603,0.968160381359448));
#95646=DIRECTION('center_axis',(0.981627005099017,-6.11029634218775E-17,
0.190809912898504));
#95647=DIRECTION('ref_axis',(-0.188313531612905,-0.1612296259912,0.968784300819441));
#95648=DIRECTION('center_axis',(0.,1.,0.));
#95649=DIRECTION('ref_axis',(1.,0.,0.));
#95650=DIRECTION('',(-0.190809912898503,0.,0.981627005099017));
#95651=DIRECTION('center_axis',(0.,1.,0.));
#95652=DIRECTION('ref_axis',(0.223670618325374,0.,0.974664790837314));
#95653=DIRECTION('center_axis',(0.,1.,0.));
#95654=DIRECTION('ref_axis',(0.215266419163362,0.,0.976555358789548));
#95655=DIRECTION('center_axis',(-0.981627005099017,0.,-0.190809912898503));
#95656=DIRECTION('ref_axis',(-0.190809912898503,0.,0.981627005099017));
#95657=DIRECTION('center_axis',(-0.981627005099017,2.21397588729509E-17,
-0.190809912898503));
#95658=DIRECTION('ref_axis',(-0.187043768767229,-0.197701226717603,0.962251969870525));
#95659=DIRECTION('center_axis',(-0.981627005099017,1.35373232356188E-16,
-0.190809912898504));
#95660=DIRECTION('ref_axis',(-0.187213397266324,-0.193241025344597,0.963124628491957));
#95661=DIRECTION('center_axis',(0.,-1.,0.));
#95662=DIRECTION('ref_axis',(0.,0.,-1.));
#95663=DIRECTION('',(-0.190809912898503,0.,0.981627005099017));
#95664=DIRECTION('center_axis',(0.,-1.,0.));
#95665=DIRECTION('ref_axis',(0.268187136288328,0.,0.963366835597669));
#95666=DIRECTION('',(-0.190809912898503,0.,0.981627005099017));
#95667=DIRECTION('center_axis',(0.,-1.,0.));
#95668=DIRECTION('ref_axis',(0.25846100454496,0.,0.966021691852523));
#95669=DIRECTION('center_axis',(0.981627005099017,0.,0.190809912898503));
#95670=DIRECTION('ref_axis',(0.,-1.,0.));
#95671=DIRECTION('',(-0.190809912898503,0.,0.981627005099017));
#95672=DIRECTION('center_axis',(0.981627005099017,-2.19603253247325E-16,
0.190809912898504));
#95673=DIRECTION('ref_axis',(-0.185380925329951,-0.236844114743192,0.953697424676886));
#95674=DIRECTION('center_axis',(0.981627005099017,3.49159790982158E-17,
0.190809912898503));
#95675=DIRECTION('ref_axis',(-0.185634283617771,-0.231329463378695,0.955000833569606));
#95676=DIRECTION('center_axis',(0.,1.,0.));
#95677=DIRECTION('ref_axis',(1.,0.,0.));
#95678=DIRECTION('',(-0.190809912898503,0.,0.981627005099017));
#95679=DIRECTION('center_axis',(0.,1.,0.));
#95680=DIRECTION('ref_axis',(0.228948751797627,0.,0.973438477280567));
#95681=DIRECTION('center_axis',(0.,1.,0.));
#95682=DIRECTION('ref_axis',(0.220229621907956,0.,0.975448057886364));
#95683=DIRECTION('center_axis',(-0.981627005099017,0.,-0.190809912898503));
#95684=DIRECTION('ref_axis',(-0.190809912898503,0.,0.981627005099017));
#95685=DIRECTION('center_axis',(-0.981627005099017,2.21397588729509E-16,
-0.190809912898504));
#95686=DIRECTION('ref_axis',(-0.183813477387126,-0.268308807688208,0.945633644308294));
#95687=DIRECTION('center_axis',(-0.981627005099017,1.18451578311665E-16,
-0.190809912898504));
#95688=DIRECTION('ref_axis',(-0.184131265371603,-0.262255677253399,0.947268513601615));
#95689=DIRECTION('center_axis',(0.,-1.,0.));
#95690=DIRECTION('ref_axis',(0.,0.,-1.));
#95691=DIRECTION('',(-0.190809912898503,0.,0.981627005099017));
#95692=DIRECTION('center_axis',(0.,-1.,0.));
#95693=DIRECTION('ref_axis',(0.277690140407669,0.,0.960670695878858));
#95694=DIRECTION('',(-0.190809912898503,0.,0.981627005099017));
#95695=DIRECTION('center_axis',(0.,-1.,0.));
#95696=DIRECTION('ref_axis',(0.26736789956837,0.,0.963594523791204));
#95697=DIRECTION('center_axis',(0.981627005099017,0.,0.190809912898503));
#95698=DIRECTION('ref_axis',(0.,-1.,0.));
#95699=DIRECTION('',(-0.190809912898503,0.,0.981627005099017));
#95700=DIRECTION('center_axis',(0.981627005099017,9.15013555197185E-18,
0.190809912898503));
#95701=DIRECTION('ref_axis',(-0.181495912294555,-0.308615058604696,0.933710865002002));
#95702=DIRECTION('center_axis',(0.981627005099017,-6.11029634218775E-17,
0.190809912898504));
#95703=DIRECTION('ref_axis',(-0.181935063338814,-0.301429300766198,0.935970089996204));
#95704=DIRECTION('center_axis',(0.,1.,0.));
#95705=DIRECTION('ref_axis',(1.,0.,0.));
#95706=DIRECTION('',(-0.190809912898503,0.,0.981627005099017));
#95707=DIRECTION('center_axis',(0.,1.,0.));
#95708=DIRECTION('ref_axis',(0.236441581346834,0.,0.97164570632006));
#95709=DIRECTION('center_axis',(0.,1.,0.));
#95710=DIRECTION('ref_axis',(0.227262546686523,0.,0.97383352523599));
#95711=DIRECTION('center_axis',(-0.981627005099017,0.,-0.190809912898503));
#95712=DIRECTION('ref_axis',(-0.190809912898503,0.,0.981627005099017));
#95713=DIRECTION('center_axis',(-0.981627005099017,1.85973974532787E-16,
-0.190809912898504));
#95714=DIRECTION('ref_axis',(-0.179517113893821,-0.338916388658794,0.923530880543642));
#95715=DIRECTION('center_axis',(-0.981627005099017,-1.52294886400712E-16,
-0.190809912898503));
#95716=DIRECTION('ref_axis',(-0.180036000309911,-0.331270329162208,0.926200306418203));
#95717=DIRECTION('center_axis',(0.,-1.,0.));
#95718=DIRECTION('ref_axis',(0.,0.,-1.));
#95719=DIRECTION('',(-0.190809912898503,0.,0.981627005099017));
#95720=DIRECTION('center_axis',(0.,-1.,0.));
#95721=DIRECTION('ref_axis',(0.204850037849769,0.,0.978793370427563));
#95722=DIRECTION('',(-0.190809912898503,0.,0.981627005099017));
#95723=DIRECTION('center_axis',(0.,-1.,0.));
#95724=DIRECTION('ref_axis',(0.196208098272871,0.,0.980562278579053));
#95725=DIRECTION('center_axis',(0.981627005099017,0.,0.190809912898503));
#95726=DIRECTION('ref_axis',(0.,-1.,0.));
#95727=DIRECTION('',(-0.190809912898503,0.,0.981627005099017));
#95728=DIRECTION('center_axis',(0.981627005099017,-2.40821729421067E-16,
0.190809912898504));
#95729=DIRECTION('ref_axis',(-0.182068555054379,-0.299207288953005,0.936656841910528));
#95730=DIRECTION('center_axis',(0.981627005099017,-2.13919040821322E-16,
0.190809912898504));
#95731=DIRECTION('ref_axis',(-0.182456464621202,-0.292645194278013,0.938652453671707));
#95732=DIRECTION('center_axis',(0.,1.,0.));
#95733=DIRECTION('ref_axis',(1.,0.,0.));
#95734=DIRECTION('',(-0.190809912898503,0.,0.981627005099017));
#95735=DIRECTION('center_axis',(0.,1.,0.));
#95736=DIRECTION('ref_axis',(0.164995567902462,0.,0.986294308293698));
#95737=DIRECTION('center_axis',(0.,1.,0.));
#95738=DIRECTION('ref_axis',(0.15741294900624,0.,0.987532867040464));
#95739=DIRECTION('center_axis',(-0.981627005099017,0.,-0.190809912898503));
#95740=DIRECTION('ref_axis',(-0.190809912898503,0.,0.981627005099017));
#95741=DIRECTION('center_axis',(-0.981627005099017,2.93287925373025E-16,
-0.190809912898504));
#95742=DIRECTION('ref_axis',(-0.180142425085377,-0.329677418408388,0.926747811692016));
#95743=DIRECTION('center_axis',(-0.981627005099017,-1.60501554366299E-17,
-0.190809912898503));
#95744=DIRECTION('ref_axis',(-0.180606576747544,-0.322627033310802,0.929135653073653));
#95745=DIRECTION('center_axis',(0.,-1.,0.));
#95746=DIRECTION('ref_axis',(0.,0.,-1.));
#95747=DIRECTION('',(-0.190809912898503,0.,0.981627005099017));
#95748=DIRECTION('center_axis',(0.,-1.,0.));
#95749=DIRECTION('ref_axis',(0.133141028786344,0.,0.991097102434324));
#95750=DIRECTION('',(-0.190809912898503,0.,0.981627005099017));
#95751=DIRECTION('center_axis',(0.,-1.,0.));
#95752=DIRECTION('ref_axis',(0.126120325699543,0.,0.992014951220717));
#95753=DIRECTION('center_axis',(0.981627005099017,0.,0.190809912898503));
#95754=DIRECTION('ref_axis',(0.,-1.,0.));
#95755=DIRECTION('',(-0.190809912898514,0.,0.981627005099015));
#95756=DIRECTION('center_axis',(0.981627005099017,-1.63768969384934E-16,
0.190809912898504));
#95757=DIRECTION('ref_axis',(-0.182497177694581,-0.291947095881692,0.938861903231651));
#95758=DIRECTION('center_axis',(0.981627005099017,-1.25592652705723E-16,
0.190809912898504));
#95759=DIRECTION('ref_axis',(-0.182848726580948,-0.285841626719414,0.940670456441641));
#95760=DIRECTION('center_axis',(0.,1.,0.));
#95761=DIRECTION('ref_axis',(1.,0.,0.));
#95762=DIRECTION('',(-0.190809912898503,0.,0.981627005099017));
#95763=DIRECTION('center_axis',(0.,1.,0.));
#95764=DIRECTION('ref_axis',(0.0946046538042337,0.,0.995514921775953));
#95765=DIRECTION('center_axis',(0.,1.,0.));
#95766=DIRECTION('ref_axis',(0.0885667405097263,0.,0.996070244749577));
#95767=DIRECTION('center_axis',(-0.981627005099017,0.,-0.190809912898503));
#95768=DIRECTION('ref_axis',(-0.190809912898503,0.,0.981627005099017));
#95769=DIRECTION('center_axis',(-0.981627005099017,1.3640552305848E-16,
-0.190809912898504));
#95770=DIRECTION('ref_axis',(-0.180608176174812,-0.3226024401748,0.929143881372564));
#95771=DIRECTION('center_axis',(-0.981627005099017,-1.53963266976712E-17,
-0.190809912898503));
#95772=DIRECTION('ref_axis',(-0.181033462471816,-0.315987346735709,0.931331778781543));
#95773=DIRECTION('center_axis',(0.,-1.,0.));
#95774=DIRECTION('ref_axis',(0.,0.,-1.));
#95775=DIRECTION('',(-0.190809912898503,0.,0.981627005099017));
#95776=DIRECTION('center_axis',(0.,-1.,0.));
#95777=DIRECTION('ref_axis',(0.0624727692896659,0.,0.998046668797246));
#95778=DIRECTION('',(-0.190809912898503,-1.10039580182E-14,0.981627005099017));
#95779=DIRECTION('center_axis',(0.,-1.,0.));
#95780=DIRECTION('ref_axis',(0.0570228775206296,0.,0.998372871946783));
#95781=DIRECTION('center_axis',(0.981627005099017,0.,0.190809912898503));
#95782=DIRECTION('ref_axis',(0.,-1.,0.));
#95783=DIRECTION('',(-0.190809912898503,0.,0.981627005099017));
#95784=DIRECTION('center_axis',(0.981627005099017,1.57664003463228E-17,
0.190809912898503));
#95785=DIRECTION('ref_axis',(-0.182813841947861,-0.286453825561204,0.94049099145798));
#95786=DIRECTION('center_axis',(0.981627005099017,-4.54116221843461E-17,
0.190809912898503));
#95787=DIRECTION('ref_axis',(-0.183139631044442,-0.280679847653606,0.942167022699295));
#95788=DIRECTION('center_axis',(0.,1.,0.));
#95789=DIRECTION('ref_axis',(1.,0.,0.));
#95790=DIRECTION('',(-0.190809912898503,0.,0.981627005099017));
#95791=DIRECTION('center_axis',(0.,1.,0.));
#95792=DIRECTION('ref_axis',(0.0251959490043322,0.,0.99968253168382));
#95793=DIRECTION('center_axis',(0.,1.,0.));
#95794=DIRECTION('ref_axis',(0.0206576469622491,0.,0.999786608042928));
#95795=DIRECTION('center_axis',(-0.981627005099017,0.,-0.190809912898503));
#95796=DIRECTION('ref_axis',(-0.190809912898503,0.,0.981627005099017));
#95797=DIRECTION('center_axis',(-0.981627005099017,1.31993506757577E-16,
-0.190809912898504));
#95798=DIRECTION('ref_axis',(-0.180947151082311,-0.317342291967003,0.930887747391878));
#95799=DIRECTION('center_axis',(-0.981627005099017,3.72948009280241E-17,
-0.190809912898503));
#95800=DIRECTION('ref_axis',(-0.18134517801343,-0.311039307001288,0.932935408220438));
#95801=DIRECTION('center_axis',(0.,-1.,0.));
#95802=DIRECTION('ref_axis',(0.,0.,-1.));
#95803=DIRECTION('',(-0.190809912898503,0.,0.981627005099017));
#95804=DIRECTION('center_axis',(0.,-1.,0.));
#95805=DIRECTION('ref_axis',(-0.00721925021943933,0.,0.999973940873596));
#95806=DIRECTION('',(-0.190809912898503,0.,0.981627005099017));
#95807=DIRECTION('center_axis',(0.,-1.,0.));
#95808=DIRECTION('ref_axis',(-0.0111429250982784,0.,0.999937915682896));
#95809=DIRECTION('center_axis',(0.981627005099017,0.,0.190809912898503));
#95810=DIRECTION('ref_axis',(0.,-1.,0.));
#95811=DIRECTION('',(-0.190809912898503,0.,0.981627005099017));
#95812=DIRECTION('center_axis',(0.981627005099017,-7.66548341238665E-18,
0.190809912898503));
#95813=DIRECTION('ref_axis',(-0.183039366361104,-0.28247051610541,0.941651208194026));
#95814=DIRECTION('center_axis',(0.981627005099017,-1.2525082703208E-16,
0.190809912898504));
#95815=DIRECTION('ref_axis',(-0.183347383985879,-0.276929479719012,0.943235813594931));
#95816=DIRECTION('center_axis',(0.,1.,0.));
#95817=DIRECTION('ref_axis',(1.,0.,0.));
#95818=DIRECTION('',(-0.190809912898503,0.,0.981627005099017));
#95819=DIRECTION('center_axis',(0.,1.,0.));
#95820=DIRECTION('ref_axis',(-0.0432822030002458,0.,0.999062886360736));
#95821=DIRECTION('center_axis',(0.,1.,0.));
#95822=DIRECTION('ref_axis',(-0.0463615215085348,0.,0.998924726555216));
#95823=DIRECTION('center_axis',(-0.981627005099017,0.,-0.190809912898503));
#95824=DIRECTION('ref_axis',(-0.190809912898503,0.,0.981627005099017));
#95825=DIRECTION('center_axis',(-0.981627005099017,1.51705767418914E-16,
-0.190809912898504));
#95826=DIRECTION('ref_axis',(-0.181180621351987,-0.313662196346486,0.932088841811555));
#95827=DIRECTION('center_axis',(-0.981627005099017,-1.23990865619567E-16,
-0.190809912898503));
#95828=DIRECTION('ref_axis',(-0.181560378435138,-0.307571801532109,0.93404251288942));
#95829=DIRECTION('center_axis',(0.,-1.,0.));
#95830=DIRECTION('ref_axis',(0.,0.,-1.));
#95831=DIRECTION('',(-0.190809912898503,0.,0.981627005099017));
#95832=DIRECTION('center_axis',(0.,-1.,0.));
#95833=DIRECTION('ref_axis',(-0.0759798223257543,0.,0.997109355386533));
#95834=DIRECTION('',(-0.190809912898503,0.,0.981627005099017));
#95835=DIRECTION('center_axis',(0.,-1.,0.));
#95836=DIRECTION('ref_axis',(-0.0784179965065422,0.,0.996920567459564));
#95837=DIRECTION('center_axis',(0.981627005099017,0.,0.190809912898503));
#95838=DIRECTION('ref_axis',(0.,-1.,0.));
#95839=DIRECTION('',(-0.190809912898503,0.,0.981627005099017));
#95840=DIRECTION('center_axis',(0.981627005099017,-1.88066225336819E-16,
0.190809912898504));
#95841=DIRECTION('ref_axis',(-0.183187172191114,-0.27982644106311,0.942411599475822));
#95842=DIRECTION('center_axis',(0.981627005099017,-1.51948603552176E-16,
0.190809912898504));
#95843=DIRECTION('ref_axis',(-0.183483802676835,-0.274436617915494,0.943937623417116));
#95844=DIRECTION('center_axis',(0.,1.,0.));
#95845=DIRECTION('ref_axis',(1.,0.,0.));
#95846=DIRECTION('',(-0.190809912898503,0.,0.981627005099017));
#95847=DIRECTION('center_axis',(0.,1.,0.));
#95848=DIRECTION('ref_axis',(-0.110864698133628,0.,0.993835508878476));
#95849=DIRECTION('center_axis',(0.,1.,0.));
#95850=DIRECTION('ref_axis',(-0.112522750034819,0.,0.993649148706223));
#95851=DIRECTION('center_axis',(-0.981627005099017,0.,-0.190809912898503));
#95852=DIRECTION('ref_axis',(-0.190809912898503,0.,0.981627005099017));
#95853=DIRECTION('center_axis',(-0.981627005099017,2.39255602982779E-16,
-0.190809912898504));
#95854=DIRECTION('ref_axis',(-0.18132202997097,-0.311409746153812,0.932816322459907));
#95855=DIRECTION('center_axis',(-0.981627005099017,4.31589770358279E-17,
-0.190809912898503));
#95856=DIRECTION('ref_axis',(-0.181690922255445,-0.305447149913308,0.934714099273036));
#95857=DIRECTION('center_axis',(0.,-1.,0.));
#95858=DIRECTION('ref_axis',(0.,0.,-1.));
#95859=DIRECTION('',(-0.190809912898503,0.,0.981627005099017));
#95860=DIRECTION('center_axis',(0.,-1.,0.));
#95861=DIRECTION('ref_axis',(-0.143837786703644,0.,0.989601278857398));
#95862=DIRECTION('',(-0.190809912898503,0.,0.981627005099017));
#95863=DIRECTION('center_axis',(0.,-1.,0.));
#95864=DIRECTION('ref_axis',(-0.1448287547547,0.,0.989456735686914));
#95865=DIRECTION('center_axis',(0.981627005099017,0.,0.190809912898503));
#95866=DIRECTION('ref_axis',(0.,-1.,0.));
#95867=DIRECTION('',(-0.190809912898503,1.137179689376E-14,0.981627005099017));
#95868=DIRECTION('center_axis',(0.981627005099017,-1.19151365507148E-16,
0.190809912898504));
#95869=DIRECTION('ref_axis',(-0.183265446925925,-0.278415153951492,0.942814286067626));
#95870=DIRECTION('center_axis',(0.981627005099017,-1.43311947025832E-17,
0.190809912898503));
#95871=DIRECTION('ref_axis',(-0.183556130616892,-0.273104936120213,0.944309716554759));
#95872=DIRECTION('center_axis',(0.,1.,0.));
#95873=DIRECTION('ref_axis',(1.,0.,0.));
#95874=DIRECTION('',(-0.190809912898503,0.,0.981627005099017));
#95875=DIRECTION('center_axis',(0.,1.,0.));
#95876=DIRECTION('ref_axis',(-0.177572401270701,0.,0.984107739176437));
#95877=DIRECTION('center_axis',(0.,1.,0.));
#95878=DIRECTION('ref_axis',(-0.177845204798666,0.,0.984058475462775));
#95879=DIRECTION('center_axis',(-0.981627005099017,0.,-0.190809912898503));
#95880=DIRECTION('ref_axis',(-0.190809912898503,0.,0.981627005099017));
#95881=DIRECTION('center_axis',(-0.981627005099017,2.45286952692658E-16,
-0.190809912898504));
#95882=DIRECTION('ref_axis',(-0.181379056342926,-0.310496268400187,0.933109696246754));
#95883=DIRECTION('center_axis',(-0.981627005099017,6.43735225938313E-17,
-0.190809912898503));
#95884=DIRECTION('ref_axis',(-0.181743610098458,-0.304585001530188,0.934985153374766));
#95885=DIRECTION('center_axis',(0.,-1.,0.));
#95886=DIRECTION('ref_axis',(0.,0.,-1.));
#95887=DIRECTION('',(-0.190809912898503,0.,0.981627005099017));
#95888=DIRECTION('center_axis',(0.,-1.,0.));
#95889=DIRECTION('ref_axis',(-0.210808250907887,0.,0.977527432530237));
#95890=DIRECTION('',(-0.190809912898503,0.,0.981627005099017));
#95891=DIRECTION('center_axis',(0.,-1.,0.));
#95892=DIRECTION('ref_axis',(-0.210389062719221,0.,0.977617738325225));
#95893=DIRECTION('center_axis',(0.981627005099017,0.,0.190809912898503));
#95894=DIRECTION('ref_axis',(0.,-1.,0.));
#95895=DIRECTION('',(-0.190809912898503,0.,0.981627005099017));
#95896=DIRECTION('center_axis',(0.981627005099017,-1.41255374499376E-16,
0.190809912898504));
#95897=DIRECTION('ref_axis',(-0.183278336628812,-0.278182009056604,0.942880597509466));
#95898=DIRECTION('center_axis',(0.981627005099017,-9.30027011440924E-17,
0.190809912898504));
#95899=DIRECTION('ref_axis',(-0.183568046602459,-0.272884868293189,0.944371018680246));
#95900=DIRECTION('center_axis',(0.,1.,0.));
#95901=DIRECTION('ref_axis',(1.,0.,0.));
#95902=DIRECTION('',(-0.190809912898503,0.,0.981627005099017));
#95903=DIRECTION('center_axis',(0.,1.,0.));
#95904=DIRECTION('ref_axis',(-0.243413668799643,0.,0.969922566930731));
#95905=DIRECTION('center_axis',(0.,1.,0.));
#95906=DIRECTION('ref_axis',(-0.242336570704233,0.,0.97019224203212));
#95907=DIRECTION('center_axis',(-0.981627005099017,0.,-0.190809912898503));
#95908=DIRECTION('ref_axis',(-0.190809912898503,0.,0.981627005099017));
#95909=DIRECTION('center_axis',(-0.981627005099017,6.70648161298212E-17,
-0.190809912898503));
#95910=DIRECTION('ref_axis',(-0.181354700681431,-0.31088677343731,0.932984397855874));
#95911=DIRECTION('center_axis',(-0.981627005099017,1.50568650592271E-16,
-0.190809912898504));
#95912=DIRECTION('ref_axis',(-0.181721104376961,-0.304953598801405,0.934869372052636));
#95913=DIRECTION('center_axis',(0.,-1.,0.));
#95914=DIRECTION('ref_axis',(0.,0.,-1.));
#95915=DIRECTION('',(-0.190809912898503,0.,0.981627005099017));
#95916=DIRECTION('center_axis',(0.,-1.,0.));
#95917=DIRECTION('ref_axis',(-0.276893691776251,0.,0.960900558567076));
#95918=DIRECTION('',(-0.190809912898503,0.,0.981627005099017));
#95919=DIRECTION('center_axis',(0.,-1.,0.));
#95920=DIRECTION('ref_axis',(-0.275101194754168,0.,0.961415275853691));
#95921=DIRECTION('center_axis',(0.981627005099017,0.,0.190809912898503));
#95922=DIRECTION('ref_axis',(0.,-1.,0.));
#95923=DIRECTION('',(-0.190809912898503,0.,0.981627005099017));
#95924=DIRECTION('center_axis',(0.981627005099017,-7.48461333200017E-17,
0.190809912898504));
#95925=DIRECTION('ref_axis',(-0.183226511622911,-0.279118121617608,0.942613982297715));
#95926=DIRECTION('center_axis',(0.981627005099017,-1.94412209408584E-16,
0.190809912898504));
#95927=DIRECTION('ref_axis',(-0.183520146118496,-0.273768347927886,0.944124593282837));
#95928=DIRECTION('center_axis',(0.,1.,0.));
#95929=DIRECTION('ref_axis',(1.,0.,0.));
#95930=DIRECTION('',(-0.190809912898503,0.,0.981627005099017));
#95931=DIRECTION('center_axis',(0.,1.,0.));
#95932=DIRECTION('ref_axis',(-0.308384935821295,0.,0.951261652416671));
#95933=DIRECTION('center_axis',(0.,1.,0.));
#95934=DIRECTION('ref_axis',(-0.305993568691603,0.,0.952033579197382));
#95935=DIRECTION('center_axis',(-0.981627005099017,0.,-0.190809912898503));
#95936=DIRECTION('ref_axis',(-0.190809912898503,0.,0.981627005099017));
#95937=DIRECTION('center_axis',(-0.981627005099017,5.27367097735159E-17,
-0.190809912898503));
#95938=DIRECTION('ref_axis',(-0.181247688350776,-0.312596151213815,0.932433869887731));
#95939=DIRECTION('center_axis',(-0.981627005099017,-2.17379342169057E-17,
-0.190809912898503));
#95940=DIRECTION('ref_axis',(-0.181622273580826,-0.306566459909599,0.934360934220726));
#95941=DIRECTION('center_axis',(0.,-1.,0.));
#95942=DIRECTION('ref_axis',(0.,0.,-1.));
#95943=DIRECTION('',(-0.190809912898503,0.,0.981627005099017));
#95944=DIRECTION('center_axis',(0.,-1.,0.));
#95945=DIRECTION('ref_axis',(-0.342084131986487,0.,0.939669328350698));
#95946=DIRECTION('',(-0.190809912898503,0.,0.981627005099017));
#95947=DIRECTION('center_axis',(0.,-1.,0.));
#95948=DIRECTION('ref_axis',(-0.338955991905877,0.,0.940802229775793));
#95949=DIRECTION('center_axis',(0.981627005099017,0.,0.190809912898503));
#95950=DIRECTION('ref_axis',(0.,-1.,0.));
#95951=DIRECTION('',(-0.190809912898503,0.,0.981627005099017));
#95952=DIRECTION('center_axis',(0.981627005099017,6.83990283108474E-17,
0.190809912898503));
#95953=DIRECTION('ref_axis',(-0.183107255498057,-0.281259409527999,0.942000465783287));
#95954=DIRECTION('center_axis',(0.981627005099017,-1.82677034101796E-16,
0.190809912898504));
#95955=DIRECTION('ref_axis',(-0.183410017255811,-0.275787971799909,0.943558032227332));
#95956=DIRECTION('center_axis',(0.,1.,0.));
#95957=DIRECTION('ref_axis',(1.,0.,0.));
#95958=DIRECTION('',(-0.190809912898503,0.,0.981627005099017));
#95959=DIRECTION('center_axis',(0.,1.,0.));
#95960=DIRECTION('ref_axis',(-0.372470467214768,0.,0.928044045858176));
#95961=DIRECTION('center_axis',(0.,1.,0.));
#95962=DIRECTION('ref_axis',(-0.368801736329265,0.,0.929508084569746));
#95963=DIRECTION('center_axis',(-0.981627005099017,0.,-0.190809912898503));
#95964=DIRECTION('ref_axis',(-0.190809912898503,0.,0.981627005099017));
#95965=DIRECTION('center_axis',(-0.981627005099017,2.68930199968124E-16,
-0.190809912898504));
#95966=DIRECTION('ref_axis',(-0.181052299422872,-0.315690778691902,0.931428686010148));
#95967=DIRECTION('center_axis',(-0.981627005099017,1.40306285732571E-16,
-0.190809912898504));
#95968=DIRECTION('ref_axis',(-0.181442047051767,-0.309483781404091,0.933433753733755));
#95969=DIRECTION('center_axis',(0.,-1.,0.));
#95970=DIRECTION('ref_axis',(0.,0.,-1.));
#95971=DIRECTION('',(-0.190809912898503,0.,0.981627005099017));
#95972=DIRECTION('center_axis',(0.,-1.,0.));
#95973=DIRECTION('ref_axis',(-0.406356421956365,0.,0.913714648199765));
#95974=DIRECTION('',(-0.190809912898503,0.,0.981627005099017));
#95975=DIRECTION('center_axis',(0.,-1.,0.));
#95976=DIRECTION('ref_axis',(-0.40193223106788,0.,0.915669417218243));
#95977=DIRECTION('center_axis',(0.981627005099017,0.,0.190809912898503));
#95978=DIRECTION('ref_axis',(0.,-1.,0.));
#95979=DIRECTION('',(-0.190809912898503,0.,0.981627005099017));
#95980=DIRECTION('center_axis',(0.981627005099017,8.56509061367008E-17,
0.190809912898503));
#95981=DIRECTION('ref_axis',(-0.182914100187073,-0.284690508229704,0.941006772811262));
#95982=DIRECTION('center_axis',(0.981627005099017,-2.61778094159889E-16,
0.190809912898504));
#95983=DIRECTION('ref_axis',(-0.18323192975892,-0.279020413474902,0.942641856051977));
#95984=DIRECTION('center_axis',(0.,1.,0.));
#95985=DIRECTION('ref_axis',(1.,0.,0.));
#95986=DIRECTION('',(-0.190809912898503,0.,0.981627005099017));
#95987=DIRECTION('center_axis',(0.,1.,0.));
#95988=DIRECTION('ref_axis',(-0.435641230883273,0.,0.900120390811422));
#95989=DIRECTION('center_axis',(0.,1.,0.));
#95990=DIRECTION('ref_axis',(-0.430734436520186,0.,0.902478722849263));
#95991=DIRECTION('center_axis',(-0.981627005099017,0.,-0.190809912898503));
#95992=DIRECTION('ref_axis',(-0.190809912898503,0.,0.981627005099017));
#95993=DIRECTION('center_axis',(-0.981627005099017,-7.90952612425299E-18,
-0.190809912898503));
#95994=DIRECTION('ref_axis',(-0.180757579546461,-0.320295888279689,0.929912491252607));
#95995=DIRECTION('center_axis',(-0.981627005099017,5.31500700570768E-17,
-0.190809912898503));
#95996=DIRECTION('ref_axis',(-0.181170744386621,-0.313818853760112,0.932038029483286));
#95997=DIRECTION('center_axis',(0.,-1.,0.));
#95998=DIRECTION('ref_axis',(0.,0.,-1.));
#95999=DIRECTION('',(-0.190809912898503,0.,0.981627005099017));
#96000=DIRECTION('center_axis',(0.,-1.,0.));
#96001=DIRECTION('ref_axis',(-0.469672502576099,0.,0.882840721944737));
#96002=DIRECTION('',(-0.190809912898503,0.,0.981627005099017));
#96003=DIRECTION('center_axis',(0.,-1.,0.));
#96004=DIRECTION('ref_axis',(-0.463995103545157,0.,0.88583776386318));
#96005=DIRECTION('center_axis',(0.981627005099017,0.,0.190809912898503));
#96006=DIRECTION('ref_axis',(0.,-1.,0.));
#96007=DIRECTION('',(-0.190809912898503,0.,0.981627005099017));
#96008=DIRECTION('center_axis',(0.981627005099017,0.,0.190809912898503));
#96009=DIRECTION('ref_axis',(-0.182635912358673,-0.2895544222692,0.939575627643281));
#96010=DIRECTION('center_axis',(0.981627005099017,-2.16345510275123E-16,
0.190809912898504));
#96011=DIRECTION('ref_axis',(-0.18297605983338,-0.283594808995592,0.941325525967826));
#96012=DIRECTION('center_axis',(0.,1.,0.));
#96013=DIRECTION('ref_axis',(1.,0.,0.));
#96014=DIRECTION('',(-0.190809912898503,0.,0.981627005099017));
#96015=DIRECTION('center_axis',(0.,1.,0.));
#96016=DIRECTION('ref_axis',(-0.497852697527391,0.,0.867261605033164));
#96017=DIRECTION('center_axis',(0.,1.,0.));
#96018=DIRECTION('ref_axis',(-0.491750929833315,0.,0.870735908877123));
#96019=DIRECTION('center_axis',(-0.981627005099017,0.,-0.190809912898503));
#96020=DIRECTION('ref_axis',(-0.190809912898503,0.,0.981627005099017));
#96021=DIRECTION('center_axis',(-0.981627005099017,1.97387161584057E-16,
-0.190809912898504));
#96022=DIRECTION('ref_axis',(-0.180345720095873,-0.326610363710094,0.927793668635576));
#96023=DIRECTION('center_axis',(-0.981627005099017,1.57652634340856E-16,
-0.190809912898504));
#96024=DIRECTION('ref_axis',(-0.180792707058803,-0.319750880716613,0.930093205735479));
#96025=DIRECTION('center_axis',(0.,-1.,0.));
#96026=DIRECTION('ref_axis',(0.,0.,-1.));
#96027=DIRECTION('',(-0.190809912898503,0.,0.981627005099017));
#96028=DIRECTION('center_axis',(0.,-1.,0.));
#96029=DIRECTION('ref_axis',(-0.464446491029698,0.,0.885601183925474));
#96030=DIRECTION('',(-0.190809912898503,0.,0.981627005099017));
#96031=DIRECTION('center_axis',(0.,-1.,0.));
#96032=DIRECTION('ref_axis',(-0.459078725961924,0.,0.888395589458422));
#96033=DIRECTION('center_axis',(0.981627005099017,0.,0.190809912898503));
#96034=DIRECTION('ref_axis',(0.,-1.,0.));
#96035=DIRECTION('',(-0.190809912898503,0.,0.981627005099017));
#96036=DIRECTION('center_axis',(0.981627005099017,8.05478041870284E-18,
0.190809912898503));
#96037=DIRECTION('ref_axis',(-0.186039172622593,-0.222216184532195,0.957083796530823));
#96038=DIRECTION('center_axis',(0.981627005099017,-1.08172755137562E-16,
0.190809912898504));
#96039=DIRECTION('ref_axis',(-0.186235922579013,-0.217642527833793,0.958095982258177));
#96040=DIRECTION('center_axis',(0.,1.,0.));
#96041=DIRECTION('ref_axis',(1.,0.,0.));
#96042=DIRECTION('',(-0.190809912898503,0.,0.981627005099017));
#96043=DIRECTION('center_axis',(0.,1.,0.));
#96044=DIRECTION('ref_axis',(-0.492873509125509,0.,0.870100973452108));
#96045=DIRECTION('center_axis',(0.,1.,0.));
#96046=DIRECTION('ref_axis',(-0.487060705905151,0.,0.873368117555923));
#96047=DIRECTION('center_axis',(-0.981627005099017,0.,-0.190809912898503));
#96048=DIRECTION('ref_axis',(-0.190809912898503,0.,0.981627005099017));
#96049=DIRECTION('center_axis',(-0.981627005099017,5.75712554620167E-17,
-0.190809912898503));
#96050=DIRECTION('ref_axis',(-0.184321126056631,-0.258566537937205,0.948245257277031));
#96051=DIRECTION('center_axis',(-0.981627005099017,3.94131585852141E-17,
-0.190809912898503));
#96052=DIRECTION('ref_axis',(-0.184595362527196,-0.253136113900701,0.949656074572634));
#96053=DIRECTION('center_axis',(0.,-1.,0.));
#96054=DIRECTION('ref_axis',(0.,0.,-1.));
#96055=DIRECTION('',(-0.190809912898503,0.,0.981627005099017));
#96056=DIRECTION('center_axis',(0.,-1.,0.));
#96057=DIRECTION('ref_axis',(-0.460630809902228,0.,0.887591830161149));
#96058=DIRECTION('',(-0.190809912898503,0.,0.981627005099017));
#96059=DIRECTION('center_axis',(0.,-1.,0.));
#96060=DIRECTION('ref_axis',(-0.455482023679629,0.,0.890244980948901));
#96061=DIRECTION('center_axis',(0.981627005099017,0.,0.190809912898503));
#96062=DIRECTION('ref_axis',(0.,-1.,0.));
#96063=DIRECTION('',(-0.190809912898503,0.,0.981627005099017));
#96064=DIRECTION('center_axis',(0.981627005099017,4.83286825122171E-17,
0.190809912898503));
#96065=DIRECTION('ref_axis',(-0.188507526443361,-0.154877946795105,0.969782312723189));
#96066=DIRECTION('center_axis',(0.981627005099017,-3.86331268348435E-17,
0.190809912898503));
#96067=DIRECTION('ref_axis',(-0.188601875825374,-0.151690246672095,0.97026769579313));
#96068=DIRECTION('center_axis',(0.,1.,0.));
#96069=DIRECTION('ref_axis',(1.,0.,0.));
#96070=DIRECTION('',(-0.190809912898503,0.,0.981627005099017));
#96071=DIRECTION('center_axis',(0.,1.,0.));
#96072=DIRECTION('ref_axis',(-0.489357122006741,0.,0.872083486336761));
#96073=DIRECTION('center_axis',(0.,1.,0.));
#96074=DIRECTION('ref_axis',(-0.483742917424828,0.,0.875210140389905));
#96075=DIRECTION('center_axis',(-0.981627005099017,0.,-0.190809912898503));
#96076=DIRECTION('ref_axis',(-0.190809912898503,0.,0.981627005099017));
#96077=DIRECTION('center_axis',(-0.981627005099017,1.64489301320047E-16,
-0.190809912898504));
#96078=DIRECTION('ref_axis',(-0.187314807261953,-0.190522712164197,0.963646335088769));
#96079=DIRECTION('center_axis',(-0.981627005099017,1.65535266057899E-16,
-0.190809912898504));
#96080=DIRECTION('ref_axis',(-0.187461372226399,-0.186521347084696,0.964400342702503));
#96081=DIRECTION('center_axis',(0.,-1.,0.));
#96082=DIRECTION('ref_axis',(0.,0.,-1.));
#96083=DIRECTION('',(-0.190809912898503,0.,0.981627005099017));
#96084=DIRECTION('center_axis',(0.,-1.,0.));
#96085=DIRECTION('ref_axis',(-0.458064609075315,0.,0.888918901763642));
#96086=DIRECTION('',(-0.190809912898517,0.,0.981627005099014));
#96087=DIRECTION('center_axis',(0.,-1.,0.));
#96088=DIRECTION('ref_axis',(-0.453059767116766,0.,0.891480144153588));
#96089=DIRECTION('center_axis',(0.981627005099017,0.,0.190809912898503));
#96090=DIRECTION('ref_axis',(0.,-1.,0.));
#96091=DIRECTION('',(-0.190809912898503,0.,0.981627005099017));
#96092=DIRECTION('center_axis',(0.981627005099017,-8.05478041870284E-18,
0.190809912898503));
#96093=DIRECTION('ref_axis',(-0.190077399524955,-0.087539709058116,0.977858569286914));
#96094=DIRECTION('center_axis',(0.981627005099017,-2.51115324426482E-17,
0.190809912898504));
#96095=DIRECTION('ref_axis',(-0.190107297572009,-0.0857379655103025,0.978012380637393));
#96096=DIRECTION('center_axis',(0.,1.,0.));
#96097=DIRECTION('ref_axis',(1.,0.,0.));
#96098=DIRECTION('',(-0.190809912898503,0.,0.981627005099017));
#96099=DIRECTION('center_axis',(0.,1.,0.));
#96100=DIRECTION('ref_axis',(-0.48716094882944,0.,0.873312206450591));
#96101=DIRECTION('center_axis',(0.,1.,0.));
#96102=DIRECTION('ref_axis',(-0.481668504198278,0.,0.876353497204977));
#96103=DIRECTION('center_axis',(-0.981627005099017,0.,-0.190809912898503));
#96104=DIRECTION('ref_axis',(-0.190809912898503,0.,0.981627005099017));
#96105=DIRECTION('center_axis',(-0.981627005099017,-2.0561162665006E-17,
-0.190809912898503));
#96106=DIRECTION('ref_axis',(-0.18937332780328,-0.122478886391301,0.974236452359004));
#96107=DIRECTION('center_axis',(-0.981627005099017,-1.97065792926071E-17,
-0.190809912898503));
#96108=DIRECTION('ref_axis',(-0.189433253567106,-0.119906580268704,0.974544742149505));
#96109=DIRECTION('center_axis',(0.,-1.,0.));
#96110=DIRECTION('ref_axis',(0.,0.,-1.));
#96111=DIRECTION('',(-0.190809912898503,0.,0.981627005099017));
#96112=DIRECTION('center_axis',(0.,-1.,0.));
#96113=DIRECTION('ref_axis',(-0.456646407116791,0.,0.889648278179262));
#96114=DIRECTION('',(-0.190809912898503,0.,0.981627005099017));
#96115=DIRECTION('center_axis',(0.,-1.,0.));
#96116=DIRECTION('ref_axis',(-0.451719976566491,0.,0.892159774239328));
#96117=DIRECTION('center_axis',(0.981627005099017,0.,0.190809912898503));
#96118=DIRECTION('ref_axis',(0.,-1.,0.));
#96119=DIRECTION('',(-0.190809912898503,0.,0.981627005099017));
#96120=DIRECTION('center_axis',(0.981627005099017,-1.56061370612367E-17,
0.190809912898504));
#96121=DIRECTION('ref_axis',(-0.190770974215747,-0.0202014713211108,0.981426683941922));
#96122=DIRECTION('center_axis',(0.981627005099017,0.,0.190809912898503));
#96123=DIRECTION('ref_axis',(-0.190772560748925,-0.0197856843485292,0.981434845906827));
#96124=DIRECTION('center_axis',(0.,1.,0.));
#96125=DIRECTION('ref_axis',(1.,0.,0.));
#96126=DIRECTION('',(-0.190809912898503,0.,0.981627005099017));
#96127=DIRECTION('center_axis',(0.,1.,0.));
#96128=DIRECTION('ref_axis',(-0.486200442577545,0.,0.873847314831029));
#96129=DIRECTION('center_axis',(0.,1.,0.));
#96130=DIRECTION('ref_axis',(-0.480760703718784,0.,0.87685183797482));
#96131=DIRECTION('center_axis',(-0.981627005099017,0.,-0.190809912898503));
#96132=DIRECTION('ref_axis',(-0.190809912898503,0.,0.981627005099017));
#96133=DIRECTION('center_axis',(-0.981627005099017,4.11223253300119E-18,
-0.190809912898503));
#96134=DIRECTION('ref_axis',(-0.190527001503476,-0.0544350606183517,0.980171559408643));
#96135=DIRECTION('center_axis',(-0.981627005099017,1.18239475755642E-17,
-0.190809912898504));
#96136=DIRECTION('ref_axis',(-0.190538768513374,-0.05329181345277,0.980232095124579));
#96137=DIRECTION('center_axis',(0.,-1.,0.));
#96138=DIRECTION('ref_axis',(0.,0.,-1.));
#96139=DIRECTION('',(-0.190809912898503,0.,0.981627005099017));
#96140=DIRECTION('center_axis',(0.,-1.,0.));
#96141=DIRECTION('ref_axis',(0.185064286707852,0.,0.982726416550056));
#96142=DIRECTION('',(-0.190809912898503,0.,0.981627005099017));
#96143=DIRECTION('center_axis',(0.,-1.,0.));
#96144=DIRECTION('ref_axis',(0.177619933460537,0.,0.984099161282782));
#96145=DIRECTION('center_axis',(0.981627005099017,0.,0.190809912898503));
#96146=DIRECTION('ref_axis',(0.,-1.,0.));
#96147=DIRECTION('',(-0.190809912898503,0.,0.981627005099017));
#96148=DIRECTION('center_axis',(0.981627005099017,-1.66640035983327E-17,
0.190809912898504));
#96149=DIRECTION('ref_axis',(-0.19076833445818,-0.0208749271362605,0.981413103634299));
#96150=DIRECTION('center_axis',(0.981627005099017,4.62805617161513E-18,
0.190809912898503));
#96151=DIRECTION('ref_axis',(-0.190770138410662,-0.0204171065775405,0.981422384118978));
#96152=DIRECTION('center_axis',(0.,1.,0.));
#96153=DIRECTION('ref_axis',(1.,0.,0.));
#96154=DIRECTION('',(-0.190809912898503,0.,0.981627005099017));
#96155=DIRECTION('center_axis',(0.,1.,0.));
#96156=DIRECTION('ref_axis',(0.150536423879934,0.,0.988604463415698));
#96157=DIRECTION('center_axis',(0.,1.,0.));
#96158=DIRECTION('ref_axis',(0.143816312892431,0.,0.989604399821477));
#96159=DIRECTION('center_axis',(-0.981627005099017,0.,-0.190809912898503));
#96160=DIRECTION('ref_axis',(-0.190809912898503,0.,0.981627005099017));
#96161=DIRECTION('center_axis',(-0.981627005099017,0.,-0.190809912898503));
#96162=DIRECTION('ref_axis',(-0.190521659123586,-0.0549462364013984,0.980144075383878));
#96163=DIRECTION('center_axis',(-0.981627005099017,2.80877720141023E-17,
-0.190809912898504));
#96164=DIRECTION('ref_axis',(-0.190533865149434,-0.0537711722184585,0.980206869629809));
#96165=DIRECTION('center_axis',(0.,-1.,0.));
#96166=DIRECTION('ref_axis',(0.,0.,-1.));
#96167=DIRECTION('',(-0.190809912898503,0.,0.981627005099017));
#96168=DIRECTION('center_axis',(0.,-1.,0.));
#96169=DIRECTION('ref_axis',(0.187211227674096,0.,0.982319681281383));
#96170=DIRECTION('',(-0.190809912898503,0.,0.981627005099017));
#96171=DIRECTION('center_axis',(0.,-1.,0.));
#96172=DIRECTION('ref_axis',(0.179642428155144,0.,0.983731974679345));
#96173=DIRECTION('center_axis',(0.981627005099017,0.,0.190809912898503));
#96174=DIRECTION('ref_axis',(0.,-1.,0.));
#96175=DIRECTION('',(-0.190809912898503,0.,0.981627005099017));
#96176=DIRECTION('center_axis',(0.981627005099017,-2.1501940126881E-18,
0.190809912898503));
#96177=DIRECTION('ref_axis',(-0.190027643704127,-0.0904580175904463,0.977602599056418));
#96178=DIRECTION('center_axis',(0.981627005099017,-2.05691385405117E-18,
0.190809912898503));
#96179=DIRECTION('ref_axis',(-0.190061647076601,-0.0884741285026728,0.97777753036988));
#96180=DIRECTION('center_axis',(0.,1.,0.));
#96181=DIRECTION('ref_axis',(1.,0.,0.));
#96182=DIRECTION('',(-0.190809912898503,0.,0.981627005099017));
#96183=DIRECTION('center_axis',(0.,1.,0.));
#96184=DIRECTION('ref_axis',(0.151724977115547,0.,0.988422749292673));
#96185=DIRECTION('center_axis',(0.,1.,0.));
#96186=DIRECTION('ref_axis',(0.144936472974812,0.,0.989440962767169));
#96187=DIRECTION('center_axis',(-0.981627005099017,0.,-0.190809912898503));
#96188=DIRECTION('ref_axis',(-0.190809912898503,0.,0.981627005099017));
#96189=DIRECTION('center_axis',(-0.981627005099017,2.51389650319736E-17,
-0.190809912898503));
#96190=DIRECTION('ref_axis',(-0.189346115666816,-0.123629031903203,0.974096458751681));
#96191=DIRECTION('center_axis',(-0.981627005099017,6.01880828873621E-17,
-0.190809912898504));
#96192=DIRECTION('ref_axis',(-0.189408284096429,-0.120985137491496,0.974416285999885));
#96193=DIRECTION('center_axis',(0.,-1.,0.));
#96194=DIRECTION('ref_axis',(0.,0.,-1.));
#96195=DIRECTION('',(-0.190809912898503,0.,0.981627005099017));
#96196=DIRECTION('center_axis',(0.,-1.,0.));
#96197=DIRECTION('ref_axis',(0.191100511883499,0.,0.981570473454588));
#96198=DIRECTION('',(-0.190809912898503,0.,0.981627005099017));
#96199=DIRECTION('center_axis',(0.,-1.,0.));
#96200=DIRECTION('ref_axis',(0.18330289149611,0.,0.983056483610767));
#96201=DIRECTION('center_axis',(0.981627005099017,0.,0.190809912898503));
#96202=DIRECTION('ref_axis',(0.,-1.,0.));
#96203=DIRECTION('',(-0.190809912898503,0.,0.981627005099017));
#96204=DIRECTION('center_axis',(0.981627005099017,-1.29011640761286E-16,
0.190809912898504));
#96205=DIRECTION('ref_axis',(-0.188350439968379,-0.160041108044595,0.968974176900281));
#96206=DIRECTION('center_axis',(0.981627005099017,-4.11382770810234E-17,
0.190809912898504));
#96207=DIRECTION('ref_axis',(-0.188457803354032,-0.156531150427793,0.969526510880814));
#96208=DIRECTION('center_axis',(0.,1.,0.));
#96209=DIRECTION('ref_axis',(1.,0.,0.));
#96210=DIRECTION('',(-0.190809912898503,0.,0.981627005099017));
#96211=DIRECTION('center_axis',(0.,1.,0.));
#96212=DIRECTION('ref_axis',(0.154444807220379,0.,0.988001417773608));
#96213=DIRECTION('center_axis',(0.,1.,0.));
#96214=DIRECTION('ref_axis',(0.147498119662627,0.,0.989062336102224));
#96215=DIRECTION('center_axis',(-0.981627005099017,0.,-0.190809912898503));
#96216=DIRECTION('ref_axis',(-0.190809912898503,0.,0.981627005099017));
#96217=DIRECTION('center_axis',(-0.981627005099017,1.63403272707828E-16,
-0.190809912898504));
#96218=DIRECTION('ref_axis',(-0.18724822993152,-0.192311827404893,0.963303826125332));
#96219=DIRECTION('center_axis',(-0.981627005099017,1.00313471478937E-16,
-0.190809912898504));
#96220=DIRECTION('ref_axis',(-0.187400310802369,-0.188199102764594,0.964086210475898));
#96221=DIRECTION('center_axis',(0.,-1.,0.));
#96222=DIRECTION('ref_axis',(0.,0.,-1.));
#96223=DIRECTION('',(-0.190809912898503,0.,0.981627005099017));
#96224=DIRECTION('center_axis',(0.,-1.,0.));
#96225=DIRECTION('ref_axis',(0.196894140539301,0.,0.980424753574332));
#96226=DIRECTION('',(-0.190809912898503,0.,0.981627005099017));
#96227=DIRECTION('center_axis',(0.,-1.,0.));
#96228=DIRECTION('ref_axis',(0.188747517532452,0.,0.982025648659615));
#96229=DIRECTION('center_axis',(0.981627005099017,0.,0.190809912898503));
#96230=DIRECTION('ref_axis',(0.,-1.,0.));
#96231=DIRECTION('',(-0.190809912898503,0.,0.981627005099017));
#96232=DIRECTION('center_axis',(0.981627005099017,-6.88062084060191E-17,
0.190809912898504));
#96233=DIRECTION('ref_axis',(-0.185711351364325,-0.229624198498799,0.955397310776109));
#96234=DIRECTION('center_axis',(0.981627005099017,-9.05042095782515E-17,
0.190809912898504));
#96235=DIRECTION('ref_axis',(-0.185935439268292,-0.224588172352909,0.956550137349469));
#96236=DIRECTION('center_axis',(0.,1.,0.));
#96237=DIRECTION('ref_axis',(1.,0.,0.));
#96238=DIRECTION('',(-0.190809912898503,0.,0.981627005099017));
#96239=DIRECTION('center_axis',(0.,1.,0.));
#96240=DIRECTION('ref_axis',(0.158806144368473,0.,0.987309783457462));
#96241=DIRECTION('center_axis',(0.,1.,0.));
#96242=DIRECTION('ref_axis',(0.15160090640473,0.,0.988441786438263));
#96243=DIRECTION('center_axis',(-0.981627005099017,0.,-0.190809912898503));
#96244=DIRECTION('ref_axis',(-0.190809912898503,0.,0.981627005099017));
#96245=DIRECTION('center_axis',(-0.981627005099017,1.00555860127894E-16,
-0.190809912898504));
#96246=DIRECTION('ref_axis',(-0.1841964898643,-0.260994622906685,0.947604062852977));
#96247=DIRECTION('center_axis',(-0.981627005099017,1.92601865239559E-16,
-0.190809912898504));
#96248=DIRECTION('ref_axis',(-0.184481134488586,-0.255413068037693,0.949068425190395));
#96249=DIRECTION('center_axis',(0.,-1.,0.));
#96250=DIRECTION('ref_axis',(0.,0.,-1.));
#96251=DIRECTION('',(-0.190809912898503,0.,0.981627005099017));
#96252=DIRECTION('center_axis',(0.,-1.,0.));
#96253=DIRECTION('ref_axis',(0.126677774296384,0.,0.991943920541537));
#96254=DIRECTION('',(-0.190809912898503,0.,0.981627005099017));
#96255=DIRECTION('center_axis',(0.,-1.,0.));
#96256=DIRECTION('ref_axis',(0.120056982034697,0.,0.992767002405258));
#96257=DIRECTION('center_axis',(0.981627005099017,0.,0.190809912898503));
#96258=DIRECTION('ref_axis',(0.,-1.,0.));
#96259=DIRECTION('',(-0.190809912898503,0.,0.981627005099017));
#96260=DIRECTION('center_axis',(0.981627005099017,0.,0.190809912898503));
#96261=DIRECTION('ref_axis',(-0.1859589704051,-0.224052422420893,0.956671193949732));
#96262=DIRECTION('center_axis',(0.981627005099017,-1.56990815882154E-16,
0.190809912898504));
#96263=DIRECTION('ref_axis',(-0.186162251270113,-0.219366829807895,0.957716978121448));
#96264=DIRECTION('center_axis',(0.,1.,0.));
#96265=DIRECTION('ref_axis',(1.,0.,0.));
#96266=DIRECTION('',(-0.190809912898503,0.,0.981627005099017));
#96267=DIRECTION('center_axis',(0.,1.,0.));
#96268=DIRECTION('ref_axis',(0.0896762875991086,0.,0.995970965160351));
#96269=DIRECTION('center_axis',(0.,1.,0.));
#96270=DIRECTION('ref_axis',(0.0839371904866857,0.,0.996471047272926));
#96271=DIRECTION('center_axis',(-0.981627005099017,0.,-0.190809912898503));
#96272=DIRECTION('ref_axis',(-0.190809912898503,0.,0.981627005099017));
#96273=DIRECTION('center_axis',(-0.981627005099017,-6.41908343804613E-17,
-0.190809912898503));
#96274=DIRECTION('ref_axis',(-0.184482115855883,-0.25539359847171,0.949073473862276));
#96275=DIRECTION('center_axis',(-0.981627005099017,6.15853067906846E-17,
-0.190809912898503));
#96276=DIRECTION('ref_axis',(-0.184743183521159,-0.250156649499107,0.950416543865819));
#96277=DIRECTION('center_axis',(0.,-1.,0.));
#96278=DIRECTION('ref_axis',(0.,0.,-1.));
#96279=DIRECTION('',(-0.190809912898503,0.,0.981627005099017));
#96280=DIRECTION('center_axis',(0.,-1.,0.));
#96281=DIRECTION('ref_axis',(0.057455673972295,0.,0.998348058308519));
#96282=DIRECTION('',(-0.190809912898503,0.,0.981627005099017));
#96283=DIRECTION('center_axis',(0.,-1.,0.));
#96284=DIRECTION('ref_axis',(0.0523145803672791,0.,0.998630654787342));
#96285=DIRECTION('center_axis',(0.981627005099017,0.,0.190809912898503));
#96286=DIRECTION('ref_axis',(0.,-1.,0.));
#96287=DIRECTION('',(-0.190809912898503,0.,0.981627005099017));
#96288=DIRECTION('center_axis',(0.981627005099017,-1.02481602251098E-16,
0.190809912898504));
#96289=DIRECTION('ref_axis',(-0.186142071902388,-0.219836656826109,0.957613164792238));
#96290=DIRECTION('center_axis',(0.981627005099017,3.78430184869551E-17,
0.190809912898503));
#96291=DIRECTION('ref_axis',(-0.186330592575348,-0.215405464478295,0.958583014737592));
#96292=DIRECTION('center_axis',(0.,1.,0.));
#96293=DIRECTION('ref_axis',(1.,0.,0.));
#96294=DIRECTION('',(-0.190809912898503,0.,0.981627005099017));
#96295=DIRECTION('center_axis',(0.,1.,0.));
#96296=DIRECTION('ref_axis',(0.0214917304669384,0.,0.999769026086294));
#96297=DIRECTION('center_axis',(0.,1.,0.));
#96298=DIRECTION('ref_axis',(0.0171769281236512,0.,0.999852465686931));
#96299=DIRECTION('center_axis',(-0.981627005099017,0.,-0.190809912898503));
#96300=DIRECTION('ref_axis',(-0.190809912898503,0.,0.981627005099017));
#96301=DIRECTION('center_axis',(-0.981627005099017,0.,-0.190809912898503));
#96302=DIRECTION('ref_axis',(-0.184690180329235,-0.251229314473896,0.950143867442679));
#96303=DIRECTION('center_axis',(-0.981627005099017,1.41720243526492E-16,
-0.190809912898504));
#96304=DIRECTION('ref_axis',(-0.184934689487586,-0.246239451375998,0.951401751738022));
#96305=DIRECTION('center_axis',(0.,-1.,0.));
#96306=DIRECTION('ref_axis',(0.,0.,-1.));
#96307=DIRECTION('',(-0.190809912898503,0.,0.981627005099017));
#96308=DIRECTION('center_axis',(0.,-1.,0.));
#96309=DIRECTION('ref_axis',(-0.0108312859749144,0.,0.999941339901561));
#96310=DIRECTION('',(-0.190809912898503,0.,0.981627005099017));
#96311=DIRECTION('center_axis',(0.,-1.,0.));
#96312=DIRECTION('ref_axis',(-0.0145336816644732,0.,0.999894380470895));
#96313=DIRECTION('center_axis',(0.981627005099017,0.,0.190809912898503));
#96314=DIRECTION('ref_axis',(0.,-1.,0.));
#96315=DIRECTION('',(-0.190809912898503,0.,0.981627005099017));
#96316=DIRECTION('center_axis',(0.981627005099017,-7.66548341238665E-18,
0.190809912898503));
#96317=DIRECTION('ref_axis',(-0.186272558126613,-0.216779698406492,0.958284454871182));
#96318=DIRECTION('center_axis',(0.981627005099017,0.,0.190809912898503));
#96319=DIRECTION('ref_axis',(-0.186450886145693,-0.212527275133194,0.959201868419753));
#96320=DIRECTION('center_axis',(0.,1.,0.));
#96321=DIRECTION('ref_axis',(1.,0.,0.));
#96322=DIRECTION('',(-0.190809912898503,0.,0.981627005099017));
#96323=DIRECTION('center_axis',(0.,1.,0.));
#96324=DIRECTION('ref_axis',(-0.0457955137113147,0.,0.998950835088453));
#96325=DIRECTION('center_axis',(0.,1.,0.));
#96326=DIRECTION('ref_axis',(-0.0487238586301981,0.,0.998812287469565));
#96327=DIRECTION('center_axis',(-0.981627005099017,0.,-0.190809912898503));
#96328=DIRECTION('ref_axis',(-0.190809912898503,0.,0.981627005099017));
#96329=DIRECTION('center_axis',(-0.981627005099017,-2.27558651128372E-17,
-0.190809912898503));
#96330=DIRECTION('ref_axis',(-0.184833575911802,-0.248315905441003,0.950881570081507));
#96331=DIRECTION('center_axis',(-0.981627005099017,1.3128444595013E-16,
-0.190809912898504));
#96332=DIRECTION('ref_axis',(-0.185066976672435,-0.243494342879606,0.95208230690994));
#96333=DIRECTION('center_axis',(0.,-1.,0.));
#96334=DIRECTION('ref_axis',(0.,0.,-1.));
#96335=DIRECTION('',(-0.190809912898503,0.,0.981627005099017));
#96336=DIRECTION('center_axis',(0.,-1.,0.));
#96337=DIRECTION('ref_axis',(-0.0782243178778391,0.,0.996935783334386));
#96338=DIRECTION('',(-0.190809912898503,0.,0.981627005099017));
#96339=DIRECTION('center_axis',(0.,-1.,0.));
#96340=DIRECTION('ref_axis',(-0.0805255845251147,0.,0.996752542127126));
#96341=DIRECTION('center_axis',(0.981627005099017,0.,0.190809912898503));
#96342=DIRECTION('ref_axis',(0.,-1.,0.));
#96343=DIRECTION('',(-0.190809912898503,0.,0.981627005099017));
#96344=DIRECTION('center_axis',(0.981627005099017,-1.50452980269455E-16,
0.190809912898504));
#96345=DIRECTION('ref_axis',(-0.186358114771361,-0.214750524536794,0.958724603455047));
#96346=DIRECTION('center_axis',(0.981627005099017,2.89425911527956E-17,
0.190809912898503));
#96347=DIRECTION('ref_axis',(-0.186529907529078,-0.210614148632799,0.959608396166308));
#96348=DIRECTION('center_axis',(0.,1.,0.));
#96349=DIRECTION('ref_axis',(1.,0.,0.));
#96350=DIRECTION('',(-0.190809912898503,0.,0.981627005099017));
#96351=DIRECTION('center_axis',(0.,1.,0.));
#96352=DIRECTION('ref_axis',(-0.11221795040211,0.,0.993683617459576));
#96353=DIRECTION('center_axis',(0.,1.,0.));
#96354=DIRECTION('ref_axis',(-0.113795052586422,0.,0.993504245590754));
#96355=DIRECTION('center_axis',(-0.981627005099017,0.,-0.190809912898503));
#96356=DIRECTION('ref_axis',(-0.190809912898503,0.,0.981627005099017));
#96357=DIRECTION('center_axis',(-0.981627005099017,1.57011489457449E-16,
-0.190809912898504));
#96358=DIRECTION('ref_axis',(-0.184920463723457,-0.246532715705106,0.951328566891254));
#96359=DIRECTION('center_axis',(-0.981627005099017,-1.00704279750265E-16,
-0.190809912898503));
#96360=DIRECTION('ref_axis',(-0.185147254406488,-0.241812327014693,0.95249529798812));
#96361=DIRECTION('center_axis',(0.,-1.,0.));
#96362=DIRECTION('ref_axis',(0.,0.,-1.));
#96363=DIRECTION('',(-0.190809912898503,0.,0.981627005099017));
#96364=DIRECTION('center_axis',(0.,-1.,0.));
#96365=DIRECTION('ref_axis',(-0.144750026222805,0.,0.989468256139881));
#96366=DIRECTION('',(-0.190809912898503,0.,0.981627005099017));
#96367=DIRECTION('center_axis',(0.,-1.,0.));
#96368=DIRECTION('ref_axis',(-0.145685581668177,0.,0.989330941239586));
#96369=DIRECTION('center_axis',(0.981627005099017,0.,0.190809912898503));
#96370=DIRECTION('ref_axis',(0.,-1.,0.));
#96371=DIRECTION('',(-0.190809912898503,-1.011721224396E-14,0.981627005099017));
#96372=DIRECTION('center_axis',(0.981627005099017,-8.93635241303609E-17,
0.190809912898504));
#96373=DIRECTION('ref_axis',(-0.186403435751544,-0.213667443730199,0.958957758522148));
#96374=DIRECTION('center_axis',(0.981627005099017,-8.59871682154991E-17,
0.190809912898504));
#96375=DIRECTION('ref_axis',(-0.186571814196846,-0.209592160278304,0.959823986206414));
#96376=DIRECTION('center_axis',(0.,1.,0.));
#96377=DIRECTION('ref_axis',(1.,0.,0.));
#96378=DIRECTION('',(-0.190809912898503,1.157372297933E-14,0.981627005099017));
#96379=DIRECTION('center_axis',(0.,1.,0.));
#96380=DIRECTION('ref_axis',(-0.177795049856396,0.,0.984067538457885));
#96381=DIRECTION('center_axis',(0.,1.,0.));
#96382=DIRECTION('ref_axis',(-0.178054589517587,0.,0.98402061114172));
#96383=DIRECTION('center_axis',(-0.981627005099017,0.,-0.190809912898503));
#96384=DIRECTION('ref_axis',(-0.190809912898503,0.,0.981627005099017));
#96385=DIRECTION('center_axis',(-0.981627005099017,2.22988138811507E-16,
-0.190809912898504));
#96386=DIRECTION('ref_axis',(-0.184955510912788,-0.245809545816807,0.951508868150121));
#96387=DIRECTION('center_axis',(-0.981627005099017,1.21594431566126E-16,
-0.190809912898504));
#96388=DIRECTION('ref_axis',(-0.185179661199109,-0.241129792878107,0.952662015651272));
#96389=DIRECTION('center_axis',(0.,-1.,0.));
#96390=DIRECTION('ref_axis',(0.,0.,-1.));
#96391=DIRECTION('',(-0.190809912898503,0.,0.981627005099017));
#96392=DIRECTION('center_axis',(0.,-1.,0.));
#96393=DIRECTION('ref_axis',(-0.210422369826518,0.,0.977610569847008));
#96394=DIRECTION('',(-0.190809912898503,0.,0.981627005099017));
#96395=DIRECTION('center_axis',(0.,-1.,0.));
#96396=DIRECTION('ref_axis',(-0.210026523774284,0.,0.977695688499898));
#96397=DIRECTION('center_axis',(0.981627005099017,0.,0.190809912898503));
#96398=DIRECTION('ref_axis',(0.,-1.,0.));
#96399=DIRECTION('',(-0.190809912898503,0.,0.981627005099017));
#96400=DIRECTION('center_axis',(0.981627005099017,-2.30469295235825E-16,
0.190809912898504));
#96401=DIRECTION('ref_axis',(-0.1864108996742,-0.213488518578295,0.958996156883801));
#96402=DIRECTION('center_axis',(0.981627005099017,-1.35927024749058E-16,
0.190809912898504));
#96403=DIRECTION('ref_axis',(-0.186578718977024,-0.209423271015703,0.959859508043743));
#96404=DIRECTION('center_axis',(0.,1.,0.));
#96405=DIRECTION('ref_axis',(1.,0.,0.));
#96406=DIRECTION('',(-0.190809912898503,1.155879430164E-14,0.981627005099017));
#96407=DIRECTION('center_axis',(0.,1.,0.));
#96408=DIRECTION('ref_axis',(-0.242534617261097,0.,0.970142752088585));
#96409=DIRECTION('center_axis',(0.,1.,0.));
#96410=DIRECTION('ref_axis',(-0.241509667213401,0.,0.970398413355294));
#96411=DIRECTION('center_axis',(-0.981627005099017,0.,-0.190809912898503));
#96412=DIRECTION('ref_axis',(-0.190809912898503,0.,0.981627005099017));
#96413=DIRECTION('center_axis',(-0.981627005099017,-1.49032924732936E-17,
-0.190809912898503));
#96414=DIRECTION('ref_axis',(-0.184940541908074,-0.246118695637908,0.951431859681103));
#96415=DIRECTION('center_axis',(-0.981627005099017,3.58496787124456E-17,
-0.190809912898503));
#96416=DIRECTION('ref_axis',(-0.185165818114719,-0.241421599051094,0.952590799511269));
#96417=DIRECTION('center_axis',(0.,-1.,0.));
#96418=DIRECTION('ref_axis',(0.,0.,-1.));
#96419=DIRECTION('',(-0.190809912898503,0.,0.981627005099017));
#96420=DIRECTION('center_axis',(0.,-1.,0.));
#96421=DIRECTION('ref_axis',(-0.275243638658276,0.,0.961374505267407));
#96422=DIRECTION('',(-0.190809912898503,0.,0.981627005099017));
#96423=DIRECTION('center_axis',(0.,-1.,0.));
#96424=DIRECTION('ref_axis',(-0.273550520375017,0.,0.961857636452795));
#96425=DIRECTION('center_axis',(0.981627005099017,0.,0.190809912898503));
#96426=DIRECTION('ref_axis',(0.,-1.,0.));
#96427=DIRECTION('',(-0.190809912898503,0.,0.981627005099017));
#96428=DIRECTION('center_axis',(0.981627005099017,-7.48461333200017E-17,
0.190809912898504));
#96429=DIRECTION('ref_axis',(-0.186380891213921,-0.214206930543801,0.958841777509359));
#96430=DIRECTION('center_axis',(0.981627005099017,-8.64054264038154E-17,
0.190809912898504));
#96431=DIRECTION('ref_axis',(-0.186550963960731,-0.210101290270208,0.959716721575755));
#96432=DIRECTION('center_axis',(0.,1.,0.));
#96433=DIRECTION('ref_axis',(1.,0.,0.));
#96434=DIRECTION('',(-0.190809912898503,0.,0.981627005099017));
#96435=DIRECTION('center_axis',(0.,1.,0.));
#96436=DIRECTION('ref_axis',(-0.306433322347889,0.,0.95189212569221));
#96437=DIRECTION('center_axis',(0.,1.,0.));
#96438=DIRECTION('ref_axis',(-0.304157214022129,0.,0.952621850031951));
#96439=DIRECTION('center_axis',(-0.981627005099017,0.,-0.190809912898503));
#96440=DIRECTION('ref_axis',(-0.190809912898503,0.,0.981627005099017));
#96441=DIRECTION('center_axis',(-0.981627005099017,-6.78043411373776E-17,
-0.190809912898503));
#96442=DIRECTION('ref_axis',(-0.184874781530203,-0.247471953044298,0.951093553553277));
#96443=DIRECTION('center_axis',(-0.981627005099017,-7.97057587953209E-17,
-0.190809912898503));
#96444=DIRECTION('ref_axis',(-0.185105036150056,-0.242698447428403,0.952278104971299));
#96445=DIRECTION('center_axis',(0.,-1.,0.));
#96446=DIRECTION('ref_axis',(0.,0.,-1.));
#96447=DIRECTION('',(-0.190809912898503,0.,0.981627005099017));
#96448=DIRECTION('center_axis',(0.,-1.,0.));
#96449=DIRECTION('ref_axis',(-0.339204610666547,0.,0.940712619295902));
#96450=DIRECTION('',(-0.190809912898503,0.,0.981627005099017));
#96451=DIRECTION('center_axis',(0.,-1.,0.));
#96452=DIRECTION('ref_axis',(-0.336249078397679,0.,0.941773092245001));
#96453=DIRECTION('center_axis',(0.981627005099017,0.,0.190809912898503));
#96454=DIRECTION('ref_axis',(0.,-1.,0.));
#96455=DIRECTION('',(-0.190809912898503,0.,0.981627005099017));
#96456=DIRECTION('center_axis',(0.981627005099017,-9.87985964490018E-17,
0.190809912898504));
#96457=DIRECTION('ref_axis',(-0.186311851707565,-0.215850244521505,0.958486601812099));
#96458=DIRECTION('center_axis',(0.981627005099017,-1.68062871373652E-16,
0.190809912898504));
#96459=DIRECTION('ref_axis',(-0.18648716372044,-0.211651234172008,0.959388499431263));
#96460=DIRECTION('center_axis',(0.,1.,0.));
#96461=DIRECTION('ref_axis',(1.,0.,0.));
#96462=DIRECTION('',(-0.190809912898503,0.,0.981627005099017));
#96463=DIRECTION('center_axis',(0.,1.,0.));
#96464=DIRECTION('ref_axis',(-0.369476474789942,0.,0.929240084465149));
#96465=DIRECTION('center_axis',(0.,1.,0.));
#96466=DIRECTION('ref_axis',(-0.365983690060656,0.,0.930621264859978));
#96467=DIRECTION('center_axis',(-0.981627005099017,0.,-0.190809912898503));
#96468=DIRECTION('ref_axis',(-0.190809912898503,0.,0.981627005099017));
#96469=DIRECTION('center_axis',(-0.981627005099017,-3.0734879996357E-17,
-0.190809912898503));
#96470=DIRECTION('ref_axis',(-0.184754752492854,-0.249921866464486,0.950476060768609));
#96471=DIRECTION('center_axis',(-0.981627005099017,-5.16917894804207E-17,
-0.190809912898503));
#96472=DIRECTION('ref_axis',(-0.184994228744489,-0.245007993611609,0.951708053132706));
#96473=DIRECTION('center_axis',(0.,-1.,0.));
#96474=DIRECTION('ref_axis',(0.,0.,-1.));
#96475=DIRECTION('',(-0.190809912898503,0.,0.981627005099017));
#96476=DIRECTION('center_axis',(0.,-1.,0.));
#96477=DIRECTION('ref_axis',(-0.402283914344989,0.,0.915514965611854));
#96478=DIRECTION('',(-0.190809912898503,0.,0.981627005099017));
#96479=DIRECTION('center_axis',(0.,-1.,0.));
#96480=DIRECTION('ref_axis',(-0.398102539409541,0.,0.917340922512277));
#96481=DIRECTION('center_axis',(0.981627005099017,0.,0.190809912898503));
#96482=DIRECTION('ref_axis',(0.,-1.,0.));
#96483=DIRECTION('',(-0.190809912898503,0.,0.981627005099017));
#96484=DIRECTION('center_axis',(0.981627005099017,-7.00780141118461E-17,
0.190809912898504));
#96485=DIRECTION('ref_axis',(-0.18620007176826,-0.218483413292492,0.957911546746127));
#96486=DIRECTION('center_axis',(0.981627005099017,-8.97524894262478E-17,
0.190809912898504));
#96487=DIRECTION('ref_axis',(-0.186384028329845,-0.214131945224895,0.958857916491146));
#96488=DIRECTION('center_axis',(0.,1.,0.));
#96489=DIRECTION('ref_axis',(1.,0.,0.));
#96490=DIRECTION('',(-0.190809912898503,0.,0.981627005099017));
#96491=DIRECTION('center_axis',(0.,1.,0.));
#96492=DIRECTION('ref_axis',(-0.431637009093733,0.,0.902047389210022));
#96493=DIRECTION('center_axis',(0.,1.,0.));
#96494=DIRECTION('ref_axis',(-0.426964190304545,0.,0.904268533234229));
#96495=DIRECTION('center_axis',(-0.981627005099017,0.,-0.190809912898503));
#96496=DIRECTION('ref_axis',(-0.190809912898503,0.,0.981627005099017));
#96497=DIRECTION('center_axis',(-0.981627005099017,-1.5819052248506E-17,
-0.190809912898503));
#96498=DIRECTION('ref_axis',(-0.184573801204179,-0.253567578221496,0.949545151735254));
#96499=DIRECTION('center_axis',(-0.981627005099017,-7.59286715101097E-18,
-0.190809912898503));
#96500=DIRECTION('ref_axis',(-0.184827508067632,-0.248439925893398,0.950850353885191));
#96501=DIRECTION('center_axis',(0.,-1.,0.));
#96502=DIRECTION('ref_axis',(0.,0.,-1.));
#96503=DIRECTION('',(-0.190809912898503,0.,0.981627005099017));
#96504=DIRECTION('center_axis',(0.,-1.,0.));
#96505=DIRECTION('ref_axis',(-0.399311414847207,0.,0.916815354350439));
#96506=DIRECTION('',(-0.190809912898503,0.,0.981627005099017));
#96507=DIRECTION('center_axis',(0.,-1.,0.));
#96508=DIRECTION('ref_axis',(-0.395301678561444,0.,0.918551350184901));
#96509=DIRECTION('center_axis',(0.981627005099017,0.,0.190809912898503));
#96510=DIRECTION('ref_axis',(0.,-1.,0.));
#96511=DIRECTION('',(-0.190809912898491,0.,0.981627005099019));
#96512=DIRECTION('center_axis',(0.981627005099017,7.78644601242735E-18,
0.190809912898503));
#96513=DIRECTION('ref_axis',(-0.188584680032072,-0.152276318355394,0.970179231547103));
#96514=DIRECTION('center_axis',(0.981627005099017,-1.00971550604529E-16,
0.190809912898504));
#96515=DIRECTION('ref_axis',(-0.188672933012422,-0.149243476974994,0.970633251505894));
#96516=DIRECTION('center_axis',(0.,1.,0.));
#96517=DIRECTION('ref_axis',(1.,0.,0.));
#96518=DIRECTION('',(-0.190809912898503,0.,0.981627005099017));
#96519=DIRECTION('center_axis',(0.,1.,0.));
#96520=DIRECTION('ref_axis',(-0.428810013970232,0.,0.903394693320062));
#96521=DIRECTION('center_axis',(0.,1.,0.));
#96522=DIRECTION('ref_axis',(-0.424297924716844,0.,0.90552265078295));
#96523=DIRECTION('center_axis',(-0.981627005099017,0.,-0.190809912898503));
#96524=DIRECTION('ref_axis',(-0.190809912898503,0.,0.981627005099017));
#96525=DIRECTION('center_axis',(-0.981627005099017,1.14688128801668E-16,
-0.190809912898504));
#96526=DIRECTION('ref_axis',(-0.187449845094609,-0.186839268163196,0.964341041046293));
#96527=DIRECTION('center_axis',(-0.981627005099017,1.25282307991681E-16,
-0.190809912898504));
#96528=DIRECTION('ref_axis',(-0.187585522425224,-0.183060998026701,0.965039036919193));
#96529=DIRECTION('center_axis',(0.,-1.,0.));
#96530=DIRECTION('ref_axis',(0.,0.,-1.));
#96531=DIRECTION('',(-0.190809912898503,0.,0.981627005099017));
#96532=DIRECTION('center_axis',(0.,-1.,0.));
#96533=DIRECTION('ref_axis',(-0.397312743751599,0.,0.91768326979006));
#96534=DIRECTION('',(-0.190809912898503,0.,0.981627005099017));
#96535=DIRECTION('center_axis',(0.,-1.,0.));
#96536=DIRECTION('ref_axis',(-0.393415793973014,0.,0.919360654505392));
#96537=DIRECTION('center_axis',(0.981627005099017,0.,0.190809912898503));
#96538=DIRECTION('ref_axis',(0.,-1.,0.));
#96539=DIRECTION('',(-0.190809912898503,0.,0.981627005099017));
#96540=DIRECTION('center_axis',(0.981627005099017,-6.42381796025256E-17,
0.190809912898504));
#96541=DIRECTION('ref_axis',(-0.190101847692576,-0.0860692234182736,0.97798434357818));
#96542=DIRECTION('center_axis',(0.981627005099017,-7.66635847182533E-17,
0.190809912898504));
#96543=DIRECTION('ref_axis',(-0.190129821407186,-0.0843550087249674,0.978128255145859));
#96544=DIRECTION('center_axis',(0.,1.,0.));
#96545=DIRECTION('ref_axis',(1.,0.,0.));
#96546=DIRECTION('',(-0.190809912898503,0.,0.981627005099017));
#96547=DIRECTION('center_axis',(0.,1.,0.));
#96548=DIRECTION('ref_axis',(-0.427044757829044,0.,0.904230487658281));
#96549=DIRECTION('center_axis',(0.,1.,0.));
#96550=DIRECTION('ref_axis',(-0.422631180074548,0.,0.906301763006558));
#96551=DIRECTION('center_axis',(-0.981627005099017,0.,-0.190809912898503));
#96552=DIRECTION('ref_axis',(-0.190809912898503,0.,0.981627005099017));
#96553=DIRECTION('center_axis',(-0.981627005099017,4.35023936833914E-17,
-0.190809912898504));
#96554=DIRECTION('ref_axis',(-0.189428539477533,-0.120110958104898,0.974520490382081));
#96555=DIRECTION('center_axis',(-0.981627005099017,1.48060909444714E-16,
-0.190809912898504));
#96556=DIRECTION('ref_axis',(-0.18948403646947,-0.117682070159998,0.974805996230067));
#96557=DIRECTION('center_axis',(0.981627005099017,0.,0.190809912898503));
#96558=DIRECTION('ref_axis',(0.,-1.,0.));
#96559=DIRECTION('',(-0.190809912898503,0.,0.981627005099017));
#96560=DIRECTION('center_axis',(0.981627005099017,-1.45995862733013E-17,
0.190809912898504));
#96561=DIRECTION('ref_axis',(-0.190772271534679,-0.0198621284811394,0.981433358035938));
#96562=DIRECTION('',(-0.190809912898492,0.,0.981627005099019));
#96563=DIRECTION('center_axis',(0.981627005099017,-5.60953058914049E-18,
0.190809912898504));
#96564=DIRECTION('ref_axis',(-0.190773756127288,-0.0194665404749907,0.981440995564696));
#96565=DIRECTION('center_axis',(0.,1.,0.));
#96566=DIRECTION('ref_axis',(1.,0.,0.));
#96567=DIRECTION('',(-0.190809912898503,0.,0.981627005099017));
#96568=DIRECTION('center_axis',(0.,1.,0.));
#96569=DIRECTION('ref_axis',(-0.426272800182109,0.,0.904594660510941));
#96570=DIRECTION('center_axis',(0.,1.,0.));
#96571=DIRECTION('ref_axis',(-0.42190185736574,0.,0.906641507295656));
#96572=DIRECTION('center_axis',(-0.981627005099017,0.,-0.190809912898503));
#96573=DIRECTION('ref_axis',(-0.190809912898503,0.,0.981627005099017));
#96574=DIRECTION('',(-0.190809912898503,0.,0.981627005099017));
#96575=DIRECTION('center_axis',(-0.981627005099017,2.17511968416957E-17,
-0.190809912898504));
#96576=DIRECTION('ref_axis',(-0.190537842747197,-0.053382648046619,0.980227332494241));
#96577=DIRECTION('center_axis',(-0.981627005099017,4.36589861183131E-17,
-0.190809912898504));
#96578=DIRECTION('ref_axis',(-0.190548742578238,-0.0523031422933503,0.980283406983967));
#96579=DIRECTION('center_axis',(0.,-1.,0.));
#96580=DIRECTION('ref_axis',(0.,0.,-1.));
#96581=DIRECTION('center_axis',(0.,-1.,0.));
#96582=DIRECTION('ref_axis',(-0.396208341225175,0.,0.918160634281167));
#96583=DIRECTION('center_axis',(0.,-1.,0.));
#96584=DIRECTION('ref_axis',(-0.392372817011327,0.,0.919806268988528));
#96585=DIRECTION('center_axis',(0.,-1.,0.));
#96586=DIRECTION('ref_axis',(0.,0.,-1.));
#96587=DIRECTION('',(-0.190809912898503,0.,0.981627005099017));
#96588=DIRECTION('center_axis',(0.,-1.,0.));
#96589=DIRECTION('ref_axis',(0.117062756021325,0.,0.993124519460018));
#96590=DIRECTION('',(-0.190809912898503,0.,0.981627005099017));
#96591=DIRECTION('center_axis',(0.,-1.,0.));
#96592=DIRECTION('ref_axis',(0.111009388690272,0.,0.993819357641323));
#96593=DIRECTION('center_axis',(0.981627005099017,0.,0.190809912898503));
#96594=DIRECTION('ref_axis',(0.,-1.,0.));
#96595=DIRECTION('',(-0.190809912898503,0.,0.981627005099017));
#96596=DIRECTION('center_axis',(0.981627005099017,-1.63768969384934E-17,
0.190809912898504));
#96597=DIRECTION('ref_axis',(-0.190770327966247,-0.0203684020382603,0.981423359293052));
#96598=DIRECTION('center_axis',(0.981627005099017,4.90596299631731E-18,
0.190809912898503));
#96599=DIRECTION('ref_axis',(-0.190771966490524,-0.0199424390734504,0.981431788727643));
#96600=DIRECTION('center_axis',(0.,1.,0.));
#96601=DIRECTION('ref_axis',(1.,0.,0.));
#96602=DIRECTION('',(-0.190809912898503,0.,0.981627005099017));
#96603=DIRECTION('center_axis',(0.,1.,0.));
#96604=DIRECTION('ref_axis',(0.0830891414914541,0.,0.996542118811951));
#96605=DIRECTION('center_axis',(0.,1.,0.));
#96606=DIRECTION('ref_axis',(0.0777343797762107,0.,0.996974105080372));
#96607=DIRECTION('center_axis',(-0.981627005099017,0.,-0.190809912898503));
#96608=DIRECTION('ref_axis',(-0.190809912898503,0.,0.981627005099017));
#96609=DIRECTION('center_axis',(-0.981627005099017,-6.01789072316824E-18,
-0.190809912898503));
#96610=DIRECTION('ref_axis',(-0.190533907263313,-0.0537670733624724,0.980207086285857));
#96611=DIRECTION('center_axis',(-0.981627005099017,7.69816334883557E-18,
-0.190809912898503));
#96612=DIRECTION('ref_axis',(-0.19054511820959,-0.0526645577892776,0.980264761316734));
#96613=DIRECTION('center_axis',(0.,-1.,0.));
#96614=DIRECTION('ref_axis',(0.,0.,-1.));
#96615=DIRECTION('',(-0.190809912898503,0.,0.981627005099017));
#96616=DIRECTION('center_axis',(0.,-1.,0.));
#96617=DIRECTION('ref_axis',(0.118808142662354,0.,0.99291722980172));
#96618=DIRECTION('',(-0.190809912898503,0.,0.981627005099017));
#96619=DIRECTION('center_axis',(0.,-1.,0.));
#96620=DIRECTION('ref_axis',(0.112654187705058,0.,0.993634255645664));
#96621=DIRECTION('center_axis',(0.981627005099017,0.,0.190809912898503));
#96622=DIRECTION('ref_axis',(0.,-1.,0.));
#96623=DIRECTION('',(-0.190809912898503,0.,0.981627005099017));
#96624=DIRECTION('center_axis',(0.981627005099017,-4.91306908154802E-17,
0.190809912898504));
#96625=DIRECTION('ref_axis',(-0.190065219745899,-0.0882630754991305,0.977795910068342));
#96626=DIRECTION('center_axis',(0.981627005099017,-1.96238519852693E-18,
0.190809912898503));
#96627=DIRECTION('ref_axis',(-0.190096099358061,-0.086417235984943,0.977954771108344));
#96628=DIRECTION('center_axis',(0.,1.,0.));
#96629=DIRECTION('ref_axis',(1.,0.,0.));
#96630=DIRECTION('',(-0.190809912898503,0.,0.981627005099017));
#96631=DIRECTION('center_axis',(0.,1.,0.));
#96632=DIRECTION('ref_axis',(0.0840360319589374,0.,0.996462716478944));
#96633=DIRECTION('center_axis',(0.,1.,0.));
#96634=DIRECTION('ref_axis',(0.0786270725857584,0.,0.996904099428122));
#96635=DIRECTION('center_axis',(-0.981627005099017,0.,-0.190809912898503));
#96636=DIRECTION('ref_axis',(-0.190809912898503,0.,0.981627005099017));
#96637=DIRECTION('center_axis',(-0.981627005099017,-2.00596357438942E-17,
-0.190809912898503));
#96638=DIRECTION('ref_axis',(-0.18940849856482,-0.120975915065594,0.974417389338605));
#96639=DIRECTION('center_axis',(-0.981627005099017,-6.54343884651024E-17,
-0.190809912898503));
#96640=DIRECTION('ref_axis',(-0.189465584281205,-0.118495255025902,0.97471106842455));
#96641=DIRECTION('center_axis',(0.,-1.,0.));
#96642=DIRECTION('ref_axis',(0.,0.,-1.));
#96643=DIRECTION('',(-0.190809912898503,0.,0.981627005099017));
#96644=DIRECTION('center_axis',(0.,-1.,0.));
#96645=DIRECTION('ref_axis',(0.121969536764593,0.,0.992533844310324));
#96646=DIRECTION('',(-0.190809912898503,0.,0.981627005099017));
#96647=DIRECTION('center_axis',(0.,-1.,0.));
#96648=DIRECTION('ref_axis',(0.115630671479797,0.,0.993292277133539));
#96649=DIRECTION('center_axis',(0.981627005099017,0.,0.190809912898503));
#96650=DIRECTION('ref_axis',(0.,-1.,0.));
#96651=DIRECTION('',(-0.190809912898492,0.,0.981627005099019));
#96652=DIRECTION('center_axis',(0.981627005099017,-3.68480181116102E-17,
0.190809912898503));
#96653=DIRECTION('ref_axis',(-0.188469081383788,-0.156157748959995,0.969584531024551));
#96654=DIRECTION('center_axis',(0.981627005099017,5.10220151617E-17,0.190809912898503));
#96655=DIRECTION('ref_axis',(-0.188566541370011,-0.152892032896403,0.970085916686021));
#96656=DIRECTION('center_axis',(0.,1.,0.));
#96657=DIRECTION('ref_axis',(1.,0.,0.));
#96658=DIRECTION('',(-0.190809912898503,0.,0.981627005099017));
#96659=DIRECTION('center_axis',(0.,1.,0.));
#96660=DIRECTION('ref_axis',(0.0862026472117667,0.,0.996277623764422));
#96661=DIRECTION('center_axis',(0.,1.,0.));
#96662=DIRECTION('ref_axis',(0.08066835433569,0.,0.996740997756574));
#96663=DIRECTION('center_axis',(-0.981627005099017,0.,-0.190809912898503));
#96664=DIRECTION('ref_axis',(-0.190809912898503,0.,0.981627005099017));
#96665=DIRECTION('center_axis',(-0.981627005099017,-2.80834900414518E-17,
-0.190809912898503));
#96666=DIRECTION('ref_axis',(-0.187400835323093,-0.18818475676861,0.964088908887633));
#96667=DIRECTION('center_axis',(-0.981627005099017,-3.46417350697601E-17,
-0.190809912898503));
#96668=DIRECTION('ref_axis',(-0.187540417568304,-0.184325952262508,0.96480699370435));
#96669=DIRECTION('center_axis',(0.,-1.,0.));
#96670=DIRECTION('ref_axis',(0.,0.,-1.));
#96671=DIRECTION('',(-0.190809912898503,0.,0.981627005099017));
#96672=DIRECTION('center_axis',(0.,-1.,0.));
#96673=DIRECTION('ref_axis',(0.0537998697696712,0.,0.998551738275372));
#96674=DIRECTION('',(-0.190809912898503,0.,0.981627005099017));
#96675=DIRECTION('center_axis',(0.,-1.,0.));
#96676=DIRECTION('ref_axis',(0.0488765616770635,0.,0.998804826639633));
#96677=DIRECTION('center_axis',(0.981627005099017,0.,0.190809912898503));
#96678=DIRECTION('ref_axis',(0.,-1.,0.));
#96679=DIRECTION('',(-0.190809912898503,0.,0.981627005099017));
#96680=DIRECTION('center_axis',(0.981627005099017,-1.65547203636389E-16,
0.190809912898504));
#96681=DIRECTION('ref_axis',(-0.188556864165061,-0.153219488090906,0.970036132030864));
#96682=DIRECTION('center_axis',(0.981627005099017,-3.78430184869551E-18,
0.190809912898503));
#96683=DIRECTION('ref_axis',(-0.188647292536475,-0.150131081303099,0.970501343350652));
#96684=DIRECTION('center_axis',(0.,1.,0.));
#96685=DIRECTION('ref_axis',(1.,0.,0.));
#96686=DIRECTION('',(-0.190809912898503,0.,0.981627005099017));
#96687=DIRECTION('center_axis',(0.,1.,0.));
#96688=DIRECTION('ref_axis',(0.0188803147301753,0.,0.999821750971487));
#96689=DIRECTION('center_axis',(0.,1.,0.));
#96690=DIRECTION('ref_axis',(0.0147187447196545,0.,0.999891673409614));
#96691=DIRECTION('center_axis',(-0.981627005099017,0.,-0.190809912898503));
#96692=DIRECTION('ref_axis',(-0.190809912898503,0.,0.981627005099017));
#96693=DIRECTION('center_axis',(-0.981627005099017,5.0468105524956E-17,
-0.190809912898504));
#96694=DIRECTION('ref_axis',(-0.187512071361184,-0.185116336980702,0.964661165838392));
#96695=DIRECTION('center_axis',(-0.981627005099017,3.35653208352217E-17,
-0.190809912898503));
#96696=DIRECTION('ref_axis',(-0.187642867377453,-0.181439595750803,0.965334049651287));
#96697=DIRECTION('center_axis',(0.,-1.,0.));
#96698=DIRECTION('ref_axis',(0.,0.,-1.));
#96699=DIRECTION('',(-0.190809912898503,0.,0.981627005099017));
#96700=DIRECTION('center_axis',(0.,-1.,0.));
#96701=DIRECTION('ref_axis',(-0.0134639270068732,0.,0.999909357226721));
#96702=DIRECTION('',(-0.190809912898503,0.,0.981627005099017));
#96703=DIRECTION('center_axis',(0.,-1.,0.));
#96704=DIRECTION('ref_axis',(-0.0170102071589267,0.,0.999855315959469));
#96705=DIRECTION('center_axis',(0.981627005099017,0.,0.190809912898503));
#96706=DIRECTION('ref_axis',(0.,-1.,0.));
#96707=DIRECTION('',(-0.190809912898503,0.,0.981627005099017));
#96708=DIRECTION('center_axis',(0.981627005099017,-1.149822511858E-16,0.190809912898504));
#96709=DIRECTION('ref_axis',(-0.188619449816688,-0.151088880707496,0.970358105689547));
#96710=DIRECTION('center_axis',(0.981627005099017,-6.99931092238096E-17,
0.190809912898504));
#96711=DIRECTION('ref_axis',(-0.188705019341167,-0.148125070547402,0.970798320533558));
#96712=DIRECTION('center_axis',(0.,1.,0.));
#96713=DIRECTION('ref_axis',(1.,0.,0.));
#96714=DIRECTION('',(-0.190809912898503,0.,0.981627005099017));
#96715=DIRECTION('center_axis',(0.,1.,0.));
#96716=DIRECTION('ref_axis',(-0.0475677174377644,0.,0.998868015434352));
#96717=DIRECTION('center_axis',(0.,1.,0.));
#96718=DIRECTION('ref_axis',(-0.0503925257524187,0.,0.998729489575777));
#96719=DIRECTION('center_axis',(-0.981627005099017,0.,-0.190809912898503));
#96720=DIRECTION('ref_axis',(-0.190809912898503,0.,0.981627005099017));
#96721=DIRECTION('center_axis',(-0.981627005099017,4.93043744111472E-17,
-0.190809912898503));
#96722=DIRECTION('ref_axis',(-0.187588768465847,-0.182969614535498,0.965055736267185));
#96723=DIRECTION('center_axis',(-0.981627005099017,-1.45871606611256E-17,
-0.190809912898503));
#96724=DIRECTION('ref_axis',(-0.187713666250361,-0.179416884227009,0.96569827645964));
#96725=DIRECTION('center_axis',(0.,-1.,0.));
#96726=DIRECTION('ref_axis',(0.,0.,-1.));
#96727=DIRECTION('',(-0.190809912898503,0.,0.981627005099017));
#96728=DIRECTION('center_axis',(0.,-1.,0.));
#96729=DIRECTION('ref_axis',(-0.0798606015889436,0.,0.996806041471385));
#96730=DIRECTION('',(-0.190809912898503,0.,0.981627005099017));
#96731=DIRECTION('center_axis',(0.,-1.,0.));
#96732=DIRECTION('ref_axis',(-0.0820652483437025,0.,0.996626958803687));
#96733=DIRECTION('center_axis',(0.981627005099017,0.,0.190809912898503));
#96734=DIRECTION('ref_axis',(0.,-1.,0.));
#96735=DIRECTION('',(-0.190809912898503,0.,0.981627005099017));
#96736=DIRECTION('center_axis',(0.981627005099017,-1.31646357735773E-16,
0.190809912898504));
#96737=DIRECTION('ref_axis',(-0.188660498233732,-0.149674608010496,0.97056928043448));
#96738=DIRECTION('center_axis',(0.981627005099017,-8.68277734583866E-17,
0.190809912898504));
#96739=DIRECTION('ref_axis',(-0.188742950996444,-0.146791679350195,0.97099346100924));
#96740=DIRECTION('center_axis',(0.,1.,0.));
#96741=DIRECTION('ref_axis',(1.,0.,0.));
#96742=DIRECTION('',(-0.190809912898503,0.,0.981627005099017));
#96743=DIRECTION('center_axis',(0.,1.,0.));
#96744=DIRECTION('ref_axis',(-0.113172347138354,0.,0.993575371999123));
#96745=DIRECTION('center_axis',(0.,1.,0.));
#96746=DIRECTION('ref_axis',(-0.114693920685021,0.,0.993400878073851));
#96747=DIRECTION('center_axis',(-0.981627005099017,0.,-0.190809912898503));
#96748=DIRECTION('ref_axis',(-0.190809912898503,0.,0.981627005099017));
#96749=DIRECTION('center_axis',(-0.981627005099017,1.12151063898178E-17,
-0.190809912898503));
#96750=DIRECTION('ref_axis',(-0.18763525530524,-0.181655685256397,0.965294889130035));
#96751=DIRECTION('center_axis',(-0.981627005099017,3.59658141965232E-17,
-0.190809912898503));
#96752=DIRECTION('ref_axis',(-0.187756641804466,-0.178177504116097,0.965919365415803));
#96753=DIRECTION('center_axis',(0.,-1.,0.));
#96754=DIRECTION('ref_axis',(0.,0.,-1.));
#96755=DIRECTION('',(-0.190809912898503,0.,0.981627005099017));
#96756=DIRECTION('center_axis',(0.,-1.,0.));
#96757=DIRECTION('ref_axis',(-0.145415214742479,0.,0.989370716830349));
#96758=DIRECTION('',(-0.190809912898503,-1.310547882E-14,0.981627005099017));
#96759=DIRECTION('center_axis',(0.,-1.,0.));
#96760=DIRECTION('ref_axis',(-0.146311652535326,0.,0.989238545717049));
#96761=DIRECTION('center_axis',(0.981627005099017,0.,0.190809912898503));
#96762=DIRECTION('ref_axis',(0.,-1.,0.));
#96763=DIRECTION('',(-0.190809912898503,1.170107715525E-14,0.981627005099017));
#96764=DIRECTION('center_axis',(0.981627005099017,-8.19165637861642E-17,
0.190809912898504));
#96765=DIRECTION('ref_axis',(-0.18868224637733,-0.148919733508905,0.970681164375636));
#96766=DIRECTION('center_axis',(0.981627005099017,-4.65763827833953E-17,
0.190809912898504));
#96767=DIRECTION('ref_axis',(-0.188763070362452,-0.146079384436406,0.971096965657921));
#96768=DIRECTION('center_axis',(0.,1.,0.));
#96769=DIRECTION('ref_axis',(1.,0.,0.));
#96770=DIRECTION('',(-0.190809912898503,-1.171213937656E-14,0.981627005099017));
#96771=DIRECTION('center_axis',(0.,1.,0.));
#96772=DIRECTION('ref_axis',(-0.177952104583987,0.,0.984039149868607));
#96773=DIRECTION('center_axis',(0.,1.,0.));
#96774=DIRECTION('ref_axis',(-0.178202543505702,0.,0.983993827972563));
#96775=DIRECTION('center_axis',(-0.981627005099017,0.,-0.190809912898503));
#96776=DIRECTION('ref_axis',(-0.190809912898503,0.,0.981627005099017));
#96777=DIRECTION('center_axis',(-0.981627005099017,5.2030565722685E-17,
-0.190809912898504));
#96778=DIRECTION('ref_axis',(-0.187654009224651,-0.181122823233507,0.965391369199994));
#96779=DIRECTION('center_axis',(-0.981627005099017,1.85967954159957E-16,
-0.190809912898504));
#96780=DIRECTION('ref_axis',(-0.187773992817113,-0.177674584225901,0.966008628192146));
#96781=DIRECTION('center_axis',(0.,-1.,0.));
#96782=DIRECTION('ref_axis',(0.,0.,-1.));
#96783=DIRECTION('',(-0.190809912898503,0.,0.981627005099017));
#96784=DIRECTION('center_axis',(0.,-1.,0.));
#96785=DIRECTION('ref_axis',(-0.210140930284338,0.,0.977671104932141));
#96786=DIRECTION('',(-0.190809912898503,0.,0.981627005099017));
#96787=DIRECTION('center_axis',(0.,-1.,0.));
#96788=DIRECTION('ref_axis',(-0.209761566952143,0.,0.977752568408686));
#96789=DIRECTION('center_axis',(0.981627005099017,0.,0.190809912898503));
#96790=DIRECTION('ref_axis',(0.,-1.,0.));
#96791=DIRECTION('',(-0.190809912898503,0.,0.981627005099017));
#96792=DIRECTION('center_axis',(0.981627005099017,-9.29311674338004E-17,
0.190809912898504));
#96793=DIRECTION('ref_axis',(-0.188685828350842,-0.1487950281,0.970699591939894));
#96794=DIRECTION('center_axis',(0.981627005099017,3.21932427037243E-17,
0.190809912898503));
#96795=DIRECTION('ref_axis',(-0.188766385571152,-0.145961673738203,0.971114020843045));
#96796=DIRECTION('center_axis',(0.,1.,0.));
#96797=DIRECTION('ref_axis',(1.,0.,0.));
#96798=DIRECTION('',(-0.190809912898503,0.,0.981627005099017));
#96799=DIRECTION('center_axis',(0.,1.,0.));
#96800=DIRECTION('ref_axis',(-0.241914422980073,0.,0.970297589378753));
#96801=DIRECTION('center_axis',(0.,1.,0.));
#96802=DIRECTION('ref_axis',(-0.240925262116702,0.,0.970543671389391));
#96803=DIRECTION('center_axis',(-0.981627005099017,0.,-0.190809912898503));
#96804=DIRECTION('ref_axis',(-0.190809912898503,0.,0.981627005099017));
#96805=DIRECTION('center_axis',(-0.981627005099017,-7.07906392481446E-17,
-0.190809912898503));
#96806=DIRECTION('ref_axis',(-0.187645999032811,-0.181350617838393,0.96535016054104));
#96807=DIRECTION('center_axis',(-0.981627005099017,2.22268008017162E-16,
-0.190809912898504));
#96808=DIRECTION('ref_axis',(-0.187766580876715,-0.177889599300794,0.965970497254689));
#96809=DIRECTION('center_axis',(0.,-1.,0.));
#96810=DIRECTION('ref_axis',(0.,0.,-1.));
#96811=DIRECTION('',(-0.190809912898503,0.,0.981627005099017));
#96812=DIRECTION('center_axis',(0.,-1.,0.));
#96813=DIRECTION('ref_axis',(-0.274039908751656,0.,0.961718320721501));
#96814=DIRECTION('',(-0.190809912898503,0.,0.981627005099017));
#96815=DIRECTION('center_axis',(0.,-1.,0.));
#96816=DIRECTION('ref_axis',(-0.272416986488902,0.,0.962179289671268));
#96817=DIRECTION('center_axis',(0.981627005099017,0.,0.190809912898503));
#96818=DIRECTION('ref_axis',(0.,-1.,0.));
#96819=DIRECTION('',(-0.190809912898503,0.,0.981627005099017));
#96820=DIRECTION('center_axis',(0.981627005099017,5.61345999900013E-17,
0.190809912898503));
#96821=DIRECTION('ref_axis',(-0.18867142759988,-0.149295739469903,0.97062550686841));
#96822=DIRECTION('center_axis',(0.981627005099017,-7.56047481033385E-17,
0.190809912898504));
#96823=DIRECTION('ref_axis',(-0.18875305987975,-0.146434232612596,0.971045466445929));
#96824=DIRECTION('center_axis',(0.,1.,0.));
#96825=DIRECTION('ref_axis',(1.,0.,0.));
#96826=DIRECTION('',(-0.190809912898503,0.,0.981627005099017));
#96827=DIRECTION('center_axis',(0.,1.,0.));
#96828=DIRECTION('ref_axis',(-0.305056130431757,0.,0.952334372626549));
#96829=DIRECTION('center_axis',(0.,1.,0.));
#96830=DIRECTION('ref_axis',(-0.30285914535448,0.,0.953035328870422));
#96831=DIRECTION('center_axis',(-0.981627005099017,0.,-0.190809912898503));
#96832=DIRECTION('ref_axis',(-0.190809912898503,0.,0.981627005099017));
#96833=DIRECTION('center_axis',(-0.981627005099017,9.04057881831701E-17,
-0.190809912898504));
#96834=DIRECTION('ref_axis',(-0.187610813066133,-0.18234775487471,0.965169145338172));
#96835=DIRECTION('center_axis',(-0.981627005099017,7.24597807230189E-17,
-0.190809912898504));
#96836=DIRECTION('ref_axis',(-0.187734039758534,-0.178830434947303,0.965803088549886));
#96837=DIRECTION('center_axis',(0.,-1.,0.));
#96838=DIRECTION('ref_axis',(0.,0.,-1.));
#96839=DIRECTION('',(-0.190809912898503,0.,0.981627005099017));
#96840=DIRECTION('center_axis',(0.,-1.,0.));
#96841=DIRECTION('ref_axis',(-0.337103451036581,0.,0.941467611391506));
#96842=DIRECTION('',(-0.190809912898503,0.,0.981627005099017));
#96843=DIRECTION('center_axis',(0.,-1.,0.));
#96844=DIRECTION('ref_axis',(-0.334269881053193,0.,0.942477398466766));
#96845=DIRECTION('center_axis',(0.981627005099017,0.,0.190809912898503));
#96846=DIRECTION('ref_axis',(0.,-1.,0.));
#96847=DIRECTION('',(-0.190809912898503,0.,0.981627005099017));
#96848=DIRECTION('center_axis',(0.981627005099017,-1.40598002638964E-16,
0.190809912898504));
#96849=DIRECTION('ref_axis',(-0.188638300882477,-0.150441079515,0.9704550855318));
#96850=DIRECTION('center_axis',(0.981627005099017,-8.03778950047904E-17,
0.190809912898504));
#96851=DIRECTION('ref_axis',(-0.188722432166707,-0.147514496544108,0.970887901308087));
#96852=DIRECTION('center_axis',(0.,1.,0.));
#96853=DIRECTION('ref_axis',(1.,0.,0.));
#96854=DIRECTION('',(-0.190809912898503,0.,0.981627005099017));
#96855=DIRECTION('center_axis',(0.,1.,0.));
#96856=DIRECTION('ref_axis',(-0.367363241275728,0.,0.930077549970641));
#96857=DIRECTION('center_axis',(0.,1.,0.));
#96858=DIRECTION('ref_axis',(-0.363991277767333,0.,0.931402356508348));
#96859=DIRECTION('center_axis',(-0.981627005099017,0.,-0.190809912898503));
#96860=DIRECTION('ref_axis',(-0.190809912898503,0.,0.981627005099017));
#96861=DIRECTION('center_axis',(-0.981627005099017,1.15255799986339E-17,
-0.190809912898503));
#96862=DIRECTION('ref_axis',(-0.187546605187899,-0.18415295423699,0.964838826088733));
#96863=DIRECTION('center_axis',(-0.981627005099017,1.69844451149954E-16,
-0.190809912898504));
#96864=DIRECTION('ref_axis',(-0.187674729274892,-0.180532205819094,0.965497964085729));
#96865=DIRECTION('center_axis',(0.,-1.,0.));
#96866=DIRECTION('ref_axis',(0.,0.,-1.));
#96867=DIRECTION('',(-0.190809912898503,0.,0.981627005099017));
#96868=DIRECTION('center_axis',(0.,-1.,0.));
#96869=DIRECTION('ref_axis',(-0.335690934126128,0.,0.941972184698427));
#96870=DIRECTION('',(-0.190809912898503,0.,0.981627005099017));
#96871=DIRECTION('center_axis',(0.,-1.,0.));
#96872=DIRECTION('ref_axis',(-0.332937485198635,0.,0.94294890155809));
#96873=DIRECTION('center_axis',(0.981627005099017,0.,0.190809912898503));
#96874=DIRECTION('ref_axis',(0.,-1.,0.));
#96875=DIRECTION('',(-0.190809912898503,0.,0.981627005099017));
#96876=DIRECTION('center_axis',(0.981627005099017,5.69991902590395E-18,
0.190809912898503));
#96877=DIRECTION('ref_axis',(-0.190118842925705,-0.0850319145084515,0.978071776036717));
#96878=DIRECTION('center_axis',(0.981627005099017,-3.65354068203592E-17,
0.190809912898504));
#96879=DIRECTION('ref_axis',(-0.190145515174684,-0.0833777589162615,0.978208992177569));
#96880=DIRECTION('center_axis',(0.,1.,0.));
#96881=DIRECTION('ref_axis',(1.,0.,0.));
#96882=DIRECTION('',(-0.190809912898503,0.,0.981627005099017));
#96883=DIRECTION('center_axis',(0.,1.,0.));
#96884=DIRECTION('ref_axis',(-0.366043901565332,0.,0.930597583344611));
#96885=DIRECTION('center_axis',(0.,1.,0.));
#96886=DIRECTION('ref_axis',(-0.362745971285859,0.,0.93188806211684));
#96887=DIRECTION('center_axis',(-0.981627005099017,0.,-0.190809912898503));
#96888=DIRECTION('ref_axis',(-0.190809912898503,0.,0.981627005099017));
#96889=DIRECTION('center_axis',(-0.981627005099017,5.76278999931694E-17,
-0.190809912898504));
#96890=DIRECTION('ref_axis',(-0.189468115451484,-0.118384042009503,0.974724090101786));
#96891=DIRECTION('center_axis',(-0.981627005099017,3.69227067717291E-18,
-0.190809912898503));
#96892=DIRECTION('ref_axis',(-0.189520538352024,-0.116056418026502,0.974993781199458));
#96893=DIRECTION('center_axis',(0.,-1.,0.));
#96894=DIRECTION('ref_axis',(0.,0.,-1.));
#96895=DIRECTION('',(-0.190809912898503,0.,0.981627005099017));
#96896=DIRECTION('center_axis',(0.,-1.,0.));
#96897=DIRECTION('ref_axis',(-0.334910516764006,0.,0.942249938052992));
#96898=DIRECTION('',(-0.190809912898503,0.,0.981627005099017));
#96899=DIRECTION('center_axis',(0.,-1.,0.));
#96900=DIRECTION('ref_axis',(-0.33220069566279,0.,0.94320872440895));
#96901=DIRECTION('center_axis',(0.981627005099017,0.,0.190809912898503));
#96902=DIRECTION('ref_axis',(0.,-1.,0.));
#96903=DIRECTION('',(-0.190809912898503,0.,0.981627005099017));
#96904=DIRECTION('center_axis',(0.981627005099017,-7.5998920345386E-18,
0.190809912898504));
#96905=DIRECTION('ref_axis',(-0.190773173463789,-0.0196227495019493,0.98143799803581));
#96906=DIRECTION('center_axis',(0.981627005099017,-9.59054429034431E-18,
0.190809912898504));
#96907=DIRECTION('ref_axis',(-0.190774589101592,-0.0192410212883709,0.981445280824611));
#96908=DIRECTION('center_axis',(0.,1.,0.));
#96909=DIRECTION('ref_axis',(1.,0.,0.));
#96910=DIRECTION('',(-0.190809912898503,0.,0.981627005099017));
#96911=DIRECTION('center_axis',(0.,1.,0.));
#96912=DIRECTION('ref_axis',(-0.365466999719524,0.,0.930824297123796));
#96913=DIRECTION('center_axis',(0.,1.,0.));
#96914=DIRECTION('ref_axis',(-0.362201106022701,0.,0.932099972532953));
#96915=DIRECTION('center_axis',(-0.981627005099017,0.,-0.190809912898503));
#96916=DIRECTION('ref_axis',(-0.190809912898503,0.,0.981627005099017));
#96917=DIRECTION('center_axis',(-0.981627005099017,-1.34465099984062E-17,
-0.190809912898503));
#96918=DIRECTION('ref_axis',(-0.190545615363852,-0.0526151297819897,0.980267318940928));
#96919=DIRECTION('center_axis',(-0.981627005099017,-1.29229473701052E-17,
-0.190809912898503));
#96920=DIRECTION('ref_axis',(-0.1905559130945,-0.0515806302340213,0.980320295908119));
#96921=DIRECTION('center_axis',(0.,-1.,0.));
#96922=DIRECTION('ref_axis',(0.,0.,-1.));
#96923=DIRECTION('',(-0.190809912898503,0.,0.981627005099017));
#96924=DIRECTION('center_axis',(0.,-1.,0.));
#96925=DIRECTION('ref_axis',(0.0499889785862565,0.,0.998749769471765));
#96926=DIRECTION('',(-0.190809912898503,0.,0.981627005099017));
#96927=DIRECTION('center_axis',(0.,-1.,0.));
#96928=DIRECTION('ref_axis',(0.0452862925115339,0.,0.998974049568136));
#96929=DIRECTION('center_axis',(0.981627005099017,0.,0.190809912898503));
#96930=DIRECTION('ref_axis',(0.,-1.,0.));
#96931=DIRECTION('',(-0.190809912898503,0.,0.981627005099017));
#96932=DIRECTION('center_axis',(0.981627005099017,-5.41970011904846E-18,
0.190809912898504));
#96933=DIRECTION('ref_axis',(-0.190771803757425,-0.0199851506205497,0.9814309515426));
#96934=DIRECTION('center_axis',(0.981627005099017,5.20341504195632E-18,
0.190809912898503));
#96935=DIRECTION('ref_axis',(-0.190773324732523,-0.019582314952569,0.981438776242104));
#96936=DIRECTION('center_axis',(0.,1.,0.));
#96937=DIRECTION('ref_axis',(1.,0.,0.));
#96938=DIRECTION('',(-0.190809912898503,0.,0.981627005099017));
#96939=DIRECTION('center_axis',(0.,1.,0.));
#96940=DIRECTION('ref_axis',(0.0165392312897058,0.,0.999863217559455));
#96941=DIRECTION('center_axis',(0.,1.,0.));
#96942=DIRECTION('ref_axis',(0.0125120179178436,0.,0.999921721640061));
#96943=DIRECTION('center_axis',(-0.981627005099017,0.,-0.190809912898503));
#96944=DIRECTION('ref_axis',(-0.190809912898503,0.,0.981627005099017));
#96945=DIRECTION('center_axis',(-0.981627005099017,2.91162147259362E-17,
-0.190809912898504));
#96946=DIRECTION('ref_axis',(-0.190542840881032,-0.0528903819944982,0.980253045535418));
#96947=DIRECTION('center_axis',(-0.981627005099017,2.42416206032157E-17,
-0.190809912898504));
#96948=DIRECTION('ref_axis',(-0.190553351649904,-0.0518398845002214,0.98030711848379));
#96949=DIRECTION('center_axis',(0.,-1.,0.));
#96950=DIRECTION('ref_axis',(0.,0.,-1.));
#96951=DIRECTION('',(-0.190809912898503,0.,0.981627005099017));
#96952=DIRECTION('center_axis',(0.,-1.,0.));
#96953=DIRECTION('ref_axis',(0.0513446549634899,0.,0.998680993314021));
#96954=DIRECTION('',(-0.190809912898503,0.,0.981627005099017));
#96955=DIRECTION('center_axis',(0.,-1.,0.));
#96956=DIRECTION('ref_axis',(0.0465642295325163,0.,0.99891529797478));
#96957=DIRECTION('center_axis',(0.981627005099017,0.,0.190809912898503));
#96958=DIRECTION('ref_axis',(0.,-1.,0.));
#96959=DIRECTION('',(-0.190809912898503,0.,0.981627005099017));
#96960=DIRECTION('center_axis',(0.981627005099017,-6.50364014285815E-17,
0.190809912898504));
#96961=DIRECTION('ref_axis',(-0.190093032704192,-0.086602319355716,0.977938994620592));
#96962=DIRECTION('center_axis',(0.981627005099017,-4.91959240330416E-17,
0.190809912898504));
#96963=DIRECTION('ref_axis',(-0.19012169317225,-0.0848566981278218,0.97808643921085));
#96964=DIRECTION('center_axis',(0.,1.,0.));
#96965=DIRECTION('ref_axis',(1.,0.,0.));
#96966=DIRECTION('',(-0.190809912898503,0.,0.981627005099017));
#96967=DIRECTION('center_axis',(0.,1.,0.));
#96968=DIRECTION('ref_axis',(0.0172512508492204,0.,0.99985118609928));
#96969=DIRECTION('center_axis',(0.,1.,0.));
#96970=DIRECTION('ref_axis',(0.0131834739886762,0.,0.999913094230489));
#96971=DIRECTION('center_axis',(-0.981627005099017,0.,-0.190809912898503));
#96972=DIRECTION('ref_axis',(-0.190809912898503,0.,0.981627005099017));
#96973=DIRECTION('center_axis',(-0.981627005099017,3.88216196345816E-18,
-0.190809912898503));
#96974=DIRECTION('ref_axis',(-0.189453989330261,-0.119003359487598,0.974651417870776));
#96975=DIRECTION('center_axis',(-0.981627005099017,1.11884402784072E-16,
-0.190809912898504));
#96976=DIRECTION('ref_axis',(-0.189507499835796,-0.116639740125495,0.974926704183162));
#96977=DIRECTION('center_axis',(0.,-1.,0.));
#96978=DIRECTION('ref_axis',(0.,0.,-1.));
#96979=DIRECTION('',(-0.190809912898503,0.,0.981627005099017));
#96980=DIRECTION('center_axis',(0.,-1.,0.));
#96981=DIRECTION('ref_axis',(-0.0152323034392406,0.,0.999883981735849));
#96982=DIRECTION('',(-0.190809912898513,0.,0.981627005099015));
#96983=DIRECTION('center_axis',(0.,-1.,0.));
#96984=DIRECTION('ref_axis',(-0.0186761357819992,0.,0.999825585765964));
#96985=DIRECTION('center_axis',(0.981627005099017,0.,0.190809912898503));
#96986=DIRECTION('ref_axis',(0.,-1.,0.));
#96987=DIRECTION('',(-0.190809912898503,0.,0.981627005099017));
#96988=DIRECTION('center_axis',(0.981627005099017,-2.68291919433533E-17,
0.190809912898504));
#96989=DIRECTION('ref_axis',(-0.19011286766609,-0.0853980630086089,0.978041036144268));
#96990=DIRECTION('center_axis',(0.981627005099017,-6.44673374429825E-17,
0.190809912898504));
#96991=DIRECTION('ref_axis',(-0.190139994095334,-0.0837228659615728,0.978180588828365));
#96992=DIRECTION('center_axis',(0.,1.,0.));
#96993=DIRECTION('ref_axis',(1.,0.,0.));
#96994=DIRECTION('',(-0.190809912898492,0.,0.981627005099019));
#96995=DIRECTION('center_axis',(0.,1.,0.));
#96996=DIRECTION('ref_axis',(-0.0486734108678654,0.,0.998814747125055));
#96997=DIRECTION('center_axis',(0.,1.,0.));
#96998=DIRECTION('ref_axis',(-0.0514348329990322,0.,0.998676352956433));
#96999=DIRECTION('center_axis',(-0.981627005099017,0.,-0.190809912898503));
#97000=DIRECTION('ref_axis',(-0.190809912898503,0.,0.981627005099017));
#97001=DIRECTION('center_axis',(-0.981627005099017,-1.89632209273643E-17,
-0.190809912898503));
#97002=DIRECTION('ref_axis',(-0.18948536451151,-0.117623323629904,0.97481282837999));
#97003=DIRECTION('center_axis',(-0.981627005099017,4.37614819833767E-17,
-0.190809912898504));
#97004=DIRECTION('ref_axis',(-0.189536473917127,-0.115339425574496,0.975075762165796));
#97005=DIRECTION('center_axis',(0.,-1.,0.));
#97006=DIRECTION('ref_axis',(0.,0.,-1.));
#97007=DIRECTION('',(-0.190809912898503,0.,0.981627005099017));
#97008=DIRECTION('center_axis',(0.,-1.,0.));
#97009=DIRECTION('ref_axis',(-0.0809598914546659,0.,0.996717360125552));
#97010=DIRECTION('',(-0.190809912898503,0.,0.981627005099017));
#97011=DIRECTION('center_axis',(0.,-1.,0.));
#97012=DIRECTION('ref_axis',(-0.0831011195422453,0.,0.996541120040124));
#97013=DIRECTION('center_axis',(0.981627005099017,0.,0.190809912898503));
#97014=DIRECTION('ref_axis',(0.,-1.,0.));
#97015=DIRECTION('',(-0.190809912898503,0.,0.981627005099017));
#97016=DIRECTION('center_axis',(0.981627005099017,-6.39425166145185E-17,
0.190809912898504));
#97017=DIRECTION('ref_axis',(-0.190125879388814,-0.0845986914841974,0.978107975320614));
#97018=DIRECTION('center_axis',(0.981627005099017,-3.79871508880441E-17,
0.190809912898504));
#97019=DIRECTION('ref_axis',(-0.190152021521919,-0.0829692100674824,0.97824246426533));
#97020=DIRECTION('center_axis',(0.,1.,0.));
#97021=DIRECTION('ref_axis',(1.,0.,0.));
#97022=DIRECTION('',(-0.190809912898503,0.,0.981627005099017));
#97023=DIRECTION('center_axis',(0.,1.,0.));
#97024=DIRECTION('ref_axis',(-0.113767879747049,0.,0.993507357566043));
#97025=DIRECTION('center_axis',(0.,1.,0.));
#97026=DIRECTION('ref_axis',(-0.115255452371297,0.,0.993335885135883));
#97027=DIRECTION('center_axis',(-0.981627005099017,0.,-0.190809912898503));
#97028=DIRECTION('ref_axis',(-0.190809912898503,0.,0.981627005099017));
#97029=DIRECTION('center_axis',(-0.981627005099017,2.24302127796356E-17,
-0.190809912898503));
#97030=DIRECTION('ref_axis',(-0.189504385020733,-0.116778654807704,0.974910679928791));
#97031=DIRECTION('center_axis',(-0.981627005099017,-3.59658141965232E-17,
-0.190809912898503));
#97032=DIRECTION('ref_axis',(-0.189554064615674,-0.114542681217505,0.975166258013054));
#97033=DIRECTION('center_axis',(0.,-1.,0.));
#97034=DIRECTION('ref_axis',(0.,0.,-1.));
#97035=DIRECTION('',(-0.190809912898503,0.,0.981627005099017));
#97036=DIRECTION('center_axis',(0.,-1.,0.));
#97037=DIRECTION('ref_axis',(-0.145862172035669,0.,0.989304921027403));
#97038=DIRECTION('',(-0.190809912898503,0.,0.981627005099017));
#97039=DIRECTION('center_axis',(0.,-1.,0.));
#97040=DIRECTION('ref_axis',(-0.146732928854605,0.,0.989176145885933));
#97041=DIRECTION('center_axis',(0.981627005099017,0.,0.190809912898503));
#97042=DIRECTION('ref_axis',(0.,-1.,0.));
#97043=DIRECTION('',(-0.190809912898503,0.,0.981627005099017));
#97044=DIRECTION('center_axis',(0.981627005099017,-2.42026211186394E-17,
0.190809912898504));
#97045=DIRECTION('ref_axis',(-0.190132774005443,-0.0841720232876468,0.978143444871282));
#97046=DIRECTION('center_axis',(0.981627005099017,-3.22451880808121E-17,
0.190809912898504));
#97047=DIRECTION('ref_axis',(-0.190158401673233,-0.0825666085944808,0.978275287134602));
#97048=DIRECTION('center_axis',(0.,1.,0.));
#97049=DIRECTION('ref_axis',(1.,0.,0.));
#97050=DIRECTION('',(-0.190809912898503,0.,0.981627005099017));
#97051=DIRECTION('center_axis',(0.,1.,0.));
#97052=DIRECTION('ref_axis',(-0.178050117193582,0.,0.984021420380345));
#97053=DIRECTION('center_axis',(0.,1.,0.));
#97054=DIRECTION('ref_axis',(-0.178294982707409,0.,0.983977082630162));
#97055=DIRECTION('center_axis',(-0.981627005099017,0.,-0.190809912898503));
#97056=DIRECTION('ref_axis',(-0.190809912898503,0.,0.981627005099017));
#97057=DIRECTION('center_axis',(-0.981627005099017,-5.94635036830686E-17,
-0.190809912898503));
#97058=DIRECTION('ref_axis',(-0.189512059149486,-0.116436100650099,0.974950159701675));
#97059=DIRECTION('center_axis',(-0.981627005099017,-2.86104544861472E-17,
-0.190809912898503));
#97060=DIRECTION('ref_axis',(-0.189561167388284,-0.114219375573802,0.975202798428061));
#97061=DIRECTION('center_axis',(0.,-1.,0.));
#97062=DIRECTION('ref_axis',(0.,0.,-1.));
#97063=DIRECTION('',(-0.190809912898503,0.,0.981627005099017));
#97064=DIRECTION('center_axis',(0.,-1.,0.));
#97065=DIRECTION('ref_axis',(-0.209951794403501,0.,0.977711738717885));
#97066=DIRECTION('',(-0.190809912898503,0.,0.981627005099017));
#97067=DIRECTION('center_axis',(0.,-1.,0.));
#97068=DIRECTION('ref_axis',(-0.209583254257496,0.,0.977790805609685));
#97069=DIRECTION('center_axis',(0.981627005099017,0.,0.190809912898503));
#97070=DIRECTION('ref_axis',(0.,-1.,0.));
#97071=DIRECTION('',(-0.190809912898503,0.,0.981627005099017));
#97072=DIRECTION('center_axis',(0.981627005099017,1.85862334867601E-17,
0.190809912898503));
#97073=DIRECTION('ref_axis',(-0.190133909618249,-0.0841015376217537,0.978149287063553));
#97074=DIRECTION('center_axis',(0.981627005099017,-1.60966213518622E-17,
0.190809912898503));
#97075=DIRECTION('ref_axis',(-0.190159453020121,-0.0825000764607267,0.978280695818466));
#97076=DIRECTION('center_axis',(0.,1.,0.));
#97077=DIRECTION('ref_axis',(1.,0.,0.));
#97078=DIRECTION('',(-0.190809912898503,0.,0.981627005099017));
#97079=DIRECTION('center_axis',(0.,1.,0.));
#97080=DIRECTION('ref_axis',(-0.2415273311514,0.,0.970394017039925));
#97081=DIRECTION('center_axis',(0.,1.,0.));
#97082=DIRECTION('ref_axis',(-0.240560091673225,0.,0.970634247435237));
#97083=DIRECTION('center_axis',(-0.981627005099017,0.,-0.190809912898503));
#97084=DIRECTION('ref_axis',(-0.190809912898503,0.,0.981627005099017));
#97085=DIRECTION('center_axis',(-0.981627005099017,1.15500516668025E-16,
-0.190809912898504));
#97086=DIRECTION('ref_axis',(-0.189508781312522,-0.116582540038997,0.974933296776502));
#97087=DIRECTION('center_axis',(-0.981627005099017,8.60392289098693E-17,
-0.190809912898504));
#97088=DIRECTION('ref_axis',(-0.189558133204824,-0.114357599550504,0.975187188985247));
#97089=DIRECTION('center_axis',(0.,-1.,0.));
#97090=DIRECTION('ref_axis',(0.,0.,-1.));
#97091=DIRECTION('',(-0.190809912898503,0.,0.981627005099017));
#97092=DIRECTION('center_axis',(0.,-1.,0.));
#97093=DIRECTION('ref_axis',(-0.273230835267042,0.,0.961948496884981));
#97094=DIRECTION('',(-0.190809912898503,0.,0.981627005099017));
#97095=DIRECTION('center_axis',(0.,-1.,0.));
#97096=DIRECTION('ref_axis',(-0.271654016185366,0.,0.962394978940747));
#97097=DIRECTION('center_axis',(0.981627005099017,0.,0.190809912898503));
#97098=DIRECTION('ref_axis',(0.,-1.,0.));
#97099=DIRECTION('',(-0.190809912898503,0.,0.981627005099017));
#97100=DIRECTION('center_axis',(0.981627005099017,-5.42634466570013E-17,
0.190809912898504));
#97101=DIRECTION('ref_axis',(-0.190129344158506,-0.0843845483960271,0.9781257999265));
#97102=DIRECTION('center_axis',(0.981627005099017,4.32027132019077E-17,
0.190809912898503));
#97103=DIRECTION('ref_axis',(-0.190155227141477,-0.0827671749549381,0.97825895566601));
#97104=DIRECTION('center_axis',(0.,1.,0.));
#97105=DIRECTION('ref_axis',(1.,0.,0.));
#97106=DIRECTION('',(-0.190809912898503,0.,0.981627005099017));
#97107=DIRECTION('center_axis',(0.,1.,0.));
#97108=DIRECTION('ref_axis',(-0.304196445644748,0.,0.952609323100032));
#97109=DIRECTION('center_axis',(0.,1.,0.));
#97110=DIRECTION('ref_axis',(-0.302047933389658,0.,0.953292738845228));
#97111=DIRECTION('center_axis',(-0.981627005099017,0.,-0.190809912898503));
#97112=DIRECTION('ref_axis',(-0.190809912898503,0.,0.981627005099017));
#97113=DIRECTION('center_axis',(-0.981627005099017,1.13007235228963E-17,
-0.190809912898503));
#97114=DIRECTION('ref_axis',(-0.189494383908818,-0.117223556705195,0.97485922892508));
#97115=DIRECTION('center_axis',(-0.981627005099017,3.62298903615095E-17,
-0.190809912898504));
#97116=DIRECTION('ref_axis',(-0.189544812876814,-0.114962422466095,0.97511866218026));
#97117=DIRECTION('center_axis',(0.,-1.,0.));
#97118=DIRECTION('ref_axis',(0.,0.,-1.));
#97119=DIRECTION('',(-0.190809912898503,0.,0.981627005099017));
#97120=DIRECTION('center_axis',(0.,-1.,0.));
#97121=DIRECTION('ref_axis',(-0.272783869673527,0.,0.96207534031693));
#97122=DIRECTION('',(-0.190809912898503,0.,0.981627005099017));
#97123=DIRECTION('center_axis',(0.,-1.,0.));
#97124=DIRECTION('ref_axis',(-0.271232151177082,0.,0.96251395842754));
#97125=DIRECTION('center_axis',(0.981627005099017,0.,0.190809912898503));
#97126=DIRECTION('ref_axis',(0.,-1.,0.));
#97127=DIRECTION('',(-0.190809912898503,0.,0.981627005099017));
#97128=DIRECTION('center_axis',(0.981627005099017,1.87115333300005E-18,
0.190809912898503));
#97129=DIRECTION('ref_axis',(-0.190773730797495,-0.0194733573221602,0.98144086525486));
#97130=DIRECTION('center_axis',(0.981627005099017,1.35008478755962E-18,
0.190809912898503));
#97131=DIRECTION('ref_axis',(-0.190775104613922,-0.0191001172972896,0.981447932892406));
#97132=DIRECTION('center_axis',(0.,1.,0.));
#97133=DIRECTION('ref_axis',(1.,0.,0.));
#97134=DIRECTION('',(-0.190809912898513,0.,0.981627005099015));
#97135=DIRECTION('center_axis',(0.,1.,0.));
#97136=DIRECTION('ref_axis',(-0.303820565781007,0.,0.952729270993869));
#97137=DIRECTION('center_axis',(0.,1.,0.));
#97138=DIRECTION('ref_axis',(-0.301693026915346,0.,0.953405117203939));
#97139=DIRECTION('center_axis',(-0.981627005099017,0.,-0.190809912898503));
#97140=DIRECTION('ref_axis',(-0.190809912898503,0.,0.981627005099017));
#97141=DIRECTION('center_axis',(-0.981627005099017,6.02705254554468E-17,
-0.190809912898504));
#97142=DIRECTION('ref_axis',(-0.190550775140863,-0.0520993585356409,0.98029386356));
#97143=DIRECTION('center_axis',(-0.981627005099017,1.99264396988302E-17,
-0.190809912898504));
#97144=DIRECTION('ref_axis',(-0.190560682254905,-0.0510944099849382,0.980344830988992));
#97145=DIRECTION('center_axis',(0.,-1.,0.));
#97146=DIRECTION('ref_axis',(0.,0.,-1.));
#97147=DIRECTION('',(-0.19080991289849,0.,0.98162700509902));
#97148=DIRECTION('center_axis',(0.,-1.,0.));
#97149=DIRECTION('ref_axis',(-0.0162088407295448,0.,0.999868628111816));
#97150=DIRECTION('',(-0.190809912898503,0.,0.981627005099017));
#97151=DIRECTION('center_axis',(0.,-1.,0.));
#97152=DIRECTION('ref_axis',(-0.0195969249883702,0.,0.99980796182617));
#97153=DIRECTION('center_axis',(0.981627005099017,0.,0.190809912898503));
#97154=DIRECTION('ref_axis',(0.,-1.,0.));
#97155=DIRECTION('',(-0.190809912898503,0.,0.981627005099017));
#97156=DIRECTION('center_axis',(0.981627005099017,-9.58185426548332E-19,
0.190809912898503));
#97157=DIRECTION('ref_axis',(-0.190772856350838,-0.0197072453096809,0.981436366639247));
#97158=DIRECTION('center_axis',(0.981627005099017,-1.93402012328947E-17,
0.190809912898504));
#97159=DIRECTION('ref_axis',(-0.190774296053174,-0.0193206613757493,0.981443773228716));
#97160=DIRECTION('center_axis',(0.,1.,0.));
#97161=DIRECTION('ref_axis',(1.,0.,0.));
#97162=DIRECTION('',(-0.190809912898503,0.,0.981627005099017));
#97163=DIRECTION('center_axis',(0.,1.,0.));
#97164=DIRECTION('ref_axis',(-0.0491567156126708,0.,0.998791077908776));
#97165=DIRECTION('center_axis',(0.,1.,0.));
#97166=DIRECTION('ref_axis',(-0.0518907218216088,0.,0.998652768978704));
#97167=DIRECTION('center_axis',(-0.981627005099017,0.,-0.190809912898503));
#97168=DIRECTION('ref_axis',(-0.190809912898503,0.,0.981627005099017));
#97169=DIRECTION('center_axis',(-0.981627005099017,-1.3274254649155E-17,
-0.190809912898503));
#97170=DIRECTION('ref_axis',(-0.190549003442479,-0.0522770327244192,0.980284749007454));
#97171=DIRECTION('center_axis',(-0.981627005099017,1.8233950826407E-18,
-0.190809912898503));
#97172=DIRECTION('ref_axis',(-0.190559043863139,-0.0512619669220116,0.980336402236117));
#97173=DIRECTION('center_axis',(0.,-1.,0.));
#97174=DIRECTION('ref_axis',(0.,0.,-1.));
#97175=DIRECTION('',(-0.190809912898503,0.,0.981627005099017));
#97176=DIRECTION('center_axis',(0.,-1.,0.));
#97177=DIRECTION('ref_axis',(-0.0815670055162436,0.,0.996667860227826));
#97178=DIRECTION('',(-0.190809912898503,0.,0.981627005099017));
#97179=DIRECTION('center_axis',(0.,-1.,0.));
#97180=DIRECTION('ref_axis',(-0.0836737189959334,0.,0.996493205571112));
#97181=DIRECTION('center_axis',(0.981627005099017,0.,0.190809912898503));
#97182=DIRECTION('ref_axis',(0.,-1.,0.));
#97183=DIRECTION('',(-0.190809912898503,0.,0.981627005099017));
#97184=DIRECTION('center_axis',(0.981627005099017,-2.30381126037603E-17,
0.190809912898504));
#97185=DIRECTION('ref_axis',(-0.190773546907965,-0.0195227749578894,0.981439919229954));
#97186=DIRECTION('center_axis',(0.981627005099017,-4.07005188086187E-18,
0.190809912898503));
#97187=DIRECTION('ref_axis',(-0.190774934456505,-0.0191467407848009,0.98144705751275));
#97188=DIRECTION('center_axis',(0.,1.,0.));
#97189=DIRECTION('ref_axis',(1.,0.,0.));
#97190=DIRECTION('',(-0.190809912898503,0.,0.981627005099017));
#97191=DIRECTION('center_axis',(0.,1.,0.));
#97192=DIRECTION('ref_axis',(-0.114028208728371,0.,0.993477512384754));
#97193=DIRECTION('center_axis',(0.,1.,0.));
#97194=DIRECTION('ref_axis',(-0.115501073839451,0.,0.993307355223917));
#97195=DIRECTION('center_axis',(-0.981627005099017,0.,-0.190809912898503));
#97196=DIRECTION('ref_axis',(-0.190809912898503,0.,0.981627005099017));
#97197=DIRECTION('center_axis',(-0.981627005099017,-1.86918439830296E-18,
-0.190809912898503));
#97198=DIRECTION('ref_axis',(-0.190552739758759,-0.0519016243589593,0.980303970592455));
#97199=DIRECTION('center_axis',(-0.981627005099017,-1.79829070982616E-17,
-0.190809912898503));
#97200=DIRECTION('ref_axis',(-0.190562500052238,-0.0509078583188802,0.980354182698899));
#97201=DIRECTION('center_axis',(0.,-1.,0.));
#97202=DIRECTION('ref_axis',(0.,0.,-1.));
#97203=DIRECTION('',(-0.190809912898503,0.,0.981627005099017));
#97204=DIRECTION('center_axis',(0.,-1.,0.));
#97205=DIRECTION('ref_axis',(-0.146109040889921,0.,0.989268491447204));
#97206=DIRECTION('',(-0.190809912898503,0.,0.981627005099017));
#97207=DIRECTION('center_axis',(0.,-1.,0.));
#97208=DIRECTION('ref_axis',(-0.146965819474498,0.,0.989141571215258));
#97209=DIRECTION('center_axis',(0.981627005099017,0.,0.190809912898503));
#97210=DIRECTION('ref_axis',(0.,-1.,0.));
#97211=DIRECTION('',(-0.190809912898503,0.,0.981627005099017));
#97212=DIRECTION('center_axis',(0.981627005099017,-7.91239536570904E-18,
0.190809912898504));
#97213=DIRECTION('ref_axis',(-0.190773912836659,-0.0194243130663802,0.981441801760497));
#97214=DIRECTION('center_axis',(0.981627005099017,-9.40484652357021E-18,
0.190809912898504));
#97215=DIRECTION('ref_axis',(-0.190775273123846,-0.0190538327525699,0.981448799796484));
#97216=DIRECTION('center_axis',(0.,1.,0.));
#97217=DIRECTION('ref_axis',(1.,0.,0.));
#97218=DIRECTION('',(-0.190809912898503,0.,0.981627005099017));
#97219=DIRECTION('center_axis',(0.,1.,0.));
#97220=DIRECTION('ref_axis',(-0.178092965033456,0.,0.984013666472977));
#97221=DIRECTION('center_axis',(0.,1.,0.));
#97222=DIRECTION('ref_axis',(-0.178335419485715,0.,0.983969754696177));
#97223=DIRECTION('center_axis',(-0.981627005099017,0.,-0.190809912898503));
#97224=DIRECTION('ref_axis',(-0.190809912898503,0.,0.981627005099017));
#97225=DIRECTION('center_axis',(-0.981627005099017,0.,-0.190809912898503));
#97226=DIRECTION('ref_axis',(-0.190554247320776,-0.0517493780667019,0.980311726287981));
#97227=DIRECTION('center_axis',(-0.981627005099017,2.50341476753788E-17,
-0.190809912898504));
#97228=DIRECTION('ref_axis',(-0.190563895665479,-0.0507641669217001,0.980361362470769));
#97229=DIRECTION('center_axis',(0.,-1.,0.));
#97230=DIRECTION('ref_axis',(0.,0.,-1.));
#97231=DIRECTION('',(-0.190809912898503,1.256366518269E-14,0.981627005099017));
#97232=DIRECTION('center_axis',(0.,-1.,0.));
#97233=DIRECTION('ref_axis',(-0.209847318452884,0.,0.977734167827909));
#97234=DIRECTION('',(-0.190809912898503,0.,0.981627005099017));
#97235=DIRECTION('center_axis',(0.,-1.,0.));
#97236=DIRECTION('ref_axis',(-0.209484670142235,0.,0.977811931291186));
#97237=DIRECTION('center_axis',(0.981627005099017,0.,0.190809912898503));
#97238=DIRECTION('ref_axis',(0.,-1.,0.));
#97239=DIRECTION('',(-0.190809912898503,0.,0.981627005099017));
#97240=DIRECTION('center_axis',(0.981627005099017,-1.5798298463746E-17,
0.190809912898504));
#97241=DIRECTION('ref_axis',(-0.190773973110007,-0.0194080471434809,0.981442111838441));
#97242=DIRECTION('center_axis',(0.981627005099017,2.2356418544253E-18,0.190809912898503));
#97243=DIRECTION('ref_axis',(-0.190775328931839,-0.0190384791832405,0.981449086902289));
#97244=DIRECTION('center_axis',(0.,1.,0.));
#97245=DIRECTION('ref_axis',(1.,0.,0.));
#97246=DIRECTION('',(-0.190809912898491,0.,0.981627005099019));
#97247=DIRECTION('center_axis',(0.,1.,0.));
#97248=DIRECTION('ref_axis',(-0.241358095629752,0.,0.970436123438312));
#97249=DIRECTION('center_axis',(0.,1.,0.));
#97250=DIRECTION('ref_axis',(-0.240400340232753,0.,0.97067382596626));
#97251=DIRECTION('center_axis',(-0.981627005099017,0.,-0.190809912898503));
#97252=DIRECTION('ref_axis',(-0.190809912898503,0.,0.981627005099017));
#97253=DIRECTION('center_axis',(-0.981627005099017,4.65727889790425E-17,
-0.190809912898504));
#97254=DIRECTION('ref_axis',(-0.190553603392484,-0.0518144622395518,0.980308413580627));
#97255=DIRECTION('center_axis',(-0.981627005099017,-2.33022911630896E-17,
-0.190809912898503));
#97256=DIRECTION('ref_axis',(-0.190563299478129,-0.0508255998002297,0.980358295368054));
#97257=DIRECTION('center_axis',(0.190809912898503,0.,-0.981627005099017));
#97258=DIRECTION('ref_axis',(0.,-1.,0.));
#97259=DIRECTION('center_axis',(0.,1.,0.));
#97260=DIRECTION('ref_axis',(1.,0.,0.));
#97261=DIRECTION('',(-0.190809912898503,0.,0.981627005099017));
#97262=DIRECTION('',(0.981627005099017,0.,0.190809912898503));
#97263=DIRECTION('',(-0.190809912898503,0.,0.981627005099017));
#97264=DIRECTION('',(0.981627005099017,0.,0.190809912898503));
#97265=DIRECTION('center_axis',(0.981627005099017,0.,0.190809912898503));
#97266=DIRECTION('ref_axis',(0.,-1.,0.));
#97267=DIRECTION('',(-0.190809912898503,0.,0.981627005099017));
#97268=DIRECTION('',(0.,-1.,0.));
#97269=DIRECTION('',(0.,-1.,0.));
#97270=DIRECTION('center_axis',(0.,-1.,0.));
#97271=DIRECTION('ref_axis',(0.,0.,-1.));
#97272=DIRECTION('',(-0.190809912898503,0.,0.981627005099017));
#97273=DIRECTION('',(-0.981627005099017,0.,-0.190809912898503));
#97274=DIRECTION('',(-0.981627005099017,0.,-0.190809912898503));
#97275=DIRECTION('center_axis',(-0.981627005099017,0.,-0.190809912898503));
#97276=DIRECTION('ref_axis',(-0.190809912898503,0.,0.981627005099017));
#97277=DIRECTION('',(0.,1.,0.));
#97278=DIRECTION('',(0.,1.,0.));
#97279=DIRECTION('center_axis',(0.,1.,0.));
#97280=DIRECTION('ref_axis',(1.,0.,0.));
#97281=DIRECTION('',(-0.190809912898503,0.,0.981627005099017));
#97282=DIRECTION('',(0.981627005099017,0.,0.190809912898503));
#97283=DIRECTION('',(-0.190809912898503,0.,0.981627005099017));
#97284=DIRECTION('',(0.981627005099017,0.,0.190809912898503));
#97285=DIRECTION('center_axis',(0.981627005099017,0.,0.190809912898503));
#97286=DIRECTION('ref_axis',(0.,-1.,0.));
#97287=DIRECTION('',(-0.190809912898503,0.,0.981627005099017));
#97288=DIRECTION('',(0.,-1.,0.));
#97289=DIRECTION('',(0.,-1.,0.));
#97290=DIRECTION('center_axis',(0.,-1.,0.));
#97291=DIRECTION('ref_axis',(0.,0.,-1.));
#97292=DIRECTION('',(-0.190809912898503,0.,0.981627005099017));
#97293=DIRECTION('',(-0.981627005099017,0.,-0.190809912898503));
#97294=DIRECTION('',(-0.981627005099017,0.,-0.190809912898503));
#97295=DIRECTION('center_axis',(-0.981627005099017,0.,-0.190809912898503));
#97296=DIRECTION('ref_axis',(-0.190809912898503,0.,0.981627005099017));
#97297=DIRECTION('',(0.,1.,0.));
#97298=DIRECTION('',(0.,1.,0.));
#97299=DIRECTION('center_axis',(0.,1.,0.));
#97300=DIRECTION('ref_axis',(1.,0.,0.));
#97301=DIRECTION('',(-0.190809912898503,0.,0.981627005099017));
#97302=DIRECTION('',(0.981627005099017,0.,0.190809912898503));
#97303=DIRECTION('',(-0.190809912898503,0.,0.981627005099017));
#97304=DIRECTION('',(0.981627005099017,0.,0.190809912898503));
#97305=DIRECTION('center_axis',(0.981627005099017,0.,0.190809912898503));
#97306=DIRECTION('ref_axis',(0.,-1.,0.));
#97307=DIRECTION('',(-0.190809912898503,0.,0.981627005099017));
#97308=DIRECTION('',(0.,-1.,0.));
#97309=DIRECTION('',(0.,-1.,0.));
#97310=DIRECTION('center_axis',(0.,-1.,0.));
#97311=DIRECTION('ref_axis',(0.,0.,-1.));
#97312=DIRECTION('',(-0.190809912898503,0.,0.981627005099017));
#97313=DIRECTION('',(-0.981627005099017,0.,-0.190809912898503));
#97314=DIRECTION('',(-0.981627005099017,0.,-0.190809912898503));
#97315=DIRECTION('center_axis',(-0.981627005099017,0.,-0.190809912898503));
#97316=DIRECTION('ref_axis',(-0.190809912898503,0.,0.981627005099017));
#97317=DIRECTION('',(0.,1.,0.));
#97318=DIRECTION('',(0.,1.,0.));
#97319=DIRECTION('center_axis',(0.,1.,0.));
#97320=DIRECTION('ref_axis',(1.,0.,0.));
#97321=DIRECTION('',(-0.190809912898503,0.,0.981627005099017));
#97322=DIRECTION('',(0.981627005099017,0.,0.190809912898503));
#97323=DIRECTION('',(-0.190809912898503,0.,0.981627005099017));
#97324=DIRECTION('',(0.981627005099017,0.,0.190809912898503));
#97325=DIRECTION('center_axis',(0.981627005099017,0.,0.190809912898503));
#97326=DIRECTION('ref_axis',(0.,-1.,0.));
#97327=DIRECTION('',(-0.190809912898503,0.,0.981627005099017));
#97328=DIRECTION('',(0.,-1.,0.));
#97329=DIRECTION('',(0.,-1.,0.));
#97330=DIRECTION('center_axis',(0.,-1.,0.));
#97331=DIRECTION('ref_axis',(0.,0.,-1.));
#97332=DIRECTION('',(-0.190809912898503,0.,0.981627005099017));
#97333=DIRECTION('',(-0.981627005099017,0.,-0.190809912898503));
#97334=DIRECTION('',(-0.981627005099017,0.,-0.190809912898503));
#97335=DIRECTION('center_axis',(-0.981627005099017,0.,-0.190809912898503));
#97336=DIRECTION('ref_axis',(-0.190809912898503,0.,0.981627005099017));
#97337=DIRECTION('',(0.,1.,0.));
#97338=DIRECTION('',(0.,1.,0.));
#97339=DIRECTION('center_axis',(0.,1.,0.));
#97340=DIRECTION('ref_axis',(1.,0.,0.));
#97341=DIRECTION('',(-0.190809912898503,0.,0.981627005099017));
#97342=DIRECTION('',(0.981627005099017,0.,0.190809912898503));
#97343=DIRECTION('',(-0.190809912898503,0.,0.981627005099017));
#97344=DIRECTION('',(0.981627005099017,0.,0.190809912898503));
#97345=DIRECTION('center_axis',(0.981627005099017,0.,0.190809912898503));
#97346=DIRECTION('ref_axis',(0.,-1.,0.));
#97347=DIRECTION('',(-0.190809912898503,0.,0.981627005099017));
#97348=DIRECTION('',(0.,-1.,0.));
#97349=DIRECTION('',(0.,-1.,0.));
#97350=DIRECTION('center_axis',(0.,-1.,0.));
#97351=DIRECTION('ref_axis',(0.,0.,-1.));
#97352=DIRECTION('',(-0.190809912898503,0.,0.981627005099017));
#97353=DIRECTION('',(-0.981627005099017,0.,-0.190809912898503));
#97354=DIRECTION('',(-0.981627005099017,0.,-0.190809912898503));
#97355=DIRECTION('center_axis',(-0.981627005099017,0.,-0.190809912898503));
#97356=DIRECTION('ref_axis',(-0.190809912898503,0.,0.981627005099017));
#97357=DIRECTION('',(0.,1.,0.));
#97358=DIRECTION('',(0.,1.,0.));
#97359=DIRECTION('center_axis',(0.,1.,0.));
#97360=DIRECTION('ref_axis',(1.,0.,0.));
#97361=DIRECTION('',(-0.190809912898503,0.,0.981627005099017));
#97362=DIRECTION('',(0.981627005099017,0.,0.190809912898503));
#97363=DIRECTION('',(-0.190809912898503,0.,0.981627005099017));
#97364=DIRECTION('',(0.981627005099017,0.,0.190809912898503));
#97365=DIRECTION('center_axis',(0.981627005099017,0.,0.190809912898503));
#97366=DIRECTION('ref_axis',(0.,-1.,0.));
#97367=DIRECTION('',(-0.190809912898503,0.,0.981627005099017));
#97368=DIRECTION('',(0.,-1.,0.));
#97369=DIRECTION('',(0.,-1.,0.));
#97370=DIRECTION('center_axis',(0.,-1.,0.));
#97371=DIRECTION('ref_axis',(0.,0.,-1.));
#97372=DIRECTION('',(-0.190809912898503,0.,0.981627005099017));
#97373=DIRECTION('',(-0.981627005099017,0.,-0.190809912898503));
#97374=DIRECTION('',(-0.981627005099017,0.,-0.190809912898503));
#97375=DIRECTION('center_axis',(-0.981627005099017,0.,-0.190809912898503));
#97376=DIRECTION('ref_axis',(-0.190809912898503,0.,0.981627005099017));
#97377=DIRECTION('',(0.,1.,0.));
#97378=DIRECTION('',(0.,1.,0.));
#97379=DIRECTION('center_axis',(0.,1.,0.));
#97380=DIRECTION('ref_axis',(1.,0.,0.));
#97381=DIRECTION('',(-0.190809912898503,0.,0.981627005099017));
#97382=DIRECTION('',(0.981627005099017,0.,0.190809912898503));
#97383=DIRECTION('',(-0.190809912898503,0.,0.981627005099017));
#97384=DIRECTION('',(0.981627005099017,0.,0.190809912898503));
#97385=DIRECTION('center_axis',(0.981627005099017,0.,0.190809912898503));
#97386=DIRECTION('ref_axis',(0.,-1.,0.));
#97387=DIRECTION('',(-0.190809912898503,0.,0.981627005099017));
#97388=DIRECTION('',(0.,-1.,0.));
#97389=DIRECTION('',(0.,-1.,0.));
#97390=DIRECTION('center_axis',(0.,-1.,0.));
#97391=DIRECTION('ref_axis',(0.,0.,-1.));
#97392=DIRECTION('',(-0.190809912898503,0.,0.981627005099017));
#97393=DIRECTION('',(-0.981627005099017,0.,-0.190809912898503));
#97394=DIRECTION('',(-0.981627005099017,0.,-0.190809912898503));
#97395=DIRECTION('center_axis',(-0.981627005099017,0.,-0.190809912898503));
#97396=DIRECTION('ref_axis',(-0.190809912898503,0.,0.981627005099017));
#97397=DIRECTION('',(0.,1.,0.));
#97398=DIRECTION('',(0.,1.,0.));
#97399=DIRECTION('center_axis',(0.,1.,0.));
#97400=DIRECTION('ref_axis',(1.,0.,0.));
#97401=DIRECTION('',(-0.190809912898503,0.,0.981627005099017));
#97402=DIRECTION('',(0.981627005099017,0.,0.190809912898503));
#97403=DIRECTION('',(-0.190809912898503,0.,0.981627005099017));
#97404=DIRECTION('',(0.981627005099017,0.,0.190809912898503));
#97405=DIRECTION('center_axis',(0.981627005099017,0.,0.190809912898503));
#97406=DIRECTION('ref_axis',(0.,-1.,0.));
#97407=DIRECTION('',(-0.190809912898503,0.,0.981627005099017));
#97408=DIRECTION('',(0.,-1.,0.));
#97409=DIRECTION('',(0.,-1.,0.));
#97410=DIRECTION('center_axis',(0.,-1.,0.));
#97411=DIRECTION('ref_axis',(0.,0.,-1.));
#97412=DIRECTION('',(-0.190809912898503,0.,0.981627005099017));
#97413=DIRECTION('',(-0.981627005099017,0.,-0.190809912898503));
#97414=DIRECTION('',(-0.981627005099017,0.,-0.190809912898503));
#97415=DIRECTION('center_axis',(-0.981627005099017,0.,-0.190809912898503));
#97416=DIRECTION('ref_axis',(-0.190809912898503,0.,0.981627005099017));
#97417=DIRECTION('',(0.,1.,0.));
#97418=DIRECTION('',(0.,1.,0.));
#97419=DIRECTION('center_axis',(0.,1.,0.));
#97420=DIRECTION('ref_axis',(1.,0.,0.));
#97421=DIRECTION('',(-0.190809912898503,0.,0.981627005099017));
#97422=DIRECTION('',(0.981627005099017,0.,0.190809912898503));
#97423=DIRECTION('',(-0.190809912898503,0.,0.981627005099017));
#97424=DIRECTION('',(0.981627005099017,0.,0.190809912898503));
#97425=DIRECTION('center_axis',(0.981627005099017,0.,0.190809912898503));
#97426=DIRECTION('ref_axis',(0.,-1.,0.));
#97427=DIRECTION('',(-0.190809912898503,0.,0.981627005099017));
#97428=DIRECTION('',(0.,-1.,0.));
#97429=DIRECTION('',(0.,-1.,0.));
#97430=DIRECTION('center_axis',(0.,-1.,0.));
#97431=DIRECTION('ref_axis',(0.,0.,-1.));
#97432=DIRECTION('',(-0.190809912898503,0.,0.981627005099017));
#97433=DIRECTION('',(-0.981627005099017,0.,-0.190809912898503));
#97434=DIRECTION('',(-0.981627005099017,0.,-0.190809912898503));
#97435=DIRECTION('center_axis',(-0.981627005099017,0.,-0.190809912898503));
#97436=DIRECTION('ref_axis',(-0.190809912898503,0.,0.981627005099017));
#97437=DIRECTION('',(0.,1.,0.));
#97438=DIRECTION('',(0.,1.,0.));
#97439=DIRECTION('center_axis',(0.,1.,0.));
#97440=DIRECTION('ref_axis',(1.,0.,0.));
#97441=DIRECTION('',(-0.190809912898503,0.,0.981627005099017));
#97442=DIRECTION('',(0.981627005099017,0.,0.190809912898503));
#97443=DIRECTION('',(-0.190809912898503,0.,0.981627005099017));
#97444=DIRECTION('',(0.981627005099017,0.,0.190809912898503));
#97445=DIRECTION('center_axis',(0.981627005099017,0.,0.190809912898503));
#97446=DIRECTION('ref_axis',(0.,-1.,0.));
#97447=DIRECTION('',(-0.190809912898503,0.,0.981627005099017));
#97448=DIRECTION('',(0.,-1.,0.));
#97449=DIRECTION('',(0.,-1.,0.));
#97450=DIRECTION('center_axis',(0.,-1.,0.));
#97451=DIRECTION('ref_axis',(0.,0.,-1.));
#97452=DIRECTION('',(-0.190809912898503,0.,0.981627005099017));
#97453=DIRECTION('',(-0.981627005099017,0.,-0.190809912898503));
#97454=DIRECTION('',(-0.981627005099017,0.,-0.190809912898503));
#97455=DIRECTION('center_axis',(-0.981627005099017,0.,-0.190809912898503));
#97456=DIRECTION('ref_axis',(-0.190809912898503,0.,0.981627005099017));
#97457=DIRECTION('',(0.,1.,0.));
#97458=DIRECTION('',(0.,1.,0.));
#97459=DIRECTION('center_axis',(0.,1.,0.));
#97460=DIRECTION('ref_axis',(1.,0.,0.));
#97461=DIRECTION('',(-0.190809912898503,0.,0.981627005099017));
#97462=DIRECTION('',(0.981627005099017,0.,0.190809912898503));
#97463=DIRECTION('',(-0.190809912898503,0.,0.981627005099017));
#97464=DIRECTION('',(0.981627005099017,0.,0.190809912898503));
#97465=DIRECTION('center_axis',(0.981627005099017,0.,0.190809912898503));
#97466=DIRECTION('ref_axis',(0.,-1.,0.));
#97467=DIRECTION('',(-0.190809912898503,0.,0.981627005099017));
#97468=DIRECTION('',(0.,-1.,0.));
#97469=DIRECTION('',(0.,-1.,0.));
#97470=DIRECTION('center_axis',(0.,-1.,0.));
#97471=DIRECTION('ref_axis',(0.,0.,-1.));
#97472=DIRECTION('',(-0.190809912898503,0.,0.981627005099017));
#97473=DIRECTION('',(-0.981627005099017,0.,-0.190809912898503));
#97474=DIRECTION('',(-0.981627005099017,0.,-0.190809912898503));
#97475=DIRECTION('center_axis',(-0.981627005099017,0.,-0.190809912898503));
#97476=DIRECTION('ref_axis',(-0.190809912898503,0.,0.981627005099017));
#97477=DIRECTION('',(0.,1.,0.));
#97478=DIRECTION('',(0.,1.,0.));
#97479=DIRECTION('center_axis',(0.,1.,0.));
#97480=DIRECTION('ref_axis',(1.,0.,0.));
#97481=DIRECTION('',(-0.190809912898503,0.,0.981627005099017));
#97482=DIRECTION('',(0.981627005099017,0.,0.190809912898503));
#97483=DIRECTION('',(-0.190809912898503,0.,0.981627005099017));
#97484=DIRECTION('',(0.981627005099017,0.,0.190809912898503));
#97485=DIRECTION('center_axis',(0.981627005099017,0.,0.190809912898503));
#97486=DIRECTION('ref_axis',(0.,-1.,0.));
#97487=DIRECTION('',(-0.190809912898503,0.,0.981627005099017));
#97488=DIRECTION('',(0.,-1.,0.));
#97489=DIRECTION('',(0.,-1.,0.));
#97490=DIRECTION('center_axis',(0.,-1.,0.));
#97491=DIRECTION('ref_axis',(0.,0.,-1.));
#97492=DIRECTION('',(-0.190809912898503,0.,0.981627005099017));
#97493=DIRECTION('',(-0.981627005099017,0.,-0.190809912898503));
#97494=DIRECTION('',(-0.981627005099017,0.,-0.190809912898503));
#97495=DIRECTION('center_axis',(-0.981627005099017,0.,-0.190809912898503));
#97496=DIRECTION('ref_axis',(-0.190809912898503,0.,0.981627005099017));
#97497=DIRECTION('',(0.,1.,0.));
#97498=DIRECTION('',(0.,1.,0.));
#97499=DIRECTION('center_axis',(0.,1.,0.));
#97500=DIRECTION('ref_axis',(1.,0.,0.));
#97501=DIRECTION('',(-0.190809912898503,0.,0.981627005099017));
#97502=DIRECTION('',(0.981627005099017,0.,0.190809912898503));
#97503=DIRECTION('',(-0.190809912898503,0.,0.981627005099017));
#97504=DIRECTION('',(0.981627005099017,0.,0.190809912898503));
#97505=DIRECTION('center_axis',(0.981627005099017,0.,0.190809912898503));
#97506=DIRECTION('ref_axis',(0.,-1.,0.));
#97507=DIRECTION('',(-0.190809912898503,0.,0.981627005099017));
#97508=DIRECTION('',(0.,-1.,0.));
#97509=DIRECTION('',(0.,-1.,0.));
#97510=DIRECTION('center_axis',(0.,-1.,0.));
#97511=DIRECTION('ref_axis',(0.,0.,-1.));
#97512=DIRECTION('',(-0.190809912898503,0.,0.981627005099017));
#97513=DIRECTION('',(-0.981627005099017,0.,-0.190809912898503));
#97514=DIRECTION('',(-0.981627005099017,0.,-0.190809912898503));
#97515=DIRECTION('center_axis',(-0.981627005099017,0.,-0.190809912898503));
#97516=DIRECTION('ref_axis',(-0.190809912898503,0.,0.981627005099017));
#97517=DIRECTION('',(0.,1.,0.));
#97518=DIRECTION('',(0.,1.,0.));
#97519=DIRECTION('center_axis',(0.,1.,0.));
#97520=DIRECTION('ref_axis',(1.,0.,0.));
#97521=DIRECTION('',(-0.190809912898503,0.,0.981627005099017));
#97522=DIRECTION('',(0.981627005099017,0.,0.190809912898503));
#97523=DIRECTION('',(-0.190809912898503,0.,0.981627005099017));
#97524=DIRECTION('',(0.981627005099017,0.,0.190809912898503));
#97525=DIRECTION('center_axis',(0.981627005099017,0.,0.190809912898503));
#97526=DIRECTION('ref_axis',(0.,-1.,0.));
#97527=DIRECTION('',(-0.190809912898503,0.,0.981627005099017));
#97528=DIRECTION('',(0.,-1.,0.));
#97529=DIRECTION('',(0.,-1.,0.));
#97530=DIRECTION('center_axis',(0.,-1.,0.));
#97531=DIRECTION('ref_axis',(0.,0.,-1.));
#97532=DIRECTION('',(-0.190809912898503,0.,0.981627005099017));
#97533=DIRECTION('',(-0.981627005099017,0.,-0.190809912898503));
#97534=DIRECTION('',(-0.981627005099017,0.,-0.190809912898503));
#97535=DIRECTION('center_axis',(-0.981627005099017,0.,-0.190809912898503));
#97536=DIRECTION('ref_axis',(-0.190809912898503,0.,0.981627005099017));
#97537=DIRECTION('',(0.,1.,0.));
#97538=DIRECTION('',(0.,1.,0.));
#97539=DIRECTION('center_axis',(0.,1.,0.));
#97540=DIRECTION('ref_axis',(1.,0.,0.));
#97541=DIRECTION('',(-0.190809912898503,0.,0.981627005099017));
#97542=DIRECTION('',(0.981627005099017,0.,0.190809912898503));
#97543=DIRECTION('',(-0.190809912898503,0.,0.981627005099017));
#97544=DIRECTION('',(0.981627005099017,0.,0.190809912898503));
#97545=DIRECTION('center_axis',(0.981627005099017,0.,0.190809912898503));
#97546=DIRECTION('ref_axis',(0.,-1.,0.));
#97547=DIRECTION('',(-0.190809912898503,0.,0.981627005099017));
#97548=DIRECTION('',(0.,-1.,0.));
#97549=DIRECTION('',(0.,-1.,0.));
#97550=DIRECTION('center_axis',(0.,-1.,0.));
#97551=DIRECTION('ref_axis',(0.,0.,-1.));
#97552=DIRECTION('',(-0.190809912898503,0.,0.981627005099017));
#97553=DIRECTION('',(-0.981627005099017,0.,-0.190809912898503));
#97554=DIRECTION('',(-0.981627005099017,0.,-0.190809912898503));
#97555=DIRECTION('center_axis',(-0.981627005099017,0.,-0.190809912898503));
#97556=DIRECTION('ref_axis',(-0.190809912898503,0.,0.981627005099017));
#97557=DIRECTION('',(0.,1.,0.));
#97558=DIRECTION('',(0.,1.,0.));
#97559=DIRECTION('center_axis',(0.,1.,0.));
#97560=DIRECTION('ref_axis',(1.,0.,0.));
#97561=DIRECTION('',(-0.190809912898503,0.,0.981627005099017));
#97562=DIRECTION('',(0.981627005099017,0.,0.190809912898503));
#97563=DIRECTION('',(-0.190809912898503,0.,0.981627005099017));
#97564=DIRECTION('',(0.981627005099017,0.,0.190809912898503));
#97565=DIRECTION('center_axis',(0.981627005099017,0.,0.190809912898503));
#97566=DIRECTION('ref_axis',(0.,-1.,0.));
#97567=DIRECTION('',(-0.190809912898503,0.,0.981627005099017));
#97568=DIRECTION('',(0.,-1.,0.));
#97569=DIRECTION('',(0.,-1.,0.));
#97570=DIRECTION('center_axis',(0.,-1.,0.));
#97571=DIRECTION('ref_axis',(0.,0.,-1.));
#97572=DIRECTION('',(-0.190809912898503,0.,0.981627005099017));
#97573=DIRECTION('',(-0.981627005099017,0.,-0.190809912898503));
#97574=DIRECTION('',(-0.981627005099017,0.,-0.190809912898503));
#97575=DIRECTION('center_axis',(-0.981627005099017,0.,-0.190809912898503));
#97576=DIRECTION('ref_axis',(-0.190809912898503,0.,0.981627005099017));
#97577=DIRECTION('',(0.,1.,0.));
#97578=DIRECTION('',(0.,1.,0.));
#97579=DIRECTION('center_axis',(0.,1.,0.));
#97580=DIRECTION('ref_axis',(1.,0.,0.));
#97581=DIRECTION('',(-0.190809912898503,0.,0.981627005099017));
#97582=DIRECTION('',(0.981627005099017,0.,0.190809912898503));
#97583=DIRECTION('',(-0.190809912898503,0.,0.981627005099017));
#97584=DIRECTION('',(0.981627005099017,0.,0.190809912898503));
#97585=DIRECTION('center_axis',(0.981627005099017,0.,0.190809912898503));
#97586=DIRECTION('ref_axis',(0.,-1.,0.));
#97587=DIRECTION('',(-0.190809912898503,0.,0.981627005099017));
#97588=DIRECTION('',(0.,-1.,0.));
#97589=DIRECTION('',(0.,-1.,0.));
#97590=DIRECTION('center_axis',(0.,-1.,0.));
#97591=DIRECTION('ref_axis',(0.,0.,-1.));
#97592=DIRECTION('',(-0.190809912898503,0.,0.981627005099017));
#97593=DIRECTION('',(-0.981627005099017,0.,-0.190809912898503));
#97594=DIRECTION('',(-0.981627005099017,0.,-0.190809912898503));
#97595=DIRECTION('center_axis',(-0.981627005099017,0.,-0.190809912898503));
#97596=DIRECTION('ref_axis',(-0.190809912898503,0.,0.981627005099017));
#97597=DIRECTION('',(0.,1.,0.));
#97598=DIRECTION('',(0.,1.,0.));
#97599=DIRECTION('center_axis',(0.,1.,0.));
#97600=DIRECTION('ref_axis',(1.,0.,0.));
#97601=DIRECTION('',(-0.190809912898503,0.,0.981627005099017));
#97602=DIRECTION('',(0.981627005099017,0.,0.190809912898503));
#97603=DIRECTION('',(-0.190809912898503,0.,0.981627005099017));
#97604=DIRECTION('',(0.981627005099017,0.,0.190809912898503));
#97605=DIRECTION('center_axis',(0.981627005099017,0.,0.190809912898503));
#97606=DIRECTION('ref_axis',(0.,-1.,0.));
#97607=DIRECTION('',(-0.190809912898503,0.,0.981627005099017));
#97608=DIRECTION('',(0.,-1.,0.));
#97609=DIRECTION('',(0.,-1.,0.));
#97610=DIRECTION('center_axis',(0.,-1.,0.));
#97611=DIRECTION('ref_axis',(0.,0.,-1.));
#97612=DIRECTION('',(-0.190809912898503,0.,0.981627005099017));
#97613=DIRECTION('',(-0.981627005099017,0.,-0.190809912898503));
#97614=DIRECTION('',(-0.981627005099017,0.,-0.190809912898503));
#97615=DIRECTION('center_axis',(-0.981627005099017,0.,-0.190809912898503));
#97616=DIRECTION('ref_axis',(-0.190809912898503,0.,0.981627005099017));
#97617=DIRECTION('',(0.,1.,0.));
#97618=DIRECTION('',(0.,1.,0.));
#97619=DIRECTION('center_axis',(0.,1.,0.));
#97620=DIRECTION('ref_axis',(1.,0.,0.));
#97621=DIRECTION('',(-0.190809912898503,0.,0.981627005099017));
#97622=DIRECTION('',(0.981627005099017,0.,0.190809912898503));
#97623=DIRECTION('',(-0.190809912898503,0.,0.981627005099017));
#97624=DIRECTION('',(0.981627005099017,0.,0.190809912898503));
#97625=DIRECTION('center_axis',(0.981627005099017,0.,0.190809912898503));
#97626=DIRECTION('ref_axis',(0.,-1.,0.));
#97627=DIRECTION('',(-0.190809912898503,0.,0.981627005099017));
#97628=DIRECTION('',(0.,-1.,0.));
#97629=DIRECTION('',(0.,-1.,0.));
#97630=DIRECTION('center_axis',(0.,-1.,0.));
#97631=DIRECTION('ref_axis',(0.,0.,-1.));
#97632=DIRECTION('',(-0.190809912898503,0.,0.981627005099017));
#97633=DIRECTION('',(-0.981627005099017,0.,-0.190809912898503));
#97634=DIRECTION('',(-0.981627005099017,0.,-0.190809912898503));
#97635=DIRECTION('center_axis',(-0.981627005099017,0.,-0.190809912898503));
#97636=DIRECTION('ref_axis',(-0.190809912898503,0.,0.981627005099017));
#97637=DIRECTION('',(0.,1.,0.));
#97638=DIRECTION('',(0.,1.,0.));
#97639=DIRECTION('center_axis',(0.,1.,0.));
#97640=DIRECTION('ref_axis',(1.,0.,0.));
#97641=DIRECTION('',(-0.190809912898503,0.,0.981627005099017));
#97642=DIRECTION('',(0.981627005099017,0.,0.190809912898503));
#97643=DIRECTION('',(-0.190809912898503,0.,0.981627005099017));
#97644=DIRECTION('',(0.981627005099017,0.,0.190809912898503));
#97645=DIRECTION('center_axis',(0.981627005099017,0.,0.190809912898503));
#97646=DIRECTION('ref_axis',(0.,-1.,0.));
#97647=DIRECTION('',(-0.190809912898503,0.,0.981627005099017));
#97648=DIRECTION('',(0.,-1.,0.));
#97649=DIRECTION('',(0.,-1.,0.));
#97650=DIRECTION('center_axis',(0.,-1.,0.));
#97651=DIRECTION('ref_axis',(0.,0.,-1.));
#97652=DIRECTION('',(-0.190809912898503,0.,0.981627005099017));
#97653=DIRECTION('',(-0.981627005099017,0.,-0.190809912898503));
#97654=DIRECTION('',(-0.981627005099017,0.,-0.190809912898503));
#97655=DIRECTION('center_axis',(-0.981627005099017,0.,-0.190809912898503));
#97656=DIRECTION('ref_axis',(-0.190809912898503,0.,0.981627005099017));
#97657=DIRECTION('',(0.,1.,0.));
#97658=DIRECTION('',(0.,1.,0.));
#97659=DIRECTION('center_axis',(0.,1.,0.));
#97660=DIRECTION('ref_axis',(1.,0.,0.));
#97661=DIRECTION('',(-0.190809912898503,0.,0.981627005099017));
#97662=DIRECTION('',(0.981627005099017,0.,0.190809912898503));
#97663=DIRECTION('',(-0.190809912898503,0.,0.981627005099017));
#97664=DIRECTION('',(0.981627005099017,0.,0.190809912898503));
#97665=DIRECTION('center_axis',(0.981627005099017,0.,0.190809912898503));
#97666=DIRECTION('ref_axis',(0.,-1.,0.));
#97667=DIRECTION('',(-0.190809912898503,0.,0.981627005099017));
#97668=DIRECTION('',(0.,-1.,0.));
#97669=DIRECTION('',(0.,-1.,0.));
#97670=DIRECTION('center_axis',(0.,-1.,0.));
#97671=DIRECTION('ref_axis',(0.,0.,-1.));
#97672=DIRECTION('',(-0.190809912898503,0.,0.981627005099017));
#97673=DIRECTION('',(-0.981627005099017,0.,-0.190809912898503));
#97674=DIRECTION('',(-0.981627005099017,0.,-0.190809912898503));
#97675=DIRECTION('center_axis',(-0.981627005099017,0.,-0.190809912898503));
#97676=DIRECTION('ref_axis',(-0.190809912898503,0.,0.981627005099017));
#97677=DIRECTION('',(0.,1.,0.));
#97678=DIRECTION('',(0.,1.,0.));
#97679=DIRECTION('center_axis',(0.,1.,0.));
#97680=DIRECTION('ref_axis',(1.,0.,0.));
#97681=DIRECTION('',(-0.190809912898503,0.,0.981627005099017));
#97682=DIRECTION('',(0.981627005099017,0.,0.190809912898503));
#97683=DIRECTION('',(-0.190809912898503,0.,0.981627005099017));
#97684=DIRECTION('',(0.981627005099017,0.,0.190809912898503));
#97685=DIRECTION('center_axis',(0.981627005099017,0.,0.190809912898503));
#97686=DIRECTION('ref_axis',(0.,-1.,0.));
#97687=DIRECTION('',(-0.190809912898503,0.,0.981627005099017));
#97688=DIRECTION('',(0.,-1.,0.));
#97689=DIRECTION('',(0.,-1.,0.));
#97690=DIRECTION('center_axis',(0.,-1.,0.));
#97691=DIRECTION('ref_axis',(0.,0.,-1.));
#97692=DIRECTION('',(-0.190809912898503,0.,0.981627005099017));
#97693=DIRECTION('',(-0.981627005099017,0.,-0.190809912898503));
#97694=DIRECTION('',(-0.981627005099017,0.,-0.190809912898503));
#97695=DIRECTION('center_axis',(-0.981627005099017,0.,-0.190809912898503));
#97696=DIRECTION('ref_axis',(-0.190809912898503,0.,0.981627005099017));
#97697=DIRECTION('',(0.,1.,0.));
#97698=DIRECTION('',(0.,1.,0.));
#97699=DIRECTION('center_axis',(0.,1.,0.));
#97700=DIRECTION('ref_axis',(1.,0.,0.));
#97701=DIRECTION('',(-0.190809912898503,0.,0.981627005099017));
#97702=DIRECTION('',(0.981627005099017,0.,0.190809912898503));
#97703=DIRECTION('',(-0.190809912898503,0.,0.981627005099017));
#97704=DIRECTION('',(0.981627005099017,0.,0.190809912898503));
#97705=DIRECTION('center_axis',(0.981627005099017,0.,0.190809912898503));
#97706=DIRECTION('ref_axis',(0.,-1.,0.));
#97707=DIRECTION('',(-0.190809912898503,0.,0.981627005099017));
#97708=DIRECTION('',(0.,-1.,0.));
#97709=DIRECTION('',(0.,-1.,0.));
#97710=DIRECTION('center_axis',(0.,-1.,0.));
#97711=DIRECTION('ref_axis',(0.,0.,-1.));
#97712=DIRECTION('',(-0.190809912898503,0.,0.981627005099017));
#97713=DIRECTION('',(-0.981627005099017,0.,-0.190809912898503));
#97714=DIRECTION('',(-0.981627005099017,0.,-0.190809912898503));
#97715=DIRECTION('center_axis',(-0.981627005099017,0.,-0.190809912898503));
#97716=DIRECTION('ref_axis',(-0.190809912898503,0.,0.981627005099017));
#97717=DIRECTION('',(0.,1.,0.));
#97718=DIRECTION('',(0.,1.,0.));
#97719=DIRECTION('center_axis',(0.,1.,0.));
#97720=DIRECTION('ref_axis',(1.,0.,0.));
#97721=DIRECTION('',(-0.190809912898503,0.,0.981627005099017));
#97722=DIRECTION('',(0.981627005099017,0.,0.190809912898503));
#97723=DIRECTION('',(-0.190809912898503,0.,0.981627005099017));
#97724=DIRECTION('',(0.981627005099017,0.,0.190809912898503));
#97725=DIRECTION('center_axis',(0.981627005099017,0.,0.190809912898503));
#97726=DIRECTION('ref_axis',(0.,-1.,0.));
#97727=DIRECTION('',(-0.190809912898503,0.,0.981627005099017));
#97728=DIRECTION('',(0.,-1.,0.));
#97729=DIRECTION('',(0.,-1.,0.));
#97730=DIRECTION('center_axis',(0.,-1.,0.));
#97731=DIRECTION('ref_axis',(0.,0.,-1.));
#97732=DIRECTION('',(-0.190809912898503,0.,0.981627005099017));
#97733=DIRECTION('',(-0.981627005099017,0.,-0.190809912898503));
#97734=DIRECTION('',(-0.981627005099017,0.,-0.190809912898503));
#97735=DIRECTION('center_axis',(-0.981627005099017,0.,-0.190809912898503));
#97736=DIRECTION('ref_axis',(-0.190809912898503,0.,0.981627005099017));
#97737=DIRECTION('',(0.,1.,0.));
#97738=DIRECTION('',(0.,1.,0.));
#97739=DIRECTION('center_axis',(0.,1.,0.));
#97740=DIRECTION('ref_axis',(1.,0.,0.));
#97741=DIRECTION('',(-0.190809912898503,0.,0.981627005099017));
#97742=DIRECTION('',(0.981627005099017,0.,0.190809912898503));
#97743=DIRECTION('',(-0.190809912898503,0.,0.981627005099017));
#97744=DIRECTION('',(0.981627005099017,0.,0.190809912898503));
#97745=DIRECTION('center_axis',(0.981627005099017,0.,0.190809912898503));
#97746=DIRECTION('ref_axis',(0.,-1.,0.));
#97747=DIRECTION('',(-0.190809912898503,0.,0.981627005099017));
#97748=DIRECTION('',(0.,-1.,0.));
#97749=DIRECTION('',(0.,-1.,0.));
#97750=DIRECTION('center_axis',(0.,-1.,0.));
#97751=DIRECTION('ref_axis',(0.,0.,-1.));
#97752=DIRECTION('',(-0.190809912898503,0.,0.981627005099017));
#97753=DIRECTION('',(-0.981627005099017,0.,-0.190809912898503));
#97754=DIRECTION('',(-0.981627005099017,0.,-0.190809912898503));
#97755=DIRECTION('center_axis',(-0.981627005099017,0.,-0.190809912898503));
#97756=DIRECTION('ref_axis',(-0.190809912898503,0.,0.981627005099017));
#97757=DIRECTION('',(0.,1.,0.));
#97758=DIRECTION('',(0.,1.,0.));
#97759=DIRECTION('center_axis',(0.,1.,0.));
#97760=DIRECTION('ref_axis',(1.,0.,0.));
#97761=DIRECTION('',(-0.190809912898503,0.,0.981627005099017));
#97762=DIRECTION('',(0.981627005099017,0.,0.190809912898503));
#97763=DIRECTION('',(-0.190809912898503,0.,0.981627005099017));
#97764=DIRECTION('',(0.981627005099017,0.,0.190809912898503));
#97765=DIRECTION('center_axis',(0.981627005099017,0.,0.190809912898503));
#97766=DIRECTION('ref_axis',(0.,-1.,0.));
#97767=DIRECTION('',(-0.190809912898503,0.,0.981627005099017));
#97768=DIRECTION('',(0.,-1.,0.));
#97769=DIRECTION('',(0.,-1.,0.));
#97770=DIRECTION('center_axis',(0.,-1.,0.));
#97771=DIRECTION('ref_axis',(0.,0.,-1.));
#97772=DIRECTION('',(-0.190809912898503,0.,0.981627005099017));
#97773=DIRECTION('',(-0.981627005099017,0.,-0.190809912898503));
#97774=DIRECTION('',(-0.981627005099017,0.,-0.190809912898503));
#97775=DIRECTION('center_axis',(-0.981627005099017,0.,-0.190809912898503));
#97776=DIRECTION('ref_axis',(-0.190809912898503,0.,0.981627005099017));
#97777=DIRECTION('',(0.,1.,0.));
#97778=DIRECTION('',(0.,1.,0.));
#97779=DIRECTION('center_axis',(0.,1.,0.));
#97780=DIRECTION('ref_axis',(1.,0.,0.));
#97781=DIRECTION('',(-0.190809912898503,0.,0.981627005099017));
#97782=DIRECTION('',(0.981627005099017,0.,0.190809912898503));
#97783=DIRECTION('',(-0.190809912898503,0.,0.981627005099017));
#97784=DIRECTION('',(0.981627005099017,0.,0.190809912898503));
#97785=DIRECTION('center_axis',(0.981627005099017,0.,0.190809912898503));
#97786=DIRECTION('ref_axis',(0.,-1.,0.));
#97787=DIRECTION('',(-0.190809912898503,0.,0.981627005099017));
#97788=DIRECTION('',(0.,-1.,0.));
#97789=DIRECTION('',(0.,-1.,0.));
#97790=DIRECTION('center_axis',(0.,-1.,0.));
#97791=DIRECTION('ref_axis',(0.,0.,-1.));
#97792=DIRECTION('',(-0.190809912898503,0.,0.981627005099017));
#97793=DIRECTION('',(-0.981627005099017,0.,-0.190809912898503));
#97794=DIRECTION('',(-0.981627005099017,0.,-0.190809912898503));
#97795=DIRECTION('center_axis',(-0.981627005099017,0.,-0.190809912898503));
#97796=DIRECTION('ref_axis',(-0.190809912898503,0.,0.981627005099017));
#97797=DIRECTION('',(0.,1.,0.));
#97798=DIRECTION('',(0.,1.,0.));
#97799=DIRECTION('center_axis',(0.,1.,0.));
#97800=DIRECTION('ref_axis',(1.,0.,0.));
#97801=DIRECTION('',(-0.190809912898503,0.,0.981627005099017));
#97802=DIRECTION('',(0.981627005099017,0.,0.190809912898503));
#97803=DIRECTION('',(-0.190809912898503,0.,0.981627005099017));
#97804=DIRECTION('',(0.981627005099017,0.,0.190809912898503));
#97805=DIRECTION('center_axis',(0.981627005099017,0.,0.190809912898503));
#97806=DIRECTION('ref_axis',(0.,-1.,0.));
#97807=DIRECTION('',(-0.190809912898503,0.,0.981627005099017));
#97808=DIRECTION('',(0.,-1.,0.));
#97809=DIRECTION('',(0.,-1.,0.));
#97810=DIRECTION('center_axis',(0.,-1.,0.));
#97811=DIRECTION('ref_axis',(0.,0.,-1.));
#97812=DIRECTION('',(-0.190809912898503,0.,0.981627005099017));
#97813=DIRECTION('',(-0.981627005099017,0.,-0.190809912898503));
#97814=DIRECTION('',(-0.981627005099017,0.,-0.190809912898503));
#97815=DIRECTION('center_axis',(-0.981627005099017,0.,-0.190809912898503));
#97816=DIRECTION('ref_axis',(-0.190809912898503,0.,0.981627005099017));
#97817=DIRECTION('',(0.,1.,0.));
#97818=DIRECTION('',(0.,1.,0.));
#97819=DIRECTION('center_axis',(0.,1.,0.));
#97820=DIRECTION('ref_axis',(1.,0.,0.));
#97821=DIRECTION('',(-0.190809912898503,0.,0.981627005099017));
#97822=DIRECTION('',(0.981627005099017,0.,0.190809912898503));
#97823=DIRECTION('',(-0.190809912898503,0.,0.981627005099017));
#97824=DIRECTION('',(0.981627005099017,0.,0.190809912898503));
#97825=DIRECTION('center_axis',(0.981627005099017,0.,0.190809912898503));
#97826=DIRECTION('ref_axis',(0.,-1.,0.));
#97827=DIRECTION('',(-0.190809912898503,0.,0.981627005099017));
#97828=DIRECTION('',(0.,-1.,0.));
#97829=DIRECTION('',(0.,-1.,0.));
#97830=DIRECTION('center_axis',(0.,-1.,0.));
#97831=DIRECTION('ref_axis',(0.,0.,-1.));
#97832=DIRECTION('',(-0.190809912898503,0.,0.981627005099017));
#97833=DIRECTION('',(-0.981627005099017,0.,-0.190809912898503));
#97834=DIRECTION('',(-0.981627005099017,0.,-0.190809912898503));
#97835=DIRECTION('center_axis',(-0.981627005099017,0.,-0.190809912898503));
#97836=DIRECTION('ref_axis',(-0.190809912898503,0.,0.981627005099017));
#97837=DIRECTION('',(0.,1.,0.));
#97838=DIRECTION('',(0.,1.,0.));
#97839=DIRECTION('center_axis',(0.,1.,0.));
#97840=DIRECTION('ref_axis',(1.,0.,0.));
#97841=DIRECTION('',(-0.190809912898503,0.,0.981627005099017));
#97842=DIRECTION('',(0.981627005099017,0.,0.190809912898503));
#97843=DIRECTION('',(-0.190809912898503,0.,0.981627005099017));
#97844=DIRECTION('',(0.981627005099017,0.,0.190809912898503));
#97845=DIRECTION('center_axis',(0.981627005099017,0.,0.190809912898503));
#97846=DIRECTION('ref_axis',(0.,-1.,0.));
#97847=DIRECTION('',(-0.190809912898503,0.,0.981627005099017));
#97848=DIRECTION('',(0.,-1.,0.));
#97849=DIRECTION('',(0.,-1.,0.));
#97850=DIRECTION('center_axis',(0.,-1.,0.));
#97851=DIRECTION('ref_axis',(0.,0.,-1.));
#97852=DIRECTION('',(-0.190809912898503,0.,0.981627005099017));
#97853=DIRECTION('',(-0.981627005099017,0.,-0.190809912898503));
#97854=DIRECTION('',(-0.981627005099017,0.,-0.190809912898503));
#97855=DIRECTION('center_axis',(-0.981627005099017,0.,-0.190809912898503));
#97856=DIRECTION('ref_axis',(-0.190809912898503,0.,0.981627005099017));
#97857=DIRECTION('',(0.,1.,0.));
#97858=DIRECTION('',(0.,1.,0.));
#97859=DIRECTION('center_axis',(0.,1.,0.));
#97860=DIRECTION('ref_axis',(1.,0.,0.));
#97861=DIRECTION('',(-0.190809912898503,0.,0.981627005099017));
#97862=DIRECTION('',(0.981627005099017,0.,0.190809912898503));
#97863=DIRECTION('',(-0.190809912898503,0.,0.981627005099017));
#97864=DIRECTION('',(0.981627005099017,0.,0.190809912898503));
#97865=DIRECTION('center_axis',(0.981627005099017,0.,0.190809912898503));
#97866=DIRECTION('ref_axis',(0.,-1.,0.));
#97867=DIRECTION('',(-0.190809912898503,0.,0.981627005099017));
#97868=DIRECTION('',(0.,-1.,0.));
#97869=DIRECTION('',(0.,-1.,0.));
#97870=DIRECTION('center_axis',(0.,-1.,0.));
#97871=DIRECTION('ref_axis',(0.,0.,-1.));
#97872=DIRECTION('',(-0.190809912898503,0.,0.981627005099017));
#97873=DIRECTION('',(-0.981627005099017,0.,-0.190809912898503));
#97874=DIRECTION('',(-0.981627005099017,0.,-0.190809912898503));
#97875=DIRECTION('center_axis',(-0.981627005099017,0.,-0.190809912898503));
#97876=DIRECTION('ref_axis',(-0.190809912898503,0.,0.981627005099017));
#97877=DIRECTION('',(0.,1.,0.));
#97878=DIRECTION('',(0.,1.,0.));
#97879=DIRECTION('center_axis',(0.,1.,0.));
#97880=DIRECTION('ref_axis',(1.,0.,0.));
#97881=DIRECTION('',(-0.190809912898503,0.,0.981627005099017));
#97882=DIRECTION('',(0.981627005099017,0.,0.190809912898503));
#97883=DIRECTION('',(-0.190809912898503,0.,0.981627005099017));
#97884=DIRECTION('',(0.981627005099017,0.,0.190809912898503));
#97885=DIRECTION('center_axis',(0.981627005099017,0.,0.190809912898503));
#97886=DIRECTION('ref_axis',(0.,-1.,0.));
#97887=DIRECTION('',(-0.190809912898503,0.,0.981627005099017));
#97888=DIRECTION('',(0.,-1.,0.));
#97889=DIRECTION('',(0.,-1.,0.));
#97890=DIRECTION('center_axis',(0.,-1.,0.));
#97891=DIRECTION('ref_axis',(0.,0.,-1.));
#97892=DIRECTION('',(-0.190809912898503,0.,0.981627005099017));
#97893=DIRECTION('',(-0.981627005099017,0.,-0.190809912898503));
#97894=DIRECTION('',(-0.981627005099017,0.,-0.190809912898503));
#97895=DIRECTION('center_axis',(-0.981627005099017,0.,-0.190809912898503));
#97896=DIRECTION('ref_axis',(-0.190809912898503,0.,0.981627005099017));
#97897=DIRECTION('',(0.,1.,0.));
#97898=DIRECTION('',(0.,1.,0.));
#97899=DIRECTION('center_axis',(0.,1.,0.));
#97900=DIRECTION('ref_axis',(1.,0.,0.));
#97901=DIRECTION('',(-0.190809912898503,0.,0.981627005099017));
#97902=DIRECTION('',(0.981627005099017,0.,0.190809912898503));
#97903=DIRECTION('',(-0.190809912898503,0.,0.981627005099017));
#97904=DIRECTION('',(0.981627005099017,0.,0.190809912898503));
#97905=DIRECTION('center_axis',(0.981627005099017,0.,0.190809912898503));
#97906=DIRECTION('ref_axis',(0.,-1.,0.));
#97907=DIRECTION('',(-0.190809912898503,0.,0.981627005099017));
#97908=DIRECTION('',(0.,-1.,0.));
#97909=DIRECTION('',(0.,-1.,0.));
#97910=DIRECTION('center_axis',(0.,-1.,0.));
#97911=DIRECTION('ref_axis',(0.,0.,-1.));
#97912=DIRECTION('',(-0.190809912898503,0.,0.981627005099017));
#97913=DIRECTION('',(-0.981627005099017,0.,-0.190809912898503));
#97914=DIRECTION('',(-0.981627005099017,0.,-0.190809912898503));
#97915=DIRECTION('center_axis',(-0.981627005099017,0.,-0.190809912898503));
#97916=DIRECTION('ref_axis',(-0.190809912898503,0.,0.981627005099017));
#97917=DIRECTION('',(0.,1.,0.));
#97918=DIRECTION('',(0.,1.,0.));
#97919=DIRECTION('center_axis',(0.,1.,0.));
#97920=DIRECTION('ref_axis',(1.,0.,0.));
#97921=DIRECTION('',(-0.190809912898503,0.,0.981627005099017));
#97922=DIRECTION('',(0.981627005099017,0.,0.190809912898503));
#97923=DIRECTION('',(-0.190809912898503,0.,0.981627005099017));
#97924=DIRECTION('',(0.981627005099017,0.,0.190809912898503));
#97925=DIRECTION('center_axis',(0.981627005099017,0.,0.190809912898503));
#97926=DIRECTION('ref_axis',(0.,-1.,0.));
#97927=DIRECTION('',(-0.190809912898503,0.,0.981627005099017));
#97928=DIRECTION('',(0.,-1.,0.));
#97929=DIRECTION('',(0.,-1.,0.));
#97930=DIRECTION('center_axis',(0.,-1.,0.));
#97931=DIRECTION('ref_axis',(0.,0.,-1.));
#97932=DIRECTION('',(-0.190809912898503,0.,0.981627005099017));
#97933=DIRECTION('',(-0.981627005099017,0.,-0.190809912898503));
#97934=DIRECTION('',(-0.981627005099017,0.,-0.190809912898503));
#97935=DIRECTION('center_axis',(-0.981627005099017,0.,-0.190809912898503));
#97936=DIRECTION('ref_axis',(-0.190809912898503,0.,0.981627005099017));
#97937=DIRECTION('',(0.,1.,0.));
#97938=DIRECTION('',(0.,1.,0.));
#97939=DIRECTION('center_axis',(0.,1.,0.));
#97940=DIRECTION('ref_axis',(1.,0.,0.));
#97941=DIRECTION('',(-0.190809912898503,0.,0.981627005099017));
#97942=DIRECTION('',(0.981627005099017,0.,0.190809912898503));
#97943=DIRECTION('',(-0.190809912898503,0.,0.981627005099017));
#97944=DIRECTION('',(0.981627005099017,0.,0.190809912898503));
#97945=DIRECTION('center_axis',(0.981627005099017,0.,0.190809912898503));
#97946=DIRECTION('ref_axis',(0.,-1.,0.));
#97947=DIRECTION('',(-0.190809912898503,0.,0.981627005099017));
#97948=DIRECTION('',(0.,-1.,0.));
#97949=DIRECTION('',(0.,-1.,0.));
#97950=DIRECTION('center_axis',(0.,-1.,0.));
#97951=DIRECTION('ref_axis',(0.,0.,-1.));
#97952=DIRECTION('',(-0.190809912898503,0.,0.981627005099017));
#97953=DIRECTION('',(-0.981627005099017,0.,-0.190809912898503));
#97954=DIRECTION('',(-0.981627005099017,0.,-0.190809912898503));
#97955=DIRECTION('center_axis',(-0.981627005099017,0.,-0.190809912898503));
#97956=DIRECTION('ref_axis',(-0.190809912898503,0.,0.981627005099017));
#97957=DIRECTION('',(0.,1.,0.));
#97958=DIRECTION('',(0.,1.,0.));
#97959=DIRECTION('center_axis',(0.,1.,0.));
#97960=DIRECTION('ref_axis',(1.,0.,0.));
#97961=DIRECTION('',(-0.190809912898503,0.,0.981627005099017));
#97962=DIRECTION('',(0.981627005099017,0.,0.190809912898503));
#97963=DIRECTION('',(-0.190809912898503,0.,0.981627005099017));
#97964=DIRECTION('',(0.981627005099017,0.,0.190809912898503));
#97965=DIRECTION('center_axis',(0.981627005099017,0.,0.190809912898503));
#97966=DIRECTION('ref_axis',(0.,-1.,0.));
#97967=DIRECTION('',(-0.190809912898503,0.,0.981627005099017));
#97968=DIRECTION('',(0.,-1.,0.));
#97969=DIRECTION('',(0.,-1.,0.));
#97970=DIRECTION('center_axis',(0.,-1.,0.));
#97971=DIRECTION('ref_axis',(0.,0.,-1.));
#97972=DIRECTION('',(-0.190809912898503,0.,0.981627005099017));
#97973=DIRECTION('',(-0.981627005099017,0.,-0.190809912898503));
#97974=DIRECTION('',(-0.981627005099017,0.,-0.190809912898503));
#97975=DIRECTION('center_axis',(-0.981627005099017,0.,-0.190809912898503));
#97976=DIRECTION('ref_axis',(-0.190809912898503,0.,0.981627005099017));
#97977=DIRECTION('',(0.,1.,0.));
#97978=DIRECTION('',(0.,1.,0.));
#97979=DIRECTION('center_axis',(0.,1.,0.));
#97980=DIRECTION('ref_axis',(1.,0.,0.));
#97981=DIRECTION('',(-0.190809912898503,0.,0.981627005099017));
#97982=DIRECTION('',(0.981627005099017,0.,0.190809912898503));
#97983=DIRECTION('',(-0.190809912898503,0.,0.981627005099017));
#97984=DIRECTION('',(0.981627005099017,0.,0.190809912898503));
#97985=DIRECTION('center_axis',(0.981627005099017,0.,0.190809912898503));
#97986=DIRECTION('ref_axis',(0.,-1.,0.));
#97987=DIRECTION('',(-0.190809912898503,0.,0.981627005099017));
#97988=DIRECTION('',(0.,-1.,0.));
#97989=DIRECTION('',(0.,-1.,0.));
#97990=DIRECTION('center_axis',(0.,-1.,0.));
#97991=DIRECTION('ref_axis',(0.,0.,-1.));
#97992=DIRECTION('',(-0.190809912898503,0.,0.981627005099017));
#97993=DIRECTION('',(-0.981627005099017,0.,-0.190809912898503));
#97994=DIRECTION('',(-0.981627005099017,0.,-0.190809912898503));
#97995=DIRECTION('center_axis',(-0.981627005099017,0.,-0.190809912898503));
#97996=DIRECTION('ref_axis',(-0.190809912898503,0.,0.981627005099017));
#97997=DIRECTION('',(0.,1.,0.));
#97998=DIRECTION('',(0.,1.,0.));
#97999=DIRECTION('center_axis',(0.,1.,0.));
#98000=DIRECTION('ref_axis',(1.,0.,0.));
#98001=DIRECTION('',(-0.190809912898503,0.,0.981627005099017));
#98002=DIRECTION('',(0.981627005099017,0.,0.190809912898503));
#98003=DIRECTION('',(-0.190809912898503,0.,0.981627005099017));
#98004=DIRECTION('',(0.981627005099017,0.,0.190809912898503));
#98005=DIRECTION('center_axis',(0.981627005099017,0.,0.190809912898503));
#98006=DIRECTION('ref_axis',(0.,-1.,0.));
#98007=DIRECTION('',(-0.190809912898503,0.,0.981627005099017));
#98008=DIRECTION('',(0.,-1.,0.));
#98009=DIRECTION('',(0.,-1.,0.));
#98010=DIRECTION('center_axis',(0.,-1.,0.));
#98011=DIRECTION('ref_axis',(0.,0.,-1.));
#98012=DIRECTION('',(-0.190809912898503,0.,0.981627005099017));
#98013=DIRECTION('',(-0.981627005099017,0.,-0.190809912898503));
#98014=DIRECTION('',(-0.981627005099017,0.,-0.190809912898503));
#98015=DIRECTION('center_axis',(-0.981627005099017,0.,-0.190809912898503));
#98016=DIRECTION('ref_axis',(-0.190809912898503,0.,0.981627005099017));
#98017=DIRECTION('',(0.,1.,0.));
#98018=DIRECTION('',(0.,1.,0.));
#98019=DIRECTION('center_axis',(0.,1.,0.));
#98020=DIRECTION('ref_axis',(1.,0.,0.));
#98021=DIRECTION('',(-0.190809912898503,0.,0.981627005099017));
#98022=DIRECTION('',(0.981627005099017,0.,0.190809912898503));
#98023=DIRECTION('',(-0.190809912898503,0.,0.981627005099017));
#98024=DIRECTION('',(0.981627005099017,0.,0.190809912898503));
#98025=DIRECTION('center_axis',(0.981627005099017,0.,0.190809912898503));
#98026=DIRECTION('ref_axis',(0.,-1.,0.));
#98027=DIRECTION('',(-0.190809912898503,0.,0.981627005099017));
#98028=DIRECTION('',(0.,-1.,0.));
#98029=DIRECTION('',(0.,-1.,0.));
#98030=DIRECTION('center_axis',(0.,-1.,0.));
#98031=DIRECTION('ref_axis',(0.,0.,-1.));
#98032=DIRECTION('',(-0.190809912898503,0.,0.981627005099017));
#98033=DIRECTION('',(-0.981627005099017,0.,-0.190809912898503));
#98034=DIRECTION('',(-0.981627005099017,0.,-0.190809912898503));
#98035=DIRECTION('center_axis',(-0.981627005099017,0.,-0.190809912898503));
#98036=DIRECTION('ref_axis',(-0.190809912898503,0.,0.981627005099017));
#98037=DIRECTION('',(0.,1.,0.));
#98038=DIRECTION('',(0.,1.,0.));
#98039=DIRECTION('center_axis',(0.,1.,0.));
#98040=DIRECTION('ref_axis',(1.,0.,0.));
#98041=DIRECTION('',(-0.190809912898503,0.,0.981627005099017));
#98042=DIRECTION('',(0.981627005099017,0.,0.190809912898503));
#98043=DIRECTION('',(-0.190809912898503,0.,0.981627005099017));
#98044=DIRECTION('',(0.981627005099017,0.,0.190809912898503));
#98045=DIRECTION('center_axis',(0.981627005099017,0.,0.190809912898503));
#98046=DIRECTION('ref_axis',(0.,-1.,0.));
#98047=DIRECTION('',(-0.190809912898503,0.,0.981627005099017));
#98048=DIRECTION('',(0.,-1.,0.));
#98049=DIRECTION('',(0.,-1.,0.));
#98050=DIRECTION('center_axis',(0.,-1.,0.));
#98051=DIRECTION('ref_axis',(0.,0.,-1.));
#98052=DIRECTION('',(-0.190809912898503,0.,0.981627005099017));
#98053=DIRECTION('',(-0.981627005099017,0.,-0.190809912898503));
#98054=DIRECTION('',(-0.981627005099017,0.,-0.190809912898503));
#98055=DIRECTION('center_axis',(-0.981627005099017,0.,-0.190809912898503));
#98056=DIRECTION('ref_axis',(-0.190809912898503,0.,0.981627005099017));
#98057=DIRECTION('',(0.,1.,0.));
#98058=DIRECTION('',(0.,1.,0.));
#98059=DIRECTION('center_axis',(0.,1.,0.));
#98060=DIRECTION('ref_axis',(1.,0.,0.));
#98061=DIRECTION('',(-0.190809912898503,0.,0.981627005099017));
#98062=DIRECTION('',(0.981627005099017,0.,0.190809912898503));
#98063=DIRECTION('',(-0.190809912898503,0.,0.981627005099017));
#98064=DIRECTION('',(0.981627005099017,0.,0.190809912898503));
#98065=DIRECTION('center_axis',(0.981627005099017,0.,0.190809912898503));
#98066=DIRECTION('ref_axis',(0.,-1.,0.));
#98067=DIRECTION('',(-0.190809912898503,0.,0.981627005099017));
#98068=DIRECTION('',(0.,-1.,0.));
#98069=DIRECTION('',(0.,-1.,0.));
#98070=DIRECTION('center_axis',(0.,-1.,0.));
#98071=DIRECTION('ref_axis',(0.,0.,-1.));
#98072=DIRECTION('',(-0.190809912898503,0.,0.981627005099017));
#98073=DIRECTION('',(-0.981627005099017,0.,-0.190809912898503));
#98074=DIRECTION('',(-0.981627005099017,0.,-0.190809912898503));
#98075=DIRECTION('center_axis',(-0.981627005099017,0.,-0.190809912898503));
#98076=DIRECTION('ref_axis',(-0.190809912898503,0.,0.981627005099017));
#98077=DIRECTION('',(0.,1.,0.));
#98078=DIRECTION('',(0.,1.,0.));
#98079=DIRECTION('center_axis',(0.,1.,0.));
#98080=DIRECTION('ref_axis',(1.,0.,0.));
#98081=DIRECTION('',(-0.190809912898503,0.,0.981627005099017));
#98082=DIRECTION('',(0.981627005099017,0.,0.190809912898503));
#98083=DIRECTION('',(-0.190809912898503,0.,0.981627005099017));
#98084=DIRECTION('',(0.981627005099017,0.,0.190809912898503));
#98085=DIRECTION('center_axis',(0.981627005099017,0.,0.190809912898503));
#98086=DIRECTION('ref_axis',(0.,-1.,0.));
#98087=DIRECTION('',(-0.190809912898503,0.,0.981627005099017));
#98088=DIRECTION('',(0.,-1.,0.));
#98089=DIRECTION('',(0.,-1.,0.));
#98090=DIRECTION('center_axis',(0.,-1.,0.));
#98091=DIRECTION('ref_axis',(0.,0.,-1.));
#98092=DIRECTION('',(-0.190809912898503,0.,0.981627005099017));
#98093=DIRECTION('',(-0.981627005099017,0.,-0.190809912898503));
#98094=DIRECTION('',(-0.981627005099017,0.,-0.190809912898503));
#98095=DIRECTION('center_axis',(-0.981627005099017,0.,-0.190809912898503));
#98096=DIRECTION('ref_axis',(-0.190809912898503,0.,0.981627005099017));
#98097=DIRECTION('',(0.,1.,0.));
#98098=DIRECTION('',(0.,1.,0.));
#98099=DIRECTION('center_axis',(0.,1.,0.));
#98100=DIRECTION('ref_axis',(1.,0.,0.));
#98101=DIRECTION('',(-0.190809912898503,0.,0.981627005099017));
#98102=DIRECTION('',(0.981627005099017,0.,0.190809912898503));
#98103=DIRECTION('',(-0.190809912898503,0.,0.981627005099017));
#98104=DIRECTION('',(0.981627005099017,0.,0.190809912898503));
#98105=DIRECTION('center_axis',(0.981627005099017,0.,0.190809912898503));
#98106=DIRECTION('ref_axis',(0.,-1.,0.));
#98107=DIRECTION('',(-0.190809912898503,0.,0.981627005099017));
#98108=DIRECTION('',(0.,-1.,0.));
#98109=DIRECTION('',(0.,-1.,0.));
#98110=DIRECTION('center_axis',(0.,-1.,0.));
#98111=DIRECTION('ref_axis',(0.,0.,-1.));
#98112=DIRECTION('',(-0.190809912898503,0.,0.981627005099017));
#98113=DIRECTION('',(-0.981627005099017,0.,-0.190809912898503));
#98114=DIRECTION('',(-0.981627005099017,0.,-0.190809912898503));
#98115=DIRECTION('center_axis',(-0.981627005099017,0.,-0.190809912898503));
#98116=DIRECTION('ref_axis',(-0.190809912898503,0.,0.981627005099017));
#98117=DIRECTION('',(0.,1.,0.));
#98118=DIRECTION('',(0.,1.,0.));
#98119=DIRECTION('center_axis',(0.,1.,0.));
#98120=DIRECTION('ref_axis',(1.,0.,0.));
#98121=DIRECTION('',(-0.190809912898503,0.,0.981627005099017));
#98122=DIRECTION('',(0.981627005099017,0.,0.190809912898503));
#98123=DIRECTION('',(-0.190809912898503,0.,0.981627005099017));
#98124=DIRECTION('',(0.981627005099017,0.,0.190809912898503));
#98125=DIRECTION('center_axis',(0.981627005099017,0.,0.190809912898503));
#98126=DIRECTION('ref_axis',(0.,-1.,0.));
#98127=DIRECTION('',(-0.190809912898503,0.,0.981627005099017));
#98128=DIRECTION('',(0.,-1.,0.));
#98129=DIRECTION('',(0.,-1.,0.));
#98130=DIRECTION('center_axis',(0.,-1.,0.));
#98131=DIRECTION('ref_axis',(0.,0.,-1.));
#98132=DIRECTION('',(-0.190809912898503,0.,0.981627005099017));
#98133=DIRECTION('',(-0.981627005099017,0.,-0.190809912898503));
#98134=DIRECTION('',(-0.981627005099017,0.,-0.190809912898503));
#98135=DIRECTION('center_axis',(-0.981627005099017,0.,-0.190809912898503));
#98136=DIRECTION('ref_axis',(-0.190809912898503,0.,0.981627005099017));
#98137=DIRECTION('',(0.,1.,0.));
#98138=DIRECTION('',(0.,1.,0.));
#98139=DIRECTION('center_axis',(0.,1.,0.));
#98140=DIRECTION('ref_axis',(1.,0.,0.));
#98141=DIRECTION('',(-0.190809912898503,0.,0.981627005099017));
#98142=DIRECTION('',(0.981627005099017,0.,0.190809912898503));
#98143=DIRECTION('',(-0.190809912898503,0.,0.981627005099017));
#98144=DIRECTION('',(0.981627005099017,0.,0.190809912898503));
#98145=DIRECTION('center_axis',(0.981627005099017,0.,0.190809912898503));
#98146=DIRECTION('ref_axis',(0.,-1.,0.));
#98147=DIRECTION('',(-0.190809912898503,0.,0.981627005099017));
#98148=DIRECTION('',(0.,-1.,0.));
#98149=DIRECTION('',(0.,-1.,0.));
#98150=DIRECTION('center_axis',(0.,-1.,0.));
#98151=DIRECTION('ref_axis',(0.,0.,-1.));
#98152=DIRECTION('',(-0.190809912898503,0.,0.981627005099017));
#98153=DIRECTION('',(-0.981627005099017,0.,-0.190809912898503));
#98154=DIRECTION('',(-0.981627005099017,0.,-0.190809912898503));
#98155=DIRECTION('center_axis',(-0.981627005099017,0.,-0.190809912898503));
#98156=DIRECTION('ref_axis',(-0.190809912898503,0.,0.981627005099017));
#98157=DIRECTION('',(0.,1.,0.));
#98158=DIRECTION('',(0.,1.,0.));
#98159=DIRECTION('center_axis',(0.,1.,0.));
#98160=DIRECTION('ref_axis',(1.,0.,0.));
#98161=DIRECTION('',(-0.190809912898503,0.,0.981627005099017));
#98162=DIRECTION('',(0.981627005099017,0.,0.190809912898503));
#98163=DIRECTION('',(-0.190809912898503,0.,0.981627005099017));
#98164=DIRECTION('',(0.981627005099017,0.,0.190809912898503));
#98165=DIRECTION('center_axis',(0.981627005099017,0.,0.190809912898503));
#98166=DIRECTION('ref_axis',(0.,-1.,0.));
#98167=DIRECTION('',(-0.190809912898503,0.,0.981627005099017));
#98168=DIRECTION('',(0.,-1.,0.));
#98169=DIRECTION('',(0.,-1.,0.));
#98170=DIRECTION('center_axis',(0.,-1.,0.));
#98171=DIRECTION('ref_axis',(0.,0.,-1.));
#98172=DIRECTION('',(-0.190809912898503,0.,0.981627005099017));
#98173=DIRECTION('',(-0.981627005099017,0.,-0.190809912898503));
#98174=DIRECTION('',(-0.981627005099017,0.,-0.190809912898503));
#98175=DIRECTION('center_axis',(-0.981627005099017,0.,-0.190809912898503));
#98176=DIRECTION('ref_axis',(-0.190809912898503,0.,0.981627005099017));
#98177=DIRECTION('',(0.,1.,0.));
#98178=DIRECTION('',(0.,1.,0.));
#98179=DIRECTION('center_axis',(0.,1.,0.));
#98180=DIRECTION('ref_axis',(1.,0.,0.));
#98181=DIRECTION('',(-0.190809912898503,0.,0.981627005099017));
#98182=DIRECTION('',(0.981627005099017,0.,0.190809912898503));
#98183=DIRECTION('',(-0.190809912898503,0.,0.981627005099017));
#98184=DIRECTION('',(0.981627005099017,0.,0.190809912898503));
#98185=DIRECTION('center_axis',(0.981627005099017,0.,0.190809912898503));
#98186=DIRECTION('ref_axis',(0.,-1.,0.));
#98187=DIRECTION('',(-0.190809912898503,0.,0.981627005099017));
#98188=DIRECTION('',(0.,-1.,0.));
#98189=DIRECTION('',(0.,-1.,0.));
#98190=DIRECTION('center_axis',(0.,-1.,0.));
#98191=DIRECTION('ref_axis',(0.,0.,-1.));
#98192=DIRECTION('',(-0.190809912898503,0.,0.981627005099017));
#98193=DIRECTION('',(-0.981627005099017,0.,-0.190809912898503));
#98194=DIRECTION('',(-0.981627005099017,0.,-0.190809912898503));
#98195=DIRECTION('center_axis',(-0.981627005099017,0.,-0.190809912898503));
#98196=DIRECTION('ref_axis',(-0.190809912898503,0.,0.981627005099017));
#98197=DIRECTION('',(0.,1.,0.));
#98198=DIRECTION('',(0.,1.,0.));
#98199=DIRECTION('center_axis',(0.,1.,0.));
#98200=DIRECTION('ref_axis',(1.,0.,0.));
#98201=DIRECTION('',(-0.190809912898503,0.,0.981627005099017));
#98202=DIRECTION('',(0.981627005099017,0.,0.190809912898503));
#98203=DIRECTION('',(-0.190809912898503,0.,0.981627005099017));
#98204=DIRECTION('',(0.981627005099017,0.,0.190809912898503));
#98205=DIRECTION('center_axis',(0.981627005099017,0.,0.190809912898503));
#98206=DIRECTION('ref_axis',(0.,-1.,0.));
#98207=DIRECTION('',(-0.190809912898503,0.,0.981627005099017));
#98208=DIRECTION('',(0.,-1.,0.));
#98209=DIRECTION('',(0.,-1.,0.));
#98210=DIRECTION('center_axis',(0.,-1.,0.));
#98211=DIRECTION('ref_axis',(0.,0.,-1.));
#98212=DIRECTION('',(-0.190809912898503,0.,0.981627005099017));
#98213=DIRECTION('',(-0.981627005099017,0.,-0.190809912898503));
#98214=DIRECTION('',(-0.981627005099017,0.,-0.190809912898503));
#98215=DIRECTION('center_axis',(-0.981627005099017,0.,-0.190809912898503));
#98216=DIRECTION('ref_axis',(-0.190809912898503,0.,0.981627005099017));
#98217=DIRECTION('',(0.,1.,0.));
#98218=DIRECTION('',(0.,1.,0.));
#98219=DIRECTION('center_axis',(0.,1.,0.));
#98220=DIRECTION('ref_axis',(1.,0.,0.));
#98221=DIRECTION('',(-0.190809912898503,0.,0.981627005099017));
#98222=DIRECTION('',(0.981627005099017,0.,0.190809912898503));
#98223=DIRECTION('',(-0.190809912898503,0.,0.981627005099017));
#98224=DIRECTION('',(0.981627005099017,0.,0.190809912898503));
#98225=DIRECTION('center_axis',(0.981627005099017,0.,0.190809912898503));
#98226=DIRECTION('ref_axis',(0.,-1.,0.));
#98227=DIRECTION('',(-0.190809912898503,0.,0.981627005099017));
#98228=DIRECTION('',(0.,-1.,0.));
#98229=DIRECTION('',(0.,-1.,0.));
#98230=DIRECTION('center_axis',(0.,-1.,0.));
#98231=DIRECTION('ref_axis',(0.,0.,-1.));
#98232=DIRECTION('',(-0.190809912898503,0.,0.981627005099017));
#98233=DIRECTION('',(-0.981627005099017,0.,-0.190809912898503));
#98234=DIRECTION('',(-0.981627005099017,0.,-0.190809912898503));
#98235=DIRECTION('center_axis',(-0.981627005099017,0.,-0.190809912898503));
#98236=DIRECTION('ref_axis',(-0.190809912898503,0.,0.981627005099017));
#98237=DIRECTION('',(0.,1.,0.));
#98238=DIRECTION('',(0.,1.,0.));
#98239=DIRECTION('center_axis',(0.,1.,0.));
#98240=DIRECTION('ref_axis',(1.,0.,0.));
#98241=DIRECTION('',(-0.190809912898503,0.,0.981627005099017));
#98242=DIRECTION('',(0.981627005099017,0.,0.190809912898503));
#98243=DIRECTION('',(-0.190809912898503,0.,0.981627005099017));
#98244=DIRECTION('',(0.981627005099017,0.,0.190809912898503));
#98245=DIRECTION('center_axis',(0.981627005099017,0.,0.190809912898503));
#98246=DIRECTION('ref_axis',(0.,-1.,0.));
#98247=DIRECTION('',(-0.190809912898503,0.,0.981627005099017));
#98248=DIRECTION('',(0.,-1.,0.));
#98249=DIRECTION('',(0.,-1.,0.));
#98250=DIRECTION('center_axis',(0.,-1.,0.));
#98251=DIRECTION('ref_axis',(0.,0.,-1.));
#98252=DIRECTION('',(-0.190809912898503,0.,0.981627005099017));
#98253=DIRECTION('',(-0.981627005099017,0.,-0.190809912898503));
#98254=DIRECTION('',(-0.981627005099017,0.,-0.190809912898503));
#98255=DIRECTION('center_axis',(-0.981627005099017,0.,-0.190809912898503));
#98256=DIRECTION('ref_axis',(-0.190809912898503,0.,0.981627005099017));
#98257=DIRECTION('',(0.,1.,0.));
#98258=DIRECTION('',(0.,1.,0.));
#98259=DIRECTION('center_axis',(0.,1.,0.));
#98260=DIRECTION('ref_axis',(1.,0.,0.));
#98261=DIRECTION('',(-0.190809912898503,0.,0.981627005099017));
#98262=DIRECTION('',(0.981627005099017,0.,0.190809912898503));
#98263=DIRECTION('',(-0.190809912898503,0.,0.981627005099017));
#98264=DIRECTION('',(0.981627005099017,0.,0.190809912898503));
#98265=DIRECTION('center_axis',(0.981627005099017,0.,0.190809912898503));
#98266=DIRECTION('ref_axis',(0.,-1.,0.));
#98267=DIRECTION('',(-0.190809912898503,0.,0.981627005099017));
#98268=DIRECTION('',(0.,-1.,0.));
#98269=DIRECTION('',(0.,-1.,0.));
#98270=DIRECTION('center_axis',(0.,-1.,0.));
#98271=DIRECTION('ref_axis',(0.,0.,-1.));
#98272=DIRECTION('',(-0.190809912898503,0.,0.981627005099017));
#98273=DIRECTION('',(-0.981627005099017,0.,-0.190809912898503));
#98274=DIRECTION('',(-0.981627005099017,0.,-0.190809912898503));
#98275=DIRECTION('center_axis',(-0.981627005099017,0.,-0.190809912898503));
#98276=DIRECTION('ref_axis',(-0.190809912898503,0.,0.981627005099017));
#98277=DIRECTION('',(0.,1.,0.));
#98278=DIRECTION('',(0.,1.,0.));
#98279=DIRECTION('center_axis',(0.,1.,0.));
#98280=DIRECTION('ref_axis',(1.,0.,0.));
#98281=DIRECTION('',(-0.190809912898503,0.,0.981627005099017));
#98282=DIRECTION('',(0.981627005099017,0.,0.190809912898503));
#98283=DIRECTION('',(-0.190809912898503,0.,0.981627005099017));
#98284=DIRECTION('',(0.981627005099017,0.,0.190809912898503));
#98285=DIRECTION('center_axis',(0.981627005099017,0.,0.190809912898503));
#98286=DIRECTION('ref_axis',(0.,-1.,0.));
#98287=DIRECTION('',(-0.190809912898503,0.,0.981627005099017));
#98288=DIRECTION('',(0.,-1.,0.));
#98289=DIRECTION('',(0.,-1.,0.));
#98290=DIRECTION('center_axis',(0.,-1.,0.));
#98291=DIRECTION('ref_axis',(0.,0.,-1.));
#98292=DIRECTION('',(-0.190809912898503,0.,0.981627005099017));
#98293=DIRECTION('',(-0.981627005099017,0.,-0.190809912898503));
#98294=DIRECTION('',(-0.981627005099017,0.,-0.190809912898503));
#98295=DIRECTION('center_axis',(-0.981627005099017,0.,-0.190809912898503));
#98296=DIRECTION('ref_axis',(-0.190809912898503,0.,0.981627005099017));
#98297=DIRECTION('',(0.,1.,0.));
#98298=DIRECTION('',(0.,1.,0.));
#98299=DIRECTION('center_axis',(0.,1.,0.));
#98300=DIRECTION('ref_axis',(1.,0.,0.));
#98301=DIRECTION('',(-0.190809912898503,0.,0.981627005099017));
#98302=DIRECTION('',(0.981627005099017,0.,0.190809912898503));
#98303=DIRECTION('',(-0.190809912898503,0.,0.981627005099017));
#98304=DIRECTION('',(0.981627005099017,0.,0.190809912898503));
#98305=DIRECTION('center_axis',(0.981627005099017,0.,0.190809912898503));
#98306=DIRECTION('ref_axis',(0.,-1.,0.));
#98307=DIRECTION('',(-0.190809912898503,0.,0.981627005099017));
#98308=DIRECTION('',(0.,-1.,0.));
#98309=DIRECTION('',(0.,-1.,0.));
#98310=DIRECTION('center_axis',(0.,-1.,0.));
#98311=DIRECTION('ref_axis',(0.,0.,-1.));
#98312=DIRECTION('',(-0.190809912898503,0.,0.981627005099017));
#98313=DIRECTION('',(-0.981627005099017,0.,-0.190809912898503));
#98314=DIRECTION('',(-0.981627005099017,0.,-0.190809912898503));
#98315=DIRECTION('center_axis',(-0.981627005099017,0.,-0.190809912898503));
#98316=DIRECTION('ref_axis',(-0.190809912898503,0.,0.981627005099017));
#98317=DIRECTION('',(0.,1.,0.));
#98318=DIRECTION('',(0.,1.,0.));
#98319=DIRECTION('center_axis',(0.,1.,0.));
#98320=DIRECTION('ref_axis',(1.,0.,0.));
#98321=DIRECTION('',(-0.190809912898503,0.,0.981627005099017));
#98322=DIRECTION('',(0.981627005099017,0.,0.190809912898503));
#98323=DIRECTION('',(-0.190809912898503,0.,0.981627005099017));
#98324=DIRECTION('',(0.981627005099017,0.,0.190809912898503));
#98325=DIRECTION('center_axis',(0.981627005099017,0.,0.190809912898503));
#98326=DIRECTION('ref_axis',(0.,-1.,0.));
#98327=DIRECTION('',(-0.190809912898503,0.,0.981627005099017));
#98328=DIRECTION('',(0.,-1.,0.));
#98329=DIRECTION('',(0.,-1.,0.));
#98330=DIRECTION('center_axis',(0.,-1.,0.));
#98331=DIRECTION('ref_axis',(0.,0.,-1.));
#98332=DIRECTION('',(-0.190809912898503,0.,0.981627005099017));
#98333=DIRECTION('',(-0.981627005099017,0.,-0.190809912898503));
#98334=DIRECTION('',(-0.981627005099017,0.,-0.190809912898503));
#98335=DIRECTION('center_axis',(-0.981627005099017,0.,-0.190809912898503));
#98336=DIRECTION('ref_axis',(-0.190809912898503,0.,0.981627005099017));
#98337=DIRECTION('',(0.,1.,0.));
#98338=DIRECTION('',(0.,1.,0.));
#98339=DIRECTION('center_axis',(0.,1.,0.));
#98340=DIRECTION('ref_axis',(1.,0.,0.));
#98341=DIRECTION('',(-0.190809912898503,0.,0.981627005099017));
#98342=DIRECTION('',(0.981627005099017,0.,0.190809912898503));
#98343=DIRECTION('',(-0.190809912898503,0.,0.981627005099017));
#98344=DIRECTION('',(0.981627005099017,0.,0.190809912898503));
#98345=DIRECTION('center_axis',(0.981627005099017,0.,0.190809912898503));
#98346=DIRECTION('ref_axis',(0.,-1.,0.));
#98347=DIRECTION('',(-0.190809912898503,0.,0.981627005099017));
#98348=DIRECTION('',(0.,-1.,0.));
#98349=DIRECTION('',(0.,-1.,0.));
#98350=DIRECTION('center_axis',(0.,-1.,0.));
#98351=DIRECTION('ref_axis',(0.,0.,-1.));
#98352=DIRECTION('',(-0.190809912898503,0.,0.981627005099017));
#98353=DIRECTION('',(-0.981627005099017,0.,-0.190809912898503));
#98354=DIRECTION('',(-0.981627005099017,0.,-0.190809912898503));
#98355=DIRECTION('center_axis',(-0.981627005099017,0.,-0.190809912898503));
#98356=DIRECTION('ref_axis',(-0.190809912898503,0.,0.981627005099017));
#98357=DIRECTION('',(0.,1.,0.));
#98358=DIRECTION('',(0.,1.,0.));
#98359=DIRECTION('center_axis',(0.,1.,0.));
#98360=DIRECTION('ref_axis',(1.,0.,0.));
#98361=DIRECTION('',(-0.190809912898503,0.,0.981627005099017));
#98362=DIRECTION('',(0.981627005099017,0.,0.190809912898503));
#98363=DIRECTION('',(-0.190809912898503,0.,0.981627005099017));
#98364=DIRECTION('',(0.981627005099017,0.,0.190809912898503));
#98365=DIRECTION('center_axis',(0.981627005099017,0.,0.190809912898503));
#98366=DIRECTION('ref_axis',(0.,-1.,0.));
#98367=DIRECTION('',(-0.190809912898503,0.,0.981627005099017));
#98368=DIRECTION('',(0.,-1.,0.));
#98369=DIRECTION('',(0.,-1.,0.));
#98370=DIRECTION('center_axis',(0.,-1.,0.));
#98371=DIRECTION('ref_axis',(0.,0.,-1.));
#98372=DIRECTION('',(-0.190809912898503,0.,0.981627005099017));
#98373=DIRECTION('',(-0.981627005099017,0.,-0.190809912898503));
#98374=DIRECTION('',(-0.981627005099017,0.,-0.190809912898503));
#98375=DIRECTION('center_axis',(-0.981627005099017,0.,-0.190809912898503));
#98376=DIRECTION('ref_axis',(-0.190809912898503,0.,0.981627005099017));
#98377=DIRECTION('',(0.,1.,0.));
#98378=DIRECTION('',(0.,1.,0.));
#98379=DIRECTION('center_axis',(0.,1.,0.));
#98380=DIRECTION('ref_axis',(1.,0.,0.));
#98381=DIRECTION('',(-0.190809912898503,0.,0.981627005099017));
#98382=DIRECTION('',(0.981627005099017,0.,0.190809912898503));
#98383=DIRECTION('',(-0.190809912898503,0.,0.981627005099017));
#98384=DIRECTION('',(0.981627005099017,0.,0.190809912898503));
#98385=DIRECTION('center_axis',(0.981627005099017,0.,0.190809912898503));
#98386=DIRECTION('ref_axis',(0.,-1.,0.));
#98387=DIRECTION('',(-0.190809912898503,0.,0.981627005099017));
#98388=DIRECTION('',(0.,-1.,0.));
#98389=DIRECTION('',(0.,-1.,0.));
#98390=DIRECTION('center_axis',(0.,-1.,0.));
#98391=DIRECTION('ref_axis',(0.,0.,-1.));
#98392=DIRECTION('',(-0.190809912898503,0.,0.981627005099017));
#98393=DIRECTION('',(-0.981627005099017,0.,-0.190809912898503));
#98394=DIRECTION('',(-0.981627005099017,0.,-0.190809912898503));
#98395=DIRECTION('center_axis',(-0.981627005099017,0.,-0.190809912898503));
#98396=DIRECTION('ref_axis',(-0.190809912898503,0.,0.981627005099017));
#98397=DIRECTION('',(0.,1.,0.));
#98398=DIRECTION('',(0.,1.,0.));
#98399=DIRECTION('center_axis',(0.,1.,0.));
#98400=DIRECTION('ref_axis',(1.,0.,0.));
#98401=DIRECTION('',(-0.190809912898503,0.,0.981627005099017));
#98402=DIRECTION('',(0.981627005099017,0.,0.190809912898503));
#98403=DIRECTION('',(-0.190809912898503,0.,0.981627005099017));
#98404=DIRECTION('',(0.981627005099017,0.,0.190809912898503));
#98405=DIRECTION('center_axis',(0.981627005099017,0.,0.190809912898503));
#98406=DIRECTION('ref_axis',(0.,-1.,0.));
#98407=DIRECTION('',(-0.190809912898503,0.,0.981627005099017));
#98408=DIRECTION('',(0.,-1.,0.));
#98409=DIRECTION('',(0.,-1.,0.));
#98410=DIRECTION('center_axis',(0.,-1.,0.));
#98411=DIRECTION('ref_axis',(0.,0.,-1.));
#98412=DIRECTION('',(-0.190809912898503,0.,0.981627005099017));
#98413=DIRECTION('',(-0.981627005099017,0.,-0.190809912898503));
#98414=DIRECTION('',(-0.981627005099017,0.,-0.190809912898503));
#98415=DIRECTION('center_axis',(-0.981627005099017,0.,-0.190809912898503));
#98416=DIRECTION('ref_axis',(-0.190809912898503,0.,0.981627005099017));
#98417=DIRECTION('',(0.,1.,0.));
#98418=DIRECTION('',(0.,1.,0.));
#98419=DIRECTION('center_axis',(0.,1.,0.));
#98420=DIRECTION('ref_axis',(1.,0.,0.));
#98421=DIRECTION('',(-0.190809912898503,0.,0.981627005099017));
#98422=DIRECTION('',(0.981627005099017,0.,0.190809912898503));
#98423=DIRECTION('',(-0.190809912898503,0.,0.981627005099017));
#98424=DIRECTION('',(0.981627005099017,0.,0.190809912898503));
#98425=DIRECTION('center_axis',(0.981627005099017,0.,0.190809912898503));
#98426=DIRECTION('ref_axis',(0.,-1.,0.));
#98427=DIRECTION('',(-0.190809912898503,0.,0.981627005099017));
#98428=DIRECTION('',(0.,-1.,0.));
#98429=DIRECTION('',(0.,-1.,0.));
#98430=DIRECTION('center_axis',(0.,-1.,0.));
#98431=DIRECTION('ref_axis',(0.,0.,-1.));
#98432=DIRECTION('',(-0.190809912898503,0.,0.981627005099017));
#98433=DIRECTION('',(-0.981627005099017,0.,-0.190809912898503));
#98434=DIRECTION('',(-0.981627005099017,0.,-0.190809912898503));
#98435=DIRECTION('center_axis',(-0.981627005099017,0.,-0.190809912898503));
#98436=DIRECTION('ref_axis',(-0.190809912898503,0.,0.981627005099017));
#98437=DIRECTION('',(0.,1.,0.));
#98438=DIRECTION('',(0.,1.,0.));
#98439=DIRECTION('center_axis',(0.,1.,0.));
#98440=DIRECTION('ref_axis',(1.,0.,0.));
#98441=DIRECTION('',(-0.190809912898503,0.,0.981627005099017));
#98442=DIRECTION('',(0.981627005099017,0.,0.190809912898503));
#98443=DIRECTION('',(-0.190809912898503,0.,0.981627005099017));
#98444=DIRECTION('',(0.981627005099017,0.,0.190809912898503));
#98445=DIRECTION('center_axis',(0.981627005099017,0.,0.190809912898503));
#98446=DIRECTION('ref_axis',(0.,-1.,0.));
#98447=DIRECTION('',(-0.190809912898503,0.,0.981627005099017));
#98448=DIRECTION('',(0.,-1.,0.));
#98449=DIRECTION('',(0.,-1.,0.));
#98450=DIRECTION('center_axis',(0.,-1.,0.));
#98451=DIRECTION('ref_axis',(0.,0.,-1.));
#98452=DIRECTION('',(-0.190809912898503,0.,0.981627005099017));
#98453=DIRECTION('',(-0.981627005099017,0.,-0.190809912898503));
#98454=DIRECTION('',(-0.981627005099017,0.,-0.190809912898503));
#98455=DIRECTION('center_axis',(-0.981627005099017,0.,-0.190809912898503));
#98456=DIRECTION('ref_axis',(-0.190809912898503,0.,0.981627005099017));
#98457=DIRECTION('',(0.,1.,0.));
#98458=DIRECTION('',(0.,1.,0.));
#98459=DIRECTION('center_axis',(0.,1.,0.));
#98460=DIRECTION('ref_axis',(1.,0.,0.));
#98461=DIRECTION('',(-0.190809912898503,0.,0.981627005099017));
#98462=DIRECTION('',(0.981627005099017,0.,0.190809912898503));
#98463=DIRECTION('',(-0.190809912898503,0.,0.981627005099017));
#98464=DIRECTION('',(0.981627005099017,0.,0.190809912898503));
#98465=DIRECTION('center_axis',(0.981627005099017,0.,0.190809912898503));
#98466=DIRECTION('ref_axis',(0.,-1.,0.));
#98467=DIRECTION('',(-0.190809912898503,0.,0.981627005099017));
#98468=DIRECTION('',(0.,-1.,0.));
#98469=DIRECTION('',(0.,-1.,0.));
#98470=DIRECTION('center_axis',(0.,-1.,0.));
#98471=DIRECTION('ref_axis',(0.,0.,-1.));
#98472=DIRECTION('',(-0.190809912898503,0.,0.981627005099017));
#98473=DIRECTION('',(-0.981627005099017,0.,-0.190809912898503));
#98474=DIRECTION('',(-0.981627005099017,0.,-0.190809912898503));
#98475=DIRECTION('center_axis',(-0.981627005099017,0.,-0.190809912898503));
#98476=DIRECTION('ref_axis',(-0.190809912898503,0.,0.981627005099017));
#98477=DIRECTION('',(0.,1.,0.));
#98478=DIRECTION('',(0.,1.,0.));
#98479=DIRECTION('center_axis',(0.,1.,0.));
#98480=DIRECTION('ref_axis',(1.,0.,0.));
#98481=DIRECTION('',(-0.190809912898503,0.,0.981627005099017));
#98482=DIRECTION('',(0.981627005099017,0.,0.190809912898503));
#98483=DIRECTION('',(-0.190809912898503,0.,0.981627005099017));
#98484=DIRECTION('',(0.981627005099017,0.,0.190809912898503));
#98485=DIRECTION('center_axis',(0.981627005099017,0.,0.190809912898503));
#98486=DIRECTION('ref_axis',(0.,-1.,0.));
#98487=DIRECTION('',(-0.190809912898503,0.,0.981627005099017));
#98488=DIRECTION('',(0.,-1.,0.));
#98489=DIRECTION('',(0.,-1.,0.));
#98490=DIRECTION('center_axis',(0.,-1.,0.));
#98491=DIRECTION('ref_axis',(0.,0.,-1.));
#98492=DIRECTION('',(-0.190809912898503,0.,0.981627005099017));
#98493=DIRECTION('',(-0.981627005099017,0.,-0.190809912898503));
#98494=DIRECTION('',(-0.981627005099017,0.,-0.190809912898503));
#98495=DIRECTION('center_axis',(-0.981627005099017,0.,-0.190809912898503));
#98496=DIRECTION('ref_axis',(-0.190809912898503,0.,0.981627005099017));
#98497=DIRECTION('',(0.,1.,0.));
#98498=DIRECTION('',(0.,1.,0.));
#98499=DIRECTION('center_axis',(0.,1.,0.));
#98500=DIRECTION('ref_axis',(1.,0.,0.));
#98501=DIRECTION('',(-0.190809912898503,0.,0.981627005099017));
#98502=DIRECTION('',(0.981627005099017,0.,0.190809912898503));
#98503=DIRECTION('',(-0.190809912898503,0.,0.981627005099017));
#98504=DIRECTION('',(0.981627005099017,0.,0.190809912898503));
#98505=DIRECTION('center_axis',(0.981627005099017,0.,0.190809912898503));
#98506=DIRECTION('ref_axis',(0.,-1.,0.));
#98507=DIRECTION('',(-0.190809912898503,0.,0.981627005099017));
#98508=DIRECTION('',(0.,-1.,0.));
#98509=DIRECTION('',(0.,-1.,0.));
#98510=DIRECTION('center_axis',(0.,-1.,0.));
#98511=DIRECTION('ref_axis',(0.,0.,-1.));
#98512=DIRECTION('',(-0.190809912898503,0.,0.981627005099017));
#98513=DIRECTION('',(-0.981627005099017,0.,-0.190809912898503));
#98514=DIRECTION('',(-0.981627005099017,0.,-0.190809912898503));
#98515=DIRECTION('center_axis',(-0.981627005099017,0.,-0.190809912898503));
#98516=DIRECTION('ref_axis',(-0.190809912898503,0.,0.981627005099017));
#98517=DIRECTION('',(0.,1.,0.));
#98518=DIRECTION('',(0.,1.,0.));
#98519=DIRECTION('center_axis',(0.,1.,0.));
#98520=DIRECTION('ref_axis',(1.,0.,0.));
#98521=DIRECTION('',(-0.190809912898503,0.,0.981627005099017));
#98522=DIRECTION('',(0.981627005099017,0.,0.190809912898503));
#98523=DIRECTION('',(-0.190809912898503,0.,0.981627005099017));
#98524=DIRECTION('',(0.981627005099017,0.,0.190809912898503));
#98525=DIRECTION('center_axis',(0.981627005099017,0.,0.190809912898503));
#98526=DIRECTION('ref_axis',(0.,-1.,0.));
#98527=DIRECTION('',(-0.190809912898503,0.,0.981627005099017));
#98528=DIRECTION('',(0.,-1.,0.));
#98529=DIRECTION('',(0.,-1.,0.));
#98530=DIRECTION('center_axis',(0.,-1.,0.));
#98531=DIRECTION('ref_axis',(0.,0.,-1.));
#98532=DIRECTION('',(-0.190809912898503,0.,0.981627005099017));
#98533=DIRECTION('',(-0.981627005099017,0.,-0.190809912898503));
#98534=DIRECTION('',(-0.981627005099017,0.,-0.190809912898503));
#98535=DIRECTION('center_axis',(-0.981627005099017,0.,-0.190809912898503));
#98536=DIRECTION('ref_axis',(-0.190809912898503,0.,0.981627005099017));
#98537=DIRECTION('',(0.,1.,0.));
#98538=DIRECTION('',(0.,1.,0.));
#98539=DIRECTION('center_axis',(0.,1.,0.));
#98540=DIRECTION('ref_axis',(1.,0.,0.));
#98541=DIRECTION('',(-0.190809912898503,0.,0.981627005099017));
#98542=DIRECTION('',(0.981627005099017,0.,0.190809912898503));
#98543=DIRECTION('',(-0.190809912898503,0.,0.981627005099017));
#98544=DIRECTION('',(0.981627005099017,0.,0.190809912898503));
#98545=DIRECTION('center_axis',(0.981627005099017,0.,0.190809912898503));
#98546=DIRECTION('ref_axis',(0.,-1.,0.));
#98547=DIRECTION('',(-0.190809912898503,0.,0.981627005099017));
#98548=DIRECTION('',(0.,-1.,0.));
#98549=DIRECTION('',(0.,-1.,0.));
#98550=DIRECTION('center_axis',(0.,-1.,0.));
#98551=DIRECTION('ref_axis',(0.,0.,-1.));
#98552=DIRECTION('',(-0.190809912898503,0.,0.981627005099017));
#98553=DIRECTION('',(-0.981627005099017,0.,-0.190809912898503));
#98554=DIRECTION('',(-0.981627005099017,0.,-0.190809912898503));
#98555=DIRECTION('center_axis',(-0.981627005099017,0.,-0.190809912898503));
#98556=DIRECTION('ref_axis',(-0.190809912898503,0.,0.981627005099017));
#98557=DIRECTION('',(0.,1.,0.));
#98558=DIRECTION('',(0.,1.,0.));
#98559=DIRECTION('center_axis',(0.,1.,0.));
#98560=DIRECTION('ref_axis',(1.,0.,0.));
#98561=DIRECTION('',(-0.190809912898503,0.,0.981627005099017));
#98562=DIRECTION('',(0.981627005099017,0.,0.190809912898503));
#98563=DIRECTION('',(-0.190809912898503,0.,0.981627005099017));
#98564=DIRECTION('',(0.981627005099017,0.,0.190809912898503));
#98565=DIRECTION('center_axis',(0.981627005099017,0.,0.190809912898503));
#98566=DIRECTION('ref_axis',(0.,-1.,0.));
#98567=DIRECTION('',(-0.190809912898503,0.,0.981627005099017));
#98568=DIRECTION('',(0.,-1.,0.));
#98569=DIRECTION('',(0.,-1.,0.));
#98570=DIRECTION('center_axis',(0.,-1.,0.));
#98571=DIRECTION('ref_axis',(0.,0.,-1.));
#98572=DIRECTION('',(-0.190809912898503,0.,0.981627005099017));
#98573=DIRECTION('',(-0.981627005099017,0.,-0.190809912898503));
#98574=DIRECTION('',(-0.981627005099017,0.,-0.190809912898503));
#98575=DIRECTION('center_axis',(-0.981627005099017,0.,-0.190809912898503));
#98576=DIRECTION('ref_axis',(-0.190809912898503,0.,0.981627005099017));
#98577=DIRECTION('',(0.,1.,0.));
#98578=DIRECTION('',(0.,1.,0.));
#98579=DIRECTION('center_axis',(0.,1.,0.));
#98580=DIRECTION('ref_axis',(1.,0.,0.));
#98581=DIRECTION('',(-0.190809912898503,0.,0.981627005099017));
#98582=DIRECTION('',(0.981627005099017,0.,0.190809912898503));
#98583=DIRECTION('',(-0.190809912898503,0.,0.981627005099017));
#98584=DIRECTION('',(0.981627005099017,0.,0.190809912898503));
#98585=DIRECTION('center_axis',(0.981627005099017,0.,0.190809912898503));
#98586=DIRECTION('ref_axis',(0.,-1.,0.));
#98587=DIRECTION('',(-0.190809912898503,0.,0.981627005099017));
#98588=DIRECTION('',(0.,-1.,0.));
#98589=DIRECTION('',(0.,-1.,0.));
#98590=DIRECTION('center_axis',(0.,-1.,0.));
#98591=DIRECTION('ref_axis',(0.,0.,-1.));
#98592=DIRECTION('',(-0.190809912898503,0.,0.981627005099017));
#98593=DIRECTION('',(-0.981627005099017,0.,-0.190809912898503));
#98594=DIRECTION('',(-0.981627005099017,0.,-0.190809912898503));
#98595=DIRECTION('center_axis',(-0.981627005099017,0.,-0.190809912898503));
#98596=DIRECTION('ref_axis',(-0.190809912898503,0.,0.981627005099017));
#98597=DIRECTION('',(0.,1.,0.));
#98598=DIRECTION('',(0.,1.,0.));
#98599=DIRECTION('center_axis',(0.,1.,0.));
#98600=DIRECTION('ref_axis',(1.,0.,0.));
#98601=DIRECTION('',(-0.190809912898503,0.,0.981627005099017));
#98602=DIRECTION('',(0.981627005099017,0.,0.190809912898503));
#98603=DIRECTION('',(-0.190809912898503,0.,0.981627005099017));
#98604=DIRECTION('',(0.981627005099017,0.,0.190809912898503));
#98605=DIRECTION('center_axis',(0.981627005099017,0.,0.190809912898503));
#98606=DIRECTION('ref_axis',(0.,-1.,0.));
#98607=DIRECTION('',(-0.190809912898503,0.,0.981627005099017));
#98608=DIRECTION('',(0.,-1.,0.));
#98609=DIRECTION('',(0.,-1.,0.));
#98610=DIRECTION('center_axis',(0.,-1.,0.));
#98611=DIRECTION('ref_axis',(0.,0.,-1.));
#98612=DIRECTION('',(-0.190809912898503,0.,0.981627005099017));
#98613=DIRECTION('',(-0.981627005099017,0.,-0.190809912898503));
#98614=DIRECTION('',(-0.981627005099017,0.,-0.190809912898503));
#98615=DIRECTION('center_axis',(-0.981627005099017,0.,-0.190809912898503));
#98616=DIRECTION('ref_axis',(-0.190809912898503,0.,0.981627005099017));
#98617=DIRECTION('',(0.,1.,0.));
#98618=DIRECTION('',(0.,1.,0.));
#98619=DIRECTION('center_axis',(0.,1.,0.));
#98620=DIRECTION('ref_axis',(1.,0.,0.));
#98621=DIRECTION('',(-0.190809912898503,0.,0.981627005099017));
#98622=DIRECTION('',(0.981627005099017,0.,0.190809912898503));
#98623=DIRECTION('',(-0.190809912898503,0.,0.981627005099017));
#98624=DIRECTION('',(0.981627005099017,0.,0.190809912898503));
#98625=DIRECTION('center_axis',(0.981627005099017,0.,0.190809912898503));
#98626=DIRECTION('ref_axis',(0.,-1.,0.));
#98627=DIRECTION('',(-0.190809912898503,0.,0.981627005099017));
#98628=DIRECTION('',(0.,-1.,0.));
#98629=DIRECTION('',(0.,-1.,0.));
#98630=DIRECTION('center_axis',(0.,-1.,0.));
#98631=DIRECTION('ref_axis',(0.,0.,-1.));
#98632=DIRECTION('',(-0.190809912898503,0.,0.981627005099017));
#98633=DIRECTION('',(-0.981627005099017,0.,-0.190809912898503));
#98634=DIRECTION('',(-0.981627005099017,0.,-0.190809912898503));
#98635=DIRECTION('center_axis',(-0.981627005099017,0.,-0.190809912898503));
#98636=DIRECTION('ref_axis',(-0.190809912898503,0.,0.981627005099017));
#98637=DIRECTION('',(0.,1.,0.));
#98638=DIRECTION('',(0.,1.,0.));
#98639=DIRECTION('center_axis',(0.,1.,0.));
#98640=DIRECTION('ref_axis',(1.,0.,0.));
#98641=DIRECTION('',(-0.190809912898503,0.,0.981627005099017));
#98642=DIRECTION('',(0.981627005099017,0.,0.190809912898503));
#98643=DIRECTION('',(-0.190809912898503,0.,0.981627005099017));
#98644=DIRECTION('',(0.981627005099017,0.,0.190809912898503));
#98645=DIRECTION('center_axis',(0.981627005099017,0.,0.190809912898503));
#98646=DIRECTION('ref_axis',(0.,-1.,0.));
#98647=DIRECTION('',(-0.190809912898503,0.,0.981627005099017));
#98648=DIRECTION('',(0.,-1.,0.));
#98649=DIRECTION('',(0.,-1.,0.));
#98650=DIRECTION('center_axis',(0.,-1.,0.));
#98651=DIRECTION('ref_axis',(0.,0.,-1.));
#98652=DIRECTION('',(-0.190809912898503,0.,0.981627005099017));
#98653=DIRECTION('',(-0.981627005099017,0.,-0.190809912898503));
#98654=DIRECTION('',(-0.981627005099017,0.,-0.190809912898503));
#98655=DIRECTION('center_axis',(-0.981627005099017,0.,-0.190809912898503));
#98656=DIRECTION('ref_axis',(-0.190809912898503,0.,0.981627005099017));
#98657=DIRECTION('',(0.,1.,0.));
#98658=DIRECTION('',(0.,1.,0.));
#98659=DIRECTION('center_axis',(0.,1.,0.));
#98660=DIRECTION('ref_axis',(1.,0.,0.));
#98661=DIRECTION('',(-0.190809912898503,0.,0.981627005099017));
#98662=DIRECTION('',(0.981627005099017,0.,0.190809912898503));
#98663=DIRECTION('',(-0.190809912898503,0.,0.981627005099017));
#98664=DIRECTION('',(0.981627005099017,0.,0.190809912898503));
#98665=DIRECTION('center_axis',(0.981627005099017,0.,0.190809912898503));
#98666=DIRECTION('ref_axis',(0.,-1.,0.));
#98667=DIRECTION('',(-0.190809912898503,0.,0.981627005099017));
#98668=DIRECTION('',(0.,-1.,0.));
#98669=DIRECTION('',(0.,-1.,0.));
#98670=DIRECTION('center_axis',(0.,-1.,0.));
#98671=DIRECTION('ref_axis',(0.,0.,-1.));
#98672=DIRECTION('',(-0.190809912898503,0.,0.981627005099017));
#98673=DIRECTION('',(-0.981627005099017,0.,-0.190809912898503));
#98674=DIRECTION('',(-0.981627005099017,0.,-0.190809912898503));
#98675=DIRECTION('center_axis',(-0.981627005099017,0.,-0.190809912898503));
#98676=DIRECTION('ref_axis',(-0.190809912898503,0.,0.981627005099017));
#98677=DIRECTION('',(0.,1.,0.));
#98678=DIRECTION('',(0.,1.,0.));
#98679=DIRECTION('center_axis',(0.,1.,0.));
#98680=DIRECTION('ref_axis',(1.,0.,0.));
#98681=DIRECTION('',(-0.190809912898503,0.,0.981627005099017));
#98682=DIRECTION('',(0.981627005099017,0.,0.190809912898503));
#98683=DIRECTION('',(-0.190809912898503,0.,0.981627005099017));
#98684=DIRECTION('',(0.981627005099017,0.,0.190809912898503));
#98685=DIRECTION('center_axis',(0.981627005099017,0.,0.190809912898503));
#98686=DIRECTION('ref_axis',(0.,-1.,0.));
#98687=DIRECTION('',(-0.190809912898503,0.,0.981627005099017));
#98688=DIRECTION('',(0.,-1.,0.));
#98689=DIRECTION('',(0.,-1.,0.));
#98690=DIRECTION('center_axis',(0.,-1.,0.));
#98691=DIRECTION('ref_axis',(0.,0.,-1.));
#98692=DIRECTION('',(-0.190809912898503,0.,0.981627005099017));
#98693=DIRECTION('',(-0.981627005099017,0.,-0.190809912898503));
#98694=DIRECTION('',(-0.981627005099017,0.,-0.190809912898503));
#98695=DIRECTION('center_axis',(-0.981627005099017,0.,-0.190809912898503));
#98696=DIRECTION('ref_axis',(-0.190809912898503,0.,0.981627005099017));
#98697=DIRECTION('',(0.,1.,0.));
#98698=DIRECTION('',(0.,1.,0.));
#98699=DIRECTION('center_axis',(0.,1.,0.));
#98700=DIRECTION('ref_axis',(1.,0.,0.));
#98701=DIRECTION('',(-0.190809912898503,0.,0.981627005099017));
#98702=DIRECTION('',(0.981627005099017,0.,0.190809912898503));
#98703=DIRECTION('',(-0.190809912898503,0.,0.981627005099017));
#98704=DIRECTION('',(0.981627005099017,0.,0.190809912898503));
#98705=DIRECTION('center_axis',(0.981627005099017,0.,0.190809912898503));
#98706=DIRECTION('ref_axis',(0.,-1.,0.));
#98707=DIRECTION('',(-0.190809912898503,0.,0.981627005099017));
#98708=DIRECTION('',(0.,-1.,0.));
#98709=DIRECTION('',(0.,-1.,0.));
#98710=DIRECTION('center_axis',(0.,-1.,0.));
#98711=DIRECTION('ref_axis',(0.,0.,-1.));
#98712=DIRECTION('',(-0.190809912898503,0.,0.981627005099017));
#98713=DIRECTION('',(-0.981627005099017,0.,-0.190809912898503));
#98714=DIRECTION('',(-0.981627005099017,0.,-0.190809912898503));
#98715=DIRECTION('center_axis',(-0.981627005099017,0.,-0.190809912898503));
#98716=DIRECTION('ref_axis',(-0.190809912898503,0.,0.981627005099017));
#98717=DIRECTION('',(0.,1.,0.));
#98718=DIRECTION('',(0.,1.,0.));
#98719=DIRECTION('center_axis',(0.,1.,0.));
#98720=DIRECTION('ref_axis',(1.,0.,0.));
#98721=DIRECTION('',(-0.190809912898503,0.,0.981627005099017));
#98722=DIRECTION('',(0.981627005099017,0.,0.190809912898503));
#98723=DIRECTION('',(-0.190809912898503,0.,0.981627005099017));
#98724=DIRECTION('',(0.981627005099017,0.,0.190809912898503));
#98725=DIRECTION('center_axis',(0.981627005099017,0.,0.190809912898503));
#98726=DIRECTION('ref_axis',(0.,-1.,0.));
#98727=DIRECTION('',(-0.190809912898503,0.,0.981627005099017));
#98728=DIRECTION('',(0.,-1.,0.));
#98729=DIRECTION('',(0.,-1.,0.));
#98730=DIRECTION('center_axis',(0.,-1.,0.));
#98731=DIRECTION('ref_axis',(0.,0.,-1.));
#98732=DIRECTION('',(-0.190809912898503,0.,0.981627005099017));
#98733=DIRECTION('',(-0.981627005099017,0.,-0.190809912898503));
#98734=DIRECTION('',(-0.981627005099017,0.,-0.190809912898503));
#98735=DIRECTION('center_axis',(-0.981627005099017,0.,-0.190809912898503));
#98736=DIRECTION('ref_axis',(-0.190809912898503,0.,0.981627005099017));
#98737=DIRECTION('',(0.,1.,0.));
#98738=DIRECTION('',(0.,1.,0.));
#98739=DIRECTION('center_axis',(0.,1.,0.));
#98740=DIRECTION('ref_axis',(1.,0.,0.));
#98741=DIRECTION('',(-0.190809912898503,0.,0.981627005099017));
#98742=DIRECTION('',(0.981627005099017,0.,0.190809912898503));
#98743=DIRECTION('',(-0.190809912898503,0.,0.981627005099017));
#98744=DIRECTION('',(0.981627005099017,0.,0.190809912898503));
#98745=DIRECTION('center_axis',(0.981627005099017,0.,0.190809912898503));
#98746=DIRECTION('ref_axis',(0.,-1.,0.));
#98747=DIRECTION('',(-0.190809912898503,0.,0.981627005099017));
#98748=DIRECTION('',(0.,-1.,0.));
#98749=DIRECTION('',(0.,-1.,0.));
#98750=DIRECTION('center_axis',(0.,-1.,0.));
#98751=DIRECTION('ref_axis',(0.,0.,-1.));
#98752=DIRECTION('',(-0.190809912898503,0.,0.981627005099017));
#98753=DIRECTION('',(-0.981627005099017,0.,-0.190809912898503));
#98754=DIRECTION('',(-0.981627005099017,0.,-0.190809912898503));
#98755=DIRECTION('center_axis',(-0.981627005099017,0.,-0.190809912898503));
#98756=DIRECTION('ref_axis',(-0.190809912898503,0.,0.981627005099017));
#98757=DIRECTION('',(0.,1.,0.));
#98758=DIRECTION('',(0.,1.,0.));
#98759=DIRECTION('center_axis',(0.,1.,0.));
#98760=DIRECTION('ref_axis',(1.,0.,0.));
#98761=DIRECTION('',(-0.190809912898503,0.,0.981627005099017));
#98762=DIRECTION('',(0.981627005099017,0.,0.190809912898503));
#98763=DIRECTION('',(-0.190809912898503,0.,0.981627005099017));
#98764=DIRECTION('',(0.981627005099017,0.,0.190809912898503));
#98765=DIRECTION('center_axis',(0.981627005099017,0.,0.190809912898503));
#98766=DIRECTION('ref_axis',(0.,-1.,0.));
#98767=DIRECTION('',(-0.190809912898503,0.,0.981627005099017));
#98768=DIRECTION('',(0.,-1.,0.));
#98769=DIRECTION('',(0.,-1.,0.));
#98770=DIRECTION('center_axis',(0.,-1.,0.));
#98771=DIRECTION('ref_axis',(0.,0.,-1.));
#98772=DIRECTION('',(-0.190809912898503,0.,0.981627005099017));
#98773=DIRECTION('',(-0.981627005099017,0.,-0.190809912898503));
#98774=DIRECTION('',(-0.981627005099017,0.,-0.190809912898503));
#98775=DIRECTION('center_axis',(-0.981627005099017,0.,-0.190809912898503));
#98776=DIRECTION('ref_axis',(-0.190809912898503,0.,0.981627005099017));
#98777=DIRECTION('',(0.,1.,0.));
#98778=DIRECTION('',(0.,1.,0.));
#98779=DIRECTION('center_axis',(0.,1.,0.));
#98780=DIRECTION('ref_axis',(1.,0.,0.));
#98781=DIRECTION('',(-0.190809912898503,0.,0.981627005099017));
#98782=DIRECTION('',(0.981627005099017,0.,0.190809912898503));
#98783=DIRECTION('',(-0.190809912898503,0.,0.981627005099017));
#98784=DIRECTION('',(0.981627005099017,0.,0.190809912898503));
#98785=DIRECTION('center_axis',(0.981627005099017,0.,0.190809912898503));
#98786=DIRECTION('ref_axis',(0.,-1.,0.));
#98787=DIRECTION('',(-0.190809912898503,0.,0.981627005099017));
#98788=DIRECTION('',(0.,-1.,0.));
#98789=DIRECTION('',(0.,-1.,0.));
#98790=DIRECTION('center_axis',(0.,-1.,0.));
#98791=DIRECTION('ref_axis',(0.,0.,-1.));
#98792=DIRECTION('',(-0.190809912898503,0.,0.981627005099017));
#98793=DIRECTION('',(-0.981627005099017,0.,-0.190809912898503));
#98794=DIRECTION('',(-0.981627005099017,0.,-0.190809912898503));
#98795=DIRECTION('center_axis',(-0.981627005099017,0.,-0.190809912898503));
#98796=DIRECTION('ref_axis',(-0.190809912898503,0.,0.981627005099017));
#98797=DIRECTION('',(0.,1.,0.));
#98798=DIRECTION('',(0.,1.,0.));
#98799=DIRECTION('center_axis',(0.,1.,0.));
#98800=DIRECTION('ref_axis',(1.,0.,0.));
#98801=DIRECTION('',(-0.190809912898503,0.,0.981627005099017));
#98802=DIRECTION('',(0.981627005099017,0.,0.190809912898503));
#98803=DIRECTION('',(-0.190809912898503,0.,0.981627005099017));
#98804=DIRECTION('',(0.981627005099017,0.,0.190809912898503));
#98805=DIRECTION('center_axis',(0.981627005099017,0.,0.190809912898503));
#98806=DIRECTION('ref_axis',(0.,-1.,0.));
#98807=DIRECTION('',(-0.190809912898503,0.,0.981627005099017));
#98808=DIRECTION('',(0.,-1.,0.));
#98809=DIRECTION('',(0.,-1.,0.));
#98810=DIRECTION('center_axis',(0.,-1.,0.));
#98811=DIRECTION('ref_axis',(0.,0.,-1.));
#98812=DIRECTION('',(-0.190809912898503,0.,0.981627005099017));
#98813=DIRECTION('',(-0.981627005099017,0.,-0.190809912898503));
#98814=DIRECTION('',(-0.981627005099017,0.,-0.190809912898503));
#98815=DIRECTION('center_axis',(-0.981627005099017,0.,-0.190809912898503));
#98816=DIRECTION('ref_axis',(-0.190809912898503,0.,0.981627005099017));
#98817=DIRECTION('',(0.,1.,0.));
#98818=DIRECTION('',(0.,1.,0.));
#98819=DIRECTION('center_axis',(0.,1.,0.));
#98820=DIRECTION('ref_axis',(1.,0.,0.));
#98821=DIRECTION('',(-0.190809912898503,0.,0.981627005099017));
#98822=DIRECTION('',(0.981627005099017,0.,0.190809912898503));
#98823=DIRECTION('',(-0.190809912898503,0.,0.981627005099017));
#98824=DIRECTION('',(0.981627005099017,0.,0.190809912898503));
#98825=DIRECTION('center_axis',(0.981627005099017,0.,0.190809912898503));
#98826=DIRECTION('ref_axis',(0.,-1.,0.));
#98827=DIRECTION('',(-0.190809912898503,0.,0.981627005099017));
#98828=DIRECTION('',(0.,-1.,0.));
#98829=DIRECTION('',(0.,-1.,0.));
#98830=DIRECTION('center_axis',(0.,-1.,0.));
#98831=DIRECTION('ref_axis',(0.,0.,-1.));
#98832=DIRECTION('',(-0.190809912898503,0.,0.981627005099017));
#98833=DIRECTION('',(-0.981627005099017,0.,-0.190809912898503));
#98834=DIRECTION('',(-0.981627005099017,0.,-0.190809912898503));
#98835=DIRECTION('center_axis',(-0.981627005099017,0.,-0.190809912898503));
#98836=DIRECTION('ref_axis',(-0.190809912898503,0.,0.981627005099017));
#98837=DIRECTION('',(0.,1.,0.));
#98838=DIRECTION('',(0.,1.,0.));
#98839=DIRECTION('center_axis',(0.,1.,0.));
#98840=DIRECTION('ref_axis',(1.,0.,0.));
#98841=DIRECTION('',(-0.190809912898503,0.,0.981627005099017));
#98842=DIRECTION('',(0.981627005099017,0.,0.190809912898503));
#98843=DIRECTION('',(-0.190809912898503,0.,0.981627005099017));
#98844=DIRECTION('',(0.981627005099017,0.,0.190809912898503));
#98845=DIRECTION('center_axis',(0.981627005099017,0.,0.190809912898503));
#98846=DIRECTION('ref_axis',(0.,-1.,0.));
#98847=DIRECTION('',(-0.190809912898503,0.,0.981627005099017));
#98848=DIRECTION('',(0.,-1.,0.));
#98849=DIRECTION('',(0.,-1.,0.));
#98850=DIRECTION('center_axis',(0.,-1.,0.));
#98851=DIRECTION('ref_axis',(0.,0.,-1.));
#98852=DIRECTION('',(-0.190809912898503,0.,0.981627005099017));
#98853=DIRECTION('',(-0.981627005099017,0.,-0.190809912898503));
#98854=DIRECTION('',(-0.981627005099017,0.,-0.190809912898503));
#98855=DIRECTION('center_axis',(-0.981627005099017,0.,-0.190809912898503));
#98856=DIRECTION('ref_axis',(-0.190809912898503,0.,0.981627005099017));
#98857=DIRECTION('',(0.,1.,0.));
#98858=DIRECTION('',(0.,1.,0.));
#98859=DIRECTION('center_axis',(0.,1.,0.));
#98860=DIRECTION('ref_axis',(1.,0.,0.));
#98861=DIRECTION('',(-0.190809912898503,0.,0.981627005099017));
#98862=DIRECTION('',(0.981627005099017,0.,0.190809912898503));
#98863=DIRECTION('',(-0.190809912898503,0.,0.981627005099017));
#98864=DIRECTION('',(0.981627005099017,0.,0.190809912898503));
#98865=DIRECTION('center_axis',(0.981627005099017,0.,0.190809912898503));
#98866=DIRECTION('ref_axis',(0.,-1.,0.));
#98867=DIRECTION('',(-0.190809912898503,0.,0.981627005099017));
#98868=DIRECTION('',(0.,-1.,0.));
#98869=DIRECTION('',(0.,-1.,0.));
#98870=DIRECTION('center_axis',(0.,-1.,0.));
#98871=DIRECTION('ref_axis',(0.,0.,-1.));
#98872=DIRECTION('',(-0.190809912898503,0.,0.981627005099017));
#98873=DIRECTION('',(-0.981627005099017,0.,-0.190809912898503));
#98874=DIRECTION('',(-0.981627005099017,0.,-0.190809912898503));
#98875=DIRECTION('center_axis',(-0.981627005099017,0.,-0.190809912898503));
#98876=DIRECTION('ref_axis',(-0.190809912898503,0.,0.981627005099017));
#98877=DIRECTION('',(0.,1.,0.));
#98878=DIRECTION('',(0.,1.,0.));
#98879=DIRECTION('center_axis',(0.,1.,0.));
#98880=DIRECTION('ref_axis',(1.,0.,0.));
#98881=DIRECTION('',(-0.190809912898503,0.,0.981627005099017));
#98882=DIRECTION('',(0.981627005099017,0.,0.190809912898503));
#98883=DIRECTION('',(-0.190809912898503,0.,0.981627005099017));
#98884=DIRECTION('',(0.981627005099017,0.,0.190809912898503));
#98885=DIRECTION('center_axis',(0.981627005099017,0.,0.190809912898503));
#98886=DIRECTION('ref_axis',(0.,-1.,0.));
#98887=DIRECTION('',(-0.190809912898503,0.,0.981627005099017));
#98888=DIRECTION('',(0.,-1.,0.));
#98889=DIRECTION('',(0.,-1.,0.));
#98890=DIRECTION('center_axis',(0.,-1.,0.));
#98891=DIRECTION('ref_axis',(0.,0.,-1.));
#98892=DIRECTION('',(-0.190809912898503,0.,0.981627005099017));
#98893=DIRECTION('',(-0.981627005099017,0.,-0.190809912898503));
#98894=DIRECTION('',(-0.981627005099017,0.,-0.190809912898503));
#98895=DIRECTION('center_axis',(-0.981627005099017,0.,-0.190809912898503));
#98896=DIRECTION('ref_axis',(-0.190809912898503,0.,0.981627005099017));
#98897=DIRECTION('',(0.,1.,0.));
#98898=DIRECTION('',(0.,1.,0.));
#98899=DIRECTION('center_axis',(0.,1.,0.));
#98900=DIRECTION('ref_axis',(1.,0.,0.));
#98901=DIRECTION('',(-0.190809912898503,0.,0.981627005099017));
#98902=DIRECTION('',(0.981627005099017,0.,0.190809912898503));
#98903=DIRECTION('',(-0.190809912898503,0.,0.981627005099017));
#98904=DIRECTION('',(0.981627005099017,0.,0.190809912898503));
#98905=DIRECTION('center_axis',(0.981627005099017,0.,0.190809912898503));
#98906=DIRECTION('ref_axis',(0.,-1.,0.));
#98907=DIRECTION('',(-0.190809912898503,0.,0.981627005099017));
#98908=DIRECTION('',(0.,-1.,0.));
#98909=DIRECTION('',(0.,-1.,0.));
#98910=DIRECTION('center_axis',(0.,-1.,0.));
#98911=DIRECTION('ref_axis',(0.,0.,-1.));
#98912=DIRECTION('',(-0.190809912898503,0.,0.981627005099017));
#98913=DIRECTION('',(-0.981627005099017,0.,-0.190809912898503));
#98914=DIRECTION('',(-0.981627005099017,0.,-0.190809912898503));
#98915=DIRECTION('center_axis',(-0.981627005099017,0.,-0.190809912898503));
#98916=DIRECTION('ref_axis',(-0.190809912898503,0.,0.981627005099017));
#98917=DIRECTION('',(0.,1.,0.));
#98918=DIRECTION('',(0.,1.,0.));
#98919=DIRECTION('center_axis',(0.,1.,0.));
#98920=DIRECTION('ref_axis',(1.,0.,0.));
#98921=DIRECTION('',(-0.190809912898503,0.,0.981627005099017));
#98922=DIRECTION('',(0.981627005099017,0.,0.190809912898503));
#98923=DIRECTION('',(-0.190809912898503,0.,0.981627005099017));
#98924=DIRECTION('',(0.981627005099017,0.,0.190809912898503));
#98925=DIRECTION('center_axis',(0.981627005099017,0.,0.190809912898503));
#98926=DIRECTION('ref_axis',(0.,-1.,0.));
#98927=DIRECTION('',(-0.190809912898503,0.,0.981627005099017));
#98928=DIRECTION('',(0.,-1.,0.));
#98929=DIRECTION('',(0.,-1.,0.));
#98930=DIRECTION('center_axis',(0.,-1.,0.));
#98931=DIRECTION('ref_axis',(0.,0.,-1.));
#98932=DIRECTION('',(-0.190809912898503,0.,0.981627005099017));
#98933=DIRECTION('',(-0.981627005099017,0.,-0.190809912898503));
#98934=DIRECTION('',(-0.981627005099017,0.,-0.190809912898503));
#98935=DIRECTION('center_axis',(-0.981627005099017,0.,-0.190809912898503));
#98936=DIRECTION('ref_axis',(-0.190809912898503,0.,0.981627005099017));
#98937=DIRECTION('',(0.,1.,0.));
#98938=DIRECTION('',(0.,1.,0.));
#98939=DIRECTION('center_axis',(0.,1.,0.));
#98940=DIRECTION('ref_axis',(1.,0.,0.));
#98941=DIRECTION('',(-0.190809912898503,0.,0.981627005099017));
#98942=DIRECTION('',(0.981627005099017,0.,0.190809912898503));
#98943=DIRECTION('',(-0.190809912898503,0.,0.981627005099017));
#98944=DIRECTION('',(0.981627005099017,0.,0.190809912898503));
#98945=DIRECTION('center_axis',(0.981627005099017,0.,0.190809912898503));
#98946=DIRECTION('ref_axis',(0.,-1.,0.));
#98947=DIRECTION('',(-0.190809912898503,0.,0.981627005099017));
#98948=DIRECTION('',(0.,-1.,0.));
#98949=DIRECTION('',(0.,-1.,0.));
#98950=DIRECTION('center_axis',(0.,-1.,0.));
#98951=DIRECTION('ref_axis',(0.,0.,-1.));
#98952=DIRECTION('',(-0.190809912898503,0.,0.981627005099017));
#98953=DIRECTION('',(-0.981627005099017,0.,-0.190809912898503));
#98954=DIRECTION('',(-0.981627005099017,0.,-0.190809912898503));
#98955=DIRECTION('center_axis',(-0.981627005099017,0.,-0.190809912898503));
#98956=DIRECTION('ref_axis',(-0.190809912898503,0.,0.981627005099017));
#98957=DIRECTION('',(0.,1.,0.));
#98958=DIRECTION('',(0.,1.,0.));
#98959=DIRECTION('center_axis',(0.,1.,0.));
#98960=DIRECTION('ref_axis',(1.,0.,0.));
#98961=DIRECTION('',(-0.190809912898503,0.,0.981627005099017));
#98962=DIRECTION('',(0.981627005099017,0.,0.190809912898503));
#98963=DIRECTION('',(-0.190809912898503,0.,0.981627005099017));
#98964=DIRECTION('',(0.981627005099017,0.,0.190809912898503));
#98965=DIRECTION('center_axis',(0.981627005099017,0.,0.190809912898503));
#98966=DIRECTION('ref_axis',(0.,-1.,0.));
#98967=DIRECTION('',(-0.190809912898503,0.,0.981627005099017));
#98968=DIRECTION('',(0.,-1.,0.));
#98969=DIRECTION('',(0.,-1.,0.));
#98970=DIRECTION('center_axis',(0.,-1.,0.));
#98971=DIRECTION('ref_axis',(0.,0.,-1.));
#98972=DIRECTION('',(-0.190809912898503,0.,0.981627005099017));
#98973=DIRECTION('',(-0.981627005099017,0.,-0.190809912898503));
#98974=DIRECTION('',(-0.981627005099017,0.,-0.190809912898503));
#98975=DIRECTION('center_axis',(-0.981627005099017,0.,-0.190809912898503));
#98976=DIRECTION('ref_axis',(-0.190809912898503,0.,0.981627005099017));
#98977=DIRECTION('',(0.,1.,0.));
#98978=DIRECTION('',(0.,1.,0.));
#98979=DIRECTION('center_axis',(0.,1.,0.));
#98980=DIRECTION('ref_axis',(1.,0.,0.));
#98981=DIRECTION('',(-0.190809912898503,0.,0.981627005099017));
#98982=DIRECTION('',(0.981627005099017,0.,0.190809912898503));
#98983=DIRECTION('',(-0.190809912898503,0.,0.981627005099017));
#98984=DIRECTION('',(0.981627005099017,0.,0.190809912898503));
#98985=DIRECTION('center_axis',(0.981627005099017,0.,0.190809912898503));
#98986=DIRECTION('ref_axis',(0.,-1.,0.));
#98987=DIRECTION('',(-0.190809912898503,0.,0.981627005099017));
#98988=DIRECTION('',(0.,-1.,0.));
#98989=DIRECTION('',(0.,-1.,0.));
#98990=DIRECTION('center_axis',(0.,-1.,0.));
#98991=DIRECTION('ref_axis',(0.,0.,-1.));
#98992=DIRECTION('',(-0.190809912898503,0.,0.981627005099017));
#98993=DIRECTION('',(-0.981627005099017,0.,-0.190809912898503));
#98994=DIRECTION('',(-0.981627005099017,0.,-0.190809912898503));
#98995=DIRECTION('center_axis',(-0.981627005099017,0.,-0.190809912898503));
#98996=DIRECTION('ref_axis',(-0.190809912898503,0.,0.981627005099017));
#98997=DIRECTION('',(0.,1.,0.));
#98998=DIRECTION('',(0.,1.,0.));
#98999=DIRECTION('center_axis',(0.,1.,0.));
#99000=DIRECTION('ref_axis',(1.,0.,0.));
#99001=DIRECTION('',(-0.190809912898503,0.,0.981627005099017));
#99002=DIRECTION('',(0.981627005099017,0.,0.190809912898503));
#99003=DIRECTION('',(-0.190809912898503,0.,0.981627005099017));
#99004=DIRECTION('',(0.981627005099017,0.,0.190809912898503));
#99005=DIRECTION('center_axis',(0.981627005099017,0.,0.190809912898503));
#99006=DIRECTION('ref_axis',(0.,-1.,0.));
#99007=DIRECTION('',(-0.190809912898503,0.,0.981627005099017));
#99008=DIRECTION('',(0.,-1.,0.));
#99009=DIRECTION('',(0.,-1.,0.));
#99010=DIRECTION('center_axis',(0.,-1.,0.));
#99011=DIRECTION('ref_axis',(0.,0.,-1.));
#99012=DIRECTION('',(-0.190809912898503,0.,0.981627005099017));
#99013=DIRECTION('',(-0.981627005099017,0.,-0.190809912898503));
#99014=DIRECTION('',(-0.981627005099017,0.,-0.190809912898503));
#99015=DIRECTION('center_axis',(-0.981627005099017,0.,-0.190809912898503));
#99016=DIRECTION('ref_axis',(-0.190809912898503,0.,0.981627005099017));
#99017=DIRECTION('',(0.,1.,0.));
#99018=DIRECTION('',(0.,1.,0.));
#99019=DIRECTION('center_axis',(0.,1.,0.));
#99020=DIRECTION('ref_axis',(1.,0.,0.));
#99021=DIRECTION('',(-0.190809912898503,0.,0.981627005099017));
#99022=DIRECTION('',(0.981627005099017,0.,0.190809912898503));
#99023=DIRECTION('',(-0.190809912898503,0.,0.981627005099017));
#99024=DIRECTION('',(0.981627005099017,0.,0.190809912898503));
#99025=DIRECTION('center_axis',(0.981627005099017,0.,0.190809912898503));
#99026=DIRECTION('ref_axis',(0.,-1.,0.));
#99027=DIRECTION('',(-0.190809912898503,0.,0.981627005099017));
#99028=DIRECTION('',(0.,-1.,0.));
#99029=DIRECTION('',(0.,-1.,0.));
#99030=DIRECTION('center_axis',(0.,-1.,0.));
#99031=DIRECTION('ref_axis',(0.,0.,-1.));
#99032=DIRECTION('',(-0.190809912898503,0.,0.981627005099017));
#99033=DIRECTION('',(-0.981627005099017,0.,-0.190809912898503));
#99034=DIRECTION('',(-0.981627005099017,0.,-0.190809912898503));
#99035=DIRECTION('center_axis',(-0.981627005099017,0.,-0.190809912898503));
#99036=DIRECTION('ref_axis',(-0.190809912898503,0.,0.981627005099017));
#99037=DIRECTION('',(0.,1.,0.));
#99038=DIRECTION('',(0.,1.,0.));
#99039=DIRECTION('center_axis',(0.,1.,0.));
#99040=DIRECTION('ref_axis',(1.,0.,0.));
#99041=DIRECTION('',(-0.190809912898503,0.,0.981627005099017));
#99042=DIRECTION('',(0.981627005099017,0.,0.190809912898503));
#99043=DIRECTION('',(-0.190809912898503,0.,0.981627005099017));
#99044=DIRECTION('',(0.981627005099017,0.,0.190809912898503));
#99045=DIRECTION('center_axis',(0.981627005099017,0.,0.190809912898503));
#99046=DIRECTION('ref_axis',(0.,-1.,0.));
#99047=DIRECTION('',(-0.190809912898503,0.,0.981627005099017));
#99048=DIRECTION('',(0.,-1.,0.));
#99049=DIRECTION('',(0.,-1.,0.));
#99050=DIRECTION('center_axis',(0.,-1.,0.));
#99051=DIRECTION('ref_axis',(0.,0.,-1.));
#99052=DIRECTION('',(-0.190809912898503,0.,0.981627005099017));
#99053=DIRECTION('',(-0.981627005099017,0.,-0.190809912898503));
#99054=DIRECTION('',(-0.981627005099017,0.,-0.190809912898503));
#99055=DIRECTION('center_axis',(-0.981627005099017,0.,-0.190809912898503));
#99056=DIRECTION('ref_axis',(-0.190809912898503,0.,0.981627005099017));
#99057=DIRECTION('',(0.,1.,0.));
#99058=DIRECTION('',(0.,1.,0.));
#99059=DIRECTION('center_axis',(0.,1.,0.));
#99060=DIRECTION('ref_axis',(1.,0.,0.));
#99061=DIRECTION('',(-0.190809912898503,0.,0.981627005099017));
#99062=DIRECTION('',(0.981627005099017,0.,0.190809912898503));
#99063=DIRECTION('',(-0.190809912898503,0.,0.981627005099017));
#99064=DIRECTION('',(0.981627005099017,0.,0.190809912898503));
#99065=DIRECTION('center_axis',(0.981627005099017,0.,0.190809912898503));
#99066=DIRECTION('ref_axis',(0.,-1.,0.));
#99067=DIRECTION('',(-0.190809912898503,0.,0.981627005099017));
#99068=DIRECTION('',(0.,-1.,0.));
#99069=DIRECTION('',(0.,-1.,0.));
#99070=DIRECTION('center_axis',(0.,-1.,0.));
#99071=DIRECTION('ref_axis',(0.,0.,-1.));
#99072=DIRECTION('',(-0.190809912898503,0.,0.981627005099017));
#99073=DIRECTION('',(-0.981627005099017,0.,-0.190809912898503));
#99074=DIRECTION('',(-0.981627005099017,0.,-0.190809912898503));
#99075=DIRECTION('center_axis',(-0.981627005099017,0.,-0.190809912898503));
#99076=DIRECTION('ref_axis',(-0.190809912898503,0.,0.981627005099017));
#99077=DIRECTION('',(0.,1.,0.));
#99078=DIRECTION('',(0.,1.,0.));
#99079=DIRECTION('center_axis',(0.,1.,0.));
#99080=DIRECTION('ref_axis',(1.,0.,0.));
#99081=DIRECTION('',(-0.190809912898503,0.,0.981627005099017));
#99082=DIRECTION('',(0.981627005099017,0.,0.190809912898503));
#99083=DIRECTION('',(-0.190809912898503,0.,0.981627005099017));
#99084=DIRECTION('',(0.981627005099017,0.,0.190809912898503));
#99085=DIRECTION('center_axis',(0.981627005099017,0.,0.190809912898503));
#99086=DIRECTION('ref_axis',(0.,-1.,0.));
#99087=DIRECTION('',(-0.190809912898503,0.,0.981627005099017));
#99088=DIRECTION('',(0.,-1.,0.));
#99089=DIRECTION('',(0.,-1.,0.));
#99090=DIRECTION('center_axis',(0.,-1.,0.));
#99091=DIRECTION('ref_axis',(0.,0.,-1.));
#99092=DIRECTION('',(-0.190809912898503,0.,0.981627005099017));
#99093=DIRECTION('',(-0.981627005099017,0.,-0.190809912898503));
#99094=DIRECTION('',(-0.981627005099017,0.,-0.190809912898503));
#99095=DIRECTION('center_axis',(-0.981627005099017,0.,-0.190809912898503));
#99096=DIRECTION('ref_axis',(-0.190809912898503,0.,0.981627005099017));
#99097=DIRECTION('',(0.,1.,0.));
#99098=DIRECTION('',(0.,1.,0.));
#99099=DIRECTION('center_axis',(0.,1.,0.));
#99100=DIRECTION('ref_axis',(1.,0.,0.));
#99101=DIRECTION('',(-0.190809912898503,0.,0.981627005099017));
#99102=DIRECTION('',(0.981627005099017,0.,0.190809912898503));
#99103=DIRECTION('',(-0.190809912898503,0.,0.981627005099017));
#99104=DIRECTION('',(0.981627005099017,0.,0.190809912898503));
#99105=DIRECTION('center_axis',(0.981627005099017,0.,0.190809912898503));
#99106=DIRECTION('ref_axis',(0.,-1.,0.));
#99107=DIRECTION('',(-0.190809912898503,0.,0.981627005099017));
#99108=DIRECTION('',(0.,-1.,0.));
#99109=DIRECTION('',(0.,-1.,0.));
#99110=DIRECTION('center_axis',(0.,-1.,0.));
#99111=DIRECTION('ref_axis',(0.,0.,-1.));
#99112=DIRECTION('',(-0.190809912898503,0.,0.981627005099017));
#99113=DIRECTION('',(-0.981627005099017,0.,-0.190809912898503));
#99114=DIRECTION('',(-0.981627005099017,0.,-0.190809912898503));
#99115=DIRECTION('center_axis',(-0.981627005099017,0.,-0.190809912898503));
#99116=DIRECTION('ref_axis',(-0.190809912898503,0.,0.981627005099017));
#99117=DIRECTION('',(0.,1.,0.));
#99118=DIRECTION('',(0.,1.,0.));
#99119=DIRECTION('center_axis',(0.,1.,0.));
#99120=DIRECTION('ref_axis',(1.,0.,0.));
#99121=DIRECTION('',(-0.190809912898503,0.,0.981627005099017));
#99122=DIRECTION('',(0.981627005099017,0.,0.190809912898503));
#99123=DIRECTION('',(-0.190809912898503,0.,0.981627005099017));
#99124=DIRECTION('',(0.981627005099017,0.,0.190809912898503));
#99125=DIRECTION('center_axis',(0.981627005099017,0.,0.190809912898503));
#99126=DIRECTION('ref_axis',(0.,-1.,0.));
#99127=DIRECTION('',(-0.190809912898503,0.,0.981627005099017));
#99128=DIRECTION('',(0.,-1.,0.));
#99129=DIRECTION('',(0.,-1.,0.));
#99130=DIRECTION('center_axis',(0.,-1.,0.));
#99131=DIRECTION('ref_axis',(0.,0.,-1.));
#99132=DIRECTION('',(-0.190809912898503,0.,0.981627005099017));
#99133=DIRECTION('',(-0.981627005099017,0.,-0.190809912898503));
#99134=DIRECTION('',(-0.981627005099017,0.,-0.190809912898503));
#99135=DIRECTION('center_axis',(-0.981627005099017,0.,-0.190809912898503));
#99136=DIRECTION('ref_axis',(-0.190809912898503,0.,0.981627005099017));
#99137=DIRECTION('',(0.,1.,0.));
#99138=DIRECTION('',(0.,1.,0.));
#99139=DIRECTION('center_axis',(0.,1.,0.));
#99140=DIRECTION('ref_axis',(1.,0.,0.));
#99141=DIRECTION('',(-0.190809912898503,0.,0.981627005099017));
#99142=DIRECTION('',(0.981627005099017,0.,0.190809912898503));
#99143=DIRECTION('',(-0.190809912898503,0.,0.981627005099017));
#99144=DIRECTION('',(0.981627005099017,0.,0.190809912898503));
#99145=DIRECTION('center_axis',(0.981627005099017,0.,0.190809912898503));
#99146=DIRECTION('ref_axis',(0.,-1.,0.));
#99147=DIRECTION('',(-0.190809912898503,0.,0.981627005099017));
#99148=DIRECTION('',(0.,-1.,0.));
#99149=DIRECTION('',(0.,-1.,0.));
#99150=DIRECTION('center_axis',(0.,-1.,0.));
#99151=DIRECTION('ref_axis',(0.,0.,-1.));
#99152=DIRECTION('',(-0.190809912898503,0.,0.981627005099017));
#99153=DIRECTION('',(-0.981627005099017,0.,-0.190809912898503));
#99154=DIRECTION('',(-0.981627005099017,0.,-0.190809912898503));
#99155=DIRECTION('center_axis',(-0.981627005099017,0.,-0.190809912898503));
#99156=DIRECTION('ref_axis',(-0.190809912898503,0.,0.981627005099017));
#99157=DIRECTION('',(0.,1.,0.));
#99158=DIRECTION('',(0.,1.,0.));
#99159=DIRECTION('center_axis',(0.,1.,0.));
#99160=DIRECTION('ref_axis',(1.,0.,0.));
#99161=DIRECTION('',(-0.190809912898503,0.,0.981627005099017));
#99162=DIRECTION('',(0.981627005099017,0.,0.190809912898503));
#99163=DIRECTION('',(-0.190809912898503,0.,0.981627005099017));
#99164=DIRECTION('',(0.981627005099017,0.,0.190809912898503));
#99165=DIRECTION('center_axis',(0.981627005099017,0.,0.190809912898503));
#99166=DIRECTION('ref_axis',(0.,-1.,0.));
#99167=DIRECTION('',(-0.190809912898503,0.,0.981627005099017));
#99168=DIRECTION('',(0.,-1.,0.));
#99169=DIRECTION('',(0.,-1.,0.));
#99170=DIRECTION('center_axis',(0.,-1.,0.));
#99171=DIRECTION('ref_axis',(0.,0.,-1.));
#99172=DIRECTION('',(-0.190809912898503,0.,0.981627005099017));
#99173=DIRECTION('',(-0.981627005099017,0.,-0.190809912898503));
#99174=DIRECTION('',(-0.981627005099017,0.,-0.190809912898503));
#99175=DIRECTION('center_axis',(-0.981627005099017,0.,-0.190809912898503));
#99176=DIRECTION('ref_axis',(-0.190809912898503,0.,0.981627005099017));
#99177=DIRECTION('',(0.,1.,0.));
#99178=DIRECTION('',(0.,1.,0.));
#99179=DIRECTION('center_axis',(0.,1.,0.));
#99180=DIRECTION('ref_axis',(1.,0.,0.));
#99181=DIRECTION('',(-0.190809912898503,0.,0.981627005099017));
#99182=DIRECTION('',(0.981627005099017,0.,0.190809912898503));
#99183=DIRECTION('',(-0.190809912898503,0.,0.981627005099017));
#99184=DIRECTION('',(0.981627005099017,0.,0.190809912898503));
#99185=DIRECTION('center_axis',(0.981627005099017,0.,0.190809912898503));
#99186=DIRECTION('ref_axis',(0.,-1.,0.));
#99187=DIRECTION('',(-0.190809912898503,0.,0.981627005099017));
#99188=DIRECTION('',(0.,-1.,0.));
#99189=DIRECTION('',(0.,-1.,0.));
#99190=DIRECTION('center_axis',(0.,-1.,0.));
#99191=DIRECTION('ref_axis',(0.,0.,-1.));
#99192=DIRECTION('',(-0.190809912898503,0.,0.981627005099017));
#99193=DIRECTION('',(-0.981627005099017,0.,-0.190809912898503));
#99194=DIRECTION('',(-0.981627005099017,0.,-0.190809912898503));
#99195=DIRECTION('center_axis',(-0.981627005099017,0.,-0.190809912898503));
#99196=DIRECTION('ref_axis',(-0.190809912898503,0.,0.981627005099017));
#99197=DIRECTION('',(0.,1.,0.));
#99198=DIRECTION('',(0.,1.,0.));
#99199=DIRECTION('center_axis',(0.,1.,0.));
#99200=DIRECTION('ref_axis',(1.,0.,0.));
#99201=DIRECTION('',(-0.190809912898503,0.,0.981627005099017));
#99202=DIRECTION('',(0.981627005099017,0.,0.190809912898503));
#99203=DIRECTION('',(-0.190809912898503,0.,0.981627005099017));
#99204=DIRECTION('',(0.981627005099017,0.,0.190809912898503));
#99205=DIRECTION('center_axis',(0.981627005099017,0.,0.190809912898503));
#99206=DIRECTION('ref_axis',(0.,-1.,0.));
#99207=DIRECTION('',(-0.190809912898503,0.,0.981627005099017));
#99208=DIRECTION('',(0.,-1.,0.));
#99209=DIRECTION('',(0.,-1.,0.));
#99210=DIRECTION('center_axis',(0.,-1.,0.));
#99211=DIRECTION('ref_axis',(0.,0.,-1.));
#99212=DIRECTION('',(-0.190809912898503,0.,0.981627005099017));
#99213=DIRECTION('',(-0.981627005099017,0.,-0.190809912898503));
#99214=DIRECTION('',(-0.981627005099017,0.,-0.190809912898503));
#99215=DIRECTION('center_axis',(-0.981627005099017,0.,-0.190809912898503));
#99216=DIRECTION('ref_axis',(-0.190809912898503,0.,0.981627005099017));
#99217=DIRECTION('',(0.,1.,0.));
#99218=DIRECTION('',(0.,1.,0.));
#99219=DIRECTION('center_axis',(0.,1.,0.));
#99220=DIRECTION('ref_axis',(1.,0.,0.));
#99221=DIRECTION('',(-0.190809912898503,0.,0.981627005099017));
#99222=DIRECTION('',(0.981627005099017,0.,0.190809912898503));
#99223=DIRECTION('',(-0.190809912898503,0.,0.981627005099017));
#99224=DIRECTION('',(0.981627005099017,0.,0.190809912898503));
#99225=DIRECTION('center_axis',(0.981627005099017,0.,0.190809912898503));
#99226=DIRECTION('ref_axis',(0.,-1.,0.));
#99227=DIRECTION('',(-0.190809912898503,0.,0.981627005099017));
#99228=DIRECTION('',(0.,-1.,0.));
#99229=DIRECTION('',(0.,-1.,0.));
#99230=DIRECTION('center_axis',(0.,-1.,0.));
#99231=DIRECTION('ref_axis',(0.,0.,-1.));
#99232=DIRECTION('',(-0.190809912898503,0.,0.981627005099017));
#99233=DIRECTION('',(-0.981627005099017,0.,-0.190809912898503));
#99234=DIRECTION('',(-0.981627005099017,0.,-0.190809912898503));
#99235=DIRECTION('center_axis',(-0.981627005099017,0.,-0.190809912898503));
#99236=DIRECTION('ref_axis',(-0.190809912898503,0.,0.981627005099017));
#99237=DIRECTION('',(0.,1.,0.));
#99238=DIRECTION('',(0.,1.,0.));
#99239=DIRECTION('center_axis',(0.,1.,0.));
#99240=DIRECTION('ref_axis',(1.,0.,0.));
#99241=DIRECTION('',(-0.190809912898503,0.,0.981627005099017));
#99242=DIRECTION('',(0.981627005099017,0.,0.190809912898503));
#99243=DIRECTION('',(-0.190809912898503,0.,0.981627005099017));
#99244=DIRECTION('',(0.981627005099017,0.,0.190809912898503));
#99245=DIRECTION('center_axis',(0.981627005099017,0.,0.190809912898503));
#99246=DIRECTION('ref_axis',(0.,-1.,0.));
#99247=DIRECTION('',(-0.190809912898503,0.,0.981627005099017));
#99248=DIRECTION('',(0.,-1.,0.));
#99249=DIRECTION('',(0.,-1.,0.));
#99250=DIRECTION('center_axis',(0.,-1.,0.));
#99251=DIRECTION('ref_axis',(0.,0.,-1.));
#99252=DIRECTION('',(-0.190809912898503,0.,0.981627005099017));
#99253=DIRECTION('',(-0.981627005099017,0.,-0.190809912898503));
#99254=DIRECTION('',(-0.981627005099017,0.,-0.190809912898503));
#99255=DIRECTION('center_axis',(-0.981627005099017,0.,-0.190809912898503));
#99256=DIRECTION('ref_axis',(-0.190809912898503,0.,0.981627005099017));
#99257=DIRECTION('',(0.,1.,0.));
#99258=DIRECTION('',(0.,1.,0.));
#99259=DIRECTION('center_axis',(0.,1.,0.));
#99260=DIRECTION('ref_axis',(1.,0.,0.));
#99261=DIRECTION('',(-0.190809912898503,0.,0.981627005099017));
#99262=DIRECTION('',(0.981627005099017,0.,0.190809912898503));
#99263=DIRECTION('',(-0.190809912898503,0.,0.981627005099017));
#99264=DIRECTION('',(0.981627005099017,0.,0.190809912898503));
#99265=DIRECTION('center_axis',(0.981627005099017,0.,0.190809912898503));
#99266=DIRECTION('ref_axis',(0.,-1.,0.));
#99267=DIRECTION('',(-0.190809912898503,0.,0.981627005099017));
#99268=DIRECTION('',(0.,-1.,0.));
#99269=DIRECTION('',(0.,-1.,0.));
#99270=DIRECTION('center_axis',(0.,-1.,0.));
#99271=DIRECTION('ref_axis',(0.,0.,-1.));
#99272=DIRECTION('',(-0.190809912898503,0.,0.981627005099017));
#99273=DIRECTION('',(-0.981627005099017,0.,-0.190809912898503));
#99274=DIRECTION('',(-0.981627005099017,0.,-0.190809912898503));
#99275=DIRECTION('center_axis',(-0.981627005099017,0.,-0.190809912898503));
#99276=DIRECTION('ref_axis',(-0.190809912898503,0.,0.981627005099017));
#99277=DIRECTION('',(0.,1.,0.));
#99278=DIRECTION('',(0.,1.,0.));
#99279=DIRECTION('center_axis',(0.,1.,0.));
#99280=DIRECTION('ref_axis',(1.,0.,0.));
#99281=DIRECTION('',(-0.190809912898503,0.,0.981627005099017));
#99282=DIRECTION('',(0.981627005099017,0.,0.190809912898503));
#99283=DIRECTION('',(-0.190809912898503,0.,0.981627005099017));
#99284=DIRECTION('',(0.981627005099017,0.,0.190809912898503));
#99285=DIRECTION('center_axis',(0.981627005099017,0.,0.190809912898503));
#99286=DIRECTION('ref_axis',(0.,-1.,0.));
#99287=DIRECTION('',(-0.190809912898503,0.,0.981627005099017));
#99288=DIRECTION('',(0.,-1.,0.));
#99289=DIRECTION('',(0.,-1.,0.));
#99290=DIRECTION('center_axis',(0.,-1.,0.));
#99291=DIRECTION('ref_axis',(0.,0.,-1.));
#99292=DIRECTION('',(-0.190809912898503,0.,0.981627005099017));
#99293=DIRECTION('',(-0.981627005099017,0.,-0.190809912898503));
#99294=DIRECTION('',(-0.981627005099017,0.,-0.190809912898503));
#99295=DIRECTION('center_axis',(-0.981627005099017,0.,-0.190809912898503));
#99296=DIRECTION('ref_axis',(-0.190809912898503,0.,0.981627005099017));
#99297=DIRECTION('',(0.,1.,0.));
#99298=DIRECTION('',(0.,1.,0.));
#99299=DIRECTION('center_axis',(0.,1.,0.));
#99300=DIRECTION('ref_axis',(1.,0.,0.));
#99301=DIRECTION('',(-0.190809912898503,0.,0.981627005099017));
#99302=DIRECTION('',(0.981627005099017,0.,0.190809912898503));
#99303=DIRECTION('',(-0.190809912898503,0.,0.981627005099017));
#99304=DIRECTION('',(0.981627005099017,0.,0.190809912898503));
#99305=DIRECTION('center_axis',(0.981627005099017,0.,0.190809912898503));
#99306=DIRECTION('ref_axis',(0.,-1.,0.));
#99307=DIRECTION('',(-0.190809912898503,0.,0.981627005099017));
#99308=DIRECTION('',(0.,-1.,0.));
#99309=DIRECTION('',(0.,-1.,0.));
#99310=DIRECTION('center_axis',(0.,-1.,0.));
#99311=DIRECTION('ref_axis',(0.,0.,-1.));
#99312=DIRECTION('',(-0.190809912898503,0.,0.981627005099017));
#99313=DIRECTION('',(-0.981627005099017,0.,-0.190809912898503));
#99314=DIRECTION('',(-0.981627005099017,0.,-0.190809912898503));
#99315=DIRECTION('center_axis',(-0.981627005099017,0.,-0.190809912898503));
#99316=DIRECTION('ref_axis',(-0.190809912898503,0.,0.981627005099017));
#99317=DIRECTION('',(0.,1.,0.));
#99318=DIRECTION('',(0.,1.,0.));
#99319=DIRECTION('center_axis',(0.,1.,0.));
#99320=DIRECTION('ref_axis',(1.,0.,0.));
#99321=DIRECTION('',(-0.190809912898503,0.,0.981627005099017));
#99322=DIRECTION('',(0.981627005099017,0.,0.190809912898503));
#99323=DIRECTION('',(-0.190809912898503,0.,0.981627005099017));
#99324=DIRECTION('',(0.981627005099017,0.,0.190809912898503));
#99325=DIRECTION('center_axis',(0.981627005099017,0.,0.190809912898503));
#99326=DIRECTION('ref_axis',(0.,-1.,0.));
#99327=DIRECTION('',(-0.190809912898503,0.,0.981627005099017));
#99328=DIRECTION('',(0.,-1.,0.));
#99329=DIRECTION('',(0.,-1.,0.));
#99330=DIRECTION('center_axis',(0.,-1.,0.));
#99331=DIRECTION('ref_axis',(0.,0.,-1.));
#99332=DIRECTION('',(-0.190809912898503,0.,0.981627005099017));
#99333=DIRECTION('',(-0.981627005099017,0.,-0.190809912898503));
#99334=DIRECTION('',(-0.981627005099017,0.,-0.190809912898503));
#99335=DIRECTION('center_axis',(-0.981627005099017,0.,-0.190809912898503));
#99336=DIRECTION('ref_axis',(-0.190809912898503,0.,0.981627005099017));
#99337=DIRECTION('',(0.,1.,0.));
#99338=DIRECTION('',(0.,1.,0.));
#99339=DIRECTION('center_axis',(0.,1.,0.));
#99340=DIRECTION('ref_axis',(1.,0.,0.));
#99341=DIRECTION('',(-0.190809912898503,0.,0.981627005099017));
#99342=DIRECTION('',(0.981627005099017,0.,0.190809912898503));
#99343=DIRECTION('',(-0.190809912898503,0.,0.981627005099017));
#99344=DIRECTION('',(0.981627005099017,0.,0.190809912898503));
#99345=DIRECTION('center_axis',(0.981627005099017,0.,0.190809912898503));
#99346=DIRECTION('ref_axis',(0.,-1.,0.));
#99347=DIRECTION('',(-0.190809912898503,0.,0.981627005099017));
#99348=DIRECTION('',(0.,-1.,0.));
#99349=DIRECTION('',(0.,-1.,0.));
#99350=DIRECTION('center_axis',(0.,-1.,0.));
#99351=DIRECTION('ref_axis',(0.,0.,-1.));
#99352=DIRECTION('',(-0.190809912898503,0.,0.981627005099017));
#99353=DIRECTION('',(-0.981627005099017,0.,-0.190809912898503));
#99354=DIRECTION('',(-0.981627005099017,0.,-0.190809912898503));
#99355=DIRECTION('center_axis',(-0.981627005099017,0.,-0.190809912898503));
#99356=DIRECTION('ref_axis',(-0.190809912898503,0.,0.981627005099017));
#99357=DIRECTION('',(0.,1.,0.));
#99358=DIRECTION('',(0.,1.,0.));
#99359=DIRECTION('center_axis',(0.,1.,0.));
#99360=DIRECTION('ref_axis',(1.,0.,0.));
#99361=DIRECTION('',(-0.190809912898503,0.,0.981627005099017));
#99362=DIRECTION('',(0.981627005099017,0.,0.190809912898503));
#99363=DIRECTION('',(-0.190809912898503,0.,0.981627005099017));
#99364=DIRECTION('',(0.981627005099017,0.,0.190809912898503));
#99365=DIRECTION('center_axis',(0.981627005099017,0.,0.190809912898503));
#99366=DIRECTION('ref_axis',(0.,-1.,0.));
#99367=DIRECTION('',(-0.190809912898503,0.,0.981627005099017));
#99368=DIRECTION('',(0.,-1.,0.));
#99369=DIRECTION('',(0.,-1.,0.));
#99370=DIRECTION('center_axis',(0.,-1.,0.));
#99371=DIRECTION('ref_axis',(0.,0.,-1.));
#99372=DIRECTION('',(-0.190809912898503,0.,0.981627005099017));
#99373=DIRECTION('',(-0.981627005099017,0.,-0.190809912898503));
#99374=DIRECTION('',(-0.981627005099017,0.,-0.190809912898503));
#99375=DIRECTION('center_axis',(-0.981627005099017,0.,-0.190809912898503));
#99376=DIRECTION('ref_axis',(-0.190809912898503,0.,0.981627005099017));
#99377=DIRECTION('',(0.,1.,0.));
#99378=DIRECTION('',(0.,1.,0.));
#99379=DIRECTION('center_axis',(0.,1.,0.));
#99380=DIRECTION('ref_axis',(1.,0.,0.));
#99381=DIRECTION('',(-0.190809912898503,0.,0.981627005099017));
#99382=DIRECTION('',(0.981627005099017,0.,0.190809912898503));
#99383=DIRECTION('',(-0.190809912898503,0.,0.981627005099017));
#99384=DIRECTION('',(0.981627005099017,0.,0.190809912898503));
#99385=DIRECTION('center_axis',(0.981627005099017,0.,0.190809912898503));
#99386=DIRECTION('ref_axis',(0.,-1.,0.));
#99387=DIRECTION('',(-0.190809912898503,0.,0.981627005099017));
#99388=DIRECTION('',(0.,-1.,0.));
#99389=DIRECTION('',(0.,-1.,0.));
#99390=DIRECTION('center_axis',(0.,-1.,0.));
#99391=DIRECTION('ref_axis',(0.,0.,-1.));
#99392=DIRECTION('',(-0.190809912898503,0.,0.981627005099017));
#99393=DIRECTION('',(-0.981627005099017,0.,-0.190809912898503));
#99394=DIRECTION('',(-0.981627005099017,0.,-0.190809912898503));
#99395=DIRECTION('center_axis',(-0.981627005099017,0.,-0.190809912898503));
#99396=DIRECTION('ref_axis',(-0.190809912898503,0.,0.981627005099017));
#99397=DIRECTION('',(0.,1.,0.));
#99398=DIRECTION('',(0.,1.,0.));
#99399=DIRECTION('center_axis',(0.,1.,0.));
#99400=DIRECTION('ref_axis',(1.,0.,0.));
#99401=DIRECTION('',(-0.190809912898503,0.,0.981627005099017));
#99402=DIRECTION('',(0.981627005099017,0.,0.190809912898503));
#99403=DIRECTION('',(-0.190809912898503,0.,0.981627005099017));
#99404=DIRECTION('',(0.981627005099017,0.,0.190809912898503));
#99405=DIRECTION('center_axis',(0.981627005099017,0.,0.190809912898503));
#99406=DIRECTION('ref_axis',(0.,-1.,0.));
#99407=DIRECTION('',(-0.190809912898503,0.,0.981627005099017));
#99408=DIRECTION('',(0.,-1.,0.));
#99409=DIRECTION('',(0.,-1.,0.));
#99410=DIRECTION('center_axis',(0.,-1.,0.));
#99411=DIRECTION('ref_axis',(0.,0.,-1.));
#99412=DIRECTION('',(-0.190809912898503,0.,0.981627005099017));
#99413=DIRECTION('',(-0.981627005099017,0.,-0.190809912898503));
#99414=DIRECTION('',(-0.981627005099017,0.,-0.190809912898503));
#99415=DIRECTION('center_axis',(-0.981627005099017,0.,-0.190809912898503));
#99416=DIRECTION('ref_axis',(-0.190809912898503,0.,0.981627005099017));
#99417=DIRECTION('',(0.,1.,0.));
#99418=DIRECTION('',(0.,1.,0.));
#99419=DIRECTION('center_axis',(0.,1.,0.));
#99420=DIRECTION('ref_axis',(1.,0.,0.));
#99421=DIRECTION('',(-0.190809912898503,0.,0.981627005099017));
#99422=DIRECTION('',(0.981627005099017,0.,0.190809912898503));
#99423=DIRECTION('',(-0.190809912898503,0.,0.981627005099017));
#99424=DIRECTION('',(0.981627005099017,0.,0.190809912898503));
#99425=DIRECTION('center_axis',(0.981627005099017,0.,0.190809912898503));
#99426=DIRECTION('ref_axis',(0.,-1.,0.));
#99427=DIRECTION('',(-0.190809912898503,0.,0.981627005099017));
#99428=DIRECTION('',(0.,-1.,0.));
#99429=DIRECTION('',(0.,-1.,0.));
#99430=DIRECTION('center_axis',(0.,-1.,0.));
#99431=DIRECTION('ref_axis',(0.,0.,-1.));
#99432=DIRECTION('',(-0.190809912898503,0.,0.981627005099017));
#99433=DIRECTION('',(-0.981627005099017,0.,-0.190809912898503));
#99434=DIRECTION('',(-0.981627005099017,0.,-0.190809912898503));
#99435=DIRECTION('center_axis',(-0.981627005099017,0.,-0.190809912898503));
#99436=DIRECTION('ref_axis',(-0.190809912898503,0.,0.981627005099017));
#99437=DIRECTION('',(0.,1.,0.));
#99438=DIRECTION('',(0.,1.,0.));
#99439=DIRECTION('center_axis',(0.,1.,0.));
#99440=DIRECTION('ref_axis',(1.,0.,0.));
#99441=DIRECTION('',(-0.190809912898503,0.,0.981627005099017));
#99442=DIRECTION('',(0.981627005099017,0.,0.190809912898503));
#99443=DIRECTION('',(-0.190809912898503,0.,0.981627005099017));
#99444=DIRECTION('',(0.981627005099017,0.,0.190809912898503));
#99445=DIRECTION('center_axis',(0.981627005099017,0.,0.190809912898503));
#99446=DIRECTION('ref_axis',(0.,-1.,0.));
#99447=DIRECTION('',(-0.190809912898503,0.,0.981627005099017));
#99448=DIRECTION('',(0.,-1.,0.));
#99449=DIRECTION('',(0.,-1.,0.));
#99450=DIRECTION('center_axis',(0.,-1.,0.));
#99451=DIRECTION('ref_axis',(0.,0.,-1.));
#99452=DIRECTION('',(-0.190809912898503,0.,0.981627005099017));
#99453=DIRECTION('',(-0.981627005099017,0.,-0.190809912898503));
#99454=DIRECTION('',(-0.981627005099017,0.,-0.190809912898503));
#99455=DIRECTION('center_axis',(-0.981627005099017,0.,-0.190809912898503));
#99456=DIRECTION('ref_axis',(-0.190809912898503,0.,0.981627005099017));
#99457=DIRECTION('',(0.,1.,0.));
#99458=DIRECTION('',(0.,1.,0.));
#99459=DIRECTION('center_axis',(0.,1.,0.));
#99460=DIRECTION('ref_axis',(1.,0.,0.));
#99461=DIRECTION('',(-0.190809912898503,0.,0.981627005099017));
#99462=DIRECTION('',(0.981627005099017,0.,0.190809912898503));
#99463=DIRECTION('',(-0.190809912898503,0.,0.981627005099017));
#99464=DIRECTION('',(0.981627005099017,0.,0.190809912898503));
#99465=DIRECTION('center_axis',(0.981627005099017,0.,0.190809912898503));
#99466=DIRECTION('ref_axis',(0.,-1.,0.));
#99467=DIRECTION('',(-0.190809912898503,0.,0.981627005099017));
#99468=DIRECTION('',(0.,-1.,0.));
#99469=DIRECTION('',(0.,-1.,0.));
#99470=DIRECTION('center_axis',(0.,-1.,0.));
#99471=DIRECTION('ref_axis',(0.,0.,-1.));
#99472=DIRECTION('',(-0.190809912898503,0.,0.981627005099017));
#99473=DIRECTION('',(-0.981627005099017,0.,-0.190809912898503));
#99474=DIRECTION('',(-0.981627005099017,0.,-0.190809912898503));
#99475=DIRECTION('center_axis',(-0.981627005099017,0.,-0.190809912898503));
#99476=DIRECTION('ref_axis',(-0.190809912898503,0.,0.981627005099017));
#99477=DIRECTION('',(0.,1.,0.));
#99478=DIRECTION('',(0.,1.,0.));
#99479=DIRECTION('center_axis',(0.,1.,0.));
#99480=DIRECTION('ref_axis',(1.,0.,0.));
#99481=DIRECTION('',(-0.190809912898503,0.,0.981627005099017));
#99482=DIRECTION('',(0.981627005099017,0.,0.190809912898503));
#99483=DIRECTION('',(-0.190809912898503,0.,0.981627005099017));
#99484=DIRECTION('',(0.981627005099017,0.,0.190809912898503));
#99485=DIRECTION('center_axis',(0.981627005099017,0.,0.190809912898503));
#99486=DIRECTION('ref_axis',(0.,-1.,0.));
#99487=DIRECTION('',(-0.190809912898503,0.,0.981627005099017));
#99488=DIRECTION('',(0.,-1.,0.));
#99489=DIRECTION('',(0.,-1.,0.));
#99490=DIRECTION('center_axis',(0.,-1.,0.));
#99491=DIRECTION('ref_axis',(0.,0.,-1.));
#99492=DIRECTION('',(-0.190809912898503,0.,0.981627005099017));
#99493=DIRECTION('',(-0.981627005099017,0.,-0.190809912898503));
#99494=DIRECTION('',(-0.981627005099017,0.,-0.190809912898503));
#99495=DIRECTION('center_axis',(-0.981627005099017,0.,-0.190809912898503));
#99496=DIRECTION('ref_axis',(-0.190809912898503,0.,0.981627005099017));
#99497=DIRECTION('',(0.,1.,0.));
#99498=DIRECTION('',(0.,1.,0.));
#99499=DIRECTION('center_axis',(0.,1.,0.));
#99500=DIRECTION('ref_axis',(1.,0.,0.));
#99501=DIRECTION('',(-0.190809912898503,0.,0.981627005099017));
#99502=DIRECTION('',(0.981627005099017,0.,0.190809912898503));
#99503=DIRECTION('',(-0.190809912898503,0.,0.981627005099017));
#99504=DIRECTION('',(0.981627005099017,0.,0.190809912898503));
#99505=DIRECTION('center_axis',(0.981627005099017,0.,0.190809912898503));
#99506=DIRECTION('ref_axis',(0.,-1.,0.));
#99507=DIRECTION('',(-0.190809912898503,0.,0.981627005099017));
#99508=DIRECTION('',(0.,-1.,0.));
#99509=DIRECTION('',(0.,-1.,0.));
#99510=DIRECTION('center_axis',(0.,-1.,0.));
#99511=DIRECTION('ref_axis',(0.,0.,-1.));
#99512=DIRECTION('',(-0.190809912898503,0.,0.981627005099017));
#99513=DIRECTION('',(-0.981627005099017,0.,-0.190809912898503));
#99514=DIRECTION('',(-0.981627005099017,0.,-0.190809912898503));
#99515=DIRECTION('center_axis',(-0.981627005099017,0.,-0.190809912898503));
#99516=DIRECTION('ref_axis',(-0.190809912898503,0.,0.981627005099017));
#99517=DIRECTION('',(0.,1.,0.));
#99518=DIRECTION('',(0.,1.,0.));
#99519=DIRECTION('center_axis',(0.,1.,0.));
#99520=DIRECTION('ref_axis',(1.,0.,0.));
#99521=DIRECTION('',(-0.190809912898503,0.,0.981627005099017));
#99522=DIRECTION('',(0.981627005099017,0.,0.190809912898503));
#99523=DIRECTION('',(-0.190809912898503,0.,0.981627005099017));
#99524=DIRECTION('',(0.981627005099017,0.,0.190809912898503));
#99525=DIRECTION('center_axis',(0.981627005099017,0.,0.190809912898503));
#99526=DIRECTION('ref_axis',(0.,-1.,0.));
#99527=DIRECTION('',(-0.190809912898503,0.,0.981627005099017));
#99528=DIRECTION('',(0.,-1.,0.));
#99529=DIRECTION('',(0.,-1.,0.));
#99530=DIRECTION('center_axis',(0.,-1.,0.));
#99531=DIRECTION('ref_axis',(0.,0.,-1.));
#99532=DIRECTION('',(-0.190809912898503,0.,0.981627005099017));
#99533=DIRECTION('',(-0.981627005099017,0.,-0.190809912898503));
#99534=DIRECTION('',(-0.981627005099017,0.,-0.190809912898503));
#99535=DIRECTION('center_axis',(-0.981627005099017,0.,-0.190809912898503));
#99536=DIRECTION('ref_axis',(-0.190809912898503,0.,0.981627005099017));
#99537=DIRECTION('',(0.,1.,0.));
#99538=DIRECTION('',(0.,1.,0.));
#99539=DIRECTION('center_axis',(0.,1.,0.));
#99540=DIRECTION('ref_axis',(1.,0.,0.));
#99541=DIRECTION('',(-0.190809912898503,0.,0.981627005099017));
#99542=DIRECTION('',(0.981627005099017,0.,0.190809912898503));
#99543=DIRECTION('',(-0.190809912898503,0.,0.981627005099017));
#99544=DIRECTION('',(0.981627005099017,0.,0.190809912898503));
#99545=DIRECTION('center_axis',(0.981627005099017,0.,0.190809912898503));
#99546=DIRECTION('ref_axis',(0.,-1.,0.));
#99547=DIRECTION('',(-0.190809912898503,0.,0.981627005099017));
#99548=DIRECTION('',(0.,-1.,0.));
#99549=DIRECTION('',(0.,-1.,0.));
#99550=DIRECTION('center_axis',(0.,-1.,0.));
#99551=DIRECTION('ref_axis',(0.,0.,-1.));
#99552=DIRECTION('',(-0.190809912898503,0.,0.981627005099017));
#99553=DIRECTION('',(-0.981627005099017,0.,-0.190809912898503));
#99554=DIRECTION('',(-0.981627005099017,0.,-0.190809912898503));
#99555=DIRECTION('center_axis',(-0.981627005099017,0.,-0.190809912898503));
#99556=DIRECTION('ref_axis',(-0.190809912898503,0.,0.981627005099017));
#99557=DIRECTION('',(0.,1.,0.));
#99558=DIRECTION('',(0.,1.,0.));
#99559=DIRECTION('center_axis',(0.,1.,0.));
#99560=DIRECTION('ref_axis',(1.,0.,0.));
#99561=DIRECTION('',(-0.190809912898503,0.,0.981627005099017));
#99562=DIRECTION('',(0.981627005099017,0.,0.190809912898503));
#99563=DIRECTION('',(-0.190809912898503,0.,0.981627005099017));
#99564=DIRECTION('',(0.981627005099017,0.,0.190809912898503));
#99565=DIRECTION('center_axis',(0.981627005099017,0.,0.190809912898503));
#99566=DIRECTION('ref_axis',(0.,-1.,0.));
#99567=DIRECTION('',(-0.190809912898503,0.,0.981627005099017));
#99568=DIRECTION('',(0.,-1.,0.));
#99569=DIRECTION('',(0.,-1.,0.));
#99570=DIRECTION('center_axis',(0.,-1.,0.));
#99571=DIRECTION('ref_axis',(0.,0.,-1.));
#99572=DIRECTION('',(-0.190809912898503,0.,0.981627005099017));
#99573=DIRECTION('',(-0.981627005099017,0.,-0.190809912898503));
#99574=DIRECTION('',(-0.981627005099017,0.,-0.190809912898503));
#99575=DIRECTION('center_axis',(-0.981627005099017,0.,-0.190809912898503));
#99576=DIRECTION('ref_axis',(-0.190809912898503,0.,0.981627005099017));
#99577=DIRECTION('',(0.,1.,0.));
#99578=DIRECTION('',(0.,1.,0.));
#99579=DIRECTION('center_axis',(0.,1.,0.));
#99580=DIRECTION('ref_axis',(1.,0.,0.));
#99581=DIRECTION('',(-0.190809912898503,0.,0.981627005099017));
#99582=DIRECTION('',(0.981627005099017,0.,0.190809912898503));
#99583=DIRECTION('',(-0.190809912898503,0.,0.981627005099017));
#99584=DIRECTION('',(0.981627005099017,0.,0.190809912898503));
#99585=DIRECTION('center_axis',(0.981627005099017,0.,0.190809912898503));
#99586=DIRECTION('ref_axis',(0.,-1.,0.));
#99587=DIRECTION('',(-0.190809912898503,0.,0.981627005099017));
#99588=DIRECTION('',(0.,-1.,0.));
#99589=DIRECTION('',(0.,-1.,0.));
#99590=DIRECTION('center_axis',(0.,-1.,0.));
#99591=DIRECTION('ref_axis',(0.,0.,-1.));
#99592=DIRECTION('',(-0.190809912898503,0.,0.981627005099017));
#99593=DIRECTION('',(-0.981627005099017,0.,-0.190809912898503));
#99594=DIRECTION('',(-0.981627005099017,0.,-0.190809912898503));
#99595=DIRECTION('center_axis',(-0.981627005099017,0.,-0.190809912898503));
#99596=DIRECTION('ref_axis',(-0.190809912898503,0.,0.981627005099017));
#99597=DIRECTION('',(0.,1.,0.));
#99598=DIRECTION('',(0.,1.,0.));
#99599=DIRECTION('center_axis',(0.,1.,0.));
#99600=DIRECTION('ref_axis',(1.,0.,0.));
#99601=DIRECTION('',(-0.190809912898503,0.,0.981627005099017));
#99602=DIRECTION('',(0.981627005099017,0.,0.190809912898503));
#99603=DIRECTION('',(-0.190809912898503,0.,0.981627005099017));
#99604=DIRECTION('',(0.981627005099017,0.,0.190809912898503));
#99605=DIRECTION('center_axis',(0.981627005099017,0.,0.190809912898503));
#99606=DIRECTION('ref_axis',(0.,-1.,0.));
#99607=DIRECTION('',(-0.190809912898503,0.,0.981627005099017));
#99608=DIRECTION('',(0.,-1.,0.));
#99609=DIRECTION('',(0.,-1.,0.));
#99610=DIRECTION('center_axis',(0.,-1.,0.));
#99611=DIRECTION('ref_axis',(0.,0.,-1.));
#99612=DIRECTION('',(-0.190809912898503,0.,0.981627005099017));
#99613=DIRECTION('',(-0.981627005099017,0.,-0.190809912898503));
#99614=DIRECTION('',(-0.981627005099017,0.,-0.190809912898503));
#99615=DIRECTION('center_axis',(-0.981627005099017,0.,-0.190809912898503));
#99616=DIRECTION('ref_axis',(-0.190809912898503,0.,0.981627005099017));
#99617=DIRECTION('',(0.,1.,0.));
#99618=DIRECTION('',(0.,1.,0.));
#99619=DIRECTION('center_axis',(0.,1.,0.));
#99620=DIRECTION('ref_axis',(1.,0.,0.));
#99621=DIRECTION('',(-0.190809912898503,0.,0.981627005099017));
#99622=DIRECTION('',(0.981627005099017,0.,0.190809912898503));
#99623=DIRECTION('',(-0.190809912898503,0.,0.981627005099017));
#99624=DIRECTION('',(0.981627005099017,0.,0.190809912898503));
#99625=DIRECTION('center_axis',(0.981627005099017,0.,0.190809912898503));
#99626=DIRECTION('ref_axis',(0.,-1.,0.));
#99627=DIRECTION('',(-0.190809912898503,0.,0.981627005099017));
#99628=DIRECTION('',(0.,-1.,0.));
#99629=DIRECTION('',(0.,-1.,0.));
#99630=DIRECTION('center_axis',(0.,-1.,0.));
#99631=DIRECTION('ref_axis',(0.,0.,-1.));
#99632=DIRECTION('',(-0.190809912898503,0.,0.981627005099017));
#99633=DIRECTION('',(-0.981627005099017,0.,-0.190809912898503));
#99634=DIRECTION('',(-0.981627005099017,0.,-0.190809912898503));
#99635=DIRECTION('center_axis',(-0.981627005099017,0.,-0.190809912898503));
#99636=DIRECTION('ref_axis',(-0.190809912898503,0.,0.981627005099017));
#99637=DIRECTION('',(0.,1.,0.));
#99638=DIRECTION('',(0.,1.,0.));
#99639=DIRECTION('center_axis',(0.,1.,0.));
#99640=DIRECTION('ref_axis',(1.,0.,0.));
#99641=DIRECTION('',(-0.190809912898503,0.,0.981627005099017));
#99642=DIRECTION('',(0.981627005099017,0.,0.190809912898503));
#99643=DIRECTION('',(-0.190809912898503,0.,0.981627005099017));
#99644=DIRECTION('',(0.981627005099017,0.,0.190809912898503));
#99645=DIRECTION('center_axis',(0.981627005099017,0.,0.190809912898503));
#99646=DIRECTION('ref_axis',(0.,-1.,0.));
#99647=DIRECTION('',(-0.190809912898503,0.,0.981627005099017));
#99648=DIRECTION('',(0.,-1.,0.));
#99649=DIRECTION('',(0.,-1.,0.));
#99650=DIRECTION('center_axis',(0.,-1.,0.));
#99651=DIRECTION('ref_axis',(0.,0.,-1.));
#99652=DIRECTION('',(-0.190809912898503,0.,0.981627005099017));
#99653=DIRECTION('',(-0.981627005099017,0.,-0.190809912898503));
#99654=DIRECTION('',(-0.981627005099017,0.,-0.190809912898503));
#99655=DIRECTION('center_axis',(-0.981627005099017,0.,-0.190809912898503));
#99656=DIRECTION('ref_axis',(-0.190809912898503,0.,0.981627005099017));
#99657=DIRECTION('',(0.,1.,0.));
#99658=DIRECTION('',(0.,1.,0.));
#99659=DIRECTION('center_axis',(0.,1.,0.));
#99660=DIRECTION('ref_axis',(1.,0.,0.));
#99661=DIRECTION('',(-0.190809912898503,0.,0.981627005099017));
#99662=DIRECTION('',(0.981627005099017,0.,0.190809912898503));
#99663=DIRECTION('',(-0.190809912898503,0.,0.981627005099017));
#99664=DIRECTION('',(0.981627005099017,0.,0.190809912898503));
#99665=DIRECTION('center_axis',(0.981627005099017,0.,0.190809912898503));
#99666=DIRECTION('ref_axis',(0.,-1.,0.));
#99667=DIRECTION('',(-0.190809912898503,0.,0.981627005099017));
#99668=DIRECTION('',(0.,-1.,0.));
#99669=DIRECTION('',(0.,-1.,0.));
#99670=DIRECTION('center_axis',(0.,-1.,0.));
#99671=DIRECTION('ref_axis',(0.,0.,-1.));
#99672=DIRECTION('',(-0.190809912898503,0.,0.981627005099017));
#99673=DIRECTION('',(-0.981627005099017,0.,-0.190809912898503));
#99674=DIRECTION('',(-0.981627005099017,0.,-0.190809912898503));
#99675=DIRECTION('center_axis',(-0.981627005099017,0.,-0.190809912898503));
#99676=DIRECTION('ref_axis',(-0.190809912898503,0.,0.981627005099017));
#99677=DIRECTION('',(0.,1.,0.));
#99678=DIRECTION('',(0.,1.,0.));
#99679=DIRECTION('center_axis',(0.,1.,0.));
#99680=DIRECTION('ref_axis',(1.,0.,0.));
#99681=DIRECTION('',(-0.190809912898503,0.,0.981627005099017));
#99682=DIRECTION('',(0.981627005099017,0.,0.190809912898503));
#99683=DIRECTION('',(-0.190809912898503,0.,0.981627005099017));
#99684=DIRECTION('',(0.981627005099017,0.,0.190809912898503));
#99685=DIRECTION('center_axis',(0.981627005099017,0.,0.190809912898503));
#99686=DIRECTION('ref_axis',(0.,-1.,0.));
#99687=DIRECTION('',(-0.190809912898503,0.,0.981627005099017));
#99688=DIRECTION('',(0.,-1.,0.));
#99689=DIRECTION('',(0.,-1.,0.));
#99690=DIRECTION('center_axis',(0.,-1.,0.));
#99691=DIRECTION('ref_axis',(0.,0.,-1.));
#99692=DIRECTION('',(-0.190809912898503,0.,0.981627005099017));
#99693=DIRECTION('',(-0.981627005099017,0.,-0.190809912898503));
#99694=DIRECTION('',(-0.981627005099017,0.,-0.190809912898503));
#99695=DIRECTION('center_axis',(-0.981627005099017,0.,-0.190809912898503));
#99696=DIRECTION('ref_axis',(-0.190809912898503,0.,0.981627005099017));
#99697=DIRECTION('',(0.,1.,0.));
#99698=DIRECTION('',(0.,1.,0.));
#99699=DIRECTION('center_axis',(0.,1.,0.));
#99700=DIRECTION('ref_axis',(1.,0.,0.));
#99701=DIRECTION('',(-0.190809912898503,0.,0.981627005099017));
#99702=DIRECTION('',(0.981627005099017,0.,0.190809912898503));
#99703=DIRECTION('',(-0.190809912898503,0.,0.981627005099017));
#99704=DIRECTION('',(0.981627005099017,0.,0.190809912898503));
#99705=DIRECTION('center_axis',(0.981627005099017,0.,0.190809912898503));
#99706=DIRECTION('ref_axis',(0.,-1.,0.));
#99707=DIRECTION('',(-0.190809912898503,0.,0.981627005099017));
#99708=DIRECTION('',(0.,-1.,0.));
#99709=DIRECTION('',(0.,-1.,0.));
#99710=DIRECTION('center_axis',(0.,-1.,0.));
#99711=DIRECTION('ref_axis',(0.,0.,-1.));
#99712=DIRECTION('',(-0.190809912898503,0.,0.981627005099017));
#99713=DIRECTION('',(-0.981627005099017,0.,-0.190809912898503));
#99714=DIRECTION('',(-0.981627005099017,0.,-0.190809912898503));
#99715=DIRECTION('center_axis',(-0.981627005099017,0.,-0.190809912898503));
#99716=DIRECTION('ref_axis',(-0.190809912898503,0.,0.981627005099017));
#99717=DIRECTION('',(0.,1.,0.));
#99718=DIRECTION('',(0.,1.,0.));
#99719=DIRECTION('center_axis',(0.,1.,0.));
#99720=DIRECTION('ref_axis',(1.,0.,0.));
#99721=DIRECTION('',(-0.190809912898503,0.,0.981627005099017));
#99722=DIRECTION('',(0.981627005099017,0.,0.190809912898503));
#99723=DIRECTION('',(-0.190809912898503,0.,0.981627005099017));
#99724=DIRECTION('',(0.981627005099017,0.,0.190809912898503));
#99725=DIRECTION('center_axis',(0.981627005099017,0.,0.190809912898503));
#99726=DIRECTION('ref_axis',(0.,-1.,0.));
#99727=DIRECTION('',(-0.190809912898503,0.,0.981627005099017));
#99728=DIRECTION('',(0.,-1.,0.));
#99729=DIRECTION('',(0.,-1.,0.));
#99730=DIRECTION('center_axis',(0.,-1.,0.));
#99731=DIRECTION('ref_axis',(0.,0.,-1.));
#99732=DIRECTION('',(-0.190809912898503,0.,0.981627005099017));
#99733=DIRECTION('',(-0.981627005099017,0.,-0.190809912898503));
#99734=DIRECTION('',(-0.981627005099017,0.,-0.190809912898503));
#99735=DIRECTION('center_axis',(-0.981627005099017,0.,-0.190809912898503));
#99736=DIRECTION('ref_axis',(-0.190809912898503,0.,0.981627005099017));
#99737=DIRECTION('',(0.,1.,0.));
#99738=DIRECTION('',(0.,1.,0.));
#99739=DIRECTION('center_axis',(0.,1.,0.));
#99740=DIRECTION('ref_axis',(1.,0.,0.));
#99741=DIRECTION('',(-0.190809912898503,0.,0.981627005099017));
#99742=DIRECTION('',(0.981627005099017,0.,0.190809912898503));
#99743=DIRECTION('',(-0.190809912898503,0.,0.981627005099017));
#99744=DIRECTION('',(0.981627005099017,0.,0.190809912898503));
#99745=DIRECTION('center_axis',(0.981627005099017,0.,0.190809912898503));
#99746=DIRECTION('ref_axis',(0.,-1.,0.));
#99747=DIRECTION('',(-0.190809912898503,0.,0.981627005099017));
#99748=DIRECTION('',(0.,-1.,0.));
#99749=DIRECTION('',(0.,-1.,0.));
#99750=DIRECTION('center_axis',(0.,-1.,0.));
#99751=DIRECTION('ref_axis',(0.,0.,-1.));
#99752=DIRECTION('',(-0.190809912898503,0.,0.981627005099017));
#99753=DIRECTION('',(-0.981627005099017,0.,-0.190809912898503));
#99754=DIRECTION('',(-0.981627005099017,0.,-0.190809912898503));
#99755=DIRECTION('center_axis',(-0.981627005099017,0.,-0.190809912898503));
#99756=DIRECTION('ref_axis',(-0.190809912898503,0.,0.981627005099017));
#99757=DIRECTION('',(0.,1.,0.));
#99758=DIRECTION('',(0.,1.,0.));
#99759=DIRECTION('center_axis',(0.,1.,0.));
#99760=DIRECTION('ref_axis',(1.,0.,0.));
#99761=DIRECTION('',(-0.190809912898503,0.,0.981627005099017));
#99762=DIRECTION('',(0.981627005099017,0.,0.190809912898503));
#99763=DIRECTION('',(-0.190809912898503,0.,0.981627005099017));
#99764=DIRECTION('',(0.981627005099017,0.,0.190809912898503));
#99765=DIRECTION('center_axis',(0.981627005099017,0.,0.190809912898503));
#99766=DIRECTION('ref_axis',(0.,-1.,0.));
#99767=DIRECTION('',(-0.190809912898503,0.,0.981627005099017));
#99768=DIRECTION('',(0.,-1.,0.));
#99769=DIRECTION('',(0.,-1.,0.));
#99770=DIRECTION('center_axis',(0.,-1.,0.));
#99771=DIRECTION('ref_axis',(0.,0.,-1.));
#99772=DIRECTION('',(-0.190809912898503,0.,0.981627005099017));
#99773=DIRECTION('',(-0.981627005099017,0.,-0.190809912898503));
#99774=DIRECTION('',(-0.981627005099017,0.,-0.190809912898503));
#99775=DIRECTION('center_axis',(-0.981627005099017,0.,-0.190809912898503));
#99776=DIRECTION('ref_axis',(-0.190809912898503,0.,0.981627005099017));
#99777=DIRECTION('',(0.,1.,0.));
#99778=DIRECTION('',(0.,1.,0.));
#99779=DIRECTION('center_axis',(0.,1.,0.));
#99780=DIRECTION('ref_axis',(1.,0.,0.));
#99781=DIRECTION('',(-0.190809912898503,0.,0.981627005099017));
#99782=DIRECTION('',(0.981627005099017,0.,0.190809912898503));
#99783=DIRECTION('',(-0.190809912898503,0.,0.981627005099017));
#99784=DIRECTION('',(0.981627005099017,0.,0.190809912898503));
#99785=DIRECTION('center_axis',(0.981627005099017,0.,0.190809912898503));
#99786=DIRECTION('ref_axis',(0.,-1.,0.));
#99787=DIRECTION('',(-0.190809912898503,0.,0.981627005099017));
#99788=DIRECTION('',(0.,-1.,0.));
#99789=DIRECTION('',(0.,-1.,0.));
#99790=DIRECTION('center_axis',(0.,-1.,0.));
#99791=DIRECTION('ref_axis',(0.,0.,-1.));
#99792=DIRECTION('',(-0.190809912898503,0.,0.981627005099017));
#99793=DIRECTION('',(-0.981627005099017,0.,-0.190809912898503));
#99794=DIRECTION('',(-0.981627005099017,0.,-0.190809912898503));
#99795=DIRECTION('center_axis',(-0.981627005099017,0.,-0.190809912898503));
#99796=DIRECTION('ref_axis',(-0.190809912898503,0.,0.981627005099017));
#99797=DIRECTION('',(0.,1.,0.));
#99798=DIRECTION('',(0.,1.,0.));
#99799=DIRECTION('center_axis',(0.,1.,0.));
#99800=DIRECTION('ref_axis',(1.,0.,0.));
#99801=DIRECTION('',(-0.190809912898503,0.,0.981627005099017));
#99802=DIRECTION('',(0.981627005099017,0.,0.190809912898503));
#99803=DIRECTION('',(-0.190809912898503,0.,0.981627005099017));
#99804=DIRECTION('',(0.981627005099017,0.,0.190809912898503));
#99805=DIRECTION('center_axis',(0.981627005099017,0.,0.190809912898503));
#99806=DIRECTION('ref_axis',(0.,-1.,0.));
#99807=DIRECTION('',(-0.190809912898503,0.,0.981627005099017));
#99808=DIRECTION('',(0.,-1.,0.));
#99809=DIRECTION('',(0.,-1.,0.));
#99810=DIRECTION('center_axis',(0.,-1.,0.));
#99811=DIRECTION('ref_axis',(0.,0.,-1.));
#99812=DIRECTION('',(-0.190809912898503,0.,0.981627005099017));
#99813=DIRECTION('',(-0.981627005099017,0.,-0.190809912898503));
#99814=DIRECTION('',(-0.981627005099017,0.,-0.190809912898503));
#99815=DIRECTION('center_axis',(-0.981627005099017,0.,-0.190809912898503));
#99816=DIRECTION('ref_axis',(-0.190809912898503,0.,0.981627005099017));
#99817=DIRECTION('',(0.,1.,0.));
#99818=DIRECTION('',(0.,1.,0.));
#99819=DIRECTION('center_axis',(0.,1.,0.));
#99820=DIRECTION('ref_axis',(1.,0.,0.));
#99821=DIRECTION('',(-0.190809912898503,0.,0.981627005099017));
#99822=DIRECTION('',(0.981627005099017,0.,0.190809912898503));
#99823=DIRECTION('',(-0.190809912898503,0.,0.981627005099017));
#99824=DIRECTION('',(0.981627005099017,0.,0.190809912898503));
#99825=DIRECTION('center_axis',(0.981627005099017,0.,0.190809912898503));
#99826=DIRECTION('ref_axis',(0.,-1.,0.));
#99827=DIRECTION('',(-0.190809912898503,0.,0.981627005099017));
#99828=DIRECTION('',(0.,-1.,0.));
#99829=DIRECTION('',(0.,-1.,0.));
#99830=DIRECTION('center_axis',(0.,-1.,0.));
#99831=DIRECTION('ref_axis',(0.,0.,-1.));
#99832=DIRECTION('',(-0.190809912898503,0.,0.981627005099017));
#99833=DIRECTION('',(-0.981627005099017,0.,-0.190809912898503));
#99834=DIRECTION('',(-0.981627005099017,0.,-0.190809912898503));
#99835=DIRECTION('center_axis',(-0.981627005099017,0.,-0.190809912898503));
#99836=DIRECTION('ref_axis',(-0.190809912898503,0.,0.981627005099017));
#99837=DIRECTION('',(0.,1.,0.));
#99838=DIRECTION('',(0.,1.,0.));
#99839=DIRECTION('center_axis',(0.,1.,0.));
#99840=DIRECTION('ref_axis',(1.,0.,0.));
#99841=DIRECTION('',(-0.190809912898503,0.,0.981627005099017));
#99842=DIRECTION('',(0.981627005099017,0.,0.190809912898503));
#99843=DIRECTION('',(-0.190809912898503,0.,0.981627005099017));
#99844=DIRECTION('',(0.981627005099017,0.,0.190809912898503));
#99845=DIRECTION('center_axis',(0.981627005099017,0.,0.190809912898503));
#99846=DIRECTION('ref_axis',(0.,-1.,0.));
#99847=DIRECTION('',(-0.190809912898503,0.,0.981627005099017));
#99848=DIRECTION('',(0.,-1.,0.));
#99849=DIRECTION('',(0.,-1.,0.));
#99850=DIRECTION('center_axis',(0.,-1.,0.));
#99851=DIRECTION('ref_axis',(0.,0.,-1.));
#99852=DIRECTION('',(-0.190809912898503,0.,0.981627005099017));
#99853=DIRECTION('',(-0.981627005099017,0.,-0.190809912898503));
#99854=DIRECTION('',(-0.981627005099017,0.,-0.190809912898503));
#99855=DIRECTION('center_axis',(-0.981627005099017,0.,-0.190809912898503));
#99856=DIRECTION('ref_axis',(-0.190809912898503,0.,0.981627005099017));
#99857=DIRECTION('',(0.,1.,0.));
#99858=DIRECTION('',(0.,1.,0.));
#99859=DIRECTION('center_axis',(0.,1.,0.));
#99860=DIRECTION('ref_axis',(1.,0.,0.));
#99861=DIRECTION('',(-0.190809912898503,0.,0.981627005099017));
#99862=DIRECTION('',(0.981627005099017,0.,0.190809912898503));
#99863=DIRECTION('',(-0.190809912898503,0.,0.981627005099017));
#99864=DIRECTION('',(0.981627005099017,0.,0.190809912898503));
#99865=DIRECTION('center_axis',(0.981627005099017,0.,0.190809912898503));
#99866=DIRECTION('ref_axis',(0.,-1.,0.));
#99867=DIRECTION('',(-0.190809912898503,0.,0.981627005099017));
#99868=DIRECTION('',(0.,-1.,0.));
#99869=DIRECTION('',(0.,-1.,0.));
#99870=DIRECTION('center_axis',(0.,-1.,0.));
#99871=DIRECTION('ref_axis',(0.,0.,-1.));
#99872=DIRECTION('',(-0.190809912898503,0.,0.981627005099017));
#99873=DIRECTION('',(-0.981627005099017,0.,-0.190809912898503));
#99874=DIRECTION('',(-0.981627005099017,0.,-0.190809912898503));
#99875=DIRECTION('center_axis',(-0.981627005099017,0.,-0.190809912898503));
#99876=DIRECTION('ref_axis',(-0.190809912898503,0.,0.981627005099017));
#99877=DIRECTION('',(0.,1.,0.));
#99878=DIRECTION('',(0.,1.,0.));
#99879=DIRECTION('center_axis',(0.,1.,0.));
#99880=DIRECTION('ref_axis',(1.,0.,0.));
#99881=DIRECTION('',(-0.190809912898503,0.,0.981627005099017));
#99882=DIRECTION('',(0.981627005099017,0.,0.190809912898503));
#99883=DIRECTION('',(-0.190809912898503,0.,0.981627005099017));
#99884=DIRECTION('',(0.981627005099017,0.,0.190809912898503));
#99885=DIRECTION('center_axis',(0.981627005099017,0.,0.190809912898503));
#99886=DIRECTION('ref_axis',(0.,-1.,0.));
#99887=DIRECTION('',(-0.190809912898503,0.,0.981627005099017));
#99888=DIRECTION('',(0.,-1.,0.));
#99889=DIRECTION('',(0.,-1.,0.));
#99890=DIRECTION('center_axis',(0.,-1.,0.));
#99891=DIRECTION('ref_axis',(0.,0.,-1.));
#99892=DIRECTION('',(-0.190809912898503,0.,0.981627005099017));
#99893=DIRECTION('',(-0.981627005099017,0.,-0.190809912898503));
#99894=DIRECTION('',(-0.981627005099017,0.,-0.190809912898503));
#99895=DIRECTION('center_axis',(-0.981627005099017,0.,-0.190809912898503));
#99896=DIRECTION('ref_axis',(-0.190809912898503,0.,0.981627005099017));
#99897=DIRECTION('',(0.,1.,0.));
#99898=DIRECTION('',(0.,1.,0.));
#99899=DIRECTION('center_axis',(0.,1.,0.));
#99900=DIRECTION('ref_axis',(1.,0.,0.));
#99901=DIRECTION('',(-0.190809912898503,0.,0.981627005099017));
#99902=DIRECTION('',(0.981627005099017,0.,0.190809912898503));
#99903=DIRECTION('',(-0.190809912898503,0.,0.981627005099017));
#99904=DIRECTION('',(0.981627005099017,0.,0.190809912898503));
#99905=DIRECTION('center_axis',(0.981627005099017,0.,0.190809912898503));
#99906=DIRECTION('ref_axis',(0.,-1.,0.));
#99907=DIRECTION('',(-0.190809912898503,0.,0.981627005099017));
#99908=DIRECTION('',(0.,-1.,0.));
#99909=DIRECTION('',(0.,-1.,0.));
#99910=DIRECTION('center_axis',(0.,-1.,0.));
#99911=DIRECTION('ref_axis',(0.,0.,-1.));
#99912=DIRECTION('',(-0.190809912898503,0.,0.981627005099017));
#99913=DIRECTION('',(-0.981627005099017,0.,-0.190809912898503));
#99914=DIRECTION('',(-0.981627005099017,0.,-0.190809912898503));
#99915=DIRECTION('center_axis',(-0.981627005099017,0.,-0.190809912898503));
#99916=DIRECTION('ref_axis',(-0.190809912898503,0.,0.981627005099017));
#99917=DIRECTION('',(0.,1.,0.));
#99918=DIRECTION('',(0.,1.,0.));
#99919=DIRECTION('center_axis',(0.,1.,0.));
#99920=DIRECTION('ref_axis',(1.,0.,0.));
#99921=DIRECTION('',(-0.190809912898503,0.,0.981627005099017));
#99922=DIRECTION('',(0.981627005099017,0.,0.190809912898503));
#99923=DIRECTION('',(-0.190809912898503,0.,0.981627005099017));
#99924=DIRECTION('',(0.981627005099017,0.,0.190809912898503));
#99925=DIRECTION('center_axis',(0.981627005099017,0.,0.190809912898503));
#99926=DIRECTION('ref_axis',(0.,-1.,0.));
#99927=DIRECTION('',(-0.190809912898503,0.,0.981627005099017));
#99928=DIRECTION('',(0.,-1.,0.));
#99929=DIRECTION('',(0.,-1.,0.));
#99930=DIRECTION('center_axis',(0.,-1.,0.));
#99931=DIRECTION('ref_axis',(0.,0.,-1.));
#99932=DIRECTION('',(-0.190809912898503,0.,0.981627005099017));
#99933=DIRECTION('',(-0.981627005099017,0.,-0.190809912898503));
#99934=DIRECTION('',(-0.981627005099017,0.,-0.190809912898503));
#99935=DIRECTION('center_axis',(-0.981627005099017,0.,-0.190809912898503));
#99936=DIRECTION('ref_axis',(-0.190809912898503,0.,0.981627005099017));
#99937=DIRECTION('',(0.,1.,0.));
#99938=DIRECTION('',(0.,1.,0.));
#99939=DIRECTION('center_axis',(0.,1.,0.));
#99940=DIRECTION('ref_axis',(1.,0.,0.));
#99941=DIRECTION('',(-0.190809912898503,0.,0.981627005099017));
#99942=DIRECTION('',(0.981627005099017,0.,0.190809912898503));
#99943=DIRECTION('',(-0.190809912898503,0.,0.981627005099017));
#99944=DIRECTION('',(0.981627005099017,0.,0.190809912898503));
#99945=DIRECTION('center_axis',(0.981627005099017,0.,0.190809912898503));
#99946=DIRECTION('ref_axis',(0.,-1.,0.));
#99947=DIRECTION('',(-0.190809912898503,0.,0.981627005099017));
#99948=DIRECTION('',(0.,-1.,0.));
#99949=DIRECTION('',(0.,-1.,0.));
#99950=DIRECTION('center_axis',(0.,-1.,0.));
#99951=DIRECTION('ref_axis',(0.,0.,-1.));
#99952=DIRECTION('',(-0.190809912898503,0.,0.981627005099017));
#99953=DIRECTION('',(-0.981627005099017,0.,-0.190809912898503));
#99954=DIRECTION('',(-0.981627005099017,0.,-0.190809912898503));
#99955=DIRECTION('center_axis',(-0.981627005099017,0.,-0.190809912898503));
#99956=DIRECTION('ref_axis',(-0.190809912898503,0.,0.981627005099017));
#99957=DIRECTION('',(0.,1.,0.));
#99958=DIRECTION('',(0.,1.,0.));
#99959=DIRECTION('center_axis',(0.,1.,0.));
#99960=DIRECTION('ref_axis',(1.,0.,0.));
#99961=DIRECTION('',(-0.190809912898503,0.,0.981627005099017));
#99962=DIRECTION('',(0.981627005099017,0.,0.190809912898503));
#99963=DIRECTION('',(-0.190809912898503,0.,0.981627005099017));
#99964=DIRECTION('',(0.981627005099017,0.,0.190809912898503));
#99965=DIRECTION('center_axis',(0.981627005099017,0.,0.190809912898503));
#99966=DIRECTION('ref_axis',(0.,-1.,0.));
#99967=DIRECTION('',(-0.190809912898503,0.,0.981627005099017));
#99968=DIRECTION('',(0.,-1.,0.));
#99969=DIRECTION('',(0.,-1.,0.));
#99970=DIRECTION('center_axis',(0.,-1.,0.));
#99971=DIRECTION('ref_axis',(0.,0.,-1.));
#99972=DIRECTION('',(-0.190809912898503,0.,0.981627005099017));
#99973=DIRECTION('',(-0.981627005099017,0.,-0.190809912898503));
#99974=DIRECTION('',(-0.981627005099017,0.,-0.190809912898503));
#99975=DIRECTION('center_axis',(-0.981627005099017,0.,-0.190809912898503));
#99976=DIRECTION('ref_axis',(-0.190809912898503,0.,0.981627005099017));
#99977=DIRECTION('',(0.,1.,0.));
#99978=DIRECTION('',(0.,1.,0.));
#99979=DIRECTION('center_axis',(0.,1.,0.));
#99980=DIRECTION('ref_axis',(1.,0.,0.));
#99981=DIRECTION('',(-0.190809912898503,0.,0.981627005099017));
#99982=DIRECTION('',(0.981627005099017,0.,0.190809912898503));
#99983=DIRECTION('',(-0.190809912898503,0.,0.981627005099017));
#99984=DIRECTION('',(0.981627005099017,0.,0.190809912898503));
#99985=DIRECTION('center_axis',(0.981627005099017,0.,0.190809912898503));
#99986=DIRECTION('ref_axis',(0.,-1.,0.));
#99987=DIRECTION('',(-0.190809912898503,0.,0.981627005099017));
#99988=DIRECTION('',(0.,-1.,0.));
#99989=DIRECTION('',(0.,-1.,0.));
#99990=DIRECTION('center_axis',(0.,-1.,0.));
#99991=DIRECTION('ref_axis',(0.,0.,-1.));
#99992=DIRECTION('',(-0.190809912898503,0.,0.981627005099017));
#99993=DIRECTION('',(-0.981627005099017,0.,-0.190809912898503));
#99994=DIRECTION('',(-0.981627005099017,0.,-0.190809912898503));
#99995=DIRECTION('center_axis',(-0.981627005099017,0.,-0.190809912898503));
#99996=DIRECTION('ref_axis',(-0.190809912898503,0.,0.981627005099017));
#99997=DIRECTION('',(0.,1.,0.));
#99998=DIRECTION('',(0.,1.,0.));
#99999=DIRECTION('center_axis',(0.,1.,0.));
#100000=DIRECTION('ref_axis',(1.,0.,0.));
#100001=DIRECTION('',(-0.190809912898503,0.,0.981627005099017));
#100002=DIRECTION('',(0.981627005099017,0.,0.190809912898503));
#100003=DIRECTION('',(-0.190809912898503,0.,0.981627005099017));
#100004=DIRECTION('',(0.981627005099017,0.,0.190809912898503));
#100005=DIRECTION('center_axis',(0.981627005099017,0.,0.190809912898503));
#100006=DIRECTION('ref_axis',(0.,-1.,0.));
#100007=DIRECTION('',(-0.190809912898503,0.,0.981627005099017));
#100008=DIRECTION('',(0.,-1.,0.));
#100009=DIRECTION('',(0.,-1.,0.));
#100010=DIRECTION('center_axis',(0.,-1.,0.));
#100011=DIRECTION('ref_axis',(0.,0.,-1.));
#100012=DIRECTION('',(-0.190809912898503,0.,0.981627005099017));
#100013=DIRECTION('',(-0.981627005099017,0.,-0.190809912898503));
#100014=DIRECTION('',(-0.981627005099017,0.,-0.190809912898503));
#100015=DIRECTION('center_axis',(-0.981627005099017,0.,-0.190809912898503));
#100016=DIRECTION('ref_axis',(-0.190809912898503,0.,0.981627005099017));
#100017=DIRECTION('',(0.,1.,0.));
#100018=DIRECTION('',(0.,1.,0.));
#100019=DIRECTION('center_axis',(0.,1.,0.));
#100020=DIRECTION('ref_axis',(1.,0.,0.));
#100021=DIRECTION('',(-0.190809912898503,0.,0.981627005099017));
#100022=DIRECTION('',(0.981627005099017,0.,0.190809912898503));
#100023=DIRECTION('',(-0.190809912898503,0.,0.981627005099017));
#100024=DIRECTION('',(0.981627005099017,0.,0.190809912898503));
#100025=DIRECTION('center_axis',(0.981627005099017,0.,0.190809912898503));
#100026=DIRECTION('ref_axis',(0.,-1.,0.));
#100027=DIRECTION('',(-0.190809912898503,0.,0.981627005099017));
#100028=DIRECTION('',(0.,-1.,0.));
#100029=DIRECTION('',(0.,-1.,0.));
#100030=DIRECTION('center_axis',(0.,-1.,0.));
#100031=DIRECTION('ref_axis',(0.,0.,-1.));
#100032=DIRECTION('',(-0.190809912898503,0.,0.981627005099017));
#100033=DIRECTION('',(-0.981627005099017,0.,-0.190809912898503));
#100034=DIRECTION('',(-0.981627005099017,0.,-0.190809912898503));
#100035=DIRECTION('center_axis',(-0.981627005099017,0.,-0.190809912898503));
#100036=DIRECTION('ref_axis',(-0.190809912898503,0.,0.981627005099017));
#100037=DIRECTION('',(0.,1.,0.));
#100038=DIRECTION('',(0.,1.,0.));
#100039=DIRECTION('center_axis',(0.,1.,0.));
#100040=DIRECTION('ref_axis',(1.,0.,0.));
#100041=DIRECTION('',(-0.190809912898503,0.,0.981627005099017));
#100042=DIRECTION('',(0.981627005099017,0.,0.190809912898503));
#100043=DIRECTION('',(-0.190809912898503,0.,0.981627005099017));
#100044=DIRECTION('',(0.981627005099017,0.,0.190809912898503));
#100045=DIRECTION('center_axis',(0.981627005099017,0.,0.190809912898503));
#100046=DIRECTION('ref_axis',(0.,-1.,0.));
#100047=DIRECTION('',(-0.190809912898503,0.,0.981627005099017));
#100048=DIRECTION('',(0.,-1.,0.));
#100049=DIRECTION('',(0.,-1.,0.));
#100050=DIRECTION('center_axis',(0.,-1.,0.));
#100051=DIRECTION('ref_axis',(0.,0.,-1.));
#100052=DIRECTION('',(-0.190809912898503,0.,0.981627005099017));
#100053=DIRECTION('',(-0.981627005099017,0.,-0.190809912898503));
#100054=DIRECTION('',(-0.981627005099017,0.,-0.190809912898503));
#100055=DIRECTION('center_axis',(-0.981627005099017,0.,-0.190809912898503));
#100056=DIRECTION('ref_axis',(-0.190809912898503,0.,0.981627005099017));
#100057=DIRECTION('',(0.,1.,0.));
#100058=DIRECTION('',(0.,1.,0.));
#100059=DIRECTION('center_axis',(0.,1.,0.));
#100060=DIRECTION('ref_axis',(1.,0.,0.));
#100061=DIRECTION('',(-0.190809912898503,0.,0.981627005099017));
#100062=DIRECTION('',(0.981627005099017,0.,0.190809912898503));
#100063=DIRECTION('',(-0.190809912898503,0.,0.981627005099017));
#100064=DIRECTION('',(0.981627005099017,0.,0.190809912898503));
#100065=DIRECTION('center_axis',(0.981627005099017,0.,0.190809912898503));
#100066=DIRECTION('ref_axis',(0.,-1.,0.));
#100067=DIRECTION('',(-0.190809912898503,0.,0.981627005099017));
#100068=DIRECTION('',(0.,-1.,0.));
#100069=DIRECTION('',(0.,-1.,0.));
#100070=DIRECTION('center_axis',(0.,-1.,0.));
#100071=DIRECTION('ref_axis',(0.,0.,-1.));
#100072=DIRECTION('',(-0.190809912898503,0.,0.981627005099017));
#100073=DIRECTION('',(-0.981627005099017,0.,-0.190809912898503));
#100074=DIRECTION('',(-0.981627005099017,0.,-0.190809912898503));
#100075=DIRECTION('center_axis',(-0.981627005099017,0.,-0.190809912898503));
#100076=DIRECTION('ref_axis',(-0.190809912898503,0.,0.981627005099017));
#100077=DIRECTION('',(0.,1.,0.));
#100078=DIRECTION('',(0.,1.,0.));
#100079=DIRECTION('center_axis',(0.,1.,0.));
#100080=DIRECTION('ref_axis',(1.,0.,0.));
#100081=DIRECTION('',(-0.190809912898503,0.,0.981627005099017));
#100082=DIRECTION('',(0.981627005099017,0.,0.190809912898503));
#100083=DIRECTION('',(-0.190809912898503,0.,0.981627005099017));
#100084=DIRECTION('',(0.981627005099017,0.,0.190809912898503));
#100085=DIRECTION('center_axis',(0.981627005099017,0.,0.190809912898503));
#100086=DIRECTION('ref_axis',(0.,-1.,0.));
#100087=DIRECTION('',(-0.190809912898503,0.,0.981627005099017));
#100088=DIRECTION('',(0.,-1.,0.));
#100089=DIRECTION('',(0.,-1.,0.));
#100090=DIRECTION('center_axis',(0.,-1.,0.));
#100091=DIRECTION('ref_axis',(0.,0.,-1.));
#100092=DIRECTION('',(-0.190809912898503,0.,0.981627005099017));
#100093=DIRECTION('',(-0.981627005099017,0.,-0.190809912898503));
#100094=DIRECTION('',(-0.981627005099017,0.,-0.190809912898503));
#100095=DIRECTION('center_axis',(-0.981627005099017,0.,-0.190809912898503));
#100096=DIRECTION('ref_axis',(-0.190809912898503,0.,0.981627005099017));
#100097=DIRECTION('',(0.,1.,0.));
#100098=DIRECTION('',(0.,1.,0.));
#100099=DIRECTION('center_axis',(0.,1.,0.));
#100100=DIRECTION('ref_axis',(1.,0.,0.));
#100101=DIRECTION('',(-0.190809912898503,0.,0.981627005099017));
#100102=DIRECTION('',(0.981627005099017,0.,0.190809912898503));
#100103=DIRECTION('',(-0.190809912898503,0.,0.981627005099017));
#100104=DIRECTION('',(0.981627005099017,0.,0.190809912898503));
#100105=DIRECTION('center_axis',(0.981627005099017,0.,0.190809912898503));
#100106=DIRECTION('ref_axis',(0.,-1.,0.));
#100107=DIRECTION('',(-0.190809912898503,0.,0.981627005099017));
#100108=DIRECTION('',(0.,-1.,0.));
#100109=DIRECTION('',(0.,-1.,0.));
#100110=DIRECTION('center_axis',(0.,-1.,0.));
#100111=DIRECTION('ref_axis',(0.,0.,-1.));
#100112=DIRECTION('',(-0.190809912898503,0.,0.981627005099017));
#100113=DIRECTION('',(-0.981627005099017,0.,-0.190809912898503));
#100114=DIRECTION('',(-0.981627005099017,0.,-0.190809912898503));
#100115=DIRECTION('center_axis',(-0.981627005099017,0.,-0.190809912898503));
#100116=DIRECTION('ref_axis',(-0.190809912898503,0.,0.981627005099017));
#100117=DIRECTION('',(0.,1.,0.));
#100118=DIRECTION('',(0.,1.,0.));
#100119=DIRECTION('center_axis',(0.,1.,0.));
#100120=DIRECTION('ref_axis',(1.,0.,0.));
#100121=DIRECTION('',(-0.190809912898503,0.,0.981627005099017));
#100122=DIRECTION('',(0.981627005099017,0.,0.190809912898503));
#100123=DIRECTION('',(-0.190809912898503,0.,0.981627005099017));
#100124=DIRECTION('',(0.981627005099017,0.,0.190809912898503));
#100125=DIRECTION('center_axis',(0.981627005099017,0.,0.190809912898503));
#100126=DIRECTION('ref_axis',(0.,-1.,0.));
#100127=DIRECTION('',(-0.190809912898503,0.,0.981627005099017));
#100128=DIRECTION('',(0.,-1.,0.));
#100129=DIRECTION('',(0.,-1.,0.));
#100130=DIRECTION('center_axis',(0.,-1.,0.));
#100131=DIRECTION('ref_axis',(0.,0.,-1.));
#100132=DIRECTION('',(-0.190809912898503,0.,0.981627005099017));
#100133=DIRECTION('',(-0.981627005099017,0.,-0.190809912898503));
#100134=DIRECTION('',(-0.981627005099017,0.,-0.190809912898503));
#100135=DIRECTION('center_axis',(-0.981627005099017,0.,-0.190809912898503));
#100136=DIRECTION('ref_axis',(-0.190809912898503,0.,0.981627005099017));
#100137=DIRECTION('',(0.,1.,0.));
#100138=DIRECTION('',(0.,1.,0.));
#100139=DIRECTION('center_axis',(0.,1.,0.));
#100140=DIRECTION('ref_axis',(1.,0.,0.));
#100141=DIRECTION('',(-0.190809912898503,0.,0.981627005099017));
#100142=DIRECTION('',(0.981627005099017,0.,0.190809912898503));
#100143=DIRECTION('',(-0.190809912898503,0.,0.981627005099017));
#100144=DIRECTION('',(0.981627005099017,0.,0.190809912898503));
#100145=DIRECTION('center_axis',(0.981627005099017,0.,0.190809912898503));
#100146=DIRECTION('ref_axis',(0.,-1.,0.));
#100147=DIRECTION('',(-0.190809912898503,0.,0.981627005099017));
#100148=DIRECTION('',(0.,-1.,0.));
#100149=DIRECTION('',(0.,-1.,0.));
#100150=DIRECTION('center_axis',(0.,-1.,0.));
#100151=DIRECTION('ref_axis',(0.,0.,-1.));
#100152=DIRECTION('',(-0.190809912898503,0.,0.981627005099017));
#100153=DIRECTION('',(-0.981627005099017,0.,-0.190809912898503));
#100154=DIRECTION('',(-0.981627005099017,0.,-0.190809912898503));
#100155=DIRECTION('center_axis',(-0.981627005099017,0.,-0.190809912898503));
#100156=DIRECTION('ref_axis',(-0.190809912898503,0.,0.981627005099017));
#100157=DIRECTION('',(0.,1.,0.));
#100158=DIRECTION('',(0.,1.,0.));
#100159=DIRECTION('center_axis',(0.,1.,0.));
#100160=DIRECTION('ref_axis',(1.,0.,0.));
#100161=DIRECTION('',(-0.190809912898503,0.,0.981627005099017));
#100162=DIRECTION('',(0.981627005099017,0.,0.190809912898503));
#100163=DIRECTION('',(-0.190809912898503,0.,0.981627005099017));
#100164=DIRECTION('',(0.981627005099017,0.,0.190809912898503));
#100165=DIRECTION('center_axis',(0.981627005099017,0.,0.190809912898503));
#100166=DIRECTION('ref_axis',(0.,-1.,0.));
#100167=DIRECTION('',(-0.190809912898503,0.,0.981627005099017));
#100168=DIRECTION('',(0.,-1.,0.));
#100169=DIRECTION('',(0.,-1.,0.));
#100170=DIRECTION('center_axis',(0.,-1.,0.));
#100171=DIRECTION('ref_axis',(0.,0.,-1.));
#100172=DIRECTION('',(-0.190809912898503,0.,0.981627005099017));
#100173=DIRECTION('',(-0.981627005099017,0.,-0.190809912898503));
#100174=DIRECTION('',(-0.981627005099017,0.,-0.190809912898503));
#100175=DIRECTION('center_axis',(-0.981627005099017,0.,-0.190809912898503));
#100176=DIRECTION('ref_axis',(-0.190809912898503,0.,0.981627005099017));
#100177=DIRECTION('',(0.,1.,0.));
#100178=DIRECTION('',(0.,1.,0.));
#100179=DIRECTION('center_axis',(0.,1.,0.));
#100180=DIRECTION('ref_axis',(1.,0.,0.));
#100181=DIRECTION('',(-0.190809912898503,0.,0.981627005099017));
#100182=DIRECTION('',(0.981627005099017,0.,0.190809912898503));
#100183=DIRECTION('',(-0.190809912898503,0.,0.981627005099017));
#100184=DIRECTION('',(0.981627005099017,0.,0.190809912898503));
#100185=DIRECTION('center_axis',(0.981627005099017,0.,0.190809912898503));
#100186=DIRECTION('ref_axis',(0.,-1.,0.));
#100187=DIRECTION('',(-0.190809912898503,0.,0.981627005099017));
#100188=DIRECTION('',(0.,-1.,0.));
#100189=DIRECTION('',(0.,-1.,0.));
#100190=DIRECTION('center_axis',(0.,-1.,0.));
#100191=DIRECTION('ref_axis',(0.,0.,-1.));
#100192=DIRECTION('',(-0.190809912898503,0.,0.981627005099017));
#100193=DIRECTION('',(-0.981627005099017,0.,-0.190809912898503));
#100194=DIRECTION('',(-0.981627005099017,0.,-0.190809912898503));
#100195=DIRECTION('center_axis',(-0.981627005099017,0.,-0.190809912898503));
#100196=DIRECTION('ref_axis',(-0.190809912898503,0.,0.981627005099017));
#100197=DIRECTION('',(0.,1.,0.));
#100198=DIRECTION('',(0.,1.,0.));
#100199=DIRECTION('center_axis',(0.,1.,0.));
#100200=DIRECTION('ref_axis',(1.,0.,0.));
#100201=DIRECTION('',(-0.190809912898503,0.,0.981627005099017));
#100202=DIRECTION('',(0.981627005099017,0.,0.190809912898503));
#100203=DIRECTION('',(-0.190809912898503,0.,0.981627005099017));
#100204=DIRECTION('',(0.981627005099017,0.,0.190809912898503));
#100205=DIRECTION('center_axis',(0.981627005099017,0.,0.190809912898503));
#100206=DIRECTION('ref_axis',(0.,-1.,0.));
#100207=DIRECTION('',(-0.190809912898503,0.,0.981627005099017));
#100208=DIRECTION('',(0.,-1.,0.));
#100209=DIRECTION('',(0.,-1.,0.));
#100210=DIRECTION('center_axis',(0.,-1.,0.));
#100211=DIRECTION('ref_axis',(0.,0.,-1.));
#100212=DIRECTION('',(-0.190809912898503,0.,0.981627005099017));
#100213=DIRECTION('',(-0.981627005099017,0.,-0.190809912898503));
#100214=DIRECTION('',(-0.981627005099017,0.,-0.190809912898503));
#100215=DIRECTION('center_axis',(-0.981627005099017,0.,-0.190809912898503));
#100216=DIRECTION('ref_axis',(-0.190809912898503,0.,0.981627005099017));
#100217=DIRECTION('',(0.,1.,0.));
#100218=DIRECTION('',(0.,1.,0.));
#100219=DIRECTION('center_axis',(0.,1.,0.));
#100220=DIRECTION('ref_axis',(1.,0.,0.));
#100221=DIRECTION('',(-0.190809912898503,0.,0.981627005099017));
#100222=DIRECTION('',(0.981627005099017,0.,0.190809912898503));
#100223=DIRECTION('',(-0.190809912898503,0.,0.981627005099017));
#100224=DIRECTION('',(0.981627005099017,0.,0.190809912898503));
#100225=DIRECTION('center_axis',(0.981627005099017,0.,0.190809912898503));
#100226=DIRECTION('ref_axis',(0.,-1.,0.));
#100227=DIRECTION('',(-0.190809912898503,0.,0.981627005099017));
#100228=DIRECTION('',(0.,-1.,0.));
#100229=DIRECTION('',(0.,-1.,0.));
#100230=DIRECTION('center_axis',(0.,-1.,0.));
#100231=DIRECTION('ref_axis',(0.,0.,-1.));
#100232=DIRECTION('',(-0.190809912898503,0.,0.981627005099017));
#100233=DIRECTION('',(-0.981627005099017,0.,-0.190809912898503));
#100234=DIRECTION('',(-0.981627005099017,0.,-0.190809912898503));
#100235=DIRECTION('center_axis',(-0.981627005099017,0.,-0.190809912898503));
#100236=DIRECTION('ref_axis',(-0.190809912898503,0.,0.981627005099017));
#100237=DIRECTION('',(0.,1.,0.));
#100238=DIRECTION('',(0.,1.,0.));
#100239=DIRECTION('center_axis',(0.,1.,0.));
#100240=DIRECTION('ref_axis',(1.,0.,0.));
#100241=DIRECTION('',(-0.190809912898503,0.,0.981627005099017));
#100242=DIRECTION('',(0.981627005099017,0.,0.190809912898503));
#100243=DIRECTION('',(-0.190809912898503,0.,0.981627005099017));
#100244=DIRECTION('',(0.981627005099017,0.,0.190809912898503));
#100245=DIRECTION('center_axis',(0.981627005099017,0.,0.190809912898503));
#100246=DIRECTION('ref_axis',(0.,-1.,0.));
#100247=DIRECTION('',(-0.190809912898503,0.,0.981627005099017));
#100248=DIRECTION('',(0.,-1.,0.));
#100249=DIRECTION('',(0.,-1.,0.));
#100250=DIRECTION('center_axis',(0.,-1.,0.));
#100251=DIRECTION('ref_axis',(0.,0.,-1.));
#100252=DIRECTION('',(-0.190809912898503,0.,0.981627005099017));
#100253=DIRECTION('',(-0.981627005099017,0.,-0.190809912898503));
#100254=DIRECTION('',(-0.981627005099017,0.,-0.190809912898503));
#100255=DIRECTION('center_axis',(-0.981627005099017,0.,-0.190809912898503));
#100256=DIRECTION('ref_axis',(-0.190809912898503,0.,0.981627005099017));
#100257=DIRECTION('',(0.,1.,0.));
#100258=DIRECTION('',(0.,1.,0.));
#100259=DIRECTION('center_axis',(0.,1.,0.));
#100260=DIRECTION('ref_axis',(1.,0.,0.));
#100261=DIRECTION('',(-0.190809912898503,0.,0.981627005099017));
#100262=DIRECTION('',(0.981627005099017,0.,0.190809912898503));
#100263=DIRECTION('',(-0.190809912898503,0.,0.981627005099017));
#100264=DIRECTION('',(0.981627005099017,0.,0.190809912898503));
#100265=DIRECTION('center_axis',(0.981627005099017,0.,0.190809912898503));
#100266=DIRECTION('ref_axis',(0.,-1.,0.));
#100267=DIRECTION('',(-0.190809912898503,0.,0.981627005099017));
#100268=DIRECTION('',(0.,-1.,0.));
#100269=DIRECTION('',(0.,-1.,0.));
#100270=DIRECTION('center_axis',(0.,-1.,0.));
#100271=DIRECTION('ref_axis',(0.,0.,-1.));
#100272=DIRECTION('',(-0.190809912898503,0.,0.981627005099017));
#100273=DIRECTION('',(-0.981627005099017,0.,-0.190809912898503));
#100274=DIRECTION('',(-0.981627005099017,0.,-0.190809912898503));
#100275=DIRECTION('center_axis',(-0.981627005099017,0.,-0.190809912898503));
#100276=DIRECTION('ref_axis',(-0.190809912898503,0.,0.981627005099017));
#100277=DIRECTION('',(0.,1.,0.));
#100278=DIRECTION('',(0.,1.,0.));
#100279=DIRECTION('center_axis',(0.,1.,0.));
#100280=DIRECTION('ref_axis',(1.,0.,0.));
#100281=DIRECTION('',(-0.190809912898503,0.,0.981627005099017));
#100282=DIRECTION('',(0.981627005099017,0.,0.190809912898503));
#100283=DIRECTION('',(-0.190809912898503,0.,0.981627005099017));
#100284=DIRECTION('',(0.981627005099017,0.,0.190809912898503));
#100285=DIRECTION('center_axis',(0.981627005099017,0.,0.190809912898503));
#100286=DIRECTION('ref_axis',(0.,-1.,0.));
#100287=DIRECTION('',(-0.190809912898503,0.,0.981627005099017));
#100288=DIRECTION('',(0.,-1.,0.));
#100289=DIRECTION('',(0.,-1.,0.));
#100290=DIRECTION('center_axis',(0.,-1.,0.));
#100291=DIRECTION('ref_axis',(0.,0.,-1.));
#100292=DIRECTION('',(-0.190809912898503,0.,0.981627005099017));
#100293=DIRECTION('',(-0.981627005099017,0.,-0.190809912898503));
#100294=DIRECTION('',(-0.981627005099017,0.,-0.190809912898503));
#100295=DIRECTION('center_axis',(-0.981627005099017,0.,-0.190809912898503));
#100296=DIRECTION('ref_axis',(-0.190809912898503,0.,0.981627005099017));
#100297=DIRECTION('',(0.,1.,0.));
#100298=DIRECTION('',(0.,1.,0.));
#100299=DIRECTION('center_axis',(0.,1.,0.));
#100300=DIRECTION('ref_axis',(1.,0.,0.));
#100301=DIRECTION('',(-0.190809912898503,0.,0.981627005099017));
#100302=DIRECTION('',(0.981627005099017,0.,0.190809912898503));
#100303=DIRECTION('',(-0.190809912898503,0.,0.981627005099017));
#100304=DIRECTION('',(0.981627005099017,0.,0.190809912898503));
#100305=DIRECTION('center_axis',(0.981627005099017,0.,0.190809912898503));
#100306=DIRECTION('ref_axis',(0.,-1.,0.));
#100307=DIRECTION('',(-0.190809912898503,0.,0.981627005099017));
#100308=DIRECTION('',(0.,-1.,0.));
#100309=DIRECTION('',(0.,-1.,0.));
#100310=DIRECTION('center_axis',(0.,-1.,0.));
#100311=DIRECTION('ref_axis',(0.,0.,-1.));
#100312=DIRECTION('',(-0.190809912898503,0.,0.981627005099017));
#100313=DIRECTION('',(-0.981627005099017,0.,-0.190809912898503));
#100314=DIRECTION('',(-0.981627005099017,0.,-0.190809912898503));
#100315=DIRECTION('center_axis',(-0.981627005099017,0.,-0.190809912898503));
#100316=DIRECTION('ref_axis',(-0.190809912898503,0.,0.981627005099017));
#100317=DIRECTION('',(0.,1.,0.));
#100318=DIRECTION('',(0.,1.,0.));
#100319=DIRECTION('center_axis',(0.,1.,0.));
#100320=DIRECTION('ref_axis',(1.,0.,0.));
#100321=DIRECTION('',(-0.190809912898503,0.,0.981627005099017));
#100322=DIRECTION('',(0.981627005099017,0.,0.190809912898503));
#100323=DIRECTION('',(-0.190809912898503,0.,0.981627005099017));
#100324=DIRECTION('',(0.981627005099017,0.,0.190809912898503));
#100325=DIRECTION('center_axis',(0.981627005099017,0.,0.190809912898503));
#100326=DIRECTION('ref_axis',(0.,-1.,0.));
#100327=DIRECTION('',(-0.190809912898503,0.,0.981627005099017));
#100328=DIRECTION('',(0.,-1.,0.));
#100329=DIRECTION('',(0.,-1.,0.));
#100330=DIRECTION('center_axis',(0.,-1.,0.));
#100331=DIRECTION('ref_axis',(0.,0.,-1.));
#100332=DIRECTION('',(-0.190809912898503,0.,0.981627005099017));
#100333=DIRECTION('',(-0.981627005099017,0.,-0.190809912898503));
#100334=DIRECTION('',(-0.981627005099017,0.,-0.190809912898503));
#100335=DIRECTION('center_axis',(-0.981627005099017,0.,-0.190809912898503));
#100336=DIRECTION('ref_axis',(-0.190809912898503,0.,0.981627005099017));
#100337=DIRECTION('',(0.,1.,0.));
#100338=DIRECTION('',(0.,1.,0.));
#100339=DIRECTION('center_axis',(0.,1.,0.));
#100340=DIRECTION('ref_axis',(1.,0.,0.));
#100341=DIRECTION('',(-0.190809912898503,0.,0.981627005099017));
#100342=DIRECTION('',(0.981627005099017,0.,0.190809912898503));
#100343=DIRECTION('',(-0.190809912898503,0.,0.981627005099017));
#100344=DIRECTION('',(0.981627005099017,0.,0.190809912898503));
#100345=DIRECTION('center_axis',(0.981627005099017,0.,0.190809912898503));
#100346=DIRECTION('ref_axis',(0.,-1.,0.));
#100347=DIRECTION('',(-0.190809912898503,0.,0.981627005099017));
#100348=DIRECTION('',(0.,-1.,0.));
#100349=DIRECTION('',(0.,-1.,0.));
#100350=DIRECTION('center_axis',(0.,-1.,0.));
#100351=DIRECTION('ref_axis',(0.,0.,-1.));
#100352=DIRECTION('',(-0.190809912898503,0.,0.981627005099017));
#100353=DIRECTION('',(-0.981627005099017,0.,-0.190809912898503));
#100354=DIRECTION('',(-0.981627005099017,0.,-0.190809912898503));
#100355=DIRECTION('center_axis',(-0.981627005099017,0.,-0.190809912898503));
#100356=DIRECTION('ref_axis',(-0.190809912898503,0.,0.981627005099017));
#100357=DIRECTION('',(0.,1.,0.));
#100358=DIRECTION('',(0.,1.,0.));
#100359=DIRECTION('center_axis',(0.,1.,0.));
#100360=DIRECTION('ref_axis',(1.,0.,0.));
#100361=DIRECTION('',(-0.190809912898503,0.,0.981627005099017));
#100362=DIRECTION('',(0.981627005099017,0.,0.190809912898503));
#100363=DIRECTION('',(-0.190809912898503,0.,0.981627005099017));
#100364=DIRECTION('',(0.981627005099017,0.,0.190809912898503));
#100365=DIRECTION('center_axis',(0.981627005099017,0.,0.190809912898503));
#100366=DIRECTION('ref_axis',(0.,-1.,0.));
#100367=DIRECTION('',(-0.190809912898503,0.,0.981627005099017));
#100368=DIRECTION('',(0.,-1.,0.));
#100369=DIRECTION('',(0.,-1.,0.));
#100370=DIRECTION('center_axis',(0.,-1.,0.));
#100371=DIRECTION('ref_axis',(0.,0.,-1.));
#100372=DIRECTION('',(-0.190809912898503,0.,0.981627005099017));
#100373=DIRECTION('',(-0.981627005099017,0.,-0.190809912898503));
#100374=DIRECTION('',(-0.981627005099017,0.,-0.190809912898503));
#100375=DIRECTION('center_axis',(-0.981627005099017,0.,-0.190809912898503));
#100376=DIRECTION('ref_axis',(-0.190809912898503,0.,0.981627005099017));
#100377=DIRECTION('',(0.,1.,0.));
#100378=DIRECTION('',(0.,1.,0.));
#100379=DIRECTION('center_axis',(0.,1.,0.));
#100380=DIRECTION('ref_axis',(1.,0.,0.));
#100381=DIRECTION('',(-0.190809912898503,0.,0.981627005099017));
#100382=DIRECTION('',(0.981627005099017,0.,0.190809912898503));
#100383=DIRECTION('',(-0.190809912898503,0.,0.981627005099017));
#100384=DIRECTION('',(0.981627005099017,0.,0.190809912898503));
#100385=DIRECTION('center_axis',(0.981627005099017,0.,0.190809912898503));
#100386=DIRECTION('ref_axis',(0.,-1.,0.));
#100387=DIRECTION('',(-0.190809912898503,0.,0.981627005099017));
#100388=DIRECTION('',(0.,-1.,0.));
#100389=DIRECTION('',(0.,-1.,0.));
#100390=DIRECTION('center_axis',(0.,-1.,0.));
#100391=DIRECTION('ref_axis',(0.,0.,-1.));
#100392=DIRECTION('',(-0.190809912898503,0.,0.981627005099017));
#100393=DIRECTION('',(-0.981627005099017,0.,-0.190809912898503));
#100394=DIRECTION('',(-0.981627005099017,0.,-0.190809912898503));
#100395=DIRECTION('center_axis',(-0.981627005099017,0.,-0.190809912898503));
#100396=DIRECTION('ref_axis',(-0.190809912898503,0.,0.981627005099017));
#100397=DIRECTION('',(0.,1.,0.));
#100398=DIRECTION('',(0.,1.,0.));
#100399=DIRECTION('center_axis',(0.,1.,0.));
#100400=DIRECTION('ref_axis',(1.,0.,0.));
#100401=DIRECTION('',(-0.190809912898503,0.,0.981627005099017));
#100402=DIRECTION('',(0.981627005099017,0.,0.190809912898503));
#100403=DIRECTION('',(-0.190809912898503,0.,0.981627005099017));
#100404=DIRECTION('',(0.981627005099017,0.,0.190809912898503));
#100405=DIRECTION('center_axis',(0.981627005099017,0.,0.190809912898503));
#100406=DIRECTION('ref_axis',(0.,-1.,0.));
#100407=DIRECTION('',(-0.190809912898503,0.,0.981627005099017));
#100408=DIRECTION('',(0.,-1.,0.));
#100409=DIRECTION('',(0.,-1.,0.));
#100410=DIRECTION('center_axis',(0.,-1.,0.));
#100411=DIRECTION('ref_axis',(0.,0.,-1.));
#100412=DIRECTION('',(-0.190809912898503,0.,0.981627005099017));
#100413=DIRECTION('',(-0.981627005099017,0.,-0.190809912898503));
#100414=DIRECTION('',(-0.981627005099017,0.,-0.190809912898503));
#100415=DIRECTION('center_axis',(-0.981627005099017,0.,-0.190809912898503));
#100416=DIRECTION('ref_axis',(-0.190809912898503,0.,0.981627005099017));
#100417=DIRECTION('',(0.,1.,0.));
#100418=DIRECTION('',(0.,1.,0.));
#100419=DIRECTION('center_axis',(0.,1.,0.));
#100420=DIRECTION('ref_axis',(1.,0.,0.));
#100421=DIRECTION('',(-0.190809912898503,0.,0.981627005099017));
#100422=DIRECTION('',(0.981627005099017,0.,0.190809912898503));
#100423=DIRECTION('',(-0.190809912898503,0.,0.981627005099017));
#100424=DIRECTION('',(0.981627005099017,0.,0.190809912898503));
#100425=DIRECTION('center_axis',(0.981627005099017,0.,0.190809912898503));
#100426=DIRECTION('ref_axis',(0.,-1.,0.));
#100427=DIRECTION('',(-0.190809912898503,0.,0.981627005099017));
#100428=DIRECTION('',(0.,-1.,0.));
#100429=DIRECTION('',(0.,-1.,0.));
#100430=DIRECTION('center_axis',(0.,-1.,0.));
#100431=DIRECTION('ref_axis',(0.,0.,-1.));
#100432=DIRECTION('',(-0.190809912898503,0.,0.981627005099017));
#100433=DIRECTION('',(-0.981627005099017,0.,-0.190809912898503));
#100434=DIRECTION('',(-0.981627005099017,0.,-0.190809912898503));
#100435=DIRECTION('center_axis',(-0.981627005099017,0.,-0.190809912898503));
#100436=DIRECTION('ref_axis',(-0.190809912898503,0.,0.981627005099017));
#100437=DIRECTION('',(0.,1.,0.));
#100438=DIRECTION('',(0.,1.,0.));
#100439=DIRECTION('center_axis',(0.,1.,0.));
#100440=DIRECTION('ref_axis',(1.,0.,0.));
#100441=DIRECTION('',(-0.190809912898503,0.,0.981627005099017));
#100442=DIRECTION('',(0.981627005099017,0.,0.190809912898503));
#100443=DIRECTION('',(-0.190809912898503,0.,0.981627005099017));
#100444=DIRECTION('',(0.981627005099017,0.,0.190809912898503));
#100445=DIRECTION('center_axis',(0.981627005099017,0.,0.190809912898503));
#100446=DIRECTION('ref_axis',(0.,-1.,0.));
#100447=DIRECTION('',(-0.190809912898503,0.,0.981627005099017));
#100448=DIRECTION('',(0.,-1.,0.));
#100449=DIRECTION('',(0.,-1.,0.));
#100450=DIRECTION('center_axis',(0.,-1.,0.));
#100451=DIRECTION('ref_axis',(0.,0.,-1.));
#100452=DIRECTION('',(-0.190809912898503,0.,0.981627005099017));
#100453=DIRECTION('',(-0.981627005099017,0.,-0.190809912898503));
#100454=DIRECTION('',(-0.981627005099017,0.,-0.190809912898503));
#100455=DIRECTION('center_axis',(-0.981627005099017,0.,-0.190809912898503));
#100456=DIRECTION('ref_axis',(-0.190809912898503,0.,0.981627005099017));
#100457=DIRECTION('',(0.,1.,0.));
#100458=DIRECTION('',(0.,1.,0.));
#100459=DIRECTION('center_axis',(0.,1.,0.));
#100460=DIRECTION('ref_axis',(1.,0.,0.));
#100461=DIRECTION('',(-0.190809912898503,0.,0.981627005099017));
#100462=DIRECTION('',(0.981627005099017,0.,0.190809912898503));
#100463=DIRECTION('',(-0.190809912898503,0.,0.981627005099017));
#100464=DIRECTION('',(0.981627005099017,0.,0.190809912898503));
#100465=DIRECTION('center_axis',(0.981627005099017,0.,0.190809912898503));
#100466=DIRECTION('ref_axis',(0.,-1.,0.));
#100467=DIRECTION('',(-0.190809912898503,0.,0.981627005099017));
#100468=DIRECTION('',(0.,-1.,0.));
#100469=DIRECTION('',(0.,-1.,0.));
#100470=DIRECTION('center_axis',(0.,-1.,0.));
#100471=DIRECTION('ref_axis',(0.,0.,-1.));
#100472=DIRECTION('',(-0.190809912898503,0.,0.981627005099017));
#100473=DIRECTION('',(-0.981627005099017,0.,-0.190809912898503));
#100474=DIRECTION('',(-0.981627005099017,0.,-0.190809912898503));
#100475=DIRECTION('center_axis',(-0.981627005099017,0.,-0.190809912898503));
#100476=DIRECTION('ref_axis',(-0.190809912898503,0.,0.981627005099017));
#100477=DIRECTION('',(0.,1.,0.));
#100478=DIRECTION('',(0.,1.,0.));
#100479=DIRECTION('center_axis',(0.,1.,0.));
#100480=DIRECTION('ref_axis',(1.,0.,0.));
#100481=DIRECTION('',(-0.190809912898503,0.,0.981627005099017));
#100482=DIRECTION('',(0.981627005099017,0.,0.190809912898503));
#100483=DIRECTION('',(-0.190809912898503,0.,0.981627005099017));
#100484=DIRECTION('',(0.981627005099017,0.,0.190809912898503));
#100485=DIRECTION('center_axis',(0.981627005099017,0.,0.190809912898503));
#100486=DIRECTION('ref_axis',(0.,-1.,0.));
#100487=DIRECTION('',(-0.190809912898503,0.,0.981627005099017));
#100488=DIRECTION('',(0.,-1.,0.));
#100489=DIRECTION('',(0.,-1.,0.));
#100490=DIRECTION('center_axis',(0.,-1.,0.));
#100491=DIRECTION('ref_axis',(0.,0.,-1.));
#100492=DIRECTION('',(-0.190809912898503,0.,0.981627005099017));
#100493=DIRECTION('',(-0.981627005099017,0.,-0.190809912898503));
#100494=DIRECTION('',(-0.981627005099017,0.,-0.190809912898503));
#100495=DIRECTION('center_axis',(-0.981627005099017,0.,-0.190809912898503));
#100496=DIRECTION('ref_axis',(-0.190809912898503,0.,0.981627005099017));
#100497=DIRECTION('',(0.,1.,0.));
#100498=DIRECTION('',(0.,1.,0.));
#100499=DIRECTION('center_axis',(0.,1.,0.));
#100500=DIRECTION('ref_axis',(1.,0.,0.));
#100501=DIRECTION('',(-0.190809912898503,0.,0.981627005099017));
#100502=DIRECTION('',(0.981627005099017,0.,0.190809912898503));
#100503=DIRECTION('',(-0.190809912898503,0.,0.981627005099017));
#100504=DIRECTION('',(0.981627005099017,0.,0.190809912898503));
#100505=DIRECTION('center_axis',(0.981627005099017,0.,0.190809912898503));
#100506=DIRECTION('ref_axis',(0.,-1.,0.));
#100507=DIRECTION('',(-0.190809912898503,0.,0.981627005099017));
#100508=DIRECTION('',(0.,-1.,0.));
#100509=DIRECTION('',(0.,-1.,0.));
#100510=DIRECTION('center_axis',(0.,-1.,0.));
#100511=DIRECTION('ref_axis',(0.,0.,-1.));
#100512=DIRECTION('',(-0.190809912898503,0.,0.981627005099017));
#100513=DIRECTION('',(-0.981627005099017,0.,-0.190809912898503));
#100514=DIRECTION('',(-0.981627005099017,0.,-0.190809912898503));
#100515=DIRECTION('center_axis',(-0.981627005099017,0.,-0.190809912898503));
#100516=DIRECTION('ref_axis',(-0.190809912898503,0.,0.981627005099017));
#100517=DIRECTION('',(0.,1.,0.));
#100518=DIRECTION('',(0.,1.,0.));
#100519=DIRECTION('center_axis',(0.,1.,0.));
#100520=DIRECTION('ref_axis',(1.,0.,0.));
#100521=DIRECTION('',(-0.190809912898503,0.,0.981627005099017));
#100522=DIRECTION('',(0.981627005099017,0.,0.190809912898503));
#100523=DIRECTION('',(-0.190809912898503,0.,0.981627005099017));
#100524=DIRECTION('',(0.981627005099017,0.,0.190809912898503));
#100525=DIRECTION('center_axis',(0.981627005099017,0.,0.190809912898503));
#100526=DIRECTION('ref_axis',(0.,-1.,0.));
#100527=DIRECTION('',(-0.190809912898503,0.,0.981627005099017));
#100528=DIRECTION('',(0.,-1.,0.));
#100529=DIRECTION('',(0.,-1.,0.));
#100530=DIRECTION('center_axis',(0.,-1.,0.));
#100531=DIRECTION('ref_axis',(0.,0.,-1.));
#100532=DIRECTION('',(-0.190809912898503,0.,0.981627005099017));
#100533=DIRECTION('',(-0.981627005099017,0.,-0.190809912898503));
#100534=DIRECTION('',(-0.981627005099017,0.,-0.190809912898503));
#100535=DIRECTION('center_axis',(-0.981627005099017,0.,-0.190809912898503));
#100536=DIRECTION('ref_axis',(-0.190809912898503,0.,0.981627005099017));
#100537=DIRECTION('',(0.,1.,0.));
#100538=DIRECTION('',(0.,1.,0.));
#100539=DIRECTION('center_axis',(0.,1.,0.));
#100540=DIRECTION('ref_axis',(1.,0.,0.));
#100541=DIRECTION('',(-0.190809912898503,0.,0.981627005099017));
#100542=DIRECTION('',(0.981627005099017,0.,0.190809912898503));
#100543=DIRECTION('',(-0.190809912898503,0.,0.981627005099017));
#100544=DIRECTION('',(0.981627005099017,0.,0.190809912898503));
#100545=DIRECTION('center_axis',(0.981627005099017,0.,0.190809912898503));
#100546=DIRECTION('ref_axis',(0.,-1.,0.));
#100547=DIRECTION('',(-0.190809912898503,0.,0.981627005099017));
#100548=DIRECTION('',(0.,-1.,0.));
#100549=DIRECTION('',(0.,-1.,0.));
#100550=DIRECTION('center_axis',(0.,-1.,0.));
#100551=DIRECTION('ref_axis',(0.,0.,-1.));
#100552=DIRECTION('',(-0.190809912898503,0.,0.981627005099017));
#100553=DIRECTION('',(-0.981627005099017,0.,-0.190809912898503));
#100554=DIRECTION('',(-0.981627005099017,0.,-0.190809912898503));
#100555=DIRECTION('center_axis',(-0.981627005099017,0.,-0.190809912898503));
#100556=DIRECTION('ref_axis',(-0.190809912898503,0.,0.981627005099017));
#100557=DIRECTION('',(0.,1.,0.));
#100558=DIRECTION('',(0.,1.,0.));
#100559=DIRECTION('center_axis',(0.,1.,0.));
#100560=DIRECTION('ref_axis',(1.,0.,0.));
#100561=DIRECTION('',(-0.190809912898503,0.,0.981627005099017));
#100562=DIRECTION('',(0.981627005099017,0.,0.190809912898503));
#100563=DIRECTION('',(-0.190809912898503,0.,0.981627005099017));
#100564=DIRECTION('',(0.981627005099017,0.,0.190809912898503));
#100565=DIRECTION('center_axis',(0.981627005099017,0.,0.190809912898503));
#100566=DIRECTION('ref_axis',(0.,-1.,0.));
#100567=DIRECTION('',(-0.190809912898503,0.,0.981627005099017));
#100568=DIRECTION('',(0.,-1.,0.));
#100569=DIRECTION('',(0.,-1.,0.));
#100570=DIRECTION('center_axis',(0.,-1.,0.));
#100571=DIRECTION('ref_axis',(0.,0.,-1.));
#100572=DIRECTION('',(-0.190809912898503,0.,0.981627005099017));
#100573=DIRECTION('',(-0.981627005099017,0.,-0.190809912898503));
#100574=DIRECTION('',(-0.981627005099017,0.,-0.190809912898503));
#100575=DIRECTION('center_axis',(-0.981627005099017,0.,-0.190809912898503));
#100576=DIRECTION('ref_axis',(-0.190809912898503,0.,0.981627005099017));
#100577=DIRECTION('',(0.,1.,0.));
#100578=DIRECTION('',(0.,1.,0.));
#100579=DIRECTION('center_axis',(0.,1.,0.));
#100580=DIRECTION('ref_axis',(1.,0.,0.));
#100581=DIRECTION('',(-0.190809912898503,0.,0.981627005099017));
#100582=DIRECTION('',(0.981627005099017,0.,0.190809912898503));
#100583=DIRECTION('',(-0.190809912898503,0.,0.981627005099017));
#100584=DIRECTION('',(0.981627005099017,0.,0.190809912898503));
#100585=DIRECTION('center_axis',(0.981627005099017,0.,0.190809912898503));
#100586=DIRECTION('ref_axis',(0.,-1.,0.));
#100587=DIRECTION('',(-0.190809912898503,0.,0.981627005099017));
#100588=DIRECTION('',(0.,-1.,0.));
#100589=DIRECTION('',(0.,-1.,0.));
#100590=DIRECTION('center_axis',(0.,-1.,0.));
#100591=DIRECTION('ref_axis',(0.,0.,-1.));
#100592=DIRECTION('',(-0.190809912898503,0.,0.981627005099017));
#100593=DIRECTION('',(-0.981627005099017,0.,-0.190809912898503));
#100594=DIRECTION('',(-0.981627005099017,0.,-0.190809912898503));
#100595=DIRECTION('center_axis',(-0.981627005099017,0.,-0.190809912898503));
#100596=DIRECTION('ref_axis',(-0.190809912898503,0.,0.981627005099017));
#100597=DIRECTION('',(0.,1.,0.));
#100598=DIRECTION('',(0.,1.,0.));
#100599=DIRECTION('center_axis',(0.,1.,0.));
#100600=DIRECTION('ref_axis',(1.,0.,0.));
#100601=DIRECTION('',(-0.190809912898503,0.,0.981627005099017));
#100602=DIRECTION('',(0.981627005099017,0.,0.190809912898503));
#100603=DIRECTION('',(-0.190809912898503,0.,0.981627005099017));
#100604=DIRECTION('',(0.981627005099017,0.,0.190809912898503));
#100605=DIRECTION('center_axis',(0.981627005099017,0.,0.190809912898503));
#100606=DIRECTION('ref_axis',(0.,-1.,0.));
#100607=DIRECTION('',(-0.190809912898503,0.,0.981627005099017));
#100608=DIRECTION('',(0.,-1.,0.));
#100609=DIRECTION('',(0.,-1.,0.));
#100610=DIRECTION('center_axis',(0.,-1.,0.));
#100611=DIRECTION('ref_axis',(0.,0.,-1.));
#100612=DIRECTION('',(-0.190809912898503,0.,0.981627005099017));
#100613=DIRECTION('',(-0.981627005099017,0.,-0.190809912898503));
#100614=DIRECTION('',(-0.981627005099017,0.,-0.190809912898503));
#100615=DIRECTION('center_axis',(-0.981627005099017,0.,-0.190809912898503));
#100616=DIRECTION('ref_axis',(-0.190809912898503,0.,0.981627005099017));
#100617=DIRECTION('',(0.,1.,0.));
#100618=DIRECTION('',(0.,1.,0.));
#100619=DIRECTION('center_axis',(0.,1.,0.));
#100620=DIRECTION('ref_axis',(1.,0.,0.));
#100621=DIRECTION('',(-0.190809912898503,0.,0.981627005099017));
#100622=DIRECTION('',(0.981627005099017,0.,0.190809912898503));
#100623=DIRECTION('',(-0.190809912898503,0.,0.981627005099017));
#100624=DIRECTION('',(0.981627005099017,0.,0.190809912898503));
#100625=DIRECTION('center_axis',(0.981627005099017,0.,0.190809912898503));
#100626=DIRECTION('ref_axis',(0.,-1.,0.));
#100627=DIRECTION('',(-0.190809912898503,0.,0.981627005099017));
#100628=DIRECTION('',(0.,-1.,0.));
#100629=DIRECTION('',(0.,-1.,0.));
#100630=DIRECTION('center_axis',(0.,-1.,0.));
#100631=DIRECTION('ref_axis',(0.,0.,-1.));
#100632=DIRECTION('',(-0.190809912898503,0.,0.981627005099017));
#100633=DIRECTION('',(-0.981627005099017,0.,-0.190809912898503));
#100634=DIRECTION('',(-0.981627005099017,0.,-0.190809912898503));
#100635=DIRECTION('center_axis',(-0.981627005099017,0.,-0.190809912898503));
#100636=DIRECTION('ref_axis',(-0.190809912898503,0.,0.981627005099017));
#100637=DIRECTION('',(0.,1.,0.));
#100638=DIRECTION('',(0.,1.,0.));
#100639=DIRECTION('center_axis',(0.,1.,0.));
#100640=DIRECTION('ref_axis',(1.,0.,0.));
#100641=DIRECTION('',(-0.190809912898503,0.,0.981627005099017));
#100642=DIRECTION('',(0.981627005099017,0.,0.190809912898503));
#100643=DIRECTION('',(-0.190809912898503,0.,0.981627005099017));
#100644=DIRECTION('',(0.981627005099017,0.,0.190809912898503));
#100645=DIRECTION('center_axis',(0.981627005099017,0.,0.190809912898503));
#100646=DIRECTION('ref_axis',(0.,-1.,0.));
#100647=DIRECTION('',(-0.190809912898503,0.,0.981627005099017));
#100648=DIRECTION('',(0.,-1.,0.));
#100649=DIRECTION('',(0.,-1.,0.));
#100650=DIRECTION('center_axis',(0.,-1.,0.));
#100651=DIRECTION('ref_axis',(0.,0.,-1.));
#100652=DIRECTION('',(-0.190809912898503,0.,0.981627005099017));
#100653=DIRECTION('',(-0.981627005099017,0.,-0.190809912898503));
#100654=DIRECTION('',(-0.981627005099017,0.,-0.190809912898503));
#100655=DIRECTION('center_axis',(-0.981627005099017,0.,-0.190809912898503));
#100656=DIRECTION('ref_axis',(-0.190809912898503,0.,0.981627005099017));
#100657=DIRECTION('',(0.,1.,0.));
#100658=DIRECTION('',(0.,1.,0.));
#100659=DIRECTION('center_axis',(0.,1.,0.));
#100660=DIRECTION('ref_axis',(1.,0.,0.));
#100661=DIRECTION('',(-0.190809912898503,0.,0.981627005099017));
#100662=DIRECTION('',(0.981627005099017,0.,0.190809912898503));
#100663=DIRECTION('',(-0.190809912898503,0.,0.981627005099017));
#100664=DIRECTION('',(0.981627005099017,0.,0.190809912898503));
#100665=DIRECTION('center_axis',(0.981627005099017,0.,0.190809912898503));
#100666=DIRECTION('ref_axis',(0.,-1.,0.));
#100667=DIRECTION('',(-0.190809912898503,0.,0.981627005099017));
#100668=DIRECTION('',(0.,-1.,0.));
#100669=DIRECTION('',(0.,-1.,0.));
#100670=DIRECTION('center_axis',(0.,-1.,0.));
#100671=DIRECTION('ref_axis',(0.,0.,-1.));
#100672=DIRECTION('',(-0.190809912898503,0.,0.981627005099017));
#100673=DIRECTION('',(-0.981627005099017,0.,-0.190809912898503));
#100674=DIRECTION('',(-0.981627005099017,0.,-0.190809912898503));
#100675=DIRECTION('center_axis',(-0.981627005099017,0.,-0.190809912898503));
#100676=DIRECTION('ref_axis',(-0.190809912898503,0.,0.981627005099017));
#100677=DIRECTION('',(0.,1.,0.));
#100678=DIRECTION('',(0.,1.,0.));
#100679=DIRECTION('center_axis',(0.,1.,0.));
#100680=DIRECTION('ref_axis',(1.,0.,0.));
#100681=DIRECTION('',(-0.190809912898503,0.,0.981627005099017));
#100682=DIRECTION('',(0.981627005099017,0.,0.190809912898503));
#100683=DIRECTION('',(-0.190809912898503,0.,0.981627005099017));
#100684=DIRECTION('',(0.981627005099017,0.,0.190809912898503));
#100685=DIRECTION('center_axis',(0.981627005099017,0.,0.190809912898503));
#100686=DIRECTION('ref_axis',(0.,-1.,0.));
#100687=DIRECTION('',(-0.190809912898503,0.,0.981627005099017));
#100688=DIRECTION('',(0.,-1.,0.));
#100689=DIRECTION('',(0.,-1.,0.));
#100690=DIRECTION('center_axis',(0.,-1.,0.));
#100691=DIRECTION('ref_axis',(0.,0.,-1.));
#100692=DIRECTION('',(-0.190809912898503,0.,0.981627005099017));
#100693=DIRECTION('',(-0.981627005099017,0.,-0.190809912898503));
#100694=DIRECTION('',(-0.981627005099017,0.,-0.190809912898503));
#100695=DIRECTION('center_axis',(-0.981627005099017,0.,-0.190809912898503));
#100696=DIRECTION('ref_axis',(-0.190809912898503,0.,0.981627005099017));
#100697=DIRECTION('',(0.,1.,0.));
#100698=DIRECTION('',(0.,1.,0.));
#100699=DIRECTION('center_axis',(0.,1.,0.));
#100700=DIRECTION('ref_axis',(1.,0.,0.));
#100701=DIRECTION('',(-0.190809912898503,0.,0.981627005099017));
#100702=DIRECTION('',(0.981627005099017,0.,0.190809912898503));
#100703=DIRECTION('',(-0.190809912898503,0.,0.981627005099017));
#100704=DIRECTION('',(0.981627005099017,0.,0.190809912898503));
#100705=DIRECTION('center_axis',(0.981627005099017,0.,0.190809912898503));
#100706=DIRECTION('ref_axis',(0.,-1.,0.));
#100707=DIRECTION('',(-0.190809912898503,0.,0.981627005099017));
#100708=DIRECTION('',(0.,-1.,0.));
#100709=DIRECTION('',(0.,-1.,0.));
#100710=DIRECTION('center_axis',(0.,-1.,0.));
#100711=DIRECTION('ref_axis',(0.,0.,-1.));
#100712=DIRECTION('',(-0.190809912898503,0.,0.981627005099017));
#100713=DIRECTION('',(-0.981627005099017,0.,-0.190809912898503));
#100714=DIRECTION('',(-0.981627005099017,0.,-0.190809912898503));
#100715=DIRECTION('center_axis',(-0.981627005099017,0.,-0.190809912898503));
#100716=DIRECTION('ref_axis',(-0.190809912898503,0.,0.981627005099017));
#100717=DIRECTION('',(0.,1.,0.));
#100718=DIRECTION('',(0.,1.,0.));
#100719=DIRECTION('center_axis',(0.,1.,0.));
#100720=DIRECTION('ref_axis',(1.,0.,0.));
#100721=DIRECTION('',(-0.190809912898503,0.,0.981627005099017));
#100722=DIRECTION('',(0.981627005099017,0.,0.190809912898503));
#100723=DIRECTION('',(-0.190809912898503,0.,0.981627005099017));
#100724=DIRECTION('',(0.981627005099017,0.,0.190809912898503));
#100725=DIRECTION('center_axis',(0.981627005099017,0.,0.190809912898503));
#100726=DIRECTION('ref_axis',(0.,-1.,0.));
#100727=DIRECTION('',(-0.190809912898503,0.,0.981627005099017));
#100728=DIRECTION('',(0.,-1.,0.));
#100729=DIRECTION('',(0.,-1.,0.));
#100730=DIRECTION('center_axis',(0.,-1.,0.));
#100731=DIRECTION('ref_axis',(0.,0.,-1.));
#100732=DIRECTION('',(-0.190809912898503,0.,0.981627005099017));
#100733=DIRECTION('',(-0.981627005099017,0.,-0.190809912898503));
#100734=DIRECTION('',(-0.981627005099017,0.,-0.190809912898503));
#100735=DIRECTION('center_axis',(-0.981627005099017,0.,-0.190809912898503));
#100736=DIRECTION('ref_axis',(-0.190809912898503,0.,0.981627005099017));
#100737=DIRECTION('',(0.,1.,0.));
#100738=DIRECTION('',(0.,1.,0.));
#100739=DIRECTION('center_axis',(0.,1.,0.));
#100740=DIRECTION('ref_axis',(1.,0.,0.));
#100741=DIRECTION('',(-0.190809912898503,0.,0.981627005099017));
#100742=DIRECTION('',(0.981627005099017,0.,0.190809912898503));
#100743=DIRECTION('',(-0.190809912898503,0.,0.981627005099017));
#100744=DIRECTION('',(0.981627005099017,0.,0.190809912898503));
#100745=DIRECTION('center_axis',(0.981627005099017,0.,0.190809912898503));
#100746=DIRECTION('ref_axis',(0.,-1.,0.));
#100747=DIRECTION('',(-0.190809912898503,0.,0.981627005099017));
#100748=DIRECTION('',(0.,-1.,0.));
#100749=DIRECTION('',(0.,-1.,0.));
#100750=DIRECTION('center_axis',(0.,-1.,0.));
#100751=DIRECTION('ref_axis',(0.,0.,-1.));
#100752=DIRECTION('',(-0.190809912898503,0.,0.981627005099017));
#100753=DIRECTION('',(-0.981627005099017,0.,-0.190809912898503));
#100754=DIRECTION('',(-0.981627005099017,0.,-0.190809912898503));
#100755=DIRECTION('center_axis',(-0.981627005099017,0.,-0.190809912898503));
#100756=DIRECTION('ref_axis',(-0.190809912898503,0.,0.981627005099017));
#100757=DIRECTION('',(0.,1.,0.));
#100758=DIRECTION('',(0.,1.,0.));
#100759=DIRECTION('center_axis',(0.,1.,0.));
#100760=DIRECTION('ref_axis',(1.,0.,0.));
#100761=DIRECTION('',(-0.190809912898503,0.,0.981627005099017));
#100762=DIRECTION('',(0.981627005099017,0.,0.190809912898503));
#100763=DIRECTION('',(-0.190809912898503,0.,0.981627005099017));
#100764=DIRECTION('',(0.981627005099017,0.,0.190809912898503));
#100765=DIRECTION('center_axis',(0.981627005099017,0.,0.190809912898503));
#100766=DIRECTION('ref_axis',(0.,-1.,0.));
#100767=DIRECTION('',(-0.190809912898503,0.,0.981627005099017));
#100768=DIRECTION('',(0.,-1.,0.));
#100769=DIRECTION('',(0.,-1.,0.));
#100770=DIRECTION('center_axis',(0.,-1.,0.));
#100771=DIRECTION('ref_axis',(0.,0.,-1.));
#100772=DIRECTION('',(-0.190809912898503,0.,0.981627005099017));
#100773=DIRECTION('',(-0.981627005099017,0.,-0.190809912898503));
#100774=DIRECTION('',(-0.981627005099017,0.,-0.190809912898503));
#100775=DIRECTION('center_axis',(-0.981627005099017,0.,-0.190809912898503));
#100776=DIRECTION('ref_axis',(-0.190809912898503,0.,0.981627005099017));
#100777=DIRECTION('',(0.,1.,0.));
#100778=DIRECTION('',(0.,1.,0.));
#100779=DIRECTION('center_axis',(0.,1.,0.));
#100780=DIRECTION('ref_axis',(1.,0.,0.));
#100781=DIRECTION('',(-0.190809912898503,0.,0.981627005099017));
#100782=DIRECTION('',(0.981627005099017,0.,0.190809912898503));
#100783=DIRECTION('',(-0.190809912898503,0.,0.981627005099017));
#100784=DIRECTION('',(0.981627005099017,0.,0.190809912898503));
#100785=DIRECTION('center_axis',(0.981627005099017,0.,0.190809912898503));
#100786=DIRECTION('ref_axis',(0.,-1.,0.));
#100787=DIRECTION('',(-0.190809912898503,0.,0.981627005099017));
#100788=DIRECTION('',(0.,-1.,0.));
#100789=DIRECTION('',(0.,-1.,0.));
#100790=DIRECTION('center_axis',(0.,-1.,0.));
#100791=DIRECTION('ref_axis',(0.,0.,-1.));
#100792=DIRECTION('',(-0.190809912898503,0.,0.981627005099017));
#100793=DIRECTION('',(-0.981627005099017,0.,-0.190809912898503));
#100794=DIRECTION('',(-0.981627005099017,0.,-0.190809912898503));
#100795=DIRECTION('center_axis',(-0.981627005099017,0.,-0.190809912898503));
#100796=DIRECTION('ref_axis',(-0.190809912898503,0.,0.981627005099017));
#100797=DIRECTION('',(0.,1.,0.));
#100798=DIRECTION('',(0.,1.,0.));
#100799=DIRECTION('center_axis',(0.,1.,0.));
#100800=DIRECTION('ref_axis',(1.,0.,0.));
#100801=DIRECTION('',(-0.190809912898503,0.,0.981627005099017));
#100802=DIRECTION('',(0.981627005099017,0.,0.190809912898503));
#100803=DIRECTION('',(-0.190809912898503,0.,0.981627005099017));
#100804=DIRECTION('',(0.981627005099017,0.,0.190809912898503));
#100805=DIRECTION('center_axis',(0.981627005099017,0.,0.190809912898503));
#100806=DIRECTION('ref_axis',(0.,-1.,0.));
#100807=DIRECTION('',(-0.190809912898503,0.,0.981627005099017));
#100808=DIRECTION('',(0.,-1.,0.));
#100809=DIRECTION('',(0.,-1.,0.));
#100810=DIRECTION('center_axis',(0.,-1.,0.));
#100811=DIRECTION('ref_axis',(0.,0.,-1.));
#100812=DIRECTION('',(-0.190809912898503,0.,0.981627005099017));
#100813=DIRECTION('',(-0.981627005099017,0.,-0.190809912898503));
#100814=DIRECTION('',(-0.981627005099017,0.,-0.190809912898503));
#100815=DIRECTION('center_axis',(-0.981627005099017,0.,-0.190809912898503));
#100816=DIRECTION('ref_axis',(-0.190809912898503,0.,0.981627005099017));
#100817=DIRECTION('',(0.,1.,0.));
#100818=DIRECTION('',(0.,1.,0.));
#100819=DIRECTION('center_axis',(0.,1.,0.));
#100820=DIRECTION('ref_axis',(1.,0.,0.));
#100821=DIRECTION('',(-0.190809912898503,0.,0.981627005099017));
#100822=DIRECTION('',(0.981627005099017,0.,0.190809912898503));
#100823=DIRECTION('',(-0.190809912898503,0.,0.981627005099017));
#100824=DIRECTION('',(0.981627005099017,0.,0.190809912898503));
#100825=DIRECTION('center_axis',(0.981627005099017,0.,0.190809912898503));
#100826=DIRECTION('ref_axis',(0.,-1.,0.));
#100827=DIRECTION('',(-0.190809912898503,0.,0.981627005099017));
#100828=DIRECTION('',(0.,-1.,0.));
#100829=DIRECTION('',(0.,-1.,0.));
#100830=DIRECTION('center_axis',(0.,-1.,0.));
#100831=DIRECTION('ref_axis',(0.,0.,-1.));
#100832=DIRECTION('',(-0.190809912898503,0.,0.981627005099017));
#100833=DIRECTION('',(-0.981627005099017,0.,-0.190809912898503));
#100834=DIRECTION('',(-0.981627005099017,0.,-0.190809912898503));
#100835=DIRECTION('center_axis',(-0.981627005099017,0.,-0.190809912898503));
#100836=DIRECTION('ref_axis',(-0.190809912898503,0.,0.981627005099017));
#100837=DIRECTION('',(0.,1.,0.));
#100838=DIRECTION('',(0.,1.,0.));
#100839=DIRECTION('center_axis',(0.,1.,0.));
#100840=DIRECTION('ref_axis',(1.,0.,0.));
#100841=DIRECTION('',(-0.190809912898503,0.,0.981627005099017));
#100842=DIRECTION('',(0.981627005099017,0.,0.190809912898503));
#100843=DIRECTION('',(-0.190809912898503,0.,0.981627005099017));
#100844=DIRECTION('',(0.981627005099017,0.,0.190809912898503));
#100845=DIRECTION('center_axis',(0.981627005099017,0.,0.190809912898503));
#100846=DIRECTION('ref_axis',(0.,-1.,0.));
#100847=DIRECTION('',(-0.190809912898503,0.,0.981627005099017));
#100848=DIRECTION('',(0.,-1.,0.));
#100849=DIRECTION('',(0.,-1.,0.));
#100850=DIRECTION('center_axis',(0.,-1.,0.));
#100851=DIRECTION('ref_axis',(0.,0.,-1.));
#100852=DIRECTION('',(-0.190809912898503,0.,0.981627005099017));
#100853=DIRECTION('',(-0.981627005099017,0.,-0.190809912898503));
#100854=DIRECTION('',(-0.981627005099017,0.,-0.190809912898503));
#100855=DIRECTION('center_axis',(-0.981627005099017,0.,-0.190809912898503));
#100856=DIRECTION('ref_axis',(-0.190809912898503,0.,0.981627005099017));
#100857=DIRECTION('',(0.,1.,0.));
#100858=DIRECTION('',(0.,1.,0.));
#100859=DIRECTION('center_axis',(0.,1.,0.));
#100860=DIRECTION('ref_axis',(1.,0.,0.));
#100861=DIRECTION('',(-0.190809912898503,0.,0.981627005099017));
#100862=DIRECTION('',(0.981627005099017,0.,0.190809912898503));
#100863=DIRECTION('',(-0.190809912898503,0.,0.981627005099017));
#100864=DIRECTION('',(0.981627005099017,0.,0.190809912898503));
#100865=DIRECTION('center_axis',(0.981627005099017,0.,0.190809912898503));
#100866=DIRECTION('ref_axis',(0.,-1.,0.));
#100867=DIRECTION('',(-0.190809912898503,0.,0.981627005099017));
#100868=DIRECTION('',(0.,-1.,0.));
#100869=DIRECTION('',(0.,-1.,0.));
#100870=DIRECTION('center_axis',(0.,-1.,0.));
#100871=DIRECTION('ref_axis',(0.,0.,-1.));
#100872=DIRECTION('',(-0.190809912898503,0.,0.981627005099017));
#100873=DIRECTION('',(-0.981627005099017,0.,-0.190809912898503));
#100874=DIRECTION('',(-0.981627005099017,0.,-0.190809912898503));
#100875=DIRECTION('center_axis',(-0.981627005099017,0.,-0.190809912898503));
#100876=DIRECTION('ref_axis',(-0.190809912898503,0.,0.981627005099017));
#100877=DIRECTION('',(0.,1.,0.));
#100878=DIRECTION('',(0.,1.,0.));
#100879=DIRECTION('center_axis',(0.,1.,0.));
#100880=DIRECTION('ref_axis',(1.,0.,0.));
#100881=DIRECTION('',(-0.190809912898503,0.,0.981627005099017));
#100882=DIRECTION('',(0.981627005099017,0.,0.190809912898503));
#100883=DIRECTION('',(-0.190809912898503,0.,0.981627005099017));
#100884=DIRECTION('',(0.981627005099017,0.,0.190809912898503));
#100885=DIRECTION('center_axis',(0.981627005099017,0.,0.190809912898503));
#100886=DIRECTION('ref_axis',(0.,-1.,0.));
#100887=DIRECTION('',(-0.190809912898503,0.,0.981627005099017));
#100888=DIRECTION('',(0.,-1.,0.));
#100889=DIRECTION('',(0.,-1.,0.));
#100890=DIRECTION('center_axis',(0.,-1.,0.));
#100891=DIRECTION('ref_axis',(0.,0.,-1.));
#100892=DIRECTION('',(-0.190809912898503,0.,0.981627005099017));
#100893=DIRECTION('',(-0.981627005099017,0.,-0.190809912898503));
#100894=DIRECTION('',(-0.981627005099017,0.,-0.190809912898503));
#100895=DIRECTION('center_axis',(-0.981627005099017,0.,-0.190809912898503));
#100896=DIRECTION('ref_axis',(-0.190809912898503,0.,0.981627005099017));
#100897=DIRECTION('',(0.,1.,0.));
#100898=DIRECTION('',(0.,1.,0.));
#100899=DIRECTION('center_axis',(0.,1.,0.));
#100900=DIRECTION('ref_axis',(1.,0.,0.));
#100901=DIRECTION('',(-0.190809912898503,0.,0.981627005099017));
#100902=DIRECTION('',(0.981627005099017,0.,0.190809912898503));
#100903=DIRECTION('',(-0.190809912898503,0.,0.981627005099017));
#100904=DIRECTION('',(0.981627005099017,0.,0.190809912898503));
#100905=DIRECTION('center_axis',(0.981627005099017,0.,0.190809912898503));
#100906=DIRECTION('ref_axis',(0.,-1.,0.));
#100907=DIRECTION('',(-0.190809912898503,0.,0.981627005099017));
#100908=DIRECTION('',(0.,-1.,0.));
#100909=DIRECTION('',(0.,-1.,0.));
#100910=DIRECTION('center_axis',(0.,-1.,0.));
#100911=DIRECTION('ref_axis',(0.,0.,-1.));
#100912=DIRECTION('',(-0.190809912898503,0.,0.981627005099017));
#100913=DIRECTION('',(-0.981627005099017,0.,-0.190809912898503));
#100914=DIRECTION('',(-0.981627005099017,0.,-0.190809912898503));
#100915=DIRECTION('center_axis',(-0.981627005099017,0.,-0.190809912898503));
#100916=DIRECTION('ref_axis',(-0.190809912898503,0.,0.981627005099017));
#100917=DIRECTION('',(0.,1.,0.));
#100918=DIRECTION('',(0.,1.,0.));
#100919=DIRECTION('center_axis',(0.,1.,0.));
#100920=DIRECTION('ref_axis',(1.,0.,0.));
#100921=DIRECTION('',(-0.190809912898503,0.,0.981627005099017));
#100922=DIRECTION('',(0.981627005099017,0.,0.190809912898503));
#100923=DIRECTION('',(-0.190809912898503,0.,0.981627005099017));
#100924=DIRECTION('',(0.981627005099017,0.,0.190809912898503));
#100925=DIRECTION('center_axis',(0.981627005099017,0.,0.190809912898503));
#100926=DIRECTION('ref_axis',(0.,-1.,0.));
#100927=DIRECTION('',(-0.190809912898503,0.,0.981627005099017));
#100928=DIRECTION('',(0.,-1.,0.));
#100929=DIRECTION('',(0.,-1.,0.));
#100930=DIRECTION('center_axis',(0.,-1.,0.));
#100931=DIRECTION('ref_axis',(0.,0.,-1.));
#100932=DIRECTION('',(-0.190809912898503,0.,0.981627005099017));
#100933=DIRECTION('',(-0.981627005099017,0.,-0.190809912898503));
#100934=DIRECTION('',(-0.981627005099017,0.,-0.190809912898503));
#100935=DIRECTION('center_axis',(-0.981627005099017,0.,-0.190809912898503));
#100936=DIRECTION('ref_axis',(-0.190809912898503,0.,0.981627005099017));
#100937=DIRECTION('',(0.,1.,0.));
#100938=DIRECTION('',(0.,1.,0.));
#100939=DIRECTION('center_axis',(0.,1.,0.));
#100940=DIRECTION('ref_axis',(1.,0.,0.));
#100941=DIRECTION('',(-0.190809912898503,0.,0.981627005099017));
#100942=DIRECTION('',(0.981627005099017,0.,0.190809912898503));
#100943=DIRECTION('',(-0.190809912898503,0.,0.981627005099017));
#100944=DIRECTION('',(0.981627005099017,0.,0.190809912898503));
#100945=DIRECTION('center_axis',(0.981627005099017,0.,0.190809912898503));
#100946=DIRECTION('ref_axis',(0.,-1.,0.));
#100947=DIRECTION('',(-0.190809912898503,0.,0.981627005099017));
#100948=DIRECTION('',(0.,-1.,0.));
#100949=DIRECTION('',(0.,-1.,0.));
#100950=DIRECTION('center_axis',(0.,-1.,0.));
#100951=DIRECTION('ref_axis',(0.,0.,-1.));
#100952=DIRECTION('',(-0.190809912898503,0.,0.981627005099017));
#100953=DIRECTION('',(-0.981627005099017,0.,-0.190809912898503));
#100954=DIRECTION('',(-0.981627005099017,0.,-0.190809912898503));
#100955=DIRECTION('center_axis',(-0.981627005099017,0.,-0.190809912898503));
#100956=DIRECTION('ref_axis',(-0.190809912898503,0.,0.981627005099017));
#100957=DIRECTION('',(0.,1.,0.));
#100958=DIRECTION('',(0.,1.,0.));
#100959=DIRECTION('center_axis',(0.,1.,0.));
#100960=DIRECTION('ref_axis',(1.,0.,0.));
#100961=DIRECTION('',(-0.190809912898503,0.,0.981627005099017));
#100962=DIRECTION('',(0.981627005099017,0.,0.190809912898503));
#100963=DIRECTION('',(-0.190809912898503,0.,0.981627005099017));
#100964=DIRECTION('',(0.981627005099017,0.,0.190809912898503));
#100965=DIRECTION('center_axis',(0.981627005099017,0.,0.190809912898503));
#100966=DIRECTION('ref_axis',(0.,-1.,0.));
#100967=DIRECTION('',(-0.190809912898503,0.,0.981627005099017));
#100968=DIRECTION('',(0.,-1.,0.));
#100969=DIRECTION('',(0.,-1.,0.));
#100970=DIRECTION('center_axis',(0.,-1.,0.));
#100971=DIRECTION('ref_axis',(0.,0.,-1.));
#100972=DIRECTION('',(-0.190809912898503,0.,0.981627005099017));
#100973=DIRECTION('',(-0.981627005099017,0.,-0.190809912898503));
#100974=DIRECTION('',(-0.981627005099017,0.,-0.190809912898503));
#100975=DIRECTION('center_axis',(-0.981627005099017,0.,-0.190809912898503));
#100976=DIRECTION('ref_axis',(-0.190809912898503,0.,0.981627005099017));
#100977=DIRECTION('',(0.,1.,0.));
#100978=DIRECTION('',(0.,1.,0.));
#100979=DIRECTION('center_axis',(0.,1.,0.));
#100980=DIRECTION('ref_axis',(1.,0.,0.));
#100981=DIRECTION('',(-0.190809912898503,0.,0.981627005099017));
#100982=DIRECTION('',(0.981627005099017,0.,0.190809912898503));
#100983=DIRECTION('',(-0.190809912898503,0.,0.981627005099017));
#100984=DIRECTION('',(0.981627005099017,0.,0.190809912898503));
#100985=DIRECTION('center_axis',(0.981627005099017,0.,0.190809912898503));
#100986=DIRECTION('ref_axis',(0.,-1.,0.));
#100987=DIRECTION('',(-0.190809912898503,0.,0.981627005099017));
#100988=DIRECTION('',(0.,-1.,0.));
#100989=DIRECTION('',(0.,-1.,0.));
#100990=DIRECTION('center_axis',(0.,-1.,0.));
#100991=DIRECTION('ref_axis',(0.,0.,-1.));
#100992=DIRECTION('',(-0.190809912898503,0.,0.981627005099017));
#100993=DIRECTION('',(-0.981627005099017,0.,-0.190809912898503));
#100994=DIRECTION('',(-0.981627005099017,0.,-0.190809912898503));
#100995=DIRECTION('center_axis',(-0.981627005099017,0.,-0.190809912898503));
#100996=DIRECTION('ref_axis',(-0.190809912898503,0.,0.981627005099017));
#100997=DIRECTION('',(0.,1.,0.));
#100998=DIRECTION('',(0.,1.,0.));
#100999=DIRECTION('center_axis',(0.,1.,0.));
#101000=DIRECTION('ref_axis',(1.,0.,0.));
#101001=DIRECTION('',(-0.190809912898503,0.,0.981627005099017));
#101002=DIRECTION('',(0.981627005099017,0.,0.190809912898503));
#101003=DIRECTION('',(-0.190809912898503,0.,0.981627005099017));
#101004=DIRECTION('',(0.981627005099017,0.,0.190809912898503));
#101005=DIRECTION('center_axis',(0.981627005099017,0.,0.190809912898503));
#101006=DIRECTION('ref_axis',(0.,-1.,0.));
#101007=DIRECTION('',(-0.190809912898503,0.,0.981627005099017));
#101008=DIRECTION('',(0.,-1.,0.));
#101009=DIRECTION('',(0.,-1.,0.));
#101010=DIRECTION('center_axis',(0.,-1.,0.));
#101011=DIRECTION('ref_axis',(0.,0.,-1.));
#101012=DIRECTION('',(-0.190809912898503,0.,0.981627005099017));
#101013=DIRECTION('',(-0.981627005099017,0.,-0.190809912898503));
#101014=DIRECTION('',(-0.981627005099017,0.,-0.190809912898503));
#101015=DIRECTION('center_axis',(-0.981627005099017,0.,-0.190809912898503));
#101016=DIRECTION('ref_axis',(-0.190809912898503,0.,0.981627005099017));
#101017=DIRECTION('',(0.,1.,0.));
#101018=DIRECTION('',(0.,1.,0.));
#101019=DIRECTION('center_axis',(0.,1.,0.));
#101020=DIRECTION('ref_axis',(1.,0.,0.));
#101021=DIRECTION('',(-0.190809912898503,0.,0.981627005099017));
#101022=DIRECTION('',(0.981627005099017,0.,0.190809912898503));
#101023=DIRECTION('',(-0.190809912898503,0.,0.981627005099017));
#101024=DIRECTION('',(0.981627005099017,0.,0.190809912898503));
#101025=DIRECTION('center_axis',(0.981627005099017,0.,0.190809912898503));
#101026=DIRECTION('ref_axis',(0.,-1.,0.));
#101027=DIRECTION('',(-0.190809912898503,0.,0.981627005099017));
#101028=DIRECTION('',(0.,-1.,0.));
#101029=DIRECTION('',(0.,-1.,0.));
#101030=DIRECTION('center_axis',(0.,-1.,0.));
#101031=DIRECTION('ref_axis',(0.,0.,-1.));
#101032=DIRECTION('',(-0.190809912898503,0.,0.981627005099017));
#101033=DIRECTION('',(-0.981627005099017,0.,-0.190809912898503));
#101034=DIRECTION('',(-0.981627005099017,0.,-0.190809912898503));
#101035=DIRECTION('center_axis',(-0.981627005099017,0.,-0.190809912898503));
#101036=DIRECTION('ref_axis',(-0.190809912898503,0.,0.981627005099017));
#101037=DIRECTION('',(0.,1.,0.));
#101038=DIRECTION('',(0.,1.,0.));
#101039=DIRECTION('center_axis',(0.,1.,0.));
#101040=DIRECTION('ref_axis',(1.,0.,0.));
#101041=DIRECTION('',(-0.190809912898503,0.,0.981627005099017));
#101042=DIRECTION('',(0.981627005099017,0.,0.190809912898503));
#101043=DIRECTION('',(-0.190809912898503,0.,0.981627005099017));
#101044=DIRECTION('',(0.981627005099017,0.,0.190809912898503));
#101045=DIRECTION('center_axis',(0.981627005099017,0.,0.190809912898503));
#101046=DIRECTION('ref_axis',(0.,-1.,0.));
#101047=DIRECTION('',(-0.190809912898503,0.,0.981627005099017));
#101048=DIRECTION('',(0.,-1.,0.));
#101049=DIRECTION('',(0.,-1.,0.));
#101050=DIRECTION('center_axis',(0.,-1.,0.));
#101051=DIRECTION('ref_axis',(0.,0.,-1.));
#101052=DIRECTION('',(-0.190809912898503,0.,0.981627005099017));
#101053=DIRECTION('',(-0.981627005099017,0.,-0.190809912898503));
#101054=DIRECTION('',(-0.981627005099017,0.,-0.190809912898503));
#101055=DIRECTION('center_axis',(-0.981627005099017,0.,-0.190809912898503));
#101056=DIRECTION('ref_axis',(-0.190809912898503,0.,0.981627005099017));
#101057=DIRECTION('',(0.,1.,0.));
#101058=DIRECTION('',(0.,1.,0.));
#101059=DIRECTION('center_axis',(0.,1.,0.));
#101060=DIRECTION('ref_axis',(1.,0.,0.));
#101061=DIRECTION('',(-0.190809912898503,0.,0.981627005099017));
#101062=DIRECTION('',(0.981627005099017,0.,0.190809912898503));
#101063=DIRECTION('',(-0.190809912898503,0.,0.981627005099017));
#101064=DIRECTION('',(0.981627005099017,0.,0.190809912898503));
#101065=DIRECTION('center_axis',(0.981627005099017,0.,0.190809912898503));
#101066=DIRECTION('ref_axis',(0.,-1.,0.));
#101067=DIRECTION('',(-0.190809912898503,0.,0.981627005099017));
#101068=DIRECTION('',(0.,-1.,0.));
#101069=DIRECTION('',(0.,-1.,0.));
#101070=DIRECTION('center_axis',(0.,-1.,0.));
#101071=DIRECTION('ref_axis',(0.,0.,-1.));
#101072=DIRECTION('',(-0.190809912898503,0.,0.981627005099017));
#101073=DIRECTION('',(-0.981627005099017,0.,-0.190809912898503));
#101074=DIRECTION('',(-0.981627005099017,0.,-0.190809912898503));
#101075=DIRECTION('center_axis',(-0.981627005099017,0.,-0.190809912898503));
#101076=DIRECTION('ref_axis',(-0.190809912898503,0.,0.981627005099017));
#101077=DIRECTION('',(0.,1.,0.));
#101078=DIRECTION('',(0.,1.,0.));
#101079=DIRECTION('center_axis',(0.,1.,0.));
#101080=DIRECTION('ref_axis',(1.,0.,0.));
#101081=DIRECTION('',(-0.190809912898503,0.,0.981627005099017));
#101082=DIRECTION('',(0.981627005099017,0.,0.190809912898503));
#101083=DIRECTION('',(-0.190809912898503,0.,0.981627005099017));
#101084=DIRECTION('',(0.981627005099017,0.,0.190809912898503));
#101085=DIRECTION('center_axis',(0.981627005099017,0.,0.190809912898503));
#101086=DIRECTION('ref_axis',(0.,-1.,0.));
#101087=DIRECTION('',(-0.190809912898503,0.,0.981627005099017));
#101088=DIRECTION('',(0.,-1.,0.));
#101089=DIRECTION('',(0.,-1.,0.));
#101090=DIRECTION('center_axis',(0.,-1.,0.));
#101091=DIRECTION('ref_axis',(0.,0.,-1.));
#101092=DIRECTION('',(-0.190809912898503,0.,0.981627005099017));
#101093=DIRECTION('',(-0.981627005099017,0.,-0.190809912898503));
#101094=DIRECTION('',(-0.981627005099017,0.,-0.190809912898503));
#101095=DIRECTION('center_axis',(-0.981627005099017,0.,-0.190809912898503));
#101096=DIRECTION('ref_axis',(-0.190809912898503,0.,0.981627005099017));
#101097=DIRECTION('',(0.,1.,0.));
#101098=DIRECTION('',(0.,1.,0.));
#101099=DIRECTION('center_axis',(0.,1.,0.));
#101100=DIRECTION('ref_axis',(1.,0.,0.));
#101101=DIRECTION('',(-0.190809912898503,0.,0.981627005099017));
#101102=DIRECTION('',(0.981627005099017,0.,0.190809912898503));
#101103=DIRECTION('',(-0.190809912898503,0.,0.981627005099017));
#101104=DIRECTION('',(0.981627005099017,0.,0.190809912898503));
#101105=DIRECTION('center_axis',(0.981627005099017,0.,0.190809912898503));
#101106=DIRECTION('ref_axis',(0.,-1.,0.));
#101107=DIRECTION('',(-0.190809912898503,0.,0.981627005099017));
#101108=DIRECTION('',(0.,-1.,0.));
#101109=DIRECTION('',(0.,-1.,0.));
#101110=DIRECTION('center_axis',(0.,-1.,0.));
#101111=DIRECTION('ref_axis',(0.,0.,-1.));
#101112=DIRECTION('',(-0.190809912898503,0.,0.981627005099017));
#101113=DIRECTION('',(-0.981627005099017,0.,-0.190809912898503));
#101114=DIRECTION('',(-0.981627005099017,0.,-0.190809912898503));
#101115=DIRECTION('center_axis',(-0.981627005099017,0.,-0.190809912898503));
#101116=DIRECTION('ref_axis',(-0.190809912898503,0.,0.981627005099017));
#101117=DIRECTION('',(0.,1.,0.));
#101118=DIRECTION('',(0.,1.,0.));
#101119=DIRECTION('center_axis',(0.,1.,0.));
#101120=DIRECTION('ref_axis',(1.,0.,0.));
#101121=DIRECTION('',(-0.190809912898503,0.,0.981627005099017));
#101122=DIRECTION('',(0.981627005099017,0.,0.190809912898503));
#101123=DIRECTION('',(-0.190809912898503,0.,0.981627005099017));
#101124=DIRECTION('',(0.981627005099017,0.,0.190809912898503));
#101125=DIRECTION('center_axis',(0.981627005099017,0.,0.190809912898503));
#101126=DIRECTION('ref_axis',(0.,-1.,0.));
#101127=DIRECTION('',(-0.190809912898503,0.,0.981627005099017));
#101128=DIRECTION('',(0.,-1.,0.));
#101129=DIRECTION('',(0.,-1.,0.));
#101130=DIRECTION('center_axis',(0.,-1.,0.));
#101131=DIRECTION('ref_axis',(0.,0.,-1.));
#101132=DIRECTION('',(-0.190809912898503,0.,0.981627005099017));
#101133=DIRECTION('',(-0.981627005099017,0.,-0.190809912898503));
#101134=DIRECTION('',(-0.981627005099017,0.,-0.190809912898503));
#101135=DIRECTION('center_axis',(-0.981627005099017,0.,-0.190809912898503));
#101136=DIRECTION('ref_axis',(-0.190809912898503,0.,0.981627005099017));
#101137=DIRECTION('',(0.,1.,0.));
#101138=DIRECTION('',(0.,1.,0.));
#101139=DIRECTION('center_axis',(0.,1.,0.));
#101140=DIRECTION('ref_axis',(1.,0.,0.));
#101141=DIRECTION('',(-0.190809912898503,0.,0.981627005099017));
#101142=DIRECTION('',(0.981627005099017,0.,0.190809912898503));
#101143=DIRECTION('',(-0.190809912898503,0.,0.981627005099017));
#101144=DIRECTION('',(0.981627005099017,0.,0.190809912898503));
#101145=DIRECTION('center_axis',(0.981627005099017,0.,0.190809912898503));
#101146=DIRECTION('ref_axis',(0.,-1.,0.));
#101147=DIRECTION('',(-0.190809912898503,0.,0.981627005099017));
#101148=DIRECTION('',(0.,-1.,0.));
#101149=DIRECTION('',(0.,-1.,0.));
#101150=DIRECTION('center_axis',(0.,-1.,0.));
#101151=DIRECTION('ref_axis',(0.,0.,-1.));
#101152=DIRECTION('',(-0.190809912898503,0.,0.981627005099017));
#101153=DIRECTION('',(-0.981627005099017,0.,-0.190809912898503));
#101154=DIRECTION('',(-0.981627005099017,0.,-0.190809912898503));
#101155=DIRECTION('center_axis',(-0.981627005099017,0.,-0.190809912898503));
#101156=DIRECTION('ref_axis',(-0.190809912898503,0.,0.981627005099017));
#101157=DIRECTION('',(0.,1.,0.));
#101158=DIRECTION('',(0.,1.,0.));
#101159=DIRECTION('center_axis',(0.,1.,0.));
#101160=DIRECTION('ref_axis',(1.,0.,0.));
#101161=DIRECTION('',(-0.190809912898503,0.,0.981627005099017));
#101162=DIRECTION('',(0.981627005099017,0.,0.190809912898503));
#101163=DIRECTION('',(-0.190809912898503,0.,0.981627005099017));
#101164=DIRECTION('',(0.981627005099017,0.,0.190809912898503));
#101165=DIRECTION('center_axis',(0.981627005099017,0.,0.190809912898503));
#101166=DIRECTION('ref_axis',(0.,-1.,0.));
#101167=DIRECTION('',(-0.190809912898503,0.,0.981627005099017));
#101168=DIRECTION('',(0.,-1.,0.));
#101169=DIRECTION('',(0.,-1.,0.));
#101170=DIRECTION('center_axis',(0.,-1.,0.));
#101171=DIRECTION('ref_axis',(0.,0.,-1.));
#101172=DIRECTION('',(-0.190809912898503,0.,0.981627005099017));
#101173=DIRECTION('',(-0.981627005099017,0.,-0.190809912898503));
#101174=DIRECTION('',(-0.981627005099017,0.,-0.190809912898503));
#101175=DIRECTION('center_axis',(-0.981627005099017,0.,-0.190809912898503));
#101176=DIRECTION('ref_axis',(-0.190809912898503,0.,0.981627005099017));
#101177=DIRECTION('',(0.,1.,0.));
#101178=DIRECTION('',(0.,1.,0.));
#101179=DIRECTION('center_axis',(0.,1.,0.));
#101180=DIRECTION('ref_axis',(1.,0.,0.));
#101181=DIRECTION('',(-0.190809912898503,0.,0.981627005099017));
#101182=DIRECTION('',(0.981627005099017,0.,0.190809912898503));
#101183=DIRECTION('',(-0.190809912898503,0.,0.981627005099017));
#101184=DIRECTION('',(0.981627005099017,0.,0.190809912898503));
#101185=DIRECTION('center_axis',(0.981627005099017,0.,0.190809912898503));
#101186=DIRECTION('ref_axis',(0.,-1.,0.));
#101187=DIRECTION('',(-0.190809912898503,0.,0.981627005099017));
#101188=DIRECTION('',(0.,-1.,0.));
#101189=DIRECTION('',(0.,-1.,0.));
#101190=DIRECTION('center_axis',(0.,-1.,0.));
#101191=DIRECTION('ref_axis',(0.,0.,-1.));
#101192=DIRECTION('',(-0.190809912898503,0.,0.981627005099017));
#101193=DIRECTION('',(-0.981627005099017,0.,-0.190809912898503));
#101194=DIRECTION('',(-0.981627005099017,0.,-0.190809912898503));
#101195=DIRECTION('center_axis',(-0.981627005099017,0.,-0.190809912898503));
#101196=DIRECTION('ref_axis',(-0.190809912898503,0.,0.981627005099017));
#101197=DIRECTION('',(0.,1.,0.));
#101198=DIRECTION('',(0.,1.,0.));
#101199=DIRECTION('center_axis',(0.,1.,0.));
#101200=DIRECTION('ref_axis',(1.,0.,0.));
#101201=DIRECTION('',(-0.190809912898503,0.,0.981627005099017));
#101202=DIRECTION('',(0.981627005099017,0.,0.190809912898503));
#101203=DIRECTION('',(-0.190809912898503,0.,0.981627005099017));
#101204=DIRECTION('',(0.981627005099017,0.,0.190809912898503));
#101205=DIRECTION('center_axis',(0.981627005099017,0.,0.190809912898503));
#101206=DIRECTION('ref_axis',(0.,-1.,0.));
#101207=DIRECTION('',(-0.190809912898503,0.,0.981627005099017));
#101208=DIRECTION('',(0.,-1.,0.));
#101209=DIRECTION('',(0.,-1.,0.));
#101210=DIRECTION('center_axis',(0.,-1.,0.));
#101211=DIRECTION('ref_axis',(0.,0.,-1.));
#101212=DIRECTION('',(-0.190809912898503,0.,0.981627005099017));
#101213=DIRECTION('',(-0.981627005099017,0.,-0.190809912898503));
#101214=DIRECTION('',(-0.981627005099017,0.,-0.190809912898503));
#101215=DIRECTION('center_axis',(-0.981627005099017,0.,-0.190809912898503));
#101216=DIRECTION('ref_axis',(-0.190809912898503,0.,0.981627005099017));
#101217=DIRECTION('',(0.,1.,0.));
#101218=DIRECTION('',(0.,1.,0.));
#101219=DIRECTION('center_axis',(0.,1.,0.));
#101220=DIRECTION('ref_axis',(1.,0.,0.));
#101221=DIRECTION('',(-0.190809912898503,0.,0.981627005099017));
#101222=DIRECTION('',(0.981627005099017,0.,0.190809912898503));
#101223=DIRECTION('',(-0.190809912898503,0.,0.981627005099017));
#101224=DIRECTION('',(0.981627005099017,0.,0.190809912898503));
#101225=DIRECTION('center_axis',(0.981627005099017,0.,0.190809912898503));
#101226=DIRECTION('ref_axis',(0.,-1.,0.));
#101227=DIRECTION('',(-0.190809912898503,0.,0.981627005099017));
#101228=DIRECTION('',(0.,-1.,0.));
#101229=DIRECTION('',(0.,-1.,0.));
#101230=DIRECTION('center_axis',(0.,-1.,0.));
#101231=DIRECTION('ref_axis',(0.,0.,-1.));
#101232=DIRECTION('',(-0.190809912898503,0.,0.981627005099017));
#101233=DIRECTION('',(-0.981627005099017,0.,-0.190809912898503));
#101234=DIRECTION('',(-0.981627005099017,0.,-0.190809912898503));
#101235=DIRECTION('center_axis',(-0.981627005099017,0.,-0.190809912898503));
#101236=DIRECTION('ref_axis',(-0.190809912898503,0.,0.981627005099017));
#101237=DIRECTION('',(0.,1.,0.));
#101238=DIRECTION('',(0.,1.,0.));
#101239=DIRECTION('center_axis',(0.,1.,0.));
#101240=DIRECTION('ref_axis',(1.,0.,0.));
#101241=DIRECTION('',(-0.190809912898503,0.,0.981627005099017));
#101242=DIRECTION('',(0.981627005099017,0.,0.190809912898503));
#101243=DIRECTION('',(-0.190809912898503,0.,0.981627005099017));
#101244=DIRECTION('',(0.981627005099017,0.,0.190809912898503));
#101245=DIRECTION('center_axis',(0.981627005099017,0.,0.190809912898503));
#101246=DIRECTION('ref_axis',(0.,-1.,0.));
#101247=DIRECTION('',(-0.190809912898503,0.,0.981627005099017));
#101248=DIRECTION('',(0.,-1.,0.));
#101249=DIRECTION('',(0.,-1.,0.));
#101250=DIRECTION('center_axis',(0.,-1.,0.));
#101251=DIRECTION('ref_axis',(0.,0.,-1.));
#101252=DIRECTION('',(-0.190809912898503,0.,0.981627005099017));
#101253=DIRECTION('',(-0.981627005099017,0.,-0.190809912898503));
#101254=DIRECTION('',(-0.981627005099017,0.,-0.190809912898503));
#101255=DIRECTION('center_axis',(-0.981627005099017,0.,-0.190809912898503));
#101256=DIRECTION('ref_axis',(-0.190809912898503,0.,0.981627005099017));
#101257=DIRECTION('',(0.,1.,0.));
#101258=DIRECTION('',(0.,1.,0.));
#101259=DIRECTION('center_axis',(0.,1.,0.));
#101260=DIRECTION('ref_axis',(1.,0.,0.));
#101261=DIRECTION('',(-0.190809912898503,0.,0.981627005099017));
#101262=DIRECTION('',(0.981627005099017,0.,0.190809912898503));
#101263=DIRECTION('',(-0.190809912898503,0.,0.981627005099017));
#101264=DIRECTION('',(0.981627005099017,0.,0.190809912898503));
#101265=DIRECTION('center_axis',(0.981627005099017,0.,0.190809912898503));
#101266=DIRECTION('ref_axis',(0.,-1.,0.));
#101267=DIRECTION('',(-0.190809912898503,0.,0.981627005099017));
#101268=DIRECTION('',(0.,-1.,0.));
#101269=DIRECTION('',(0.,-1.,0.));
#101270=DIRECTION('center_axis',(0.,-1.,0.));
#101271=DIRECTION('ref_axis',(0.,0.,-1.));
#101272=DIRECTION('',(-0.190809912898503,0.,0.981627005099017));
#101273=DIRECTION('',(-0.981627005099017,0.,-0.190809912898503));
#101274=DIRECTION('',(-0.981627005099017,0.,-0.190809912898503));
#101275=DIRECTION('center_axis',(-0.981627005099017,0.,-0.190809912898503));
#101276=DIRECTION('ref_axis',(-0.190809912898503,0.,0.981627005099017));
#101277=DIRECTION('',(0.,1.,0.));
#101278=DIRECTION('',(0.,1.,0.));
#101279=DIRECTION('center_axis',(0.,1.,0.));
#101280=DIRECTION('ref_axis',(1.,0.,0.));
#101281=DIRECTION('',(-0.190809912898503,0.,0.981627005099017));
#101282=DIRECTION('',(0.981627005099017,0.,0.190809912898503));
#101283=DIRECTION('',(-0.190809912898503,0.,0.981627005099017));
#101284=DIRECTION('',(0.981627005099017,0.,0.190809912898503));
#101285=DIRECTION('center_axis',(0.981627005099017,0.,0.190809912898503));
#101286=DIRECTION('ref_axis',(0.,-1.,0.));
#101287=DIRECTION('',(-0.190809912898503,0.,0.981627005099017));
#101288=DIRECTION('',(0.,-1.,0.));
#101289=DIRECTION('',(0.,-1.,0.));
#101290=DIRECTION('center_axis',(0.,-1.,0.));
#101291=DIRECTION('ref_axis',(0.,0.,-1.));
#101292=DIRECTION('',(-0.190809912898503,0.,0.981627005099017));
#101293=DIRECTION('',(-0.981627005099017,0.,-0.190809912898503));
#101294=DIRECTION('',(-0.981627005099017,0.,-0.190809912898503));
#101295=DIRECTION('center_axis',(-0.981627005099017,0.,-0.190809912898503));
#101296=DIRECTION('ref_axis',(-0.190809912898503,0.,0.981627005099017));
#101297=DIRECTION('',(0.,1.,0.));
#101298=DIRECTION('',(0.,1.,0.));
#101299=DIRECTION('center_axis',(0.,1.,0.));
#101300=DIRECTION('ref_axis',(1.,0.,0.));
#101301=DIRECTION('',(-0.190809912898503,0.,0.981627005099017));
#101302=DIRECTION('',(0.981627005099017,0.,0.190809912898503));
#101303=DIRECTION('',(-0.190809912898503,0.,0.981627005099017));
#101304=DIRECTION('',(0.981627005099017,0.,0.190809912898503));
#101305=DIRECTION('center_axis',(0.981627005099017,0.,0.190809912898503));
#101306=DIRECTION('ref_axis',(0.,-1.,0.));
#101307=DIRECTION('',(-0.190809912898503,0.,0.981627005099017));
#101308=DIRECTION('',(0.,-1.,0.));
#101309=DIRECTION('',(0.,-1.,0.));
#101310=DIRECTION('center_axis',(0.,-1.,0.));
#101311=DIRECTION('ref_axis',(0.,0.,-1.));
#101312=DIRECTION('',(-0.190809912898503,0.,0.981627005099017));
#101313=DIRECTION('',(-0.981627005099017,0.,-0.190809912898503));
#101314=DIRECTION('',(-0.981627005099017,0.,-0.190809912898503));
#101315=DIRECTION('center_axis',(-0.981627005099017,0.,-0.190809912898503));
#101316=DIRECTION('ref_axis',(-0.190809912898503,0.,0.981627005099017));
#101317=DIRECTION('',(0.,1.,0.));
#101318=DIRECTION('',(0.,1.,0.));
#101319=DIRECTION('center_axis',(0.,1.,0.));
#101320=DIRECTION('ref_axis',(1.,0.,0.));
#101321=DIRECTION('',(-0.190809912898503,0.,0.981627005099017));
#101322=DIRECTION('',(0.981627005099017,0.,0.190809912898503));
#101323=DIRECTION('',(-0.190809912898503,0.,0.981627005099017));
#101324=DIRECTION('',(0.981627005099017,0.,0.190809912898503));
#101325=DIRECTION('center_axis',(0.981627005099017,0.,0.190809912898503));
#101326=DIRECTION('ref_axis',(0.,-1.,0.));
#101327=DIRECTION('',(-0.190809912898503,0.,0.981627005099017));
#101328=DIRECTION('',(0.,-1.,0.));
#101329=DIRECTION('',(0.,-1.,0.));
#101330=DIRECTION('center_axis',(0.,-1.,0.));
#101331=DIRECTION('ref_axis',(0.,0.,-1.));
#101332=DIRECTION('',(-0.190809912898503,0.,0.981627005099017));
#101333=DIRECTION('',(-0.981627005099017,0.,-0.190809912898503));
#101334=DIRECTION('',(-0.981627005099017,0.,-0.190809912898503));
#101335=DIRECTION('center_axis',(-0.981627005099017,0.,-0.190809912898503));
#101336=DIRECTION('ref_axis',(-0.190809912898503,0.,0.981627005099017));
#101337=DIRECTION('',(0.,1.,0.));
#101338=DIRECTION('',(0.,1.,0.));
#101339=DIRECTION('center_axis',(0.,1.,0.));
#101340=DIRECTION('ref_axis',(1.,0.,0.));
#101341=DIRECTION('',(-0.190809912898503,0.,0.981627005099017));
#101342=DIRECTION('',(0.981627005099017,0.,0.190809912898503));
#101343=DIRECTION('',(-0.190809912898503,0.,0.981627005099017));
#101344=DIRECTION('',(0.981627005099017,0.,0.190809912898503));
#101345=DIRECTION('center_axis',(0.981627005099017,0.,0.190809912898503));
#101346=DIRECTION('ref_axis',(0.,-1.,0.));
#101347=DIRECTION('',(-0.190809912898503,0.,0.981627005099017));
#101348=DIRECTION('',(0.,-1.,0.));
#101349=DIRECTION('',(0.,-1.,0.));
#101350=DIRECTION('center_axis',(0.,-1.,0.));
#101351=DIRECTION('ref_axis',(0.,0.,-1.));
#101352=DIRECTION('',(-0.190809912898503,0.,0.981627005099017));
#101353=DIRECTION('',(-0.981627005099017,0.,-0.190809912898503));
#101354=DIRECTION('',(-0.981627005099017,0.,-0.190809912898503));
#101355=DIRECTION('center_axis',(-0.981627005099017,0.,-0.190809912898503));
#101356=DIRECTION('ref_axis',(-0.190809912898503,0.,0.981627005099017));
#101357=DIRECTION('',(0.,1.,0.));
#101358=DIRECTION('',(0.,1.,0.));
#101359=DIRECTION('center_axis',(0.,1.,0.));
#101360=DIRECTION('ref_axis',(1.,0.,0.));
#101361=DIRECTION('',(-0.190809912898503,0.,0.981627005099017));
#101362=DIRECTION('',(0.981627005099017,0.,0.190809912898503));
#101363=DIRECTION('',(-0.190809912898503,0.,0.981627005099017));
#101364=DIRECTION('',(0.981627005099017,0.,0.190809912898503));
#101365=DIRECTION('center_axis',(0.981627005099017,0.,0.190809912898503));
#101366=DIRECTION('ref_axis',(0.,-1.,0.));
#101367=DIRECTION('',(-0.190809912898503,0.,0.981627005099017));
#101368=DIRECTION('',(0.,-1.,0.));
#101369=DIRECTION('',(0.,-1.,0.));
#101370=DIRECTION('center_axis',(0.,-1.,0.));
#101371=DIRECTION('ref_axis',(0.,0.,-1.));
#101372=DIRECTION('',(-0.190809912898503,0.,0.981627005099017));
#101373=DIRECTION('',(-0.981627005099017,0.,-0.190809912898503));
#101374=DIRECTION('',(-0.981627005099017,0.,-0.190809912898503));
#101375=DIRECTION('center_axis',(-0.981627005099017,0.,-0.190809912898503));
#101376=DIRECTION('ref_axis',(-0.190809912898503,0.,0.981627005099017));
#101377=DIRECTION('',(0.,1.,0.));
#101378=DIRECTION('',(0.,1.,0.));
#101379=DIRECTION('center_axis',(0.,1.,0.));
#101380=DIRECTION('ref_axis',(1.,0.,0.));
#101381=DIRECTION('',(-0.190809912898503,0.,0.981627005099017));
#101382=DIRECTION('',(0.981627005099017,0.,0.190809912898503));
#101383=DIRECTION('',(-0.190809912898503,0.,0.981627005099017));
#101384=DIRECTION('',(0.981627005099017,0.,0.190809912898503));
#101385=DIRECTION('center_axis',(0.981627005099017,0.,0.190809912898503));
#101386=DIRECTION('ref_axis',(0.,-1.,0.));
#101387=DIRECTION('',(-0.190809912898503,0.,0.981627005099017));
#101388=DIRECTION('',(0.,-1.,0.));
#101389=DIRECTION('',(0.,-1.,0.));
#101390=DIRECTION('center_axis',(0.,-1.,0.));
#101391=DIRECTION('ref_axis',(0.,0.,-1.));
#101392=DIRECTION('',(-0.190809912898503,0.,0.981627005099017));
#101393=DIRECTION('',(-0.981627005099017,0.,-0.190809912898503));
#101394=DIRECTION('',(-0.981627005099017,0.,-0.190809912898503));
#101395=DIRECTION('center_axis',(-0.981627005099017,0.,-0.190809912898503));
#101396=DIRECTION('ref_axis',(-0.190809912898503,0.,0.981627005099017));
#101397=DIRECTION('',(0.,1.,0.));
#101398=DIRECTION('',(0.,1.,0.));
#101399=DIRECTION('center_axis',(0.,1.,0.));
#101400=DIRECTION('ref_axis',(1.,0.,0.));
#101401=DIRECTION('',(-0.190809912898503,0.,0.981627005099017));
#101402=DIRECTION('',(0.981627005099017,0.,0.190809912898503));
#101403=DIRECTION('',(-0.190809912898503,0.,0.981627005099017));
#101404=DIRECTION('',(0.981627005099017,0.,0.190809912898503));
#101405=DIRECTION('center_axis',(0.981627005099017,0.,0.190809912898503));
#101406=DIRECTION('ref_axis',(0.,-1.,0.));
#101407=DIRECTION('',(-0.190809912898503,0.,0.981627005099017));
#101408=DIRECTION('',(0.,-1.,0.));
#101409=DIRECTION('',(0.,-1.,0.));
#101410=DIRECTION('center_axis',(0.,-1.,0.));
#101411=DIRECTION('ref_axis',(0.,0.,-1.));
#101412=DIRECTION('',(-0.190809912898503,0.,0.981627005099017));
#101413=DIRECTION('',(-0.981627005099017,0.,-0.190809912898503));
#101414=DIRECTION('',(-0.981627005099017,0.,-0.190809912898503));
#101415=DIRECTION('center_axis',(-0.981627005099017,0.,-0.190809912898503));
#101416=DIRECTION('ref_axis',(-0.190809912898503,0.,0.981627005099017));
#101417=DIRECTION('',(0.,1.,0.));
#101418=DIRECTION('',(0.,1.,0.));
#101419=DIRECTION('center_axis',(0.,1.,0.));
#101420=DIRECTION('ref_axis',(1.,0.,0.));
#101421=DIRECTION('',(-0.190809912898503,0.,0.981627005099017));
#101422=DIRECTION('',(0.981627005099017,0.,0.190809912898503));
#101423=DIRECTION('',(-0.190809912898503,0.,0.981627005099017));
#101424=DIRECTION('',(0.981627005099017,0.,0.190809912898503));
#101425=DIRECTION('center_axis',(0.981627005099017,0.,0.190809912898503));
#101426=DIRECTION('ref_axis',(0.,-1.,0.));
#101427=DIRECTION('',(-0.190809912898503,0.,0.981627005099017));
#101428=DIRECTION('',(0.,-1.,0.));
#101429=DIRECTION('',(0.,-1.,0.));
#101430=DIRECTION('center_axis',(0.,-1.,0.));
#101431=DIRECTION('ref_axis',(0.,0.,-1.));
#101432=DIRECTION('',(-0.190809912898503,0.,0.981627005099017));
#101433=DIRECTION('',(-0.981627005099017,0.,-0.190809912898503));
#101434=DIRECTION('',(-0.981627005099017,0.,-0.190809912898503));
#101435=DIRECTION('center_axis',(-0.981627005099017,0.,-0.190809912898503));
#101436=DIRECTION('ref_axis',(-0.190809912898503,0.,0.981627005099017));
#101437=DIRECTION('',(0.,1.,0.));
#101438=DIRECTION('',(0.,1.,0.));
#101439=DIRECTION('center_axis',(0.,1.,0.));
#101440=DIRECTION('ref_axis',(1.,0.,0.));
#101441=DIRECTION('',(-0.190809912898503,0.,0.981627005099017));
#101442=DIRECTION('',(0.981627005099017,0.,0.190809912898503));
#101443=DIRECTION('',(-0.190809912898503,0.,0.981627005099017));
#101444=DIRECTION('',(0.981627005099017,0.,0.190809912898503));
#101445=DIRECTION('center_axis',(0.981627005099017,0.,0.190809912898503));
#101446=DIRECTION('ref_axis',(0.,-1.,0.));
#101447=DIRECTION('',(-0.190809912898503,0.,0.981627005099017));
#101448=DIRECTION('',(0.,-1.,0.));
#101449=DIRECTION('',(0.,-1.,0.));
#101450=DIRECTION('center_axis',(0.,-1.,0.));
#101451=DIRECTION('ref_axis',(0.,0.,-1.));
#101452=DIRECTION('',(-0.190809912898503,0.,0.981627005099017));
#101453=DIRECTION('',(-0.981627005099017,0.,-0.190809912898503));
#101454=DIRECTION('',(-0.981627005099017,0.,-0.190809912898503));
#101455=DIRECTION('center_axis',(-0.981627005099017,0.,-0.190809912898503));
#101456=DIRECTION('ref_axis',(-0.190809912898503,0.,0.981627005099017));
#101457=DIRECTION('',(0.,1.,0.));
#101458=DIRECTION('',(0.,1.,0.));
#101459=DIRECTION('center_axis',(0.,1.,0.));
#101460=DIRECTION('ref_axis',(1.,0.,0.));
#101461=DIRECTION('',(-0.190809912898503,0.,0.981627005099017));
#101462=DIRECTION('',(0.981627005099017,0.,0.190809912898503));
#101463=DIRECTION('',(-0.190809912898503,0.,0.981627005099017));
#101464=DIRECTION('',(0.981627005099017,0.,0.190809912898503));
#101465=DIRECTION('center_axis',(0.981627005099017,0.,0.190809912898503));
#101466=DIRECTION('ref_axis',(0.,-1.,0.));
#101467=DIRECTION('',(-0.190809912898503,0.,0.981627005099017));
#101468=DIRECTION('',(0.,-1.,0.));
#101469=DIRECTION('',(0.,-1.,0.));
#101470=DIRECTION('center_axis',(0.,-1.,0.));
#101471=DIRECTION('ref_axis',(0.,0.,-1.));
#101472=DIRECTION('',(-0.190809912898503,0.,0.981627005099017));
#101473=DIRECTION('',(-0.981627005099017,0.,-0.190809912898503));
#101474=DIRECTION('',(-0.981627005099017,0.,-0.190809912898503));
#101475=DIRECTION('center_axis',(-0.981627005099017,0.,-0.190809912898503));
#101476=DIRECTION('ref_axis',(-0.190809912898503,0.,0.981627005099017));
#101477=DIRECTION('',(0.,1.,0.));
#101478=DIRECTION('',(0.,1.,0.));
#101479=DIRECTION('center_axis',(0.,1.,0.));
#101480=DIRECTION('ref_axis',(1.,0.,0.));
#101481=DIRECTION('',(-0.190809912898503,0.,0.981627005099017));
#101482=DIRECTION('',(0.981627005099017,0.,0.190809912898503));
#101483=DIRECTION('',(-0.190809912898503,0.,0.981627005099017));
#101484=DIRECTION('',(0.981627005099017,0.,0.190809912898503));
#101485=DIRECTION('center_axis',(0.981627005099017,0.,0.190809912898503));
#101486=DIRECTION('ref_axis',(0.,-1.,0.));
#101487=DIRECTION('',(-0.190809912898503,0.,0.981627005099017));
#101488=DIRECTION('',(0.,-1.,0.));
#101489=DIRECTION('',(0.,-1.,0.));
#101490=DIRECTION('center_axis',(0.,-1.,0.));
#101491=DIRECTION('ref_axis',(0.,0.,-1.));
#101492=DIRECTION('',(-0.190809912898503,0.,0.981627005099017));
#101493=DIRECTION('',(-0.981627005099017,0.,-0.190809912898503));
#101494=DIRECTION('',(-0.981627005099017,0.,-0.190809912898503));
#101495=DIRECTION('center_axis',(-0.981627005099017,0.,-0.190809912898503));
#101496=DIRECTION('ref_axis',(-0.190809912898503,0.,0.981627005099017));
#101497=DIRECTION('',(0.,1.,0.));
#101498=DIRECTION('',(0.,1.,0.));
#101499=DIRECTION('center_axis',(0.,1.,0.));
#101500=DIRECTION('ref_axis',(1.,0.,0.));
#101501=DIRECTION('',(-0.190809912898503,0.,0.981627005099017));
#101502=DIRECTION('',(0.981627005099017,0.,0.190809912898503));
#101503=DIRECTION('',(-0.190809912898503,0.,0.981627005099017));
#101504=DIRECTION('',(0.981627005099017,0.,0.190809912898503));
#101505=DIRECTION('center_axis',(0.981627005099017,0.,0.190809912898503));
#101506=DIRECTION('ref_axis',(0.,-1.,0.));
#101507=DIRECTION('',(-0.190809912898503,0.,0.981627005099017));
#101508=DIRECTION('',(0.,-1.,0.));
#101509=DIRECTION('',(0.,-1.,0.));
#101510=DIRECTION('center_axis',(0.,-1.,0.));
#101511=DIRECTION('ref_axis',(0.,0.,-1.));
#101512=DIRECTION('',(-0.190809912898503,0.,0.981627005099017));
#101513=DIRECTION('',(-0.981627005099017,0.,-0.190809912898503));
#101514=DIRECTION('',(-0.981627005099017,0.,-0.190809912898503));
#101515=DIRECTION('center_axis',(-0.981627005099017,0.,-0.190809912898503));
#101516=DIRECTION('ref_axis',(-0.190809912898503,0.,0.981627005099017));
#101517=DIRECTION('',(0.,1.,0.));
#101518=DIRECTION('',(0.,1.,0.));
#101519=DIRECTION('center_axis',(0.,1.,0.));
#101520=DIRECTION('ref_axis',(1.,0.,0.));
#101521=DIRECTION('',(-0.190809912898503,0.,0.981627005099017));
#101522=DIRECTION('',(0.981627005099017,0.,0.190809912898503));
#101523=DIRECTION('',(-0.190809912898503,0.,0.981627005099017));
#101524=DIRECTION('',(0.981627005099017,0.,0.190809912898503));
#101525=DIRECTION('center_axis',(0.981627005099017,0.,0.190809912898503));
#101526=DIRECTION('ref_axis',(0.,-1.,0.));
#101527=DIRECTION('',(-0.190809912898503,0.,0.981627005099017));
#101528=DIRECTION('',(0.,-1.,0.));
#101529=DIRECTION('',(0.,-1.,0.));
#101530=DIRECTION('center_axis',(0.,-1.,0.));
#101531=DIRECTION('ref_axis',(0.,0.,-1.));
#101532=DIRECTION('',(-0.190809912898503,0.,0.981627005099017));
#101533=DIRECTION('',(-0.981627005099017,0.,-0.190809912898503));
#101534=DIRECTION('',(-0.981627005099017,0.,-0.190809912898503));
#101535=DIRECTION('center_axis',(-0.981627005099017,0.,-0.190809912898503));
#101536=DIRECTION('ref_axis',(-0.190809912898503,0.,0.981627005099017));
#101537=DIRECTION('',(0.,1.,0.));
#101538=DIRECTION('',(0.,1.,0.));
#101539=DIRECTION('center_axis',(0.,1.,0.));
#101540=DIRECTION('ref_axis',(1.,0.,0.));
#101541=DIRECTION('',(-0.190809912898503,0.,0.981627005099017));
#101542=DIRECTION('',(0.981627005099017,0.,0.190809912898503));
#101543=DIRECTION('',(-0.190809912898503,0.,0.981627005099017));
#101544=DIRECTION('',(0.981627005099017,0.,0.190809912898503));
#101545=DIRECTION('center_axis',(0.981627005099017,0.,0.190809912898503));
#101546=DIRECTION('ref_axis',(0.,-1.,0.));
#101547=DIRECTION('',(-0.190809912898503,0.,0.981627005099017));
#101548=DIRECTION('',(0.,-1.,0.));
#101549=DIRECTION('',(0.,-1.,0.));
#101550=DIRECTION('center_axis',(0.,-1.,0.));
#101551=DIRECTION('ref_axis',(0.,0.,-1.));
#101552=DIRECTION('',(-0.190809912898503,0.,0.981627005099017));
#101553=DIRECTION('',(-0.981627005099017,0.,-0.190809912898503));
#101554=DIRECTION('',(-0.981627005099017,0.,-0.190809912898503));
#101555=DIRECTION('center_axis',(-0.981627005099017,0.,-0.190809912898503));
#101556=DIRECTION('ref_axis',(-0.190809912898503,0.,0.981627005099017));
#101557=DIRECTION('',(0.,1.,0.));
#101558=DIRECTION('',(0.,1.,0.));
#101559=DIRECTION('center_axis',(0.,1.,0.));
#101560=DIRECTION('ref_axis',(1.,0.,0.));
#101561=DIRECTION('',(-0.190809912898503,0.,0.981627005099017));
#101562=DIRECTION('',(0.981627005099017,0.,0.190809912898503));
#101563=DIRECTION('',(-0.190809912898503,0.,0.981627005099017));
#101564=DIRECTION('',(0.981627005099017,0.,0.190809912898503));
#101565=DIRECTION('center_axis',(0.981627005099017,0.,0.190809912898503));
#101566=DIRECTION('ref_axis',(0.,-1.,0.));
#101567=DIRECTION('',(-0.190809912898503,0.,0.981627005099017));
#101568=DIRECTION('',(0.,-1.,0.));
#101569=DIRECTION('',(0.,-1.,0.));
#101570=DIRECTION('center_axis',(0.,-1.,0.));
#101571=DIRECTION('ref_axis',(0.,0.,-1.));
#101572=DIRECTION('',(-0.190809912898503,0.,0.981627005099017));
#101573=DIRECTION('',(-0.981627005099017,0.,-0.190809912898503));
#101574=DIRECTION('',(-0.981627005099017,0.,-0.190809912898503));
#101575=DIRECTION('center_axis',(-0.981627005099017,0.,-0.190809912898503));
#101576=DIRECTION('ref_axis',(-0.190809912898503,0.,0.981627005099017));
#101577=DIRECTION('',(0.,1.,0.));
#101578=DIRECTION('',(0.,1.,0.));
#101579=DIRECTION('center_axis',(0.,1.,0.));
#101580=DIRECTION('ref_axis',(1.,0.,0.));
#101581=DIRECTION('',(-0.190809912898503,0.,0.981627005099017));
#101582=DIRECTION('',(0.981627005099017,0.,0.190809912898503));
#101583=DIRECTION('',(-0.190809912898503,0.,0.981627005099017));
#101584=DIRECTION('',(0.981627005099017,0.,0.190809912898503));
#101585=DIRECTION('center_axis',(0.981627005099017,0.,0.190809912898503));
#101586=DIRECTION('ref_axis',(0.,-1.,0.));
#101587=DIRECTION('',(-0.190809912898503,0.,0.981627005099017));
#101588=DIRECTION('',(0.,-1.,0.));
#101589=DIRECTION('',(0.,-1.,0.));
#101590=DIRECTION('center_axis',(0.,-1.,0.));
#101591=DIRECTION('ref_axis',(0.,0.,-1.));
#101592=DIRECTION('',(-0.190809912898503,0.,0.981627005099017));
#101593=DIRECTION('',(-0.981627005099017,0.,-0.190809912898503));
#101594=DIRECTION('',(-0.981627005099017,0.,-0.190809912898503));
#101595=DIRECTION('center_axis',(-0.981627005099017,0.,-0.190809912898503));
#101596=DIRECTION('ref_axis',(-0.190809912898503,0.,0.981627005099017));
#101597=DIRECTION('',(0.,1.,0.));
#101598=DIRECTION('',(0.,1.,0.));
#101599=DIRECTION('center_axis',(0.,1.,0.));
#101600=DIRECTION('ref_axis',(1.,0.,0.));
#101601=DIRECTION('',(-0.190809912898503,0.,0.981627005099017));
#101602=DIRECTION('',(0.981627005099017,0.,0.190809912898503));
#101603=DIRECTION('',(-0.190809912898503,0.,0.981627005099017));
#101604=DIRECTION('',(0.981627005099017,0.,0.190809912898503));
#101605=DIRECTION('center_axis',(0.981627005099017,0.,0.190809912898503));
#101606=DIRECTION('ref_axis',(0.,-1.,0.));
#101607=DIRECTION('',(-0.190809912898503,0.,0.981627005099017));
#101608=DIRECTION('',(0.,-1.,0.));
#101609=DIRECTION('',(0.,-1.,0.));
#101610=DIRECTION('center_axis',(0.,-1.,0.));
#101611=DIRECTION('ref_axis',(0.,0.,-1.));
#101612=DIRECTION('',(-0.190809912898503,0.,0.981627005099017));
#101613=DIRECTION('',(-0.981627005099017,0.,-0.190809912898503));
#101614=DIRECTION('',(-0.981627005099017,0.,-0.190809912898503));
#101615=DIRECTION('center_axis',(-0.981627005099017,0.,-0.190809912898503));
#101616=DIRECTION('ref_axis',(-0.190809912898503,0.,0.981627005099017));
#101617=DIRECTION('',(0.,1.,0.));
#101618=DIRECTION('',(0.,1.,0.));
#101619=DIRECTION('center_axis',(0.,1.,0.));
#101620=DIRECTION('ref_axis',(1.,0.,0.));
#101621=DIRECTION('',(-0.190809912898503,0.,0.981627005099017));
#101622=DIRECTION('',(0.981627005099017,0.,0.190809912898503));
#101623=DIRECTION('',(-0.190809912898503,0.,0.981627005099017));
#101624=DIRECTION('',(0.981627005099017,0.,0.190809912898503));
#101625=DIRECTION('center_axis',(0.981627005099017,0.,0.190809912898503));
#101626=DIRECTION('ref_axis',(0.,-1.,0.));
#101627=DIRECTION('',(-0.190809912898503,0.,0.981627005099017));
#101628=DIRECTION('',(0.,-1.,0.));
#101629=DIRECTION('',(0.,-1.,0.));
#101630=DIRECTION('center_axis',(0.,-1.,0.));
#101631=DIRECTION('ref_axis',(0.,0.,-1.));
#101632=DIRECTION('',(-0.190809912898503,0.,0.981627005099017));
#101633=DIRECTION('',(-0.981627005099017,0.,-0.190809912898503));
#101634=DIRECTION('',(-0.981627005099017,0.,-0.190809912898503));
#101635=DIRECTION('center_axis',(-0.981627005099017,0.,-0.190809912898503));
#101636=DIRECTION('ref_axis',(-0.190809912898503,0.,0.981627005099017));
#101637=DIRECTION('',(0.,1.,0.));
#101638=DIRECTION('',(0.,1.,0.));
#101639=DIRECTION('center_axis',(0.,1.,0.));
#101640=DIRECTION('ref_axis',(1.,0.,0.));
#101641=DIRECTION('',(-0.190809912898503,0.,0.981627005099017));
#101642=DIRECTION('',(0.981627005099017,0.,0.190809912898503));
#101643=DIRECTION('',(-0.190809912898503,0.,0.981627005099017));
#101644=DIRECTION('',(0.981627005099017,0.,0.190809912898503));
#101645=DIRECTION('center_axis',(0.981627005099017,0.,0.190809912898503));
#101646=DIRECTION('ref_axis',(0.,-1.,0.));
#101647=DIRECTION('',(-0.190809912898503,0.,0.981627005099017));
#101648=DIRECTION('',(0.,-1.,0.));
#101649=DIRECTION('',(0.,-1.,0.));
#101650=DIRECTION('center_axis',(0.,-1.,0.));
#101651=DIRECTION('ref_axis',(0.,0.,-1.));
#101652=DIRECTION('',(-0.190809912898503,0.,0.981627005099017));
#101653=DIRECTION('',(-0.981627005099017,0.,-0.190809912898503));
#101654=DIRECTION('',(-0.981627005099017,0.,-0.190809912898503));
#101655=DIRECTION('center_axis',(-0.981627005099017,0.,-0.190809912898503));
#101656=DIRECTION('ref_axis',(-0.190809912898503,0.,0.981627005099017));
#101657=DIRECTION('',(0.,1.,0.));
#101658=DIRECTION('',(0.,1.,0.));
#101659=DIRECTION('center_axis',(0.,1.,0.));
#101660=DIRECTION('ref_axis',(1.,0.,0.));
#101661=DIRECTION('',(-0.190809912898503,0.,0.981627005099017));
#101662=DIRECTION('',(0.981627005099017,0.,0.190809912898503));
#101663=DIRECTION('',(-0.190809912898503,0.,0.981627005099017));
#101664=DIRECTION('',(0.981627005099017,0.,0.190809912898503));
#101665=DIRECTION('center_axis',(0.981627005099017,0.,0.190809912898503));
#101666=DIRECTION('ref_axis',(0.,-1.,0.));
#101667=DIRECTION('',(-0.190809912898503,0.,0.981627005099017));
#101668=DIRECTION('',(0.,-1.,0.));
#101669=DIRECTION('',(0.,-1.,0.));
#101670=DIRECTION('center_axis',(0.,-1.,0.));
#101671=DIRECTION('ref_axis',(0.,0.,-1.));
#101672=DIRECTION('',(-0.190809912898503,0.,0.981627005099017));
#101673=DIRECTION('',(-0.981627005099017,0.,-0.190809912898503));
#101674=DIRECTION('',(-0.981627005099017,0.,-0.190809912898503));
#101675=DIRECTION('center_axis',(-0.981627005099017,0.,-0.190809912898503));
#101676=DIRECTION('ref_axis',(-0.190809912898503,0.,0.981627005099017));
#101677=DIRECTION('',(0.,1.,0.));
#101678=DIRECTION('',(0.,1.,0.));
#101679=DIRECTION('center_axis',(0.,1.,0.));
#101680=DIRECTION('ref_axis',(1.,0.,0.));
#101681=DIRECTION('',(-0.190809912898503,0.,0.981627005099017));
#101682=DIRECTION('',(0.981627005099017,0.,0.190809912898503));
#101683=DIRECTION('',(-0.190809912898503,0.,0.981627005099017));
#101684=DIRECTION('',(0.981627005099017,0.,0.190809912898503));
#101685=DIRECTION('center_axis',(0.981627005099017,0.,0.190809912898503));
#101686=DIRECTION('ref_axis',(0.,-1.,0.));
#101687=DIRECTION('',(-0.190809912898503,0.,0.981627005099017));
#101688=DIRECTION('',(0.,-1.,0.));
#101689=DIRECTION('',(0.,-1.,0.));
#101690=DIRECTION('center_axis',(0.,-1.,0.));
#101691=DIRECTION('ref_axis',(0.,0.,-1.));
#101692=DIRECTION('',(-0.190809912898503,0.,0.981627005099017));
#101693=DIRECTION('',(-0.981627005099017,0.,-0.190809912898503));
#101694=DIRECTION('',(-0.981627005099017,0.,-0.190809912898503));
#101695=DIRECTION('center_axis',(-0.981627005099017,0.,-0.190809912898503));
#101696=DIRECTION('ref_axis',(-0.190809912898503,0.,0.981627005099017));
#101697=DIRECTION('',(0.,1.,0.));
#101698=DIRECTION('',(0.,1.,0.));
#101699=DIRECTION('center_axis',(0.,1.,0.));
#101700=DIRECTION('ref_axis',(1.,0.,0.));
#101701=DIRECTION('',(-0.190809912898503,0.,0.981627005099017));
#101702=DIRECTION('',(0.981627005099017,0.,0.190809912898503));
#101703=DIRECTION('',(-0.190809912898503,0.,0.981627005099017));
#101704=DIRECTION('',(0.981627005099017,0.,0.190809912898503));
#101705=DIRECTION('center_axis',(0.981627005099017,0.,0.190809912898503));
#101706=DIRECTION('ref_axis',(0.,-1.,0.));
#101707=DIRECTION('',(-0.190809912898503,0.,0.981627005099017));
#101708=DIRECTION('',(0.,-1.,0.));
#101709=DIRECTION('',(0.,-1.,0.));
#101710=DIRECTION('center_axis',(0.,-1.,0.));
#101711=DIRECTION('ref_axis',(0.,0.,-1.));
#101712=DIRECTION('',(-0.190809912898503,0.,0.981627005099017));
#101713=DIRECTION('',(-0.981627005099017,0.,-0.190809912898503));
#101714=DIRECTION('',(-0.981627005099017,0.,-0.190809912898503));
#101715=DIRECTION('center_axis',(-0.981627005099017,0.,-0.190809912898503));
#101716=DIRECTION('ref_axis',(-0.190809912898503,0.,0.981627005099017));
#101717=DIRECTION('',(0.,1.,0.));
#101718=DIRECTION('',(0.,1.,0.));
#101719=DIRECTION('center_axis',(0.,1.,0.));
#101720=DIRECTION('ref_axis',(1.,0.,0.));
#101721=DIRECTION('',(-0.190809912898503,0.,0.981627005099017));
#101722=DIRECTION('',(0.981627005099017,0.,0.190809912898503));
#101723=DIRECTION('',(-0.190809912898503,0.,0.981627005099017));
#101724=DIRECTION('',(0.981627005099017,0.,0.190809912898503));
#101725=DIRECTION('center_axis',(0.981627005099017,0.,0.190809912898503));
#101726=DIRECTION('ref_axis',(0.,-1.,0.));
#101727=DIRECTION('',(-0.190809912898503,0.,0.981627005099017));
#101728=DIRECTION('',(0.,-1.,0.));
#101729=DIRECTION('',(0.,-1.,0.));
#101730=DIRECTION('center_axis',(0.,-1.,0.));
#101731=DIRECTION('ref_axis',(0.,0.,-1.));
#101732=DIRECTION('',(-0.190809912898503,0.,0.981627005099017));
#101733=DIRECTION('',(-0.981627005099017,0.,-0.190809912898503));
#101734=DIRECTION('',(-0.981627005099017,0.,-0.190809912898503));
#101735=DIRECTION('center_axis',(-0.981627005099017,0.,-0.190809912898503));
#101736=DIRECTION('ref_axis',(-0.190809912898503,0.,0.981627005099017));
#101737=DIRECTION('',(0.,1.,0.));
#101738=DIRECTION('',(0.,1.,0.));
#101739=DIRECTION('center_axis',(0.,1.,0.));
#101740=DIRECTION('ref_axis',(1.,0.,0.));
#101741=DIRECTION('',(-0.190809912898503,0.,0.981627005099017));
#101742=DIRECTION('',(0.981627005099017,0.,0.190809912898503));
#101743=DIRECTION('',(-0.190809912898503,0.,0.981627005099017));
#101744=DIRECTION('',(0.981627005099017,0.,0.190809912898503));
#101745=DIRECTION('center_axis',(0.981627005099017,0.,0.190809912898503));
#101746=DIRECTION('ref_axis',(0.,-1.,0.));
#101747=DIRECTION('',(-0.190809912898503,0.,0.981627005099017));
#101748=DIRECTION('',(0.,-1.,0.));
#101749=DIRECTION('',(0.,-1.,0.));
#101750=DIRECTION('center_axis',(0.,-1.,0.));
#101751=DIRECTION('ref_axis',(0.,0.,-1.));
#101752=DIRECTION('',(-0.190809912898503,0.,0.981627005099017));
#101753=DIRECTION('',(-0.981627005099017,0.,-0.190809912898503));
#101754=DIRECTION('',(-0.981627005099017,0.,-0.190809912898503));
#101755=DIRECTION('center_axis',(-0.981627005099017,0.,-0.190809912898503));
#101756=DIRECTION('ref_axis',(-0.190809912898503,0.,0.981627005099017));
#101757=DIRECTION('',(0.,1.,0.));
#101758=DIRECTION('',(0.,1.,0.));
#101759=DIRECTION('center_axis',(0.,1.,0.));
#101760=DIRECTION('ref_axis',(1.,0.,0.));
#101761=DIRECTION('',(-0.190809912898503,0.,0.981627005099017));
#101762=DIRECTION('',(0.981627005099017,0.,0.190809912898503));
#101763=DIRECTION('',(-0.190809912898503,0.,0.981627005099017));
#101764=DIRECTION('',(0.981627005099017,0.,0.190809912898503));
#101765=DIRECTION('center_axis',(0.981627005099017,0.,0.190809912898503));
#101766=DIRECTION('ref_axis',(0.,-1.,0.));
#101767=DIRECTION('',(-0.190809912898503,0.,0.981627005099017));
#101768=DIRECTION('',(0.,-1.,0.));
#101769=DIRECTION('',(0.,-1.,0.));
#101770=DIRECTION('center_axis',(0.,-1.,0.));
#101771=DIRECTION('ref_axis',(0.,0.,-1.));
#101772=DIRECTION('',(-0.190809912898503,0.,0.981627005099017));
#101773=DIRECTION('',(-0.981627005099017,0.,-0.190809912898503));
#101774=DIRECTION('',(-0.981627005099017,0.,-0.190809912898503));
#101775=DIRECTION('center_axis',(-0.981627005099017,0.,-0.190809912898503));
#101776=DIRECTION('ref_axis',(-0.190809912898503,0.,0.981627005099017));
#101777=DIRECTION('',(0.,1.,0.));
#101778=DIRECTION('',(0.,1.,0.));
#101779=DIRECTION('center_axis',(0.,1.,0.));
#101780=DIRECTION('ref_axis',(1.,0.,0.));
#101781=DIRECTION('',(-0.190809912898503,0.,0.981627005099017));
#101782=DIRECTION('',(0.981627005099017,0.,0.190809912898503));
#101783=DIRECTION('',(-0.190809912898503,0.,0.981627005099017));
#101784=DIRECTION('',(0.981627005099017,0.,0.190809912898503));
#101785=DIRECTION('center_axis',(0.981627005099017,0.,0.190809912898503));
#101786=DIRECTION('ref_axis',(0.,-1.,0.));
#101787=DIRECTION('',(-0.190809912898503,0.,0.981627005099017));
#101788=DIRECTION('',(0.,-1.,0.));
#101789=DIRECTION('',(0.,-1.,0.));
#101790=DIRECTION('center_axis',(0.,-1.,0.));
#101791=DIRECTION('ref_axis',(0.,0.,-1.));
#101792=DIRECTION('',(-0.190809912898503,0.,0.981627005099017));
#101793=DIRECTION('',(-0.981627005099017,0.,-0.190809912898503));
#101794=DIRECTION('',(-0.981627005099017,0.,-0.190809912898503));
#101795=DIRECTION('center_axis',(-0.981627005099017,0.,-0.190809912898503));
#101796=DIRECTION('ref_axis',(-0.190809912898503,0.,0.981627005099017));
#101797=DIRECTION('',(0.,1.,0.));
#101798=DIRECTION('',(0.,1.,0.));
#101799=DIRECTION('center_axis',(0.,1.,0.));
#101800=DIRECTION('ref_axis',(1.,0.,0.));
#101801=DIRECTION('',(-0.190809912898503,0.,0.981627005099017));
#101802=DIRECTION('',(0.981627005099017,0.,0.190809912898503));
#101803=DIRECTION('',(-0.190809912898503,0.,0.981627005099017));
#101804=DIRECTION('',(0.981627005099017,0.,0.190809912898503));
#101805=DIRECTION('center_axis',(0.981627005099017,0.,0.190809912898503));
#101806=DIRECTION('ref_axis',(0.,-1.,0.));
#101807=DIRECTION('',(-0.190809912898503,0.,0.981627005099017));
#101808=DIRECTION('',(0.,-1.,0.));
#101809=DIRECTION('',(0.,-1.,0.));
#101810=DIRECTION('center_axis',(0.,-1.,0.));
#101811=DIRECTION('ref_axis',(0.,0.,-1.));
#101812=DIRECTION('',(-0.190809912898503,0.,0.981627005099017));
#101813=DIRECTION('',(-0.981627005099017,0.,-0.190809912898503));
#101814=DIRECTION('',(-0.981627005099017,0.,-0.190809912898503));
#101815=DIRECTION('center_axis',(-0.981627005099017,0.,-0.190809912898503));
#101816=DIRECTION('ref_axis',(-0.190809912898503,0.,0.981627005099017));
#101817=DIRECTION('',(0.,1.,0.));
#101818=DIRECTION('',(0.,1.,0.));
#101819=DIRECTION('center_axis',(0.,1.,0.));
#101820=DIRECTION('ref_axis',(1.,0.,0.));
#101821=DIRECTION('',(-0.190809912898503,0.,0.981627005099017));
#101822=DIRECTION('',(0.981627005099017,0.,0.190809912898503));
#101823=DIRECTION('',(-0.190809912898503,0.,0.981627005099017));
#101824=DIRECTION('',(0.981627005099017,0.,0.190809912898503));
#101825=DIRECTION('center_axis',(0.981627005099017,0.,0.190809912898503));
#101826=DIRECTION('ref_axis',(0.,-1.,0.));
#101827=DIRECTION('',(-0.190809912898503,0.,0.981627005099017));
#101828=DIRECTION('',(0.,-1.,0.));
#101829=DIRECTION('',(0.,-1.,0.));
#101830=DIRECTION('center_axis',(0.,-1.,0.));
#101831=DIRECTION('ref_axis',(0.,0.,-1.));
#101832=DIRECTION('',(-0.190809912898503,0.,0.981627005099017));
#101833=DIRECTION('',(-0.981627005099017,0.,-0.190809912898503));
#101834=DIRECTION('',(-0.981627005099017,0.,-0.190809912898503));
#101835=DIRECTION('center_axis',(-0.981627005099017,0.,-0.190809912898503));
#101836=DIRECTION('ref_axis',(-0.190809912898503,0.,0.981627005099017));
#101837=DIRECTION('',(0.,1.,0.));
#101838=DIRECTION('',(0.,1.,0.));
#101839=DIRECTION('center_axis',(0.,1.,0.));
#101840=DIRECTION('ref_axis',(1.,0.,0.));
#101841=DIRECTION('',(-0.190809912898503,0.,0.981627005099017));
#101842=DIRECTION('',(0.981627005099017,0.,0.190809912898503));
#101843=DIRECTION('',(-0.190809912898503,0.,0.981627005099017));
#101844=DIRECTION('',(0.981627005099017,0.,0.190809912898503));
#101845=DIRECTION('center_axis',(0.981627005099017,0.,0.190809912898503));
#101846=DIRECTION('ref_axis',(0.,-1.,0.));
#101847=DIRECTION('',(-0.190809912898503,0.,0.981627005099017));
#101848=DIRECTION('',(0.,-1.,0.));
#101849=DIRECTION('',(0.,-1.,0.));
#101850=DIRECTION('center_axis',(0.,-1.,0.));
#101851=DIRECTION('ref_axis',(0.,0.,-1.));
#101852=DIRECTION('',(-0.190809912898503,0.,0.981627005099017));
#101853=DIRECTION('',(-0.981627005099017,0.,-0.190809912898503));
#101854=DIRECTION('',(-0.981627005099017,0.,-0.190809912898503));
#101855=DIRECTION('center_axis',(-0.981627005099017,0.,-0.190809912898503));
#101856=DIRECTION('ref_axis',(-0.190809912898503,0.,0.981627005099017));
#101857=DIRECTION('',(0.,1.,0.));
#101858=DIRECTION('',(0.,1.,0.));
#101859=DIRECTION('center_axis',(0.,1.,0.));
#101860=DIRECTION('ref_axis',(1.,0.,0.));
#101861=DIRECTION('',(-0.190809912898503,0.,0.981627005099017));
#101862=DIRECTION('',(0.981627005099017,0.,0.190809912898503));
#101863=DIRECTION('',(-0.190809912898503,0.,0.981627005099017));
#101864=DIRECTION('',(0.981627005099017,0.,0.190809912898503));
#101865=DIRECTION('center_axis',(0.981627005099017,0.,0.190809912898503));
#101866=DIRECTION('ref_axis',(0.,-1.,0.));
#101867=DIRECTION('',(-0.190809912898503,0.,0.981627005099017));
#101868=DIRECTION('',(0.,-1.,0.));
#101869=DIRECTION('',(0.,-1.,0.));
#101870=DIRECTION('center_axis',(0.,-1.,0.));
#101871=DIRECTION('ref_axis',(0.,0.,-1.));
#101872=DIRECTION('',(-0.190809912898503,0.,0.981627005099017));
#101873=DIRECTION('',(-0.981627005099017,0.,-0.190809912898503));
#101874=DIRECTION('',(-0.981627005099017,0.,-0.190809912898503));
#101875=DIRECTION('center_axis',(-0.981627005099017,0.,-0.190809912898503));
#101876=DIRECTION('ref_axis',(-0.190809912898503,0.,0.981627005099017));
#101877=DIRECTION('',(0.,1.,0.));
#101878=DIRECTION('',(0.,1.,0.));
#101879=DIRECTION('center_axis',(0.,1.,0.));
#101880=DIRECTION('ref_axis',(1.,0.,0.));
#101881=DIRECTION('',(-0.190809912898503,0.,0.981627005099017));
#101882=DIRECTION('',(0.981627005099017,0.,0.190809912898503));
#101883=DIRECTION('',(-0.190809912898503,0.,0.981627005099017));
#101884=DIRECTION('',(0.981627005099017,0.,0.190809912898503));
#101885=DIRECTION('center_axis',(0.981627005099017,0.,0.190809912898503));
#101886=DIRECTION('ref_axis',(0.,-1.,0.));
#101887=DIRECTION('',(-0.190809912898503,0.,0.981627005099017));
#101888=DIRECTION('',(0.,-1.,0.));
#101889=DIRECTION('',(0.,-1.,0.));
#101890=DIRECTION('center_axis',(0.,-1.,0.));
#101891=DIRECTION('ref_axis',(0.,0.,-1.));
#101892=DIRECTION('',(-0.190809912898503,0.,0.981627005099017));
#101893=DIRECTION('',(-0.981627005099017,0.,-0.190809912898503));
#101894=DIRECTION('',(-0.981627005099017,0.,-0.190809912898503));
#101895=DIRECTION('center_axis',(-0.981627005099017,0.,-0.190809912898503));
#101896=DIRECTION('ref_axis',(-0.190809912898503,0.,0.981627005099017));
#101897=DIRECTION('',(0.,1.,0.));
#101898=DIRECTION('',(0.,1.,0.));
#101899=DIRECTION('center_axis',(0.,1.,0.));
#101900=DIRECTION('ref_axis',(1.,0.,0.));
#101901=DIRECTION('',(-0.190809912898503,0.,0.981627005099017));
#101902=DIRECTION('',(0.981627005099017,0.,0.190809912898503));
#101903=DIRECTION('',(-0.190809912898503,0.,0.981627005099017));
#101904=DIRECTION('',(0.981627005099017,0.,0.190809912898503));
#101905=DIRECTION('center_axis',(0.981627005099017,0.,0.190809912898503));
#101906=DIRECTION('ref_axis',(0.,-1.,0.));
#101907=DIRECTION('',(-0.190809912898503,0.,0.981627005099017));
#101908=DIRECTION('',(0.,-1.,0.));
#101909=DIRECTION('',(0.,-1.,0.));
#101910=DIRECTION('center_axis',(0.,-1.,0.));
#101911=DIRECTION('ref_axis',(0.,0.,-1.));
#101912=DIRECTION('',(-0.190809912898503,0.,0.981627005099017));
#101913=DIRECTION('',(-0.981627005099017,0.,-0.190809912898503));
#101914=DIRECTION('',(-0.981627005099017,0.,-0.190809912898503));
#101915=DIRECTION('center_axis',(-0.981627005099017,0.,-0.190809912898503));
#101916=DIRECTION('ref_axis',(-0.190809912898503,0.,0.981627005099017));
#101917=DIRECTION('',(0.,1.,0.));
#101918=DIRECTION('',(0.,1.,0.));
#101919=DIRECTION('center_axis',(0.,1.,0.));
#101920=DIRECTION('ref_axis',(1.,0.,0.));
#101921=DIRECTION('',(-0.190809912898503,0.,0.981627005099017));
#101922=DIRECTION('',(0.981627005099017,0.,0.190809912898503));
#101923=DIRECTION('',(-0.190809912898503,0.,0.981627005099017));
#101924=DIRECTION('',(0.981627005099017,0.,0.190809912898503));
#101925=DIRECTION('center_axis',(0.981627005099017,0.,0.190809912898503));
#101926=DIRECTION('ref_axis',(0.,-1.,0.));
#101927=DIRECTION('',(-0.190809912898503,0.,0.981627005099017));
#101928=DIRECTION('',(0.,-1.,0.));
#101929=DIRECTION('',(0.,-1.,0.));
#101930=DIRECTION('center_axis',(0.,-1.,0.));
#101931=DIRECTION('ref_axis',(0.,0.,-1.));
#101932=DIRECTION('',(-0.190809912898503,0.,0.981627005099017));
#101933=DIRECTION('',(-0.981627005099017,0.,-0.190809912898503));
#101934=DIRECTION('',(-0.981627005099017,0.,-0.190809912898503));
#101935=DIRECTION('center_axis',(-0.981627005099017,0.,-0.190809912898503));
#101936=DIRECTION('ref_axis',(-0.190809912898503,0.,0.981627005099017));
#101937=DIRECTION('',(0.,1.,0.));
#101938=DIRECTION('',(0.,1.,0.));
#101939=DIRECTION('center_axis',(0.,1.,0.));
#101940=DIRECTION('ref_axis',(1.,0.,0.));
#101941=DIRECTION('',(-0.190809912898503,0.,0.981627005099017));
#101942=DIRECTION('',(0.981627005099017,0.,0.190809912898503));
#101943=DIRECTION('',(-0.190809912898503,0.,0.981627005099017));
#101944=DIRECTION('',(0.981627005099017,0.,0.190809912898503));
#101945=DIRECTION('center_axis',(0.981627005099017,0.,0.190809912898503));
#101946=DIRECTION('ref_axis',(0.,-1.,0.));
#101947=DIRECTION('',(-0.190809912898503,0.,0.981627005099017));
#101948=DIRECTION('',(0.,-1.,0.));
#101949=DIRECTION('',(0.,-1.,0.));
#101950=DIRECTION('center_axis',(0.,-1.,0.));
#101951=DIRECTION('ref_axis',(0.,0.,-1.));
#101952=DIRECTION('',(-0.190809912898503,0.,0.981627005099017));
#101953=DIRECTION('',(-0.981627005099017,0.,-0.190809912898503));
#101954=DIRECTION('',(-0.981627005099017,0.,-0.190809912898503));
#101955=DIRECTION('center_axis',(-0.981627005099017,0.,-0.190809912898503));
#101956=DIRECTION('ref_axis',(-0.190809912898503,0.,0.981627005099017));
#101957=DIRECTION('',(0.,1.,0.));
#101958=DIRECTION('',(0.,1.,0.));
#101959=DIRECTION('center_axis',(0.,1.,0.));
#101960=DIRECTION('ref_axis',(1.,0.,0.));
#101961=DIRECTION('',(-0.190809912898503,0.,0.981627005099017));
#101962=DIRECTION('',(0.981627005099017,0.,0.190809912898503));
#101963=DIRECTION('',(-0.190809912898503,0.,0.981627005099017));
#101964=DIRECTION('',(0.981627005099017,0.,0.190809912898503));
#101965=DIRECTION('center_axis',(0.981627005099017,0.,0.190809912898503));
#101966=DIRECTION('ref_axis',(0.,-1.,0.));
#101967=DIRECTION('',(-0.190809912898503,0.,0.981627005099017));
#101968=DIRECTION('',(0.,-1.,0.));
#101969=DIRECTION('',(0.,-1.,0.));
#101970=DIRECTION('center_axis',(0.,-1.,0.));
#101971=DIRECTION('ref_axis',(0.,0.,-1.));
#101972=DIRECTION('',(-0.190809912898503,0.,0.981627005099017));
#101973=DIRECTION('',(-0.981627005099017,0.,-0.190809912898503));
#101974=DIRECTION('',(-0.981627005099017,0.,-0.190809912898503));
#101975=DIRECTION('center_axis',(-0.981627005099017,0.,-0.190809912898503));
#101976=DIRECTION('ref_axis',(-0.190809912898503,0.,0.981627005099017));
#101977=DIRECTION('',(0.,1.,0.));
#101978=DIRECTION('',(0.,1.,0.));
#101979=DIRECTION('center_axis',(0.,1.,0.));
#101980=DIRECTION('ref_axis',(1.,0.,0.));
#101981=DIRECTION('',(-0.190809912898503,0.,0.981627005099017));
#101982=DIRECTION('',(0.981627005099017,0.,0.190809912898503));
#101983=DIRECTION('',(-0.190809912898503,0.,0.981627005099017));
#101984=DIRECTION('',(0.981627005099017,0.,0.190809912898503));
#101985=DIRECTION('center_axis',(0.981627005099017,0.,0.190809912898503));
#101986=DIRECTION('ref_axis',(0.,-1.,0.));
#101987=DIRECTION('',(-0.190809912898503,0.,0.981627005099017));
#101988=DIRECTION('',(0.,-1.,0.));
#101989=DIRECTION('',(0.,-1.,0.));
#101990=DIRECTION('center_axis',(0.,-1.,0.));
#101991=DIRECTION('ref_axis',(0.,0.,-1.));
#101992=DIRECTION('',(-0.190809912898503,0.,0.981627005099017));
#101993=DIRECTION('',(-0.981627005099017,0.,-0.190809912898503));
#101994=DIRECTION('',(-0.981627005099017,0.,-0.190809912898503));
#101995=DIRECTION('center_axis',(-0.981627005099017,0.,-0.190809912898503));
#101996=DIRECTION('ref_axis',(-0.190809912898503,0.,0.981627005099017));
#101997=DIRECTION('',(0.,1.,0.));
#101998=DIRECTION('',(0.,1.,0.));
#101999=DIRECTION('center_axis',(0.,1.,0.));
#102000=DIRECTION('ref_axis',(1.,0.,0.));
#102001=DIRECTION('',(-0.190809912898503,0.,0.981627005099017));
#102002=DIRECTION('',(0.981627005099017,0.,0.190809912898503));
#102003=DIRECTION('',(-0.190809912898503,0.,0.981627005099017));
#102004=DIRECTION('',(0.981627005099017,0.,0.190809912898503));
#102005=DIRECTION('center_axis',(0.981627005099017,0.,0.190809912898503));
#102006=DIRECTION('ref_axis',(0.,-1.,0.));
#102007=DIRECTION('',(-0.190809912898503,0.,0.981627005099017));
#102008=DIRECTION('',(0.,-1.,0.));
#102009=DIRECTION('',(0.,-1.,0.));
#102010=DIRECTION('center_axis',(0.,-1.,0.));
#102011=DIRECTION('ref_axis',(0.,0.,-1.));
#102012=DIRECTION('',(-0.190809912898503,0.,0.981627005099017));
#102013=DIRECTION('',(-0.981627005099017,0.,-0.190809912898503));
#102014=DIRECTION('',(-0.981627005099017,0.,-0.190809912898503));
#102015=DIRECTION('center_axis',(-0.981627005099017,0.,-0.190809912898503));
#102016=DIRECTION('ref_axis',(-0.190809912898503,0.,0.981627005099017));
#102017=DIRECTION('',(0.,1.,0.));
#102018=DIRECTION('',(0.,1.,0.));
#102019=DIRECTION('center_axis',(0.,1.,0.));
#102020=DIRECTION('ref_axis',(1.,0.,0.));
#102021=DIRECTION('',(-0.190809912898503,0.,0.981627005099017));
#102022=DIRECTION('',(0.981627005099017,0.,0.190809912898503));
#102023=DIRECTION('',(-0.190809912898503,0.,0.981627005099017));
#102024=DIRECTION('',(0.981627005099017,0.,0.190809912898503));
#102025=DIRECTION('center_axis',(0.981627005099017,0.,0.190809912898503));
#102026=DIRECTION('ref_axis',(0.,-1.,0.));
#102027=DIRECTION('',(-0.190809912898503,0.,0.981627005099017));
#102028=DIRECTION('',(0.,-1.,0.));
#102029=DIRECTION('',(0.,-1.,0.));
#102030=DIRECTION('center_axis',(0.,-1.,0.));
#102031=DIRECTION('ref_axis',(0.,0.,-1.));
#102032=DIRECTION('',(-0.190809912898503,0.,0.981627005099017));
#102033=DIRECTION('',(-0.981627005099017,0.,-0.190809912898503));
#102034=DIRECTION('',(-0.981627005099017,0.,-0.190809912898503));
#102035=DIRECTION('center_axis',(-0.981627005099017,0.,-0.190809912898503));
#102036=DIRECTION('ref_axis',(-0.190809912898503,0.,0.981627005099017));
#102037=DIRECTION('',(0.,1.,0.));
#102038=DIRECTION('',(0.,1.,0.));
#102039=DIRECTION('center_axis',(0.,1.,0.));
#102040=DIRECTION('ref_axis',(1.,0.,0.));
#102041=DIRECTION('',(-0.190809912898503,0.,0.981627005099017));
#102042=DIRECTION('',(0.981627005099017,0.,0.190809912898503));
#102043=DIRECTION('',(-0.190809912898503,0.,0.981627005099017));
#102044=DIRECTION('',(0.981627005099017,0.,0.190809912898503));
#102045=DIRECTION('center_axis',(0.981627005099017,0.,0.190809912898503));
#102046=DIRECTION('ref_axis',(0.,-1.,0.));
#102047=DIRECTION('',(-0.190809912898503,0.,0.981627005099017));
#102048=DIRECTION('',(0.,-1.,0.));
#102049=DIRECTION('',(0.,-1.,0.));
#102050=DIRECTION('center_axis',(0.,-1.,0.));
#102051=DIRECTION('ref_axis',(0.,0.,-1.));
#102052=DIRECTION('',(-0.190809912898503,0.,0.981627005099017));
#102053=DIRECTION('',(-0.981627005099017,0.,-0.190809912898503));
#102054=DIRECTION('',(-0.981627005099017,0.,-0.190809912898503));
#102055=DIRECTION('center_axis',(-0.981627005099017,0.,-0.190809912898503));
#102056=DIRECTION('ref_axis',(-0.190809912898503,0.,0.981627005099017));
#102057=DIRECTION('',(0.,1.,0.));
#102058=DIRECTION('',(0.,1.,0.));
#102059=DIRECTION('center_axis',(0.,1.,0.));
#102060=DIRECTION('ref_axis',(1.,0.,0.));
#102061=DIRECTION('',(-0.190809912898503,0.,0.981627005099017));
#102062=DIRECTION('',(0.981627005099017,0.,0.190809912898503));
#102063=DIRECTION('',(-0.190809912898503,0.,0.981627005099017));
#102064=DIRECTION('',(0.981627005099017,0.,0.190809912898503));
#102065=DIRECTION('center_axis',(0.981627005099017,0.,0.190809912898503));
#102066=DIRECTION('ref_axis',(0.,-1.,0.));
#102067=DIRECTION('',(-0.190809912898503,0.,0.981627005099017));
#102068=DIRECTION('',(0.,-1.,0.));
#102069=DIRECTION('',(0.,-1.,0.));
#102070=DIRECTION('center_axis',(0.,-1.,0.));
#102071=DIRECTION('ref_axis',(0.,0.,-1.));
#102072=DIRECTION('',(-0.190809912898503,0.,0.981627005099017));
#102073=DIRECTION('',(-0.981627005099017,0.,-0.190809912898503));
#102074=DIRECTION('',(-0.981627005099017,0.,-0.190809912898503));
#102075=DIRECTION('center_axis',(-0.981627005099017,0.,-0.190809912898503));
#102076=DIRECTION('ref_axis',(-0.190809912898503,0.,0.981627005099017));
#102077=DIRECTION('',(0.,1.,0.));
#102078=DIRECTION('',(0.,1.,0.));
#102079=DIRECTION('center_axis',(0.,1.,0.));
#102080=DIRECTION('ref_axis',(1.,0.,0.));
#102081=DIRECTION('',(-0.190809912898503,0.,0.981627005099017));
#102082=DIRECTION('',(0.981627005099017,0.,0.190809912898503));
#102083=DIRECTION('',(-0.190809912898503,0.,0.981627005099017));
#102084=DIRECTION('',(0.981627005099017,0.,0.190809912898503));
#102085=DIRECTION('center_axis',(0.981627005099017,0.,0.190809912898503));
#102086=DIRECTION('ref_axis',(0.,-1.,0.));
#102087=DIRECTION('',(-0.190809912898503,0.,0.981627005099017));
#102088=DIRECTION('',(0.,-1.,0.));
#102089=DIRECTION('',(0.,-1.,0.));
#102090=DIRECTION('center_axis',(0.,-1.,0.));
#102091=DIRECTION('ref_axis',(0.,0.,-1.));
#102092=DIRECTION('',(-0.190809912898503,0.,0.981627005099017));
#102093=DIRECTION('',(-0.981627005099017,0.,-0.190809912898503));
#102094=DIRECTION('',(-0.981627005099017,0.,-0.190809912898503));
#102095=DIRECTION('center_axis',(-0.981627005099017,0.,-0.190809912898503));
#102096=DIRECTION('ref_axis',(-0.190809912898503,0.,0.981627005099017));
#102097=DIRECTION('',(0.,1.,0.));
#102098=DIRECTION('',(0.,1.,0.));
#102099=DIRECTION('center_axis',(0.,1.,0.));
#102100=DIRECTION('ref_axis',(1.,0.,0.));
#102101=DIRECTION('',(-0.190809912898503,0.,0.981627005099017));
#102102=DIRECTION('',(0.981627005099017,0.,0.190809912898503));
#102103=DIRECTION('',(-0.190809912898503,0.,0.981627005099017));
#102104=DIRECTION('',(0.981627005099017,0.,0.190809912898503));
#102105=DIRECTION('center_axis',(0.981627005099017,0.,0.190809912898503));
#102106=DIRECTION('ref_axis',(0.,-1.,0.));
#102107=DIRECTION('',(-0.190809912898503,0.,0.981627005099017));
#102108=DIRECTION('',(0.,-1.,0.));
#102109=DIRECTION('',(0.,-1.,0.));
#102110=DIRECTION('center_axis',(0.,-1.,0.));
#102111=DIRECTION('ref_axis',(0.,0.,-1.));
#102112=DIRECTION('',(-0.190809912898503,0.,0.981627005099017));
#102113=DIRECTION('',(-0.981627005099017,0.,-0.190809912898503));
#102114=DIRECTION('',(-0.981627005099017,0.,-0.190809912898503));
#102115=DIRECTION('center_axis',(-0.981627005099017,0.,-0.190809912898503));
#102116=DIRECTION('ref_axis',(-0.190809912898503,0.,0.981627005099017));
#102117=DIRECTION('',(0.,1.,0.));
#102118=DIRECTION('',(0.,1.,0.));
#102119=DIRECTION('center_axis',(0.,1.,0.));
#102120=DIRECTION('ref_axis',(1.,0.,0.));
#102121=DIRECTION('',(-0.190809912898503,0.,0.981627005099017));
#102122=DIRECTION('',(0.981627005099017,0.,0.190809912898503));
#102123=DIRECTION('',(-0.190809912898503,0.,0.981627005099017));
#102124=DIRECTION('',(0.981627005099017,0.,0.190809912898503));
#102125=DIRECTION('center_axis',(0.981627005099017,0.,0.190809912898503));
#102126=DIRECTION('ref_axis',(0.,-1.,0.));
#102127=DIRECTION('',(-0.190809912898503,0.,0.981627005099017));
#102128=DIRECTION('',(0.,-1.,0.));
#102129=DIRECTION('',(0.,-1.,0.));
#102130=DIRECTION('center_axis',(0.,-1.,0.));
#102131=DIRECTION('ref_axis',(0.,0.,-1.));
#102132=DIRECTION('',(-0.190809912898503,0.,0.981627005099017));
#102133=DIRECTION('',(-0.981627005099017,0.,-0.190809912898503));
#102134=DIRECTION('',(-0.981627005099017,0.,-0.190809912898503));
#102135=DIRECTION('center_axis',(-0.981627005099017,0.,-0.190809912898503));
#102136=DIRECTION('ref_axis',(-0.190809912898503,0.,0.981627005099017));
#102137=DIRECTION('',(0.,1.,0.));
#102138=DIRECTION('',(0.,1.,0.));
#102139=DIRECTION('center_axis',(0.,1.,0.));
#102140=DIRECTION('ref_axis',(1.,0.,0.));
#102141=DIRECTION('',(-0.190809912898503,0.,0.981627005099017));
#102142=DIRECTION('',(0.981627005099017,0.,0.190809912898503));
#102143=DIRECTION('',(-0.190809912898503,0.,0.981627005099017));
#102144=DIRECTION('',(0.981627005099017,0.,0.190809912898503));
#102145=DIRECTION('center_axis',(0.981627005099017,0.,0.190809912898503));
#102146=DIRECTION('ref_axis',(0.,-1.,0.));
#102147=DIRECTION('',(-0.190809912898503,0.,0.981627005099017));
#102148=DIRECTION('',(0.,-1.,0.));
#102149=DIRECTION('',(0.,-1.,0.));
#102150=DIRECTION('center_axis',(0.,-1.,0.));
#102151=DIRECTION('ref_axis',(0.,0.,-1.));
#102152=DIRECTION('',(-0.190809912898503,0.,0.981627005099017));
#102153=DIRECTION('',(-0.981627005099017,0.,-0.190809912898503));
#102154=DIRECTION('',(-0.981627005099017,0.,-0.190809912898503));
#102155=DIRECTION('center_axis',(-0.981627005099017,0.,-0.190809912898503));
#102156=DIRECTION('ref_axis',(-0.190809912898503,0.,0.981627005099017));
#102157=DIRECTION('',(0.,1.,0.));
#102158=DIRECTION('',(0.,1.,0.));
#102159=DIRECTION('center_axis',(0.,1.,0.));
#102160=DIRECTION('ref_axis',(1.,0.,0.));
#102161=DIRECTION('',(-0.190809912898503,0.,0.981627005099017));
#102162=DIRECTION('',(0.981627005099017,0.,0.190809912898503));
#102163=DIRECTION('',(-0.190809912898503,0.,0.981627005099017));
#102164=DIRECTION('',(0.981627005099017,0.,0.190809912898503));
#102165=DIRECTION('center_axis',(0.981627005099017,0.,0.190809912898503));
#102166=DIRECTION('ref_axis',(0.,-1.,0.));
#102167=DIRECTION('',(-0.190809912898503,0.,0.981627005099017));
#102168=DIRECTION('',(0.,-1.,0.));
#102169=DIRECTION('',(0.,-1.,0.));
#102170=DIRECTION('center_axis',(0.,-1.,0.));
#102171=DIRECTION('ref_axis',(0.,0.,-1.));
#102172=DIRECTION('',(-0.190809912898503,0.,0.981627005099017));
#102173=DIRECTION('',(-0.981627005099017,0.,-0.190809912898503));
#102174=DIRECTION('',(-0.981627005099017,0.,-0.190809912898503));
#102175=DIRECTION('center_axis',(-0.981627005099017,0.,-0.190809912898503));
#102176=DIRECTION('ref_axis',(-0.190809912898503,0.,0.981627005099017));
#102177=DIRECTION('',(0.,1.,0.));
#102178=DIRECTION('',(0.,1.,0.));
#102179=DIRECTION('center_axis',(0.,1.,0.));
#102180=DIRECTION('ref_axis',(1.,0.,0.));
#102181=DIRECTION('',(-0.190809912898503,0.,0.981627005099017));
#102182=DIRECTION('',(0.981627005099017,0.,0.190809912898503));
#102183=DIRECTION('',(-0.190809912898503,0.,0.981627005099017));
#102184=DIRECTION('',(0.981627005099017,0.,0.190809912898503));
#102185=DIRECTION('center_axis',(0.981627005099017,0.,0.190809912898503));
#102186=DIRECTION('ref_axis',(0.,-1.,0.));
#102187=DIRECTION('',(-0.190809912898503,0.,0.981627005099017));
#102188=DIRECTION('',(0.,-1.,0.));
#102189=DIRECTION('',(0.,-1.,0.));
#102190=DIRECTION('center_axis',(0.,-1.,0.));
#102191=DIRECTION('ref_axis',(0.,0.,-1.));
#102192=DIRECTION('',(-0.190809912898503,0.,0.981627005099017));
#102193=DIRECTION('',(-0.981627005099017,0.,-0.190809912898503));
#102194=DIRECTION('',(-0.981627005099017,0.,-0.190809912898503));
#102195=DIRECTION('center_axis',(-0.981627005099017,0.,-0.190809912898503));
#102196=DIRECTION('ref_axis',(-0.190809912898503,0.,0.981627005099017));
#102197=DIRECTION('',(0.,1.,0.));
#102198=DIRECTION('',(0.,1.,0.));
#102199=DIRECTION('center_axis',(0.,1.,0.));
#102200=DIRECTION('ref_axis',(1.,0.,0.));
#102201=DIRECTION('',(-0.190809912898503,0.,0.981627005099017));
#102202=DIRECTION('',(0.981627005099017,0.,0.190809912898503));
#102203=DIRECTION('',(-0.190809912898503,0.,0.981627005099017));
#102204=DIRECTION('',(0.981627005099017,0.,0.190809912898503));
#102205=DIRECTION('center_axis',(0.981627005099017,0.,0.190809912898503));
#102206=DIRECTION('ref_axis',(0.,-1.,0.));
#102207=DIRECTION('',(-0.190809912898503,0.,0.981627005099017));
#102208=DIRECTION('',(0.,-1.,0.));
#102209=DIRECTION('',(0.,-1.,0.));
#102210=DIRECTION('center_axis',(0.,-1.,0.));
#102211=DIRECTION('ref_axis',(0.,0.,-1.));
#102212=DIRECTION('',(-0.190809912898503,0.,0.981627005099017));
#102213=DIRECTION('',(-0.981627005099017,0.,-0.190809912898503));
#102214=DIRECTION('',(-0.981627005099017,0.,-0.190809912898503));
#102215=DIRECTION('center_axis',(-0.981627005099017,0.,-0.190809912898503));
#102216=DIRECTION('ref_axis',(-0.190809912898503,0.,0.981627005099017));
#102217=DIRECTION('',(0.,1.,0.));
#102218=DIRECTION('',(0.,1.,0.));
#102219=DIRECTION('center_axis',(0.,1.,0.));
#102220=DIRECTION('ref_axis',(1.,0.,0.));
#102221=DIRECTION('',(-0.190809912898503,0.,0.981627005099017));
#102222=DIRECTION('',(0.981627005099017,0.,0.190809912898503));
#102223=DIRECTION('',(-0.190809912898503,0.,0.981627005099017));
#102224=DIRECTION('',(0.981627005099017,0.,0.190809912898503));
#102225=DIRECTION('center_axis',(0.981627005099017,0.,0.190809912898503));
#102226=DIRECTION('ref_axis',(0.,-1.,0.));
#102227=DIRECTION('',(-0.190809912898503,0.,0.981627005099017));
#102228=DIRECTION('',(0.,-1.,0.));
#102229=DIRECTION('',(0.,-1.,0.));
#102230=DIRECTION('center_axis',(0.,-1.,0.));
#102231=DIRECTION('ref_axis',(0.,0.,-1.));
#102232=DIRECTION('',(-0.190809912898503,0.,0.981627005099017));
#102233=DIRECTION('',(-0.981627005099017,0.,-0.190809912898503));
#102234=DIRECTION('',(-0.981627005099017,0.,-0.190809912898503));
#102235=DIRECTION('center_axis',(-0.981627005099017,0.,-0.190809912898503));
#102236=DIRECTION('ref_axis',(-0.190809912898503,0.,0.981627005099017));
#102237=DIRECTION('',(0.,1.,0.));
#102238=DIRECTION('',(0.,1.,0.));
#102239=DIRECTION('center_axis',(0.,1.,0.));
#102240=DIRECTION('ref_axis',(1.,0.,0.));
#102241=DIRECTION('',(-0.190809912898503,0.,0.981627005099017));
#102242=DIRECTION('',(0.981627005099017,0.,0.190809912898503));
#102243=DIRECTION('',(-0.190809912898503,0.,0.981627005099017));
#102244=DIRECTION('',(0.981627005099017,0.,0.190809912898503));
#102245=DIRECTION('center_axis',(0.981627005099017,0.,0.190809912898503));
#102246=DIRECTION('ref_axis',(0.,-1.,0.));
#102247=DIRECTION('',(-0.190809912898503,0.,0.981627005099017));
#102248=DIRECTION('',(0.,-1.,0.));
#102249=DIRECTION('',(0.,-1.,0.));
#102250=DIRECTION('center_axis',(0.,-1.,0.));
#102251=DIRECTION('ref_axis',(0.,0.,-1.));
#102252=DIRECTION('',(-0.190809912898503,0.,0.981627005099017));
#102253=DIRECTION('',(-0.981627005099017,0.,-0.190809912898503));
#102254=DIRECTION('',(-0.981627005099017,0.,-0.190809912898503));
#102255=DIRECTION('center_axis',(-0.981627005099017,0.,-0.190809912898503));
#102256=DIRECTION('ref_axis',(-0.190809912898503,0.,0.981627005099017));
#102257=DIRECTION('',(0.,1.,0.));
#102258=DIRECTION('',(0.,1.,0.));
#102259=DIRECTION('center_axis',(0.,1.,0.));
#102260=DIRECTION('ref_axis',(1.,0.,0.));
#102261=DIRECTION('',(-0.190809912898503,0.,0.981627005099017));
#102262=DIRECTION('',(0.981627005099017,0.,0.190809912898503));
#102263=DIRECTION('',(-0.190809912898503,0.,0.981627005099017));
#102264=DIRECTION('',(0.981627005099017,0.,0.190809912898503));
#102265=DIRECTION('center_axis',(0.981627005099017,0.,0.190809912898503));
#102266=DIRECTION('ref_axis',(0.,-1.,0.));
#102267=DIRECTION('',(-0.190809912898503,0.,0.981627005099017));
#102268=DIRECTION('',(0.,-1.,0.));
#102269=DIRECTION('',(0.,-1.,0.));
#102270=DIRECTION('center_axis',(0.,-1.,0.));
#102271=DIRECTION('ref_axis',(0.,0.,-1.));
#102272=DIRECTION('',(-0.190809912898503,0.,0.981627005099017));
#102273=DIRECTION('',(-0.981627005099017,0.,-0.190809912898503));
#102274=DIRECTION('',(-0.981627005099017,0.,-0.190809912898503));
#102275=DIRECTION('center_axis',(-0.981627005099017,0.,-0.190809912898503));
#102276=DIRECTION('ref_axis',(-0.190809912898503,0.,0.981627005099017));
#102277=DIRECTION('',(0.,1.,0.));
#102278=DIRECTION('',(0.,1.,0.));
#102279=DIRECTION('center_axis',(0.,1.,0.));
#102280=DIRECTION('ref_axis',(1.,0.,0.));
#102281=DIRECTION('',(-0.190809912898503,0.,0.981627005099017));
#102282=DIRECTION('',(0.981627005099017,0.,0.190809912898503));
#102283=DIRECTION('',(-0.190809912898503,0.,0.981627005099017));
#102284=DIRECTION('',(0.981627005099017,0.,0.190809912898503));
#102285=DIRECTION('center_axis',(0.981627005099017,0.,0.190809912898503));
#102286=DIRECTION('ref_axis',(0.,-1.,0.));
#102287=DIRECTION('',(-0.190809912898503,0.,0.981627005099017));
#102288=DIRECTION('',(0.,-1.,0.));
#102289=DIRECTION('',(0.,-1.,0.));
#102290=DIRECTION('center_axis',(0.,-1.,0.));
#102291=DIRECTION('ref_axis',(0.,0.,-1.));
#102292=DIRECTION('',(-0.190809912898503,0.,0.981627005099017));
#102293=DIRECTION('',(-0.981627005099017,0.,-0.190809912898503));
#102294=DIRECTION('',(-0.981627005099017,0.,-0.190809912898503));
#102295=DIRECTION('center_axis',(-0.981627005099017,0.,-0.190809912898503));
#102296=DIRECTION('ref_axis',(-0.190809912898503,0.,0.981627005099017));
#102297=DIRECTION('',(0.,1.,0.));
#102298=DIRECTION('',(0.,1.,0.));
#102299=DIRECTION('center_axis',(0.,1.,0.));
#102300=DIRECTION('ref_axis',(1.,0.,0.));
#102301=DIRECTION('',(-0.190809912898503,0.,0.981627005099017));
#102302=DIRECTION('',(0.981627005099017,0.,0.190809912898503));
#102303=DIRECTION('',(-0.190809912898503,0.,0.981627005099017));
#102304=DIRECTION('',(0.981627005099017,0.,0.190809912898503));
#102305=DIRECTION('center_axis',(0.981627005099017,0.,0.190809912898503));
#102306=DIRECTION('ref_axis',(0.,-1.,0.));
#102307=DIRECTION('',(-0.190809912898503,0.,0.981627005099017));
#102308=DIRECTION('',(0.,-1.,0.));
#102309=DIRECTION('',(0.,-1.,0.));
#102310=DIRECTION('center_axis',(0.,-1.,0.));
#102311=DIRECTION('ref_axis',(0.,0.,-1.));
#102312=DIRECTION('',(-0.190809912898503,0.,0.981627005099017));
#102313=DIRECTION('',(-0.981627005099017,0.,-0.190809912898503));
#102314=DIRECTION('',(-0.981627005099017,0.,-0.190809912898503));
#102315=DIRECTION('center_axis',(-0.981627005099017,0.,-0.190809912898503));
#102316=DIRECTION('ref_axis',(-0.190809912898503,0.,0.981627005099017));
#102317=DIRECTION('',(0.,1.,0.));
#102318=DIRECTION('',(0.,1.,0.));
#102319=DIRECTION('center_axis',(0.,1.,0.));
#102320=DIRECTION('ref_axis',(1.,0.,0.));
#102321=DIRECTION('',(-0.190809912898503,0.,0.981627005099017));
#102322=DIRECTION('',(0.981627005099017,0.,0.190809912898503));
#102323=DIRECTION('',(-0.190809912898503,0.,0.981627005099017));
#102324=DIRECTION('',(0.981627005099017,0.,0.190809912898503));
#102325=DIRECTION('center_axis',(0.981627005099017,0.,0.190809912898503));
#102326=DIRECTION('ref_axis',(0.,-1.,0.));
#102327=DIRECTION('',(-0.190809912898503,0.,0.981627005099017));
#102328=DIRECTION('',(0.,-1.,0.));
#102329=DIRECTION('',(0.,-1.,0.));
#102330=DIRECTION('center_axis',(0.,-1.,0.));
#102331=DIRECTION('ref_axis',(0.,0.,-1.));
#102332=DIRECTION('',(-0.190809912898503,0.,0.981627005099017));
#102333=DIRECTION('',(-0.981627005099017,0.,-0.190809912898503));
#102334=DIRECTION('',(-0.981627005099017,0.,-0.190809912898503));
#102335=DIRECTION('center_axis',(-0.981627005099017,0.,-0.190809912898503));
#102336=DIRECTION('ref_axis',(-0.190809912898503,0.,0.981627005099017));
#102337=DIRECTION('',(0.,1.,0.));
#102338=DIRECTION('',(0.,1.,0.));
#102339=DIRECTION('center_axis',(0.,1.,0.));
#102340=DIRECTION('ref_axis',(1.,0.,0.));
#102341=DIRECTION('',(-0.190809912898503,0.,0.981627005099017));
#102342=DIRECTION('',(0.981627005099017,0.,0.190809912898503));
#102343=DIRECTION('',(-0.190809912898503,0.,0.981627005099017));
#102344=DIRECTION('',(0.981627005099017,0.,0.190809912898503));
#102345=DIRECTION('center_axis',(0.981627005099017,0.,0.190809912898503));
#102346=DIRECTION('ref_axis',(0.,-1.,0.));
#102347=DIRECTION('',(-0.190809912898503,0.,0.981627005099017));
#102348=DIRECTION('',(0.,-1.,0.));
#102349=DIRECTION('',(0.,-1.,0.));
#102350=DIRECTION('center_axis',(0.,-1.,0.));
#102351=DIRECTION('ref_axis',(0.,0.,-1.));
#102352=DIRECTION('',(-0.190809912898503,0.,0.981627005099017));
#102353=DIRECTION('',(-0.981627005099017,0.,-0.190809912898503));
#102354=DIRECTION('',(-0.981627005099017,0.,-0.190809912898503));
#102355=DIRECTION('center_axis',(-0.981627005099017,0.,-0.190809912898503));
#102356=DIRECTION('ref_axis',(-0.190809912898503,0.,0.981627005099017));
#102357=DIRECTION('',(0.,1.,0.));
#102358=DIRECTION('',(0.,1.,0.));
#102359=DIRECTION('center_axis',(0.,1.,0.));
#102360=DIRECTION('ref_axis',(1.,0.,0.));
#102361=DIRECTION('',(-0.190809912898503,0.,0.981627005099017));
#102362=DIRECTION('',(0.981627005099017,0.,0.190809912898503));
#102363=DIRECTION('',(-0.190809912898503,0.,0.981627005099017));
#102364=DIRECTION('',(0.981627005099017,0.,0.190809912898503));
#102365=DIRECTION('center_axis',(0.981627005099017,0.,0.190809912898503));
#102366=DIRECTION('ref_axis',(0.,-1.,0.));
#102367=DIRECTION('',(-0.190809912898503,0.,0.981627005099017));
#102368=DIRECTION('',(0.,-1.,0.));
#102369=DIRECTION('',(0.,-1.,0.));
#102370=DIRECTION('center_axis',(0.,-1.,0.));
#102371=DIRECTION('ref_axis',(0.,0.,-1.));
#102372=DIRECTION('',(-0.190809912898503,0.,0.981627005099017));
#102373=DIRECTION('',(-0.981627005099017,0.,-0.190809912898503));
#102374=DIRECTION('',(-0.981627005099017,0.,-0.190809912898503));
#102375=DIRECTION('center_axis',(-0.981627005099017,0.,-0.190809912898503));
#102376=DIRECTION('ref_axis',(-0.190809912898503,0.,0.981627005099017));
#102377=DIRECTION('',(0.,1.,0.));
#102378=DIRECTION('',(0.,1.,0.));
#102379=DIRECTION('center_axis',(0.,1.,0.));
#102380=DIRECTION('ref_axis',(1.,0.,0.));
#102381=DIRECTION('',(-0.190809912898503,0.,0.981627005099017));
#102382=DIRECTION('',(0.981627005099017,0.,0.190809912898503));
#102383=DIRECTION('',(-0.190809912898503,0.,0.981627005099017));
#102384=DIRECTION('',(0.981627005099017,0.,0.190809912898503));
#102385=DIRECTION('center_axis',(0.981627005099017,0.,0.190809912898503));
#102386=DIRECTION('ref_axis',(0.,-1.,0.));
#102387=DIRECTION('',(-0.190809912898503,0.,0.981627005099017));
#102388=DIRECTION('',(0.,-1.,0.));
#102389=DIRECTION('',(0.,-1.,0.));
#102390=DIRECTION('center_axis',(0.,-1.,0.));
#102391=DIRECTION('ref_axis',(0.,0.,-1.));
#102392=DIRECTION('',(-0.190809912898503,0.,0.981627005099017));
#102393=DIRECTION('',(-0.981627005099017,0.,-0.190809912898503));
#102394=DIRECTION('',(-0.981627005099017,0.,-0.190809912898503));
#102395=DIRECTION('center_axis',(-0.981627005099017,0.,-0.190809912898503));
#102396=DIRECTION('ref_axis',(-0.190809912898503,0.,0.981627005099017));
#102397=DIRECTION('',(0.,1.,0.));
#102398=DIRECTION('',(0.,1.,0.));
#102399=DIRECTION('center_axis',(0.,1.,0.));
#102400=DIRECTION('ref_axis',(1.,0.,0.));
#102401=DIRECTION('',(-0.190809912898503,0.,0.981627005099017));
#102402=DIRECTION('',(0.981627005099017,0.,0.190809912898503));
#102403=DIRECTION('',(-0.190809912898503,0.,0.981627005099017));
#102404=DIRECTION('',(0.981627005099017,0.,0.190809912898503));
#102405=DIRECTION('center_axis',(0.981627005099017,0.,0.190809912898503));
#102406=DIRECTION('ref_axis',(0.,-1.,0.));
#102407=DIRECTION('',(-0.190809912898503,0.,0.981627005099017));
#102408=DIRECTION('',(0.,-1.,0.));
#102409=DIRECTION('',(0.,-1.,0.));
#102410=DIRECTION('center_axis',(0.,-1.,0.));
#102411=DIRECTION('ref_axis',(0.,0.,-1.));
#102412=DIRECTION('',(-0.190809912898503,0.,0.981627005099017));
#102413=DIRECTION('',(-0.981627005099017,0.,-0.190809912898503));
#102414=DIRECTION('',(-0.981627005099017,0.,-0.190809912898503));
#102415=DIRECTION('center_axis',(-0.981627005099017,0.,-0.190809912898503));
#102416=DIRECTION('ref_axis',(-0.190809912898503,0.,0.981627005099017));
#102417=DIRECTION('',(0.,1.,0.));
#102418=DIRECTION('',(0.,1.,0.));
#102419=DIRECTION('center_axis',(0.,1.,0.));
#102420=DIRECTION('ref_axis',(1.,0.,0.));
#102421=DIRECTION('',(-0.190809912898503,0.,0.981627005099017));
#102422=DIRECTION('',(0.981627005099017,0.,0.190809912898503));
#102423=DIRECTION('',(-0.190809912898503,0.,0.981627005099017));
#102424=DIRECTION('',(0.981627005099017,0.,0.190809912898503));
#102425=DIRECTION('center_axis',(0.981627005099017,0.,0.190809912898503));
#102426=DIRECTION('ref_axis',(0.,-1.,0.));
#102427=DIRECTION('',(-0.190809912898503,0.,0.981627005099017));
#102428=DIRECTION('',(0.,-1.,0.));
#102429=DIRECTION('',(0.,-1.,0.));
#102430=DIRECTION('center_axis',(0.,-1.,0.));
#102431=DIRECTION('ref_axis',(0.,0.,-1.));
#102432=DIRECTION('',(-0.190809912898503,0.,0.981627005099017));
#102433=DIRECTION('',(-0.981627005099017,0.,-0.190809912898503));
#102434=DIRECTION('',(-0.981627005099017,0.,-0.190809912898503));
#102435=DIRECTION('center_axis',(-0.981627005099017,0.,-0.190809912898503));
#102436=DIRECTION('ref_axis',(-0.190809912898503,0.,0.981627005099017));
#102437=DIRECTION('',(0.,1.,0.));
#102438=DIRECTION('',(0.,1.,0.));
#102439=DIRECTION('center_axis',(0.,1.,0.));
#102440=DIRECTION('ref_axis',(1.,0.,0.));
#102441=DIRECTION('',(-0.190809912898503,0.,0.981627005099017));
#102442=DIRECTION('',(0.981627005099017,0.,0.190809912898503));
#102443=DIRECTION('',(-0.190809912898503,0.,0.981627005099017));
#102444=DIRECTION('',(0.981627005099017,0.,0.190809912898503));
#102445=DIRECTION('center_axis',(0.981627005099017,0.,0.190809912898503));
#102446=DIRECTION('ref_axis',(0.,-1.,0.));
#102447=DIRECTION('',(-0.190809912898503,0.,0.981627005099017));
#102448=DIRECTION('',(0.,-1.,0.));
#102449=DIRECTION('',(0.,-1.,0.));
#102450=DIRECTION('center_axis',(0.,-1.,0.));
#102451=DIRECTION('ref_axis',(0.,0.,-1.));
#102452=DIRECTION('',(-0.190809912898503,0.,0.981627005099017));
#102453=DIRECTION('',(-0.981627005099017,0.,-0.190809912898503));
#102454=DIRECTION('',(-0.981627005099017,0.,-0.190809912898503));
#102455=DIRECTION('center_axis',(-0.981627005099017,0.,-0.190809912898503));
#102456=DIRECTION('ref_axis',(-0.190809912898503,0.,0.981627005099017));
#102457=DIRECTION('',(0.,1.,0.));
#102458=DIRECTION('',(0.,1.,0.));
#102459=DIRECTION('center_axis',(0.,1.,0.));
#102460=DIRECTION('ref_axis',(1.,0.,0.));
#102461=DIRECTION('',(-0.190809912898503,0.,0.981627005099017));
#102462=DIRECTION('',(0.981627005099017,0.,0.190809912898503));
#102463=DIRECTION('',(-0.190809912898503,0.,0.981627005099017));
#102464=DIRECTION('',(0.981627005099017,0.,0.190809912898503));
#102465=DIRECTION('center_axis',(0.981627005099017,0.,0.190809912898503));
#102466=DIRECTION('ref_axis',(0.,-1.,0.));
#102467=DIRECTION('',(-0.190809912898503,0.,0.981627005099017));
#102468=DIRECTION('',(0.,-1.,0.));
#102469=DIRECTION('',(0.,-1.,0.));
#102470=DIRECTION('center_axis',(0.,-1.,0.));
#102471=DIRECTION('ref_axis',(0.,0.,-1.));
#102472=DIRECTION('',(-0.190809912898503,0.,0.981627005099017));
#102473=DIRECTION('',(-0.981627005099017,0.,-0.190809912898503));
#102474=DIRECTION('',(-0.981627005099017,0.,-0.190809912898503));
#102475=DIRECTION('center_axis',(-0.981627005099017,0.,-0.190809912898503));
#102476=DIRECTION('ref_axis',(-0.190809912898503,0.,0.981627005099017));
#102477=DIRECTION('',(0.,1.,0.));
#102478=DIRECTION('',(0.,1.,0.));
#102479=DIRECTION('center_axis',(0.,1.,0.));
#102480=DIRECTION('ref_axis',(1.,0.,0.));
#102481=DIRECTION('',(-0.190809912898503,0.,0.981627005099017));
#102482=DIRECTION('',(0.981627005099017,0.,0.190809912898503));
#102483=DIRECTION('',(-0.190809912898503,0.,0.981627005099017));
#102484=DIRECTION('',(0.981627005099017,0.,0.190809912898503));
#102485=DIRECTION('center_axis',(0.981627005099017,0.,0.190809912898503));
#102486=DIRECTION('ref_axis',(0.,-1.,0.));
#102487=DIRECTION('',(-0.190809912898503,0.,0.981627005099017));
#102488=DIRECTION('',(0.,-1.,0.));
#102489=DIRECTION('',(0.,-1.,0.));
#102490=DIRECTION('center_axis',(0.,-1.,0.));
#102491=DIRECTION('ref_axis',(0.,0.,-1.));
#102492=DIRECTION('',(-0.190809912898503,0.,0.981627005099017));
#102493=DIRECTION('',(-0.981627005099017,0.,-0.190809912898503));
#102494=DIRECTION('',(-0.981627005099017,0.,-0.190809912898503));
#102495=DIRECTION('center_axis',(-0.981627005099017,0.,-0.190809912898503));
#102496=DIRECTION('ref_axis',(-0.190809912898503,0.,0.981627005099017));
#102497=DIRECTION('',(0.,1.,0.));
#102498=DIRECTION('',(0.,1.,0.));
#102499=DIRECTION('center_axis',(0.,1.,0.));
#102500=DIRECTION('ref_axis',(1.,0.,0.));
#102501=DIRECTION('',(-0.190809912898503,0.,0.981627005099017));
#102502=DIRECTION('',(0.981627005099017,0.,0.190809912898503));
#102503=DIRECTION('',(-0.190809912898503,0.,0.981627005099017));
#102504=DIRECTION('',(0.981627005099017,0.,0.190809912898503));
#102505=DIRECTION('center_axis',(0.981627005099017,0.,0.190809912898503));
#102506=DIRECTION('ref_axis',(0.,-1.,0.));
#102507=DIRECTION('',(-0.190809912898503,0.,0.981627005099017));
#102508=DIRECTION('',(0.,-1.,0.));
#102509=DIRECTION('',(0.,-1.,0.));
#102510=DIRECTION('center_axis',(0.,-1.,0.));
#102511=DIRECTION('ref_axis',(0.,0.,-1.));
#102512=DIRECTION('',(-0.190809912898503,0.,0.981627005099017));
#102513=DIRECTION('',(-0.981627005099017,0.,-0.190809912898503));
#102514=DIRECTION('',(-0.981627005099017,0.,-0.190809912898503));
#102515=DIRECTION('center_axis',(-0.981627005099017,0.,-0.190809912898503));
#102516=DIRECTION('ref_axis',(-0.190809912898503,0.,0.981627005099017));
#102517=DIRECTION('',(0.,1.,0.));
#102518=DIRECTION('',(0.,1.,0.));
#102519=DIRECTION('center_axis',(0.,1.,0.));
#102520=DIRECTION('ref_axis',(1.,0.,0.));
#102521=DIRECTION('',(-0.190809912898503,0.,0.981627005099017));
#102522=DIRECTION('',(0.981627005099017,0.,0.190809912898503));
#102523=DIRECTION('',(-0.190809912898503,0.,0.981627005099017));
#102524=DIRECTION('',(0.981627005099017,0.,0.190809912898503));
#102525=DIRECTION('center_axis',(0.981627005099017,0.,0.190809912898503));
#102526=DIRECTION('ref_axis',(0.,-1.,0.));
#102527=DIRECTION('',(-0.190809912898503,0.,0.981627005099017));
#102528=DIRECTION('',(0.,-1.,0.));
#102529=DIRECTION('',(0.,-1.,0.));
#102530=DIRECTION('center_axis',(0.,-1.,0.));
#102531=DIRECTION('ref_axis',(0.,0.,-1.));
#102532=DIRECTION('',(-0.190809912898503,0.,0.981627005099017));
#102533=DIRECTION('',(-0.981627005099017,0.,-0.190809912898503));
#102534=DIRECTION('',(-0.981627005099017,0.,-0.190809912898503));
#102535=DIRECTION('center_axis',(-0.981627005099017,0.,-0.190809912898503));
#102536=DIRECTION('ref_axis',(-0.190809912898503,0.,0.981627005099017));
#102537=DIRECTION('',(0.,1.,0.));
#102538=DIRECTION('',(0.,1.,0.));
#102539=DIRECTION('center_axis',(0.,1.,0.));
#102540=DIRECTION('ref_axis',(1.,0.,0.));
#102541=DIRECTION('',(-0.190809912898503,0.,0.981627005099017));
#102542=DIRECTION('',(0.981627005099017,0.,0.190809912898503));
#102543=DIRECTION('',(-0.190809912898503,0.,0.981627005099017));
#102544=DIRECTION('',(0.981627005099017,0.,0.190809912898503));
#102545=DIRECTION('center_axis',(0.981627005099017,0.,0.190809912898503));
#102546=DIRECTION('ref_axis',(0.,-1.,0.));
#102547=DIRECTION('',(-0.190809912898503,0.,0.981627005099017));
#102548=DIRECTION('',(0.,-1.,0.));
#102549=DIRECTION('',(0.,-1.,0.));
#102550=DIRECTION('center_axis',(0.,-1.,0.));
#102551=DIRECTION('ref_axis',(0.,0.,-1.));
#102552=DIRECTION('',(-0.190809912898503,0.,0.981627005099017));
#102553=DIRECTION('',(-0.981627005099017,0.,-0.190809912898503));
#102554=DIRECTION('',(-0.981627005099017,0.,-0.190809912898503));
#102555=DIRECTION('center_axis',(-0.981627005099017,0.,-0.190809912898503));
#102556=DIRECTION('ref_axis',(-0.190809912898503,0.,0.981627005099017));
#102557=DIRECTION('',(0.,1.,0.));
#102558=DIRECTION('',(0.,1.,0.));
#102559=DIRECTION('center_axis',(0.,1.,0.));
#102560=DIRECTION('ref_axis',(1.,0.,0.));
#102561=DIRECTION('',(-0.190809912898503,0.,0.981627005099017));
#102562=DIRECTION('',(0.981627005099017,0.,0.190809912898503));
#102563=DIRECTION('',(-0.190809912898503,0.,0.981627005099017));
#102564=DIRECTION('',(0.981627005099017,0.,0.190809912898503));
#102565=DIRECTION('center_axis',(0.981627005099017,0.,0.190809912898503));
#102566=DIRECTION('ref_axis',(0.,-1.,0.));
#102567=DIRECTION('',(-0.190809912898503,0.,0.981627005099017));
#102568=DIRECTION('',(0.,-1.,0.));
#102569=DIRECTION('',(0.,-1.,0.));
#102570=DIRECTION('center_axis',(0.,-1.,0.));
#102571=DIRECTION('ref_axis',(0.,0.,-1.));
#102572=DIRECTION('',(-0.190809912898503,0.,0.981627005099017));
#102573=DIRECTION('',(-0.981627005099017,0.,-0.190809912898503));
#102574=DIRECTION('',(-0.981627005099017,0.,-0.190809912898503));
#102575=DIRECTION('center_axis',(-0.981627005099017,0.,-0.190809912898503));
#102576=DIRECTION('ref_axis',(-0.190809912898503,0.,0.981627005099017));
#102577=DIRECTION('',(0.,1.,0.));
#102578=DIRECTION('',(0.,1.,0.));
#102579=DIRECTION('center_axis',(0.,1.,0.));
#102580=DIRECTION('ref_axis',(1.,0.,0.));
#102581=DIRECTION('',(-0.190809912898503,0.,0.981627005099017));
#102582=DIRECTION('',(0.981627005099017,0.,0.190809912898503));
#102583=DIRECTION('',(-0.190809912898503,0.,0.981627005099017));
#102584=DIRECTION('',(0.981627005099017,0.,0.190809912898503));
#102585=DIRECTION('center_axis',(0.981627005099017,0.,0.190809912898503));
#102586=DIRECTION('ref_axis',(0.,-1.,0.));
#102587=DIRECTION('',(-0.190809912898503,0.,0.981627005099017));
#102588=DIRECTION('',(0.,-1.,0.));
#102589=DIRECTION('',(0.,-1.,0.));
#102590=DIRECTION('center_axis',(0.,-1.,0.));
#102591=DIRECTION('ref_axis',(0.,0.,-1.));
#102592=DIRECTION('',(-0.190809912898503,0.,0.981627005099017));
#102593=DIRECTION('',(-0.981627005099017,0.,-0.190809912898503));
#102594=DIRECTION('',(-0.981627005099017,0.,-0.190809912898503));
#102595=DIRECTION('center_axis',(-0.981627005099017,0.,-0.190809912898503));
#102596=DIRECTION('ref_axis',(-0.190809912898503,0.,0.981627005099017));
#102597=DIRECTION('',(0.,1.,0.));
#102598=DIRECTION('',(0.,1.,0.));
#102599=DIRECTION('center_axis',(0.,1.,0.));
#102600=DIRECTION('ref_axis',(1.,0.,0.));
#102601=DIRECTION('',(-0.190809912898503,0.,0.981627005099017));
#102602=DIRECTION('',(0.981627005099017,0.,0.190809912898503));
#102603=DIRECTION('',(-0.190809912898503,0.,0.981627005099017));
#102604=DIRECTION('',(0.981627005099017,0.,0.190809912898503));
#102605=DIRECTION('center_axis',(0.981627005099017,0.,0.190809912898503));
#102606=DIRECTION('ref_axis',(0.,-1.,0.));
#102607=DIRECTION('',(-0.190809912898503,0.,0.981627005099017));
#102608=DIRECTION('',(0.,-1.,0.));
#102609=DIRECTION('',(0.,-1.,0.));
#102610=DIRECTION('center_axis',(0.,-1.,0.));
#102611=DIRECTION('ref_axis',(0.,0.,-1.));
#102612=DIRECTION('',(-0.190809912898503,0.,0.981627005099017));
#102613=DIRECTION('',(-0.981627005099017,0.,-0.190809912898503));
#102614=DIRECTION('',(-0.981627005099017,0.,-0.190809912898503));
#102615=DIRECTION('center_axis',(-0.981627005099017,0.,-0.190809912898503));
#102616=DIRECTION('ref_axis',(-0.190809912898503,0.,0.981627005099017));
#102617=DIRECTION('',(0.,1.,0.));
#102618=DIRECTION('',(0.,1.,0.));
#102619=DIRECTION('center_axis',(0.,1.,0.));
#102620=DIRECTION('ref_axis',(1.,0.,0.));
#102621=DIRECTION('',(-0.190809912898503,0.,0.981627005099017));
#102622=DIRECTION('',(0.981627005099017,0.,0.190809912898503));
#102623=DIRECTION('',(-0.190809912898503,0.,0.981627005099017));
#102624=DIRECTION('',(0.981627005099017,0.,0.190809912898503));
#102625=DIRECTION('center_axis',(0.981627005099017,0.,0.190809912898503));
#102626=DIRECTION('ref_axis',(0.,-1.,0.));
#102627=DIRECTION('',(-0.190809912898503,0.,0.981627005099017));
#102628=DIRECTION('',(0.,-1.,0.));
#102629=DIRECTION('',(0.,-1.,0.));
#102630=DIRECTION('center_axis',(0.,-1.,0.));
#102631=DIRECTION('ref_axis',(0.,0.,-1.));
#102632=DIRECTION('',(-0.190809912898503,0.,0.981627005099017));
#102633=DIRECTION('',(-0.981627005099017,0.,-0.190809912898503));
#102634=DIRECTION('',(-0.981627005099017,0.,-0.190809912898503));
#102635=DIRECTION('center_axis',(-0.981627005099017,0.,-0.190809912898503));
#102636=DIRECTION('ref_axis',(-0.190809912898503,0.,0.981627005099017));
#102637=DIRECTION('',(0.,1.,0.));
#102638=DIRECTION('',(0.,1.,0.));
#102639=DIRECTION('center_axis',(0.,1.,0.));
#102640=DIRECTION('ref_axis',(1.,0.,0.));
#102641=DIRECTION('',(-0.190809912898503,0.,0.981627005099017));
#102642=DIRECTION('',(0.981627005099017,0.,0.190809912898503));
#102643=DIRECTION('',(-0.190809912898503,0.,0.981627005099017));
#102644=DIRECTION('',(0.981627005099017,0.,0.190809912898503));
#102645=DIRECTION('center_axis',(0.981627005099017,0.,0.190809912898503));
#102646=DIRECTION('ref_axis',(0.,-1.,0.));
#102647=DIRECTION('',(-0.190809912898503,0.,0.981627005099017));
#102648=DIRECTION('',(0.,-1.,0.));
#102649=DIRECTION('',(0.,-1.,0.));
#102650=DIRECTION('center_axis',(0.,-1.,0.));
#102651=DIRECTION('ref_axis',(0.,0.,-1.));
#102652=DIRECTION('',(-0.190809912898503,0.,0.981627005099017));
#102653=DIRECTION('',(-0.981627005099017,0.,-0.190809912898503));
#102654=DIRECTION('',(-0.981627005099017,0.,-0.190809912898503));
#102655=DIRECTION('center_axis',(-0.981627005099017,0.,-0.190809912898503));
#102656=DIRECTION('ref_axis',(-0.190809912898503,0.,0.981627005099017));
#102657=DIRECTION('',(0.,1.,0.));
#102658=DIRECTION('',(0.,1.,0.));
#102659=DIRECTION('center_axis',(0.,1.,0.));
#102660=DIRECTION('ref_axis',(1.,0.,0.));
#102661=DIRECTION('',(-0.190809912898503,0.,0.981627005099017));
#102662=DIRECTION('',(0.981627005099017,0.,0.190809912898503));
#102663=DIRECTION('',(-0.190809912898503,0.,0.981627005099017));
#102664=DIRECTION('',(0.981627005099017,0.,0.190809912898503));
#102665=DIRECTION('center_axis',(0.981627005099017,0.,0.190809912898503));
#102666=DIRECTION('ref_axis',(0.,-1.,0.));
#102667=DIRECTION('',(-0.190809912898503,0.,0.981627005099017));
#102668=DIRECTION('',(0.,-1.,0.));
#102669=DIRECTION('',(0.,-1.,0.));
#102670=DIRECTION('center_axis',(0.,-1.,0.));
#102671=DIRECTION('ref_axis',(0.,0.,-1.));
#102672=DIRECTION('',(-0.190809912898503,0.,0.981627005099017));
#102673=DIRECTION('',(-0.981627005099017,0.,-0.190809912898503));
#102674=DIRECTION('',(-0.981627005099017,0.,-0.190809912898503));
#102675=DIRECTION('center_axis',(-0.981627005099017,0.,-0.190809912898503));
#102676=DIRECTION('ref_axis',(-0.190809912898503,0.,0.981627005099017));
#102677=DIRECTION('',(0.,1.,0.));
#102678=DIRECTION('',(0.,1.,0.));
#102679=DIRECTION('center_axis',(0.,1.,0.));
#102680=DIRECTION('ref_axis',(1.,0.,0.));
#102681=DIRECTION('',(-0.190809912898503,0.,0.981627005099017));
#102682=DIRECTION('',(0.981627005099017,0.,0.190809912898503));
#102683=DIRECTION('',(-0.190809912898503,0.,0.981627005099017));
#102684=DIRECTION('',(0.981627005099017,0.,0.190809912898503));
#102685=DIRECTION('center_axis',(0.981627005099017,0.,0.190809912898503));
#102686=DIRECTION('ref_axis',(0.,-1.,0.));
#102687=DIRECTION('',(-0.190809912898503,0.,0.981627005099017));
#102688=DIRECTION('',(0.,-1.,0.));
#102689=DIRECTION('',(0.,-1.,0.));
#102690=DIRECTION('center_axis',(0.,-1.,0.));
#102691=DIRECTION('ref_axis',(0.,0.,-1.));
#102692=DIRECTION('',(-0.190809912898503,0.,0.981627005099017));
#102693=DIRECTION('',(-0.981627005099017,0.,-0.190809912898503));
#102694=DIRECTION('',(-0.981627005099017,0.,-0.190809912898503));
#102695=DIRECTION('center_axis',(-0.981627005099017,0.,-0.190809912898503));
#102696=DIRECTION('ref_axis',(-0.190809912898503,0.,0.981627005099017));
#102697=DIRECTION('',(0.,1.,0.));
#102698=DIRECTION('',(0.,1.,0.));
#102699=DIRECTION('center_axis',(0.,1.,0.));
#102700=DIRECTION('ref_axis',(1.,0.,0.));
#102701=DIRECTION('',(-0.190809912898503,0.,0.981627005099017));
#102702=DIRECTION('',(0.981627005099017,0.,0.190809912898503));
#102703=DIRECTION('',(-0.190809912898503,0.,0.981627005099017));
#102704=DIRECTION('',(0.981627005099017,0.,0.190809912898503));
#102705=DIRECTION('center_axis',(0.981627005099017,0.,0.190809912898503));
#102706=DIRECTION('ref_axis',(0.,-1.,0.));
#102707=DIRECTION('',(-0.190809912898503,0.,0.981627005099017));
#102708=DIRECTION('',(0.,-1.,0.));
#102709=DIRECTION('',(0.,-1.,0.));
#102710=DIRECTION('center_axis',(0.,-1.,0.));
#102711=DIRECTION('ref_axis',(0.,0.,-1.));
#102712=DIRECTION('',(-0.190809912898503,0.,0.981627005099017));
#102713=DIRECTION('',(-0.981627005099017,0.,-0.190809912898503));
#102714=DIRECTION('',(-0.981627005099017,0.,-0.190809912898503));
#102715=DIRECTION('center_axis',(-0.981627005099017,0.,-0.190809912898503));
#102716=DIRECTION('ref_axis',(-0.190809912898503,0.,0.981627005099017));
#102717=DIRECTION('',(0.,1.,0.));
#102718=DIRECTION('',(0.,1.,0.));
#102719=DIRECTION('center_axis',(0.,1.,0.));
#102720=DIRECTION('ref_axis',(1.,0.,0.));
#102721=DIRECTION('',(-0.190809912898503,0.,0.981627005099017));
#102722=DIRECTION('',(0.981627005099017,0.,0.190809912898503));
#102723=DIRECTION('',(-0.190809912898503,0.,0.981627005099017));
#102724=DIRECTION('',(0.981627005099017,0.,0.190809912898503));
#102725=DIRECTION('center_axis',(0.981627005099017,0.,0.190809912898503));
#102726=DIRECTION('ref_axis',(0.,-1.,0.));
#102727=DIRECTION('',(-0.190809912898503,0.,0.981627005099017));
#102728=DIRECTION('',(0.,-1.,0.));
#102729=DIRECTION('',(0.,-1.,0.));
#102730=DIRECTION('center_axis',(0.,-1.,0.));
#102731=DIRECTION('ref_axis',(0.,0.,-1.));
#102732=DIRECTION('',(-0.190809912898503,0.,0.981627005099017));
#102733=DIRECTION('',(-0.981627005099017,0.,-0.190809912898503));
#102734=DIRECTION('',(-0.981627005099017,0.,-0.190809912898503));
#102735=DIRECTION('center_axis',(-0.981627005099017,0.,-0.190809912898503));
#102736=DIRECTION('ref_axis',(-0.190809912898503,0.,0.981627005099017));
#102737=DIRECTION('',(0.,1.,0.));
#102738=DIRECTION('',(0.,1.,0.));
#102739=DIRECTION('center_axis',(0.,1.,0.));
#102740=DIRECTION('ref_axis',(1.,0.,0.));
#102741=DIRECTION('',(-0.190809912898503,0.,0.981627005099017));
#102742=DIRECTION('',(0.981627005099017,0.,0.190809912898503));
#102743=DIRECTION('',(-0.190809912898503,0.,0.981627005099017));
#102744=DIRECTION('',(0.981627005099017,0.,0.190809912898503));
#102745=DIRECTION('center_axis',(0.981627005099017,0.,0.190809912898503));
#102746=DIRECTION('ref_axis',(0.,-1.,0.));
#102747=DIRECTION('',(-0.190809912898503,0.,0.981627005099017));
#102748=DIRECTION('',(0.,-1.,0.));
#102749=DIRECTION('',(0.,-1.,0.));
#102750=DIRECTION('center_axis',(0.,-1.,0.));
#102751=DIRECTION('ref_axis',(0.,0.,-1.));
#102752=DIRECTION('',(-0.190809912898503,0.,0.981627005099017));
#102753=DIRECTION('',(-0.981627005099017,0.,-0.190809912898503));
#102754=DIRECTION('',(-0.981627005099017,0.,-0.190809912898503));
#102755=DIRECTION('center_axis',(-0.981627005099017,0.,-0.190809912898503));
#102756=DIRECTION('ref_axis',(-0.190809912898503,0.,0.981627005099017));
#102757=DIRECTION('',(0.,1.,0.));
#102758=DIRECTION('',(0.,1.,0.));
#102759=DIRECTION('center_axis',(0.,1.,0.));
#102760=DIRECTION('ref_axis',(1.,0.,0.));
#102761=DIRECTION('',(-0.190809912898503,0.,0.981627005099017));
#102762=DIRECTION('',(0.981627005099017,0.,0.190809912898503));
#102763=DIRECTION('',(-0.190809912898503,0.,0.981627005099017));
#102764=DIRECTION('',(0.981627005099017,0.,0.190809912898503));
#102765=DIRECTION('center_axis',(0.981627005099017,0.,0.190809912898503));
#102766=DIRECTION('ref_axis',(0.,-1.,0.));
#102767=DIRECTION('',(-0.190809912898503,0.,0.981627005099017));
#102768=DIRECTION('',(0.,-1.,0.));
#102769=DIRECTION('',(0.,-1.,0.));
#102770=DIRECTION('center_axis',(0.,-1.,0.));
#102771=DIRECTION('ref_axis',(0.,0.,-1.));
#102772=DIRECTION('',(-0.190809912898503,0.,0.981627005099017));
#102773=DIRECTION('',(-0.981627005099017,0.,-0.190809912898503));
#102774=DIRECTION('',(-0.981627005099017,0.,-0.190809912898503));
#102775=DIRECTION('center_axis',(-0.981627005099017,0.,-0.190809912898503));
#102776=DIRECTION('ref_axis',(-0.190809912898503,0.,0.981627005099017));
#102777=DIRECTION('',(0.,1.,0.));
#102778=DIRECTION('',(0.,1.,0.));
#102779=DIRECTION('center_axis',(0.,1.,0.));
#102780=DIRECTION('ref_axis',(1.,0.,0.));
#102781=DIRECTION('',(-0.190809912898503,0.,0.981627005099017));
#102782=DIRECTION('',(0.981627005099017,0.,0.190809912898503));
#102783=DIRECTION('',(-0.190809912898503,0.,0.981627005099017));
#102784=DIRECTION('',(0.981627005099017,0.,0.190809912898503));
#102785=DIRECTION('center_axis',(0.981627005099017,0.,0.190809912898503));
#102786=DIRECTION('ref_axis',(0.,-1.,0.));
#102787=DIRECTION('',(-0.190809912898503,0.,0.981627005099017));
#102788=DIRECTION('',(0.,-1.,0.));
#102789=DIRECTION('',(0.,-1.,0.));
#102790=DIRECTION('center_axis',(0.,-1.,0.));
#102791=DIRECTION('ref_axis',(0.,0.,-1.));
#102792=DIRECTION('',(-0.190809912898503,0.,0.981627005099017));
#102793=DIRECTION('',(-0.981627005099017,0.,-0.190809912898503));
#102794=DIRECTION('',(-0.981627005099017,0.,-0.190809912898503));
#102795=DIRECTION('center_axis',(-0.981627005099017,0.,-0.190809912898503));
#102796=DIRECTION('ref_axis',(-0.190809912898503,0.,0.981627005099017));
#102797=DIRECTION('',(0.,1.,0.));
#102798=DIRECTION('',(0.,1.,0.));
#102799=DIRECTION('center_axis',(0.,1.,0.));
#102800=DIRECTION('ref_axis',(1.,0.,0.));
#102801=DIRECTION('',(-0.190809912898503,0.,0.981627005099017));
#102802=DIRECTION('',(0.981627005099017,0.,0.190809912898503));
#102803=DIRECTION('',(-0.190809912898503,0.,0.981627005099017));
#102804=DIRECTION('',(0.981627005099017,0.,0.190809912898503));
#102805=DIRECTION('center_axis',(0.981627005099017,0.,0.190809912898503));
#102806=DIRECTION('ref_axis',(0.,-1.,0.));
#102807=DIRECTION('',(-0.190809912898503,0.,0.981627005099017));
#102808=DIRECTION('',(0.,-1.,0.));
#102809=DIRECTION('',(0.,-1.,0.));
#102810=DIRECTION('center_axis',(0.,-1.,0.));
#102811=DIRECTION('ref_axis',(0.,0.,-1.));
#102812=DIRECTION('',(-0.190809912898503,0.,0.981627005099017));
#102813=DIRECTION('',(-0.981627005099017,0.,-0.190809912898503));
#102814=DIRECTION('',(-0.981627005099017,0.,-0.190809912898503));
#102815=DIRECTION('center_axis',(-0.981627005099017,0.,-0.190809912898503));
#102816=DIRECTION('ref_axis',(-0.190809912898503,0.,0.981627005099017));
#102817=DIRECTION('',(0.,1.,0.));
#102818=DIRECTION('',(0.,1.,0.));
#102819=DIRECTION('center_axis',(0.,1.,0.));
#102820=DIRECTION('ref_axis',(1.,0.,0.));
#102821=DIRECTION('',(-0.190809912898503,0.,0.981627005099017));
#102822=DIRECTION('',(0.981627005099017,0.,0.190809912898503));
#102823=DIRECTION('',(-0.190809912898503,0.,0.981627005099017));
#102824=DIRECTION('',(0.981627005099017,0.,0.190809912898503));
#102825=DIRECTION('center_axis',(0.981627005099017,0.,0.190809912898503));
#102826=DIRECTION('ref_axis',(0.,-1.,0.));
#102827=DIRECTION('',(-0.190809912898503,0.,0.981627005099017));
#102828=DIRECTION('',(0.,-1.,0.));
#102829=DIRECTION('',(0.,-1.,0.));
#102830=DIRECTION('center_axis',(0.,-1.,0.));
#102831=DIRECTION('ref_axis',(0.,0.,-1.));
#102832=DIRECTION('',(-0.190809912898503,0.,0.981627005099017));
#102833=DIRECTION('',(-0.981627005099017,0.,-0.190809912898503));
#102834=DIRECTION('',(-0.981627005099017,0.,-0.190809912898503));
#102835=DIRECTION('center_axis',(-0.981627005099017,0.,-0.190809912898503));
#102836=DIRECTION('ref_axis',(-0.190809912898503,0.,0.981627005099017));
#102837=DIRECTION('',(0.,1.,0.));
#102838=DIRECTION('',(0.,1.,0.));
#102839=DIRECTION('center_axis',(0.,1.,0.));
#102840=DIRECTION('ref_axis',(1.,0.,0.));
#102841=DIRECTION('',(-0.190809912898503,0.,0.981627005099017));
#102842=DIRECTION('',(0.981627005099017,0.,0.190809912898503));
#102843=DIRECTION('',(-0.190809912898503,0.,0.981627005099017));
#102844=DIRECTION('',(0.981627005099017,0.,0.190809912898503));
#102845=DIRECTION('center_axis',(0.981627005099017,0.,0.190809912898503));
#102846=DIRECTION('ref_axis',(0.,-1.,0.));
#102847=DIRECTION('',(-0.190809912898503,0.,0.981627005099017));
#102848=DIRECTION('',(0.,-1.,0.));
#102849=DIRECTION('',(0.,-1.,0.));
#102850=DIRECTION('center_axis',(0.,-1.,0.));
#102851=DIRECTION('ref_axis',(0.,0.,-1.));
#102852=DIRECTION('',(-0.190809912898503,0.,0.981627005099017));
#102853=DIRECTION('',(-0.981627005099017,0.,-0.190809912898503));
#102854=DIRECTION('',(-0.981627005099017,0.,-0.190809912898503));
#102855=DIRECTION('center_axis',(-0.981627005099017,0.,-0.190809912898503));
#102856=DIRECTION('ref_axis',(-0.190809912898503,0.,0.981627005099017));
#102857=DIRECTION('',(0.,1.,0.));
#102858=DIRECTION('',(0.,1.,0.));
#102859=DIRECTION('center_axis',(0.,1.,0.));
#102860=DIRECTION('ref_axis',(1.,0.,0.));
#102861=DIRECTION('',(-0.190809912898503,0.,0.981627005099017));
#102862=DIRECTION('',(0.981627005099017,0.,0.190809912898503));
#102863=DIRECTION('',(-0.190809912898503,0.,0.981627005099017));
#102864=DIRECTION('',(0.981627005099017,0.,0.190809912898503));
#102865=DIRECTION('center_axis',(0.981627005099017,0.,0.190809912898503));
#102866=DIRECTION('ref_axis',(0.,-1.,0.));
#102867=DIRECTION('',(-0.190809912898503,0.,0.981627005099017));
#102868=DIRECTION('',(0.,-1.,0.));
#102869=DIRECTION('',(0.,-1.,0.));
#102870=DIRECTION('center_axis',(0.,-1.,0.));
#102871=DIRECTION('ref_axis',(0.,0.,-1.));
#102872=DIRECTION('',(-0.190809912898503,0.,0.981627005099017));
#102873=DIRECTION('',(-0.981627005099017,0.,-0.190809912898503));
#102874=DIRECTION('',(-0.981627005099017,0.,-0.190809912898503));
#102875=DIRECTION('center_axis',(-0.981627005099017,0.,-0.190809912898503));
#102876=DIRECTION('ref_axis',(-0.190809912898503,0.,0.981627005099017));
#102877=DIRECTION('',(0.,1.,0.));
#102878=DIRECTION('',(0.,1.,0.));
#102879=DIRECTION('center_axis',(0.,1.,0.));
#102880=DIRECTION('ref_axis',(1.,0.,0.));
#102881=DIRECTION('',(-0.190809912898503,0.,0.981627005099017));
#102882=DIRECTION('',(0.981627005099017,0.,0.190809912898503));
#102883=DIRECTION('',(-0.190809912898503,0.,0.981627005099017));
#102884=DIRECTION('',(0.981627005099017,0.,0.190809912898503));
#102885=DIRECTION('center_axis',(0.981627005099017,0.,0.190809912898503));
#102886=DIRECTION('ref_axis',(0.,-1.,0.));
#102887=DIRECTION('',(-0.190809912898503,0.,0.981627005099017));
#102888=DIRECTION('',(0.,-1.,0.));
#102889=DIRECTION('',(0.,-1.,0.));
#102890=DIRECTION('center_axis',(0.,-1.,0.));
#102891=DIRECTION('ref_axis',(0.,0.,-1.));
#102892=DIRECTION('',(-0.190809912898503,0.,0.981627005099017));
#102893=DIRECTION('',(-0.981627005099017,0.,-0.190809912898503));
#102894=DIRECTION('',(-0.981627005099017,0.,-0.190809912898503));
#102895=DIRECTION('center_axis',(-0.981627005099017,0.,-0.190809912898503));
#102896=DIRECTION('ref_axis',(-0.190809912898503,0.,0.981627005099017));
#102897=DIRECTION('',(0.,1.,0.));
#102898=DIRECTION('',(0.,1.,0.));
#102899=DIRECTION('center_axis',(0.,1.,0.));
#102900=DIRECTION('ref_axis',(1.,0.,0.));
#102901=DIRECTION('',(-0.190809912898503,0.,0.981627005099017));
#102902=DIRECTION('',(0.981627005099017,0.,0.190809912898503));
#102903=DIRECTION('',(-0.190809912898503,0.,0.981627005099017));
#102904=DIRECTION('',(0.981627005099017,0.,0.190809912898503));
#102905=DIRECTION('center_axis',(0.981627005099017,0.,0.190809912898503));
#102906=DIRECTION('ref_axis',(0.,-1.,0.));
#102907=DIRECTION('',(-0.190809912898503,0.,0.981627005099017));
#102908=DIRECTION('',(0.,-1.,0.));
#102909=DIRECTION('',(0.,-1.,0.));
#102910=DIRECTION('center_axis',(0.,-1.,0.));
#102911=DIRECTION('ref_axis',(0.,0.,-1.));
#102912=DIRECTION('',(-0.190809912898503,0.,0.981627005099017));
#102913=DIRECTION('',(-0.981627005099017,0.,-0.190809912898503));
#102914=DIRECTION('',(-0.981627005099017,0.,-0.190809912898503));
#102915=DIRECTION('center_axis',(-0.981627005099017,0.,-0.190809912898503));
#102916=DIRECTION('ref_axis',(-0.190809912898503,0.,0.981627005099017));
#102917=DIRECTION('',(0.,1.,0.));
#102918=DIRECTION('',(0.,1.,0.));
#102919=DIRECTION('center_axis',(0.,1.,0.));
#102920=DIRECTION('ref_axis',(1.,0.,0.));
#102921=DIRECTION('',(-0.190809912898503,0.,0.981627005099017));
#102922=DIRECTION('',(0.981627005099017,0.,0.190809912898503));
#102923=DIRECTION('',(-0.190809912898503,0.,0.981627005099017));
#102924=DIRECTION('',(0.981627005099017,0.,0.190809912898503));
#102925=DIRECTION('center_axis',(0.981627005099017,0.,0.190809912898503));
#102926=DIRECTION('ref_axis',(0.,-1.,0.));
#102927=DIRECTION('',(-0.190809912898503,0.,0.981627005099017));
#102928=DIRECTION('',(0.,-1.,0.));
#102929=DIRECTION('',(0.,-1.,0.));
#102930=DIRECTION('center_axis',(0.,-1.,0.));
#102931=DIRECTION('ref_axis',(0.,0.,-1.));
#102932=DIRECTION('',(-0.190809912898503,0.,0.981627005099017));
#102933=DIRECTION('',(-0.981627005099017,0.,-0.190809912898503));
#102934=DIRECTION('',(-0.981627005099017,0.,-0.190809912898503));
#102935=DIRECTION('center_axis',(-0.981627005099017,0.,-0.190809912898503));
#102936=DIRECTION('ref_axis',(-0.190809912898503,0.,0.981627005099017));
#102937=DIRECTION('',(0.,1.,0.));
#102938=DIRECTION('',(0.,1.,0.));
#102939=DIRECTION('center_axis',(0.,1.,0.));
#102940=DIRECTION('ref_axis',(1.,0.,0.));
#102941=DIRECTION('',(-0.190809912898503,0.,0.981627005099017));
#102942=DIRECTION('',(0.981627005099017,0.,0.190809912898503));
#102943=DIRECTION('',(-0.190809912898503,0.,0.981627005099017));
#102944=DIRECTION('',(0.981627005099017,0.,0.190809912898503));
#102945=DIRECTION('center_axis',(0.981627005099017,0.,0.190809912898503));
#102946=DIRECTION('ref_axis',(0.,-1.,0.));
#102947=DIRECTION('',(-0.190809912898503,0.,0.981627005099017));
#102948=DIRECTION('',(0.,-1.,0.));
#102949=DIRECTION('',(0.,-1.,0.));
#102950=DIRECTION('center_axis',(0.,-1.,0.));
#102951=DIRECTION('ref_axis',(0.,0.,-1.));
#102952=DIRECTION('',(-0.190809912898503,0.,0.981627005099017));
#102953=DIRECTION('',(-0.981627005099017,0.,-0.190809912898503));
#102954=DIRECTION('',(-0.981627005099017,0.,-0.190809912898503));
#102955=DIRECTION('center_axis',(-0.981627005099017,0.,-0.190809912898503));
#102956=DIRECTION('ref_axis',(-0.190809912898503,0.,0.981627005099017));
#102957=DIRECTION('',(0.,1.,0.));
#102958=DIRECTION('',(0.,1.,0.));
#102959=DIRECTION('center_axis',(0.,1.,0.));
#102960=DIRECTION('ref_axis',(1.,0.,0.));
#102961=DIRECTION('',(-0.190809912898503,0.,0.981627005099017));
#102962=DIRECTION('',(0.981627005099017,0.,0.190809912898503));
#102963=DIRECTION('',(-0.190809912898503,0.,0.981627005099017));
#102964=DIRECTION('',(0.981627005099017,0.,0.190809912898503));
#102965=DIRECTION('center_axis',(0.981627005099017,0.,0.190809912898503));
#102966=DIRECTION('ref_axis',(0.,-1.,0.));
#102967=DIRECTION('',(-0.190809912898503,0.,0.981627005099017));
#102968=DIRECTION('',(0.,-1.,0.));
#102969=DIRECTION('',(0.,-1.,0.));
#102970=DIRECTION('center_axis',(0.,-1.,0.));
#102971=DIRECTION('ref_axis',(0.,0.,-1.));
#102972=DIRECTION('',(-0.190809912898503,0.,0.981627005099017));
#102973=DIRECTION('',(-0.981627005099017,0.,-0.190809912898503));
#102974=DIRECTION('',(-0.981627005099017,0.,-0.190809912898503));
#102975=DIRECTION('center_axis',(-0.981627005099017,0.,-0.190809912898503));
#102976=DIRECTION('ref_axis',(-0.190809912898503,0.,0.981627005099017));
#102977=DIRECTION('',(0.,1.,0.));
#102978=DIRECTION('',(0.,1.,0.));
#102979=DIRECTION('center_axis',(0.,1.,0.));
#102980=DIRECTION('ref_axis',(1.,0.,0.));
#102981=DIRECTION('',(-0.190809912898503,0.,0.981627005099017));
#102982=DIRECTION('',(0.981627005099017,0.,0.190809912898503));
#102983=DIRECTION('',(-0.190809912898503,0.,0.981627005099017));
#102984=DIRECTION('',(0.981627005099017,0.,0.190809912898503));
#102985=DIRECTION('center_axis',(0.981627005099017,0.,0.190809912898503));
#102986=DIRECTION('ref_axis',(0.,-1.,0.));
#102987=DIRECTION('',(-0.190809912898503,0.,0.981627005099017));
#102988=DIRECTION('',(0.,-1.,0.));
#102989=DIRECTION('',(0.,-1.,0.));
#102990=DIRECTION('center_axis',(0.,-1.,0.));
#102991=DIRECTION('ref_axis',(0.,0.,-1.));
#102992=DIRECTION('',(-0.190809912898503,0.,0.981627005099017));
#102993=DIRECTION('',(-0.981627005099017,0.,-0.190809912898503));
#102994=DIRECTION('',(-0.981627005099017,0.,-0.190809912898503));
#102995=DIRECTION('center_axis',(-0.981627005099017,0.,-0.190809912898503));
#102996=DIRECTION('ref_axis',(-0.190809912898503,0.,0.981627005099017));
#102997=DIRECTION('',(0.,1.,0.));
#102998=DIRECTION('',(0.,1.,0.));
#102999=DIRECTION('center_axis',(0.,1.,0.));
#103000=DIRECTION('ref_axis',(1.,0.,0.));
#103001=DIRECTION('',(-0.190809912898503,0.,0.981627005099017));
#103002=DIRECTION('',(0.981627005099017,0.,0.190809912898503));
#103003=DIRECTION('',(-0.190809912898503,0.,0.981627005099017));
#103004=DIRECTION('',(0.981627005099017,0.,0.190809912898503));
#103005=DIRECTION('center_axis',(0.981627005099017,0.,0.190809912898503));
#103006=DIRECTION('ref_axis',(0.,-1.,0.));
#103007=DIRECTION('',(-0.190809912898503,0.,0.981627005099017));
#103008=DIRECTION('',(0.,-1.,0.));
#103009=DIRECTION('',(0.,-1.,0.));
#103010=DIRECTION('center_axis',(0.,-1.,0.));
#103011=DIRECTION('ref_axis',(0.,0.,-1.));
#103012=DIRECTION('',(-0.190809912898503,0.,0.981627005099017));
#103013=DIRECTION('',(-0.981627005099017,0.,-0.190809912898503));
#103014=DIRECTION('',(-0.981627005099017,0.,-0.190809912898503));
#103015=DIRECTION('center_axis',(-0.981627005099017,0.,-0.190809912898503));
#103016=DIRECTION('ref_axis',(-0.190809912898503,0.,0.981627005099017));
#103017=DIRECTION('',(0.,1.,0.));
#103018=DIRECTION('',(0.,1.,0.));
#103019=DIRECTION('center_axis',(0.,1.,0.));
#103020=DIRECTION('ref_axis',(1.,0.,0.));
#103021=DIRECTION('',(-0.190809912898503,0.,0.981627005099017));
#103022=DIRECTION('',(0.981627005099017,0.,0.190809912898503));
#103023=DIRECTION('',(-0.190809912898503,0.,0.981627005099017));
#103024=DIRECTION('',(0.981627005099017,0.,0.190809912898503));
#103025=DIRECTION('center_axis',(0.981627005099017,0.,0.190809912898503));
#103026=DIRECTION('ref_axis',(0.,-1.,0.));
#103027=DIRECTION('',(-0.190809912898503,0.,0.981627005099017));
#103028=DIRECTION('',(0.,-1.,0.));
#103029=DIRECTION('',(0.,-1.,0.));
#103030=DIRECTION('center_axis',(0.,-1.,0.));
#103031=DIRECTION('ref_axis',(0.,0.,-1.));
#103032=DIRECTION('',(-0.190809912898503,0.,0.981627005099017));
#103033=DIRECTION('',(-0.981627005099017,0.,-0.190809912898503));
#103034=DIRECTION('',(-0.981627005099017,0.,-0.190809912898503));
#103035=DIRECTION('center_axis',(-0.981627005099017,0.,-0.190809912898503));
#103036=DIRECTION('ref_axis',(-0.190809912898503,0.,0.981627005099017));
#103037=DIRECTION('',(0.,1.,0.));
#103038=DIRECTION('',(0.,1.,0.));
#103039=DIRECTION('center_axis',(0.,1.,0.));
#103040=DIRECTION('ref_axis',(1.,0.,0.));
#103041=DIRECTION('',(-0.190809912898503,0.,0.981627005099017));
#103042=DIRECTION('',(0.981627005099017,0.,0.190809912898503));
#103043=DIRECTION('',(-0.190809912898503,0.,0.981627005099017));
#103044=DIRECTION('',(0.981627005099017,0.,0.190809912898503));
#103045=DIRECTION('center_axis',(0.981627005099017,0.,0.190809912898503));
#103046=DIRECTION('ref_axis',(0.,-1.,0.));
#103047=DIRECTION('',(-0.190809912898503,0.,0.981627005099017));
#103048=DIRECTION('',(0.,-1.,0.));
#103049=DIRECTION('',(0.,-1.,0.));
#103050=DIRECTION('center_axis',(0.,-1.,0.));
#103051=DIRECTION('ref_axis',(0.,0.,-1.));
#103052=DIRECTION('',(-0.190809912898503,0.,0.981627005099017));
#103053=DIRECTION('',(-0.981627005099017,0.,-0.190809912898503));
#103054=DIRECTION('',(-0.981627005099017,0.,-0.190809912898503));
#103055=DIRECTION('center_axis',(-0.981627005099017,0.,-0.190809912898503));
#103056=DIRECTION('ref_axis',(-0.190809912898503,0.,0.981627005099017));
#103057=DIRECTION('',(0.,1.,0.));
#103058=DIRECTION('',(0.,1.,0.));
#103059=DIRECTION('center_axis',(0.,1.,0.));
#103060=DIRECTION('ref_axis',(1.,0.,0.));
#103061=DIRECTION('',(-0.190809912898503,0.,0.981627005099017));
#103062=DIRECTION('',(0.981627005099017,0.,0.190809912898503));
#103063=DIRECTION('',(-0.190809912898503,0.,0.981627005099017));
#103064=DIRECTION('',(0.981627005099017,0.,0.190809912898503));
#103065=DIRECTION('center_axis',(0.981627005099017,0.,0.190809912898503));
#103066=DIRECTION('ref_axis',(0.,-1.,0.));
#103067=DIRECTION('',(-0.190809912898503,0.,0.981627005099017));
#103068=DIRECTION('',(0.,-1.,0.));
#103069=DIRECTION('',(0.,-1.,0.));
#103070=DIRECTION('center_axis',(0.,-1.,0.));
#103071=DIRECTION('ref_axis',(0.,0.,-1.));
#103072=DIRECTION('',(-0.190809912898503,0.,0.981627005099017));
#103073=DIRECTION('',(-0.981627005099017,0.,-0.190809912898503));
#103074=DIRECTION('',(-0.981627005099017,0.,-0.190809912898503));
#103075=DIRECTION('center_axis',(-0.981627005099017,0.,-0.190809912898503));
#103076=DIRECTION('ref_axis',(-0.190809912898503,0.,0.981627005099017));
#103077=DIRECTION('',(0.,1.,0.));
#103078=DIRECTION('',(0.,1.,0.));
#103079=DIRECTION('center_axis',(0.,1.,0.));
#103080=DIRECTION('ref_axis',(1.,0.,0.));
#103081=DIRECTION('',(-0.190809912898503,0.,0.981627005099017));
#103082=DIRECTION('',(0.981627005099017,0.,0.190809912898503));
#103083=DIRECTION('',(-0.190809912898503,0.,0.981627005099017));
#103084=DIRECTION('',(0.981627005099017,0.,0.190809912898503));
#103085=DIRECTION('center_axis',(0.981627005099017,0.,0.190809912898503));
#103086=DIRECTION('ref_axis',(0.,-1.,0.));
#103087=DIRECTION('',(-0.190809912898503,0.,0.981627005099017));
#103088=DIRECTION('',(0.,-1.,0.));
#103089=DIRECTION('',(0.,-1.,0.));
#103090=DIRECTION('center_axis',(0.,-1.,0.));
#103091=DIRECTION('ref_axis',(0.,0.,-1.));
#103092=DIRECTION('',(-0.190809912898503,0.,0.981627005099017));
#103093=DIRECTION('',(-0.981627005099017,0.,-0.190809912898503));
#103094=DIRECTION('',(-0.981627005099017,0.,-0.190809912898503));
#103095=DIRECTION('center_axis',(-0.981627005099017,0.,-0.190809912898503));
#103096=DIRECTION('ref_axis',(-0.190809912898503,0.,0.981627005099017));
#103097=DIRECTION('',(0.,1.,0.));
#103098=DIRECTION('',(0.,1.,0.));
#103099=DIRECTION('center_axis',(0.,1.,0.));
#103100=DIRECTION('ref_axis',(1.,0.,0.));
#103101=DIRECTION('',(-0.190809912898503,0.,0.981627005099017));
#103102=DIRECTION('',(0.981627005099017,0.,0.190809912898503));
#103103=DIRECTION('',(-0.190809912898503,0.,0.981627005099017));
#103104=DIRECTION('',(0.981627005099017,0.,0.190809912898503));
#103105=DIRECTION('center_axis',(0.981627005099017,0.,0.190809912898503));
#103106=DIRECTION('ref_axis',(0.,-1.,0.));
#103107=DIRECTION('',(-0.190809912898503,0.,0.981627005099017));
#103108=DIRECTION('',(0.,-1.,0.));
#103109=DIRECTION('',(0.,-1.,0.));
#103110=DIRECTION('center_axis',(0.,-1.,0.));
#103111=DIRECTION('ref_axis',(0.,0.,-1.));
#103112=DIRECTION('',(-0.190809912898503,0.,0.981627005099017));
#103113=DIRECTION('',(-0.981627005099017,0.,-0.190809912898503));
#103114=DIRECTION('',(-0.981627005099017,0.,-0.190809912898503));
#103115=DIRECTION('center_axis',(-0.981627005099017,0.,-0.190809912898503));
#103116=DIRECTION('ref_axis',(-0.190809912898503,0.,0.981627005099017));
#103117=DIRECTION('',(0.,1.,0.));
#103118=DIRECTION('',(0.,1.,0.));
#103119=DIRECTION('center_axis',(0.,1.,0.));
#103120=DIRECTION('ref_axis',(1.,0.,0.));
#103121=DIRECTION('',(-0.190809912898503,0.,0.981627005099017));
#103122=DIRECTION('',(0.981627005099017,0.,0.190809912898503));
#103123=DIRECTION('',(-0.190809912898503,0.,0.981627005099017));
#103124=DIRECTION('',(0.981627005099017,0.,0.190809912898503));
#103125=DIRECTION('center_axis',(0.981627005099017,0.,0.190809912898503));
#103126=DIRECTION('ref_axis',(0.,-1.,0.));
#103127=DIRECTION('',(-0.190809912898503,0.,0.981627005099017));
#103128=DIRECTION('',(0.,-1.,0.));
#103129=DIRECTION('',(0.,-1.,0.));
#103130=DIRECTION('center_axis',(0.,-1.,0.));
#103131=DIRECTION('ref_axis',(0.,0.,-1.));
#103132=DIRECTION('',(-0.190809912898503,0.,0.981627005099017));
#103133=DIRECTION('',(-0.981627005099017,0.,-0.190809912898503));
#103134=DIRECTION('',(-0.981627005099017,0.,-0.190809912898503));
#103135=DIRECTION('center_axis',(-0.981627005099017,0.,-0.190809912898503));
#103136=DIRECTION('ref_axis',(-0.190809912898503,0.,0.981627005099017));
#103137=DIRECTION('',(0.,1.,0.));
#103138=DIRECTION('',(0.,1.,0.));
#103139=DIRECTION('center_axis',(0.,1.,0.));
#103140=DIRECTION('ref_axis',(1.,0.,0.));
#103141=DIRECTION('',(-0.190809912898503,0.,0.981627005099017));
#103142=DIRECTION('',(0.981627005099017,0.,0.190809912898503));
#103143=DIRECTION('',(-0.190809912898503,0.,0.981627005099017));
#103144=DIRECTION('',(0.981627005099017,0.,0.190809912898503));
#103145=DIRECTION('center_axis',(0.981627005099017,0.,0.190809912898503));
#103146=DIRECTION('ref_axis',(0.,-1.,0.));
#103147=DIRECTION('',(-0.190809912898503,0.,0.981627005099017));
#103148=DIRECTION('',(0.,-1.,0.));
#103149=DIRECTION('',(0.,-1.,0.));
#103150=DIRECTION('center_axis',(0.,-1.,0.));
#103151=DIRECTION('ref_axis',(0.,0.,-1.));
#103152=DIRECTION('',(-0.190809912898503,0.,0.981627005099017));
#103153=DIRECTION('',(-0.981627005099017,0.,-0.190809912898503));
#103154=DIRECTION('',(-0.981627005099017,0.,-0.190809912898503));
#103155=DIRECTION('center_axis',(-0.981627005099017,0.,-0.190809912898503));
#103156=DIRECTION('ref_axis',(-0.190809912898503,0.,0.981627005099017));
#103157=DIRECTION('',(0.,1.,0.));
#103158=DIRECTION('',(0.,1.,0.));
#103159=DIRECTION('center_axis',(0.,1.,0.));
#103160=DIRECTION('ref_axis',(1.,0.,0.));
#103161=DIRECTION('',(-0.190809912898503,0.,0.981627005099017));
#103162=DIRECTION('',(0.981627005099017,0.,0.190809912898503));
#103163=DIRECTION('',(-0.190809912898503,0.,0.981627005099017));
#103164=DIRECTION('',(0.981627005099017,0.,0.190809912898503));
#103165=DIRECTION('center_axis',(0.981627005099017,0.,0.190809912898503));
#103166=DIRECTION('ref_axis',(0.,-1.,0.));
#103167=DIRECTION('',(-0.190809912898503,0.,0.981627005099017));
#103168=DIRECTION('',(0.,-1.,0.));
#103169=DIRECTION('',(0.,-1.,0.));
#103170=DIRECTION('center_axis',(0.,-1.,0.));
#103171=DIRECTION('ref_axis',(0.,0.,-1.));
#103172=DIRECTION('',(-0.190809912898503,0.,0.981627005099017));
#103173=DIRECTION('',(-0.981627005099017,0.,-0.190809912898503));
#103174=DIRECTION('',(-0.981627005099017,0.,-0.190809912898503));
#103175=DIRECTION('center_axis',(-0.981627005099017,0.,-0.190809912898503));
#103176=DIRECTION('ref_axis',(-0.190809912898503,0.,0.981627005099017));
#103177=DIRECTION('',(0.,1.,0.));
#103178=DIRECTION('',(0.,1.,0.));
#103179=DIRECTION('center_axis',(0.,1.,0.));
#103180=DIRECTION('ref_axis',(1.,0.,0.));
#103181=DIRECTION('',(-0.190809912898503,0.,0.981627005099017));
#103182=DIRECTION('',(0.981627005099017,0.,0.190809912898503));
#103183=DIRECTION('',(-0.190809912898503,0.,0.981627005099017));
#103184=DIRECTION('',(0.981627005099017,0.,0.190809912898503));
#103185=DIRECTION('center_axis',(0.981627005099017,0.,0.190809912898503));
#103186=DIRECTION('ref_axis',(0.,-1.,0.));
#103187=DIRECTION('',(-0.190809912898503,0.,0.981627005099017));
#103188=DIRECTION('',(0.,-1.,0.));
#103189=DIRECTION('',(0.,-1.,0.));
#103190=DIRECTION('center_axis',(0.,-1.,0.));
#103191=DIRECTION('ref_axis',(0.,0.,-1.));
#103192=DIRECTION('',(-0.190809912898503,0.,0.981627005099017));
#103193=DIRECTION('',(-0.981627005099017,0.,-0.190809912898503));
#103194=DIRECTION('',(-0.981627005099017,0.,-0.190809912898503));
#103195=DIRECTION('center_axis',(-0.981627005099017,0.,-0.190809912898503));
#103196=DIRECTION('ref_axis',(-0.190809912898503,0.,0.981627005099017));
#103197=DIRECTION('',(0.,1.,0.));
#103198=DIRECTION('',(0.,1.,0.));
#103199=DIRECTION('center_axis',(0.,1.,0.));
#103200=DIRECTION('ref_axis',(1.,0.,0.));
#103201=DIRECTION('',(-0.190809912898503,0.,0.981627005099017));
#103202=DIRECTION('',(0.981627005099017,0.,0.190809912898503));
#103203=DIRECTION('',(-0.190809912898503,0.,0.981627005099017));
#103204=DIRECTION('',(0.981627005099017,0.,0.190809912898503));
#103205=DIRECTION('center_axis',(0.981627005099017,0.,0.190809912898503));
#103206=DIRECTION('ref_axis',(0.,-1.,0.));
#103207=DIRECTION('',(-0.190809912898503,0.,0.981627005099017));
#103208=DIRECTION('',(0.,-1.,0.));
#103209=DIRECTION('',(0.,-1.,0.));
#103210=DIRECTION('center_axis',(0.,-1.,0.));
#103211=DIRECTION('ref_axis',(0.,0.,-1.));
#103212=DIRECTION('',(-0.190809912898503,0.,0.981627005099017));
#103213=DIRECTION('',(-0.981627005099017,0.,-0.190809912898503));
#103214=DIRECTION('',(-0.981627005099017,0.,-0.190809912898503));
#103215=DIRECTION('center_axis',(-0.981627005099017,0.,-0.190809912898503));
#103216=DIRECTION('ref_axis',(-0.190809912898503,0.,0.981627005099017));
#103217=DIRECTION('',(0.,1.,0.));
#103218=DIRECTION('',(0.,1.,0.));
#103219=DIRECTION('center_axis',(0.,1.,0.));
#103220=DIRECTION('ref_axis',(1.,0.,0.));
#103221=DIRECTION('',(-0.190809912898503,0.,0.981627005099017));
#103222=DIRECTION('',(0.981627005099017,0.,0.190809912898503));
#103223=DIRECTION('',(-0.190809912898503,0.,0.981627005099017));
#103224=DIRECTION('',(0.981627005099017,0.,0.190809912898503));
#103225=DIRECTION('center_axis',(0.981627005099017,0.,0.190809912898503));
#103226=DIRECTION('ref_axis',(0.,-1.,0.));
#103227=DIRECTION('',(-0.190809912898503,0.,0.981627005099017));
#103228=DIRECTION('',(0.,-1.,0.));
#103229=DIRECTION('',(0.,-1.,0.));
#103230=DIRECTION('center_axis',(0.,-1.,0.));
#103231=DIRECTION('ref_axis',(0.,0.,-1.));
#103232=DIRECTION('',(-0.190809912898503,0.,0.981627005099017));
#103233=DIRECTION('',(-0.981627005099017,0.,-0.190809912898503));
#103234=DIRECTION('',(-0.981627005099017,0.,-0.190809912898503));
#103235=DIRECTION('center_axis',(-0.981627005099017,0.,-0.190809912898503));
#103236=DIRECTION('ref_axis',(-0.190809912898503,0.,0.981627005099017));
#103237=DIRECTION('',(0.,1.,0.));
#103238=DIRECTION('',(0.,1.,0.));
#103239=DIRECTION('center_axis',(0.,1.,0.));
#103240=DIRECTION('ref_axis',(1.,0.,0.));
#103241=DIRECTION('',(-0.190809912898503,0.,0.981627005099017));
#103242=DIRECTION('',(0.981627005099017,0.,0.190809912898503));
#103243=DIRECTION('',(-0.190809912898503,0.,0.981627005099017));
#103244=DIRECTION('',(0.981627005099017,0.,0.190809912898503));
#103245=DIRECTION('center_axis',(0.981627005099017,0.,0.190809912898503));
#103246=DIRECTION('ref_axis',(0.,-1.,0.));
#103247=DIRECTION('',(-0.190809912898503,0.,0.981627005099017));
#103248=DIRECTION('',(0.,-1.,0.));
#103249=DIRECTION('',(0.,-1.,0.));
#103250=DIRECTION('center_axis',(0.,-1.,0.));
#103251=DIRECTION('ref_axis',(0.,0.,-1.));
#103252=DIRECTION('',(-0.190809912898503,0.,0.981627005099017));
#103253=DIRECTION('',(-0.981627005099017,0.,-0.190809912898503));
#103254=DIRECTION('',(-0.981627005099017,0.,-0.190809912898503));
#103255=DIRECTION('center_axis',(-0.981627005099017,0.,-0.190809912898503));
#103256=DIRECTION('ref_axis',(-0.190809912898503,0.,0.981627005099017));
#103257=DIRECTION('',(0.,1.,0.));
#103258=DIRECTION('',(0.,1.,0.));
#103259=DIRECTION('center_axis',(0.,1.,0.));
#103260=DIRECTION('ref_axis',(1.,0.,0.));
#103261=DIRECTION('',(-0.190809912898503,0.,0.981627005099017));
#103262=DIRECTION('',(0.981627005099017,0.,0.190809912898503));
#103263=DIRECTION('',(-0.190809912898503,0.,0.981627005099017));
#103264=DIRECTION('',(0.981627005099017,0.,0.190809912898503));
#103265=DIRECTION('center_axis',(0.981627005099017,0.,0.190809912898503));
#103266=DIRECTION('ref_axis',(0.,-1.,0.));
#103267=DIRECTION('',(-0.190809912898503,0.,0.981627005099017));
#103268=DIRECTION('',(0.,-1.,0.));
#103269=DIRECTION('',(0.,-1.,0.));
#103270=DIRECTION('center_axis',(0.,-1.,0.));
#103271=DIRECTION('ref_axis',(0.,0.,-1.));
#103272=DIRECTION('',(-0.190809912898503,0.,0.981627005099017));
#103273=DIRECTION('',(-0.981627005099017,0.,-0.190809912898503));
#103274=DIRECTION('',(-0.981627005099017,0.,-0.190809912898503));
#103275=DIRECTION('center_axis',(-0.981627005099017,0.,-0.190809912898503));
#103276=DIRECTION('ref_axis',(-0.190809912898503,0.,0.981627005099017));
#103277=DIRECTION('',(0.,1.,0.));
#103278=DIRECTION('',(0.,1.,0.));
#103279=DIRECTION('center_axis',(0.,1.,0.));
#103280=DIRECTION('ref_axis',(1.,0.,0.));
#103281=DIRECTION('',(-0.190809912898503,0.,0.981627005099017));
#103282=DIRECTION('',(0.981627005099017,0.,0.190809912898503));
#103283=DIRECTION('',(-0.190809912898503,0.,0.981627005099017));
#103284=DIRECTION('',(0.981627005099017,0.,0.190809912898503));
#103285=DIRECTION('center_axis',(0.981627005099017,0.,0.190809912898503));
#103286=DIRECTION('ref_axis',(0.,-1.,0.));
#103287=DIRECTION('',(-0.190809912898503,0.,0.981627005099017));
#103288=DIRECTION('',(0.,-1.,0.));
#103289=DIRECTION('',(0.,-1.,0.));
#103290=DIRECTION('center_axis',(0.,-1.,0.));
#103291=DIRECTION('ref_axis',(0.,0.,-1.));
#103292=DIRECTION('',(-0.190809912898503,0.,0.981627005099017));
#103293=DIRECTION('',(-0.981627005099017,0.,-0.190809912898503));
#103294=DIRECTION('',(-0.981627005099017,0.,-0.190809912898503));
#103295=DIRECTION('center_axis',(-0.981627005099017,0.,-0.190809912898503));
#103296=DIRECTION('ref_axis',(-0.190809912898503,0.,0.981627005099017));
#103297=DIRECTION('',(0.,1.,0.));
#103298=DIRECTION('',(0.,1.,0.));
#103299=DIRECTION('center_axis',(0.,1.,0.));
#103300=DIRECTION('ref_axis',(1.,0.,0.));
#103301=DIRECTION('',(-0.190809912898503,0.,0.981627005099017));
#103302=DIRECTION('',(0.981627005099017,0.,0.190809912898503));
#103303=DIRECTION('',(-0.190809912898503,0.,0.981627005099017));
#103304=DIRECTION('',(0.981627005099017,0.,0.190809912898503));
#103305=DIRECTION('center_axis',(0.981627005099017,0.,0.190809912898503));
#103306=DIRECTION('ref_axis',(0.,-1.,0.));
#103307=DIRECTION('',(-0.190809912898503,0.,0.981627005099017));
#103308=DIRECTION('',(0.,-1.,0.));
#103309=DIRECTION('',(0.,-1.,0.));
#103310=DIRECTION('center_axis',(0.,-1.,0.));
#103311=DIRECTION('ref_axis',(0.,0.,-1.));
#103312=DIRECTION('',(-0.190809912898503,0.,0.981627005099017));
#103313=DIRECTION('',(-0.981627005099017,0.,-0.190809912898503));
#103314=DIRECTION('',(-0.981627005099017,0.,-0.190809912898503));
#103315=DIRECTION('center_axis',(-0.981627005099017,0.,-0.190809912898503));
#103316=DIRECTION('ref_axis',(-0.190809912898503,0.,0.981627005099017));
#103317=DIRECTION('',(0.,1.,0.));
#103318=DIRECTION('',(0.,1.,0.));
#103319=DIRECTION('center_axis',(0.,1.,0.));
#103320=DIRECTION('ref_axis',(1.,0.,0.));
#103321=DIRECTION('',(-0.190809912898503,0.,0.981627005099017));
#103322=DIRECTION('',(0.981627005099017,0.,0.190809912898503));
#103323=DIRECTION('',(-0.190809912898503,0.,0.981627005099017));
#103324=DIRECTION('',(0.981627005099017,0.,0.190809912898503));
#103325=DIRECTION('center_axis',(0.981627005099017,0.,0.190809912898503));
#103326=DIRECTION('ref_axis',(0.,-1.,0.));
#103327=DIRECTION('',(-0.190809912898503,0.,0.981627005099017));
#103328=DIRECTION('',(0.,-1.,0.));
#103329=DIRECTION('',(0.,-1.,0.));
#103330=DIRECTION('center_axis',(0.,-1.,0.));
#103331=DIRECTION('ref_axis',(0.,0.,-1.));
#103332=DIRECTION('',(-0.190809912898503,0.,0.981627005099017));
#103333=DIRECTION('',(-0.981627005099017,0.,-0.190809912898503));
#103334=DIRECTION('',(-0.981627005099017,0.,-0.190809912898503));
#103335=DIRECTION('center_axis',(-0.981627005099017,0.,-0.190809912898503));
#103336=DIRECTION('ref_axis',(-0.190809912898503,0.,0.981627005099017));
#103337=DIRECTION('',(0.,1.,0.));
#103338=DIRECTION('',(0.,1.,0.));
#103339=DIRECTION('center_axis',(0.,1.,0.));
#103340=DIRECTION('ref_axis',(1.,0.,0.));
#103341=DIRECTION('',(-0.190809912898503,0.,0.981627005099017));
#103342=DIRECTION('',(0.981627005099017,0.,0.190809912898503));
#103343=DIRECTION('',(-0.190809912898503,0.,0.981627005099017));
#103344=DIRECTION('',(0.981627005099017,0.,0.190809912898503));
#103345=DIRECTION('center_axis',(0.981627005099017,0.,0.190809912898503));
#103346=DIRECTION('ref_axis',(0.,-1.,0.));
#103347=DIRECTION('',(-0.190809912898503,0.,0.981627005099017));
#103348=DIRECTION('',(0.,-1.,0.));
#103349=DIRECTION('',(0.,-1.,0.));
#103350=DIRECTION('center_axis',(0.,-1.,0.));
#103351=DIRECTION('ref_axis',(0.,0.,-1.));
#103352=DIRECTION('',(-0.190809912898503,0.,0.981627005099017));
#103353=DIRECTION('',(-0.981627005099017,0.,-0.190809912898503));
#103354=DIRECTION('',(-0.981627005099017,0.,-0.190809912898503));
#103355=DIRECTION('center_axis',(-0.981627005099017,0.,-0.190809912898503));
#103356=DIRECTION('ref_axis',(-0.190809912898503,0.,0.981627005099017));
#103357=DIRECTION('',(0.,1.,0.));
#103358=DIRECTION('',(0.,1.,0.));
#103359=DIRECTION('center_axis',(0.,1.,0.));
#103360=DIRECTION('ref_axis',(1.,0.,0.));
#103361=DIRECTION('',(-0.190809912898503,0.,0.981627005099017));
#103362=DIRECTION('',(0.981627005099017,0.,0.190809912898503));
#103363=DIRECTION('',(-0.190809912898503,0.,0.981627005099017));
#103364=DIRECTION('',(0.981627005099017,0.,0.190809912898503));
#103365=DIRECTION('center_axis',(0.981627005099017,0.,0.190809912898503));
#103366=DIRECTION('ref_axis',(0.,-1.,0.));
#103367=DIRECTION('',(-0.190809912898503,0.,0.981627005099017));
#103368=DIRECTION('',(0.,-1.,0.));
#103369=DIRECTION('',(0.,-1.,0.));
#103370=DIRECTION('center_axis',(0.,-1.,0.));
#103371=DIRECTION('ref_axis',(0.,0.,-1.));
#103372=DIRECTION('',(-0.190809912898503,0.,0.981627005099017));
#103373=DIRECTION('',(-0.981627005099017,0.,-0.190809912898503));
#103374=DIRECTION('',(-0.981627005099017,0.,-0.190809912898503));
#103375=DIRECTION('center_axis',(-0.981627005099017,0.,-0.190809912898503));
#103376=DIRECTION('ref_axis',(-0.190809912898503,0.,0.981627005099017));
#103377=DIRECTION('',(0.,1.,0.));
#103378=DIRECTION('',(0.,1.,0.));
#103379=DIRECTION('center_axis',(0.,1.,0.));
#103380=DIRECTION('ref_axis',(1.,0.,0.));
#103381=DIRECTION('',(-0.190809912898503,0.,0.981627005099017));
#103382=DIRECTION('',(0.981627005099017,0.,0.190809912898503));
#103383=DIRECTION('',(-0.190809912898503,0.,0.981627005099017));
#103384=DIRECTION('',(0.981627005099017,0.,0.190809912898503));
#103385=DIRECTION('center_axis',(0.981627005099017,0.,0.190809912898503));
#103386=DIRECTION('ref_axis',(0.,-1.,0.));
#103387=DIRECTION('',(-0.190809912898503,0.,0.981627005099017));
#103388=DIRECTION('',(0.,-1.,0.));
#103389=DIRECTION('',(0.,-1.,0.));
#103390=DIRECTION('center_axis',(0.,-1.,0.));
#103391=DIRECTION('ref_axis',(0.,0.,-1.));
#103392=DIRECTION('',(-0.190809912898503,0.,0.981627005099017));
#103393=DIRECTION('',(-0.981627005099017,0.,-0.190809912898503));
#103394=DIRECTION('',(-0.981627005099017,0.,-0.190809912898503));
#103395=DIRECTION('center_axis',(-0.981627005099017,0.,-0.190809912898503));
#103396=DIRECTION('ref_axis',(-0.190809912898503,0.,0.981627005099017));
#103397=DIRECTION('',(0.,1.,0.));
#103398=DIRECTION('',(0.,1.,0.));
#103399=DIRECTION('center_axis',(0.,1.,0.));
#103400=DIRECTION('ref_axis',(1.,0.,0.));
#103401=DIRECTION('',(-0.190809912898503,0.,0.981627005099017));
#103402=DIRECTION('',(0.981627005099017,0.,0.190809912898503));
#103403=DIRECTION('',(-0.190809912898503,0.,0.981627005099017));
#103404=DIRECTION('',(0.981627005099017,0.,0.190809912898503));
#103405=DIRECTION('center_axis',(0.981627005099017,0.,0.190809912898503));
#103406=DIRECTION('ref_axis',(0.,-1.,0.));
#103407=DIRECTION('',(-0.190809912898503,0.,0.981627005099017));
#103408=DIRECTION('',(0.,-1.,0.));
#103409=DIRECTION('',(0.,-1.,0.));
#103410=DIRECTION('center_axis',(0.,-1.,0.));
#103411=DIRECTION('ref_axis',(0.,0.,-1.));
#103412=DIRECTION('',(-0.190809912898503,0.,0.981627005099017));
#103413=DIRECTION('',(-0.981627005099017,0.,-0.190809912898503));
#103414=DIRECTION('',(-0.981627005099017,0.,-0.190809912898503));
#103415=DIRECTION('center_axis',(-0.981627005099017,0.,-0.190809912898503));
#103416=DIRECTION('ref_axis',(-0.190809912898503,0.,0.981627005099017));
#103417=DIRECTION('',(0.,1.,0.));
#103418=DIRECTION('',(0.,1.,0.));
#103419=DIRECTION('center_axis',(0.,1.,0.));
#103420=DIRECTION('ref_axis',(1.,0.,0.));
#103421=DIRECTION('',(-0.190809912898503,0.,0.981627005099017));
#103422=DIRECTION('',(0.981627005099017,0.,0.190809912898503));
#103423=DIRECTION('',(-0.190809912898503,0.,0.981627005099017));
#103424=DIRECTION('',(0.981627005099017,0.,0.190809912898503));
#103425=DIRECTION('center_axis',(0.981627005099017,0.,0.190809912898503));
#103426=DIRECTION('ref_axis',(0.,-1.,0.));
#103427=DIRECTION('',(-0.190809912898503,0.,0.981627005099017));
#103428=DIRECTION('',(0.,-1.,0.));
#103429=DIRECTION('',(0.,-1.,0.));
#103430=DIRECTION('center_axis',(0.,-1.,0.));
#103431=DIRECTION('ref_axis',(0.,0.,-1.));
#103432=DIRECTION('',(-0.190809912898503,0.,0.981627005099017));
#103433=DIRECTION('',(-0.981627005099017,0.,-0.190809912898503));
#103434=DIRECTION('',(-0.981627005099017,0.,-0.190809912898503));
#103435=DIRECTION('center_axis',(-0.981627005099017,0.,-0.190809912898503));
#103436=DIRECTION('ref_axis',(-0.190809912898503,0.,0.981627005099017));
#103437=DIRECTION('',(0.,1.,0.));
#103438=DIRECTION('',(0.,1.,0.));
#103439=DIRECTION('center_axis',(0.,1.,0.));
#103440=DIRECTION('ref_axis',(1.,0.,0.));
#103441=DIRECTION('',(-0.190809912898503,0.,0.981627005099017));
#103442=DIRECTION('',(0.981627005099017,0.,0.190809912898503));
#103443=DIRECTION('',(-0.190809912898503,0.,0.981627005099017));
#103444=DIRECTION('',(0.981627005099017,0.,0.190809912898503));
#103445=DIRECTION('center_axis',(0.981627005099017,0.,0.190809912898503));
#103446=DIRECTION('ref_axis',(0.,-1.,0.));
#103447=DIRECTION('',(-0.190809912898503,0.,0.981627005099017));
#103448=DIRECTION('',(0.,-1.,0.));
#103449=DIRECTION('',(0.,-1.,0.));
#103450=DIRECTION('center_axis',(0.,-1.,0.));
#103451=DIRECTION('ref_axis',(0.,0.,-1.));
#103452=DIRECTION('',(-0.190809912898503,0.,0.981627005099017));
#103453=DIRECTION('',(-0.981627005099017,0.,-0.190809912898503));
#103454=DIRECTION('',(-0.981627005099017,0.,-0.190809912898503));
#103455=DIRECTION('center_axis',(-0.981627005099017,0.,-0.190809912898503));
#103456=DIRECTION('ref_axis',(-0.190809912898503,0.,0.981627005099017));
#103457=DIRECTION('',(0.,1.,0.));
#103458=DIRECTION('',(0.,1.,0.));
#103459=DIRECTION('center_axis',(0.,1.,0.));
#103460=DIRECTION('ref_axis',(1.,0.,0.));
#103461=DIRECTION('',(-0.190809912898503,0.,0.981627005099017));
#103462=DIRECTION('',(0.981627005099017,0.,0.190809912898503));
#103463=DIRECTION('',(-0.190809912898503,0.,0.981627005099017));
#103464=DIRECTION('',(0.981627005099017,0.,0.190809912898503));
#103465=DIRECTION('center_axis',(0.981627005099017,0.,0.190809912898503));
#103466=DIRECTION('ref_axis',(0.,-1.,0.));
#103467=DIRECTION('',(-0.190809912898503,0.,0.981627005099017));
#103468=DIRECTION('',(0.,-1.,0.));
#103469=DIRECTION('',(0.,-1.,0.));
#103470=DIRECTION('center_axis',(0.,-1.,0.));
#103471=DIRECTION('ref_axis',(0.,0.,-1.));
#103472=DIRECTION('',(-0.190809912898503,0.,0.981627005099017));
#103473=DIRECTION('',(-0.981627005099017,0.,-0.190809912898503));
#103474=DIRECTION('',(-0.981627005099017,0.,-0.190809912898503));
#103475=DIRECTION('center_axis',(-0.981627005099017,0.,-0.190809912898503));
#103476=DIRECTION('ref_axis',(-0.190809912898503,0.,0.981627005099017));
#103477=DIRECTION('',(0.,1.,0.));
#103478=DIRECTION('',(0.,1.,0.));
#103479=DIRECTION('center_axis',(0.,1.,0.));
#103480=DIRECTION('ref_axis',(1.,0.,0.));
#103481=DIRECTION('',(-0.190809912898503,0.,0.981627005099017));
#103482=DIRECTION('',(0.981627005099017,0.,0.190809912898503));
#103483=DIRECTION('',(-0.190809912898503,0.,0.981627005099017));
#103484=DIRECTION('',(0.981627005099017,0.,0.190809912898503));
#103485=DIRECTION('center_axis',(0.981627005099017,0.,0.190809912898503));
#103486=DIRECTION('ref_axis',(0.,-1.,0.));
#103487=DIRECTION('',(-0.190809912898503,0.,0.981627005099017));
#103488=DIRECTION('',(0.,-1.,0.));
#103489=DIRECTION('',(0.,-1.,0.));
#103490=DIRECTION('center_axis',(0.,-1.,0.));
#103491=DIRECTION('ref_axis',(0.,0.,-1.));
#103492=DIRECTION('',(-0.190809912898503,0.,0.981627005099017));
#103493=DIRECTION('',(-0.981627005099017,0.,-0.190809912898503));
#103494=DIRECTION('',(-0.981627005099017,0.,-0.190809912898503));
#103495=DIRECTION('center_axis',(-0.981627005099017,0.,-0.190809912898503));
#103496=DIRECTION('ref_axis',(-0.190809912898503,0.,0.981627005099017));
#103497=DIRECTION('',(0.,1.,0.));
#103498=DIRECTION('',(0.,1.,0.));
#103499=DIRECTION('center_axis',(0.,1.,0.));
#103500=DIRECTION('ref_axis',(1.,0.,0.));
#103501=DIRECTION('',(-0.190809912898503,0.,0.981627005099017));
#103502=DIRECTION('',(0.981627005099017,0.,0.190809912898503));
#103503=DIRECTION('',(-0.190809912898503,0.,0.981627005099017));
#103504=DIRECTION('',(0.981627005099017,0.,0.190809912898503));
#103505=DIRECTION('center_axis',(0.981627005099017,0.,0.190809912898503));
#103506=DIRECTION('ref_axis',(0.,-1.,0.));
#103507=DIRECTION('',(-0.190809912898503,0.,0.981627005099017));
#103508=DIRECTION('',(0.,-1.,0.));
#103509=DIRECTION('',(0.,-1.,0.));
#103510=DIRECTION('center_axis',(0.,-1.,0.));
#103511=DIRECTION('ref_axis',(0.,0.,-1.));
#103512=DIRECTION('',(-0.190809912898503,0.,0.981627005099017));
#103513=DIRECTION('',(-0.981627005099017,0.,-0.190809912898503));
#103514=DIRECTION('',(-0.981627005099017,0.,-0.190809912898503));
#103515=DIRECTION('center_axis',(-0.981627005099017,0.,-0.190809912898503));
#103516=DIRECTION('ref_axis',(-0.190809912898503,0.,0.981627005099017));
#103517=DIRECTION('',(0.,1.,0.));
#103518=DIRECTION('',(0.,1.,0.));
#103519=DIRECTION('center_axis',(0.,1.,0.));
#103520=DIRECTION('ref_axis',(1.,0.,0.));
#103521=DIRECTION('',(-0.190809912898503,0.,0.981627005099017));
#103522=DIRECTION('',(0.981627005099017,0.,0.190809912898503));
#103523=DIRECTION('',(-0.190809912898503,0.,0.981627005099017));
#103524=DIRECTION('',(0.981627005099017,0.,0.190809912898503));
#103525=DIRECTION('center_axis',(0.981627005099017,0.,0.190809912898503));
#103526=DIRECTION('ref_axis',(0.,-1.,0.));
#103527=DIRECTION('',(-0.190809912898503,0.,0.981627005099017));
#103528=DIRECTION('',(0.,-1.,0.));
#103529=DIRECTION('',(0.,-1.,0.));
#103530=DIRECTION('center_axis',(0.,-1.,0.));
#103531=DIRECTION('ref_axis',(0.,0.,-1.));
#103532=DIRECTION('',(-0.190809912898503,0.,0.981627005099017));
#103533=DIRECTION('',(-0.981627005099017,0.,-0.190809912898503));
#103534=DIRECTION('',(-0.981627005099017,0.,-0.190809912898503));
#103535=DIRECTION('center_axis',(-0.981627005099017,0.,-0.190809912898503));
#103536=DIRECTION('ref_axis',(-0.190809912898503,0.,0.981627005099017));
#103537=DIRECTION('',(0.,1.,0.));
#103538=DIRECTION('',(0.,1.,0.));
#103539=DIRECTION('center_axis',(0.,1.,0.));
#103540=DIRECTION('ref_axis',(1.,0.,0.));
#103541=DIRECTION('',(-0.190809912898503,0.,0.981627005099017));
#103542=DIRECTION('',(0.981627005099017,0.,0.190809912898503));
#103543=DIRECTION('',(-0.190809912898503,0.,0.981627005099017));
#103544=DIRECTION('',(0.981627005099017,0.,0.190809912898503));
#103545=DIRECTION('center_axis',(0.981627005099017,0.,0.190809912898503));
#103546=DIRECTION('ref_axis',(0.,-1.,0.));
#103547=DIRECTION('',(-0.190809912898503,0.,0.981627005099017));
#103548=DIRECTION('',(0.,-1.,0.));
#103549=DIRECTION('',(0.,-1.,0.));
#103550=DIRECTION('center_axis',(0.,-1.,0.));
#103551=DIRECTION('ref_axis',(0.,0.,-1.));
#103552=DIRECTION('',(-0.190809912898503,0.,0.981627005099017));
#103553=DIRECTION('',(-0.981627005099017,0.,-0.190809912898503));
#103554=DIRECTION('',(-0.981627005099017,0.,-0.190809912898503));
#103555=DIRECTION('center_axis',(-0.981627005099017,0.,-0.190809912898503));
#103556=DIRECTION('ref_axis',(-0.190809912898503,0.,0.981627005099017));
#103557=DIRECTION('',(0.,1.,0.));
#103558=DIRECTION('',(0.,1.,0.));
#103559=DIRECTION('center_axis',(0.,1.,0.));
#103560=DIRECTION('ref_axis',(1.,0.,0.));
#103561=DIRECTION('',(-0.190809912898503,0.,0.981627005099017));
#103562=DIRECTION('',(0.981627005099017,0.,0.190809912898503));
#103563=DIRECTION('',(-0.190809912898503,0.,0.981627005099017));
#103564=DIRECTION('',(0.981627005099017,0.,0.190809912898503));
#103565=DIRECTION('center_axis',(0.981627005099017,0.,0.190809912898503));
#103566=DIRECTION('ref_axis',(0.,-1.,0.));
#103567=DIRECTION('',(-0.190809912898503,0.,0.981627005099017));
#103568=DIRECTION('',(0.,-1.,0.));
#103569=DIRECTION('',(0.,-1.,0.));
#103570=DIRECTION('center_axis',(0.,-1.,0.));
#103571=DIRECTION('ref_axis',(0.,0.,-1.));
#103572=DIRECTION('',(-0.190809912898503,0.,0.981627005099017));
#103573=DIRECTION('',(-0.981627005099017,0.,-0.190809912898503));
#103574=DIRECTION('',(-0.981627005099017,0.,-0.190809912898503));
#103575=DIRECTION('center_axis',(-0.981627005099017,0.,-0.190809912898503));
#103576=DIRECTION('ref_axis',(-0.190809912898503,0.,0.981627005099017));
#103577=DIRECTION('',(0.,1.,0.));
#103578=DIRECTION('',(0.,1.,0.));
#103579=DIRECTION('center_axis',(0.,1.,0.));
#103580=DIRECTION('ref_axis',(1.,0.,0.));
#103581=DIRECTION('',(-0.190809912898503,0.,0.981627005099017));
#103582=DIRECTION('',(0.981627005099017,0.,0.190809912898503));
#103583=DIRECTION('',(-0.190809912898503,0.,0.981627005099017));
#103584=DIRECTION('',(0.981627005099017,0.,0.190809912898503));
#103585=DIRECTION('center_axis',(0.981627005099017,0.,0.190809912898503));
#103586=DIRECTION('ref_axis',(0.,-1.,0.));
#103587=DIRECTION('',(-0.190809912898503,0.,0.981627005099017));
#103588=DIRECTION('',(0.,-1.,0.));
#103589=DIRECTION('',(0.,-1.,0.));
#103590=DIRECTION('center_axis',(0.,-1.,0.));
#103591=DIRECTION('ref_axis',(0.,0.,-1.));
#103592=DIRECTION('',(-0.190809912898503,0.,0.981627005099017));
#103593=DIRECTION('',(-0.981627005099017,0.,-0.190809912898503));
#103594=DIRECTION('',(-0.981627005099017,0.,-0.190809912898503));
#103595=DIRECTION('center_axis',(-0.981627005099017,0.,-0.190809912898503));
#103596=DIRECTION('ref_axis',(-0.190809912898503,0.,0.981627005099017));
#103597=DIRECTION('',(0.,1.,0.));
#103598=DIRECTION('',(0.,1.,0.));
#103599=DIRECTION('center_axis',(0.,1.,0.));
#103600=DIRECTION('ref_axis',(1.,0.,0.));
#103601=DIRECTION('',(-0.190809912898503,0.,0.981627005099017));
#103602=DIRECTION('',(0.981627005099017,0.,0.190809912898503));
#103603=DIRECTION('',(-0.190809912898503,0.,0.981627005099017));
#103604=DIRECTION('',(0.981627005099017,0.,0.190809912898503));
#103605=DIRECTION('center_axis',(0.981627005099017,0.,0.190809912898503));
#103606=DIRECTION('ref_axis',(0.,-1.,0.));
#103607=DIRECTION('',(-0.190809912898503,0.,0.981627005099017));
#103608=DIRECTION('',(0.,-1.,0.));
#103609=DIRECTION('',(0.,-1.,0.));
#103610=DIRECTION('center_axis',(0.,-1.,0.));
#103611=DIRECTION('ref_axis',(0.,0.,-1.));
#103612=DIRECTION('',(-0.190809912898503,0.,0.981627005099017));
#103613=DIRECTION('',(-0.981627005099017,0.,-0.190809912898503));
#103614=DIRECTION('',(-0.981627005099017,0.,-0.190809912898503));
#103615=DIRECTION('center_axis',(-0.981627005099017,0.,-0.190809912898503));
#103616=DIRECTION('ref_axis',(-0.190809912898503,0.,0.981627005099017));
#103617=DIRECTION('',(0.,1.,0.));
#103618=DIRECTION('',(0.,1.,0.));
#103619=DIRECTION('center_axis',(0.,1.,0.));
#103620=DIRECTION('ref_axis',(1.,0.,0.));
#103621=DIRECTION('',(-0.190809912898503,0.,0.981627005099017));
#103622=DIRECTION('',(0.981627005099017,0.,0.190809912898503));
#103623=DIRECTION('',(-0.190809912898503,0.,0.981627005099017));
#103624=DIRECTION('',(0.981627005099017,0.,0.190809912898503));
#103625=DIRECTION('center_axis',(0.981627005099017,0.,0.190809912898503));
#103626=DIRECTION('ref_axis',(0.,-1.,0.));
#103627=DIRECTION('',(-0.190809912898503,0.,0.981627005099017));
#103628=DIRECTION('',(0.,-1.,0.));
#103629=DIRECTION('',(0.,-1.,0.));
#103630=DIRECTION('center_axis',(0.,-1.,0.));
#103631=DIRECTION('ref_axis',(0.,0.,-1.));
#103632=DIRECTION('',(-0.190809912898503,0.,0.981627005099017));
#103633=DIRECTION('',(-0.981627005099017,0.,-0.190809912898503));
#103634=DIRECTION('',(-0.981627005099017,0.,-0.190809912898503));
#103635=DIRECTION('center_axis',(-0.981627005099017,0.,-0.190809912898503));
#103636=DIRECTION('ref_axis',(-0.190809912898503,0.,0.981627005099017));
#103637=DIRECTION('',(0.,1.,0.));
#103638=DIRECTION('',(0.,1.,0.));
#103639=DIRECTION('center_axis',(0.,1.,0.));
#103640=DIRECTION('ref_axis',(1.,0.,0.));
#103641=DIRECTION('',(-0.190809912898503,0.,0.981627005099017));
#103642=DIRECTION('',(0.981627005099017,0.,0.190809912898503));
#103643=DIRECTION('',(-0.190809912898503,0.,0.981627005099017));
#103644=DIRECTION('',(0.981627005099017,0.,0.190809912898503));
#103645=DIRECTION('center_axis',(0.981627005099017,0.,0.190809912898503));
#103646=DIRECTION('ref_axis',(0.,-1.,0.));
#103647=DIRECTION('',(-0.190809912898503,0.,0.981627005099017));
#103648=DIRECTION('',(0.,-1.,0.));
#103649=DIRECTION('',(0.,-1.,0.));
#103650=DIRECTION('center_axis',(0.,-1.,0.));
#103651=DIRECTION('ref_axis',(0.,0.,-1.));
#103652=DIRECTION('',(-0.190809912898503,0.,0.981627005099017));
#103653=DIRECTION('',(-0.981627005099017,0.,-0.190809912898503));
#103654=DIRECTION('',(-0.981627005099017,0.,-0.190809912898503));
#103655=DIRECTION('center_axis',(-0.981627005099017,0.,-0.190809912898503));
#103656=DIRECTION('ref_axis',(-0.190809912898503,0.,0.981627005099017));
#103657=DIRECTION('',(0.,1.,0.));
#103658=DIRECTION('',(0.,1.,0.));
#103659=DIRECTION('center_axis',(0.,1.,0.));
#103660=DIRECTION('ref_axis',(1.,0.,0.));
#103661=DIRECTION('',(-0.190809912898503,0.,0.981627005099017));
#103662=DIRECTION('',(0.981627005099017,0.,0.190809912898503));
#103663=DIRECTION('',(-0.190809912898503,0.,0.981627005099017));
#103664=DIRECTION('',(0.981627005099017,0.,0.190809912898503));
#103665=DIRECTION('center_axis',(0.981627005099017,0.,0.190809912898503));
#103666=DIRECTION('ref_axis',(0.,-1.,0.));
#103667=DIRECTION('',(-0.190809912898503,0.,0.981627005099017));
#103668=DIRECTION('',(0.,-1.,0.));
#103669=DIRECTION('',(0.,-1.,0.));
#103670=DIRECTION('center_axis',(0.,-1.,0.));
#103671=DIRECTION('ref_axis',(0.,0.,-1.));
#103672=DIRECTION('',(-0.190809912898503,0.,0.981627005099017));
#103673=DIRECTION('',(-0.981627005099017,0.,-0.190809912898503));
#103674=DIRECTION('',(-0.981627005099017,0.,-0.190809912898503));
#103675=DIRECTION('center_axis',(-0.981627005099017,0.,-0.190809912898503));
#103676=DIRECTION('ref_axis',(-0.190809912898503,0.,0.981627005099017));
#103677=DIRECTION('',(0.,1.,0.));
#103678=DIRECTION('',(0.,1.,0.));
#103679=DIRECTION('center_axis',(0.,1.,0.));
#103680=DIRECTION('ref_axis',(1.,0.,0.));
#103681=DIRECTION('',(-0.190809912898503,0.,0.981627005099017));
#103682=DIRECTION('',(0.981627005099017,0.,0.190809912898503));
#103683=DIRECTION('',(-0.190809912898503,0.,0.981627005099017));
#103684=DIRECTION('',(0.981627005099017,0.,0.190809912898503));
#103685=DIRECTION('center_axis',(0.981627005099017,0.,0.190809912898503));
#103686=DIRECTION('ref_axis',(0.,-1.,0.));
#103687=DIRECTION('',(-0.190809912898503,0.,0.981627005099017));
#103688=DIRECTION('',(0.,-1.,0.));
#103689=DIRECTION('',(0.,-1.,0.));
#103690=DIRECTION('center_axis',(0.,-1.,0.));
#103691=DIRECTION('ref_axis',(0.,0.,-1.));
#103692=DIRECTION('',(-0.190809912898503,0.,0.981627005099017));
#103693=DIRECTION('',(-0.981627005099017,0.,-0.190809912898503));
#103694=DIRECTION('',(-0.981627005099017,0.,-0.190809912898503));
#103695=DIRECTION('center_axis',(-0.981627005099017,0.,-0.190809912898503));
#103696=DIRECTION('ref_axis',(-0.190809912898503,0.,0.981627005099017));
#103697=DIRECTION('',(0.,1.,0.));
#103698=DIRECTION('',(0.,1.,0.));
#103699=DIRECTION('center_axis',(0.,1.,0.));
#103700=DIRECTION('ref_axis',(1.,0.,0.));
#103701=DIRECTION('',(-0.190809912898503,0.,0.981627005099017));
#103702=DIRECTION('',(0.981627005099017,0.,0.190809912898503));
#103703=DIRECTION('',(-0.190809912898503,0.,0.981627005099017));
#103704=DIRECTION('',(0.981627005099017,0.,0.190809912898503));
#103705=DIRECTION('center_axis',(0.981627005099017,0.,0.190809912898503));
#103706=DIRECTION('ref_axis',(0.,-1.,0.));
#103707=DIRECTION('',(-0.190809912898503,0.,0.981627005099017));
#103708=DIRECTION('',(0.,-1.,0.));
#103709=DIRECTION('',(0.,-1.,0.));
#103710=DIRECTION('center_axis',(0.,-1.,0.));
#103711=DIRECTION('ref_axis',(0.,0.,-1.));
#103712=DIRECTION('',(-0.190809912898503,0.,0.981627005099017));
#103713=DIRECTION('',(-0.981627005099017,0.,-0.190809912898503));
#103714=DIRECTION('',(-0.981627005099017,0.,-0.190809912898503));
#103715=DIRECTION('center_axis',(-0.981627005099017,0.,-0.190809912898503));
#103716=DIRECTION('ref_axis',(-0.190809912898503,0.,0.981627005099017));
#103717=DIRECTION('',(0.,1.,0.));
#103718=DIRECTION('',(0.,1.,0.));
#103719=DIRECTION('center_axis',(0.,1.,0.));
#103720=DIRECTION('ref_axis',(1.,0.,0.));
#103721=DIRECTION('',(-0.190809912898503,0.,0.981627005099017));
#103722=DIRECTION('',(0.981627005099017,0.,0.190809912898503));
#103723=DIRECTION('',(-0.190809912898503,0.,0.981627005099017));
#103724=DIRECTION('',(0.981627005099017,0.,0.190809912898503));
#103725=DIRECTION('center_axis',(0.981627005099017,0.,0.190809912898503));
#103726=DIRECTION('ref_axis',(0.,-1.,0.));
#103727=DIRECTION('',(-0.190809912898503,0.,0.981627005099017));
#103728=DIRECTION('',(0.,-1.,0.));
#103729=DIRECTION('',(0.,-1.,0.));
#103730=DIRECTION('center_axis',(0.,-1.,0.));
#103731=DIRECTION('ref_axis',(0.,0.,-1.));
#103732=DIRECTION('',(-0.190809912898503,0.,0.981627005099017));
#103733=DIRECTION('',(-0.981627005099017,0.,-0.190809912898503));
#103734=DIRECTION('',(-0.981627005099017,0.,-0.190809912898503));
#103735=DIRECTION('center_axis',(-0.981627005099017,0.,-0.190809912898503));
#103736=DIRECTION('ref_axis',(-0.190809912898503,0.,0.981627005099017));
#103737=DIRECTION('',(0.,1.,0.));
#103738=DIRECTION('',(0.,1.,0.));
#103739=DIRECTION('center_axis',(0.,1.,0.));
#103740=DIRECTION('ref_axis',(1.,0.,0.));
#103741=DIRECTION('',(-0.190809912898503,0.,0.981627005099017));
#103742=DIRECTION('',(0.981627005099017,0.,0.190809912898503));
#103743=DIRECTION('',(-0.190809912898503,0.,0.981627005099017));
#103744=DIRECTION('',(0.981627005099017,0.,0.190809912898503));
#103745=DIRECTION('center_axis',(0.981627005099017,0.,0.190809912898503));
#103746=DIRECTION('ref_axis',(0.,-1.,0.));
#103747=DIRECTION('',(-0.190809912898503,0.,0.981627005099017));
#103748=DIRECTION('',(0.,-1.,0.));
#103749=DIRECTION('',(0.,-1.,0.));
#103750=DIRECTION('center_axis',(0.,-1.,0.));
#103751=DIRECTION('ref_axis',(0.,0.,-1.));
#103752=DIRECTION('',(-0.190809912898503,0.,0.981627005099017));
#103753=DIRECTION('',(-0.981627005099017,0.,-0.190809912898503));
#103754=DIRECTION('',(-0.981627005099017,0.,-0.190809912898503));
#103755=DIRECTION('center_axis',(-0.981627005099017,0.,-0.190809912898503));
#103756=DIRECTION('ref_axis',(-0.190809912898503,0.,0.981627005099017));
#103757=DIRECTION('',(0.,1.,0.));
#103758=DIRECTION('',(0.,1.,0.));
#103759=DIRECTION('center_axis',(0.,1.,0.));
#103760=DIRECTION('ref_axis',(1.,0.,0.));
#103761=DIRECTION('',(-0.190809912898503,0.,0.981627005099017));
#103762=DIRECTION('',(0.981627005099017,0.,0.190809912898503));
#103763=DIRECTION('',(-0.190809912898503,0.,0.981627005099017));
#103764=DIRECTION('',(0.981627005099017,0.,0.190809912898503));
#103765=DIRECTION('center_axis',(0.981627005099017,0.,0.190809912898503));
#103766=DIRECTION('ref_axis',(0.,-1.,0.));
#103767=DIRECTION('',(-0.190809912898503,0.,0.981627005099017));
#103768=DIRECTION('',(0.,-1.,0.));
#103769=DIRECTION('',(0.,-1.,0.));
#103770=DIRECTION('center_axis',(0.,-1.,0.));
#103771=DIRECTION('ref_axis',(0.,0.,-1.));
#103772=DIRECTION('',(-0.190809912898503,0.,0.981627005099017));
#103773=DIRECTION('',(-0.981627005099017,0.,-0.190809912898503));
#103774=DIRECTION('',(-0.981627005099017,0.,-0.190809912898503));
#103775=DIRECTION('center_axis',(-0.981627005099017,0.,-0.190809912898503));
#103776=DIRECTION('ref_axis',(-0.190809912898503,0.,0.981627005099017));
#103777=DIRECTION('',(0.,1.,0.));
#103778=DIRECTION('',(0.,1.,0.));
#103779=DIRECTION('center_axis',(0.,1.,0.));
#103780=DIRECTION('ref_axis',(1.,0.,0.));
#103781=DIRECTION('',(-0.190809912898503,0.,0.981627005099017));
#103782=DIRECTION('',(0.981627005099017,0.,0.190809912898503));
#103783=DIRECTION('',(-0.190809912898503,0.,0.981627005099017));
#103784=DIRECTION('',(0.981627005099017,0.,0.190809912898503));
#103785=DIRECTION('center_axis',(0.981627005099017,0.,0.190809912898503));
#103786=DIRECTION('ref_axis',(0.,-1.,0.));
#103787=DIRECTION('',(-0.190809912898503,0.,0.981627005099017));
#103788=DIRECTION('',(0.,-1.,0.));
#103789=DIRECTION('',(0.,-1.,0.));
#103790=DIRECTION('center_axis',(0.,-1.,0.));
#103791=DIRECTION('ref_axis',(0.,0.,-1.));
#103792=DIRECTION('',(-0.190809912898503,0.,0.981627005099017));
#103793=DIRECTION('',(-0.981627005099017,0.,-0.190809912898503));
#103794=DIRECTION('',(-0.981627005099017,0.,-0.190809912898503));
#103795=DIRECTION('center_axis',(-0.981627005099017,0.,-0.190809912898503));
#103796=DIRECTION('ref_axis',(-0.190809912898503,0.,0.981627005099017));
#103797=DIRECTION('',(0.,1.,0.));
#103798=DIRECTION('',(0.,1.,0.));
#103799=DIRECTION('center_axis',(0.,1.,0.));
#103800=DIRECTION('ref_axis',(1.,0.,0.));
#103801=DIRECTION('',(-0.190809912898503,0.,0.981627005099017));
#103802=DIRECTION('',(0.981627005099017,0.,0.190809912898503));
#103803=DIRECTION('',(-0.190809912898503,0.,0.981627005099017));
#103804=DIRECTION('',(0.981627005099017,0.,0.190809912898503));
#103805=DIRECTION('center_axis',(0.981627005099017,0.,0.190809912898503));
#103806=DIRECTION('ref_axis',(0.,-1.,0.));
#103807=DIRECTION('',(-0.190809912898503,0.,0.981627005099017));
#103808=DIRECTION('',(0.,-1.,0.));
#103809=DIRECTION('',(0.,-1.,0.));
#103810=DIRECTION('center_axis',(0.,-1.,0.));
#103811=DIRECTION('ref_axis',(0.,0.,-1.));
#103812=DIRECTION('',(-0.190809912898503,0.,0.981627005099017));
#103813=DIRECTION('',(-0.981627005099017,0.,-0.190809912898503));
#103814=DIRECTION('',(-0.981627005099017,0.,-0.190809912898503));
#103815=DIRECTION('center_axis',(-0.981627005099017,0.,-0.190809912898503));
#103816=DIRECTION('ref_axis',(-0.190809912898503,0.,0.981627005099017));
#103817=DIRECTION('',(0.,1.,0.));
#103818=DIRECTION('',(0.,1.,0.));
#103819=DIRECTION('center_axis',(0.,1.,0.));
#103820=DIRECTION('ref_axis',(1.,0.,0.));
#103821=DIRECTION('',(-0.190809912898503,0.,0.981627005099017));
#103822=DIRECTION('',(0.981627005099017,0.,0.190809912898503));
#103823=DIRECTION('',(-0.190809912898503,0.,0.981627005099017));
#103824=DIRECTION('',(0.981627005099017,0.,0.190809912898503));
#103825=DIRECTION('center_axis',(0.981627005099017,0.,0.190809912898503));
#103826=DIRECTION('ref_axis',(0.,-1.,0.));
#103827=DIRECTION('',(-0.190809912898503,0.,0.981627005099017));
#103828=DIRECTION('',(0.,-1.,0.));
#103829=DIRECTION('',(0.,-1.,0.));
#103830=DIRECTION('center_axis',(0.,-1.,0.));
#103831=DIRECTION('ref_axis',(0.,0.,-1.));
#103832=DIRECTION('',(-0.190809912898503,0.,0.981627005099017));
#103833=DIRECTION('',(-0.981627005099017,0.,-0.190809912898503));
#103834=DIRECTION('',(-0.981627005099017,0.,-0.190809912898503));
#103835=DIRECTION('center_axis',(-0.981627005099017,0.,-0.190809912898503));
#103836=DIRECTION('ref_axis',(-0.190809912898503,0.,0.981627005099017));
#103837=DIRECTION('',(0.,1.,0.));
#103838=DIRECTION('',(0.,1.,0.));
#103839=DIRECTION('center_axis',(0.,1.,0.));
#103840=DIRECTION('ref_axis',(1.,0.,0.));
#103841=DIRECTION('',(-0.190809912898503,0.,0.981627005099017));
#103842=DIRECTION('',(0.981627005099017,0.,0.190809912898503));
#103843=DIRECTION('',(-0.190809912898503,0.,0.981627005099017));
#103844=DIRECTION('',(0.981627005099017,0.,0.190809912898503));
#103845=DIRECTION('center_axis',(0.981627005099017,0.,0.190809912898503));
#103846=DIRECTION('ref_axis',(0.,-1.,0.));
#103847=DIRECTION('',(-0.190809912898503,0.,0.981627005099017));
#103848=DIRECTION('',(0.,-1.,0.));
#103849=DIRECTION('',(0.,-1.,0.));
#103850=DIRECTION('center_axis',(0.,-1.,0.));
#103851=DIRECTION('ref_axis',(0.,0.,-1.));
#103852=DIRECTION('',(-0.190809912898503,0.,0.981627005099017));
#103853=DIRECTION('',(-0.981627005099017,0.,-0.190809912898503));
#103854=DIRECTION('',(-0.981627005099017,0.,-0.190809912898503));
#103855=DIRECTION('center_axis',(-0.981627005099017,0.,-0.190809912898503));
#103856=DIRECTION('ref_axis',(-0.190809912898503,0.,0.981627005099017));
#103857=DIRECTION('',(0.,1.,0.));
#103858=DIRECTION('',(0.,1.,0.));
#103859=DIRECTION('center_axis',(0.,1.,0.));
#103860=DIRECTION('ref_axis',(1.,0.,0.));
#103861=DIRECTION('',(-0.190809912898503,0.,0.981627005099017));
#103862=DIRECTION('',(0.981627005099017,0.,0.190809912898503));
#103863=DIRECTION('',(-0.190809912898503,0.,0.981627005099017));
#103864=DIRECTION('',(0.981627005099017,0.,0.190809912898503));
#103865=DIRECTION('center_axis',(0.981627005099017,0.,0.190809912898503));
#103866=DIRECTION('ref_axis',(0.,-1.,0.));
#103867=DIRECTION('',(-0.190809912898503,0.,0.981627005099017));
#103868=DIRECTION('',(0.,-1.,0.));
#103869=DIRECTION('',(0.,-1.,0.));
#103870=DIRECTION('center_axis',(0.,-1.,0.));
#103871=DIRECTION('ref_axis',(0.,0.,-1.));
#103872=DIRECTION('',(-0.190809912898503,0.,0.981627005099017));
#103873=DIRECTION('',(-0.981627005099017,0.,-0.190809912898503));
#103874=DIRECTION('',(-0.981627005099017,0.,-0.190809912898503));
#103875=DIRECTION('center_axis',(-0.981627005099017,0.,-0.190809912898503));
#103876=DIRECTION('ref_axis',(-0.190809912898503,0.,0.981627005099017));
#103877=DIRECTION('',(0.,1.,0.));
#103878=DIRECTION('',(0.,1.,0.));
#103879=DIRECTION('center_axis',(0.,1.,0.));
#103880=DIRECTION('ref_axis',(1.,0.,0.));
#103881=DIRECTION('',(-0.190809912898503,0.,0.981627005099017));
#103882=DIRECTION('',(0.981627005099017,0.,0.190809912898503));
#103883=DIRECTION('',(-0.190809912898503,0.,0.981627005099017));
#103884=DIRECTION('',(0.981627005099017,0.,0.190809912898503));
#103885=DIRECTION('center_axis',(0.981627005099017,0.,0.190809912898503));
#103886=DIRECTION('ref_axis',(0.,-1.,0.));
#103887=DIRECTION('',(-0.190809912898503,0.,0.981627005099017));
#103888=DIRECTION('',(0.,-1.,0.));
#103889=DIRECTION('',(0.,-1.,0.));
#103890=DIRECTION('center_axis',(0.,-1.,0.));
#103891=DIRECTION('ref_axis',(0.,0.,-1.));
#103892=DIRECTION('',(-0.190809912898503,0.,0.981627005099017));
#103893=DIRECTION('',(-0.981627005099017,0.,-0.190809912898503));
#103894=DIRECTION('',(-0.981627005099017,0.,-0.190809912898503));
#103895=DIRECTION('center_axis',(-0.981627005099017,0.,-0.190809912898503));
#103896=DIRECTION('ref_axis',(-0.190809912898503,0.,0.981627005099017));
#103897=DIRECTION('',(0.,1.,0.));
#103898=DIRECTION('',(0.,1.,0.));
#103899=DIRECTION('center_axis',(0.,1.,0.));
#103900=DIRECTION('ref_axis',(1.,0.,0.));
#103901=DIRECTION('',(-0.190809912898503,0.,0.981627005099017));
#103902=DIRECTION('',(0.981627005099017,0.,0.190809912898503));
#103903=DIRECTION('',(-0.190809912898503,0.,0.981627005099017));
#103904=DIRECTION('',(0.981627005099017,0.,0.190809912898503));
#103905=DIRECTION('center_axis',(0.981627005099017,0.,0.190809912898503));
#103906=DIRECTION('ref_axis',(0.,-1.,0.));
#103907=DIRECTION('',(-0.190809912898503,0.,0.981627005099017));
#103908=DIRECTION('',(0.,-1.,0.));
#103909=DIRECTION('',(0.,-1.,0.));
#103910=DIRECTION('center_axis',(0.,-1.,0.));
#103911=DIRECTION('ref_axis',(0.,0.,-1.));
#103912=DIRECTION('',(-0.190809912898503,0.,0.981627005099017));
#103913=DIRECTION('',(-0.981627005099017,0.,-0.190809912898503));
#103914=DIRECTION('',(-0.981627005099017,0.,-0.190809912898503));
#103915=DIRECTION('center_axis',(-0.981627005099017,0.,-0.190809912898503));
#103916=DIRECTION('ref_axis',(-0.190809912898503,0.,0.981627005099017));
#103917=DIRECTION('',(0.,1.,0.));
#103918=DIRECTION('',(0.,1.,0.));
#103919=DIRECTION('center_axis',(0.,1.,0.));
#103920=DIRECTION('ref_axis',(1.,0.,0.));
#103921=DIRECTION('',(-0.190809912898503,0.,0.981627005099017));
#103922=DIRECTION('',(0.981627005099017,0.,0.190809912898503));
#103923=DIRECTION('',(-0.190809912898503,0.,0.981627005099017));
#103924=DIRECTION('',(0.981627005099017,0.,0.190809912898503));
#103925=DIRECTION('center_axis',(0.981627005099017,0.,0.190809912898503));
#103926=DIRECTION('ref_axis',(0.,-1.,0.));
#103927=DIRECTION('',(-0.190809912898503,0.,0.981627005099017));
#103928=DIRECTION('',(0.,-1.,0.));
#103929=DIRECTION('',(0.,-1.,0.));
#103930=DIRECTION('center_axis',(0.,-1.,0.));
#103931=DIRECTION('ref_axis',(0.,0.,-1.));
#103932=DIRECTION('',(-0.190809912898503,0.,0.981627005099017));
#103933=DIRECTION('',(-0.981627005099017,0.,-0.190809912898503));
#103934=DIRECTION('',(-0.981627005099017,0.,-0.190809912898503));
#103935=DIRECTION('center_axis',(-0.981627005099017,0.,-0.190809912898503));
#103936=DIRECTION('ref_axis',(-0.190809912898503,0.,0.981627005099017));
#103937=DIRECTION('',(0.,1.,0.));
#103938=DIRECTION('',(0.,1.,0.));
#103939=DIRECTION('center_axis',(0.,1.,0.));
#103940=DIRECTION('ref_axis',(1.,0.,0.));
#103941=DIRECTION('',(-0.190809912898503,0.,0.981627005099017));
#103942=DIRECTION('',(0.981627005099017,0.,0.190809912898503));
#103943=DIRECTION('',(-0.190809912898503,0.,0.981627005099017));
#103944=DIRECTION('',(0.981627005099017,0.,0.190809912898503));
#103945=DIRECTION('center_axis',(0.981627005099017,0.,0.190809912898503));
#103946=DIRECTION('ref_axis',(0.,-1.,0.));
#103947=DIRECTION('',(-0.190809912898503,0.,0.981627005099017));
#103948=DIRECTION('',(0.,-1.,0.));
#103949=DIRECTION('',(0.,-1.,0.));
#103950=DIRECTION('center_axis',(0.,-1.,0.));
#103951=DIRECTION('ref_axis',(0.,0.,-1.));
#103952=DIRECTION('',(-0.190809912898503,0.,0.981627005099017));
#103953=DIRECTION('',(-0.981627005099017,0.,-0.190809912898503));
#103954=DIRECTION('',(-0.981627005099017,0.,-0.190809912898503));
#103955=DIRECTION('center_axis',(-0.981627005099017,0.,-0.190809912898503));
#103956=DIRECTION('ref_axis',(-0.190809912898503,0.,0.981627005099017));
#103957=DIRECTION('',(0.,1.,0.));
#103958=DIRECTION('',(0.,1.,0.));
#103959=DIRECTION('center_axis',(0.,1.,0.));
#103960=DIRECTION('ref_axis',(1.,0.,0.));
#103961=DIRECTION('',(-0.190809912898503,0.,0.981627005099017));
#103962=DIRECTION('',(0.981627005099017,0.,0.190809912898503));
#103963=DIRECTION('',(-0.190809912898503,0.,0.981627005099017));
#103964=DIRECTION('',(0.981627005099017,0.,0.190809912898503));
#103965=DIRECTION('center_axis',(0.981627005099017,0.,0.190809912898503));
#103966=DIRECTION('ref_axis',(0.,-1.,0.));
#103967=DIRECTION('',(-0.190809912898503,0.,0.981627005099017));
#103968=DIRECTION('',(0.,-1.,0.));
#103969=DIRECTION('',(0.,-1.,0.));
#103970=DIRECTION('center_axis',(0.,-1.,0.));
#103971=DIRECTION('ref_axis',(0.,0.,-1.));
#103972=DIRECTION('',(-0.190809912898503,0.,0.981627005099017));
#103973=DIRECTION('',(-0.981627005099017,0.,-0.190809912898503));
#103974=DIRECTION('',(-0.981627005099017,0.,-0.190809912898503));
#103975=DIRECTION('center_axis',(-0.981627005099017,0.,-0.190809912898503));
#103976=DIRECTION('ref_axis',(-0.190809912898503,0.,0.981627005099017));
#103977=DIRECTION('',(0.,1.,0.));
#103978=DIRECTION('',(0.,1.,0.));
#103979=DIRECTION('center_axis',(0.,1.,0.));
#103980=DIRECTION('ref_axis',(1.,0.,0.));
#103981=DIRECTION('',(-0.190809912898503,0.,0.981627005099017));
#103982=DIRECTION('',(0.981627005099017,0.,0.190809912898503));
#103983=DIRECTION('',(-0.190809912898503,0.,0.981627005099017));
#103984=DIRECTION('',(0.981627005099017,0.,0.190809912898503));
#103985=DIRECTION('center_axis',(0.981627005099017,0.,0.190809912898503));
#103986=DIRECTION('ref_axis',(0.,-1.,0.));
#103987=DIRECTION('',(-0.190809912898503,0.,0.981627005099017));
#103988=DIRECTION('',(0.,-1.,0.));
#103989=DIRECTION('',(0.,-1.,0.));
#103990=DIRECTION('center_axis',(0.,-1.,0.));
#103991=DIRECTION('ref_axis',(0.,0.,-1.));
#103992=DIRECTION('',(-0.190809912898503,0.,0.981627005099017));
#103993=DIRECTION('',(-0.981627005099017,0.,-0.190809912898503));
#103994=DIRECTION('',(-0.981627005099017,0.,-0.190809912898503));
#103995=DIRECTION('center_axis',(-0.981627005099017,0.,-0.190809912898503));
#103996=DIRECTION('ref_axis',(-0.190809912898503,0.,0.981627005099017));
#103997=DIRECTION('',(0.,1.,0.));
#103998=DIRECTION('',(0.,1.,0.));
#103999=DIRECTION('center_axis',(0.,1.,0.));
#104000=DIRECTION('ref_axis',(1.,0.,0.));
#104001=DIRECTION('',(-0.190809912898503,0.,0.981627005099017));
#104002=DIRECTION('',(0.981627005099017,0.,0.190809912898503));
#104003=DIRECTION('',(-0.190809912898503,0.,0.981627005099017));
#104004=DIRECTION('',(0.981627005099017,0.,0.190809912898503));
#104005=DIRECTION('center_axis',(0.981627005099017,0.,0.190809912898503));
#104006=DIRECTION('ref_axis',(0.,-1.,0.));
#104007=DIRECTION('',(-0.190809912898503,0.,0.981627005099017));
#104008=DIRECTION('',(0.,-1.,0.));
#104009=DIRECTION('',(0.,-1.,0.));
#104010=DIRECTION('center_axis',(0.,-1.,0.));
#104011=DIRECTION('ref_axis',(0.,0.,-1.));
#104012=DIRECTION('',(-0.190809912898503,0.,0.981627005099017));
#104013=DIRECTION('',(-0.981627005099017,0.,-0.190809912898503));
#104014=DIRECTION('',(-0.981627005099017,0.,-0.190809912898503));
#104015=DIRECTION('center_axis',(-0.981627005099017,0.,-0.190809912898503));
#104016=DIRECTION('ref_axis',(-0.190809912898503,0.,0.981627005099017));
#104017=DIRECTION('',(0.,1.,0.));
#104018=DIRECTION('',(0.,1.,0.));
#104019=DIRECTION('center_axis',(0.,1.,0.));
#104020=DIRECTION('ref_axis',(1.,0.,0.));
#104021=DIRECTION('',(-0.190809912898503,0.,0.981627005099017));
#104022=DIRECTION('',(0.981627005099017,0.,0.190809912898503));
#104023=DIRECTION('',(-0.190809912898503,0.,0.981627005099017));
#104024=DIRECTION('',(0.981627005099017,0.,0.190809912898503));
#104025=DIRECTION('center_axis',(0.981627005099017,0.,0.190809912898503));
#104026=DIRECTION('ref_axis',(0.,-1.,0.));
#104027=DIRECTION('',(-0.190809912898503,0.,0.981627005099017));
#104028=DIRECTION('',(0.,-1.,0.));
#104029=DIRECTION('',(0.,-1.,0.));
#104030=DIRECTION('center_axis',(0.,-1.,0.));
#104031=DIRECTION('ref_axis',(0.,0.,-1.));
#104032=DIRECTION('',(-0.190809912898503,0.,0.981627005099017));
#104033=DIRECTION('',(-0.981627005099017,0.,-0.190809912898503));
#104034=DIRECTION('',(-0.981627005099017,0.,-0.190809912898503));
#104035=DIRECTION('center_axis',(-0.981627005099017,0.,-0.190809912898503));
#104036=DIRECTION('ref_axis',(-0.190809912898503,0.,0.981627005099017));
#104037=DIRECTION('',(0.,1.,0.));
#104038=DIRECTION('',(0.,1.,0.));
#104039=DIRECTION('center_axis',(0.,1.,0.));
#104040=DIRECTION('ref_axis',(1.,0.,0.));
#104041=DIRECTION('',(-0.190809912898503,0.,0.981627005099017));
#104042=DIRECTION('',(0.981627005099017,0.,0.190809912898503));
#104043=DIRECTION('',(-0.190809912898503,0.,0.981627005099017));
#104044=DIRECTION('',(0.981627005099017,0.,0.190809912898503));
#104045=DIRECTION('center_axis',(0.981627005099017,0.,0.190809912898503));
#104046=DIRECTION('ref_axis',(0.,-1.,0.));
#104047=DIRECTION('',(-0.190809912898503,0.,0.981627005099017));
#104048=DIRECTION('',(0.,-1.,0.));
#104049=DIRECTION('',(0.,-1.,0.));
#104050=DIRECTION('center_axis',(0.,-1.,0.));
#104051=DIRECTION('ref_axis',(0.,0.,-1.));
#104052=DIRECTION('',(-0.190809912898503,0.,0.981627005099017));
#104053=DIRECTION('',(-0.981627005099017,0.,-0.190809912898503));
#104054=DIRECTION('',(-0.981627005099017,0.,-0.190809912898503));
#104055=DIRECTION('center_axis',(-0.981627005099017,0.,-0.190809912898503));
#104056=DIRECTION('ref_axis',(-0.190809912898503,0.,0.981627005099017));
#104057=DIRECTION('',(0.,1.,0.));
#104058=DIRECTION('',(0.,1.,0.));
#104059=DIRECTION('center_axis',(0.,1.,0.));
#104060=DIRECTION('ref_axis',(1.,0.,0.));
#104061=DIRECTION('',(-0.190809912898503,0.,0.981627005099017));
#104062=DIRECTION('',(0.981627005099017,0.,0.190809912898503));
#104063=DIRECTION('',(-0.190809912898503,0.,0.981627005099017));
#104064=DIRECTION('',(0.981627005099017,0.,0.190809912898503));
#104065=DIRECTION('center_axis',(0.981627005099017,0.,0.190809912898503));
#104066=DIRECTION('ref_axis',(0.,-1.,0.));
#104067=DIRECTION('',(-0.190809912898503,0.,0.981627005099017));
#104068=DIRECTION('',(0.,-1.,0.));
#104069=DIRECTION('',(0.,-1.,0.));
#104070=DIRECTION('center_axis',(0.,-1.,0.));
#104071=DIRECTION('ref_axis',(0.,0.,-1.));
#104072=DIRECTION('',(-0.190809912898503,0.,0.981627005099017));
#104073=DIRECTION('',(-0.981627005099017,0.,-0.190809912898503));
#104074=DIRECTION('',(-0.981627005099017,0.,-0.190809912898503));
#104075=DIRECTION('center_axis',(-0.981627005099017,0.,-0.190809912898503));
#104076=DIRECTION('ref_axis',(-0.190809912898503,0.,0.981627005099017));
#104077=DIRECTION('',(0.,1.,0.));
#104078=DIRECTION('',(0.,1.,0.));
#104079=DIRECTION('center_axis',(0.,1.,0.));
#104080=DIRECTION('ref_axis',(1.,0.,0.));
#104081=DIRECTION('',(-0.190809912898503,0.,0.981627005099017));
#104082=DIRECTION('',(0.981627005099017,0.,0.190809912898503));
#104083=DIRECTION('',(-0.190809912898503,0.,0.981627005099017));
#104084=DIRECTION('',(0.981627005099017,0.,0.190809912898503));
#104085=DIRECTION('center_axis',(0.981627005099017,0.,0.190809912898503));
#104086=DIRECTION('ref_axis',(0.,-1.,0.));
#104087=DIRECTION('',(-0.190809912898503,0.,0.981627005099017));
#104088=DIRECTION('',(0.,-1.,0.));
#104089=DIRECTION('',(0.,-1.,0.));
#104090=DIRECTION('center_axis',(0.,-1.,0.));
#104091=DIRECTION('ref_axis',(0.,0.,-1.));
#104092=DIRECTION('',(-0.190809912898503,0.,0.981627005099017));
#104093=DIRECTION('',(-0.981627005099017,0.,-0.190809912898503));
#104094=DIRECTION('',(-0.981627005099017,0.,-0.190809912898503));
#104095=DIRECTION('center_axis',(-0.981627005099017,0.,-0.190809912898503));
#104096=DIRECTION('ref_axis',(-0.190809912898503,0.,0.981627005099017));
#104097=DIRECTION('',(0.,1.,0.));
#104098=DIRECTION('',(0.,1.,0.));
#104099=DIRECTION('center_axis',(0.,1.,0.));
#104100=DIRECTION('ref_axis',(1.,0.,0.));
#104101=DIRECTION('',(-0.190809912898503,0.,0.981627005099017));
#104102=DIRECTION('',(0.981627005099017,0.,0.190809912898503));
#104103=DIRECTION('',(-0.190809912898503,0.,0.981627005099017));
#104104=DIRECTION('',(0.981627005099017,0.,0.190809912898503));
#104105=DIRECTION('center_axis',(0.981627005099017,0.,0.190809912898503));
#104106=DIRECTION('ref_axis',(0.,-1.,0.));
#104107=DIRECTION('',(-0.190809912898503,0.,0.981627005099017));
#104108=DIRECTION('',(0.,-1.,0.));
#104109=DIRECTION('',(0.,-1.,0.));
#104110=DIRECTION('center_axis',(0.,-1.,0.));
#104111=DIRECTION('ref_axis',(0.,0.,-1.));
#104112=DIRECTION('',(-0.190809912898503,0.,0.981627005099017));
#104113=DIRECTION('',(-0.981627005099017,0.,-0.190809912898503));
#104114=DIRECTION('',(-0.981627005099017,0.,-0.190809912898503));
#104115=DIRECTION('center_axis',(-0.981627005099017,0.,-0.190809912898503));
#104116=DIRECTION('ref_axis',(-0.190809912898503,0.,0.981627005099017));
#104117=DIRECTION('',(0.,1.,0.));
#104118=DIRECTION('',(0.,1.,0.));
#104119=DIRECTION('center_axis',(0.,1.,0.));
#104120=DIRECTION('ref_axis',(1.,0.,0.));
#104121=DIRECTION('',(-0.190809912898503,0.,0.981627005099017));
#104122=DIRECTION('',(0.981627005099017,0.,0.190809912898503));
#104123=DIRECTION('',(-0.190809912898503,0.,0.981627005099017));
#104124=DIRECTION('',(0.981627005099017,0.,0.190809912898503));
#104125=DIRECTION('center_axis',(0.981627005099017,0.,0.190809912898503));
#104126=DIRECTION('ref_axis',(0.,-1.,0.));
#104127=DIRECTION('',(-0.190809912898503,0.,0.981627005099017));
#104128=DIRECTION('',(0.,-1.,0.));
#104129=DIRECTION('',(0.,-1.,0.));
#104130=DIRECTION('center_axis',(0.,-1.,0.));
#104131=DIRECTION('ref_axis',(0.,0.,-1.));
#104132=DIRECTION('',(-0.190809912898503,0.,0.981627005099017));
#104133=DIRECTION('',(-0.981627005099017,0.,-0.190809912898503));
#104134=DIRECTION('',(-0.981627005099017,0.,-0.190809912898503));
#104135=DIRECTION('center_axis',(-0.981627005099017,0.,-0.190809912898503));
#104136=DIRECTION('ref_axis',(-0.190809912898503,0.,0.981627005099017));
#104137=DIRECTION('',(0.,1.,0.));
#104138=DIRECTION('',(0.,1.,0.));
#104139=DIRECTION('center_axis',(0.,1.,0.));
#104140=DIRECTION('ref_axis',(1.,0.,0.));
#104141=DIRECTION('',(-0.190809912898503,0.,0.981627005099017));
#104142=DIRECTION('',(0.981627005099017,0.,0.190809912898503));
#104143=DIRECTION('',(-0.190809912898503,0.,0.981627005099017));
#104144=DIRECTION('',(0.981627005099017,0.,0.190809912898503));
#104145=DIRECTION('center_axis',(0.981627005099017,0.,0.190809912898503));
#104146=DIRECTION('ref_axis',(0.,-1.,0.));
#104147=DIRECTION('',(-0.190809912898503,0.,0.981627005099017));
#104148=DIRECTION('',(0.,-1.,0.));
#104149=DIRECTION('',(0.,-1.,0.));
#104150=DIRECTION('center_axis',(0.,-1.,0.));
#104151=DIRECTION('ref_axis',(0.,0.,-1.));
#104152=DIRECTION('',(-0.190809912898503,0.,0.981627005099017));
#104153=DIRECTION('',(-0.981627005099017,0.,-0.190809912898503));
#104154=DIRECTION('',(-0.981627005099017,0.,-0.190809912898503));
#104155=DIRECTION('center_axis',(-0.981627005099017,0.,-0.190809912898503));
#104156=DIRECTION('ref_axis',(-0.190809912898503,0.,0.981627005099017));
#104157=DIRECTION('',(0.,1.,0.));
#104158=DIRECTION('',(0.,1.,0.));
#104159=DIRECTION('center_axis',(0.,1.,0.));
#104160=DIRECTION('ref_axis',(1.,0.,0.));
#104161=DIRECTION('',(-0.190809912898503,0.,0.981627005099017));
#104162=DIRECTION('',(0.981627005099017,0.,0.190809912898503));
#104163=DIRECTION('',(-0.190809912898503,0.,0.981627005099017));
#104164=DIRECTION('',(0.981627005099017,0.,0.190809912898503));
#104165=DIRECTION('center_axis',(0.981627005099017,0.,0.190809912898503));
#104166=DIRECTION('ref_axis',(0.,-1.,0.));
#104167=DIRECTION('',(-0.190809912898503,0.,0.981627005099017));
#104168=DIRECTION('',(0.,-1.,0.));
#104169=DIRECTION('',(0.,-1.,0.));
#104170=DIRECTION('center_axis',(0.,-1.,0.));
#104171=DIRECTION('ref_axis',(0.,0.,-1.));
#104172=DIRECTION('',(-0.190809912898503,0.,0.981627005099017));
#104173=DIRECTION('',(-0.981627005099017,0.,-0.190809912898503));
#104174=DIRECTION('',(-0.981627005099017,0.,-0.190809912898503));
#104175=DIRECTION('center_axis',(-0.981627005099017,0.,-0.190809912898503));
#104176=DIRECTION('ref_axis',(-0.190809912898503,0.,0.981627005099017));
#104177=DIRECTION('',(0.,1.,0.));
#104178=DIRECTION('',(0.,1.,0.));
#104179=DIRECTION('center_axis',(0.,1.,0.));
#104180=DIRECTION('ref_axis',(1.,0.,0.));
#104181=DIRECTION('',(-0.190809912898503,0.,0.981627005099017));
#104182=DIRECTION('',(0.981627005099017,0.,0.190809912898503));
#104183=DIRECTION('',(-0.190809912898503,0.,0.981627005099017));
#104184=DIRECTION('',(0.981627005099017,0.,0.190809912898503));
#104185=DIRECTION('center_axis',(0.981627005099017,0.,0.190809912898503));
#104186=DIRECTION('ref_axis',(0.,-1.,0.));
#104187=DIRECTION('',(-0.190809912898503,0.,0.981627005099017));
#104188=DIRECTION('',(0.,-1.,0.));
#104189=DIRECTION('',(0.,-1.,0.));
#104190=DIRECTION('center_axis',(0.,-1.,0.));
#104191=DIRECTION('ref_axis',(0.,0.,-1.));
#104192=DIRECTION('',(-0.190809912898503,0.,0.981627005099017));
#104193=DIRECTION('',(-0.981627005099017,0.,-0.190809912898503));
#104194=DIRECTION('',(-0.981627005099017,0.,-0.190809912898503));
#104195=DIRECTION('center_axis',(-0.981627005099017,0.,-0.190809912898503));
#104196=DIRECTION('ref_axis',(-0.190809912898503,0.,0.981627005099017));
#104197=DIRECTION('',(0.,1.,0.));
#104198=DIRECTION('',(0.,1.,0.));
#104199=DIRECTION('center_axis',(0.,1.,0.));
#104200=DIRECTION('ref_axis',(1.,0.,0.));
#104201=DIRECTION('',(-0.190809912898503,0.,0.981627005099017));
#104202=DIRECTION('',(0.981627005099017,0.,0.190809912898503));
#104203=DIRECTION('',(-0.190809912898503,0.,0.981627005099017));
#104204=DIRECTION('',(0.981627005099017,0.,0.190809912898503));
#104205=DIRECTION('center_axis',(0.981627005099017,0.,0.190809912898503));
#104206=DIRECTION('ref_axis',(0.,-1.,0.));
#104207=DIRECTION('',(-0.190809912898503,0.,0.981627005099017));
#104208=DIRECTION('',(0.,-1.,0.));
#104209=DIRECTION('',(0.,-1.,0.));
#104210=DIRECTION('center_axis',(0.,-1.,0.));
#104211=DIRECTION('ref_axis',(0.,0.,-1.));
#104212=DIRECTION('',(-0.190809912898503,0.,0.981627005099017));
#104213=DIRECTION('',(-0.981627005099017,0.,-0.190809912898503));
#104214=DIRECTION('',(-0.981627005099017,0.,-0.190809912898503));
#104215=DIRECTION('center_axis',(-0.981627005099017,0.,-0.190809912898503));
#104216=DIRECTION('ref_axis',(-0.190809912898503,0.,0.981627005099017));
#104217=DIRECTION('',(0.,1.,0.));
#104218=DIRECTION('',(0.,1.,0.));
#104219=DIRECTION('center_axis',(0.,1.,0.));
#104220=DIRECTION('ref_axis',(1.,0.,0.));
#104221=DIRECTION('',(-0.190809912898503,0.,0.981627005099017));
#104222=DIRECTION('',(0.981627005099017,0.,0.190809912898503));
#104223=DIRECTION('',(-0.190809912898503,0.,0.981627005099017));
#104224=DIRECTION('',(0.981627005099017,0.,0.190809912898503));
#104225=DIRECTION('center_axis',(0.981627005099017,0.,0.190809912898503));
#104226=DIRECTION('ref_axis',(0.,-1.,0.));
#104227=DIRECTION('',(-0.190809912898503,0.,0.981627005099017));
#104228=DIRECTION('',(0.,-1.,0.));
#104229=DIRECTION('',(0.,-1.,0.));
#104230=DIRECTION('center_axis',(0.,-1.,0.));
#104231=DIRECTION('ref_axis',(0.,0.,-1.));
#104232=DIRECTION('',(-0.190809912898503,0.,0.981627005099017));
#104233=DIRECTION('',(-0.981627005099017,0.,-0.190809912898503));
#104234=DIRECTION('',(-0.981627005099017,0.,-0.190809912898503));
#104235=DIRECTION('center_axis',(-0.981627005099017,0.,-0.190809912898503));
#104236=DIRECTION('ref_axis',(-0.190809912898503,0.,0.981627005099017));
#104237=DIRECTION('',(0.,1.,0.));
#104238=DIRECTION('',(0.,1.,0.));
#104239=DIRECTION('center_axis',(0.,1.,0.));
#104240=DIRECTION('ref_axis',(1.,0.,0.));
#104241=DIRECTION('',(-0.190809912898503,0.,0.981627005099017));
#104242=DIRECTION('',(0.981627005099017,0.,0.190809912898503));
#104243=DIRECTION('',(-0.190809912898503,0.,0.981627005099017));
#104244=DIRECTION('',(0.981627005099017,0.,0.190809912898503));
#104245=DIRECTION('center_axis',(0.981627005099017,0.,0.190809912898503));
#104246=DIRECTION('ref_axis',(0.,-1.,0.));
#104247=DIRECTION('',(-0.190809912898503,0.,0.981627005099017));
#104248=DIRECTION('',(0.,-1.,0.));
#104249=DIRECTION('',(0.,-1.,0.));
#104250=DIRECTION('center_axis',(0.,-1.,0.));
#104251=DIRECTION('ref_axis',(0.,0.,-1.));
#104252=DIRECTION('',(-0.190809912898503,0.,0.981627005099017));
#104253=DIRECTION('',(-0.981627005099017,0.,-0.190809912898503));
#104254=DIRECTION('',(-0.981627005099017,0.,-0.190809912898503));
#104255=DIRECTION('center_axis',(-0.981627005099017,0.,-0.190809912898503));
#104256=DIRECTION('ref_axis',(-0.190809912898503,0.,0.981627005099017));
#104257=DIRECTION('',(0.,1.,0.));
#104258=DIRECTION('',(0.,1.,0.));
#104259=DIRECTION('center_axis',(0.,1.,0.));
#104260=DIRECTION('ref_axis',(1.,0.,0.));
#104261=DIRECTION('',(-0.190809912898503,0.,0.981627005099017));
#104262=DIRECTION('',(0.981627005099017,0.,0.190809912898503));
#104263=DIRECTION('',(-0.190809912898503,0.,0.981627005099017));
#104264=DIRECTION('',(0.981627005099017,0.,0.190809912898503));
#104265=DIRECTION('center_axis',(0.981627005099017,0.,0.190809912898503));
#104266=DIRECTION('ref_axis',(0.,-1.,0.));
#104267=DIRECTION('',(-0.190809912898503,0.,0.981627005099017));
#104268=DIRECTION('',(0.,-1.,0.));
#104269=DIRECTION('',(0.,-1.,0.));
#104270=DIRECTION('center_axis',(0.,-1.,0.));
#104271=DIRECTION('ref_axis',(0.,0.,-1.));
#104272=DIRECTION('',(-0.190809912898503,0.,0.981627005099017));
#104273=DIRECTION('',(-0.981627005099017,0.,-0.190809912898503));
#104274=DIRECTION('',(-0.981627005099017,0.,-0.190809912898503));
#104275=DIRECTION('center_axis',(-0.981627005099017,0.,-0.190809912898503));
#104276=DIRECTION('ref_axis',(-0.190809912898503,0.,0.981627005099017));
#104277=DIRECTION('',(0.,1.,0.));
#104278=DIRECTION('',(0.,1.,0.));
#104279=DIRECTION('center_axis',(0.,1.,0.));
#104280=DIRECTION('ref_axis',(1.,0.,0.));
#104281=DIRECTION('',(-0.190809912898503,0.,0.981627005099017));
#104282=DIRECTION('',(0.981627005099017,0.,0.190809912898503));
#104283=DIRECTION('',(-0.190809912898503,0.,0.981627005099017));
#104284=DIRECTION('',(0.981627005099017,0.,0.190809912898503));
#104285=DIRECTION('center_axis',(0.981627005099017,0.,0.190809912898503));
#104286=DIRECTION('ref_axis',(0.,-1.,0.));
#104287=DIRECTION('',(-0.190809912898503,0.,0.981627005099017));
#104288=DIRECTION('',(0.,-1.,0.));
#104289=DIRECTION('',(0.,-1.,0.));
#104290=DIRECTION('center_axis',(0.,-1.,0.));
#104291=DIRECTION('ref_axis',(0.,0.,-1.));
#104292=DIRECTION('',(-0.190809912898503,0.,0.981627005099017));
#104293=DIRECTION('',(-0.981627005099017,0.,-0.190809912898503));
#104294=DIRECTION('',(-0.981627005099017,0.,-0.190809912898503));
#104295=DIRECTION('center_axis',(-0.981627005099017,0.,-0.190809912898503));
#104296=DIRECTION('ref_axis',(-0.190809912898503,0.,0.981627005099017));
#104297=DIRECTION('',(0.,1.,0.));
#104298=DIRECTION('',(0.,1.,0.));
#104299=DIRECTION('center_axis',(0.,1.,0.));
#104300=DIRECTION('ref_axis',(1.,0.,0.));
#104301=DIRECTION('',(-0.190809912898503,0.,0.981627005099017));
#104302=DIRECTION('',(0.981627005099017,0.,0.190809912898503));
#104303=DIRECTION('',(-0.190809912898503,0.,0.981627005099017));
#104304=DIRECTION('',(0.981627005099017,0.,0.190809912898503));
#104305=DIRECTION('center_axis',(0.981627005099017,0.,0.190809912898503));
#104306=DIRECTION('ref_axis',(0.,-1.,0.));
#104307=DIRECTION('',(-0.190809912898503,0.,0.981627005099017));
#104308=DIRECTION('',(0.,-1.,0.));
#104309=DIRECTION('',(0.,-1.,0.));
#104310=DIRECTION('center_axis',(0.,-1.,0.));
#104311=DIRECTION('ref_axis',(0.,0.,-1.));
#104312=DIRECTION('',(-0.190809912898503,0.,0.981627005099017));
#104313=DIRECTION('',(-0.981627005099017,0.,-0.190809912898503));
#104314=DIRECTION('',(-0.981627005099017,0.,-0.190809912898503));
#104315=DIRECTION('center_axis',(-0.981627005099017,0.,-0.190809912898503));
#104316=DIRECTION('ref_axis',(-0.190809912898503,0.,0.981627005099017));
#104317=DIRECTION('',(0.,1.,0.));
#104318=DIRECTION('',(0.,1.,0.));
#104319=DIRECTION('center_axis',(0.,1.,0.));
#104320=DIRECTION('ref_axis',(1.,0.,0.));
#104321=DIRECTION('',(-0.190809912898503,0.,0.981627005099017));
#104322=DIRECTION('',(0.981627005099017,0.,0.190809912898503));
#104323=DIRECTION('',(-0.190809912898503,0.,0.981627005099017));
#104324=DIRECTION('',(0.981627005099017,0.,0.190809912898503));
#104325=DIRECTION('center_axis',(0.981627005099017,0.,0.190809912898503));
#104326=DIRECTION('ref_axis',(0.,-1.,0.));
#104327=DIRECTION('',(-0.190809912898503,0.,0.981627005099017));
#104328=DIRECTION('',(0.,-1.,0.));
#104329=DIRECTION('',(0.,-1.,0.));
#104330=DIRECTION('center_axis',(0.,-1.,0.));
#104331=DIRECTION('ref_axis',(0.,0.,-1.));
#104332=DIRECTION('',(-0.190809912898503,0.,0.981627005099017));
#104333=DIRECTION('',(-0.981627005099017,0.,-0.190809912898503));
#104334=DIRECTION('',(-0.981627005099017,0.,-0.190809912898503));
#104335=DIRECTION('center_axis',(-0.981627005099017,0.,-0.190809912898503));
#104336=DIRECTION('ref_axis',(-0.190809912898503,0.,0.981627005099017));
#104337=DIRECTION('',(0.,1.,0.));
#104338=DIRECTION('',(0.,1.,0.));
#104339=DIRECTION('center_axis',(0.,1.,0.));
#104340=DIRECTION('ref_axis',(1.,0.,0.));
#104341=DIRECTION('',(-0.190809912898503,0.,0.981627005099017));
#104342=DIRECTION('',(0.981627005099017,0.,0.190809912898503));
#104343=DIRECTION('',(-0.190809912898503,0.,0.981627005099017));
#104344=DIRECTION('',(0.981627005099017,0.,0.190809912898503));
#104345=DIRECTION('center_axis',(0.981627005099017,0.,0.190809912898503));
#104346=DIRECTION('ref_axis',(0.,-1.,0.));
#104347=DIRECTION('',(-0.190809912898503,0.,0.981627005099017));
#104348=DIRECTION('',(0.,-1.,0.));
#104349=DIRECTION('',(0.,-1.,0.));
#104350=DIRECTION('center_axis',(0.,-1.,0.));
#104351=DIRECTION('ref_axis',(0.,0.,-1.));
#104352=DIRECTION('',(-0.190809912898503,0.,0.981627005099017));
#104353=DIRECTION('',(-0.981627005099017,0.,-0.190809912898503));
#104354=DIRECTION('',(-0.981627005099017,0.,-0.190809912898503));
#104355=DIRECTION('center_axis',(-0.981627005099017,0.,-0.190809912898503));
#104356=DIRECTION('ref_axis',(-0.190809912898503,0.,0.981627005099017));
#104357=DIRECTION('',(0.,1.,0.));
#104358=DIRECTION('',(0.,1.,0.));
#104359=DIRECTION('center_axis',(0.,1.,0.));
#104360=DIRECTION('ref_axis',(1.,0.,0.));
#104361=DIRECTION('',(-0.190809912898503,0.,0.981627005099017));
#104362=DIRECTION('',(0.981627005099017,0.,0.190809912898503));
#104363=DIRECTION('',(-0.190809912898503,0.,0.981627005099017));
#104364=DIRECTION('',(0.981627005099017,0.,0.190809912898503));
#104365=DIRECTION('center_axis',(0.981627005099017,0.,0.190809912898503));
#104366=DIRECTION('ref_axis',(0.,-1.,0.));
#104367=DIRECTION('',(-0.190809912898503,0.,0.981627005099017));
#104368=DIRECTION('',(0.,-1.,0.));
#104369=DIRECTION('',(0.,-1.,0.));
#104370=DIRECTION('center_axis',(0.,-1.,0.));
#104371=DIRECTION('ref_axis',(0.,0.,-1.));
#104372=DIRECTION('',(-0.190809912898503,0.,0.981627005099017));
#104373=DIRECTION('',(-0.981627005099017,0.,-0.190809912898503));
#104374=DIRECTION('',(-0.981627005099017,0.,-0.190809912898503));
#104375=DIRECTION('center_axis',(-0.981627005099017,0.,-0.190809912898503));
#104376=DIRECTION('ref_axis',(-0.190809912898503,0.,0.981627005099017));
#104377=DIRECTION('',(0.,1.,0.));
#104378=DIRECTION('',(0.,1.,0.));
#104379=DIRECTION('center_axis',(0.,1.,0.));
#104380=DIRECTION('ref_axis',(1.,0.,0.));
#104381=DIRECTION('',(-0.190809912898503,0.,0.981627005099017));
#104382=DIRECTION('',(0.981627005099017,0.,0.190809912898503));
#104383=DIRECTION('',(-0.190809912898503,0.,0.981627005099017));
#104384=DIRECTION('',(0.981627005099017,0.,0.190809912898503));
#104385=DIRECTION('center_axis',(0.981627005099017,0.,0.190809912898503));
#104386=DIRECTION('ref_axis',(0.,-1.,0.));
#104387=DIRECTION('',(-0.190809912898503,0.,0.981627005099017));
#104388=DIRECTION('',(0.,-1.,0.));
#104389=DIRECTION('',(0.,-1.,0.));
#104390=DIRECTION('center_axis',(0.,-1.,0.));
#104391=DIRECTION('ref_axis',(0.,0.,-1.));
#104392=DIRECTION('',(-0.190809912898503,0.,0.981627005099017));
#104393=DIRECTION('',(-0.981627005099017,0.,-0.190809912898503));
#104394=DIRECTION('',(-0.981627005099017,0.,-0.190809912898503));
#104395=DIRECTION('center_axis',(-0.981627005099017,0.,-0.190809912898503));
#104396=DIRECTION('ref_axis',(-0.190809912898503,0.,0.981627005099017));
#104397=DIRECTION('',(0.,1.,0.));
#104398=DIRECTION('',(0.,1.,0.));
#104399=DIRECTION('center_axis',(0.,1.,0.));
#104400=DIRECTION('ref_axis',(1.,0.,0.));
#104401=DIRECTION('',(-0.190809912898503,0.,0.981627005099017));
#104402=DIRECTION('',(0.981627005099017,0.,0.190809912898503));
#104403=DIRECTION('',(-0.190809912898503,0.,0.981627005099017));
#104404=DIRECTION('',(0.981627005099017,0.,0.190809912898503));
#104405=DIRECTION('center_axis',(0.981627005099017,0.,0.190809912898503));
#104406=DIRECTION('ref_axis',(0.,-1.,0.));
#104407=DIRECTION('',(-0.190809912898503,0.,0.981627005099017));
#104408=DIRECTION('',(0.,-1.,0.));
#104409=DIRECTION('',(0.,-1.,0.));
#104410=DIRECTION('center_axis',(0.,-1.,0.));
#104411=DIRECTION('ref_axis',(0.,0.,-1.));
#104412=DIRECTION('',(-0.190809912898503,0.,0.981627005099017));
#104413=DIRECTION('',(-0.981627005099017,0.,-0.190809912898503));
#104414=DIRECTION('',(-0.981627005099017,0.,-0.190809912898503));
#104415=DIRECTION('center_axis',(-0.981627005099017,0.,-0.190809912898503));
#104416=DIRECTION('ref_axis',(-0.190809912898503,0.,0.981627005099017));
#104417=DIRECTION('',(0.,1.,0.));
#104418=DIRECTION('',(0.,1.,0.));
#104419=DIRECTION('center_axis',(0.,1.,0.));
#104420=DIRECTION('ref_axis',(1.,0.,0.));
#104421=DIRECTION('',(-0.190809912898503,0.,0.981627005099017));
#104422=DIRECTION('',(0.981627005099017,0.,0.190809912898503));
#104423=DIRECTION('',(-0.190809912898503,0.,0.981627005099017));
#104424=DIRECTION('',(0.981627005099017,0.,0.190809912898503));
#104425=DIRECTION('center_axis',(0.981627005099017,0.,0.190809912898503));
#104426=DIRECTION('ref_axis',(0.,-1.,0.));
#104427=DIRECTION('',(-0.190809912898503,0.,0.981627005099017));
#104428=DIRECTION('',(0.,-1.,0.));
#104429=DIRECTION('',(0.,-1.,0.));
#104430=DIRECTION('center_axis',(0.,-1.,0.));
#104431=DIRECTION('ref_axis',(0.,0.,-1.));
#104432=DIRECTION('',(-0.190809912898503,0.,0.981627005099017));
#104433=DIRECTION('',(-0.981627005099017,0.,-0.190809912898503));
#104434=DIRECTION('',(-0.981627005099017,0.,-0.190809912898503));
#104435=DIRECTION('center_axis',(-0.981627005099017,0.,-0.190809912898503));
#104436=DIRECTION('ref_axis',(-0.190809912898503,0.,0.981627005099017));
#104437=DIRECTION('',(0.,1.,0.));
#104438=DIRECTION('',(0.,1.,0.));
#104439=DIRECTION('center_axis',(0.,1.,0.));
#104440=DIRECTION('ref_axis',(1.,0.,0.));
#104441=DIRECTION('',(-0.190809912898503,0.,0.981627005099017));
#104442=DIRECTION('',(0.981627005099017,0.,0.190809912898503));
#104443=DIRECTION('',(-0.190809912898503,0.,0.981627005099017));
#104444=DIRECTION('',(0.981627005099017,0.,0.190809912898503));
#104445=DIRECTION('center_axis',(0.981627005099017,0.,0.190809912898503));
#104446=DIRECTION('ref_axis',(0.,-1.,0.));
#104447=DIRECTION('',(-0.190809912898503,0.,0.981627005099017));
#104448=DIRECTION('',(0.,-1.,0.));
#104449=DIRECTION('',(0.,-1.,0.));
#104450=DIRECTION('center_axis',(0.,-1.,0.));
#104451=DIRECTION('ref_axis',(0.,0.,-1.));
#104452=DIRECTION('',(-0.190809912898503,0.,0.981627005099017));
#104453=DIRECTION('',(-0.981627005099017,0.,-0.190809912898503));
#104454=DIRECTION('',(-0.981627005099017,0.,-0.190809912898503));
#104455=DIRECTION('center_axis',(-0.981627005099017,0.,-0.190809912898503));
#104456=DIRECTION('ref_axis',(-0.190809912898503,0.,0.981627005099017));
#104457=DIRECTION('',(0.,1.,0.));
#104458=DIRECTION('',(0.,1.,0.));
#104459=DIRECTION('center_axis',(0.,1.,0.));
#104460=DIRECTION('ref_axis',(1.,0.,0.));
#104461=DIRECTION('',(-0.190809912898503,0.,0.981627005099017));
#104462=DIRECTION('',(0.981627005099017,0.,0.190809912898503));
#104463=DIRECTION('',(-0.190809912898503,0.,0.981627005099017));
#104464=DIRECTION('',(0.981627005099017,0.,0.190809912898503));
#104465=DIRECTION('center_axis',(0.981627005099017,0.,0.190809912898503));
#104466=DIRECTION('ref_axis',(0.,-1.,0.));
#104467=DIRECTION('',(-0.190809912898503,0.,0.981627005099017));
#104468=DIRECTION('',(0.,-1.,0.));
#104469=DIRECTION('',(0.,-1.,0.));
#104470=DIRECTION('center_axis',(0.,-1.,0.));
#104471=DIRECTION('ref_axis',(0.,0.,-1.));
#104472=DIRECTION('',(-0.190809912898503,0.,0.981627005099017));
#104473=DIRECTION('',(-0.981627005099017,0.,-0.190809912898503));
#104474=DIRECTION('',(-0.981627005099017,0.,-0.190809912898503));
#104475=DIRECTION('center_axis',(-0.981627005099017,0.,-0.190809912898503));
#104476=DIRECTION('ref_axis',(-0.190809912898503,0.,0.981627005099017));
#104477=DIRECTION('',(0.,1.,0.));
#104478=DIRECTION('',(0.,1.,0.));
#104479=DIRECTION('center_axis',(0.,1.,0.));
#104480=DIRECTION('ref_axis',(1.,0.,0.));
#104481=DIRECTION('',(-0.190809912898503,0.,0.981627005099017));
#104482=DIRECTION('',(0.981627005099017,0.,0.190809912898503));
#104483=DIRECTION('',(-0.190809912898503,0.,0.981627005099017));
#104484=DIRECTION('',(0.981627005099017,0.,0.190809912898503));
#104485=DIRECTION('center_axis',(0.981627005099017,0.,0.190809912898503));
#104486=DIRECTION('ref_axis',(0.,-1.,0.));
#104487=DIRECTION('',(-0.190809912898503,0.,0.981627005099017));
#104488=DIRECTION('',(0.,-1.,0.));
#104489=DIRECTION('',(0.,-1.,0.));
#104490=DIRECTION('center_axis',(0.,-1.,0.));
#104491=DIRECTION('ref_axis',(0.,0.,-1.));
#104492=DIRECTION('',(-0.190809912898503,0.,0.981627005099017));
#104493=DIRECTION('',(-0.981627005099017,0.,-0.190809912898503));
#104494=DIRECTION('',(-0.981627005099017,0.,-0.190809912898503));
#104495=DIRECTION('center_axis',(-0.981627005099017,0.,-0.190809912898503));
#104496=DIRECTION('ref_axis',(-0.190809912898503,0.,0.981627005099017));
#104497=DIRECTION('',(0.,1.,0.));
#104498=DIRECTION('',(0.,1.,0.));
#104499=DIRECTION('center_axis',(0.,1.,0.));
#104500=DIRECTION('ref_axis',(1.,0.,0.));
#104501=DIRECTION('',(-0.190809912898503,0.,0.981627005099017));
#104502=DIRECTION('',(0.981627005099017,0.,0.190809912898503));
#104503=DIRECTION('',(-0.190809912898503,0.,0.981627005099017));
#104504=DIRECTION('',(0.981627005099017,0.,0.190809912898503));
#104505=DIRECTION('center_axis',(0.981627005099017,0.,0.190809912898503));
#104506=DIRECTION('ref_axis',(0.,-1.,0.));
#104507=DIRECTION('',(-0.190809912898503,0.,0.981627005099017));
#104508=DIRECTION('',(0.,-1.,0.));
#104509=DIRECTION('',(0.,-1.,0.));
#104510=DIRECTION('center_axis',(0.,-1.,0.));
#104511=DIRECTION('ref_axis',(0.,0.,-1.));
#104512=DIRECTION('',(-0.190809912898503,0.,0.981627005099017));
#104513=DIRECTION('',(-0.981627005099017,0.,-0.190809912898503));
#104514=DIRECTION('',(-0.981627005099017,0.,-0.190809912898503));
#104515=DIRECTION('center_axis',(-0.981627005099017,0.,-0.190809912898503));
#104516=DIRECTION('ref_axis',(-0.190809912898503,0.,0.981627005099017));
#104517=DIRECTION('',(0.,1.,0.));
#104518=DIRECTION('',(0.,1.,0.));
#104519=DIRECTION('center_axis',(0.,1.,0.));
#104520=DIRECTION('ref_axis',(1.,0.,0.));
#104521=DIRECTION('',(-0.190809912898503,0.,0.981627005099017));
#104522=DIRECTION('',(0.981627005099017,0.,0.190809912898503));
#104523=DIRECTION('',(-0.190809912898503,0.,0.981627005099017));
#104524=DIRECTION('',(0.981627005099017,0.,0.190809912898503));
#104525=DIRECTION('center_axis',(0.981627005099017,0.,0.190809912898503));
#104526=DIRECTION('ref_axis',(0.,-1.,0.));
#104527=DIRECTION('',(-0.190809912898503,0.,0.981627005099017));
#104528=DIRECTION('',(0.,-1.,0.));
#104529=DIRECTION('',(0.,-1.,0.));
#104530=DIRECTION('center_axis',(0.,-1.,0.));
#104531=DIRECTION('ref_axis',(0.,0.,-1.));
#104532=DIRECTION('',(-0.190809912898503,0.,0.981627005099017));
#104533=DIRECTION('',(-0.981627005099017,0.,-0.190809912898503));
#104534=DIRECTION('',(-0.981627005099017,0.,-0.190809912898503));
#104535=DIRECTION('center_axis',(-0.981627005099017,0.,-0.190809912898503));
#104536=DIRECTION('ref_axis',(-0.190809912898503,0.,0.981627005099017));
#104537=DIRECTION('',(0.,1.,0.));
#104538=DIRECTION('',(0.,1.,0.));
#104539=DIRECTION('center_axis',(0.,1.,0.));
#104540=DIRECTION('ref_axis',(1.,0.,0.));
#104541=DIRECTION('',(-0.190809912898503,0.,0.981627005099017));
#104542=DIRECTION('',(0.981627005099017,0.,0.190809912898503));
#104543=DIRECTION('',(-0.190809912898503,0.,0.981627005099017));
#104544=DIRECTION('',(0.981627005099017,0.,0.190809912898503));
#104545=DIRECTION('center_axis',(0.981627005099017,0.,0.190809912898503));
#104546=DIRECTION('ref_axis',(0.,-1.,0.));
#104547=DIRECTION('',(-0.190809912898503,0.,0.981627005099017));
#104548=DIRECTION('',(0.,-1.,0.));
#104549=DIRECTION('',(0.,-1.,0.));
#104550=DIRECTION('center_axis',(0.,-1.,0.));
#104551=DIRECTION('ref_axis',(0.,0.,-1.));
#104552=DIRECTION('',(-0.190809912898503,0.,0.981627005099017));
#104553=DIRECTION('',(-0.981627005099017,0.,-0.190809912898503));
#104554=DIRECTION('',(-0.981627005099017,0.,-0.190809912898503));
#104555=DIRECTION('center_axis',(-0.981627005099017,0.,-0.190809912898503));
#104556=DIRECTION('ref_axis',(-0.190809912898503,0.,0.981627005099017));
#104557=DIRECTION('',(0.,1.,0.));
#104558=DIRECTION('',(0.,1.,0.));
#104559=DIRECTION('center_axis',(0.,1.,0.));
#104560=DIRECTION('ref_axis',(1.,0.,0.));
#104561=DIRECTION('',(-0.190809912898503,0.,0.981627005099017));
#104562=DIRECTION('',(0.981627005099017,0.,0.190809912898503));
#104563=DIRECTION('',(-0.190809912898503,0.,0.981627005099017));
#104564=DIRECTION('',(0.981627005099017,0.,0.190809912898503));
#104565=DIRECTION('center_axis',(0.981627005099017,0.,0.190809912898503));
#104566=DIRECTION('ref_axis',(0.,-1.,0.));
#104567=DIRECTION('',(-0.190809912898503,0.,0.981627005099017));
#104568=DIRECTION('',(0.,-1.,0.));
#104569=DIRECTION('',(0.,-1.,0.));
#104570=DIRECTION('center_axis',(0.,-1.,0.));
#104571=DIRECTION('ref_axis',(0.,0.,-1.));
#104572=DIRECTION('',(-0.190809912898503,0.,0.981627005099017));
#104573=DIRECTION('',(-0.981627005099017,0.,-0.190809912898503));
#104574=DIRECTION('',(-0.981627005099017,0.,-0.190809912898503));
#104575=DIRECTION('center_axis',(-0.981627005099017,0.,-0.190809912898503));
#104576=DIRECTION('ref_axis',(-0.190809912898503,0.,0.981627005099017));
#104577=DIRECTION('',(0.,1.,0.));
#104578=DIRECTION('',(0.,1.,0.));
#104579=DIRECTION('center_axis',(0.,1.,0.));
#104580=DIRECTION('ref_axis',(1.,0.,0.));
#104581=DIRECTION('',(-0.190809912898503,0.,0.981627005099017));
#104582=DIRECTION('',(0.981627005099017,0.,0.190809912898503));
#104583=DIRECTION('',(-0.190809912898503,0.,0.981627005099017));
#104584=DIRECTION('',(0.981627005099017,0.,0.190809912898503));
#104585=DIRECTION('center_axis',(0.981627005099017,0.,0.190809912898503));
#104586=DIRECTION('ref_axis',(0.,-1.,0.));
#104587=DIRECTION('',(-0.190809912898503,0.,0.981627005099017));
#104588=DIRECTION('',(0.,-1.,0.));
#104589=DIRECTION('',(0.,-1.,0.));
#104590=DIRECTION('center_axis',(0.,-1.,0.));
#104591=DIRECTION('ref_axis',(0.,0.,-1.));
#104592=DIRECTION('',(-0.190809912898503,0.,0.981627005099017));
#104593=DIRECTION('',(-0.981627005099017,0.,-0.190809912898503));
#104594=DIRECTION('',(-0.981627005099017,0.,-0.190809912898503));
#104595=DIRECTION('center_axis',(-0.981627005099017,0.,-0.190809912898503));
#104596=DIRECTION('ref_axis',(-0.190809912898503,0.,0.981627005099017));
#104597=DIRECTION('',(0.,1.,0.));
#104598=DIRECTION('',(0.,1.,0.));
#104599=DIRECTION('center_axis',(0.,1.,0.));
#104600=DIRECTION('ref_axis',(1.,0.,0.));
#104601=DIRECTION('',(-0.190809912898503,0.,0.981627005099017));
#104602=DIRECTION('',(0.981627005099017,0.,0.190809912898503));
#104603=DIRECTION('',(-0.190809912898503,0.,0.981627005099017));
#104604=DIRECTION('',(0.981627005099017,0.,0.190809912898503));
#104605=DIRECTION('center_axis',(0.981627005099017,0.,0.190809912898503));
#104606=DIRECTION('ref_axis',(0.,-1.,0.));
#104607=DIRECTION('',(-0.190809912898503,0.,0.981627005099017));
#104608=DIRECTION('',(0.,-1.,0.));
#104609=DIRECTION('',(0.,-1.,0.));
#104610=DIRECTION('center_axis',(0.,-1.,0.));
#104611=DIRECTION('ref_axis',(0.,0.,-1.));
#104612=DIRECTION('',(-0.190809912898503,0.,0.981627005099017));
#104613=DIRECTION('',(-0.981627005099017,0.,-0.190809912898503));
#104614=DIRECTION('',(-0.981627005099017,0.,-0.190809912898503));
#104615=DIRECTION('center_axis',(-0.981627005099017,0.,-0.190809912898503));
#104616=DIRECTION('ref_axis',(-0.190809912898503,0.,0.981627005099017));
#104617=DIRECTION('',(0.,1.,0.));
#104618=DIRECTION('',(0.,1.,0.));
#104619=DIRECTION('center_axis',(0.,1.,0.));
#104620=DIRECTION('ref_axis',(1.,0.,0.));
#104621=DIRECTION('',(-0.190809912898503,0.,0.981627005099017));
#104622=DIRECTION('',(0.981627005099017,0.,0.190809912898503));
#104623=DIRECTION('',(-0.190809912898503,0.,0.981627005099017));
#104624=DIRECTION('',(0.981627005099017,0.,0.190809912898503));
#104625=DIRECTION('center_axis',(0.981627005099017,0.,0.190809912898503));
#104626=DIRECTION('ref_axis',(0.,-1.,0.));
#104627=DIRECTION('',(-0.190809912898503,0.,0.981627005099017));
#104628=DIRECTION('',(0.,-1.,0.));
#104629=DIRECTION('',(0.,-1.,0.));
#104630=DIRECTION('center_axis',(0.,-1.,0.));
#104631=DIRECTION('ref_axis',(0.,0.,-1.));
#104632=DIRECTION('',(-0.190809912898503,0.,0.981627005099017));
#104633=DIRECTION('',(-0.981627005099017,0.,-0.190809912898503));
#104634=DIRECTION('',(-0.981627005099017,0.,-0.190809912898503));
#104635=DIRECTION('center_axis',(-0.981627005099017,0.,-0.190809912898503));
#104636=DIRECTION('ref_axis',(-0.190809912898503,0.,0.981627005099017));
#104637=DIRECTION('',(0.,1.,0.));
#104638=DIRECTION('',(0.,1.,0.));
#104639=DIRECTION('center_axis',(0.,1.,0.));
#104640=DIRECTION('ref_axis',(1.,0.,0.));
#104641=DIRECTION('',(-0.190809912898503,0.,0.981627005099017));
#104642=DIRECTION('',(0.981627005099017,0.,0.190809912898503));
#104643=DIRECTION('',(-0.190809912898503,0.,0.981627005099017));
#104644=DIRECTION('',(0.981627005099017,0.,0.190809912898503));
#104645=DIRECTION('center_axis',(0.981627005099017,0.,0.190809912898503));
#104646=DIRECTION('ref_axis',(0.,-1.,0.));
#104647=DIRECTION('',(-0.190809912898503,0.,0.981627005099017));
#104648=DIRECTION('',(0.,-1.,0.));
#104649=DIRECTION('',(0.,-1.,0.));
#104650=DIRECTION('center_axis',(0.,-1.,0.));
#104651=DIRECTION('ref_axis',(0.,0.,-1.));
#104652=DIRECTION('',(-0.190809912898503,0.,0.981627005099017));
#104653=DIRECTION('',(-0.981627005099017,0.,-0.190809912898503));
#104654=DIRECTION('',(-0.981627005099017,0.,-0.190809912898503));
#104655=DIRECTION('center_axis',(-0.981627005099017,0.,-0.190809912898503));
#104656=DIRECTION('ref_axis',(-0.190809912898503,0.,0.981627005099017));
#104657=DIRECTION('',(0.,1.,0.));
#104658=DIRECTION('',(0.,1.,0.));
#104659=DIRECTION('center_axis',(0.,1.,0.));
#104660=DIRECTION('ref_axis',(1.,0.,0.));
#104661=DIRECTION('',(-0.190809912898503,0.,0.981627005099017));
#104662=DIRECTION('',(0.981627005099017,0.,0.190809912898503));
#104663=DIRECTION('',(-0.190809912898503,0.,0.981627005099017));
#104664=DIRECTION('',(0.981627005099017,0.,0.190809912898503));
#104665=DIRECTION('center_axis',(0.981627005099017,0.,0.190809912898503));
#104666=DIRECTION('ref_axis',(0.,-1.,0.));
#104667=DIRECTION('',(-0.190809912898503,0.,0.981627005099017));
#104668=DIRECTION('',(0.,-1.,0.));
#104669=DIRECTION('',(0.,-1.,0.));
#104670=DIRECTION('center_axis',(0.,-1.,0.));
#104671=DIRECTION('ref_axis',(0.,0.,-1.));
#104672=DIRECTION('',(-0.190809912898503,0.,0.981627005099017));
#104673=DIRECTION('',(-0.981627005099017,0.,-0.190809912898503));
#104674=DIRECTION('',(-0.981627005099017,0.,-0.190809912898503));
#104675=DIRECTION('center_axis',(-0.981627005099017,0.,-0.190809912898503));
#104676=DIRECTION('ref_axis',(-0.190809912898503,0.,0.981627005099017));
#104677=DIRECTION('',(0.,1.,0.));
#104678=DIRECTION('',(0.,1.,0.));
#104679=DIRECTION('center_axis',(0.,1.,0.));
#104680=DIRECTION('ref_axis',(1.,0.,0.));
#104681=DIRECTION('',(-0.190809912898503,0.,0.981627005099017));
#104682=DIRECTION('',(0.981627005099017,0.,0.190809912898503));
#104683=DIRECTION('',(-0.190809912898503,0.,0.981627005099017));
#104684=DIRECTION('',(0.981627005099017,0.,0.190809912898503));
#104685=DIRECTION('center_axis',(0.981627005099017,0.,0.190809912898503));
#104686=DIRECTION('ref_axis',(0.,-1.,0.));
#104687=DIRECTION('',(-0.190809912898503,0.,0.981627005099017));
#104688=DIRECTION('',(0.,-1.,0.));
#104689=DIRECTION('',(0.,-1.,0.));
#104690=DIRECTION('center_axis',(0.,-1.,0.));
#104691=DIRECTION('ref_axis',(0.,0.,-1.));
#104692=DIRECTION('',(-0.190809912898503,0.,0.981627005099017));
#104693=DIRECTION('',(-0.981627005099017,0.,-0.190809912898503));
#104694=DIRECTION('',(-0.981627005099017,0.,-0.190809912898503));
#104695=DIRECTION('center_axis',(-0.981627005099017,0.,-0.190809912898503));
#104696=DIRECTION('ref_axis',(-0.190809912898503,0.,0.981627005099017));
#104697=DIRECTION('',(0.,1.,0.));
#104698=DIRECTION('',(0.,1.,0.));
#104699=DIRECTION('center_axis',(0.,1.,0.));
#104700=DIRECTION('ref_axis',(1.,0.,0.));
#104701=DIRECTION('',(-0.190809912898503,0.,0.981627005099017));
#104702=DIRECTION('',(0.981627005099017,0.,0.190809912898503));
#104703=DIRECTION('',(-0.190809912898503,0.,0.981627005099017));
#104704=DIRECTION('',(0.981627005099017,0.,0.190809912898503));
#104705=DIRECTION('center_axis',(0.981627005099017,0.,0.190809912898503));
#104706=DIRECTION('ref_axis',(0.,-1.,0.));
#104707=DIRECTION('',(-0.190809912898503,0.,0.981627005099017));
#104708=DIRECTION('',(0.,-1.,0.));
#104709=DIRECTION('',(0.,-1.,0.));
#104710=DIRECTION('center_axis',(0.,-1.,0.));
#104711=DIRECTION('ref_axis',(0.,0.,-1.));
#104712=DIRECTION('',(-0.190809912898503,0.,0.981627005099017));
#104713=DIRECTION('',(-0.981627005099017,0.,-0.190809912898503));
#104714=DIRECTION('',(-0.981627005099017,0.,-0.190809912898503));
#104715=DIRECTION('center_axis',(-0.981627005099017,0.,-0.190809912898503));
#104716=DIRECTION('ref_axis',(-0.190809912898503,0.,0.981627005099017));
#104717=DIRECTION('',(0.,1.,0.));
#104718=DIRECTION('',(0.,1.,0.));
#104719=DIRECTION('center_axis',(0.,1.,0.));
#104720=DIRECTION('ref_axis',(1.,0.,0.));
#104721=DIRECTION('',(-0.190809912898503,0.,0.981627005099017));
#104722=DIRECTION('',(0.981627005099017,0.,0.190809912898503));
#104723=DIRECTION('',(-0.190809912898503,0.,0.981627005099017));
#104724=DIRECTION('',(0.981627005099017,0.,0.190809912898503));
#104725=DIRECTION('center_axis',(0.981627005099017,0.,0.190809912898503));
#104726=DIRECTION('ref_axis',(0.,-1.,0.));
#104727=DIRECTION('',(-0.190809912898503,0.,0.981627005099017));
#104728=DIRECTION('',(0.,-1.,0.));
#104729=DIRECTION('',(0.,-1.,0.));
#104730=DIRECTION('center_axis',(0.,-1.,0.));
#104731=DIRECTION('ref_axis',(0.,0.,-1.));
#104732=DIRECTION('',(-0.190809912898503,0.,0.981627005099017));
#104733=DIRECTION('',(-0.981627005099017,0.,-0.190809912898503));
#104734=DIRECTION('',(-0.981627005099017,0.,-0.190809912898503));
#104735=DIRECTION('center_axis',(-0.981627005099017,0.,-0.190809912898503));
#104736=DIRECTION('ref_axis',(-0.190809912898503,0.,0.981627005099017));
#104737=DIRECTION('',(0.,1.,0.));
#104738=DIRECTION('',(0.,1.,0.));
#104739=DIRECTION('center_axis',(0.,1.,0.));
#104740=DIRECTION('ref_axis',(1.,0.,0.));
#104741=DIRECTION('',(-0.190809912898503,0.,0.981627005099017));
#104742=DIRECTION('',(0.981627005099017,0.,0.190809912898503));
#104743=DIRECTION('',(-0.190809912898503,0.,0.981627005099017));
#104744=DIRECTION('',(0.981627005099017,0.,0.190809912898503));
#104745=DIRECTION('center_axis',(0.981627005099017,0.,0.190809912898503));
#104746=DIRECTION('ref_axis',(0.,-1.,0.));
#104747=DIRECTION('',(-0.190809912898503,0.,0.981627005099017));
#104748=DIRECTION('',(0.,-1.,0.));
#104749=DIRECTION('',(0.,-1.,0.));
#104750=DIRECTION('center_axis',(0.,-1.,0.));
#104751=DIRECTION('ref_axis',(0.,0.,-1.));
#104752=DIRECTION('',(-0.190809912898503,0.,0.981627005099017));
#104753=DIRECTION('',(-0.981627005099017,0.,-0.190809912898503));
#104754=DIRECTION('',(-0.981627005099017,0.,-0.190809912898503));
#104755=DIRECTION('center_axis',(-0.981627005099017,0.,-0.190809912898503));
#104756=DIRECTION('ref_axis',(-0.190809912898503,0.,0.981627005099017));
#104757=DIRECTION('',(0.,1.,0.));
#104758=DIRECTION('',(0.,1.,0.));
#104759=DIRECTION('center_axis',(0.,1.,0.));
#104760=DIRECTION('ref_axis',(1.,0.,0.));
#104761=DIRECTION('',(-0.190809912898503,0.,0.981627005099017));
#104762=DIRECTION('',(0.981627005099017,0.,0.190809912898503));
#104763=DIRECTION('',(-0.190809912898503,0.,0.981627005099017));
#104764=DIRECTION('',(0.981627005099017,0.,0.190809912898503));
#104765=DIRECTION('center_axis',(0.981627005099017,0.,0.190809912898503));
#104766=DIRECTION('ref_axis',(0.,-1.,0.));
#104767=DIRECTION('',(-0.190809912898503,0.,0.981627005099017));
#104768=DIRECTION('',(0.,-1.,0.));
#104769=DIRECTION('',(0.,-1.,0.));
#104770=DIRECTION('center_axis',(0.,-1.,0.));
#104771=DIRECTION('ref_axis',(0.,0.,-1.));
#104772=DIRECTION('',(-0.190809912898503,0.,0.981627005099017));
#104773=DIRECTION('',(-0.981627005099017,0.,-0.190809912898503));
#104774=DIRECTION('',(-0.981627005099017,0.,-0.190809912898503));
#104775=DIRECTION('center_axis',(-0.981627005099017,0.,-0.190809912898503));
#104776=DIRECTION('ref_axis',(-0.190809912898503,0.,0.981627005099017));
#104777=DIRECTION('',(0.,1.,0.));
#104778=DIRECTION('',(0.,1.,0.));
#104779=DIRECTION('center_axis',(0.,1.,0.));
#104780=DIRECTION('ref_axis',(1.,0.,0.));
#104781=DIRECTION('',(-0.190809912898503,0.,0.981627005099017));
#104782=DIRECTION('',(0.981627005099017,0.,0.190809912898503));
#104783=DIRECTION('',(-0.190809912898503,0.,0.981627005099017));
#104784=DIRECTION('',(0.981627005099017,0.,0.190809912898503));
#104785=DIRECTION('center_axis',(0.981627005099017,0.,0.190809912898503));
#104786=DIRECTION('ref_axis',(0.,-1.,0.));
#104787=DIRECTION('',(-0.190809912898503,0.,0.981627005099017));
#104788=DIRECTION('',(0.,-1.,0.));
#104789=DIRECTION('',(0.,-1.,0.));
#104790=DIRECTION('center_axis',(0.,-1.,0.));
#104791=DIRECTION('ref_axis',(0.,0.,-1.));
#104792=DIRECTION('',(-0.190809912898503,0.,0.981627005099017));
#104793=DIRECTION('',(-0.981627005099017,0.,-0.190809912898503));
#104794=DIRECTION('',(-0.981627005099017,0.,-0.190809912898503));
#104795=DIRECTION('center_axis',(-0.981627005099017,0.,-0.190809912898503));
#104796=DIRECTION('ref_axis',(-0.190809912898503,0.,0.981627005099017));
#104797=DIRECTION('',(0.,1.,0.));
#104798=DIRECTION('',(0.,1.,0.));
#104799=DIRECTION('center_axis',(0.,1.,0.));
#104800=DIRECTION('ref_axis',(1.,0.,0.));
#104801=DIRECTION('',(-0.190809912898503,0.,0.981627005099017));
#104802=DIRECTION('',(0.981627005099017,0.,0.190809912898503));
#104803=DIRECTION('',(-0.190809912898503,0.,0.981627005099017));
#104804=DIRECTION('',(0.981627005099017,0.,0.190809912898503));
#104805=DIRECTION('center_axis',(0.981627005099017,0.,0.190809912898503));
#104806=DIRECTION('ref_axis',(0.,-1.,0.));
#104807=DIRECTION('',(-0.190809912898503,0.,0.981627005099017));
#104808=DIRECTION('',(0.,-1.,0.));
#104809=DIRECTION('',(0.,-1.,0.));
#104810=DIRECTION('center_axis',(0.,-1.,0.));
#104811=DIRECTION('ref_axis',(0.,0.,-1.));
#104812=DIRECTION('',(-0.190809912898503,0.,0.981627005099017));
#104813=DIRECTION('',(-0.981627005099017,0.,-0.190809912898503));
#104814=DIRECTION('',(-0.981627005099017,0.,-0.190809912898503));
#104815=DIRECTION('center_axis',(-0.981627005099017,0.,-0.190809912898503));
#104816=DIRECTION('ref_axis',(-0.190809912898503,0.,0.981627005099017));
#104817=DIRECTION('',(0.,1.,0.));
#104818=DIRECTION('',(0.,1.,0.));
#104819=DIRECTION('center_axis',(0.,1.,0.));
#104820=DIRECTION('ref_axis',(1.,0.,0.));
#104821=DIRECTION('',(-0.190809912898503,0.,0.981627005099017));
#104822=DIRECTION('',(0.981627005099017,0.,0.190809912898503));
#104823=DIRECTION('',(-0.190809912898503,0.,0.981627005099017));
#104824=DIRECTION('',(0.981627005099017,0.,0.190809912898503));
#104825=DIRECTION('center_axis',(0.981627005099017,0.,0.190809912898503));
#104826=DIRECTION('ref_axis',(0.,-1.,0.));
#104827=DIRECTION('',(-0.190809912898503,0.,0.981627005099017));
#104828=DIRECTION('',(0.,-1.,0.));
#104829=DIRECTION('',(0.,-1.,0.));
#104830=DIRECTION('center_axis',(0.,-1.,0.));
#104831=DIRECTION('ref_axis',(0.,0.,-1.));
#104832=DIRECTION('',(-0.190809912898503,0.,0.981627005099017));
#104833=DIRECTION('',(-0.981627005099017,0.,-0.190809912898503));
#104834=DIRECTION('',(-0.981627005099017,0.,-0.190809912898503));
#104835=DIRECTION('center_axis',(-0.981627005099017,0.,-0.190809912898503));
#104836=DIRECTION('ref_axis',(-0.190809912898503,0.,0.981627005099017));
#104837=DIRECTION('',(0.,1.,0.));
#104838=DIRECTION('',(0.,1.,0.));
#104839=DIRECTION('center_axis',(0.,1.,0.));
#104840=DIRECTION('ref_axis',(1.,0.,0.));
#104841=DIRECTION('',(-0.190809912898503,0.,0.981627005099017));
#104842=DIRECTION('',(0.981627005099017,0.,0.190809912898503));
#104843=DIRECTION('',(-0.190809912898503,0.,0.981627005099017));
#104844=DIRECTION('',(0.981627005099017,0.,0.190809912898503));
#104845=DIRECTION('center_axis',(0.981627005099017,0.,0.190809912898503));
#104846=DIRECTION('ref_axis',(0.,-1.,0.));
#104847=DIRECTION('',(-0.190809912898503,0.,0.981627005099017));
#104848=DIRECTION('',(0.,-1.,0.));
#104849=DIRECTION('',(0.,-1.,0.));
#104850=DIRECTION('center_axis',(0.,-1.,0.));
#104851=DIRECTION('ref_axis',(0.,0.,-1.));
#104852=DIRECTION('',(-0.190809912898503,0.,0.981627005099017));
#104853=DIRECTION('',(-0.981627005099017,0.,-0.190809912898503));
#104854=DIRECTION('',(-0.981627005099017,0.,-0.190809912898503));
#104855=DIRECTION('center_axis',(-0.981627005099017,0.,-0.190809912898503));
#104856=DIRECTION('ref_axis',(-0.190809912898503,0.,0.981627005099017));
#104857=DIRECTION('',(0.,1.,0.));
#104858=DIRECTION('',(0.,1.,0.));
#104859=DIRECTION('center_axis',(0.,1.,0.));
#104860=DIRECTION('ref_axis',(1.,0.,0.));
#104861=DIRECTION('',(-0.190809912898503,0.,0.981627005099017));
#104862=DIRECTION('',(0.981627005099017,0.,0.190809912898503));
#104863=DIRECTION('',(-0.190809912898503,0.,0.981627005099017));
#104864=DIRECTION('',(0.981627005099017,0.,0.190809912898503));
#104865=DIRECTION('center_axis',(0.981627005099017,0.,0.190809912898503));
#104866=DIRECTION('ref_axis',(0.,-1.,0.));
#104867=DIRECTION('',(-0.190809912898503,0.,0.981627005099017));
#104868=DIRECTION('',(0.,-1.,0.));
#104869=DIRECTION('',(0.,-1.,0.));
#104870=DIRECTION('center_axis',(0.,-1.,0.));
#104871=DIRECTION('ref_axis',(0.,0.,-1.));
#104872=DIRECTION('',(-0.190809912898503,0.,0.981627005099017));
#104873=DIRECTION('',(-0.981627005099017,0.,-0.190809912898503));
#104874=DIRECTION('',(-0.981627005099017,0.,-0.190809912898503));
#104875=DIRECTION('center_axis',(-0.981627005099017,0.,-0.190809912898503));
#104876=DIRECTION('ref_axis',(-0.190809912898503,0.,0.981627005099017));
#104877=DIRECTION('',(0.,1.,0.));
#104878=DIRECTION('',(0.,1.,0.));
#104879=DIRECTION('center_axis',(0.,1.,0.));
#104880=DIRECTION('ref_axis',(1.,0.,0.));
#104881=DIRECTION('',(-0.190809912898503,0.,0.981627005099017));
#104882=DIRECTION('',(0.981627005099017,0.,0.190809912898503));
#104883=DIRECTION('',(-0.190809912898503,0.,0.981627005099017));
#104884=DIRECTION('',(0.981627005099017,0.,0.190809912898503));
#104885=DIRECTION('center_axis',(0.981627005099017,0.,0.190809912898503));
#104886=DIRECTION('ref_axis',(0.,-1.,0.));
#104887=DIRECTION('',(-0.190809912898503,0.,0.981627005099017));
#104888=DIRECTION('',(0.,-1.,0.));
#104889=DIRECTION('',(0.,-1.,0.));
#104890=DIRECTION('center_axis',(0.,-1.,0.));
#104891=DIRECTION('ref_axis',(0.,0.,-1.));
#104892=DIRECTION('',(-0.190809912898503,0.,0.981627005099017));
#104893=DIRECTION('',(-0.981627005099017,0.,-0.190809912898503));
#104894=DIRECTION('',(-0.981627005099017,0.,-0.190809912898503));
#104895=DIRECTION('center_axis',(-0.981627005099017,0.,-0.190809912898503));
#104896=DIRECTION('ref_axis',(-0.190809912898503,0.,0.981627005099017));
#104897=DIRECTION('',(0.,1.,0.));
#104898=DIRECTION('',(0.,1.,0.));
#104899=DIRECTION('center_axis',(0.,1.,0.));
#104900=DIRECTION('ref_axis',(1.,0.,0.));
#104901=DIRECTION('',(-0.190809912898503,0.,0.981627005099017));
#104902=DIRECTION('',(0.981627005099017,0.,0.190809912898503));
#104903=DIRECTION('',(-0.190809912898503,0.,0.981627005099017));
#104904=DIRECTION('',(0.981627005099017,0.,0.190809912898503));
#104905=DIRECTION('center_axis',(0.981627005099017,0.,0.190809912898503));
#104906=DIRECTION('ref_axis',(0.,-1.,0.));
#104907=DIRECTION('',(-0.190809912898503,0.,0.981627005099017));
#104908=DIRECTION('',(0.,-1.,0.));
#104909=DIRECTION('',(0.,-1.,0.));
#104910=DIRECTION('center_axis',(0.,-1.,0.));
#104911=DIRECTION('ref_axis',(0.,0.,-1.));
#104912=DIRECTION('',(-0.190809912898503,0.,0.981627005099017));
#104913=DIRECTION('',(-0.981627005099017,0.,-0.190809912898503));
#104914=DIRECTION('',(-0.981627005099017,0.,-0.190809912898503));
#104915=DIRECTION('center_axis',(-0.981627005099017,0.,-0.190809912898503));
#104916=DIRECTION('ref_axis',(-0.190809912898503,0.,0.981627005099017));
#104917=DIRECTION('',(0.,1.,0.));
#104918=DIRECTION('',(0.,1.,0.));
#104919=DIRECTION('center_axis',(0.,1.,0.));
#104920=DIRECTION('ref_axis',(1.,0.,0.));
#104921=DIRECTION('',(-0.190809912898503,0.,0.981627005099017));
#104922=DIRECTION('',(0.981627005099017,0.,0.190809912898503));
#104923=DIRECTION('',(-0.190809912898503,0.,0.981627005099017));
#104924=DIRECTION('',(0.981627005099017,0.,0.190809912898503));
#104925=DIRECTION('center_axis',(0.981627005099017,0.,0.190809912898503));
#104926=DIRECTION('ref_axis',(0.,-1.,0.));
#104927=DIRECTION('',(-0.190809912898503,0.,0.981627005099017));
#104928=DIRECTION('',(0.,-1.,0.));
#104929=DIRECTION('',(0.,-1.,0.));
#104930=DIRECTION('center_axis',(0.,-1.,0.));
#104931=DIRECTION('ref_axis',(0.,0.,-1.));
#104932=DIRECTION('',(-0.190809912898503,0.,0.981627005099017));
#104933=DIRECTION('',(-0.981627005099017,0.,-0.190809912898503));
#104934=DIRECTION('',(-0.981627005099017,0.,-0.190809912898503));
#104935=DIRECTION('center_axis',(-0.981627005099017,0.,-0.190809912898503));
#104936=DIRECTION('ref_axis',(-0.190809912898503,0.,0.981627005099017));
#104937=DIRECTION('',(0.,1.,0.));
#104938=DIRECTION('',(0.,1.,0.));
#104939=DIRECTION('center_axis',(0.,1.,0.));
#104940=DIRECTION('ref_axis',(1.,0.,0.));
#104941=DIRECTION('',(-0.190809912898503,0.,0.981627005099017));
#104942=DIRECTION('',(0.981627005099017,0.,0.190809912898503));
#104943=DIRECTION('',(-0.190809912898503,0.,0.981627005099017));
#104944=DIRECTION('',(0.981627005099017,0.,0.190809912898503));
#104945=DIRECTION('center_axis',(0.981627005099017,0.,0.190809912898503));
#104946=DIRECTION('ref_axis',(0.,-1.,0.));
#104947=DIRECTION('',(-0.190809912898503,0.,0.981627005099017));
#104948=DIRECTION('',(0.,-1.,0.));
#104949=DIRECTION('',(0.,-1.,0.));
#104950=DIRECTION('center_axis',(0.,-1.,0.));
#104951=DIRECTION('ref_axis',(0.,0.,-1.));
#104952=DIRECTION('',(-0.190809912898503,0.,0.981627005099017));
#104953=DIRECTION('',(-0.981627005099017,0.,-0.190809912898503));
#104954=DIRECTION('',(-0.981627005099017,0.,-0.190809912898503));
#104955=DIRECTION('center_axis',(-0.981627005099017,0.,-0.190809912898503));
#104956=DIRECTION('ref_axis',(-0.190809912898503,0.,0.981627005099017));
#104957=DIRECTION('',(0.,1.,0.));
#104958=DIRECTION('',(0.,1.,0.));
#104959=DIRECTION('center_axis',(0.,1.,0.));
#104960=DIRECTION('ref_axis',(1.,0.,0.));
#104961=DIRECTION('',(-0.190809912898503,0.,0.981627005099017));
#104962=DIRECTION('',(0.981627005099017,0.,0.190809912898503));
#104963=DIRECTION('',(-0.190809912898503,0.,0.981627005099017));
#104964=DIRECTION('',(0.981627005099017,0.,0.190809912898503));
#104965=DIRECTION('center_axis',(0.981627005099017,0.,0.190809912898503));
#104966=DIRECTION('ref_axis',(0.,-1.,0.));
#104967=DIRECTION('',(-0.190809912898503,0.,0.981627005099017));
#104968=DIRECTION('',(0.,-1.,0.));
#104969=DIRECTION('',(0.,-1.,0.));
#104970=DIRECTION('center_axis',(0.,-1.,0.));
#104971=DIRECTION('ref_axis',(0.,0.,-1.));
#104972=DIRECTION('',(-0.190809912898503,0.,0.981627005099017));
#104973=DIRECTION('',(-0.981627005099017,0.,-0.190809912898503));
#104974=DIRECTION('',(-0.981627005099017,0.,-0.190809912898503));
#104975=DIRECTION('center_axis',(-0.981627005099017,0.,-0.190809912898503));
#104976=DIRECTION('ref_axis',(-0.190809912898503,0.,0.981627005099017));
#104977=DIRECTION('',(0.,1.,0.));
#104978=DIRECTION('',(0.,1.,0.));
#104979=DIRECTION('center_axis',(0.,1.,0.));
#104980=DIRECTION('ref_axis',(1.,0.,0.));
#104981=DIRECTION('',(-0.190809912898503,0.,0.981627005099017));
#104982=DIRECTION('',(0.981627005099017,0.,0.190809912898503));
#104983=DIRECTION('',(-0.190809912898503,0.,0.981627005099017));
#104984=DIRECTION('',(0.981627005099017,0.,0.190809912898503));
#104985=DIRECTION('center_axis',(0.981627005099017,0.,0.190809912898503));
#104986=DIRECTION('ref_axis',(0.,-1.,0.));
#104987=DIRECTION('',(-0.190809912898503,0.,0.981627005099017));
#104988=DIRECTION('',(0.,-1.,0.));
#104989=DIRECTION('',(0.,-1.,0.));
#104990=DIRECTION('center_axis',(0.,-1.,0.));
#104991=DIRECTION('ref_axis',(0.,0.,-1.));
#104992=DIRECTION('',(-0.190809912898503,0.,0.981627005099017));
#104993=DIRECTION('',(-0.981627005099017,0.,-0.190809912898503));
#104994=DIRECTION('',(-0.981627005099017,0.,-0.190809912898503));
#104995=DIRECTION('center_axis',(-0.981627005099017,0.,-0.190809912898503));
#104996=DIRECTION('ref_axis',(-0.190809912898503,0.,0.981627005099017));
#104997=DIRECTION('',(0.,1.,0.));
#104998=DIRECTION('',(0.,1.,0.));
#104999=DIRECTION('center_axis',(0.,1.,0.));
#105000=DIRECTION('ref_axis',(1.,0.,0.));
#105001=DIRECTION('',(-0.190809912898503,0.,0.981627005099017));
#105002=DIRECTION('',(0.981627005099017,0.,0.190809912898503));
#105003=DIRECTION('',(-0.190809912898503,0.,0.981627005099017));
#105004=DIRECTION('',(0.981627005099017,0.,0.190809912898503));
#105005=DIRECTION('center_axis',(0.981627005099017,0.,0.190809912898503));
#105006=DIRECTION('ref_axis',(0.,-1.,0.));
#105007=DIRECTION('',(-0.190809912898503,0.,0.981627005099017));
#105008=DIRECTION('',(0.,-1.,0.));
#105009=DIRECTION('',(0.,-1.,0.));
#105010=DIRECTION('center_axis',(0.,-1.,0.));
#105011=DIRECTION('ref_axis',(0.,0.,-1.));
#105012=DIRECTION('',(-0.190809912898503,0.,0.981627005099017));
#105013=DIRECTION('',(-0.981627005099017,0.,-0.190809912898503));
#105014=DIRECTION('',(-0.981627005099017,0.,-0.190809912898503));
#105015=DIRECTION('center_axis',(-0.981627005099017,0.,-0.190809912898503));
#105016=DIRECTION('ref_axis',(-0.190809912898503,0.,0.981627005099017));
#105017=DIRECTION('',(0.,1.,0.));
#105018=DIRECTION('',(0.,1.,0.));
#105019=DIRECTION('center_axis',(0.,1.,0.));
#105020=DIRECTION('ref_axis',(1.,0.,0.));
#105021=DIRECTION('',(-0.190809912898503,0.,0.981627005099017));
#105022=DIRECTION('',(0.981627005099017,0.,0.190809912898503));
#105023=DIRECTION('',(-0.190809912898503,0.,0.981627005099017));
#105024=DIRECTION('',(0.981627005099017,0.,0.190809912898503));
#105025=DIRECTION('center_axis',(0.981627005099017,0.,0.190809912898503));
#105026=DIRECTION('ref_axis',(0.,-1.,0.));
#105027=DIRECTION('',(-0.190809912898503,0.,0.981627005099017));
#105028=DIRECTION('',(0.,-1.,0.));
#105029=DIRECTION('',(0.,-1.,0.));
#105030=DIRECTION('center_axis',(0.,-1.,0.));
#105031=DIRECTION('ref_axis',(0.,0.,-1.));
#105032=DIRECTION('',(-0.190809912898503,0.,0.981627005099017));
#105033=DIRECTION('',(-0.981627005099017,0.,-0.190809912898503));
#105034=DIRECTION('',(-0.981627005099017,0.,-0.190809912898503));
#105035=DIRECTION('center_axis',(-0.981627005099017,0.,-0.190809912898503));
#105036=DIRECTION('ref_axis',(-0.190809912898503,0.,0.981627005099017));
#105037=DIRECTION('',(0.,1.,0.));
#105038=DIRECTION('',(0.,1.,0.));
#105039=DIRECTION('center_axis',(0.,1.,0.));
#105040=DIRECTION('ref_axis',(1.,0.,0.));
#105041=DIRECTION('',(-0.190809912898503,0.,0.981627005099017));
#105042=DIRECTION('',(0.981627005099017,0.,0.190809912898503));
#105043=DIRECTION('',(-0.190809912898503,0.,0.981627005099017));
#105044=DIRECTION('',(0.981627005099017,0.,0.190809912898503));
#105045=DIRECTION('center_axis',(0.981627005099017,0.,0.190809912898503));
#105046=DIRECTION('ref_axis',(0.,-1.,0.));
#105047=DIRECTION('',(-0.190809912898503,0.,0.981627005099017));
#105048=DIRECTION('',(0.,-1.,0.));
#105049=DIRECTION('',(0.,-1.,0.));
#105050=DIRECTION('center_axis',(0.,-1.,0.));
#105051=DIRECTION('ref_axis',(0.,0.,-1.));
#105052=DIRECTION('',(-0.190809912898503,0.,0.981627005099017));
#105053=DIRECTION('',(-0.981627005099017,0.,-0.190809912898503));
#105054=DIRECTION('',(-0.981627005099017,0.,-0.190809912898503));
#105055=DIRECTION('center_axis',(-0.981627005099017,0.,-0.190809912898503));
#105056=DIRECTION('ref_axis',(-0.190809912898503,0.,0.981627005099017));
#105057=DIRECTION('',(0.,1.,0.));
#105058=DIRECTION('',(0.,1.,0.));
#105059=DIRECTION('center_axis',(0.,1.,0.));
#105060=DIRECTION('ref_axis',(1.,0.,0.));
#105061=DIRECTION('',(-0.190809912898503,0.,0.981627005099017));
#105062=DIRECTION('',(0.981627005099017,0.,0.190809912898503));
#105063=DIRECTION('',(-0.190809912898503,0.,0.981627005099017));
#105064=DIRECTION('',(0.981627005099017,0.,0.190809912898503));
#105065=DIRECTION('center_axis',(0.981627005099017,0.,0.190809912898503));
#105066=DIRECTION('ref_axis',(0.,-1.,0.));
#105067=DIRECTION('',(-0.190809912898503,0.,0.981627005099017));
#105068=DIRECTION('',(0.,-1.,0.));
#105069=DIRECTION('',(0.,-1.,0.));
#105070=DIRECTION('center_axis',(0.,-1.,0.));
#105071=DIRECTION('ref_axis',(0.,0.,-1.));
#105072=DIRECTION('',(-0.190809912898503,0.,0.981627005099017));
#105073=DIRECTION('',(-0.981627005099017,0.,-0.190809912898503));
#105074=DIRECTION('',(-0.981627005099017,0.,-0.190809912898503));
#105075=DIRECTION('center_axis',(-0.981627005099017,0.,-0.190809912898503));
#105076=DIRECTION('ref_axis',(-0.190809912898503,0.,0.981627005099017));
#105077=DIRECTION('',(0.,1.,0.));
#105078=DIRECTION('',(0.,1.,0.));
#105079=DIRECTION('center_axis',(0.,1.,0.));
#105080=DIRECTION('ref_axis',(1.,0.,0.));
#105081=DIRECTION('',(-0.190809912898503,0.,0.981627005099017));
#105082=DIRECTION('',(0.981627005099017,0.,0.190809912898503));
#105083=DIRECTION('',(-0.190809912898503,0.,0.981627005099017));
#105084=DIRECTION('',(0.981627005099017,0.,0.190809912898503));
#105085=DIRECTION('center_axis',(0.981627005099017,0.,0.190809912898503));
#105086=DIRECTION('ref_axis',(0.,-1.,0.));
#105087=DIRECTION('',(-0.190809912898503,0.,0.981627005099017));
#105088=DIRECTION('',(0.,-1.,0.));
#105089=DIRECTION('',(0.,-1.,0.));
#105090=DIRECTION('center_axis',(0.,-1.,0.));
#105091=DIRECTION('ref_axis',(0.,0.,-1.));
#105092=DIRECTION('',(-0.190809912898503,0.,0.981627005099017));
#105093=DIRECTION('',(-0.981627005099017,0.,-0.190809912898503));
#105094=DIRECTION('',(-0.981627005099017,0.,-0.190809912898503));
#105095=DIRECTION('center_axis',(-0.981627005099017,0.,-0.190809912898503));
#105096=DIRECTION('ref_axis',(-0.190809912898503,0.,0.981627005099017));
#105097=DIRECTION('',(0.,1.,0.));
#105098=DIRECTION('',(0.,1.,0.));
#105099=DIRECTION('center_axis',(0.,1.,0.));
#105100=DIRECTION('ref_axis',(1.,0.,0.));
#105101=DIRECTION('',(-0.190809912898503,0.,0.981627005099017));
#105102=DIRECTION('',(0.981627005099017,0.,0.190809912898503));
#105103=DIRECTION('',(-0.190809912898503,0.,0.981627005099017));
#105104=DIRECTION('',(0.981627005099017,0.,0.190809912898503));
#105105=DIRECTION('center_axis',(0.981627005099017,0.,0.190809912898503));
#105106=DIRECTION('ref_axis',(0.,-1.,0.));
#105107=DIRECTION('',(-0.190809912898503,0.,0.981627005099017));
#105108=DIRECTION('',(0.,-1.,0.));
#105109=DIRECTION('',(0.,-1.,0.));
#105110=DIRECTION('center_axis',(0.,-1.,0.));
#105111=DIRECTION('ref_axis',(0.,0.,-1.));
#105112=DIRECTION('',(-0.190809912898503,0.,0.981627005099017));
#105113=DIRECTION('',(-0.981627005099017,0.,-0.190809912898503));
#105114=DIRECTION('',(-0.981627005099017,0.,-0.190809912898503));
#105115=DIRECTION('center_axis',(-0.981627005099017,0.,-0.190809912898503));
#105116=DIRECTION('ref_axis',(-0.190809912898503,0.,0.981627005099017));
#105117=DIRECTION('',(0.,1.,0.));
#105118=DIRECTION('',(0.,1.,0.));
#105119=DIRECTION('center_axis',(0.,1.,0.));
#105120=DIRECTION('ref_axis',(1.,0.,0.));
#105121=DIRECTION('',(-0.190809912898503,0.,0.981627005099017));
#105122=DIRECTION('',(0.981627005099017,0.,0.190809912898503));
#105123=DIRECTION('',(-0.190809912898503,0.,0.981627005099017));
#105124=DIRECTION('',(0.981627005099017,0.,0.190809912898503));
#105125=DIRECTION('center_axis',(0.981627005099017,0.,0.190809912898503));
#105126=DIRECTION('ref_axis',(0.,-1.,0.));
#105127=DIRECTION('',(-0.190809912898503,0.,0.981627005099017));
#105128=DIRECTION('',(0.,-1.,0.));
#105129=DIRECTION('',(0.,-1.,0.));
#105130=DIRECTION('center_axis',(0.,-1.,0.));
#105131=DIRECTION('ref_axis',(0.,0.,-1.));
#105132=DIRECTION('',(-0.190809912898503,0.,0.981627005099017));
#105133=DIRECTION('',(-0.981627005099017,0.,-0.190809912898503));
#105134=DIRECTION('',(-0.981627005099017,0.,-0.190809912898503));
#105135=DIRECTION('center_axis',(-0.981627005099017,0.,-0.190809912898503));
#105136=DIRECTION('ref_axis',(-0.190809912898503,0.,0.981627005099017));
#105137=DIRECTION('',(0.,1.,0.));
#105138=DIRECTION('',(0.,1.,0.));
#105139=DIRECTION('center_axis',(0.,1.,0.));
#105140=DIRECTION('ref_axis',(1.,0.,0.));
#105141=DIRECTION('',(-0.190809912898503,0.,0.981627005099017));
#105142=DIRECTION('',(0.981627005099017,0.,0.190809912898503));
#105143=DIRECTION('',(-0.190809912898503,0.,0.981627005099017));
#105144=DIRECTION('',(0.981627005099017,0.,0.190809912898503));
#105145=DIRECTION('center_axis',(0.981627005099017,0.,0.190809912898503));
#105146=DIRECTION('ref_axis',(0.,-1.,0.));
#105147=DIRECTION('',(-0.190809912898503,0.,0.981627005099017));
#105148=DIRECTION('',(0.,-1.,0.));
#105149=DIRECTION('',(0.,-1.,0.));
#105150=DIRECTION('center_axis',(0.,-1.,0.));
#105151=DIRECTION('ref_axis',(0.,0.,-1.));
#105152=DIRECTION('',(-0.190809912898503,0.,0.981627005099017));
#105153=DIRECTION('',(-0.981627005099017,0.,-0.190809912898503));
#105154=DIRECTION('',(-0.981627005099017,0.,-0.190809912898503));
#105155=DIRECTION('center_axis',(-0.981627005099017,0.,-0.190809912898503));
#105156=DIRECTION('ref_axis',(-0.190809912898503,0.,0.981627005099017));
#105157=DIRECTION('',(0.,1.,0.));
#105158=DIRECTION('',(0.,1.,0.));
#105159=DIRECTION('center_axis',(0.,1.,0.));
#105160=DIRECTION('ref_axis',(1.,0.,0.));
#105161=DIRECTION('',(-0.190809912898503,0.,0.981627005099017));
#105162=DIRECTION('',(0.981627005099017,0.,0.190809912898503));
#105163=DIRECTION('',(-0.190809912898503,0.,0.981627005099017));
#105164=DIRECTION('',(0.981627005099017,0.,0.190809912898503));
#105165=DIRECTION('center_axis',(0.981627005099017,0.,0.190809912898503));
#105166=DIRECTION('ref_axis',(0.,-1.,0.));
#105167=DIRECTION('',(-0.190809912898503,0.,0.981627005099017));
#105168=DIRECTION('',(0.,-1.,0.));
#105169=DIRECTION('',(0.,-1.,0.));
#105170=DIRECTION('center_axis',(0.,-1.,0.));
#105171=DIRECTION('ref_axis',(0.,0.,-1.));
#105172=DIRECTION('',(-0.190809912898503,0.,0.981627005099017));
#105173=DIRECTION('',(-0.981627005099017,0.,-0.190809912898503));
#105174=DIRECTION('',(-0.981627005099017,0.,-0.190809912898503));
#105175=DIRECTION('center_axis',(-0.981627005099017,0.,-0.190809912898503));
#105176=DIRECTION('ref_axis',(-0.190809912898503,0.,0.981627005099017));
#105177=DIRECTION('',(0.,1.,0.));
#105178=DIRECTION('',(0.,1.,0.));
#105179=DIRECTION('center_axis',(0.,1.,0.));
#105180=DIRECTION('ref_axis',(1.,0.,0.));
#105181=DIRECTION('',(-0.190809912898503,0.,0.981627005099017));
#105182=DIRECTION('',(0.981627005099017,0.,0.190809912898503));
#105183=DIRECTION('',(-0.190809912898503,0.,0.981627005099017));
#105184=DIRECTION('',(0.981627005099017,0.,0.190809912898503));
#105185=DIRECTION('center_axis',(0.981627005099017,0.,0.190809912898503));
#105186=DIRECTION('ref_axis',(0.,-1.,0.));
#105187=DIRECTION('',(-0.190809912898503,0.,0.981627005099017));
#105188=DIRECTION('',(0.,-1.,0.));
#105189=DIRECTION('',(0.,-1.,0.));
#105190=DIRECTION('center_axis',(0.,-1.,0.));
#105191=DIRECTION('ref_axis',(0.,0.,-1.));
#105192=DIRECTION('',(-0.190809912898503,0.,0.981627005099017));
#105193=DIRECTION('',(-0.981627005099017,0.,-0.190809912898503));
#105194=DIRECTION('',(-0.981627005099017,0.,-0.190809912898503));
#105195=DIRECTION('center_axis',(-0.981627005099017,0.,-0.190809912898503));
#105196=DIRECTION('ref_axis',(-0.190809912898503,0.,0.981627005099017));
#105197=DIRECTION('',(0.,1.,0.));
#105198=DIRECTION('',(0.,1.,0.));
#105199=DIRECTION('center_axis',(0.,1.,0.));
#105200=DIRECTION('ref_axis',(1.,0.,0.));
#105201=DIRECTION('',(-0.190809912898503,0.,0.981627005099017));
#105202=DIRECTION('',(0.981627005099017,0.,0.190809912898503));
#105203=DIRECTION('',(-0.190809912898503,0.,0.981627005099017));
#105204=DIRECTION('',(0.981627005099017,0.,0.190809912898503));
#105205=DIRECTION('center_axis',(0.981627005099017,0.,0.190809912898503));
#105206=DIRECTION('ref_axis',(0.,-1.,0.));
#105207=DIRECTION('',(-0.190809912898503,0.,0.981627005099017));
#105208=DIRECTION('',(0.,-1.,0.));
#105209=DIRECTION('',(0.,-1.,0.));
#105210=DIRECTION('center_axis',(0.,-1.,0.));
#105211=DIRECTION('ref_axis',(0.,0.,-1.));
#105212=DIRECTION('',(-0.190809912898503,0.,0.981627005099017));
#105213=DIRECTION('',(-0.981627005099017,0.,-0.190809912898503));
#105214=DIRECTION('',(-0.981627005099017,0.,-0.190809912898503));
#105215=DIRECTION('center_axis',(-0.981627005099017,0.,-0.190809912898503));
#105216=DIRECTION('ref_axis',(-0.190809912898503,0.,0.981627005099017));
#105217=DIRECTION('',(0.,1.,0.));
#105218=DIRECTION('',(0.,1.,0.));
#105219=DIRECTION('center_axis',(0.,1.,0.));
#105220=DIRECTION('ref_axis',(1.,0.,0.));
#105221=DIRECTION('',(-0.190809912898503,0.,0.981627005099017));
#105222=DIRECTION('',(0.981627005099017,0.,0.190809912898503));
#105223=DIRECTION('',(-0.190809912898503,0.,0.981627005099017));
#105224=DIRECTION('',(0.981627005099017,0.,0.190809912898503));
#105225=DIRECTION('center_axis',(0.981627005099017,0.,0.190809912898503));
#105226=DIRECTION('ref_axis',(0.,-1.,0.));
#105227=DIRECTION('',(-0.190809912898503,0.,0.981627005099017));
#105228=DIRECTION('',(0.,-1.,0.));
#105229=DIRECTION('',(0.,-1.,0.));
#105230=DIRECTION('center_axis',(0.,-1.,0.));
#105231=DIRECTION('ref_axis',(0.,0.,-1.));
#105232=DIRECTION('',(-0.190809912898503,0.,0.981627005099017));
#105233=DIRECTION('',(-0.981627005099017,0.,-0.190809912898503));
#105234=DIRECTION('',(-0.981627005099017,0.,-0.190809912898503));
#105235=DIRECTION('center_axis',(-0.981627005099017,0.,-0.190809912898503));
#105236=DIRECTION('ref_axis',(-0.190809912898503,0.,0.981627005099017));
#105237=DIRECTION('',(0.,1.,0.));
#105238=DIRECTION('',(0.,1.,0.));
#105239=DIRECTION('center_axis',(0.,1.,0.));
#105240=DIRECTION('ref_axis',(1.,0.,0.));
#105241=DIRECTION('',(-0.190809912898503,0.,0.981627005099017));
#105242=DIRECTION('',(0.981627005099017,0.,0.190809912898503));
#105243=DIRECTION('',(-0.190809912898503,0.,0.981627005099017));
#105244=DIRECTION('',(0.981627005099017,0.,0.190809912898503));
#105245=DIRECTION('center_axis',(0.981627005099017,0.,0.190809912898503));
#105246=DIRECTION('ref_axis',(0.,-1.,0.));
#105247=DIRECTION('',(-0.190809912898503,0.,0.981627005099017));
#105248=DIRECTION('',(0.,-1.,0.));
#105249=DIRECTION('',(0.,-1.,0.));
#105250=DIRECTION('center_axis',(0.,-1.,0.));
#105251=DIRECTION('ref_axis',(0.,0.,-1.));
#105252=DIRECTION('',(-0.190809912898503,0.,0.981627005099017));
#105253=DIRECTION('',(-0.981627005099017,0.,-0.190809912898503));
#105254=DIRECTION('',(-0.981627005099017,0.,-0.190809912898503));
#105255=DIRECTION('center_axis',(-0.981627005099017,0.,-0.190809912898503));
#105256=DIRECTION('ref_axis',(-0.190809912898503,0.,0.981627005099017));
#105257=DIRECTION('',(0.,1.,0.));
#105258=DIRECTION('',(0.,1.,0.));
#105259=DIRECTION('center_axis',(0.,1.,0.));
#105260=DIRECTION('ref_axis',(1.,0.,0.));
#105261=DIRECTION('',(-0.190809912898503,0.,0.981627005099017));
#105262=DIRECTION('',(0.981627005099017,0.,0.190809912898503));
#105263=DIRECTION('',(-0.190809912898503,0.,0.981627005099017));
#105264=DIRECTION('',(0.981627005099017,0.,0.190809912898503));
#105265=DIRECTION('center_axis',(0.981627005099017,0.,0.190809912898503));
#105266=DIRECTION('ref_axis',(0.,-1.,0.));
#105267=DIRECTION('',(-0.190809912898503,0.,0.981627005099017));
#105268=DIRECTION('',(0.,-1.,0.));
#105269=DIRECTION('',(0.,-1.,0.));
#105270=DIRECTION('center_axis',(0.,-1.,0.));
#105271=DIRECTION('ref_axis',(0.,0.,-1.));
#105272=DIRECTION('',(-0.190809912898503,0.,0.981627005099017));
#105273=DIRECTION('',(-0.981627005099017,0.,-0.190809912898503));
#105274=DIRECTION('',(-0.981627005099017,0.,-0.190809912898503));
#105275=DIRECTION('center_axis',(-0.981627005099017,0.,-0.190809912898503));
#105276=DIRECTION('ref_axis',(-0.190809912898503,0.,0.981627005099017));
#105277=DIRECTION('',(0.,1.,0.));
#105278=DIRECTION('',(0.,1.,0.));
#105279=DIRECTION('center_axis',(0.,1.,0.));
#105280=DIRECTION('ref_axis',(1.,0.,0.));
#105281=DIRECTION('',(-0.190809912898503,0.,0.981627005099017));
#105282=DIRECTION('',(0.981627005099017,0.,0.190809912898503));
#105283=DIRECTION('',(-0.190809912898503,0.,0.981627005099017));
#105284=DIRECTION('',(0.981627005099017,0.,0.190809912898503));
#105285=DIRECTION('center_axis',(0.981627005099017,0.,0.190809912898503));
#105286=DIRECTION('ref_axis',(0.,-1.,0.));
#105287=DIRECTION('',(-0.190809912898503,0.,0.981627005099017));
#105288=DIRECTION('',(0.,-1.,0.));
#105289=DIRECTION('',(0.,-1.,0.));
#105290=DIRECTION('center_axis',(0.,-1.,0.));
#105291=DIRECTION('ref_axis',(0.,0.,-1.));
#105292=DIRECTION('',(-0.190809912898503,0.,0.981627005099017));
#105293=DIRECTION('',(-0.981627005099017,0.,-0.190809912898503));
#105294=DIRECTION('',(-0.981627005099017,0.,-0.190809912898503));
#105295=DIRECTION('center_axis',(-0.981627005099017,0.,-0.190809912898503));
#105296=DIRECTION('ref_axis',(-0.190809912898503,0.,0.981627005099017));
#105297=DIRECTION('',(0.,1.,0.));
#105298=DIRECTION('',(0.,1.,0.));
#105299=DIRECTION('center_axis',(0.,1.,0.));
#105300=DIRECTION('ref_axis',(1.,0.,0.));
#105301=DIRECTION('',(-0.190809912898503,0.,0.981627005099017));
#105302=DIRECTION('',(0.981627005099017,0.,0.190809912898503));
#105303=DIRECTION('',(-0.190809912898503,0.,0.981627005099017));
#105304=DIRECTION('',(0.981627005099017,0.,0.190809912898503));
#105305=DIRECTION('center_axis',(0.981627005099017,0.,0.190809912898503));
#105306=DIRECTION('ref_axis',(0.,-1.,0.));
#105307=DIRECTION('',(-0.190809912898503,0.,0.981627005099017));
#105308=DIRECTION('',(0.,-1.,0.));
#105309=DIRECTION('',(0.,-1.,0.));
#105310=DIRECTION('center_axis',(0.,-1.,0.));
#105311=DIRECTION('ref_axis',(0.,0.,-1.));
#105312=DIRECTION('',(-0.190809912898503,0.,0.981627005099017));
#105313=DIRECTION('',(-0.981627005099017,0.,-0.190809912898503));
#105314=DIRECTION('',(-0.981627005099017,0.,-0.190809912898503));
#105315=DIRECTION('center_axis',(-0.981627005099017,0.,-0.190809912898503));
#105316=DIRECTION('ref_axis',(-0.190809912898503,0.,0.981627005099017));
#105317=DIRECTION('',(0.,1.,0.));
#105318=DIRECTION('',(0.,1.,0.));
#105319=DIRECTION('center_axis',(0.,1.,0.));
#105320=DIRECTION('ref_axis',(1.,0.,0.));
#105321=DIRECTION('',(-0.190809912898503,0.,0.981627005099017));
#105322=DIRECTION('',(0.981627005099017,0.,0.190809912898503));
#105323=DIRECTION('',(-0.190809912898503,0.,0.981627005099017));
#105324=DIRECTION('',(0.981627005099017,0.,0.190809912898503));
#105325=DIRECTION('center_axis',(0.981627005099017,0.,0.190809912898503));
#105326=DIRECTION('ref_axis',(0.,-1.,0.));
#105327=DIRECTION('',(-0.190809912898503,0.,0.981627005099017));
#105328=DIRECTION('',(0.,-1.,0.));
#105329=DIRECTION('',(0.,-1.,0.));
#105330=DIRECTION('center_axis',(0.,-1.,0.));
#105331=DIRECTION('ref_axis',(0.,0.,-1.));
#105332=DIRECTION('',(-0.190809912898503,0.,0.981627005099017));
#105333=DIRECTION('',(-0.981627005099017,0.,-0.190809912898503));
#105334=DIRECTION('',(-0.981627005099017,0.,-0.190809912898503));
#105335=DIRECTION('center_axis',(-0.981627005099017,0.,-0.190809912898503));
#105336=DIRECTION('ref_axis',(-0.190809912898503,0.,0.981627005099017));
#105337=DIRECTION('',(0.,1.,0.));
#105338=DIRECTION('',(0.,1.,0.));
#105339=DIRECTION('center_axis',(0.,1.,0.));
#105340=DIRECTION('ref_axis',(1.,0.,0.));
#105341=DIRECTION('',(-0.190809912898503,0.,0.981627005099017));
#105342=DIRECTION('',(0.981627005099017,0.,0.190809912898503));
#105343=DIRECTION('',(-0.190809912898503,0.,0.981627005099017));
#105344=DIRECTION('',(0.981627005099017,0.,0.190809912898503));
#105345=DIRECTION('center_axis',(0.981627005099017,0.,0.190809912898503));
#105346=DIRECTION('ref_axis',(0.,-1.,0.));
#105347=DIRECTION('',(-0.190809912898503,0.,0.981627005099017));
#105348=DIRECTION('',(0.,-1.,0.));
#105349=DIRECTION('',(0.,-1.,0.));
#105350=DIRECTION('center_axis',(0.,-1.,0.));
#105351=DIRECTION('ref_axis',(0.,0.,-1.));
#105352=DIRECTION('',(-0.190809912898503,0.,0.981627005099017));
#105353=DIRECTION('',(-0.981627005099017,0.,-0.190809912898503));
#105354=DIRECTION('',(-0.981627005099017,0.,-0.190809912898503));
#105355=DIRECTION('center_axis',(-0.981627005099017,0.,-0.190809912898503));
#105356=DIRECTION('ref_axis',(-0.190809912898503,0.,0.981627005099017));
#105357=DIRECTION('',(0.,1.,0.));
#105358=DIRECTION('',(0.,1.,0.));
#105359=DIRECTION('center_axis',(0.,1.,0.));
#105360=DIRECTION('ref_axis',(1.,0.,0.));
#105361=DIRECTION('',(-0.190809912898503,0.,0.981627005099017));
#105362=DIRECTION('',(0.981627005099017,0.,0.190809912898503));
#105363=DIRECTION('',(-0.190809912898503,0.,0.981627005099017));
#105364=DIRECTION('',(0.981627005099017,0.,0.190809912898503));
#105365=DIRECTION('center_axis',(0.981627005099017,0.,0.190809912898503));
#105366=DIRECTION('ref_axis',(0.,-1.,0.));
#105367=DIRECTION('',(-0.190809912898503,0.,0.981627005099017));
#105368=DIRECTION('',(0.,-1.,0.));
#105369=DIRECTION('',(0.,-1.,0.));
#105370=DIRECTION('center_axis',(0.,-1.,0.));
#105371=DIRECTION('ref_axis',(0.,0.,-1.));
#105372=DIRECTION('',(-0.190809912898503,0.,0.981627005099017));
#105373=DIRECTION('',(-0.981627005099017,0.,-0.190809912898503));
#105374=DIRECTION('',(-0.981627005099017,0.,-0.190809912898503));
#105375=DIRECTION('center_axis',(-0.981627005099017,0.,-0.190809912898503));
#105376=DIRECTION('ref_axis',(-0.190809912898503,0.,0.981627005099017));
#105377=DIRECTION('',(0.,1.,0.));
#105378=DIRECTION('',(0.,1.,0.));
#105379=DIRECTION('center_axis',(0.,1.,0.));
#105380=DIRECTION('ref_axis',(1.,0.,0.));
#105381=DIRECTION('',(-0.190809912898503,0.,0.981627005099017));
#105382=DIRECTION('',(0.981627005099017,0.,0.190809912898503));
#105383=DIRECTION('',(-0.190809912898503,0.,0.981627005099017));
#105384=DIRECTION('',(0.981627005099017,0.,0.190809912898503));
#105385=DIRECTION('center_axis',(0.981627005099017,0.,0.190809912898503));
#105386=DIRECTION('ref_axis',(0.,-1.,0.));
#105387=DIRECTION('',(-0.190809912898503,0.,0.981627005099017));
#105388=DIRECTION('',(0.,-1.,0.));
#105389=DIRECTION('',(0.,-1.,0.));
#105390=DIRECTION('center_axis',(0.,-1.,0.));
#105391=DIRECTION('ref_axis',(0.,0.,-1.));
#105392=DIRECTION('',(-0.190809912898503,0.,0.981627005099017));
#105393=DIRECTION('',(-0.981627005099017,0.,-0.190809912898503));
#105394=DIRECTION('',(-0.981627005099017,0.,-0.190809912898503));
#105395=DIRECTION('center_axis',(-0.981627005099017,0.,-0.190809912898503));
#105396=DIRECTION('ref_axis',(-0.190809912898503,0.,0.981627005099017));
#105397=DIRECTION('',(0.,1.,0.));
#105398=DIRECTION('',(0.,1.,0.));
#105399=DIRECTION('center_axis',(0.,1.,0.));
#105400=DIRECTION('ref_axis',(1.,0.,0.));
#105401=DIRECTION('',(-0.190809912898503,0.,0.981627005099017));
#105402=DIRECTION('',(0.981627005099017,0.,0.190809912898503));
#105403=DIRECTION('',(-0.190809912898503,0.,0.981627005099017));
#105404=DIRECTION('',(0.981627005099017,0.,0.190809912898503));
#105405=DIRECTION('center_axis',(0.981627005099017,0.,0.190809912898503));
#105406=DIRECTION('ref_axis',(0.,-1.,0.));
#105407=DIRECTION('',(-0.190809912898503,0.,0.981627005099017));
#105408=DIRECTION('',(0.,-1.,0.));
#105409=DIRECTION('',(0.,-1.,0.));
#105410=DIRECTION('center_axis',(0.,-1.,0.));
#105411=DIRECTION('ref_axis',(0.,0.,-1.));
#105412=DIRECTION('',(-0.190809912898503,0.,0.981627005099017));
#105413=DIRECTION('',(-0.981627005099017,0.,-0.190809912898503));
#105414=DIRECTION('',(-0.981627005099017,0.,-0.190809912898503));
#105415=DIRECTION('center_axis',(-0.981627005099017,0.,-0.190809912898503));
#105416=DIRECTION('ref_axis',(-0.190809912898503,0.,0.981627005099017));
#105417=DIRECTION('',(0.,1.,0.));
#105418=DIRECTION('',(0.,1.,0.));
#105419=DIRECTION('center_axis',(0.,1.,0.));
#105420=DIRECTION('ref_axis',(1.,0.,0.));
#105421=DIRECTION('',(-0.190809912898503,0.,0.981627005099017));
#105422=DIRECTION('',(0.981627005099017,0.,0.190809912898503));
#105423=DIRECTION('',(-0.190809912898503,0.,0.981627005099017));
#105424=DIRECTION('',(0.981627005099017,0.,0.190809912898503));
#105425=DIRECTION('center_axis',(0.981627005099017,0.,0.190809912898503));
#105426=DIRECTION('ref_axis',(0.,-1.,0.));
#105427=DIRECTION('',(-0.190809912898503,0.,0.981627005099017));
#105428=DIRECTION('',(0.,-1.,0.));
#105429=DIRECTION('',(0.,-1.,0.));
#105430=DIRECTION('center_axis',(0.,-1.,0.));
#105431=DIRECTION('ref_axis',(0.,0.,-1.));
#105432=DIRECTION('',(-0.190809912898503,0.,0.981627005099017));
#105433=DIRECTION('',(-0.981627005099017,0.,-0.190809912898503));
#105434=DIRECTION('',(-0.981627005099017,0.,-0.190809912898503));
#105435=DIRECTION('center_axis',(-0.981627005099017,0.,-0.190809912898503));
#105436=DIRECTION('ref_axis',(-0.190809912898503,0.,0.981627005099017));
#105437=DIRECTION('',(0.,1.,0.));
#105438=DIRECTION('',(0.,1.,0.));
#105439=DIRECTION('center_axis',(0.,1.,0.));
#105440=DIRECTION('ref_axis',(1.,0.,0.));
#105441=DIRECTION('',(-0.190809912898503,0.,0.981627005099017));
#105442=DIRECTION('',(0.981627005099017,0.,0.190809912898503));
#105443=DIRECTION('',(-0.190809912898503,0.,0.981627005099017));
#105444=DIRECTION('',(0.981627005099017,0.,0.190809912898503));
#105445=DIRECTION('center_axis',(0.981627005099017,0.,0.190809912898503));
#105446=DIRECTION('ref_axis',(0.,-1.,0.));
#105447=DIRECTION('',(-0.190809912898503,0.,0.981627005099017));
#105448=DIRECTION('',(0.,-1.,0.));
#105449=DIRECTION('',(0.,-1.,0.));
#105450=DIRECTION('center_axis',(0.,-1.,0.));
#105451=DIRECTION('ref_axis',(0.,0.,-1.));
#105452=DIRECTION('',(-0.190809912898503,0.,0.981627005099017));
#105453=DIRECTION('',(-0.981627005099017,0.,-0.190809912898503));
#105454=DIRECTION('',(-0.981627005099017,0.,-0.190809912898503));
#105455=DIRECTION('center_axis',(-0.981627005099017,0.,-0.190809912898503));
#105456=DIRECTION('ref_axis',(-0.190809912898503,0.,0.981627005099017));
#105457=DIRECTION('',(0.,1.,0.));
#105458=DIRECTION('',(0.,1.,0.));
#105459=DIRECTION('center_axis',(0.,1.,0.));
#105460=DIRECTION('ref_axis',(1.,0.,0.));
#105461=DIRECTION('',(-0.190809912898503,0.,0.981627005099017));
#105462=DIRECTION('',(0.981627005099017,0.,0.190809912898503));
#105463=DIRECTION('',(-0.190809912898503,0.,0.981627005099017));
#105464=DIRECTION('',(0.981627005099017,0.,0.190809912898503));
#105465=DIRECTION('center_axis',(0.981627005099017,0.,0.190809912898503));
#105466=DIRECTION('ref_axis',(0.,-1.,0.));
#105467=DIRECTION('',(-0.190809912898503,0.,0.981627005099017));
#105468=DIRECTION('',(0.,-1.,0.));
#105469=DIRECTION('',(0.,-1.,0.));
#105470=DIRECTION('center_axis',(0.,-1.,0.));
#105471=DIRECTION('ref_axis',(0.,0.,-1.));
#105472=DIRECTION('',(-0.190809912898503,0.,0.981627005099017));
#105473=DIRECTION('',(-0.981627005099017,0.,-0.190809912898503));
#105474=DIRECTION('',(-0.981627005099017,0.,-0.190809912898503));
#105475=DIRECTION('center_axis',(-0.981627005099017,0.,-0.190809912898503));
#105476=DIRECTION('ref_axis',(-0.190809912898503,0.,0.981627005099017));
#105477=DIRECTION('',(0.,1.,0.));
#105478=DIRECTION('',(0.,1.,0.));
#105479=DIRECTION('center_axis',(0.,1.,0.));
#105480=DIRECTION('ref_axis',(1.,0.,0.));
#105481=DIRECTION('',(-0.190809912898503,0.,0.981627005099017));
#105482=DIRECTION('',(0.981627005099017,0.,0.190809912898503));
#105483=DIRECTION('',(-0.190809912898503,0.,0.981627005099017));
#105484=DIRECTION('',(0.981627005099017,0.,0.190809912898503));
#105485=DIRECTION('center_axis',(0.981627005099017,0.,0.190809912898503));
#105486=DIRECTION('ref_axis',(0.,-1.,0.));
#105487=DIRECTION('',(-0.190809912898503,0.,0.981627005099017));
#105488=DIRECTION('',(0.,-1.,0.));
#105489=DIRECTION('',(0.,-1.,0.));
#105490=DIRECTION('center_axis',(0.,-1.,0.));
#105491=DIRECTION('ref_axis',(0.,0.,-1.));
#105492=DIRECTION('',(-0.190809912898503,0.,0.981627005099017));
#105493=DIRECTION('',(-0.981627005099017,0.,-0.190809912898503));
#105494=DIRECTION('',(-0.981627005099017,0.,-0.190809912898503));
#105495=DIRECTION('center_axis',(-0.981627005099017,0.,-0.190809912898503));
#105496=DIRECTION('ref_axis',(-0.190809912898503,0.,0.981627005099017));
#105497=DIRECTION('',(0.,1.,0.));
#105498=DIRECTION('',(0.,1.,0.));
#105499=DIRECTION('center_axis',(0.,1.,0.));
#105500=DIRECTION('ref_axis',(1.,0.,0.));
#105501=DIRECTION('',(-0.190809912898503,0.,0.981627005099017));
#105502=DIRECTION('',(0.981627005099017,0.,0.190809912898503));
#105503=DIRECTION('',(-0.190809912898503,0.,0.981627005099017));
#105504=DIRECTION('',(0.981627005099017,0.,0.190809912898503));
#105505=DIRECTION('center_axis',(0.981627005099017,0.,0.190809912898503));
#105506=DIRECTION('ref_axis',(0.,-1.,0.));
#105507=DIRECTION('',(-0.190809912898503,0.,0.981627005099017));
#105508=DIRECTION('',(0.,-1.,0.));
#105509=DIRECTION('',(0.,-1.,0.));
#105510=DIRECTION('center_axis',(0.,-1.,0.));
#105511=DIRECTION('ref_axis',(0.,0.,-1.));
#105512=DIRECTION('',(-0.190809912898503,0.,0.981627005099017));
#105513=DIRECTION('',(-0.981627005099017,0.,-0.190809912898503));
#105514=DIRECTION('',(-0.981627005099017,0.,-0.190809912898503));
#105515=DIRECTION('center_axis',(-0.981627005099017,0.,-0.190809912898503));
#105516=DIRECTION('ref_axis',(-0.190809912898503,0.,0.981627005099017));
#105517=DIRECTION('',(0.,1.,0.));
#105518=DIRECTION('',(0.,1.,0.));
#105519=DIRECTION('center_axis',(0.,1.,0.));
#105520=DIRECTION('ref_axis',(1.,0.,0.));
#105521=DIRECTION('',(-0.190809912898503,0.,0.981627005099017));
#105522=DIRECTION('',(0.981627005099017,0.,0.190809912898503));
#105523=DIRECTION('',(-0.190809912898503,0.,0.981627005099017));
#105524=DIRECTION('',(0.981627005099017,0.,0.190809912898503));
#105525=DIRECTION('center_axis',(0.981627005099017,0.,0.190809912898503));
#105526=DIRECTION('ref_axis',(0.,-1.,0.));
#105527=DIRECTION('',(-0.190809912898503,0.,0.981627005099017));
#105528=DIRECTION('',(0.,-1.,0.));
#105529=DIRECTION('',(0.,-1.,0.));
#105530=DIRECTION('center_axis',(0.,-1.,0.));
#105531=DIRECTION('ref_axis',(0.,0.,-1.));
#105532=DIRECTION('',(-0.190809912898503,0.,0.981627005099017));
#105533=DIRECTION('',(-0.981627005099017,0.,-0.190809912898503));
#105534=DIRECTION('',(-0.981627005099017,0.,-0.190809912898503));
#105535=DIRECTION('center_axis',(-0.981627005099017,0.,-0.190809912898503));
#105536=DIRECTION('ref_axis',(-0.190809912898503,0.,0.981627005099017));
#105537=DIRECTION('',(0.,1.,0.));
#105538=DIRECTION('',(0.,1.,0.));
#105539=DIRECTION('center_axis',(0.,1.,0.));
#105540=DIRECTION('ref_axis',(1.,0.,0.));
#105541=DIRECTION('',(-0.190809912898503,0.,0.981627005099017));
#105542=DIRECTION('',(0.981627005099017,0.,0.190809912898503));
#105543=DIRECTION('',(-0.190809912898503,0.,0.981627005099017));
#105544=DIRECTION('',(0.981627005099017,0.,0.190809912898503));
#105545=DIRECTION('center_axis',(0.981627005099017,0.,0.190809912898503));
#105546=DIRECTION('ref_axis',(0.,-1.,0.));
#105547=DIRECTION('',(-0.190809912898503,0.,0.981627005099017));
#105548=DIRECTION('',(0.,-1.,0.));
#105549=DIRECTION('',(0.,-1.,0.));
#105550=DIRECTION('center_axis',(0.,-1.,0.));
#105551=DIRECTION('ref_axis',(0.,0.,-1.));
#105552=DIRECTION('',(-0.190809912898503,0.,0.981627005099017));
#105553=DIRECTION('',(-0.981627005099017,0.,-0.190809912898503));
#105554=DIRECTION('',(-0.981627005099017,0.,-0.190809912898503));
#105555=DIRECTION('center_axis',(-0.981627005099017,0.,-0.190809912898503));
#105556=DIRECTION('ref_axis',(-0.190809912898503,0.,0.981627005099017));
#105557=DIRECTION('',(0.,1.,0.));
#105558=DIRECTION('',(0.,1.,0.));
#105559=DIRECTION('center_axis',(0.,1.,0.));
#105560=DIRECTION('ref_axis',(1.,0.,0.));
#105561=DIRECTION('',(-0.190809912898503,0.,0.981627005099017));
#105562=DIRECTION('',(0.981627005099017,0.,0.190809912898503));
#105563=DIRECTION('',(-0.190809912898503,0.,0.981627005099017));
#105564=DIRECTION('',(0.981627005099017,0.,0.190809912898503));
#105565=DIRECTION('center_axis',(0.981627005099017,0.,0.190809912898503));
#105566=DIRECTION('ref_axis',(0.,-1.,0.));
#105567=DIRECTION('',(-0.190809912898503,0.,0.981627005099017));
#105568=DIRECTION('',(0.,-1.,0.));
#105569=DIRECTION('',(0.,-1.,0.));
#105570=DIRECTION('center_axis',(0.,-1.,0.));
#105571=DIRECTION('ref_axis',(0.,0.,-1.));
#105572=DIRECTION('',(-0.190809912898503,0.,0.981627005099017));
#105573=DIRECTION('',(-0.981627005099017,0.,-0.190809912898503));
#105574=DIRECTION('',(-0.981627005099017,0.,-0.190809912898503));
#105575=DIRECTION('center_axis',(-0.981627005099017,0.,-0.190809912898503));
#105576=DIRECTION('ref_axis',(-0.190809912898503,0.,0.981627005099017));
#105577=DIRECTION('',(0.,1.,0.));
#105578=DIRECTION('',(0.,1.,0.));
#105579=DIRECTION('center_axis',(0.,1.,0.));
#105580=DIRECTION('ref_axis',(1.,0.,0.));
#105581=DIRECTION('',(-0.190809912898503,0.,0.981627005099017));
#105582=DIRECTION('',(0.981627005099017,0.,0.190809912898503));
#105583=DIRECTION('',(-0.190809912898503,0.,0.981627005099017));
#105584=DIRECTION('',(0.981627005099017,0.,0.190809912898503));
#105585=DIRECTION('center_axis',(0.981627005099017,0.,0.190809912898503));
#105586=DIRECTION('ref_axis',(0.,-1.,0.));
#105587=DIRECTION('',(-0.190809912898503,0.,0.981627005099017));
#105588=DIRECTION('',(0.,-1.,0.));
#105589=DIRECTION('',(0.,-1.,0.));
#105590=DIRECTION('center_axis',(0.,-1.,0.));
#105591=DIRECTION('ref_axis',(0.,0.,-1.));
#105592=DIRECTION('',(-0.190809912898503,0.,0.981627005099017));
#105593=DIRECTION('',(-0.981627005099017,0.,-0.190809912898503));
#105594=DIRECTION('',(-0.981627005099017,0.,-0.190809912898503));
#105595=DIRECTION('center_axis',(-0.981627005099017,0.,-0.190809912898503));
#105596=DIRECTION('ref_axis',(-0.190809912898503,0.,0.981627005099017));
#105597=DIRECTION('',(0.,1.,0.));
#105598=DIRECTION('',(0.,1.,0.));
#105599=DIRECTION('center_axis',(0.,1.,0.));
#105600=DIRECTION('ref_axis',(1.,0.,0.));
#105601=DIRECTION('',(-0.190809912898503,0.,0.981627005099017));
#105602=DIRECTION('',(0.981627005099017,0.,0.190809912898503));
#105603=DIRECTION('',(-0.190809912898503,0.,0.981627005099017));
#105604=DIRECTION('',(0.981627005099017,0.,0.190809912898503));
#105605=DIRECTION('center_axis',(0.981627005099017,0.,0.190809912898503));
#105606=DIRECTION('ref_axis',(0.,-1.,0.));
#105607=DIRECTION('',(-0.190809912898503,0.,0.981627005099017));
#105608=DIRECTION('',(0.,-1.,0.));
#105609=DIRECTION('',(0.,-1.,0.));
#105610=DIRECTION('center_axis',(0.,-1.,0.));
#105611=DIRECTION('ref_axis',(0.,0.,-1.));
#105612=DIRECTION('',(-0.190809912898503,0.,0.981627005099017));
#105613=DIRECTION('',(-0.981627005099017,0.,-0.190809912898503));
#105614=DIRECTION('',(-0.981627005099017,0.,-0.190809912898503));
#105615=DIRECTION('center_axis',(-0.981627005099017,0.,-0.190809912898503));
#105616=DIRECTION('ref_axis',(-0.190809912898503,0.,0.981627005099017));
#105617=DIRECTION('',(0.,1.,0.));
#105618=DIRECTION('',(0.,1.,0.));
#105619=DIRECTION('center_axis',(0.,1.,0.));
#105620=DIRECTION('ref_axis',(1.,0.,0.));
#105621=DIRECTION('',(-0.190809912898503,0.,0.981627005099017));
#105622=DIRECTION('',(0.981627005099017,0.,0.190809912898503));
#105623=DIRECTION('',(-0.190809912898503,0.,0.981627005099017));
#105624=DIRECTION('',(0.981627005099017,0.,0.190809912898503));
#105625=DIRECTION('center_axis',(0.981627005099017,0.,0.190809912898503));
#105626=DIRECTION('ref_axis',(0.,-1.,0.));
#105627=DIRECTION('',(-0.190809912898503,0.,0.981627005099017));
#105628=DIRECTION('',(0.,-1.,0.));
#105629=DIRECTION('',(0.,-1.,0.));
#105630=DIRECTION('center_axis',(0.,-1.,0.));
#105631=DIRECTION('ref_axis',(0.,0.,-1.));
#105632=DIRECTION('',(-0.190809912898503,0.,0.981627005099017));
#105633=DIRECTION('',(-0.981627005099017,0.,-0.190809912898503));
#105634=DIRECTION('',(-0.981627005099017,0.,-0.190809912898503));
#105635=DIRECTION('center_axis',(-0.981627005099017,0.,-0.190809912898503));
#105636=DIRECTION('ref_axis',(-0.190809912898503,0.,0.981627005099017));
#105637=DIRECTION('',(0.,1.,0.));
#105638=DIRECTION('',(0.,1.,0.));
#105639=DIRECTION('center_axis',(0.,1.,0.));
#105640=DIRECTION('ref_axis',(1.,0.,0.));
#105641=DIRECTION('',(-0.190809912898503,0.,0.981627005099017));
#105642=DIRECTION('',(0.981627005099017,0.,0.190809912898503));
#105643=DIRECTION('',(-0.190809912898503,0.,0.981627005099017));
#105644=DIRECTION('',(0.981627005099017,0.,0.190809912898503));
#105645=DIRECTION('center_axis',(0.981627005099017,0.,0.190809912898503));
#105646=DIRECTION('ref_axis',(0.,-1.,0.));
#105647=DIRECTION('',(-0.190809912898503,0.,0.981627005099017));
#105648=DIRECTION('',(0.,-1.,0.));
#105649=DIRECTION('',(0.,-1.,0.));
#105650=DIRECTION('center_axis',(0.,-1.,0.));
#105651=DIRECTION('ref_axis',(0.,0.,-1.));
#105652=DIRECTION('',(-0.190809912898503,0.,0.981627005099017));
#105653=DIRECTION('',(-0.981627005099017,0.,-0.190809912898503));
#105654=DIRECTION('',(-0.981627005099017,0.,-0.190809912898503));
#105655=DIRECTION('center_axis',(-0.981627005099017,0.,-0.190809912898503));
#105656=DIRECTION('ref_axis',(-0.190809912898503,0.,0.981627005099017));
#105657=DIRECTION('',(0.,1.,0.));
#105658=DIRECTION('',(0.,1.,0.));
#105659=DIRECTION('center_axis',(0.,1.,0.));
#105660=DIRECTION('ref_axis',(1.,0.,0.));
#105661=DIRECTION('',(-0.190809912898503,0.,0.981627005099017));
#105662=DIRECTION('',(0.981627005099017,0.,0.190809912898503));
#105663=DIRECTION('',(-0.190809912898503,0.,0.981627005099017));
#105664=DIRECTION('',(0.981627005099017,0.,0.190809912898503));
#105665=DIRECTION('center_axis',(0.981627005099017,0.,0.190809912898503));
#105666=DIRECTION('ref_axis',(0.,-1.,0.));
#105667=DIRECTION('',(-0.190809912898503,0.,0.981627005099017));
#105668=DIRECTION('',(0.,-1.,0.));
#105669=DIRECTION('',(0.,-1.,0.));
#105670=DIRECTION('center_axis',(0.,-1.,0.));
#105671=DIRECTION('ref_axis',(0.,0.,-1.));
#105672=DIRECTION('',(-0.190809912898503,0.,0.981627005099017));
#105673=DIRECTION('',(-0.981627005099017,0.,-0.190809912898503));
#105674=DIRECTION('',(-0.981627005099017,0.,-0.190809912898503));
#105675=DIRECTION('center_axis',(-0.981627005099017,0.,-0.190809912898503));
#105676=DIRECTION('ref_axis',(-0.190809912898503,0.,0.981627005099017));
#105677=DIRECTION('',(0.,1.,0.));
#105678=DIRECTION('',(0.,1.,0.));
#105679=DIRECTION('center_axis',(0.,1.,0.));
#105680=DIRECTION('ref_axis',(1.,0.,0.));
#105681=DIRECTION('',(-0.190809912898503,0.,0.981627005099017));
#105682=DIRECTION('',(0.981627005099017,0.,0.190809912898503));
#105683=DIRECTION('',(-0.190809912898503,0.,0.981627005099017));
#105684=DIRECTION('',(0.981627005099017,0.,0.190809912898503));
#105685=DIRECTION('center_axis',(0.981627005099017,0.,0.190809912898503));
#105686=DIRECTION('ref_axis',(0.,-1.,0.));
#105687=DIRECTION('',(-0.190809912898503,0.,0.981627005099017));
#105688=DIRECTION('',(0.,-1.,0.));
#105689=DIRECTION('',(0.,-1.,0.));
#105690=DIRECTION('center_axis',(0.,-1.,0.));
#105691=DIRECTION('ref_axis',(0.,0.,-1.));
#105692=DIRECTION('',(-0.190809912898503,0.,0.981627005099017));
#105693=DIRECTION('',(-0.981627005099017,0.,-0.190809912898503));
#105694=DIRECTION('',(-0.981627005099017,0.,-0.190809912898503));
#105695=DIRECTION('center_axis',(-0.981627005099017,0.,-0.190809912898503));
#105696=DIRECTION('ref_axis',(-0.190809912898503,0.,0.981627005099017));
#105697=DIRECTION('',(0.,1.,0.));
#105698=DIRECTION('',(0.,1.,0.));
#105699=DIRECTION('center_axis',(0.,1.,0.));
#105700=DIRECTION('ref_axis',(1.,0.,0.));
#105701=DIRECTION('',(-0.190809912898503,0.,0.981627005099017));
#105702=DIRECTION('',(0.981627005099017,0.,0.190809912898503));
#105703=DIRECTION('',(-0.190809912898503,0.,0.981627005099017));
#105704=DIRECTION('',(0.981627005099017,0.,0.190809912898503));
#105705=DIRECTION('center_axis',(0.981627005099017,0.,0.190809912898503));
#105706=DIRECTION('ref_axis',(0.,-1.,0.));
#105707=DIRECTION('',(-0.190809912898503,0.,0.981627005099017));
#105708=DIRECTION('',(0.,-1.,0.));
#105709=DIRECTION('',(0.,-1.,0.));
#105710=DIRECTION('center_axis',(0.,-1.,0.));
#105711=DIRECTION('ref_axis',(0.,0.,-1.));
#105712=DIRECTION('',(-0.190809912898503,0.,0.981627005099017));
#105713=DIRECTION('',(-0.981627005099017,0.,-0.190809912898503));
#105714=DIRECTION('',(-0.981627005099017,0.,-0.190809912898503));
#105715=DIRECTION('center_axis',(-0.981627005099017,0.,-0.190809912898503));
#105716=DIRECTION('ref_axis',(-0.190809912898503,0.,0.981627005099017));
#105717=DIRECTION('',(0.,1.,0.));
#105718=DIRECTION('',(0.,1.,0.));
#105719=DIRECTION('center_axis',(0.,1.,0.));
#105720=DIRECTION('ref_axis',(1.,0.,0.));
#105721=DIRECTION('',(-0.190809912898503,0.,0.981627005099017));
#105722=DIRECTION('',(0.981627005099017,0.,0.190809912898503));
#105723=DIRECTION('',(-0.190809912898503,0.,0.981627005099017));
#105724=DIRECTION('',(0.981627005099017,0.,0.190809912898503));
#105725=DIRECTION('center_axis',(0.981627005099017,0.,0.190809912898503));
#105726=DIRECTION('ref_axis',(0.,-1.,0.));
#105727=DIRECTION('',(-0.190809912898503,0.,0.981627005099017));
#105728=DIRECTION('',(0.,-1.,0.));
#105729=DIRECTION('',(0.,-1.,0.));
#105730=DIRECTION('center_axis',(0.,-1.,0.));
#105731=DIRECTION('ref_axis',(0.,0.,-1.));
#105732=DIRECTION('',(-0.190809912898503,0.,0.981627005099017));
#105733=DIRECTION('',(-0.981627005099017,0.,-0.190809912898503));
#105734=DIRECTION('',(-0.981627005099017,0.,-0.190809912898503));
#105735=DIRECTION('center_axis',(-0.981627005099017,0.,-0.190809912898503));
#105736=DIRECTION('ref_axis',(-0.190809912898503,0.,0.981627005099017));
#105737=DIRECTION('',(0.,1.,0.));
#105738=DIRECTION('',(0.,1.,0.));
#105739=DIRECTION('center_axis',(0.,1.,0.));
#105740=DIRECTION('ref_axis',(1.,0.,0.));
#105741=DIRECTION('',(-0.190809912898503,0.,0.981627005099017));
#105742=DIRECTION('',(0.981627005099017,0.,0.190809912898503));
#105743=DIRECTION('',(-0.190809912898503,0.,0.981627005099017));
#105744=DIRECTION('',(0.981627005099017,0.,0.190809912898503));
#105745=DIRECTION('center_axis',(0.981627005099017,0.,0.190809912898503));
#105746=DIRECTION('ref_axis',(0.,-1.,0.));
#105747=DIRECTION('',(-0.190809912898503,0.,0.981627005099017));
#105748=DIRECTION('',(0.,-1.,0.));
#105749=DIRECTION('',(0.,-1.,0.));
#105750=DIRECTION('center_axis',(0.,-1.,0.));
#105751=DIRECTION('ref_axis',(0.,0.,-1.));
#105752=DIRECTION('',(-0.190809912898503,0.,0.981627005099017));
#105753=DIRECTION('',(-0.981627005099017,0.,-0.190809912898503));
#105754=DIRECTION('',(-0.981627005099017,0.,-0.190809912898503));
#105755=DIRECTION('center_axis',(-0.981627005099017,0.,-0.190809912898503));
#105756=DIRECTION('ref_axis',(-0.190809912898503,0.,0.981627005099017));
#105757=DIRECTION('',(0.,1.,0.));
#105758=DIRECTION('',(0.,1.,0.));
#105759=DIRECTION('center_axis',(0.,1.,0.));
#105760=DIRECTION('ref_axis',(1.,0.,0.));
#105761=DIRECTION('',(-0.190809912898503,0.,0.981627005099017));
#105762=DIRECTION('',(0.981627005099017,0.,0.190809912898503));
#105763=DIRECTION('',(-0.190809912898503,0.,0.981627005099017));
#105764=DIRECTION('',(0.981627005099017,0.,0.190809912898503));
#105765=DIRECTION('center_axis',(0.981627005099017,0.,0.190809912898503));
#105766=DIRECTION('ref_axis',(0.,-1.,0.));
#105767=DIRECTION('',(-0.190809912898503,0.,0.981627005099017));
#105768=DIRECTION('',(0.,-1.,0.));
#105769=DIRECTION('',(0.,-1.,0.));
#105770=DIRECTION('center_axis',(0.,-1.,0.));
#105771=DIRECTION('ref_axis',(0.,0.,-1.));
#105772=DIRECTION('',(-0.190809912898503,0.,0.981627005099017));
#105773=DIRECTION('',(-0.981627005099017,0.,-0.190809912898503));
#105774=DIRECTION('',(-0.981627005099017,0.,-0.190809912898503));
#105775=DIRECTION('center_axis',(-0.981627005099017,0.,-0.190809912898503));
#105776=DIRECTION('ref_axis',(-0.190809912898503,0.,0.981627005099017));
#105777=DIRECTION('',(0.,1.,0.));
#105778=DIRECTION('',(0.,1.,0.));
#105779=DIRECTION('center_axis',(0.,1.,0.));
#105780=DIRECTION('ref_axis',(1.,0.,0.));
#105781=DIRECTION('',(-0.190809912898503,0.,0.981627005099017));
#105782=DIRECTION('',(0.981627005099017,0.,0.190809912898503));
#105783=DIRECTION('',(-0.190809912898503,0.,0.981627005099017));
#105784=DIRECTION('',(0.981627005099017,0.,0.190809912898503));
#105785=DIRECTION('center_axis',(0.981627005099017,0.,0.190809912898503));
#105786=DIRECTION('ref_axis',(0.,-1.,0.));
#105787=DIRECTION('',(-0.190809912898503,0.,0.981627005099017));
#105788=DIRECTION('',(0.,-1.,0.));
#105789=DIRECTION('',(0.,-1.,0.));
#105790=DIRECTION('center_axis',(0.,-1.,0.));
#105791=DIRECTION('ref_axis',(0.,0.,-1.));
#105792=DIRECTION('',(-0.190809912898503,0.,0.981627005099017));
#105793=DIRECTION('',(-0.981627005099017,0.,-0.190809912898503));
#105794=DIRECTION('',(-0.981627005099017,0.,-0.190809912898503));
#105795=DIRECTION('center_axis',(-0.981627005099017,0.,-0.190809912898503));
#105796=DIRECTION('ref_axis',(-0.190809912898503,0.,0.981627005099017));
#105797=DIRECTION('',(0.,1.,0.));
#105798=DIRECTION('',(0.,1.,0.));
#105799=DIRECTION('center_axis',(0.,1.,0.));
#105800=DIRECTION('ref_axis',(1.,0.,0.));
#105801=DIRECTION('',(-0.190809912898503,0.,0.981627005099017));
#105802=DIRECTION('',(0.981627005099017,0.,0.190809912898503));
#105803=DIRECTION('',(-0.190809912898503,0.,0.981627005099017));
#105804=DIRECTION('',(0.981627005099017,0.,0.190809912898503));
#105805=DIRECTION('center_axis',(0.981627005099017,0.,0.190809912898503));
#105806=DIRECTION('ref_axis',(0.,-1.,0.));
#105807=DIRECTION('',(-0.190809912898503,0.,0.981627005099017));
#105808=DIRECTION('',(0.,-1.,0.));
#105809=DIRECTION('',(0.,-1.,0.));
#105810=DIRECTION('center_axis',(0.,-1.,0.));
#105811=DIRECTION('ref_axis',(0.,0.,-1.));
#105812=DIRECTION('',(-0.190809912898503,0.,0.981627005099017));
#105813=DIRECTION('',(-0.981627005099017,0.,-0.190809912898503));
#105814=DIRECTION('',(-0.981627005099017,0.,-0.190809912898503));
#105815=DIRECTION('center_axis',(-0.981627005099017,0.,-0.190809912898503));
#105816=DIRECTION('ref_axis',(-0.190809912898503,0.,0.981627005099017));
#105817=DIRECTION('',(0.,1.,0.));
#105818=DIRECTION('',(0.,1.,0.));
#105819=DIRECTION('center_axis',(0.,1.,0.));
#105820=DIRECTION('ref_axis',(1.,0.,0.));
#105821=DIRECTION('',(-0.190809912898503,0.,0.981627005099017));
#105822=DIRECTION('',(0.981627005099017,0.,0.190809912898503));
#105823=DIRECTION('',(-0.190809912898503,0.,0.981627005099017));
#105824=DIRECTION('',(0.981627005099017,0.,0.190809912898503));
#105825=DIRECTION('center_axis',(0.981627005099017,0.,0.190809912898503));
#105826=DIRECTION('ref_axis',(0.,-1.,0.));
#105827=DIRECTION('',(-0.190809912898503,0.,0.981627005099017));
#105828=DIRECTION('',(0.,-1.,0.));
#105829=DIRECTION('',(0.,-1.,0.));
#105830=DIRECTION('center_axis',(0.,-1.,0.));
#105831=DIRECTION('ref_axis',(0.,0.,-1.));
#105832=DIRECTION('',(-0.190809912898503,0.,0.981627005099017));
#105833=DIRECTION('',(-0.981627005099017,0.,-0.190809912898503));
#105834=DIRECTION('',(-0.981627005099017,0.,-0.190809912898503));
#105835=DIRECTION('center_axis',(-0.981627005099017,0.,-0.190809912898503));
#105836=DIRECTION('ref_axis',(-0.190809912898503,0.,0.981627005099017));
#105837=DIRECTION('',(0.,1.,0.));
#105838=DIRECTION('',(0.,1.,0.));
#105839=DIRECTION('center_axis',(0.,1.,0.));
#105840=DIRECTION('ref_axis',(1.,0.,0.));
#105841=DIRECTION('',(-0.190809912898503,0.,0.981627005099017));
#105842=DIRECTION('',(0.981627005099017,0.,0.190809912898503));
#105843=DIRECTION('',(-0.190809912898503,0.,0.981627005099017));
#105844=DIRECTION('',(0.981627005099017,0.,0.190809912898503));
#105845=DIRECTION('center_axis',(0.981627005099017,0.,0.190809912898503));
#105846=DIRECTION('ref_axis',(0.,-1.,0.));
#105847=DIRECTION('',(-0.190809912898503,0.,0.981627005099017));
#105848=DIRECTION('',(0.,-1.,0.));
#105849=DIRECTION('',(0.,-1.,0.));
#105850=DIRECTION('center_axis',(0.,-1.,0.));
#105851=DIRECTION('ref_axis',(0.,0.,-1.));
#105852=DIRECTION('',(-0.190809912898503,0.,0.981627005099017));
#105853=DIRECTION('',(-0.981627005099017,0.,-0.190809912898503));
#105854=DIRECTION('',(-0.981627005099017,0.,-0.190809912898503));
#105855=DIRECTION('center_axis',(-0.981627005099017,0.,-0.190809912898503));
#105856=DIRECTION('ref_axis',(-0.190809912898503,0.,0.981627005099017));
#105857=DIRECTION('',(0.,1.,0.));
#105858=DIRECTION('',(0.,1.,0.));
#105859=DIRECTION('center_axis',(0.,1.,0.));
#105860=DIRECTION('ref_axis',(1.,0.,0.));
#105861=DIRECTION('',(-0.190809912898503,0.,0.981627005099017));
#105862=DIRECTION('',(0.981627005099017,0.,0.190809912898503));
#105863=DIRECTION('',(-0.190809912898503,0.,0.981627005099017));
#105864=DIRECTION('',(0.981627005099017,0.,0.190809912898503));
#105865=DIRECTION('center_axis',(0.981627005099017,0.,0.190809912898503));
#105866=DIRECTION('ref_axis',(0.,-1.,0.));
#105867=DIRECTION('',(-0.190809912898503,0.,0.981627005099017));
#105868=DIRECTION('',(0.,-1.,0.));
#105869=DIRECTION('',(0.,-1.,0.));
#105870=DIRECTION('center_axis',(0.,-1.,0.));
#105871=DIRECTION('ref_axis',(0.,0.,-1.));
#105872=DIRECTION('',(-0.190809912898503,0.,0.981627005099017));
#105873=DIRECTION('',(-0.981627005099017,0.,-0.190809912898503));
#105874=DIRECTION('',(-0.981627005099017,0.,-0.190809912898503));
#105875=DIRECTION('center_axis',(-0.981627005099017,0.,-0.190809912898503));
#105876=DIRECTION('ref_axis',(-0.190809912898503,0.,0.981627005099017));
#105877=DIRECTION('',(0.,1.,0.));
#105878=DIRECTION('',(0.,1.,0.));
#105879=DIRECTION('center_axis',(0.,1.,0.));
#105880=DIRECTION('ref_axis',(1.,0.,0.));
#105881=DIRECTION('',(-0.190809912898503,0.,0.981627005099017));
#105882=DIRECTION('',(0.981627005099017,0.,0.190809912898503));
#105883=DIRECTION('',(-0.190809912898503,0.,0.981627005099017));
#105884=DIRECTION('',(0.981627005099017,0.,0.190809912898503));
#105885=DIRECTION('center_axis',(0.981627005099017,0.,0.190809912898503));
#105886=DIRECTION('ref_axis',(0.,-1.,0.));
#105887=DIRECTION('',(-0.190809912898503,0.,0.981627005099017));
#105888=DIRECTION('',(0.,-1.,0.));
#105889=DIRECTION('',(0.,-1.,0.));
#105890=DIRECTION('center_axis',(0.,-1.,0.));
#105891=DIRECTION('ref_axis',(0.,0.,-1.));
#105892=DIRECTION('',(-0.190809912898503,0.,0.981627005099017));
#105893=DIRECTION('',(-0.981627005099017,0.,-0.190809912898503));
#105894=DIRECTION('',(-0.981627005099017,0.,-0.190809912898503));
#105895=DIRECTION('center_axis',(-0.981627005099017,0.,-0.190809912898503));
#105896=DIRECTION('ref_axis',(-0.190809912898503,0.,0.981627005099017));
#105897=DIRECTION('',(0.,1.,0.));
#105898=DIRECTION('',(0.,1.,0.));
#105899=DIRECTION('center_axis',(0.,1.,0.));
#105900=DIRECTION('ref_axis',(1.,0.,0.));
#105901=DIRECTION('',(-0.190809912898503,0.,0.981627005099017));
#105902=DIRECTION('',(0.981627005099017,0.,0.190809912898503));
#105903=DIRECTION('',(-0.190809912898503,0.,0.981627005099017));
#105904=DIRECTION('',(0.981627005099017,0.,0.190809912898503));
#105905=DIRECTION('center_axis',(0.981627005099017,0.,0.190809912898503));
#105906=DIRECTION('ref_axis',(0.,-1.,0.));
#105907=DIRECTION('',(-0.190809912898503,0.,0.981627005099017));
#105908=DIRECTION('',(0.,-1.,0.));
#105909=DIRECTION('',(0.,-1.,0.));
#105910=DIRECTION('center_axis',(0.,-1.,0.));
#105911=DIRECTION('ref_axis',(0.,0.,-1.));
#105912=DIRECTION('',(-0.190809912898503,0.,0.981627005099017));
#105913=DIRECTION('',(-0.981627005099017,0.,-0.190809912898503));
#105914=DIRECTION('',(-0.981627005099017,0.,-0.190809912898503));
#105915=DIRECTION('center_axis',(-0.981627005099017,0.,-0.190809912898503));
#105916=DIRECTION('ref_axis',(-0.190809912898503,0.,0.981627005099017));
#105917=DIRECTION('',(0.,1.,0.));
#105918=DIRECTION('',(0.,1.,0.));
#105919=DIRECTION('center_axis',(0.,1.,0.));
#105920=DIRECTION('ref_axis',(1.,0.,0.));
#105921=DIRECTION('',(-0.190809912898503,0.,0.981627005099017));
#105922=DIRECTION('',(0.981627005099017,0.,0.190809912898503));
#105923=DIRECTION('',(-0.190809912898503,0.,0.981627005099017));
#105924=DIRECTION('',(0.981627005099017,0.,0.190809912898503));
#105925=DIRECTION('center_axis',(0.981627005099017,0.,0.190809912898503));
#105926=DIRECTION('ref_axis',(0.,-1.,0.));
#105927=DIRECTION('',(-0.190809912898503,0.,0.981627005099017));
#105928=DIRECTION('',(0.,-1.,0.));
#105929=DIRECTION('',(0.,-1.,0.));
#105930=DIRECTION('center_axis',(0.,-1.,0.));
#105931=DIRECTION('ref_axis',(0.,0.,-1.));
#105932=DIRECTION('',(-0.190809912898503,0.,0.981627005099017));
#105933=DIRECTION('',(-0.981627005099017,0.,-0.190809912898503));
#105934=DIRECTION('',(-0.981627005099017,0.,-0.190809912898503));
#105935=DIRECTION('center_axis',(-0.981627005099017,0.,-0.190809912898503));
#105936=DIRECTION('ref_axis',(-0.190809912898503,0.,0.981627005099017));
#105937=DIRECTION('',(0.,1.,0.));
#105938=DIRECTION('',(0.,1.,0.));
#105939=DIRECTION('center_axis',(0.,1.,0.));
#105940=DIRECTION('ref_axis',(1.,0.,0.));
#105941=DIRECTION('',(-0.190809912898503,0.,0.981627005099017));
#105942=DIRECTION('',(0.981627005099017,0.,0.190809912898503));
#105943=DIRECTION('',(-0.190809912898503,0.,0.981627005099017));
#105944=DIRECTION('',(0.981627005099017,0.,0.190809912898503));
#105945=DIRECTION('center_axis',(0.981627005099017,0.,0.190809912898503));
#105946=DIRECTION('ref_axis',(0.,-1.,0.));
#105947=DIRECTION('',(-0.190809912898503,0.,0.981627005099017));
#105948=DIRECTION('',(0.,-1.,0.));
#105949=DIRECTION('',(0.,-1.,0.));
#105950=DIRECTION('center_axis',(0.,-1.,0.));
#105951=DIRECTION('ref_axis',(0.,0.,-1.));
#105952=DIRECTION('',(-0.190809912898503,0.,0.981627005099017));
#105953=DIRECTION('',(-0.981627005099017,0.,-0.190809912898503));
#105954=DIRECTION('',(-0.981627005099017,0.,-0.190809912898503));
#105955=DIRECTION('center_axis',(-0.981627005099017,0.,-0.190809912898503));
#105956=DIRECTION('ref_axis',(-0.190809912898503,0.,0.981627005099017));
#105957=DIRECTION('',(0.,1.,0.));
#105958=DIRECTION('',(0.,1.,0.));
#105959=DIRECTION('center_axis',(0.,1.,0.));
#105960=DIRECTION('ref_axis',(1.,0.,0.));
#105961=DIRECTION('',(-0.190809912898503,0.,0.981627005099017));
#105962=DIRECTION('',(0.981627005099017,0.,0.190809912898503));
#105963=DIRECTION('',(-0.190809912898503,0.,0.981627005099017));
#105964=DIRECTION('',(0.981627005099017,0.,0.190809912898503));
#105965=DIRECTION('center_axis',(0.981627005099017,0.,0.190809912898503));
#105966=DIRECTION('ref_axis',(0.,-1.,0.));
#105967=DIRECTION('',(-0.190809912898503,0.,0.981627005099017));
#105968=DIRECTION('',(0.,-1.,0.));
#105969=DIRECTION('',(0.,-1.,0.));
#105970=DIRECTION('center_axis',(0.,-1.,0.));
#105971=DIRECTION('ref_axis',(0.,0.,-1.));
#105972=DIRECTION('',(-0.190809912898503,0.,0.981627005099017));
#105973=DIRECTION('',(-0.981627005099017,0.,-0.190809912898503));
#105974=DIRECTION('',(-0.981627005099017,0.,-0.190809912898503));
#105975=DIRECTION('center_axis',(-0.981627005099017,0.,-0.190809912898503));
#105976=DIRECTION('ref_axis',(-0.190809912898503,0.,0.981627005099017));
#105977=DIRECTION('',(0.,1.,0.));
#105978=DIRECTION('',(0.,1.,0.));
#105979=DIRECTION('center_axis',(0.190809912898503,0.,-0.981627005099017));
#105980=DIRECTION('ref_axis',(0.,-1.,0.));
#105981=DIRECTION('center_axis',(0.190809912898503,0.,-0.981627005099017));
#105982=DIRECTION('ref_axis',(0.,-1.,0.));
#105983=DIRECTION('',(0.981627005099017,0.,0.190809912898503));
#105984=DIRECTION('',(0.,-1.,0.));
#105985=DIRECTION('',(-0.981627005099017,0.,-0.190809912898503));
#105986=DIRECTION('',(0.,1.,0.));
#105987=DIRECTION('center_axis',(0.,1.,0.));
#105988=DIRECTION('ref_axis',(1.,0.,0.));
#105989=DIRECTION('',(-0.190809912898503,0.,0.981627005099017));
#105990=DIRECTION('',(-0.190809912898503,0.,0.981627005099017));
#105991=DIRECTION('',(0.981627005099017,0.,0.190809912898503));
#105992=DIRECTION('center_axis',(0.981627005099017,0.,0.190809912898503));
#105993=DIRECTION('ref_axis',(0.,-1.,0.));
#105994=DIRECTION('',(-0.190809912898503,0.,0.981627005099017));
#105995=DIRECTION('',(0.,-1.,0.));
#105996=DIRECTION('center_axis',(0.,-1.,0.));
#105997=DIRECTION('ref_axis',(0.,0.,-1.));
#105998=DIRECTION('',(-0.190809912898503,0.,0.981627005099017));
#105999=DIRECTION('',(-0.981627005099017,0.,-0.190809912898503));
#106000=DIRECTION('center_axis',(-0.981627005099017,0.,-0.190809912898503));
#106001=DIRECTION('ref_axis',(-0.190809912898503,0.,0.981627005099017));
#106002=DIRECTION('',(0.,1.,0.));
#106003=DIRECTION('center_axis',(0.190809912898503,0.,-0.981627005099017));
#106004=DIRECTION('ref_axis',(0.,-1.,0.));
#106005=DIRECTION('center_axis',(0.190809912898503,0.,-0.981627005099017));
#106006=DIRECTION('ref_axis',(0.,-1.,0.));
#106007=DIRECTION('center_axis',(0.190809912898503,0.,-0.981627005099017));
#106008=DIRECTION('ref_axis',(0.,-1.,0.));
#106009=DIRECTION('',(-0.981627005099017,0.,-0.190809912898503));
#106010=DIRECTION('center_axis',(0.190809912898503,0.,-0.981627005099017));
#106011=DIRECTION('ref_axis',(0.,-1.,0.));
#106012=DIRECTION('',(-0.981627005099017,-1.340542928837E-14,-0.190809912898503));
#106013=DIRECTION('center_axis',(-0.190809912898503,0.,0.981627005099017));
#106014=DIRECTION('ref_axis',(0.,1.,0.));
#106015=DIRECTION('',(-0.981627005099017,0.,-0.190809912898503));
#106016=DIRECTION('center_axis',(-0.190809912898503,0.,0.981627005099017));
#106017=DIRECTION('ref_axis',(0.,1.,0.));
#106018=DIRECTION('',(-0.981627005099017,1.608651514604E-14,-0.190809912898503));
#106019=DIRECTION('center_axis',(-0.981627005099017,0.,-0.190809912898503));
#106020=DIRECTION('ref_axis',(-1.19712313814501E-14,1.,6.15863391467038E-14));
#106021=DIRECTION('center_axis',(-0.981627005099017,0.,-0.190809912898503));
#106022=DIRECTION('ref_axis',(4.2134636976251E-15,1.,-2.16762834161202E-14));
#106023=DIRECTION('center_axis',(-0.190809912898503,0.,0.981627005099017));
#106024=DIRECTION('ref_axis',(0.,1.,0.));
#106025=DIRECTION('',(0.,-1.,0.));
#106026=DIRECTION('center_axis',(-0.190809912898503,0.,0.981627005099017));
#106027=DIRECTION('ref_axis',(0.,1.,0.));
#106028=DIRECTION('',(0.,-1.,0.));
#106029=DIRECTION('center_axis',(0.190809912898503,0.,-0.981627005099017));
#106030=DIRECTION('ref_axis',(0.,-1.,0.));
#106031=DIRECTION('',(0.,-1.,0.));
#106032=DIRECTION('center_axis',(0.190809912898503,0.,-0.981627005099017));
#106033=DIRECTION('ref_axis',(0.,-1.,0.));
#106034=DIRECTION('',(0.,-1.,0.));
#106035=DIRECTION('center_axis',(0.,-1.,0.));
#106036=DIRECTION('ref_axis',(-0.981627005099094,0.,-0.190809912898106));
#106037=DIRECTION('center_axis',(0.,-1.,0.));
#106038=DIRECTION('ref_axis',(-0.981627005099092,0.,-0.190809912898117));
#106039=DIRECTION('center_axis',(0.190809912898503,0.,-0.981627005099017));
#106040=DIRECTION('ref_axis',(0.,-1.,0.));
#106041=DIRECTION('center_axis',(-0.190809912898503,0.,0.981627005099017));
#106042=DIRECTION('ref_axis',(0.981627005099017,0.,0.190809912898503));
#106043=DIRECTION('center_axis',(1.,-6.12323399573677E-17,0.));
#106044=DIRECTION('ref_axis',(0.,-1.,0.));
#106045=DIRECTION('center_axis',(0.,-1.,0.));
#106046=DIRECTION('ref_axis',(-0.146165436076237,0.,0.989260160572861));
#106047=DIRECTION('center_axis',(0.981627005099017,2.42026211186394E-17,
0.190809912898504));
#106048=DIRECTION('ref_axis',(-0.190613830300973,0.0453233971548897,0.980618252618384));
#106049=DIRECTION('center_axis',(0.,1.,0.));
#106050=DIRECTION('ref_axis',(-0.17808229353532,0.,0.98401559780788));
#106051=DIRECTION('center_axis',(-0.981627005099017,-1.25430828081473E-17,
-0.190809912898504));
#106052=DIRECTION('ref_axis',(-0.190793943836834,0.0129373445166805,0.981544851808639));
#106053=DIRECTION('center_axis',(0.,-1.,0.));
#106054=DIRECTION('ref_axis',(0.,0.,-1.));
#106055=DIRECTION('',(-0.190809912898503,0.,0.981627005099017));
#106056=DIRECTION('',(-0.190809912898503,0.,0.981627005099017));
#106057=DIRECTION('center_axis',(0.,-1.,0.));
#106058=DIRECTION('ref_axis',(-0.147019041943122,0.,0.989133662002323));
#106059=DIRECTION('center_axis',(0.981627005099017,0.,0.190809912898503));
#106060=DIRECTION('ref_axis',(0.,-1.,0.));
#106061=DIRECTION('',(-0.190809912898503,0.,0.981627005099017));
#106062=DIRECTION('center_axis',(0.981627005099017,1.7913993378229E-18,
0.190809912898503));
#106063=DIRECTION('ref_axis',(-0.190621242411065,0.0444589430893387,0.980656384428838));
#106064=DIRECTION('center_axis',(0.,1.,0.));
#106065=DIRECTION('ref_axis',(1.,0.,0.));
#106066=DIRECTION('',(-0.190809912898503,0.,0.981627005099017));
#106067=DIRECTION('center_axis',(0.,1.,0.));
#106068=DIRECTION('ref_axis',(-0.178325347032483,0.,0.98397158018194));
#106069=DIRECTION('center_axis',(-0.981627005099017,0.,-0.190809912898503));
#106070=DIRECTION('ref_axis',(-0.190809912898503,0.,0.981627005099017));
#106071=DIRECTION('center_axis',(-0.981627005099017,8.94076702692101E-19,
-0.190809912898503));
#106072=DIRECTION('ref_axis',(-0.190794546115091,0.0126910417304199,0.981547950246208));
#106073=DIRECTION('center_axis',(1.,-6.12323399573677E-17,0.));
#106074=DIRECTION('ref_axis',(0.,-1.,0.));
#106075=DIRECTION('center_axis',(-0.190809912898504,0.,0.981627005099017));
#106076=DIRECTION('ref_axis',(0.981627005099017,0.,0.190809912898504));
#106077=DIRECTION('center_axis',(0.190809912898503,0.,-0.981627005099017));
#106078=DIRECTION('ref_axis',(0.,-1.,0.));
#106079=DIRECTION('axis',(0.,0.,1.));
#106080=DIRECTION('refdir',(1.,0.,0.));
#106081=DIRECTION('center_axis',(-1.,0.,0.));
#106082=DIRECTION('ref_axis',(0.,-0.924224592736303,-0.381849318686593));
#106083=DIRECTION('',(1.,0.,0.));
#106084=DIRECTION('',(1.,0.,0.));
#106085=DIRECTION('center_axis',(-1.,0.,0.));
#106086=DIRECTION('ref_axis',(0.,0.924224592736303,0.381849318686593));
#106087=DIRECTION('center_axis',(-1.,0.,0.));
#106088=DIRECTION('ref_axis',(0.,0.924224592736303,0.381849318686593));
#106089=DIRECTION('',(-1.,0.,0.));
#106090=DIRECTION('center_axis',(-1.,0.,0.));
#106091=DIRECTION('ref_axis',(0.,-0.924224592736303,-0.381849318686593));
#106092=DIRECTION('',(1.,0.,0.));
#106093=DIRECTION('center_axis',(-1.,0.,0.));
#106094=DIRECTION('ref_axis',(0.,-0.924224592736303,-0.381849318686593));
#106095=DIRECTION('',(1.,0.,0.));
#106096=DIRECTION('center_axis',(-1.,0.,0.));
#106097=DIRECTION('ref_axis',(0.,-0.924224592736303,-0.381849318686593));
#106098=DIRECTION('',(1.,0.,0.));
#106099=DIRECTION('center_axis',(-1.,0.,0.));
#106100=DIRECTION('ref_axis',(0.,-0.924224592736303,-0.381849318686593));
#106101=DIRECTION('',(1.,0.,0.));
#106102=DIRECTION('center_axis',(-1.,0.,0.));
#106103=DIRECTION('ref_axis',(0.,-0.924224592736303,-0.381849318686593));
#106104=DIRECTION('',(1.,0.,0.));
#106105=DIRECTION('center_axis',(-1.,0.,0.));
#106106=DIRECTION('ref_axis',(0.,-0.924224592736303,-0.381849318686593));
#106107=DIRECTION('',(1.,0.,0.));
#106108=DIRECTION('center_axis',(-1.,0.,0.));
#106109=DIRECTION('ref_axis',(0.,-0.924224592736303,-0.381849318686593));
#106110=DIRECTION('',(1.,0.,0.));
#106111=DIRECTION('center_axis',(-1.,0.,0.));
#106112=DIRECTION('ref_axis',(0.,-0.924224592736303,-0.381849318686593));
#106113=DIRECTION('',(1.,0.,0.));
#106114=DIRECTION('center_axis',(1.,0.,0.));
#106115=DIRECTION('ref_axis',(0.,0.999244149014678,-0.0388732640761329));
#106116=DIRECTION('center_axis',(-1.,0.,0.));
#106117=DIRECTION('ref_axis',(0.,-0.924224592736303,-0.381849318686593));
#106118=DIRECTION('',(1.,0.,0.));
#106119=DIRECTION('center_axis',(1.,0.,0.));
#106120=DIRECTION('ref_axis',(0.,0.999244149014678,-0.0388732640761329));
#106121=DIRECTION('center_axis',(-1.,0.,0.));
#106122=DIRECTION('ref_axis',(0.,-0.924224592736303,-0.381849318686593));
#106123=DIRECTION('',(1.,0.,0.));
#106124=DIRECTION('center_axis',(-1.,0.,0.));
#106125=DIRECTION('ref_axis',(0.,-0.924224592736303,-0.381849318686593));
#106126=DIRECTION('',(1.,0.,0.));
#106127=DIRECTION('center_axis',(-1.,0.,0.));
#106128=DIRECTION('ref_axis',(0.,-0.924224592736303,-0.381849318686593));
#106129=DIRECTION('',(1.,0.,0.));
#106130=DIRECTION('center_axis',(-1.,0.,0.));
#106131=DIRECTION('ref_axis',(0.,-0.924224592736303,-0.381849318686593));
#106132=DIRECTION('',(1.,0.,0.));
#106133=DIRECTION('center_axis',(-1.,0.,0.));
#106134=DIRECTION('ref_axis',(0.,-0.924224592736303,-0.381849318686593));
#106135=DIRECTION('',(1.,0.,0.));
#106136=DIRECTION('center_axis',(-1.,0.,0.));
#106137=DIRECTION('ref_axis',(0.,-0.924224592736303,-0.381849318686593));
#106138=DIRECTION('',(1.,0.,0.));
#106139=DIRECTION('center_axis',(-1.,0.,0.));
#106140=DIRECTION('ref_axis',(0.,-0.924224592736303,-0.381849318686593));
#106141=DIRECTION('center_axis',(1.,0.,0.));
#106142=DIRECTION('ref_axis',(0.,-0.924224592736303,-0.381849318686593));
#106143=DIRECTION('center_axis',(1.,0.,0.));
#106144=DIRECTION('ref_axis',(0.,-0.924224592736303,-0.381849318686593));
#106145=DIRECTION('',(1.,0.,0.));
#106146=DIRECTION('',(-1.,0.,0.));
#106147=DIRECTION('',(1.,0.,0.));
#106148=DIRECTION('center_axis',(-1.,7.59792509022099E-17,3.13913148593356E-17));
#106149=DIRECTION('ref_axis',(-8.2208644413218E-17,-0.924224592736303,-0.381849318686593));
#106150=DIRECTION('',(0.70710665146941,-0.653525596750962,-0.270008292167144));
#106151=DIRECTION('center_axis',(1.,0.,0.));
#106152=DIRECTION('ref_axis',(0.,-0.050910732461195,0.99870320782516));
#106153=DIRECTION('center_axis',(1.,0.,0.));
#106154=DIRECTION('ref_axis',(0.,0.924224592736303,0.381849318686593));
#106155=DIRECTION('',(-1.,0.,0.));
#106156=DIRECTION('',(0.999999999998702,-7.34588796642656E-7,-1.43405400215834E-6));
#106157=DIRECTION('center_axis',(1.,0.,0.));
#106158=DIRECTION('ref_axis',(0.,0.924224592736303,0.381849318686593));
#106159=DIRECTION('',(-1.,0.,0.));
#106160=DIRECTION('center_axis',(1.,0.,0.));
#106161=DIRECTION('ref_axis',(0.,0.924224592736303,0.381849318686593));
#106162=DIRECTION('',(-1.,0.,0.));
#106163=DIRECTION('center_axis',(1.,0.,0.));
#106164=DIRECTION('ref_axis',(0.,0.924224592736303,0.381849318686593));
#106165=DIRECTION('',(-1.,0.,0.));
#106166=DIRECTION('center_axis',(1.,0.,0.));
#106167=DIRECTION('ref_axis',(0.,0.924224592736303,0.381849318686592));
#106168=DIRECTION('',(-1.,0.,0.));
#106169=DIRECTION('',(0.999999999947399,4.18358171207589E-7,1.02482902784251E-5));
#106170=DIRECTION('center_axis',(1.,0.,0.));
#106171=DIRECTION('ref_axis',(0.,0.924224592736303,0.381849318686592));
#106172=DIRECTION('',(-1.,0.,0.));
#106173=DIRECTION('center_axis',(1.,0.,0.));
#106174=DIRECTION('ref_axis',(0.,0.924224592736303,0.381849318686592));
#106175=DIRECTION('',(-1.,0.,0.));
#106176=DIRECTION('center_axis',(1.,0.,0.));
#106177=DIRECTION('ref_axis',(0.,0.924224592736303,0.381849318686592));
#106178=DIRECTION('',(-1.,0.,0.));
#106179=DIRECTION('center_axis',(1.,0.,0.));
#106180=DIRECTION('ref_axis',(0.,0.924224592736303,0.381849318686592));
#106181=DIRECTION('',(-1.,0.,0.));
#106182=DIRECTION('center_axis',(-1.,0.,0.));
#106183=DIRECTION('ref_axis',(0.,0.924224592736303,0.381849318686592));
#106184=DIRECTION('center_axis',(1.,1.82571941840305E-14,2.33421417227065E-14));
#106185=DIRECTION('ref_axis',(-2.57869287727445E-14,0.924224592736303,0.381849318686593));
#106186=DIRECTION('',(-1.,-1.82571941840305E-14,-2.33421417227065E-14));
#106187=DIRECTION('center_axis',(0.,-0.695858933987439,0.718178490341966));
#106188=DIRECTION('ref_axis',(-0.0305944370091769,0.717842297089703,0.69553318895152));
#106189=DIRECTION('center_axis',(1.,1.82571941840305E-14,2.33421417227065E-14));
#106190=DIRECTION('ref_axis',(-2.57869287727445E-14,0.924224592736303,0.381849318686593));
#106191=DIRECTION('',(-1.,-1.82571941840305E-14,-2.33421417227065E-14));
#106192=DIRECTION('center_axis',(1.,1.82571941840305E-14,2.33421417227065E-14));
#106193=DIRECTION('ref_axis',(-2.57869287727445E-14,0.924224592736303,0.381849318686593));
#106194=DIRECTION('',(-1.,-1.82571941840305E-14,-2.33421417227065E-14));
#106195=DIRECTION('center_axis',(1.,0.,0.));
#106196=DIRECTION('ref_axis',(0.,0.924224592736303,0.381849318686593));
#106197=DIRECTION('',(-1.,0.,0.));
#106198=DIRECTION('',(-0.999999999940701,1.01456975879523E-5,3.95770558922334E-6));
#106199=DIRECTION('center_axis',(1.,0.,0.));
#106200=DIRECTION('ref_axis',(0.,0.924224592736303,0.381849318686593));
#106201=DIRECTION('',(-1.,0.,0.));
#106202=DIRECTION('center_axis',(1.,0.,0.));
#106203=DIRECTION('ref_axis',(0.,0.924224592736303,0.381849318686593));
#106204=DIRECTION('',(-1.,0.,0.));
#106205=DIRECTION('center_axis',(1.,0.,0.));
#106206=DIRECTION('ref_axis',(0.,0.924224592736303,0.381849318686593));
#106207=DIRECTION('',(-1.,0.,0.));
#106208=DIRECTION('center_axis',(1.,-2.54046812768854E-17,-1.04961070212471E-17));
#106209=DIRECTION('ref_axis',(2.74875625216498E-17,0.924224592736303,0.381849318686593));
#106210=DIRECTION('',(-0.707106662296841,0.653525586743986,0.270008288032699));
#106211=DIRECTION('center_axis',(-1.,0.,0.));
#106212=DIRECTION('ref_axis',(0.,-0.316348137924587,-0.948643165595814));
#106213=DIRECTION('center_axis',(-1.,0.,0.));
#106214=DIRECTION('ref_axis',(0.,-0.916443657855559,0.400163743955299));
#106215=DIRECTION('center_axis',(1.,-2.54046812768854E-17,-1.04961070212471E-17));
#106216=DIRECTION('ref_axis',(2.74875625216498E-17,0.924224592736303,0.381849318686593));
#106217=DIRECTION('center_axis',(-1.,0.,0.));
#106218=DIRECTION('ref_axis',(0.,-0.316348137924587,-0.948643165595814));
#106219=DIRECTION('center_axis',(0.965925826289076,0.239206926552251,0.0988298760355017));
#106220=DIRECTION('ref_axis',(-0.258819045102494,0.892732403415498,0.368838118670266));
#106221=DIRECTION('center_axis',(1.,2.30623636574203E-15,5.83716380003748E-15));
#106222=DIRECTION('ref_axis',(-4.3603973859905E-15,0.924224592736086,0.381849318687119));
#106223=DIRECTION('',(0.965925826289076,0.239206926552251,0.0988298760355017));
#106224=DIRECTION('center_axis',(1.,-2.30623636574271E-15,-5.83716380003825E-15));
#106225=DIRECTION('ref_axis',(4.36039738597361E-15,0.924224592737593,0.381849318683469));
#106226=DIRECTION('center_axis',(1.,0.,0.));
#106227=DIRECTION('ref_axis',(0.,0.924224592736303,0.381849318686593));
#106228=DIRECTION('center_axis',(1.,1.82571941840305E-14,2.33421417227065E-14));
#106229=DIRECTION('ref_axis',(-2.57869287727445E-14,0.924224592736303,0.381849318686593));
#106230=DIRECTION('center_axis',(0.,-0.393059646033816,-0.919512976884922));
#106231=DIRECTION('ref_axis',(-0.013064730535851,-0.919434498995661,0.393026099480206));
#106232=DIRECTION('center_axis',(0.965925826289076,0.239206926552251,0.0988298760355016));
#106233=DIRECTION('ref_axis',(-0.258819045102493,0.892732403415498,0.368838118670267));
#106234=DIRECTION('',(0.965925826289076,0.239206926552251,0.0988298760355015));
#106235=DIRECTION('',(0.965925826289076,0.239206926552251,0.0988298760355015));
#106236=DIRECTION('center_axis',(1.,0.,0.));
#106237=DIRECTION('ref_axis',(0.,0.924224592736303,0.381849318686592));
#106238=DIRECTION('center_axis',(-1.,0.,0.));
#106239=DIRECTION('ref_axis',(0.,0.924224592736303,0.381849318686592));
#106240=DIRECTION('center_axis',(1.,0.,0.));
#106241=DIRECTION('ref_axis',(0.,0.924224592736303,0.381849318686592));
#106242=DIRECTION('center_axis',(1.,0.,0.));
#106243=DIRECTION('ref_axis',(0.,0.924224592736303,0.381849318686593));
#106244=DIRECTION('',(1.,0.,0.));
#106245=DIRECTION('',(0.461762345735445,0.886264698784526,-0.0361997202927374));
#106246=DIRECTION('',(0.461762444463603,0.789444381060389,-0.404416881565516));
#106247=DIRECTION('center_axis',(0.,0.888370688458611,-0.459126910437161));
#106248=DIRECTION('ref_axis',(-1.,0.,0.));
#106249=DIRECTION('',(0.461762450482966,-0.789465505391419,0.404375636161525));
#106250=DIRECTION('',(0.461762365531076,-0.886266296190208,0.0361603376150716));
#106251=DIRECTION('center_axis',(0.,0.381849318686593,-0.924224592736303));
#106252=DIRECTION('ref_axis',(-1.,0.,0.));
#106253=DIRECTION('',(0.965925826289076,0.239206926552251,0.0988298760355015));
#106254=DIRECTION('center_axis',(-3.19816689560775E-17,0.381849318686593,
-0.924224592736303));
#106255=DIRECTION('ref_axis',(0.995486289304339,0.0877139672710818,0.0362395881964125));
#106256=DIRECTION('center_axis',(-3.19816689560775E-17,0.381849318686593,
-0.924224592736303));
#106257=DIRECTION('ref_axis',(0.995486289304339,0.0877139672710818,0.0362395881964125));
#106258=DIRECTION('center_axis',(-2.85555636349464E-16,0.381849318686593,
-0.924224592736303));
#106259=DIRECTION('ref_axis',(-0.989158808077185,-0.135722160860674,-0.0560744813139883));
#106260=DIRECTION('center_axis',(1.,0.,0.));
#106261=DIRECTION('ref_axis',(0.,-0.381849318686593,0.924224592736303));
#106262=DIRECTION('center_axis',(0.,0.924224592736303,0.381849318686593));
#106263=DIRECTION('ref_axis',(0.,0.381849318686593,-0.924224592736303));
#106264=DIRECTION('center_axis',(-8.53563043435897E-18,-0.381849318686593,
0.924224592736303));
#106265=DIRECTION('ref_axis',(-0.999927597212881,-0.0111214726821253,-0.00459490777440583));
#106266=DIRECTION('center_axis',(-1.,7.59792509022099E-17,3.13913148593356E-17));
#106267=DIRECTION('ref_axis',(-8.2208644413218E-17,-0.924224592736303,-0.381849318686593));
#106268=DIRECTION('',(-1.,0.,0.));
#106269=DIRECTION('',(-0.46175507312697,0.636992745624861,0.617270195670266));
#106270=DIRECTION('center_axis',(0.,-0.0569081128227818,-0.998379420208044));
#106271=DIRECTION('ref_axis',(0.,-0.998379420208044,0.0569081128227818));
#106272=DIRECTION('',(-0.461755065119691,-0.636985304497725,-0.617277880447899));
#106273=DIRECTION('',(-0.461755171831996,0.815781579343936,-0.348256480326666));
#106274=DIRECTION('center_axis',(-1.,0.,0.));
#106275=DIRECTION('ref_axis',(0.,-0.924224592736303,-0.381849318686593));
#106276=DIRECTION('',(-0.461755171705888,-0.815781579302173,0.348256480591701));
#106277=DIRECTION('center_axis',(-1.,0.,0.));
#106278=DIRECTION('ref_axis',(0.,-0.924224592736303,-0.381849318686592));
#106279=DIRECTION('center_axis',(-1.,0.,0.));
#106280=DIRECTION('ref_axis',(0.,-0.924224592736303,-0.381849318686592));
#106281=DIRECTION('',(-1.,0.,0.));
#106282=DIRECTION('center_axis',(-1.,0.,0.));
#106283=DIRECTION('ref_axis',(0.,-0.924224592736303,-0.381849318686592));
#106284=DIRECTION('center_axis',(-1.,0.,0.));
#106285=DIRECTION('ref_axis',(0.,-0.924224592736303,-0.381849318686592));
#106286=DIRECTION('center_axis',(1.,3.80693114761575E-17,1.57285802220435E-17));
#106287=DIRECTION('ref_axis',(-4.11905415364978E-17,0.924224592736303,0.381849318686593));
#106288=DIRECTION('',(0.707106580681804,-0.653525662174577,-0.270008319197331));
#106289=DIRECTION('center_axis',(-1.,0.,0.));
#106290=DIRECTION('ref_axis',(-4.11905415364978E-17,0.924224592736303,0.381849318686593));
#106291=DIRECTION('center_axis',(-1.,0.,0.));
#106292=DIRECTION('ref_axis',(0.,0.,1.));
#106293=DIRECTION('center_axis',(-1.,0.,0.));
#106294=DIRECTION('ref_axis',(0.,0.,1.));
#106295=DIRECTION('center_axis',(-1.,0.,0.));
#106296=DIRECTION('ref_axis',(0.,0.,1.));
#106297=DIRECTION('center_axis',(-1.,0.,0.));
#106298=DIRECTION('ref_axis',(0.,-0.924224592736303,-0.381849318686592));
#106299=DIRECTION('center_axis',(-1.,0.,0.));
#106300=DIRECTION('ref_axis',(0.,-0.924224592736303,-0.381849318686592));
#106301=DIRECTION('',(-1.,0.,0.));
#106302=DIRECTION('center_axis',(1.,0.,0.));
#106303=DIRECTION('ref_axis',(0.,0.924224592736303,0.381849318686592));
#106304=DIRECTION('center_axis',(-1.,2.54488112923718E-17,1.05143396202058E-17));
#106305=DIRECTION('ref_axis',(-2.75353106727304E-17,-0.924224592736303,
-0.381849318686592));
#106306=DIRECTION('',(-0.7071070062405,0.653525268862752,0.270008156698027));
#106307=DIRECTION('center_axis',(1.,0.,0.));
#106308=DIRECTION('ref_axis',(0.,-0.924224592736303,-0.381849318686592));
#106309=DIRECTION('center_axis',(-1.,0.,0.));
#106310=DIRECTION('ref_axis',(0.,0.,1.));
#106311=DIRECTION('center_axis',(-1.,0.,0.));
#106312=DIRECTION('ref_axis',(0.,-0.924224592736303,-0.381849318686593));
#106313=DIRECTION('center_axis',(1.,0.,0.));
#106314=DIRECTION('ref_axis',(0.,-0.381849318686592,0.924224592736303));
#106315=DIRECTION('center_axis',(7.6756005494586E-17,-0.381849318686593,
0.924224592736303));
#106316=DIRECTION('ref_axis',(0.99903497276754,-0.0405935937462799,-0.0167715036332949));
#106317=DIRECTION('center_axis',(0.,0.924224592736303,0.381849318686592));
#106318=DIRECTION('ref_axis',(0.,0.381849318686592,-0.924224592736303));
#106319=DIRECTION('center_axis',(0.,-0.381849318686593,0.924224592736303));
#106320=DIRECTION('ref_axis',(-1.,0.,0.));
#106321=DIRECTION('',(0.965925826289076,0.239206926552251,0.0988298760355015));
#106322=DIRECTION('center_axis',(0.965925826289076,0.239206926552251,0.0988298760355016));
#106323=DIRECTION('ref_axis',(0.258819045102494,-0.892732403415497,-0.36883811867027));
#106324=DIRECTION('axis',(0.,0.,1.));
#106325=DIRECTION('refdir',(1.,0.,0.));
#106326=DIRECTION('center_axis',(-1.,0.,0.));
#106327=DIRECTION('ref_axis',(0.,-0.924224592736303,-0.381849318686592));
#106328=DIRECTION('',(1.,0.,0.));
#106329=DIRECTION('',(1.,0.,0.));
#106330=DIRECTION('center_axis',(-1.,0.,0.));
#106331=DIRECTION('ref_axis',(0.,0.924224592736302,0.381849318686594));
#106332=DIRECTION('center_axis',(-1.,0.,0.));
#106333=DIRECTION('ref_axis',(0.,0.924224592736302,0.381849318686594));
#106334=DIRECTION('',(-1.,0.,0.));
#106335=DIRECTION('center_axis',(-1.,0.,0.));
#106336=DIRECTION('ref_axis',(0.,-0.924224592736303,-0.381849318686592));
#106337=DIRECTION('',(1.,0.,0.));
#106338=DIRECTION('center_axis',(-1.,0.,0.));
#106339=DIRECTION('ref_axis',(0.,-0.924224592736303,-0.381849318686592));
#106340=DIRECTION('',(1.,0.,0.));
#106341=DIRECTION('center_axis',(-1.,0.,0.));
#106342=DIRECTION('ref_axis',(0.,-0.924224592736303,-0.381849318686592));
#106343=DIRECTION('',(1.,0.,0.));
#106344=DIRECTION('center_axis',(-1.,0.,0.));
#106345=DIRECTION('ref_axis',(0.,-0.924224592736303,-0.381849318686592));
#106346=DIRECTION('',(1.,0.,0.));
#106347=DIRECTION('center_axis',(-1.,0.,0.));
#106348=DIRECTION('ref_axis',(0.,-0.924224592736303,-0.381849318686592));
#106349=DIRECTION('',(1.,0.,0.));
#106350=DIRECTION('center_axis',(-1.,0.,0.));
#106351=DIRECTION('ref_axis',(0.,-0.924224592736303,-0.381849318686592));
#106352=DIRECTION('',(1.,0.,0.));
#106353=DIRECTION('center_axis',(-1.,0.,0.));
#106354=DIRECTION('ref_axis',(0.,-0.924224592736303,-0.381849318686592));
#106355=DIRECTION('',(1.,0.,0.));
#106356=DIRECTION('center_axis',(-1.,0.,0.));
#106357=DIRECTION('ref_axis',(0.,-0.924224592736303,-0.381849318686593));
#106358=DIRECTION('',(1.,0.,0.));
#106359=DIRECTION('center_axis',(1.,0.,0.));
#106360=DIRECTION('ref_axis',(0.,0.999244149014678,-0.0388732640761329));
#106361=DIRECTION('center_axis',(-1.,0.,0.));
#106362=DIRECTION('ref_axis',(0.,-0.924224592736303,-0.381849318686593));
#106363=DIRECTION('',(1.,0.,0.));
#106364=DIRECTION('center_axis',(1.,0.,0.));
#106365=DIRECTION('ref_axis',(0.,0.999244149014678,-0.0388732640761329));
#106366=DIRECTION('center_axis',(-1.,0.,0.));
#106367=DIRECTION('ref_axis',(0.,-0.924224592736303,-0.381849318686593));
#106368=DIRECTION('',(1.,0.,0.));
#106369=DIRECTION('center_axis',(-1.,0.,0.));
#106370=DIRECTION('ref_axis',(0.,-0.924224592736303,-0.381849318686593));
#106371=DIRECTION('',(1.,0.,0.));
#106372=DIRECTION('center_axis',(-1.,0.,0.));
#106373=DIRECTION('ref_axis',(0.,-0.924224592736303,-0.381849318686593));
#106374=DIRECTION('',(1.,0.,0.));
#106375=DIRECTION('center_axis',(-1.,0.,0.));
#106376=DIRECTION('ref_axis',(0.,-0.924224592736303,-0.381849318686593));
#106377=DIRECTION('',(1.,0.,0.));
#106378=DIRECTION('center_axis',(-1.,0.,0.));
#106379=DIRECTION('ref_axis',(0.,-0.924224592736303,-0.381849318686593));
#106380=DIRECTION('',(1.,0.,0.));
#106381=DIRECTION('center_axis',(-1.,0.,0.));
#106382=DIRECTION('ref_axis',(0.,-0.924224592736303,-0.381849318686593));
#106383=DIRECTION('',(1.,0.,0.));
#106384=DIRECTION('center_axis',(-1.,0.,0.));
#106385=DIRECTION('ref_axis',(0.,-0.924224592736303,-0.381849318686593));
#106386=DIRECTION('center_axis',(1.,0.,0.));
#106387=DIRECTION('ref_axis',(0.,-0.924224592736303,-0.381849318686593));
#106388=DIRECTION('center_axis',(1.,0.,0.));
#106389=DIRECTION('ref_axis',(0.,-0.924224592736303,-0.381849318686593));
#106390=DIRECTION('',(1.,0.,0.));
#106391=DIRECTION('',(-1.,0.,0.));
#106392=DIRECTION('',(1.,0.,0.));
#106393=DIRECTION('center_axis',(-1.,7.59792509022099E-17,3.13913148593356E-17));
#106394=DIRECTION('ref_axis',(-8.2208644413218E-17,-0.924224592736303,-0.381849318686593));
#106395=DIRECTION('',(0.70710665146941,-0.653525596750962,-0.270008292167144));
#106396=DIRECTION('center_axis',(1.,0.,0.));
#106397=DIRECTION('ref_axis',(0.,-0.050910732461195,0.99870320782516));
#106398=DIRECTION('center_axis',(1.,0.,0.));
#106399=DIRECTION('ref_axis',(0.,0.924224592736303,0.381849318686593));
#106400=DIRECTION('',(-1.,0.,0.));
#106401=DIRECTION('',(0.999999999998702,-7.34588841051575E-7,-1.43405422420294E-6));
#106402=DIRECTION('center_axis',(1.,0.,0.));
#106403=DIRECTION('ref_axis',(0.,0.924224592736303,0.381849318686593));
#106404=DIRECTION('',(-1.,0.,0.));
#106405=DIRECTION('center_axis',(1.,0.,0.));
#106406=DIRECTION('ref_axis',(0.,0.924224592736303,0.381849318686593));
#106407=DIRECTION('',(-1.,0.,0.));
#106408=DIRECTION('center_axis',(1.,0.,0.));
#106409=DIRECTION('ref_axis',(0.,0.924224592736303,0.381849318686593));
#106410=DIRECTION('',(-1.,0.,0.));
#106411=DIRECTION('center_axis',(1.,0.,0.));
#106412=DIRECTION('ref_axis',(0.,0.924224592736303,0.381849318686592));
#106413=DIRECTION('',(-1.,0.,0.));
#106414=DIRECTION('',(0.999999999947399,4.18358171207589E-7,1.02482904113352E-5));
#106415=DIRECTION('center_axis',(1.,0.,0.));
#106416=DIRECTION('ref_axis',(0.,0.924224592736303,0.381849318686592));
#106417=DIRECTION('',(-1.,0.,0.));
#106418=DIRECTION('center_axis',(1.,0.,0.));
#106419=DIRECTION('ref_axis',(0.,0.924224592736303,0.381849318686592));
#106420=DIRECTION('',(-1.,0.,0.));
#106421=DIRECTION('center_axis',(1.,0.,0.));
#106422=DIRECTION('ref_axis',(0.,0.924224592736303,0.381849318686592));
#106423=DIRECTION('',(-1.,0.,0.));
#106424=DIRECTION('center_axis',(1.,0.,0.));
#106425=DIRECTION('ref_axis',(0.,0.924224592736303,0.381849318686592));
#106426=DIRECTION('',(-1.,0.,0.));
#106427=DIRECTION('center_axis',(-1.,0.,0.));
#106428=DIRECTION('ref_axis',(0.,0.924224592736303,0.381849318686592));
#106429=DIRECTION('center_axis',(1.,1.82571941840305E-14,2.33421417227065E-14));
#106430=DIRECTION('ref_axis',(-2.57869287727445E-14,0.924224592736303,0.381849318686593));
#106431=DIRECTION('',(-1.,-1.82571941840305E-14,-2.33421417227065E-14));
#106432=DIRECTION('center_axis',(-2.33885900086631E-13,-0.695858933998045,
0.71817849033169));
#106433=DIRECTION('ref_axis',(-0.0305944370088395,0.717842297079444,0.695533188962123));
#106434=DIRECTION('center_axis',(1.,1.82571941840305E-14,2.33421417227065E-14));
#106435=DIRECTION('ref_axis',(-2.57869287727445E-14,0.924224592736303,0.381849318686593));
#106436=DIRECTION('',(-1.,-1.82571941840305E-14,-2.33421417227065E-14));
#106437=DIRECTION('center_axis',(1.,1.82571941840305E-14,2.33421417227065E-14));
#106438=DIRECTION('ref_axis',(-2.57869287727445E-14,0.924224592736303,0.381849318686593));
#106439=DIRECTION('',(-1.,-1.82571941840305E-14,-2.33421417227065E-14));
#106440=DIRECTION('center_axis',(1.,0.,0.));
#106441=DIRECTION('ref_axis',(0.,0.924224592736303,0.381849318686593));
#106442=DIRECTION('',(-1.,0.,0.));
#106443=DIRECTION('',(-0.999999999940701,1.01456975879523E-5,3.95770553001597E-6));
#106444=DIRECTION('center_axis',(1.,0.,0.));
#106445=DIRECTION('ref_axis',(0.,0.924224592736303,0.381849318686593));
#106446=DIRECTION('',(-1.,0.,0.));
#106447=DIRECTION('center_axis',(1.,0.,0.));
#106448=DIRECTION('ref_axis',(0.,0.924224592736303,0.381849318686593));
#106449=DIRECTION('',(-1.,0.,0.));
#106450=DIRECTION('center_axis',(1.,0.,0.));
#106451=DIRECTION('ref_axis',(0.,0.924224592736303,0.381849318686593));
#106452=DIRECTION('',(-1.,0.,0.));
#106453=DIRECTION('center_axis',(1.,-2.54046812768854E-17,-1.04961070212471E-17));
#106454=DIRECTION('ref_axis',(2.74875625216498E-17,0.924224592736303,0.381849318686593));
#106455=DIRECTION('',(-0.707106662296841,0.653525586743986,0.270008288032699));
#106456=DIRECTION('center_axis',(-1.,0.,0.));
#106457=DIRECTION('ref_axis',(0.,-0.316348137924587,-0.948643165595814));
#106458=DIRECTION('center_axis',(-1.,0.,0.));
#106459=DIRECTION('ref_axis',(0.,-0.916443657855559,0.400163743955299));
#106460=DIRECTION('center_axis',(1.,-2.54046812768854E-17,-1.04961070212471E-17));
#106461=DIRECTION('ref_axis',(2.74875625216498E-17,0.924224592736303,0.381849318686593));
#106462=DIRECTION('center_axis',(-1.,0.,0.));
#106463=DIRECTION('ref_axis',(0.,-0.316348137924587,-0.948643165595814));
#106464=DIRECTION('center_axis',(0.965925826289076,0.239206926552251,0.0988298760355017));
#106465=DIRECTION('ref_axis',(-0.258819045102494,0.892732403415498,0.368838118670266));
#106466=DIRECTION('center_axis',(1.,2.30623636574202E-15,5.83716380003748E-15));
#106467=DIRECTION('ref_axis',(-4.36039738599217E-15,0.924224592735944,0.381849318687461));
#106468=DIRECTION('',(0.965925826289076,0.239206926552251,0.0988298760355017));
#106469=DIRECTION('center_axis',(1.,1.15311818287128E-15,2.91858190001905E-15));
#106470=DIRECTION('ref_axis',(-2.18019869299788E-15,0.924224592735703,0.381849318688045));
#106471=DIRECTION('center_axis',(1.,0.,0.));
#106472=DIRECTION('ref_axis',(0.,0.924224592736303,0.381849318686593));
#106473=DIRECTION('center_axis',(1.,1.82571941840305E-14,2.33421417227065E-14));
#106474=DIRECTION('ref_axis',(-2.57869287727445E-14,0.924224592736303,0.381849318686593));
#106475=DIRECTION('center_axis',(0.,-0.393059646019601,-0.919512976890999));
#106476=DIRECTION('ref_axis',(-0.0130647305360937,-0.919434499001734,0.39302609946599));
#106477=DIRECTION('center_axis',(0.965925826289076,0.239206926552251,0.0988298760355016));
#106478=DIRECTION('ref_axis',(-0.258819045102493,0.892732403415498,0.368838118670267));
#106479=DIRECTION('',(0.965925826289076,0.239206926552251,0.0988298760355015));
#106480=DIRECTION('',(0.965925826289076,0.239206926552251,0.0988298760355015));
#106481=DIRECTION('center_axis',(1.,0.,0.));
#106482=DIRECTION('ref_axis',(0.,0.924224592736303,0.381849318686592));
#106483=DIRECTION('center_axis',(-1.,0.,0.));
#106484=DIRECTION('ref_axis',(0.,0.924224592736303,0.381849318686592));
#106485=DIRECTION('center_axis',(1.,0.,0.));
#106486=DIRECTION('ref_axis',(0.,0.924224592736303,0.381849318686592));
#106487=DIRECTION('center_axis',(1.,0.,0.));
#106488=DIRECTION('ref_axis',(0.,0.924224592736303,0.381849318686593));
#106489=DIRECTION('',(1.,0.,0.));
#106490=DIRECTION('',(0.461762345735437,0.88626469878453,-0.0361997202927509));
#106491=DIRECTION('',(0.46176244446361,0.789444381060382,-0.404416881565523));
#106492=DIRECTION('center_axis',(0.,0.888370688458611,-0.459126910437161));
#106493=DIRECTION('ref_axis',(-1.,0.,0.));
#106494=DIRECTION('',(0.461762450482974,-0.789465505391398,0.404375636161556));
#106495=DIRECTION('',(0.461762365531073,-0.886266296190209,0.0361603376150781));
#106496=DIRECTION('center_axis',(0.,0.381849318686593,-0.924224592736303));
#106497=DIRECTION('ref_axis',(-1.,0.,0.));
#106498=DIRECTION('',(0.965925826289076,0.239206926552251,0.0988298760355015));
#106499=DIRECTION('center_axis',(-3.19816689560775E-17,0.381849318686593,
-0.924224592736303));
#106500=DIRECTION('ref_axis',(0.995486289304339,0.0877139672710818,0.0362395881964125));
#106501=DIRECTION('center_axis',(-3.19816689560775E-17,0.381849318686593,
-0.924224592736303));
#106502=DIRECTION('ref_axis',(0.995486289304339,0.0877139672710818,0.0362395881964125));
#106503=DIRECTION('center_axis',(-2.85555636349464E-16,0.381849318686593,
-0.924224592736303));
#106504=DIRECTION('ref_axis',(-0.989158808077185,-0.135722160860674,-0.0560744813139883));
#106505=DIRECTION('center_axis',(1.,0.,0.));
#106506=DIRECTION('ref_axis',(0.,-0.381849318686593,0.924224592736303));
#106507=DIRECTION('center_axis',(0.,0.924224592736303,0.381849318686593));
#106508=DIRECTION('ref_axis',(0.,0.381849318686593,-0.924224592736303));
#106509=DIRECTION('center_axis',(-8.53563043435897E-18,-0.381849318686593,
0.924224592736303));
#106510=DIRECTION('ref_axis',(-0.999927597212881,-0.0111214726821253,-0.00459490777440583));
#106511=DIRECTION('center_axis',(-1.,7.59792509022099E-17,3.13913148593356E-17));
#106512=DIRECTION('ref_axis',(-8.2208644413218E-17,-0.924224592736303,-0.381849318686593));
#106513=DIRECTION('',(-1.,0.,0.));
#106514=DIRECTION('',(-0.461755073126971,0.63699274562483,0.617270195670297));
#106515=DIRECTION('center_axis',(0.,-0.0569081128227818,-0.998379420208044));
#106516=DIRECTION('ref_axis',(0.,-0.998379420208044,0.0569081128227818));
#106517=DIRECTION('',(-0.461755065119693,-0.636985304497731,-0.617277880447891));
#106518=DIRECTION('',(-0.461755171832,0.815781579343933,-0.348256480326666));
#106519=DIRECTION('center_axis',(-1.,0.,0.));
#106520=DIRECTION('ref_axis',(0.,-0.924224592736303,-0.381849318686593));
#106521=DIRECTION('',(-0.461755171705888,-0.815781579302177,0.348256480591692));
#106522=DIRECTION('center_axis',(-1.,0.,0.));
#106523=DIRECTION('ref_axis',(0.,-0.924224592736303,-0.381849318686592));
#106524=DIRECTION('center_axis',(-1.,0.,0.));
#106525=DIRECTION('ref_axis',(0.,-0.924224592736303,-0.381849318686592));
#106526=DIRECTION('',(-1.,0.,0.));
#106527=DIRECTION('center_axis',(-1.,0.,0.));
#106528=DIRECTION('ref_axis',(0.,-0.924224592736303,-0.381849318686592));
#106529=DIRECTION('center_axis',(-1.,0.,0.));
#106530=DIRECTION('ref_axis',(0.,-0.924224592736303,-0.381849318686592));
#106531=DIRECTION('center_axis',(1.,3.80693114761575E-17,1.57285802220435E-17));
#106532=DIRECTION('ref_axis',(-4.11905415364978E-17,0.924224592736303,0.381849318686593));
#106533=DIRECTION('',(0.707106580681804,-0.653525662174577,-0.270008319197331));
#106534=DIRECTION('center_axis',(-1.,0.,0.));
#106535=DIRECTION('ref_axis',(-4.11905415364978E-17,0.924224592736303,0.381849318686593));
#106536=DIRECTION('center_axis',(-1.,0.,0.));
#106537=DIRECTION('ref_axis',(0.,0.,1.));
#106538=DIRECTION('center_axis',(-1.,0.,0.));
#106539=DIRECTION('ref_axis',(0.,0.,1.));
#106540=DIRECTION('center_axis',(-1.,0.,0.));
#106541=DIRECTION('ref_axis',(0.,0.,1.));
#106542=DIRECTION('center_axis',(-1.,0.,0.));
#106543=DIRECTION('ref_axis',(0.,-0.924224592736303,-0.381849318686592));
#106544=DIRECTION('center_axis',(-1.,0.,0.));
#106545=DIRECTION('ref_axis',(0.,-0.924224592736303,-0.381849318686592));
#106546=DIRECTION('',(-1.,0.,0.));
#106547=DIRECTION('center_axis',(1.,0.,0.));
#106548=DIRECTION('ref_axis',(0.,0.924224592736303,0.381849318686592));
#106549=DIRECTION('center_axis',(-1.,2.54488112923718E-17,1.05143396202058E-17));
#106550=DIRECTION('ref_axis',(-2.75353106727304E-17,-0.924224592736303,
-0.381849318686592));
#106551=DIRECTION('',(-0.7071070062405,0.653525268862752,0.270008156698027));
#106552=DIRECTION('center_axis',(1.,0.,0.));
#106553=DIRECTION('ref_axis',(0.,-0.924224592736303,-0.381849318686592));
#106554=DIRECTION('center_axis',(-1.,0.,0.));
#106555=DIRECTION('ref_axis',(0.,0.,1.));
#106556=DIRECTION('center_axis',(-1.,0.,0.));
#106557=DIRECTION('ref_axis',(0.,-0.924224592736303,-0.381849318686592));
#106558=DIRECTION('center_axis',(1.,0.,0.));
#106559=DIRECTION('ref_axis',(0.,-0.381849318686592,0.924224592736303));
#106560=DIRECTION('center_axis',(7.6756005494586E-17,-0.381849318686593,
0.924224592736303));
#106561=DIRECTION('ref_axis',(0.99903497276754,-0.0405935937462799,-0.0167715036332949));
#106562=DIRECTION('center_axis',(0.,0.924224592736303,0.381849318686592));
#106563=DIRECTION('ref_axis',(0.,0.381849318686592,-0.924224592736303));
#106564=DIRECTION('center_axis',(0.,-0.381849318686593,0.924224592736303));
#106565=DIRECTION('ref_axis',(-1.,0.,0.));
#106566=DIRECTION('',(0.965925826289076,0.239206926552251,0.0988298760355015));
#106567=DIRECTION('center_axis',(0.965925826289076,0.239206926552251,0.0988298760355016));
#106568=DIRECTION('ref_axis',(0.258819045102493,-0.8927324034155,-0.368838118670263));
#106569=DIRECTION('',(0.,0.,1.));
#106570=DIRECTION('',(1.,0.,0.));
#106571=DIRECTION('',(0.,0.,1.));
#106572=DIRECTION('',(1.,0.,0.));
#106573=DIRECTION('',(0.,0.,1.));
#106574=DIRECTION('',(1.,0.,0.));
#106575=DIRECTION('',(0.,0.,1.));
#106576=DIRECTION('',(1.,0.,0.));
#106577=DIRECTION('',(0.,0.,1.));
#106578=DIRECTION('',(1.,0.,0.));
#106579=DIRECTION('',(0.,0.,1.));
#106580=DIRECTION('',(1.,0.,0.));
#106581=DIRECTION('',(0.,0.,1.));
#106582=DIRECTION('',(1.,0.,0.));
#106583=DIRECTION('',(0.,0.,1.));
#106584=DIRECTION('',(1.,0.,0.));
#106585=DIRECTION('',(0.,0.,1.));
#106586=DIRECTION('',(1.,0.,0.));
#106587=DIRECTION('',(0.,0.,1.));
#106588=DIRECTION('',(1.,0.,0.));
#106589=DIRECTION('',(0.,0.,1.));
#106590=DIRECTION('',(1.,0.,0.));
#106591=DIRECTION('',(0.,0.,1.));
#106592=DIRECTION('',(1.,0.,0.));
#106593=DIRECTION('',(0.,0.,1.));
#106594=DIRECTION('',(1.,0.,0.));
#106595=CARTESIAN_POINT('',(0.,0.,0.));
#106596=CARTESIAN_POINT('',(0.,0.,0.));
#106597=CARTESIAN_POINT('Origin',(31.9617040371891,10.34163775063,83.3647327807));
#106598=CARTESIAN_POINT('',(32.421019273976,10.3416377503736,81.9367868757674));
#106599=CARTESIAN_POINT('',(33.4389250502851,10.3415988823771,83.1043137625697));
#106600=CARTESIAN_POINT('Origin',(31.9617040310391,10.34163775061,83.36473278179));
#106601=CARTESIAN_POINT('',(32.4699883443439,11.6438812726382,83.90861341978));
#106602=CARTESIAN_POINT('Origin',(31.9617228057091,10.34158590019,83.36483925822));
#106603=CARTESIAN_POINT('',(31.9729372056209,11.0982732621064,82.0695976383883));
#106604=CARTESIAN_POINT('Origin',(31.9617047093191,10.34163562137,83.36473266219));
#106605=CARTESIAN_POINT('Ctrl Pts',(32.4210192738911,10.3416377499008,81.9367868736946));
#106606=CARTESIAN_POINT('Ctrl Pts',(32.3549889539164,10.4466228903284,81.9155474612096));
#106607=CARTESIAN_POINT('Ctrl Pts',(32.2886439073279,10.5550142815435,81.9117786873653));
#106608=CARTESIAN_POINT('Ctrl Pts',(32.1430793277252,10.7979905465623,81.9374456501848));
#106609=CARTESIAN_POINT('Ctrl Pts',(32.050142777925,10.9583234002542,81.9885060907966));
#106610=CARTESIAN_POINT('Ctrl Pts',(31.9729370250153,11.0982734359973,82.0695971663286));
#106611=CARTESIAN_POINT('Origin',(36.3793934194391,111.0724296188,99.78053857024));
#106612=CARTESIAN_POINT('',(33.438915661672,8.83176086632608,83.1042605178143));
#106613=CARTESIAN_POINT('',(33.4389156626291,10.3416377002,83.10426051803));
#106614=CARTESIAN_POINT('',(33.9717701135603,8.83176086676542,86.1262282870246));
#106615=CARTESIAN_POINT('',(30.0527761960508,8.83176086632608,63.9005093315515));
#106616=CARTESIAN_POINT('Origin',(33.6200489988073,9.47404346582926,84.1315187227546));
#106617=CARTESIAN_POINT('Ctrl Pts',(24.1636631729991,13.15706499277,83.51582887991));
#106618=CARTESIAN_POINT('Ctrl Pts',(24.5647380964491,12.88709995962,83.42585917656));
#106619=CARTESIAN_POINT('Ctrl Pts',(25.4508459341791,12.34148054708,83.2280134562701));
#106620=CARTESIAN_POINT('Ctrl Pts',(26.8687546205291,11.61824835454,82.916179282399));
#106621=CARTESIAN_POINT('Ctrl Pts',(28.4012687778591,10.9828277336,82.586899286296));
#106622=CARTESIAN_POINT('Ctrl Pts',(29.9889244426091,10.45524575259,82.256303592466));
#106623=CARTESIAN_POINT('Ctrl Pts',(31.1186113700191,10.16416102927,82.030294447124));
#106624=CARTESIAN_POINT('Ctrl Pts',(31.7224785782191,10.03238128861,81.9125938256419));
#106625=CARTESIAN_POINT('Ctrl Pts',(31.7734801582891,10.0214207908,81.902675068567));
#106626=CARTESIAN_POINT('Ctrl Pts',(24.7567927563091,14.20870211163,82.429604786895));
#106627=CARTESIAN_POINT('Ctrl Pts',(25.1496452921491,13.97393099452,82.369217803208));
#106628=CARTESIAN_POINT('Ctrl Pts',(26.0172627104391,13.5023674652,82.23949810871));
#106629=CARTESIAN_POINT('Ctrl Pts',(27.4045007518391,12.88486233543,82.046577005672));
#106630=CARTESIAN_POINT('Ctrl Pts',(28.9020017624291,12.3485388144,81.8573104046351));
#106631=CARTESIAN_POINT('Ctrl Pts',(30.4496606056791,11.90711756859,81.682769592993));
#106632=CARTESIAN_POINT('Ctrl Pts',(31.5457868459891,11.6648961111,81.574632069656));
#106633=CARTESIAN_POINT('Ctrl Pts',(32.1290979354391,11.55534512451,81.521562061191));
#106634=CARTESIAN_POINT('Ctrl Pts',(32.1783435389591,11.54623433425,81.517112921513));
#106635=CARTESIAN_POINT('Ctrl Pts',(25.7080286493391,15.3150149528,83.14294079435));
#106636=CARTESIAN_POINT('Ctrl Pts',(26.0688989135491,15.0850238123,83.11779004187));
#106637=CARTESIAN_POINT('Ctrl Pts',(26.8689813841791,14.6149583415,83.06541100723));
#106638=CARTESIAN_POINT('Ctrl Pts',(28.1588544048491,13.97195308165,82.99307250027));
#106639=CARTESIAN_POINT('Ctrl Pts',(29.5625282155191,13.3798239155,82.9283215114359));
#106640=CARTESIAN_POINT('Ctrl Pts',(31.0232600341691,12.85540818655,82.874068928702));
#106641=CARTESIAN_POINT('Ctrl Pts',(32.0637075460491,12.53884471205,82.843263250066));
#106642=CARTESIAN_POINT('Ctrl Pts',(32.6188587936791,12.38578792754,82.828526454707));
#106643=CARTESIAN_POINT('Ctrl Pts',(32.6657375309591,12.37297656687,82.827293324418));
#106644=CARTESIAN_POINT('Ctrl Pts',(25.8021387379591,15.06265599365,84.7445289598801));
#106645=CARTESIAN_POINT('Ctrl Pts',(26.1481251487091,14.80092432819,84.71525261791));
#106646=CARTESIAN_POINT('Ctrl Pts',(26.9179060455191,14.25788527696,84.6506238864801));
#106647=CARTESIAN_POINT('Ctrl Pts',(28.1681063763591,13.49072986795,84.54648965191));
#106648=CARTESIAN_POINT('Ctrl Pts',(29.5390059693791,12.75918568124,84.4316840985199));
#106649=CARTESIAN_POINT('Ctrl Pts',(30.9769324167991,12.08864816876,84.30828130528));
#106650=CARTESIAN_POINT('Ctrl Pts',(32.0107143886891,11.66951152981,84.21547396494));
#106651=CARTESIAN_POINT('Ctrl Pts',(32.5660771059891,11.46279434478,84.16380116418));
#106652=CARTESIAN_POINT('Ctrl Pts',(32.6130018292691,11.44545972437,84.15942188772));
#106653=CARTESIAN_POINT('',(31.7476216575109,11.9111986398664,83.9673641909233));
#106654=CARTESIAN_POINT('Ctrl Pts',(31.9729374161714,11.0982730962909,82.0695981250249));
#106655=CARTESIAN_POINT('Ctrl Pts',(31.8773816796382,11.271485744938,82.1699618473536));
#106656=CARTESIAN_POINT('Ctrl Pts',(31.7859691125908,11.4387437257982,82.2941296376232));
#106657=CARTESIAN_POINT('Ctrl Pts',(31.6474513598846,11.7051229822608,82.5594239510954));
#106658=CARTESIAN_POINT('Ctrl Pts',(31.5929885036314,11.8155387095055,82.6976241757693));
#106659=CARTESIAN_POINT('Ctrl Pts',(31.532073047221,11.9664225268417,82.9716240612167));
#106660=CARTESIAN_POINT('Ctrl Pts',(31.51764374752,12.0171944655651,83.1016289408218));
#106661=CARTESIAN_POINT('Ctrl Pts',(31.5267010611325,12.0648278916674,83.3521318330441));
#106662=CARTESIAN_POINT('Ctrl Pts',(31.5440498678541,12.0682904053271,83.4651019787565));
#106663=CARTESIAN_POINT('Ctrl Pts',(31.5950376430365,12.0429521873511,83.6482075907876));
#106664=CARTESIAN_POINT('Ctrl Pts',(31.6203585852615,12.0251659449056,83.7174101258522));
#106665=CARTESIAN_POINT('Ctrl Pts',(31.6790720264413,11.9766646105216,83.8487103915418));
#106666=CARTESIAN_POINT('Ctrl Pts',(31.7121562819556,11.9462064447579,83.910154915883));
#106667=CARTESIAN_POINT('Ctrl Pts',(31.7476258558315,11.9111910957313,83.9673569696238));
#106668=CARTESIAN_POINT('Ctrl Pts',(31.7476216518526,11.9111986410501,83.9673641947199));
#106669=CARTESIAN_POINT('Ctrl Pts',(31.9883196141856,11.8187715270328,83.9478615827402));
#106670=CARTESIAN_POINT('Ctrl Pts',(32.2291184983712,11.7297634578707,83.9280729607192));
#106671=CARTESIAN_POINT('Ctrl Pts',(32.4699886792762,11.6438823126913,83.9086129755005));
#106672=CARTESIAN_POINT('Ctrl Pts',(16.7315271092291,25.77957474242,75.8056538642681));
#106673=CARTESIAN_POINT('Ctrl Pts',(16.8902739491491,25.78276104928,76.726755143248));
#106674=CARTESIAN_POINT('Ctrl Pts',(17.4170423638691,25.68741378017,79.011155596728));
#106675=CARTESIAN_POINT('Ctrl Pts',(18.6971928491291,25.1486541372,82.327981456666));
#106676=CARTESIAN_POINT('Ctrl Pts',(20.3541926191191,24.21296098443,85.29757061493));
#106677=CARTESIAN_POINT('Ctrl Pts',(21.9876235905991,23.12636897321,87.62326197554));
#106678=CARTESIAN_POINT('Ctrl Pts',(23.5303110581191,21.96974605327,89.49482082956));
#106679=CARTESIAN_POINT('Ctrl Pts',(25.0147293345491,20.73535636643,91.08394632963));
#106680=CARTESIAN_POINT('Ctrl Pts',(26.4477039632491,19.42122041898,92.4661164628101));
#106681=CARTESIAN_POINT('Ctrl Pts',(27.8040593501691,18.0525443245,93.66246634875));
#106682=CARTESIAN_POINT('Ctrl Pts',(29.0976297887891,16.61722673478,94.7173081814599));
#106683=CARTESIAN_POINT('Ctrl Pts',(30.3859883571291,15.03805899871,95.692928827));
#106684=CARTESIAN_POINT('Ctrl Pts',(31.6846191544191,13.2490375268,96.6017522016999));
#106685=CARTESIAN_POINT('Ctrl Pts',(32.9283641549091,11.27078505501,97.39922069443));
#106686=CARTESIAN_POINT('Ctrl Pts',(34.0024905191591,9.24026551673301,98.0256740975701));
#106687=CARTESIAN_POINT('Ctrl Pts',(34.8835248980591,7.19980133487202,98.4916705583199));
#106688=CARTESIAN_POINT('Ctrl Pts',(35.5865206621291,5.09129120886101,98.8275149094299));
#106689=CARTESIAN_POINT('Ctrl Pts',(36.0644764908891,2.94897602587201,99.0360923986901));
#106690=CARTESIAN_POINT('Ctrl Pts',(36.2175390832591,1.50759720120401,99.1082321058299));
#106691=CARTESIAN_POINT('Ctrl Pts',(36.2511547877691,0.817200229439614,
99.1309346670101));
#106692=CARTESIAN_POINT('Ctrl Pts',(16.5657307648391,19.34436604072,75.8499470296021));
#106693=CARTESIAN_POINT('Ctrl Pts',(16.7027032210391,19.34727467235,76.647687526976));
#106694=CARTESIAN_POINT('Ctrl Pts',(17.1758927443291,19.26031994756,78.623309386718));
#106695=CARTESIAN_POINT('Ctrl Pts',(18.3744374416091,18.77127275203,81.451029832546));
#106696=CARTESIAN_POINT('Ctrl Pts',(19.9464727370091,17.9342387447,83.90371085737));
#106697=CARTESIAN_POINT('Ctrl Pts',(21.5011129654591,16.97934371574,85.75395997948));
#106698=CARTESIAN_POINT('Ctrl Pts',(22.9701058542891,15.98027083986,87.18714704112));
#106699=CARTESIAN_POINT('Ctrl Pts',(24.3829496628191,14.93205005415,88.35697360021));
#106700=CARTESIAN_POINT('Ctrl Pts',(25.7455828440791,13.83506997747,89.33304121868));
#106701=CARTESIAN_POINT('Ctrl Pts',(27.0338235509591,12.71200151814,90.14134599812));
#106702=CARTESIAN_POINT('Ctrl Pts',(28.2606989614091,11.55431815225,90.82076231519));
#106703=CARTESIAN_POINT('Ctrl Pts',(29.4805515038791,10.30341122855,91.41513380966));
#106704=CARTESIAN_POINT('Ctrl Pts',(30.7073346580191,8.91606547149402,91.92891446662));
#106705=CARTESIAN_POINT('Ctrl Pts',(31.8785519228191,7.42186252822301,92.33283454608));
#106706=CARTESIAN_POINT('Ctrl Pts',(32.8858034194691,5.93611159812901,92.60136415471));
#106707=CARTESIAN_POINT('Ctrl Pts',(33.7077479385191,4.49637949617201,92.75525280737));
#106708=CARTESIAN_POINT('Ctrl Pts',(34.3594477230791,3.06936714330901,92.82352537927));
#106709=CARTESIAN_POINT('Ctrl Pts',(34.7987841186091,1.68933111557601,92.83289655037));
#106710=CARTESIAN_POINT('Ctrl Pts',(34.9379185776691,0.799874261541514,
92.83329103801));
#106711=CARTESIAN_POINT('Ctrl Pts',(34.9680789093591,0.377412282680914,
92.8379453280101));
#106712=CARTESIAN_POINT('Ctrl Pts',(21.0648245475691,14.80356751578,75.088574197736));
#106713=CARTESIAN_POINT('Ctrl Pts',(21.1562893009191,14.80542149402,75.624814594272));
#106714=CARTESIAN_POINT('Ctrl Pts',(21.4915191590391,14.74994267437,76.949273101324));
#106715=CARTESIAN_POINT('Ctrl Pts',(22.4029329257891,14.43645292234,78.850401178621));
#106716=CARTESIAN_POINT('Ctrl Pts',(23.6728411634791,13.89196197301,80.525093828825));
#106717=CARTESIAN_POINT('Ctrl Pts',(24.9938756020691,13.25961078348,81.813737319686));
#106718=CARTESIAN_POINT('Ctrl Pts',(26.2936708744891,12.5864534242,82.832583999374));
#106719=CARTESIAN_POINT('Ctrl Pts',(27.5870975206191,11.86798256843,83.68225710374));
#106720=CARTESIAN_POINT('Ctrl Pts',(28.8717832775691,11.10303997034,84.4077907698501));
#106721=CARTESIAN_POINT('Ctrl Pts',(30.1179515221891,10.306293006,85.0241310085501));
#106722=CARTESIAN_POINT('Ctrl Pts',(31.3323143284891,9.47069299188402,85.55730149859));
#106723=CARTESIAN_POINT('Ctrl Pts',(32.5667384548491,8.55128051724301,86.04034306038));
#106724=CARTESIAN_POINT('Ctrl Pts',(33.8387497469191,7.50960072681501,86.47900335892));
#106725=CARTESIAN_POINT('Ctrl Pts',(35.0880429676691,6.35762147075602,86.85127259704));
#106726=CARTESIAN_POINT('Ctrl Pts',(36.1977391360291,5.17506491544101,87.13119140558));
#106727=CARTESIAN_POINT('Ctrl Pts',(37.1355508905091,3.98655984369701,87.32815521361));
#106728=CARTESIAN_POINT('Ctrl Pts',(37.9083300473991,2.75824145710901,87.46012871543));
#106729=CARTESIAN_POINT('Ctrl Pts',(38.4524854874891,1.51002426311401,87.5351100622101));
#106730=CARTESIAN_POINT('Ctrl Pts',(38.6303209632591,0.670091817760814,
87.56162468684));
#106731=CARTESIAN_POINT('Ctrl Pts',(38.6686985395891,0.267767345835414,
87.57156379687));
#106732=CARTESIAN_POINT('Ctrl Pts',(27.4060955579191,15.00605745049,73.9992175459301));
#106733=CARTESIAN_POINT('Ctrl Pts',(27.4568706345291,15.00674148237,74.299882608077));
#106734=CARTESIAN_POINT('Ctrl Pts',(27.6563153791591,14.98607407549,75.03933020766));
#106735=CARTESIAN_POINT('Ctrl Pts',(28.2552178354491,14.86384274642,76.157719195735));
#106736=CARTESIAN_POINT('Ctrl Pts',(29.1953897033191,14.62223845856,77.28144993045));
#106737=CARTESIAN_POINT('Ctrl Pts',(30.2745666151391,14.3009152899,78.274673456111));
#106738=CARTESIAN_POINT('Ctrl Pts',(31.4158151207291,13.9175608677,79.163166612491));
#106739=CARTESIAN_POINT('Ctrl Pts',(32.6169037455491,13.46553722345,79.992694706598));
#106740=CARTESIAN_POINT('Ctrl Pts',(33.8649399941491,12.93919476597,80.780446952018));
#106741=CARTESIAN_POINT('Ctrl Pts',(35.1214740837291,12.3447503952,81.5213409775531));
#106742=CARTESIAN_POINT('Ctrl Pts',(36.3853570661891,11.67360909312,82.229199358404));
#106743=CARTESIAN_POINT('Ctrl Pts',(37.7082882345091,10.88094645291,82.940678146904));
#106744=CARTESIAN_POINT('Ctrl Pts',(39.1142274982291,9.91205347783502,83.67127064968));
#106745=CARTESIAN_POINT('Ctrl Pts',(40.5432158335391,8.74576233655301,84.3936442258099));
#106746=CARTESIAN_POINT('Ctrl Pts',(41.8604028480391,7.43460302127903,85.0471196915701));
#106747=CARTESIAN_POINT('Ctrl Pts',(43.0163443071791,5.99020112655302,85.6153164434601));
#106748=CARTESIAN_POINT('Ctrl Pts',(44.0066134889891,4.35311312370201,86.1022978834));
#106749=CARTESIAN_POINT('Ctrl Pts',(44.7332634147991,2.52355184883601,86.4665423458501));
#106750=CARTESIAN_POINT('Ctrl Pts',(44.9781481988991,1.19967484028401,86.60065479763));
#106751=CARTESIAN_POINT('Ctrl Pts',(45.0312601718991,0.557056200456914,
86.6358961446099));
#106752=CARTESIAN_POINT('',(33.0354774640918,10.5124754612176,86.002764223517));
#106753=CARTESIAN_POINT('Ctrl Pts',(33.0354780894153,10.5124757937565,86.0027640773287));
#106754=CARTESIAN_POINT('Ctrl Pts',(32.9691045419567,10.6496448112258,85.7569864680321));
#106755=CARTESIAN_POINT('Ctrl Pts',(32.902549203369,10.7855491860502,85.510603787654));
#106756=CARTESIAN_POINT('Ctrl Pts',(32.8358217036925,10.9202489626629,85.2636140420121));
#106757=CARTESIAN_POINT('Ctrl Pts',(32.7745997949839,11.0438348525407,85.0370030685314));
#106758=CARTESIAN_POINT('Ctrl Pts',(32.7132325472932,11.1664063529086,84.8098803739346));
#106759=CARTESIAN_POINT('Ctrl Pts',(32.6517508198401,11.2879736864104,84.582215596186));
#106760=CARTESIAN_POINT('Ctrl Pts',(32.5912567207905,11.40758819008,84.3582079733403));
#106761=CARTESIAN_POINT('Ctrl Pts',(32.5306515604465,11.5262302794122,84.1336755607773));
#106762=CARTESIAN_POINT('Ctrl Pts',(32.4699952977599,11.6438781598893,83.9086117339545));
#106763=CARTESIAN_POINT('Ctrl Pts',(33.0354771921691,10.5124760026091,86.0027648146029));
#106764=CARTESIAN_POINT('Ctrl Pts',(32.8495032264868,10.7349756256776,85.71341610164));
#106765=CARTESIAN_POINT('Ctrl Pts',(32.6612298048798,10.9502089020156,85.4190598393288));
#106766=CARTESIAN_POINT('Ctrl Pts',(32.2322622376353,11.4204983429167,84.7433742626294));
#106767=CARTESIAN_POINT('Ctrl Pts',(31.9898460045153,11.6720717461064,84.3579809310497));
#106768=CARTESIAN_POINT('Ctrl Pts',(31.7476174649718,11.9112061826963,83.967371408625));
#106769=CARTESIAN_POINT('Ctrl Pts',(34.9120188309791,1.82413434249001,99.4682297448801));
#106770=CARTESIAN_POINT('Ctrl Pts',(34.8888109995891,1.96245987573901,99.3366115926799));
#106771=CARTESIAN_POINT('Ctrl Pts',(34.8360618828891,2.26922408414201,99.0374564860999));
#106772=CARTESIAN_POINT('Ctrl Pts',(34.7492177463391,2.74567423970901,98.54493891335));
#106773=CARTESIAN_POINT('Ctrl Pts',(34.6484936587391,3.26480374793701,97.9737042265299));
#106774=CARTESIAN_POINT('Ctrl Pts',(34.5359614399391,3.81065575291701,97.3355022999601));
#106775=CARTESIAN_POINT('Ctrl Pts',(34.4101441832991,4.38332781361301,96.6219571797501));
#106776=CARTESIAN_POINT('Ctrl Pts',(34.2705880299791,4.97863539521901,95.8304949046499));
#106777=CARTESIAN_POINT('Ctrl Pts',(34.1165979297191,5.59573370623801,94.9571736486099));
#106778=CARTESIAN_POINT('Ctrl Pts',(33.9472609320191,6.23487974368301,93.99681581216));
#106779=CARTESIAN_POINT('Ctrl Pts',(33.7618129557691,6.89641662361901,92.9450880759699));
#106780=CARTESIAN_POINT('Ctrl Pts',(33.5583897547991,7.58563568723501,91.79141777467));
#106781=CARTESIAN_POINT('Ctrl Pts',(33.3359577127391,8.30505069308301,90.52994297838));
#106782=CARTESIAN_POINT('Ctrl Pts',(33.1018473233491,9.03167481851102,89.2022369832699));
#106783=CARTESIAN_POINT('Ctrl Pts',(32.8669035260691,9.73654502702002,87.86980449715));
#106784=CARTESIAN_POINT('Ctrl Pts',(32.6426145809191,10.39144635472,86.5977986801901));
#106785=CARTESIAN_POINT('Ctrl Pts',(32.4344532189191,10.98582291601,85.4172569323101));
#106786=CARTESIAN_POINT('Ctrl Pts',(32.2728252408591,11.4384757794,84.5006191187901));
#106787=CARTESIAN_POINT('Ctrl Pts',(32.1812853801191,11.6913539044,83.9814707708001));
#106788=CARTESIAN_POINT('Ctrl Pts',(32.1528289263991,11.76961293267,83.8200862021699));
#106789=CARTESIAN_POINT('Ctrl Pts',(35.8569731920691,1.77503969967301,99.2500041970801));
#106790=CARTESIAN_POINT('Ctrl Pts',(35.8338338435991,1.91295717426201,99.11877443079));
#106791=CARTESIAN_POINT('Ctrl Pts',(35.7812545230591,2.21873308346601,98.82058228613));
#106792=CARTESIAN_POINT('Ctrl Pts',(35.6946777064391,2.69371897512001,98.3295807600601));
#106793=CARTESIAN_POINT('Ctrl Pts',(35.5942347622291,3.21140170079501,97.75994051661));
#106794=CARTESIAN_POINT('Ctrl Pts',(35.4819850014691,3.75588538366201,97.1233404892));
#106795=CARTESIAN_POINT('Ctrl Pts',(35.3564735177891,4.32716670554801,96.41152949362));
#106796=CARTESIAN_POINT('Ctrl Pts',(35.2172185777891,4.92119264231101,95.62177548413));
#106797=CARTESIAN_POINT('Ctrl Pts',(35.0635160609991,5.53714074858301,94.7500851949999));
#106798=CARTESIAN_POINT('Ctrl Pts',(34.8944557496991,6.17524495260401,93.7912965251));
#106799=CARTESIAN_POINT('Ctrl Pts',(34.7092578581891,6.83589212217101,92.74098708999));
#106800=CARTESIAN_POINT('Ctrl Pts',(34.5060627443091,7.52434013691602,91.58861033481));
#106801=CARTESIAN_POINT('Ctrl Pts',(34.2838298479891,8.243112828341,90.32826495015));
#106802=CARTESIAN_POINT('Ctrl Pts',(34.0498859524991,8.96922127464301,89.00150318887));
#106803=CARTESIAN_POINT('Ctrl Pts',(33.8150764760691,9.67368911335601,87.6698324741));
#106804=CARTESIAN_POINT('Ctrl Pts',(33.5908950508691,10.32827676712,86.39843643309));
#106805=CARTESIAN_POINT('Ctrl Pts',(33.3828234160891,10.92239720819,85.21840355359));
#106806=CARTESIAN_POINT('Ctrl Pts',(33.2212636287591,11.37485908179,84.30215246888));
#106807=CARTESIAN_POINT('Ctrl Pts',(33.1297640948691,11.62762578662,83.78323282584));
#106808=CARTESIAN_POINT('Ctrl Pts',(33.1013204765891,11.7058495157,83.62192105062));
#106809=CARTESIAN_POINT('Ctrl Pts',(36.3377183773691,1.23722166550801,98.59992195691));
#106810=CARTESIAN_POINT('Ctrl Pts',(36.3153292400091,1.37066897199701,98.47294684921));
#106811=CARTESIAN_POINT('Ctrl Pts',(36.2646099888591,1.66561834083701,98.1853036822601));
#106812=CARTESIAN_POINT('Ctrl Pts',(36.1809615870791,2.12456363225101,97.710910022));
#106813=CARTESIAN_POINT('Ctrl Pts',(36.0835984897391,2.62639726107801,97.1587364582));
#106814=CARTESIAN_POINT('Ctrl Pts',(35.9744429775691,3.15589135920801,96.53968478651));
#106815=CARTESIAN_POINT('Ctrl Pts',(35.8522811508591,3.71193752772301,95.84687063963));
#106816=CARTESIAN_POINT('Ctrl Pts',(35.7163259182091,4.29192340492101,95.07583020039));
#106817=CARTESIAN_POINT('Ctrl Pts',(35.5657737976391,4.89527134097302,94.22200669614));
#106818=CARTESIAN_POINT('Ctrl Pts',(35.3997445082091,5.52196255221501,93.28040780544));
#106819=CARTESIAN_POINT('Ctrl Pts',(35.2172862249291,6.17286319437901,92.2456354606199));
#106820=CARTESIAN_POINT('Ctrl Pts',(35.0165897410091,6.85286458512201,91.10742914014));
#106821=CARTESIAN_POINT('Ctrl Pts',(34.7965384304091,7.56460090229802,89.85945614293));
#106822=CARTESIAN_POINT('Ctrl Pts',(34.5644184288691,8.28506022851301,88.54303819824));
#106823=CARTESIAN_POINT('Ctrl Pts',(34.3310803995691,8.98512021902701,87.21971247486));
#106824=CARTESIAN_POINT('Ctrl Pts',(34.1080768252691,9.63627166286102,85.9549963582099));
#106825=CARTESIAN_POINT('Ctrl Pts',(33.9009881270591,10.22758637869,84.78053798901));
#106826=CARTESIAN_POINT('Ctrl Pts',(33.7401753499791,10.67795601284,83.8685234099599));
#106827=CARTESIAN_POINT('Ctrl Pts',(33.6491175854391,10.92950214096,83.35210916544));
#106828=CARTESIAN_POINT('Ctrl Pts',(33.6208145758291,11.00733917725,83.1915948215801));
#106829=CARTESIAN_POINT('Ctrl Pts',(36.0275410752391,0.576180127216414,
97.95977740531));
#106830=CARTESIAN_POINT('Ctrl Pts',(36.0060740354391,0.704133072025914,
97.83803177278));
#106831=CARTESIAN_POINT('Ctrl Pts',(35.9576410280591,0.985775351029713,
97.56335453857));
#106832=CARTESIAN_POINT('Ctrl Pts',(35.8775919920991,1.42500486055401,97.1093738962301));
#106833=CARTESIAN_POINT('Ctrl Pts',(35.7840143883591,1.90735808765601,96.5786689334199));
#106834=CARTESIAN_POINT('Ctrl Pts',(35.6786620711491,2.41842822540601,95.9811862522101));
#106835=CARTESIAN_POINT('Ctrl Pts',(35.5606173663291,2.95574860084301,95.31172146382));
#106836=CARTESIAN_POINT('Ctrl Pts',(35.4287178615891,3.51847759563302,94.5636822006001));
#106837=CARTESIAN_POINT('Ctrl Pts',(35.2820379480591,4.10633844242001,93.73181907368));
#106838=CARTESIAN_POINT('Ctrl Pts',(35.1197341405291,4.71900174491701,92.8113484407899));
#106839=CARTESIAN_POINT('Ctrl Pts',(34.9406431575591,5.35792276003501,91.79567300499));
#106840=CARTESIAN_POINT('Ctrl Pts',(34.7430177833691,6.02754225770801,90.6748838132699));
#106841=CARTESIAN_POINT('Ctrl Pts',(34.5256478978791,6.73063004441001,89.44211793354));
#106842=CARTESIAN_POINT('Ctrl Pts',(34.2957696762391,7.44414593846902,88.1384137544699));
#106843=CARTESIAN_POINT('Ctrl Pts',(34.0642402283191,8.13878816578302,86.82534500575));
#106844=CARTESIAN_POINT('Ctrl Pts',(33.8426843711191,8.785716103976,85.5688393007899));
#106845=CARTESIAN_POINT('Ctrl Pts',(33.6368038174091,9.37358225391602,84.4012326595499));
#106846=CARTESIAN_POINT('Ctrl Pts',(33.4769092036691,9.82138028003303,83.49442524359));
#106847=CARTESIAN_POINT('Ctrl Pts',(33.3863944255791,10.07142617598,82.981090428146));
#106848=CARTESIAN_POINT('Ctrl Pts',(33.3582642405291,10.14878792142,82.821556221103));
#106849=CARTESIAN_POINT('Ctrl Pts',(33.0354776265489,10.5124749757193,86.0027637457613));
#106850=CARTESIAN_POINT('Ctrl Pts',(33.3173179037196,10.1752792325235,86.4412617191918));
#106851=CARTESIAN_POINT('Ctrl Pts',(33.5525634430571,9.85417994660021,86.750215496027));
#106852=CARTESIAN_POINT('Ctrl Pts',(33.772028026241,9.50836650597176,86.9414312064967));
#106853=CARTESIAN_POINT('Ctrl Pts',(33.8248976959827,9.42095261698334,86.9789367692075));
#106854=CARTESIAN_POINT('Ctrl Pts',(33.9013819844101,9.28133355483486,87.0015489199111));
#106855=CARTESIAN_POINT('Ctrl Pts',(33.9294254915404,9.22693873504601,87.0021052933605));
#106856=CARTESIAN_POINT('Ctrl Pts',(33.9721748577027,9.13459135675974,86.9784254921267));
#106857=CARTESIAN_POINT('Ctrl Pts',(33.9877318762359,9.09759012230128,86.9609410997307));
#106858=CARTESIAN_POINT('Ctrl Pts',(34.0126495147909,9.02972409352531,86.9096124910328));
#106859=CARTESIAN_POINT('Ctrl Pts',(34.0212542780569,9.00101992606884,86.8775770431024));
#106860=CARTESIAN_POINT('Ctrl Pts',(34.0348285005369,8.94246589968673,86.7903234150622));
#106861=CARTESIAN_POINT('Ctrl Pts',(34.0368443275895,8.91728874581814,86.7317483654917));
#106862=CARTESIAN_POINT('Ctrl Pts',(34.0324568799591,8.84706856689204,86.5120214361058));
#106863=CARTESIAN_POINT('Ctrl Pts',(34.0047398726329,8.83176059863746,86.313208346417));
#106864=CARTESIAN_POINT('Ctrl Pts',(33.9717701135441,8.83176086632613,86.1262282870275));
#106865=CARTESIAN_POINT('Origin',(31.9617040310391,11.38539957172,83.36473278179));
#106866=CARTESIAN_POINT('Ctrl Pts',(33.4389156605574,8.83176086632183,83.1042605152897));
#106867=CARTESIAN_POINT('Ctrl Pts',(33.4217631809711,8.83176086595217,83.0069839686339));
#106868=CARTESIAN_POINT('Ctrl Pts',(33.3959952397706,8.85207982387865,82.9165557092094));
#106869=CARTESIAN_POINT('Ctrl Pts',(33.3323712217024,8.92179561683953,82.7488570392455));
#106870=CARTESIAN_POINT('Ctrl Pts',(33.2944921671943,8.97119818785721,82.6715977317027));
#106871=CARTESIAN_POINT('Ctrl Pts',(33.1692793088435,9.14763475437354,82.4599992368818));
#106872=CARTESIAN_POINT('Ctrl Pts',(33.0701990377864,9.30262812111028,82.3460559650253));
#106873=CARTESIAN_POINT('Ctrl Pts',(32.8081714962699,9.71888469733861,82.1057109973505));
#106874=CARTESIAN_POINT('Ctrl Pts',(32.6191364880251,10.026640586823,82.0005135599871));
#106875=CARTESIAN_POINT('Ctrl Pts',(32.4210192740185,10.34163775061,81.9367868768039));
#106876=CARTESIAN_POINT('Origin',(11.833832765324,1.4210854715202E-14,67.1130006183894));
#106877=CARTESIAN_POINT('Origin',(31.9617040240391,-10.34163791147,83.36473278302));
#106878=CARTESIAN_POINT('',(31.9729369794551,-11.0982737000556,82.0695978531518));
#106879=CARTESIAN_POINT('',(32.4699922398292,-11.64390462692,83.9085557935526));
#106880=CARTESIAN_POINT('Origin',(31.9617042108291,-10.34163673913,83.36473275008));
#106881=CARTESIAN_POINT('',(33.4389248775025,-10.3415989969539,83.1043127923001));
#106882=CARTESIAN_POINT('Origin',(31.9617224686691,-10.34158709855,83.3648373468));
#106883=CARTESIAN_POINT('',(32.4210191725084,-10.3416379115649,81.9367868456364));
#106884=CARTESIAN_POINT('Origin',(31.9617040310391,-10.34163791149,83.36473278179));
#106885=CARTESIAN_POINT('Ctrl Pts',(31.9729367628468,-11.0982738819268,
82.069597333042));
#106886=CARTESIAN_POINT('Ctrl Pts',(32.0501425538371,-10.9583237686893,
81.9885061566232));
#106887=CARTESIAN_POINT('Ctrl Pts',(32.1430791794419,-10.7979907825697,
81.9374456442463));
#106888=CARTESIAN_POINT('Ctrl Pts',(32.2886438200371,-10.5550144197122,
81.9117786706722));
#106889=CARTESIAN_POINT('Ctrl Pts',(32.3549888593241,-10.446623041826,81.9155474419251));
#106890=CARTESIAN_POINT('Ctrl Pts',(32.4210191729779,-10.3416379122948,
81.9367868477846));
#106891=CARTESIAN_POINT('Ctrl Pts',(31.7735817980591,-10.02140058805,81.9026562156629));
#106892=CARTESIAN_POINT('Ctrl Pts',(31.7357761748391,-10.02952473272,81.910008510489));
#106893=CARTESIAN_POINT('Ctrl Pts',(31.1628542188291,-10.15405062092,82.0216114688509));
#106894=CARTESIAN_POINT('Ctrl Pts',(30.0808930105491,-10.42968733766,82.237676912063));
#106895=CARTESIAN_POINT('Ctrl Pts',(28.5280497869291,-10.93691556809,82.56013369893));
#106896=CARTESIAN_POINT('Ctrl Pts',(26.9921340261691,-11.56119523671,82.889318848888));
#106897=CARTESIAN_POINT('Ctrl Pts',(25.5251460669191,-12.29779125652,83.21142902479));
#106898=CARTESIAN_POINT('Ctrl Pts',(24.5918694655791,-12.86877044185,83.41980202981));
#106899=CARTESIAN_POINT('Ctrl Pts',(24.1635532058191,-13.15708445208,83.5158789747301));
#106900=CARTESIAN_POINT('Ctrl Pts',(32.1784416282891,-11.54621773089,81.5171042031791));
#106901=CARTESIAN_POINT('Ctrl Pts',(32.1419378425891,-11.55297077673,81.5204020721341));
#106902=CARTESIAN_POINT('Ctrl Pts',(31.5885791824291,-11.65648792141,81.57065409752));
#106903=CARTESIAN_POINT('Ctrl Pts',(30.5390466775791,-11.88582952014,81.673590761524));
#106904=CARTESIAN_POINT('Ctrl Pts',(29.0257581845491,-12.31002881764,81.8426957379871));
#106905=CARTESIAN_POINT('Ctrl Pts',(27.5251181140391,-12.83644124757,82.0304770381));
#106906=CARTESIAN_POINT('Ctrl Pts',(26.0900655677491,-13.46474790953,82.2287773907151));
#106907=CARTESIAN_POINT('Ctrl Pts',(25.1761650785191,-13.9579744701,82.365120608326));
#106908=CARTESIAN_POINT('Ctrl Pts',(24.7566393447891,-14.20870689459,82.429615994405));
#106909=CARTESIAN_POINT('Ctrl Pts',(32.6658315200591,-12.37295378417,82.827290215174));
#106910=CARTESIAN_POINT('Ctrl Pts',(32.6310822289791,-12.38244981272,82.828204304523));
#106911=CARTESIAN_POINT('Ctrl Pts',(32.1044073017791,-12.52731765498,82.842152237755));
#106912=CARTESIAN_POINT('Ctrl Pts',(31.1079834548191,-12.82839202105,82.87139447125));
#106913=CARTESIAN_POINT('Ctrl Pts',(29.6790572130991,-13.33539347479,82.923631504117));
#106914=CARTESIAN_POINT('Ctrl Pts',(28.2714383294591,-13.9202137689,82.987255072456));
#106915=CARTESIAN_POINT('Ctrl Pts',(26.9362729380191,-14.57705521407,83.0612022033301));
#106916=CARTESIAN_POINT('Ctrl Pts',(26.0932368319491,-15.06943775184,83.11603253511));
#106917=CARTESIAN_POINT('Ctrl Pts',(25.7078677337091,-15.3150566876,83.14290604076));
#106918=CARTESIAN_POINT('Ctrl Pts',(32.6130962564491,-11.44542862336,84.15941229294));
#106919=CARTESIAN_POINT('Ctrl Pts',(32.5783126975491,-11.4582774734,84.16265859895));
#106920=CARTESIAN_POINT('Ctrl Pts',(32.0513526705791,-11.65402869693,84.21172884833));
#106921=CARTESIAN_POINT('Ctrl Pts',(31.0608695313391,-12.05322295219,84.30085784711));
#106922=CARTESIAN_POINT('Ctrl Pts',(29.6533377532591,-12.70307541124,84.4220131092));
#106923=CARTESIAN_POINT('Ctrl Pts',(28.2776481946291,-13.42796087265,84.53734029307));
#106924=CARTESIAN_POINT('Ctrl Pts',(26.9827128612591,-14.21370720002,84.6452557772899));
#106925=CARTESIAN_POINT('Ctrl Pts',(26.1714980327591,-14.78323258141,84.71322528326));
#106926=CARTESIAN_POINT('Ctrl Pts',(25.8020155523191,-15.06273876079,84.74449966846));
#106927=CARTESIAN_POINT('',(31.7476734280839,-11.9111478604859,83.9674490301228));
#106928=CARTESIAN_POINT('Ctrl Pts',(31.747677586831,-11.9111403866478,83.9674418750385));
#106929=CARTESIAN_POINT('Ctrl Pts',(31.7122146011112,-11.9461515111606,
83.9102588915761));
#106930=CARTESIAN_POINT('Ctrl Pts',(31.6791349693868,-11.9766086818139,
83.8488354653028));
#106931=CARTESIAN_POINT('Ctrl Pts',(31.6204251122535,-12.0251166490527,
83.71758176436));
#106932=CARTESIAN_POINT('Ctrl Pts',(31.5951025357537,-12.0429110201326,
83.6484034469622));
#106933=CARTESIAN_POINT('Ctrl Pts',(31.5440974535816,-12.0682846266406,
83.4653474362906));
#106934=CARTESIAN_POINT('Ctrl Pts',(31.5267301910395,-12.0648516576147,
83.3523970290102));
#106935=CARTESIAN_POINT('Ctrl Pts',(31.5176271818919,-12.0172908463836,
83.1019371589877));
#106936=CARTESIAN_POINT('Ctrl Pts',(31.5320257410619,-11.9665665931259,
82.9719537520677));
#106937=CARTESIAN_POINT('Ctrl Pts',(31.5928693301599,-11.8157968166564,
82.6979996654286));
#106938=CARTESIAN_POINT('Ctrl Pts',(31.6472844110669,-11.7054576729801,
82.5598219677352));
#106939=CARTESIAN_POINT('Ctrl Pts',(31.7857998765308,-11.4390530565216,
82.2943601436417));
#106940=CARTESIAN_POINT('Ctrl Pts',(31.8772946926597,-11.271643725901,82.1700543601994));
#106941=CARTESIAN_POINT('Ctrl Pts',(31.9729371943684,-11.0982735071633,
82.0695983906671));
#106942=CARTESIAN_POINT('Ctrl Pts',(32.4699845397491,-11.64392959724,83.90850213227));
#106943=CARTESIAN_POINT('Ctrl Pts',(32.2291347908734,-11.7297341943093,
83.9281305264186));
#106944=CARTESIAN_POINT('Ctrl Pts',(31.9883508873569,-11.8187156032077,
83.9479776127812));
#106945=CARTESIAN_POINT('Ctrl Pts',(31.7476734278368,-11.9111478582041,
83.9674490379002));
#106946=CARTESIAN_POINT('Origin',(36.3793934194391,111.0724296188,99.78053857024));
#106947=CARTESIAN_POINT('',(33.9717729269383,-8.83176086632605,86.1262442425792));
#106948=CARTESIAN_POINT('Origin',(33.6121664459681,-9.4442782170463,84.0868145463581));
#106949=CARTESIAN_POINT('',(33.4389156594987,-8.83176086632605,83.1042605136998));
#106950=CARTESIAN_POINT('',(30.0527761960508,-8.83176086632605,63.9005093315515));
#106951=CARTESIAN_POINT('',(33.4389156626291,10.3416377002,83.10426051803));
#106952=CARTESIAN_POINT('Ctrl Pts',(32.1527935626691,-11.76968665633,83.8199367020899));
#106953=CARTESIAN_POINT('Ctrl Pts',(32.1877822675091,-11.67346394932,84.01836750773));
#106954=CARTESIAN_POINT('Ctrl Pts',(32.2841012636091,-11.40711317747,84.5646196792199));
#106955=CARTESIAN_POINT('Ctrl Pts',(32.4466951508991,-10.95100845184,85.48673543616));
#106956=CARTESIAN_POINT('Ctrl Pts',(32.6453419112291,-10.38330562976,86.61331719654));
#106957=CARTESIAN_POINT('Ctrl Pts',(32.8601514696091,-9.75625684908599,
87.83156273969));
#106958=CARTESIAN_POINT('Ctrl Pts',(33.0925703565391,-9.05996744084198,
89.1496757476299));
#106959=CARTESIAN_POINT('Ctrl Pts',(33.3361679293591,-8.30506871146998,
90.5311862337));
#106960=CARTESIAN_POINT('Ctrl Pts',(33.5787157856791,-7.51970410304498,
91.90674348165));
#106961=CARTESIAN_POINT('Ctrl Pts',(33.8058023593191,-6.74443968379098,
93.19461543817));
#106962=CARTESIAN_POINT('Ctrl Pts',(34.0112736614491,-5.99939457948999,
94.35990109842));
#106963=CARTESIAN_POINT('Ctrl Pts',(34.1938753301091,-5.29221424379899,
95.39548662213));
#106964=CARTESIAN_POINT('Ctrl Pts',(34.3549807040891,-4.62437962601499,
96.3091606005901));
#106965=CARTESIAN_POINT('Ctrl Pts',(34.4968257910291,-3.99387220682299,
97.11360406338));
#106966=CARTESIAN_POINT('Ctrl Pts',(34.6214195941091,-3.39980514907699,
97.8202106336001));
#106967=CARTESIAN_POINT('Ctrl Pts',(34.7311021597591,-2.84190083195199,
98.44225137414));
#106968=CARTESIAN_POINT('Ctrl Pts',(34.8268721630791,-2.32213954720699,
98.98539005283));
#106969=CARTESIAN_POINT('Ctrl Pts',(34.8855200472191,-1.98268592649499,
99.31799873191));
#106970=CARTESIAN_POINT('Ctrl Pts',(34.9121603553391,-1.82376272593199,
99.469083427));
#106971=CARTESIAN_POINT('Ctrl Pts',(33.1013825708891,-11.70592189092,83.62175380312));
#106972=CARTESIAN_POINT('Ctrl Pts',(33.1363554891591,-11.6097425978,83.82009507874));
#106973=CARTESIAN_POINT('Ctrl Pts',(33.2326322715791,-11.34350858072,84.36610784449));
#106974=CARTESIAN_POINT('Ctrl Pts',(33.3951576120491,-10.8875961498,85.28783485311));
#106975=CARTESIAN_POINT('Ctrl Pts',(33.5937184049891,-10.32013893385,86.4139290682));
#106976=CARTESIAN_POINT('Ctrl Pts',(33.8084250678791,-9.69339027966398,
87.63159106202));
#106977=CARTESIAN_POINT('Ctrl Pts',(34.0407123335591,-8.99749464293698,
88.94895760882));
#106978=CARTESIAN_POINT('Ctrl Pts',(34.2841385092591,-8.24312584709699,
90.32949605346));
#106979=CARTESIAN_POINT('Ctrl Pts',(34.5264675374691,-7.45846750889399,
91.70381226553));
#106980=CARTESIAN_POINT('Ctrl Pts',(34.7532919425091,-6.68409523848699,
92.99019739006));
#106981=CARTESIAN_POINT('Ctrl Pts',(34.9584686160591,-5.94011501678899,
94.15381212856));
#106982=CARTESIAN_POINT('Ctrl Pts',(35.1407525862991,-5.23416156772599,
95.18759589499));
#106983=CARTESIAN_POINT('Ctrl Pts',(35.3015331683191,-4.56766984296199,
96.09942788677));
#106984=CARTESIAN_POINT('Ctrl Pts',(35.4430462540291,-3.93863492368899,
96.90198847698));
#106985=CARTESIAN_POINT('Ctrl Pts',(35.5673227817091,-3.34607958808899,
97.60679568904));
#106986=CARTESIAN_POINT('Ctrl Pts',(35.6767165726691,-2.78964237687799,
98.22719870685));
#106987=CARTESIAN_POINT('Ctrl Pts',(35.7721962938191,-2.27145287258899,
98.76869111359));
#106988=CARTESIAN_POINT('Ctrl Pts',(35.8306532491991,-1.93310428852799,
99.10021698185));
#106989=CARTESIAN_POINT('Ctrl Pts',(35.8572087491291,-1.77468696691499,
99.2508207058));
#106990=CARTESIAN_POINT('Ctrl Pts',(33.6208806990891,-11.00730786661,83.19137758022));
#106991=CARTESIAN_POINT('Ctrl Pts',(33.6556806580191,-10.91160422097,83.38873795465));
#106992=CARTESIAN_POINT('Ctrl Pts',(33.7514949424591,-10.64664938247,83.93212776405));
#106993=CARTESIAN_POINT('Ctrl Pts',(33.9132692761891,-10.19284375433,84.8495956017999));
#106994=CARTESIAN_POINT('Ctrl Pts',(34.1108882006291,-9.62807742703399,
85.97034821521));
#106995=CARTESIAN_POINT('Ctrl Pts',(34.3244675288191,-9.00461699282098,
87.1816167761799));
#106996=CARTESIAN_POINT('Ctrl Pts',(34.5553127372291,-8.31303556163099,
88.49080500981));
#106997=CARTESIAN_POINT('Ctrl Pts',(34.7968610664691,-7.56447277785898,
89.86069365796));
#106998=CARTESIAN_POINT('Ctrl Pts',(35.0367925890191,-6.78755241657298,
91.22141293976));
#106999=CARTESIAN_POINT('Ctrl Pts',(35.2607446450891,-6.02295463041499,
92.49150816386));
#107000=CARTESIAN_POINT('Ctrl Pts',(35.4626933343091,-5.29064138366899,
93.63681609352));
#107001=CARTESIAN_POINT('Ctrl Pts',(35.6414965645091,-4.59812984409599,
94.6508596022301));
#107002=CARTESIAN_POINT('Ctrl Pts',(35.7987186889691,-3.94635100803099,
95.54251057833));
#107003=CARTESIAN_POINT('Ctrl Pts',(35.9365943313691,-3.33344896539199,
96.3244422024101));
#107004=CARTESIAN_POINT('Ctrl Pts',(36.0573947537591,-2.75745622962399,
97.00953544173));
#107005=CARTESIAN_POINT('Ctrl Pts',(36.1636246962091,-2.21709279770699,
97.61199538306));
#107006=CARTESIAN_POINT('Ctrl Pts',(36.2559240529591,-1.71612389891399,
98.13545104697));
#107007=CARTESIAN_POINT('Ctrl Pts',(36.3122891710791,-1.38988222212499,
98.45511351659));
#107008=CARTESIAN_POINT('Ctrl Pts',(36.3379155028391,-1.23700736783499,
98.60044766601));
#107009=CARTESIAN_POINT('Ctrl Pts',(33.3581861538791,-10.14869107751,82.821333853779));
#107010=CARTESIAN_POINT('Ctrl Pts',(33.3927735407891,-10.05357201637,83.01748867236));
#107011=CARTESIAN_POINT('Ctrl Pts',(33.4880194018791,-9.79018932523798,
83.55765479273));
#107012=CARTESIAN_POINT('Ctrl Pts',(33.6488707266591,-9.33897301848499,
84.4698879866199));
#107013=CARTESIAN_POINT('Ctrl Pts',(33.8453320675491,-8.77751387096399,
85.5840756174799));
#107014=CARTESIAN_POINT('Ctrl Pts',(34.0575258688491,-8.15809475395498,
86.78748646502));
#107015=CARTESIAN_POINT('Ctrl Pts',(34.2865987472891,-7.47181560582498,
88.0866233158599));
#107016=CARTESIAN_POINT('Ctrl Pts',(34.5258391490491,-6.73038857837198,
89.44342305689));
#107017=CARTESIAN_POINT('Ctrl Pts',(34.7628240679791,-5.96297841393798,
90.7874313191499));
#107018=CARTESIAN_POINT('Ctrl Pts',(34.9832459243291,-5.21039375089199,
92.03750578569));
#107019=CARTESIAN_POINT('Ctrl Pts',(35.1812273276891,-4.49241955292199,
93.16031411919));
#107020=CARTESIAN_POINT('Ctrl Pts',(35.3557526279591,-3.81642850787699,
94.15009628172));
#107021=CARTESIAN_POINT('Ctrl Pts',(35.5086013054291,-3.18273223645299,
95.01694420737));
#107022=CARTESIAN_POINT('Ctrl Pts',(35.6420064250591,-2.58965796458799,
95.77352223697));
#107023=CARTESIAN_POINT('Ctrl Pts',(35.7585346137691,-2.03402114180199,
96.4343864351));
#107024=CARTESIAN_POINT('Ctrl Pts',(35.8608760951491,-1.51341284832599,
97.01479381783));
#107025=CARTESIAN_POINT('Ctrl Pts',(35.9492666922991,-1.03360857045599,
97.51608180449));
#107026=CARTESIAN_POINT('Ctrl Pts',(36.0030608820791,-0.722246631958186,
97.82116381497));
#107027=CARTESIAN_POINT('Ctrl Pts',(36.0275452393591,-0.576183629892886,
97.9600215052599));
#107028=CARTESIAN_POINT('',(33.0354798288136,-10.5124724840881,86.0027674120725));
#107029=CARTESIAN_POINT('Ctrl Pts',(33.9717729269291,-8.83176086634574,
86.1262442425808));
#107030=CARTESIAN_POINT('Ctrl Pts',(34.00452240054,-8.83176153466786,86.3119775742192));
#107031=CARTESIAN_POINT('Ctrl Pts',(34.0320451313447,-8.84686882170987,
86.5091543621162));
#107032=CARTESIAN_POINT('Ctrl Pts',(34.0369090716926,-8.91605932710747,
86.7286962704357));
#107033=CARTESIAN_POINT('Ctrl Pts',(34.0350299303198,-8.94118685479987,
86.7878948736568));
#107034=CARTESIAN_POINT('Ctrl Pts',(34.0216294684122,-8.99967893519797,
86.8759322099713));
#107035=CARTESIAN_POINT('Ctrl Pts',(34.0131139926901,-9.02830243620887,
86.9082308063866));
#107036=CARTESIAN_POINT('Ctrl Pts',(33.9883890414468,-9.09594990342112,
86.959993287345));
#107037=CARTESIAN_POINT('Ctrl Pts',(33.9729527871185,-9.13279899518379,
86.9777020439548));
#107038=CARTESIAN_POINT('Ctrl Pts',(33.9305535618018,-9.22464467891043,
87.0018535956066));
#107039=CARTESIAN_POINT('Ctrl Pts',(33.9027796998228,-9.27865799813915,
87.0016595140628));
#107040=CARTESIAN_POINT('Ctrl Pts',(33.826939384157,-9.41742371476679,86.9800230277075));
#107041=CARTESIAN_POINT('Ctrl Pts',(33.7745078388006,-9.50429852151224,
86.9432471052056));
#107042=CARTESIAN_POINT('Ctrl Pts',(33.5552084117402,-9.85055375321946,
86.753681284039));
#107043=CARTESIAN_POINT('Ctrl Pts',(33.3189371657181,-10.1733419857233,
86.4437816445647));
#107044=CARTESIAN_POINT('Ctrl Pts',(33.0354799802535,-10.5124720315184,
86.0027669667207));
#107045=CARTESIAN_POINT('Ctrl Pts',(32.4699982866135,-11.6439041840734,
83.9085524108676));
#107046=CARTESIAN_POINT('Ctrl Pts',(32.5078283245398,-11.5705218613496,
84.0489368478963));
#107047=CARTESIAN_POINT('Ctrl Pts',(32.5456303929192,-11.4967563984524,
84.189108156906));
#107048=CARTESIAN_POINT('Ctrl Pts',(32.5833984613449,-11.4226113402587,
84.3290758031173));
#107049=CARTESIAN_POINT('Ctrl Pts',(32.6746058513949,-11.2435559232135,
84.6670884215676));
#107050=CARTESIAN_POINT('Ctrl Pts',(32.7656155737303,-11.0622855248061,
85.0039134635798));
#107051=CARTESIAN_POINT('Ctrl Pts',(32.8563236438861,-10.8787683159464,
85.3396126365442));
#107052=CARTESIAN_POINT('Ctrl Pts',(32.916185525905,-10.7576579727725,85.56115394209));
#107053=CARTESIAN_POINT('Ctrl Pts',(32.9759158306451,-10.6355694329657,
85.7822048579121));
#107054=CARTESIAN_POINT('Ctrl Pts',(33.0354799802617,-10.5124720315087,
86.0027669667333));
#107055=CARTESIAN_POINT('Ctrl Pts',(36.2511910984291,-0.816951121684487,
99.13095237507));
#107056=CARTESIAN_POINT('Ctrl Pts',(36.2200982088991,-1.45683196280799,
99.1098451401801));
#107057=CARTESIAN_POINT('Ctrl Pts',(36.0778630790891,-2.85039942836099,
99.0419676728901));
#107058=CARTESIAN_POINT('Ctrl Pts',(35.6275483510391,-4.94247000735899,
98.84599903898));
#107059=CARTESIAN_POINT('Ctrl Pts',(34.9397597871691,-7.05113172994599,
98.51977184372));
#107060=CARTESIAN_POINT('Ctrl Pts',(34.0734741662491,-9.09163743804897,
98.0649602571899));
#107061=CARTESIAN_POINT('Ctrl Pts',(33.0099168483791,-11.12983443612,97.44906592845));
#107062=CARTESIAN_POINT('Ctrl Pts',(31.7699785170891,-13.12298748389,96.6589115129399));
#107063=CARTESIAN_POINT('Ctrl Pts',(30.4746258290591,-14.92251334854,95.75721789378));
#107064=CARTESIAN_POINT('Ctrl Pts',(29.1968815731991,-16.50069944243,94.7947864407199));
#107065=CARTESIAN_POINT('Ctrl Pts',(27.9225293421991,-17.92619343051,93.76208048801));
#107066=CARTESIAN_POINT('Ctrl Pts',(26.5896727465691,-19.28349187111,92.5956876894801));
#107067=CARTESIAN_POINT('Ctrl Pts',(25.1814694175691,-20.58838494568,91.25117303266));
#107068=CARTESIAN_POINT('Ctrl Pts',(23.7249591534991,-21.81419974781,89.71266771848));
#107069=CARTESIAN_POINT('Ctrl Pts',(22.2142909846591,-22.9637208008,87.91364117654));
#107070=CARTESIAN_POINT('Ctrl Pts',(20.6065395382091,-24.05476593901,85.68623624305));
#107071=CARTESIAN_POINT('Ctrl Pts',(18.9416778012191,-25.02348229969,82.825890425796));
#107072=CARTESIAN_POINT('Ctrl Pts',(17.5339994345191,-25.65356630387,79.417420667109));
#107073=CARTESIAN_POINT('Ctrl Pts',(16.9242179391691,-25.78353110717,76.926255793732));
#107074=CARTESIAN_POINT('Ctrl Pts',(16.7312453442491,-25.77964745785,75.805602355198));
#107075=CARTESIAN_POINT('Ctrl Pts',(34.9680768531591,-0.377262712455286,
92.83793248162));
#107076=CARTESIAN_POINT('Ctrl Pts',(34.9401900659091,-0.768818210978587,
92.83356221903));
#107077=CARTESIAN_POINT('Ctrl Pts',(34.8109275223991,-1.62812620872499,
92.8325719567701));
#107078=CARTESIAN_POINT('Ctrl Pts',(34.3972755661991,-2.97122279462399,
92.8255990532501));
#107079=CARTESIAN_POINT('Ctrl Pts',(33.7599966114291,-4.39375486831299,
92.76261787049));
#107080=CARTESIAN_POINT('Ctrl Pts',(32.9521573659891,-5.82931930270299,
92.61621541888));
#107081=CARTESIAN_POINT('Ctrl Pts',(31.9551618598791,-7.31697565127499,
92.35621163472));
#107082=CARTESIAN_POINT('Ctrl Pts',(30.7878189799691,-8.81951599642399,
91.9596113594201));
#107083=CARTESIAN_POINT('Ctrl Pts',(29.5643467643691,-10.21287137887,91.45281600972));
#107084=CARTESIAN_POINT('Ctrl Pts',(28.3547145027491,-11.46125770319,90.86912642514));
#107085=CARTESIAN_POINT('Ctrl Pts',(27.1462246720591,-12.60932492795,90.2068010813201));
#107086=CARTESIAN_POINT('Ctrl Pts',(25.8804633212691,-13.72121825748,89.42218714027));
#107087=CARTESIAN_POINT('Ctrl Pts',(24.5415426038291,-14.80846467629,88.4770655865801));
#107088=CARTESIAN_POINT('Ctrl Pts',(23.1553900553591,-15.84725088264,87.34998754959));
#107089=CARTESIAN_POINT('Ctrl Pts',(21.7169286490991,-16.83785256507,85.9795861337301));
#107090=CARTESIAN_POINT('Ctrl Pts',(20.1864646779891,-17.79411649535,84.2176273015201));
#107091=CARTESIAN_POINT('Ctrl Pts',(18.6056376920291,-18.65837811088,81.868380902977));
#107092=CARTESIAN_POINT('Ctrl Pts',(17.2833457609491,-19.22934869733,78.9739891356611));
#107093=CARTESIAN_POINT('Ctrl Pts',(16.7318898964791,-19.34793907064,76.820460370021));
#107094=CARTESIAN_POINT('Ctrl Pts',(16.5654152065891,-19.34439445674,75.849914932886));
#107095=CARTESIAN_POINT('Ctrl Pts',(38.6686947048191,-0.267618408180286,
87.57152762521));
#107096=CARTESIAN_POINT('Ctrl Pts',(38.6331457099391,-0.640502714598286,
87.56228047755));
#107097=CARTESIAN_POINT('Ctrl Pts',(38.4681697649291,-1.45257130791499,
87.5371031361401));
#107098=CARTESIAN_POINT('Ctrl Pts',(37.9543196144491,-2.67152049410099,
87.46697907679));
#107099=CARTESIAN_POINT('Ctrl Pts',(37.1964789572891,-3.89993484531899,
87.33954011223));
#107100=CARTESIAN_POINT('Ctrl Pts',(36.2722354399091,-5.08847143352099,
87.1482156939501));
#107101=CARTESIAN_POINT('Ctrl Pts',(35.1711071623791,-6.27550574943099,
86.8740206795701));
#107102=CARTESIAN_POINT('Ctrl Pts',(33.9234036585391,-7.436166673543,86.50611895787));
#107103=CARTESIAN_POINT('Ctrl Pts',(32.6526782149891,-8.48396598041999,
86.07171874038));
#107104=CARTESIAN_POINT('Ctrl Pts',(31.4266015655591,-9.40280963542199,
85.5959755830301));
#107105=CARTESIAN_POINT('Ctrl Pts',(30.2282183070691,-10.23269364386,85.07485106796));
#107106=CARTESIAN_POINT('Ctrl Pts',(29.0009821455491,-11.02282107056,84.4750277186701));
#107107=CARTESIAN_POINT('Ctrl Pts',(27.7349646372491,-11.7823880216,83.77066674245));
#107108=CARTESIAN_POINT('Ctrl Pts',(26.4611997445191,-12.49587308951,82.949856613029));
#107109=CARTESIAN_POINT('Ctrl Pts',(25.1820693516891,-13.16490311603,81.9728674396441));
#107110=CARTESIAN_POINT('Ctrl Pts',(23.8728795301391,-13.79985263807,80.741966022882));
#107111=CARTESIAN_POINT('Ctrl Pts',(22.5850112147791,-14.36356654138,79.133191069062));
#107112=CARTESIAN_POINT('Ctrl Pts',(21.5697113092491,-14.73019815096,77.183930116823));
#107113=CARTESIAN_POINT('Ctrl Pts',(21.1758003549191,-14.80581932552,75.7409655371681));
#107114=CARTESIAN_POINT('Ctrl Pts',(21.0646250899491,-14.8035595922,75.088550558094));
#107115=CARTESIAN_POINT('Ctrl Pts',(45.0312706731691,-0.556809233210386,
86.63588923546));
#107116=CARTESIAN_POINT('Ctrl Pts',(44.9819984429591,-1.15239083593299,
86.6032111113799));
#107117=CARTESIAN_POINT('Ctrl Pts',(44.7550297579291,-2.43387817146999,
86.47794742155));
#107118=CARTESIAN_POINT('Ctrl Pts',(44.0669849657891,-4.23139684260399,
86.1321464635101));
#107119=CARTESIAN_POINT('Ctrl Pts',(43.0931519133991,-5.87949518942999,
85.65298684557));
#107120=CARTESIAN_POINT('Ctrl Pts',(41.9506857162891,-7.33390305288999,
85.0915934778799));
#107121=CARTESIAN_POINT('Ctrl Pts',(40.6400631633491,-8.65884473130499,
84.44202906066));
#107122=CARTESIAN_POINT('Ctrl Pts',(39.2094613534091,-9.84085525044999,
83.71996478425));
#107123=CARTESIAN_POINT('Ctrl Pts',(37.8019957376891,-10.82051536224,82.99003573172));
#107124=CARTESIAN_POINT('Ctrl Pts',(36.4852355554891,-11.6168290835,82.283717786993));
#107125=CARTESIAN_POINT('Ctrl Pts',(35.2348621603691,-12.28740211764,81.586024678646));
#107126=CARTESIAN_POINT('Ctrl Pts',(33.9934103628291,-12.88127932846,80.858065721516));
#107127=CARTESIAN_POINT('Ctrl Pts',(32.7581770629291,-13.40872065919,80.08477919832));
#107128=CARTESIAN_POINT('Ctrl Pts',(31.5683175582891,-13.86272653758,79.272924596943));
#107129=CARTESIAN_POINT('Ctrl Pts',(30.4356778789491,-14.24928723071,78.407307267481));
#107130=CARTESIAN_POINT('Ctrl Pts',(29.3529211006491,-14.57798235441,77.439888248051));
#107131=CARTESIAN_POINT('Ctrl Pts',(28.3831326036191,-14.83361972799,76.336383711929));
#107132=CARTESIAN_POINT('Ctrl Pts',(27.7038229907891,-14.97888942575,75.170329705841));
#107133=CARTESIAN_POINT('Ctrl Pts',(27.4678322792991,-15.00690558171,74.365048202755));
#107134=CARTESIAN_POINT('Ctrl Pts',(27.4060630052191,-15.00607043787,73.999190543978));
#107135=CARTESIAN_POINT('Ctrl Pts',(31.7476692742198,-11.9111553334129,
83.9674561810205));
#107136=CARTESIAN_POINT('Ctrl Pts',(31.9900350122681,-11.6718844892141,
84.3582893314217));
#107137=CARTESIAN_POINT('Ctrl Pts',(32.2325023891363,-11.420244524838,84.7437537826362));
#107138=CARTESIAN_POINT('Ctrl Pts',(32.6614487604326,-10.9499616738916,
85.4194048480172));
#107139=CARTESIAN_POINT('Ctrl Pts',(32.8496143409744,-10.7348422493249,
85.7135871729915));
#107140=CARTESIAN_POINT('Ctrl Pts',(33.0354795753356,-10.5124729887581,
86.002767963063));
#107141=CARTESIAN_POINT('Origin',(31.9617040310391,11.38539957172,83.36473278179));
#107142=CARTESIAN_POINT('Ctrl Pts',(32.4210191728332,-10.34163791149,81.9367868442564));
#107143=CARTESIAN_POINT('Ctrl Pts',(32.5625988328022,-10.1165328327363,
81.9823275610893));
#107144=CARTESIAN_POINT('Ctrl Pts',(32.69839419895,-9.89738949147113,82.049406907544));
#107145=CARTESIAN_POINT('Ctrl Pts',(32.9735010138201,-9.45516064419882,
82.2420387731289));
#107146=CARTESIAN_POINT('Ctrl Pts',(33.1455699418812,-9.17784383559699,
82.409453065027));
#107147=CARTESIAN_POINT('Ctrl Pts',(33.304585399266,-8.95817382749374,82.6925802044263));
#107148=CARTESIAN_POINT('Ctrl Pts',(33.3403472037622,-8.91216026273485,
82.7673290310841));
#107149=CARTESIAN_POINT('Ctrl Pts',(33.400100434177,-8.84867606677267,82.9304931696846));
#107150=CARTESIAN_POINT('Ctrl Pts',(33.423915194776,-8.8317608663218,83.0191886464178));
#107151=CARTESIAN_POINT('Ctrl Pts',(33.4389156605574,-8.8317608663218,83.1042605152897));
#107152=CARTESIAN_POINT('Origin',(11.833832765324,1.4210854715202E-14,67.1130006183894));
#107153=CARTESIAN_POINT('Origin',(11.833832765324,1.4210854715202E-14,67.1130006183894));
#107154=CARTESIAN_POINT('',(-4.35610816560352,-4.33090945180056,90.6854703082044));
#107155=CARTESIAN_POINT('',(5.52231334906584,-17.4578705567949,93.2013353119523));
#107156=CARTESIAN_POINT('Ctrl Pts',(-4.35611010952668,-4.33091289415503,
90.685455311287));
#107157=CARTESIAN_POINT('Ctrl Pts',(-3.98956300814287,-5.77320552148352,
90.9690031198165));
#107158=CARTESIAN_POINT('Ctrl Pts',(-3.45353720107494,-7.14208397764978,
91.3707045991231));
#107159=CARTESIAN_POINT('Ctrl Pts',(-2.19019201912765,-9.58743742151509,
92.1835171115637));
#107160=CARTESIAN_POINT('Ctrl Pts',(-1.47920675948711,-10.6934433015076,
92.5940797795233));
#107161=CARTESIAN_POINT('Ctrl Pts',(0.341152214773563,-13.0620281433899,
93.4022734954383));
#107162=CARTESIAN_POINT('Ctrl Pts',(1.44307216932659,-14.2005867443726,
93.732227499844));
#107163=CARTESIAN_POINT('Ctrl Pts',(3.05159459760781,-15.6229944483531,
93.8400521806102));
#107164=CARTESIAN_POINT('Ctrl Pts',(3.58482881504141,-16.0578814173498,
93.8206256404535));
#107165=CARTESIAN_POINT('Ctrl Pts',(4.76564826470288,-16.9510727199715,
93.5866875535521));
#107166=CARTESIAN_POINT('Ctrl Pts',(5.22912462942103,-17.2624413963519,
93.3669714685417));
#107167=CARTESIAN_POINT('Ctrl Pts',(5.52227383940231,-17.4578559214869,
93.2012481656177));
#107168=CARTESIAN_POINT('',(-3.38209691493766,-8.56599685566968,88.073658572396));
#107169=CARTESIAN_POINT('Ctrl Pts',(-4.35610633752318,-4.33090605764581,
90.6854852128844));
#107170=CARTESIAN_POINT('Ctrl Pts',(-4.54154600199715,-3.60121467706104,
90.5420613441333));
#107171=CARTESIAN_POINT('Ctrl Pts',(-4.66228844482028,-2.97979138225131,
90.3835003204796));
#107172=CARTESIAN_POINT('Ctrl Pts',(-4.76846785957156,-2.41966836721192,
90.1896898800142));
#107173=CARTESIAN_POINT('Ctrl Pts',(-4.79766454744446,-2.26180047015079,
90.1269979540808));
#107174=CARTESIAN_POINT('Ctrl Pts',(-4.83130822577944,-2.10288053743367,
90.0326105277975));
#107175=CARTESIAN_POINT('Ctrl Pts',(-4.84077737827289,-2.06137827664836,
90.0031576448214));
#107176=CARTESIAN_POINT('Ctrl Pts',(-4.85403047519485,-2.01453819592731,
89.9548442851971));
#107177=CARTESIAN_POINT('Ctrl Pts',(-4.85878442471103,-1.99986733184758,
89.9361737747806));
#107178=CARTESIAN_POINT('Ctrl Pts',(-4.86661900096031,-1.98284914892481,
89.9012996077116));
#107179=CARTESIAN_POINT('Ctrl Pts',(-4.86975107961287,-1.97815774911654,
89.8861523758613));
#107180=CARTESIAN_POINT('Ctrl Pts',(-4.87567409040339,-1.97529418204614,
89.8541588802312));
#107181=CARTESIAN_POINT('Ctrl Pts',(-4.87825684110292,-1.97726621084453,
89.8384146145568));
#107182=CARTESIAN_POINT('Ctrl Pts',(-4.88353893083735,-1.98889666576724,
89.8019517129379));
#107183=CARTESIAN_POINT('Ctrl Pts',(-4.88578599526452,-2.00071050952999,
89.7825769301279));
#107184=CARTESIAN_POINT('Ctrl Pts',(-4.89060144205847,-2.04027600096942,
89.7327681179324));
#107185=CARTESIAN_POINT('Ctrl Pts',(-4.89256783986115,-2.07947111499586,
89.6991459647543));
#107186=CARTESIAN_POINT('Ctrl Pts',(-4.89580440699033,-2.4346495038435,
89.4667340267194));
#107187=CARTESIAN_POINT('Ctrl Pts',(-4.85124311607859,-3.16900005450152,
89.2318596900765));
#107188=CARTESIAN_POINT('Ctrl Pts',(-4.48170045661541,-5.56983424992605,
88.5574293003622));
#107189=CARTESIAN_POINT('Ctrl Pts',(-4.00535207593041,-7.18998713465117,
88.1835494250047));
#107190=CARTESIAN_POINT('Ctrl Pts',(-3.38209691507343,-8.56599685566973,
88.0736585716266));
#107191=CARTESIAN_POINT('',(3.67711001798258,-16.9999999999988,86.8289313159581));
#107192=CARTESIAN_POINT('Origin',(14.9594999633274,1.4210854715202E-14,
84.8395401726047));
#107193=CARTESIAN_POINT('',(6.52236793072597,-18.4999999837107,87.8502704807592));
#107194=CARTESIAN_POINT('Ctrl Pts',(3.67710978043326,-17.,86.8289299687314));
#107195=CARTESIAN_POINT('Ctrl Pts',(3.99139559239029,-17.2150671358623,
86.7735129004292));
#107196=CARTESIAN_POINT('Ctrl Pts',(4.34754070270756,-17.4389532379846,
86.7591293140106));
#107197=CARTESIAN_POINT('Ctrl Pts',(5.06665893878612,-17.8504223940439,
86.8312090840392));
#107198=CARTESIAN_POINT('Ctrl Pts',(5.42965862838439,-18.0384248294259,
86.9149877608384));
#107199=CARTESIAN_POINT('Ctrl Pts',(5.91789315169195,-18.2685458496827,
87.1337400811896));
#107200=CARTESIAN_POINT('Ctrl Pts',(6.09300490374504,-18.346334827275,87.2342769515633));
#107201=CARTESIAN_POINT('Ctrl Pts',(6.30672210579366,-18.432901727933,87.4302697426805));
#107202=CARTESIAN_POINT('Ctrl Pts',(6.36972845372232,-18.4567893765268,
87.503098430441));
#107203=CARTESIAN_POINT('Ctrl Pts',(6.46896467655097,-18.490320459441,87.6644868989771));
#107204=CARTESIAN_POINT('Ctrl Pts',(6.50520812449229,-18.4999932787823,
87.7530334383063));
#107205=CARTESIAN_POINT('Ctrl Pts',(6.52236792752664,-18.4999999965284,
87.8502704813229));
#107206=CARTESIAN_POINT('',(7.18082331871055,-18.4999999999755,91.584556528483));
#107207=CARTESIAN_POINT('',(3.13624619141446,-18.5,68.6466197984171));
#107208=CARTESIAN_POINT('',(6.72291618991372,-18.2006285964414,92.4517527605434));
#107209=CARTESIAN_POINT('Ctrl Pts',(7.18082331870226,-18.4999999999971,
91.5845565284845));
#107210=CARTESIAN_POINT('Ctrl Pts',(7.18850613867666,-18.5000000709139,
91.6281271102621));
#107211=CARTESIAN_POINT('Ctrl Pts',(7.1923228389523,-18.4981595928469,91.6719941835109));
#107212=CARTESIAN_POINT('Ctrl Pts',(7.19155915231309,-18.4904703123138,
91.7602655374697));
#107213=CARTESIAN_POINT('Ctrl Pts',(7.18696014363605,-18.4846829765142,
91.8038203409861));
#107214=CARTESIAN_POINT('Ctrl Pts',(7.15984955096027,-18.4606687798121,
91.9378269873827));
#107215=CARTESIAN_POINT('Ctrl Pts',(7.12379243649138,-18.4364837977388,
92.0217596633147));
#107216=CARTESIAN_POINT('Ctrl Pts',(7.03345361994085,-18.3804809940909,
92.1672910669025));
#107217=CARTESIAN_POINT('Ctrl Pts',(6.981424799771,-18.3497232834015,92.2298483634182));
#107218=CARTESIAN_POINT('Ctrl Pts',(6.86282535622547,-18.2807333702774,
92.3477958645267));
#107219=CARTESIAN_POINT('Ctrl Pts',(6.79392622567087,-18.241259822421,92.403017754057));
#107220=CARTESIAN_POINT('Ctrl Pts',(6.72291494162312,-18.200628154702,92.4517505732837));
#107221=CARTESIAN_POINT('Ctrl Pts',(5.52235284477145,-17.4578851823617,
93.2014224682222));
#107222=CARTESIAN_POINT('Ctrl Pts',(5.72370338494148,-17.5920989308729,
93.0876563122291));
#107223=CARTESIAN_POINT('Ctrl Pts',(5.92504705677759,-17.7212905264079,
92.9681277382207));
#107224=CARTESIAN_POINT('Ctrl Pts',(6.32572080308318,-17.9689211252111,
92.7180495304402));
#107225=CARTESIAN_POINT('Ctrl Pts',(6.52475300915694,-18.0872399127614,
92.5877736764462));
#107226=CARTESIAN_POINT('Ctrl Pts',(6.72291744207803,-18.2006290368992,
92.4517549519884));
#107227=CARTESIAN_POINT('Ctrl Pts',(-3.02748297213691,-16.72098536733,90.87050995462));
#107228=CARTESIAN_POINT('Ctrl Pts',(-2.76741589283891,-16.72098536733,90.9223387409));
#107229=CARTESIAN_POINT('Ctrl Pts',(-2.20315940912091,-16.72098536733,91.04438774742));
#107230=CARTESIAN_POINT('Ctrl Pts',(-1.36204058715091,-16.72098536733,91.25306306065));
#107231=CARTESIAN_POINT('Ctrl Pts',(-0.530947724290913,-16.72098536733,
91.4804220205299));
#107232=CARTESIAN_POINT('Ctrl Pts',(0.220249863419087,-16.72098536733,91.6980000211799));
#107233=CARTESIAN_POINT('Ctrl Pts',(0.895988512819086,-16.72098536733,91.8987274439699));
#107234=CARTESIAN_POINT('Ctrl Pts',(1.50513857083909,-16.72098536733,92.0797274483699));
#107235=CARTESIAN_POINT('Ctrl Pts',(2.05850149532909,-16.72098536733,92.24052148621));
#107236=CARTESIAN_POINT('Ctrl Pts',(2.56464571939909,-16.72098536733,92.38151018466));
#107237=CARTESIAN_POINT('Ctrl Pts',(3.03062126430909,-16.72098536733,92.50329230408));
#107238=CARTESIAN_POINT('Ctrl Pts',(3.46055536031908,-16.72098536733,92.6062344343699));
#107239=CARTESIAN_POINT('Ctrl Pts',(3.85857840518909,-16.72098536733,92.69139482375));
#107240=CARTESIAN_POINT('Ctrl Pts',(4.22948852246909,-16.72098536733,92.76008351918));
#107241=CARTESIAN_POINT('Ctrl Pts',(4.57751175258909,-16.72098536733,92.81335828303));
#107242=CARTESIAN_POINT('Ctrl Pts',(4.82900967236909,-16.72098536733,92.84336104984));
#107243=CARTESIAN_POINT('Ctrl Pts',(4.96464306063909,-16.72098536733,92.8564918230699));
#107244=CARTESIAN_POINT('Ctrl Pts',(4.99018242526908,-16.72098536733,92.8588546212399));
#107245=CARTESIAN_POINT('Ctrl Pts',(-3.07030643866891,-17.87841055123,91.0854009342301));
#107246=CARTESIAN_POINT('Ctrl Pts',(-2.81258371044191,-17.87841055123,91.1367624857301));
#107247=CARTESIAN_POINT('Ctrl Pts',(-2.25302994109091,-17.87841055123,91.2577878440801));
#107248=CARTESIAN_POINT('Ctrl Pts',(-1.41756024129091,-17.87841055123,91.4650501435));
#107249=CARTESIAN_POINT('Ctrl Pts',(-0.590567647620912,-17.87841055123,
91.6912794621601));
#107250=CARTESIAN_POINT('Ctrl Pts',(0.158357462979087,-17.87841055123,91.90819507323));
#107251=CARTESIAN_POINT('Ctrl Pts',(0.833361273419087,-17.87841055123,92.10870296934));
#107252=CARTESIAN_POINT('Ctrl Pts',(1.44313497812909,-17.87841055123,92.28988942047));
#107253=CARTESIAN_POINT('Ctrl Pts',(1.99830874984909,-17.87841055123,92.4512124919601));
#107254=CARTESIAN_POINT('Ctrl Pts',(2.50728843127908,-17.87841055123,92.59299586447));
#107255=CARTESIAN_POINT('Ctrl Pts',(2.97716951007909,-17.87841055123,92.71580500278));
#107256=CARTESIAN_POINT('Ctrl Pts',(3.41188248195909,-17.87841055123,92.81989834208));
#107257=CARTESIAN_POINT('Ctrl Pts',(3.81545655558909,-17.87841055123,92.90625460732));
#107258=CARTESIAN_POINT('Ctrl Pts',(4.19272113607909,-17.87841055123,92.97612920327));
#107259=CARTESIAN_POINT('Ctrl Pts',(4.54778442056909,-17.87841055123,93.03048953972));
#107260=CARTESIAN_POINT('Ctrl Pts',(4.80494170520909,-17.87841055123,93.061172168));
#107261=CARTESIAN_POINT('Ctrl Pts',(4.94384757402909,-17.87841055123,93.0746201759801));
#107262=CARTESIAN_POINT('Ctrl Pts',(4.97001116901909,-17.87841055123,93.07704084778));
#107263=CARTESIAN_POINT('Ctrl Pts',(-2.90635108794991,-18.70537143846,90.26266217014));
#107264=CARTESIAN_POINT('Ctrl Pts',(-2.63965269910391,-18.70537143846,90.31581259229));
#107265=CARTESIAN_POINT('Ctrl Pts',(-2.06209396084091,-18.70537143846,90.4407571241401));
#107266=CARTESIAN_POINT('Ctrl Pts',(-1.20499584369091,-18.70537143846,90.6534293353001));
#107267=CARTESIAN_POINT('Ctrl Pts',(-0.362304822780912,-18.70537143846,
90.8839836359601));
#107268=CARTESIAN_POINT('Ctrl Pts',(0.395320769359087,-18.70537143846,91.10343529384));
#107269=CARTESIAN_POINT('Ctrl Pts',(1.07313800872909,-18.70537143846,91.3047836771201));
#107270=CARTESIAN_POINT('Ctrl Pts',(1.68052399893909,-18.70537143846,91.4852562921));
#107271=CARTESIAN_POINT('Ctrl Pts',(2.22876470065909,-18.70537143846,91.64455388772));
#107272=CARTESIAN_POINT('Ctrl Pts',(2.72688845555909,-18.70537143846,91.78329474466));
#107273=CARTESIAN_POINT('Ctrl Pts',(3.18181667720909,-18.70537143846,91.90217180423));
#107274=CARTESIAN_POINT('Ctrl Pts',(3.59823308570909,-18.70537143846,92.00185758637));
#107275=CARTESIAN_POINT('Ctrl Pts',(3.98055430565909,-18.70537143846,92.08363528142));
#107276=CARTESIAN_POINT('Ctrl Pts',(4.33348997659909,-18.70537143846,92.1489694991201));
#107277=CARTESIAN_POINT('Ctrl Pts',(4.66159947439909,-18.70537143846,92.19917357618));
#107278=CARTESIAN_POINT('Ctrl Pts',(4.89708912615909,-18.70537143846,92.2272532641701));
#107279=CARTESIAN_POINT('Ctrl Pts',(5.02346586689909,-18.70537143846,92.23948669662));
#107280=CARTESIAN_POINT('Ctrl Pts',(5.04723951276909,-18.70537143846,92.2416857915));
#107281=CARTESIAN_POINT('Ctrl Pts',(-2.68078525475691,-18.46966542386,89.1307579413));
#107282=CARTESIAN_POINT('Ctrl Pts',(-2.40173836763091,-18.46966542386,89.18636944872));
#107283=CARTESIAN_POINT('Ctrl Pts',(-1.79940882562091,-18.46966542386,89.31670588532));
#107284=CARTESIAN_POINT('Ctrl Pts',(-0.912554851410912,-18.46966542386,
89.5368209230901));
#107285=CARTESIAN_POINT('Ctrl Pts',(-0.0482663113909114,-18.46966542386,
89.7733254300899));
#107286=CARTESIAN_POINT('Ctrl Pts',(0.721329194239087,-18.46966542386,89.99626612027));
#107287=CARTESIAN_POINT('Ctrl Pts',(1.40301708156909,-18.46966542386,90.1987708256));
#107288=CARTESIAN_POINT('Ctrl Pts',(2.00711811150908,-18.46966542386,90.3782613619799));
#107289=CARTESIAN_POINT('Ctrl Pts',(2.54582046205908,-18.46966542386,90.53477235655));
#107290=CARTESIAN_POINT('Ctrl Pts',(3.02900889400909,-18.46966542386,90.66932739364));
#107291=CARTESIAN_POINT('Ctrl Pts',(3.46336533396909,-18.46966542386,90.78279479372));
#107292=CARTESIAN_POINT('Ctrl Pts',(3.85460977005909,-18.46966542386,90.8764167646));
#107293=CARTESIAN_POINT('Ctrl Pts',(4.20769182441909,-18.46966542386,90.9518953727701));
#107294=CARTESIAN_POINT('Ctrl Pts',(4.52715636601909,-18.46966542386,91.01098304712));
#107295=CARTESIAN_POINT('Ctrl Pts',(4.81818349152909,-18.46966542386,91.05546904236));
#107296=CARTESIAN_POINT('Ctrl Pts',(5.02386333443909,-18.46966542386,91.0799676676101));
#107297=CARTESIAN_POINT('Ctrl Pts',(5.13300280174909,-18.46966542386,91.09053011623));
#107298=CARTESIAN_POINT('Ctrl Pts',(5.15348841302909,-18.46966542386,91.0924243709));
#107299=CARTESIAN_POINT('',(4.84744046295298,-18.0488789356219,92.4405620175361));
#107300=CARTESIAN_POINT('',(4.96802222338909,-18.49999999899,91.37511854801));
#107301=CARTESIAN_POINT('Ctrl Pts',(4.84744046295299,-18.0488789356218,
92.440562017536));
#107302=CARTESIAN_POINT('Ctrl Pts',(4.85102555078097,-18.0815232141951,
92.4088329939532));
#107303=CARTESIAN_POINT('Ctrl Pts',(4.85478207102745,-18.1127201945377,
92.3756064273925));
#107304=CARTESIAN_POINT('Ctrl Pts',(4.85868549383694,-18.1422807586517,
92.3410948468652));
#107305=CARTESIAN_POINT('Ctrl Pts',(4.86260561708453,-18.1719677949405,
92.3064356116915));
#107306=CARTESIAN_POINT('Ctrl Pts',(4.86667382820382,-18.2000039257964,
92.2704809975323));
#107307=CARTESIAN_POINT('Ctrl Pts',(4.87086197000954,-18.2262411725814,
92.2334756604867));
#107308=CARTESIAN_POINT('Ctrl Pts',(4.87506446674988,-18.2525683480221,
92.1963434869542));
#107309=CARTESIAN_POINT('Ctrl Pts',(4.87938763195323,-18.2770840322067,
92.1581541306553));
#107310=CARTESIAN_POINT('Ctrl Pts',(4.88380090536888,-18.2996878866408,
92.1191736136303));
#107311=CARTESIAN_POINT('Ctrl Pts',(4.88825477898303,-18.3224996867175,
92.07983449278));
#107312=CARTESIAN_POINT('Ctrl Pts',(4.89280033628601,-18.3433642290032,
92.0396903814176));
#107313=CARTESIAN_POINT('Ctrl Pts',(4.89740535261491,-18.362231073403,91.9990221095588));
#107314=CARTESIAN_POINT('Ctrl Pts',(4.89993844674995,-18.3726092109562,
91.9766516001902));
#107315=CARTESIAN_POINT('Ctrl Pts',(4.90248952589719,-18.382383822476,91.9541225481696));
#107316=CARTESIAN_POINT('Ctrl Pts',(4.9050532720603,-18.3915532115038,91.9314813226531));
#107317=CARTESIAN_POINT('Ctrl Pts',(4.90978228961777,-18.408466821099,91.8897179240253));
#107318=CARTESIAN_POINT('Ctrl Pts',(4.9145543126211,-18.4233184390315,91.8475736367873));
#107319=CARTESIAN_POINT('Ctrl Pts',(4.91933724298231,-18.4361372479446,
91.8053295547132));
#107320=CARTESIAN_POINT('Ctrl Pts',(4.92421230508372,-18.4492029806228,
91.7622717412023));
#107321=CARTESIAN_POINT('Ctrl Pts',(4.9290986181819,-18.4601571995976,91.7191109638508));
#107322=CARTESIAN_POINT('Ctrl Pts',(4.93396478461095,-18.4690800708054,
91.6761221600157));
#107323=CARTESIAN_POINT('Ctrl Pts',(4.93889011969135,-18.4781114369162,
91.6326106470659));
#107324=CARTESIAN_POINT('Ctrl Pts',(4.94379475346279,-18.4850623405295,
91.5892758617947));
#107325=CARTESIAN_POINT('Ctrl Pts',(4.94864984772086,-18.4900585310788,
91.5463702061315));
#107326=CARTESIAN_POINT('Ctrl Pts',(4.95360660584777,-18.4951593400008,
91.5025661219893));
#107327=CARTESIAN_POINT('Ctrl Pts',(4.95851167916532,-18.4982233765136,
91.4592097608613));
#107328=CARTESIAN_POINT('Ctrl Pts',(4.96333909424765,-18.499419121208,91.4165282140099));
#107329=CARTESIAN_POINT('Ctrl Pts',(4.96490856559217,-18.4998078773023,
91.402651747292));
#107330=CARTESIAN_POINT('Ctrl Pts',(4.96646986780409,-18.4999993792627,
91.3888462619152));
#107331=CARTESIAN_POINT('Ctrl Pts',(4.96802222338909,-18.4999999984913,
91.37511854801));
#107332=CARTESIAN_POINT('',(-2.58464131998993,-18.4999999121182,89.4559753223385));
#107333=CARTESIAN_POINT('Ctrl Pts',(-2.58464131998983,-18.4999999284356,
89.4559753223381));
#107334=CARTESIAN_POINT('Ctrl Pts',(-2.42247927437401,-18.4999999283618,
89.4893110383322));
#107335=CARTESIAN_POINT('Ctrl Pts',(-2.26335533538253,-18.4999999529729,
89.5236774280323));
#107336=CARTESIAN_POINT('Ctrl Pts',(-2.10688850553027,-18.4999999715301,
89.5588228176755));
#107337=CARTESIAN_POINT('Ctrl Pts',(-2.04276780678778,-18.4999999791349,
89.5732255312961));
#107338=CARTESIAN_POINT('Ctrl Pts',(-1.97909337321858,-18.499999985739,
89.587759699513));
#107339=CARTESIAN_POINT('Ctrl Pts',(-1.91583913818256,-18.49999999043,89.6024104702437));
#107340=CARTESIAN_POINT('Ctrl Pts',(-1.8205009702631,-18.4999999975004,
89.6244924326495));
#107341=CARTESIAN_POINT('Ctrl Pts',(-1.72611730868866,-18.499999999998,
89.646838986621));
#107342=CARTESIAN_POINT('Ctrl Pts',(-1.63259488358994,-18.499999999998,
89.6694020422784));
#107343=CARTESIAN_POINT('Ctrl Pts',(-1.43742956816962,-18.499999999998,
89.716487282739));
#107344=CARTESIAN_POINT('Ctrl Pts',(-1.24601784666857,-18.4999999972403,
89.7644910558193));
#107345=CARTESIAN_POINT('Ctrl Pts',(-1.06015417158908,-18.4999999985324,
89.8125315836417));
#107346=CARTESIAN_POINT('Ctrl Pts',(-1.02723545567207,-18.4999999987613,
89.8210401450226));
#107347=CARTESIAN_POINT('Ctrl Pts',(-0.994490687489129,-18.4999999990028,
89.8295497600841));
#107348=CARTESIAN_POINT('Ctrl Pts',(-0.961929727974486,-18.4999999992167,
89.8380554342449));
#107349=CARTESIAN_POINT('Ctrl Pts',(-0.889157904801211,-18.499999999695,
89.8570651140955));
#107350=CARTESIAN_POINT('Ctrl Pts',(-0.817304239126653,-18.499999999998,
89.8760550782654));
#107351=CARTESIAN_POINT('Ctrl Pts',(-0.746477846876206,-18.499999999998,
89.8949680126866));
#107352=CARTESIAN_POINT('Ctrl Pts',(-0.60356647905789,-18.499999999998,
89.933129963927));
#107353=CARTESIAN_POINT('Ctrl Pts',(-0.464844365327987,-18.4999999995685,
89.970995089684));
#107354=CARTESIAN_POINT('Ctrl Pts',(-0.329968692827295,-18.4999999996937,
90.0084006617666));
#107355=CARTESIAN_POINT('Ctrl Pts',(-0.252794460947361,-18.4999999997653,
90.0298036786338));
#107356=CARTESIAN_POINT('Ctrl Pts',(-0.176879758684409,-18.4999999998833,
90.0510572704772));
#107357=CARTESIAN_POINT('Ctrl Pts',(-0.102161930483246,-18.4999999999422,
90.0721383232775));
#107358=CARTESIAN_POINT('Ctrl Pts',(-0.0502963668242797,-18.499999999983,
90.086771787771));
#107359=CARTESIAN_POINT('Ctrl Pts',(0.000992469381286637,-18.499999999998,
90.1013222121036));
#107360=CARTESIAN_POINT('Ctrl Pts',(0.0517258844157116,-18.499999999998,
90.1157821369));
#107361=CARTESIAN_POINT('Ctrl Pts',(0.193134512360498,-18.499999999998,
90.1560861086365));
#107362=CARTESIAN_POINT('Ctrl Pts',(0.33022671944429,-18.4999999999633,
90.1956827469086));
#107363=CARTESIAN_POINT('Ctrl Pts',(0.46302310172386,-18.4999999999761,
90.2343586844309));
#107364=CARTESIAN_POINT('Ctrl Pts',(0.531039009910421,-18.4999999999826,
90.2541678009925));
#107365=CARTESIAN_POINT('Ctrl Pts',(0.597927807241826,-18.4999999999913,
90.2737362471997));
#107366=CARTESIAN_POINT('Ctrl Pts',(0.663691145680396,-18.4999999999951,
90.2930404695069));
#107367=CARTESIAN_POINT('Ctrl Pts',(0.697937951951777,-18.4999999999972,
90.3030933040691));
#107368=CARTESIAN_POINT('Ctrl Pts',(0.731879533548189,-18.499999999998,
90.3130745357137));
#107369=CARTESIAN_POINT('Ctrl Pts',(0.765516009892471,-18.499999999998,
90.3229808414617));
#107370=CARTESIAN_POINT('Ctrl Pts',(0.895913684424494,-18.499999999998,
90.3613843656453));
#107371=CARTESIAN_POINT('Ctrl Pts',(1.02172716610423,-18.4999999999955,
90.398659670361));
#107372=CARTESIAN_POINT('Ctrl Pts',(1.14344094134313,-18.4999999999968,
90.4347827934306));
#107373=CARTESIAN_POINT('Ctrl Pts',(1.2104749224429,-18.4999999999976,90.4546776388937));
#107374=CARTESIAN_POINT('Ctrl Pts',(1.27626507277148,-18.499999999998,90.4742240041735));
#107375=CARTESIAN_POINT('Ctrl Pts',(1.34089047774472,-18.499999999998,90.4934241691768));
#107376=CARTESIAN_POINT('Ctrl Pts',(1.36079879604639,-18.499999999998,90.499338917355));
#107377=CARTESIAN_POINT('Ctrl Pts',(1.38059657252599,-18.499999999998,90.5052208381738));
#107378=CARTESIAN_POINT('Ctrl Pts',(1.40028612569937,-18.499999999998,90.5110699428851));
#107379=CARTESIAN_POINT('Ctrl Pts',(1.52644468342528,-18.499999999998,90.548547411666));
#107380=CARTESIAN_POINT('Ctrl Pts',(1.64816139383854,-18.499999999998,90.5846746827562));
#107381=CARTESIAN_POINT('Ctrl Pts',(1.76585682848137,-18.4999999999979,
90.6194412743614));
#107382=CARTESIAN_POINT('Ctrl Pts',(1.82568407703918,-18.4999999999979,
90.6371139183666));
#107383=CARTESIAN_POINT('Ctrl Pts',(1.88447200669,-18.499999999998,90.6544358703474));
#107384=CARTESIAN_POINT('Ctrl Pts',(1.94227444066315,-18.499999999998,90.6714105346848));
#107385=CARTESIAN_POINT('Ctrl Pts',(1.95071832499579,-18.499999999998,90.673890224421));
#107386=CARTESIAN_POINT('Ctrl Pts',(1.95914117746727,-18.499999999998,90.6763625078161));
#107387=CARTESIAN_POINT('Ctrl Pts',(1.96754316566384,-18.499999999998,90.6788273937299));
#107388=CARTESIAN_POINT('Ctrl Pts',(2.09512410234678,-18.499999999998,90.7162557316824));
#107389=CARTESIAN_POINT('Ctrl Pts',(2.21789632546597,-18.4999999999977,
90.7519713117329));
#107390=CARTESIAN_POINT('Ctrl Pts',(2.33648048522128,-18.4999999999979,
90.786049104768));
#107391=CARTESIAN_POINT('Ctrl Pts',(2.38433447329468,-18.499999999998,90.7998010114715));
#107392=CARTESIAN_POINT('Ctrl Pts',(2.43150622941636,-18.499999999998,90.8132868222452));
#107393=CARTESIAN_POINT('Ctrl Pts',(2.47803575426742,-18.499999999998,90.826513582735));
#107394=CARTESIAN_POINT('Ctrl Pts',(2.47881274636391,-18.499999999998,90.8267344551465));
#107395=CARTESIAN_POINT('Ctrl Pts',(2.47958955946783,-18.499999999998,90.8269552553909));
#107396=CARTESIAN_POINT('Ctrl Pts',(2.48036619365538,-18.499999999998,90.8271759834721));
#107397=CARTESIAN_POINT('Ctrl Pts',(2.59599001793783,-18.499999999998,90.8600375614012));
#107398=CARTESIAN_POINT('Ctrl Pts',(2.70764837268176,-18.4999999999976,
90.8912949119218));
#107399=CARTESIAN_POINT('Ctrl Pts',(2.81556632146251,-18.4999999999978,
90.920943621444));
#107400=CARTESIAN_POINT('Ctrl Pts',(2.85790008751792,-18.4999999999979,
90.9325741383964));
#107401=CARTESIAN_POINT('Ctrl Pts',(2.89965825399694,-18.499999999998,90.9439577145226));
#107402=CARTESIAN_POINT('Ctrl Pts',(2.94085432970763,-18.499999999998,90.9550961870934));
#107403=CARTESIAN_POINT('Ctrl Pts',(2.94914642739974,-18.499999999998,90.9573381798343));
#107404=CARTESIAN_POINT('Ctrl Pts',(2.95741575404617,-18.499999999998,90.9595702252726));
#107405=CARTESIAN_POINT('Ctrl Pts',(2.96566243524428,-18.499999999998,90.9617923484759));
#107406=CARTESIAN_POINT('Ctrl Pts',(3.07761262151744,-18.4999999999979,
90.9919580721831));
#107407=CARTESIAN_POINT('Ctrl Pts',(3.18539085749446,-18.499999999998,91.0202907326444));
#107408=CARTESIAN_POINT('Ctrl Pts',(3.28933672475092,-18.499999999998,91.0468531181577));
#107409=CARTESIAN_POINT('Ctrl Pts',(3.31340128417257,-18.499999999998,91.0530025892376));
#107410=CARTESIAN_POINT('Ctrl Pts',(3.33726037793146,-18.499999999998,91.0590573938579));
#107411=CARTESIAN_POINT('Ctrl Pts',(3.36091811406057,-18.499999999998,91.0650186686483));
#107412=CARTESIAN_POINT('Ctrl Pts',(3.3753343264924,-18.499999999998,91.0686512649066));
#107413=CARTESIAN_POINT('Ctrl Pts',(3.3896757551439,-18.499999999998,91.0722490588392));
#107414=CARTESIAN_POINT('Ctrl Pts',(3.40394331686185,-18.499999999998,91.0758123249327));
#107415=CARTESIAN_POINT('Ctrl Pts',(3.52167444174278,-18.499999999998,91.1052151993504));
#107416=CARTESIAN_POINT('Ctrl Pts',(3.63437646858574,-18.499999999998,91.1322618551093));
#107417=CARTESIAN_POINT('Ctrl Pts',(3.74253208016573,-18.499999999998,91.1571146440383));
#107418=CARTESIAN_POINT('Ctrl Pts',(3.7618984974429,-18.499999999998,91.1615648013059));
#107419=CARTESIAN_POINT('Ctrl Pts',(3.78111903871853,-18.499999999998,91.1659445281595));
#107420=CARTESIAN_POINT('Ctrl Pts',(3.80019667602617,-18.499999999998,91.1702549980734));
#107421=CARTESIAN_POINT('Ctrl Pts',(3.90057358324263,-18.499999999998,91.192934517116));
#107422=CARTESIAN_POINT('Ctrl Pts',(3.99699359909732,-18.499999999998,91.213693972243));
#107423=CARTESIAN_POINT('Ctrl Pts',(4.08986202778578,-18.499999999998,91.2326836615883));
#107424=CARTESIAN_POINT('Ctrl Pts',(4.11321407376547,-18.499999999998,91.2374586761438));
#107425=CARTESIAN_POINT('Ctrl Pts',(4.13634181685589,-18.4999999999978,
91.2421216703581));
#107426=CARTESIAN_POINT('Ctrl Pts',(4.15925062103235,-18.4999999999975,
91.2466749152964));
#107427=CARTESIAN_POINT('Ctrl Pts',(4.24476307603062,-18.4999999999964,
91.2636709640594));
#107428=CARTESIAN_POINT('Ctrl Pts',(4.32722530770209,-18.499999999998,91.2791362303439));
#107429=CARTESIAN_POINT('Ctrl Pts',(4.4069358511759,-18.499999999998,91.2931767758584));
#107430=CARTESIAN_POINT('Ctrl Pts',(4.43352619799537,-18.499999999998,91.2978605097597));
#107431=CARTESIAN_POINT('Ctrl Pts',(4.4598108703507,-18.4999999999967,91.3023857892519));
#107432=CARTESIAN_POINT('Ctrl Pts',(4.48581020126748,-18.4999999999932,
91.3067590894636));
#107433=CARTESIAN_POINT('Ctrl Pts',(4.55862954204631,-18.4999999999834,
91.3190078984604));
#107434=CARTESIAN_POINT('Ctrl Pts',(4.62921135945304,-18.499999999998,91.3300662706501));
#107435=CARTESIAN_POINT('Ctrl Pts',(4.6980281630798,-18.499999999998,91.3400811393066));
#107436=CARTESIAN_POINT('Ctrl Pts',(4.72731383018175,-18.499999999998,91.3443430650877));
#107437=CARTESIAN_POINT('Ctrl Pts',(4.75627755155606,-18.4999999999705,
91.3484164128833));
#107438=CARTESIAN_POINT('Ctrl Pts',(4.7849101034947,-18.4999999998331,91.3523016553103));
#107439=CARTESIAN_POINT('Ctrl Pts',(4.84758195043468,-18.4999999995324,
91.3608057984001));
#107440=CARTESIAN_POINT('Ctrl Pts',(4.90866663149108,-18.4999999984913,
91.368407217816));
#107441=CARTESIAN_POINT('Ctrl Pts',(4.96802222338909,-18.4999999984913,
91.37511854801));
#107442=CARTESIAN_POINT('',(-2.88651065708645,-17.0216929393251,90.9254156321813));
#107443=CARTESIAN_POINT('Ctrl Pts',(-2.88651065708645,-17.0216929393251,
90.9254156321813));
#107444=CARTESIAN_POINT('Ctrl Pts',(-2.88640145180437,-17.0995628086248,
90.9240272056507));
#107445=CARTESIAN_POINT('Ctrl Pts',(-2.88729944606883,-17.170132058898,
90.9182441598227));
#107446=CARTESIAN_POINT('Ctrl Pts',(-2.88408965246998,-17.3078577072757,
90.8939618230676));
#107447=CARTESIAN_POINT('Ctrl Pts',(-2.88165190999378,-17.3582840935947,
90.8831196587877));
#107448=CARTESIAN_POINT('Ctrl Pts',(-2.87552901840975,-17.4404493016207,
90.8603531966015));
#107449=CARTESIAN_POINT('Ctrl Pts',(-2.87310852973623,-17.468898354374,
90.8516715121079));
#107450=CARTESIAN_POINT('Ctrl Pts',(-2.86918206784385,-17.5129573190361,
90.8366384861846));
#107451=CARTESIAN_POINT('Ctrl Pts',(-2.86714859023221,-17.5353318776479,
90.8286186440903));
#107452=CARTESIAN_POINT('Ctrl Pts',(-2.86475180509675,-17.5619825690364,
90.8182933829514));
#107453=CARTESIAN_POINT('Ctrl Pts',(-2.863732365432,-17.5735147448426,90.8136508779198));
#107454=CARTESIAN_POINT('Ctrl Pts',(-2.86305596572654,-17.5812266358903,
90.8105064691031));
#107455=CARTESIAN_POINT('Ctrl Pts',(-2.86255639671044,-17.586986281638,
90.8081184917741));
#107456=CARTESIAN_POINT('Ctrl Pts',(-2.85690609956517,-17.6525742813425,
90.7806925204851));
#107457=CARTESIAN_POINT('Ctrl Pts',(-2.85015602453725,-17.7273084397827,
90.7444067214191));
#107458=CARTESIAN_POINT('Ctrl Pts',(-2.83431530931937,-17.8501475630206,
90.6673151810356));
#107459=CARTESIAN_POINT('Ctrl Pts',(-2.82812127750925,-17.8928217227995,
90.6378193587231));
#107460=CARTESIAN_POINT('Ctrl Pts',(-2.8173670861126,-17.9580952571083,
90.5867852678644));
#107461=CARTESIAN_POINT('Ctrl Pts',(-2.81354134391614,-17.9800592712919,
90.5686422926648));
#107462=CARTESIAN_POINT('Ctrl Pts',(-2.80745541916469,-18.0131096158549,
90.539600189903));
#107463=CARTESIAN_POINT('Ctrl Pts',(-2.80432589827305,-18.0296604584008,
90.5246223378286));
#107464=CARTESIAN_POINT('Ctrl Pts',(-2.80052923960525,-18.0489654998569,
90.5063217870538));
#107465=CARTESIAN_POINT('Ctrl Pts',(-2.79887172307984,-18.0572326206646,
90.4982988410398));
#107466=CARTESIAN_POINT('Ctrl Pts',(-2.79776005649735,-18.0627419725255,
90.4929099399053));
#107467=CARTESIAN_POINT('Ctrl Pts',(-2.79688285041213,-18.0670519694588,
90.4886488573163));
#107468=CARTESIAN_POINT('Ctrl Pts',(-2.7809971705961,-18.1447885552345,
90.4114045008268));
#107469=CARTESIAN_POINT('Ctrl Pts',(-2.76011268807195,-18.2451010616449,
90.2967069554987));
#107470=CARTESIAN_POINT('Ctrl Pts',(-2.69081716629771,-18.4229990851704,
89.9576497125368));
#107471=CARTESIAN_POINT('Ctrl Pts',(-2.64099778080791,-18.5000050727964,
89.7303413150615));
#107472=CARTESIAN_POINT('Ctrl Pts',(-2.58464131999691,-18.49999991758,89.45597532234));
#107473=CARTESIAN_POINT('Ctrl Pts',(-2.88654644014915,-17.0216953618235,
90.9255898508946));
#107474=CARTESIAN_POINT('Ctrl Pts',(-2.69742490916333,-17.041410134392,
90.9641774992515));
#107475=CARTESIAN_POINT('Ctrl Pts',(-2.51120236344264,-17.0612039407382,
91.0040506043034));
#107476=CARTESIAN_POINT('Ctrl Pts',(-2.32785216427436,-17.0810959232659,
91.0447708513586));
#107477=CARTESIAN_POINT('Ctrl Pts',(-2.14045947996118,-17.1014264820495,
91.0863888939688));
#107478=CARTESIAN_POINT('Ctrl Pts',(-1.95606671680399,-17.1218596123584,
91.1288915704916));
#107479=CARTESIAN_POINT('Ctrl Pts',(-1.77461315546025,-17.1423912528085,
91.1718473703202));
#107480=CARTESIAN_POINT('Ctrl Pts',(-1.69875208969935,-17.1509750034654,
91.1898060851091));
#107481=CARTESIAN_POINT('Ctrl Pts',(-1.62340441551236,-17.1595756812106,
91.2078444544791));
#107482=CARTESIAN_POINT('Ctrl Pts',(-1.5485643763496,-17.1681917671988,
91.2259329295346));
#107483=CARTESIAN_POINT('Ctrl Pts',(-1.36386673018872,-17.189455395852,
91.27057345622));
#107484=CARTESIAN_POINT('Ctrl Pts',(-1.1822620916855,-17.210814547539,91.3155161541178));
#107485=CARTESIAN_POINT('Ctrl Pts',(-1.00367274643416,-17.2322304456851,
91.360358654297));
#107486=CARTESIAN_POINT('Ctrl Pts',(-0.821153209633123,-17.2541176406033,
91.4061879973085));
#107487=CARTESIAN_POINT('Ctrl Pts',(-0.64178274964877,-17.2760639662355,
91.4519125695349));
#107488=CARTESIAN_POINT('Ctrl Pts',(-0.465462221090628,-17.2980036926607,
91.4971491013743));
#107489=CARTESIAN_POINT('Ctrl Pts',(-0.369787773236968,-17.3099085526844,
91.521695195025));
#107490=CARTESIAN_POINT('Ctrl Pts',(-0.27501108593264,-17.3218110634227,
91.5460983993004));
#107491=CARTESIAN_POINT('Ctrl Pts',(-0.181114947793367,-17.3336980941036,
91.5703031290285));
#107492=CARTESIAN_POINT('Ctrl Pts',(-0.0790942960888194,-17.3466136691308,
91.5966022117184));
#107493=CARTESIAN_POINT('Ctrl Pts',(0.0218789296780678,-17.3595252062434,
91.6226614043843));
#107494=CARTESIAN_POINT('Ctrl Pts',(0.12182234793271,-17.3724259044824,
91.6484080358699));
#107495=CARTESIAN_POINT('Ctrl Pts',(0.30998982251177,-17.39671456551,91.6968822496818));
#107496=CARTESIAN_POINT('Ctrl Pts',(0.494506517524576,-17.4209664306911,
91.7442458924625));
#107497=CARTESIAN_POINT('Ctrl Pts',(0.675467730717484,-17.4451363296152,
91.7900785790369));
#107498=CARTESIAN_POINT('Ctrl Pts',(0.789151121036989,-17.4603203350985,
91.8188715734322));
#107499=CARTESIAN_POINT('Ctrl Pts',(0.901431491157078,-17.4754714086846,
91.8470612859899));
#107500=CARTESIAN_POINT('Ctrl Pts',(1.01233389736521,-17.4905731708789,
91.8745524394624));
#107501=CARTESIAN_POINT('Ctrl Pts',(1.19516693491735,-17.5154698448898,
91.9198741891616));
#107502=CARTESIAN_POINT('Ctrl Pts',(1.37425545371614,-17.5402425452337,
91.9632925176879));
#107503=CARTESIAN_POINT('Ctrl Pts',(1.54966415730625,-17.5648280185183,
92.0043877322477));
#107504=CARTESIAN_POINT('Ctrl Pts',(1.55711643999401,-17.5658725385061,
92.006133672727));
#107505=CARTESIAN_POINT('Ctrl Pts',(1.56456208233662,-17.5669167174875,
92.0078754261942));
#107506=CARTESIAN_POINT('Ctrl Pts',(1.57200108815818,-17.5679605542422,
92.0096129661756));
#107507=CARTESIAN_POINT('Ctrl Pts',(1.66326869021053,-17.5807671684348,
92.0309304797484));
#107508=CARTESIAN_POINT('Ctrl Pts',(1.75353600577784,-17.5935218518874,
92.0516133663183));
#107509=CARTESIAN_POINT('Ctrl Pts',(1.84280452510977,-17.6062185966182,
92.0716139593751));
#107510=CARTESIAN_POINT('Ctrl Pts',(1.88743878477574,-17.6125669689836,
92.0816142559036));
#107511=CARTESIAN_POINT('Ctrl Pts',(1.93182334131449,-17.6189008808474,
92.091443999122));
#107512=CARTESIAN_POINT('Ctrl Pts',(1.97595786838733,-17.6252192062876,
92.1010974690801));
#107513=CARTESIAN_POINT('Ctrl Pts',(1.99802513192375,-17.6283783690077,
92.1059242040592));
#107514=CARTESIAN_POINT('Ctrl Pts',(2.02002988749721,-17.6315336357843,
92.1107068726981));
#107515=CARTESIAN_POINT('Ctrl Pts',(2.04197208025779,-17.6346848579343,
92.115444774685));
#107516=CARTESIAN_POINT('Ctrl Pts',(2.05294317663808,-17.6362604690094,
92.1178137256784));
#107517=CARTESIAN_POINT('Ctrl Pts',(2.06389863227572,-17.6378350689654,
92.1201714851346));
#107518=CARTESIAN_POINT('Ctrl Pts',(2.07483843855079,-17.6394086378195,
92.1225179666464));
#107519=CARTESIAN_POINT('Ctrl Pts',(2.08030834168832,-17.6401954222466,
92.1236912074023));
#107520=CARTESIAN_POINT('Ctrl Pts',(2.08577433248242,-17.6409819489,92.1248616286805));
#107521=CARTESIAN_POINT('Ctrl Pts',(2.09123640974304,-17.6417682151897,
92.1260292197551));
#107522=CARTESIAN_POINT('Ctrl Pts',(2.09669848700366,-17.6425544814794,
92.1271968108297));
#107523=CARTESIAN_POINT('Ctrl Pts',(2.10351059955061,-17.6435355382329,
92.1286500037437));
#107524=CARTESIAN_POINT('Ctrl Pts',(2.10761089969447,-17.6441262303533,
92.1295234916842));
#107525=CARTESIAN_POINT('Ctrl Pts',(2.24213694842401,-17.6635061474786,
92.158181608681));
#107526=CARTESIAN_POINT('Ctrl Pts',(2.37612643197818,-17.6830114011268,
92.1854976283726));
#107527=CARTESIAN_POINT('Ctrl Pts',(2.5096587865986,-17.702596240886,92.2112306127136));
#107528=CARTESIAN_POINT('Ctrl Pts',(2.63660724765655,-17.7212154382676,
92.2356948166873));
#107529=CARTESIAN_POINT('Ctrl Pts',(2.76314226648604,-17.7399063896977,
92.2587286478074));
#107530=CARTESIAN_POINT('Ctrl Pts',(2.88931162583231,-17.7586288569726,
92.2800864466862));
#107531=CARTESIAN_POINT('Ctrl Pts',(2.91200856687956,-17.761996891321,92.283928557834));
#107532=CARTESIAN_POINT('Ctrl Pts',(2.93469327762316,-17.765365993577,92.2877161953679));
#107533=CARTESIAN_POINT('Ctrl Pts',(2.95736544668735,-17.7687356707034,
92.2914478033765));
#107534=CARTESIAN_POINT('Ctrl Pts',(3.06399310547184,-17.7845833287652,
92.3089976295241));
#107535=CARTESIAN_POINT('Ctrl Pts',(3.17034340538539,-17.8004430770719,
92.3253095598612));
#107536=CARTESIAN_POINT('Ctrl Pts',(3.2764152873118,-17.8162938077448,92.3402375054109));
#107537=CARTESIAN_POINT('Ctrl Pts',(3.34072822557292,-17.8259043383081,
92.3492885378152));
#107538=CARTESIAN_POINT('Ctrl Pts',(3.40493909975878,-17.8355114884629,
92.3578306426863));
#107539=CARTESIAN_POINT('Ctrl Pts',(3.4690461953169,-17.8451081528638,92.3658301801403));
#107540=CARTESIAN_POINT('Ctrl Pts',(3.50109974309596,-17.8499064850642,
92.3698299488672));
#107541=CARTESIAN_POINT('Ctrl Pts',(3.5331273495993,-17.8547021827024,92.3736940590896));
#107542=CARTESIAN_POINT('Ctrl Pts',(3.56512883049294,-17.8594942505125,
92.3774182247455));
#107543=CARTESIAN_POINT('Ctrl Pts',(3.58112957093976,-17.8618902844176,
92.3792803075735));
#107544=CARTESIAN_POINT('Ctrl Pts',(3.59712377991582,-17.8642854098686,
92.3811074036578));
#107545=CARTESIAN_POINT('Ctrl Pts',(3.61311160553143,-17.8666795875392,
92.382898941446));
#107546=CARTESIAN_POINT('Ctrl Pts',(3.62110551833924,-17.8678766763745,
92.3837947103401));
#107547=CARTESIAN_POINT('Ctrl Pts',(3.62909783536523,-17.869073528213,92.3846815895001));
#107548=CARTESIAN_POINT('Ctrl Pts',(3.63708856106238,-17.8702701303337,
92.3855595089788));
#107549=CARTESIAN_POINT('Ctrl Pts',(3.64108392391096,-17.870868431394,92.3859984687182));
#107550=CARTESIAN_POINT('Ctrl Pts',(3.64507888892851,-17.8714666700209,
92.3864351885318));
#107551=CARTESIAN_POINT('Ctrl Pts',(3.64907345713086,-17.8720648448385,
92.3868696595651));
#107552=CARTESIAN_POINT('Ctrl Pts',(3.65306802533321,-17.8726630196562,
92.3873041305985));
#107553=CARTESIAN_POINT('Ctrl Pts',(3.658527814823,-17.8734805988681,92.3878941393569));
#107554=CARTESIAN_POINT('Ctrl Pts',(3.66105597228307,-17.8738591764567,
92.3881663174479));
#107555=CARTESIAN_POINT('Ctrl Pts',(3.72371374321079,-17.8832418308994,
92.394911970258));
#107556=CARTESIAN_POINT('Ctrl Pts',(3.78901989206686,-17.8931014191951,
92.4013404584845));
#107557=CARTESIAN_POINT('Ctrl Pts',(3.85701405172134,-17.9033669342938,
92.4073040728435));
#107558=CARTESIAN_POINT('Ctrl Pts',(3.92249284713516,-17.9132526886935,
92.4130470702793));
#107559=CARTESIAN_POINT('Ctrl Pts',(3.99046428990993,-17.9235147273393,
92.4183593456255));
#107560=CARTESIAN_POINT('Ctrl Pts',(4.06094707366189,-17.9340966321926,
92.4230648892938));
#107561=CARTESIAN_POINT('Ctrl Pts',(4.12765142717222,-17.9441112639164,
92.4275181789001));
#107562=CARTESIAN_POINT('Ctrl Pts',(4.19660487502362,-17.9544123001695,
92.4314283106798));
#107563=CARTESIAN_POINT('Ctrl Pts',(4.2678107284946,-17.9649600297792,92.4346013919948));
#107564=CARTESIAN_POINT('Ctrl Pts',(4.28593821212532,-17.967645255593,92.4354091904663));
#107565=CARTESIAN_POINT('Ctrl Pts',(4.30421161719959,-17.9703465160244,
92.4361689716465));
#107566=CARTESIAN_POINT('Ctrl Pts',(4.3226308844424,-17.9730632553954,92.4368770012617));
#107567=CARTESIAN_POINT('Ctrl Pts',(4.39257963099959,-17.9833803060804,
92.4395658044295));
#107568=CARTESIAN_POINT('Ctrl Pts',(4.46463198547307,-17.9939194501827,
92.4415119953763));
#107569=CARTESIAN_POINT('Ctrl Pts',(4.53880237008988,-18.0046684519818,
92.4424903462829));
#107570=CARTESIAN_POINT('Ctrl Pts',(4.60912854064787,-18.0148603383764,
92.4434179897498));
#107571=CARTESIAN_POINT('Ctrl Pts',(4.68135875542199,-18.0252409159418,
92.443475716865));
#107572=CARTESIAN_POINT('Ctrl Pts',(4.75550555857239,-18.0358125205007,
92.4424264461874));
#107573=CARTESIAN_POINT('Ctrl Pts',(4.7858295892246,-18.0401360199243,92.4419973229503));
#107574=CARTESIAN_POINT('Ctrl Pts',(4.81647419910139,-18.0444916218126,
92.4413824851498));
#107575=CARTESIAN_POINT('Ctrl Pts',(4.84744032554683,-18.0488801253806,
92.4405632308584));
#107576=CARTESIAN_POINT('Origin',(-2.58407189360391,-17.,89.45612065267));
#107577=CARTESIAN_POINT('',(-2.84482658273101,-17.,87.9789588497187));
#107578=CARTESIAN_POINT('Ctrl Pts',(-2.844826582731,-17.,87.9789588497187));
#107579=CARTESIAN_POINT('Ctrl Pts',(-2.84474020216979,-17.0600615703758,
87.9789436014661));
#107580=CARTESIAN_POINT('Ctrl Pts',(-2.8440475178467,-17.1201226165087,
87.9824888876553));
#107581=CARTESIAN_POINT('Ctrl Pts',(-2.84275231695818,-17.1797509891795,
87.9895689077724));
#107582=CARTESIAN_POINT('Ctrl Pts',(-2.84145949696887,-17.2392697501704,
87.9966359130634));
#107583=CARTESIAN_POINT('Ctrl Pts',(-2.8395666208452,-17.2983570253343,
88.0072246503357));
#107584=CARTESIAN_POINT('Ctrl Pts',(-2.83708086449162,-17.3565891473593,
88.0212580666932));
#107585=CARTESIAN_POINT('Ctrl Pts',(-2.83460337899347,-17.4146275136843,
88.0352447896741));
#107586=CARTESIAN_POINT('Ctrl Pts',(-2.83153717694925,-17.4718160252179,
88.0526532298416));
#107587=CARTESIAN_POINT('Ctrl Pts',(-2.82788921019877,-17.5277471632685,
88.0733567365258));
#107588=CARTESIAN_POINT('Ctrl Pts',(-2.82687791655771,-17.543252459264,
88.0790961870442));
#107589=CARTESIAN_POINT('Ctrl Pts',(-2.82582190161409,-17.5586612136524,
88.085088574193));
#107590=CARTESIAN_POINT('Ctrl Pts',(-2.82472127710851,-17.5739649677497,
88.0913305259417));
#107591=CARTESIAN_POINT('Ctrl Pts',(-2.82093444903734,-17.6266193338087,
88.1128066951359));
#107592=CARTESIAN_POINT('Ctrl Pts',(-2.81659341444049,-17.67802873488,88.1372352251746));
#107593=CARTESIAN_POINT('Ctrl Pts',(-2.81176864354748,-17.727860714738,
88.1644655245471));
#107594=CARTESIAN_POINT('Ctrl Pts',(-2.80704684540288,-17.7766291547849,
88.1911146608284));
#107595=CARTESIAN_POINT('Ctrl Pts',(-2.80186227329621,-17.8238866061767,
88.2204471003098));
#107596=CARTESIAN_POINT('Ctrl Pts',(-2.79625730851192,-17.8693397954361,
88.2522827608542));
#107597=CARTESIAN_POINT('Ctrl Pts',(-2.79079275113092,-17.9136543576889,
88.2833209208611));
#107598=CARTESIAN_POINT('Ctrl Pts',(-2.78492891390007,-17.9562537995739,
88.3167382778251));
#107599=CARTESIAN_POINT('Ctrl Pts',(-2.77867621237408,-17.996886142221,
88.3523330016412));
#107600=CARTESIAN_POINT('Ctrl Pts',(-2.7753205860046,-18.0186922303374,
88.3714355596884));
#107601=CARTESIAN_POINT('Ctrl Pts',(-2.77185243299703,-18.0399321213815,
88.391164640377));
#107602=CARTESIAN_POINT('Ctrl Pts',(-2.76826940460755,-18.0605694879468,
88.4114850041416));
#107603=CARTESIAN_POINT('Ctrl Pts',(-2.76382050087944,-18.0861940845367,
88.4367159909722));
#107604=CARTESIAN_POINT('Ctrl Pts',(-2.75906875878666,-18.1108870680876,
88.4628338346189));
#107605=CARTESIAN_POINT('Ctrl Pts',(-2.75415514434749,-18.134586226575,
88.4897947333846));
#107606=CARTESIAN_POINT('Ctrl Pts',(-2.74937681705425,-18.1576328732399,
88.5160133144347));
#107607=CARTESIAN_POINT('Ctrl Pts',(-2.74444561035497,-18.1797396741942,
88.543029197706));
#107608=CARTESIAN_POINT('Ctrl Pts',(-2.739443581773,-18.2008531725149,88.5707894736323));
#107609=CARTESIAN_POINT('Ctrl Pts',(-2.73457786914399,-18.2213912829511,
88.5977932228004));
#107610=CARTESIAN_POINT('Ctrl Pts',(-2.72964521534768,-18.2409894988228,
88.6255013502613));
#107611=CARTESIAN_POINT('Ctrl Pts',(-2.72467353158546,-18.2596021255553,
88.6538528266334));
#107612=CARTESIAN_POINT('Ctrl Pts',(-2.71975273425192,-18.2780242473909,
88.6819141185429));
#107613=CARTESIAN_POINT('Ctrl Pts',(-2.71479380706206,-18.2954808490119,
88.7106057229541));
#107614=CARTESIAN_POINT('Ctrl Pts',(-2.70977500459608,-18.3119311025169,
88.7398556806549));
#107615=CARTESIAN_POINT('Ctrl Pts',(-2.70480151656836,-18.3282328277619,
88.7688415424062));
#107616=CARTESIAN_POINT('Ctrl Pts',(-2.69976924048947,-18.3435462913634,
88.7983758543922));
#107617=CARTESIAN_POINT('Ctrl Pts',(-2.69460795995078,-18.3578352494326,
88.82837451494));
#107618=CARTESIAN_POINT('Ctrl Pts',(-2.69107233906138,-18.3676235835986,
88.8489244327543));
#107619=CARTESIAN_POINT('Ctrl Pts',(-2.68747515275225,-18.3769312270556,
88.8696919758207));
#107620=CARTESIAN_POINT('Ctrl Pts',(-2.68378046657837,-18.3857475041723,
88.890645582348));
#107621=CARTESIAN_POINT('Ctrl Pts',(-2.68068893666533,-18.3931245270492,
88.9081785197387));
#107622=CARTESIAN_POINT('Ctrl Pts',(-2.67751265990192,-18.4001570894256,
88.9258375172323));
#107623=CARTESIAN_POINT('Ctrl Pts',(-2.67432824416882,-18.406841537776,
88.9436260880443));
#107624=CARTESIAN_POINT('Ctrl Pts',(-2.67115577032227,-18.4135009187574,
88.961347949886));
#107625=CARTESIAN_POINT('Ctrl Pts',(-2.66797525212034,-18.4198147923675,
88.9791984837008));
#107626=CARTESIAN_POINT('Ctrl Pts',(-2.66481204782588,-18.4257790286698,
88.9971705585405));
#107627=CARTESIAN_POINT('Ctrl Pts',(-2.66165739729203,-18.4317271368171,
89.0150940342978));
#107628=CARTESIAN_POINT('Ctrl Pts',(-2.65851995839964,-18.4373274958245,
89.0331385181964));
#107629=CARTESIAN_POINT('Ctrl Pts',(-2.65537445049633,-18.4425754901149,
89.0512850061412));
#107630=CARTESIAN_POINT('Ctrl Pts',(-2.65256394272583,-18.4472645671053,
89.0674988726912));
#107631=CARTESIAN_POINT('Ctrl Pts',(-2.64974628004101,-18.4516723293873,
89.0837941498156));
#107632=CARTESIAN_POINT('Ctrl Pts',(-2.64686962412422,-18.455795140746,
89.100147404768));
#107633=CARTESIAN_POINT('Ctrl Pts',(-2.64475583480513,-18.458824614853,
89.1121639047076));
#107634=CARTESIAN_POINT('Ctrl Pts',(-2.64259558971588,-18.4616999411796,
89.124207642478));
#107635=CARTESIAN_POINT('Ctrl Pts',(-2.64044693112396,-18.4644212918646,
89.1362892360171));
#107636=CARTESIAN_POINT('Ctrl Pts',(-2.63829611592801,-18.4671453739635,
89.1483829558259));
#107637=CARTESIAN_POINT('Ctrl Pts',(-2.63615687923395,-18.4697151704312,
89.1605147188521));
#107638=CARTESIAN_POINT('Ctrl Pts',(-2.63403658004556,-18.4721299785418,
89.1726830821413));
#107639=CARTESIAN_POINT('Ctrl Pts',(-2.63190762092946,-18.4745546494416,
89.1849011446178));
#107640=CARTESIAN_POINT('Ctrl Pts',(-2.6297976686,-18.4768230613495,89.1971563476236));
#107641=CARTESIAN_POINT('Ctrl Pts',(-2.62766371298307,-18.4789336396701,
89.2094325039168));
#107642=CARTESIAN_POINT('Ctrl Pts',(-2.62709742376013,-18.4794937252444,
89.2126902356863));
#107643=CARTESIAN_POINT('Ctrl Pts',(-2.62652917481738,-18.4800426913482,
89.2159493503241));
#107644=CARTESIAN_POINT('Ctrl Pts',(-2.62595758703253,-18.480580498822,
89.2192093291882));
#107645=CARTESIAN_POINT('Ctrl Pts',(-2.62462385353926,-18.4818354098958,
89.2268161100078));
#107646=CARTESIAN_POINT('Ctrl Pts',(-2.62318817961284,-18.4830281746304,
89.2344037695635));
#107647=CARTESIAN_POINT('Ctrl Pts',(-2.6217508037341,-18.4841603604451,
89.2419984347316));
#107648=CARTESIAN_POINT('Ctrl Pts',(-2.62026232970538,-18.4853327950224,
89.2498630872742));
#107649=CARTESIAN_POINT('Ctrl Pts',(-2.61877225546264,-18.4864402702817,
89.2577354084537));
#107650=CARTESIAN_POINT('Ctrl Pts',(-2.61733491242798,-18.4874835549421,
89.2656311638377));
#107651=CARTESIAN_POINT('Ctrl Pts',(-2.61591966620904,-18.4885108007945,
89.273405534801));
#107652=CARTESIAN_POINT('Ctrl Pts',(-2.61455522039739,-18.4894758080587,
89.2812026800263));
#107653=CARTESIAN_POINT('Ctrl Pts',(-2.61324055925401,-18.4903784200692,
89.2890238126748));
#107654=CARTESIAN_POINT('Ctrl Pts',(-2.61189237703854,-18.4913040467724,
89.2970443676251));
#107655=CARTESIAN_POINT('Ctrl Pts',(-2.61059639061934,-18.492164050674,
89.3050905346638));
#107656=CARTESIAN_POINT('Ctrl Pts',(-2.60929846758452,-18.4929573944076,
89.3131456952514));
#107657=CARTESIAN_POINT('Ctrl Pts',(-2.60800580401295,-18.4937475233419,
89.3211682145961));
#107658=CARTESIAN_POINT('Ctrl Pts',(-2.60671047140018,-18.4944715129502,
89.3292003116569));
#107659=CARTESIAN_POINT('Ctrl Pts',(-2.6053141106307,-18.4951276644591,
89.3372003634645));
#107660=CARTESIAN_POINT('Ctrl Pts',(-2.60359036706128,-18.495937653517,
89.3470760618941));
#107661=CARTESIAN_POINT('Ctrl Pts',(-2.60208835986755,-18.4966913730579,
89.3576070931148));
#107662=CARTESIAN_POINT('Ctrl Pts',(-2.60052610129894,-18.4973293747359,
89.3681774744119));
#107663=CARTESIAN_POINT('Ctrl Pts',(-2.59959542101573,-18.4977094498363,
89.3744745405039));
#107664=CARTESIAN_POINT('Ctrl Pts',(-2.5986409882585,-18.4980492903023,
89.3807838546492));
#107665=CARTESIAN_POINT('Ctrl Pts',(-2.59762776174937,-18.4983445857785,
89.386984983822));
#107666=CARTESIAN_POINT('Ctrl Pts',(-2.5967439113196,-18.4986021757953,
89.3923943080305));
#107667=CARTESIAN_POINT('Ctrl Pts',(-2.59581530167916,-18.4988259903366,
89.3977200824184));
#107668=CARTESIAN_POINT('Ctrl Pts',(-2.59485026613534,-18.4990170956462,
89.4029081198794));
#107669=CARTESIAN_POINT('Ctrl Pts',(-2.59397531173422,-18.4991903622505,
89.4076118805221));
#107670=CARTESIAN_POINT('Ctrl Pts',(-2.59307121798518,-18.4993368371467,
89.4122014131159));
#107671=CARTESIAN_POINT('Ctrl Pts',(-2.59216621619928,-18.4994593854841,
89.4166740656765));
#107672=CARTESIAN_POINT('Ctrl Pts',(-2.5913496748404,-18.4995699551951,
89.4207095337347));
#107673=CARTESIAN_POINT('Ctrl Pts',(-2.59053363947096,-18.4996611364727,
89.4246494796461));
#107674=CARTESIAN_POINT('Ctrl Pts',(-2.58974341667261,-18.4997355651259,
89.4285331822771));
#107675=CARTESIAN_POINT('Ctrl Pts',(-2.58900398229582,-18.4998052101739,
89.4321672753968));
#107676=CARTESIAN_POINT('Ctrl Pts',(-2.58828859201009,-18.4998602719844,
89.4357520928298));
#107677=CARTESIAN_POINT('Ctrl Pts',(-2.58760355029172,-18.49990220908,89.4393608615583));
#107678=CARTESIAN_POINT('Ctrl Pts',(-2.58698361203457,-18.4999401606517,
89.4426266682034));
#107679=CARTESIAN_POINT('Ctrl Pts',(-2.58638959666555,-18.4999674238679,
89.4459127838703));
#107680=CARTESIAN_POINT('Ctrl Pts',(-2.58579704771983,-18.4999835144342,
89.4493030087189));
#107681=CARTESIAN_POINT('Ctrl Pts',(-2.5854174500935,-18.4999938223434,
89.4514748483864));
#107682=CARTESIAN_POINT('Ctrl Pts',(-2.58503785322051,-18.4999995129327,
89.4536900404362));
#107683=CARTESIAN_POINT('Ctrl Pts',(-2.58464131998469,-18.4999998848776,
89.455975322342));
#107684=CARTESIAN_POINT('Ctrl Pts',(-2.844826582731,-17.,87.9789588497187));
#107685=CARTESIAN_POINT('Ctrl Pts',(-2.90394614502961,-17.0023824172101,
87.9893948784988));
#107686=CARTESIAN_POINT('Ctrl Pts',(-2.96243772530833,-17.0047618946116,
88.0033899799603));
#107687=CARTESIAN_POINT('Ctrl Pts',(-3.01987982764382,-17.0071215359131,
88.0208434221831));
#107688=CARTESIAN_POINT('Ctrl Pts',(-3.07731807936984,-17.009481019037,
88.038295694421));
#107689=CARTESIAN_POINT('Ctrl Pts',(-3.1337065942239,-17.0118206522327,
88.0592057220766));
#107690=CARTESIAN_POINT('Ctrl Pts',(-3.18863907715103,-17.0141237898126,
88.0834229295207));
#107691=CARTESIAN_POINT('Ctrl Pts',(-3.24358165494329,-17.016427350637,
88.107644587327));
#107692=CARTESIAN_POINT('Ctrl Pts',(-3.2970672824039,-17.0186943862732,
88.1351744735706));
#107693=CARTESIAN_POINT('Ctrl Pts',(-3.34871044104395,-17.0209087342735,
88.1658142097659));
#107694=CARTESIAN_POINT('Ctrl Pts',(-3.40034592654931,-17.0231227532662,
88.1964493935126));
#107695=CARTESIAN_POINT('Ctrl Pts',(-3.45013913187528,-17.0252840847486,
88.2301932888778));
#107696=CARTESIAN_POINT('Ctrl Pts',(-3.49773127128024,-17.0273773035317,
88.2668027705058));
#107697=CARTESIAN_POINT('Ctrl Pts',(-3.54532853070358,-17.0294707475058,
88.303416190625));
#107698=CARTESIAN_POINT('Ctrl Pts',(-3.59072391869511,-17.0314960493733,
88.3428955594524));
#107699=CARTESIAN_POINT('Ctrl Pts',(-3.63359028942193,-17.0334387366064,
88.3849563386015));
#107700=CARTESIAN_POINT('Ctrl Pts',(-3.66571876688184,-17.0348947866971,
88.416481022682));
#107701=CARTESIAN_POINT('Ctrl Pts',(-3.69642718496859,-17.0363044461387,
88.4494549470133));
#107702=CARTESIAN_POINT('Ctrl Pts',(-3.72559111921561,-17.0376620472082,
88.4837444766152));
#107703=CARTESIAN_POINT('Ctrl Pts',(-3.76450732905361,-17.0394736233711,
88.5295002555828));
#107704=CARTESIAN_POINT('Ctrl Pts',(-3.80067189167083,-17.0411925807839,
88.5775997590202));
#107705=CARTESIAN_POINT('Ctrl Pts',(-3.83382415408655,-17.0428068444602,
88.6276963281322));
#107706=CARTESIAN_POINT('Ctrl Pts',(-3.86697445142636,-17.0444210124521,
88.677789927807));
#107707=CARTESIAN_POINT('Ctrl Pts',(-3.89711257570302,-17.045930487707,
88.7298800079881));
#107708=CARTESIAN_POINT('Ctrl Pts',(-3.92402133297399,-17.0473246982119,
88.7835911939316));
#107709=CARTESIAN_POINT('Ctrl Pts',(-3.950935205338,-17.0487191737428,88.8373125898491));
#107710=CARTESIAN_POINT('Ctrl Pts',(-3.97461829425342,-17.0499983307383,
88.8926553351392));
#107711=CARTESIAN_POINT('Ctrl Pts',(-3.9948998575191,-17.0511532531476,
88.9492204643416));
#107712=CARTESIAN_POINT('Ctrl Pts',(-4.01517844818267,-17.0523080062837,
89.0057773029788));
#107713=CARTESIAN_POINT('Ctrl Pts',(-4.03205637045371,-17.0533385530554,
89.0635557736215));
#107714=CARTESIAN_POINT('Ctrl Pts',(-4.04541197564839,-17.0542377788039,
89.1221394736184));
#107715=CARTESIAN_POINT('Ctrl Pts',(-4.05876899438231,-17.0551370997252,
89.1807293740352));
#107716=CARTESIAN_POINT('Ctrl Pts',(-4.06860285666184,-17.05590506534,89.2401242671352));
#107717=CARTESIAN_POINT('Ctrl Pts',(-4.07484266374113,-17.0565364670105,
89.2998960105598));
#107718=CARTESIAN_POINT('Ctrl Pts',(-4.07951153127009,-17.0570089064177,
89.3446195650669));
#107719=CARTESIAN_POINT('Ctrl Pts',(-4.08216927023329,-17.057404927918,
89.3895538271932));
#107720=CARTESIAN_POINT('Ctrl Pts',(-4.0828051389793,-17.0577230769003,
89.4345172825691));
#107721=CARTESIAN_POINT('Ctrl Pts',(-4.08365488216529,-17.0581482352863,
89.4946041952602));
#107722=CARTESIAN_POINT('Ctrl Pts',(-4.08089198932617,-17.0584343992759,
89.5547429724985));
#107723=CARTESIAN_POINT('Ctrl Pts',(-4.0745363644185,-17.058579722477,89.6145001884501));
#107724=CARTESIAN_POINT('Ctrl Pts',(-4.06818111413334,-17.0587250371122,
89.6742538821047));
#107725=CARTESIAN_POINT('Ctrl Pts',(-4.05823359998992,-17.0587295264416,
89.7336256442276));
#107726=CARTESIAN_POINT('Ctrl Pts',(-4.04476549631919,-17.0585934095053,
89.7921876271694));
#107727=CARTESIAN_POINT('Ctrl Pts',(-4.03129482724969,-17.0584572666415,
89.8507607649733));
#107728=CARTESIAN_POINT('Ctrl Pts',(-4.01430231938096,-17.0581804647287,
89.9085234074744));
#107729=CARTESIAN_POINT('Ctrl Pts',(-3.99391045981778,-17.0577652915182,
89.9650591443483));
#107730=CARTESIAN_POINT('Ctrl Pts',(-3.97352158583064,-17.0573501790932,
90.0215866038142));
#107731=CARTESIAN_POINT('Ctrl Pts',(-3.94973449841905,-17.056796738769,
90.0768871243478));
#107732=CARTESIAN_POINT('Ctrl Pts',(-3.92272061459661,-17.0561092973433,
90.1305621612801));
#107733=CARTESIAN_POINT('Ctrl Pts',(-3.89570386870406,-17.0554217830845,
90.1842428849814));
#107734=CARTESIAN_POINT('Ctrl Pts',(-3.86545982963037,-17.0546002440683,
90.2362974070196));
#107735=CARTESIAN_POINT('Ctrl Pts',(-3.83220649265228,-17.0536509920008,
90.2863504965781));
#107736=CARTESIAN_POINT('Ctrl Pts',(-3.80732503994394,-17.0529407243233,
90.3238021839554));
#107737=CARTESIAN_POINT('Ctrl Pts',(-3.78075977716049,-17.052158996523,
90.3601337988618));
#107738=CARTESIAN_POINT('Ctrl Pts',(-3.75261800855695,-17.0513091504894,
90.3951985771812));
#107739=CARTESIAN_POINT('Ctrl Pts',(-3.7150919602065,-17.0501759110048,
90.4419562129626));
#107740=CARTESIAN_POINT('Ctrl Pts',(-3.6747602537301,-17.0489215300774,
90.4864612103411));
#107741=CARTESIAN_POINT('Ctrl Pts',(-3.63191259383891,-17.0475550414524,
90.5283931856407));
#107742=CARTESIAN_POINT('Ctrl Pts',(-3.58906842455738,-17.0461886641492,
90.5703217449275));
#107743=CARTESIAN_POINT('Ctrl Pts',(-3.54370901311723,-17.044710207171,
90.6096774060446));
#107744=CARTESIAN_POINT('Ctrl Pts',(-3.49616044245401,-17.0431303861969,
90.6461770584101));
#107745=CARTESIAN_POINT('Ctrl Pts',(-3.44860185021139,-17.0415502322517,
90.6826844036286));
#107746=CARTESIAN_POINT('Ctrl Pts',(-3.39885350965945,-17.0398686828611,
90.7163342776236));
#107747=CARTESIAN_POINT('Ctrl Pts',(-3.34727340964406,-17.0380979875471,
90.7468847632878));
#107748=CARTESIAN_POINT('Ctrl Pts',(-3.29569951794632,-17.0363275053587,
90.7774315718144));
#107749=CARTESIAN_POINT('Ctrl Pts',(-3.24229467194259,-17.0344679114925,
90.8048795248662));
#107750=CARTESIAN_POINT('Ctrl Pts',(-3.187443176895,-17.0325327967545,90.8290316882564));
#107751=CARTESIAN_POINT('Ctrl Pts',(-3.13258096101438,-17.0305973037944,
90.8531885722347));
#107752=CARTESIAN_POINT('Ctrl Pts',(-3.07627191706294,-17.0285862743993,
90.8740482084431));
#107753=CARTESIAN_POINT('Ctrl Pts',(-3.01892139861794,-17.026514452939,
90.8914613410692));
#107754=CARTESIAN_POINT('Ctrl Pts',(-2.97530773108157,-17.0249388833572,
90.9047036028257));
#107755=CARTESIAN_POINT('Ctrl Pts',(-2.93109222531984,-17.0233281814062,
90.9159536361465));
#107756=CARTESIAN_POINT('Ctrl Pts',(-2.88645908594721,-17.0216891971845,
90.9251650919679));
#107757=CARTESIAN_POINT('Origin',(17.1910233941991,-17.,85.96920230149));
#107758=CARTESIAN_POINT('',(9.44018183429909,-17.,85.81274487387));
#107759=CARTESIAN_POINT('',(16.4933237498291,-18.49999999514,86.09223866229));
#107760=CARTESIAN_POINT('Origin',(157.369850611169,-18.5,67.852165916321));
#107761=CARTESIAN_POINT('Ctrl Pts',(4.96802222338909,-18.49999999899,91.37511854801));
#107762=CARTESIAN_POINT('Ctrl Pts',(5.22543100101909,-18.49999999899,91.40426861974));
#107763=CARTESIAN_POINT('Ctrl Pts',(5.75020154047909,-18.50000000047,91.46158478716));
#107764=CARTESIAN_POINT('Ctrl Pts',(6.50334881420368,-18.4999999999262,
91.5330830665222));
#107765=CARTESIAN_POINT('Ctrl Pts',(6.98169776546952,-18.4999999999567,
91.5705426281902));
#107766=CARTESIAN_POINT('Ctrl Pts',(7.18082331871055,-18.4999999999755,
91.584556528483));
#107767=CARTESIAN_POINT('Ctrl Pts',(4.67429866745909,-17.81329231081,92.6102332020699));
#107768=CARTESIAN_POINT('Ctrl Pts',(4.92175734799909,-17.81329231081,92.6386607895801));
#107769=CARTESIAN_POINT('Ctrl Pts',(5.44974328288909,-17.81329231081,92.69732199839));
#107770=CARTESIAN_POINT('Ctrl Pts',(6.26767800558908,-17.81329231081,92.77811241642));
#107771=CARTESIAN_POINT('Ctrl Pts',(7.12392866528909,-17.81329231081,92.8472667652099));
#107772=CARTESIAN_POINT('Ctrl Pts',(7.97259535655909,-17.81329231081,92.89672929314));
#107773=CARTESIAN_POINT('Ctrl Pts',(8.78502947769909,-17.81329231081,92.92332784864));
#107774=CARTESIAN_POINT('Ctrl Pts',(9.5332741592491,-17.81329231081,92.9279180420902));
#107775=CARTESIAN_POINT('Ctrl Pts',(10.2041285991891,-17.81329231081,92.9146854325099));
#107776=CARTESIAN_POINT('Ctrl Pts',(10.8004329265091,-17.81329231081,92.8886586089702));
#107777=CARTESIAN_POINT('Ctrl Pts',(11.3349840960491,-17.81329231081,92.8534030050999));
#107778=CARTESIAN_POINT('Ctrl Pts',(11.8178226086691,-17.81329231081,92.8116449801501));
#107779=CARTESIAN_POINT('Ctrl Pts',(12.2554929002391,-17.81329231081,92.7654341535601));
#107780=CARTESIAN_POINT('Ctrl Pts',(12.6533731109991,-17.81329231081,92.71641060703));
#107781=CARTESIAN_POINT('Ctrl Pts',(13.0164525305191,-17.81329231081,92.6657791293399));
#107782=CARTESIAN_POINT('Ctrl Pts',(13.3492734982491,-17.81329231081,92.61435605809));
#107783=CARTESIAN_POINT('Ctrl Pts',(13.6561665865191,-17.81329231081,92.56262780457));
#107784=CARTESIAN_POINT('Ctrl Pts',(13.9403800542091,-17.81329231081,92.51100282361));
#107785=CARTESIAN_POINT('Ctrl Pts',(14.2033497191691,-17.81329231081,92.46001789955));
#107786=CARTESIAN_POINT('Ctrl Pts',(14.4452961696591,-17.81329231081,92.41035496115));
#107787=CARTESIAN_POINT('Ctrl Pts',(14.6666699797891,-17.81329231081,92.36258963016));
#107788=CARTESIAN_POINT('Ctrl Pts',(14.8689728993491,-17.81329231081,92.31698073567));
#107789=CARTESIAN_POINT('Ctrl Pts',(15.0542645826791,-17.81329231081,92.2735532422199));
#107790=CARTESIAN_POINT('Ctrl Pts',(15.2253800918591,-17.81329231082,92.2320415865899));
#107791=CARTESIAN_POINT('Ctrl Pts',(15.3859455327891,-17.81329231077,92.1918578513101));
#107792=CARTESIAN_POINT('Ctrl Pts',(15.5409358917991,-17.81329231096,92.1519372765301));
#107793=CARTESIAN_POINT('Ctrl Pts',(15.6976425511091,-17.81329231023,92.1104475421901));
#107794=CARTESIAN_POINT('Ctrl Pts',(15.8618783881191,-17.81329231324,92.06573309792));
#107795=CARTESIAN_POINT('Ctrl Pts',(16.0323492246791,-17.81329230114,92.0179448915599));
#107796=CARTESIAN_POINT('Ctrl Pts',(16.1990043638691,-17.81329234446,91.96984383322));
#107797=CARTESIAN_POINT('Ctrl Pts',(16.3585633685591,-17.81329220026,91.9225113535201));
#107798=CARTESIAN_POINT('Ctrl Pts',(16.4564706533791,-17.81318796283,91.8929129181599));
#107799=CARTESIAN_POINT('Ctrl Pts',(16.5032491374491,-17.81308325173,91.8786745656599));
#107800=CARTESIAN_POINT('Ctrl Pts',(4.71381130773909,-18.34983158812,92.26627944992));
#107801=CARTESIAN_POINT('Ctrl Pts',(4.96040944056908,-18.34983158812,92.29460814837));
#107802=CARTESIAN_POINT('Ctrl Pts',(5.48608879843909,-18.34983158812,92.35301088002));
#107803=CARTESIAN_POINT('Ctrl Pts',(6.29888635805909,-18.34983158812,92.43328754518));
#107804=CARTESIAN_POINT('Ctrl Pts',(7.14817026536909,-18.34983158812,92.50187169504));
#107805=CARTESIAN_POINT('Ctrl Pts',(7.98856602530908,-18.34983158812,92.55084458026));
#107806=CARTESIAN_POINT('Ctrl Pts',(8.79196326731908,-18.34983158812,92.5771400222));
#107807=CARTESIAN_POINT('Ctrl Pts',(9.53108736363908,-18.34983158812,92.5816705939));
#107808=CARTESIAN_POINT('Ctrl Pts',(10.1933161338291,-18.34983158812,92.5686051930199));
#107809=CARTESIAN_POINT('Ctrl Pts',(10.7815791528391,-18.34983158812,92.54292787439));
#107810=CARTESIAN_POINT('Ctrl Pts',(11.3087547861991,-18.34983158812,92.50815797892));
#107811=CARTESIAN_POINT('Ctrl Pts',(11.7848039744491,-18.34983158812,92.46698641252));
#107812=CARTESIAN_POINT('Ctrl Pts',(12.2161926086191,-18.34983158812,92.42143843311));
#107813=CARTESIAN_POINT('Ctrl Pts',(12.6083398427691,-18.34983158812,92.37312122294));
#107814=CARTESIAN_POINT('Ctrl Pts',(12.9661518810891,-18.34983158812,92.32322406105));
#107815=CARTESIAN_POINT('Ctrl Pts',(13.2940991431591,-18.34983158812,92.27255390755));
#107816=CARTESIAN_POINT('Ctrl Pts',(13.5964793927291,-18.34983158812,92.22158628161));
#107817=CARTESIAN_POINT('Ctrl Pts',(13.8765160809191,-18.34983158812,92.17071999012));
#107818=CARTESIAN_POINT('Ctrl Pts',(14.1356179414191,-18.34983158812,92.12048494285));
#107819=CARTESIAN_POINT('Ctrl Pts',(14.3740019301191,-18.34983158812,92.07155324491));
#107820=CARTESIAN_POINT('Ctrl Pts',(14.5921111933091,-18.34983158812,92.02449226612));
#107821=CARTESIAN_POINT('Ctrl Pts',(14.7914186857591,-18.34983158812,91.9795586751801));
#107822=CARTESIAN_POINT('Ctrl Pts',(14.9739675871691,-18.34983158811,91.93677402423));
#107823=CARTESIAN_POINT('Ctrl Pts',(15.1425533262591,-18.34983158813,91.89587608238));
#107824=CARTESIAN_POINT('Ctrl Pts',(15.3007471565291,-18.34983158809,91.85628587938));
#107825=CARTESIAN_POINT('Ctrl Pts',(15.4534503714491,-18.34983158823,91.81695440386));
#107826=CARTESIAN_POINT('Ctrl Pts',(15.6078464560491,-18.34983158769,91.776076421));
#107827=CARTESIAN_POINT('Ctrl Pts',(15.7696623981791,-18.34983158988,91.73202081673));
#107828=CARTESIAN_POINT('Ctrl Pts',(15.9376211881691,-18.3498315811,91.6849367963501));
#107829=CARTESIAN_POINT('Ctrl Pts',(16.1018113089291,-18.34983161252,91.63754721276));
#107830=CARTESIAN_POINT('Ctrl Pts',(16.2588839577391,-18.34983150793,91.5909515159));
#107831=CARTESIAN_POINT('Ctrl Pts',(16.3563226329691,-18.34975599539,91.56154888587));
#107832=CARTESIAN_POINT('Ctrl Pts',(16.4034488759691,-18.34968013935,91.54726170511));
#107833=CARTESIAN_POINT('Ctrl Pts',(4.78098568915909,-18.59741772268,91.68153288839));
#107834=CARTESIAN_POINT('Ctrl Pts',(5.02612082787908,-18.59741772268,91.7096934681901));
#107835=CARTESIAN_POINT('Ctrl Pts',(5.54787883593908,-18.59741772268,91.76765676975));
#107836=CARTESIAN_POINT('Ctrl Pts',(6.35194284219909,-18.59741772268,91.84706001742));
#107837=CARTESIAN_POINT('Ctrl Pts',(7.18938276036909,-18.59741772268,91.91467478736));
#107838=CARTESIAN_POINT('Ctrl Pts',(8.01571733149909,-18.59741772268,91.9628152441));
#107839=CARTESIAN_POINT('Ctrl Pts',(8.80375121733909,-18.59741772268,91.98859537081));
#107840=CARTESIAN_POINT('Ctrl Pts',(9.52736965098908,-18.59741772268,91.99302458115));
#107841=CARTESIAN_POINT('Ctrl Pts',(10.1749341510891,-18.59741772268,91.98024344731));
#107842=CARTESIAN_POINT('Ctrl Pts',(10.7495263572191,-18.59741772268,91.95516031264));
#107843=CARTESIAN_POINT('Ctrl Pts',(11.2641630390591,-18.59741772268,91.921216157));
#107844=CARTESIAN_POINT('Ctrl Pts',(11.7286698787791,-18.59741772268,91.88104161308));
#107845=CARTESIAN_POINT('Ctrl Pts',(12.1493792354491,-18.59741772268,91.83662052239));
#107846=CARTESIAN_POINT('Ctrl Pts',(12.5317799896291,-18.59741772268,91.78950413574));
#107847=CARTESIAN_POINT('Ctrl Pts',(12.8806370942491,-18.59741772268,91.74085536449));
#107848=CARTESIAN_POINT('Ctrl Pts',(13.2002986998791,-18.59741772268,91.69146522629));
#107849=CARTESIAN_POINT('Ctrl Pts',(13.4950067932391,-18.59741772268,91.64179072293));
#107850=CARTESIAN_POINT('Ctrl Pts',(13.7679426504591,-18.59741772268,91.59221425908));
#107851=CARTESIAN_POINT('Ctrl Pts',(14.0204689601991,-18.59741772268,91.54325405724));
#107852=CARTESIAN_POINT('Ctrl Pts',(14.2527965030291,-18.59741772268,91.49556552163));
#107853=CARTESIAN_POINT('Ctrl Pts',(14.4653557974191,-18.59741772268,91.44970199315));
#107854=CARTESIAN_POINT('Ctrl Pts',(14.6595708444491,-18.59741772268,91.40591646769));
#107855=CARTESIAN_POINT('Ctrl Pts',(14.8374568157691,-18.59741772268,91.36422469606));
#107856=CARTESIAN_POINT('Ctrl Pts',(15.0017417605091,-18.59741772268,91.32437011257));
#107857=CARTESIAN_POINT('Ctrl Pts',(15.1559036790191,-18.59741772267,91.28578895791));
#107858=CARTESIAN_POINT('Ctrl Pts',(15.3047185815191,-18.59741772272,91.24745899426));
#107859=CARTESIAN_POINT('Ctrl Pts',(15.4551865199491,-18.59741772253,91.2076210337));
#107860=CARTESIAN_POINT('Ctrl Pts',(15.6128884636191,-18.5974177233,91.16468550567));
#107861=CARTESIAN_POINT('Ctrl Pts',(15.7765765905091,-18.59741772018,91.11879865301));
#107862=CARTESIAN_POINT('Ctrl Pts',(15.9365759994591,-18.59741773137,91.0726186286001));
#107863=CARTESIAN_POINT('Ctrl Pts',(16.0894216612391,-18.59741769412,91.0272755165199));
#107864=CARTESIAN_POINT('Ctrl Pts',(16.1860844388491,-18.59739084079,90.99814207378));
#107865=CARTESIAN_POINT('Ctrl Pts',(16.2338226818491,-18.59736386515,90.98370815039));
#107866=CARTESIAN_POINT('Ctrl Pts',(4.85238799116909,-18.46968015288,91.05998268273));
#107867=CARTESIAN_POINT('Ctrl Pts',(5.09596805569909,-18.46968015288,91.08796456258));
#107868=CARTESIAN_POINT('Ctrl Pts',(5.6135579062291,-18.46968015288,91.1454607765601));
#107869=CARTESIAN_POINT('Ctrl Pts',(6.40833867382909,-18.46968015288,91.22393563429));
#107870=CARTESIAN_POINT('Ctrl Pts',(7.2331891483591,-18.46968015288,91.2905200120401));
#107871=CARTESIAN_POINT('Ctrl Pts',(8.04457752675909,-18.46968015288,91.3377756476999));
#107872=CARTESIAN_POINT('Ctrl Pts',(8.81628109478909,-18.46968015288,91.3630080254999));
#107873=CARTESIAN_POINT('Ctrl Pts',(9.52341794744909,-18.46968015288,91.36732949485));
#107874=CARTESIAN_POINT('Ctrl Pts',(10.1553952159191,-18.46968015288,91.3548505196701));
#107875=CARTESIAN_POINT('Ctrl Pts',(10.7154561753291,-18.46968015288,91.33039896658));
#107876=CARTESIAN_POINT('Ctrl Pts',(11.2167647105691,-18.46968015288,91.2973325223999));
#107877=CARTESIAN_POINT('Ctrl Pts',(11.6690027323691,-18.46968015288,91.2582177530301));
#107878=CARTESIAN_POINT('Ctrl Pts',(12.0783606633591,-18.46968015288,91.21499447685));
#107879=CARTESIAN_POINT('Ctrl Pts',(12.4504014991991,-18.46968015288,91.16915449294));
#107880=CARTESIAN_POINT('Ctrl Pts',(12.7897400512391,-18.46968015288,91.12183268539));
#107881=CARTESIAN_POINT('Ctrl Pts',(13.1005945055291,-18.46968015288,91.0738031259901));
#107882=CARTESIAN_POINT('Ctrl Pts',(13.3871475611691,-18.46968015288,91.02550313366));
#107883=CARTESIAN_POINT('Ctrl Pts',(13.6525356648191,-18.46968015288,90.97729767853));
#107884=CARTESIAN_POINT('Ctrl Pts',(13.8980725620591,-18.46968015288,90.92969256024));
#107885=CARTESIAN_POINT('Ctrl Pts',(14.1239624694591,-18.46968015288,90.88332543094));
#107886=CARTESIAN_POINT('Ctrl Pts',(14.3306224828991,-18.46968015288,90.83873471968));
#107887=CARTESIAN_POINT('Ctrl Pts',(14.5194245686591,-18.46968015288,90.79616951834));
#107888=CARTESIAN_POINT('Ctrl Pts',(14.6923541275091,-18.46968015288,90.75563941128));
#107889=CARTESIAN_POINT('Ctrl Pts',(14.8520675881291,-18.46968015288,90.71689385458));
#107890=CARTESIAN_POINT('Ctrl Pts',(15.0019438284491,-18.46968015289,90.6793852572301));
#107891=CARTESIAN_POINT('Ctrl Pts',(15.1466256901691,-18.46968015285,90.6421198401));
#107892=CARTESIAN_POINT('Ctrl Pts',(15.2929182469491,-18.46968015302,90.6033873603001));
#107893=CARTESIAN_POINT('Ctrl Pts',(15.4462472592391,-18.4696801523,90.56164240552));
#107894=CARTESIAN_POINT('Ctrl Pts',(15.6053959297191,-18.46968015519,90.5170280697));
#107895=CARTESIAN_POINT('Ctrl Pts',(15.7609408656491,-18.46968014487,90.47213373348));
#107896=CARTESIAN_POINT('Ctrl Pts',(15.9092934960191,-18.4696801792,90.42812204322));
#107897=CARTESIAN_POINT('Ctrl Pts',(16.0051437602991,-18.46970494463,90.39923726359));
#107898=CARTESIAN_POINT('Ctrl Pts',(16.0535447478491,-18.46972982279,90.38460987447));
#107899=CARTESIAN_POINT('Ctrl Pts',(4.84743272606783,-18.0489462436203,
92.4406303885482));
#107900=CARTESIAN_POINT('Ctrl Pts',(5.03040185937532,-18.0650463395508,
92.4454996674276));
#107901=CARTESIAN_POINT('Ctrl Pts',(5.2085737446796,-18.0803746691731,92.4493084336499));
#107902=CARTESIAN_POINT('Ctrl Pts',(5.38188039330711,-18.0949545072779,
92.4520603727252));
#107903=CARTESIAN_POINT('Ctrl Pts',(5.4026891322958,-18.0967050924287,92.452390795028));
#107904=CARTESIAN_POINT('Ctrl Pts',(5.42342773905644,-18.0984448968291,
92.4527060415585));
#107905=CARTESIAN_POINT('Ctrl Pts',(5.44409610243779,-18.1001739686197,
92.4530061664326));
#107906=CARTESIAN_POINT('Ctrl Pts',(5.62803093192004,-18.1155615694235,
92.4556770802594));
#107907=CARTESIAN_POINT('Ctrl Pts',(5.80640080237462,-18.1300984623534,
92.4571460825411));
#107908=CARTESIAN_POINT('Ctrl Pts',(5.97911713546014,-18.1438235369843,
92.4574880960229));
#107909=CARTESIAN_POINT('Ctrl Pts',(6.08580373840904,-18.1523014936513,
92.4576993572041));
#107910=CARTESIAN_POINT('Ctrl Pts',(6.19033366455821,-18.1604698783647,
92.4574816912358));
#107911=CARTESIAN_POINT('Ctrl Pts',(6.29268999604011,-18.1683392495622,
92.4568615559032));
#107912=CARTESIAN_POINT('Ctrl Pts',(6.44065786997315,-18.1797153325893,
92.4559650788082));
#107913=CARTESIAN_POINT('Ctrl Pts',(6.58408260085334,-18.1904664472246,
92.4542269470687));
#107914=CARTESIAN_POINT('Ctrl Pts',(6.72291626644099,-18.2006273153123,
92.4517518039631));
#107915=CARTESIAN_POINT('Ctrl Pts',(20.3703076195591,-17.48636025246,80.6160118299));
#107916=CARTESIAN_POINT('Ctrl Pts',(20.1881103583291,-17.59469264276,81.383197007755));
#107917=CARTESIAN_POINT('Ctrl Pts',(19.7633142133291,-17.81559800981,82.9726719728399));
#107918=CARTESIAN_POINT('Ctrl Pts',(19.0018167096191,-18.10372872761,85.2475673257499));
#107919=CARTESIAN_POINT('Ctrl Pts',(18.1317679720991,-18.32477803286,87.36843783982));
#107920=CARTESIAN_POINT('Ctrl Pts',(17.2370610827991,-18.45951303147,89.2032198305499));
#107921=CARTESIAN_POINT('Ctrl Pts',(16.3494952333791,-18.51446227549,90.7700178089799));
#107922=CARTESIAN_POINT('Ctrl Pts',(15.4867758268391,-18.50123398135,92.10529605495));
#107923=CARTESIAN_POINT('Ctrl Pts',(14.6453959780491,-18.43037008788,93.26267617499));
#107924=CARTESIAN_POINT('Ctrl Pts',(13.8009845953991,-18.30490819777,94.3025568640399));
#107925=CARTESIAN_POINT('Ctrl Pts',(12.9307100320291,-18.12021817286,95.2628709280001));
#107926=CARTESIAN_POINT('Ctrl Pts',(12.0275979803391,-17.86955305763,96.15310194351));
#107927=CARTESIAN_POINT('Ctrl Pts',(11.1010176724691,-17.54986176095,96.96608256951));
#107928=CARTESIAN_POINT('Ctrl Pts',(10.1635981391591,-17.16111541643,97.6955323958101));
#107929=CARTESIAN_POINT('Ctrl Pts',(9.27968364505908,-16.73052720888,98.30286534269));
#107930=CARTESIAN_POINT('Ctrl Pts',(8.71271538374908,-16.41504543997,98.64913661867));
#107931=CARTESIAN_POINT('Ctrl Pts',(8.45819912877909,-16.26514131694,98.79644286584));
#107932=CARTESIAN_POINT('Ctrl Pts',(14.7248846521991,-18.94108804276,77.911688731006));
#107933=CARTESIAN_POINT('Ctrl Pts',(14.5694350031491,-18.93552267139,78.561742613804));
#107934=CARTESIAN_POINT('Ctrl Pts',(14.2134049487491,-18.91245218656,79.908309787637));
#107935=CARTESIAN_POINT('Ctrl Pts',(13.6004443439491,-18.832257487,81.827642780919));
#107936=CARTESIAN_POINT('Ctrl Pts',(12.9289464995691,-18.69869734538,83.60280410874));
#107937=CARTESIAN_POINT('Ctrl Pts',(12.2646619608891,-18.52485132822,85.12309497776));
#107938=CARTESIAN_POINT('Ctrl Pts',(11.6278705382591,-18.32183553005,86.4073429830001));
#107939=CARTESIAN_POINT('Ctrl Pts',(11.0263774792591,-18.09933417041,87.4904580833699));
#107940=CARTESIAN_POINT('Ctrl Pts',(10.4529512601791,-17.86094059021,88.4205103504401));
#107941=CARTESIAN_POINT('Ctrl Pts',(9.88731078157909,-17.60178133109,89.249386304));
#107942=CARTESIAN_POINT('Ctrl Pts',(9.31126387016909,-17.31409529898,90.0096973799401));
#107943=CARTESIAN_POINT('Ctrl Pts',(8.71693645522909,-16.9926399648,90.7110627126001));
#107944=CARTESIAN_POINT('Ctrl Pts',(8.10624510203909,-16.63664836235,91.35001588189));
#107945=CARTESIAN_POINT('Ctrl Pts',(7.48260991328909,-16.24618559887,91.92364883475));
#107946=CARTESIAN_POINT('Ctrl Pts',(6.88447228887909,-15.84456366131,92.40307208249));
#107947=CARTESIAN_POINT('Ctrl Pts',(6.49233429628909,-15.56370842049,92.67816808986));
#107948=CARTESIAN_POINT('Ctrl Pts',(6.31420645011909,-15.43222415467,92.79562051845));
#107949=CARTESIAN_POINT('Ctrl Pts',(12.5063401363191,-24.60762905604,75.845594438731));
#107950=CARTESIAN_POINT('Ctrl Pts',(12.2868497584891,-24.55389093248,76.4322774261809));
#107951=CARTESIAN_POINT('Ctrl Pts',(11.7948949593591,-24.42464703364,77.649532278307));
#107952=CARTESIAN_POINT('Ctrl Pts',(10.9814946228591,-24.17202064863,79.385448634424));
#107953=CARTESIAN_POINT('Ctrl Pts',(10.1222707621991,-23.85736527914,80.987352988331));
#107954=CARTESIAN_POINT('Ctrl Pts',(9.29846527963909,-23.5105055521,82.353880287081));
#107955=CARTESIAN_POINT('Ctrl Pts',(8.52998276490909,-23.14741348718,83.50305548649));
#107956=CARTESIAN_POINT('Ctrl Pts',(7.82085548590909,-22.77957706661,84.4682620618799));
#107957=CARTESIAN_POINT('Ctrl Pts',(7.15797738393909,-22.40870352106,85.2944825448601));
#107958=CARTESIAN_POINT('Ctrl Pts',(6.5147643722091,-22.02537234206,86.0295402695));
#107959=CARTESIAN_POINT('Ctrl Pts',(5.86851416204909,-21.61846160989,86.7038509520601));
#107960=CARTESIAN_POINT('Ctrl Pts',(5.20849832309909,-21.1819420503,87.32752168855));
#107961=CARTESIAN_POINT('Ctrl Pts',(4.53433886995909,-20.71577757791,87.89907590832));
#107962=CARTESIAN_POINT('Ctrl Pts',(3.84677854591909,-20.22008924508,88.41723900531));
#107963=CARTESIAN_POINT('Ctrl Pts',(3.18516755758909,-19.72283039656,88.85636793195));
#107964=CARTESIAN_POINT('Ctrl Pts',(2.74853368799909,-19.38098595465,89.11251172142));
#107965=CARTESIAN_POINT('Ctrl Pts',(2.54938093874909,-19.22185467038,89.22278927536));
#107966=CARTESIAN_POINT('Ctrl Pts',(15.3202955475791,-30.38495224307,75.913018023323));
#107967=CARTESIAN_POINT('Ctrl Pts',(14.9923241307591,-30.38363031797,76.535953769073));
#107968=CARTESIAN_POINT('Ctrl Pts',(14.2581262150091,-30.36285605286,77.831078640661));
#107969=CARTESIAN_POINT('Ctrl Pts',(13.0403732440191,-30.25848525137,79.688467729779));
#107970=CARTESIAN_POINT('Ctrl Pts',(11.7430089211191,-30.06731245317,81.414958143033));
#107971=CARTESIAN_POINT('Ctrl Pts',(10.4851888796891,-29.80822108623,82.899732333371));
#107972=CARTESIAN_POINT('Ctrl Pts',(9.29785820693909,-29.4987931119,84.15906778619));
#107973=CARTESIAN_POINT('Ctrl Pts',(8.19013397563909,-29.15474260213,85.2259540885799));
#107974=CARTESIAN_POINT('Ctrl Pts',(7.14513725765909,-28.78231819477,86.14698476448));
#107975=CARTESIAN_POINT('Ctrl Pts',(6.12414964407909,-28.37420716695,86.97330959057));
#107976=CARTESIAN_POINT('Ctrl Pts',(5.09407323602909,-27.91812922517,87.73786331633));
#107977=CARTESIAN_POINT('Ctrl Pts',(4.04143642525909,-27.40554656753,88.4512402521699));
#107978=CARTESIAN_POINT('Ctrl Pts',(2.97038542110909,-26.83507178681,89.11080249674));
#107979=CARTESIAN_POINT('Ctrl Pts',(1.88745485450909,-26.20680336296,89.71398781054));
#107980=CARTESIAN_POINT('Ctrl Pts',(0.859057681899087,-25.55851947637,90.2295998987501));
#107981=CARTESIAN_POINT('Ctrl Pts',(0.190804675379086,-25.10420966072,90.53273076058));
#107982=CARTESIAN_POINT('Ctrl Pts',(-0.111569990190912,-24.89137338738,
90.6637050372499));
#107983=CARTESIAN_POINT('Origin',(4.09260801170157,-24.6802428299903,99.1716370966873));
#107984=CARTESIAN_POINT('Ctrl Pts',(-3.41678053768791,0.170871362272414,
91.1025096700299));
#107985=CARTESIAN_POINT('Ctrl Pts',(-3.41738790502791,-0.166941914098586,
91.1026167652799));
#107986=CARTESIAN_POINT('Ctrl Pts',(-3.41552781040091,-0.908042807109186,
91.10228878041));
#107987=CARTESIAN_POINT('Ctrl Pts',(-3.39950555870891,-2.09245643556899,
91.0994636251401));
#107988=CARTESIAN_POINT('Ctrl Pts',(-3.36766182185891,-3.42224563324099,
91.09384871517));
#107989=CARTESIAN_POINT('Ctrl Pts',(-3.31682650133491,-4.87342127067699,
91.0848850765899));
#107990=CARTESIAN_POINT('Ctrl Pts',(-3.24468846482291,-6.455970844648,91.07216519442));
#107991=CARTESIAN_POINT('Ctrl Pts',(-3.14948284460091,-8.18752141444799,
91.0553778748601));
#107992=CARTESIAN_POINT('Ctrl Pts',(-3.02972032711291,-10.08904585353,91.03426051175));
#107993=CARTESIAN_POINT('Ctrl Pts',(-2.88692697078091,-12.17223757961,91.00908219036));
#107994=CARTESIAN_POINT('Ctrl Pts',(-2.72810852295691,-14.41821021101,90.98107821297));
#107995=CARTESIAN_POINT('Ctrl Pts',(-2.62472810958691,-16.1057824444,90.96284945682));
#107996=CARTESIAN_POINT('Ctrl Pts',(-2.58507228687091,-17.0405025299,90.95585706533));
#107997=CARTESIAN_POINT('Ctrl Pts',(-2.57998503310891,-17.17969442164,90.9549600452399));
#107998=CARTESIAN_POINT('Ctrl Pts',(-4.30429771344191,0.172489972228314,
91.10115797901));
#107999=CARTESIAN_POINT('Ctrl Pts',(-4.30490948529191,-0.167863353432186,
91.1012658508999));
#108000=CARTESIAN_POINT('Ctrl Pts',(-4.30303535257491,-0.915276061279186,
91.10093539073));
#108001=CARTESIAN_POINT('Ctrl Pts',(-4.28687480850291,-2.10963246135999,
91.0980858507901));
#108002=CARTESIAN_POINT('Ctrl Pts',(-4.25481409995891,-3.44832552765999,
91.09243268285));
#108003=CARTESIAN_POINT('Ctrl Pts',(-4.20362125539891,-4.90968613310399,
91.08340600314));
#108004=CARTESIAN_POINT('Ctrl Pts',(-4.13108944412291,-6.500757297294,91.07061668785));
#108005=CARTESIAN_POINT('Ctrl Pts',(-4.03543691811291,-8.24026573706799,
91.05375056674));
#108006=CARTESIAN_POINT('Ctrl Pts',(-3.91531379550691,-10.1478954092,91.0325696192201));
#108007=CARTESIAN_POINT('Ctrl Pts',(-3.77216277153791,-12.23436059257,91.00732823138));
#108008=CARTESIAN_POINT('Ctrl Pts',(-3.61391434248391,-14.4799922945,90.97942476368));
#108009=CARTESIAN_POINT('Ctrl Pts',(-3.50990930126091,-16.15377302025,90.96108586878));
#108010=CARTESIAN_POINT('Ctrl Pts',(-3.47236980401791,-17.07391474723,90.95446664258));
#108011=CARTESIAN_POINT('Ctrl Pts',(-3.46758380301991,-17.21040361506,90.95362274147));
#108012=CARTESIAN_POINT('Ctrl Pts',(-4.92692319961491,0.173422346322314,
90.4686804169501));
#108013=CARTESIAN_POINT('Ctrl Pts',(-4.92753750861191,-0.168394133661686,
90.4687887362));
#108014=CARTESIAN_POINT('Ctrl Pts',(-4.92565528948092,-0.919442660390486,
90.4684568501801));
#108015=CARTESIAN_POINT('Ctrl Pts',(-4.90941508431792,-2.11952643330099,
90.46559326384));
#108016=CARTESIAN_POINT('Ctrl Pts',(-4.87722939273791,-3.46334842915799,
90.45991805802));
#108017=CARTESIAN_POINT('Ctrl Pts',(-4.82583060223791,-4.93057592074299,
90.4508550644801));
#108018=CARTESIAN_POINT('Ctrl Pts',(-4.75307196337691,-6.52655580919599,
90.43802575337));
#108019=CARTESIAN_POINT('Ctrl Pts',(-4.65716200451291,-8.270648251298,90.4211142399));
#108020=CARTESIAN_POINT('Ctrl Pts',(-4.53683116115991,-10.18179474421,90.39989666561));
#108021=CARTESIAN_POINT('Ctrl Pts',(-4.39347410853091,-12.27014554973,90.37461894936));
#108022=CARTESIAN_POINT('Ctrl Pts',(-4.23555402957291,-14.51558086475,90.34677337864));
#108023=CARTESIAN_POINT('Ctrl Pts',(-4.13118918157491,-16.18141721551,90.3283710401));
#108024=CARTESIAN_POINT('Ctrl Pts',(-4.09486875940191,-17.09316131479,90.32196676972));
#108025=CARTESIAN_POINT('Ctrl Pts',(-4.09025629018791,-17.2280931494,90.32115346695));
#108026=CARTESIAN_POINT('Ctrl Pts',(-4.91434370485591,0.173113944903914,
89.58124990466));
#108027=CARTESIAN_POINT('Ctrl Pts',(-4.91495717464091,-0.168218567462786,
89.58135807593));
#108028=CARTESIAN_POINT('Ctrl Pts',(-4.91307763025291,-0.918064474226685,
89.58102666155));
#108029=CARTESIAN_POINT('Ctrl Pts',(-4.89686377459191,-2.11625380378499,
89.57816772133));
#108030=CARTESIAN_POINT('Ctrl Pts',(-4.86471942365691,-3.45837930339599,
89.57249980499));
#108031=CARTESIAN_POINT('Ctrl Pts',(-4.81338875390391,-4.92366620480499,
89.56344882297));
#108032=CARTESIAN_POINT('Ctrl Pts',(-4.74070514281191,-6.51802243432599,
89.55063274128));
#108033=CARTESIAN_POINT('Ctrl Pts',(-4.64488033502391,-8.26059862578499,
89.5337362422501));
#108034=CARTESIAN_POINT('Ctrl Pts',(-4.52461819947191,-10.17058185974,89.51253078299));
#108035=CARTESIAN_POINT('Ctrl Pts',(-4.38132929495091,-12.25830895794,89.48726508309));
#108036=CARTESIAN_POINT('Ctrl Pts',(-4.22330060761791,-14.50380923186,89.4594003617801));
#108037=CARTESIAN_POINT('Ctrl Pts',(-4.11905477292291,-16.17227334388,89.4410190084999));
#108038=CARTESIAN_POINT('Ctrl Pts',(-4.08233111723691,-17.08679512682,89.4345436371699));
#108039=CARTESIAN_POINT('Ctrl Pts',(-4.07766124890791,-17.22224198138,89.4337202133899));
#108040=CARTESIAN_POINT('Ctrl Pts',(-4.90176421009691,0.172805543485514,
88.69381939237));
#108041=CARTESIAN_POINT('Ctrl Pts',(-4.90237684066891,-0.168043001263886,
88.69392741567));
#108042=CARTESIAN_POINT('Ctrl Pts',(-4.90049997102491,-0.916686288062986,
88.69359647291));
#108043=CARTESIAN_POINT('Ctrl Pts',(-4.88431246486691,-2.11298117426899,
88.69074217883));
#108044=CARTESIAN_POINT('Ctrl Pts',(-4.85220945457491,-3.45341017763399,
88.68508155195));
#108045=CARTESIAN_POINT('Ctrl Pts',(-4.80094690556891,-4.91675648886699,
88.67604258146));
#108046=CARTESIAN_POINT('Ctrl Pts',(-4.72833832224791,-6.50948905945699,
88.66323972919));
#108047=CARTESIAN_POINT('Ctrl Pts',(-4.63259866553591,-8.25054900027199,
88.64635824459));
#108048=CARTESIAN_POINT('Ctrl Pts',(-4.51240523778391,-10.15936897527,88.62516490037));
#108049=CARTESIAN_POINT('Ctrl Pts',(-4.36918448137191,-12.24647236615,88.59991121682));
#108050=CARTESIAN_POINT('Ctrl Pts',(-4.21104718566391,-14.49203759898,88.5720273449301));
#108051=CARTESIAN_POINT('Ctrl Pts',(-4.10692036426991,-16.16312947225,88.5536669769));
#108052=CARTESIAN_POINT('Ctrl Pts',(-4.06979347507191,-17.08042893886,88.54712050463));
#108053=CARTESIAN_POINT('Ctrl Pts',(-4.06506620762691,-17.21639081336,88.54628695983));
#108054=CARTESIAN_POINT('Ctrl Pts',(-4.26146152596491,0.171439791658314,
88.07924489552));
#108055=CARTESIAN_POINT('Ctrl Pts',(-4.26207044009691,-0.167265508546186,
88.07935226351));
#108056=CARTESIAN_POINT('Ctrl Pts',(-4.26020541552291,-0.910583007860386,
88.0790234093601));
#108057=CARTESIAN_POINT('Ctrl Pts',(-4.24413459780491,-2.09848837535599,
88.0761896905901));
#108058=CARTESIAN_POINT('Ctrl Pts',(-4.21221466403891,-3.43140446629699,
88.07056134505));
#108059=CARTESIAN_POINT('Ctrl Pts',(-4.16125378691191,-4.88615689818499,
88.06157556745));
#108060=CARTESIAN_POINT('Ctrl Pts',(-4.08897746313191,-6.47169911548999,
88.0488313015));
#108061=CARTESIAN_POINT('Ctrl Pts',(-3.99361489689491,-8.20604435927999,
88.03201630812));
#108062=CARTESIAN_POINT('Ctrl Pts',(-3.87372574077891,-10.10971285652,88.0108766152));
#108063=CARTESIAN_POINT('Ctrl Pts',(-3.73080677741191,-12.19405416734,87.98567614591));
#108064=CARTESIAN_POINT('Ctrl Pts',(-3.57218851087291,-14.43990706988,87.9577074658801));
#108065=CARTESIAN_POINT('Ctrl Pts',(-3.46858873840091,-16.12263595099,87.9394400308));
#108066=CARTESIAN_POINT('Ctrl Pts',(-3.42967613463191,-17.05223635503,87.9325786888701));
#108067=CARTESIAN_POINT('Ctrl Pts',(-3.42469467592191,-17.19047898892,87.93170032329));
#108068=CARTESIAN_POINT('Ctrl Pts',(-3.37426264989091,0.169828985201214,
88.10305129184));
#108069=CARTESIAN_POINT('Ctrl Pts',(-3.37486718074691,-0.166348511574186,
88.1031578869399));
#108070=CARTESIAN_POINT('Ctrl Pts',(-3.37301612658291,-0.903384626014186,
88.1028314961499));
#108071=CARTESIAN_POINT('Ctrl Pts',(-3.35708293452291,-2.08139515709799,
88.1000220444999));
#108072=CARTESIAN_POINT('Ctrl Pts',(-3.32537892640591,-3.40545030595299,
88.09443177248));
#108073=CARTESIAN_POINT('Ctrl Pts',(-3.27477384965191,-4.85006687269799,
88.0855087320801));
#108074=CARTESIAN_POINT('Ctrl Pts',(-3.20288940220391,-6.42712858331899,
88.0728335645001));
#108075=CARTESIAN_POINT('Ctrl Pts',(-3.10797158717391,-8.15355432291199,
88.05609699276));
#108076=CARTESIAN_POINT('Ctrl Pts',(-2.98844129765691,-10.05114702111,88.0350205777099));
#108077=CARTESIAN_POINT('Ctrl Pts',(-2.84587827757191,-12.13223065634,88.0098828708199));
#108078=CARTESIAN_POINT('Ctrl Pts',(-2.68669274038691,-14.37842284469,87.98181416567));
#108079=CARTESIAN_POINT('Ctrl Pts',(-2.58371458436691,-16.07487674305,87.96365633834));
#108080=CARTESIAN_POINT('Ctrl Pts',(-2.54269585817091,-17.01898522172,87.9564236302));
#108081=CARTESIAN_POINT('Ctrl Pts',(-2.53741459906091,-17.15991784794,87.95549240173));
#108082=CARTESIAN_POINT('Ctrl Pts',(-4.35610804235899,-4.33090944307451,
90.6854704057514));
#108083=CARTESIAN_POINT('Ctrl Pts',(-4.30478949183536,-5.19990479673094,
90.6983684594538));
#108084=CARTESIAN_POINT('Ctrl Pts',(-4.23851111109544,-6.08684801638409,
90.7143224144303));
#108085=CARTESIAN_POINT('Ctrl Pts',(-4.11702828591693,-7.44606667250624,
90.7415669150335));
#108086=CARTESIAN_POINT('Ctrl Pts',(-4.07285971719824,-7.90392354852698,
90.7511901306072));
#108087=CARTESIAN_POINT('Ctrl Pts',(-4.00126272227492,-8.59776393941472,
90.7661321174809));
#108088=CARTESIAN_POINT('Ctrl Pts',(-3.96413053486937,-8.94644949098537,
90.7737290222104));
#108089=CARTESIAN_POINT('Ctrl Pts',(-3.91853774183228,-9.35632602828725,
90.7827359385487));
#108090=CARTESIAN_POINT('Ctrl Pts',(-3.89518250948977,-9.56203226857026,
90.7872649522662));
#108091=CARTESIAN_POINT('Ctrl Pts',(-3.88210036207672,-9.67611777792289,
90.7897776925425));
#108092=CARTESIAN_POINT('Ctrl Pts',(-3.87572411872776,-9.73138466025277,
90.7909950050756));
#108093=CARTESIAN_POINT('Ctrl Pts',(-3.87231200968099,-9.76087630926258,
90.791644554892));
#108094=CARTESIAN_POINT('Ctrl Pts',(-3.87204372056444,-9.76319481202625,
90.7916956195023));
#108095=CARTESIAN_POINT('Ctrl Pts',(-3.72160846660589,-11.0623980380779,
90.8203099123148));
#108096=CARTESIAN_POINT('Ctrl Pts',(-3.5552983746618,-12.3138422799621,
90.8474815345162));
#108097=CARTESIAN_POINT('Ctrl Pts',(-3.21377379456242,-14.7310381632549,
90.8932818883911));
#108098=CARTESIAN_POINT('Ctrl Pts',(-3.03762539304358,-15.893806171053,
90.9116387028507));
#108099=CARTESIAN_POINT('Ctrl Pts',(-2.88651065714691,-17.02169289621,90.92541563295));
#108100=CARTESIAN_POINT('Ctrl Pts',(-3.38209691507323,-8.56599685566967,
88.0736585716266));
#108101=CARTESIAN_POINT('Ctrl Pts',(-3.37193957246855,-8.73337111009727,
88.0718675580392));
#108102=CARTESIAN_POINT('Ctrl Pts',(-3.36148105368786,-8.90295580922593,
88.0700234389496));
#108103=CARTESIAN_POINT('Ctrl Pts',(-3.35072027313829,-9.07482982075256,
88.0681260230053));
#108104=CARTESIAN_POINT('Ctrl Pts',(-3.33169141523008,-9.37876373413238,
88.0647707219443));
#108105=CARTESIAN_POINT('Ctrl Pts',(-3.31172221608685,-9.68986200064915,
88.0612496136998));
#108106=CARTESIAN_POINT('Ctrl Pts',(-3.29083243179542,-10.0082637043351,
88.0575661812411));
#108107=CARTESIAN_POINT('Ctrl Pts',(-3.27269011607683,-10.2847885431281,
88.054367201603));
#108108=CARTESIAN_POINT('Ctrl Pts',(-3.25385379261577,-10.5668216859292,
88.0510458489647));
#108109=CARTESIAN_POINT('Ctrl Pts',(-3.23435072463955,-10.8544713275498,
88.0476069318742));
#108110=CARTESIAN_POINT('Ctrl Pts',(-3.20984726940729,-11.2158713967401,
88.0432863115966));
#108111=CARTESIAN_POINT('Ctrl Pts',(-3.18434819247011,-11.5861270547559,
88.0387901381542));
#108112=CARTESIAN_POINT('Ctrl Pts',(-3.15797463306237,-11.9658298297435,
88.0341397678366));
#108113=CARTESIAN_POINT('Ctrl Pts',(-3.15506081267406,-12.0077803935696,
88.0336259826613));
#108114=CARTESIAN_POINT('Ctrl Pts',(-3.15213636882712,-12.0498462841331,
88.0331103242645));
#108115=CARTESIAN_POINT('Ctrl Pts',(-3.1492015040689,-12.0920283078329,
88.032592828362));
#108116=CARTESIAN_POINT('Ctrl Pts',(-3.13321219304193,-12.3218383850417,
88.0297734810933));
#108117=CARTESIAN_POINT('Ctrl Pts',(-3.11691166401527,-12.5550954111528,
88.0268992568975));
#108118=CARTESIAN_POINT('Ctrl Pts',(-3.1004258518812,-12.791923953235,88.0239923634191));
#108119=CARTESIAN_POINT('Ctrl Pts',(-3.07705345276688,-13.1276824322344,
88.0198711788509));
#108120=CARTESIAN_POINT('Ctrl Pts',(-3.05325235874796,-13.470646096045,
88.0156744064028));
#108121=CARTESIAN_POINT('Ctrl Pts',(-3.02969158386299,-13.8174000592347,
88.0115200063467));
#108122=CARTESIAN_POINT('Ctrl Pts',(-3.01740308839832,-13.998255083096,
88.0093532131704));
#108123=CARTESIAN_POINT('Ctrl Pts',(-3.00518106525742,-14.1801411304469,
88.0071981402658));
#108124=CARTESIAN_POINT('Ctrl Pts',(-2.99312329150158,-14.3625732882036,
88.0050720286504));
#108125=CARTESIAN_POINT('Ctrl Pts',(-2.98190843170579,-14.5322522947031,
88.0030945455627));
#108126=CARTESIAN_POINT('Ctrl Pts',(-2.97083578203845,-14.7024036909771,
88.0011421376712));
#108127=CARTESIAN_POINT('Ctrl Pts',(-2.96001108679389,-14.8726675221283,
87.9992334518416));
#108128=CARTESIAN_POINT('Ctrl Pts',(-2.9388409874884,-15.2056563160088,
87.9955005921496));
#108129=CARTESIAN_POINT('Ctrl Pts',(-2.9187171752877,-15.5390060018737,
87.991952222616));
#108130=CARTESIAN_POINT('Ctrl Pts',(-2.90016396545698,-15.8737256740298,
87.988680790621));
#108131=CARTESIAN_POINT('Ctrl Pts',(-2.88402936386314,-16.1648110767787,
87.9858358245821));
#108132=CARTESIAN_POINT('Ctrl Pts',(-2.86908215708997,-16.4569322750347,
87.9832002282526));
#108133=CARTESIAN_POINT('Ctrl Pts',(-2.85569754787586,-16.7507633239214,
87.9808401604872));
#108134=CARTESIAN_POINT('Ctrl Pts',(-2.85191950242244,-16.8337023952505,
87.9801739891296));
#108135=CARTESIAN_POINT('Ctrl Pts',(-2.84826607231398,-16.9167777891168,
87.9795297908316));
#108136=CARTESIAN_POINT('Ctrl Pts',(-2.84483266429344,-17.,87.978924388362));
#108137=CARTESIAN_POINT('Ctrl Pts',(8.76687408897909,-16.44294428525,98.6115064056));
#108138=CARTESIAN_POINT('Ctrl Pts',(8.50448839268907,-16.29482593816,98.7748340168099));
#108139=CARTESIAN_POINT('Ctrl Pts',(7.73803846225909,-15.84050813694,99.1889282148399));
#108140=CARTESIAN_POINT('Ctrl Pts',(6.5349477692391,-15.02004513321,99.57986765328));
#108141=CARTESIAN_POINT('Ctrl Pts',(5.27236547025909,-14.00812222941,99.71688058005));
#108142=CARTESIAN_POINT('Ctrl Pts',(4.18367013900909,-13.00986029655,99.6525682338999));
#108143=CARTESIAN_POINT('Ctrl Pts',(3.20714073810909,-11.9973978225,99.4540121251699));
#108144=CARTESIAN_POINT('Ctrl Pts',(2.30415558486909,-10.93738557134,99.14726582813));
#108145=CARTESIAN_POINT('Ctrl Pts',(1.48684448748909,-9.84723726948199,
98.7638938018301));
#108146=CARTESIAN_POINT('Ctrl Pts',(0.762911702719089,-8.74553579959698,
98.3366761029799));
#108147=CARTESIAN_POINT('Ctrl Pts',(0.112673674949087,-7.60752902450998,
97.87904754731));
#108148=CARTESIAN_POINT('Ctrl Pts',(-0.488386309690911,-6.37224922945299,
97.3887134898101));
#108149=CARTESIAN_POINT('Ctrl Pts',(-1.04213634100091,-4.97114208044499,
96.8726660516999));
#108150=CARTESIAN_POINT('Ctrl Pts',(-1.51067364081091,-3.36802983074299,
96.3809404461301));
#108151=CARTESIAN_POINT('Ctrl Pts',(-1.81701727702091,-1.61981132427399,
96.0275490175501));
#108152=CARTESIAN_POINT('Ctrl Pts',(-1.87689058580091,-0.403435681896786,
95.95525979127));
#108153=CARTESIAN_POINT('Ctrl Pts',(-1.86852961382091,0.200651371990514,
95.9651297134299));
#108154=CARTESIAN_POINT('Ctrl Pts',(6.48819653156909,-15.56528785696,92.69131734964));
#108155=CARTESIAN_POINT('Ctrl Pts',(6.38630096531909,-15.47758556196,92.78395944648));
#108156=CARTESIAN_POINT('Ctrl Pts',(6.06771745324909,-15.21581444004,93.0220629079301));
#108157=CARTESIAN_POINT('Ctrl Pts',(5.4599981715091,-14.7540110982,93.25770281466));
#108158=CARTESIAN_POINT('Ctrl Pts',(4.67600680749909,-14.1542490297,93.3348504985));
#108159=CARTESIAN_POINT('Ctrl Pts',(3.89225004337909,-13.51762150969,93.2708681228701));
#108160=CARTESIAN_POINT('Ctrl Pts',(3.10219061563909,-12.82180106148,93.10110938746));
#108161=CARTESIAN_POINT('Ctrl Pts',(2.29351899611909,-12.03547497051,92.8361696333));
#108162=CARTESIAN_POINT('Ctrl Pts',(1.49269764718909,-11.16347023105,92.4954481808701));
#108163=CARTESIAN_POINT('Ctrl Pts',(0.723899763099089,-10.21566958806,92.10308906725));
#108164=CARTESIAN_POINT('Ctrl Pts',(-0.0200535606409112,-9.16446753653399,
91.66798555359));
#108165=CARTESIAN_POINT('Ctrl Pts',(-0.760996247700911,-7.93604781061299,
91.18364248321));
#108166=CARTESIAN_POINT('Ctrl Pts',(-1.50146348324091,-6.42271318686499,
90.65003751555));
#108167=CARTESIAN_POINT('Ctrl Pts',(-2.18733220258091,-4.52156727656799,
90.1121766327));
#108168=CARTESIAN_POINT('Ctrl Pts',(-2.67864361223591,-2.24136809065099,
89.70052285778));
#108169=CARTESIAN_POINT('Ctrl Pts',(-2.78026244461691,-0.556674570830786,
89.61294403093));
#108170=CARTESIAN_POINT('Ctrl Pts',(-2.76634006182491,0.277047208448614,
89.6246271184));
#108171=CARTESIAN_POINT('Ctrl Pts',(2.72889798757909,-19.34707978044,89.1447316619801));
#108172=CARTESIAN_POINT('Ctrl Pts',(2.66091020417909,-19.26097438926,89.20317193542));
#108173=CARTESIAN_POINT('Ctrl Pts',(2.42996072068909,-19.00901506437,89.3612231288901));
#108174=CARTESIAN_POINT('Ctrl Pts',(1.89825599140909,-18.57235792605,89.54995470502));
#108175=CARTESIAN_POINT('Ctrl Pts',(1.10699433400909,-17.98310305551,89.64471299023));
#108176=CARTESIAN_POINT('Ctrl Pts',(0.252027388659088,-17.32630382037,89.6293082806));
#108177=CARTESIAN_POINT('Ctrl Pts',(-0.654644487020914,-16.5759732809,89.5211787480401));
#108178=CARTESIAN_POINT('Ctrl Pts',(-1.61859475251091,-15.69330276297,89.32252842609));
#108179=CARTESIAN_POINT('Ctrl Pts',(-2.60190967346991,-14.67920705201,89.04432012876));
#108180=CARTESIAN_POINT('Ctrl Pts',(-3.56872088692091,-13.5426076308,88.7048190356501));
#108181=CARTESIAN_POINT('Ctrl Pts',(-4.52340351538191,-12.24737090716,88.3108681836801));
#108182=CARTESIAN_POINT('Ctrl Pts',(-5.49218708965691,-10.69472182793,87.8542655723));
#108183=CARTESIAN_POINT('Ctrl Pts',(-6.47884434265791,-8.73212611500698,
87.33045821777));
#108184=CARTESIAN_POINT('Ctrl Pts',(-7.41072188100292,-6.20174180863199,
86.77974038575));
#108185=CARTESIAN_POINT('Ctrl Pts',(-8.09046417872891,-3.09478014856899,
86.34080207947));
#108186=CARTESIAN_POINT('Ctrl Pts',(-8.23255272084991,-0.768163226373987,
86.24527748657));
#108187=CARTESIAN_POINT('Ctrl Pts',(-8.21314998798691,0.382355724809714,
86.2578544693));
#108188=CARTESIAN_POINT('Ctrl Pts',(0.196332399109088,-25.06476693734,90.52591274045));
#108189=CARTESIAN_POINT('Ctrl Pts',(0.011250503809089,-24.92028925106,90.61126618974));
#108190=CARTESIAN_POINT('Ctrl Pts',(-0.555409203350912,-24.48834062706,
90.84285524963));
#108191=CARTESIAN_POINT('Ctrl Pts',(-1.58520004181091,-23.72520655934,91.1268519171499));
#108192=CARTESIAN_POINT('Ctrl Pts',(-2.86435733527191,-22.73723822501,91.3040139279599));
#108193=CARTESIAN_POINT('Ctrl Pts',(-4.11539939684391,-21.69298831769,91.35045014482));
#108194=CARTESIAN_POINT('Ctrl Pts',(-5.35778473735791,-20.55625239098,91.29239781524));
#108195=CARTESIAN_POINT('Ctrl Pts',(-6.61477798365991,-19.27659173514,91.13677980334));
#108196=CARTESIAN_POINT('Ctrl Pts',(-7.84814243484691,-17.86250092626,90.8959268123599));
#108197=CARTESIAN_POINT('Ctrl Pts',(-9.02351089959392,-16.33037133773,90.58921613446));
#108198=CARTESIAN_POINT('Ctrl Pts',(-10.1541748021089,-14.63600828855,90.2254084335399));
#108199=CARTESIAN_POINT('Ctrl Pts',(-11.2746720699649,-12.6615424041,89.79831775978));
#108200=CARTESIAN_POINT('Ctrl Pts',(-12.3896921849461,-10.2361987255,89.30460716211));
#108201=CARTESIAN_POINT('Ctrl Pts',(-13.4190864676907,-7.19853323577899,
88.78356996623));
#108202=CARTESIAN_POINT('Ctrl Pts',(-14.1550194975079,-3.56544121650899,
88.3679745890099));
#108203=CARTESIAN_POINT('Ctrl Pts',(-14.3071566503109,-0.885592743395686,
88.2775704089799));
#108204=CARTESIAN_POINT('Ctrl Pts',(-14.2863014408449,0.440736329119914,
88.28947825565));
#108205=CARTESIAN_POINT('Origin',(33.1784433940591,111.0724296188,81.627048885766));
#108206=CARTESIAN_POINT('Origin',(11.833832765324,1.4210854715202E-14,67.1130006183894));
#108207=CARTESIAN_POINT('',(-3.38212037980694,8.56594505080956,88.0736627081359));
#108208=CARTESIAN_POINT('',(3.67711006996132,17.0000002064554,86.8289298464967));
#108209=CARTESIAN_POINT('Origin',(14.9594999633274,1.4210854715202E-14,
84.8395401726047));
#108210=CARTESIAN_POINT('',(-4.35611211213986,4.33088850455625,90.6854742262428));
#108211=CARTESIAN_POINT('Ctrl Pts',(-3.38212037964035,8.56594505080956,
88.0736627090807));
#108212=CARTESIAN_POINT('Ctrl Pts',(-4.01196786573672,7.17537091305373,
88.1847154552553));
#108213=CARTESIAN_POINT('Ctrl Pts',(-4.48931101496871,5.53882790374305,
88.5644810324709));
#108214=CARTESIAN_POINT('Ctrl Pts',(-4.85197636679152,3.15389859767277,
89.2370189724097));
#108215=CARTESIAN_POINT('Ctrl Pts',(-4.89577428506616,2.43186608701334,
89.4685758852254));
#108216=CARTESIAN_POINT('Ctrl Pts',(-4.89257765146922,2.07960258734854,
89.6990122597812));
#108217=CARTESIAN_POINT('Ctrl Pts',(-4.8906158368644,2.04033106029839,89.732655216438));
#108218=CARTESIAN_POINT('Ctrl Pts',(-4.88579454993422,2.00069680433019,
89.7825361835878));
#108219=CARTESIAN_POINT('Ctrl Pts',(-4.88354722702825,1.98887487582002,
89.8019169065442));
#108220=CARTESIAN_POINT('Ctrl Pts',(-4.87826443336458,1.97723449897512,
89.8383892585974));
#108221=CARTESIAN_POINT('Ctrl Pts',(-4.87568144241096,1.97525889172666,
89.8541368575422));
#108222=CARTESIAN_POINT('Ctrl Pts',(-4.86975792746109,1.97811725859756,
89.8861361443495));
#108223=CARTESIAN_POINT('Ctrl Pts',(-4.86662571171048,1.98280632649891,
89.90128551083));
#108224=CARTESIAN_POINT('Ctrl Pts',(-4.85879125914699,1.99981904456653,
89.936162260766));
#108225=CARTESIAN_POINT('Ctrl Pts',(-4.85403768892131,2.01448559580851,
89.9548332706941));
#108226=CARTESIAN_POINT('Ctrl Pts',(-4.84078559510826,2.06131459243085,
90.0031480412483));
#108227=CARTESIAN_POINT('Ctrl Pts',(-4.83131844154325,2.10280479749029,
90.0325972743869));
#108228=CARTESIAN_POINT('Ctrl Pts',(-4.79769422275787,2.26162274419331,
90.1269406929706));
#108229=CARTESIAN_POINT('Ctrl Pts',(-4.76852086425854,2.41936528606566,
90.1895927082715));
#108230=CARTESIAN_POINT('Ctrl Pts',(-4.6623556101869,2.97945480151193,90.3834105370763));
#108231=CARTESIAN_POINT('Ctrl Pts',(-4.54150792694898,3.60135784152189,
90.5420939486474));
#108232=CARTESIAN_POINT('Ctrl Pts',(-4.35610890955664,4.33088267781939,
90.6854997272617));
#108233=CARTESIAN_POINT('',(5.5223959989754,17.4579257767337,93.2012874099244));
#108234=CARTESIAN_POINT('Ctrl Pts',(5.52235604123134,17.4579109754503,93.2011992796923));
#108235=CARTESIAN_POINT('Ctrl Pts',(5.22894280014455,17.2623218249119,93.367079946153));
#108236=CARTESIAN_POINT('Ctrl Pts',(4.76538644319997,16.9508835888659,93.5867638396279));
#108237=CARTESIAN_POINT('Ctrl Pts',(3.58451633043917,16.0576376588373,93.8206675950891));
#108238=CARTESIAN_POINT('Ctrl Pts',(3.05115204928158,15.6226268077262,93.8400596368745));
#108239=CARTESIAN_POINT('Ctrl Pts',(1.44251906803305,14.200046478662,93.7321110206254));
#108240=CARTESIAN_POINT('Ctrl Pts',(0.340389916588458,13.0612424878892,
93.4020444225624));
#108241=CARTESIAN_POINT('Ctrl Pts',(-1.48003977708628,10.6921991318613,
92.5936247707043));
#108242=CARTESIAN_POINT('Ctrl Pts',(-2.19080611119185,9.58637988894192,
92.1831451763138));
#108243=CARTESIAN_POINT('Ctrl Pts',(-3.45378489947922,7.14145905979051,
91.3705187372968));
#108244=CARTESIAN_POINT('Ctrl Pts',(-3.98965312113643,5.77285420037568,
90.9689374055126));
#108245=CARTESIAN_POINT('Ctrl Pts',(-4.35611534545078,4.33089434326653,
90.6854487074141));
#108246=CARTESIAN_POINT('',(6.72284169586273,18.2005858292129,92.4518055721481));
#108247=CARTESIAN_POINT('Ctrl Pts',(6.72284226036562,18.2005860182602,92.4518065521755));
#108248=CARTESIAN_POINT('Ctrl Pts',(6.52447441211948,18.0870793782497,92.5879632910271));
#108249=CARTESIAN_POINT('Ctrl Pts',(6.32523711499546,17.9686329849413,92.7183652975874));
#108250=CARTESIAN_POINT('Ctrl Pts',(5.92461392813651,17.7210119573958,92.9683840841069));
#108251=CARTESIAN_POINT('Ctrl Pts',(5.72352843386396,17.5919809286868,93.087753641798));
#108252=CARTESIAN_POINT('Ctrl Pts',(5.52243594124477,17.4579405679198,93.2013755505527));
#108253=CARTESIAN_POINT('',(7.18082400639694,18.5000000000005,91.584560428554));
#108254=CARTESIAN_POINT('Ctrl Pts',(6.72284115829969,18.2005856294418,92.4518046221571));
#108255=CARTESIAN_POINT('Ctrl Pts',(6.79273197664956,18.240576093798,92.4038466295081));
#108256=CARTESIAN_POINT('Ctrl Pts',(6.86056063905956,18.2794361008248,92.3496148573615));
#108257=CARTESIAN_POINT('Ctrl Pts',(6.97969843358352,18.3487004919864,92.2319577470068));
#108258=CARTESIAN_POINT('Ctrl Pts',(7.0329599010906,18.3801663787552,92.1682058175694));
#108259=CARTESIAN_POINT('Ctrl Pts',(7.12351536852898,18.4363205837614,92.0220852314388));
#108260=CARTESIAN_POINT('Ctrl Pts',(7.15921714211905,18.4602533155557,91.9391925959291));
#108261=CARTESIAN_POINT('Ctrl Pts',(7.18668920593521,18.4843760087887,91.805974202742));
#108262=CARTESIAN_POINT('Ctrl Pts',(7.19146209592983,18.4902813775617,91.7619889127895));
#108263=CARTESIAN_POINT('Ctrl Pts',(7.19239576516467,18.4981238590837,91.6728396062505));
#108264=CARTESIAN_POINT('Ctrl Pts',(7.1885807496804,18.5000000202485,91.6285508614658));
#108265=CARTESIAN_POINT('Ctrl Pts',(7.1808240063969,18.5000000000005,91.584560428554));
#108266=CARTESIAN_POINT('',(6.52234847239187,18.4999999410994,87.8501601928846));
#108267=CARTESIAN_POINT('',(3.13624619141446,18.5,68.6466197984171));
#108268=CARTESIAN_POINT('Ctrl Pts',(6.52234845610643,18.4999999847284,87.8501601957549));
#108269=CARTESIAN_POINT('Ctrl Pts',(6.50518062854233,18.4999859008965,87.7529665002294));
#108270=CARTESIAN_POINT('Ctrl Pts',(6.4689459203091,18.4903141218653,87.664456395585));
#108271=CARTESIAN_POINT('Ctrl Pts',(6.36972845372158,18.4567893765268,87.5030984304372));
#108272=CARTESIAN_POINT('Ctrl Pts',(6.30672210579292,18.432901727933,87.4302697426766));
#108273=CARTESIAN_POINT('Ctrl Pts',(6.09300490374429,18.346334827275,87.2342769515595));
#108274=CARTESIAN_POINT('Ctrl Pts',(5.91789315169122,18.2685458496827,87.1337400811857));
#108275=CARTESIAN_POINT('Ctrl Pts',(5.42965862838366,18.0384248294259,86.9149877608346));
#108276=CARTESIAN_POINT('Ctrl Pts',(5.06665893878539,17.8504223940439,86.8312090840354));
#108277=CARTESIAN_POINT('Ctrl Pts',(4.34754070270684,17.4389532379846,86.7591293140068));
#108278=CARTESIAN_POINT('Ctrl Pts',(3.99139559238964,17.2150671358623,86.7735129004256));
#108279=CARTESIAN_POINT('Ctrl Pts',(3.67710978043254,17.,86.8289299687275));
#108280=CARTESIAN_POINT('Origin',(-2.58324905909591,17.,89.45593823501));
#108281=CARTESIAN_POINT('',(-2.84368888085373,17.0000004240545,87.9787221388565));
#108282=CARTESIAN_POINT('',(-2.58374595121974,18.4999998795018,89.4555997193086));
#108283=CARTESIAN_POINT('Origin',(-2.58324874406691,17.,89.45594000334));
#108284=CARTESIAN_POINT('',(-2.88564989564837,17.021544099749,90.9249820008041));
#108285=CARTESIAN_POINT('Ctrl Pts',(-2.88564989564837,17.021544099749,90.9249820008041));
#108286=CARTESIAN_POINT('Ctrl Pts',(-2.89272275172126,17.0341859203076,
90.9233406649279));
#108287=CARTESIAN_POINT('Ctrl Pts',(-2.89875888973422,17.0483838508755,
90.9216770896837));
#108288=CARTESIAN_POINT('Ctrl Pts',(-2.90373721386657,17.0641913692076,
90.9198941123406));
#108289=CARTESIAN_POINT('Ctrl Pts',(-2.90863603335344,17.0797464389029,
90.9181396094355));
#108290=CARTESIAN_POINT('Ctrl Pts',(-2.91251038467502,17.0968604310834,
90.9162695931292));
#108291=CARTESIAN_POINT('Ctrl Pts',(-2.91533029213212,17.1155732692065,
90.9141442815309));
#108292=CARTESIAN_POINT('Ctrl Pts',(-2.91806979840219,17.1337525669846,
90.912079566806));
#108293=CARTESIAN_POINT('Ctrl Pts',(-2.91981384580904,17.1534411860481,
90.909773888665));
#108294=CARTESIAN_POINT('Ctrl Pts',(-2.92052895027268,17.1746602860845,
90.9070536885397));
#108295=CARTESIAN_POINT('Ctrl Pts',(-2.92116428945037,17.1935125325099,
90.9046369091758));
#108296=CARTESIAN_POINT('Ctrl Pts',(-2.92098715652524,17.2135729063995,
90.9018923789284));
#108297=CARTESIAN_POINT('Ctrl Pts',(-2.91997316350144,17.2348417505946,
90.898666979331));
#108298=CARTESIAN_POINT('Ctrl Pts',(-2.91884217783387,17.2585645547814,
90.8950694390805));
#108299=CARTESIAN_POINT('Ctrl Pts',(-2.91666985230917,17.2838009544818,
90.8908731213832));
#108300=CARTESIAN_POINT('Ctrl Pts',(-2.91338863854326,17.3105273658752,
90.8858265569166));
#108301=CARTESIAN_POINT('Ctrl Pts',(-2.91036157979191,17.3351836130058,
90.8811708873313));
#108302=CARTESIAN_POINT('Ctrl Pts',(-2.9063903424519,17.3611081211397,90.875791137097));
#108303=CARTESIAN_POINT('Ctrl Pts',(-2.90143338018716,17.3882532510825,
90.8694509342227));
#108304=CARTESIAN_POINT('Ctrl Pts',(-2.90101718845782,17.3905323845458,
90.868918604167));
#108305=CARTESIAN_POINT('Ctrl Pts',(-2.90059405731327,17.3928201037254,
90.8683794812995));
#108306=CARTESIAN_POINT('Ctrl Pts',(-2.90016396772038,17.3951163696448,
90.8678334135308));
#108307=CARTESIAN_POINT('Ctrl Pts',(-2.89525968391285,17.4213005413903,
90.8616066380865));
#108308=CARTESIAN_POINT('Ctrl Pts',(-2.88944428307568,17.4485976869347,
90.8544806107943));
#108309=CARTESIAN_POINT('Ctrl Pts',(-2.88266400361103,17.4769183999902,
90.8462258062526));
#108310=CARTESIAN_POINT('Ctrl Pts',(-2.88176772082657,17.4806621051999,
90.8451346065111));
#108311=CARTESIAN_POINT('Ctrl Pts',(-2.88085461529801,17.4844236483625,
90.844023638876));
#108312=CARTESIAN_POINT('Ctrl Pts',(-2.87992459944332,17.4882027778685,
90.8428923335443));
#108313=CARTESIAN_POINT('Ctrl Pts',(-2.87594185832357,17.5043866895776,
90.8380475814458));
#108314=CARTESIAN_POINT('Ctrl Pts',(-2.87164793871547,17.5208931022076,
90.8328303477065));
#108315=CARTESIAN_POINT('Ctrl Pts',(-2.86703278793527,17.5376973896157,
90.8271961656877));
#108316=CARTESIAN_POINT('Ctrl Pts',(-2.86472521254517,17.5460995333198,
90.8243790746783));
#108317=CARTESIAN_POINT('Ctrl Pts',(-2.86233732272639,17.5545761164248,
90.8214577022601));
#108318=CARTESIAN_POINT('Ctrl Pts',(-2.85986784195119,17.563123412719,90.8184264261586));
#108319=CARTESIAN_POINT('Ctrl Pts',(-2.8586331015636,17.567397060866,90.8169107881079));
#108320=CARTESIAN_POINT('Ctrl Pts',(-2.85737796314338,17.5716883855217,
90.8153676717458));
#108321=CARTESIAN_POINT('Ctrl Pts',(-2.85610226614962,17.5759968930406,
90.8137963669988));
#108322=CARTESIAN_POINT('Ctrl Pts',(-2.85546441765275,17.5781511468,90.8130107146253));
#108323=CARTESIAN_POINT('Ctrl Pts',(-2.85482142949836,17.5803096961521,
90.8122180150108));
#108324=CARTESIAN_POINT('Ctrl Pts',(-2.85417328159823,17.5824724768591,
90.8114181792966));
#108325=CARTESIAN_POINT('Ctrl Pts',(-2.85363989194418,17.5842523250277,
90.8107599590126));
#108326=CARTESIAN_POINT('Ctrl Pts',(-2.85275716260682,17.5871762193749,
90.8096706293563));
#108327=CARTESIAN_POINT('Ctrl Pts',(-2.85237889573469,17.5884265878567,
90.809202171474));
#108328=CARTESIAN_POINT('Ctrl Pts',(-2.85229751199868,17.5886956033744,
90.8091013832332));
#108329=CARTESIAN_POINT('Ctrl Pts',(-2.85223948918946,17.5888872233252,
90.8090295090512));
#108330=CARTESIAN_POINT('Ctrl Pts',(-2.85221333854556,17.5889734477422,
90.8089971746851));
#108331=CARTESIAN_POINT('Ctrl Pts',(-2.84981137671696,17.5968932434863,
90.8060272320208));
#108332=CARTESIAN_POINT('Ctrl Pts',(-2.84742439317891,17.6066031853638,
90.8021939861059));
#108333=CARTESIAN_POINT('Ctrl Pts',(-2.84503553822777,17.6180765319828,
90.7973737496568));
#108334=CARTESIAN_POINT('Ctrl Pts',(-2.84267434922401,17.6294170028056,
90.7926093376135));
#108335=CARTESIAN_POINT('Ctrl Pts',(-2.84031138095239,17.6424806348029,
90.78688052455));
#108336=CARTESIAN_POINT('Ctrl Pts',(-2.83791736788481,17.6572145956106,
90.7800277439991));
#108337=CARTESIAN_POINT('Ctrl Pts',(-2.83555953805227,17.6717258665865,
90.7732785367214));
#108338=CARTESIAN_POINT('Ctrl Pts',(-2.83317165642656,17.6878577743391,
90.7654388297756));
#108339=CARTESIAN_POINT('Ctrl Pts',(-2.8307122729031,17.7055277305542,90.7563199402147));
#108340=CARTESIAN_POINT('Ctrl Pts',(-2.82825288937964,17.7231976867694,
90.7472010506538));
#108341=CARTESIAN_POINT('Ctrl Pts',(-2.82572211830423,17.7424062805898,
90.7368026951786));
#108342=CARTESIAN_POINT('Ctrl Pts',(-2.82306354352082,17.7630309283082,
90.7249034888705));
#108343=CARTESIAN_POINT('Ctrl Pts',(-2.82037666239594,17.7838751704968,
90.7128775894938));
#108344=CARTESIAN_POINT('Ctrl Pts',(-2.8175619937707,17.8061702443592,90.6993152921338));
#108345=CARTESIAN_POINT('Ctrl Pts',(-2.81457900890531,17.8297261572579,
90.6839614262744));
#108346=CARTESIAN_POINT('Ctrl Pts',(-2.81183054654266,17.8514301024475,
90.6698146825462));
#108347=CARTESIAN_POINT('Ctrl Pts',(-2.80893917040494,17.8742043080774,
90.6541462654809));
#108348=CARTESIAN_POINT('Ctrl Pts',(-2.80585388277503,17.8978548379212,
90.6367446469575));
#108349=CARTESIAN_POINT('Ctrl Pts',(-2.80559061943676,17.8998729050142,
90.635259790849));
#108350=CARTESIAN_POINT('Ctrl Pts',(-2.80532593181083,17.9018973237863,
90.6337623114634));
#108351=CARTESIAN_POINT('Ctrl Pts',(-2.80505978110586,17.9039279573148,
90.6322520756096));
#108352=CARTESIAN_POINT('Ctrl Pts',(-2.80205444120059,17.9268576128145,
90.6151986844556));
#108353=CARTESIAN_POINT('Ctrl Pts',(-2.79886835716004,17.9505812957136,
90.5965189872643));
#108354=CARTESIAN_POINT('Ctrl Pts',(-2.79546721016593,17.9748626055492,
90.5760303547297));
#108355=CARTESIAN_POINT('Ctrl Pts',(-2.79503723540175,17.977932261312,90.5734401711952));
#108356=CARTESIAN_POINT('Ctrl Pts',(-2.79460378775201,17.9810107717434,
90.5708210887861));
#108357=CARTESIAN_POINT('Ctrl Pts',(-2.79416676592282,17.9840976086969,
90.5681727505254));
#108358=CARTESIAN_POINT('Ctrl Pts',(-2.79221980998713,17.9978496346318,
90.5563742600336));
#108359=CARTESIAN_POINT('Ctrl Pts',(-2.79020290218355,18.0117669734879,
90.5439950698029));
#108360=CARTESIAN_POINT('Ctrl Pts',(-2.78811029496996,18.0257981614033,
90.531005677591));
#108361=CARTESIAN_POINT('Ctrl Pts',(-2.78706399136317,18.032813755361,90.5245109814851));
#108362=CARTESIAN_POINT('Ctrl Pts',(-2.78599875847823,18.0398577888693,
90.5178637116599));
#108363=CARTESIAN_POINT('Ctrl Pts',(-2.78491395993615,18.0469231884083,
90.5110605527259));
#108364=CARTESIAN_POINT('Ctrl Pts',(-2.78437156066511,18.0504558881778,
90.5076589732588));
#108365=CARTESIAN_POINT('Ctrl Pts',(-2.78382426979793,18.0539939285704,
90.5042184205558));
#108366=CARTESIAN_POINT('Ctrl Pts',(-2.78327201036165,18.0575364026759,
90.5007384915099));
#108367=CARTESIAN_POINT('Ctrl Pts',(-2.7829958806435,18.0593076397286,90.498998526987));
#108368=CARTESIAN_POINT('Ctrl Pts',(-2.78271850877296,18.0610799851526,
90.4972487183256));
#108369=CARTESIAN_POINT('Ctrl Pts',(-2.782439885476,18.0628533233283,90.4954890167306));
#108370=CARTESIAN_POINT('Ctrl Pts',(-2.78221394952778,18.0642913252708,
90.494062072707));
#108371=CARTESIAN_POINT('Ctrl Pts',(-2.78185106072081,18.0665937852198,
90.4917650752688));
#108372=CARTESIAN_POINT('Ctrl Pts',(-2.78168224811797,18.0676589240395,
90.4906984446302));
#108373=CARTESIAN_POINT('Ctrl Pts',(-2.78164288170219,18.0679073101016,
90.4904497106821));
#108374=CARTESIAN_POINT('Ctrl Pts',(-2.78161413020944,18.0680885676011,
90.490268030535));
#108375=CARTESIAN_POINT('Ctrl Pts',(-2.78160025212524,18.0681761996918,
90.4901801847663));
#108376=CARTESIAN_POINT('Ctrl Pts',(-2.78032215971842,18.0762466154791,
90.4820900904573));
#108377=CARTESIAN_POINT('Ctrl Pts',(-2.7786805815117,18.0856953119116,90.4724605539379));
#108378=CARTESIAN_POINT('Ctrl Pts',(-2.77666920797862,18.0963860070905,
90.4611876416064));
#108379=CARTESIAN_POINT('Ctrl Pts',(-2.77466627508606,18.1070318392374,
90.4499620355554));
#108380=CARTESIAN_POINT('Ctrl Pts',(-2.77229676958671,18.1189095058335,
90.4371062886785));
#108381=CARTESIAN_POINT('Ctrl Pts',(-2.76954033978892,18.1318401729579,
90.422495725083));
#108382=CARTESIAN_POINT('Ctrl Pts',(-2.76682548303308,18.1445758170975,
90.408105521017));
#108383=CARTESIAN_POINT('Ctrl Pts',(-2.7637353738569,18.1583331058328,90.3920123883352));
#108384=CARTESIAN_POINT('Ctrl Pts',(-2.76023529491343,18.1728952424158,
90.3740845319854));
#108385=CARTESIAN_POINT('Ctrl Pts',(-2.75774287675484,18.1832649895654,
90.3613180443053));
#108386=CARTESIAN_POINT('Ctrl Pts',(-2.75504225355344,18.1940419267948,
90.3476208806931));
#108387=CARTESIAN_POINT('Ctrl Pts',(-2.75211568209974,18.2051324832473,
90.3329443703691));
#108388=CARTESIAN_POINT('Ctrl Pts',(-2.74826585928658,18.2197217997621,
90.313637831931));
#108389=CARTESIAN_POINT('Ctrl Pts',(-2.74402945369785,18.2348512605904,
90.2926396949604));
#108390=CARTESIAN_POINT('Ctrl Pts',(-2.73940734219813,18.2502548534008,
90.2698653768146));
#108391=CARTESIAN_POINT('Ctrl Pts',(-2.73478523069841,18.2656584462113,
90.2470910586688));
#108392=CARTESIAN_POINT('Ctrl Pts',(-2.72977787187187,18.2813361189648,
90.2225397489312));
#108393=CARTESIAN_POINT('Ctrl Pts',(-2.72435293204009,18.2969874788806,
90.1961498106201));
#108394=CARTESIAN_POINT('Ctrl Pts',(-2.71975402191694,18.3102556808865,
90.173778142323));
#108395=CARTESIAN_POINT('Ctrl Pts',(-2.71486064322452,18.3235025090161,
90.150086575742));
#108396=CARTESIAN_POINT('Ctrl Pts',(-2.70967491430402,18.3365199956771,
90.1250651320109));
#108397=CARTESIAN_POINT('Ctrl Pts',(-2.70874348358792,18.338858121543,90.120570924618));
#108398=CARTESIAN_POINT('Ctrl Pts',(-2.70780251144841,18.3411888157279,
90.116033885955));
#108399=CARTESIAN_POINT('Ctrl Pts',(-2.70685186153706,18.3435108313772,
90.1114540572454));
#108400=CARTESIAN_POINT('Ctrl Pts',(-2.70373017080596,18.3511357358172,
90.0964150732175));
#108401=CARTESIAN_POINT('Ctrl Pts',(-2.70050598929708,18.3586669961609,
90.0809143766248));
#108402=CARTESIAN_POINT('Ctrl Pts',(-2.69718010601399,18.3660589508997,
90.064956017357));
#108403=CARTESIAN_POINT('Ctrl Pts',(-2.69551716437245,18.3697549282691,
90.0569768377231));
#108404=CARTESIAN_POINT('Ctrl Pts',(-2.69382879758791,18.3734160829511,
90.0488832440363));
#108405=CARTESIAN_POINT('Ctrl Pts',(-2.69211520430522,18.3770365424535,
90.0406762303334));
#108406=CARTESIAN_POINT('Ctrl Pts',(-2.69111684674479,18.3791458604306,
90.0358947373959));
#108407=CARTESIAN_POINT('Ctrl Pts',(-2.68998177548008,18.3815123624915,
90.0304489795216));
#108408=CARTESIAN_POINT('Ctrl Pts',(-2.68893247195787,18.3836575502816,
90.0254316939668));
#108409=CARTESIAN_POINT('Ctrl Pts',(-2.68818073791755,18.3851943893854,
90.0218372484496));
#108410=CARTESIAN_POINT('Ctrl Pts',(-2.68747356905611,18.3866189610764,
90.0184631770783));
#108411=CARTESIAN_POINT('Ctrl Pts',(-2.68689895589015,18.3877699993807,
90.0157159835079));
#108412=CARTESIAN_POINT('Ctrl Pts',(-2.68273502555585,18.3961109904947,
89.995808464294));
#108413=CARTESIAN_POINT('Ctrl Pts',(-2.67857173349699,18.4038633633472,
89.9760659407918));
#108414=CARTESIAN_POINT('Ctrl Pts',(-2.6744950233554,18.411069615988,89.9564946382672));
#108415=CARTESIAN_POINT('Ctrl Pts',(-2.67033515986297,18.4184228557909,
89.9365241365529));
#108416=CARTESIAN_POINT('Ctrl Pts',(-2.66626541080946,18.4252074926367,
89.9167318884532));
#108417=CARTESIAN_POINT('Ctrl Pts',(-2.66232301180073,18.4314664027915,
89.8971312173691));
#108418=CARTESIAN_POINT('Ctrl Pts',(-2.65832134318844,18.4378194087297,
89.8772358718996));
#108419=CARTESIAN_POINT('Ctrl Pts',(-2.65445073071921,18.4436307789762,
89.8575378564482));
#108420=CARTESIAN_POINT('Ctrl Pts',(-2.65069644096881,18.4489427237725,
89.8380584175511));
#108421=CARTESIAN_POINT('Ctrl Pts',(-2.64684123627611,18.4543974531267,
89.8180553732365));
#108422=CARTESIAN_POINT('Ctrl Pts',(-2.64310853898396,18.4593255648351,
89.7982826110807));
#108423=CARTESIAN_POINT('Ctrl Pts',(-2.63942836724829,18.4637697337413,
89.7787726382549));
#108424=CARTESIAN_POINT('Ctrl Pts',(-2.63842739594567,18.4649785049233,
89.7734661133653));
#108425=CARTESIAN_POINT('Ctrl Pts',(-2.63743001768668,18.4661514569317,
89.7681790936903));
#108426=CARTESIAN_POINT('Ctrl Pts',(-2.6364341883642,18.4672894089015,89.76291239117));
#108427=CARTESIAN_POINT('Ctrl Pts',(-2.63412054764574,18.4699332475128,
89.7506761001432));
#108428=CARTESIAN_POINT('Ctrl Pts',(-2.6318089098615,18.4723877734019,89.7385526465792));
#108429=CARTESIAN_POINT('Ctrl Pts',(-2.62955528816091,18.4746640081669,
89.7265334976566));
#108430=CARTESIAN_POINT('Ctrl Pts',(-2.62727008962927,18.4769721366081,
89.7143459413057));
#108431=CARTESIAN_POINT('Ctrl Pts',(-2.62504439302348,18.4790969404991,
89.7022655671137));
#108432=CARTESIAN_POINT('Ctrl Pts',(-2.62288393166343,18.4810488921174,
89.690295347201));
#108433=CARTESIAN_POINT('Ctrl Pts',(-2.62066950419694,18.4830496014828,
89.6780261234856));
#108434=CARTESIAN_POINT('Ctrl Pts',(-2.61852342927454,18.4848687105302,
89.6658723930533));
#108435=CARTESIAN_POINT('Ctrl Pts',(-2.61639927614851,18.4865164796311,
89.6538519002648));
#108436=CARTESIAN_POINT('Ctrl Pts',(-2.61600399982798,18.4868231072933,
89.6516150482686));
#108437=CARTESIAN_POINT('Ctrl Pts',(-2.61560934480965,18.4871237991489,
89.6493828564495));
#108438=CARTESIAN_POINT('Ctrl Pts',(-2.61521482799771,18.4874186178726,
89.6471555062605));
#108439=CARTESIAN_POINT('Ctrl Pts',(-2.61386181693006,18.4884297103889,
89.6395167203683));
#108440=CARTESIAN_POINT('Ctrl Pts',(-2.61245735898484,18.4893710309274,
89.6319494481471));
#108441=CARTESIAN_POINT('Ctrl Pts',(-2.61108133794674,18.4902464545109,
89.6244341372504));
#108442=CARTESIAN_POINT('Ctrl Pts',(-2.60966686342039,18.4911463421755,
89.6167088078211));
#108443=CARTESIAN_POINT('Ctrl Pts',(-2.60828238466218,18.4919765958269,
89.6090383053057));
#108444=CARTESIAN_POINT('Ctrl Pts',(-2.60696055857762,18.4927406253114,
89.6014139729777));
#108445=CARTESIAN_POINT('Ctrl Pts',(-2.60560833229972,18.4935222264298,
89.5936142914267));
#108446=CARTESIAN_POINT('Ctrl Pts',(-2.60432141487863,18.4942345143377,
89.585862782367));
#108447=CARTESIAN_POINT('Ctrl Pts',(-2.60308124819483,18.4948803903919,
89.5781646752645));
#108448=CARTESIAN_POINT('Ctrl Pts',(-2.60178322759524,18.4955563966369,
89.5701074505968));
#108449=CARTESIAN_POINT('Ctrl Pts',(-2.60053598823274,18.4961596313639,
89.5621081813244));
#108450=CARTESIAN_POINT('Ctrl Pts',(-2.59926508718496,18.496692802091,89.554193733652));
#108451=CARTESIAN_POINT('Ctrl Pts',(-2.59892621066429,18.4968349681874,
89.5520834037447));
#108452=CARTESIAN_POINT('Ctrl Pts',(-2.5985853957473,18.4969721506261,89.5499792438945));
#108453=CARTESIAN_POINT('Ctrl Pts',(-2.59824072044925,18.4971043973977,
89.5478820949598));
#108454=CARTESIAN_POINT('Ctrl Pts',(-2.59726065128508,18.4974804353198,
89.541918943509));
#108455=CARTESIAN_POINT('Ctrl Pts',(-2.59625246810505,18.4978217715933,
89.5359236463374));
#108456=CARTESIAN_POINT('Ctrl Pts',(-2.59526777887276,18.4981250455876,
89.5299443033961));
#108457=CARTESIAN_POINT('Ctrl Pts',(-2.59405837501909,18.4984975293373,
89.5226004225468));
#108458=CARTESIAN_POINT('Ctrl Pts',(-2.59288333407229,18.4988123908878,
89.5152823187125));
#108459=CARTESIAN_POINT('Ctrl Pts',(-2.59175342134928,18.4990691230242,
89.5080864873127));
#108460=CARTESIAN_POINT('Ctrl Pts',(-2.59084788868234,18.4992748728413,
89.5023196167698));
#108461=CARTESIAN_POINT('Ctrl Pts',(-2.58996850226688,18.4994434439634,
89.4966331171326));
#108462=CARTESIAN_POINT('Ctrl Pts',(-2.58910961638368,18.4995774188085,
89.4910554511265));
#108463=CARTESIAN_POINT('Ctrl Pts',(-2.58836825370421,18.4996930615873,
89.4862409891632));
#108464=CARTESIAN_POINT('Ctrl Pts',(-2.58764226881396,18.4997830320815,
89.4815087705558));
#108465=CARTESIAN_POINT('Ctrl Pts',(-2.58693155413368,18.4998498277382,
89.4768411884873));
#108466=CARTESIAN_POINT('Ctrl Pts',(-2.58632491345824,18.4999068421258,
89.4728571070868));
#108467=CARTESIAN_POINT('Ctrl Pts',(-2.58573036890802,18.4999470490274,
89.4689203158292));
#108468=CARTESIAN_POINT('Ctrl Pts',(-2.58514232825975,18.4999715297978,
89.4649839703477));
#108469=CARTESIAN_POINT('Ctrl Pts',(-2.58467724319737,18.4999908917938,
89.461870689847));
#108470=CARTESIAN_POINT('Ctrl Pts',(-2.58421667937964,18.5000004361134,
89.4587570869406));
#108471=CARTESIAN_POINT('Ctrl Pts',(-2.58374595121974,18.4999998795018,
89.4555997193086));
#108472=CARTESIAN_POINT('Ctrl Pts',(-2.88564989564837,17.021544099749,90.9249820008041));
#108473=CARTESIAN_POINT('Ctrl Pts',(-2.94425494600512,17.0236905283469,
90.9128867456866));
#108474=CARTESIAN_POINT('Ctrl Pts',(-3.00214169784583,17.0257878045666,
90.8972746305873));
#108475=CARTESIAN_POINT('Ctrl Pts',(-3.05889396442204,17.0278206146711,
90.8782560396643));
#108476=CARTESIAN_POINT('Ctrl Pts',(-3.11563625018334,17.0298530672727,
90.8592407934717));
#108477=CARTESIAN_POINT('Ctrl Pts',(-3.17124404617029,17.0318210616847,
90.8368204011847));
#108478=CARTESIAN_POINT('Ctrl Pts',(-3.22531755484121,17.0337102576852,
90.8111546993795));
#108479=CARTESIAN_POINT('Ctrl Pts',(-3.2793964272523,17.0355996410817,90.7854864517037));
#108480=CARTESIAN_POINT('Ctrl Pts',(-3.33194032250968,17.0374101967068,
90.7565724291325));
#108481=CARTESIAN_POINT('Ctrl Pts',(-3.38257142258566,17.0391287596191,
90.7246197156803));
#108482=CARTESIAN_POINT('Ctrl Pts',(-3.43319372601489,17.0408470239483,
90.6926725536922));
#108483=CARTESIAN_POINT('Ctrl Pts',(-3.48190353970458,17.04247331515,90.6576879833429));
#108484=CARTESIAN_POINT('Ctrl Pts',(-3.52835092027089,17.0439958500997,
90.6199171167676));
#108485=CARTESIAN_POINT('Ctrl Pts',(-3.57480482369066,17.0455185988672,
90.5821409458279));
#108486=CARTESIAN_POINT('Ctrl Pts',(-3.6189953282331,17.0469375512594,90.5415779633663));
#108487=CARTESIAN_POINT('Ctrl Pts',(-3.66060520918311,17.0482424701167,
90.4985198337093));
#108488=CARTESIAN_POINT('Ctrl Pts',(-3.69259236151813,17.0492456125751,
90.4654193556219));
#108489=CARTESIAN_POINT('Ctrl Pts',(-3.72305509711362,17.0501813960177,
90.4308452036344));
#108490=CARTESIAN_POINT('Ctrl Pts',(-3.7518642681655,17.0510458502037,90.3949445258879));
#108491=CARTESIAN_POINT('Ctrl Pts',(-3.78946888608619,17.0521742224611,
90.3480833625686));
#108492=CARTESIAN_POINT('Ctrl Pts',(-3.82425641745817,17.0531809947735,
90.2989589153202));
#108493=CARTESIAN_POINT('Ctrl Pts',(-3.85597615794192,17.0540585932871,
90.2479252300767));
#108494=CARTESIAN_POINT('Ctrl Pts',(-3.88769401396993,17.0549361396629,
90.1968945767219));
#108495=CARTESIAN_POINT('Ctrl Pts',(-3.91634422361392,17.0556845214828,
90.1439552671422));
#108496=CARTESIAN_POINT('Ctrl Pts',(-3.94172033754719,17.0562980686622,
90.0894887958083));
#108497=CARTESIAN_POINT('Ctrl Pts',(-3.96710126713341,17.0569117322751,
90.0350119883125));
#108498=CARTESIAN_POINT('Ctrl Pts',(-3.98920668027896,17.0573905057506,
89.9790078174381));
#108499=CARTESIAN_POINT('Ctrl Pts',(-4.00787722915267,17.0577306973398,
89.921880016422));
#108500=CARTESIAN_POINT('Ctrl Pts',(-4.02654503603207,17.0580708389678,
89.8647606053095));
#108501=CARTESIAN_POINT('Ctrl Pts',(-4.04177885889447,17.0582724371425,
89.806518291553));
#108502=CARTESIAN_POINT('Ctrl Pts',(-4.05346891781446,17.0583338318022,
89.7475728198879));
#108503=CARTESIAN_POINT('Ctrl Pts',(-4.06516020881029,17.0583952329326,
89.6886211356542));
#108504=CARTESIAN_POINT('Ctrl Pts',(-4.07330690665017,17.0583164006063,
89.6289665549535));
#108505=CARTESIAN_POINT('Ctrl Pts',(-4.07785029379567,17.0580977249397,
89.5690390908458));
#108506=CARTESIAN_POINT('Ctrl Pts',(-4.08125199755465,17.0579339991084,
89.524170477762));
#108507=CARTESIAN_POINT('Ctrl Pts',(-4.08263482891519,17.057691923133,89.4791491395646));
#108508=CARTESIAN_POINT('Ctrl Pts',(-4.08199319731286,17.0573724106553,
89.4341571731456));
#108509=CARTESIAN_POINT('Ctrl Pts',(-4.0811362969349,17.0569457010576,89.3740703057139));
#108510=CARTESIAN_POINT('Ctrl Pts',(-4.07666673783311,17.0563806968148,
89.3140361496127));
#108511=CARTESIAN_POINT('Ctrl Pts',(-4.06861674219757,17.0556812172046,
89.2544873773602));
#108512=CARTESIAN_POINT('Ctrl Pts',(-4.0605672245926,17.0549817791313,89.1949421412753));
#108513=CARTESIAN_POINT('Ctrl Pts',(-4.04893775211773,17.054147886678,89.135882645154));
#108514=CARTESIAN_POINT('Ctrl Pts',(-4.03381213850186,17.0531853114299,
89.0777344865986));
#108515=CARTESIAN_POINT('Ctrl Pts',(-4.01868365241601,17.0522225533814,
89.0195752852621));
#108516=CARTESIAN_POINT('Ctrl Pts',(-4.00005780075606,17.051131070441,88.9623281724327));
#108517=CARTESIAN_POINT('Ctrl Pts',(-3.97806886527228,17.0499185028006,
88.9064058416279));
#108518=CARTESIAN_POINT('Ctrl Pts',(-3.95608315669126,17.048706113106,88.8504917174925));
#108519=CARTESIAN_POINT('Ctrl Pts',(-3.93073550530722,17.0473726828737,
88.79590237483));
#108520=CARTESIAN_POINT('Ctrl Pts',(-3.90220859640684,17.0459275976915,
88.743031232164));
#108521=CARTESIAN_POINT('Ctrl Pts',(-3.87367867435884,17.0444823598725,
88.6901545049968));
#108522=CARTESIAN_POINT('Ctrl Pts',(-3.84196902067873,17.042925453691,88.6389967088623));
#108523=CARTESIAN_POINT('Ctrl Pts',(-3.80730821890185,17.0412678759289,
88.5899266093886));
#108524=CARTESIAN_POINT('Ctrl Pts',(-3.78135715586258,17.0400268225547,
88.5531870886763));
#108525=CARTESIAN_POINT('Ctrl Pts',(-3.75375272349364,17.0387293695425,
88.5176173955231));
#108526=CARTESIAN_POINT('Ctrl Pts',(-3.72460657631882,17.0373806672224,
88.4833613981499));
#108527=CARTESIAN_POINT('Ctrl Pts',(-3.68568139893112,17.0355794522373,
88.4376119285427));
#108528=CARTESIAN_POINT('Ctrl Pts',(-3.6440051618024,17.0336866954822,88.3942070434139));
#108529=CARTESIAN_POINT('Ctrl Pts',(-3.59987823703332,17.031715959433,88.3534595674234));
#108530=CARTESIAN_POINT('Ctrl Pts',(-3.55575391791031,17.0297453397537,
88.3127144975263));
#108531=CARTESIAN_POINT('Ctrl Pts',(-3.50917950754176,17.027696763826,88.2746268057133));
#108532=CARTESIAN_POINT('Ctrl Pts',(-3.46049063955607,17.0255848993722,
88.2394709635901));
#108533=CARTESIAN_POINT('Ctrl Pts',(-3.4117925185039,17.0234726335696,88.2043084402816));
#108534=CARTESIAN_POINT('Ctrl Pts',(-3.36097947365895,17.021297069954,88.1720791269206));
#108535=CARTESIAN_POINT('Ctrl Pts',(-3.30841782215132,17.0190737780021,
88.1430153674807));
#108536=CARTESIAN_POINT('Ctrl Pts',(-3.25586388483155,17.0168508123506,
88.1139558735707));
#108537=CARTESIAN_POINT('Ctrl Pts',(-3.20156222001496,17.0145801479348,
88.0880612053631));
#108538=CARTESIAN_POINT('Ctrl Pts',(-3.1459041800945,17.0122780126348,88.065517987308));
#108539=CARTESIAN_POINT('Ctrl Pts',(-3.09024028320291,17.009975635078,88.0429723969993));
#108540=CARTESIAN_POINT('Ctrl Pts',(-3.03322011233942,17.0076417960823,
88.0237791198216));
#108541=CARTESIAN_POINT('Ctrl Pts',(-2.97525469926286,17.0052931566727,
88.0080765148966));
#108542=CARTESIAN_POINT('Ctrl Pts',(-2.93186940227286,17.0035352736024,
87.9963236067048));
#108543=CARTESIAN_POINT('Ctrl Pts',(-2.88795501514177,17.0017691095523,
87.9865252034533));
#108544=CARTESIAN_POINT('Ctrl Pts',(-2.84368904488424,17.0000017248341,
87.9787209138959));
#108545=CARTESIAN_POINT('Ctrl Pts',(4.99091733589909,16.72092210659,92.8589087628099));
#108546=CARTESIAN_POINT('Ctrl Pts',(4.9667657052791,16.72092210659,92.8566764327501));
#108547=CARTESIAN_POINT('Ctrl Pts',(4.83237115732909,16.72092210659,92.84370830857));
#108548=CARTESIAN_POINT('Ctrl Pts',(4.58105099422909,16.72092210659,92.81384884849));
#108549=CARTESIAN_POINT('Ctrl Pts',(4.23026429059909,16.72092210659,92.76024569411));
#108550=CARTESIAN_POINT('Ctrl Pts',(3.85488118854909,16.72092210659,92.69069139225));
#108551=CARTESIAN_POINT('Ctrl Pts',(3.45147771125909,16.72092210659,92.60420128478));
#108552=CARTESIAN_POINT('Ctrl Pts',(3.01590860903909,16.72092210659,92.4996154625501));
#108553=CARTESIAN_POINT('Ctrl Pts',(2.54470817102909,16.72092210659,92.37611183637));
#108554=CARTESIAN_POINT('Ctrl Pts',(2.03458068702909,16.72092210659,92.2336813754001));
#108555=CARTESIAN_POINT('Ctrl Pts',(1.48085160723909,16.72092210659,92.0725401253));
#108556=CARTESIAN_POINT('Ctrl Pts',(0.879179917559089,16.72092210659,91.8936980027499));
#108557=CARTESIAN_POINT('Ctrl Pts',(0.223663970489089,16.72092210659,91.6990548324));
#108558=CARTESIAN_POINT('Ctrl Pts',(-0.496523475400911,16.72092210659,91.49034500414));
#108559=CARTESIAN_POINT('Ctrl Pts',(-1.29838121732091,16.72092210659,91.2700006865301));
#108560=CARTESIAN_POINT('Ctrl Pts',(-2.15052846082091,16.72092210659,91.0563866516499));
#108561=CARTESIAN_POINT('Ctrl Pts',(-2.73844970172191,16.72092210659,90.92810809411));
#108562=CARTESIAN_POINT('Ctrl Pts',(-3.02681279946791,16.72092210659,90.8706313150801));
#108563=CARTESIAN_POINT('Ctrl Pts',(4.97075622012909,17.878482928,93.07717336913));
#108564=CARTESIAN_POINT('Ctrl Pts',(4.94601405284909,17.878482928,93.07488634949));
#108565=CARTESIAN_POINT('Ctrl Pts',(4.80837330780909,17.878482928,93.06160460452));
#108566=CARTESIAN_POINT('Ctrl Pts',(4.55138762180909,17.878482928,93.0310672706));
#108567=CARTESIAN_POINT('Ctrl Pts',(4.19349622708909,17.878482928,92.97637036656));
#108568=CARTESIAN_POINT('Ctrl Pts',(3.81168120185909,17.878482928,92.90561486059));
#108569=CARTESIAN_POINT('Ctrl Pts',(3.40266948939909,17.878482928,92.81791383544));
#108570=CARTESIAN_POINT('Ctrl Pts',(2.96229009133909,17.878482928,92.71216580768));
#108571=CARTESIAN_POINT('Ctrl Pts',(2.48719060390909,17.878482928,92.5876337928));
#108572=CARTESIAN_POINT('Ctrl Pts',(1.97426210470909,17.878482928,92.4444164613201));
#108573=CARTESIAN_POINT('Ctrl Pts',(1.41877633195909,17.878482928,92.28276124204));
#108574=CARTESIAN_POINT('Ctrl Pts',(0.816542904509091,17.878482928,92.10375113626));
#108575=CARTESIAN_POINT('Ctrl Pts',(0.161760017919087,17.878482928,91.90932682469));
#108576=CARTESIAN_POINT('Ctrl Pts',(-0.556279413340908,17.878482928,91.70124310188));
#108577=CARTESIAN_POINT('Ctrl Pts',(-1.35427477140091,17.878482928,91.4819669887));
#108578=CARTESIAN_POINT('Ctrl Pts',(-2.20083077152091,17.878482928,91.26976572553));
#108579=CARTESIAN_POINT('Ctrl Pts',(-2.78389374754391,17.878482928,91.14255536753));
#108580=CARTESIAN_POINT('Ctrl Pts',(-3.06965715457391,17.878482928,91.08559680638));
#108581=CARTESIAN_POINT('Ctrl Pts',(5.0479315220591,18.70551127491,92.2416721455));
#108582=CARTESIAN_POINT('Ctrl Pts',(5.02544988667909,18.70551127491,92.23959447365));
#108583=CARTESIAN_POINT('Ctrl Pts',(4.90023535074909,18.70551127491,92.2275132465));
#108584=CARTESIAN_POINT('Ctrl Pts',(4.66493687916909,18.70551127491,92.1995707649));
#108585=CARTESIAN_POINT('Ctrl Pts',(4.33424173121909,18.70551127491,92.1490606559601));
#108586=CARTESIAN_POINT('Ctrl Pts',(3.97704764559909,18.70551127491,92.0829032729701));
#108587=CARTESIAN_POINT('Ctrl Pts',(3.58950385423909,18.70551127491,91.99983755366));
#108588=CARTESIAN_POINT('Ctrl Pts',(3.16753792284909,18.70551127491,91.8985383651201));
#108589=CARTESIAN_POINT('Ctrl Pts',(2.70736371634909,18.70551127491,91.7779429482401));
#108590=CARTESIAN_POINT('Ctrl Pts',(2.20515730198909,18.70551127491,91.63773770054));
#108591=CARTESIAN_POINT('Ctrl Pts',(1.65639602359909,18.70551127491,91.4780499183101));
#108592=CARTESIAN_POINT('Ctrl Pts',(1.05631288796909,18.70551127491,91.2996828402801));
#108593=CARTESIAN_POINT('Ctrl Pts',(0.398723898549089,18.70551127491,91.10442075303));
#108594=CARTESIAN_POINT('Ctrl Pts',(-0.32753797830091,18.70551127491,90.8939403435401));
#108595=CARTESIAN_POINT('Ctrl Pts',(-1.14031826414091,18.70551127491,90.67057522062));
#108596=CARTESIAN_POINT('Ctrl Pts',(-2.00827714201091,18.70551127491,90.45296596887));
#108597=CARTESIAN_POINT('Ctrl Pts',(-2.60993720675791,18.70551127491,90.3216666198201));
#108598=CARTESIAN_POINT('Ctrl Pts',(-2.90565204297691,18.70551127491,90.2627243579));
#108599=CARTESIAN_POINT('Ctrl Pts',(5.15410013561909,18.46962664964,91.09228880238));
#108600=CARTESIAN_POINT('Ctrl Pts',(5.13472827152909,18.46962664964,91.0904991263699));
#108601=CARTESIAN_POINT('Ctrl Pts',(5.02660823810909,18.46962664964,91.08006942904));
#108602=CARTESIAN_POINT('Ctrl Pts',(4.82114446012908,18.46962664964,91.05569663703));
#108603=CARTESIAN_POINT('Ctrl Pts',(4.52786267812909,18.46962664964,91.0109462235));
#108604=CARTESIAN_POINT('Ctrl Pts',(4.20453915676909,18.46962664964,90.9511143919301));
#108605=CARTESIAN_POINT('Ctrl Pts',(3.84652838130909,18.46962664964,90.87442537583));
#108606=CARTESIAN_POINT('Ctrl Pts',(3.44989351020909,18.46962664964,90.77924637184));
#108607=CARTESIAN_POINT('Ctrl Pts',(3.01025173241909,18.46962664964,90.6640664589099));
#108608=CARTESIAN_POINT('Ctrl Pts',(2.52279548879909,18.46962664964,90.5280048783));
#108609=CARTESIAN_POINT('Ctrl Pts',(1.98328497102909,18.46962664964,90.37102366228));
#108610=CARTESIAN_POINT('Ctrl Pts',(1.38615995146909,18.46962664964,90.1935411854399));
#108611=CARTESIAN_POINT('Ctrl Pts',(0.72471065908909,18.46962664964,89.99712658593));
#108612=CARTESIAN_POINT('Ctrl Pts',(-0.0128626817609094,18.46962664964,
89.7833490995701));
#108613=CARTESIAN_POINT('Ctrl Pts',(-0.845982315090913,18.46962664964,89.55435880276));
#108614=CARTESIAN_POINT('Ctrl Pts',(-1.74338472995091,18.46962664964,89.3293098826599));
#108615=CARTESIAN_POINT('Ctrl Pts',(-2.37062846040091,18.46962664964,89.19238538542));
#108616=CARTESIAN_POINT('Ctrl Pts',(-2.68003329087591,18.46962664964,89.1307141835901));
#108617=CARTESIAN_POINT('',(4.96810338032909,18.4999999989654,91.37512691991));
#108618=CARTESIAN_POINT('Ctrl Pts',(4.96810338032909,18.49999999896,91.37512691991));
#108619=CARTESIAN_POINT('Ctrl Pts',(4.88114290831909,18.49999999896,91.36529516959));
#108620=CARTESIAN_POINT('Ctrl Pts',(4.69919234968909,18.50000000048,91.34173652012));
#108621=CARTESIAN_POINT('Ctrl Pts',(4.40440989175909,18.49999999987,91.29429551851));
#108622=CARTESIAN_POINT('Ctrl Pts',(4.08146866854909,18.50000000003,91.23249710617));
#108623=CARTESIAN_POINT('Ctrl Pts',(3.72713024749909,18.49999999999,91.1550615909));
#108624=CARTESIAN_POINT('Ctrl Pts',(3.33778568867909,18.50000000001,91.0605802439));
#108625=CARTESIAN_POINT('Ctrl Pts',(2.90976010514909,18.49999999999,90.9478782426));
#108626=CARTESIAN_POINT('Ctrl Pts',(2.43912217626909,18.50000000005,90.81636240186));
#108627=CARTESIAN_POINT('Ctrl Pts',(1.92237783813909,18.4999999998,90.66612537853));
#108628=CARTESIAN_POINT('Ctrl Pts',(1.35481786031909,18.50000000073,90.49759288502));
#108629=CARTESIAN_POINT('Ctrl Pts',(0.731044259609088,18.49999999728,90.3121755411));
#108630=CARTESIAN_POINT('Ctrl Pts',(0.0458698878690877,18.50000001013,90.11263961256));
#108631=CARTESIAN_POINT('Ctrl Pts',(-0.714595015070913,18.49999996218,89.9005103584));
#108632=CARTESIAN_POINT('Ctrl Pts',(-1.59425516731442,18.5000001411387,
89.6744034239708));
#108633=CARTESIAN_POINT('Ctrl Pts',(-2.24165009651391,18.4999996959444,
89.5259395502124));
#108634=CARTESIAN_POINT('Ctrl Pts',(-2.58355159951403,18.49999969586,89.455639680019));
#108635=CARTESIAN_POINT('',(4.84756322776217,18.0488923264225,92.4405611323625));
#108636=CARTESIAN_POINT('Ctrl Pts',(4.84756322776218,18.0488923264225,92.4405611323624));
#108637=CARTESIAN_POINT('Ctrl Pts',(4.85108865467572,18.0808891883013,92.4094618791462));
#108638=CARTESIAN_POINT('Ctrl Pts',(4.85480491613432,18.1117722156623,92.3766550456964));
#108639=CARTESIAN_POINT('Ctrl Pts',(4.85869826376457,18.1412880203712,92.342267321212));
#108640=CARTESIAN_POINT('Ctrl Pts',(4.86255042152504,18.170491561119,92.3082434034122));
#108641=CARTESIAN_POINT('Ctrl Pts',(4.86657590878541,18.1983559273946,92.272672132448));
#108642=CARTESIAN_POINT('Ctrl Pts',(4.87075610737188,18.2246553376688,92.2357229972551));
#108643=CARTESIAN_POINT('Ctrl Pts',(4.87491517490048,18.2508218034551,92.198960641302));
#108644=CARTESIAN_POINT('Ctrl Pts',(4.87922734699014,18.2754384318051,92.1608347313778));
#108645=CARTESIAN_POINT('Ctrl Pts',(4.88366957173433,18.2983128308262,92.121553735949));
#108646=CARTESIAN_POINT('Ctrl Pts',(4.88809513870236,18.3211014537688,92.0824200392424));
#108647=CARTESIAN_POINT('Ctrl Pts',(4.89264972013234,18.3421603511356,92.0421404780596));
#108648=CARTESIAN_POINT('Ctrl Pts',(4.89730666423195,18.3613381441414,92.0009551042941));
#108649=CARTESIAN_POINT('Ctrl Pts',(4.89909677213828,18.3687099996225,91.9851236359265));
#108650=CARTESIAN_POINT('Ctrl Pts',(4.90090196980804,18.3758043538445,91.9691586349514));
#108651=CARTESIAN_POINT('Ctrl Pts',(4.90272062489739,18.3826143754992,91.9530747754237));
#108652=CARTESIAN_POINT('Ctrl Pts',(4.90745910576851,18.4003577934409,91.9111685002032));
#108653=CARTESIAN_POINT('Ctrl Pts',(4.91228901451279,18.4161672956054,91.868454656171));
#108654=CARTESIAN_POINT('Ctrl Pts',(4.91718001881137,18.429956549144,91.8252042611727));
#108655=CARTESIAN_POINT('Ctrl Pts',(4.92209115163039,18.443802551206,91.7817758727795));
#108656=CARTESIAN_POINT('Ctrl Pts',(4.92706379558328,18.4556114950119,91.7378072895491));
#108657=CARTESIAN_POINT('Ctrl Pts',(4.93206617755245,18.4653477652398,91.6935821240343));
#108658=CARTESIAN_POINT('Ctrl Pts',(4.93708571018732,18.4751174162685,91.6492053325472));
#108659=CARTESIAN_POINT('Ctrl Pts',(4.94213509559067,18.4828002340483,91.604570987581));
#108660=CARTESIAN_POINT('Ctrl Pts',(4.94718251049573,18.4884127970871,91.5599629899558));
#108661=CARTESIAN_POINT('Ctrl Pts',(4.95227349442145,18.4940738074756,91.5149699384352));
#108662=CARTESIAN_POINT('Ctrl Pts',(4.95736238798444,18.4976289148035,91.4700044479895));
#108663=CARTESIAN_POINT('Ctrl Pts',(4.96241815198147,18.499146125442,91.4253433749732));
#108664=CARTESIAN_POINT('Ctrl Pts',(4.96431840339645,18.4997163818196,91.4085571351005));
#108665=CARTESIAN_POINT('Ctrl Pts',(4.96621399740515,18.4999992365987,91.3918136968969));
#108666=CARTESIAN_POINT('Ctrl Pts',(4.96810338032909,18.4999999984587,91.37512691991));
#108667=CARTESIAN_POINT('Ctrl Pts',(4.84756322776218,18.0488923264225,92.4405611323624));
#108668=CARTESIAN_POINT('Ctrl Pts',(4.77863748925725,18.0391235192895,92.4423846537365));
#108669=CARTESIAN_POINT('Ctrl Pts',(4.70997125933779,18.0293209872038,92.4432370767815));
#108670=CARTESIAN_POINT('Ctrl Pts',(4.64157809200293,18.0194976485252,92.4431933791652));
#108671=CARTESIAN_POINT('Ctrl Pts',(4.52594851367706,18.0028897247599,92.4431195013621));
#108672=CARTESIAN_POINT('Ctrl Pts',(4.41109803083324,17.986222594221,92.4404834705022));
#108673=CARTESIAN_POINT('Ctrl Pts',(4.29724836321367,17.9695550215731,92.435660158109));
#108674=CARTESIAN_POINT('Ctrl Pts',(4.17169109641864,17.951173458328,92.4303408459524));
#108675=CARTESIAN_POINT('Ctrl Pts',(4.04735487367925,17.9327914945713,92.4223623638395));
#108676=CARTESIAN_POINT('Ctrl Pts',(3.92427963714316,17.9144809687944,92.4122312825809));
#108677=CARTESIAN_POINT('Ctrl Pts',(3.80178290438126,17.8962565099517,92.4021478215333));
#108678=CARTESIAN_POINT('Ctrl Pts',(3.68053568025839,17.8781028263318,92.3899325406664));
#108679=CARTESIAN_POINT('Ctrl Pts',(3.56046442767764,17.8600832142125,92.3759622120109));
#108680=CARTESIAN_POINT('Ctrl Pts',(3.54683918999336,17.8580384158713,92.3743769112468));
#108681=CARTESIAN_POINT('Ctrl Pts',(3.53322904170923,17.855995335902,92.3727690020822));
#108682=CARTESIAN_POINT('Ctrl Pts',(3.51963383569171,17.8539540606116,92.3711390280173));
#108683=CARTESIAN_POINT('Ctrl Pts',(3.48008197200912,17.8480154788849,92.3663970247009));
#108684=CARTESIAN_POINT('Ctrl Pts',(3.44065660212661,17.8420921781034,92.3614682762439));
#108685=CARTESIAN_POINT('Ctrl Pts',(3.40135667910275,17.8361862228892,92.3563640314303));
#108686=CARTESIAN_POINT('Ctrl Pts',(3.29331967364858,17.8199505240228,92.3423322654026));
#108687=CARTESIAN_POINT('Ctrl Pts',(3.18623194199405,17.8038461336087,92.3269747296614));
#108688=CARTESIAN_POINT('Ctrl Pts',(3.08005801224797,17.787912355629,92.3105213482678));
#108689=CARTESIAN_POINT('Ctrl Pts',(2.93466117010058,17.7660923004868,92.2879897371368));
#108690=CARTESIAN_POINT('Ctrl Pts',(2.79097894314264,17.7445928313063,92.2634039732281));
#108691=CARTESIAN_POINT('Ctrl Pts',(2.64892471577811,17.7234998276821,92.2372815745539));
#108692=CARTESIAN_POINT('Ctrl Pts',(2.63349649122928,17.7212089588895,92.2344444732583));
#108693=CARTESIAN_POINT('Ctrl Pts',(2.61808742790506,17.7189228682825,92.2315892244038));
#108694=CARTESIAN_POINT('Ctrl Pts',(2.6026973852413,17.7166416540508,92.2287164747354));
#108695=CARTESIAN_POINT('Ctrl Pts',(2.52991459082119,17.7058533053713,92.2151306288017));
#108696=CARTESIAN_POINT('Ctrl Pts',(2.45755743279404,17.6951741066982,92.2011535006045));
#108697=CARTESIAN_POINT('Ctrl Pts',(2.38560353455431,17.6846137707613,92.1868376533435));
#108698=CARTESIAN_POINT('Ctrl Pts',(2.33067763417641,17.6765525541516,92.1759096727931));
#108699=CARTESIAN_POINT('Ctrl Pts',(2.27598664675078,17.6685605757371,92.1647842866499));
#108700=CARTESIAN_POINT('Ctrl Pts',(2.22151959346614,17.6606417338181,92.153484228638));
#108701=CARTESIAN_POINT('Ctrl Pts',(2.19428606682382,17.6566823128585,92.1478341996321));
#108702=CARTESIAN_POINT('Ctrl Pts',(2.16710852539423,17.652741173016,92.142140496716));
#108703=CARTESIAN_POINT('Ctrl Pts',(2.13998550900522,17.6488187657813,92.1364059063002));
#108704=CARTESIAN_POINT('Ctrl Pts',(2.12642400081072,17.646857562164,92.1335386110924));
#108705=CARTESIAN_POINT('Ctrl Pts',(2.11287612398475,17.6449010414981,92.1306610936225));
#108706=CARTESIAN_POINT('Ctrl Pts',(2.09934169429784,17.6429492585768,92.1277736994122));
#108707=CARTESIAN_POINT('Ctrl Pts',(2.09454050070415,17.6422568845445,92.1267494273221));
#108708=CARTESIAN_POINT('Ctrl Pts',(2.08974099961185,17.6415651068035,92.1257239123675));
#108709=CARTESIAN_POINT('Ctrl Pts',(2.08494318251133,17.6408739276938,92.1246971698815));
#108710=CARTESIAN_POINT('Ctrl Pts',(2.08297854388802,17.6405908995695,92.1242767332742));
#108711=CARTESIAN_POINT('Ctrl Pts',(2.08101418763385,17.6403079718227,92.1238560908356));
#108712=CARTESIAN_POINT('Ctrl Pts',(2.07905011346576,17.640025144613,92.1234352434809));
#108713=CARTESIAN_POINT('Ctrl Pts',(2.07566985705564,17.6395383867788,92.1227109470202));
#108714=CARTESIAN_POINT('Ctrl Pts',(2.07229043580454,17.6390519266124,92.121986043553));
#108715=CARTESIAN_POINT('Ctrl Pts',(2.0689118489881,17.6385657651584,92.1212605378308));
#108716=CARTESIAN_POINT('Ctrl Pts',(2.06553326217166,17.6380796037045,92.1205350321085));
#108717=CARTESIAN_POINT('Ctrl Pts',(2.06419545146993,17.637887061752,92.1202479150636));
#108718=CARTESIAN_POINT('Ctrl Pts',(2.05877858970523,17.6371081775176,92.1190822184667));
#108719=CARTESIAN_POINT('Ctrl Pts',(1.93197314754368,17.6188749709064,92.0917939695089));
#108720=CARTESIAN_POINT('Ctrl Pts',(1.80308271629193,17.6005065693028,92.0630007856599));
#108721=CARTESIAN_POINT('Ctrl Pts',(1.67211378071565,17.5820272808739,92.0328432618983));
#108722=CARTESIAN_POINT('Ctrl Pts',(1.6228660587514,17.5750785883871,92.0215032495602));
#108723=CARTESIAN_POINT('Ctrl Pts',(1.57332416328396,17.5681142187702,92.0099707585996));
#108724=CARTESIAN_POINT('Ctrl Pts',(1.52348737127662,17.5611354685922,91.9982548760115));
#108725=CARTESIAN_POINT('Ctrl Pts',(1.39072766294977,17.5425448490759,91.9670450590761));
#108726=CARTESIAN_POINT('Ctrl Pts',(1.25587748125058,17.5238521878038,91.9345310659547));
#108727=CARTESIAN_POINT('Ctrl Pts',(1.11891188088551,17.5050819682797,91.9008811477652));
#108728=CARTESIAN_POINT('Ctrl Pts',(1.05127012774792,17.4958121183903,91.8842628183949));
#108729=CARTESIAN_POINT('Ctrl Pts',(0.983111955639909,17.4865233509836,
91.867368051501));
#108730=CARTESIAN_POINT('Ctrl Pts',(0.914431433187615,17.4772185998306,
91.8502208383066));
#108731=CARTESIAN_POINT('Ctrl Pts',(0.771048344925136,17.4577932386337,
91.8144229105225));
#108732=CARTESIAN_POINT('Ctrl Pts',(0.62539050942459,17.4382982430918,91.7775223526176));
#108733=CARTESIAN_POINT('Ctrl Pts',(0.477413059436499,17.4187600360463,
91.7397211622103));
#108734=CARTESIAN_POINT('Ctrl Pts',(0.403227685597623,17.4089649679875,
91.7207703325931));
#108735=CARTESIAN_POINT('Ctrl Pts',(0.328458829786943,17.3991590329485,
91.7015937659605));
#108736=CARTESIAN_POINT('Ctrl Pts',(0.253097736293403,17.3893455114241,
91.682220803364));
#108737=CARTESIAN_POINT('Ctrl Pts',(0.101000508020681,17.3695394105002,
91.6431213983823));
#108738=CARTESIAN_POINT('Ctrl Pts',(-0.0535077743595639,17.3497024578493,
91.6032193796216));
#108739=CARTESIAN_POINT('Ctrl Pts',(-0.210473329951067,17.3298610909504,
91.5627670240531));
#108740=CARTESIAN_POINT('Ctrl Pts',(-0.295423188605298,17.3191229305482,
91.5408741834561));
#108741=CARTESIAN_POINT('Ctrl Pts',(-0.381093334328116,17.3083837371342,
91.5188207794666));
#108742=CARTESIAN_POINT('Ctrl Pts',(-0.467494193863738,17.2976475111883,
91.4966522549976));
#108743=CARTESIAN_POINT('Ctrl Pts',(-0.630669617962847,17.277371228853,
91.4547850976415));
#108744=CARTESIAN_POINT('Ctrl Pts',(-0.796449849872686,17.2571056016649,
91.4125048865914));
#108745=CARTESIAN_POINT('Ctrl Pts',(-0.964904430483136,17.23687674083,91.3701121771337));
#108746=CARTESIAN_POINT('Ctrl Pts',(-1.06436517031682,17.2249330023022,
91.345082224069));
#108747=CARTESIAN_POINT('Ctrl Pts',(-1.16475869454555,17.2130020596482,
91.3200138638997));
#108748=CARTESIAN_POINT('Ctrl Pts',(-1.26610367830689,17.2010890878669,
91.2949763539329));
#108749=CARTESIAN_POINT('Ctrl Pts',(-1.43884669881289,17.1807833691985,
91.2522997957345));
#108750=CARTESIAN_POINT('Ctrl Pts',(-1.61435350422044,17.1605299420458,
91.2097102767348));
#108751=CARTESIAN_POINT('Ctrl Pts',(-1.79267599243096,17.1403533403081,
91.167573167666));
#108752=CARTESIAN_POINT('Ctrl Pts',(-1.91617722419394,17.1263795830304,
91.1383901693513));
#108753=CARTESIAN_POINT('Ctrl Pts',(-2.04102934044662,17.1124426471024,
91.1094251287446));
#108754=CARTESIAN_POINT('Ctrl Pts',(-2.16725422868345,17.0985502660013,
91.0808133862865));
#108755=CARTESIAN_POINT('Ctrl Pts',(-2.35033670000424,17.0784001078191,
91.039313579147));
#108756=CARTESIAN_POINT('Ctrl Pts',(-2.53630681046979,17.0583437581363,
90.9985550023606));
#108757=CARTESIAN_POINT('Ctrl Pts',(-2.72521885022047,17.0384034578628,
90.9589637064745));
#108758=CARTESIAN_POINT('Ctrl Pts',(-2.77851356008927,17.0327780222411,
90.9477944520936));
#108759=CARTESIAN_POINT('Ctrl Pts',(-2.8320424923009,17.0271618127094,90.9367184053569));
#108760=CARTESIAN_POINT('Ctrl Pts',(-2.88580705358031,17.0215553046092,
90.9257458669384));
#108761=CARTESIAN_POINT('Ctrl Pts',(7.13360610883155,18.0489603905536,92.656111537346));
#108762=CARTESIAN_POINT('Ctrl Pts',(7.08720655217987,18.0489603905536,92.6528812781694));
#108763=CARTESIAN_POINT('Ctrl Pts',(6.78071640479514,18.0489603905535,92.630985806519));
#108764=CARTESIAN_POINT('Ctrl Pts',(6.2119828023362,18.0489603905535,92.583698020234));
#108765=CARTESIAN_POINT('Ctrl Pts',(5.49686859880516,18.0489603905535,92.5126619062047));
#108766=CARTESIAN_POINT('Ctrl Pts',(5.04175854429137,18.0489603905536,92.4626226012838));
#108767=CARTESIAN_POINT('Ctrl Pts',(4.84744750318331,18.0489603905535,92.4406180506049));
#108768=CARTESIAN_POINT('Ctrl Pts',(7.15347472990633,18.3413983276278,92.3707114414248));
#108769=CARTESIAN_POINT('Ctrl Pts',(7.10741885836741,18.3413983276278,92.3675051220259));
#108770=CARTESIAN_POINT('Ctrl Pts',(6.80316531209303,18.3413983276278,92.3457695710735));
#108771=CARTESIAN_POINT('Ctrl Pts',(6.23816628212326,18.3413983276278,92.2987954908767));
#108772=CARTESIAN_POINT('Ctrl Pts',(5.52672801243274,18.3413983276278,92.2281285588862));
#108773=CARTESIAN_POINT('Ctrl Pts',(5.07333129942109,18.3413983276278,92.178278547464));
#108774=CARTESIAN_POINT('Ctrl Pts',(4.87963860009015,18.3413983276278,92.1563440553926));
#108775=CARTESIAN_POINT('Ctrl Pts',(7.17966409107166,18.5000186763427,91.9945179370873));
#108776=CARTESIAN_POINT('Ctrl Pts',(7.1340612400775,18.5000186763427,91.99134317335));
#108777=CARTESIAN_POINT('Ctrl Pts',(6.83275581758214,18.5000186763427,91.9698184181487));
#108778=CARTESIAN_POINT('Ctrl Pts',(6.27267942755774,18.5000186763427,91.9232578423394));
#108779=CARTESIAN_POINT('Ctrl Pts',(5.56608650463578,18.5000186763427,91.8530775390801));
#108780=CARTESIAN_POINT('Ctrl Pts',(5.11494819291141,18.5000186763427,91.8034770404832));
#108781=CARTESIAN_POINT('Ctrl Pts',(4.92207054642514,18.5000186763427,91.7816348945371));
#108782=CARTESIAN_POINT('Ctrl Pts',(7.20807595092437,18.4999999984374,91.5863996536418));
#108783=CARTESIAN_POINT('Ctrl Pts',(7.16296456500068,18.4999999984374,91.5832591234633));
#108784=CARTESIAN_POINT('Ctrl Pts',(6.86485745189238,18.4999999984374,91.5619630527001));
#108785=CARTESIAN_POINT('Ctrl Pts',(6.31012145010241,18.4999999984374,91.5158510723617));
#108786=CARTESIAN_POINT('Ctrl Pts',(5.60878506293612,18.4999999984374,91.4461986944349));
#108787=CARTESIAN_POINT('Ctrl Pts',(5.16009680642433,18.4999999984374,91.3968688829852));
#108788=CARTESIAN_POINT('Ctrl Pts',(4.96810338033001,18.4999999984374,91.3751269199019));
#108789=CARTESIAN_POINT('Ctrl Pts',(6.72284172768286,18.2005852686258,92.4518051511202));
#108790=CARTESIAN_POINT('Ctrl Pts',(6.56248534649459,18.1888402301925,92.4546733255583));
#108791=CARTESIAN_POINT('Ctrl Pts',(6.39755478889078,18.1764291564116,92.4565176179318));
#108792=CARTESIAN_POINT('Ctrl Pts',(6.22811698030556,18.1633144621374,92.4572506935924));
#108793=CARTESIAN_POINT('Ctrl Pts',(6.05247392496364,18.1497194741508,92.4580106163623));
#108794=CARTESIAN_POINT('Ctrl Pts',(5.87198765880911,18.1353682168452,92.4575754540388));
#108795=CARTESIAN_POINT('Ctrl Pts',(5.6867391554217,18.1202251711888,92.4558938992821));
#108796=CARTESIAN_POINT('Ctrl Pts',(5.60442573979155,18.1134965024642,92.4551467163734));
#108797=CARTESIAN_POINT('Ctrl Pts',(5.52117232550561,18.1066116018656,92.4541540424841));
#108798=CARTESIAN_POINT('Ctrl Pts',(5.43698724844798,18.0995678722315,92.4529144738207));
#108799=CARTESIAN_POINT('Ctrl Pts',(5.25646043165824,18.0844632701615,92.4502563378088));
#108800=CARTESIAN_POINT('Ctrl Pts',(5.07164929495735,18.0686277269766,92.4464594893415));
#108801=CARTESIAN_POINT('Ctrl Pts',(4.88262110769245,18.0520415606046,92.441552020789));
#108802=CARTESIAN_POINT('Ctrl Pts',(4.87094861310268,18.0510173644779,92.4412489845013));
#108803=CARTESIAN_POINT('Ctrl Pts',(4.8592600399789,18.0499903089639,92.4409417297409));
#108804=CARTESIAN_POINT('Ctrl Pts',(4.8475554046566,18.0489603905536,92.4406302697285));
#108805=CARTESIAN_POINT('Ctrl Pts',(7.18082400639694,18.5000000000005,91.584560428554));
#108806=CARTESIAN_POINT('Ctrl Pts',(7.14487677550867,18.5000000000002,91.5820310344745));
#108807=CARTESIAN_POINT('Ctrl Pts',(7.10884978221285,18.4999999999997,91.5794443189311));
#108808=CARTESIAN_POINT('Ctrl Pts',(7.07274752685978,18.4999999999993,91.5768011237233));
#108809=CARTESIAN_POINT('Ctrl Pts',(6.88293336141999,18.499999999997,91.5629040447862));
#108810=CARTESIAN_POINT('Ctrl Pts',(6.69103906347306,18.5000000000007,91.5474409142852));
#108811=CARTESIAN_POINT('Ctrl Pts',(6.49769479188341,18.5000000000007,91.5305920653784));
#108812=CARTESIAN_POINT('Ctrl Pts',(6.4366209629962,18.5000000000007,91.5252698300382));
#108813=CARTESIAN_POINT('Ctrl Pts',(6.3754022841721,18.5,91.5198101796099));
#108814=CARTESIAN_POINT('Ctrl Pts',(6.31407521179294,18.4999999999975,91.5142211124991));
#108815=CARTESIAN_POINT('Ctrl Pts',(6.12154672848197,18.4999999999896,91.4966749526676));
#108816=CARTESIAN_POINT('Ctrl Pts',(5.92795006091614,18.5000000000007,91.4778488501071));
#108817=CARTESIAN_POINT('Ctrl Pts',(5.73440041763818,18.5000000000007,91.4580452702999));
#108818=CARTESIAN_POINT('Ctrl Pts',(5.67091376130322,18.5000000000007,91.4515494532882));
#108819=CARTESIAN_POINT('Ctrl Pts',(5.60743228514628,18.4999999999864,91.4449481438494));
#108820=CARTESIAN_POINT('Ctrl Pts',(5.54394144600132,18.499999999908,91.4382493462182));
#108821=CARTESIAN_POINT('Ctrl Pts',(5.35221348028708,18.4999999996713,91.4180204933653));
#108822=CARTESIAN_POINT('Ctrl Pts',(5.1604002946779,18.4999999984373,91.396903250989));
#108823=CARTESIAN_POINT('Ctrl Pts',(4.96810338032909,18.4999999984373,91.37512691991));
#108824=CARTESIAN_POINT('Origin',(155.459720656869,18.5,57.01928063319));
#108825=CARTESIAN_POINT('',(-2.58374595115891,18.49999969586,89.45559971935));
#108826=CARTESIAN_POINT('Origin',(-3.78022426533191,17.,89.66699908298));
#108827=CARTESIAN_POINT('',(-2.84365663233891,17.00000044005,87.97871656704));
#108828=CARTESIAN_POINT('Ctrl Pts',(8.45816176827909,16.26511926842,98.7964653589499));
#108829=CARTESIAN_POINT('Ctrl Pts',(8.71225114275908,16.41477280571,98.6494070076199));
#108830=CARTESIAN_POINT('Ctrl Pts',(9.27881268981909,16.73006084598,98.30341626023));
#108831=CARTESIAN_POINT('Ctrl Pts',(10.1626398113191,17.16069654247,97.6962496853799));
#108832=CARTESIAN_POINT('Ctrl Pts',(11.1008309226691,17.54981639277,96.96627400869));
#108833=CARTESIAN_POINT('Ctrl Pts',(12.0284701745891,17.86984908755,96.1523318668001));
#108834=CARTESIAN_POINT('Ctrl Pts',(12.9325147810891,18.12067756051,95.26102236673));
#108835=CARTESIAN_POINT('Ctrl Pts',(13.8034582743191,18.30536666785,94.2997004316301));
#108836=CARTESIAN_POINT('Ctrl Pts',(14.6483615697391,18.43072561429,93.2588424428));
#108837=CARTESIAN_POINT('Ctrl Pts',(15.4901719996691,18.50141397362,92.10037160054));
#108838=CARTESIAN_POINT('Ctrl Pts',(16.3530907398691,18.51438369082,90.76409474325));
#108839=CARTESIAN_POINT('Ctrl Pts',(17.2403956363891,18.45914837749,89.19684938304));
#108840=CARTESIAN_POINT('Ctrl Pts',(18.1343401599191,18.32423291388,87.36260202144));
#108841=CARTESIAN_POINT('Ctrl Pts',(19.0033848293491,18.10320054974,85.24319884147));
#108842=CARTESIAN_POINT('Ctrl Pts',(19.7639909942691,17.81526535809,82.9702592037509));
#108843=CARTESIAN_POINT('Ctrl Pts',(20.1883444225591,17.59455708305,81.382235884647));
#108844=CARTESIAN_POINT('Ctrl Pts',(20.3703684052891,17.48632437673,80.615759308313));
#108845=CARTESIAN_POINT('Ctrl Pts',(6.31418014116909,15.43220418763,92.79563719768));
#108846=CARTESIAN_POINT('Ctrl Pts',(6.49200941171909,15.56346847277,92.67838236751));
#108847=CARTESIAN_POINT('Ctrl Pts',(6.88387432291909,15.84414338516,92.4035075448201));
#108848=CARTESIAN_POINT('Ctrl Pts',(7.48196966441909,16.24577547329,91.9242120499101));
#108849=CARTESIAN_POINT('Ctrl Pts',(8.10612356461909,16.6365848729,91.3501649846601));
#108850=CARTESIAN_POINT('Ctrl Pts',(8.71750994518909,16.99297183984,90.71045662041));
#108851=CARTESIAN_POINT('Ctrl Pts',(9.3124519476191,17.31472032014,90.0082381109));
#108852=CARTESIAN_POINT('Ctrl Pts',(9.88895414563909,17.60257331209,89.2471181028301));
#108853=CARTESIAN_POINT('Ctrl Pts',(10.4549508437891,17.8618188302,88.41744323317));
#108854=CARTESIAN_POINT('Ctrl Pts',(11.0287137839791,18.10025681166,87.4864837035));
#108855=CARTESIAN_POINT('Ctrl Pts',(11.6304101411391,18.32271215478,86.40251363781));
#108856=CARTESIAN_POINT('Ctrl Pts',(12.2670974264291,18.52555248364,85.11784149556));
#108857=CARTESIAN_POINT('Ctrl Pts',(12.9309003101591,18.69913435731,83.5979370835401));
#108858=CARTESIAN_POINT('Ctrl Pts',(13.6016889453491,18.83244677012,81.8239640921051));
#108859=CARTESIAN_POINT('Ctrl Pts',(14.2139669773891,18.91249476228,79.9062655709491));
#108860=CARTESIAN_POINT('Ctrl Pts',(14.5696327416291,18.93553052461,78.560927762134));
#108861=CARTESIAN_POINT('Ctrl Pts',(14.7249351849991,18.94108956235,77.911474252923));
#108862=CARTESIAN_POINT('Ctrl Pts',(2.54935064044909,19.22183178223,89.2228044174901));
#108863=CARTESIAN_POINT('Ctrl Pts',(2.74816966526909,19.38069675838,89.11271227861));
#108864=CARTESIAN_POINT('Ctrl Pts',(3.18450270870909,19.72231812323,88.8567707992701));
#108865=CARTESIAN_POINT('Ctrl Pts',(3.84607183220909,20.21957457743,88.41774917846));
#108866=CARTESIAN_POINT('Ctrl Pts',(4.53420387286909,20.71569136082,87.89920721743));
#108867=CARTESIAN_POINT('Ctrl Pts',(5.20913049307909,21.18237918094,87.3269794904301));
#108868=CARTESIAN_POINT('Ctrl Pts',(5.86983667115909,21.61932357701,86.70255461879));
#108869=CARTESIAN_POINT('Ctrl Pts',(6.5166169471191,22.02651478544,86.02752892074));
#108870=CARTESIAN_POINT('Ctrl Pts',(7.16026643121909,22.41003287152,85.29176070735));
#108871=CARTESIAN_POINT('Ctrl Pts',(7.82357909374909,22.78105285215,84.46472655768));
#108872=CARTESIAN_POINT('Ctrl Pts',(8.5330095959891,23.14891805727,83.49874325701));
#108873=CARTESIAN_POINT('Ctrl Pts',(9.30144695145909,23.51183300341,82.349167312438));
#108874=CARTESIAN_POINT('Ctrl Pts',(10.1247389211891,23.8583235636,80.982966536629));
#108875=CARTESIAN_POINT('Ctrl Pts',(10.9831261496691,24.1725563834,79.382122199941));
#108876=CARTESIAN_POINT('Ctrl Pts',(11.7956651902091,24.42485648488,77.6476829007421));
#108877=CARTESIAN_POINT('Ctrl Pts',(12.2871279910191,24.55396132786,76.431541471836));
#108878=CARTESIAN_POINT('Ctrl Pts',(12.5064116716291,24.60764795684,75.845400513527));
#108879=CARTESIAN_POINT('Ctrl Pts',(-0.111615554140913,24.89134380645,90.66372486418));
#108880=CARTESIAN_POINT('Ctrl Pts',(0.19025221778909,25.10382403371,90.53297074905));
#108881=CARTESIAN_POINT('Ctrl Pts',(0.85803534504909,25.557842799,90.23007744772));
#108882=CARTESIAN_POINT('Ctrl Pts',(1.88634608190909,26.20614559666,89.71458517922));
#108883=CARTESIAN_POINT('Ctrl Pts',(2.97016886586909,26.83497373368,89.11095423698));
#108884=CARTESIAN_POINT('Ctrl Pts',(4.04244300886909,27.40608121153,88.4506164042799));
#108885=CARTESIAN_POINT('Ctrl Pts',(5.09618479047909,27.91912696323,87.73638641167));
#108886=CARTESIAN_POINT('Ctrl Pts',(6.1271003298391,28.37546235392,86.9710385745999));
#108887=CARTESIAN_POINT('Ctrl Pts',(7.14876251537909,28.78369951161,86.14393771161));
#108888=CARTESIAN_POINT('Ctrl Pts',(8.19441250288909,29.15618061071,85.2220293390399));
#108889=CARTESIAN_POINT('Ctrl Pts',(9.30256349945909,29.50014277728,84.1543224935201));
#108890=CARTESIAN_POINT('Ctrl Pts',(10.4897674388291,29.80928089036,82.894592873641));
#108891=CARTESIAN_POINT('Ctrl Pts',(11.7467525600991,30.0679526902,81.410216850361));
#108892=CARTESIAN_POINT('Ctrl Pts',(13.0428227217091,30.25874444737,79.684901641459));
#108893=CARTESIAN_POINT('Ctrl Pts',(14.2592774845091,30.36290197067,77.829109904896));
#108894=CARTESIAN_POINT('Ctrl Pts',(14.9927419533391,30.38363581186,76.53517273404));
#108895=CARTESIAN_POINT('Ctrl Pts',(15.3204046577991,30.3849546111,75.912812767194));
#108896=CARTESIAN_POINT('Origin',(4.08384678615258,24.7092212049592,99.2019244382985));
#108897=CARTESIAN_POINT('Ctrl Pts',(-1.86852584115091,-0.200657301970986,
95.96514097396));
#108898=CARTESIAN_POINT('Ctrl Pts',(-1.87679361636091,0.397260618019714,
95.95539499753));
#108899=CARTESIAN_POINT('Ctrl Pts',(-1.81764502158091,1.61545674784001,
96.02675082903));
#108900=CARTESIAN_POINT('Ctrl Pts',(-1.51056034305091,3.37210791261202,
96.3812545342701));
#108901=CARTESIAN_POINT('Ctrl Pts',(-1.03549752546091,4.99180633572701,
96.87949059878));
#108902=CARTESIAN_POINT('Ctrl Pts',(-0.47565565201091,6.40141962980201,
97.39996719591));
#108903=CARTESIAN_POINT('Ctrl Pts',(0.128959222729088,7.63825880799903,
97.89143667163));
#108904=CARTESIAN_POINT('Ctrl Pts',(0.78047764573909,8.77397550221601,98.34798763131));
#108905=CARTESIAN_POINT('Ctrl Pts',(1.50402784399909,9.87146117248002,98.77288024243));
#108906=CARTESIAN_POINT('Ctrl Pts',(2.31936621098909,10.95615772036,99.1532466824299));
#108907=CARTESIAN_POINT('Ctrl Pts',(3.21879357943909,12.01000937004,99.45696306809));
#108908=CARTESIAN_POINT('Ctrl Pts',(4.1912683517691,13.0170795927,99.65335362598));
#108909=CARTESIAN_POINT('Ctrl Pts',(5.2757469215191,14.01086777604,99.7165874722901));
#108910=CARTESIAN_POINT('Ctrl Pts',(6.5351502248891,15.02007613619,99.5796055175001));
#108911=CARTESIAN_POINT('Ctrl Pts',(7.73731890968909,15.84006914657,99.1892695249101));
#108912=CARTESIAN_POINT('Ctrl Pts',(8.5044225018091,16.29480837482,98.77493643233));
#108913=CARTESIAN_POINT('Ctrl Pts',(8.76798669870909,16.44357118509,98.6108142135001));
#108914=CARTESIAN_POINT('Ctrl Pts',(-2.76633335145391,-0.277061106735686,
89.62464525754));
#108915=CARTESIAN_POINT('Ctrl Pts',(-2.78010061236391,0.548141406161314,
89.61313564381));
#108916=CARTESIAN_POINT('Ctrl Pts',(-2.67974655644691,2.23539163023501,
89.69951614818));
#108917=CARTESIAN_POINT('Ctrl Pts',(-2.18690829439091,4.52753916756702,
90.11267233159));
#108918=CARTESIAN_POINT('Ctrl Pts',(-1.49193309304091,6.44657897676101,
90.65739218289));
#108919=CARTESIAN_POINT('Ctrl Pts',(-0.744560214060911,7.96637647141302,
91.1950322953901));
#108920=CARTESIAN_POINT('Ctrl Pts',(-0.000714101840911076,9.19387013708703,
91.67997579193));
#108921=CARTESIAN_POINT('Ctrl Pts',(0.743218764159092,10.2409288401,92.11363373692));
#108922=CARTESIAN_POINT('Ctrl Pts',(1.51015059767909,11.1834522333,92.50353807267));
#108923=CARTESIAN_POINT('Ctrl Pts',(2.30766423261909,12.04981733614,92.84138179648));
#108924=CARTESIAN_POINT('Ctrl Pts',(3.11198293474909,12.83069438562,93.10362209738));
#108925=CARTESIAN_POINT('Ctrl Pts',(3.89792431306909,13.52231896489,93.27156799052));
#108926=CARTESIAN_POINT('Ctrl Pts',(4.67814510883909,14.15587807635,93.33468615681));
#108927=CARTESIAN_POINT('Ctrl Pts',(5.4599957395091,14.75400852768,93.25754212455));
#108928=CARTESIAN_POINT('Ctrl Pts',(6.06740744298909,15.2155704877,93.02226348412));
#108929=CARTESIAN_POINT('Ctrl Pts',(6.38629556221909,15.47756556229,92.7840149103));
#108930=CARTESIAN_POINT('Ctrl Pts',(6.48862860801909,15.56565674012,92.69092482342));
#108931=CARTESIAN_POINT('Ctrl Pts',(-8.21314323670391,-0.382376649944286,
86.25787732271));
#108932=CARTESIAN_POINT('Ctrl Pts',(-8.23233050746892,0.756384491850314,
86.2455034223201));
#108933=CARTESIAN_POINT('Ctrl Pts',(-8.09201734092391,3.08654305365901,
86.33967991873));
#108934=CARTESIAN_POINT('Ctrl Pts',(-7.41007493507491,6.21008628532401,
86.78035394901));
#108935=CARTESIAN_POINT('Ctrl Pts',(-6.46595117430891,8.76366891642203,
87.33791220527));
#108936=CARTESIAN_POINT('Ctrl Pts',(-5.47046355413091,10.73360469488,87.86524851897));
#108937=CARTESIAN_POINT('Ctrl Pts',(-4.49835120662891,12.28405501304,88.3219438496));
#108938=CARTESIAN_POINT('Ctrl Pts',(-3.54419140703191,13.57328011442,88.71413997378));
#108939=CARTESIAN_POINT('Ctrl Pts',(-2.58024571757991,14.70275906295,89.05110200106));
#108940=CARTESIAN_POINT('Ctrl Pts',(-1.60151740187091,15.70963613843,89.32658646923));
#108941=CARTESIAN_POINT('Ctrl Pts',(-0.643241151590912,16.5857007526,89.52289696124));
#108942=CARTESIAN_POINT('Ctrl Pts',(0.258320540729089,17.33121239699,89.6296159923701));
#108943=CARTESIAN_POINT('Ctrl Pts',(1.10917349098909,17.98470665617,89.644481026));
#108944=CARTESIAN_POINT('Ctrl Pts',(1.89817703664909,18.57234274478,89.5498507959201));
#108945=CARTESIAN_POINT('Ctrl Pts',(2.42972632590909,19.00878869518,89.36136454575));
#108946=CARTESIAN_POINT('Ctrl Pts',(2.66092298708909,19.26095009207,89.20319983242));
#108947=CARTESIAN_POINT('Ctrl Pts',(2.72918498241909,19.3474423808,89.14448415142));
#108948=CARTESIAN_POINT('Ctrl Pts',(-14.2862958551049,-0.440758245828086,
88.2895013269199));
#108949=CARTESIAN_POINT('Ctrl Pts',(-14.3069203009679,0.872018283434913,
88.2777849287));
#108950=CARTESIAN_POINT('Ctrl Pts',(-14.1566719512549,3.55593252096201,
88.36691425296));
#108951=CARTESIAN_POINT('Ctrl Pts',(-13.4184630337948,7.20801986586801,
88.78415381662));
#108952=CARTESIAN_POINT('Ctrl Pts',(-12.3753852541951,10.27436448968,89.3116591898701));
#108953=CARTESIAN_POINT('Ctrl Pts',(-11.2498853426949,12.71021402121,89.8086449352));
#108954=CARTESIAN_POINT('Ctrl Pts',(-10.1248635377679,14.68333765206,90.23571355337));
#108955=CARTESIAN_POINT('Ctrl Pts',(-8.99406462449291,16.37115120725,90.59773884278));
#108956=CARTESIAN_POINT('Ctrl Pts',(-7.82135743268891,17.89486271208,90.90193228787));
#108957=CARTESIAN_POINT('Ctrl Pts',(-6.59288141698792,19.29990188201,91.1401305760401));
#108958=CARTESIAN_POINT('Ctrl Pts',(-5.34245787553691,20.5707644631,91.2935385755));
#108959=CARTESIAN_POINT('Ctrl Pts',(-4.10638909157991,21.70068773103,91.3503426401699));
#108960=CARTESIAN_POINT('Ctrl Pts',(-2.86088161342491,22.73992455031,91.30356781784));
#108961=CARTESIAN_POINT('Ctrl Pts',(-1.58517092003091,23.72520760639,91.1267204027899));
#108962=CARTESIAN_POINT('Ctrl Pts',(-0.555955217310912,24.48794052554,90.8430628426899));
#108963=CARTESIAN_POINT('Ctrl Pts',(0.0112272501190876,24.92026069551,90.6113068883499));
#108964=CARTESIAN_POINT('Ctrl Pts',(0.19711543522909,25.06537831943,90.52555227838));
#108965=CARTESIAN_POINT('Ctrl Pts',(-2.88573408563691,17.02155009774,90.92539099034));
#108966=CARTESIAN_POINT('Ctrl Pts',(-2.96183724836951,16.4511697392406,
90.9180810733755));
#108967=CARTESIAN_POINT('Ctrl Pts',(-3.04690368141671,15.8694125167351,
90.9103090292122));
#108968=CARTESIAN_POINT('Ctrl Pts',(-3.21791408217198,14.6867343619779,
90.8916484242105));
#108969=CARTESIAN_POINT('Ctrl Pts',(-3.3054459106508,14.0847518433696,90.8810444512336));
#108970=CARTESIAN_POINT('Ctrl Pts',(-3.4784887655845,12.8570207383856,90.8576637353644));
#108971=CARTESIAN_POINT('Ctrl Pts',(-3.56417210664204,12.2314460226776,
90.8449209670427));
#108972=CARTESIAN_POINT('Ctrl Pts',(-3.68821978087207,11.276327570869,90.8246954161696));
#108973=CARTESIAN_POINT('Ctrl Pts',(-3.749143296294,10.794578024796,90.8143068483821));
#108974=CARTESIAN_POINT('Ctrl Pts',(-3.81793083944601,10.2250983369176,
90.8018485621806));
#108975=CARTESIAN_POINT('Ctrl Pts',(-3.8517045182457,9.93848577016983,90.7955508744864));
#108976=CARTESIAN_POINT('Ctrl Pts',(-3.87022234814949,9.77930508945704,
90.7920478215217));
#108977=CARTESIAN_POINT('Ctrl Pts',(-3.87912764195531,9.70212460187384,
90.7903480188845));
#108978=CARTESIAN_POINT('Ctrl Pts',(-3.883863232778,9.66092239636872,90.7894403356581));
#108979=CARTESIAN_POINT('Ctrl Pts',(-3.88463248027389,9.654224946255,90.7892927837586));
#108980=CARTESIAN_POINT('Ctrl Pts',(-4.09696574678048,7.80475446997897,
90.7485457770365));
#108981=CARTESIAN_POINT('Ctrl Pts',(-4.25603208569112,6.03090266346487,
90.7104679588609));
#108982=CARTESIAN_POINT('Ctrl Pts',(-4.35611208131979,4.33088849294624,
90.6854742441241));
#108983=CARTESIAN_POINT('Ctrl Pts',(-2.57931668725691,17.178594621,90.9548069667399));
#108984=CARTESIAN_POINT('Ctrl Pts',(-2.58855911478591,16.91432196328,90.9564366560799));
#108985=CARTESIAN_POINT('Ctrl Pts',(-2.63992248125991,15.8335002163,90.96549340341));
#108986=CARTESIAN_POINT('Ctrl Pts',(-2.75745612978091,13.99840023162,90.98621775678));
#108987=CARTESIAN_POINT('Ctrl Pts',(-2.91746701901391,11.74002179927,91.0144319937601));
#108988=CARTESIAN_POINT('Ctrl Pts',(-3.05666088400791,9.68164557974802,
91.03897562771));
#108989=CARTESIAN_POINT('Ctrl Pts',(-3.17062879146191,7.82843465735002,
91.05907124473));
#108990=CARTESIAN_POINT('Ctrl Pts',(-3.25937285896191,6.15995521921902,
91.0747192182));
#108991=CARTESIAN_POINT('Ctrl Pts',(-3.32585864265091,4.64679437283801,
91.0864424557));
#108992=CARTESIAN_POINT('Ctrl Pts',(-3.37219209949591,3.26397330020801,
91.09461229425));
#108993=CARTESIAN_POINT('Ctrl Pts',(-3.40128627417591,1.99700231674801,
91.09974238223));
#108994=CARTESIAN_POINT('Ctrl Pts',(-3.41591456021491,0.864740186840713,
91.10232174374));
#108995=CARTESIAN_POINT('Ctrl Pts',(-3.41758620937791,0.154606727500314,
91.10261650059));
#108996=CARTESIAN_POINT('Ctrl Pts',(-3.41699227803491,-0.170855566085486,
91.10251177447));
#108997=CARTESIAN_POINT('Ctrl Pts',(-3.46696900914091,17.21014669308,90.95337008737));
#108998=CARTESIAN_POINT('Ctrl Pts',(-3.47583374334891,16.95150699925,90.95493317919));
#108999=CARTESIAN_POINT('Ctrl Pts',(-3.52514838430391,15.88442344691,90.96362868093));
#109000=CARTESIAN_POINT('Ctrl Pts',(-3.64301280433791,14.06098388959,90.98441135825));
#109001=CARTESIAN_POINT('Ctrl Pts',(-3.80271901722991,11.80179697056,91.01257187257));
#109002=CARTESIAN_POINT('Ctrl Pts',(-3.94227500929891,9.73936414453901,
91.03717935929));
#109003=CARTESIAN_POINT('Ctrl Pts',(-4.05662374314791,7.87974649728102,
91.05734212628));
#109004=CARTESIAN_POINT('Ctrl Pts',(-4.14580292510191,6.20322316682401,
91.07306682217));
#109005=CARTESIAN_POINT('Ctrl Pts',(-4.21266473965291,4.68161991703801,
91.08485636406));
#109006=CARTESIAN_POINT('Ctrl Pts',(-4.25933036892191,3.28889700319401,
91.09308477357));
#109007=CARTESIAN_POINT('Ctrl Pts',(-4.28862172007191,2.01347313433601,
91.09824962908));
#109008=CARTESIAN_POINT('Ctrl Pts',(-4.30337790490591,0.871605021979214,
91.1008515426));
#109009=CARTESIAN_POINT('Ctrl Pts',(-4.30506192324491,0.155435836660514,
91.10114848047));
#109010=CARTESIAN_POINT('Ctrl Pts',(-4.30446363595191,-0.172497509604886,
91.10104298627));
#109011=CARTESIAN_POINT('Ctrl Pts',(-4.08960379568891,17.22831955499,90.3208814529201));
#109012=CARTESIAN_POINT('Ctrl Pts',(-4.09825099208891,16.97292424633,90.32240618695));
#109013=CARTESIAN_POINT('Ctrl Pts',(-4.14638564062291,15.91375340138,90.3308936241901));
#109014=CARTESIAN_POINT('Ctrl Pts',(-4.26444057318591,14.09702983202,90.35170989401));
#109015=CARTESIAN_POINT('Ctrl Pts',(-4.42397130343291,11.83737725366,90.3798394660001));
#109016=CARTESIAN_POINT('Ctrl Pts',(-4.56373586770891,9.77260796779402,
90.4044837296301));
#109017=CARTESIAN_POINT('Ctrl Pts',(-4.67830394390391,7.90930027679202,
90.42468517259));
#109018=CARTESIAN_POINT('Ctrl Pts',(-4.76773373617791,6.22814395284801,
90.44045405785));
#109019=CARTESIAN_POINT('Ctrl Pts',(-4.83481213101691,4.70167818148601,
90.45228178868));
#109020=CARTESIAN_POINT('Ctrl Pts',(-4.88166907968991,3.30325216223001,
90.46054393297));
#109021=CARTESIAN_POINT('Ctrl Pts',(-4.91107399741491,2.02295973454401,
90.46572881333));
#109022=CARTESIAN_POINT('Ctrl Pts',(-4.92590384736791,0.875558920813114,
90.46834371599));
#109023=CARTESIAN_POINT('Ctrl Pts',(-4.92759498990891,0.155913373800914,
90.46864191005));
#109024=CARTESIAN_POINT('Ctrl Pts',(-4.92699419374391,-0.173443210183986,
90.4685359734801));
#109025=CARTESIAN_POINT('Ctrl Pts',(-4.07693104810691,17.2223055404,89.4334912894));
#109026=CARTESIAN_POINT('Ctrl Pts',(-4.08565023512491,16.96583655497,89.4350287173199));
#109027=CARTESIAN_POINT('Ctrl Pts',(-4.13417538305591,15.90404712755,89.44358501014));
#109028=CARTESIAN_POINT('Ctrl Pts',(-4.25216726858091,14.08510101065,89.46439016306));
#109029=CARTESIAN_POINT('Ctrl Pts',(-4.41175607196891,11.82560253471,89.49252997492));
#109030=CARTESIAN_POINT('Ctrl Pts',(-4.55145161264891,9.76160646242102,
89.5171620678199));
#109031=CARTESIAN_POINT('Ctrl Pts',(-4.66594710104291,7.89951993168502,
89.5373507115999));
#109032=CARTESIAN_POINT('Ctrl Pts',(-4.75529395788691,6.21989682196801,
89.5531049731));
#109033=CARTESIAN_POINT('Ctrl Pts',(-4.82230067898491,4.69504022343901,
89.5649200659201));
#109034=CARTESIAN_POINT('Ctrl Pts',(-4.86909431359692,3.29850155463401,
89.57317104623));
#109035=CARTESIAN_POINT('Ctrl Pts',(-4.89846164830091,2.01982029771201,
89.57834929969));
#109036=CARTESIAN_POINT('Ctrl Pts',(-4.91326711997491,0.874250441973816,
89.5809599038099));
#109037=CARTESIAN_POINT('Ctrl Pts',(-4.91495590487691,0.155755340611514,
89.58125768215));
#109038=CARTESIAN_POINT('Ctrl Pts',(-4.91435593898191,-0.173130245880086,
89.58115189197));
#109039=CARTESIAN_POINT('Ctrl Pts',(-4.06425830052491,17.21629152582,88.5461011258701));
#109040=CARTESIAN_POINT('Ctrl Pts',(-4.07304947815991,16.95874886361,88.54765124768));
#109041=CARTESIAN_POINT('Ctrl Pts',(-4.12196512548991,15.89434085372,88.55627639609));
#109042=CARTESIAN_POINT('Ctrl Pts',(-4.23989396397591,14.07317218928,88.57707043212));
#109043=CARTESIAN_POINT('Ctrl Pts',(-4.39954084050591,11.81382781576,88.60522048383));
#109044=CARTESIAN_POINT('Ctrl Pts',(-4.53916735758791,9.75060495704802,
88.6298404060201));
#109045=CARTESIAN_POINT('Ctrl Pts',(-4.65359025818291,7.88973958657902,
88.6500162506));
#109046=CARTESIAN_POINT('Ctrl Pts',(-4.74285417959691,6.21164969108801,
88.66575588835));
#109047=CARTESIAN_POINT('Ctrl Pts',(-4.80978922695191,4.68840226539201,
88.67755834316));
#109048=CARTESIAN_POINT('Ctrl Pts',(-4.85651954750292,3.29375094703901,
88.68579815949));
#109049=CARTESIAN_POINT('Ctrl Pts',(-4.88584929918791,2.01668086088001,
88.6909697860501));
#109050=CARTESIAN_POINT('Ctrl Pts',(-4.90063039258292,0.872941963134614,
88.69357609162));
#109051=CARTESIAN_POINT('Ctrl Pts',(-4.90231681984491,0.155597307422214,
88.69387345424));
#109052=CARTESIAN_POINT('Ctrl Pts',(-4.90171768422091,-0.172817281576286,
88.69376781047));
#109053=CARTESIAN_POINT('Ctrl Pts',(-3.42381468683891,17.18966725702,87.9315533205201));
#109054=CARTESIAN_POINT('Ctrl Pts',(-3.43292456964391,16.92737138735,87.93315963865));
#109055=CARTESIAN_POINT('Ctrl Pts',(-3.48356897249791,15.85137081435,87.94208961329));
#109056=CARTESIAN_POINT('Ctrl Pts',(-3.60121869937191,14.02036284834,87.96283443442));
#109057=CARTESIAN_POINT('Ctrl Pts',(-3.76112266788591,11.76170069203,87.99102981839));
#109058=CARTESIAN_POINT('Ctrl Pts',(-3.90044361490791,9.70190087892902,
88.01559586032));
#109059=CARTESIAN_POINT('Ctrl Pts',(-4.01454516658091,7.84644163089602,
88.03571504243));
#109060=CARTESIAN_POINT('Ctrl Pts',(-4.10344192972591,6.17513933245601,
88.05138994027));
#109061=CARTESIAN_POINT('Ctrl Pts',(-4.17005967472791,4.65901577542201,
88.0631364461));
#109062=CARTESIAN_POINT('Ctrl Pts',(-4.21650970155091,3.27271982851301,
88.07132683909));
#109063=CARTESIAN_POINT('Ctrl Pts',(-4.24567307178991,2.00278245593201,
88.0764691281101));
#109064=CARTESIAN_POINT('Ctrl Pts',(-4.26034624162691,0.867149278093414,
88.07905640384));
#109065=CARTESIAN_POINT('Ctrl Pts',(-4.26202223153091,0.154897688548214,
88.07935192608));
#109066=CARTESIAN_POINT('Ctrl Pts',(-4.26142677154591,-0.171431776830586,
88.0792469304201));
#109067=CARTESIAN_POINT('Ctrl Pts',(-2.53648137537091,17.15826657542,87.9553284263299));
#109068=CARTESIAN_POINT('Ctrl Pts',(-2.54596713928091,16.89036476946,87.95700102244));
#109069=CARTESIAN_POINT('Ctrl Pts',(-2.59865043763191,15.80069191927,87.96629050937));
#109070=CARTESIAN_POINT('Ctrl Pts',(-2.71597098007291,13.95807947397,87.9869772863899));
#109071=CARTESIAN_POINT('Ctrl Pts',(-2.87617816305591,11.70022192514,88.01522613526));
#109072=CARTESIAN_POINT('Ctrl Pts',(-3.01513872052991,9.64445925446003,
88.0397286308001));
#109073=CARTESIAN_POINT('Ctrl Pts',(-3.12886127305691,7.79537599108401,
88.05978098512));
#109074=CARTESIAN_POINT('Ctrl Pts',(-3.21732500947791,6.13207898944801,
88.0753795286699));
#109075=CARTESIAN_POINT('Ctrl Pts',(-3.28356852785791,4.62435732819501,
88.08706004825));
#109076=CARTESIAN_POINT('Ctrl Pts',(-3.32968797605691,3.24791571232601,
88.09519215131));
#109077=CARTESIAN_POINT('Ctrl Pts',(-3.35865511590291,1.98639066722401,
88.1002998396201));
#109078=CARTESIAN_POINT('Ctrl Pts',(-3.37320100061691,0.860317381224614,
88.10286467155));
#109079=CARTESIAN_POINT('Ctrl Pts',(-3.37486468069391,0.154072557549214,
88.10315802323));
#109080=CARTESIAN_POINT('Ctrl Pts',(-3.37427355575891,-0.169797711545386,
88.10305379196));
#109081=CARTESIAN_POINT('Ctrl Pts',(-2.84365660865327,16.99999909128,87.978717018185));
#109082=CARTESIAN_POINT('Ctrl Pts',(-2.85128898638368,16.8100157247129,
87.9800628123056));
#109083=CARTESIAN_POINT('Ctrl Pts',(-2.86030160140771,16.62112233734,87.9816519784134));
#109084=CARTESIAN_POINT('Ctrl Pts',(-2.86985949636735,16.433171083534,87.9833372963379));
#109085=CARTESIAN_POINT('Ctrl Pts',(-2.87089428355535,16.4128225078039,
87.983519757581));
#109086=CARTESIAN_POINT('Ctrl Pts',(-2.871935511102,16.3924849781326,87.9837033544802));
#109087=CARTESIAN_POINT('Ctrl Pts',(-2.87298215385083,16.3721583088458,
87.9838879062745));
#109088=CARTESIAN_POINT('Ctrl Pts',(-2.88977696089625,16.0459892421528,
87.9868492909288));
#109089=CARTESIAN_POINT('Ctrl Pts',(-2.90796161402391,15.7226145279182,
87.9900557624761));
#109090=CARTESIAN_POINT('Ctrl Pts',(-2.92728126454367,15.4012022162267,
87.9934623326708));
#109091=CARTESIAN_POINT('Ctrl Pts',(-2.94004101473621,15.1889240074776,
87.9957122172975));
#109092=CARTESIAN_POINT('Ctrl Pts',(-2.95329710436232,14.9775023794641,
87.9980495955924));
#109093=CARTESIAN_POINT('Ctrl Pts',(-2.96698725787661,14.7667019575818,
88.000463539027));
#109094=CARTESIAN_POINT('Ctrl Pts',(-2.98536063308268,14.4837894803185,
88.0037032608026));
#109095=CARTESIAN_POINT('Ctrl Pts',(-3.0041303113058,14.2020331886729,88.0070129077448));
#109096=CARTESIAN_POINT('Ctrl Pts',(-3.02297301800919,13.9229688465034,
88.0103353860029));
#109097=CARTESIAN_POINT('Ctrl Pts',(-3.04601735495912,13.5816775005789,
88.0143987251873));
#109098=CARTESIAN_POINT('Ctrl Pts',(-3.06916808788408,13.2444133997815,
88.0184807898914));
#109099=CARTESIAN_POINT('Ctrl Pts',(-3.09199769385465,12.9141590882853,
88.0225062558434));
#109100=CARTESIAN_POINT('Ctrl Pts',(-3.09890463996465,12.8142428332681,
88.0237241339107));
#109101=CARTESIAN_POINT('Ctrl Pts',(-3.10578251136168,12.7149682011028,
88.0249368870126));
#109102=CARTESIAN_POINT('Ctrl Pts',(-3.1126205328836,12.6164177761549,88.0261426147017));
#109103=CARTESIAN_POINT('Ctrl Pts',(-3.1328805235663,12.3244282460229,88.0297149976884));
#109104=CARTESIAN_POINT('Ctrl Pts',(-3.15280524949456,12.0387689042729,
88.0332282706136));
#109105=CARTESIAN_POINT('Ctrl Pts',(-3.17219919081432,11.759013804942,88.0366479458216));
#109106=CARTESIAN_POINT('Ctrl Pts',(-3.17474417065642,11.7223027993354,
88.0370966944451));
#109107=CARTESIAN_POINT('Ctrl Pts',(-3.17728008219073,11.6856934685625,
88.0375438440236));
#109108=CARTESIAN_POINT('Ctrl Pts',(-3.17980654662979,11.6491848528322,
88.0379893277735));
#109109=CARTESIAN_POINT('Ctrl Pts',(-3.20356570844914,11.3058536364788,
88.0421787081336));
#109110=CARTESIAN_POINT('Ctrl Pts',(-3.22648679759717,10.9714287895626,
88.0462203093649));
#109111=CARTESIAN_POINT('Ctrl Pts',(-3.24849572832879,10.6451066340725,
88.0501010776695));
#109112=CARTESIAN_POINT('Ctrl Pts',(-3.27279220147798,10.2848675299772,
88.0543852014218));
#109113=CARTESIAN_POINT('Ctrl Pts',(-3.29590271860032,9.9345090800762,88.0584602108139));
#109114=CARTESIAN_POINT('Ctrl Pts',(-3.31782060896809,9.59382982703874,
88.0623249255647));
#109115=CARTESIAN_POINT('Ctrl Pts',(-3.33395684807769,9.34301728101119,
88.0651701793853));
#109116=CARTESIAN_POINT('Ctrl Pts',(-3.34944754773256,9.09745133352557,
88.0679016071817));
#109117=CARTESIAN_POINT('Ctrl Pts',(-3.36429765338097,8.85706270226158,
88.0705200814737));
#109118=CARTESIAN_POINT('Ctrl Pts',(-3.37034490299891,8.75917181225816,
88.0715863747404));
#109119=CARTESIAN_POINT('Ctrl Pts',(-3.37628552874775,8.66213886284631,
88.0726338673872));
#109120=CARTESIAN_POINT('Ctrl Pts',(-3.38212037964037,8.56594505080956,
88.0736627090807));
#109121=CARTESIAN_POINT('Origin',(33.1784433940591,111.0724296188,81.627048885766));
#109122=CARTESIAN_POINT('Origin',(-15.9175364833309,75.,72.98888938658));
#109123=CARTESIAN_POINT('',(-11.8763230992193,66.6,72.98888938658));
#109124=CARTESIAN_POINT('',(-12.3474397125099,66.60000000001,72.9889023406097));
#109125=CARTESIAN_POINT('',(-15.9175364833309,66.6,72.98888938658));
#109126=CARTESIAN_POINT('',(-12.9675940002345,76.1753006967198,81.3061780149303));
#109127=CARTESIAN_POINT('Ctrl Pts',(-11.8763230992193,66.6,72.98888938658));
#109128=CARTESIAN_POINT('Ctrl Pts',(-11.8794256424916,66.6,72.8812206761461));
#109129=CARTESIAN_POINT('Ctrl Pts',(-11.8825189875651,66.6020700932764,
72.7735197025896));
#109130=CARTESIAN_POINT('Ctrl Pts',(-11.900761960782,66.626655646913,72.1347020616983));
#109131=CARTESIAN_POINT('Ctrl Pts',(-11.9153598856798,66.6974656030097,
71.6066954305637));
#109132=CARTESIAN_POINT('Ctrl Pts',(-11.9379572243418,66.8792771008636,
70.8237123401298));
#109133=CARTESIAN_POINT('Ctrl Pts',(-11.9456748218442,66.9537189666686,
70.5616499255183));
#109134=CARTESIAN_POINT('Ctrl Pts',(-11.9694331575962,67.2189017455611,
69.7756235539929));
#109135=CARTESIAN_POINT('Ctrl Pts',(-11.9857513677395,67.4491534718115,
69.2666213176648));
#109136=CARTESIAN_POINT('Ctrl Pts',(-12.0167052040164,67.9950043751541,
68.3225914726985));
#109137=CARTESIAN_POINT('Ctrl Pts',(-12.0313527545475,68.305247981938,67.8874572684421));
#109138=CARTESIAN_POINT('Ctrl Pts',(-12.07658598756,69.3568392141455,66.6751650879817));
#109139=CARTESIAN_POINT('Ctrl Pts',(-12.107875343283,70.207495708555,66.0074653700156));
#109140=CARTESIAN_POINT('Ctrl Pts',(-12.1684779816568,72.138815149854,65.0149854075845));
#109141=CARTESIAN_POINT('Ctrl Pts',(-12.2005292908041,73.2062524150642,
64.7092791039551));
#109142=CARTESIAN_POINT('Ctrl Pts',(-12.2520666938747,75.0277649752649,
64.5574415914327));
#109143=CARTESIAN_POINT('Ctrl Pts',(-12.2720637571735,75.7581081018806,
64.5915460803062));
#109144=CARTESIAN_POINT('Ctrl Pts',(-12.3082103090711,76.9989263241938,
64.8128478597517));
#109145=CARTESIAN_POINT('Ctrl Pts',(-12.323785515563,77.5128997370045,64.95591407137));
#109146=CARTESIAN_POINT('Ctrl Pts',(-12.3544290082357,78.5202646589675,
65.3425428320663));
#109147=CARTESIAN_POINT('Ctrl Pts',(-12.3694367591572,79.0103247715392,
65.5877955532602));
#109148=CARTESIAN_POINT('Ctrl Pts',(-12.3925318410277,79.7034362081076,
66.0238511648671));
#109149=CARTESIAN_POINT('Ctrl Pts',(-12.4002783916204,79.9266152453759,
66.1798858198389));
#109150=CARTESIAN_POINT('Ctrl Pts',(-12.4233639007157,80.5619990642387,
66.6717299659978));
#109151=CARTESIAN_POINT('Ctrl Pts',(-12.4389080979838,80.9503678544398,
67.0361195597719));
#109152=CARTESIAN_POINT('Ctrl Pts',(-12.4699035192427,81.6746959344526,
67.8579397968622));
#109153=CARTESIAN_POINT('Ctrl Pts',(-12.4853975164757,82.0041091067518,
68.317628453921));
#109154=CARTESIAN_POINT('Ctrl Pts',(-12.5164577767264,82.5506589458763,
69.2697002216737));
#109155=CARTESIAN_POINT('Ctrl Pts',(-12.5318997793577,82.771643506454,69.7568065604022));
#109156=CARTESIAN_POINT('Ctrl Pts',(-12.5790126465749,83.3011886052007,
71.2994128987627));
#109157=CARTESIAN_POINT('Ctrl Pts',(-12.6085889564851,83.4506698019872,
72.3970740519697));
#109158=CARTESIAN_POINT('Ctrl Pts',(-12.6555902003529,83.3530105295161,
74.0233805265858));
#109159=CARTESIAN_POINT('Ctrl Pts',(-12.671054833758,83.2707593068306,74.5501463571698));
#109160=CARTESIAN_POINT('Ctrl Pts',(-12.7001594794235,83.0144392652775,
75.5547432858472));
#109161=CARTESIAN_POINT('Ctrl Pts',(-12.7141074504808,82.8457938294387,
76.0316455773091));
#109162=CARTESIAN_POINT('Ctrl Pts',(-12.7432694102026,82.4168316491393,
76.9670048874546));
#109163=CARTESIAN_POINT('Ctrl Pts',(-12.7584573263868,82.1541870779306,
77.421990656059));
#109164=CARTESIAN_POINT('Ctrl Pts',(-12.8051857015011,81.2176184601508,
78.7420486803291));
#109165=CARTESIAN_POINT('Ctrl Pts',(-12.8346827098319,80.4160229325183,
79.5022844929333));
#109166=CARTESIAN_POINT('Ctrl Pts',(-12.8830862236364,78.998746325473,80.3989939153691));
#109167=CARTESIAN_POINT('Ctrl Pts',(-12.8999445714155,78.4751645492438,
80.6584971787898));
#109168=CARTESIAN_POINT('Ctrl Pts',(-12.9331626931529,77.3621037193998,
81.0725918226183));
#109169=CARTESIAN_POINT('Ctrl Pts',(-12.9499554666097,76.7741495751895,
81.2216391404873));
#109170=CARTESIAN_POINT('Ctrl Pts',(-12.9672880448682,76.175305272257,81.3062602161754));
#109171=CARTESIAN_POINT('',(-12.9679003706342,82.2015397612608,68.6647904662762));
#109172=CARTESIAN_POINT('Origin',(-12.9678999777142,75.,72.98888938658));
#109173=CARTESIAN_POINT('Ctrl Pts',(-12.9685679372243,82.2015206898752,
68.6647594448114));
#109174=CARTESIAN_POINT('Ctrl Pts',(-12.9512109568237,81.8931531007796,
68.1511958833865));
#109175=CARTESIAN_POINT('Ctrl Pts',(-12.9337253072393,81.5307214119955,
67.6720706009241));
#109176=CARTESIAN_POINT('Ctrl Pts',(-12.9004039599864,80.7129408499974,
66.8021108354724));
#109177=CARTESIAN_POINT('Ctrl Pts',(-12.8840699634639,80.2605796608795,
66.4131592514108));
#109178=CARTESIAN_POINT('Ctrl Pts',(-12.8500679374412,79.2785032522322,
65.7354507606752));
#109179=CARTESIAN_POINT('Ctrl Pts',(-12.8324865342193,78.7511883261723,
65.4492260302083));
#109180=CARTESIAN_POINT('Ctrl Pts',(-12.7926048066351,77.4689065878324,
64.9212923585615));
#109181=CARTESIAN_POINT('Ctrl Pts',(-12.7714181795333,76.7012242270995,
64.7252666633013));
#109182=CARTESIAN_POINT('Ctrl Pts',(-12.7339958847424,75.3905477198483,
64.58124318139));
#109183=CARTESIAN_POINT('Ctrl Pts',(-12.7185507516877,74.8592910802119,
64.5733546507774));
#109184=CARTESIAN_POINT('Ctrl Pts',(-12.6876698145568,73.798389978797,64.6581350928868));
#109185=CARTESIAN_POINT('Ctrl Pts',(-12.6727423882883,73.2711981139356,
64.7513784901045));
#109186=CARTESIAN_POINT('Ctrl Pts',(-12.6274069825214,71.6977037102964,
65.1874891058586));
#109187=CARTESIAN_POINT('Ctrl Pts',(-12.5953164764482,70.7068140489425,
65.6857855976466));
#109188=CARTESIAN_POINT('Ctrl Pts',(-12.552215583075,69.510898997823,66.6167862897298));
#109189=CARTESIAN_POINT('Ctrl Pts',(-12.5407531485254,69.2013466168084,
66.8971280564601));
#109190=CARTESIAN_POINT('Ctrl Pts',(-12.4984264527959,68.1527467713009,
67.999432534347));
#109191=CARTESIAN_POINT('Ctrl Pts',(-12.4657516690204,67.5568226075881,
68.9418400910791));
#109192=CARTESIAN_POINT('Ctrl Pts',(-12.4205238030014,66.9788430599908,
70.4440307130539));
#109193=CARTESIAN_POINT('Ctrl Pts',(-12.4066962527423,66.8403263929509,
70.9309779345929));
#109194=CARTESIAN_POINT('Ctrl Pts',(-12.3777612751823,66.6490141176107,
71.9422119441106));
#109195=CARTESIAN_POINT('Ctrl Pts',(-12.3626760155638,66.6,72.4649816273617));
#109196=CARTESIAN_POINT('Ctrl Pts',(-12.3474400892301,66.6,72.9888893865802));
#109197=CARTESIAN_POINT('Origin',(-15.9175364833309,75.,72.98888938658));
#109198=CARTESIAN_POINT('',(-10.8470411184477,66.6,72.98888938658));
#109199=CARTESIAN_POINT('Ctrl Pts',(-12.3474397125099,66.60000000001,72.9889023406097));
#109200=CARTESIAN_POINT('Ctrl Pts',(-12.3383509580487,66.6000004819755,
73.3014313418396));
#109201=CARTESIAN_POINT('Ctrl Pts',(-12.3292493655496,66.6174420671942,
73.6137087450362));
#109202=CARTESIAN_POINT('Ctrl Pts',(-12.3116088837576,66.6864578250661,
74.2296180169422));
#109203=CARTESIAN_POINT('Ctrl Pts',(-12.3030894322364,66.7373957872832,
74.5328343294614));
#109204=CARTESIAN_POINT('Ctrl Pts',(-12.2774181628908,66.9403542840846,
75.4349814090962));
#109205=CARTESIAN_POINT('Ctrl Pts',(-12.2601792027666,67.1418836663396,
76.0205964076443));
#109206=CARTESIAN_POINT('Ctrl Pts',(-12.2285210830866,67.6106647331949,
77.0122701558534));
#109207=CARTESIAN_POINT('Ctrl Pts',(-12.2144350846763,67.8522989305133,
77.4273838901755));
#109208=CARTESIAN_POINT('Ctrl Pts',(-12.1771390318329,68.6025865050576,
78.4947112709424));
#109209=CARTESIAN_POINT('Ctrl Pts',(-12.1549803016089,69.1740505608182,
79.0962064068379));
#109210=CARTESIAN_POINT('Ctrl Pts',(-12.1154884969256,70.2621959758581,
79.9475357845932));
#109211=CARTESIAN_POINT('Ctrl Pts',(-12.0991485817419,70.7333585456637,
80.2459755813694));
#109212=CARTESIAN_POINT('Ctrl Pts',(-12.0513754127791,72.2171434724447,
80.9910458322196));
#109213=CARTESIAN_POINT('Ctrl Pts',(-12.0219258723555,73.2917784530345,
81.2871298976208));
#109214=CARTESIAN_POINT('Ctrl Pts',(-11.9777841360304,74.8094404338569,
81.3971062763845));
#109215=CARTESIAN_POINT('Ctrl Pts',(-11.9655484061879,75.2276607939307,
81.3961835994181));
#109216=CARTESIAN_POINT('Ctrl Pts',(-11.9389370364639,76.1605855364148,
81.3244399458181));
#109217=CARTESIAN_POINT('Ctrl Pts',(-11.924798111761,76.6723223983046,81.2370235285619));
#109218=CARTESIAN_POINT('Ctrl Pts',(-11.8883656217225,77.9306403582969,
80.9000800766076));
#109219=CARTESIAN_POINT('Ctrl Pts',(-11.865523905305,78.6563677532716,80.5919473838761));
#109220=CARTESIAN_POINT('Ctrl Pts',(-11.8198903226285,80.0097942736113,
79.7781119315346));
#109221=CARTESIAN_POINT('Ctrl Pts',(-11.7984831150536,80.629293919866,79.2740008508438));
#109222=CARTESIAN_POINT('Ctrl Pts',(-11.7571269120672,81.6219728872003,
78.1999760414976));
#109223=CARTESIAN_POINT('Ctrl Pts',(-11.7375490091182,82.0151282350308,
77.6572813161279));
#109224=CARTESIAN_POINT('Ctrl Pts',(-11.6955578934579,82.7236236098708,
76.3842391094113));
#109225=CARTESIAN_POINT('Ctrl Pts',(-11.6743352616283,83.0082997423443,
75.6440530719495));
#109226=CARTESIAN_POINT('Ctrl Pts',(-11.6335629805257,83.331436047082,74.2417196239464));
#109227=CARTESIAN_POINT('Ctrl Pts',(-11.6144948961672,83.4033738342296,
73.5936053899774));
#109228=CARTESIAN_POINT('Ctrl Pts',(-11.56715692772,83.3945360094672,71.9503684339933));
#109229=CARTESIAN_POINT('Ctrl Pts',(-11.5406728190485,83.2130361389485,
70.9658202476124));
#109230=CARTESIAN_POINT('Ctrl Pts',(-11.4939427868069,82.6428557649125,
69.4474468619433));
#109231=CARTESIAN_POINT('Ctrl Pts',(-11.4753999707528,82.3565430009873,
68.8856748376966));
#109232=CARTESIAN_POINT('Ctrl Pts',(-11.4445545009936,81.7515669255104,
67.96924674705));
#109233=CARTESIAN_POINT('Ctrl Pts',(-11.4316851221503,81.4604832241331,
67.5997677967607));
#109234=CARTESIAN_POINT('Ctrl Pts',(-11.3874716606328,80.3846960034667,
66.447465324252));
#109235=CARTESIAN_POINT('Ctrl Pts',(-11.3546465824438,79.4768262218802,
65.7956130795486));
#109236=CARTESIAN_POINT('Ctrl Pts',(-11.3085845959489,77.9678758003413,
65.1114450860482));
#109237=CARTESIAN_POINT('Ctrl Pts',(-11.293383090747,77.4459446868923,64.9340917042076));
#109238=CARTESIAN_POINT('Ctrl Pts',(-11.2618693998766,76.3714034649417,
64.6831288206911));
#109239=CARTESIAN_POINT('Ctrl Pts',(-11.2456263390625,75.8212568036285,
64.6108272221902));
#109240=CARTESIAN_POINT('Ctrl Pts',(-11.2069496675176,74.479608726194,64.5679980523296));
#109241=CARTESIAN_POINT('Ctrl Pts',(-11.1857392457571,73.6915951787152,
64.6540052900576));
#109242=CARTESIAN_POINT('Ctrl Pts',(-11.1482998568107,72.411316536888,64.9800136749814));
#109243=CARTESIAN_POINT('Ctrl Pts',(-11.1328125992985,71.9091107365945,
65.1601119126757));
#109244=CARTESIAN_POINT('Ctrl Pts',(-11.0849228184656,70.4163518701671,
65.8616173735125));
#109245=CARTESIAN_POINT('Ctrl Pts',(-11.0551958568246,69.5102241308512,
66.5336426772762));
#109246=CARTESIAN_POINT('Ctrl Pts',(-11.0088266082509,68.4329835720872,
67.728112221449));
#109247=CARTESIAN_POINT('Ctrl Pts',(-10.9943850016843,68.1365353688722,
68.1212073427534));
#109248=CARTESIAN_POINT('Ctrl Pts',(-10.9552963721232,67.4125776501631,
69.2799215107));
#109249=CARTESIAN_POINT('Ctrl Pts',(-10.9318432305127,67.0677511953457,
70.0897711514179));
#109250=CARTESIAN_POINT('Ctrl Pts',(-10.8868982190948,66.6852367557343,
71.6092142509929));
#109251=CARTESIAN_POINT('Ctrl Pts',(-10.8664411741287,66.6,72.2980067817921));
#109252=CARTESIAN_POINT('Ctrl Pts',(-10.8470411184477,66.6,72.98888938658));
#109253=CARTESIAN_POINT('',(-10.3758119169399,66.6000000000181,72.9888719572421));
#109254=CARTESIAN_POINT('',(-15.9175364833309,66.6,72.98888938658));
#109255=CARTESIAN_POINT('',(-10.4866907823956,67.6032721057859,69.0114531423211));
#109256=CARTESIAN_POINT('Ctrl Pts',(-10.3758119169399,66.6000000000181,
72.9888719572421));
#109257=CARTESIAN_POINT('Ctrl Pts',(-10.3859052171345,66.600000718797,72.6424593122746));
#109258=CARTESIAN_POINT('Ctrl Pts',(-10.3960457745143,66.6214302853707,
72.2963769232993));
#109259=CARTESIAN_POINT('Ctrl Pts',(-10.4157751272758,66.7066657642043,
71.6107443794253));
#109260=CARTESIAN_POINT('Ctrl Pts',(-10.4253085028644,66.7701553475043,
71.2718173942441));
#109261=CARTESIAN_POINT('Ctrl Pts',(-10.4540473375612,67.0231409069194,
70.2671330393793));
#109262=CARTESIAN_POINT('Ctrl Pts',(-10.4734283552966,67.2741698468866,
69.6199504765713));
#109263=CARTESIAN_POINT('Ctrl Pts',(-10.4934825642517,67.6016542759913,
69.0108898204612));
#109264=CARTESIAN_POINT('',(-11.1260798196334,83.4,72.98888938658));
#109265=CARTESIAN_POINT('Ctrl Pts',(-10.4857108324479,67.6017520181465,
69.0107080434282));
#109266=CARTESIAN_POINT('Ctrl Pts',(-10.4924440164462,67.7339470320748,
68.7648641739199));
#109267=CARTESIAN_POINT('Ctrl Pts',(-10.499325309094,67.8783113993465,68.5257670142111));
#109268=CARTESIAN_POINT('Ctrl Pts',(-10.5135966694059,68.1881179038954,
68.0660849034585));
#109269=CARTESIAN_POINT('Ctrl Pts',(-10.5209698190774,68.3530447724227,
67.8455715258234));
#109270=CARTESIAN_POINT('Ctrl Pts',(-10.5358034440303,68.6897328404269,
67.4387099411056));
#109271=CARTESIAN_POINT('Ctrl Pts',(-10.5431999929194,68.8596837833846,
67.2512529638297));
#109272=CARTESIAN_POINT('Ctrl Pts',(-10.5724885452809,69.5391969302741,
66.5665678032324));
#109273=CARTESIAN_POINT('Ctrl Pts',(-10.5964606357472,70.1027165875061,
66.1271814359369));
#109274=CARTESIAN_POINT('Ctrl Pts',(-10.6326053288691,71.0408445180282,
65.5707490580701));
#109275=CARTESIAN_POINT('Ctrl Pts',(-10.6449129433804,71.3796577283306,
65.3996270238521));
#109276=CARTESIAN_POINT('Ctrl Pts',(-10.6807263893499,72.4715428263888,
64.9379895553254));
#109277=CARTESIAN_POINT('Ctrl Pts',(-10.7023444507398,73.2555833569729,
64.7325398660417));
#109278=CARTESIAN_POINT('Ctrl Pts',(-10.7375866509904,74.5047875528942,
64.5913936931575));
#109279=CARTESIAN_POINT('Ctrl Pts',(-10.750356719919,74.9560252480495,64.5769197805323));
#109280=CARTESIAN_POINT('Ctrl Pts',(-10.7784516536322,75.9596370940102,
64.6255129461359));
#109281=CARTESIAN_POINT('Ctrl Pts',(-10.793645490965,76.5090279203329,64.7069929965395));
#109282=CARTESIAN_POINT('Ctrl Pts',(-10.824938254612,77.5819324145609,64.9764908537815));
#109283=CARTESIAN_POINT('Ctrl Pts',(-10.8409642773336,78.1029043627951,
65.1634903643253));
#109284=CARTESIAN_POINT('Ctrl Pts',(-10.8889317335777,79.5973141318404,
65.8727697249272));
#109285=CARTESIAN_POINT('Ctrl Pts',(-10.9185809685849,80.490233907639,66.5366185927917));
#109286=CARTESIAN_POINT('Ctrl Pts',(-10.9648095287159,81.5661897535722,
67.7260919052978));
#109287=CARTESIAN_POINT('Ctrl Pts',(-10.9794537614335,81.8688404238527,
68.1277234058784));
#109288=CARTESIAN_POINT('Ctrl Pts',(-11.0141928601179,82.5190872820912,
69.1736833146776));
#109289=CARTESIAN_POINT('Ctrl Pts',(-11.0342434566204,82.8219593005975,
69.8409625684042));
#109290=CARTESIAN_POINT('Ctrl Pts',(-11.0670101304895,83.1551947333564,
70.9338395463009));
#109291=CARTESIAN_POINT('Ctrl Pts',(-11.0790157657935,83.2463255339559,
71.3370593530283));
#109292=CARTESIAN_POINT('Ctrl Pts',(-11.1028514344624,83.3690627793617,
72.1569958322429));
#109293=CARTESIAN_POINT('Ctrl Pts',(-11.114463408048,83.4,72.5726453795531));
#109294=CARTESIAN_POINT('Ctrl Pts',(-11.1260798196334,83.4,72.98888938658));
#109295=CARTESIAN_POINT('Ctrl Pts',(-11.1260798196334,83.4,72.9888893865797));
#109296=CARTESIAN_POINT('Ctrl Pts',(-11.1554998323271,83.4,74.0430793040412));
#109297=CARTESIAN_POINT('Ctrl Pts',(-11.1862019338463,83.2015541254395,
75.087874801693));
#109298=CARTESIAN_POINT('Ctrl Pts',(-11.2258266429589,82.6880724176838,
76.390877188071));
#109299=CARTESIAN_POINT('Ctrl Pts',(-11.2354316893231,82.5412658088397,
76.7049749887674));
#109300=CARTESIAN_POINT('Ctrl Pts',(-11.2755123268849,81.8551462172399,
77.9637275658652));
#109301=CARTESIAN_POINT('Ctrl Pts',(-11.3074061933692,81.1543949381981,
78.8082936456724));
#109302=CARTESIAN_POINT('Ctrl Pts',(-11.3523708202787,79.9111548984504,
79.8232571031621));
#109303=CARTESIAN_POINT('Ctrl Pts',(-11.3667007821648,79.4807084235242,
80.1128824671349));
#109304=CARTESIAN_POINT('Ctrl Pts',(-11.3964561316438,78.5619975928432,
80.614642384779));
#109305=CARTESIAN_POINT('Ctrl Pts',(-11.4118382800914,78.0747278790574,
80.8238092853373));
#109306=CARTESIAN_POINT('Ctrl Pts',(-11.4423982312788,77.0643921043933,
81.1486390847459));
#109307=CARTESIAN_POINT('Ctrl Pts',(-11.4571319688664,76.5434166536166,
81.2630113542134));
#109308=CARTESIAN_POINT('Ctrl Pts',(-11.5026741622249,74.9276128008205,
81.4597198802285));
#109309=CARTESIAN_POINT('Ctrl Pts',(-11.5348230919039,73.8246440317065,
81.37809373512));
#109310=CARTESIAN_POINT('Ctrl Pts',(-11.5802118851425,72.2603915529493,
80.9470480447898));
#109311=CARTESIAN_POINT('Ctrl Pts',(-11.5948326656458,71.7666205744012,
80.7595392724667));
#109312=CARTESIAN_POINT('Ctrl Pts',(-11.6240674195689,70.8462231857547,
80.3070011735023));
#109313=CARTESIAN_POINT('Ctrl Pts',(-11.6385739156917,70.4192425309839,
80.047591272425));
#109314=CARTESIAN_POINT('Ctrl Pts',(-11.6682293590274,69.5895796955461,
79.4363888042523));
#109315=CARTESIAN_POINT('Ctrl Pts',(-11.6829378663155,69.1922932146571,
79.0809692818794));
#109316=CARTESIAN_POINT('Ctrl Pts',(-11.7285458471771,68.0862449392967,
77.8842805068686));
#109317=CARTESIAN_POINT('Ctrl Pts',(-11.7607556287622,67.5063910632311,
76.9399260467962));
#109318=CARTESIAN_POINT('Ctrl Pts',(-11.8064350524018,66.9381212087432,
75.4082731100625));
#109319=CARTESIAN_POINT('Ctrl Pts',(-11.8213191649983,66.8002007400394,
74.8890464485664));
#109320=CARTESIAN_POINT('Ctrl Pts',(-11.8497371850303,66.6376609935873,
73.9067834969859));
#109321=CARTESIAN_POINT('Ctrl Pts',(-11.8630898072636,66.6,73.4481292277721));
#109322=CARTESIAN_POINT('Ctrl Pts',(-11.8763230992193,66.6,72.98888938658));
#109323=CARTESIAN_POINT('Origin',(-15.9175364833309,75.,72.98888938658));
#109324=CARTESIAN_POINT('',(-8.87591635085981,66.6,72.98888938658));
#109325=CARTESIAN_POINT('',(-9.34771011126149,66.6,72.98888938658));
#109326=CARTESIAN_POINT('',(-15.9175364833309,66.6,72.98888938658));
#109327=CARTESIAN_POINT('Ctrl Pts',(-8.87591635085981,66.6,72.98888938658));
#109328=CARTESIAN_POINT('Ctrl Pts',(-8.88449608043677,66.6,72.6943442545088));
#109329=CARTESIAN_POINT('Ctrl Pts',(-8.89310105129781,66.6154919764157,
72.3996085824049));
#109330=CARTESIAN_POINT('Ctrl Pts',(-8.91696499178457,66.7032110037113,
71.5697455179493));
#109331=CARTESIAN_POINT('Ctrl Pts',(-8.93163466681888,66.8113717174765,
71.0402876251429));
#109332=CARTESIAN_POINT('Ctrl Pts',(-8.97231498264731,67.2393816268824,
69.6453701576608));
#109333=CARTESIAN_POINT('Ctrl Pts',(-8.99937164587288,67.6518739977052,
68.8162145713841));
#109334=CARTESIAN_POINT('Ctrl Pts',(-9.04117877128941,68.5061653281516,
67.6334439600081));
#109335=CARTESIAN_POINT('Ctrl Pts',(-9.05586138994771,68.8631892543803,
67.2277922757505));
#109336=CARTESIAN_POINT('Ctrl Pts',(-9.09678992714188,69.9352207416046,
66.2233315275476));
#109337=CARTESIAN_POINT('Ctrl Pts',(-9.12411309596022,70.7146673702538,
65.7046231506142));
#109338=CARTESIAN_POINT('Ctrl Pts',(-9.16621738663198,72.0550820069518,
65.1035771293466));
#109339=CARTESIAN_POINT('Ctrl Pts',(-9.18090250737464,72.5671309922688,
64.9308598009226));
#109340=CARTESIAN_POINT('Ctrl Pts',(-9.22593400499185,74.141454380223,64.5637061751752));
#109341=CARTESIAN_POINT('Ctrl Pts',(-9.25802141137251,75.2280193048841,
64.5231482682749));
#109342=CARTESIAN_POINT('Ctrl Pts',(-9.3034231618538,76.8271756355542,64.7721894632313));
#109343=CARTESIAN_POINT('Ctrl Pts',(-9.31817680449446,77.3524838278333,
64.9068996005011));
#109344=CARTESIAN_POINT('Ctrl Pts',(-9.34874701182155,78.3732696137243,
65.2767106127798));
#109345=CARTESIAN_POINT('Ctrl Pts',(-9.36450654423863,78.866090679307,65.5115924641901));
#109346=CARTESIAN_POINT('Ctrl Pts',(-9.41173371854036,80.2547458158857,
66.3476528170148));
#109347=CARTESIAN_POINT('Ctrl Pts',(-9.44055676979217,81.0615816358009,
67.0748687131144));
#109348=CARTESIAN_POINT('Ctrl Pts',(-9.48673413389458,82.0354732697045,
68.3676186459088));
#109349=CARTESIAN_POINT('Ctrl Pts',(-9.50264227275593,82.3190421147218,
68.8312901615648));
#109350=CARTESIAN_POINT('Ctrl Pts',(-9.54990550765018,83.0321398232053,
70.2994991511134));
#109351=CARTESIAN_POINT('Ctrl Pts',(-9.57874851143997,83.3129795650303,
71.3633240025041));
#109352=CARTESIAN_POINT('Ctrl Pts',(-9.62583420939872,83.4172951747497,
72.9892902885587));
#109353=CARTESIAN_POINT('Ctrl Pts',(-9.64176296726587,83.3999121453814,
73.5295696880987));
#109354=CARTESIAN_POINT('Ctrl Pts',(-9.68868706052882,83.1881877996304,
75.1695097513576));
#109355=CARTESIAN_POINT('Ctrl Pts',(-9.71876568409483,82.8270554848739,
76.2352539354287));
#109356=CARTESIAN_POINT('Ctrl Pts',(-9.76701768319113,81.9967495730251,
77.6685695133176));
#109357=CARTESIAN_POINT('Ctrl Pts',(-9.7826694323724,81.6802126532702,78.1102864171987));
#109358=CARTESIAN_POINT('Ctrl Pts',(-9.81278076262282,80.9672925865527,
78.9255488299831));
#109359=CARTESIAN_POINT('Ctrl Pts',(-9.82763853111115,80.5727859169826,
79.297341095552));
#109360=CARTESIAN_POINT('Ctrl Pts',(-9.85844211034537,79.7158078402704,
79.9614333002833));
#109361=CARTESIAN_POINT('Ctrl Pts',(-9.87432389642801,79.2550575699069,
80.2517866465711));
#109362=CARTESIAN_POINT('Ctrl Pts',(-9.92193760820865,77.7901137913412,
80.9874131258493));
#109363=CARTESIAN_POINT('Ctrl Pts',(-9.95095877328019,76.723882182416,81.2828240847856));
#109364=CARTESIAN_POINT('Ctrl Pts',(-9.99809891811017,75.0926985586027,
81.4057084587841));
#109365=CARTESIAN_POINT('Ctrl Pts',(-10.0140330284361,74.5517268190234,
81.3942732064712));
#109366=CARTESIAN_POINT('Ctrl Pts',(-10.0612792385604,72.9088747898517,
81.2004123098757));
#109367=CARTESIAN_POINT('Ctrl Pts',(-10.0911063217156,71.8391043920893,
80.8508712653943));
#109368=CARTESIAN_POINT('Ctrl Pts',(-10.1314663963532,70.6317532579358,
80.1688967431122));
#109369=CARTESIAN_POINT('Ctrl Pts',(-10.1394214898618,70.401407398868,80.023591355259));
#109370=CARTESIAN_POINT('Ctrl Pts',(-10.1785641430454,69.2914325261035,
79.2455523637897));
#109371=CARTESIAN_POINT('Ctrl Pts',(-10.2072704941516,68.5329638524829,
78.4579868704499));
#109372=CARTESIAN_POINT('Ctrl Pts',(-10.2501942049362,67.7280848548892,
77.2125051977263));
#109373=CARTESIAN_POINT('Ctrl Pts',(-10.2619173627264,67.5354218102325,
76.8618405428289));
#109374=CARTESIAN_POINT('Ctrl Pts',(-10.2908350061065,67.1162919785189,
75.9505322913265));
#109375=CARTESIAN_POINT('Ctrl Pts',(-10.3072480931363,66.9239555181329,
75.3767085877148));
#109376=CARTESIAN_POINT('Ctrl Pts',(-10.3409113672873,66.6652958693488,
74.1965300373668));
#109377=CARTESIAN_POINT('Ctrl Pts',(-10.3581925699977,66.6,73.5935864999432));
#109378=CARTESIAN_POINT('Ctrl Pts',(-10.3758114091077,66.6,72.9888893865795));
#109379=CARTESIAN_POINT('',(-9.46554775786244,67.6016909082801,69.0108216919104));
#109380=CARTESIAN_POINT('Ctrl Pts',(-10.8470411184477,66.6,72.98888938658));
#109381=CARTESIAN_POINT('Ctrl Pts',(-10.8429974544575,66.6,73.1328939789574));
#109382=CARTESIAN_POINT('Ctrl Pts',(-10.8389830318835,66.6037030877524,
73.2769889125608));
#109383=CARTESIAN_POINT('Ctrl Pts',(-10.8200995945198,66.6386538757395,
73.9554652693975));
#109384=CARTESIAN_POINT('Ctrl Pts',(-10.8052994167985,66.7171918370302,
74.4860408086064));
#109385=CARTESIAN_POINT('Ctrl Pts',(-10.7673672606253,67.0362804855674,
75.776284033232));
#109386=CARTESIAN_POINT('Ctrl Pts',(-10.7438334944375,67.335214583143,76.5161413930023));
#109387=CARTESIAN_POINT('Ctrl Pts',(-10.7000502611941,68.1205210414441,
77.8702571798004));
#109388=CARTESIAN_POINT('Ctrl Pts',(-10.678911890322,68.5975578161451,78.4810410280505));
#109389=CARTESIAN_POINT('Ctrl Pts',(-10.6423478202938,69.5079009543939,
79.3641382481171));
#109390=CARTESIAN_POINT('Ctrl Pts',(-10.6277391305027,69.8945857817826,
79.6778122874029));
#109391=CARTESIAN_POINT('Ctrl Pts',(-10.5997334830968,70.7071291608878,
80.2252111110413));
#109392=CARTESIAN_POINT('Ctrl Pts',(-10.5865090312781,71.1300498424614,
80.4599389249407));
#109393=CARTESIAN_POINT('Ctrl Pts',(-10.5424090237105,72.5750704014388,
81.1061557090216));
#109394=CARTESIAN_POINT('Ctrl Pts',(-10.5097800041221,73.6578460320961,
81.3536303441462));
#109395=CARTESIAN_POINT('Ctrl Pts',(-10.4594583183132,75.453211984091,81.4054804054051));
#109396=CARTESIAN_POINT('Ctrl Pts',(-10.4404402495851,76.148717327638,81.339031228331));
#109397=CARTESIAN_POINT('Ctrl Pts',(-10.3972128535349,77.6224670548347,
81.0104327503222));
#109398=CARTESIAN_POINT('Ctrl Pts',(-10.3731988605783,78.3869641936456,
80.7187680563788));
#109399=CARTESIAN_POINT('Ctrl Pts',(-10.3358043235385,79.5589275625022,
80.0638838608808));
#109400=CARTESIAN_POINT('Ctrl Pts',(-10.3212492026392,79.9949626824068,
79.7630841569993));
#109401=CARTESIAN_POINT('Ctrl Pts',(-10.2838028980019,81.0045835734316,
78.9157996540609));
#109402=CARTESIAN_POINT('Ctrl Pts',(-10.2603558941316,81.534768850004,78.3255639741675));
#109403=CARTESIAN_POINT('Ctrl Pts',(-10.2228371947749,82.2777896155877,
77.2184883213856));
#109404=CARTESIAN_POINT('Ctrl Pts',(-10.207982765868,82.5362805922708,76.738584788694));
#109405=CARTESIAN_POINT('Ctrl Pts',(-10.1685899659626,83.0769591001059,
75.449122455846));
#109406=CARTESIAN_POINT('Ctrl Pts',(-10.1432360276034,83.2851949198924,
74.6153923607755));
#109407=CARTESIAN_POINT('Ctrl Pts',(-10.1054806048686,83.4085236854867,
73.2857075566512));
#109408=CARTESIAN_POINT('Ctrl Pts',(-10.0923185055741,83.4117258184702,
72.8038168581635));
#109409=CARTESIAN_POINT('Ctrl Pts',(-10.0476349101555,83.285332993399,71.2112930426171));
#109410=CARTESIAN_POINT('Ctrl Pts',(-10.0144854685635,82.9759767394019,
70.1270021722388));
#109411=CARTESIAN_POINT('Ctrl Pts',(-9.9686471877387,82.2205249119231,68.6639642151414));
#109412=CARTESIAN_POINT('Ctrl Pts',(-9.95403766156621,81.9333031210872,
68.2170695755514));
#109413=CARTESIAN_POINT('Ctrl Pts',(-9.91654046434544,81.1188692089366,
67.1801816090873));
#109414=CARTESIAN_POINT('Ctrl Pts',(-9.89312700168102,80.5469717865591,
66.6317855236956));
#109415=CARTESIAN_POINT('Ctrl Pts',(-9.85419328296166,79.4225378831116,
65.8224746710984));
#109416=CARTESIAN_POINT('Ctrl Pts',(-9.83790478950418,78.9022466608465,
65.5263947517448));
#109417=CARTESIAN_POINT('Ctrl Pts',(-9.8054291819373,77.8509918913373,65.0684064454306));
#109418=CARTESIAN_POINT('Ctrl Pts',(-9.7894267946388,77.3266785902673,64.898849201525));
#109419=CARTESIAN_POINT('Ctrl Pts',(-9.74144977797055,75.7116660419685,
64.5466924361694));
#109420=CARTESIAN_POINT('Ctrl Pts',(-9.71208081141942,74.5979439719732,
64.5262941293461));
#109421=CARTESIAN_POINT('Ctrl Pts',(-9.66596321343898,73.0231094515633,
64.809720962872));
#109422=CARTESIAN_POINT('Ctrl Pts',(-9.6513603589804,72.5428617473836,64.9409481708741));
#109423=CARTESIAN_POINT('Ctrl Pts',(-9.62320555521004,71.6195450110593,
65.2836536488962));
#109424=CARTESIAN_POINT('Ctrl Pts',(-9.60985108382497,71.1777185616237,
65.4930037924682));
#109425=CARTESIAN_POINT('Ctrl Pts',(-9.58555856277631,70.4248560092225,
65.9336930808021));
#109426=CARTESIAN_POINT('Ctrl Pts',(-9.57474051005098,70.1068634346352,
66.1503993784754));
#109427=CARTESIAN_POINT('Ctrl Pts',(-9.54743719458288,69.3589885197844,
66.7390174365363));
#109428=CARTESIAN_POINT('Ctrl Pts',(-9.53071392835463,68.949851159647,67.134182469978));
#109429=CARTESIAN_POINT('Ctrl Pts',(-9.49779589939924,68.2071166842069,
68.0132323026672));
#109430=CARTESIAN_POINT('Ctrl Pts',(-9.48191110280316,67.8780097698654,
68.4969309030181));
#109431=CARTESIAN_POINT('Ctrl Pts',(-9.46554775786244,67.6016909082801,
69.0108216919104));
#109432=CARTESIAN_POINT('Ctrl Pts',(-9.46562408938853,67.6016900154045,
69.010823352458));
#109433=CARTESIAN_POINT('Ctrl Pts',(-9.44541854529748,67.2454679990037,
69.6733163523391));
#109434=CARTESIAN_POINT('Ctrl Pts',(-9.42553707582171,66.979848802812,70.3806400212566));
#109435=CARTESIAN_POINT('Ctrl Pts',(-9.38575705560963,66.671022391848,71.7292457946473));
#109436=CARTESIAN_POINT('Ctrl Pts',(-9.36658493103693,66.6,72.3582310229932));
#109437=CARTESIAN_POINT('Ctrl Pts',(-9.34771011126149,66.6,72.98888938658));
#109438=CARTESIAN_POINT('Origin',(-15.9175364833309,-75.,72.98888938658));
#109439=CARTESIAN_POINT('',(-9.34771011126148,-66.6,72.98888938658));
#109440=CARTESIAN_POINT('',(-8.87591635085981,-66.6,72.98888938658));
#109441=CARTESIAN_POINT('',(-15.9175364833309,-66.6,72.98888938658));
#109442=CARTESIAN_POINT('',(-8.56753648333097,-72.6784966214785,81.06172173115));
#109443=CARTESIAN_POINT('Ctrl Pts',(-8.87591635085981,-66.6,72.9888893865799));
#109444=CARTESIAN_POINT('Ctrl Pts',(-8.85294957915599,-66.6,73.7773467317762));
#109445=CARTESIAN_POINT('Ctrl Pts',(-8.83059301219102,-66.7110222695729,
74.5635770776098));
#109446=CARTESIAN_POINT('Ctrl Pts',(-8.79362233623142,-67.0818223436479,
75.8448230515217));
#109447=CARTESIAN_POINT('Ctrl Pts',(-8.77850802983328,-67.2825837564249,
76.3497484918026));
#109448=CARTESIAN_POINT('Ctrl Pts',(-8.7470324735349,-67.7779596867464,
77.312601823614));
#109449=CARTESIAN_POINT('Ctrl Pts',(-8.73122077996138,-68.0711761988425,
77.7684057885426));
#109450=CARTESIAN_POINT('Ctrl Pts',(-8.69128771667201,-68.9417992746947,
78.8715534955591));
#109451=CARTESIAN_POINT('Ctrl Pts',(-8.66821704523819,-69.579004898322,
79.4634820331365));
#109452=CARTESIAN_POINT('Ctrl Pts',(-8.61776368352287,-71.0262048035655,
80.4419034519592));
#109453=CARTESIAN_POINT('Ctrl Pts',(-8.59210212382877,-71.8304934245268,
80.8178615588208));
#109454=CARTESIAN_POINT('Ctrl Pts',(-8.56753648333109,-72.6784966214791,
81.0617217311488));
#109455=CARTESIAN_POINT('',(-8.56920282870944,-83.3330658671999,71.9536543098738));
#109456=CARTESIAN_POINT('Origin',(-8.56753648333091,-75.,72.98888938658));
#109457=CARTESIAN_POINT('',(-8.59969205422499,-83.3999999999891,72.9889028996933));
#109458=CARTESIAN_POINT('Ctrl Pts',(-8.59969205422499,-83.3999999999891,
72.9889028996933));
#109459=CARTESIAN_POINT('Ctrl Pts',(-8.59443361344606,-83.4000003125319,
72.7946205818928));
#109460=CARTESIAN_POINT('Ctrl Pts',(-8.58911455314039,-83.3932603589226,
72.6003991553237));
#109461=CARTESIAN_POINT('Ctrl Pts',(-8.57948092673193,-83.3692714773426,
72.2551795052892));
#109462=CARTESIAN_POINT('Ctrl Pts',(-8.57520339899112,-83.3546488080667,
72.1040856703524));
#109463=CARTESIAN_POINT('Ctrl Pts',(-8.57086917408796,-83.3359409660147,
71.9534724603524));
#109464=CARTESIAN_POINT('Ctrl Pts',(-8.599692054225,-83.3999999999891,72.9889028996933));
#109465=CARTESIAN_POINT('Ctrl Pts',(-8.6245653979019,-83.3999985216074,
73.9078922092929));
#109466=CARTESIAN_POINT('Ctrl Pts',(-8.64831456326027,-83.2492082149449,
74.8206009565659));
#109467=CARTESIAN_POINT('Ctrl Pts',(-8.70336173029356,-82.6585704764233,
76.5592681833137));
#109468=CARTESIAN_POINT('Ctrl Pts',(-8.73114014016359,-82.2232308308517,
77.3736939600486));
#109469=CARTESIAN_POINT('Ctrl Pts',(-8.78168057817269,-81.105995936845,
78.8301160315007));
#109470=CARTESIAN_POINT('Ctrl Pts',(-8.80454434265513,-80.431498229985,
79.4620648581349));
#109471=CARTESIAN_POINT('Ctrl Pts',(-8.86363004660202,-78.758610123619,
80.5803073614369));
#109472=CARTESIAN_POINT('Ctrl Pts',(-8.89744283053813,-77.7390120598963,
81.0048193525973));
#109473=CARTESIAN_POINT('Ctrl Pts',(-8.94677625803638,-75.9714687934765,
81.362608468677));
#109474=CARTESIAN_POINT('Ctrl Pts',(-8.96482541908273,-75.2614168589107,
81.4147123771282));
#109475=CARTESIAN_POINT('Ctrl Pts',(-8.99989289624195,-74.0131601630423,
81.3482398684911));
#109476=CARTESIAN_POINT('Ctrl Pts',(-9.01641208642739,-73.4770816484086,
81.2673699331499));
#109477=CARTESIAN_POINT('Ctrl Pts',(-9.04925276003734,-72.4207468549019,
81.0018865159534));
#109478=CARTESIAN_POINT('Ctrl Pts',(-9.06543988179121,-71.903296508067,
80.8164779418256));
#109479=CARTESIAN_POINT('Ctrl Pts',(-9.11063813073376,-70.4483117239719,
80.1281016998877));
#109480=CARTESIAN_POINT('Ctrl Pts',(-9.13661289890309,-69.5837422354327,
79.4966102182232));
#109481=CARTESIAN_POINT('Ctrl Pts',(-9.19621508389475,-68.2075509289092,
78.0223409841654));
#109482=CARTESIAN_POINT('Ctrl Pts',(-9.22587045537373,-67.6794386529001,
77.2176855012128));
#109483=CARTESIAN_POINT('Ctrl Pts',(-9.28192979902723,-66.8764390499947,
75.3728996039502));
#109484=CARTESIAN_POINT('Ctrl Pts',(-9.3078635989614,-66.6413166549408,
74.3336028706724));
#109485=CARTESIAN_POINT('Ctrl Pts',(-9.34195635427578,-66.6016563503745,
73.1815483385072));
#109486=CARTESIAN_POINT('Ctrl Pts',(-9.34482767571643,-66.6,73.0851992907596));
#109487=CARTESIAN_POINT('Ctrl Pts',(-9.34771011126147,-66.6,72.98888938658));
#109488=CARTESIAN_POINT('Origin',(-15.9175364833309,-75.,72.98888938658));
#109489=CARTESIAN_POINT('',(-10.8470411184476,-66.6,72.98888938658));
#109490=CARTESIAN_POINT('',(-10.3758114091077,-66.6,72.9888893865795));
#109491=CARTESIAN_POINT('',(-15.9175364833309,-66.6,72.98888938658));
#109492=CARTESIAN_POINT('Ctrl Pts',(-10.3758114091077,-66.6,72.9888893865795));
#109493=CARTESIAN_POINT('Ctrl Pts',(-10.3582032242367,-66.6,73.5932208352387));
#109494=CARTESIAN_POINT('Ctrl Pts',(-10.3409320423887,-66.6652169238319,
74.1958019008719));
#109495=CARTESIAN_POINT('Ctrl Pts',(-10.3072885316604,-66.9235651935971,
75.3752941690252));
#109496=CARTESIAN_POINT('Ctrl Pts',(-10.2908864868318,-67.1156700307945,
75.9488004864642));
#109497=CARTESIAN_POINT('Ctrl Pts',(-10.261988887019,-67.5343032730094,
76.8596586711068));
#109498=CARTESIAN_POINT('Ctrl Pts',(-10.2502728742011,-67.7267405915717,
77.2101667049502));
#109499=CARTESIAN_POINT('Ctrl Pts',(-10.2073631419159,-68.5308733934261,
78.4554491819985));
#109500=CARTESIAN_POINT('Ctrl Pts',(-10.178663586788,-69.2887876200924,
79.2430814255604));
#109501=CARTESIAN_POINT('Ctrl Pts',(-10.1395351689805,-70.3981401823001,
80.0214548742716));
#109502=CARTESIAN_POINT('Ctrl Pts',(-10.1315799689027,-70.6284270331717,
80.1668724205897));
#109503=CARTESIAN_POINT('Ctrl Pts',(-10.091218362305,-71.8354636456972,
80.8494052481719));
#109504=CARTESIAN_POINT('Ctrl Pts',(-10.0613841675067,-72.9050626819587,
81.1994391953708));
#109505=CARTESIAN_POINT('Ctrl Pts',(-10.0141484050549,-74.5477937036023,
81.3940612038461));
#109506=CARTESIAN_POINT('Ctrl Pts',(-9.99821434084186,-75.0887392883698,
81.4057498077921));
#109507=CARTESIAN_POINT('Ctrl Pts',(-9.95107381499787,-76.7198313848376,
81.2836479343613));
#109508=CARTESIAN_POINT('Ctrl Pts',(-9.92205777752795,-77.7860811621063,
80.98880100083));
#109509=CARTESIAN_POINT('Ctrl Pts',(-9.87445272111629,-79.2512592478914,
80.2540079646784));
#109510=CARTESIAN_POINT('Ctrl Pts',(-9.85856994315616,-79.7121317522274,
79.9639154167409));
#109511=CARTESIAN_POINT('Ctrl Pts',(-9.82776141766458,-80.5694853043513,
79.3002607780479));
#109512=CARTESIAN_POINT('Ctrl Pts',(-9.81289998677686,-80.9642323271672,
78.9286291622983));
#109513=CARTESIAN_POINT('Ctrl Pts',(-9.78278800959738,-81.6776414021401,
78.1136437405388));
#109514=CARTESIAN_POINT('Ctrl Pts',(-9.76713950264915,-81.9944277630583,
77.6720447722223));
#109515=CARTESIAN_POINT('Ctrl Pts',(-9.71888511166521,-82.8254614118745,
76.2390944889405));
#109516=CARTESIAN_POINT('Ctrl Pts',(-9.68879677956511,-83.1871168803284,
75.1735273461357));
#109517=CARTESIAN_POINT('Ctrl Pts',(-9.64188376543304,-83.3996442407148,
73.5337033427581));
#109518=CARTESIAN_POINT('Ctrl Pts',(-9.62595552208944,-83.4172930830374,
72.9934457186032));
#109519=CARTESIAN_POINT('Ctrl Pts',(-9.57887456877193,-83.3138029716328,
71.3677448194764));
#109520=CARTESIAN_POINT('Ctrl Pts',(-9.55003901146819,-83.0336270035935,
70.3040682601755));
#109521=CARTESIAN_POINT('Ctrl Pts',(-9.50279219367472,-82.3215645216885,
68.8357389347262));
#109522=CARTESIAN_POINT('Ctrl Pts',(-9.48688325147918,-82.0382993760529,
68.3719286886787));
#109523=CARTESIAN_POINT('Ctrl Pts',(-9.44069579575573,-81.0651421331075,
67.078493779823));
#109524=CARTESIAN_POINT('Ctrl Pts',(-9.4118759893924,-80.2586258546887,
66.350701061303));
#109525=CARTESIAN_POINT('Ctrl Pts',(-9.36464665559067,-78.8703628922013,
65.5138066548259));
#109526=CARTESIAN_POINT('Ctrl Pts',(-9.34888578959923,-78.3777232856237,
65.2786637690214));
#109527=CARTESIAN_POINT('Ctrl Pts',(-9.31831182400894,-77.3571698893145,
64.9082628219543));
#109528=CARTESIAN_POINT('Ctrl Pts',(-9.30355600029347,-76.8319066547898,
64.7732407130955));
#109529=CARTESIAN_POINT('Ctrl Pts',(-9.25814827124965,-75.2323844378279,
64.5232057622288));
#109530=CARTESIAN_POINT('Ctrl Pts',(-9.22604336406828,-74.1453066792442,
64.5632531277902));
#109531=CARTESIAN_POINT('Ctrl Pts',(-9.18099559830346,-72.5703710338625,
64.9298824555297));
#109532=CARTESIAN_POINT('Ctrl Pts',(-9.16631182716657,-72.0582549323504,
65.1023930613214));
#109533=CARTESIAN_POINT('Ctrl Pts',(-9.12434353015912,-70.7217192794661,
65.7010534404074));
#109534=CARTESIAN_POINT('Ctrl Pts',(-9.09714179453877,-69.9454865696347,
66.2162767140583));
#109535=CARTESIAN_POINT('Ctrl Pts',(-9.05632554412384,-68.8747503124929,
67.2155027246282));
#109536=CARTESIAN_POINT('Ctrl Pts',(-9.04164869831569,-68.516913096469,
67.6204391047425));
#109537=CARTESIAN_POINT('Ctrl Pts',(-9.00049457750973,-67.6729590190129,
68.7839745058294));
#109538=CARTESIAN_POINT('Ctrl Pts',(-8.97402578865247,-67.265570842812,
69.5910103927026));
#109539=CARTESIAN_POINT('Ctrl Pts',(-8.93387272636529,-66.830570845959,
70.9612572108593));
#109540=CARTESIAN_POINT('Ctrl Pts',(-8.91921129277492,-66.7172708014753,
71.4898077375009));
#109541=CARTESIAN_POINT('Ctrl Pts',(-8.89466879617357,-66.6184301835754,
72.3459818232941));
#109542=CARTESIAN_POINT('Ctrl Pts',(-8.88527448264431,-66.6,72.6676214331228));
#109543=CARTESIAN_POINT('Ctrl Pts',(-8.87591635085981,-66.6,72.9888893865799));
#109544=CARTESIAN_POINT('',(-9.46554776533453,-67.6016910344572,69.0108214572493));
#109545=CARTESIAN_POINT('Ctrl Pts',(-9.34771011126148,-66.6,72.98888938658));
#109546=CARTESIAN_POINT('Ctrl Pts',(-9.36658462513265,-66.6,72.3582412440757));
#109547=CARTESIAN_POINT('Ctrl Pts',(-9.38575644244071,-66.6710200899113,
71.7292661134848));
#109548=CARTESIAN_POINT('Ctrl Pts',(-9.42553652362212,-66.9798415869828,
70.3806592999566));
#109549=CARTESIAN_POINT('Ctrl Pts',(-9.44541826576314,-67.2454630876286,
69.6733255319622));
#109550=CARTESIAN_POINT('Ctrl Pts',(-9.46562408291506,-67.6016899012779,
69.0108235647079));
#109551=CARTESIAN_POINT('Ctrl Pts',(-9.46554776533453,-67.6016910344572,
69.0108214572493));
#109552=CARTESIAN_POINT('Ctrl Pts',(-9.48496609064942,-67.9295977010525,
68.4009890274292));
#109553=CARTESIAN_POINT('Ctrl Pts',(-9.50382515141497,-68.3316390992661,
67.8340483629832));
#109554=CARTESIAN_POINT('Ctrl Pts',(-9.54381168935438,-69.2636569651681,
66.8139762343873));
#109555=CARTESIAN_POINT('Ctrl Pts',(-9.56393837215954,-69.7895316897335,
66.3642193638286));
#109556=CARTESIAN_POINT('Ctrl Pts',(-9.59578124995521,-70.733377952405,
65.7396362524334));
#109557=CARTESIAN_POINT('Ctrl Pts',(-9.60794544192018,-71.1210391147184,
65.5250166898597));
#109558=CARTESIAN_POINT('Ctrl Pts',(-9.65053370411021,-72.5113857746416,
64.8929838099454));
#109559=CARTESIAN_POINT('Ctrl Pts',(-9.68276932829838,-73.5766360222517,
64.639583181404));
#109560=CARTESIAN_POINT('Ctrl Pts',(-9.72645125455699,-75.1374200423614,
64.5764667995703));
#109561=CARTESIAN_POINT('Ctrl Pts',(-9.73951499541836,-75.6150181377391,
64.5978537338206));
#109562=CARTESIAN_POINT('Ctrl Pts',(-9.77652195402752,-76.9122512082918,
64.7673359949956));
#109563=CARTESIAN_POINT('Ctrl Pts',(-9.8011822115001,-77.7157749353004,
64.9966897689716));
#109564=CARTESIAN_POINT('Ctrl Pts',(-9.8381660531439,-78.9091070172569,
65.5384675429136));
#109565=CARTESIAN_POINT('Ctrl Pts',(-9.85134595007298,-79.3279246808202,
65.7736992106172));
#109566=CARTESIAN_POINT('Ctrl Pts',(-9.88711752027425,-80.3877596955818,
66.4946051587608));
#109567=CARTESIAN_POINT('Ctrl Pts',(-9.91085166060931,-80.9830638831558,
67.0385469351782));
#109568=CARTESIAN_POINT('Ctrl Pts',(-9.95325056715723,-81.9242945269183,
68.1849397024771));
#109569=CARTESIAN_POINT('Ctrl Pts',(-9.97185214123004,-82.2908245884359,
68.7618751612809));
#109570=CARTESIAN_POINT('Ctrl Pts',(-10.0130713776169,-82.9232271672781,
70.0895844055562));
#109571=CARTESIAN_POINT('Ctrl Pts',(-10.0365015998053,-83.160564716385,
70.8467766916736));
#109572=CARTESIAN_POINT('Ctrl Pts',(-10.0741925591459,-83.3751732762724,
72.1518753417865));
#109573=CARTESIAN_POINT('Ctrl Pts',(-10.0889121225787,-83.4114029662636,
72.6848775572873));
#109574=CARTESIAN_POINT('Ctrl Pts',(-10.1348078381706,-83.3664488347047,
74.334518176599));
#109575=CARTESIAN_POINT('Ctrl Pts',(-10.1679540153276,-83.1135172714937,
75.434090013385));
#109576=CARTESIAN_POINT('Ctrl Pts',(-10.2131067043693,-82.448898112568,
76.9028173560589));
#109577=CARTESIAN_POINT('Ctrl Pts',(-10.2266396820162,-82.2054284024345,
77.33477306549));
#109578=CARTESIAN_POINT('Ctrl Pts',(-10.2654764363646,-81.427322458614,
78.4683014836411));
#109579=CARTESIAN_POINT('Ctrl Pts',(-10.2915976540544,-80.8183581845854,
79.1110775103155));
#109580=CARTESIAN_POINT('Ctrl Pts',(-10.3361756194551,-79.5622038415008,
80.077102840578));
#109581=CARTESIAN_POINT('Ctrl Pts',(-10.3552431054305,-78.9518458281728,
80.4346528318297));
#109582=CARTESIAN_POINT('Ctrl Pts',(-10.3888191919241,-77.8810753502658,
80.8927515485621));
#109583=CARTESIAN_POINT('Ctrl Pts',(-10.4023024920715,-77.4439700459721,
81.0386502139542));
#109584=CARTESIAN_POINT('Ctrl Pts',(-10.4368868675726,-76.2758307719957,
81.3245766780089));
#109585=CARTESIAN_POINT('Ctrl Pts',(-10.4572104458872,-75.5343220112447,
81.4047026315808));
#109586=CARTESIAN_POINT('Ctrl Pts',(-10.5087059409012,-73.6948718203082,
81.3591355804513));
#109587=CARTESIAN_POINT('Ctrl Pts',(-10.5412791004055,-72.613667306826,
81.1172234537493));
#109588=CARTESIAN_POINT('Ctrl Pts',(-10.5842616617643,-71.2030947285683,
80.494946788034));
#109589=CARTESIAN_POINT('Ctrl Pts',(-10.5964449208363,-70.8114820507407,
80.2836610881585));
#109590=CARTESIAN_POINT('Ctrl Pts',(-10.6239200527003,-69.9977607466304,
79.7574197422417));
#109591=CARTESIAN_POINT('Ctrl Pts',(-10.6393725027132,-69.5847744400246,
79.4317713352398));
#109592=CARTESIAN_POINT('Ctrl Pts',(-10.6773931560393,-68.6316145595861,
78.5233971989891));
#109593=CARTESIAN_POINT('Ctrl Pts',(-10.6991172465038,-68.1384856218894,
77.8987486456542));
#109594=CARTESIAN_POINT('Ctrl Pts',(-10.7434898581446,-67.3401635464417,
76.5271293521389));
#109595=CARTESIAN_POINT('Ctrl Pts',(-10.7670506978084,-67.0397922124725,
75.7866174143636));
#109596=CARTESIAN_POINT('Ctrl Pts',(-10.8050362051295,-66.7188429847764,
74.4952819336274));
#109597=CARTESIAN_POINT('Ctrl Pts',(-10.8198511362895,-66.6396689067076,
73.964414260643));
#109598=CARTESIAN_POINT('Ctrl Pts',(-10.8388232541245,-66.6038519551218,
73.2827238758526));
#109599=CARTESIAN_POINT('Ctrl Pts',(-10.8429169758835,-66.6,73.1357600143794));
#109600=CARTESIAN_POINT('Ctrl Pts',(-10.8470411184476,-66.6,72.98888938658));
#109601=CARTESIAN_POINT('Origin',(-15.9175364833309,-75.,72.98888938658));
#109602=CARTESIAN_POINT('',(-12.3474397125752,-66.60000000001,72.9889023383631));
#109603=CARTESIAN_POINT('',(-11.8763230992193,-66.6,72.98888938658));
#109604=CARTESIAN_POINT('',(-15.9175364833309,-66.6,72.98888938658));
#109605=CARTESIAN_POINT('',(-12.9679003706341,-82.2015397612608,68.6647904662762));
#109606=CARTESIAN_POINT('Ctrl Pts',(-12.3474400892301,-66.6,72.9888893865802));
#109607=CARTESIAN_POINT('Ctrl Pts',(-12.3626760155633,-66.6,72.4649816273803));
#109608=CARTESIAN_POINT('Ctrl Pts',(-12.3777612751813,-66.6490141176073,
71.9422119441476));
#109609=CARTESIAN_POINT('Ctrl Pts',(-12.4066962527405,-66.8403263929348,
70.9309779346599));
#109610=CARTESIAN_POINT('Ctrl Pts',(-12.4205238029993,-66.9788430599666,
70.4440307131329));
#109611=CARTESIAN_POINT('Ctrl Pts',(-12.4657516690178,-67.5568226075387,
68.9418400911724));
#109612=CARTESIAN_POINT('Ctrl Pts',(-12.4984264527936,-68.1527467712344,
67.9994325344402));
#109613=CARTESIAN_POINT('Ctrl Pts',(-12.5407531485241,-69.2013466167469,
66.8971280565159));
#109614=CARTESIAN_POINT('Ctrl Pts',(-12.5522155830747,-69.5108989977885,
66.616786289757));
#109615=CARTESIAN_POINT('Ctrl Pts',(-12.5953164764488,-70.7068140489397,
65.6857855976481));
#109616=CARTESIAN_POINT('Ctrl Pts',(-12.6274069825217,-71.6977037102949,
65.187489105859));
#109617=CARTESIAN_POINT('Ctrl Pts',(-12.6727423882884,-73.2711981139386,
64.7513784901037));
#109618=CARTESIAN_POINT('Ctrl Pts',(-12.687669814557,-73.7983899788031,
64.6581350928857));
#109619=CARTESIAN_POINT('Ctrl Pts',(-12.718550751688,-74.8592910802199,
64.5733546507773));
#109620=CARTESIAN_POINT('Ctrl Pts',(-12.7339958847427,-75.3905477198548,
64.5812431813904));
#109621=CARTESIAN_POINT('Ctrl Pts',(-12.7714181795336,-76.7012242271057,
64.7252666633024));
#109622=CARTESIAN_POINT('Ctrl Pts',(-12.7926048066354,-77.4689065878398,
64.9212923585636));
#109623=CARTESIAN_POINT('Ctrl Pts',(-12.8324865342203,-78.7511883261983,
65.4492260302197));
#109624=CARTESIAN_POINT('Ctrl Pts',(-12.8500679374427,-79.2785032522741,
65.7354507606983));
#109625=CARTESIAN_POINT('Ctrl Pts',(-12.8840699634655,-80.2605796609222,
66.4131592514461));
#109626=CARTESIAN_POINT('Ctrl Pts',(-12.9004039599877,-80.7129408500286,
66.8021108355024));
#109627=CARTESIAN_POINT('Ctrl Pts',(-12.9337253072399,-81.530721412008,
67.6720706009407));
#109628=CARTESIAN_POINT('Ctrl Pts',(-12.951210956824,-81.8931531007849,
68.1511958833952));
#109629=CARTESIAN_POINT('Ctrl Pts',(-12.9685679372243,-82.2015206898752,
68.6647594448114));
#109630=CARTESIAN_POINT('',(-12.9675940210686,-76.1752999551703,81.3061781097492));
#109631=CARTESIAN_POINT('Origin',(-12.9678999777142,-75.,72.98888938658));
#109632=CARTESIAN_POINT('Ctrl Pts',(-12.9672881034143,-76.1753032494785,
81.3062605020086));
#109633=CARTESIAN_POINT('Ctrl Pts',(-12.9456997237206,-76.9211863996156,
81.2008619478354));
#109634=CARTESIAN_POINT('Ctrl Pts',(-12.9250931772649,-77.6494936947553,
80.9956117455372));
#109635=CARTESIAN_POINT('Ctrl Pts',(-12.8827991508676,-79.0202689687081,
80.4014544074433));
#109636=CARTESIAN_POINT('Ctrl Pts',(-12.8610339737836,-79.6579587132031,
80.0182650931779));
#109637=CARTESIAN_POINT('Ctrl Pts',(-12.8264255828997,-80.6134893801562,
79.2563033741515));
#109638=CARTESIAN_POINT('Ctrl Pts',(-12.8131104264417,-80.9633694694468,
78.9243728348466));
#109639=CARTESIAN_POINT('Ctrl Pts',(-12.7846753651269,-81.6362980936601,
78.1660556733353));
#109640=CARTESIAN_POINT('Ctrl Pts',(-12.7692207392664,-81.9510335467936,
77.735109896772));
#109641=CARTESIAN_POINT('Ctrl Pts',(-12.7222821677812,-82.781285547952,
76.3367388231498));
#109642=CARTESIAN_POINT('Ctrl Pts',(-12.6927985335859,-83.1506594241578,
75.2961069719951));
#109643=CARTESIAN_POINT('Ctrl Pts',(-12.646115702509,-83.3865027676399,
73.6962723693769));
#109644=CARTESIAN_POINT('Ctrl Pts',(-12.6309515956989,-83.4142790606389,
73.1725797116149));
#109645=CARTESIAN_POINT('Ctrl Pts',(-12.6017435937532,-83.3726721322348,
72.1429828209544));
#109646=CARTESIAN_POINT('Ctrl Pts',(-12.5877313565474,-83.306346769762,
71.6391498446068));
#109647=CARTESIAN_POINT('Ctrl Pts',(-12.5585622960045,-83.0781712073388,
70.6253840143067));
#109648=CARTESIAN_POINT('Ctrl Pts',(-12.5430982084136,-82.912318620317,
70.1186636650525));
#109649=CARTESIAN_POINT('Ctrl Pts',(-12.4960994835157,-82.2610964223792,
68.6253809566896));
#109650=CARTESIAN_POINT('Ctrl Pts',(-12.4665274681307,-81.6297184639939,
67.7153177363067));
#109651=CARTESIAN_POINT('Ctrl Pts',(-12.4194435134014,-80.4583362182937,
66.5818216027056));
#109652=CARTESIAN_POINT('Ctrl Pts',(-12.4040232416618,-80.0409972621814,
66.2485396381113));
#109653=CARTESIAN_POINT('Ctrl Pts',(-12.3751276187305,-79.186146298515,
65.689943901073));
#109654=CARTESIAN_POINT('Ctrl Pts',(-12.3616365734621,-78.7548794823978,
65.4589954364309));
#109655=CARTESIAN_POINT('Ctrl Pts',(-12.3329899953647,-77.8171230685113,
65.0575196182307));
#109656=CARTESIAN_POINT('Ctrl Pts',(-12.3175212803872,-77.3094826241488,
64.8951218378516));
#109657=CARTESIAN_POINT('Ctrl Pts',(-12.2705039573595,-75.7168016277099,
64.5477663236539));
#109658=CARTESIAN_POINT('Ctrl Pts',(-12.2408979718944,-74.6081372569116,
64.5264545930802));
#109659=CARTESIAN_POINT('Ctrl Pts',(-12.1935275275859,-72.9940114982936,
64.8139948810565));
#109660=CARTESIAN_POINT('Ctrl Pts',(-12.1778786286812,-72.4716137046989,
64.9601802674696));
#109661=CARTESIAN_POINT('Ctrl Pts',(-12.1468429563381,-71.4477448127881,
65.3566266280318));
#109662=CARTESIAN_POINT('Ctrl Pts',(-12.1315521837551,-70.9498506072715,
65.6087655502416));
#109663=CARTESIAN_POINT('Ctrl Pts',(-12.1007394784222,-70.0325547170444,
66.194260241545));
#109664=CARTESIAN_POINT('Ctrl Pts',(-12.0851889193739,-69.6126902487047,
66.5220985011274));
#109665=CARTESIAN_POINT('Ctrl Pts',(-12.0621049879559,-69.0288807199379,
67.0745129171562));
#109666=CARTESIAN_POINT('Ctrl Pts',(-12.0543598138416,-68.840346558027,
67.2711287936886));
#109667=CARTESIAN_POINT('Ctrl Pts',(-12.0316473743537,-68.3116677833476,
67.8790251409699));
#109668=CARTESIAN_POINT('Ctrl Pts',(-12.0169935993769,-68.0007787500592,
68.3139146928697));
#109669=CARTESIAN_POINT('Ctrl Pts',(-11.9857968177324,-67.4492373973459,
69.2651114990225));
#109670=CARTESIAN_POINT('Ctrl Pts',(-11.9692137356407,-67.2154872687839,
69.7823487810449));
#109671=CARTESIAN_POINT('Ctrl Pts',(-11.9452118668441,-66.9490366567213,
70.5772348364475));
#109672=CARTESIAN_POINT('Ctrl Pts',(-11.9374997910295,-66.8751218618912,
70.839367153819));
#109673=CARTESIAN_POINT('Ctrl Pts',(-11.9149154892498,-66.6948599518037,
71.6224916727647));
#109674=CARTESIAN_POINT('Ctrl Pts',(-11.9003192101525,-66.6250678775911,
72.1504973487997));
#109675=CARTESIAN_POINT('Ctrl Pts',(-11.8822182814411,-66.6018737675323,
72.7839881357388));
#109676=CARTESIAN_POINT('Ctrl Pts',(-11.8792748568318,-66.6,72.8864534468495));
#109677=CARTESIAN_POINT('Ctrl Pts',(-11.8763230992193,-66.6,72.98888938658));
#109678=CARTESIAN_POINT('Origin',(20.412052742069,1.37771738462078E-14,
115.762503617193));
#109679=CARTESIAN_POINT('',(4.63472787570938,-6.63404734029626E-9,124.183946153848));
#109680=CARTESIAN_POINT('',(4.68550323141337,7.30187960605121E-9,124.471907505537));
#109681=CARTESIAN_POINT('',(3.67032094086137,1.16952742876573E-14,118.71452263753));
#109682=CARTESIAN_POINT('',(30.2384437550856,-14.4989439202996,120.376781885352));
#109683=CARTESIAN_POINT('Ctrl Pts',(4.68550323141337,1.46037510969853E-8,
124.471907505537));
#109684=CARTESIAN_POINT('Ctrl Pts',(4.68564827370219,-0.0743379810781902,
124.4727300816));
#109685=CARTESIAN_POINT('Ctrl Pts',(4.68627286904241,-0.148681666873179,
124.473464359407));
#109686=CARTESIAN_POINT('Ctrl Pts',(4.69257555007263,-0.572921405614114,
124.477154396249));
#109687=CARTESIAN_POINT('Ctrl Pts',(4.70840025566492,-0.922591984769783,
124.478256410096));
#109688=CARTESIAN_POINT('Ctrl Pts',(4.79765327972258,-2.10050392452701,
124.475642272939));
#109689=CARTESIAN_POINT('Ctrl Pts',(4.92026554240755,-2.92379093403069,
124.463270047188));
#109690=CARTESIAN_POINT('Ctrl Pts',(5.23049420774179,-4.31005019464808,
124.424904003855));
#109691=CARTESIAN_POINT('Ctrl Pts',(5.38864643116668,-4.87819396260196,
124.403924131801));
#109692=CARTESIAN_POINT('Ctrl Pts',(5.72449970156122,-5.88215598968838,
124.357091151595));
#109693=CARTESIAN_POINT('Ctrl Pts',(5.891563799614,-6.32098936543384,124.333097915783));
#109694=CARTESIAN_POINT('Ctrl Pts',(6.39590073385846,-7.49844651927192,
124.258670844125));
#109695=CARTESIAN_POINT('Ctrl Pts',(6.76776540910955,-8.22049418077532,
124.201991251208));
#109696=CARTESIAN_POINT('Ctrl Pts',(7.55229337962165,-9.5095650593795,124.080723281539));
#109697=CARTESIAN_POINT('Ctrl Pts',(7.95146783756154,-10.0829863563159,
124.018416423071));
#109698=CARTESIAN_POINT('Ctrl Pts',(8.82277626176177,-11.18364055349,123.881264840435));
#109699=CARTESIAN_POINT('Ctrl Pts',(9.29491914946344,-11.7091190057174,
123.806386896715));
#109700=CARTESIAN_POINT('Ctrl Pts',(10.3889305316597,-12.7836098358227,
123.630927636382));
#109701=CARTESIAN_POINT('Ctrl Pts',(11.0210922270172,-13.3192253171763,
123.528559568179));
#109702=CARTESIAN_POINT('Ctrl Pts',(12.262108460875,-14.2225124881724,123.327179453397));
#109703=CARTESIAN_POINT('Ctrl Pts',(12.8600982777439,-14.602348817636,123.229976122717));
#109704=CARTESIAN_POINT('Ctrl Pts',(14.0686669900347,-15.2665387834022,
123.033146520733));
#109705=CARTESIAN_POINT('Ctrl Pts',(14.6760428194664,-15.5541209818477,
122.934038709541));
#109706=CARTESIAN_POINT('Ctrl Pts',(16.0579033604686,-16.1090380798308,
122.707406272866));
#109707=CARTESIAN_POINT('Ctrl Pts',(16.8379981425549,-16.3573452565906,
122.578898903116));
#109708=CARTESIAN_POINT('Ctrl Pts',(18.3253530897156,-16.712404758408,122.334106834635));
#109709=CARTESIAN_POINT('Ctrl Pts',(19.0275441866904,-16.8329062920111,
122.218618283029));
#109710=CARTESIAN_POINT('Ctrl Pts',(20.4144969794751,-16.979830770254,121.990588689274));
#109711=CARTESIAN_POINT('Ctrl Pts',(21.0975413897469,-17.0096851753466,
121.878299745259));
#109712=CARTESIAN_POINT('Ctrl Pts',(22.597464642579,-16.9823965839081,121.63098305236));
#109713=CARTESIAN_POINT('Ctrl Pts',(23.4122980386457,-16.9070459274975,
121.496350274446));
#109714=CARTESIAN_POINT('Ctrl Pts',(24.9340099703691,-16.6517959298589,
121.245655591693));
#109715=CARTESIAN_POINT('Ctrl Pts',(25.6411075310777,-16.4848888458814,
121.129465369349));
#109716=CARTESIAN_POINT('Ctrl Pts',(26.6318113393197,-16.1812956925445,
120.967037051241));
#109717=CARTESIAN_POINT('Ctrl Pts',(26.9257278238795,-16.0821510867243,
120.918889926016));
#109718=CARTESIAN_POINT('Ctrl Pts',(27.5878226962084,-15.8379819205855,
120.810455249672));
#109719=CARTESIAN_POINT('Ctrl Pts',(27.9539936514165,-15.6879134099066,
120.750483768592));
#109720=CARTESIAN_POINT('Ctrl Pts',(28.9770567766332,-15.2254104878708,
120.582852082652));
#109721=CARTESIAN_POINT('Ctrl Pts',(29.6196615370995,-14.8827084382633,
120.477610290641));
#109722=CARTESIAN_POINT('Ctrl Pts',(30.2384437550856,-14.4989439202997,
120.376781885352));
#109723=CARTESIAN_POINT('',(30.1878779053518,-14.4989439202996,120.090008701063));
#109724=CARTESIAN_POINT('',(29.1530537532117,-14.4989439202996,114.221229300528));
#109725=CARTESIAN_POINT('Ctrl Pts',(30.1878779053518,-14.4989439202996,
120.090008701063));
#109726=CARTESIAN_POINT('Ctrl Pts',(29.5701295220062,-14.8820451102276,
120.190460271193));
#109727=CARTESIAN_POINT('Ctrl Pts',(28.9285701908142,-15.2242262275709,
120.294914406511));
#109728=CARTESIAN_POINT('Ctrl Pts',(27.9073160249098,-15.6861599886167,
120.461871165917));
#109729=CARTESIAN_POINT('Ctrl Pts',(27.5418339166123,-15.8360734413756,
120.521789705476));
#109730=CARTESIAN_POINT('Ctrl Pts',(26.8646223178921,-16.0861078665858,
120.633036292489));
#109731=CARTESIAN_POINT('Ctrl Pts',(26.5545570371305,-16.1903051542107,
120.684039716594));
#109732=CARTESIAN_POINT('Ctrl Pts',(25.5570642222654,-16.4930572565071,
120.848181542795));
#109733=CARTESIAN_POINT('Ctrl Pts',(24.8600455730495,-16.6563022852734,
120.962939974118));
#109734=CARTESIAN_POINT('Ctrl Pts',(23.3507635550836,-16.9082118704466,
121.211177868491));
#109735=CARTESIAN_POINT('Ctrl Pts',(22.5380569345925,-16.9828670967508,
121.344681854524));
#109736=CARTESIAN_POINT('Ctrl Pts',(21.0480142701009,-17.0094006459033,
121.590004776062));
#109737=CARTESIAN_POINT('Ctrl Pts',(20.3727177501221,-16.9800894283706,
121.701531418683));
#109738=CARTESIAN_POINT('Ctrl Pts',(18.9896530367671,-16.8349601996727,
121.929735369205));
#109739=CARTESIAN_POINT('Ctrl Pts',(18.2837348045804,-16.7142929021189,
122.046064271911));
#109740=CARTESIAN_POINT('Ctrl Pts',(16.7908971654717,-16.3584520046763,
122.291371962011));
#109741=CARTESIAN_POINT('Ctrl Pts',(16.0089806753838,-16.1097518691709,
122.419412700195));
#109742=CARTESIAN_POINT('Ctrl Pts',(14.6252517891792,-15.5541270414664,
122.646037158988));
#109743=CARTESIAN_POINT('Ctrl Pts',(14.0177604233313,-15.2664441128617,
122.745669266514));
#109744=CARTESIAN_POINT('Ctrl Pts',(12.8092235798815,-14.6021563898349,
122.94325916373));
#109745=CARTESIAN_POINT('Ctrl Pts',(12.2113582116683,-14.2223614982591,
123.040639736479));
#109746=CARTESIAN_POINT('Ctrl Pts',(10.9703857883329,-13.319140548469,123.241587762053));
#109747=CARTESIAN_POINT('Ctrl Pts',(10.3381161873546,-12.783541683539,123.34317782452));
#109748=CARTESIAN_POINT('Ctrl Pts',(9.24412514645092,-11.7091171754883,
123.518306828543));
#109749=CARTESIAN_POINT('Ctrl Pts',(8.77212271484894,-11.1836890435598,
123.593730560265));
#109750=CARTESIAN_POINT('Ctrl Pts',(7.90096264894464,-10.0830689066474,
123.731645860865));
#109751=CARTESIAN_POINT('Ctrl Pts',(7.50180343829981,-9.50962956334363,
123.7941365166));
#109752=CARTESIAN_POINT('Ctrl Pts',(6.71725850540307,-8.22065362099649,
123.915004885026));
#109753=CARTESIAN_POINT('Ctrl Pts',(6.34531547753253,-7.4987275441189,123.970953455009));
#109754=CARTESIAN_POINT('Ctrl Pts',(5.84016412446256,-6.31956294685888,
124.045228617864));
#109755=CARTESIAN_POINT('Ctrl Pts',(5.67248743109575,-5.87882814455977,
124.069518606313));
#109756=CARTESIAN_POINT('Ctrl Pts',(5.33660785118728,-4.87340004955567,
124.116937905333));
#109757=CARTESIAN_POINT('Ctrl Pts',(5.1788295887776,-4.30577333755577,124.138227112189));
#109758=CARTESIAN_POINT('Ctrl Pts',(4.868097817236,-2.91562234570062,124.1768908874));
#109759=CARTESIAN_POINT('Ctrl Pts',(4.74525087389593,-2.0877918727058,124.188805864713));
#109760=CARTESIAN_POINT('Ctrl Pts',(4.65694693069434,-0.908304068096513,
124.190531793008));
#109761=CARTESIAN_POINT('Ctrl Pts',(4.64148162450515,-0.561621361795577,
124.189204435518));
#109762=CARTESIAN_POINT('Ctrl Pts',(4.63545287952606,-0.14314631240032,
124.185455054707));
#109763=CARTESIAN_POINT('Ctrl Pts',(4.63486751849338,-0.0715705611967255,
124.184738107108));
#109764=CARTESIAN_POINT('Ctrl Pts',(4.63472787570938,-1.32681063758668E-8,
124.183946153848));
#109765=CARTESIAN_POINT('Origin',(20.412052742069,1.37771738462078E-14,
115.762503617193));
#109766=CARTESIAN_POINT('',(4.42635006251054,-6.99305973109813E-9,123.002176850242));
#109767=CARTESIAN_POINT('',(4.47712541821256,7.41991074646819E-9,123.290138201919));
#109768=CARTESIAN_POINT('',(3.67032094086137,1.16952742876573E-14,118.71452263753));
#109769=CARTESIAN_POINT('Ctrl Pts',(4.47712541821256,1.48397794296156E-8,
123.290138201919));
#109770=CARTESIAN_POINT('Ctrl Pts',(4.47726710739396,-0.0726194254213628,
123.290941761563));
#109771=CARTESIAN_POINT('Ctrl Pts',(4.47786642876489,-0.145242030801444,
123.291661033145));
#109772=CARTESIAN_POINT('Ctrl Pts',(4.4839900234646,-0.565888684765446,
123.295342776981));
#109773=CARTESIAN_POINT('Ctrl Pts',(4.49956960224922,-0.913695551972098,
123.296467862352));
#109774=CARTESIAN_POINT('Ctrl Pts',(4.5881584050187,-2.09260838461004,123.293981907897));
#109775=CARTESIAN_POINT('Ctrl Pts',(4.71087360778027,-2.91874233122078,
123.281620794682));
#109776=CARTESIAN_POINT('Ctrl Pts',(5.02145288530558,-4.30744933963609,
123.243220534685));
#109777=CARTESIAN_POINT('Ctrl Pts',(5.17941587740385,-4.87527836343719,
123.222269549424));
#109778=CARTESIAN_POINT('Ctrl Pts',(5.51534037461342,-5.88011093708854,
123.175434153231));
#109779=CARTESIAN_POINT('Ctrl Pts',(5.68279148735017,-6.32008300865983,
123.151387016631));
#109780=CARTESIAN_POINT('Ctrl Pts',(6.1928471241179,-7.51085101143989,123.076115498515));
#109781=CARTESIAN_POINT('Ctrl Pts',(6.57167088586724,-8.24429588437859,
123.018351219207));
#109782=CARTESIAN_POINT('Ctrl Pts',(7.37775550214019,-9.56183272718522,
122.893697423682));
#109783=CARTESIAN_POINT('Ctrl Pts',(7.79222255393772,-10.1517879468699,
122.828968417862));
#109784=CARTESIAN_POINT('Ctrl Pts',(8.65107706329844,-11.2228313172068,
122.693663517979));
#109785=CARTESIAN_POINT('Ctrl Pts',(9.08844495476356,-11.7080474871114,
122.6242758755));
#109786=CARTESIAN_POINT('Ctrl Pts',(9.79559488252792,-12.4068905234439,
122.51091543823));
#109787=CARTESIAN_POINT('Ctrl Pts',(10.0460199870314,-12.6397930351342,
122.470590049202));
#109788=CARTESIAN_POINT('Ctrl Pts',(10.9291441118157,-13.4124499277954,
122.328005155286));
#109789=CARTESIAN_POINT('Ctrl Pts',(11.5940608970191,-13.9124565891058,
122.220074715601));
#109790=CARTESIAN_POINT('Ctrl Pts',(12.7826564008686,-14.6752591008048,
122.026875198773));
#109791=CARTESIAN_POINT('Ctrl Pts',(13.2884442990623,-14.9637962926425,
121.944572128034));
#109792=CARTESIAN_POINT('Ctrl Pts',(14.229393597922,-15.4373161629874,121.791102013483));
#109793=CARTESIAN_POINT('Ctrl Pts',(14.659459240168,-15.6313578002585,121.720816239832));
#109794=CARTESIAN_POINT('Ctrl Pts',(15.8542046992472,-16.1105360086866,
121.524865880265));
#109795=CARTESIAN_POINT('Ctrl Pts',(16.6321701366166,-16.357971279845,121.396709931516));
#109796=CARTESIAN_POINT('Ctrl Pts',(18.1175366256271,-16.7125236047627,
121.152245156299));
#109797=CARTESIAN_POINT('Ctrl Pts',(18.8199602692764,-16.833035010911,121.03671845183));
#109798=CARTESIAN_POINT('Ctrl Pts',(20.1759966418076,-16.9765988721232,
120.813771847341));
#109799=CARTESIAN_POINT('Ctrl Pts',(20.827583214368,-17.0068888142712,120.706660954248));
#109800=CARTESIAN_POINT('Ctrl Pts',(21.820209012274,-16.9943992689521,120.543023716793));
#109801=CARTESIAN_POINT('Ctrl Pts',(22.1609957504813,-16.9795708430236,
120.486779729856));
#109802=CARTESIAN_POINT('Ctrl Pts',(23.325454646438,-16.8927916932291,120.294602461011));
#109803=CARTESIAN_POINT('Ctrl Pts',(24.1442118184467,-16.7696892735206,
120.159547596836));
#109804=CARTESIAN_POINT('Ctrl Pts',(25.5176572295265,-16.4567561936441,
119.93376984732));
#109805=CARTESIAN_POINT('Ctrl Pts',(26.0775963611282,-16.2978290350979,
119.841933221202));
#109806=CARTESIAN_POINT('Ctrl Pts',(27.0706331175051,-15.9587349207325,
119.679247215503));
#109807=CARTESIAN_POINT('Ctrl Pts',(27.506582159557,-15.7890434224299,119.607878628462));
#109808=CARTESIAN_POINT('Ctrl Pts',(28.6822938465005,-15.2733798568659,
119.415240504232));
#109809=CARTESIAN_POINT('Ctrl Pts',(29.4050751174609,-14.890910317626,119.296813994894));
#109810=CARTESIAN_POINT('Ctrl Pts',(30.7029291554557,-14.0774185471333,
119.085409354161));
#109811=CARTESIAN_POINT('Ctrl Pts',(31.2838112138742,-13.659438615725,118.991311323907));
#109812=CARTESIAN_POINT('Ctrl Pts',(32.3436767356981,-12.7891934101714,
118.82059023505));
#109813=CARTESIAN_POINT('Ctrl Pts',(32.8262181267685,-12.3434373449856,
118.74329168774));
#109814=CARTESIAN_POINT('Ctrl Pts',(33.5203587225289,-11.6228610168815,
118.632291722921));
#109815=CARTESIAN_POINT('Ctrl Pts',(33.7512839999439,-11.368044617997,118.595420807397));
#109816=CARTESIAN_POINT('Ctrl Pts',(34.5148247305714,-10.4722093879614,
118.473935462488));
#109817=CARTESIAN_POINT('Ctrl Pts',(35.0083733806634,-9.79857835634418,
118.396221496327));
#109818=CARTESIAN_POINT('Ctrl Pts',(35.7623443492901,-8.59329982286537,
118.279671845147));
#109819=CARTESIAN_POINT('Ctrl Pts',(36.047962815817,-8.07969204257989,118.236205745305));
#109820=CARTESIAN_POINT('Ctrl Pts',(36.5145795284203,-7.12849545794011,
118.166340750437));
#109821=CARTESIAN_POINT('Ctrl Pts',(36.7048996527446,-6.69627012201427,
118.138281759079));
#109822=CARTESIAN_POINT('Ctrl Pts',(37.1775286435375,-5.49021941209475,
118.06960451221));
#109823=CARTESIAN_POINT('Ctrl Pts',(37.4225200973712,-4.7028020707478,118.035415526615));
#109824=CARTESIAN_POINT('Ctrl Pts',(37.7742471616853,-3.2005590827442,117.990806851836));
#109825=CARTESIAN_POINT('Ctrl Pts',(37.8942651576518,-2.49078908479819,
117.977949248992));
#109826=CARTESIAN_POINT('Ctrl Pts',(38.0393918667326,-1.11430684535171,
117.968546067397));
#109827=CARTESIAN_POINT('Ctrl Pts',(38.0708575434234,-0.449571596658077,
117.970832686332));
#109828=CARTESIAN_POINT('Ctrl Pts',(38.0601978907253,0.562330993406072,
117.984167448484));
#109829=CARTESIAN_POINT('Ctrl Pts',(38.0460622599845,0.909200456291852,
117.990521993183));
#109830=CARTESIAN_POINT('Ctrl Pts',(37.9623049703988,2.08859751610441,118.018430670423));
#109831=CARTESIAN_POINT('Ctrl Pts',(37.8427218298197,2.91614475365796,118.048807782335));
#109832=CARTESIAN_POINT('Ctrl Pts',(37.5375804721073,4.30605508152657,118.118989196761));
#109833=CARTESIAN_POINT('Ctrl Pts',(37.3820784757013,4.87371622890115,118.153308155663));
#109834=CARTESIAN_POINT('Ctrl Pts',(37.0503498179034,5.87903954221305,118.224203757609));
#109835=CARTESIAN_POINT('Ctrl Pts',(36.8845582822338,6.31964458661868,118.258924257963));
#109836=CARTESIAN_POINT('Ctrl Pts',(36.3772894788796,7.5156312662834,118.363098743256));
#109837=CARTESIAN_POINT('Ctrl Pts',(35.9989345561713,8.25337230171225,118.438899254589));
#109838=CARTESIAN_POINT('Ctrl Pts',(35.1889221097438,9.58454817338106,118.599402767094));
#109839=CARTESIAN_POINT('Ctrl Pts',(34.7693860529488,10.1833906406674,118.681875995441));
#109840=CARTESIAN_POINT('Ctrl Pts',(33.9015402757136,11.2659977141092,118.851253797059));
#109841=CARTESIAN_POINT('Ctrl Pts',(33.4608494056369,11.7543667180551,118.936756265481));
#109842=CARTESIAN_POINT('Ctrl Pts',(32.4088127439031,12.7911693969336,119.139099846695));
#109843=CARTESIAN_POINT('Ctrl Pts',(31.783759835985,13.3228138808301,119.258353971258));
#109844=CARTESIAN_POINT('Ctrl Pts',(30.5529657072893,14.222935742887,119.492760409275));
#109845=CARTESIAN_POINT('Ctrl Pts',(29.9575394264109,14.6028899201329,119.605991973676));
#109846=CARTESIAN_POINT('Ctrl Pts',(28.7548010288241,15.2668114071306,119.834336761636));
#109847=CARTESIAN_POINT('Ctrl Pts',(28.1507279910629,15.5541070166201,119.948832320717));
#109848=CARTESIAN_POINT('Ctrl Pts',(26.7795332931003,16.1071303561815,120.207578457541));
#109849=CARTESIAN_POINT('Ctrl Pts',(26.007001721396,16.3543933621251,120.352791411082));
#109850=CARTESIAN_POINT('Ctrl Pts',(24.5388686012415,16.7076229142211,120.628974248775));
#109851=CARTESIAN_POINT('Ctrl Pts',(23.8483729754278,16.8277840263982,120.758944926695));
#109852=CARTESIAN_POINT('Ctrl Pts',(22.4868589598444,16.9759982442222,121.015307040707));
#109853=CARTESIAN_POINT('Ctrl Pts',(21.8175169347674,17.0076877567862,121.141361231551));
#109854=CARTESIAN_POINT('Ctrl Pts',(20.8012630487746,16.9936341543844,121.332253163968));
#109855=CARTESIAN_POINT('Ctrl Pts',(20.4546880305645,16.9778537650809,121.39728774047));
#109856=CARTESIAN_POINT('Ctrl Pts',(19.2985521900949,16.888455261997,121.61425092934));
#109857=CARTESIAN_POINT('Ctrl Pts',(18.4938436921505,16.7657433432543,121.76534324417));
#109858=CARTESIAN_POINT('Ctrl Pts',(17.1353543843919,16.4541818642168,122.02117199174));
#109859=CARTESIAN_POINT('Ctrl Pts',(16.5765828552586,16.2945175961528,122.126611493036));
#109860=CARTESIAN_POINT('Ctrl Pts',(15.5911296520151,15.9557097573121,122.312747046023));
#109861=CARTESIAN_POINT('Ctrl Pts',(15.16141311943,15.7875404630745,122.393962901539));
#109862=CARTESIAN_POINT('Ctrl Pts',(14.0057919657937,15.2785940527204,122.612212836553));
#109863=CARTESIAN_POINT('Ctrl Pts',(13.2962367064769,14.9025423280946,122.74621669592));
#109864=CARTESIAN_POINT('Ctrl Pts',(12.0297019974583,14.1089057733664,122.986605875152));
#109865=CARTESIAN_POINT('Ctrl Pts',(11.4664028315628,13.7050046544477,123.094008585962));
#109866=CARTESIAN_POINT('Ctrl Pts',(10.3852265119859,12.8230888014638,123.301133501878));
#109867=CARTESIAN_POINT('Ctrl Pts',(9.86908329909161,12.3450451709572,123.400518359888));
#109868=CARTESIAN_POINT('Ctrl Pts',(8.81379677784519,11.2370635297596,123.604040065611));
#109869=CARTESIAN_POINT('Ctrl Pts',(8.28784808843838,10.5966828690373,123.705878681044));
#109870=CARTESIAN_POINT('Ctrl Pts',(7.4011641493878,9.33936280823163,123.879672015218));
#109871=CARTESIAN_POINT('Ctrl Pts',(7.0284410076656,8.73343022202691,123.953633541791));
#109872=CARTESIAN_POINT('Ctrl Pts',(6.37727593432207,7.50919786515016,124.084722821822));
#109873=CARTESIAN_POINT('Ctrl Pts',(6.09559017557435,6.89417277130976,124.142376107457));
#109874=CARTESIAN_POINT('Ctrl Pts',(5.55309807168489,5.49682657683749,124.255024330068));
#109875=CARTESIAN_POINT('Ctrl Pts',(5.31070621857193,4.70892781309154,124.306779935966));
#109876=CARTESIAN_POINT('Ctrl Pts',(4.96510428886854,3.20971846714564,124.385093552756));
#109877=CARTESIAN_POINT('Ctrl Pts',(4.84805761747887,2.50358477454962,124.413992821971));
#109878=CARTESIAN_POINT('Ctrl Pts',(4.71425788489729,1.19668922403474,124.452953463954));
#109879=CARTESIAN_POINT('Ctrl Pts',(4.68433543010682,0.598528962184033,
124.465284572257));
#109880=CARTESIAN_POINT('Ctrl Pts',(4.68550323141337,1.46037466841609E-8,
124.471907505537));
#109881=CARTESIAN_POINT('Ctrl Pts',(4.63472787570938,-1.32681063758668E-8,
124.183946153848));
#109882=CARTESIAN_POINT('Ctrl Pts',(4.63357157043953,0.592636422127183,
124.177388423457));
#109883=CARTESIAN_POINT('Ctrl Pts',(4.66297372869761,1.18491592147218,124.165673028352));
#109884=CARTESIAN_POINT('Ctrl Pts',(4.79535858097764,2.48992208384337,124.127738563659));
#109885=CARTESIAN_POINT('Ctrl Pts',(4.91258361015162,3.1999427312807,124.098981089495));
#109886=CARTESIAN_POINT('Ctrl Pts',(5.25855027326533,4.70347259587108,124.02016279834));
#109887=CARTESIAN_POINT('Ctrl Pts',(5.50069974380765,5.49189538696322,123.967681467881));
#109888=CARTESIAN_POINT('Ctrl Pts',(5.9729331803421,6.70938852304439,123.869335083525));
#109889=CARTESIAN_POINT('Ctrl Pts',(6.16643530167966,7.15174597138867,123.829807597709));
#109890=CARTESIAN_POINT('Ctrl Pts',(6.63427325815816,8.10874803164791,123.735420060841));
#109891=CARTESIAN_POINT('Ctrl Pts',(6.91673549416129,8.61859562765863,123.679122811554));
#109892=CARTESIAN_POINT('Ctrl Pts',(7.66404939373591,9.81809160784466,123.531261478371));
#109893=CARTESIAN_POINT('Ctrl Pts',(8.15418404773268,10.4896091503913,123.435085626319));
#109894=CARTESIAN_POINT('Ctrl Pts',(8.91077529748588,11.3805295719812,123.287890510379));
#109895=CARTESIAN_POINT('Ctrl Pts',(9.13825790805126,11.6325708872509,123.243780892955));
#109896=CARTESIAN_POINT('Ctrl Pts',(9.81917170333162,12.3426106797737,123.112310209786));
#109897=CARTESIAN_POINT('Ctrl Pts',(10.2912190591203,12.7813310244438,123.021909785701));
#109898=CARTESIAN_POINT('Ctrl Pts',(11.3402602602008,13.6493968402062,122.821635047057));
#109899=CARTESIAN_POINT('Ctrl Pts',(11.921991240648,14.0707877586969,122.710903425858));
#109900=CARTESIAN_POINT('Ctrl Pts',(13.2195939591294,14.8886845370294,122.464188312415));
#109901=CARTESIAN_POINT('Ctrl Pts',(13.9411142114959,15.2723924140214,122.327155221566));
#109902=CARTESIAN_POINT('Ctrl Pts',(15.1141058611886,15.7891010123792,122.10534577233));
#109903=CARTESIAN_POINT('Ctrl Pts',(15.5484701412069,15.9588860860178,122.023465292593));
#109904=CARTESIAN_POINT('Ctrl Pts',(16.5375748734356,16.2980065214732,121.837243554514));
#109905=CARTESIAN_POINT('Ctrl Pts',(17.0951546556599,16.4568941708419,121.732399387658));
#109906=CARTESIAN_POINT('Ctrl Pts',(18.4634379763096,16.7698780388701,121.474983543641));
#109907=CARTESIAN_POINT('Ctrl Pts',(19.2794125264515,16.8929924618159,121.321329198961));
#109908=CARTESIAN_POINT('Ctrl Pts',(20.4394063893845,16.9796485897213,121.102938142948));
#109909=CARTESIAN_POINT('Ctrl Pts',(20.7785206470763,16.9944338485635,121.039108612961));
#109910=CARTESIAN_POINT('Ctrl Pts',(21.7659172030619,17.006851832197,120.853452568004));
#109911=CARTESIAN_POINT('Ctrl Pts',(22.4139513849207,16.9766294906685,120.731921604675));
#109912=CARTESIAN_POINT('Ctrl Pts',(23.7640956552689,16.8332861610225,120.478497874152));
#109913=CARTESIAN_POINT('Ctrl Pts',(24.4641618784954,16.7127549740021,120.346946306104));
#109914=CARTESIAN_POINT('Ctrl Pts',(25.9449995939361,16.3579054491669,120.067983022337));
#109915=CARTESIAN_POINT('Ctrl Pts',(26.7207744482822,16.1100930037214,119.921396678967));
#109916=CARTESIAN_POINT('Ctrl Pts',(27.9174338041455,15.6278795962631,119.695311392062));
#109917=CARTESIAN_POINT('Ctrl Pts',(28.351459801186,15.4308092630801,119.613381450854));
#109918=CARTESIAN_POINT('Ctrl Pts',(29.291496151248,14.9540699813087,119.435738308823));
#109919=CARTESIAN_POINT('Ctrl Pts',(29.7927425512057,14.6660643413089,119.340860955432));
#109920=CARTESIAN_POINT('Ctrl Pts',(30.9717280914689,13.904309659069,119.116879611861));
#109921=CARTESIAN_POINT('Ctrl Pts',(31.6315847950258,13.40485592162,118.990775086813));
#109922=CARTESIAN_POINT('Ctrl Pts',(32.5069739183114,12.6339912528137,118.822627782942));
#109923=CARTESIAN_POINT('Ctrl Pts',(32.7546636230453,12.4021788087266,118.774952628272));
#109924=CARTESIAN_POINT('Ctrl Pts',(33.452587944606,11.7082093421025,118.640472513404));
#109925=CARTESIAN_POINT('Ctrl Pts',(33.8838359623335,11.2271475981415,118.557259176847));
#109926=CARTESIAN_POINT('Ctrl Pts',(34.7362228595714,10.158936018922,118.391656022213));
#109927=CARTESIAN_POINT('Ctrl Pts',(35.1496104240714,9.56704498839497,118.310611140704));
#109928=CARTESIAN_POINT('Ctrl Pts',(35.9524576718099,8.24551765601765,118.151124099521));
#109929=CARTESIAN_POINT('Ctrl Pts',(36.3291196246265,7.51002525281455,118.074883742046));
#109930=CARTESIAN_POINT('Ctrl Pts',(36.9168427607941,6.12344419029734,117.953856293388));
#109931=CARTESIAN_POINT('Ctrl Pts',(37.1449006259391,5.4816989161467,117.90612396153));
#109932=CARTESIAN_POINT('Ctrl Pts',(37.5323543182424,4.14422801197669,117.822276593452));
#109933=CARTESIAN_POINT('Ctrl Pts',(37.6878035740198,3.44869736947842,117.786842040869));
#109934=CARTESIAN_POINT('Ctrl Pts',(37.9296721133059,1.92890058915011,117.726415139698));
#109935=CARTESIAN_POINT('Ctrl Pts',(38.0006893590256,1.10391386477906,117.704076319898));
#109936=CARTESIAN_POINT('Ctrl Pts',(38.021701197603,-0.389567927783994,
117.683161829751));
#109937=CARTESIAN_POINT('Ctrl Pts',(37.9925285049393,-1.05603275334111,
117.680953085576));
#109938=CARTESIAN_POINT('Ctrl Pts',(37.8505778491347,-2.44754414582975,
117.690434762363));
#109939=CARTESIAN_POINT('Ctrl Pts',(37.7299864086294,-3.17042983055582,
117.703476486874));
#109940=CARTESIAN_POINT('Ctrl Pts',(37.3754127767892,-4.69161292819189,
117.747983257673));
#109941=CARTESIAN_POINT('Ctrl Pts',(37.1288750518075,-5.4849853461492,117.781610581606));
#109942=CARTESIAN_POINT('Ctrl Pts',(36.6543687488704,-6.69561257472272,
117.850284748281));
#109943=CARTESIAN_POINT('Ctrl Pts',(36.4645789815986,-7.12680305931145,
117.878476313845));
#109944=CARTESIAN_POINT('Ctrl Pts',(35.998595574586,-8.07733625586983,117.948838191852));
#109945=CARTESIAN_POINT('Ctrl Pts',(35.7129648268933,-8.59125722700539,
117.992670610368));
#109946=CARTESIAN_POINT('Ctrl Pts',(34.9601596152666,-9.79506354990021,
118.109288374321));
#109947=CARTESIAN_POINT('Ctrl Pts',(34.4680167975701,-10.4671064186872,
118.186325741409));
#109948=CARTESIAN_POINT('Ctrl Pts',(33.705247540462,-11.3628036701157,118.3069797176));
#109949=CARTESIAN_POINT('Ctrl Pts',(33.4733982350078,-11.6187942389264,
118.34380303707));
#109950=CARTESIAN_POINT('Ctrl Pts',(32.9244829807059,-12.1888654406497,
118.431436221565));
#109951=CARTESIAN_POINT('Ctrl Pts',(32.6025707023191,-12.4977728391668,
118.483182864766));
#109952=CARTESIAN_POINT('Ctrl Pts',(31.8279519028623,-13.184307498477,118.608177692849));
#109953=CARTESIAN_POINT('Ctrl Pts',(31.3670494630096,-13.5515373741682,
118.682876301331));
#109954=CARTESIAN_POINT('Ctrl Pts',(30.2678209441983,-14.3366710872971,
118.861301853471));
#109955=CARTESIAN_POINT('Ctrl Pts',(29.6185613468078,-14.7366042885872,
118.966860616838));
#109956=CARTESIAN_POINT('Ctrl Pts',(28.6050470860586,-15.2692166691634,
119.132039055448));
#109957=CARTESIAN_POINT('Ctrl Pts',(28.2593100844575,-15.4359608484853,
119.188460202513));
#109958=CARTESIAN_POINT('Ctrl Pts',(27.2632907286753,-15.8746670555202,
119.351402760385));
#109959=CARTESIAN_POINT('Ctrl Pts',(26.6014253488124,-16.1173823843318,
119.460260186855));
#109960=CARTESIAN_POINT('Ctrl Pts',(25.2629728430788,-16.5138257147529,
119.680526481603));
#109961=CARTESIAN_POINT('Ctrl Pts',(24.5881053523096,-16.6686070365398,
119.791627848937));
#109962=CARTESIAN_POINT('Ctrl Pts',(23.1047903648245,-16.9123829267381,
120.035588552737));
#109963=CARTESIAN_POINT('Ctrl Pts',(22.2954612659473,-16.9849535060156,
120.168537177851));
#109964=CARTESIAN_POINT('Ctrl Pts',(20.7767940116893,-17.0091783921386,
120.418590169224));
#109965=CARTESIAN_POINT('Ctrl Pts',(20.0694661877503,-16.9751003325265,
120.535428990361));
#109966=CARTESIAN_POINT('Ctrl Pts',(18.6818127374102,-16.8187217732458,
120.764362358282));
#109967=CARTESIAN_POINT('Ctrl Pts',(18.0025818287076,-16.6989230056301,
120.876265683671));
#109968=CARTESIAN_POINT('Ctrl Pts',(16.55159241383,-16.3486215821669,121.114669651962));
#109969=CARTESIAN_POINT('Ctrl Pts',(15.7849805428881,-16.1035399671801,
121.240201911816));
#109970=CARTESIAN_POINT('Ctrl Pts',(14.4169345960471,-15.5541003951089,
121.464257992389));
#109971=CARTESIAN_POINT('Ctrl Pts',(13.8105395415181,-15.2669658625495,
121.563710072064));
#109972=CARTESIAN_POINT('Ctrl Pts',(12.6025112117024,-14.6031918160419,
121.761218343765));
#109973=CARTESIAN_POINT('Ctrl Pts',(12.0041572769462,-14.2231713457374,
121.858679413648));
#109974=CARTESIAN_POINT('Ctrl Pts',(10.762564819961,-13.3196002833448,122.059728813854));
#109975=CARTESIAN_POINT('Ctrl Pts',(10.1301410017152,-12.7839116009468,
122.161343974529));
#109976=CARTESIAN_POINT('Ctrl Pts',(9.03574689592426,-11.7091384543426,
122.336537673811));
#109977=CARTESIAN_POINT('Ctrl Pts',(8.56351023550782,-11.1834393583186,
122.411998858786));
#109978=CARTESIAN_POINT('Ctrl Pts',(7.69225645978352,-10.082607814245,122.549928097048));
#109979=CARTESIAN_POINT('Ctrl Pts',(7.29319076719589,-9.50926708152108,
122.61240366853));
#109980=CARTESIAN_POINT('Ctrl Pts',(6.5087410661157,-8.22039708219152,122.733256775656));
#109981=CARTESIAN_POINT('Ctrl Pts',(6.1368128910113,-7.49846994060657,122.789202773831));
#109982=CARTESIAN_POINT('Ctrl Pts',(5.63207897067354,-6.32022659135211,
122.863416122778));
#109983=CARTESIAN_POINT('Ctrl Pts',(5.46472899018517,-5.88044523697474,
122.887659451084));
#109984=CARTESIAN_POINT('Ctrl Pts',(5.12891853630154,-4.87575600939705,
122.93507439902));
#109985=CARTESIAN_POINT('Ctrl Pts',(4.97098785085551,-4.30787607249436,
122.956387598468));
#109986=CARTESIAN_POINT('Ctrl Pts',(4.66050378214033,-2.91954573294833,
122.995029007191));
#109987=CARTESIAN_POINT('Ctrl Pts',(4.53772711179818,-2.09385284645138,
123.00695774643));
#109988=CARTESIAN_POINT('Ctrl Pts',(4.4489132903695,-0.915098142296885,
123.008781287776));
#109989=CARTESIAN_POINT('Ctrl Pts',(4.43326164955744,-0.566998360719908,
123.007469667049));
#109990=CARTESIAN_POINT('Ctrl Pts',(4.42709678199761,-0.145783148343236,
123.003712137728));
#109991=CARTESIAN_POINT('Ctrl Pts',(4.42649227748553,-0.0728888749453103,
123.002983391098));
#109992=CARTESIAN_POINT('Ctrl Pts',(4.42635006251054,-1.39861311574705E-8,
123.002176850242));
#109993=CARTESIAN_POINT('Origin',(20.412052742069,1.37771738462078E-14,
115.762503617193));
#109994=CARTESIAN_POINT('',(4.21797224931213,-7.48108295635842E-9,121.820407546638));
#109995=CARTESIAN_POINT('',(4.268747604916,3.20880881083766E-8,122.108368897758));
#109996=CARTESIAN_POINT('',(3.67032094086137,1.16952742876573E-14,118.71452263753));
#109997=CARTESIAN_POINT('Ctrl Pts',(4.26874760497861,3.20921647476068E-8,
122.108368898113));
#109998=CARTESIAN_POINT('Ctrl Pts',(4.26922578105566,-0.245077937043624,
122.11108077207));
#109999=CARTESIAN_POINT('Ctrl Pts',(4.27491609622479,-0.490145535982509,
122.112832525391));
#110000=CARTESIAN_POINT('Ctrl Pts',(4.31460988481392,-1.38148983558192,
122.115800970694));
#110001=CARTESIAN_POINT('Ctrl Pts',(4.37970572076675,-2.02582311938549,
122.111446643934));
#110002=CARTESIAN_POINT('Ctrl Pts',(4.65258566839347,-3.75010336431689,
122.082974676197));
#110003=CARTESIAN_POINT('Ctrl Pts',(4.92763931498512,-4.81606470696867,
122.04738051702));
#110004=CARTESIAN_POINT('Ctrl Pts',(5.43041779136617,-6.20151981287087,
121.97589295334));
#110005=CARTESIAN_POINT('Ctrl Pts',(5.5703177277972,-6.55083984830884,121.955550379125));
#110006=CARTESIAN_POINT('Ctrl Pts',(5.90317041322273,-7.30887149178157,
121.90619135937));
#110007=CARTESIAN_POINT('Ctrl Pts',(6.10100653230635,-7.71506902449926,
121.876314022122));
#110008=CARTESIAN_POINT('Ctrl Pts',(6.65087384397907,-8.73909267470954,
121.792330168304));
#110009=CARTESIAN_POINT('Ctrl Pts',(7.02564035484147,-9.34337611439463,
121.734271880608));
#110010=CARTESIAN_POINT('Ctrl Pts',(7.79730458877285,-10.4297829004104,
121.613652762633));
#110011=CARTESIAN_POINT('Ctrl Pts',(8.18525864543109,-10.9169706484482,
121.552603236519));
#110012=CARTESIAN_POINT('Ctrl Pts',(8.8764010067179,-11.6932848732858,121.442933199805));
#110013=CARTESIAN_POINT('Ctrl Pts',(9.16532811656547,-11.9946348163095,
121.39683388151));
#110014=CARTESIAN_POINT('Ctrl Pts',(9.76188543663381,-12.572499963897,121.301060850977));
#110015=CARTESIAN_POINT('Ctrl Pts',(10.069131949181,-12.8490141287323,121.251492205614));
#110016=CARTESIAN_POINT('Ctrl Pts',(10.9409499914763,-13.5774709358778,
121.110486537189));
#110017=CARTESIAN_POINT('Ctrl Pts',(11.5246262249861,-14.004498412734,121.015729503029));
#110018=CARTESIAN_POINT('Ctrl Pts',(12.6325232329256,-14.7100638358718,
120.835630921363));
#110019=CARTESIAN_POINT('Ctrl Pts',(13.147691806078,-15.0010010569616,120.751792961646));
#110020=CARTESIAN_POINT('Ctrl Pts',(14.0999968181132,-15.474074229105,120.596432063886));
#110021=CARTESIAN_POINT('Ctrl Pts',(14.531661680017,-15.6661218708745,120.52585381895));
#110022=CARTESIAN_POINT('Ctrl Pts',(15.3543879492404,-15.9910375019631,
120.390871062148));
#110023=CARTESIAN_POINT('Ctrl Pts',(15.7434360335537,-16.1282026394312,
120.32689518932));
#110024=CARTESIAN_POINT('Ctrl Pts',(16.8214329581016,-16.4637383442564,
120.149525212716));
#110025=CARTESIAN_POINT('Ctrl Pts',(17.5185404773362,-16.6321392771732,
120.03474102879));
#110026=CARTESIAN_POINT('Ctrl Pts',(18.8049764836848,-16.8559396958193,
119.823140172198));
#110027=CARTESIAN_POINT('Ctrl Pts',(19.390668969565,-16.9259000800183,119.726874316849));
#110028=CARTESIAN_POINT('Ctrl Pts',(20.4118125445504,-16.9928945734978,
119.558947212145));
#110029=CARTESIAN_POINT('Ctrl Pts',(20.8457800227687,-17.0042675743559,
119.487541600333));
#110030=CARTESIAN_POINT('Ctrl Pts',(21.6238500200444,-16.9940616799006,
119.35927191314));
#110031=CARTESIAN_POINT('Ctrl Pts',(21.967798567634,-16.9788123479304,119.302505055594));
#110032=CARTESIAN_POINT('Ctrl Pts',(23.1306430468139,-16.8908558569782,
119.110594309425));
#110033=CARTESIAN_POINT('Ctrl Pts',(23.9446521586234,-16.7678978870977,
118.97632734953));
#110034=CARTESIAN_POINT('Ctrl Pts',(25.314065606752,-16.4555105804068,118.751214710938));
#110035=CARTESIAN_POINT('Ctrl Pts',(25.8745803394607,-16.2962279601715,
118.659284895716));
#110036=CARTESIAN_POINT('Ctrl Pts',(26.8658954554874,-15.9573061992548,
118.496882056151));
#110037=CARTESIAN_POINT('Ctrl Pts',(27.2996362454932,-15.7883920250589,
118.425874689034));
#110038=CARTESIAN_POINT('Ctrl Pts',(28.4787023790733,-15.2713218021169,
118.232687005525));
#110039=CARTESIAN_POINT('Ctrl Pts',(29.206605539129,-14.8856848318245,118.113421928544));
#110040=CARTESIAN_POINT('Ctrl Pts',(30.5197274065888,-14.060748716363,117.899547151737));
#110041=CARTESIAN_POINT('Ctrl Pts',(31.1102978616076,-13.6338377179082,
117.803901028091));
#110042=CARTESIAN_POINT('Ctrl Pts',(32.1796635484378,-12.7497983493209,
117.631699377159));
#110043=CARTESIAN_POINT('Ctrl Pts',(32.6628294720299,-12.3002285959972,
117.55431497686));
#110044=CARTESIAN_POINT('Ctrl Pts',(33.6874534434968,-11.2283228924822,
117.390498614205));
#110045=CARTESIAN_POINT('Ctrl Pts',(34.2124853699605,-10.5921788479245,
117.306960192879));
#110046=CARTESIAN_POINT('Ctrl Pts',(35.1016834115052,-9.33977052382531,
117.167549589658));
#110047=CARTESIAN_POINT('Ctrl Pts',(35.4771486772781,-8.73400707182166,
117.109583065626));
#110048=CARTESIAN_POINT('Ctrl Pts',(36.1340523610338,-7.50959849603877,
117.010027222943));
#110049=CARTESIAN_POINT('Ctrl Pts',(36.4186544895027,-6.89419357669269,
116.967833746061));
#110050=CARTESIAN_POINT('Ctrl Pts',(36.9682105400366,-5.49355860504427,
116.887964031573));
#110051=CARTESIAN_POINT('Ctrl Pts',(37.2143795904827,-4.70261592559153,
116.853606363927));
#110052=CARTESIAN_POINT('Ctrl Pts',(37.567202504456,-3.19414006987481,116.808877021735));
#110053=CARTESIAN_POINT('Ctrl Pts',(37.6873336021067,-2.4817292229359,116.796031434694));
#110054=CARTESIAN_POINT('Ctrl Pts',(37.8311967659277,-1.10824752902771,
116.786815832772));
#110055=CARTESIAN_POINT('Ctrl Pts',(37.8622688870937,-0.44924647811183,
116.789102921073));
#110056=CARTESIAN_POINT('Ctrl Pts',(37.8520046164646,0.555001953746123,
116.802283320546));
#110057=CARTESIAN_POINT('Ctrl Pts',(37.8381133692295,0.899951732173469,
116.80857402443));
#110058=CARTESIAN_POINT('Ctrl Pts',(37.7550577179883,2.08029606342998,116.836369510181));
#110059=CARTESIAN_POINT('Ctrl Pts',(37.6354043097739,2.91069438385204,116.866788158877));
#110060=CARTESIAN_POINT('Ctrl Pts',(37.3299675200659,4.30300537692423,116.937048493882));
#110061=CARTESIAN_POINT('Ctrl Pts',(37.1746842275698,4.87030139368984,116.971323685906));
#110062=CARTESIAN_POINT('Ctrl Pts',(36.8428324157756,5.8767783994531,117.042254530924));
#110063=CARTESIAN_POINT('Ctrl Pts',(36.6765399127249,6.31884390923729,117.07708173275));
#110064=CARTESIAN_POINT('Ctrl Pts',(36.1698548571281,7.51332556017059,117.181134700329));
#110065=CARTESIAN_POINT('Ctrl Pts',(35.7931167136252,8.24834462327949,117.256616361301));
#110066=CARTESIAN_POINT('Ctrl Pts',(34.9891371451983,9.57113961632986,117.415936297328));
#110067=CARTESIAN_POINT('Ctrl Pts',(34.5743914697279,10.1645922131245,117.497477088718));
#110068=CARTESIAN_POINT('Ctrl Pts',(33.7111835169657,11.2453580826172,117.665982715174));
#110069=CARTESIAN_POINT('Ctrl Pts',(33.2693802063037,11.7364807138392,117.751719889345));
#110070=CARTESIAN_POINT('Ctrl Pts',(32.5451259901296,12.452103837052,117.891042111501));
#110071=CARTESIAN_POINT('Ctrl Pts',(32.282060619084,12.695883451979,117.941450752898));
#110072=CARTESIAN_POINT('Ctrl Pts',(31.4047118389416,13.4581411858243,118.109194059376));
#110073=CARTESIAN_POINT('Ctrl Pts',(30.7614749911917,13.9404113350938,118.231661276034));
#110074=CARTESIAN_POINT('Ctrl Pts',(29.5955081108851,14.6898098144848,118.45339165233));
#110075=CARTESIAN_POINT('Ctrl Pts',(29.0883285852308,14.9792760205531,118.549749775195));
#110076=CARTESIAN_POINT('Ctrl Pts',(28.1580964293806,15.4470237411149,118.726118052834));
#110077=CARTESIAN_POINT('Ctrl Pts',(27.7407221329023,15.635640853154,118.805112556122));
#110078=CARTESIAN_POINT('Ctrl Pts',(26.5570474418163,16.1124324319238,119.02846759665));
#110079=CARTESIAN_POINT('Ctrl Pts',(25.7767468246243,16.361193587035,119.175136230472));
#110080=CARTESIAN_POINT('Ctrl Pts',(24.2798199157637,16.7184022161233,119.45673831598));
#110081=CARTESIAN_POINT('Ctrl Pts',(23.5680137179802,16.8394956152179,119.590728982892));
#110082=CARTESIAN_POINT('Ctrl Pts',(22.2008319538071,16.9804246455505,119.848158649967));
#110083=CARTESIAN_POINT('Ctrl Pts',(21.5475966526756,17.0085771131263,119.971162418197));
#110084=CARTESIAN_POINT('Ctrl Pts',(20.0808846288693,16.9842460025931,120.246643619123));
#110085=CARTESIAN_POINT('Ctrl Pts',(19.2694064281265,16.9103191445245,120.398766621102));
#110086=CARTESIAN_POINT('Ctrl Pts',(17.7739648420178,16.6611601615662,120.679827743417));
#110087=CARTESIAN_POINT('Ctrl Pts',(17.0892911480912,16.5014931290457,120.808789070103));
#110088=CARTESIAN_POINT('Ctrl Pts',(15.7765516085603,16.1053733008256,121.056538377752));
#110089=CARTESIAN_POINT('Ctrl Pts',(15.1485226021275,15.8733867766072,121.175273743084));
#110090=CARTESIAN_POINT('Ctrl Pts',(13.8024410870976,15.2811026726017,121.429494432319));
#110091=CARTESIAN_POINT('Ctrl Pts',(13.0927751535077,14.9053001636955,121.563517158405));
#110092=CARTESIAN_POINT('Ctrl Pts',(11.8280975477732,14.1134251875143,121.803548531652));
#110093=CARTESIAN_POINT('Ctrl Pts',(11.2666051199481,13.7112976507818,121.910601620428));
#110094=CARTESIAN_POINT('Ctrl Pts',(10.1814656425597,12.8275657510704,122.118473609818));
#110095=CARTESIAN_POINT('Ctrl Pts',(9.66028068805985,12.3450280691722,122.218829316659));
#110096=CARTESIAN_POINT('Ctrl Pts',(8.6145489160732,11.2461578048294,122.420511876081));
#110097=CARTESIAN_POINT('Ctrl Pts',(8.10049093622967,10.6219759350091,122.520039818756));
#110098=CARTESIAN_POINT('Ctrl Pts',(7.2356298339529,9.40367904704014,122.689465305852));
#110099=CARTESIAN_POINT('Ctrl Pts',(6.87269184362794,8.82055580199039,122.761399387814));
#110100=CARTESIAN_POINT('Ctrl Pts',(6.19453999831229,7.56803599931309,122.897674388497));
#110101=CARTESIAN_POINT('Ctrl Pts',(5.88553989068536,6.8967812321402,122.9608959521));
#110102=CARTESIAN_POINT('Ctrl Pts',(5.47759320660585,5.83489147349971,123.045699215811));
#110103=CARTESIAN_POINT('Ctrl Pts',(5.34756315637579,5.4576450533461,123.073061755979));
#110104=CARTESIAN_POINT('Ctrl Pts',(5.01152414200896,4.35990681645709,123.145103436831));
#110105=CARTESIAN_POINT('Ctrl Pts',(4.83924298210524,3.6296981447072,123.183881045035));
#110106=CARTESIAN_POINT('Ctrl Pts',(4.61666920953987,2.30411464104747,123.238613832434));
#110107=CARTESIAN_POINT('Ctrl Pts',(4.54863964978615,1.71309618313185,123.257586231491));
#110108=CARTESIAN_POINT('Ctrl Pts',(4.48777356302406,0.746898958496295,
123.279645302893));
#110109=CARTESIAN_POINT('Ctrl Pts',(4.47639669214102,0.37349133505058,123.286005389121));
#110110=CARTESIAN_POINT('Ctrl Pts',(4.47712541821256,1.48397781563059E-8,
123.290138201919));
#110111=CARTESIAN_POINT('Ctrl Pts',(4.42635006251054,-1.39861311574705E-8,
123.002176850242));
#110112=CARTESIAN_POINT('Ctrl Pts',(4.42518823885667,0.595464723605533,
122.995587823697));
#110113=CARTESIAN_POINT('Ctrl Pts',(4.45487722577497,1.19056805989309,122.983791647929));
#110114=CARTESIAN_POINT('Ctrl Pts',(4.58800175956766,2.49647221385867,122.945715111161));
#110115=CARTESIAN_POINT('Ctrl Pts',(4.70515673536992,3.20461407594884,122.916989531995));
#110116=CARTESIAN_POINT('Ctrl Pts',(5.05108720935585,4.70682566645807,122.838191577909));
#110117=CARTESIAN_POINT('Ctrl Pts',(5.29357530148929,5.49573681876531,122.785643279264));
#110118=CARTESIAN_POINT('Ctrl Pts',(5.83642561318191,6.89417724721876,122.672604724397));
#110119=CARTESIAN_POINT('Ctrl Pts',(6.11826003702824,7.50933148956035,122.615429588997));
#110120=CARTESIAN_POINT('Ctrl Pts',(6.76961792463418,8.73362924750353,122.485072826534));
#110121=CARTESIAN_POINT('Ctrl Pts',(7.14234934471908,9.33950362308899,122.411308921857));
#110122=CARTESIAN_POINT('Ctrl Pts',(8.02891881487089,10.5967482036702,122.237110984286));
#110123=CARTESIAN_POINT('Ctrl Pts',(8.55472085039083,11.2371107144602,122.134500999833));
#110124=CARTESIAN_POINT('Ctrl Pts',(9.60990963140838,12.3450429607679,121.930669263089));
#110125=CARTESIAN_POINT('Ctrl Pts',(10.1261191608978,12.8230593294005,121.831843143575));
#110126=CARTESIAN_POINT('Ctrl Pts',(11.2074112670327,13.7049681910703,121.625487493729));
#110127=CARTESIAN_POINT('Ctrl Pts',(11.7707534210822,14.1088796990682,121.518263708808));
#110128=CARTESIAN_POINT('Ctrl Pts',(13.0372380170141,14.9025317613241,121.277479187999));
#110129=CARTESIAN_POINT('Ctrl Pts',(13.7466757175853,15.2785897683167,121.142749461357));
#110130=CARTESIAN_POINT('Ctrl Pts',(14.9025577128908,15.7876715404586,120.9241762995));
#110131=CARTESIAN_POINT('Ctrl Pts',(15.3326185914562,15.9559470883754,120.843104847876));
#110132=CARTESIAN_POINT('Ctrl Pts',(16.3184072501254,16.2947699017502,120.657503523335));
#110133=CARTESIAN_POINT('Ctrl Pts',(16.8771500368237,16.4543775322675,120.552440811145));
#110134=CARTESIAN_POINT('Ctrl Pts',(18.2365561266768,16.7660811102088,120.296695924692));
#110135=CARTESIAN_POINT('Ctrl Pts',(19.0421840745574,16.8888366537347,120.144994671488));
#110136=CARTESIAN_POINT('Ctrl Pts',(20.1985621184983,16.9780071879278,119.927280061992));
#110137=CARTESIAN_POINT('Ctrl Pts',(20.5444717051969,16.9937026550759,119.86216880481));
#110138=CARTESIAN_POINT('Ctrl Pts',(21.5583159176972,17.0076175455186,119.671532332386));
#110139=CARTESIAN_POINT('Ctrl Pts',(22.226005753672,16.9760474101932,119.546321070406));
#110140=CARTESIAN_POINT('Ctrl Pts',(23.5866935336157,16.8282317911089,119.290910042905));
#110141=CARTESIAN_POINT('Ctrl Pts',(24.2779701576123,16.7080446167473,119.161001259895));
#110142=CARTESIAN_POINT('Ctrl Pts',(25.7471798827798,16.354662299431,118.88422038468));
#110143=CARTESIAN_POINT('Ctrl Pts',(26.5199871827589,16.107304431488,118.738192946537));
#110144=CARTESIAN_POINT('Ctrl Pts',(27.8915679713764,15.5541093609196,118.479060318859));
#110145=CARTESIAN_POINT('Ctrl Pts',(28.4957815409686,15.2667869647624,118.365044885245));
#110146=CARTESIAN_POINT('Ctrl Pts',(29.6986816465838,14.6028370891587,118.137438674895));
#110147=CARTESIAN_POINT('Ctrl Pts',(30.2941171099273,14.2228940492812,118.024404403553));
#110148=CARTESIAN_POINT('Ctrl Pts',(31.5248025858741,13.3227936279907,117.789593515893));
#110149=CARTESIAN_POINT('Ctrl Pts',(32.1497105993425,12.7911564093607,117.669578676146));
#110150=CARTESIAN_POINT('Ctrl Pts',(33.2017300678859,11.7543133945301,117.466902307042));
#110151=CARTESIAN_POINT('Ctrl Pts',(33.642545181654,11.2658923909258,117.381860926172));
#110152=CARTESIAN_POINT('Ctrl Pts',(34.5105334763716,10.1832532918875,117.213274495814));
#110153=CARTESIAN_POINT('Ctrl Pts',(34.930075761167,9.58445085798915,117.131046945627));
#110154=CARTESIAN_POINT('Ctrl Pts',(35.7382201691088,8.2562273634107,116.970531287632));
#110155=CARTESIAN_POINT('Ctrl Pts',(36.115098400205,7.52164509304977,116.894262589128));
#110156=CARTESIAN_POINT('Ctrl Pts',(36.7090499882621,6.12346260200393,116.77197805045));
#110157=CARTESIAN_POINT('Ctrl Pts',(36.9414830724226,5.46854639923365,116.723325208009));
#110158=CARTESIAN_POINT('Ctrl Pts',(37.3290081942046,4.12266167533976,116.639371904947));
#110159=CARTESIAN_POINT('Ctrl Pts',(37.4824241879757,3.43260171775824,116.604356477421));
#110160=CARTESIAN_POINT('Ctrl Pts',(37.7227204437875,1.91667604733677,116.54425048954));
#110161=CARTESIAN_POINT('Ctrl Pts',(37.7932539849284,1.0899329692338,116.521975019881));
#110162=CARTESIAN_POINT('Ctrl Pts',(37.8135153901447,-0.449614347336989,
116.500670877354));
#110163=CARTESIAN_POINT('Ctrl Pts',(37.7790188154657,-1.16036323419767,
116.498936940417));
#110164=CARTESIAN_POINT('Ctrl Pts',(37.623719464608,-2.56296318541711,116.510617543849));
#110165=CARTESIAN_POINT('Ctrl Pts',(37.5043513905107,-3.25359763791229,
116.523778424962));
#110166=CARTESIAN_POINT('Ctrl Pts',(37.1564999871574,-4.72543705329675,
116.567654538254));
#110167=CARTESIAN_POINT('Ctrl Pts',(36.9140292009834,-5.50149868860622,
116.600777237718));
#110168=CARTESIAN_POINT('Ctrl Pts',(36.4460644223716,-6.69541860127829,
116.668504892631));
#110169=CARTESIAN_POINT('Ctrl Pts',(36.2564019608999,-7.1263439271623,116.696677210133));
#110170=CARTESIAN_POINT('Ctrl Pts',(35.7905552454678,-8.07670967684446,
116.767017281745));
#110171=CARTESIAN_POINT('Ctrl Pts',(35.504904359474,-8.5907143095185,116.810852414028));
#110172=CARTESIAN_POINT('Ctrl Pts',(34.7524148658142,-9.79410140326056,
116.927420623407));
#110173=CARTESIAN_POINT('Ctrl Pts',(34.2606879220935,-10.4656966310228,
117.004392176695));
#110174=CARTESIAN_POINT('Ctrl Pts',(33.4981693682653,-11.3613513360252,
117.125004150784));
#110175=CARTESIAN_POINT('Ctrl Pts',(33.2660724455843,-11.6176682910296,
117.161866203193));
#110176=CARTESIAN_POINT('Ctrl Pts',(32.7177335663459,-12.1872171454491,
117.249406404016));
#110177=CARTESIAN_POINT('Ctrl Pts',(32.3967281981065,-12.4953602506554,
117.301005833612));
#110178=CARTESIAN_POINT('Ctrl Pts',(31.6227921700325,-13.1816730404354,
117.425887298958));
#110179=CARTESIAN_POINT('Ctrl Pts',(31.1615657934469,-13.549335617007,117.500637689857));
#110180=CARTESIAN_POINT('Ctrl Pts',(30.0691559510562,-14.3299050013909,
117.677955381894));
#110181=CARTESIAN_POINT('Ctrl Pts',(29.4277185931807,-14.7258749417959,
117.782241291571));
#110182=CARTESIAN_POINT('Ctrl Pts',(28.4178969084008,-15.2588015226943,
117.946806360488));
#110183=CARTESIAN_POINT('Ctrl Pts',(28.0673504512446,-15.4284053136147,
118.004008162687));
#110184=CARTESIAN_POINT('Ctrl Pts',(27.0546732857834,-15.8753556275927,
118.169666944165));
#110185=CARTESIAN_POINT('Ctrl Pts',(26.3804775649806,-16.1222727430435,
118.280557649367));
#110186=CARTESIAN_POINT('Ctrl Pts',(25.0337183560893,-16.5188477748547,
118.502194647031));
#110187=CARTESIAN_POINT('Ctrl Pts',(24.3635262076723,-16.671750021719,118.61252396392));
#110188=CARTESIAN_POINT('Ctrl Pts',(22.8946307203057,-16.9121059059674,
118.854111373357));
#110189=CARTESIAN_POINT('Ctrl Pts',(22.0951339373954,-16.9839494300226,
118.985447737349));
#110190=CARTESIAN_POINT('Ctrl Pts',(20.5695232625194,-17.0099335780774,
119.236633819618));
#110191=CARTESIAN_POINT('Ctrl Pts',(19.8454000325533,-16.9747275626374,
119.35625195382));
#110192=CARTESIAN_POINT('Ctrl Pts',(18.4472366962676,-16.8143918726589,
119.58691123482));
#110193=CARTESIAN_POINT('Ctrl Pts',(17.774006315727,-16.6946639187595,119.697818708374));
#110194=CARTESIAN_POINT('Ctrl Pts',(16.3288919004593,-16.3444236125222,
119.935249124945));
#110195=CARTESIAN_POINT('Ctrl Pts',(15.5623250163285,-16.0985937302408,
120.060769943235));
#110196=CARTESIAN_POINT('Ctrl Pts',(14.4103913286245,-15.6347218299559,
120.249433175712));
#110197=CARTESIAN_POINT('Ctrl Pts',(14.0111484769824,-15.4553678980557,
120.314879599975));
#110198=CARTESIAN_POINT('Ctrl Pts',(12.9309599351056,-14.9180868301962,
120.491774242061));
#110199=CARTESIAN_POINT('Ctrl Pts',(12.2665926131983,-14.5283273120543,
120.600309544538));
#110200=CARTESIAN_POINT('Ctrl Pts',(11.1709308024953,-13.7797306432325,
120.778200256408));
#110201=CARTESIAN_POINT('Ctrl Pts',(10.7267032987619,-13.4426600147459,
120.849987117073));
#110202=CARTESIAN_POINT('Ctrl Pts',(9.83461053574349,-12.6931677986486,
120.993545212399));
#110203=CARTESIAN_POINT('Ctrl Pts',(9.39061182533935,-12.2772483278458,
121.064650320127));
#110204=CARTESIAN_POINT('Ctrl Pts',(8.41027111392335,-11.2541508344559,
121.221396334212));
#110205=CARTESIAN_POINT('Ctrl Pts',(7.89287333866819,-10.6304032098477,
121.30374416078));
#110206=CARTESIAN_POINT('Ctrl Pts',(7.02372265835108,-9.41584385666745,
121.440119166576));
#110207=CARTESIAN_POINT('Ctrl Pts',(6.65952050852146,-8.83628073833126,
121.49644641522));
#110208=CARTESIAN_POINT('Ctrl Pts',(5.97069636036473,-7.57855377714445,
121.60112800413));
#110209=CARTESIAN_POINT('Ctrl Pts',(5.65392176226136,-6.89763556146838,
121.648117648005));
#110210=CARTESIAN_POINT('Ctrl Pts',(5.23660743187802,-5.82109881654923,
121.708659428415));
#110211=CARTESIAN_POINT('Ctrl Pts',(5.10389172906911,-5.43928253380061,
121.727575231636));
#110212=CARTESIAN_POINT('Ctrl Pts',(4.76567825046675,-4.34321696884615,
121.774446822623));
#110213=CARTESIAN_POINT('Ctrl Pts',(4.59272480727977,-3.61965369280211,
121.796617516938));
#110214=CARTESIAN_POINT('Ctrl Pts',(4.36618777270672,-2.30033662389662,
121.821147845938));
#110215=CARTESIAN_POINT('Ctrl Pts',(4.29584625684108,-1.70874879397981,
121.826567012219));
#110216=CARTESIAN_POINT('Ctrl Pts',(4.23145416377887,-0.743617261714217,
121.826607423141));
#110217=CARTESIAN_POINT('Ctrl Pts',(4.21869777333078,-0.371849869633078,
121.824522195929));
#110218=CARTESIAN_POINT('Ctrl Pts',(4.21797224931213,-1.49621590811444E-8,
121.820407546637));
#110219=CARTESIAN_POINT('Origin',(20.412052742069,1.37771738462078E-14,
115.762503617193));
#110220=CARTESIAN_POINT('',(4.00959443613148,-1.25155352558489E-8,120.638638243134));
#110221=CARTESIAN_POINT('',(4.06036979181168,7.51633154241203E-9,120.926599594688));
#110222=CARTESIAN_POINT('',(3.67032094086137,1.16952742876573E-14,118.71452263753));
#110223=CARTESIAN_POINT('Ctrl Pts',(4.06036979181167,1.50326513895498E-8,
120.926599594688));
#110224=CARTESIAN_POINT('Ctrl Pts',(4.06109544462189,-0.371916179869893,
120.930714978172));
#110225=CARTESIAN_POINT('Ctrl Pts',(4.07382447319043,-0.743751311529452,
120.93261993144));
#110226=CARTESIAN_POINT('Ctrl Pts',(4.13813558699207,-1.70892963326076,
120.932035879093));
#110227=CARTESIAN_POINT('Ctrl Pts',(4.20841260663817,-2.30049309592992,
120.926232593849));
#110228=CARTESIAN_POINT('Ctrl Pts',(4.43495233645074,-3.62005035895633,
120.901417407863));
#110229=CARTESIAN_POINT('Ctrl Pts',(4.60804054799553,-4.34386905761117,
120.879516002255));
#110230=CARTESIAN_POINT('Ctrl Pts',(4.94644995248541,-5.43999188903374,
120.833272837139));
#110231=CARTESIAN_POINT('Ctrl Pts',(5.07916398511592,-5.82163057348125,
120.814611024077));
#110232=CARTESIAN_POINT('Ctrl Pts',(5.49633802576137,-6.89760324021201,
120.754383332977));
#110233=CARTESIAN_POINT('Ctrl Pts',(5.8128239647134,-7.57814692831025,120.706838878165));
#110234=CARTESIAN_POINT('Ctrl Pts',(6.5013318175681,-8.83567939597569,120.601457736364));
#110235=CARTESIAN_POINT('Ctrl Pts',(6.86556315951656,-9.41537576858684,
120.544981836645));
#110236=CARTESIAN_POINT('Ctrl Pts',(7.73468917633917,-10.6298566517034,
120.409061807226));
#110237=CARTESIAN_POINT('Ctrl Pts',(8.25202139551287,-11.2534276399576,
120.327492256401));
#110238=CARTESIAN_POINT('Ctrl Pts',(9.29791710675212,-12.3450378068388,
120.160585238406));
#110239=CARTESIAN_POINT('Ctrl Pts',(9.8152613163429,-12.821693631004,120.07714587458));
#110240=CARTESIAN_POINT('Ctrl Pts',(10.9007270404882,-13.7030613063849,
119.901428864123));
#110241=CARTESIAN_POINT('Ctrl Pts',(11.467329392624,-14.1075182097664,119.809421046338));
#110242=CARTESIAN_POINT('Ctrl Pts',(12.7403827366668,-14.9017191458757,
119.60242520546));
#110243=CARTESIAN_POINT('Ctrl Pts',(13.4531005949596,-15.2778589958563,
119.486390672741));
#110244=CARTESIAN_POINT('Ctrl Pts',(14.6051338146059,-15.7831725684149,
119.297904325861));
#110245=CARTESIAN_POINT('Ctrl Pts',(15.0277996072462,-15.9483399326344,
119.228511323325));
#110246=CARTESIAN_POINT('Ctrl Pts',(16.0109712043684,-16.2869127197307,
119.066862362756));
#110247=CARTESIAN_POINT('Ctrl Pts',(16.5748809865819,-16.4482975056573,
118.974004987576));
#110248=CARTESIAN_POINT('Ctrl Pts',(17.8933528720093,-16.7511354713472,
118.757020040198));
#110249=CARTESIAN_POINT('Ctrl Pts',(18.6514828656597,-16.8706999705766,
118.632365084318));
#110250=CARTESIAN_POINT('Ctrl Pts',(19.7924944048013,-16.9702626993189,
118.444762699985));
#110251=CARTESIAN_POINT('Ctrl Pts',(20.1709676059958,-16.990232882454,118.382526683596));
#110252=CARTESIAN_POINT('Ctrl Pts',(21.2215668936329,-17.009557256875,118.209558102306));
#110253=CARTESIAN_POINT('Ctrl Pts',(21.8934232023662,-16.9810008623432,
118.098603337571));
#110254=CARTESIAN_POINT('Ctrl Pts',(23.2778320456319,-16.8374273796617,
117.870173739578));
#110255=CARTESIAN_POINT('Ctrl Pts',(23.9884331540669,-16.7165387172295,
117.753068684323));
#110256=CARTESIAN_POINT('Ctrl Pts',(25.4858427290076,-16.3601965710916,
117.507006115782));
#110257=CARTESIAN_POINT('Ctrl Pts',(26.2677773528003,-16.1118164769959,
117.378960611836));
#110258=CARTESIAN_POINT('Ctrl Pts',(27.461378990354,-15.6330692554134,117.183475500784));
#110259=CARTESIAN_POINT('Ctrl Pts',(27.8867428746152,-15.4413547639464,
117.113743690127));
#110260=CARTESIAN_POINT('Ctrl Pts',(28.824741496229,-14.9703264372935,116.960151234113));
#110261=CARTESIAN_POINT('Ctrl Pts',(29.3320277909594,-14.6814098934801,
116.877235529233));
#110262=CARTESIAN_POINT('Ctrl Pts',(30.5200234922694,-13.9200066850356,
116.683877814602));
#110263=CARTESIAN_POINT('Ctrl Pts',(31.1832239089646,-13.4222474326742,
116.576673304186));
#110264=CARTESIAN_POINT('Ctrl Pts',(32.0676524444043,-12.6502865281376,
116.434566029903));
#110265=CARTESIAN_POINT('Ctrl Pts',(32.320665559984,-12.4153959824999,116.394014288617));
#110266=CARTESIAN_POINT('Ctrl Pts',(32.883316441135,-11.8599741383261,116.303953678213));
#110267=CARTESIAN_POINT('Ctrl Pts',(33.1878999803028,-11.5345626300269,
116.255254336194));
#110268=CARTESIAN_POINT('Ctrl Pts',(33.8658480358207,-10.7504542905743,
116.147300651274));
#110269=CARTESIAN_POINT('Ctrl Pts',(34.2289019142407,-10.2833682469229,
116.089858873882));
#110270=CARTESIAN_POINT('Ctrl Pts',(35.0017255995861,-9.17446803628632,
115.968924223625));
#110271=CARTESIAN_POINT('Ctrl Pts',(35.3944932714994,-8.5220283295332,115.90852091134));
#110272=CARTESIAN_POINT('Ctrl Pts',(35.9215227012237,-7.49773719808307,
115.829097564491));
#110273=CARTESIAN_POINT('Ctrl Pts',(36.0883888348419,-7.14421732426023,
115.804260958309));
#110274=CARTESIAN_POINT('Ctrl Pts',(36.5078750567658,-6.17057397482726,
115.742535773449));
#110275=CARTESIAN_POINT('Ctrl Pts',(36.7365888964586,-5.54067853283166,
115.709610892267));
#110276=CARTESIAN_POINT('Ctrl Pts',(37.1364677050348,-4.20035394824862,
115.654676203586));
#110277=CARTESIAN_POINT('Ctrl Pts',(37.3003759135926,-3.48911486135417,
115.633973745358));
#110278=CARTESIAN_POINT('Ctrl Pts',(37.5549425128948,-1.94261459356428,
115.607174294891));
#110279=CARTESIAN_POINT('Ctrl Pts',(37.6306993636554,-1.10678654481858,
115.603764661473));
#110280=CARTESIAN_POINT('Ctrl Pts',(37.6580008868524,0.449255408351833,
115.616876542939));
#110281=CARTESIAN_POINT('Ctrl Pts',(37.6257113101545,1.16734086829877,115.630465228205));
#110282=CARTESIAN_POINT('Ctrl Pts',(37.474126663482,2.57441242725769,115.672949977547));
#110283=CARTESIAN_POINT('Ctrl Pts',(37.357498913966,3.2623082269617,115.701373413403));
#110284=CARTESIAN_POINT('Ctrl Pts',(37.0155854992617,4.73189528757101,115.779098184567));
#110285=CARTESIAN_POINT('Ctrl Pts',(36.775943788676,5.50834935822597,115.83099179919));
#110286=CARTESIAN_POINT('Ctrl Pts',(36.237928244285,6.89413317065628,115.943021002455));
#110287=CARTESIAN_POINT('Ctrl Pts',(35.9564756108636,7.50849876363283,116.000119389192));
#110288=CARTESIAN_POINT('Ctrl Pts',(35.3054756825945,8.73243132318426,116.130407331724));
#110289=CARTESIAN_POINT('Ctrl Pts',(34.932587025956,9.33865756381279,116.204202977392));
#110290=CARTESIAN_POINT('Ctrl Pts',(34.0490423119042,10.5917125048151,116.377807323092));
#110291=CARTESIAN_POINT('Ctrl Pts',(33.5271020059831,11.2280571996377,116.479667474439));
#110292=CARTESIAN_POINT('Ctrl Pts',(32.5096589584696,12.2985478687273,116.676235186642));
#110293=CARTESIAN_POINT('Ctrl Pts',(32.0307840403966,12.7467082442256,116.767975473656));
#110294=CARTESIAN_POINT('Ctrl Pts',(30.9676561601478,13.6308165559435,116.970966648253));
#110295=CARTESIAN_POINT('Ctrl Pts',(30.37874014994,14.0588335895466,117.083068264223));
#110296=CARTESIAN_POINT('Ctrl Pts',(29.0703325658575,14.8848513335703,117.331841683419));
#110297=CARTESIAN_POINT('Ctrl Pts',(28.3455828782913,15.270625341966,117.469490503562));
#110298=CARTESIAN_POINT('Ctrl Pts',(27.1820993001986,15.7831897086887,117.689502444031));
#110299=CARTESIAN_POINT('Ctrl Pts',(26.7611566381927,15.9483682206002,117.768860753313));
#110300=CARTESIAN_POINT('Ctrl Pts',(25.7819669730114,16.2869416279052,117.953229272502));
#110301=CARTESIAN_POINT('Ctrl Pts',(25.220316996997,16.4483197999396,118.058838323665));
#110302=CARTESIAN_POINT('Ctrl Pts',(23.9069281257681,16.7512015630847,118.30592400931));
#110303=CARTESIAN_POINT('Ctrl Pts',(23.1516496604424,16.8707831999228,118.448126679876));
#110304=CARTESIAN_POINT('Ctrl Pts',(22.0151939335348,16.9702998825412,118.662104273353));
#110305=CARTESIAN_POINT('Ctrl Pts',(21.6384049546807,16.9902495533383,118.733039571959));
#110306=CARTESIAN_POINT('Ctrl Pts',(20.5928773358012,17.0095363499679,118.929664362102));
#110307=CARTESIAN_POINT('Ctrl Pts',(19.9243161809923,16.9810415369076,119.055053500864));
#110308=CARTESIAN_POINT('Ctrl Pts',(18.545547260635,16.8376528902263,119.313843191662));
#110309=CARTESIAN_POINT('Ctrl Pts',(17.8373130342597,16.7167427401791,119.44692171617));
#110310=CARTESIAN_POINT('Ctrl Pts',(16.3453737444248,16.360291317995,119.727969834639));
#110311=CARTESIAN_POINT('Ctrl Pts',(15.5665580978345,16.1118423960987,119.875129810112));
#110312=CARTESIAN_POINT('Ctrl Pts',(14.37867728749,15.6333185454838,120.09955675401));
#110313=CARTESIAN_POINT('Ctrl Pts',(13.9559160325654,15.4420006776234,120.179362472352));
#110314=CARTESIAN_POINT('Ctrl Pts',(13.0224523267959,14.9713976198448,120.355752339874));
#110315=CARTESIAN_POINT('Ctrl Pts',(12.5171416344494,14.6824170858708,120.451387438507));
#110316=CARTESIAN_POINT('Ctrl Pts',(11.3360163783748,13.9220584206545,120.675749590544));
#110317=CARTESIAN_POINT('Ctrl Pts',(10.6775849076177,13.4256718427779,120.801559896098));
#110318=CARTESIAN_POINT('Ctrl Pts',(9.79803698539848,12.6545442361247,120.970481932679));
#110319=CARTESIAN_POINT('Ctrl Pts',(9.54537267352967,12.4188408271241,121.019110755335));
#110320=CARTESIAN_POINT('Ctrl Pts',(8.99077749930881,11.8685479042255,121.125969378757));
#110321=CARTESIAN_POINT('Ctrl Pts',(8.69335281993779,11.5496063558978,121.183328850132));
#110322=CARTESIAN_POINT('Ctrl Pts',(8.02140865543179,10.7705783759609,121.313342361084));
#110323=CARTESIAN_POINT('Ctrl Pts',(7.65793145009093,10.3014135595615,121.384041356307));
#110324=CARTESIAN_POINT('Ctrl Pts',(6.90864144572742,9.22154136682129,121.531101377255));
#110325=CARTESIAN_POINT('Ctrl Pts',(6.53551147681524,8.60315882163496,121.605289843067));
#110326=CARTESIAN_POINT('Ctrl Pts',(6.0107063838496,7.5935333625272,121.711189517807));
#110327=CARTESIAN_POINT('Ctrl Pts',(5.83242531068412,7.21760455240921,121.747521818373));
#110328=CARTESIAN_POINT('Ctrl Pts',(5.47996472507408,6.39852644682126,121.819998722905));
#110329=CARTESIAN_POINT('Ctrl Pts',(5.31015689405443,5.9538132267194,121.855290924592));
#110330=CARTESIAN_POINT('Ctrl Pts',(4.96974432108495,4.93727940226185,121.927274640659));
#110331=CARTESIAN_POINT('Ctrl Pts',(4.80995622911867,4.36236813765725,121.962064049053));
#110332=CARTESIAN_POINT('Ctrl Pts',(4.54038106457611,3.1514337907947,122.023640752274));
#110333=CARTESIAN_POINT('Ctrl Pts',(4.43579978837447,2.5151696095759,122.049525683068));
#110334=CARTESIAN_POINT('Ctrl Pts',(4.31712855678972,1.40853117727905,122.083462606372));
#110335=CARTESIAN_POINT('Ctrl Pts',(4.2861748988376,0.940781164514785,122.094433492682));
#110336=CARTESIAN_POINT('Ctrl Pts',(4.27028424358903,0.314887353539518,
122.104488267717));
#110337=CARTESIAN_POINT('Ctrl Pts',(4.26844041796647,0.157441553515873,
122.106626752285));
#110338=CARTESIAN_POINT('Ctrl Pts',(4.26874760497861,3.2092153691432E-8,
122.108368898113));
#110339=CARTESIAN_POINT('Ctrl Pts',(4.21797224931213,-1.49621579481794E-8,
121.820407546637));
#110340=CARTESIAN_POINT('Ctrl Pts',(4.21783007352557,0.0728687587915521,
121.819601228053));
#110341=CARTESIAN_POINT('Ctrl Pts',(4.21814991592475,0.145740700221469,
121.818717063283));
#110342=CARTESIAN_POINT('Ctrl Pts',(4.22266880094517,0.566906322356731,
121.813153004183));
#110343=CARTESIAN_POINT('Ctrl Pts',(4.23695833476989,0.914981990905322,
121.80675828228));
#110344=CARTESIAN_POINT('Ctrl Pts',(4.32115168954176,2.09375351741002,121.778779644602));
#110345=CARTESIAN_POINT('Ctrl Pts',(4.44068155455545,2.91947981692603,121.748430600617));
#110346=CARTESIAN_POINT('Ctrl Pts',(4.74561713539064,4.30783822857224,121.678302906396));
#110347=CARTESIAN_POINT('Ctrl Pts',(4.90124747141045,4.87571418267818,121.643958258756));
#110348=CARTESIAN_POINT('Ctrl Pts',(5.23292063371056,5.88041316543007,121.573079734022));
#110349=CARTESIAN_POINT('Ctrl Pts',(5.39843933003303,6.3202117767867,121.538417493381));
#110350=CARTESIAN_POINT('Ctrl Pts',(5.90493826090496,7.51442804791732,121.434400542965));
#110351=CARTESIAN_POINT('Ctrl Pts',(6.28271877495383,8.25124570795247,121.358712944208));
#110352=CARTESIAN_POINT('Ctrl Pts',(7.0903687141081,9.57914747154308,121.198672867327));
#110353=CARTESIAN_POINT('Ctrl Pts',(7.50793467658244,10.1757668092679,121.116583161096));
#110354=CARTESIAN_POINT('Ctrl Pts',(8.3754602350813,11.2595861350958,120.947254350687));
#110355=CARTESIAN_POINT('Ctrl Pts',(8.81842145140748,11.7508678075734,120.861306141922));
#110356=CARTESIAN_POINT('Ctrl Pts',(9.87127348920574,12.7886305633914,120.658803828637));
#110357=CARTESIAN_POINT('Ctrl Pts',(10.4943313434594,13.3188908012687,120.539927611143));
#110358=CARTESIAN_POINT('Ctrl Pts',(11.7188431948899,14.215372447492,120.306714107406));
#110359=CARTESIAN_POINT('Ctrl Pts',(12.3098477369955,14.5932889240075,120.194321988777));
#110360=CARTESIAN_POINT('Ctrl Pts',(13.517375790144,15.262027798887,119.965058414874));
#110361=CARTESIAN_POINT('Ctrl Pts',(14.1315804472529,15.5544121254239,119.848638715276));
#110362=CARTESIAN_POINT('Ctrl Pts',(15.516280524145,16.1118115997861,119.587354466938));
#110363=CARTESIAN_POINT('Ctrl Pts',(16.2917849850941,16.3592337341959,119.4415850402));
#110364=CARTESIAN_POINT('Ctrl Pts',(17.7752309220187,16.7142811876715,119.16251995002));
#110365=CARTESIAN_POINT('Ctrl Pts',(18.4783003209709,16.8349470402301,119.030177290372));
#110366=CARTESIAN_POINT('Ctrl Pts',(19.8249977354605,16.976833183057,118.776604568924));
#110367=CARTESIAN_POINT('Ctrl Pts',(20.4664967481208,17.0066111080161,118.655800410499));
#110368=CARTESIAN_POINT('Ctrl Pts',(21.4453715317864,16.9946575107851,118.471919832153));
#110369=CARTESIAN_POINT('Ctrl Pts',(21.782415201859,16.9801521685154,118.408670719453));
#110370=CARTESIAN_POINT('Ctrl Pts',(22.93891554042,16.894638106131,118.191639474227));
#110371=CARTESIAN_POINT('Ctrl Pts',(23.7535040221942,16.7724884813998,118.038707528667));
#110372=CARTESIAN_POINT('Ctrl Pts',(25.1180935327818,16.4618282631648,117.781744274011));
#110373=CARTESIAN_POINT('Ctrl Pts',(25.6734094801816,16.3043253562443,117.676964302909));
#110374=CARTESIAN_POINT('Ctrl Pts',(26.6676959571963,15.9650441009021,117.489167290262));
#110375=CARTESIAN_POINT('Ctrl Pts',(27.1092092516129,15.7928567789812,117.405719931934));
#110376=CARTESIAN_POINT('Ctrl Pts',(28.27614666206,15.2789934710198,117.185332752019));
#110377=CARTESIAN_POINT('Ctrl Pts',(28.9856268843385,14.9030339797141,117.051343368819));
#110378=CARTESIAN_POINT('Ctrl Pts',(30.2516948583679,14.1098087462447,116.811043835562));
#110379=CARTESIAN_POINT('Ctrl Pts',(30.8146274662093,13.7062664407844,116.703712047057));
#110380=CARTESIAN_POINT('Ctrl Pts',(31.896593767231,12.8239901004098,116.496438226064));
#110381=CARTESIAN_POINT('Ctrl Pts',(32.4137474342056,12.3450458660301,116.396858793694));
#110382=CARTESIAN_POINT('Ctrl Pts',(33.1490703295368,11.5728759390271,116.255044514662));
#110383=CARTESIAN_POINT('Ctrl Pts',(33.3899025178613,11.3031259146185,116.208530158652));
#110384=CARTESIAN_POINT('Ctrl Pts',(34.1366969902277,10.4105223481146,116.063824153262));
#110385=CARTESIAN_POINT('Ctrl Pts',(34.6075179955994,9.75874629390605,115.971799749524));
#110386=CARTESIAN_POINT('Ctrl Pts',(35.3407421564116,8.57500772105226,115.826415111035));
#110387=CARTESIAN_POINT('Ctrl Pts',(35.6246907724818,8.05853561231405,115.76941529427));
#110388=CARTESIAN_POINT('Ctrl Pts',(36.0828661064104,7.11219814942125,115.676289499588));
#110389=CARTESIAN_POINT('Ctrl Pts',(36.2673549594015,6.68813953265294,115.638368245058));
#110390=CARTESIAN_POINT('Ctrl Pts',(36.7318591556047,5.49018382018588,115.541901750737));
#110391=CARTESIAN_POINT('Ctrl Pts',(36.9738736735577,4.70238708866722,115.490214278083));
#110392=CARTESIAN_POINT('Ctrl Pts',(37.3197824840578,3.19922061230053,115.411800154912));
#110393=CARTESIAN_POINT('Ctrl Pts',(37.43698064961,2.48890638024839,115.382823561136));
#110394=CARTESIAN_POINT('Ctrl Pts',(37.5763106157877,1.11305312917326,115.342076736139));
#110395=CARTESIAN_POINT('Ctrl Pts',(37.6050197380707,0.449510452110751,
115.329194011537));
#110396=CARTESIAN_POINT('Ctrl Pts',(37.5905312631139,-0.560796264490243,
115.320311188467));
#110397=CARTESIAN_POINT('Ctrl Pts',(37.5751276169684,-0.907262466138281,
115.31916957441));
#110398=CARTESIAN_POINT('Ctrl Pts',(37.4870220068825,-2.08686360062308,
115.321562699139));
#110399=CARTESIAN_POINT('Ctrl Pts',(37.3642426354005,-2.91501470291571,
115.333914454204));
#110400=CARTESIAN_POINT('Ctrl Pts',(37.0534327155429,-4.30543659385099,
115.372336136456));
#110401=CARTESIAN_POINT('Ctrl Pts',(36.8956156583974,-4.87302346203984,
115.393264838432));
#110402=CARTESIAN_POINT('Ctrl Pts',(36.55962228171,-5.8785710340372,115.440104022816));
#110403=CARTESIAN_POINT('Ctrl Pts',(36.3918551493605,-6.3194630569091,115.464195304428));
#110404=CARTESIAN_POINT('Ctrl Pts',(35.8812923243715,-7.51135910002527,
115.539542383863));
#110405=CARTESIAN_POINT('Ctrl Pts',(35.5023164122996,-8.24502594434764,
115.597330608199));
#110406=CARTESIAN_POINT('Ctrl Pts',(34.6956101408257,-9.56338991659232,
115.722081992826));
#110407=CARTESIAN_POINT('Ctrl Pts',(34.280625505383,-10.1539171429642,115.786892888107));
#110408=CARTESIAN_POINT('Ctrl Pts',(33.4221029348028,-11.224110773041,115.92214910304));
#110409=CARTESIAN_POINT('Ctrl Pts',(32.9858025621622,-11.7080892166949,
115.991368216351));
#110410=CARTESIAN_POINT('Ctrl Pts',(32.2802501152059,-12.4054779115737,
116.104471010753));
#110411=CARTESIAN_POINT('Ctrl Pts',(32.0302456959124,-12.6380528025974,
116.144727981398));
#110412=CARTESIAN_POINT('Ctrl Pts',(31.1480639693456,-13.4101715841841,
116.287158460895));
#110413=CARTESIAN_POINT('Ctrl Pts',(30.4836903100857,-13.9100111801613,
116.39499994806));
#110414=CARTESIAN_POINT('Ctrl Pts',(29.2963274999843,-14.6724924285829,
116.587997707063));
#110415=CARTESIAN_POINT('Ctrl Pts',(28.7912288149617,-14.9608651822966,
116.670187978247));
#110416=CARTESIAN_POINT('Ctrl Pts',(27.8493300721744,-15.4353386551804,
116.8238100423));
#110417=CARTESIAN_POINT('Ctrl Pts',(27.4175263038477,-15.6302829320919,
116.894378486576));
#110418=CARTESIAN_POINT('Ctrl Pts',(26.2174918118913,-16.1116555507339,
117.091195595799));
#110419=CARTESIAN_POINT('Ctrl Pts',(25.4358484636341,-16.3600132846689,
117.219959307463));
#110420=CARTESIAN_POINT('Ctrl Pts',(23.9392718611159,-16.7162478435817,
117.466268183718));
#110421=CARTESIAN_POINT('Ctrl Pts',(23.2292505514606,-16.8371059063296,
117.583041448304));
#110422=CARTESIAN_POINT('Ctrl Pts',(21.8443102255085,-16.9809423852526,
117.810740120362));
#110423=CARTESIAN_POINT('Ctrl Pts',(21.171323745976,-17.0095872170374,117.921381200104));
#110424=CARTESIAN_POINT('Ctrl Pts',(20.1195190096776,-16.9902089287595,
118.094810677757));
#110425=CARTESIAN_POINT('Ctrl Pts',(19.7408769089898,-16.9702093049175,
118.157314067149));
#110426=CARTESIAN_POINT('Ctrl Pts',(18.6001131992247,-16.8705800755323,
118.345572825384));
#110427=CARTESIAN_POINT('Ctrl Pts',(17.8423841689354,-16.7510401190566,
118.470513173372));
#110428=CARTESIAN_POINT('Ctrl Pts',(16.5241842295137,-16.4482659024811,
118.687194231464));
#110429=CARTESIAN_POINT('Ctrl Pts',(15.9601934378477,-16.2868714560458,
118.779687049748));
#110430=CARTESIAN_POINT('Ctrl Pts',(14.976957725779,-15.9483006906574,118.940759997379));
#110431=CARTESIAN_POINT('Ctrl Pts',(14.5543047309711,-15.7831491857126,
119.009953977652));
#110432=CARTESIAN_POINT('Ctrl Pts',(13.3846165242419,-15.2700698900897,
119.201605219728));
#110433=CARTESIAN_POINT('Ctrl Pts',(12.6554664143251,-14.8835653687048,
119.321073815261));
#110434=CARTESIAN_POINT('Ctrl Pts',(11.3367736332283,-14.0544760261983,
119.535850083452));
#110435=CARTESIAN_POINT('Ctrl Pts',(10.7421480016747,-13.6238745881955,
119.632144648683));
#110436=CARTESIAN_POINT('Ctrl Pts',(9.67542669824277,-12.7396495519746,
119.803901001889));
#110437=CARTESIAN_POINT('Ctrl Pts',(9.19796648560238,-12.2947976368726,
119.880369953539));
#110438=CARTESIAN_POINT('Ctrl Pts',(8.17827012923428,-11.2280299160028,
120.043398424638));
#110439=CARTESIAN_POINT('Ctrl Pts',(7.65308893296738,-10.5916644716746,
120.126960316678));
#110440=CARTESIAN_POINT('Ctrl Pts',(6.76348485086405,-9.33853972082531,
120.266432958544));
#110441=CARTESIAN_POINT('Ctrl Pts',(6.38778879405164,-8.73226459447408,
120.324433377056));
#110442=CARTESIAN_POINT('Ctrl Pts',(5.73140868668388,-7.50838739786742,
120.423905018338));
#110443=CARTESIAN_POINT('Ctrl Pts',(5.4473668784054,-6.89412965705805,120.466015011068));
#110444=CARTESIAN_POINT('Ctrl Pts',(4.90360031729592,-5.50854092235599,
120.54504572343));
#110445=CARTESIAN_POINT('Ctrl Pts',(4.66080535888424,-4.73217529540783,
120.578967518694));
#110446=CARTESIAN_POINT('Ctrl Pts',(4.31302249985493,-3.26283597988525,
120.623265249966));
#110447=CARTESIAN_POINT('Ctrl Pts',(4.19367911309405,-2.57510314607509,
120.636271151057));
#110448=CARTESIAN_POINT('Ctrl Pts',(4.04643707067672,-1.25699276336321,
120.646735609308));
#110449=CARTESIAN_POINT('Ctrl Pts',(4.0108211163763,-0.628705474055431,
120.645595089839));
#110450=CARTESIAN_POINT('Ctrl Pts',(4.00959443610706,-1.25170827869336E-8,
120.638638242996));
#110451=CARTESIAN_POINT('Origin',(20.412052742069,1.37771738462078E-14,
115.762503617193));
#110452=CARTESIAN_POINT('',(3.80489827855296,1.16952742876573E-14,119.477748646113));
#110453=CARTESIAN_POINT('',(3.85199197861135,7.51016167425201E-9,119.744830291073));
#110454=CARTESIAN_POINT('',(3.67032094086137,1.16952742876573E-14,118.71452263753));
#110455=CARTESIAN_POINT('',(17.9811304327022,16.7992135480526,116.97809643255));
#110456=CARTESIAN_POINT('Origin',(20.5466300797608,1.37771738462078E-14,
116.525729625777));
#110457=CARTESIAN_POINT('Ctrl Pts',(17.9811304327023,16.7992135480526,116.97809643255));
#110458=CARTESIAN_POINT('Ctrl Pts',(16.7897846372373,16.6112487406192,117.201949554145));
#110459=CARTESIAN_POINT('Ctrl Pts',(15.6221214752571,16.2926540637075,117.422346711372));
#110460=CARTESIAN_POINT('Ctrl Pts',(13.7984931675232,15.5726780929255,117.766899663695));
#110461=CARTESIAN_POINT('Ctrl Pts',(13.1176819238496,15.2486694483281,117.89535197941));
#110462=CARTESIAN_POINT('Ctrl Pts',(11.8683145822032,14.5460375899264,118.13183797067));
#110463=CARTESIAN_POINT('Ctrl Pts',(11.2964699645734,14.1765810026866,118.240442965548));
#110464=CARTESIAN_POINT('Ctrl Pts',(10.1000199300896,13.2953484678201,118.468781311182));
#110465=CARTESIAN_POINT('Ctrl Pts',(9.48641127866864,12.7710444737475,118.58664290091));
#110466=CARTESIAN_POINT('Ctrl Pts',(8.41106966230483,11.7091865788779,118.793819869014));
#110467=CARTESIAN_POINT('Ctrl Pts',(7.94098286826109,11.1828822588,118.884524327492));
#110468=CARTESIAN_POINT('Ctrl Pts',(7.07488977840765,10.0815779627471,119.052942000803));
#110469=CARTESIAN_POINT('Ctrl Pts',(6.67873017827656,9.50845691218004,119.130682972688));
#110470=CARTESIAN_POINT('Ctrl Pts',(5.90057500006669,8.22000395384214,119.285353401939));
#110471=CARTESIAN_POINT('Ctrl Pts',(5.53205869993802,7.49827075882032,119.35996502358));
#110472=CARTESIAN_POINT('Ctrl Pts',(5.03245268068873,6.32019700437465,119.462841783204));
#110473=CARTESIAN_POINT('Ctrl Pts',(4.86689017575074,5.88037631964747,119.497300359212));
#110474=CARTESIAN_POINT('Ctrl Pts',(4.53511218387901,4.87565684204279,119.567599586156));
#110475=CARTESIAN_POINT('Ctrl Pts',(4.3794227228022,4.30778758820975,119.601585958567));
#110476=CARTESIAN_POINT('Ctrl Pts',(4.07443613362868,2.91937729590652,119.671469568118));
#110477=CARTESIAN_POINT('Ctrl Pts',(3.9549810780892,2.09359099508143,119.702253960006));
#110478=CARTESIAN_POINT('Ctrl Pts',(3.8709218449021,0.914803833709377,119.730912944905));
#110479=CARTESIAN_POINT('Ctrl Pts',(3.85667055737714,0.566765573452197,
119.737496515519));
#110480=CARTESIAN_POINT('Ctrl Pts',(3.85216809223894,0.145671403107022,
119.743133563671));
#110481=CARTESIAN_POINT('Ctrl Pts',(3.85184987052789,0.0728341540194984,
119.744024355712));
#110482=CARTESIAN_POINT('Ctrl Pts',(3.85199197861135,1.50203116532297E-8,
119.744830291073));
#110483=CARTESIAN_POINT('Origin',(20.5162416486691,1.37771738462078E-14,
116.353388269));
#110484=CARTESIAN_POINT('',(21.2294226865383,16.375,120.398038737828));
#110485=CARTESIAN_POINT('',(21.261705303182,16.375,120.581122925479));
#110486=CARTESIAN_POINT('',(20.5162416486691,16.375,116.353388269));
#110487=CARTESIAN_POINT('',(29.803853834021,-13.9658945114651,119.791289468368));
#110488=CARTESIAN_POINT('Ctrl Pts',(21.2617053031124,16.375,120.581122925109));
#110489=CARTESIAN_POINT('Ctrl Pts',(21.1269512056705,16.3749999997303,120.606507815194));
#110490=CARTESIAN_POINT('Ctrl Pts',(20.9921933482164,16.3732778189865,120.63190684463));
#110491=CARTESIAN_POINT('Ctrl Pts',(20.4234668755599,16.3587364271667,120.739138712706));
#110492=CARTESIAN_POINT('Ctrl Pts',(19.9901057026894,16.3297742801148,120.820938220858));
#110493=CARTESIAN_POINT('Ctrl Pts',(18.9074685346542,16.2125102897728,121.025273537121));
#110494=CARTESIAN_POINT('Ctrl Pts',(18.2613381062145,16.1016481834457,121.147187874784));
#110495=CARTESIAN_POINT('Ctrl Pts',(17.040237438277,15.8132755463647,121.377460830846));
#110496=CARTESIAN_POINT('Ctrl Pts',(16.464849099634,15.6424711480854,121.485914365438));
#110497=CARTESIAN_POINT('Ctrl Pts',(15.5273800888505,15.3053767234912,121.662938424917));
#110498=CARTESIAN_POINT('Ctrl Pts',(15.1595706886934,15.1573850569893,121.732498702259));
#110499=CARTESIAN_POINT('Ctrl Pts',(14.4252491828481,14.8295638279538,121.871755302321));
#110500=CARTESIAN_POINT('Ctrl Pts',(14.0593279911024,14.6490727431445,121.941311346875));
#110501=CARTESIAN_POINT('Ctrl Pts',(13.0802953667339,14.1186195775368,122.127631897839));
#110502=CARTESIAN_POINT('Ctrl Pts',(12.4823912340228,13.7415689404671,122.241638539003));
#110503=CARTESIAN_POINT('Ctrl Pts',(11.4207751138345,12.969825138321,122.444387053643));
#110504=CARTESIAN_POINT('Ctrl Pts',(10.9509477020293,12.5859985757552,122.534257344454));
#110505=CARTESIAN_POINT('Ctrl Pts',(10.1918732035576,11.8910283622617,122.68013809973));
#110506=CARTESIAN_POINT('Ctrl Pts',(9.8914274046672,11.5934999012115,122.738110135063));
#110507=CARTESIAN_POINT('Ctrl Pts',(9.30389691116128,10.9642473591434,122.852132975335));
#110508=CARTESIAN_POINT('Ctrl Pts',(9.01790100642259,10.6319450589894,122.907948037655));
#110509=CARTESIAN_POINT('Ctrl Pts',(8.3346946432277,9.77002890623512,123.041852891722));
#110510=CARTESIAN_POINT('Ctrl Pts',(7.95541465582553,9.22672979937164,123.116714236926));
#110511=CARTESIAN_POINT('Ctrl Pts',(7.29353055361505,8.14421917103656,123.24838215676));
#110512=CARTESIAN_POINT('Ctrl Pts',(7.00596235598823,7.6094465227335,123.306085224782));
#110513=CARTESIAN_POINT('Ctrl Pts',(6.57839874640348,6.69652825631077,123.393199208712));
#110514=CARTESIAN_POINT('Ctrl Pts',(6.42160935731405,6.32721063845961,123.42555097996));
#110515=CARTESIAN_POINT('Ctrl Pts',(6.13113819043648,5.56695197763243,123.486544787148));
#110516=CARTESIAN_POINT('Ctrl Pts',(5.99833290099452,5.17597196389945,123.514996189111));
#110517=CARTESIAN_POINT('Ctrl Pts',(5.67612605157289,4.09624359164223,123.585500638579));
#110518=CARTESIAN_POINT('Ctrl Pts',(5.51633769147871,3.39926906699333,123.622255672012));
#110519=CARTESIAN_POINT('Ctrl Pts',(5.30385533983494,2.08939589378513,123.675279010022));
#110520=CARTESIAN_POINT('Ctrl Pts',(5.23927219752487,1.47978403044136,123.693693797234));
#110521=CARTESIAN_POINT('Ctrl Pts',(5.18708047007613,0.441860951021354,
123.714932049854));
#110522=CARTESIAN_POINT('Ctrl Pts',(5.1820715209045,0.0151378861207446,
123.720810605118));
#110523=CARTESIAN_POINT('Ctrl Pts',(5.20533579560537,-0.852946561745866,
123.727133846083));
#110524=CARTESIAN_POINT('Ctrl Pts',(5.23477924860972,-1.29392967011017,
123.727328428485));
#110525=CARTESIAN_POINT('Ctrl Pts',(5.35255986801764,-2.39559987145586,
123.719997679546));
#110526=CARTESIAN_POINT('Ctrl Pts',(5.4631026600747,-3.05308131739314,123.708490076003));
#110527=CARTESIAN_POINT('Ctrl Pts',(5.74965155641503,-4.29561372888164,
123.672923694812));
#110528=CARTESIAN_POINT('Ctrl Pts',(5.91905732867391,-4.88109286318209,
123.650049926354));
#110529=CARTESIAN_POINT('Ctrl Pts',(6.25303511544757,-5.83505987818467,
123.602883613529));
#110530=CARTESIAN_POINT('Ctrl Pts',(6.39958339676622,-6.20936127595935,
123.581748763323));
#110531=CARTESIAN_POINT('Ctrl Pts',(6.72409593944177,-6.95670839164034,
123.534304350866));
#110532=CARTESIAN_POINT('Ctrl Pts',(6.90270537908738,-7.32914786893943,
123.507844941356));
#110533=CARTESIAN_POINT('Ctrl Pts',(7.42744081686339,-8.32566133521726,
123.429010612853));
#110534=CARTESIAN_POINT('Ctrl Pts',(7.80023096658084,-8.93428005939323,
123.371857676562));
#110535=CARTESIAN_POINT('Ctrl Pts',(8.56291104944619,-10.0149755171322,
123.252933560257));
#110536=CARTESIAN_POINT('Ctrl Pts',(8.94210788683628,-10.4932708191696,
123.193097965516));
#110537=CARTESIAN_POINT('Ctrl Pts',(9.62857811287774,-11.2661453947988,
123.084090185315));
#110538=CARTESIAN_POINT('Ctrl Pts',(9.92244097039273,-11.5720938239209,
123.037269574351));
#110539=CARTESIAN_POINT('Ctrl Pts',(10.5439165031095,-12.1704982453563,
122.938112031132));
#110540=CARTESIAN_POINT('Ctrl Pts',(10.8720910784943,-12.4618411075081,
122.88563226067));
#110541=CARTESIAN_POINT('Ctrl Pts',(11.7232110728059,-13.1579209029844,
122.748993988834));
#110542=CARTESIAN_POINT('Ctrl Pts',(12.2596225237396,-13.5444390127188,
122.662394241632));
#110543=CARTESIAN_POINT('Ctrl Pts',(13.3282468833882,-14.2191321682476,
122.488926845304));
#110544=CARTESIAN_POINT('Ctrl Pts',(13.8560919154325,-14.5123516537041,
122.402850562903));
#110545=CARTESIAN_POINT('Ctrl Pts',(14.7571455984442,-14.9485466527617,
122.255693470097));
#110546=CARTESIAN_POINT('Ctrl Pts',(15.1216568623872,-15.1085717248892,
122.196125867526));
#110547=CARTESIAN_POINT('Ctrl Pts',(15.8720373112074,-15.4052214253995,
122.073589452596));
#110548=CARTESIAN_POINT('Ctrl Pts',(16.2579387225977,-15.5409497290459,
122.010578872716));
#110549=CARTESIAN_POINT('Ctrl Pts',(17.323604807395,-15.8705043590967,121.83636387708));
#110550=CARTESIAN_POINT('Ctrl Pts',(18.0114575793266,-16.0342474679337,
121.72365690338));
#110551=CARTESIAN_POINT('Ctrl Pts',(19.3040909184839,-16.2527090462653,
121.511287731991));
#110552=CARTESIAN_POINT('Ctrl Pts',(19.9056432154307,-16.3195087069062,
121.412244869666));
#110553=CARTESIAN_POINT('Ctrl Pts',(20.9298560428971,-16.374595452193,121.243683956606));
#110554=CARTESIAN_POINT('Ctrl Pts',(21.350950315253,-16.3805490867381,121.174429015541));
#110555=CARTESIAN_POINT('Ctrl Pts',(22.2076294821451,-16.3587362487866,
121.033798725361));
#110556=CARTESIAN_POINT('Ctrl Pts',(22.6428343647055,-16.3297738665615,
120.962446622456));
#110557=CARTESIAN_POINT('Ctrl Pts',(23.7567701834067,-16.2096293183694,
120.779796878244));
#110558=CARTESIAN_POINT('Ctrl Pts',(24.4319001791433,-16.092525994299,120.669056267746));
#110559=CARTESIAN_POINT('Ctrl Pts',(25.7011748832876,-15.7872685860135,
120.460728725052));
#110560=CARTESIAN_POINT('Ctrl Pts',(26.2959353891529,-15.6070341040097,
120.363059305307));
#110561=CARTESIAN_POINT('Ctrl Pts',(27.2530063170519,-15.2550803340175,
120.206278780732));
#110562=CARTESIAN_POINT('Ctrl Pts',(27.6218563501888,-15.1036121468542,
120.145985071172));
#110563=CARTESIAN_POINT('Ctrl Pts',(28.6108934709591,-14.6537505947678,
119.984795098443));
#110564=CARTESIAN_POINT('Ctrl Pts',(29.2184750314435,-14.3288893674278,
119.886175468315));
#110565=CARTESIAN_POINT('Ctrl Pts',(29.8038538340209,-13.9658945114651,
119.791289468367));
#110566=CARTESIAN_POINT('',(29.9797471638325,-13.9658945114651,120.78883011192));
#110567=CARTESIAN_POINT('',(28.9358823285198,-13.9658945114651,114.868778449272));
#110568=CARTESIAN_POINT('',(21.4378004997014,16.375,121.57980804145));
#110569=CARTESIAN_POINT('Ctrl Pts',(29.9797471638324,-13.9658945114651,
120.78883011192));
#110570=CARTESIAN_POINT('Ctrl Pts',(29.3944021100277,-14.3288894249513,
120.883908051799));
#110571=CARTESIAN_POINT('Ctrl Pts',(28.7869186269802,-14.6537508697208,
120.983086135754));
#110572=CARTESIAN_POINT('Ctrl Pts',(27.7979459389566,-15.1036132821563,
121.144653755592));
#110573=CARTESIAN_POINT('Ctrl Pts',(27.4290848004083,-15.2550818060388,
121.204892044499));
#110574=CARTESIAN_POINT('Ctrl Pts',(26.4719346799092,-15.6070341116341,
121.361202243655));
#110575=CARTESIAN_POINT('Ctrl Pts',(25.8770929701107,-15.7872689181212,
121.458416794086));
#110576=CARTESIAN_POINT('Ctrl Pts',(24.6077612876369,-16.0925256255625,
121.666406371788));
#110577=CARTESIAN_POINT('Ctrl Pts',(23.932665983966,-16.2096292700361,121.777342911966));
#110578=CARTESIAN_POINT('Ctrl Pts',(22.8188369260007,-16.3297740799414,
121.960622120204));
#110579=CARTESIAN_POINT('Ctrl Pts',(22.3836860223534,-16.3587363282615,
122.032277261078));
#110580=CARTESIAN_POINT('Ctrl Pts',(21.5270543386933,-16.3805491248486,
122.173179027013));
#110581=CARTESIAN_POINT('Ctrl Pts',(21.1059385050175,-16.3745952485427,
122.242325956352));
#110582=CARTESIAN_POINT('Ctrl Pts',(20.0816359839474,-16.3195085930257,
122.410352281758));
#110583=CARTESIAN_POINT('Ctrl Pts',(19.4800062015085,-16.2527088833392,
122.508960347141));
#110584=CARTESIAN_POINT('Ctrl Pts',(18.1873191735067,-16.0342478697915,
122.721001538412));
#110585=CARTESIAN_POINT('Ctrl Pts',(17.4995094847756,-15.8705056928154,
122.833941613525));
#110586=CARTESIAN_POINT('Ctrl Pts',(16.4339496735706,-15.540950150731,123.008779836653));
#110587=CARTESIAN_POINT('Ctrl Pts',(16.0480942764558,-15.4052216747475,
123.072054053034));
#110588=CARTESIAN_POINT('Ctrl Pts',(15.2977511897487,-15.1085719611476,
123.194803313129));
#110589=CARTESIAN_POINT('Ctrl Pts',(14.9332184555073,-14.9485461801693,
123.254257208779));
#110590=CARTESIAN_POINT('Ctrl Pts',(14.0320796358113,-14.5123532582918,
123.400908319161));
#110591=CARTESIAN_POINT('Ctrl Pts',(13.5041600021885,-14.219133267749,123.486568992282));
#110592=CARTESIAN_POINT('Ctrl Pts',(12.4354863194849,-13.5444404384541,
123.659754835075));
#110593=CARTESIAN_POINT('Ctrl Pts',(11.8991092132909,-13.1579220206212,
123.746555154068));
#110594=CARTESIAN_POINT('Ctrl Pts',(11.0480938874283,-12.461839043354,123.883807708687));
#110595=CARTESIAN_POINT('Ctrl Pts',(10.7199733362648,-12.1704965455087,
123.936590510773));
#110596=CARTESIAN_POINT('Ctrl Pts',(10.0985454486913,-11.5720918322731,
124.036019501507));
#110597=CARTESIAN_POINT('Ctrl Pts',(9.80466184291277,-11.2661413923323,
124.082731956147));
#110598=CARTESIAN_POINT('Ctrl Pts',(9.11810056555315,-10.493270010477,124.191205387751));
#110599=CARTESIAN_POINT('Ctrl Pts',(8.73882656970699,-10.0149741521335,
124.250606128712));
#110600=CARTESIAN_POINT('Ctrl Pts',(7.97609112199115,-8.93428178111615,
124.369202557721));
#110601=CARTESIAN_POINT('Ctrl Pts',(7.60334271648535,-8.32566482224343,
124.426588827785));
#110602=CARTESIAN_POINT('Ctrl Pts',(7.07871526636778,-7.32914810760958,
124.506046080878));
#110603=CARTESIAN_POINT('Ctrl Pts',(6.90015222220985,-6.95670839502068,
124.532769062744));
#110604=CARTESIAN_POINT('Ctrl Pts',(6.57567713062222,-6.20936116622651,
124.580426305091));
#110605=CARTESIAN_POINT('Ctrl Pts',(6.42910821308334,-5.83505806167831,
124.601447298829));
#110606=CARTESIAN_POINT('Ctrl Pts',(6.09504272613763,-4.88109526449257,
124.64810808053));
#110607=CARTESIAN_POINT('Ctrl Pts',(5.92556315345833,-4.29561499013365,
124.670566100082));
#110608=CARTESIAN_POINT('Ctrl Pts',(5.63896487902089,-3.05308393470428,
124.705850948283));
#110609=CARTESIAN_POINT('Ctrl Pts',(5.52845704873351,-2.39560234093178,
124.71755902434));
#110610=CARTESIAN_POINT('Ctrl Pts',(5.41078428677368,-1.29392779961911,
124.725503499201));
#110611=CARTESIAN_POINT('Ctrl Pts',(5.38139438319101,-0.852945015804496,
124.725612027869));
#110612=CARTESIAN_POINT('Ctrl Pts',(5.35817798569936,0.0151398450618967,
124.719560192696));
#110613=CARTESIAN_POINT('Ctrl Pts',(5.36316803309009,0.441865208087525,
124.713573158733));
#110614=CARTESIAN_POINT('Ctrl Pts',(5.41526548781392,1.47978373344985,124.691801126435));
#110615=CARTESIAN_POINT('Ctrl Pts',(5.47977197340088,2.08939652759494,124.672951394821));
#110616=CARTESIAN_POINT('Ctrl Pts',(5.6921959618452,3.39926527619464,124.619600905232));
#110617=CARTESIAN_POINT('Ctrl Pts',(5.85202440596573,4.0962373951753,124.58307950803));
#110618=CARTESIAN_POINT('Ctrl Pts',(6.17434178503615,5.1759692947472,124.513197536662));
#110619=CARTESIAN_POINT('Ctrl Pts',(6.30719381190663,5.56695016223244,124.485009638771));
#110620=CARTESIAN_POINT('Ctrl Pts',(6.59770249544839,6.32720904056206,124.424228648833));
#110621=CARTESIAN_POINT('Ctrl Pts',(6.75447232087668,6.69652774090623,124.391762838437));
#110622=CARTESIAN_POINT('Ctrl Pts',(7.18194463766329,7.60944193100352,124.304143958711));
#110623=CARTESIAN_POINT('Ctrl Pts',(7.46944007558031,8.1442161164386,124.246024954014));
#110624=CARTESIAN_POINT('Ctrl Pts',(8.13127492523547,9.22672774730711,124.114075450868));
#110625=CARTESIAN_POINT('Ctrl Pts',(8.51059129421667,9.77002887131228,124.039414303072));
#110626=CARTESIAN_POINT('Ctrl Pts',(9.19390956598191,10.6319490500238,123.906122446443));
#110627=CARTESIAN_POINT('Ctrl Pts',(9.4799582384132,10.9642503171294,123.850610644148));
#110628=CARTESIAN_POINT('Ctrl Pts',(10.0675368529298,11.5935029744899,123.736859168768));
#110629=CARTESIAN_POINT('Ctrl Pts',(10.3679658697001,11.8910333821555,123.678778272639));
#110630=CARTESIAN_POINT('Ctrl Pts',(11.1269433076025,12.5860004639231,123.532364226923));
#110631=CARTESIAN_POINT('Ctrl Pts',(11.5966943771743,12.9698272473745,123.442058941853));
#110632=CARTESIAN_POINT('Ctrl Pts',(12.6582505577837,13.7415691161477,123.238983535326));
#110633=CARTESIAN_POINT('Ctrl Pts',(13.2561952297131,14.1186196962087,123.12521042485));
#110634=CARTESIAN_POINT('Ctrl Pts',(14.2353411786659,14.6490744678662,122.939511854664));
#110635=CARTESIAN_POINT('Ctrl Pts',(14.6013081951695,14.8295650960931,122.870219495883));
#110636=CARTESIAN_POINT('Ctrl Pts',(15.3356672835137,15.1573862653283,122.731175704262));
#110637=CARTESIAN_POINT('Ctrl Pts',(15.7034591555473,15.3053787483099,122.66150101211));
#110638=CARTESIAN_POINT('Ctrl Pts',(16.6408352988461,15.6424715764168,122.483972329681));
#110639=CARTESIAN_POINT('Ctrl Pts',(17.2161508849222,15.8132761446567,122.375102868236));
#110640=CARTESIAN_POINT('Ctrl Pts',(18.4371969010661,16.1016474159221,122.144549354173));
#110641=CARTESIAN_POINT('Ctrl Pts',(19.0833596182917,16.2125094357943,122.022835999945));
#110642=CARTESIAN_POINT('Ctrl Pts',(20.1661074307351,16.3297740472679,121.819113940843));
#110643=CARTESIAN_POINT('Ctrl Pts',(20.5995231439279,16.3587363141683,121.737617351258));
#110644=CARTESIAN_POINT('Ctrl Pts',(21.1682825795621,16.3732778015187,121.630566221165));
#110645=CARTESIAN_POINT('Ctrl Pts',(21.3030457948456,16.3750000002692,121.605193046341));
#110646=CARTESIAN_POINT('Ctrl Pts',(21.4378004997708,16.375,121.579808041818));
#110647=CARTESIAN_POINT('',(21.9054270700044,16.375,124.231850293098));
#110648=CARTESIAN_POINT('',(20.5162416486691,16.375,116.353388269));
#110649=CARTESIAN_POINT('',(38.0316540255793,1.18260248212283E-14,121.388361383802));
#110650=CARTESIAN_POINT('Origin',(21.9054270700043,1.37771738462078E-14,
124.231850293098));
#110651=CARTESIAN_POINT('Origin',(21.9054270700043,1.37771738462078E-14,
124.231850293098));
#110652=CARTESIAN_POINT('Ctrl Pts',(21.4378004997708,16.375,121.579808041818));
#110653=CARTESIAN_POINT('Ctrl Pts',(21.7222361261571,16.3749999994318,121.526226241716));
#110654=CARTESIAN_POINT('Ctrl Pts',(22.0066339771936,16.3673270421196,121.47259248499));
#110655=CARTESIAN_POINT('Ctrl Pts',(22.8920517384166,16.3195086361738,121.305544195588));
#110656=CARTESIAN_POINT('Ctrl Pts',(23.491124819392,16.2527089343712,121.192435949445));
#110657=CARTESIAN_POINT('Ctrl Pts',(24.7783754467992,16.0342479790364,120.949564525856));
#110658=CARTESIAN_POINT('Ctrl Pts',(25.46333266265,15.8705058949884,120.820448760452));
#110659=CARTESIAN_POINT('Ctrl Pts',(26.5244295283424,15.5409504402565,120.620300033193));
#110660=CARTESIAN_POINT('Ctrl Pts',(26.9086562714279,15.4052219085772,120.547787988342));
#110661=CARTESIAN_POINT('Ctrl Pts',(27.6557308815608,15.1085722073146,120.406502106944));
#110662=CARTESIAN_POINT('Ctrl Pts',(28.0186138551774,14.9485465243931,120.337692989708));
#110663=CARTESIAN_POINT('Ctrl Pts',(28.9155649566073,14.5123536902484,120.167292334214));
#110664=CARTESIAN_POINT('Ctrl Pts',(29.4409449496387,14.2191336615093,120.067227862616));
#110665=CARTESIAN_POINT('Ctrl Pts',(30.5044035067849,13.5444404241436,119.864461254712));
#110666=CARTESIAN_POINT('Ctrl Pts',(31.0381211372528,13.157921576383,119.762574991515));
#110667=CARTESIAN_POINT('Ctrl Pts',(31.8847573402336,12.4618382692119,119.600485773276));
#110668=CARTESIAN_POINT('Ctrl Pts',(32.2111423310358,12.1704959589415,119.537861592847));
#110669=CARTESIAN_POINT('Ctrl Pts',(32.8291001932741,11.5720912592585,119.418753436823));
#110670=CARTESIAN_POINT('Ctrl Pts',(33.121237213726,11.266140611681,119.362134640409));
#110671=CARTESIAN_POINT('Ctrl Pts',(33.8034938719758,10.4932691090054,119.229248537044));
#110672=CARTESIAN_POINT('Ctrl Pts',(34.1802109554807,10.0149733658491,119.155347655861));
#110673=CARTESIAN_POINT('Ctrl Pts',(34.9375104429859,8.93428052790522,119.005920908103));
#110674=CARTESIAN_POINT('Ctrl Pts',(35.3074069273513,8.32566292344506,118.932358839238));
#110675=CARTESIAN_POINT('Ctrl Pts',(35.8275713306143,7.32914601069121,118.827591098178));
#110676=CARTESIAN_POINT('Ctrl Pts',(36.0045052055848,6.95670680667804,118.791630388278));
#110677=CARTESIAN_POINT('Ctrl Pts',(36.3257117160693,6.20935960933227,118.72543654362));
#110678=CARTESIAN_POINT('Ctrl Pts',(36.4706311965658,5.8350559938846,118.695060261463));
#110679=CARTESIAN_POINT('Ctrl Pts',(36.8005088957717,4.88109297625686,118.624649943295));
#110680=CARTESIAN_POINT('Ctrl Pts',(36.9674485190917,4.29561302139565,118.587788186366));
#110681=CARTESIAN_POINT('Ctrl Pts',(37.248830317375,3.05308409461299,118.522922850208));
#110682=CARTESIAN_POINT('Ctrl Pts',(37.3566778499744,2.39560434712044,118.49612900573));
#110683=CARTESIAN_POINT('Ctrl Pts',(37.4699713981878,1.29393086671745,118.463347900124));
#110684=CARTESIAN_POINT('Ctrl Pts',(37.4976261147887,0.852947267673733,
118.453397913905));
#110685=CARTESIAN_POINT('Ctrl Pts',(37.5173726205114,-0.0151377222979068,
118.439770558581));
#110686=CARTESIAN_POINT('Ctrl Pts',(37.5106358978946,-0.441862395858203,
118.435851279401));
#110687=CARTESIAN_POINT('Ctrl Pts',(37.4542340612267,-1.47978071072371,
118.433210602794));
#110688=CARTESIAN_POINT('Ctrl Pts',(37.3871708562621,-2.08939398164617,
118.437560151437));
#110689=CARTESIAN_POINT('Ctrl Pts',(37.1693110498983,-3.39926140698662,
118.460080320012));
#110690=CARTESIAN_POINT('Ctrl Pts',(37.0066310088258,-4.09623178047477,
118.480425890428));
#110691=CARTESIAN_POINT('Ctrl Pts',(36.6798512862242,-5.17596354202306,
118.524997254247));
#110692=CARTESIAN_POINT('Ctrl Pts',(36.5453700143859,-5.56694590290851,
118.543947412508));
#110693=CARTESIAN_POINT('Ctrl Pts',(36.2515929072055,-6.32720498028925,
118.586191770913));
#110694=CARTESIAN_POINT('Ctrl Pts',(36.0931741535806,-6.69652246503088,
118.609302228583));
#110695=CARTESIAN_POINT('Ctrl Pts',(35.6615147351133,-7.60943643762439,
118.673171460244));
#110696=CARTESIAN_POINT('Ctrl Pts',(35.3714792670182,-8.14421153955864,
118.716886724508));
#110697=CARTESIAN_POINT('Ctrl Pts',(34.7044258267118,-9.22672823825842,
118.819256011129));
#110698=CARTESIAN_POINT('Ctrl Pts',(34.3224465464673,-9.77003324424218,
118.878831771153));
#110699=CARTESIAN_POINT('Ctrl Pts',(33.6347467080441,-10.6319550936825,
118.987287368102));
#110700=CARTESIAN_POINT('Ctrl Pts',(33.346963979321,-10.9642546314623,119.032957548238));
#110701=CARTESIAN_POINT('Ctrl Pts',(32.7559154858868,-11.5935069059218,
119.127029835159));
#110702=CARTESIAN_POINT('Ctrl Pts',(32.4537383334366,-11.8910384451211,
119.175204642437));
#110703=CARTESIAN_POINT('Ctrl Pts',(31.690455477193,-12.5860054842662,119.297206149842));
#110704=CARTESIAN_POINT('Ctrl Pts',(31.2181484062862,-12.9698312933602,
119.373011148012));
#110705=CARTESIAN_POINT('Ctrl Pts',(30.1511529021958,-13.7415748715436,
119.54525679231));
#110706=CARTESIAN_POINT('Ctrl Pts',(29.5503517047452,-14.1186275058327,
119.642854869179));
#110707=CARTESIAN_POINT('Ctrl Pts',(28.5667415101329,-14.6490814459875,
119.803243155691));
#110708=CARTESIAN_POINT('Ctrl Pts',(28.1991490155244,-14.8295700208867,
119.863297175526));
#110709=CARTESIAN_POINT('Ctrl Pts',(27.4615216312337,-15.1573906711399,
119.98380431688));
#110710=CARTESIAN_POINT('Ctrl Pts',(27.0920767663623,-15.3053841706741,
120.044124306935));
#110711=CARTESIAN_POINT('Ctrl Pts',(26.1505114659207,-15.6424763086833,
120.197903679364));
#110712=CARTESIAN_POINT('Ctrl Pts',(25.5726582382064,-15.8132796665848,
120.292369024202));
#110713=CARTESIAN_POINT('Ctrl Pts',(24.3464105618023,-16.101646690875,120.493339600122));
#110714=CARTESIAN_POINT('Ctrl Pts',(23.6976001202803,-16.2125069155516,
120.599965097211));
#110715=CARTESIAN_POINT('Ctrl Pts',(22.6104800182628,-16.3297725545985,
120.778849374753));
#110716=CARTESIAN_POINT('Ctrl Pts',(22.1753235581518,-16.3587356703288,
120.85050543153));
#110717=CARTESIAN_POINT('Ctrl Pts',(21.3186909946927,-16.3805490143385,
120.991407344687));
#110718=CARTESIAN_POINT('Ctrl Pts',(20.897579861281,-16.3745956486072,121.060553506266));
#110719=CARTESIAN_POINT('Ctrl Pts',(19.8732787757631,-16.3195106073079,
121.228579600857));
#110720=CARTESIAN_POINT('Ctrl Pts',(19.2716457430119,-16.2527112656557,
121.327188197699));
#110721=CARTESIAN_POINT('Ctrl Pts',(17.9789677331887,-16.0342529693121,
121.539227907782));
#110722=CARTESIAN_POINT('Ctrl Pts',(17.2911699400339,-15.8705151299385,
121.65216602469));
#110723=CARTESIAN_POINT('Ctrl Pts',(16.2256110707781,-15.5409636651203,
121.827004102874));
#110724=CARTESIAN_POINT('Ctrl Pts',(15.8397454956958,-15.4052325893497,
121.890279994752));
#110725=CARTESIAN_POINT('Ctrl Pts',(15.089401052641,-15.1085834508617,122.01302948704));
#110726=CARTESIAN_POINT('Ctrl Pts',(14.7248766060145,-14.9485622461053,
122.072482042681));
#110727=CARTESIAN_POINT('Ctrl Pts',(13.8237392726469,-14.5123734185352,
122.219132935716));
#110728=CARTESIAN_POINT('Ctrl Pts',(13.2958133916514,-14.2191516452739,
122.304794627804));
#110729=CARTESIAN_POINT('Ctrl Pts',(12.2271051636115,-13.5444397730029,
122.477986077817));
#110730=CARTESIAN_POINT('Ctrl Pts',(11.6907015942455,-13.1579012925143,
122.564790680211));
#110731=CARTESIAN_POINT('Ctrl Pts',(10.8396748707199,-12.4618029196469,
122.702045035395));
#110732=CARTESIAN_POINT('Ctrl Pts',(10.5115661066434,-12.1704691744574,
122.754825925016));
#110733=CARTESIAN_POINT('Ctrl Pts',(9.89014082440581,-11.5720650916264,
122.854254476866));
#110734=CARTESIAN_POINT('Ctrl Pts',(9.5962494959249,-11.2661049607716,122.900968134615));
#110735=CARTESIAN_POINT('Ctrl Pts',(8.9096884978164,-10.493227939379,123.009441458972));
#110736=CARTESIAN_POINT('Ctrl Pts',(8.53042114646386,-10.0149374565039,
123.068841136596));
#110737=CARTESIAN_POINT('Ctrl Pts',(7.76767401985128,-8.93422328457483,
123.187439341529));
#110738=CARTESIAN_POINT('Ctrl Pts',(7.39491157825789,-8.3255761861697,123.244827724305));
#110739=CARTESIAN_POINT('Ctrl Pts',(6.8702897731879,-7.32905021976876,123.324283926982));
#110740=CARTESIAN_POINT('Ctrl Pts',(6.69174074833573,-6.95663424770594,
123.35100474664));
#110741=CARTESIAN_POINT('Ctrl Pts',(6.36726918610559,-6.20928847661341,
123.398661384592));
#110742=CARTESIAN_POINT('Ctrl Pts',(6.22069329714319,-5.83496151244486,
123.419683291972));
#110743=CARTESIAN_POINT('Ctrl Pts',(5.88663248396758,-4.88098841719496,
123.466343133131));
#110744=CARTESIAN_POINT('Ctrl Pts',(5.71716118231043,-4.29552306043338,
123.488799909125));
#110745=CARTESIAN_POINT('Ctrl Pts',(5.43059202460564,-3.05309143511461,
123.524080882845));
#110746=CARTESIAN_POINT('Ctrl Pts',(5.32009658211262,-2.39569608842982,
123.535787770744));
#110747=CARTESIAN_POINT('Ctrl Pts',(5.20241691740778,-1.29407109911206,
123.543734006921));
#110748=CARTESIAN_POINT('Ctrl Pts',(5.17302116161042,-0.853050225325708,
123.543843135581));
#110749=CARTESIAN_POINT('Ctrl Pts',(5.14980110809517,0.015040685568975,
123.537791891366));
#110750=CARTESIAN_POINT('Ctrl Pts',(5.15478782601776,0.441733852511547,
123.531805857046));
#110751=CARTESIAN_POINT('Ctrl Pts',(5.20687455744126,1.47964255425242,123.510035866345));
#110752=CARTESIAN_POINT('Ctrl Pts',(5.2713785440764,2.08927761857135,123.491186293648));
#110753=CARTESIAN_POINT('Ctrl Pts',(5.48378457540696,3.39908464039202,123.437839706366));
#110754=CARTESIAN_POINT('Ctrl Pts',(5.64358431556042,4.09597530786932,123.401324311695));
#110755=CARTESIAN_POINT('Ctrl Pts',(5.96587458919859,5.17570078817396,123.331447262404));
#110756=CARTESIAN_POINT('Ctrl Pts',(6.09874378158368,5.56675136468612,123.303255532476));
#110757=CARTESIAN_POINT('Ctrl Pts',(6.38924865359715,6.32701960449139,123.242475166738));
#110758=CARTESIAN_POINT('Ctrl Pts',(6.54598818995834,6.69628163084384,123.210015516241));
#110759=CARTESIAN_POINT('Ctrl Pts',(6.9734333383126,7.60918570681968,123.122401728821));
#110760=CARTESIAN_POINT('Ctrl Pts',(7.26094054104113,8.14400264683535,123.064280091628));
#110761=CARTESIAN_POINT('Ctrl Pts',(7.92290138239413,9.22675044927814,122.932305105973));
#110762=CARTESIAN_POINT('Ctrl Pts',(8.30235062028651,9.7702324418394,122.857617947061));
#110763=CARTESIAN_POINT('Ctrl Pts',(8.98577097363052,10.632230507092,122.724306678918));
#110764=CARTESIAN_POINT('Ctrl Pts',(9.2717617017989,10.9644512454239,122.668806212761));
#110765=CARTESIAN_POINT('Ctrl Pts',(9.85933622795868,11.593686162692,122.555055595291));
#110766=CARTESIAN_POINT('Ctrl Pts',(10.1598295101648,11.8912693453428,122.496962296319));
#110767=CARTESIAN_POINT('Ctrl Pts',(10.9188444059412,12.5862344768742,122.350541253647));
#110768=CARTESIAN_POINT('Ctrl Pts',(11.3885598734022,12.9700158503167,122.260242976885));
#110769=CARTESIAN_POINT('Ctrl Pts',(12.4502610211082,13.7418377013528,122.057140090391));
#110770=CARTESIAN_POINT('Ctrl Pts',(13.0484060276627,14.1189842703515,121.943329205423));
#110771=CARTESIAN_POINT('Ctrl Pts',(14.0276136304381,14.6494002917169,121.757619390156));
#110772=CARTESIAN_POINT('Ctrl Pts',(14.3934229711875,14.8297950632316,121.688356927724));
#110773=CARTESIAN_POINT('Ctrl Pts',(15.1277727842966,15.1575922049497,121.549314887423));
#110774=CARTESIAN_POINT('Ctrl Pts',(15.4957235374569,15.3056323090703,121.479610041343));
#110775=CARTESIAN_POINT('Ctrl Pts',(16.4331684038946,15.6426929327914,121.302068450448));
#110776=CARTESIAN_POINT('Ctrl Pts',(17.0083848058396,15.8134409010177,121.193217932046));
#110777=CARTESIAN_POINT('Ctrl Pts',(18.2287678622979,16.1016131421324,120.962789861783));
#110778=CARTESIAN_POINT('Ctrl Pts',(18.8743551492525,16.2123909860811,120.841184733511));
#110779=CARTESIAN_POINT('Ctrl Pts',(19.9567726164627,16.329703915597,120.637524613471));
#110780=CARTESIAN_POINT('Ctrl Pts',(20.3904427658092,16.3587060661075,120.555980224506));
#110781=CARTESIAN_POINT('Ctrl Pts',(20.9596068191691,16.373273991557,120.448853015039));
#110782=CARTESIAN_POINT('Ctrl Pts',(21.0945190072874,16.3750000002698,120.42345180642));
#110783=CARTESIAN_POINT('Ctrl Pts',(21.2294226866078,16.375,120.398038738197));
#110784=CARTESIAN_POINT('Origin',(20.5162416486691,1.37771738462078E-14,
116.353388269));
#110785=CARTESIAN_POINT('',(21.0210448802951,16.375,119.216269432819));
#110786=CARTESIAN_POINT('',(21.0533274904221,16.375,119.399353621776));
#110787=CARTESIAN_POINT('',(20.5162416486691,16.375,116.353388269));
#110788=CARTESIAN_POINT('Ctrl Pts',(21.0533274903535,16.375,119.399353621412));
#110789=CARTESIAN_POINT('Ctrl Pts',(20.9203211694499,16.3749999997375,119.424409266478));
#110790=CARTESIAN_POINT('Ctrl Pts',(20.787310940857,16.3733222029923,119.449478733801));
#110791=CARTESIAN_POINT('Ctrl Pts',(20.223311877966,16.3590887925773,119.555818253589));
#110792=CARTESIAN_POINT('Ctrl Pts',(19.7929163837166,16.3305905185551,119.637057184513));
#110793=CARTESIAN_POINT('Ctrl Pts',(18.706310635637,16.2138830881319,119.842141607053));
#110794=CARTESIAN_POINT('Ctrl Pts',(18.0533556863278,16.1020153840184,119.965344249535));
#110795=CARTESIAN_POINT('Ctrl Pts',(16.8243375113227,15.8112481300296,120.197109812991));
#110796=CARTESIAN_POINT('Ctrl Pts',(16.2477196224269,15.639743939766,120.305795095491));
#110797=CARTESIAN_POINT('Ctrl Pts',(15.3110610197882,15.3022399929439,120.482670398818));
#110798=CARTESIAN_POINT('Ctrl Pts',(14.9451802915709,15.1548230278232,120.551868434007));
#110799=CARTESIAN_POINT('Ctrl Pts',(14.2106624607454,14.8266636041101,120.691164705906));
#110800=CARTESIAN_POINT('Ctrl Pts',(13.8427471830319,14.6449592201731,120.761101545049));
#110801=CARTESIAN_POINT('Ctrl Pts',(12.8644674178109,14.1140035657481,120.947283267502));
#110802=CARTESIAN_POINT('Ctrl Pts',(12.269071580547,13.738151853777,121.060812352906));
#110803=CARTESIAN_POINT('Ctrl Pts',(11.2092537319603,12.967388111256,121.263218700575));
#110804=CARTESIAN_POINT('Ctrl Pts',(10.7389642239055,12.582973013223,121.353178343621));
#110805=CARTESIAN_POINT('Ctrl Pts',(9.98036692713541,11.8879708463641,121.498971884623));
#110806=CARTESIAN_POINT('Ctrl Pts',(9.68074672249082,11.5911190077017,121.556786709824));
#110807=CARTESIAN_POINT('Ctrl Pts',(9.09314685787904,10.9616171643645,121.670825146726));
#110808=CARTESIAN_POINT('Ctrl Pts',(8.80639161607317,10.6282588820644,121.726790240221));
#110809=CARTESIAN_POINT('Ctrl Pts',(8.12450912160487,9.76734771833107,121.86044132184));
#110810=CARTESIAN_POINT('Ctrl Pts',(7.74695906800277,9.2264018404562,121.934962020054));
#110811=CARTESIAN_POINT('Ctrl Pts',(7.08671283228585,8.14695424881023,122.066301029016));
#110812=CARTESIAN_POINT('Ctrl Pts',(6.79929494091541,7.61272789194618,122.12397168301));
#110813=CARTESIAN_POINT('Ctrl Pts',(6.37138053991541,6.69967450997289,122.211150104128));
#110814=CARTESIAN_POINT('Ctrl Pts',(6.21420115195372,6.32962665016487,122.243579672943));
#110815=CARTESIAN_POINT('Ctrl Pts',(5.92367649377749,5.56947388984342,122.304581487186));
#110816=CARTESIAN_POINT('Ctrl Pts',(5.79108858117378,5.17937697230912,122.332983319625));
#110817=CARTESIAN_POINT('Ctrl Pts',(5.46853690991656,4.09956317065931,122.403551083865));
#110818=CARTESIAN_POINT('Ctrl Pts',(5.30838414218357,3.40155243658729,122.440384139609));
#110819=CARTESIAN_POINT('Ctrl Pts',(5.09567395443404,2.09089021655711,122.493457579947));
#110820=CARTESIAN_POINT('Ctrl Pts',(5.03105950660445,1.48155784575182,122.511874950285));
#110821=CARTESIAN_POINT('Ctrl Pts',(4.97873285833206,0.443509922682552,
122.533138202167));
#110822=CARTESIAN_POINT('Ctrl Pts',(4.97368194114913,0.0163812447033533,
122.53902856126));
#110823=CARTESIAN_POINT('Ctrl Pts',(4.99690048968756,-0.851630836139298,
122.545358757691));
#110824=CARTESIAN_POINT('Ctrl Pts',(5.02627073630446,-1.29213789742799,
122.545560310107));
#110825=CARTESIAN_POINT('Ctrl Pts',(5.14396538610984,-2.39443033312803,
122.538252324801));
#110826=CARTESIAN_POINT('Ctrl Pts',(5.25466371609234,-3.05299260799227,
122.526730519826));
#110827=CARTESIAN_POINT('Ctrl Pts',(5.54157816173008,-4.29677235990008,
122.491114630378));
#110828=CARTESIAN_POINT('Ctrl Pts',(5.71108818507745,-4.88243972612774,
122.468224727865));
#110829=CARTESIAN_POINT('Ctrl Pts',(6.04512526822682,-5.83627775691152,
122.421047016773));
#110830=CARTESIAN_POINT('Ctrl Pts',(6.19158602804546,-6.21027903407446,
122.399924203801));
#110831=CARTESIAN_POINT('Ctrl Pts',(6.51614407093082,-6.95764641941092,
122.352472395808));
#110832=CARTESIAN_POINT('Ctrl Pts',(6.6949310428006,-7.3303863901784,122.325986002426));
#110833=CARTESIAN_POINT('Ctrl Pts',(7.21973815462455,-8.32678334842395,
122.247138095185));
#110834=CARTESIAN_POINT('Ctrl Pts',(7.59235085335232,-8.93502113634534,
122.19001118376));
#110835=CARTESIAN_POINT('Ctrl Pts',(8.35488375627462,-10.0154414310004,
122.071109242689));
#110836=CARTESIAN_POINT('Ctrl Pts',(8.73416495622996,-10.4938050238189,
122.01125991514));
#110837=CARTESIAN_POINT('Ctrl Pts',(9.42063891439798,-11.2666081456444,
121.902251015821));
#110838=CARTESIAN_POINT('Ctrl Pts',(9.71440388248239,-11.5724336430292,
121.855445961392));
#110839=CARTESIAN_POINT('Ctrl Pts',(10.3359129459459,-12.1708464294893,
121.756282958297));
#110840=CARTESIAN_POINT('Ctrl Pts',(10.6642375415716,-12.4623006592341,
121.70377905762));
#110841=CARTESIAN_POINT('Ctrl Pts',(11.5152127959518,-13.1581848632437,
121.567163350992));
#110842=CARTESIAN_POINT('Ctrl Pts',(12.0512878497855,-13.5444479422492,
121.480617765594));
#110843=CARTESIAN_POINT('Ctrl Pts',(13.1194733942859,-14.2188990982748,
121.307221926128));
#110844=CARTESIAN_POINT('Ctrl Pts',(13.6472392606898,-14.5120959898824,
121.221158734329));
#110845=CARTESIAN_POINT('Ctrl Pts',(14.5483118791373,-14.9483429681753,
121.0739986727));
#110846=CARTESIAN_POINT('Ctrl Pts',(14.9129282941774,-15.1084261115253,
121.014413846435));
#110847=CARTESIAN_POINT('Ctrl Pts',(15.6632918186689,-15.4050832054591,
120.891880185983));
#110848=CARTESIAN_POINT('Ctrl Pts',(16.0490643426953,-15.5407785915894,
120.828890670378));
#110849=CARTESIAN_POINT('Ctrl Pts',(17.1147424581502,-15.870384877501,120.654673919081));
#110850=CARTESIAN_POINT('Ctrl Pts',(17.8027459788404,-16.0341829287138,
120.541942393758));
#110851=CARTESIAN_POINT('Ctrl Pts',(19.0954936622483,-16.252678919039,120.329554519236));
#110852=CARTESIAN_POINT('Ctrl Pts',(19.6970048808091,-16.3194832338718,
120.230518462596));
#110853=CARTESIAN_POINT('Ctrl Pts',(20.7212358750149,-16.374590393029,120.061954524187));
#110854=CARTESIAN_POINT('Ctrl Pts',(21.142389585171,-16.3805504838629,119.99268975654));
#110855=CARTESIAN_POINT('Ctrl Pts',(21.9990576940155,-16.3587445618759,
119.852061246133));
#110856=CARTESIAN_POINT('Ctrl Pts',(22.4341923546796,-16.3297931391106,
119.780720637706));
#110857=CARTESIAN_POINT('Ctrl Pts',(23.5215147846586,-16.2125421285139,
119.602434637965));
#110858=CARTESIAN_POINT('Ctrl Pts',(24.1705316150466,-16.1016573271302,
119.495981499937));
#110859=CARTESIAN_POINT('Ctrl Pts',(25.3969283948824,-15.8132309897795,
119.294696800569));
#110860=CARTESIAN_POINT('Ctrl Pts',(25.974736828262,-15.6424112777742,119.199810956528));
#110861=CARTESIAN_POINT('Ctrl Pts',(26.9161967631457,-15.3053081163725,
119.045529009866));
#110862=CARTESIAN_POINT('Ctrl Pts',(27.2855724649651,-15.157329304571,118.985103169793));
#110863=CARTESIAN_POINT('Ctrl Pts',(28.023240228696,-14.8295014890817,118.864808434484));
#110864=CARTESIAN_POINT('Ctrl Pts',(28.3909261992793,-14.6489844107888,
118.805010368604));
#110865=CARTESIAN_POINT('Ctrl Pts',(29.3746246089003,-14.1185207132103,
118.645248345325));
#110866=CARTESIAN_POINT('Ctrl Pts',(29.97540876194,-13.7414960737775,118.547893137023));
#110867=CARTESIAN_POINT('Ctrl Pts',(31.0423062514426,-12.9697738961824,
118.375326725267));
#110868=CARTESIAN_POINT('Ctrl Pts',(31.5145467914741,-12.5859349926871,
118.299085183482));
#110869=CARTESIAN_POINT('Ctrl Pts',(32.2777274600128,-11.8909642364878,
118.176551214403));
#110870=CARTESIAN_POINT('Ctrl Pts',(32.579864222179,-11.5934501033141,118.128271439765));
#110871=CARTESIAN_POINT('Ctrl Pts',(33.1709615602311,-10.964192702631,118.034470457708));
#110872=CARTESIAN_POINT('Ctrl Pts',(33.4588155505253,-10.6318684935042,
117.98910063556));
#110873=CARTESIAN_POINT('Ctrl Pts',(34.1465898024254,-9.76997349919565,
117.881264190221));
#110874=CARTESIAN_POINT('Ctrl Pts',(34.5285641225073,-9.22672356489209,
117.821895117977));
#110875=CARTESIAN_POINT('Ctrl Pts',(35.1955302645163,-8.14427712583293,
117.719250046472));
#110876=CARTESIAN_POINT('Ctrl Pts',(35.4854883493288,-7.60951608184327,
117.675119523227));
#110877=CARTESIAN_POINT('Ctrl Pts',(35.9170688595763,-6.6965950582735,117.610743271828));
#110878=CARTESIAN_POINT('Ctrl Pts',(36.0754759458669,-6.3272620461677,117.587517590566));
#110879=CARTESIAN_POINT('Ctrl Pts',(36.3692917044827,-5.56700589872329,
117.545485814655));
#110880=CARTESIAN_POINT('Ctrl Pts',(36.5038140735533,-5.17604479014849,
117.526799897119));
#110881=CARTESIAN_POINT('Ctrl Pts',(36.8307107840002,-4.09631466879815,
117.482849928519));
#110882=CARTESIAN_POINT('Ctrl Pts',(36.9934415693796,-3.39931804535262,
117.462736428478));
#110883=CARTESIAN_POINT('Ctrl Pts',(37.21124965804,-2.08942811743555,117.439888163318));
#110884=CARTESIAN_POINT('Ctrl Pts',(37.278236841777,-1.47982228835419,117.435103488774));
#110885=CARTESIAN_POINT('Ctrl Pts',(37.3345478505745,-0.441896543833017,
117.437209807254));
#110886=CARTESIAN_POINT('Ctrl Pts',(37.3412662450185,-0.015164752207746,
117.441020610151));
#110887=CARTESIAN_POINT('Ctrl Pts',(37.3215686369823,0.852918063577151,
117.454919165428));
#110888=CARTESIAN_POINT('Ctrl Pts',(37.2939689355986,1.29389085507792,117.465171866321));
#110889=CARTESIAN_POINT('Ctrl Pts',(37.1807860154667,2.3955744835109,117.498566385078));
#110890=CARTESIAN_POINT('Ctrl Pts',(37.0729706758541,3.05307929587065,117.525561497503));
#110891=CARTESIAN_POINT('Ctrl Pts',(36.7915305971816,4.29563864808195,117.590147220212));
#110892=CARTESIAN_POINT('Ctrl Pts',(36.6245157295591,4.88112182644342,117.626593535732));
#110893=CARTESIAN_POINT('Ctrl Pts',(36.2945461623767,5.8350860514661,117.696499034697));
#110894=CARTESIAN_POINT('Ctrl Pts',(36.1496091413967,6.20938098297544,117.726760834597));
#110895=CARTESIAN_POINT('Ctrl Pts',(35.8284391994415,6.95672849750201,117.793167678135));
#110896=CARTESIAN_POINT('Ctrl Pts',(35.6515478044601,7.3291744126154,117.829392749982));
#110897=CARTESIAN_POINT('Ctrl Pts',(35.1314933200213,8.32568537129509,117.934783053638));
#110898=CARTESIAN_POINT('Ctrl Pts',(34.7616414812724,8.93429592342269,118.008577823979));
#110899=CARTESIAN_POINT('Ctrl Pts',(34.0042853307297,10.0149854708791,118.15767702614));
#110900=CARTESIAN_POINT('Ctrl Pts',(33.6274900889191,10.4932822310832,118.231143256561));
#110901=CARTESIAN_POINT('Ctrl Pts',(32.9451361461289,11.2661552772443,118.363496099272));
#110902=CARTESIAN_POINT('Ctrl Pts',(32.6529838762402,11.5721010779937,118.420005729933));
#110903=CARTESIAN_POINT('Ctrl Pts',(32.0350733220317,12.1705056711608,118.539385402889));
#110904=CARTESIAN_POINT('Ctrl Pts',(31.7087377748204,12.4618509079776,118.602313475707));
#110905=CARTESIAN_POINT('Ctrl Pts',(30.862216626452,13.1579265271975,118.765015077745));
#110906=CARTESIAN_POINT('Ctrl Pts',(30.3285430287005,13.5444391942604,118.867100086278));
#110907=CARTESIAN_POINT('Ctrl Pts',(29.2650445871458,14.219127183877,119.069583341767));
#110908=CARTESIAN_POINT('Ctrl Pts',(28.7395943704859,14.5123461858667,119.169231411785));
#110909=CARTESIAN_POINT('Ctrl Pts',(27.8425497836647,14.9485422955191,119.339127565797));
#110910=CARTESIAN_POINT('Ctrl Pts',(27.479645681317,15.1085686088602,119.407822946635));
#110911=CARTESIAN_POINT('Ctrl Pts',(26.7326091546206,15.4052184655695,119.549321540871));
#110912=CARTESIAN_POINT('Ctrl Pts',(26.3484323068186,15.5409460642146,119.622096499745));
#110913=CARTESIAN_POINT('Ctrl Pts',(25.2874484596572,15.8705017999792,119.822867273445));
#110914=CARTESIAN_POINT('Ctrl Pts',(24.6025270182626,16.0342460851285,119.952217475419));
#110915=CARTESIAN_POINT('Ctrl Pts',(23.3152120382096,16.2527084003158,120.194762832753));
#110916=CARTESIAN_POINT('Ctrl Pts',(22.7160640075198,16.3195081607478,120.307435824552));
#110917=CARTESIAN_POINT('Ctrl Pts',(21.8305604320732,16.3673270491397,120.474021465835));
#110918=CARTESIAN_POINT('Ctrl Pts',(21.5461413107245,16.3750000005693,120.527541053192));
#110919=CARTESIAN_POINT('Ctrl Pts',(21.2617053031124,16.375,120.581122925109));
#110920=CARTESIAN_POINT('Ctrl Pts',(21.2294226866078,16.375,120.398038738197));
#110921=CARTESIAN_POINT('Ctrl Pts',(21.5134950186656,16.3749999994318,120.344525375246));
#110922=CARTESIAN_POINT('Ctrl Pts',(21.7975297616614,16.367346630148,120.290960168832));
#110923=CARTESIAN_POINT('Ctrl Pts',(22.6827331462377,16.3196009721879,120.123952511932));
#110924=CARTESIAN_POINT('Ctrl Pts',(23.2819546901568,16.2528181429115,120.010816176577));
#110925=CARTESIAN_POINT('Ctrl Pts',(24.5687969606972,16.0344811631837,119.768021711038));
#110926=CARTESIAN_POINT('Ctrl Pts',(25.2532141858301,15.8709368925073,119.639007509549));
#110927=CARTESIAN_POINT('Ctrl Pts',(26.3142694095287,15.5415672362654,119.438867076751));
#110928=CARTESIAN_POINT('Ctrl Pts',(26.6989591193503,15.4057199974352,119.366267956656));
#110929=CARTESIAN_POINT('Ctrl Pts',(27.446098706323,15.1090952657638,119.224970259076));
#110930=CARTESIAN_POINT('Ctrl Pts',(27.8086081227856,14.9492770272043,119.156232507818));
#110931=CARTESIAN_POINT('Ctrl Pts',(28.7054937632722,14.5132695459897,118.985845409194));
#110932=CARTESIAN_POINT('Ctrl Pts',(29.2311566231379,14.2199683764795,118.885727302902));
#110933=CARTESIAN_POINT('Ctrl Pts',(30.2961682586649,13.5444157137362,118.682664981306));
#110934=CARTESIAN_POINT('Ctrl Pts',(30.8310736797733,13.156992257377,118.580552014395));
#110935=CARTESIAN_POINT('Ctrl Pts',(31.6782227121215,12.4602135473578,118.41836290964));
#110936=CARTESIAN_POINT('Ctrl Pts',(32.0040804852523,12.1692646809031,118.355839149194));
#110937=CARTESIAN_POINT('Ctrl Pts',(32.6219255216258,11.5708843841068,118.236751742782));
#110938=CARTESIAN_POINT('Ctrl Pts',(32.9144108478208,11.2644938878675,118.180064331312));
#110939=CARTESIAN_POINT('Ctrl Pts',(33.5966555831746,10.4913653907742,118.047177677072));
#110940=CARTESIAN_POINT('Ctrl Pts',(33.9730740610909,10.0133124755201,117.973334340165));
#110941=CARTESIAN_POINT('Ctrl Pts',(34.7309110549308,8.93161365123495,117.823799708292));
#110942=CARTESIAN_POINT('Ctrl Pts',(35.1014474999196,8.32161139607146,117.750108148327));
#110943=CARTESIAN_POINT('Ctrl Pts',(35.6213560086873,7.32466447116878,117.645382917825));
#110944=CARTESIAN_POINT('Ctrl Pts',(35.7976539053324,6.9533107674858,117.609548510462));
#110945=CARTESIAN_POINT('Ctrl Pts',(36.1187085349124,6.20600803773903,117.543381981358));
#110946=CARTESIAN_POINT('Ctrl Pts',(36.2639492666251,5.83059064731746,117.512934325067));
#110947=CARTESIAN_POINT('Ctrl Pts',(36.5936120273196,4.87614005920006,117.442556383083));
#110948=CARTESIAN_POINT('Ctrl Pts',(36.760172508637,4.29134926168896,117.405771407614));
#110949=CARTESIAN_POINT('Ctrl Pts',(37.0402072941495,3.05350876708511,117.341202943854));
#110950=CARTESIAN_POINT('Ctrl Pts',(37.1474869706935,2.40011050524573,117.314556358608));
#110951=CARTESIAN_POINT('Ctrl Pts',(37.2611212435697,1.30076518070404,117.281740711355));
#110952=CARTESIAN_POINT('Ctrl Pts',(37.2890488080266,0.857962089651411,
117.271721981588));
#110953=CARTESIAN_POINT('Ctrl Pts',(37.3089695168339,-0.0104534301986359,
117.258060854832));
#110954=CARTESIAN_POINT('Ctrl Pts',(37.30239556291,-0.435681649274366,117.254132065725));
#110955=CARTESIAN_POINT('Ctrl Pts',(37.2464983072271,-1.47315699711677,
117.25140928359));
#110956=CARTESIAN_POINT('Ctrl Pts',(37.1795476867236,-2.0838190717909,117.255725714679));
#110957=CARTESIAN_POINT('Ctrl Pts',(36.9625138030023,-3.39095251483045,
117.278132817292));
#110958=CARTESIAN_POINT('Ctrl Pts',(36.8011462652692,-4.08425517116368,
117.298289335757));
#110959=CARTESIAN_POINT('Ctrl Pts',(36.4755879127764,-5.16374285414751,
117.342651212008));
#110960=CARTESIAN_POINT('Ctrl Pts',(36.3403113393078,-5.55790844978006,
117.361704829998));
#110961=CARTESIAN_POINT('Ctrl Pts',(36.046651535411,-6.31873447366145,117.403924538607));
#110962=CARTESIAN_POINT('Ctrl Pts',(35.889561717105,-6.68559912228108,117.426836200389));
#110963=CARTESIAN_POINT('Ctrl Pts',(35.4590773767904,-7.59812727527399,
117.490510771011));
#110964=CARTESIAN_POINT('Ctrl Pts',(35.1685081090666,-8.13480279741698,
117.534295347848));
#110965=CARTESIAN_POINT('Ctrl Pts',(34.4960675767682,-9.22738818677147,
117.637475357967));
#110966=CARTESIAN_POINT('Ctrl Pts',(34.1084526938852,-9.77833358789352,
117.697935793953));
#110967=CARTESIAN_POINT('Ctrl Pts',(33.416383995336,-10.6436219415005,117.807101069928));
#110968=CARTESIAN_POINT('Ctrl Pts',(33.131012518227,-10.9725954024996,117.852392309609));
#110969=CARTESIAN_POINT('Ctrl Pts',(32.539977143262,-11.6012786268155,117.94646524767));
#110970=CARTESIAN_POINT('Ctrl Pts',(32.2349583370586,-11.9011408908722,
117.995094008439));
#110971=CARTESIAN_POINT('Ctrl Pts',(31.4699808953676,-12.5960909724161,
118.117376241431));
#110972=CARTESIAN_POINT('Ctrl Pts',(30.9992033483422,-12.9779742156819,
118.192942771545));
#110973=CARTESIAN_POINT('Ctrl Pts',(29.9250603095167,-13.7537834162604,
118.366353178728));
#110974=CARTESIAN_POINT('Ctrl Pts',(29.3146540222838,-14.135455454452,118.46552758637));
#110975=CARTESIAN_POINT('Ctrl Pts',(28.327869273885,-14.664258237489,118.62645404104));
#110976=CARTESIAN_POINT('Ctrl Pts',(27.9676056914279,-14.8403204286184,
118.685312586953));
#110977=CARTESIAN_POINT('Ctrl Pts',(27.2292288878491,-15.1675370351931,
118.805941883212));
#110978=CARTESIAN_POINT('Ctrl Pts',(26.8511828923902,-15.3181436920486,
118.86766342998));
#110979=CARTESIAN_POINT('Ctrl Pts',(25.9055255215102,-15.6537839281739,
119.022116858353));
#110980=CARTESIAN_POINT('Ctrl Pts',(25.3326509320719,-15.8217348348208,
119.115777143231));
#110981=CARTESIAN_POINT('Ctrl Pts',(24.0065756121728,-16.1312006587827,
119.333123395314));
#110982=CARTESIAN_POINT('Ctrl Pts',(23.2499989853418,-16.2513106809087,
119.457537478582));
#110983=CARTESIAN_POINT('Ctrl Pts',(22.1227437429084,-16.3479883612805,
119.643070487807));
#110984=CARTESIAN_POINT('Ctrl Pts',(21.7566465286155,-16.3667080583793,
119.703340805535));
#110985=CARTESIAN_POINT('Ctrl Pts',(20.8509494577884,-16.3817609729779,
119.85227071464));
#110986=CARTESIAN_POINT('Ctrl Pts',(20.3115332160797,-16.3633578094981,
119.940752286598));
#110987=CARTESIAN_POINT('Ctrl Pts',(19.0644156927292,-16.2573254768737,
120.145251878545));
#110988=CARTESIAN_POINT('Ctrl Pts',(18.3595019569084,-16.1495300631213,
120.260835762513));
#110989=CARTESIAN_POINT('Ctrl Pts',(17.0462771970741,-15.8577388354913,
120.476353311716));
#110990=CARTESIAN_POINT('Ctrl Pts',(16.4371244339281,-15.6838853730086,
120.576395890592));
#110991=CARTESIAN_POINT('Ctrl Pts',(15.4086815197983,-15.3231972943878,
120.744975702729));
#110992=CARTESIAN_POINT('Ctrl Pts',(14.984286088183,-15.1536732490818,120.814411242365));
#110993=CARTESIAN_POINT('Ctrl Pts',(14.019459617361,-14.7196821609465,120.971700053072));
#110994=CARTESIAN_POINT('Ctrl Pts',(13.4853391346778,-14.4424664880218,
121.05844865307));
#110995=CARTESIAN_POINT('Ctrl Pts',(12.4106527360227,-13.8059228770537,
121.232750503302));
#110996=CARTESIAN_POINT('Ctrl Pts',(11.8736392465029,-13.4425311238772,
121.319713505817));
#110997=CARTESIAN_POINT('Ctrl Pts',(10.8962105912107,-12.6917782189329,
121.477620651626));
#110998=CARTESIAN_POINT('Ctrl Pts',(10.4522088180043,-12.3109009030544,
121.549177682248));
#110999=CARTESIAN_POINT('Ctrl Pts',(9.7323682879697,-11.6227014300553,121.664410347319));
#111000=CARTESIAN_POINT('Ctrl Pts',(9.44606700080452,-11.3274815466299,
121.709959799127));
#111001=CARTESIAN_POINT('Ctrl Pts',(8.44457766653677,-10.2135459013248,
121.868335081255));
#111002=CARTESIAN_POINT('Ctrl Pts',(7.79952923274599,-9.3338974006903,121.968794657567));
#111003=CARTESIAN_POINT('Ctrl Pts',(6.98470864934987,-7.95388116015941,
122.093722028873));
#111004=CARTESIAN_POINT('Ctrl Pts',(6.74444855758325,-7.49973829971881,
122.130172937738));
#111005=CARTESIAN_POINT('Ctrl Pts',(6.35676924302653,-6.67615368529231,
122.187960184991));
#111006=CARTESIAN_POINT('Ctrl Pts',(6.20080184169789,-6.31130816008181,
122.210811075314));
#111007=CARTESIAN_POINT('Ctrl Pts',(5.90711967765701,-5.54973986342869,
122.252802015243));
#111008=CARTESIAN_POINT('Ctrl Pts',(5.77107244244981,-5.15267225547731,
122.271679117935));
#111009=CARTESIAN_POINT('Ctrl Pts',(5.44648629185545,-4.07332177614223,
122.315236415625));
#111010=CARTESIAN_POINT('Ctrl Pts',(5.28625235340208,-3.38326786220082,
122.33500205284));
#111011=CARTESIAN_POINT('Ctrl Pts',(5.07001927447514,-2.07846844334889,
122.357637112328));
#111012=CARTESIAN_POINT('Ctrl Pts',(5.00325407383151,-1.46679183650972,
122.362360869277));
#111013=CARTESIAN_POINT('Ctrl Pts',(4.9479330168173,-0.429702895801508,
122.360087896895));
#111014=CARTESIAN_POINT('Ctrl Pts',(4.94153372538027,-0.00588754931961123,
122.356252426584));
#111015=CARTESIAN_POINT('Ctrl Pts',(4.96158031325555,0.862936647225923,
122.342281629526));
#111016=CARTESIAN_POINT('Ctrl Pts',(4.98972630475043,1.30755231507119,122.331887164767));
#111017=CARTESIAN_POINT('Ctrl Pts',(5.10874054183148,2.45421185624014,122.296916007331));
#111018=CARTESIAN_POINT('Ctrl Pts',(5.22667370910118,3.152369041336,122.267652327832));
#111019=CARTESIAN_POINT('Ctrl Pts',(5.53647173456419,4.46763733519119,122.197199906973));
#111020=CARTESIAN_POINT('Ctrl Pts',(5.72058753228943,5.08529560591196,122.15735274927));
#111021=CARTESIAN_POINT('Ctrl Pts',(6.06783396324989,6.04232408048288,122.084251450398));
#111022=CARTESIAN_POINT('Ctrl Pts',(6.20746183008263,6.38981961711627,122.055196857674));
#111023=CARTESIAN_POINT('Ctrl Pts',(6.56731607752931,7.20417263369571,121.980998791448));
#111024=CARTESIAN_POINT('Ctrl Pts',(6.79783575642474,7.66587204476267,121.934030527408));
#111025=CARTESIAN_POINT('Ctrl Pts',(7.35679082933926,8.66475997968274,121.821582389694));
#111026=CARTESIAN_POINT('Ctrl Pts',(7.69513997257765,9.19526362312,121.754408161279));
#111027=CARTESIAN_POINT('Ctrl Pts',(8.45821567499527,10.2519815156924,121.604552448363));
#111028=CARTESIAN_POINT('Ctrl Pts',(8.88677888690755,10.7738515475117,121.521233898674));
#111029=CARTESIAN_POINT('Ctrl Pts',(9.63158800698643,11.5738169376985,121.37703187855));
#111030=CARTESIAN_POINT('Ctrl Pts',(9.92874292365523,11.8691743884886,121.319581877576));
#111031=CARTESIAN_POINT('Ctrl Pts',(11.0050331535403,12.859006320224,121.11192815584));
#111032=CARTESIAN_POINT('Ctrl Pts',(11.8386494501844,13.4883431855134,120.952137861313));
#111033=CARTESIAN_POINT('Ctrl Pts',(13.2599293459805,14.3585888964025,120.681820147208));
#111034=CARTESIAN_POINT('Ctrl Pts',(13.8120274687105,14.6536137994961,120.577218345849));
#111035=CARTESIAN_POINT('Ctrl Pts',(14.7577228673034,15.0896958540015,120.398154731455));
#111036=CARTESIAN_POINT('Ctrl Pts',(15.1423785142069,15.2491169886058,120.325302905041));
#111037=CARTESIAN_POINT('Ctrl Pts',(16.5514679300861,15.7693902158067,120.05841558232));
#111038=CARTESIAN_POINT('Ctrl Pts',(17.6050970628226,16.0398471248037,119.859235114274));
#111039=CARTESIAN_POINT('Ctrl Pts',(19.2551233974631,16.2869590738737,119.548520591475));
#111040=CARTESIAN_POINT('Ctrl Pts',(19.8369249065093,16.3414155687272,119.439137578772));
#111041=CARTESIAN_POINT('Ctrl Pts',(20.6204999588461,16.3711961105069,119.291694285519));
#111042=CARTESIAN_POINT('Ctrl Pts',(20.820774550801,16.3750000004889,119.253996228967));
#111043=CARTESIAN_POINT('Ctrl Pts',(21.0210448803799,16.375,119.216269433269));
#111044=CARTESIAN_POINT('Origin',(20.5162416486691,1.37771738462078E-14,
116.353388269));
#111045=CARTESIAN_POINT('',(20.8126670601567,16.375,118.034500130595));
#111046=CARTESIAN_POINT('',(20.8449496768525,16.375,118.217584318235));
#111047=CARTESIAN_POINT('',(20.5162416486691,16.375,116.353388269));
#111048=CARTESIAN_POINT('',(4.53968745634911,0.597925404686674,119.982827120865));
#111049=CARTESIAN_POINT('Ctrl Pts',(20.8126670602263,16.375,118.034500130964));
#111050=CARTESIAN_POINT('Ctrl Pts',(20.9474177181623,16.3749999997303,118.009115888811));
#111051=CARTESIAN_POINT('Ctrl Pts',(21.0821721364041,16.3732779069003,117.983717507935));
#111052=CARTESIAN_POINT('Ctrl Pts',(21.650889271568,16.3587371251268,117.876487402412));
#111053=CARTESIAN_POINT('Ctrl Pts',(22.0842445742341,16.3297758982501,117.794689003852));
#111054=CARTESIAN_POINT('Ctrl Pts',(23.1668893823753,16.2125130218164,117.590352245407));
#111055=CARTESIAN_POINT('Ctrl Pts',(23.8130331065345,16.1016489691972,117.46843539781));
#111056=CARTESIAN_POINT('Ctrl Pts',(25.0341491046181,15.8132717274978,117.238159551688));
#111057=CARTESIAN_POINT('Ctrl Pts',(25.6095397444326,15.6424660168222,117.129705583372));
#111058=CARTESIAN_POINT('Ctrl Pts',(26.5470071663356,15.3053708438713,116.952681815915));
#111059=CARTESIAN_POINT('Ctrl Pts',(26.9148128865843,15.1573802795131,116.883122229806));
#111060=CARTESIAN_POINT('Ctrl Pts',(27.6491346185028,14.8295584874304,116.743865582365));
#111061=CARTESIAN_POINT('Ctrl Pts',(28.0150594719487,14.649065175926,116.674308838569));
#111062=CARTESIAN_POINT('Ctrl Pts',(28.9940906684615,14.1186111085074,116.487988551128));
#111063=CARTESIAN_POINT('Ctrl Pts',(29.5919901526024,13.741562699019,116.373982795026));
#111064=CARTESIAN_POINT('Ctrl Pts',(30.6536029107296,12.9698207503721,116.171234920188));
#111065=CARTESIAN_POINT('Ctrl Pts',(31.1234311515611,12.5859931310865,116.081364469071));
#111066=CARTESIAN_POINT('Ctrl Pts',(31.8825047789103,11.8910228713346,115.935483873129));
#111067=CARTESIAN_POINT('Ctrl Pts',(32.1829490827144,11.5934956373737,115.877512122518));
#111068=CARTESIAN_POINT('Ctrl Pts',(32.7704796731808,10.9642426798957,115.763489259629));
#111069=CARTESIAN_POINT('Ctrl Pts',(33.0564769270319,10.6319385041319,115.707673930753));
#111070=CARTESIAN_POINT('Ctrl Pts',(33.7396809151958,9.77002416324843,115.573769532027));
#111071=CARTESIAN_POINT('Ctrl Pts',(34.1189578101089,9.22672926659155,115.498908795801));
#111072=CARTESIAN_POINT('Ctrl Pts',(34.7808389790396,8.14422413452029,115.367241465105));
#111073=CARTESIAN_POINT('Ctrl Pts',(35.0684069028315,7.6094524801085,115.309538456126));
#111074=CARTESIAN_POINT('Ctrl Pts',(35.4959711448949,6.69653397773241,115.222424356109));
#111075=CARTESIAN_POINT('Ctrl Pts',(35.6527612389367,6.32721504158711,115.19007244426));
#111076=CARTESIAN_POINT('Ctrl Pts',(35.9432324953718,5.56695659646977,115.129078624169));
#111077=CARTESIAN_POINT('Ctrl Pts',(36.0760373863462,5.17597820217734,115.100627313078));
#111078=CARTESIAN_POINT('Ctrl Pts',(36.3982448654725,4.09624968022862,115.030122748054));
#111079=CARTESIAN_POINT('Ctrl Pts',(36.5580338919987,3.39927326271342,114.993367571957));
#111080=CARTESIAN_POINT('Ctrl Pts',(36.7705166607077,2.08939865451389,114.940344142336));
#111081=CARTESIAN_POINT('Ctrl Pts',(36.8350998608482,1.47978730816307,114.921929350359));
#111082=CARTESIAN_POINT('Ctrl Pts',(36.8872918374902,0.441864000461987,
114.900691051595));
#111083=CARTESIAN_POINT('Ctrl Pts',(36.8923008642108,0.0151401879435104,
114.894812474543));
#111084=CARTESIAN_POINT('Ctrl Pts',(36.8690366745017,-0.852944119966995,
114.888489220714));
#111085=CARTESIAN_POINT('Ctrl Pts',(36.8395933574814,-1.29392634435125,
114.88829462536));
#111086=CARTESIAN_POINT('Ctrl Pts',(36.7218128980036,-2.3955976960719,114.895625332039));
#111087=CARTESIAN_POINT('Ctrl Pts',(36.6112698181393,-3.05308114401722,
114.907132961835));
#111088=CARTESIAN_POINT('Ctrl Pts',(36.3247202460831,-4.29561586371514,
114.942699434511));
#111089=CARTESIAN_POINT('Ctrl Pts',(36.1553142818853,-4.88109534446592,
114.965573232676));
#111090=CARTESIAN_POINT('Ctrl Pts',(35.821336386373,-5.83506212042791,115.012739566429));
#111091=CARTESIAN_POINT('Ctrl Pts',(35.6747882667282,-6.20936296421926,
115.033874394396));
#111092=CARTESIAN_POINT('Ctrl Pts',(35.3502756418419,-6.95671011401383,
115.081318820238));
#111093=CARTESIAN_POINT('Ctrl Pts',(35.1716658764011,-7.32915014280427,
115.107778279266));
#111094=CARTESIAN_POINT('Ctrl Pts',(34.6469303075316,-8.32566339425024,
115.186612632623));
#111095=CARTESIAN_POINT('Ctrl Pts',(34.2741404840464,-8.93428141835405,
115.243765521066));
#111096=CARTESIAN_POINT('Ctrl Pts',(33.5114606724523,-10.0149763697651,
115.362689596489));
#111097=CARTESIAN_POINT('Ctrl Pts',(33.1322636807448,-10.4932717967061,
115.422525216352));
#111098=CARTESIAN_POINT('Ctrl Pts',(32.4457934481117,-11.2661462413179,
115.531532998563));
#111099=CARTESIAN_POINT('Ctrl Pts',(32.1519307699161,-11.5720944452931,
115.578353581029));
#111100=CARTESIAN_POINT('Ctrl Pts',(31.5304551765431,-12.1704988814298,
115.677511134126));
#111101=CARTESIAN_POINT('Ctrl Pts',(31.2022803271675,-12.4618419469874,
115.729990948659));
#111102=CARTESIAN_POINT('Ctrl Pts',(30.3511605977657,-13.157921384732,115.866629179193));
#111103=CARTESIAN_POINT('Ctrl Pts',(29.8147497618534,-13.5444390282589,
115.953228827373));
#111104=CARTESIAN_POINT('Ctrl Pts',(28.7461262048072,-14.2191317412877,
116.126696092821));
#111105=CARTESIAN_POINT('Ctrl Pts',(28.2182813178402,-14.5123511853317,
116.212772351232));
#111106=CARTESIAN_POINT('Ctrl Pts',(27.3172276003375,-14.9485462795208,
116.359929449445));
#111107=CARTESIAN_POINT('Ctrl Pts',(26.952716143915,-15.108571457968,116.419497083543));
#111108=CARTESIAN_POINT('Ctrl Pts',(26.2023357266079,-15.4052211718541,
116.542033493345));
#111109=CARTESIAN_POINT('Ctrl Pts',(25.8164345516943,-15.5409494151087,
116.605044034577));
#111110=CARTESIAN_POINT('Ctrl Pts',(24.7507684449807,-15.8705041398745,
116.779259033408));
#111111=CARTESIAN_POINT('Ctrl Pts',(24.0629153966277,-16.0342473494753,
116.891966052128));
#111112=CARTESIAN_POINT('Ctrl Pts',(22.7702818479534,-16.2527089909263,
117.104335257787));
#111113=CARTESIAN_POINT('Ctrl Pts',(22.1687296264827,-16.3195086601159,
117.203378107608));
#111114=CARTESIAN_POINT('Ctrl Pts',(21.144516765698,-16.3745954429001,117.371939026216));
#111115=CARTESIAN_POINT('Ctrl Pts',(20.7234223841939,-16.3805490893052,
117.441193985326));
#111116=CARTESIAN_POINT('Ctrl Pts',(19.8667432377462,-16.3587362640687,
117.581824272215));
#111117=CARTESIAN_POINT('Ctrl Pts',(19.4315384842745,-16.3297739019914,
117.65317635399));
#111118=CARTESIAN_POINT('Ctrl Pts',(18.3443073251155,-16.2125096513466,
117.831447390598));
#111119=CARTESIAN_POINT('Ctrl Pts',(17.6954492902166,-16.1016479997975,
117.937874497409));
#111120=CARTESIAN_POINT('Ctrl Pts',(16.4692356109282,-15.8132764386314,
118.13912913472));
#111121=CARTESIAN_POINT('Ctrl Pts',(15.8914546814622,-15.6424723469864,
118.234010461954));
#111122=CARTESIAN_POINT('Ctrl Pts',(14.9499758033932,-15.3053780972287,
118.388295607853));
#111123=CARTESIAN_POINT('Ctrl Pts',(14.5805561449671,-15.157386173201,118.448728694602));
#111124=CARTESIAN_POINT('Ctrl Pts',(13.8428911356548,-14.8295650756713,
118.569023034157));
#111125=CARTESIAN_POINT('Ctrl Pts',(13.47524898342,-14.6490745110845,118.628814011724));
#111126=CARTESIAN_POINT('Ctrl Pts',(12.4915335346939,-14.1186215561567,
118.788578899634));
#111127=CARTESIAN_POINT('Ctrl Pts',(11.890693774203,-13.7415703986437,118.885943134522));
#111128=CARTESIAN_POINT('Ctrl Pts',(10.8237560746531,-12.9698261634361,
119.058516077216));
#111129=CARTESIAN_POINT('Ctrl Pts',(10.3515254677957,-12.5859998477385,
119.134756035788));
#111130=CARTESIAN_POINT('Ctrl Pts',(9.58833440215207,-11.8910296450469,
119.25729176993));
#111131=CARTESIAN_POINT('Ctrl Pts',(9.28617974718461,-11.5935008973214,
119.30557444827));
#111132=CARTESIAN_POINT('Ctrl Pts',(8.69508359286318,-10.9642484522917,
119.399375287481));
#111133=CARTESIAN_POINT('Ctrl Pts',(8.40724579345633,-10.6319465903103,
119.44474259634));
#111134=CARTESIAN_POINT('Ctrl Pts',(7.71944310032966,-9.77003001425979,
119.552583621157));
#111135=CARTESIAN_POINT('Ctrl Pts',(7.33743167938567,-9.2267299238087,119.611958476547));
#111136=CARTESIAN_POINT('Ctrl Pts',(6.6704303008902,-8.14421801142984,119.714608904431));
#111137=CARTESIAN_POINT('Ctrl Pts',(6.38046891117741,-7.60944513092628,
119.758739882301));
#111138=CARTESIAN_POINT('Ctrl Pts',(5.94889595319164,-6.69652691962459,
119.823114856413));
#111139=CARTESIAN_POINT('Ctrl Pts',(5.79049732980452,-6.32720960975904,
119.846339239568));
#111140=CARTESIAN_POINT('Ctrl Pts',(5.49668262775027,-5.5669508985232,119.888370794844));
#111141=CARTESIAN_POINT('Ctrl Pts',(5.36215542994127,-5.1759705064359,119.907057318389));
#111142=CARTESIAN_POINT('Ctrl Pts',(5.04268487019767,-4.12074621802567,
119.950008615385));
#111143=CARTESIAN_POINT('Ctrl Pts',(4.88425103526154,-3.44916259355946,
119.969665869807));
#111144=CARTESIAN_POINT('Ctrl Pts',(4.67427441302864,-2.2214623544002,119.992076449368));
#111145=CARTESIAN_POINT('Ctrl Pts',(4.60811190145251,-1.66895874402597,
119.997342580495));
#111146=CARTESIAN_POINT('Ctrl Pts',(4.54679574234008,-0.782153931310234,
119.99788609547));
#111147=CARTESIAN_POINT('Ctrl Pts',(4.53381034943788,-0.449528224858523,
119.996321834545));
#111148=CARTESIAN_POINT('Ctrl Pts',(4.5286489093189,0.121525185001767,119.990497869703));
#111149=CARTESIAN_POINT('Ctrl Pts',(4.53161016399367,0.359801506295293,
119.987124333779));
#111150=CARTESIAN_POINT('Ctrl Pts',(4.53968745733423,0.597925404661066,
119.982827121192));
#111151=CARTESIAN_POINT('',(12.1252604242132,13.8967357372103,118.645285943241));
#111152=CARTESIAN_POINT('Origin',(20.6551601908026,1.37771738462078E-14,
117.14123447141));
#111153=CARTESIAN_POINT('Ctrl Pts',(12.1252604242941,13.8967357370058,118.645285942984));
#111154=CARTESIAN_POINT('Ctrl Pts',(11.1597404820724,13.284169320124,118.829378902758));
#111155=CARTESIAN_POINT('Ctrl Pts',(10.2608304550041,12.5690806535172,119.000961473646));
#111156=CARTESIAN_POINT('Ctrl Pts',(9.14198063508577,11.4657858073982,119.216854573139));
#111157=CARTESIAN_POINT('Ctrl Pts',(8.85173726715739,11.1561735043244,119.273187269843));
#111158=CARTESIAN_POINT('Ctrl Pts',(8.18795432151583,10.3900038555159,119.402623091456));
#111159=CARTESIAN_POINT('Ctrl Pts',(7.8262818696854,9.92361049551718,119.473627072773));
#111160=CARTESIAN_POINT('Ctrl Pts',(7.10391730568458,8.87989942007041,119.616258849931));
#111161=CARTESIAN_POINT('Ctrl Pts',(6.75224905246574,8.29746930661533,119.686228287655));
#111162=CARTESIAN_POINT('Ctrl Pts',(6.24680245725592,7.32914896187816,119.788031668799));
#111163=CARTESIAN_POINT('Ctrl Pts',(6.06986816280178,6.95670904209967,119.823992462004));
#111164=CARTESIAN_POINT('Ctrl Pts',(5.74866154596584,6.20936180049674,119.89018632596));
#111165=CARTESIAN_POINT('Ctrl Pts',(5.60374227229688,5.83505890408794,119.920562562136));
#111166=CARTESIAN_POINT('Ctrl Pts',(5.27386443097109,4.88109619671092,119.990972901856));
#111167=CARTESIAN_POINT('Ctrl Pts',(5.10692456055938,4.29561579219025,120.02783470883));
#111168=CARTESIAN_POINT('Ctrl Pts',(4.82554189788938,3.05308386956103,120.092700235354));
#111169=CARTESIAN_POINT('Ctrl Pts',(4.71769400230651,2.39560152362369,120.119494173849));
#111170=CARTESIAN_POINT('Ctrl Pts',(4.60440066759678,1.29392655010024,120.152275258206));
#111171=CARTESIAN_POINT('Ctrl Pts',(4.57674612282201,0.852944098403716,
120.162225201117));
#111172=CARTESIAN_POINT('Ctrl Pts',(4.55699972666702,-0.015140709895495,
120.175852535511));
#111173=CARTESIAN_POINT('Ctrl Pts',(4.56373655386578,-0.441866353833341,
120.179771808684));
#111174=CARTESIAN_POINT('Ctrl Pts',(4.62013871523287,-1.47978496496699,
120.182412432585));
#111175=CARTESIAN_POINT('Ctrl Pts',(4.68720199259863,-2.08939756486391,
120.178062862687));
#111176=CARTESIAN_POINT('Ctrl Pts',(4.90506234807178,-3.39926685260381,
120.155542619496));
#111177=CARTESIAN_POINT('Ctrl Pts',(5.06774326451499,-4.09623968274988,
120.135196923117));
#111178=CARTESIAN_POINT('Ctrl Pts',(5.39452380613574,-5.17597163856225,
120.090625419194));
#111179=CARTESIAN_POINT('Ctrl Pts',(5.5290045520822,-5.56695189759738,120.071675329381));
#111180=CARTESIAN_POINT('Ctrl Pts',(5.82278177455425,-6.32721069485949,
120.02943094923));
#111181=CARTESIAN_POINT('Ctrl Pts',(5.981201450926,-6.69652989050191,120.006320353581));
#111182=CARTESIAN_POINT('Ctrl Pts',(6.41286169276523,-7.60944416923135,
119.942450985857));
#111183=CARTESIAN_POINT('Ctrl Pts',(6.70289680019166,-8.14421798124779,
119.898735768352));
#111184=CARTESIAN_POINT('Ctrl Pts',(7.36994640105912,-9.22672754721024,
119.796367060064));
#111185=CARTESIAN_POINT('Ctrl Pts',(7.75192164063493,-9.77002708947801,
119.736791934498));
#111186=CARTESIAN_POINT('Ctrl Pts',(8.43961838140779,-10.6319465874527,
119.628336841119));
#111187=CARTESIAN_POINT('Ctrl Pts',(8.72740287301182,-10.9642485591961,
119.582666383961));
#111188=CARTESIAN_POINT('Ctrl Pts',(9.31845149407982,-11.5935013725925,
119.488594078722));
#111189=CARTESIAN_POINT('Ctrl Pts',(9.62062669594056,-11.8910313192151,
119.440419583059));
#111190=CARTESIAN_POINT('Ctrl Pts',(10.3839084183464,-12.5859984183609,
119.31841826376));
#111191=CARTESIAN_POINT('Ctrl Pts',(10.8562165720411,-12.9698255988242,
119.242613096732));
#111192=CARTESIAN_POINT('Ctrl Pts',(11.9232076920776,-13.7415667711839,
119.070368167729));
#111193=CARTESIAN_POINT('Ctrl Pts',(12.5240028290975,-14.1186165143113,
118.972771085672));
#111194=CARTESIAN_POINT('Ctrl Pts',(13.5076111657763,-14.6490716247697,
118.812383115556));
#111195=CARTESIAN_POINT('Ctrl Pts',(13.8752084354256,-14.8295630895892,
118.752328316877));
#111196=CARTESIAN_POINT('Ctrl Pts',(14.6128361148113,-15.1573844703328,
118.631821127168));
#111197=CARTESIAN_POINT('Ctrl Pts',(14.9822761825338,-15.3053765391856,
118.571501918693));
#111198=CARTESIAN_POINT('Ctrl Pts',(15.9238394137623,-15.6424696484626,
118.417722887415));
#111199=CARTESIAN_POINT('Ctrl Pts',(16.5016956420056,-15.8132747098046,
118.323257057273));
#111200=CARTESIAN_POINT('Ctrl Pts',(17.7279633038988,-16.1016477112175,
118.122283213894));
#111201=CARTESIAN_POINT('Ctrl Pts',(18.3767910765389,-16.2125104624114,
118.015654863716));
#111202=CARTESIAN_POINT('Ctrl Pts',(19.4639211362957,-16.3297746553102,
117.836768941188));
#111203=CARTESIAN_POINT('Ctrl Pts',(19.8990699440025,-16.3587365764383,
117.765114145799));
#111204=CARTESIAN_POINT('Ctrl Pts',(20.7557012960041,-16.3805491665361,
117.624212435363));
#111205=CARTESIAN_POINT('Ctrl Pts',(21.1768189028637,-16.3745950976222,
117.555065216385));
#111206=CARTESIAN_POINT('Ctrl Pts',(22.2011219655674,-16.3195078331578,
117.387038803892));
#111207=CARTESIAN_POINT('Ctrl Pts',(22.802750521889,-16.2527079846344,117.288430938992));
#111208=CARTESIAN_POINT('Ctrl Pts',(24.0954409527593,-16.0342459459005,
117.076389188818));
#111209=CARTESIAN_POINT('Ctrl Pts',(24.7832551297753,-15.8705021323465,
116.963448374861));
#111210=CARTESIAN_POINT('Ctrl Pts',(25.8488152966293,-15.540945051873,116.788610097004));
#111211=CARTESIAN_POINT('Ctrl Pts',(26.2346668537666,-15.4052175567522,
116.725336512761));
#111212=CARTESIAN_POINT('Ctrl Pts',(26.9850094295564,-15.1085676258394,
116.602587340136));
#111213=CARTESIAN_POINT('Ctrl Pts',(27.3495452913619,-14.9485401179305,
116.543132938794));
#111214=CARTESIAN_POINT('Ctrl Pts',(28.2506846722699,-14.5123456509191,
116.39648174634));
#111215=CARTESIAN_POINT('Ctrl Pts',(28.7786019485646,-14.2191263330367,
116.310821457708));
#111216=CARTESIAN_POINT('Ctrl Pts',(29.8472625934313,-13.5444406910131,
116.137637731149));
#111217=CARTESIAN_POINT('Ctrl Pts',(30.3836297116358,-13.1579298455225,
116.050839028838));
#111218=CARTESIAN_POINT('Ctrl Pts',(31.2346407361918,-12.4618526787663,
115.913587153723));
#111219=CARTESIAN_POINT('Ctrl Pts',(31.5627657366584,-12.170506877048,115.860803629732));
#111220=CARTESIAN_POINT('Ctrl Pts',(32.1841946087007,-11.5721019248384,
115.761374473169));
#111221=CARTESIAN_POINT('Ctrl Pts',(32.4780753003173,-11.2661551418455,
115.714662472521));
#111222=CARTESIAN_POINT('Ctrl Pts',(33.1646366834815,-10.4932858878529,
115.606189000377));
#111223=CARTESIAN_POINT('Ctrl Pts',(33.5439131870178,-10.0149880007349,
115.546787858102));
#111224=CARTESIAN_POINT('Ctrl Pts',(34.3066442306287,-8.93430385228874,
115.428192098782));
#111225=CARTESIAN_POINT('Ctrl Pts',(34.6793873416775,-8.32569826259176,
115.370806625637));
#111226=CARTESIAN_POINT('Ctrl Pts',(35.204016922313,-7.32918503662734,115.291348976133));
#111227=CARTESIAN_POINT('Ctrl Pts',(35.3825852556302,-6.95673636736924,
115.264625178516));
#111228=CARTESIAN_POINT('Ctrl Pts',(35.7070616810594,-6.20938858312028,
115.216967707811));
#111229=CARTESIAN_POINT('Ctrl Pts',(35.8536279703331,-5.83509447451018,
115.19594705851));
#111230=CARTESIAN_POINT('Ctrl Pts',(36.187695220726,-4.88113555837382,115.149285921989));
#111231=CARTESIAN_POINT('Ctrl Pts',(36.3571779127582,-4.2956496577634,115.126827433441));
#111232=CARTESIAN_POINT('Ctrl Pts',(36.6437871634858,-3.05308112414139,
115.091541124607));
#111233=CARTESIAN_POINT('Ctrl Pts',(36.7542996631356,-2.39556702471343,
115.079832600655));
#111234=CARTESIAN_POINT('Ctrl Pts',(36.8719698247605,-1.29387380383542,
115.071888789447));
#111235=CARTESIAN_POINT('Ctrl Pts',(36.9013575233924,-0.852905371791337,
115.071780486834));
#111236=CARTESIAN_POINT('Ctrl Pts',(36.9245725434912,0.015177219437159,
115.077832544763));
#111237=CARTESIAN_POINT('Ctrl Pts',(36.9195812409251,0.441914723418851,
115.083819955621));
#111238=CARTESIAN_POINT('Ctrl Pts',(36.8674797434211,1.47983695648695,115.105592757666));
#111239=CARTESIAN_POINT('Ctrl Pts',(36.8029723157261,2.08944135597091,115.124442549207));
#111240=CARTESIAN_POINT('Ctrl Pts',(36.5905415507011,3.39933341551244,115.17779451164));
#111241=CARTESIAN_POINT('Ctrl Pts',(36.4307022732685,4.09633627939259,115.214318174334));
#111242=CARTESIAN_POINT('Ctrl Pts',(36.1083746625847,5.17607061333654,115.2842020038));
#111243=CARTESIAN_POINT('Ctrl Pts',(35.9755291125928,5.56702517943654,115.312388455803));
#111244=CARTESIAN_POINT('Ctrl Pts',(35.6850189760879,6.32728056310422,115.373169684351));
#111245=CARTESIAN_POINT('Ctrl Pts',(35.5282377047074,6.69662068296697,115.405637822536));
#111246=CARTESIAN_POINT('Ctrl Pts',(35.1007551184061,7.60953870969189,115.493258627251));
#111247=CARTESIAN_POINT('Ctrl Pts',(34.8132641225272,8.14429674990551,115.551376637967));
#111248=CARTESIAN_POINT('Ctrl Pts',(34.1514769290961,9.22671906732955,115.683316502601));
#111249=CARTESIAN_POINT('Ctrl Pts',(33.7722108273899,9.76995177071023,115.757967809877));
#111250=CARTESIAN_POINT('Ctrl Pts',(33.0889311609431,10.6318425093477,115.891252325604));
#111251=CARTESIAN_POINT('Ctrl Pts',(32.8028605527277,10.9641742629319,115.946768419396));
#111252=CARTESIAN_POINT('Ctrl Pts',(32.2152803445484,11.5934336842087,116.060520228445));
#111253=CARTESIAN_POINT('Ctrl Pts',(31.914875607173,11.8909441565963,116.118596438801));
#111254=CARTESIAN_POINT('Ctrl Pts',(31.1559123088391,12.5859119951017,116.265007843428));
#111255=CARTESIAN_POINT('Ctrl Pts',(30.6861477754281,12.9697559499969,116.355315778851));
#111256=CARTESIAN_POINT('Ctrl Pts',(29.624646174555,13.7414677420151,116.558380839602));
#111257=CARTESIAN_POINT('Ctrl Pts',(29.0267769981518,14.1184821586303,116.672139714958));
#111258=CARTESIAN_POINT('Ctrl Pts',(28.0476542264764,14.6489515843629,116.857834058432));
#111259=CARTESIAN_POINT('Ctrl Pts',(27.6816277312548,14.8294783740573,116.927137694783));
#111260=CARTESIAN_POINT('Ctrl Pts',(26.9472648962211,15.1573087139211,117.066182193985));
#111261=CARTESIAN_POINT('Ctrl Pts',(26.5795327025556,15.3052833195346,117.135845559782));
#111262=CARTESIAN_POINT('Ctrl Pts',(25.6421822967489,15.642388302828,117.313369407985));
#111263=CARTESIAN_POINT('Ctrl Pts',(25.066829375572,15.8132141715895,117.422245999975));
#111264=CARTESIAN_POINT('Ctrl Pts',(23.8455348165031,16.1016601203548,117.652846543175));
#111265=CARTESIAN_POINT('Ctrl Pts',(23.1991565265732,16.2125536994563,117.774600442061));
#111266=CARTESIAN_POINT('Ctrl Pts',(22.1162847810566,16.3298002668299,117.978345738686));
#111267=CARTESIAN_POINT('Ctrl Pts',(21.6829642090882,16.358747623884,118.059824454681));
#111268=CARTESIAN_POINT('Ctrl Pts',(21.1143561097026,16.3732792260656,118.166847129352));
#111269=CARTESIAN_POINT('Ctrl Pts',(20.9796486377732,16.375000000269,118.192209814351));
#111270=CARTESIAN_POINT('Ctrl Pts',(20.8449496767831,16.375,118.217584317867));
#111271=CARTESIAN_POINT('Ctrl Pts',(1.80489434143683,2.28935384663574E-14,
119.652703644671));
#111272=CARTESIAN_POINT('Ctrl Pts',(1.80489434143683,-19.,119.652703644671));
#111273=CARTESIAN_POINT('Ctrl Pts',(20.5162416486687,-19.,116.353388268999));
#111274=CARTESIAN_POINT('Ctrl Pts',(39.2275889559007,-19.,113.054072893327));
#111275=CARTESIAN_POINT('Ctrl Pts',(39.2275889559007,2.28935384663574E-14,
113.054072893327));
#111276=CARTESIAN_POINT('Ctrl Pts',(39.2275889559007,19.0000000000001,113.054072893327));
#111277=CARTESIAN_POINT('Ctrl Pts',(20.5162416486688,19.0000000000001,116.353388268999));
#111278=CARTESIAN_POINT('Ctrl Pts',(1.80489434143685,19.0000000000001,119.652703644671));
#111279=CARTESIAN_POINT('Ctrl Pts',(1.80489434143683,2.28935384663574E-14,
119.652703644671));
#111280=CARTESIAN_POINT('Ctrl Pts',(2.8899419709034,4.93317397042308E-15,
125.818834058975));
#111281=CARTESIAN_POINT('Ctrl Pts',(2.8899419709034,-19.0021739918144,125.818834058975));
#111282=CARTESIAN_POINT('Ctrl Pts',(21.6034302421291,-19.0021739918144,
122.519141173586));
#111283=CARTESIAN_POINT('Ctrl Pts',(40.3169185133548,-19.0021739918144,
119.219448288197));
#111284=CARTESIAN_POINT('Ctrl Pts',(40.3169185133548,4.93317397042304E-15,
119.219448288197));
#111285=CARTESIAN_POINT('Ctrl Pts',(40.3169185133548,19.0021739918144,119.219448288197));
#111286=CARTESIAN_POINT('Ctrl Pts',(21.6034302421291,19.0021739918144,122.519141173586));
#111287=CARTESIAN_POINT('Ctrl Pts',(2.88994197090342,19.0021739918144,125.818834058975));
#111288=CARTESIAN_POINT('Ctrl Pts',(2.8899419709034,4.93317397042308E-15,
125.818834058975));
#111289=CARTESIAN_POINT('Ctrl Pts',(6.3506918559717,-1.15304933939532E-14,
131.036276236652));
#111290=CARTESIAN_POINT('Ctrl Pts',(6.35069185597169,-16.4999999999995,
131.036276236652));
#111291=CARTESIAN_POINT('Ctrl Pts',(22.6000197806726,-16.4999999999995,
128.171081305148));
#111292=CARTESIAN_POINT('Ctrl Pts',(38.8493477053735,-16.4999999999995,
125.305886373643));
#111293=CARTESIAN_POINT('Ctrl Pts',(38.8493477053735,-1.15304933939532E-14,
125.305886373643));
#111294=CARTESIAN_POINT('Ctrl Pts',(38.8493477053735,16.4999999999995,125.305886373643));
#111295=CARTESIAN_POINT('Ctrl Pts',(22.6000197806726,16.4999999999995,128.171081305148));
#111296=CARTESIAN_POINT('Ctrl Pts',(6.35069185597171,16.4999999999995,131.036276236652));
#111297=CARTESIAN_POINT('Ctrl Pts',(6.3506918559717,-1.15304933939532E-14,
131.036276236652));
#111298=CARTESIAN_POINT('',(6.35069185597038,-1.35511606125414E-14,131.036276236651));
#111299=CARTESIAN_POINT('Origin',(22.6000197806719,1.4210854715202E-14,
128.171081305147));
#111300=CARTESIAN_POINT('',(1.80489434143704,2.05667095479774E-14,119.652703644671));
#111301=CARTESIAN_POINT('Origin',(31.3509340513116,2.42107666709492E-14,
114.453517413878));
#111302=CARTESIAN_POINT('Origin',(20.5162416486691,1.4210854715202E-14,
116.353388269));
#111303=CARTESIAN_POINT('Origin',(11.833832765324,1.4210854715202E-14,67.1130006183894));
#111304=CARTESIAN_POINT('',(30.8903745807654,6.7681155228249,63.7528181373285));
#111305=CARTESIAN_POINT('',(30.8903812387965,-6.76809619335572,63.752816963338));
#111306=CARTESIAN_POINT('Origin',(11.833832765324,1.4210854715202E-14,67.1130006183894));
#111307=CARTESIAN_POINT('',(29.6607179812714,9.94038463627826,64.9669467867612));
#111308=CARTESIAN_POINT('Ctrl Pts',(29.6610694362665,9.94001765225634,64.9677683546378));
#111309=CARTESIAN_POINT('Ctrl Pts',(29.8626606590662,9.4922765200743,64.6815301868754));
#111310=CARTESIAN_POINT('Ctrl Pts',(30.0620247360424,9.02635699468926,64.4486981628682));
#111311=CARTESIAN_POINT('Ctrl Pts',(30.4831429543247,7.96380978435469,64.036809917008));
#111312=CARTESIAN_POINT('Ctrl Pts',(30.6973043635228,7.37286267557426,63.8759507130258));
#111313=CARTESIAN_POINT('Ctrl Pts',(30.8903745807654,6.76811552282492,63.7528181373285));
#111314=CARTESIAN_POINT('',(29.4810298430695,10.3418191817547,65.2638887238806));
#111315=CARTESIAN_POINT('Ctrl Pts',(29.4810568782271,10.3417884885121,65.2639387748332));
#111316=CARTESIAN_POINT('Ctrl Pts',(29.5093629970405,10.277887407849,65.2094624539339));
#111317=CARTESIAN_POINT('Ctrl Pts',(29.5383983492446,10.212682227821,65.157394501546));
#111318=CARTESIAN_POINT('Ctrl Pts',(29.5982881786419,10.0787826880955,65.0578607606596));
#111319=CARTESIAN_POINT('Ctrl Pts',(29.6289217697167,10.0105820158188,65.0107648292185));
#111320=CARTESIAN_POINT('Ctrl Pts',(29.6603665235238,9.94075156122962,64.9661252283734));
#111321=CARTESIAN_POINT('',(27.2015660631669,14.9604792914755,73.5557281547034));
#111322=CARTESIAN_POINT('Ctrl Pts',(27.2015705014209,14.9604739009962,73.5557285683884));
#111323=CARTESIAN_POINT('Ctrl Pts',(27.1654392493044,14.8743896900466,72.8216543486108));
#111324=CARTESIAN_POINT('Ctrl Pts',(27.2634348909743,14.6533579394755,72.0350130048608));
#111325=CARTESIAN_POINT('Ctrl Pts',(27.5421046041987,14.1098263590445,70.5236291817684));
#111326=CARTESIAN_POINT('Ctrl Pts',(27.7602914012229,13.7295898281507,69.7103575348371));
#111327=CARTESIAN_POINT('Ctrl Pts',(28.4255514554632,12.52946564147,67.586530187656));
#111328=CARTESIAN_POINT('Ctrl Pts',(28.9609479436267,11.5159364690254,66.2649476939623));
#111329=CARTESIAN_POINT('Ctrl Pts',(29.4810028050673,10.3418498799905,65.2638386757534));
#111330=CARTESIAN_POINT('',(27.2861971804113,14.998680114819,74.2711694581623));
#111331=CARTESIAN_POINT('Ctrl Pts',(27.2015616815609,14.9604819552268,73.5557280582404));
#111332=CARTESIAN_POINT('Ctrl Pts',(27.2121892020169,14.9857764789281,73.7714865315729));
#111333=CARTESIAN_POINT('Ctrl Pts',(27.236302938614,14.998378496898,73.9863406668699));
#111334=CARTESIAN_POINT('Ctrl Pts',(27.2778506876385,14.998378496898,74.2219696605585));
#111335=CARTESIAN_POINT('Ctrl Pts',(27.2823600271523,14.9982089721856,74.2464956078967));
#111336=CARTESIAN_POINT('Ctrl Pts',(27.2870497423904,14.9978696111192,74.2709950325846));
#111337=CARTESIAN_POINT('',(27.6070995425304,14.9199507410733,75.6071390537838));
#111338=CARTESIAN_POINT('Ctrl Pts',(27.2853446200354,14.9994906183976,74.2713438920009));
#111339=CARTESIAN_POINT('Ctrl Pts',(27.3712939315444,14.9932698714981,74.7203331224154));
#111340=CARTESIAN_POINT('Ctrl Pts',(27.4789460295974,14.9667633499927,75.1665245541753));
#111341=CARTESIAN_POINT('Ctrl Pts',(27.6070861523114,14.9199505879433,75.6071429300643));
#111342=CARTESIAN_POINT('',(28.5837286483844,14.4236088234574,78.2159945046497));
#111343=CARTESIAN_POINT('Ctrl Pts',(28.5837271422992,14.4236103938593,78.2159956036932));
#111344=CARTESIAN_POINT('Ctrl Pts',(28.3970080708632,14.5362294106934,77.799204136978));
#111345=CARTESIAN_POINT('Ctrl Pts',(28.2181098367699,14.6364962450901,77.3714384121405));
#111346=CARTESIAN_POINT('Ctrl Pts',(27.8891286847039,14.8042078675273,76.5021371343503));
#111347=CARTESIAN_POINT('Ctrl Pts',(27.738486650416,14.8719150396164,76.0587797395723));
#111348=CARTESIAN_POINT('Ctrl Pts',(27.6071124825729,14.9199244469508,75.6071324936865));
#111349=CARTESIAN_POINT('',(29.8215734155925,13.2678234653359,79.1320791187414));
#111350=CARTESIAN_POINT('Ctrl Pts',(28.5837298611721,14.4236073308178,78.2159935579633));
#111351=CARTESIAN_POINT('Ctrl Pts',(28.633171177856,14.3937861564346,78.3263512175926));
#111352=CARTESIAN_POINT('Ctrl Pts',(28.6946666043271,14.3500018857306,78.4264750537417));
#111353=CARTESIAN_POINT('Ctrl Pts',(28.8785087936175,14.2067869650545,78.6665485169518));
#111354=CARTESIAN_POINT('Ctrl Pts',(29.0141762283142,14.0893218683042,78.7878804462047));
#111355=CARTESIAN_POINT('Ctrl Pts',(29.2616910886977,13.8583103887882,78.9544730956887));
#111356=CARTESIAN_POINT('Ctrl Pts',(29.3748367764198,13.7470705966664,79.0119053447665));
#111357=CARTESIAN_POINT('Ctrl Pts',(29.5992739331012,13.5150320471622,79.0951625262152));
#111358=CARTESIAN_POINT('Ctrl Pts',(29.7118528383796,13.3929287157044,79.1214954015636));
#111359=CARTESIAN_POINT('Ctrl Pts',(29.8215734564531,13.2678235744527,79.1320799848902));
#111360=CARTESIAN_POINT('',(30.1098517192201,12.9238074747324,79.1218447623392));
#111361=CARTESIAN_POINT('Ctrl Pts',(29.8215733551035,13.2678233399104,79.1320782633696));
#111362=CARTESIAN_POINT('Ctrl Pts',(29.9225981941962,13.15263341247,79.14182474059));
#111363=CARTESIAN_POINT('Ctrl Pts',(30.0199654553166,13.0361914615023,79.1376939286814));
#111364=CARTESIAN_POINT('Ctrl Pts',(30.1098481430753,12.92381190166,79.1218451857309));
#111365=CARTESIAN_POINT('',(33.6423066138275,6.32455532063251,78.4989774482698));
#111366=CARTESIAN_POINT('Origin',(14.4385554303262,1.4210854715202E-14,
81.8851169135651));
#111367=CARTESIAN_POINT('',(33.6423066138211,-6.32455532067118,78.4989774483005));
#111368=CARTESIAN_POINT('Ctrl Pts',(33.6423066139704,6.3245553206325,78.49897744908));
#111369=CARTESIAN_POINT('Ctrl Pts',(33.6665909588537,6.24852627328648,78.4946954638666));
#111370=CARTESIAN_POINT('Ctrl Pts',(33.6906077282209,6.17214997068385,78.4910778646682));
#111371=CARTESIAN_POINT('Ctrl Pts',(33.9161865198445,5.44288016546143,78.4625119450618));
#111372=CARTESIAN_POINT('Ctrl Pts',(34.096465981114,4.76669862057734,78.4810806785018));
#111373=CARTESIAN_POINT('Ctrl Pts',(34.3912241285691,3.39678433761039,78.5498773566916));
#111374=CARTESIAN_POINT('Ctrl Pts',(34.5056891678386,2.70299030631043,78.6000742831831));
#111375=CARTESIAN_POINT('Ctrl Pts',(34.6569683004298,1.33087702156853,78.6768075863797));
#111376=CARTESIAN_POINT('Ctrl Pts',(34.6934420688607,0.65241734777343,78.7014923606593));
#111377=CARTESIAN_POINT('Ctrl Pts',(34.6934420688607,1.33226762955019E-14,
78.7014923606593));
#111378=CARTESIAN_POINT('Ctrl Pts',(34.6934420688607,-0.652417347773404,
78.7014923606593));
#111379=CARTESIAN_POINT('Ctrl Pts',(34.6569683004298,-1.3308770215685,78.6768075863797));
#111380=CARTESIAN_POINT('Ctrl Pts',(34.5056891678386,-2.70299030631041,
78.6000742831831));
#111381=CARTESIAN_POINT('Ctrl Pts',(34.3912241285691,-3.39678433761036,
78.5498773566916));
#111382=CARTESIAN_POINT('Ctrl Pts',(34.096465981114,-4.76669862057732,78.4810806785018));
#111383=CARTESIAN_POINT('Ctrl Pts',(33.9161865198445,-5.4428801654614,78.4625119450618));
#111384=CARTESIAN_POINT('Ctrl Pts',(33.6906077282169,-6.17214997069675,
78.4910778646687));
#111385=CARTESIAN_POINT('Ctrl Pts',(33.6665909588457,-6.24852627331219,
78.4946954638678));
#111386=CARTESIAN_POINT('Ctrl Pts',(33.6423066139581,-6.3245553206709,78.4989774490822));
#111387=CARTESIAN_POINT('',(30.109851949332,-12.9238077427022,79.1218473206622));
#111388=CARTESIAN_POINT('Origin',(14.4385554303262,1.4210854715202E-14,
81.8851169135651));
#111389=CARTESIAN_POINT('',(29.8216059073926,-13.2677862231535,79.1320814034235));
#111390=CARTESIAN_POINT('Ctrl Pts',(30.1098481430752,-12.92381190166,79.1218451857304));
#111391=CARTESIAN_POINT('Ctrl Pts',(30.0199751912077,-13.0361794164536,
79.1376925283409));
#111392=CARTESIAN_POINT('Ctrl Pts',(29.9226191337965,-13.1526083961398,
79.1418238949043));
#111393=CARTESIAN_POINT('Ctrl Pts',(29.8216059073926,-13.2677862231535,
79.1320814034235));
#111394=CARTESIAN_POINT('',(28.5838100706278,-14.4235289931938,78.2160017787004));
#111395=CARTESIAN_POINT('Ctrl Pts',(29.8216061616813,-13.2677868117196,
79.1320857232078));
#111396=CARTESIAN_POINT('Ctrl Pts',(29.7118038601082,-13.3929843766212,
79.1214868546364));
#111397=CARTESIAN_POINT('Ctrl Pts',(29.5991328833806,-13.5151805798363,
79.0951067676584));
#111398=CARTESIAN_POINT('Ctrl Pts',(29.3745120791704,-13.7473861843611,
79.0116991693966));
#111399=CARTESIAN_POINT('Ctrl Pts',(29.2612652340829,-13.8587081819794,
78.9541551381127));
#111400=CARTESIAN_POINT('Ctrl Pts',(29.0138299095263,-14.0895961234492,
78.7874271059373));
#111401=CARTESIAN_POINT('Ctrl Pts',(28.8783329260922,-14.2068946013881,
78.666154980642));
#111402=CARTESIAN_POINT('Ctrl Pts',(28.6947017762484,-14.3499295063546,
78.4262685171615));
#111403=CARTESIAN_POINT('Ctrl Pts',(28.6332644595127,-14.3936694520259,
78.3262180844277));
#111404=CARTESIAN_POINT('Ctrl Pts',(28.5838650340229,-14.4234670709579,
78.2159604183534));
#111405=CARTESIAN_POINT('',(27.60718386578,-14.9199168893285,75.6074591138482));
#111406=CARTESIAN_POINT('Ctrl Pts',(27.6071889912212,-14.9199064677107,
75.6074565146134));
#111407=CARTESIAN_POINT('Ctrl Pts',(27.7385049392646,-14.871907393202,76.0588374809969));
#111408=CARTESIAN_POINT('Ctrl Pts',(27.8893213549521,-14.8041048629894,
76.502615799427));
#111409=CARTESIAN_POINT('Ctrl Pts',(28.2182237838036,-14.6364415875546,
77.3717619195238));
#111410=CARTESIAN_POINT('Ctrl Pts',(28.3970555586945,-14.53619934482,77.7993003034521));
#111411=CARTESIAN_POINT('Ctrl Pts',(28.5837551075604,-14.4235909146646,
78.2160431338438));
#111412=CARTESIAN_POINT('',(27.286197390388,-14.9986800996203,74.2711705550149));
#111413=CARTESIAN_POINT('Ctrl Pts',(27.607178555543,-14.9199168285301,75.6074606516617));
#111414=CARTESIAN_POINT('Ctrl Pts',(27.4789995375747,-14.9667499667782,
75.1667448437143));
#111415=CARTESIAN_POINT('Ctrl Pts',(27.3713177919504,-14.9932681141233,
74.7204575783766));
#111416=CARTESIAN_POINT('Ctrl Pts',(27.2853448300283,-14.9994906031988,
74.2713449889783));
#111417=CARTESIAN_POINT('',(27.2015513600941,-14.9604539661155,73.555495291127));
#111418=CARTESIAN_POINT('Ctrl Pts',(27.2870499522845,-14.9978695959315,
74.2709961290926));
#111419=CARTESIAN_POINT('Ctrl Pts',(27.2823583510579,-14.998209098153,74.246486880775));
#111420=CARTESIAN_POINT('Ctrl Pts',(27.2778490441633,-14.998378496899,74.2219603399536));
#111421=CARTESIAN_POINT('Ctrl Pts',(27.2735220998427,-14.998378496899,74.1974210192936));
#111422=CARTESIAN_POINT('Ctrl Pts',(27.2361828882004,-14.998378496899,73.9856598271479));
#111423=CARTESIAN_POINT('Ctrl Pts',(27.2121477368108,-14.9857096904479,
73.7708402126313));
#111424=CARTESIAN_POINT('Ctrl Pts',(27.2015502202211,-14.9604546588834,
73.5554952659763));
#111425=CARTESIAN_POINT('',(29.4810598079121,-10.3417456735051,65.2638113433947));
#111426=CARTESIAN_POINT('Ctrl Pts',(29.4810610160957,-10.3417443046597,
65.2638135766404));
#111427=CARTESIAN_POINT('Ctrl Pts',(28.9598726194414,-11.518367656918,66.266975312665));
#111428=CARTESIAN_POINT('Ctrl Pts',(28.4243894486928,-12.5316424744244,
67.5898019444641));
#111429=CARTESIAN_POINT('Ctrl Pts',(27.758603110063,-13.7325957068466,69.7160102001576));
#111430=CARTESIAN_POINT('Ctrl Pts',(27.5414584630106,-14.1111311675135,
70.5272572949658));
#111431=CARTESIAN_POINT('Ctrl Pts',(27.2515878014758,-14.6764247608876,
72.0991554516062));
#111432=CARTESIAN_POINT('Ctrl Pts',(27.1675460400784,-14.879596606879,72.8656112330152));
#111433=CARTESIAN_POINT('Ctrl Pts',(27.2015525140621,-14.9604525641422,
73.5554953985588));
#111434=CARTESIAN_POINT('',(29.6609510243113,-9.94007378487892,64.9665024957973));
#111435=CARTESIAN_POINT('Ctrl Pts',(29.6605379238539,-9.94033539790784,
64.9657684968317));
#111436=CARTESIAN_POINT('Ctrl Pts',(29.6290590195802,-10.0102283533256,
65.0104017735973));
#111437=CARTESIAN_POINT('Ctrl Pts',(29.5983883914081,-10.0784994646189,
65.0575068363893));
#111438=CARTESIAN_POINT('Ctrl Pts',(29.5384375241501,-10.2125277434113,
65.1571032917546));
#111439=CARTESIAN_POINT('Ctrl Pts',(29.5093737895855,-10.2778012664117,
65.2092349779954));
#111440=CARTESIAN_POINT('Ctrl Pts',(29.4810586060414,-10.3417470414456,
65.2638091169701));
#111441=CARTESIAN_POINT('Ctrl Pts',(30.8903812387965,-6.76809619335574,
63.752816963338));
#111442=CARTESIAN_POINT('Ctrl Pts',(30.7097331720569,-7.33393380168619,
63.8680233812832));
#111443=CARTESIAN_POINT('Ctrl Pts',(30.5107179020567,-7.88750373573765,
64.0162157526285));
#111444=CARTESIAN_POINT('Ctrl Pts',(30.0922727058573,-8.95553598274615,
64.4139142005288));
#111445=CARTESIAN_POINT('Ctrl Pts',(29.8782495861902,-9.45763958307992,
64.6594445903658));
#111446=CARTESIAN_POINT('Ctrl Pts',(29.6612765321668,-9.93956440248096,
64.9674957905432));
#111447=CARTESIAN_POINT('Origin',(24.4068934345791,10.33198790001,60.67496948644));
#111448=CARTESIAN_POINT('',(24.9372762730815,10.3319816626968,59.2718678127106));
#111449=CARTESIAN_POINT('',(25.4229129967449,10.8757238874463,59.714731596499));
#111450=CARTESIAN_POINT('Origin',(24.4069004573991,10.33198058441,60.67497202932));
#111451=CARTESIAN_POINT('',(23.4739833876933,11.4523981580514,60.322322782081));
#111452=CARTESIAN_POINT('Origin',(24.4068934345791,10.33198790001,60.67496948644));
#111453=CARTESIAN_POINT('',(25.5799750648999,11.2436334983186,60.4681263249483));
#111454=CARTESIAN_POINT('Origin',(24.4069004573991,10.33198058441,60.67497202932));
#111455=CARTESIAN_POINT('',(22.9296818101862,10.3319887778349,60.9354417820097));
#111456=CARTESIAN_POINT('Origin',(24.4068934339491,10.33198915989,60.67496948286));
#111457=CARTESIAN_POINT('Origin',(24.4068932609991,10.33198790252,60.67496850203));
#111458=CARTESIAN_POINT('Origin',(6.43246351666909,-92.5,72.98888938658));
#111459=CARTESIAN_POINT('',(16.5158721300291,-92.,68.592883160925));
#111460=CARTESIAN_POINT('',(16.5158721300291,-92.,77.384895612235));
#111461=CARTESIAN_POINT('Origin',(6.43246351666909,-92.,72.98888938658));
#111462=CARTESIAN_POINT('',(16.5158709386063,-25.6802783436,68.5928804239554));
#111463=CARTESIAN_POINT('',(16.5158709400891,-25.6802783436,68.592880423309));
#111464=CARTESIAN_POINT('',(17.4324750363818,-25.5800482337938,72.9889222937213));
#111465=CARTESIAN_POINT('Ctrl Pts',(17.4324635166199,-25.5800482332938,
72.9889222889149));
#111466=CARTESIAN_POINT('Ctrl Pts',(17.4324645777424,-25.5354140613111,
72.6341648714431));
#111467=CARTESIAN_POINT('Ctrl Pts',(17.4152996369824,-25.5033048623799,
72.2793470851132));
#111468=CARTESIAN_POINT('Ctrl Pts',(17.3809768139068,-25.4836548570278,
71.9258481925477));
#111469=CARTESIAN_POINT('Ctrl Pts',(17.3480073399888,-25.4647796515264,
71.5862877638267));
#111470=CARTESIAN_POINT('Ctrl Pts',(17.2992064827594,-25.4574004780469,
71.2479437277912));
#111471=CARTESIAN_POINT('Ctrl Pts',(17.2346272733976,-25.4614590353976,
70.9120508823093));
#111472=CARTESIAN_POINT('Ctrl Pts',(17.1719357280398,-25.4653989602551,
70.5859762560326));
#111473=CARTESIAN_POINT('Ctrl Pts',(17.0943746508061,-25.4801177337986,
70.2622112095332));
#111474=CARTESIAN_POINT('Ctrl Pts',(17.0020368595677,-25.5055620193224,
69.9419040979565));
#111475=CARTESIAN_POINT('Ctrl Pts',(16.9137689448968,-25.5298848235974,
69.6357148290351));
#111476=CARTESIAN_POINT('Ctrl Pts',(16.8119981402997,-25.5640085017763,
69.3326851862224));
#111477=CARTESIAN_POINT('Ctrl Pts',(16.6968477217908,-25.6078864634696,
69.0338398433192));
#111478=CARTESIAN_POINT('Ctrl Pts',(16.6397990529275,-25.6296248065816,
68.8857836813928));
#111479=CARTESIAN_POINT('Ctrl Pts',(16.5794670519359,-25.6537573217834,
68.7387549080006));
#111480=CARTESIAN_POINT('Ctrl Pts',(16.5158709370957,-25.6802783436,68.592880424614));
#111481=CARTESIAN_POINT('',(16.5158721346073,-26.62691877498,77.3848956151154));
#111482=CARTESIAN_POINT('Ctrl Pts',(16.5158721453875,-26.6269187749801,
77.3848956198152));
#111483=CARTESIAN_POINT('Ctrl Pts',(16.8127630709596,-26.408358380933,76.703897373734));
#111484=CARTESIAN_POINT('Ctrl Pts',(17.0412431892719,-26.1956003393225,
75.9870348538324));
#111485=CARTESIAN_POINT('Ctrl Pts',(17.1956813601443,-26.0131972847863,
75.2521770695883));
#111486=CARTESIAN_POINT('Ctrl Pts',(17.3501194912107,-25.8307942772641,
74.5173194747521));
#111487=CARTESIAN_POINT('Ctrl Pts',(17.4305157170817,-25.6787462270838,
73.7644666170394));
#111488=CARTESIAN_POINT('Ctrl Pts',(17.4324409979989,-25.5828615251574,
73.0111529932187));
#111489=CARTESIAN_POINT('Ctrl Pts',(17.4324599365955,-25.5819183268572,
73.0037428004011));
#111490=CARTESIAN_POINT('Ctrl Pts',(17.432471282139,-25.5809805630684,72.9963325629999));
#111491=CARTESIAN_POINT('Ctrl Pts',(17.4324750363818,-25.5800482337938,
72.9889222937213));
#111492=CARTESIAN_POINT('',(16.5158721336291,-26.62691877498,77.384895614689));
#111493=CARTESIAN_POINT('Origin',(82.8534541851791,9.38083151964701,62.64107301909));
#111494=CARTESIAN_POINT('',(83.1139265236516,9.38085957612367,64.1182846358727));
#111495=CARTESIAN_POINT('',(84.3306658152022,9.38085639185424,62.3806007557379));
#111496=CARTESIAN_POINT('Origin',(82.8534541851791,9.38088126242801,62.64107301909));
#111497=CARTESIAN_POINT('',(83.9303998448743,8.3540709653061,62.4514288517342));
#111498=CARTESIAN_POINT('Ctrl Pts',(84.3306658154406,9.38085639185472,62.3806007579587));
#111499=CARTESIAN_POINT('Ctrl Pts',(84.3306679192988,9.34196946191789,62.3806089762619));
#111500=CARTESIAN_POINT('Ctrl Pts',(84.3291773724665,9.30344979713916,62.3808354481103));
#111501=CARTESIAN_POINT('Ctrl Pts',(84.3262566203095,9.26521743471116,62.3812916153508));
#111502=CARTESIAN_POINT('Ctrl Pts',(84.3233100507629,9.22664712515764,62.381751814788));
#111503=CARTESIAN_POINT('Ctrl Pts',(84.3189078623632,9.18836848325348,62.3824457913877));
#111504=CARTESIAN_POINT('Ctrl Pts',(84.3130622625201,9.15029712543912,62.3833944459789));
#111505=CARTESIAN_POINT('Ctrl Pts',(84.3072340119843,9.11233876059393,62.3843402850336));
#111506=CARTESIAN_POINT('Ctrl Pts',(84.2999707739129,9.07458573152475,62.385539315736));
#111507=CARTESIAN_POINT('Ctrl Pts',(84.2912345465586,9.0369630513843,62.3870210874909));
#111508=CARTESIAN_POINT('Ctrl Pts',(84.2826299686156,8.99990732119721,62.3884805298844));
#111509=CARTESIAN_POINT('Ctrl Pts',(84.2725962251058,8.96297738491442,62.3902142976612));
#111510=CARTESIAN_POINT('Ctrl Pts',(84.2610511945124,8.92612011196809,62.3922587022747));
#111511=CARTESIAN_POINT('Ctrl Pts',(84.253721429992,8.90271998934595,62.3935566637032));
#111512=CARTESIAN_POINT('Ctrl Pts',(84.2457815887353,8.87934955357341,62.3949799965243));
#111513=CARTESIAN_POINT('Ctrl Pts',(84.2372015097695,8.85600103677115,62.3965396057256));
#111514=CARTESIAN_POINT('Ctrl Pts',(84.2213960220003,8.81299039570091,62.3994125844308));
#111515=CARTESIAN_POINT('Ctrl Pts',(84.2033988237252,8.77003483830633,62.4026755011808));
#111516=CARTESIAN_POINT('Ctrl Pts',(84.1830317439484,8.72727946222033,62.4063534010779));
#111517=CARTESIAN_POINT('Ctrl Pts',(84.1641545930883,8.6876518036017,62.4097622486872));
#111518=CARTESIAN_POINT('Ctrl Pts',(84.1432409919603,8.64819608240158,62.4135276940112));
#111519=CARTESIAN_POINT('Ctrl Pts',(84.1201358387748,8.60907405684465,62.4176720128793));
#111520=CARTESIAN_POINT('Ctrl Pts',(84.0976541007213,8.57100760804725,62.4217045111906));
#111521=CARTESIAN_POINT('Ctrl Pts',(84.0730969576522,8.53325678692265,62.426095805446));
#111522=CARTESIAN_POINT('Ctrl Pts',(84.046316430218,8.49601897319737,62.4308673152347));
#111523=CARTESIAN_POINT('Ctrl Pts',(84.0205599190037,8.46020503453727,62.4354563751659));
#111524=CARTESIAN_POINT('Ctrl Pts',(83.9927462711912,8.42486550657697,62.4403972238464));
#111525=CARTESIAN_POINT('Ctrl Pts',(83.9627466674285,8.3902241733661,62.4457084182725));
#111526=CARTESIAN_POINT('Ctrl Pts',(83.9522334255182,8.37808425581839,62.4475697052506));
#111527=CARTESIAN_POINT('Ctrl Pts',(83.941451784926,8.36603053885286,62.4494764640261));
#111528=CARTESIAN_POINT('Ctrl Pts',(83.9303964859696,8.35407416969622,62.451429443095));
#111529=CARTESIAN_POINT('',(83.2009909796241,7.9420820879518,62.8844210194974));
#111530=CARTESIAN_POINT('Ctrl Pts',(83.2009909626467,7.942082062319,62.8844208921972));
#111531=CARTESIAN_POINT('Ctrl Pts',(83.222046508233,7.94653931462841,62.8807031398782));
#111532=CARTESIAN_POINT('Ctrl Pts',(83.2429357698035,7.95132157984317,62.8761972279364));
#111533=CARTESIAN_POINT('Ctrl Pts',(83.2635687047957,7.95643767493921,62.871090966125));
#111534=CARTESIAN_POINT('Ctrl Pts',(83.2842193969547,7.96155817306146,62.8659803097501));
#111535=CARTESIAN_POINT('Ctrl Pts',(83.3046143507272,7.96701310580604,62.8602693081362));
#111536=CARTESIAN_POINT('Ctrl Pts',(83.3247033968147,7.97280522806796,62.8541132564984));
#111537=CARTESIAN_POINT('Ctrl Pts',(83.3446240476281,7.97854879819796,62.8480088076095));
#111538=CARTESIAN_POINT('Ctrl Pts',(83.3642448422555,7.98462393869616,62.8414672964301));
#111539=CARTESIAN_POINT('Ctrl Pts',(83.383541384477,7.99102707214922,62.8345960380203));
#111540=CARTESIAN_POINT('Ctrl Pts',(83.4026576805979,7.99737039489514,62.8277889630026));
#111541=CARTESIAN_POINT('Ctrl Pts',(83.421456488262,8.0040356111001,62.8206585172748));
#111542=CARTESIAN_POINT('Ctrl Pts',(83.4399258027391,8.01101300250228,62.8132597545955));
#111543=CARTESIAN_POINT('Ctrl Pts',(83.4582588180922,8.01793890242455,62.8059155930153));
#111544=CARTESIAN_POINT('Ctrl Pts',(83.4762677324473,8.02517237978557,62.7983071209058));
#111545=CARTESIAN_POINT('Ctrl Pts',(83.4939429395274,8.03269780909502,62.7904371848953));
#111546=CARTESIAN_POINT('Ctrl Pts',(83.5116060615294,8.04021809303896,62.7825726298001));
#111547=CARTESIAN_POINT('Ctrl Pts',(83.5289363689357,8.04802992154145,62.7744469479267));
#111548=CARTESIAN_POINT('Ctrl Pts',(83.5459191289626,8.05611167223378,62.7660115139603));
#111549=CARTESIAN_POINT('Ctrl Pts',(83.5629790145414,8.06423012541038,62.7575377712915));
#111550=CARTESIAN_POINT('Ctrl Pts',(83.5796886050667,8.07262094713688,62.7487513653927));
#111551=CARTESIAN_POINT('Ctrl Pts',(83.5960214164399,8.08125626970302,62.7395518330078));
#111552=CARTESIAN_POINT('Ctrl Pts',(83.6086053828994,8.08790954004676,62.7324638550516));
#111553=CARTESIAN_POINT('Ctrl Pts',(83.6209655150557,8.09470782886237,62.725129557547));
#111554=CARTESIAN_POINT('Ctrl Pts',(83.6330826272214,8.1016360813663,62.7174832477284));
#111555=CARTESIAN_POINT('Ctrl Pts',(83.6567703444014,8.11518010766737,62.7025354926875));
#111556=CARTESIAN_POINT('Ctrl Pts',(83.6795771016034,8.12928191424406,62.6868902425315));
#111557=CARTESIAN_POINT('Ctrl Pts',(83.7014877431072,8.14391670430066,62.6707517017523));
#111558=CARTESIAN_POINT('Ctrl Pts',(83.7244532122668,8.15925604612889,62.6538362152531));
#111559=CARTESIAN_POINT('Ctrl Pts',(83.7464350423128,8.17518092904151,62.6363791547347));
#111560=CARTESIAN_POINT('Ctrl Pts',(83.7674378978759,8.19166080634232,62.6185610768498));
#111561=CARTESIAN_POINT('Ctrl Pts',(83.7886019840947,8.20826719317491,62.6006062165939));
#111562=CARTESIAN_POINT('Ctrl Pts',(83.8087728368686,8.22543711768918,62.5822846068703));
#111563=CARTESIAN_POINT('Ctrl Pts',(83.827964089698,8.24313741331777,62.5637259673144));
#111564=CARTESIAN_POINT('Ctrl Pts',(83.8477357437988,8.26137301918273,62.5446060586172));
#111565=CARTESIAN_POINT('Ctrl Pts',(83.8664683468657,8.28017155560093,62.5252344585607));
#111566=CARTESIAN_POINT('Ctrl Pts',(83.8841744418319,8.29949484755758,62.5056966765476));
#111567=CARTESIAN_POINT('Ctrl Pts',(83.9004482213411,8.31725500265072,62.4877393823397));
#111568=CARTESIAN_POINT('Ctrl Pts',(83.9158551085819,8.33545841735704,62.4696407985449));
#111569=CARTESIAN_POINT('Ctrl Pts',(83.930396470504,8.35407418254754,62.4514294460597));
#111570=CARTESIAN_POINT('',(81.9035260502888,8.32029685538484,63.1131988121113));
#111571=CARTESIAN_POINT('Origin',(82.9055487053591,9.38083151964701,62.93651572428));
#111572=CARTESIAN_POINT('Origin',(82.8534541851791,9.38083151964701,62.64107301909));
#111573=CARTESIAN_POINT('Origin',(72.4794067363791,-4.5075054799778E-14,
55.63586067514));
#111574=CARTESIAN_POINT('',(63.1758688215082,1.34031149749143E-14,57.5808113821829));
#111575=CARTESIAN_POINT('',(81.8872355012805,1.51070582845848E-14,54.28158621401));
#111576=CARTESIAN_POINT('Origin',(72.5314653386492,-4.5075054799778E-14,
55.9310996797491));
#111577=CARTESIAN_POINT('',(82.3736337596115,-2.14063710640059E-14,53.5869134266698));
#111578=CARTESIAN_POINT('',(81.8871110497795,1.47525070273786E-14,54.2817578235612));
#111579=CARTESIAN_POINT('',(62.4811376251638,-1.81697385251322E-14,57.0943371416662));
#111580=CARTESIAN_POINT('Origin',(72.4273508090685,-4.5075054799778E-14,
55.3406368409801));
#111581=CARTESIAN_POINT('',(63.1760167402064,1.34099672619711E-14,57.58091496094));
#111582=CARTESIAN_POINT('Origin',(71.6139524734691,1.4210854715202E-14,
50.72762564822));
#111583=CARTESIAN_POINT('',(82.5073599491905,1.54967338543067E-14,52.0401193459587));
#111584=CARTESIAN_POINT('',(82.5003366733922,-0.386927879893151,52.0413577389749));
#111585=CARTESIAN_POINT('Origin',(72.1668785425691,1.4210854715202E-14,
53.86342521146));
#111586=CARTESIAN_POINT('',(82.7678322156911,1.54967338543067E-14,53.5173309754786));
#111587=CARTESIAN_POINT('',(81.9544338800974,1.54967338543067E-14,48.9043197827175));
#111588=CARTESIAN_POINT('Origin',(72.4273508090691,1.4210854715202E-14,
55.34063684098));
#111589=CARTESIAN_POINT('Origin',(72.1668785425691,1.4210854715202E-14,
53.86342521146));
#111590=CARTESIAN_POINT('Origin',(72.1668785425691,1.4210854715202E-14,
53.86342521146));
#111591=CARTESIAN_POINT('',(82.9055752351331,-0.405352763000806,51.4621899410204));
#111592=CARTESIAN_POINT('Origin',(72.0800544537391,1.4210854715202E-14,
53.371021335));
#111593=CARTESIAN_POINT('Origin',(82.9924061081933,-0.405353017030921,51.9545926212376));
#111594=CARTESIAN_POINT('Origin',(71.6139524734691,1.4210854715202E-14,
50.72762564822));
#111595=CARTESIAN_POINT('',(83.072317586283,1.55885823642428E-14,50.925075459698));
#111596=CARTESIAN_POINT('',(83.0657624332148,-0.386939173054244,50.9262313100466));
#111597=CARTESIAN_POINT('Origin',(71.9932303648991,1.4210854715202E-14,
52.87861745845));
#111598=CARTESIAN_POINT('',(83.1591416751154,1.55885823642428E-14,51.4174793361976));
#111599=CARTESIAN_POINT('',(82.6930396948565,1.55885823642428E-14,48.7740836494674));
#111600=CARTESIAN_POINT('Origin',(72.0800544537291,1.4210854715202E-14,
53.37102133495));
#111601=CARTESIAN_POINT('Origin',(71.9932303648991,1.4210854715202E-14,
52.87861745845));
#111602=CARTESIAN_POINT('Origin',(71.9932303648991,1.4210854715202E-14,
52.87861745845));
#111603=CARTESIAN_POINT('',(83.4710450568977,-0.404136266114647,50.3470557427728));
#111604=CARTESIAN_POINT('Origin',(71.9064062760691,1.4210854715202E-14,
52.38621358198));
#111605=CARTESIAN_POINT('Origin',(83.5578749695843,-0.404136469634433,50.8394585923398));
#111606=CARTESIAN_POINT('Origin',(6.43246351666909,92.,72.98888938658));
#111607=CARTESIAN_POINT('',(16.5158721300291,92.,77.384895612235));
#111608=CARTESIAN_POINT('',(16.5158721300291,92.,68.592883160925));
#111609=CARTESIAN_POINT('Origin',(6.43246351666909,92.,72.98888938658));
#111610=CARTESIAN_POINT('',(16.0575353748791,92.5,68.792701625727));
#111611=CARTESIAN_POINT('Origin',(16.0575353748791,92.,68.792701625727));
#111612=CARTESIAN_POINT('',(16.0575353748791,92.5,77.185077147433));
#111613=CARTESIAN_POINT('Origin',(6.43246351666909,92.5,72.98888938658));
#111614=CARTESIAN_POINT('Origin',(16.0575353748791,92.,77.185077147433));
#111615=CARTESIAN_POINT('Origin',(6.43246351666909,-92.5,72.98888938658));
#111616=CARTESIAN_POINT('',(17.4324600236772,25.5801002023223,72.9888894061479));
#111617=CARTESIAN_POINT('',(16.5158721312486,26.62691877866,77.3848956129324));
#111618=CARTESIAN_POINT('Ctrl Pts',(17.4324565306852,25.5801002023224,72.9888894061479));
#111619=CARTESIAN_POINT('Ctrl Pts',(17.4331138485723,25.6746776183602,73.745453096432));
#111620=CARTESIAN_POINT('Ctrl Pts',(17.3542127226475,25.8261249661036,74.4979998452865));
#111621=CARTESIAN_POINT('Ctrl Pts',(17.0463140803605,26.1912967232894,75.9719859573303));
#111622=CARTESIAN_POINT('Ctrl Pts',(16.8173238247368,26.405009893619,76.6934360403765));
#111623=CARTESIAN_POINT('Ctrl Pts',(16.5158721306991,26.62691877866,77.384895612693));
#111624=CARTESIAN_POINT('',(16.5158747362626,25.68037166863,68.5928891373664));
#111625=CARTESIAN_POINT('Ctrl Pts',(16.515874735658,25.68037166863,68.59288913763));
#111626=CARTESIAN_POINT('Ctrl Pts',(16.5986513774045,25.6458493068531,68.7827596723862));
#111627=CARTESIAN_POINT('Ctrl Pts',(16.6762707643978,25.6153134130533,68.9754506479589));
#111628=CARTESIAN_POINT('Ctrl Pts',(16.748483349918,25.588832917128,69.1705474951282));
#111629=CARTESIAN_POINT('Ctrl Pts',(16.8206436166596,25.5623716066008,69.3655029925774));
#111630=CARTESIAN_POINT('Ctrl Pts',(16.8874047263992,25.5399598197198,69.5628605425677));
#111631=CARTESIAN_POINT('Ctrl Pts',(16.948563454897,25.5216663366697,69.7621817628245));
#111632=CARTESIAN_POINT('Ctrl Pts',(17.0096942990628,25.503381194237,69.9614121057976));
#111633=CARTESIAN_POINT('Ctrl Pts',(17.0652277220566,25.4892106011433,70.1626039740258));
#111634=CARTESIAN_POINT('Ctrl Pts',(17.1150090469596,25.4792232435384,70.3653000526195));
#111635=CARTESIAN_POINT('Ctrl Pts',(17.1457649251256,25.4730528582726,70.4905296625209));
#111636=CARTESIAN_POINT('Ctrl Pts',(17.1743261824005,25.4684792184117,70.6163330668643));
#111637=CARTESIAN_POINT('Ctrl Pts',(17.2006658845956,25.465518521688,70.742599609329));
#111638=CARTESIAN_POINT('Ctrl Pts',(17.2467648332579,25.4603367999942,70.9635874859473));
#111639=CARTESIAN_POINT('Ctrl Pts',(17.286051845598,25.4600965467122,71.1859717032842));
#111640=CARTESIAN_POINT('Ctrl Pts',(17.3184481782116,25.4648114312984,71.4092255145296));
#111641=CARTESIAN_POINT('Ctrl Pts',(17.3508491400659,25.4695269896132,71.6325112273989));
#111642=CARTESIAN_POINT('Ctrl Pts',(17.3763574227755,25.4791991020161,71.8566664110209));
#111643=CARTESIAN_POINT('Ctrl Pts',(17.3949461950319,25.4938414438245,72.0811595112339));
#111644=CARTESIAN_POINT('Ctrl Pts',(17.4135468568908,25.508493151051,72.3057961999368));
#111645=CARTESIAN_POINT('Ctrl Pts',(17.4252191627864,25.5281214477534,72.5307708650725));
#111646=CARTESIAN_POINT('Ctrl Pts',(17.4299884033709,25.5527400355065,72.755551934862));
#111647=CARTESIAN_POINT('Ctrl Pts',(17.4316393110341,25.5612619405056,72.8333615534126));
#111648=CARTESIAN_POINT('Ctrl Pts',(17.4324635168074,25.5703818066716,72.9111480090886));
#111649=CARTESIAN_POINT('Ctrl Pts',(17.4324635166691,25.5801002023223,72.9888894061479));
#111650=CARTESIAN_POINT('',(16.5158721300291,92.,68.592883160925));
#111651=CARTESIAN_POINT('',(16.5158721300291,92.,77.384895612235));
#111652=CARTESIAN_POINT('Origin',(17.7894674803291,1.4210854715202E-14,
100.88908350184));
#111653=CARTESIAN_POINT('',(-4.38226888389591,-1.31660223688345E-7,96.08109859282));
#111654=CARTESIAN_POINT('',(7.33390977337979,-18.5189601959142,98.6155810268129));
#111655=CARTESIAN_POINT('Ctrl Pts',(-4.38226888389591,-1.31660223688345E-7,
96.08109859282));
#111656=CARTESIAN_POINT('Ctrl Pts',(-4.38226740849383,-0.395879795914794,
96.0811066634897));
#111657=CARTESIAN_POINT('Ctrl Pts',(-4.36836546848751,-0.794239500360881,
96.0954673000493));
#111658=CARTESIAN_POINT('Ctrl Pts',(-4.32606480122498,-1.39451379175889,
96.1384318258752));
#111659=CARTESIAN_POINT('Ctrl Pts',(-4.29955327484655,-1.69533351275973,
96.1652701131746));
#111660=CARTESIAN_POINT('Ctrl Pts',(-4.2591188739944,-2.04725725181565,
96.2059329439757));
#111661=CARTESIAN_POINT('Ctrl Pts',(-4.2365109977993,-2.22343172549005,
96.228599658187));
#111662=CARTESIAN_POINT('Ctrl Pts',(-4.22630807341278,-2.29897747604772,
96.2388141126869));
#111663=CARTESIAN_POINT('Ctrl Pts',(-4.21939176836248,-2.34935038034874,
96.2457348631364));
#111664=CARTESIAN_POINT('Ctrl Pts',(-4.21611286433566,-2.37287399529721,
96.2490144430748));
#111665=CARTESIAN_POINT('Ctrl Pts',(-4.15135954270303,-2.82954021094412,
96.313747497813));
#111666=CARTESIAN_POINT('Ctrl Pts',(-4.07099976598698,-3.27913917903879,
96.3943244434559));
#111667=CARTESIAN_POINT('Ctrl Pts',(-3.91545475344492,-3.98089845402761,
96.5436302590383));
#111668=CARTESIAN_POINT('Ctrl Pts',(-3.85776822453298,-4.21936941677387,
96.5981382309613));
#111669=CARTESIAN_POINT('Ctrl Pts',(-3.76171544626494,-4.58352350096052,
96.6868742257576));
#111670=CARTESIAN_POINT('Ctrl Pts',(-3.7113080371269,-4.76721148175515,
96.7329856841091));
#111671=CARTESIAN_POINT('Ctrl Pts',(-3.648162566933,-4.98423966769277,96.7898034593372));
#111672=CARTESIAN_POINT('Ctrl Pts',(-3.61548421214779,-5.0934226157687,
96.8189638396919));
#111673=CARTESIAN_POINT('Ctrl Pts',(-3.60123998781038,-5.14035727020337,
96.8316217747574));
#111674=CARTESIAN_POINT('Ctrl Pts',(-3.59169042377515,-5.17167843320581,
96.8400960484506));
#111675=CARTESIAN_POINT('Ctrl Pts',(-3.58636743023429,-5.18904958358344,
96.8448125091018));
#111676=CARTESIAN_POINT('Ctrl Pts',(-3.44424236895454,-5.65095142284287,
96.9705842863248));
#111677=CARTESIAN_POINT('Ctrl Pts',(-3.2720713912644,-6.15256771946993,
97.1189231221924));
#111678=CARTESIAN_POINT('Ctrl Pts',(-2.9441812821162,-6.97785834618417,
97.3778065444133));
#111679=CARTESIAN_POINT('Ctrl Pts',(-2.82324375543532,-7.26505900893829,
97.4701573369327));
#111680=CARTESIAN_POINT('Ctrl Pts',(-2.62183713875804,-7.71262231887509,
97.6173202930935));
#111681=CARTESIAN_POINT('Ctrl Pts',(-2.55136652007071,-7.86460046030084,
97.6678137746956));
#111682=CARTESIAN_POINT('Ctrl Pts',(-2.44032705660128,-8.09654677529307,
97.7456543920469));
#111683=CARTESIAN_POINT('Ctrl Pts',(-2.38347381396219,-8.21351435473895,
97.7850997770581));
#111684=CARTESIAN_POINT('Ctrl Pts',(-2.31473776421149,-8.35166775047382,
97.8320252948431));
#111685=CARTESIAN_POINT('Ctrl Pts',(-2.27975863749924,-8.42116082762791,
97.8557128919944));
#111686=CARTESIAN_POINT('Ctrl Pts',(-2.26463563642141,-8.45103210312728,
97.8659127232834));
#111687=CARTESIAN_POINT('Ctrl Pts',(-2.25452420328234,-8.47096588156003,
97.8727232587939));
#111688=CARTESIAN_POINT('Ctrl Pts',(-2.24889450428614,-8.48204086843337,
97.8765095288148));
#111689=CARTESIAN_POINT('Ctrl Pts',(-2.09953854167641,-8.77534963713818,
97.9768370423297));
#111690=CARTESIAN_POINT('Ctrl Pts',(-1.94846674521134,-9.05697686800579,
98.073135296074));
#111691=CARTESIAN_POINT('Ctrl Pts',(-1.63409619546405,-9.61408890046589,
98.2637989826697));
#111692=CARTESIAN_POINT('Ctrl Pts',(-1.47017163101268,-9.89057982332896,
98.3585098232659));
#111693=CARTESIAN_POINT('Ctrl Pts',(-0.964233481725216,-10.7039866099445,
98.6377449207042));
#111694=CARTESIAN_POINT('Ctrl Pts',(-0.612751142896682,-11.2209512901646,
98.8036853265539));
#111695=CARTESIAN_POINT('Ctrl Pts',(0.10450987898053,-12.1973811850675,
99.0945813177457));
#111696=CARTESIAN_POINT('Ctrl Pts',(0.463979741155269,-12.6487435089947,
99.2162585783067));
#111697=CARTESIAN_POINT('Ctrl Pts',(0.994936356724773,-13.2742324080916,
99.3647947432687));
#111698=CARTESIAN_POINT('Ctrl Pts',(1.17056338743409,-13.4741453696707,
99.4086406561457));
#111699=CARTESIAN_POINT('Ctrl Pts',(1.43092046996534,-13.7616699130789,
99.4660946977389));
#111700=CARTESIAN_POINT('Ctrl Pts',(1.51719322763612,-13.8554543000973,
99.4838600685593));
#111701=CARTESIAN_POINT('Ctrl Pts',(1.68855009682205,-14.0390007881235,
99.516647558742));
#111702=CARTESIAN_POINT('Ctrl Pts',(1.77440983548494,-14.1295696360823,
99.5317952307266));
#111703=CARTESIAN_POINT('Ctrl Pts',(2.19259251099756,-14.5645253456288,
99.5994883737387));
#111704=CARTESIAN_POINT('Ctrl Pts',(2.52711263534736,-14.8925987630755,
99.6339837749765));
#111705=CARTESIAN_POINT('Ctrl Pts',(3.02526127117294,-15.356361515315,99.6568716664454));
#111706=CARTESIAN_POINT('Ctrl Pts',(3.1907097246831,-15.5062274705087,99.6596910271714));
#111707=CARTESIAN_POINT('Ctrl Pts',(3.43756894799691,-15.7241533429341,
99.6567777784696));
#111708=CARTESIAN_POINT('Ctrl Pts',(3.56067058119804,-15.8313982301523,
99.6535355136471));
#111709=CARTESIAN_POINT('Ctrl Pts',(3.70362915460082,-15.9535585987621,
99.6466431710621));
#111710=CARTESIAN_POINT('Ctrl Pts',(3.76474672461133,-16.0052842994467,
99.6430245258013));
#111711=CARTESIAN_POINT('Ctrl Pts',(3.80545736235971,-16.0396289661334,
99.6404645401892));
#111712=CARTESIAN_POINT('Ctrl Pts',(3.82721096178525,-16.0579182564491,
99.6390113352449));
#111713=CARTESIAN_POINT('Ctrl Pts',(5.05603156831833,-17.0879713083793,
99.5526895815698));
#111714=CARTESIAN_POINT('Ctrl Pts',(6.24087891321929,-17.8883939937044,
99.2080656541756));
#111715=CARTESIAN_POINT('Ctrl Pts',(7.33390977282909,-18.51896019696,98.61558102691));
#111716=CARTESIAN_POINT('',(20.8003130802284,-19.9701890893778,80.5583314866612));
#111717=CARTESIAN_POINT('Ctrl Pts',(20.8003130790713,-19.9701890857655,
80.5583314868652));
#111718=CARTESIAN_POINT('Ctrl Pts',(20.7653319117175,-19.987994824802,80.6751964237543));
#111719=CARTESIAN_POINT('Ctrl Pts',(20.7262218203834,-20.0075988348333,
80.8048120490032));
#111720=CARTESIAN_POINT('Ctrl Pts',(20.6825233107631,-20.0289315329255,
80.9468047609331));
#111721=CARTESIAN_POINT('Ctrl Pts',(20.6406279657392,-20.0493839637894,
81.0829383203812));
#111722=CARTESIAN_POINT('Ctrl Pts',(20.5945149707442,-20.0714254468934,
81.2304486066214));
#111723=CARTESIAN_POINT('Ctrl Pts',(20.5437688867959,-20.0949485475054,
81.3890082378651));
#111724=CARTESIAN_POINT('Ctrl Pts',(20.4940782529224,-20.1179823993643,
81.5442700427224));
#111725=CARTESIAN_POINT('Ctrl Pts',(20.4399451680258,-20.1424370973425,
81.7101263638527));
#111726=CARTESIAN_POINT('Ctrl Pts',(20.3809704781416,-20.1681641667881,
81.8862714296551));
#111727=CARTESIAN_POINT('Ctrl Pts',(20.3223276737648,-20.1937464547771,
82.0614252228514));
#111728=CARTESIAN_POINT('Ctrl Pts',(20.2588975070578,-20.220587175818,82.2467523019759));
#111729=CARTESIAN_POINT('Ctrl Pts',(20.1902797183793,-20.2484884442895,
82.4419534052279));
#111730=CARTESIAN_POINT('Ctrl Pts',(20.1216619297008,-20.2763897127609,
82.63715450848));
#111731=CARTESIAN_POINT('Ctrl Pts',(20.0478563792751,-20.3053519379154,
82.8422296605058));
#111732=CARTESIAN_POINT('Ctrl Pts',(19.9684567327649,-20.3351194882471,
83.0568806706376));
#111733=CARTESIAN_POINT('Ctrl Pts',(19.898207261829,-20.361456565977,83.2467948649744));
#111734=CARTESIAN_POINT('Ctrl Pts',(19.823519635129,-20.3884370978636,83.4441575159233));
#111735=CARTESIAN_POINT('Ctrl Pts',(19.7439596888234,-20.4158699133918,
83.6486878978924));
#111736=CARTESIAN_POINT('Ctrl Pts',(19.6670364254486,-20.4423935825492,
83.8464399725348));
#111737=CARTESIAN_POINT('Ctrl Pts',(19.5855582997632,-20.4693401437796,
84.0508925855895));
#111738=CARTESIAN_POINT('Ctrl Pts',(19.4991306420753,-20.4964891051933,
84.261792405076));
#111739=CARTESIAN_POINT('Ctrl Pts',(19.4171160814392,-20.5222518089578,
84.4619234336858));
#111740=CARTESIAN_POINT('Ctrl Pts',(19.3306444054264,-20.5481966833614,
84.6678600984616));
#111741=CARTESIAN_POINT('Ctrl Pts',(19.2393782527093,-20.5740918708992,
84.879385946047));
#111742=CARTESIAN_POINT('Ctrl Pts',(19.1500280070395,-20.5994434530497,
85.0864713318617));
#111743=CARTESIAN_POINT('Ctrl Pts',(19.0560658076384,-20.624751139383,85.2989083256206));
#111744=CARTESIAN_POINT('Ctrl Pts',(18.9571047420586,-20.6497644783627,
85.5164798154753));
#111745=CARTESIAN_POINT('Ctrl Pts',(18.8971764585829,-20.664911914986,85.6482355301482));
#111746=CARTESIAN_POINT('Ctrl Pts',(18.8354150145491,-20.6799504595488,
85.7818741643341));
#111747=CARTESIAN_POINT('Ctrl Pts',(18.7717350493916,-20.6948151419852,
85.9173474032424));
#111748=CARTESIAN_POINT('Ctrl Pts',(18.6873169113696,-20.7145206931811,
86.0969391877568));
#111749=CARTESIAN_POINT('Ctrl Pts',(18.5995231590073,-20.7339224297437,
86.2797556801146));
#111750=CARTESIAN_POINT('Ctrl Pts',(18.5081361122369,-20.7528508611175,
86.4656796928624));
#111751=CARTESIAN_POINT('Ctrl Pts',(18.4624425888517,-20.7623150768044,
86.5586416992363));
#111752=CARTESIAN_POINT('Ctrl Pts',(18.4158514891404,-20.771660387363,86.6523786905016));
#111753=CARTESIAN_POINT('Ctrl Pts',(18.3683406589989,-20.7808622225757,
86.7468635635245));
#111754=CARTESIAN_POINT('Ctrl Pts',(18.3445852439282,-20.7854631401821,
86.7941060000359));
#111755=CARTESIAN_POINT('Ctrl Pts',(18.3205998936028,-20.7900281673136,
86.8415354074536));
#111756=CARTESIAN_POINT('Ctrl Pts',(18.2963818441927,-20.7945540934904,
86.8891482101765));
#111757=CARTESIAN_POINT('Ctrl Pts',(18.2842728194877,-20.7968170565788,
86.9129546115379));
#111758=CARTESIAN_POINT('Ctrl Pts',(18.2721056198366,-20.7990702430506,
86.9368068617565));
#111759=CARTESIAN_POINT('Ctrl Pts',(18.2598798995501,-20.8013132430092,
86.9607045083562));
#111760=CARTESIAN_POINT('Ctrl Pts',(18.2537670394069,-20.8024347429884,
86.972653331656));
#111761=CARTESIAN_POINT('Ctrl Pts',(18.2476395490946,-20.8035536962519,
86.9846135040529));
#111762=CARTESIAN_POINT('Ctrl Pts',(18.2414973854199,-20.8046700510096,
86.9965849683362));
#111763=CARTESIAN_POINT('Ctrl Pts',(18.2368907626639,-20.8055073170779,
87.0055635665487));
#111764=CARTESIAN_POINT('Ctrl Pts',(18.2322758861407,-20.8063431214795,
87.0145485164474));
#111765=CARTESIAN_POINT('Ctrl Pts',(18.2276527376309,-20.8071774422296,
87.0235397937539));
#111766=CARTESIAN_POINT('Ctrl Pts',(18.2261116881277,-20.8074555491462,
87.0265368861894));
#111767=CARTESIAN_POINT('Ctrl Pts',(18.2236400469036,-20.8079008663174,
87.0313414365281));
#111768=CARTESIAN_POINT('Ctrl Pts',(18.2230268311186,-20.8080112676088,
87.0325331792842));
#111769=CARTESIAN_POINT('Ctrl Pts',(18.1533013936453,-20.8205643990277,
87.1680397775557));
#111770=CARTESIAN_POINT('Ctrl Pts',(18.0784123332618,-20.8333737895828,
87.311317704187));
#111771=CARTESIAN_POINT('Ctrl Pts',(17.9980045836939,-20.8461945100127,
87.4619762758188));
#111772=CARTESIAN_POINT('Ctrl Pts',(17.9200700604966,-20.8586208835789,
87.6080008071459));
#111773=CARTESIAN_POINT('Ctrl Pts',(17.8369509634185,-20.8710579465556,
87.7609589579823));
#111774=CARTESIAN_POINT('Ctrl Pts',(17.7483263582346,-20.8832340293166,
87.9204945809405));
#111775=CARTESIAN_POINT('Ctrl Pts',(17.6611683978886,-20.8952086105995,
88.0773900556306));
#111776=CARTESIAN_POINT('Ctrl Pts',(17.5686854591308,-20.9069309183669,
88.2406471355186));
#111777=CARTESIAN_POINT('Ctrl Pts',(17.4705771026812,-20.9180932140501,
88.4099262132584));
#111778=CARTESIAN_POINT('Ctrl Pts',(17.3748863402747,-20.9289804475415,
88.5750339022932));
#111779=CARTESIAN_POINT('Ctrl Pts',(17.2738437991793,-20.939334975306,88.7458704901516));
#111780=CARTESIAN_POINT('Ctrl Pts',(17.1671780469306,-20.9488226713765,
88.9221195676893));
#111781=CARTESIAN_POINT('Ctrl Pts',(17.0925185791883,-20.9554634752315,
89.0454830844847));
#111782=CARTESIAN_POINT('Ctrl Pts',(17.0151043630113,-20.9616786102941,
89.1714982304492));
#111783=CARTESIAN_POINT('Ctrl Pts',(16.9348453643333,-20.9673385492286,
89.3000559693276));
#111784=CARTESIAN_POINT('Ctrl Pts',(16.825042534418,-20.9750819465099,89.4759366028872));
#111785=CARTESIAN_POINT('Ctrl Pts',(16.7098893736243,-20.9817890778163,
89.6565138298478));
#111786=CARTESIAN_POINT('Ctrl Pts',(16.5891011991341,-20.9870881773623,
89.8413160432456));
#111787=CARTESIAN_POINT('Ctrl Pts',(16.4711138718983,-20.9922644009027,
90.021833045991));
#111788=CARTESIAN_POINT('Ctrl Pts',(16.3477496186044,-20.9960971507281,
90.2063814056935));
#111789=CARTESIAN_POINT('Ctrl Pts',(16.2187573001304,-20.9981925841403,
90.3945190644661));
#111790=CARTESIAN_POINT('Ctrl Pts',(16.1458501215178,-20.9993769348045,
90.5008555196454));
#111791=CARTESIAN_POINT('Ctrl Pts',(16.0711452907451,-21.0000054222429,
90.6083385543735));
#111792=CARTESIAN_POINT('Ctrl Pts',(15.9945999617102,-20.9999999647811,
90.7168879103833));
#111793=CARTESIAN_POINT('Ctrl Pts',(15.8639252795662,-20.9999906480521,
90.9021984025108));
#111794=CARTESIAN_POINT('Ctrl Pts',(15.7278791641397,-20.9981364242747,
91.0905957924792));
#111795=CARTESIAN_POINT('Ctrl Pts',(15.5862297149464,-20.9940124499549,
91.2815743670219));
#111796=CARTESIAN_POINT('Ctrl Pts',(15.5378464502222,-20.9926038222309,
91.3468070028096));
#111797=CARTESIAN_POINT('Ctrl Pts',(15.4888096188265,-20.9909299770618,
91.4123407552541));
#111798=CARTESIAN_POINT('Ctrl Pts',(15.4391105631588,-20.9889727067707,
91.4781553681437));
#111799=CARTESIAN_POINT('Ctrl Pts',(15.3415102205454,-20.9851289667152,
91.6074038755989));
#111800=CARTESIAN_POINT('Ctrl Pts',(15.241354021653,-20.9801928015274,91.7377286021338));
#111801=CARTESIAN_POINT('Ctrl Pts',(15.1385783549149,-20.9740185000755,
91.8689881476138));
#111802=CARTESIAN_POINT('Ctrl Pts',(15.0871905215459,-20.9709313493496,
91.9346179203538));
#111803=CARTESIAN_POINT('Ctrl Pts',(15.0351478300591,-20.9675344999767,
92.0004813962707));
#111804=CARTESIAN_POINT('Ctrl Pts',(14.9824426596947,-20.9638087425081,
92.0665607210304));
#111805=CARTESIAN_POINT('Ctrl Pts',(14.9560900745125,-20.9619458637738,
92.0996003834102));
#111806=CARTESIAN_POINT('Ctrl Pts',(14.9295718702518,-20.9600007473097,
92.1326940078877));
#111807=CARTESIAN_POINT('Ctrl Pts',(14.9028870985181,-20.9579709275709,
92.1658392895054));
#111808=CARTESIAN_POINT('Ctrl Pts',(14.8895447126513,-20.9569560177015,
92.1824119303143));
#111809=CARTESIAN_POINT('Ctrl Pts',(14.8761606849662,-20.9559199313282,
92.1989974853993));
#111810=CARTESIAN_POINT('Ctrl Pts',(14.8627348982699,-20.954862356187,92.2155956664944));
#111811=CARTESIAN_POINT('Ctrl Pts',(14.8560220049218,-20.9543335686164,
92.2238947570419));
#111812=CARTESIAN_POINT('Ctrl Pts',(14.8492986718242,-20.9537994088106,
92.2321970040914));
#111813=CARTESIAN_POINT('Ctrl Pts',(14.8425648843961,-20.9532598374809,
92.2405023714394));
#111814=CARTESIAN_POINT('Ctrl Pts',(14.8358310969679,-20.9527202661512,
92.2488077387874));
#111815=CARTESIAN_POINT('Ctrl Pts',(14.8277837298359,-20.9520690930638,
92.2587197029694));
#111816=CARTESIAN_POINT('Ctrl Pts',(14.8223321445671,-20.9516248494587,
92.265427798123));
#111817=CARTESIAN_POINT('Ctrl Pts',(14.6197148893987,-20.9351137952504,
92.5147453379572));
#111818=CARTESIAN_POINT('Ctrl Pts',(14.4184351440027,-20.9145672747272,
92.7538762471074));
#111819=CARTESIAN_POINT('Ctrl Pts',(14.2190755019638,-20.8903363637757,
92.9833072479781));
#111820=CARTESIAN_POINT('Ctrl Pts',(14.0175137590704,-20.8658378013116,
93.2152725140488));
#111821=CARTESIAN_POINT('Ctrl Pts',(13.8179149930755,-20.8375732619276,
93.437322361534));
#111822=CARTESIAN_POINT('Ctrl Pts',(13.6208541261277,-20.8059516975061,
93.6499646150171));
#111823=CARTESIAN_POINT('Ctrl Pts',(13.4198692877072,-20.773700469171,93.8668411040918));
#111824=CARTESIAN_POINT('Ctrl Pts',(13.2215246559016,-20.7379574539372,
94.0739315713755));
#111825=CARTESIAN_POINT('Ctrl Pts',(13.0263985330229,-20.6992003520432,
94.2717803668916));
#111826=CARTESIAN_POINT('Ctrl Pts',(12.950382145547,-20.6841015286179,94.3488574413484));
#111827=CARTESIAN_POINT('Ctrl Pts',(12.8748538757691,-20.6685457010464,
94.4245319769535));
#111828=CARTESIAN_POINT('Ctrl Pts',(12.7998465499645,-20.6525627178891,
94.4988363996149));
#111829=CARTESIAN_POINT('Ctrl Pts',(12.5995488236742,-20.6098821510059,
94.6972571105621));
#111830=CARTESIAN_POINT('Ctrl Pts',(12.4030580629536,-20.564173130271,94.8857858123521));
#111831=CARTESIAN_POINT('Ctrl Pts',(12.2109457221164,-20.5160407252881,
95.0649321222251));
#111832=CARTESIAN_POINT('Ctrl Pts',(12.0946798390561,-20.4869111204706,
95.1733509974708));
#111833=CARTESIAN_POINT('Ctrl Pts',(11.9800168330081,-20.4568946482348,
95.2783335792123));
#111834=CARTESIAN_POINT('Ctrl Pts',(11.8670762772347,-20.4261311415844,
95.3799940814724));
#111835=CARTESIAN_POINT('Ctrl Pts',(11.7172971370492,-20.3853332940472,
95.5148138768514));
#111836=CARTESIAN_POINT('Ctrl Pts',(11.5705393370016,-20.3432198853979,
95.6437907033954));
#111837=CARTESIAN_POINT('Ctrl Pts',(11.4270094765659,-20.3001074782512,
95.7672229849734));
#111838=CARTESIAN_POINT('Ctrl Pts',(11.3552445463481,-20.2785512746779,
95.8289391257624));
#111839=CARTESIAN_POINT('Ctrl Pts',(11.2842843329623,-20.2567446980296,
95.8892731513699));
#111840=CARTESIAN_POINT('Ctrl Pts',(11.2141462900269,-20.2347248452646,
95.9482742817537));
#111841=CARTESIAN_POINT('Ctrl Pts',(11.1790772685592,-20.2237149188821,
95.9777748469456));
#111842=CARTESIAN_POINT('Ctrl Pts',(11.1442137907282,-20.212651672305,96.006942188151));
#111843=CARTESIAN_POINT('Ctrl Pts',(11.1095578622534,-20.2015396909313,
96.0357822745056));
#111844=CARTESIAN_POINT('Ctrl Pts',(11.092229898016,-20.1959837002445,96.0502023176828));
#111845=CARTESIAN_POINT('Ctrl Pts',(11.0749538211899,-20.1904155257147,
96.0645405471347));
#111846=CARTESIAN_POINT('Ctrl Pts',(11.0577298778451,-20.1848357384477,
96.0787977035608));
#111847=CARTESIAN_POINT('Ctrl Pts',(11.0405059345003,-20.1792559511808,
96.0930548599869));
#111848=CARTESIAN_POINT('Ctrl Pts',(11.0223622512192,-20.1733464993521,
96.1080311634234));
#111849=CARTESIAN_POINT('Ctrl Pts',(11.0062146916286,-20.1680621081994,
96.121326691339));
#111850=CARTESIAN_POINT('Ctrl Pts',(10.8884352616903,-20.1295180437516,
96.2183035558513));
#111851=CARTESIAN_POINT('Ctrl Pts',(10.7650451892595,-20.0878025554444,
96.3182483504631));
#111852=CARTESIAN_POINT('Ctrl Pts',(10.6359923950788,-20.0424861616342,
96.4207018070726));
#111853=CARTESIAN_POINT('Ctrl Pts',(10.5090870124052,-19.9979238231403,
96.5214504595896));
#111854=CARTESIAN_POINT('Ctrl Pts',(10.3767055579604,-19.9498793225477,
96.6246250229459));
#111855=CARTESIAN_POINT('Ctrl Pts',(10.2388294415599,-19.8979046255969,
96.7297833218371));
#111856=CARTESIAN_POINT('Ctrl Pts',(10.2093519003149,-19.8867925757868,
96.7522658820785));
#111857=CARTESIAN_POINT('Ctrl Pts',(10.179623323687,-19.8755007363343,96.7748390959961));
#111858=CARTESIAN_POINT('Ctrl Pts',(10.1496437342186,-19.8640244953124,
96.7974986064136));
#111859=CARTESIAN_POINT('Ctrl Pts',(10.0131088563521,-19.8117586973457,
96.900695933069));
#111860=CARTESIAN_POINT('Ctrl Pts',(9.87136065174339,-19.7556701351067,
97.0056761354688));
#111861=CARTESIAN_POINT('Ctrl Pts',(9.72439985909457,-19.6952952121385,
97.1119880032428));
#111862=CARTESIAN_POINT('Ctrl Pts',(9.70301722964254,-19.6865107289933,
97.127456260007));
#111863=CARTESIAN_POINT('Ctrl Pts',(9.68152431320116,-19.6776354405432,
97.1429526968982));
#111864=CARTESIAN_POINT('Ctrl Pts',(9.65992117791659,-19.6686678541629,
97.1584759124834));
#111865=CARTESIAN_POINT('Ctrl Pts',(9.57488145606972,-19.6333673738679,
97.2195823175561));
#111866=CARTESIAN_POINT('Ctrl Pts',(9.48813335101792,-19.5966369901423,
97.2811030929347));
#111867=CARTESIAN_POINT('Ctrl Pts',(9.39968075361787,-19.5583821832216,
97.3429497450282));
#111868=CARTESIAN_POINT('Ctrl Pts',(9.35545445491785,-19.5392547797613,
97.373873071075));
#111869=CARTESIAN_POINT('Ctrl Pts',(9.31080177844068,-19.5197460783091,
97.404877982857));
#111870=CARTESIAN_POINT('Ctrl Pts',(9.26572212530421,-19.4998432260331,
97.4359539001361));
#111871=CARTESIAN_POINT('Ctrl Pts',(9.24318229873596,-19.4898917998951,
97.4514918587756));
#111872=CARTESIAN_POINT('Ctrl Pts',(9.2205357302005,-19.4798418302812,97.4670475684018));
#111873=CARTESIAN_POINT('Ctrl Pts',(9.19778234848026,-19.4696916719074,
97.4826196977618));
#111874=CARTESIAN_POINT('Ctrl Pts',(9.17759947653245,-19.4606882037976,
97.4964326024408));
#111875=CARTESIAN_POINT('Ctrl Pts',(9.15850227514913,-19.4521318460541,
97.509463956387));
#111876=CARTESIAN_POINT('Ctrl Pts',(9.13737792818021,-19.442622036599,97.5238269917626));
#111877=CARTESIAN_POINT('Ctrl Pts',(9.13468751125341,-19.4414108582195,
97.5256562816125));
#111878=CARTESIAN_POINT('Ctrl Pts',(9.13196423804468,-19.4401841502082,
97.5275071678908));
#111879=CARTESIAN_POINT('Ctrl Pts',(9.12920170123955,-19.438938961009,97.5293840121857));
#111880=CARTESIAN_POINT('Ctrl Pts',(8.97159247985769,-19.3678979888895,
97.6364623929759));
#111881=CARTESIAN_POINT('Ctrl Pts',(8.82132163286598,-19.297661080258,97.7355501748584));
#111882=CARTESIAN_POINT('Ctrl Pts',(8.67847795146037,-19.2289123285112,
97.827347023819));
#111883=CARTESIAN_POINT('Ctrl Pts',(8.53637141728977,-19.1605183558611,
97.9186701535871));
#111884=CARTESIAN_POINT('Ctrl Pts',(8.40161506174884,-19.0935973385942,
98.0027774994623));
#111885=CARTESIAN_POINT('Ctrl Pts',(8.2742860773703,-19.0287724910504,98.0803597553401));
#111886=CARTESIAN_POINT('Ctrl Pts',(8.21188246514141,-18.9970019977204,
98.118382622131));
#111887=CARTESIAN_POINT('Ctrl Pts',(8.15126276779457,-18.9657342161231,
98.1548382102798));
#111888=CARTESIAN_POINT('Ctrl Pts',(8.09243574634408,-18.9350379362716,
98.189807885219));
#111889=CARTESIAN_POINT('Ctrl Pts',(7.97432291785049,-18.8734059795942,
98.2600199598188));
#111890=CARTESIAN_POINT('Ctrl Pts',(7.86344177255187,-18.8140842306675,
98.3242349742202));
#111891=CARTESIAN_POINT('Ctrl Pts',(7.75982152702706,-18.7575887951892,
98.3829026523117));
#111892=CARTESIAN_POINT('Ctrl Pts',(7.65766080209592,-18.7018891139683,
98.4407439794915));
#111893=CARTESIAN_POINT('Ctrl Pts',(7.56255748665104,-18.6489366720524,
98.4931932096756));
#111894=CARTESIAN_POINT('Ctrl Pts',(7.47454698907051,-18.599176189517,98.5406800232808));
#111895=CARTESIAN_POINT('Ctrl Pts',(7.42545862910158,-18.5714219948916,
98.5671660660156));
#111896=CARTESIAN_POINT('Ctrl Pts',(7.37857695068473,-18.5446598983877,
98.5921083139664));
#111897=CARTESIAN_POINT('Ctrl Pts',(7.3339097744812,-18.5189601938225,98.6155810266187));
#111898=CARTESIAN_POINT('',(20.1853266918894,-19.2601884204994,66.2798123698034));
#111899=CARTESIAN_POINT('Ctrl Pts',(20.8003130805373,-19.9701890903422,
80.5583314866067));
#111900=CARTESIAN_POINT('Ctrl Pts',(20.8693517674825,-19.9348504256637,
80.3241935365105));
#111901=CARTESIAN_POINT('Ctrl Pts',(20.9340572556619,-19.8998450129912,
80.0878996375295));
#111902=CARTESIAN_POINT('Ctrl Pts',(20.9945301042509,-19.8653108990239,
79.8495426717956));
#111903=CARTESIAN_POINT('Ctrl Pts',(21.0567390479627,-19.8297853565356,
79.6043427943189));
#111904=CARTESIAN_POINT('Ctrl Pts',(21.114469100563,-19.7947582593351,79.3569593518495));
#111905=CARTESIAN_POINT('Ctrl Pts',(21.1677909493497,-19.7603764178263,
79.1074541702422));
#111906=CARTESIAN_POINT('Ctrl Pts',(21.2217202654601,-19.7256028823736,
78.8551065094565));
#111907=CARTESIAN_POINT('Ctrl Pts',(21.2711405458537,-19.69148904593,78.6005880097649));
#111908=CARTESIAN_POINT('Ctrl Pts',(21.3160825670536,-19.6581882435229,
78.3439294715529));
#111909=CARTESIAN_POINT('Ctrl Pts',(21.3613562815535,-19.6246416654977,
78.0853766723521));
#111910=CARTESIAN_POINT('Ctrl Pts',(21.4020855646709,-19.5919198042393,
77.8246516127711));
#111911=CARTESIAN_POINT('Ctrl Pts',(21.4382564880266,-19.5601862163097,
77.5617598999891));
#111912=CARTESIAN_POINT('Ctrl Pts',(21.457389480998,-19.5434003989049,77.4227005444004));
#111913=CARTESIAN_POINT('Ctrl Pts',(21.4752462723882,-19.526891246666,77.2830345749271));
#111914=CARTESIAN_POINT('Ctrl Pts',(21.4918194609359,-19.5106842624389,
77.1427606810275));
#111915=CARTESIAN_POINT('Ctrl Pts',(21.4944245268027,-19.5081367586021,
77.1207116509367));
#111916=CARTESIAN_POINT('Ctrl Pts',(21.4969978707424,-19.5055967227096,
77.0986475982832));
#111917=CARTESIAN_POINT('Ctrl Pts',(21.4995394653114,-19.5030642620853,
77.0765685070557));
#111918=CARTESIAN_POINT('Ctrl Pts',(21.530476373452,-19.4722385345451,76.8078164309129));
#111919=CARTESIAN_POINT('Ctrl Pts',(21.5565518241076,-19.4427769274193,
76.5394083958368));
#111920=CARTESIAN_POINT('Ctrl Pts',(21.5778555625257,-19.4148397515947,
76.2713465444692));
#111921=CARTESIAN_POINT('Ctrl Pts',(21.5996338853268,-19.3862802179901,
75.9973130666279));
#111922=CARTESIAN_POINT('Ctrl Pts',(21.616425632465,-19.3593134816969,75.7236407970041));
#111923=CARTESIAN_POINT('Ctrl Pts',(21.6282776573137,-19.3341145590584,
75.4503097843522));
#111924=CARTESIAN_POINT('Ctrl Pts',(21.6308381967374,-19.3286705243326,
75.3912587072136));
#111925=CARTESIAN_POINT('Ctrl Pts',(21.6331679963451,-19.3233090247849,
75.3322234956698));
#111926=CARTESIAN_POINT('Ctrl Pts',(21.6352672286914,-19.318031869621,75.2732038565701));
#111927=CARTESIAN_POINT('Ctrl Pts',(21.6449021796313,-19.2938110485219,
75.0023184883027));
#111928=CARTESIAN_POINT('Ctrl Pts',(21.6496981660391,-19.2713608165736,
74.7317683257853));
#111929=CARTESIAN_POINT('Ctrl Pts',(21.6497200847025,-19.2508299383448,
74.461543434535));
#111930=CARTESIAN_POINT('Ctrl Pts',(21.6497224177521,-19.248644606381,74.432780364311));
#111931=CARTESIAN_POINT('Ctrl Pts',(21.6496706180902,-19.2464810275705,
74.4040209596642));
#111932=CARTESIAN_POINT('Ctrl Pts',(21.649564732648,-19.2443393870614,74.3752651953395));
#111933=CARTESIAN_POINT('Ctrl Pts',(21.6490144007076,-19.2332083651463,
74.2258091864862));
#111934=CARTESIAN_POINT('Ctrl Pts',(21.6470044611232,-19.2226694685617,
74.0764521542778));
#111935=CARTESIAN_POINT('Ctrl Pts',(21.6435453264523,-19.2127466707316,
73.9271922751806));
#111936=CARTESIAN_POINT('Ctrl Pts',(21.6418157591168,-19.2077852718166,
73.852562335632));
#111937=CARTESIAN_POINT('Ctrl Pts',(21.6397238894754,-19.2029778865437,
73.7779566852953));
#111938=CARTESIAN_POINT('Ctrl Pts',(21.6372710124363,-19.1983274454553,
73.7033751000254));
#111939=CARTESIAN_POINT('Ctrl Pts',(21.6360445739167,-19.1960022249111,
73.6660843073905));
#111940=CARTESIAN_POINT('Ctrl Pts',(21.6347278833634,-19.1937162398297,
73.6287995310882));
#111941=CARTESIAN_POINT('Ctrl Pts',(21.6333211017679,-19.1914698531506,
73.591520743483));
#111942=CARTESIAN_POINT('Ctrl Pts',(21.63240594926,-19.1900085130181,73.5672698035514));
#111943=CARTESIAN_POINT('Ctrl Pts',(21.631475228432,-19.1885975748809,73.5435881702707));
#111944=CARTESIAN_POINT('Ctrl Pts',(21.6304856119411,-19.1871711967383,
73.5193697745296));
#111945=CARTESIAN_POINT('Ctrl Pts',(21.6299539800565,-19.1864049321227,
73.5063594099209));
#111946=CARTESIAN_POINT('Ctrl Pts',(21.6294051186618,-19.1856343118572,
73.4931941227504));
#111947=CARTESIAN_POINT('Ctrl Pts',(21.6288306371666,-19.1848498327995,
73.4797023206213));
#111948=CARTESIAN_POINT('Ctrl Pts',(21.6157703631309,-19.1670154698935,
73.1729794156769));
#111949=CARTESIAN_POINT('Ctrl Pts',(21.5968588497906,-19.1518257309308,
72.8673669315517));
#111950=CARTESIAN_POINT('Ctrl Pts',(21.5721718462519,-19.1392405801733,
72.56284336669));
#111951=CARTESIAN_POINT('Ctrl Pts',(21.5481808736999,-19.1270102580157,
72.2669056084043));
#111952=CARTESIAN_POINT('Ctrl Pts',(21.5187351461639,-19.1172400266441,
71.9719958689088));
#111953=CARTESIAN_POINT('Ctrl Pts',(21.4838572420696,-19.1099176660947,
71.6781041186082));
#111954=CARTESIAN_POINT('Ctrl Pts',(21.4474615106792,-19.1022766488198,
71.3714226972449));
#111955=CARTESIAN_POINT('Ctrl Pts',(21.4051507480994,-19.0973011977332,
71.0658491976107));
#111956=CARTESIAN_POINT('Ctrl Pts',(21.356898873141,-19.0950025685149,70.7613904286314));
#111957=CARTESIAN_POINT('Ctrl Pts',(21.3086469981827,-19.0927039392965,
70.4569316596521));
#111958=CARTESIAN_POINT('Ctrl Pts',(21.2544538761582,-19.0930823045507,
70.1535870956215));
#111959=CARTESIAN_POINT('Ctrl Pts',(21.1942425951636,-19.0961719049028,
69.8513897421172));
#111960=CARTESIAN_POINT('Ctrl Pts',(21.1925947750517,-19.0962564589185,
69.8431194168786));
#111961=CARTESIAN_POINT('Ctrl Pts',(21.1909424444303,-19.096343044904,69.8348499527977));
#111962=CARTESIAN_POINT('Ctrl Pts',(21.1892856007267,-19.0964316635041,
69.8265813512942));
#111963=CARTESIAN_POINT('Ctrl Pts',(21.1291719765333,-19.099646924672,69.5265798470562));
#111964=CARTESIAN_POINT('Ctrl Pts',(21.0631154256295,-19.1055357127208,
69.2276730546282));
#111965=CARTESIAN_POINT('Ctrl Pts',(20.9911889415531,-19.1140355588776,
68.9298794956225));
#111966=CARTESIAN_POINT('Ctrl Pts',(20.9222243626543,-19.1221853846119,
68.6443489617823));
#111967=CARTESIAN_POINT('Ctrl Pts',(20.8478629914071,-19.132735653614,68.3598413343251));
#111968=CARTESIAN_POINT('Ctrl Pts',(20.7681210589116,-19.1456510231459,
68.0763599944801));
#111969=CARTESIAN_POINT('Ctrl Pts',(20.6884849972535,-19.1585492453508,
67.7932550238287));
#111970=CARTESIAN_POINT('Ctrl Pts',(20.6034826469697,-19.1738061512652,
67.5111732148898));
#111971=CARTESIAN_POINT('Ctrl Pts',(20.5130832815626,-19.1914078429555,
67.230111460685));
#111972=CARTESIAN_POINT('Ctrl Pts',(20.4232562861313,-19.2088980882899,
66.9508292688561));
#111973=CARTESIAN_POINT('Ctrl Pts',(20.3281003670252,-19.2287033836298,
66.6725538637127));
#111974=CARTESIAN_POINT('Ctrl Pts',(20.2275394059576,-19.2508331871437,
66.3952817249783));
#111975=CARTESIAN_POINT('Ctrl Pts',(20.2135729243897,-19.2539067008572,
66.3567725841169));
#111976=CARTESIAN_POINT('Ctrl Pts',(20.1995021111998,-19.2570250911829,
66.3182828002111));
#111977=CARTESIAN_POINT('Ctrl Pts',(20.185326692289,-19.2601884214332,66.279812369733));
#111978=CARTESIAN_POINT('',(13.2733353822638,-20.6712011577472,53.9604717079333));
#111979=CARTESIAN_POINT('Ctrl Pts',(20.1853266911301,-19.2601884187249,
66.2798123699373));
#111980=CARTESIAN_POINT('Ctrl Pts',(19.9639238128775,-19.3096532241205,
65.6797118301511));
#111981=CARTESIAN_POINT('Ctrl Pts',(19.7324395957548,-19.3632476924122,
65.0873419883912));
#111982=CARTESIAN_POINT('Ctrl Pts',(19.4905820811039,-19.4200461661253,
64.5026985997605));
#111983=CARTESIAN_POINT('Ctrl Pts',(19.2540984564514,-19.4755826209582,
63.9310455424963));
#111984=CARTESIAN_POINT('Ctrl Pts',(19.0076974411245,-19.5341827396344,
63.3667794154196));
#111985=CARTESIAN_POINT('Ctrl Pts',(18.7510919294293,-19.5949556358985,
62.8099349966494));
#111986=CARTESIAN_POINT('Ctrl Pts',(18.5010868593336,-19.6541653235239,
62.2674138051626));
#111987=CARTESIAN_POINT('Ctrl Pts',(18.2413954218763,-19.7154377803506,
61.7319375615219));
#111988=CARTESIAN_POINT('Ctrl Pts',(17.9717387621731,-19.7779188948128,
61.2035744117988));
#111989=CARTESIAN_POINT('Ctrl Pts',(17.7264912021937,-19.8347442700271,
60.7230382611426));
#111990=CARTESIAN_POINT('Ctrl Pts',(17.4730006172305,-19.8925692715409,
60.2483861746423));
#111991=CARTESIAN_POINT('Ctrl Pts',(17.2110485793565,-19.9507253148562,
59.7796949716318));
#111992=CARTESIAN_POINT('Ctrl Pts',(16.8765459538633,-20.0249883339003,
59.1811944246422));
#111993=CARTESIAN_POINT('Ctrl Pts',(16.5282261267346,-20.0997910946465,
58.5923244407021));
#111994=CARTESIAN_POINT('Ctrl Pts',(16.1659512285725,-20.1735844006505,
58.0131600374827));
#111995=CARTESIAN_POINT('Ctrl Pts',(15.8003816564756,-20.2480488127208,
57.4287284797547));
#111996=CARTESIAN_POINT('Ctrl Pts',(15.4206023598391,-20.3214850259089,
56.8541798870247));
#111997=CARTESIAN_POINT('Ctrl Pts',(15.02646619411,-20.3922681421323,56.2895497896133));
#111998=CARTESIAN_POINT('Ctrl Pts',(14.633836087486,-20.4627807844282,55.7270772366576));
#111999=CARTESIAN_POINT('Ctrl Pts',(14.2269592157691,-20.5306601412776,
55.174447565923));
#112000=CARTESIAN_POINT('Ctrl Pts',(13.8056778443051,-20.5942727051615,
54.6316544273006));
#112001=CARTESIAN_POINT('Ctrl Pts',(13.6307190985375,-20.6206910923631,
54.4062316738221));
#112002=CARTESIAN_POINT('Ctrl Pts',(13.4532757341929,-20.6463732760865,
54.1825049800934));
#112003=CARTESIAN_POINT('Ctrl Pts',(13.2733353822638,-20.6712011577472,
53.9604717079333));
#112004=CARTESIAN_POINT('',(28.7710188797691,-10.4923807534,58.41162797882));
#112005=CARTESIAN_POINT('Ctrl Pts',(13.2733141368383,-20.6710805729304,
53.9604754110713));
#112006=CARTESIAN_POINT('Ctrl Pts',(13.9841764899668,-20.5495789480866,
54.0805152897853));
#112007=CARTESIAN_POINT('Ctrl Pts',(14.7282334585067,-20.3881365720002,
54.2176652013888));
#112008=CARTESIAN_POINT('Ctrl Pts',(15.8847581423893,-20.0711689328545,
54.4507042540058));
#112009=CARTESIAN_POINT('Ctrl Pts',(16.2769694543064,-19.9530421498621,
54.5329427913844));
#112010=CARTESIAN_POINT('Ctrl Pts',(16.873811067161,-19.7552656153632,54.6634086502063));
#112011=CARTESIAN_POINT('Ctrl Pts',(17.1743591090601,-19.6512310990377,
54.7304192850255));
#112012=CARTESIAN_POINT('Ctrl Pts',(17.528343737373,-19.5204462814834,54.8117758920654));
#112013=CARTESIAN_POINT('Ctrl Pts',(17.7061218899511,-19.4526510713967,
54.8532574786262));
#112014=CARTESIAN_POINT('Ctrl Pts',(17.8047452127824,-19.4144496322295,
54.8764440875232));
#112015=CARTESIAN_POINT('Ctrl Pts',(17.8525287220213,-19.3957608171072,
54.8877312234457));
#112016=CARTESIAN_POINT('Ctrl Pts',(17.8780285888305,-19.3857423884871,
54.8937679482584));
#112017=CARTESIAN_POINT('Ctrl Pts',(17.8826006853678,-19.3839445927825,
54.8948507695666));
#112018=CARTESIAN_POINT('Ctrl Pts',(18.3461491916568,-19.2015909106345,
55.004658230301));
#112019=CARTESIAN_POINT('Ctrl Pts',(18.9423634053891,-18.9517707804932,
55.1520850386185));
#112020=CARTESIAN_POINT('Ctrl Pts',(20.0118215345656,-18.4256300462586,
55.4349797018328));
#112021=CARTESIAN_POINT('Ctrl Pts',(20.3973067217419,-18.2248068595463,
55.5396038906132));
#112022=CARTESIAN_POINT('Ctrl Pts',(21.0135595061523,-17.877726763274,55.7129942885508));
#112023=CARTESIAN_POINT('Ctrl Pts',(21.2252972341605,-17.7543836707307,
55.7735365026662));
#112024=CARTESIAN_POINT('Ctrl Pts',(21.5515283692713,-17.5568701641081,
55.8686188214076));
#112025=CARTESIAN_POINT('Ctrl Pts',(21.7167981636613,-17.4549881517412,
55.9172275667681));
#112026=CARTESIAN_POINT('Ctrl Pts',(21.9131746404238,-17.3304278318108,
55.9758427529778));
#112027=CARTESIAN_POINT('Ctrl Pts',(21.9980755025342,-17.2757991118417,
56.0013759384972));
#112028=CARTESIAN_POINT('Ctrl Pts',(22.0548377387607,-17.239100387009,56.0184901764203));
#112029=CARTESIAN_POINT('Ctrl Pts',(22.0850046758637,-17.2194983132274,
56.0276100469492));
#112030=CARTESIAN_POINT('Ctrl Pts',(22.970607285989,-16.6414242908076,56.2959916733566));
#112031=CARTESIAN_POINT('Ctrl Pts',(23.6941088994417,-16.0887360872919,
56.5305409235564));
#112032=CARTESIAN_POINT('Ctrl Pts',(24.6061141279826,-15.3253454244035,
56.838587368009));
#112033=CARTESIAN_POINT('Ctrl Pts',(24.881279478639,-15.0816052976648,56.9339665526185));
#112034=CARTESIAN_POINT('Ctrl Pts',(25.2544866897691,-14.7370181148781,
57.0654260457647));
#112035=CARTESIAN_POINT('Ctrl Pts',(25.372297233081,-14.6256479916899,57.1073113002769));
#112036=CARTESIAN_POINT('Ctrl Pts',(25.5395659314602,-14.4643497436218,
57.1671596145233));
#112037=CARTESIAN_POINT('Ctrl Pts',(25.6208381919006,-14.3851388691851,
57.1963389343571));
#112038=CARTESIAN_POINT('Ctrl Pts',(25.7116149185979,-14.295346440036,57.2290616554915));
#112039=CARTESIAN_POINT('Ctrl Pts',(25.7560043421324,-14.2511174768788,
57.2450910710458));
#112040=CARTESIAN_POINT('Ctrl Pts',(25.779518318372,-14.2276037293349,57.253589079426));
#112041=CARTESIAN_POINT('Ctrl Pts',(25.7904192795905,-14.216679956226,57.2575305044926));
#112042=CARTESIAN_POINT('Ctrl Pts',(25.7966307490415,-14.210449915369,57.2597767868312));
#112043=CARTESIAN_POINT('Ctrl Pts',(25.7972859739144,-14.2097928030817,
57.2600137336337));
#112044=CARTESIAN_POINT('Ctrl Pts',(27.052134281417,-12.950440255771,57.7138669097972));
#112045=CARTESIAN_POINT('Ctrl Pts',(28.0205851764319,-11.680375794482,58.1013187451067));
#112046=CARTESIAN_POINT('Ctrl Pts',(28.7710188797691,-10.4923807534,58.41162797882));
#112047=CARTESIAN_POINT('',(28.0568193669707,-11.8824454183442,59.4053060271813));
#112048=CARTESIAN_POINT('Ctrl Pts',(28.7710784579986,-10.4924156479171,
58.4116174735707));
#112049=CARTESIAN_POINT('Ctrl Pts',(28.6520180730878,-10.7462094425941,
58.5794007290748));
#112050=CARTESIAN_POINT('Ctrl Pts',(28.5266025564978,-11.0009695937572,
58.7551107743632));
#112051=CARTESIAN_POINT('Ctrl Pts',(28.3944692472976,-11.2561596613471,
58.9388115563428));
#112052=CARTESIAN_POINT('Ctrl Pts',(28.2864693695974,-11.4647406486609,
59.0889603879079));
#112053=CARTESIAN_POINT('Ctrl Pts',(28.173981775152,-11.6736080079964,59.2444475481057));
#112054=CARTESIAN_POINT('Ctrl Pts',(28.0568192479267,-11.8824453353875,
59.4053060481747));
#112055=CARTESIAN_POINT('',(23.3999522636103,-18.464444554609,75.101511144554));
#112056=CARTESIAN_POINT('Ctrl Pts',(23.3999522655726,-18.464444558287,75.101511144208));
#112057=CARTESIAN_POINT('Ctrl Pts',(23.2442504171342,-18.4724359023458,
74.3034287395727));
#112058=CARTESIAN_POINT('Ctrl Pts',(23.1780163711756,-18.4339280942775,
73.5030778454822));
#112059=CARTESIAN_POINT('Ctrl Pts',(23.1802594857303,-18.3571062469603,
72.7196600622127));
#112060=CARTESIAN_POINT('Ctrl Pts',(23.180481137904,-18.3495151369095,72.6422470499488));
#112061=CARTESIAN_POINT('Ctrl Pts',(23.1813714219944,-18.3415498815759,
72.5649993563833));
#112062=CARTESIAN_POINT('Ctrl Pts',(23.1829100823713,-18.3332183575115,
72.4879354920009));
#112063=CARTESIAN_POINT('Ctrl Pts',(23.1861430175238,-18.3157126899674,
72.326013810071));
#112064=CARTESIAN_POINT('Ctrl Pts',(23.1922383893482,-18.2965900320351,
72.1649036942477));
#112065=CARTESIAN_POINT('Ctrl Pts',(23.2009883276532,-18.2759250242208,
72.0047382896764));
#112066=CARTESIAN_POINT('Ctrl Pts',(23.2101646253119,-18.2542530699494,
71.8367684851189));
#112067=CARTESIAN_POINT('Ctrl Pts',(23.2222604923313,-18.2308847946912,
71.6698377009382));
#112068=CARTESIAN_POINT('Ctrl Pts',(23.2370361194293,-18.2059062397654,
71.5040994657693));
#112069=CARTESIAN_POINT('Ctrl Pts',(23.2444239329783,-18.1934169623025,
71.4212303481849));
#112070=CARTESIAN_POINT('Ctrl Pts',(23.2524816860625,-18.1805251140686,
71.3386593679393));
#112071=CARTESIAN_POINT('Ctrl Pts',(23.2611793963984,-18.167241446654,71.2564057115819));
#112072=CARTESIAN_POINT('Ctrl Pts',(23.2655282515664,-18.1605996129467,
71.2152788834032));
#112073=CARTESIAN_POINT('Ctrl Pts',(23.2700370960191,-18.1538598243939,
71.1742313862016));
#112074=CARTESIAN_POINT('Ctrl Pts',(23.2747021816155,-18.1470234247457,
71.1332656182255));
#112075=CARTESIAN_POINT('Ctrl Pts',(23.2770347244138,-18.1436052249216,
71.1127827342374));
#112076=CARTESIAN_POINT('Ctrl Pts',(23.2794063274962,-18.1401628723206,
71.092320282556));
#112077=CARTESIAN_POINT('Ctrl Pts',(23.2818165223192,-18.1366965349008,
71.0718785629479));
#112078=CARTESIAN_POINT('Ctrl Pts',(23.2840165943302,-18.1335323956928,
71.0532189696487));
#112079=CARTESIAN_POINT('Ctrl Pts',(23.2863812828526,-18.1301605764761,
71.0334842977952));
#112080=CARTESIAN_POINT('Ctrl Pts',(23.2885475771853,-18.1270951478395,
71.0156661841902));
#112081=CARTESIAN_POINT('Ctrl Pts',(23.2887544739842,-18.1268023772022,
71.013964425287));
#112082=CARTESIAN_POINT('Ctrl Pts',(23.2889595309406,-18.1265124201898,
71.0122801319039));
#112083=CARTESIAN_POINT('Ctrl Pts',(23.2891624134535,-18.1262257361339,
71.0106159001072));
#112084=CARTESIAN_POINT('Ctrl Pts',(23.308094929816,-18.0994730579322,70.8553137241134));
#112085=CARTESIAN_POINT('Ctrl Pts',(23.3295344879901,-18.0708858315582,
70.6984480982839));
#112086=CARTESIAN_POINT('Ctrl Pts',(23.3534887181918,-18.0403985244464,
70.5402898531891));
#112087=CARTESIAN_POINT('Ctrl Pts',(23.3768886626381,-18.0106166743629,
70.3857912899808));
#112088=CARTESIAN_POINT('Ctrl Pts',(23.4026883528905,-17.9790216141216,
70.2300592039702));
#112089=CARTESIAN_POINT('Ctrl Pts',(23.4308580534758,-17.9455637192767,
70.0733780640497));
#112090=CARTESIAN_POINT('Ctrl Pts',(23.434960689978,-17.9406909099168,70.0505590155512));
#112091=CARTESIAN_POINT('Ctrl Pts',(23.4391135300745,-17.9357786088941,
70.0277198937643));
#112092=CARTESIAN_POINT('Ctrl Pts',(23.4433164126347,-17.9308266847173,
70.0048616365201));
#112093=CARTESIAN_POINT('Ctrl Pts',(23.4736395632365,-17.8950993141736,
69.8399428297306));
#112094=CARTESIAN_POINT('Ctrl Pts',(23.5065711797814,-17.8573088992603,
69.6740301896288));
#112095=CARTESIAN_POINT('Ctrl Pts',(23.5420629608149,-17.8173624707892,
69.5071378111653));
#112096=CARTESIAN_POINT('Ctrl Pts',(23.5766664919729,-17.7784157782876,
69.3444222344871));
#112097=CARTESIAN_POINT('Ctrl Pts',(23.6137037244022,-17.7374196096513,
69.1807754044067));
#112098=CARTESIAN_POINT('Ctrl Pts',(23.6530876871092,-17.6942940673088,
69.016184996999));
#112099=CARTESIAN_POINT('Ctrl Pts',(23.6666626215029,-17.6794294785841,
68.959453682301));
#112100=CARTESIAN_POINT('Ctrl Pts',(23.680515979294,-17.6643119662137,68.902610035373));
#112101=CARTESIAN_POINT('Ctrl Pts',(23.69464296705,-17.6489384467432,68.8456528067277));
#112102=CARTESIAN_POINT('Ctrl Pts',(23.7421345988904,-17.5972562665504,
68.6541759129838));
#112103=CARTESIAN_POINT('Ctrl Pts',(23.7927217955473,-17.5426802486052,
68.4614134562826));
#112104=CARTESIAN_POINT('Ctrl Pts',(23.8463804832646,-17.4850732140897,
68.2676445481524));
#112105=CARTESIAN_POINT('Ctrl Pts',(23.8950188452369,-17.4328559140378,
68.0920047273971));
#112106=CARTESIAN_POINT('Ctrl Pts',(23.9461804840968,-17.378148278424,67.9155381604963));
#112107=CARTESIAN_POINT('Ctrl Pts',(23.9998135602292,-17.3208544174594,
67.7384663116596));
#112108=CARTESIAN_POINT('Ctrl Pts',(24.0090663139398,-17.3109701068276,
67.7079179574627));
#112109=CARTESIAN_POINT('Ctrl Pts',(24.0183925442965,-17.3010088373864,
67.6773516204896));
#112110=CARTESIAN_POINT('Ctrl Pts',(24.0277914314848,-17.2909703431112,
67.6467683916423));
#112111=CARTESIAN_POINT('Ctrl Pts',(24.0532747215613,-17.2637528804033,
67.5638477993878));
#112112=CARTESIAN_POINT('Ctrl Pts',(24.0792923072638,-17.2359676727507,
67.4808029949137));
#112113=CARTESIAN_POINT('Ctrl Pts',(24.1058261298632,-17.2076098987618,
67.3976560725148));
#112114=CARTESIAN_POINT('Ctrl Pts',(24.1190930411629,-17.1934310117674,
67.3560826113154));
#112115=CARTESIAN_POINT('Ctrl Pts',(24.1324890037314,-17.1791089716587,
67.3144836220376));
#112116=CARTESIAN_POINT('Ctrl Pts',(24.1460114838888,-17.1646432685094,
67.2728619224439));
#112117=CARTESIAN_POINT('Ctrl Pts',(24.1527727239675,-17.1574104169348,
67.252051072647));
#112118=CARTESIAN_POINT('Ctrl Pts',(24.159565592941,-17.1501416488662,67.2312345453598));
#112119=CARTESIAN_POINT('Ctrl Pts',(24.1663897642528,-17.1428369009422,
67.2104126946916));
#112120=CARTESIAN_POINT('Ctrl Pts',(24.1698018499088,-17.1391845269801,
67.2000017693575));
#112121=CARTESIAN_POINT('Ctrl Pts',(24.1732217611164,-17.135523158007,67.189589513184));
#112122=CARTESIAN_POINT('Ctrl Pts',(24.1766494560711,-17.1318527863852,
67.1791759706309));
#112123=CARTESIAN_POINT('Ctrl Pts',(24.1792202272872,-17.1291000076689,
67.1713658137161));
#112124=CARTESIAN_POINT('Ctrl Pts',(24.1817953768583,-17.1263421649588,
67.1635549332133));
#112125=CARTESIAN_POINT('Ctrl Pts',(24.1843748869266,-17.1235792550871,
67.1557433479229));
#112126=CARTESIAN_POINT('Ctrl Pts',(24.1852347236161,-17.1226582851298,
67.1531394861594));
#112127=CARTESIAN_POINT('Ctrl Pts',(24.1856906524357,-17.1221699380917,
67.1517588717565));
#112128=CARTESIAN_POINT('Ctrl Pts',(24.1869558498151,-17.1208146560523,
67.1479315284031));
#112129=CARTESIAN_POINT('Ctrl Pts',(24.2387975889492,-17.0652816782834,
66.991105298017));
#112130=CARTESIAN_POINT('Ctrl Pts',(24.2917423143794,-17.0084117511973,
66.8360284700413));
#112131=CARTESIAN_POINT('Ctrl Pts',(24.3455586218895,-16.9502826065249,
66.6827206321942));
#112132=CARTESIAN_POINT('Ctrl Pts',(24.4660146818045,-16.8201732018215,
66.3395744938665));
#112133=CARTESIAN_POINT('Ctrl Pts',(24.590837042828,-16.6837553719516,66.0052910913828));
#112134=CARTESIAN_POINT('Ctrl Pts',(24.7188691138333,-16.5407604417291,
65.6781616273983));
#112135=CARTESIAN_POINT('Ctrl Pts',(24.8016663349788,-16.4482868703236,
65.4666098625941));
#112136=CARTESIAN_POINT('Ctrl Pts',(24.8858059845019,-16.3530626625801,
65.2580498152435));
#112137=CARTESIAN_POINT('Ctrl Pts',(24.971082998648,-16.2551183064043,65.0525478755764));
#112138=CARTESIAN_POINT('Ctrl Pts',(25.0170926495023,-16.2022742232019,
64.9416730684712));
#112139=CARTESIAN_POINT('Ctrl Pts',(25.0634333874147,-16.1486383100985,
64.8316884608845));
#112140=CARTESIAN_POINT('Ctrl Pts',(25.1100730529789,-16.0942152806723,
64.7226044908374));
#112141=CARTESIAN_POINT('Ctrl Pts',(25.133392885761,-16.0670037659592,64.6680625058139));
#112142=CARTESIAN_POINT('Ctrl Pts',(25.1567874502383,-16.0395954719033,
64.6137456802135));
#112143=CARTESIAN_POINT('Ctrl Pts',(25.1802527304421,-16.0119909817087,
64.5596553197284));
#112144=CARTESIAN_POINT('Ctrl Pts',(25.2007848506203,-15.9878370527884,
64.5123262543039));
#112145=CARTESIAN_POINT('Ctrl Pts',(25.2213711125132,-15.963532911182,64.4651705762356));
#112146=CARTESIAN_POINT('Ctrl Pts',(25.2420088260471,-15.9390789460828,
64.4181891604787));
#112147=CARTESIAN_POINT('Ctrl Pts',(25.2449570708376,-15.9355855224972,
64.4114775296563));
#112148=CARTESIAN_POINT('Ctrl Pts',(25.2485512358567,-15.9313241295077,
64.4033040151405));
#112149=CARTESIAN_POINT('Ctrl Pts',(25.2508567027187,-15.9285895035509,
64.3980649396906));
#112150=CARTESIAN_POINT('Ctrl Pts',(25.3407766308797,-15.8219311196724,
64.1937257249921));
#112151=CARTESIAN_POINT('Ctrl Pts',(25.4304975710006,-15.7138504718903,
63.9955752199972));
#112152=CARTESIAN_POINT('Ctrl Pts',(25.5197348311737,-15.6046045178627,
63.8034270030152));
#112153=CARTESIAN_POINT('Ctrl Pts',(25.6111577516963,-15.4926828367948,
63.6065725597521));
#112154=CARTESIAN_POINT('Ctrl Pts',(25.7020723508946,-15.3795390166899,
63.4160187616832));
#112155=CARTESIAN_POINT('Ctrl Pts',(25.7921676115896,-15.2654993087428,
63.2316090580315));
#112156=CARTESIAN_POINT('Ctrl Pts',(25.8305858240952,-15.2168707604686,
63.1529734990873));
#112157=CARTESIAN_POINT('Ctrl Pts',(25.8688556221805,-15.1680790293793,
63.0754549574394));
#112158=CARTESIAN_POINT('Ctrl Pts',(25.9069553595192,-15.1191481839815,
62.9990405418654));
#112159=CARTESIAN_POINT('Ctrl Pts',(25.9427321045609,-15.0732007181261,
62.9272852161212));
#112160=CARTESIAN_POINT('Ctrl Pts',(25.9783589090034,-15.0271305776088,
62.856503476091));
#112161=CARTESIAN_POINT('Ctrl Pts',(26.0138189917453,-14.9809571170856,
62.7866843092614));
#112162=CARTESIAN_POINT('Ctrl Pts',(26.0315490331163,-14.957870386824,62.7517747258466));
#112163=CARTESIAN_POINT('Ctrl Pts',(26.0492373984288,-14.9347578310493,
62.7171057849726));
#112164=CARTESIAN_POINT('Ctrl Pts',(26.0668821056934,-14.9116218032023,
62.6826760758216));
#112165=CARTESIAN_POINT('Ctrl Pts',(26.0757044593257,-14.9000537892788,
62.6654612212461));
#112166=CARTESIAN_POINT('Ctrl Pts',(26.0845158987059,-14.8884799076072,
62.6483061745562));
#112167=CARTESIAN_POINT('Ctrl Pts',(26.0933161800254,-14.8769004515561,
62.6312107583831));
#112168=CARTESIAN_POINT('Ctrl Pts',(26.099916391015,-14.8682158595178,62.6183891962533));
#112169=CARTESIAN_POINT('Ctrl Pts',(26.1065103256176,-14.8595281319135,
62.6056011762853));
#112170=CARTESIAN_POINT('Ctrl Pts',(26.1130978824016,-14.8508373918367,
62.5928466232461));
#112171=CARTESIAN_POINT('Ctrl Pts',(26.1152937346629,-14.8479404784777,
62.5885951055664));
#112172=CARTESIAN_POINT('Ctrl Pts',(26.1183068164103,-14.8439632058128,
62.5827653942718));
#112173=CARTESIAN_POINT('Ctrl Pts',(26.1196833095973,-14.8421456520831,
62.580103223031));
#112174=CARTESIAN_POINT('Ctrl Pts',(26.1495148755876,-14.8027553561176,
62.5224082501823));
#112175=CARTESIAN_POINT('Ctrl Pts',(26.182170738001,-14.7594242261849,62.4597989844644));
#112176=CARTESIAN_POINT('Ctrl Pts',(26.2176473167757,-14.7119972228234,
62.3925134181239));
#112177=CARTESIAN_POINT('Ctrl Pts',(26.2526277367343,-14.6652335113195,
62.3261688762026));
#112178=CARTESIAN_POINT('Ctrl Pts',(26.2903508399422,-14.6144875115488,
62.2552778627649));
#112179=CARTESIAN_POINT('Ctrl Pts',(26.3308008173732,-14.5595899140302,
62.1801130968392));
#112180=CARTESIAN_POINT('Ctrl Pts',(26.3415601610262,-14.544987628567,62.1601199201168));
#112181=CARTESIAN_POINT('Ctrl Pts',(26.3525123514416,-14.5300915053854,
62.1398246195584));
#112182=CARTESIAN_POINT('Ctrl Pts',(26.3636568951483,-14.5148981324929,
62.1192328782769));
#112183=CARTESIAN_POINT('Ctrl Pts',(26.4046448515626,-14.4590191909865,
62.0434995493625));
#112184=CARTESIAN_POINT('Ctrl Pts',(26.4482349442434,-14.3991219719376,
61.9637532974569));
#112185=CARTESIAN_POINT('Ctrl Pts',(26.4944163670492,-14.3350007186598,
61.8802978336112));
#112186=CARTESIAN_POINT('Ctrl Pts',(26.5412166875894,-14.2700201480208,
61.7957239460714));
#112187=CARTESIAN_POINT('Ctrl Pts',(26.5906783534958,-14.2007018204385,
61.7073405613577));
#112188=CARTESIAN_POINT('Ctrl Pts',(26.6427848634371,-14.126797388866,61.6155069626122));
#112189=CARTESIAN_POINT('Ctrl Pts',(26.6948913733785,-14.0528929572935,
61.5236733638667));
#112190=CARTESIAN_POINT('Ctrl Pts',(26.7496428216296,-13.9744026194313,
61.4283894311402));
#112191=CARTESIAN_POINT('Ctrl Pts',(26.8070160790248,-13.8910407683245,
61.3300596385221));
#112192=CARTESIAN_POINT('Ctrl Pts',(26.8286817045993,-13.8595611777403,
61.2929277661759));
#112193=CARTESIAN_POINT('Ctrl Pts',(26.8507211285977,-13.8273865079625,
61.2553620201456));
#112194=CARTESIAN_POINT('Ctrl Pts',(26.8731328192345,-13.7944999020021,
61.2173859214206));
#112195=CARTESIAN_POINT('Ctrl Pts',(26.8843386645529,-13.7780565990218,
61.1983978720581));
#112196=CARTESIAN_POINT('Ctrl Pts',(26.895637567286,-13.7614353038493,61.1793072361356));
#112197=CARTESIAN_POINT('Ctrl Pts',(26.9070293274744,-13.7446338246987,
61.1601170608852));
#112198=CARTESIAN_POINT('Ctrl Pts',(26.9127252075685,-13.7362330851234,
61.1505219732599));
#112199=CARTESIAN_POINT('Ctrl Pts',(26.9184443014333,-13.7277872990275,
61.1409020009062));
#112200=CARTESIAN_POINT('Ctrl Pts',(26.9241865818617,-13.7192961882546,
61.1312575281269));
#112201=CARTESIAN_POINT('Ctrl Pts',(26.927057722076,-13.7150506328682,61.1264352917372));
#112202=CARTESIAN_POINT('Ctrl Pts',(26.9299346588935,-13.7107937462796,
61.1216069302478));
#112203=CARTESIAN_POINT('Ctrl Pts',(26.9328173888506,-13.7065254933995,
61.1167724920681));
#112204=CARTESIAN_POINT('Ctrl Pts',(26.9342587538292,-13.7043913669594,
61.1143552729782));
#112205=CARTESIAN_POINT('Ctrl Pts',(26.9357015670903,-13.7022543989444,
61.1119365347162));
#112206=CARTESIAN_POINT('Ctrl Pts',(26.9371458281976,-13.7001145849478,
61.1095162833576));
#112207=CARTESIAN_POINT('Ctrl Pts',(26.9385900893049,-13.6979747709512,
61.107096031999));
#112208=CARTESIAN_POINT('Ctrl Pts',(26.9393230538677,-13.6968888043132,
61.1058677620329));
#112209=CARTESIAN_POINT('Ctrl Pts',(26.9414829546153,-13.6936866005958,
61.1022509960756));
#112210=CARTESIAN_POINT('Ctrl Pts',(27.0187193827629,-13.5791782012597,
60.9729181624769));
#112211=CARTESIAN_POINT('Ctrl Pts',(27.0923797168953,-13.4679359954866,
60.8520372952937));
#112212=CARTESIAN_POINT('Ctrl Pts',(27.1624720225538,-13.3603870981355,
60.7389430187677));
#112213=CARTESIAN_POINT('Ctrl Pts',(27.2311829274812,-13.2549578075519,
60.6280776390487));
#112214=CARTESIAN_POINT('Ctrl Pts',(27.296465288087,-13.1530780797369,60.5246948441136));
#112215=CARTESIAN_POINT('Ctrl Pts',(27.3583354933923,-13.0551344576139,
60.4282135322513));
#112216=CARTESIAN_POINT('Ctrl Pts',(27.4185576656764,-12.9597997539951,
60.3343021874207));
#112217=CARTESIAN_POINT('Ctrl Pts',(27.4755472245224,-12.8681945215141,
60.246929548252));
#112218=CARTESIAN_POINT('Ctrl Pts',(27.5293246809172,-12.7806553500093,
60.1656041894029));
#112219=CARTESIAN_POINT('Ctrl Pts',(27.5656780519623,-12.7214791785048,
60.11062853336));
#112220=CARTESIAN_POINT('Ctrl Pts',(27.600563690595,-12.6641606650941,60.0584172229083));
#112221=CARTESIAN_POINT('Ctrl Pts',(27.6339887949749,-12.6087975633783,
60.0088304806025));
#112222=CARTESIAN_POINT('Ctrl Pts',(27.6818519320055,-12.529520272461,59.9378246577062));
#112223=CARTESIAN_POINT('Ctrl Pts',(27.7267202670337,-12.4542537088115,
59.8721985660002));
#112224=CARTESIAN_POINT('Ctrl Pts',(27.7686161579487,-12.3832641878405,
59.8115780830282));
#112225=CARTESIAN_POINT('Ctrl Pts',(27.8100628946962,-12.3130357257345,
59.7516074953553));
#112226=CARTESIAN_POINT('Ctrl Pts',(27.848600669005,-12.2469932419356,59.6965357243602));
#112227=CARTESIAN_POINT('Ctrl Pts',(27.8842512191725,-12.1853682390402,
59.6460434001692));
#112228=CARTESIAN_POINT('Ctrl Pts',(27.91939608697,-12.1246173510566,59.5962672803017));
#112229=CARTESIAN_POINT('Ctrl Pts',(27.9517351264143,-12.0681596070252,
59.5509416213708));
#112230=CARTESIAN_POINT('Ctrl Pts',(27.9812880817654,-12.0161893006359,
59.5098025229151));
#112231=CARTESIAN_POINT('Ctrl Pts',(28.0088908883515,-11.9676484255036,
59.4713781229079));
#112232=CARTESIAN_POINT('Ctrl Pts',(28.0340632047671,-11.9230221225772,
59.4366063232373));
#112233=CARTESIAN_POINT('Ctrl Pts',(28.0568195157664,-11.8824455220351,
59.4053060009392));
#112234=CARTESIAN_POINT('',(38.6333985430991,-1.20459248512199,98.36583228337));
#112235=CARTESIAN_POINT('Ctrl Pts',(38.6333985430991,-1.20459248512199,
98.36583228337));
#112236=CARTESIAN_POINT('Ctrl Pts',(38.5366002152195,-2.46830688119351,
98.2349959150518));
#112237=CARTESIAN_POINT('Ctrl Pts',(38.0688555603353,-4.89683171878626,
97.6805363924601));
#112238=CARTESIAN_POINT('Ctrl Pts',(37.1095611647792,-7.15936829257837,
96.5833073808643));
#112239=CARTESIAN_POINT('Ctrl Pts',(36.2609354234713,-8.73058637062551,
95.6084465035992));
#112240=CARTESIAN_POINT('Ctrl Pts',(35.6521334167721,-9.73616974679085,
94.9078930628315));
#112241=CARTESIAN_POINT('Ctrl Pts',(34.9681261465269,-10.6688054360461,
94.1123973243883));
#112242=CARTESIAN_POINT('Ctrl Pts',(33.8978354227833,-12.0086232552646,
92.8564947258115));
#112243=CARTESIAN_POINT('Ctrl Pts',(33.1279964816629,-12.8209446465096,
91.9377075741904));
#112244=CARTESIAN_POINT('Ctrl Pts',(31.5241780468789,-14.2851195759495,
89.9695310692828));
#112245=CARTESIAN_POINT('Ctrl Pts',(30.6848812388159,-14.9412747048976,
88.91639447817));
#112246=CARTESIAN_POINT('Ctrl Pts',(29.4134476720632,-15.813447849705,87.2192561730067));
#112247=CARTESIAN_POINT('Ctrl Pts',(28.5629570853225,-16.3564140531643,
86.0495465015485));
#112248=CARTESIAN_POINT('Ctrl Pts',(27.308980739206,-17.0508777267664,84.1836367945689));
#112249=CARTESIAN_POINT('Ctrl Pts',(26.0883942100227,-17.6290940152154,
82.178465418237));
#112250=CARTESIAN_POINT('Ctrl Pts',(24.5910880959154,-18.2270657215307,
79.2772309226755));
#112251=CARTESIAN_POINT('Ctrl Pts',(23.7402842168438,-18.4469370871498,
76.8455281617186));
#112252=CARTESIAN_POINT('Ctrl Pts',(23.3999522626291,-18.46444455277,75.101511144727));
#112253=CARTESIAN_POINT('',(38.6794466444702,5.17649275224089E-11,98.4280216145082));
#112254=CARTESIAN_POINT('Origin',(31.1126367795517,0.000775488753213954,
88.2087611921047));
#112255=CARTESIAN_POINT('',(41.1972044619337,1.16390964369926E-14,112.706776537994));
#112256=CARTESIAN_POINT('',(38.4704302935856,1.16390964369926E-14,97.2424717708351));
#112257=CARTESIAN_POINT('Origin',(20.5162416486691,1.4210854715202E-14,
116.353388269));
#112258=CARTESIAN_POINT('',(38.6333954984551,1.20463046397926,98.3658274732794));
#112259=CARTESIAN_POINT('Origin',(31.1126367795517,0.000775488753213954,
88.2087611921047));
#112260=CARTESIAN_POINT('',(23.3999522626816,18.4644445525526,75.101511144713));
#112261=CARTESIAN_POINT('Ctrl Pts',(23.3999522612866,18.4644445499379,75.101511144959));
#112262=CARTESIAN_POINT('Ctrl Pts',(23.45961890053,18.461375785637,75.4072770176154));
#112263=CARTESIAN_POINT('Ctrl Pts',(23.5261343935816,18.4542914438561,75.7091799541492));
#112264=CARTESIAN_POINT('Ctrl Pts',(23.5991425426504,18.4433532934531,76.0075409544095));
#112265=CARTESIAN_POINT('Ctrl Pts',(23.676959267289,18.4316947176801,76.3255530680745));
#112266=CARTESIAN_POINT('Ctrl Pts',(23.7621520465881,18.4156577543503,76.6395413160084));
#112267=CARTESIAN_POINT('Ctrl Pts',(23.8542600959466,18.3953847954478,76.949899589864));
#112268=CARTESIAN_POINT('Ctrl Pts',(23.9198098214053,18.3809573170726,77.1707695332269));
#112269=CARTESIAN_POINT('Ctrl Pts',(23.9888612270989,18.3643832927569,77.3898011465229));
#112270=CARTESIAN_POINT('Ctrl Pts',(24.0612402519916,18.3457004295971,77.6071378070134));
#112271=CARTESIAN_POINT('Ctrl Pts',(24.1957690600846,18.3109751301561,78.0110951956914));
#112272=CARTESIAN_POINT('Ctrl Pts',(24.3417937836676,18.2689668465408,78.4091970786755));
#112273=CARTESIAN_POINT('Ctrl Pts',(24.4971961404488,18.2202185729628,78.8006560385329));
#112274=CARTESIAN_POINT('Ctrl Pts',(24.6531129926202,18.1713089069675,79.1934110136793));
#112275=CARTESIAN_POINT('Ctrl Pts',(24.818467695171,18.1156103124022,79.5794793560188));
#112276=CARTESIAN_POINT('Ctrl Pts',(24.9910976581544,18.0536592348641,79.9580698919787));
#112277=CARTESIAN_POINT('Ctrl Pts',(25.1634427984296,17.9918103705998,80.3360357902462));
#112278=CARTESIAN_POINT('Ctrl Pts',(25.3430368339901,17.9237286179672,80.7065489563957));
#112279=CARTESIAN_POINT('Ctrl Pts',(25.528086338763,17.8498440729799,81.0694906196872));
#112280=CARTESIAN_POINT('Ctrl Pts',(25.6880971184625,17.7859567166441,81.3833232808445));
#112281=CARTESIAN_POINT('Ctrl Pts',(25.8521862832049,17.7177302616557,81.6914949014036));
#112282=CARTESIAN_POINT('Ctrl Pts',(26.0192052724661,17.6454844942854,81.993926765999));
#112283=CARTESIAN_POINT('Ctrl Pts',(26.0453406526073,17.6341793690289,82.0412517545107));
#112284=CARTESIAN_POINT('Ctrl Pts',(26.0715478076392,17.6227759234653,82.0884361907658));
#112285=CARTESIAN_POINT('Ctrl Pts',(26.0978223780965,17.6112754976626,82.1354797658442));
#112286=CARTESIAN_POINT('Ctrl Pts',(26.302079891663,17.5218716239349,82.501194733113));
#112287=CARTESIAN_POINT('Ctrl Pts',(26.5104101217341,17.4266045074234,82.8583970920815));
#112288=CARTESIAN_POINT('Ctrl Pts',(26.7220462389472,17.3255160396653,83.2087303809841));
#112289=CARTESIAN_POINT('Ctrl Pts',(26.9128055892252,17.2343994066253,83.524505171468));
#112290=CARTESIAN_POINT('Ctrl Pts',(27.1062503495027,17.1385532496861,83.8346993201741));
#112291=CARTESIAN_POINT('Ctrl Pts',(27.3018210400026,17.0380447426029,84.1405160230136));
#112292=CARTESIAN_POINT('Ctrl Pts',(27.5080933913095,16.9320363932463,84.4630670668454));
#112293=CARTESIAN_POINT('Ctrl Pts',(27.7167216246146,16.8208468487113,84.7807500887177));
#112294=CARTESIAN_POINT('Ctrl Pts',(27.926810630039,16.7045966516856,85.0934841667746));
#112295=CARTESIAN_POINT('Ctrl Pts',(28.1227320257951,16.5961859292292,85.3851286388382));
#112296=CARTESIAN_POINT('Ctrl Pts',(28.3199235433799,16.4833742725223,85.6724691858054));
#112297=CARTESIAN_POINT('Ctrl Pts',(28.5176729072871,16.3663061368233,85.9554377650852));
#112298=CARTESIAN_POINT('Ctrl Pts',(28.711664099302,16.2514628486201,86.2330286048869));
#112299=CARTESIAN_POINT('Ctrl Pts',(28.9061918146068,16.1325232534556,86.5064121306224));
#112300=CARTESIAN_POINT('Ctrl Pts',(29.1006016876849,16.0096699843988,86.775520920119));
#112301=CARTESIAN_POINT('Ctrl Pts',(29.2910029919315,15.8893498469027,87.0390809116622));
#112302=CARTESIAN_POINT('Ctrl Pts',(29.481290996414,15.7652757942784,87.2985406796168));
#112303=CARTESIAN_POINT('Ctrl Pts',(29.6708727721434,15.6376644893672,87.5538330451626));
#112304=CARTESIAN_POINT('Ctrl Pts',(29.7251711571417,15.6011151547197,87.6269516932932));
#112305=CARTESIAN_POINT('Ctrl Pts',(29.7794117619617,15.5642759399319,87.699728456207));
#112306=CARTESIAN_POINT('Ctrl Pts',(29.8335810411833,15.5271526278358,87.7721616876146));
#112307=CARTESIAN_POINT('Ctrl Pts',(30.0748187458443,15.3618275076167,88.0947361567057));
#112308=CARTESIAN_POINT('Ctrl Pts',(30.3146457647922,15.19086977782,88.4104967426328));
#112309=CARTESIAN_POINT('Ctrl Pts',(30.5529445467657,15.0139252472042,88.719987132609));
#112310=CARTESIAN_POINT('Ctrl Pts',(30.7879734861698,14.8394086801468,89.0252308166492));
#112311=CARTESIAN_POINT('Ctrl Pts',(31.0215160082487,14.6590682647923,89.3243751689556));
#112312=CARTESIAN_POINT('Ctrl Pts',(31.2534107667758,14.4725553129748,89.61795036547));
#112313=CARTESIAN_POINT('Ctrl Pts',(31.4804877752156,14.2899172775012,89.9054263644965));
#112314=CARTESIAN_POINT('Ctrl Pts',(31.7059848681178,14.1013602822068,90.187562192574));
#112315=CARTESIAN_POINT('Ctrl Pts',(31.9297018364177,13.9065516870498,90.4648642524105));
#112316=CARTESIAN_POINT('Ctrl Pts',(32.056649470055,13.796008037387,90.6222186121021));
#112317=CARTESIAN_POINT('Ctrl Pts',(32.183023011221,13.6834513153511,90.7780166729506));
#112318=CARTESIAN_POINT('Ctrl Pts',(32.3087784870946,13.5688204265169,90.9323522662342));
#112319=CARTESIAN_POINT('Ctrl Pts',(32.5174358981477,13.3786212775358,91.1884307002285));
#112320=CARTESIAN_POINT('Ctrl Pts',(32.724388686809,13.1827084851237,91.4404834298436));
#112321=CARTESIAN_POINT('Ctrl Pts',(32.9289295915244,12.9812207204148,91.6880188239592));
#112322=CARTESIAN_POINT('Ctrl Pts',(33.1315961155715,12.7815793578794,91.9332858426707));
#112323=CARTESIAN_POINT('Ctrl Pts',(33.3318944302162,12.5764647539265,92.1741179965264));
#112324=CARTESIAN_POINT('Ctrl Pts',(33.529153850941,12.3660592360816,92.4100339942283));
#112325=CARTESIAN_POINT('Ctrl Pts',(33.7240072615387,12.1582200737743,92.6430724802884));
#112326=CARTESIAN_POINT('Ctrl Pts',(33.9158951642116,11.9452183770992,92.8713140571761));
#112327=CARTESIAN_POINT('Ctrl Pts',(34.1041926695823,11.7272754394601,93.0942910306846));
#112328=CARTESIAN_POINT('Ctrl Pts',(34.2734101142786,11.5314165143814,93.2946738961344));
#112329=CARTESIAN_POINT('Ctrl Pts',(34.4397280338224,11.3315676163555,93.4908050009544));
#112330=CARTESIAN_POINT('Ctrl Pts',(34.6027109913217,11.127920264297,93.6823417145347));
#112331=CARTESIAN_POINT('Ctrl Pts',(34.7990850568156,10.8825506927515,93.9131194824327));
#112332=CARTESIAN_POINT('Ctrl Pts',(34.9906219329704,10.6316734309369,94.1372267151763));
#112333=CARTESIAN_POINT('Ctrl Pts',(35.1769653584792,10.3750945491389,94.3544033086576));
#112334=CARTESIAN_POINT('Ctrl Pts',(35.3608788294736,10.1218615058667,94.5687478771169));
#112335=CARTESIAN_POINT('Ctrl Pts',(35.5397334897653,9.8630742641629,94.7763413681739));
#112336=CARTESIAN_POINT('Ctrl Pts',(35.7131380216892,9.59855363349448,94.9769423280029));
#112337=CARTESIAN_POINT('Ctrl Pts',(35.8829721861427,9.33947943403824,95.1734129509049));
#112338=CARTESIAN_POINT('Ctrl Pts',(36.047578338922,9.07490522105732,95.3631760292744));
#112339=CARTESIAN_POINT('Ctrl Pts',(36.2065413023706,8.80467404873674,95.5460131008675));
#112340=CARTESIAN_POINT('Ctrl Pts',(36.3181117639983,8.61500838078534,95.6743399515864));
#112341=CARTESIAN_POINT('Ctrl Pts',(36.4269013338651,8.42255624048273,95.7992551285144));
#112342=CARTESIAN_POINT('Ctrl Pts',(36.5327520178202,8.22726805508603,95.9206856461797));
#112343=CARTESIAN_POINT('Ctrl Pts',(36.6634217362688,7.9861902344369,96.0705882350107));
#112344=CARTESIAN_POINT('Ctrl Pts',(36.7896095664863,7.74078502350917,96.2151810512529));
#112345=CARTESIAN_POINT('Ctrl Pts',(36.9107931256386,7.49140320525122,96.354049383852));
#112346=CARTESIAN_POINT('Ctrl Pts',(37.0308658560298,7.24430734474327,96.491644780263));
#112347=CARTESIAN_POINT('Ctrl Pts',(37.1460254141818,6.99330765368619,96.6236201984513));
#112348=CARTESIAN_POINT('Ctrl Pts',(37.2558003327317,6.73878044478437,96.7495657595519));
#112349=CARTESIAN_POINT('Ctrl Pts',(37.3650785385787,6.48540492790448,96.874941438562));
#112350=CARTESIAN_POINT('Ctrl Pts',(37.4690205017941,6.22853395672561,96.9943417443013));
#112351=CARTESIAN_POINT('Ctrl Pts',(37.5672010075701,5.96857059401915,97.1073553044701));
#112352=CARTESIAN_POINT('Ctrl Pts',(37.6648629078788,5.70998040025437,97.2197719085555));
#112353=CARTESIAN_POINT('Ctrl Pts',(37.7568238718426,5.44833064182346,97.3258690929956));
#112354=CARTESIAN_POINT('Ctrl Pts',(37.8427079581854,5.18404618060724,97.4252344635266));
#112355=CARTESIAN_POINT('Ctrl Pts',(37.8758234340989,5.08214248596012,97.4635480985035));
#112356=CARTESIAN_POINT('Ctrl Pts',(37.9080358982251,4.97984735659777,97.5008608021213));
#112357=CARTESIAN_POINT('Ctrl Pts',(37.9393255877055,4.87718615189641,97.5371486179259));
#112358=CARTESIAN_POINT('Ctrl Pts',(38.0405433699397,4.54509147042374,97.6545346418482));
#112359=CARTESIAN_POINT('Ctrl Pts',(38.1321140636492,4.2091457966541,97.7611943001836));
#112360=CARTESIAN_POINT('Ctrl Pts',(38.2136417514429,3.86940501031531,97.8567832599188));
#112361=CARTESIAN_POINT('Ctrl Pts',(38.294046705557,3.53434286056575,97.9510558454578));
#112362=CARTESIAN_POINT('Ctrl Pts',(38.3646832865444,3.19558900540544,98.0345605588972));
#112363=CARTESIAN_POINT('Ctrl Pts',(38.4251283250865,2.85322082336216,98.1069747477039));
#112364=CARTESIAN_POINT('Ctrl Pts',(38.484275895867,2.5182016593606,98.1778345479666));
#112365=CARTESIAN_POINT('Ctrl Pts',(38.5336646070965,2.17972133100617,98.2380748616099));
#112366=CARTESIAN_POINT('Ctrl Pts',(38.5728578338096,1.83788060811413,98.2874004459044));
#112367=CARTESIAN_POINT('Ctrl Pts',(38.5969153115092,1.62805288384956,98.3176773392277));
#112368=CARTESIAN_POINT('Ctrl Pts',(38.6171306416519,1.41695963082921,98.3438420099546));
#112369=CARTESIAN_POINT('Ctrl Pts',(38.6333954797472,1.20463046288776,98.365827476578));
#112370=CARTESIAN_POINT('',(28.0568193311413,11.8824453975844,59.4053060263899));
#112371=CARTESIAN_POINT('Ctrl Pts',(28.0568193741291,11.88244542754,59.40530601881));
#112372=CARTESIAN_POINT('Ctrl Pts',(27.7243204687509,12.4753479870479,59.8627458820805));
#112373=CARTESIAN_POINT('Ctrl Pts',(27.3871488482182,13.0249815959646,60.3740379473461));
#112374=CARTESIAN_POINT('Ctrl Pts',(26.7070209696829,14.050902424375,61.4995241253409));
#112375=CARTESIAN_POINT('Ctrl Pts',(26.3632478725192,14.528011115418,62.1138216849645));
#112376=CARTESIAN_POINT('Ctrl Pts',(25.9349524358028,15.083850920924,62.9426971932013));
#112377=CARTESIAN_POINT('Ctrl Pts',(25.8387793290717,15.2065182721143,63.132611768099));
#112378=CARTESIAN_POINT('Ctrl Pts',(25.7430785079378,15.3263951382971,63.326297480956));
#112379=CARTESIAN_POINT('Ctrl Pts',(25.7218241106203,15.3529652490661,63.3694316382038));
#112380=CARTESIAN_POINT('Ctrl Pts',(25.7127984000554,15.3642261876238,63.3878072603337));
#112381=CARTESIAN_POINT('Ctrl Pts',(25.6840150790617,15.4000878249556,63.4465935348418));
#112382=CARTESIAN_POINT('Ctrl Pts',(25.6265681449639,15.4714305157428,63.5646879742171));
#112383=CARTESIAN_POINT('Ctrl Pts',(25.5695017601332,15.5416253702554,63.6843333208089));
#112384=CARTESIAN_POINT('Ctrl Pts',(25.3802203896199,15.7730314350455,64.0865319974358));
#112385=CARTESIAN_POINT('Ctrl Pts',(25.2318102003903,15.9499041554838,64.4191291739736));
#112386=CARTESIAN_POINT('Ctrl Pts',(25.0153167124731,16.2025590137327,64.9319759177368));
#112387=CARTESIAN_POINT('Ctrl Pts',(24.9085991289255,16.3257238429192,65.1918868774778));
#112388=CARTESIAN_POINT('Ctrl Pts',(24.7914467284545,16.4588957048741,65.4896866658859));
#112389=CARTESIAN_POINT('Ctrl Pts',(24.7442899524852,16.5121400547645,65.6119756838965));
#112390=CARTESIAN_POINT('Ctrl Pts',(24.7293361171015,16.528993566515,65.6509679401623));
#112391=CARTESIAN_POINT('Ctrl Pts',(24.726687619279,16.5319774138165,65.6578821834526));
#112392=CARTESIAN_POINT('Ctrl Pts',(24.724218261392,16.5347587713352,65.6643313770844));
#112393=CARTESIAN_POINT('Ctrl Pts',(24.7130624479885,16.5473202637082,65.6934702352849));
#112394=CARTESIAN_POINT('Ctrl Pts',(24.7015138760334,16.5602890191069,65.7236674345157));
#112395=CARTESIAN_POINT('Ctrl Pts',(24.606377727762,16.6668599454623,65.972849716348));
#112396=CARTESIAN_POINT('Ctrl Pts',(24.5020068601432,16.7818280567286,66.2480874865797));
#112397=CARTESIAN_POINT('Ctrl Pts',(24.2621677955456,17.0412413761153,66.9193266199932));
#112398=CARTESIAN_POINT('Ctrl Pts',(24.1265333019407,17.1856918201085,67.3151772540794));
#112399=CARTESIAN_POINT('Ctrl Pts',(23.9662642473337,17.3560993520012,67.8417223220284));
#112400=CARTESIAN_POINT('Ctrl Pts',(23.9461197147708,17.3775202437756,67.9088199119513));
#112401=CARTESIAN_POINT('Ctrl Pts',(23.9258821889579,17.3990529752298,67.97739921814));
#112402=CARTESIAN_POINT('Ctrl Pts',(23.922507629734,17.4026437778802,67.9888566520998));
#112403=CARTESIAN_POINT('Ctrl Pts',(23.9224051106616,17.4027528840716,67.9892061353641));
#112404=CARTESIAN_POINT('Ctrl Pts',(23.9219433244521,17.4032442896881,67.9907754120686));
#112405=CARTESIAN_POINT('Ctrl Pts',(23.9207864672607,17.4044753791621,67.994707681693));
#112406=CARTESIAN_POINT('Ctrl Pts',(23.9177475773,17.4077096634628,68.0050496368859));
#112407=CARTESIAN_POINT('Ctrl Pts',(23.9072108398732,17.4189272136881,68.0410135841617));
#112408=CARTESIAN_POINT('Ctrl Pts',(23.8968763662478,17.4299398638417,68.0766263973682));
#112409=CARTESIAN_POINT('Ctrl Pts',(23.8706760779252,17.4578852510944,68.1677733316712));
#112410=CARTESIAN_POINT('Ctrl Pts',(23.851342654348,17.4785377378293,68.2361021100229));
#112411=CARTESIAN_POINT('Ctrl Pts',(23.7882754916749,17.5460872093337,68.4645044517986));
#112412=CARTESIAN_POINT('Ctrl Pts',(23.7394076875455,17.5986140173638,68.6479150520402));
#112413=CARTESIAN_POINT('Ctrl Pts',(23.6590361667568,17.6860971594474,68.9739302125424));
#112414=CARTESIAN_POINT('Ctrl Pts',(23.6310851470077,17.7166965723575,69.0911012373308));
#112415=CARTESIAN_POINT('Ctrl Pts',(23.5880604984235,17.76430278348,69.2802207229952));
#112416=CARTESIAN_POINT('Ctrl Pts',(23.5662763612532,17.7885312912849,69.3781224134856));
#112417=CARTESIAN_POINT('Ctrl Pts',(23.5442320193917,17.8133002545793,69.4811630348402));
#112418=CARTESIAN_POINT('Ctrl Pts',(23.5331803275671,17.8257659416173,69.5335508954396));
#112419=CARTESIAN_POINT('Ctrl Pts',(23.5281273300357,17.8314746765208,69.557653479824));
#112420=CARTESIAN_POINT('Ctrl Pts',(23.5189906281387,17.841816471269,69.6015838168922));
#112421=CARTESIAN_POINT('Ctrl Pts',(23.5144489689002,17.8469662730383,69.6235792677627));
#112422=CARTESIAN_POINT('Ctrl Pts',(23.4377049240434,17.9341505450947,69.9980191665425));
#112423=CARTESIAN_POINT('Ctrl Pts',(23.3722679640801,18.0108631114948,70.3586080252768));
#112424=CARTESIAN_POINT('Ctrl Pts',(23.2896219181467,18.1156770894603,70.9095876822499));
#112425=CARTESIAN_POINT('Ctrl Pts',(23.2646831375625,18.1488918983225,71.0948845703221));
#112426=CARTESIAN_POINT('Ctrl Pts',(23.2318893863806,18.1958368605783,71.3749305704336));
#112427=CARTESIAN_POINT('Ctrl Pts',(23.2166390354395,18.2185942366947,71.5154862756931));
#112428=CARTESIAN_POINT('Ctrl Pts',(23.2009542680947,18.2438603952527,71.6803782636731));
#112429=CARTESIAN_POINT('Ctrl Pts',(23.1946945650232,18.2544101672144,71.7512390465093));
#112430=CARTESIAN_POINT('Ctrl Pts',(23.1916426671543,18.2596383402766,71.7867013803973));
#112431=CARTESIAN_POINT('Ctrl Pts',(23.1912659007525,18.2602959595756,71.791207649484));
#112432=CARTESIAN_POINT('Ctrl Pts',(23.1900739387607,18.262401303487,71.8057153804048));
#112433=CARTESIAN_POINT('Ctrl Pts',(23.1894717408811,18.2634825402461,71.8132266082456));
#112434=CARTESIAN_POINT('Ctrl Pts',(23.1791487916456,18.2823374133391,71.9452992336258));
#112435=CARTESIAN_POINT('Ctrl Pts',(23.1676231854454,18.3074993310288,72.1355250601407));
#112436=CARTESIAN_POINT('Ctrl Pts',(23.15971483603,18.3494862191041,72.5228176091576));
#112437=CARTESIAN_POINT('Ctrl Pts',(23.158735305727,18.3641388360826,72.6689234206449));
#112438=CARTESIAN_POINT('Ctrl Pts',(23.1623186709509,18.3856996206964,72.913972835298));
#112439=CARTESIAN_POINT('Ctrl Pts',(23.1643636747112,18.3928126370994,72.9999703254755));
#112440=CARTESIAN_POINT('Ctrl Pts',(23.1691109587509,18.4031551990834,73.135474511414));
#112441=CARTESIAN_POINT('Ctrl Pts',(23.1719054695799,18.4082442930824,73.2048534438938));
#112442=CARTESIAN_POINT('Ctrl Pts',(23.1754157853588,18.413165394377,73.2766778839518));
#112443=CARTESIAN_POINT('Ctrl Pts',(23.1772977650755,18.4155939929091,73.3129980290335));
#112444=CARTESIAN_POINT('Ctrl Pts',(23.1781587151562,18.4166627047207,73.3291724630669));
#112445=CARTESIAN_POINT('Ctrl Pts',(23.1797820783799,18.4185769114322,73.3586179279733));
#112446=CARTESIAN_POINT('Ctrl Pts',(23.2072483677226,18.4495082153164,73.8416758352283));
#112447=CARTESIAN_POINT('Ctrl Pts',(23.2554887086179,18.4600321078001,74.2313583768614));
#112448=CARTESIAN_POINT('Ctrl Pts',(23.3412924764406,18.4677758676054,74.8038516240253));
#112449=CARTESIAN_POINT('Ctrl Pts',(23.379899241412,18.4654735461107,74.998722729572));
#112450=CARTESIAN_POINT('Ctrl Pts',(23.3999522633791,18.46444455386,75.10151114459));
#112451=CARTESIAN_POINT('',(28.7709983219891,10.49234437565,58.41163725334));
#112452=CARTESIAN_POINT('Ctrl Pts',(28.0568192451658,11.8824453376732,59.4053060415497));
#112453=CARTESIAN_POINT('Ctrl Pts',(28.2006128658113,11.6261391970008,59.207884342463));
#112454=CARTESIAN_POINT('Ctrl Pts',(28.3373915772597,11.3697415610487,59.0185211727151));
#112455=CARTESIAN_POINT('Ctrl Pts',(28.4674976733393,11.1138285219291,58.8371561766688));
#112456=CARTESIAN_POINT('Ctrl Pts',(28.5730192009864,10.9062722609512,58.6900615206828));
#112457=CARTESIAN_POINT('Ctrl Pts',(28.6741521197716,10.6990338477355,58.5482278784034));
#112458=CARTESIAN_POINT('Ctrl Pts',(28.7710895317811,10.4923978628195,58.4116212007229));
#112459=CARTESIAN_POINT('',(13.2726083411502,20.6713283131467,53.9604380084771));
#112460=CARTESIAN_POINT('Ctrl Pts',(13.2725470758821,20.670980255801,53.9604489574278));
#112461=CARTESIAN_POINT('Ctrl Pts',(13.3983326199236,20.6495706071341,53.9827646797933));
#112462=CARTESIAN_POINT('Ctrl Pts',(13.531387176427,20.6258486398982,54.0065477088826));
#112463=CARTESIAN_POINT('Ctrl Pts',(13.6715832064528,20.5994311438589,54.0319088395874));
#112464=CARTESIAN_POINT('Ctrl Pts',(13.7714197113082,20.5806186962375,54.0499690275135));
#112465=CARTESIAN_POINT('Ctrl Pts',(13.8748772205112,20.5604384421668,54.0688297144999));
#112466=CARTESIAN_POINT('Ctrl Pts',(13.9818997410914,20.5387396048791,54.0885338755379));
#112467=CARTESIAN_POINT('Ctrl Pts',(14.0974696012661,20.5153077927924,54.1098117068175));
#112468=CARTESIAN_POINT('Ctrl Pts',(14.2171963593889,20.4901051805436,54.1320732233102));
#112469=CARTESIAN_POINT('Ctrl Pts',(14.3410132816261,20.4629320551245,54.1553717026691));
#112470=CARTESIAN_POINT('Ctrl Pts',(14.5137202363644,20.4250294190627,54.1878697598603));
#112471=CARTESIAN_POINT('Ctrl Pts',(14.6943870318908,20.3832944228992,54.2223854561454));
#112472=CARTESIAN_POINT('Ctrl Pts',(14.8828092918702,20.3371466051706,54.2590671495918));
#112473=CARTESIAN_POINT('Ctrl Pts',(14.9123065986212,20.3299222128107,54.2648096301451));
#112474=CARTESIAN_POINT('Ctrl Pts',(14.9419939140507,20.3225895875837,54.2706051992886));
#112475=CARTESIAN_POINT('Ctrl Pts',(14.9718703872864,20.3151464087435,54.2764544309475));
#112476=CARTESIAN_POINT('Ctrl Pts',(15.0822307696412,20.2876521306787,54.2980608447053));
#112477=CARTESIAN_POINT('Ctrl Pts',(15.1951724544689,20.2586497117875,54.3203994742456));
#112478=CARTESIAN_POINT('Ctrl Pts',(15.3106502727804,20.2280193281412,54.3434992717584));
#112479=CARTESIAN_POINT('Ctrl Pts',(15.3683891819361,20.212704136318,54.3550491705148));
#112480=CARTESIAN_POINT('Ctrl Pts',(15.4267621027678,20.1969818742966,54.3667893638777));
#112481=CARTESIAN_POINT('Ctrl Pts',(15.4857629994355,20.1808371688332,54.378723458483));
#112482=CARTESIAN_POINT('Ctrl Pts',(15.5152634477693,20.1727648161015,54.3846905057856));
#112483=CARTESIAN_POINT('Ctrl Pts',(15.5449208887949,20.1645868477245,54.3907060285509));
#112484=CARTESIAN_POINT('Ctrl Pts',(15.5747345513607,20.1563013159571,54.3967704764909));
#112485=CARTESIAN_POINT('Ctrl Pts',(15.5896413826436,20.1521585500734,54.3998027004609));
#112486=CARTESIAN_POINT('Ctrl Pts',(15.604587269227,20.1479888930469,54.4028471557349));
#112487=CARTESIAN_POINT('Ctrl Pts',(15.6195721132309,20.1437920999199,54.4059038984308));
#112488=CARTESIAN_POINT('Ctrl Pts',(15.6345569572348,20.1395953067928,54.4089606411267));
#112489=CARTESIAN_POINT('Ctrl Pts',(15.6481522477201,20.1357745629695,54.4117374402641));
#112490=CARTESIAN_POINT('Ctrl Pts',(15.6646434189796,20.1311200661957,54.415111044885));
#112491=CARTESIAN_POINT('Ctrl Pts',(15.8328267221155,20.0836517190703,54.449516361505));
#112492=CARTESIAN_POINT('Ctrl Pts',(15.9934146374075,20.0362881729058,54.4830079349232));
#112493=CARTESIAN_POINT('Ctrl Pts',(16.1465409572366,19.9894925441059,54.5154517122097));
#112494=CARTESIAN_POINT('Ctrl Pts',(16.3017481192989,19.9420610068557,54.5483363698234));
#112495=CARTESIAN_POINT('Ctrl Pts',(16.4492896509013,19.895212890308,54.5801446504592));
#112496=CARTESIAN_POINT('Ctrl Pts',(16.5892991581977,19.8493805976035,54.6107561641212));
#112497=CARTESIAN_POINT('Ctrl Pts',(16.6705959948486,19.8227679733233,54.6285308086712));
#112498=CARTESIAN_POINT('Ctrl Pts',(16.7493532392507,19.7964969186979,54.6459023039302));
#112499=CARTESIAN_POINT('Ctrl Pts',(16.825595914603,19.7706446140519,54.6628498087903));
#112500=CARTESIAN_POINT('Ctrl Pts',(16.9590472852794,19.7253940313014,54.6925138747832));
#112501=CARTESIAN_POINT('Ctrl Pts',(17.0847944325676,19.6814291917678,54.7208780337367));
#112502=CARTESIAN_POINT('Ctrl Pts',(17.2029519193958,19.6391261391975,54.7478438524984));
#112503=CARTESIAN_POINT('Ctrl Pts',(17.3226347922806,19.5962769639204,54.775157793796));
#112504=CARTESIAN_POINT('Ctrl Pts',(17.4345310839538,19.5551327185357,54.8010371418669));
#112505=CARTESIAN_POINT('Ctrl Pts',(17.5387575365312,19.5160331038114,54.8253961014855));
#112506=CARTESIAN_POINT('Ctrl Pts',(17.6201968381364,19.4854818834884,54.8444294333327));
#112507=CARTESIAN_POINT('Ctrl Pts',(17.6969534080328,19.4561779490565,54.8625348551515));
#112508=CARTESIAN_POINT('Ctrl Pts',(17.7690802329903,19.4282623570324,54.8796778113961));
#112509=CARTESIAN_POINT('Ctrl Pts',(17.8037775298157,19.4148332953333,54.8879245939438));
#112510=CARTESIAN_POINT('Ctrl Pts',(17.8374033749867,19.4017252527957,54.8959487237115));
#112511=CARTESIAN_POINT('Ctrl Pts',(17.8699633866476,19.3889524563322,54.9037467823189));
#112512=CARTESIAN_POINT('Ctrl Pts',(17.886243392478,19.3825660581005,54.9076458116227));
#112513=CARTESIAN_POINT('Ctrl Pts',(17.9022569342675,19.376263457397,54.9114883238176));
#112514=CARTESIAN_POINT('Ctrl Pts',(17.9180046971456,19.3700463431641,54.9152739206525));
#112515=CARTESIAN_POINT('Ctrl Pts',(17.9258785785847,19.3669377860476,54.91716671907));
#112516=CARTESIAN_POINT('Ctrl Pts',(17.9336860149447,19.3638505996751,54.9190452886899));
#112517=CARTESIAN_POINT('Ctrl Pts',(17.9414270900674,19.3607849898339,54.9209095806218));
#112518=CARTESIAN_POINT('Ctrl Pts',(17.9482005307998,19.3581025812228,54.9225408360622));
#112519=CARTESIAN_POINT('Ctrl Pts',(17.9549231636888,19.3554366920914,54.9241611601502));
#112520=CARTESIAN_POINT('Ctrl Pts',(17.9615950443003,19.3527874580197,54.9257705207019));
#112521=CARTESIAN_POINT('Ctrl Pts',(17.9620716072011,19.3525982270146,54.925885475027));
#112522=CARTESIAN_POINT('Ctrl Pts',(17.962257232792,19.3525245107963,54.9259302457957));
#112523=CARTESIAN_POINT('Ctrl Pts',(17.9625879435656,19.3523931767217,54.9260100238398));
#112524=CARTESIAN_POINT('Ctrl Pts',(17.9629186543391,19.3522618426471,54.926089801884));
#112525=CARTESIAN_POINT('Ctrl Pts',(17.9633944550144,19.3520729022509,54.9262045866393));
#112526=CARTESIAN_POINT('Ctrl Pts',(17.964451314587,19.3516530920658,54.9264595753351));
#112527=CARTESIAN_POINT('Ctrl Pts',(18.1681663588649,19.2707325491052,54.9756099400571));
#112528=CARTESIAN_POINT('Ctrl Pts',(18.3646898914307,19.189396868016,55.0239377208772));
#112529=CARTESIAN_POINT('Ctrl Pts',(18.5541472030898,19.1081622375069,55.0713015000461));
#112530=CARTESIAN_POINT('Ctrl Pts',(18.7485133668291,19.0248228120894,55.119892478017));
#112531=CARTESIAN_POINT('Ctrl Pts',(18.9354426488189,18.9415897734647,55.1674689038007));
#112532=CARTESIAN_POINT('Ctrl Pts',(19.1150897843592,18.8589725928745,55.213898600522));
#112533=CARTESIAN_POINT('Ctrl Pts',(19.260647254864,18.792032767807,55.2515178433266));
#112534=CARTESIAN_POINT('Ctrl Pts',(19.4014245088014,18.7254962996004,55.2883846896468));
#112535=CARTESIAN_POINT('Ctrl Pts',(19.5375110188955,18.6596119982858,55.324437893159));
#112536=CARTESIAN_POINT('Ctrl Pts',(19.7134947248391,18.5744120508345,55.3710610034204));
#112537=CARTESIAN_POINT('Ctrl Pts',(19.8816351338832,18.4903038972743,55.4163223459423));
#112538=CARTESIAN_POINT('Ctrl Pts',(20.0421640303715,18.407768078151,55.4600957917956));
#112539=CARTESIAN_POINT('Ctrl Pts',(20.2047686202212,18.3241650427472,55.5044352432276));
#112540=CARTESIAN_POINT('Ctrl Pts',(20.3595638260116,18.2421752263657,55.5472482728489));
#112541=CARTESIAN_POINT('Ctrl Pts',(20.5067845132278,18.1622509049083,55.5884287453757));
#112542=CARTESIAN_POINT('Ctrl Pts',(20.6564303125084,18.0810100195911,55.6302875686333));
#112543=CARTESIAN_POINT('Ctrl Pts',(20.7982502424243,18.0019032324527,55.670459795706));
#112544=CARTESIAN_POINT('Ctrl Pts',(20.9324810363312,17.9253574474708,55.7088566072134));
#112545=CARTESIAN_POINT('Ctrl Pts',(21.0676708251577,17.8482647908153,55.7475277398812));
#112546=CARTESIAN_POINT('Ctrl Pts',(21.1951628772056,17.7737697907286,55.78439821155));
#112547=CARTESIAN_POINT('Ctrl Pts',(21.315185457343,17.7022608641087,55.8193969583901));
#112548=CARTESIAN_POINT('Ctrl Pts',(21.4362280291454,17.6301442309302,55.8546931361805));
#112549=CARTESIAN_POINT('Ctrl Pts',(21.5496738518478,17.5610645912574,55.8880858373269));
#112550=CARTESIAN_POINT('Ctrl Pts',(21.6557399270599,17.4953728891182,55.9195190062841));
#112551=CARTESIAN_POINT('Ctrl Pts',(21.7435139199357,17.4410103327208,55.9455312325553));
#112552=CARTESIAN_POINT('Ctrl Pts',(21.8262338218732,17.3889670330136,55.9702018787292));
#112553=CARTESIAN_POINT('Ctrl Pts',(21.9040123380698,17.3394180031356,55.9935063851894));
#112554=CARTESIAN_POINT('Ctrl Pts',(21.9595325848506,17.3040486685032,56.0101417237513));
#112555=CARTESIAN_POINT('Ctrl Pts',(22.0125347737628,17.2699498293013,56.0260810869046));
#112556=CARTESIAN_POINT('Ctrl Pts',(22.0630567118334,17.2371785721442,56.0413172514788));
#112557=CARTESIAN_POINT('Ctrl Pts',(22.0883176808687,17.2207929435656,56.0489353337659));
#112558=CARTESIAN_POINT('Ctrl Pts',(22.1129585339961,17.2047391316149,56.0563776226435));
#112559=CARTESIAN_POINT('Ctrl Pts',(22.1369837451694,17.1890237610659,56.0636433486403));
#112560=CARTESIAN_POINT('Ctrl Pts',(22.1489963507561,17.1811660757914,56.0672762116387));
#112561=CARTESIAN_POINT('Ctrl Pts',(22.160855042549,17.1733929959198,56.0708649343019));
#112562=CARTESIAN_POINT('Ctrl Pts',(22.1725603608703,17.1657053193998,56.0744094244494));
#112563=CARTESIAN_POINT('Ctrl Pts',(22.178413020031,17.1618614811399,56.0761816695231));
#112564=CARTESIAN_POINT('Ctrl Pts',(22.1842273356144,17.1580389934109,56.0779428564926));
#112565=CARTESIAN_POINT('Ctrl Pts',(22.1900033741081,17.1542379539996,56.0796929742694));
#112566=CARTESIAN_POINT('Ctrl Pts',(22.1943354029784,17.1513871744411,56.081005562602));
#112567=CARTESIAN_POINT('Ctrl Pts',(22.1986459009686,17.148548459536,56.0823119245156));
#112568=CARTESIAN_POINT('Ctrl Pts',(22.2029348958593,17.1457218500621,56.0836120554263));
#112569=CARTESIAN_POINT('Ctrl Pts',(22.2036497283411,17.1452507484831,56.0838287439115));
#112570=CARTESIAN_POINT('Ctrl Pts',(22.2039246071545,17.1450695659692,56.0839120788244));
#112571=CARTESIAN_POINT('Ctrl Pts',(22.2044185879296,17.1447439591707,56.0840618283974));
#112572=CARTESIAN_POINT('Ctrl Pts',(22.2049125687048,17.1444183523722,56.0842115779703));
#112573=CARTESIAN_POINT('Ctrl Pts',(22.2056256717387,17.1439483509576,56.0844277397999));
#112574=CARTESIAN_POINT('Ctrl Pts',(22.2072167240695,17.1428992772211,56.0849101091727));
#112575=CARTESIAN_POINT('Ctrl Pts',(22.4232631234304,17.0004472666548,56.1504102590644));
#112576=CARTESIAN_POINT('Ctrl Pts',(22.6313077906992,16.8580575607652,56.2145538222262));
#112577=CARTESIAN_POINT('Ctrl Pts',(22.8316436620993,16.7163048221399,56.2772017465106));
#112578=CARTESIAN_POINT('Ctrl Pts',(23.0350088497684,16.5724086137791,56.3407969818029));
#112579=CARTESIAN_POINT('Ctrl Pts',(23.2304305725263,16.4291687516019,56.4028511969841));
#112580=CARTESIAN_POINT('Ctrl Pts',(23.4182208717324,16.2871422952561,56.4632510848778));
#112581=CARTESIAN_POINT('Ctrl Pts',(23.6104241266593,16.1417783051521,56.5250703327275));
#112582=CARTESIAN_POINT('Ctrl Pts',(23.7946333175536,15.9976854511902,56.5851567549806));
#112583=CARTESIAN_POINT('Ctrl Pts',(23.9711852633733,15.8554150786589,56.6434195964039));
#112584=CARTESIAN_POINT('Ctrl Pts',(24.1202371250588,15.7353050238531,56.6926073011381));
#112585=CARTESIAN_POINT('Ctrl Pts',(24.2638314927311,15.6164930851575,56.7404958867728));
#112586=CARTESIAN_POINT('Ctrl Pts',(24.4021703284857,15.4992863804217,56.7870457428963));
#112587=CARTESIAN_POINT('Ctrl Pts',(24.5657007214818,15.3607362879427,56.8420723464113));
#112588=CARTESIAN_POINT('Ctrl Pts',(24.721886796623,15.2244306559942,56.8952276754609));
#112589=CARTESIAN_POINT('Ctrl Pts',(24.8710398764416,15.0908494029051,56.9464618033456));
#112590=CARTESIAN_POINT('Ctrl Pts',(25.0237389492806,14.9540923642962,56.9989139809019));
#112591=CARTESIAN_POINT('Ctrl Pts',(25.1690669787661,14.8201907764638,57.04935272528));
#112592=CARTESIAN_POINT('Ctrl Pts',(25.3073581524276,14.6896102615281,57.0977484391436));
#112593=CARTESIAN_POINT('Ctrl Pts',(25.3814685192842,14.6196320437577,57.1236837466094));
#112594=CARTESIAN_POINT('Ctrl Pts',(25.4535579439844,14.5506067710419,57.149032702733));
#112595=CARTESIAN_POINT('Ctrl Pts',(25.5236773638562,14.4826005075336,57.1737931672091));
#112596=CARTESIAN_POINT('Ctrl Pts',(25.5817728389014,14.4262558288157,57.1943077543051));
#112597=CARTESIAN_POINT('Ctrl Pts',(25.638516003415,14.370610575918,57.2144184047141));
#112598=CARTESIAN_POINT('Ctrl Pts',(25.6939355208178,14.3157003634769,57.2341246640445));
#112599=CARTESIAN_POINT('Ctrl Pts',(25.7216452795192,14.2882452572563,57.2439777937097));
#112600=CARTESIAN_POINT('Ctrl Pts',(25.7490241095723,14.2609738950902,57.2537298281413));
#112601=CARTESIAN_POINT('Ctrl Pts',(25.7760755746848,14.2338905536095,57.2633807782122));
#112602=CARTESIAN_POINT('Ctrl Pts',(25.7896013072411,14.2203488828692,57.2682062532476));
#112603=CARTESIAN_POINT('Ctrl Pts',(25.8030451974999,14.2068542162773,57.2730064573516));
#112604=CARTESIAN_POINT('Ctrl Pts',(25.816407686443,14.193407080461,57.2777813938924));
#112605=CARTESIAN_POINT('Ctrl Pts',(25.8230889309145,14.1866835125528,57.2801688621628));
#112606=CARTESIAN_POINT('Ctrl Pts',(25.8297498249901,14.1799718272756,57.2825500135525));
#112607=CARTESIAN_POINT('Ctrl Pts',(25.8363904236561,14.1732720898237,57.2849248487048));
#112608=CARTESIAN_POINT('Ctrl Pts',(25.8413708726557,14.1682472867348,57.2867059750689));
#112609=CARTESIAN_POINT('Ctrl Pts',(25.8463399054818,14.1632292042925,57.2884835485503));
#112610=CARTESIAN_POINT('Ctrl Pts',(25.8512975452887,14.1582178698532,57.2902575694684));
#112611=CARTESIAN_POINT('Ctrl Pts',(25.852950091891,14.1565474250401,57.2908489097744));
#112612=CARTESIAN_POINT('Ctrl Pts',(25.8560371622284,14.1534254693535,57.2919537333789));
#112613=CARTESIAN_POINT('Ctrl Pts',(25.8562513882808,14.1532087857527,57.292030406214));
#112614=CARTESIAN_POINT('Ctrl Pts',(25.8620994629914,14.1472936233727,57.2941234684845));
#112615=CARTESIAN_POINT('Ctrl Pts',(25.8735776967432,14.1356810419393,57.2982181067595));
#112616=CARTESIAN_POINT('Ctrl Pts',(25.8906482847789,14.1183340826607,57.304310381592));
#112617=CARTESIAN_POINT('Ctrl Pts',(25.9076983413253,14.1010079872743,57.3103953289983));
#112618=CARTESIAN_POINT('Ctrl Pts',(25.9303273488426,14.0779612618749,57.3184731525455));
#112619=CARTESIAN_POINT('Ctrl Pts',(25.9584601922357,14.0491212848265,57.3285356587346));
#112620=CARTESIAN_POINT('Ctrl Pts',(25.9864949993255,14.0203818082751,57.3385630994702));
#112621=CARTESIAN_POINT('Ctrl Pts',(26.0199954067525,13.9858893157332,57.3505614815991));
#112622=CARTESIAN_POINT('Ctrl Pts',(26.058849163281,13.9455372029293,57.3645176427207));
#112623=CARTESIAN_POINT('Ctrl Pts',(26.0975892260193,13.905303168403,57.3784329653495));
#112624=CARTESIAN_POINT('Ctrl Pts',(26.1416514425737,13.8592436714862,57.3942947188479));
#112625=CARTESIAN_POINT('Ctrl Pts',(26.1908856865504,13.8072195986701,57.4120836267462));
#112626=CARTESIAN_POINT('Ctrl Pts',(26.2397975092592,13.7555362169292,57.4297560400713));
#112627=CARTESIAN_POINT('Ctrl Pts',(26.2938139308273,13.697966004636,57.4493305605161));
#112628=CARTESIAN_POINT('Ctrl Pts',(26.3527480492319,13.6343410642143,57.4707806166182));
#112629=CARTESIAN_POINT('Ctrl Pts',(26.3956365561786,13.5880388750389,57.4863906046022));
#112630=CARTESIAN_POINT('Ctrl Pts',(26.4411286678883,13.5385294399888,57.5029937293787));
#112631=CARTESIAN_POINT('Ctrl Pts',(26.4891385100757,13.485738019396,57.5205766097949));
#112632=CARTESIAN_POINT('Ctrl Pts',(26.554119601433,13.4142850845785,57.5443749541882));
#112633=CARTESIAN_POINT('Ctrl Pts',(26.6237145012724,13.3368210896554,57.5699686138886));
#112634=CARTESIAN_POINT('Ctrl Pts',(26.697678079691,13.2531302347554,57.5973159560468));
#112635=CARTESIAN_POINT('Ctrl Pts',(26.7707907027383,13.1704022481214,57.6243486654059));
#112636=CARTESIAN_POINT('Ctrl Pts',(26.848172101239,13.0815898112931,57.6530950629175));
#112637=CARTESIAN_POINT('Ctrl Pts',(26.9295465905642,12.9864541213655,57.683503211984));
#112638=CARTESIAN_POINT('Ctrl Pts',(26.9791042032982,12.9285158446683,57.7020219798177));
#112639=CARTESIAN_POINT('Ctrl Pts',(27.0301420512111,12.8682317541113,57.7211568382924));
#112640=CARTESIAN_POINT('Ctrl Pts',(27.0825905397635,12.8055423906308,57.7408935664254));
#112641=CARTESIAN_POINT('Ctrl Pts',(27.1351740721451,12.7426916152215,57.7606811124831));
#112642=CARTESIAN_POINT('Ctrl Pts',(27.1891755326363,12.6774231685811,57.7810736474008));
#112643=CARTESIAN_POINT('Ctrl Pts',(27.2445189896879,12.6096728855716,57.8020546543642));
#112644=CARTESIAN_POINT('Ctrl Pts',(27.2721907182137,12.5757977440668,57.812545157846));
#112645=CARTESIAN_POINT('Ctrl Pts',(27.3001978611984,12.5413020791577,57.8231827941772));
#112646=CARTESIAN_POINT('Ctrl Pts',(27.3285303604243,12.5061774672578,57.8339652179499));
#112647=CARTESIAN_POINT('Ctrl Pts',(27.3426966100372,12.4886151613078,57.8393564298362));
#112648=CARTESIAN_POINT('Ctrl Pts',(27.3569441933603,12.4708956144904,57.8447838395127));
#112649=CARTESIAN_POINT('Ctrl Pts',(27.3712718188045,12.453017749092,57.850247147685));
#112650=CARTESIAN_POINT('Ctrl Pts',(27.3784356315265,12.4440788163928,57.8529788017711));
#112651=CARTESIAN_POINT('Ctrl Pts',(27.3856194544388,12.4351003037946,57.8557194305414));
#112652=CARTESIAN_POINT('Ctrl Pts',(27.3928231238543,12.4260820750035,57.8584689956263));
#112653=CARTESIAN_POINT('Ctrl Pts',(27.3964249585621,12.421572960608,57.8598437781688));
#112654=CARTESIAN_POINT('Ctrl Pts',(27.4000317548744,12.4170539171483,57.8612207947937));
#112655=CARTESIAN_POINT('Ctrl Pts',(27.4036434921889,12.4125249274888,57.862600040639));
#112656=CARTESIAN_POINT('Ctrl Pts',(27.4072552295035,12.4079959378294,57.8639792864843));
#112657=CARTESIAN_POINT('Ctrl Pts',(27.4121604782024,12.4018384965928,57.8658530839424));
#112658=CARTESIAN_POINT('Ctrl Pts',(27.4144935064473,12.3989081027107,57.8667444609622));
#112659=CARTESIAN_POINT('Ctrl Pts',(27.5443731982542,12.2357730634706,57.9163674232507));
#112660=CARTESIAN_POINT('Ctrl Pts',(27.6666333539921,12.0773904465288,57.9636925254359));
#112661=CARTESIAN_POINT('Ctrl Pts',(27.7817898329975,11.9242236513042,58.0087751429393));
#112662=CARTESIAN_POINT('Ctrl Pts',(27.8963722738334,11.7718203701043,58.0536330302021));
#112663=CARTESIAN_POINT('Ctrl Pts',(28.0039219461057,11.6245809497874,58.0962710866615));
#112664=CARTESIAN_POINT('Ctrl Pts',(28.1049157238554,11.4829233739343,58.136757159939));
#112665=CARTESIAN_POINT('Ctrl Pts',(28.1713804642806,11.3896974919233,58.1634013395229));
#112666=CARTESIAN_POINT('Ctrl Pts',(28.2350051607492,11.2988883550859,58.1891137418305));
#112667=CARTESIAN_POINT('Ctrl Pts',(28.2959175074842,11.2106061487287,58.2139158100153));
#112668=CARTESIAN_POINT('Ctrl Pts',(28.3897816383863,11.0745658708867,58.2521350660368));
#112669=CARTESIAN_POINT('Ctrl Pts',(28.4772065834014,10.9445274666595,58.2881919157419));
#112670=CARTESIAN_POINT('Ctrl Pts',(28.5586195289291,10.8208529693944,58.3221601998858));
#112671=CARTESIAN_POINT('Ctrl Pts',(28.6344289501963,10.7056907921461,58.3537905007636));
#112672=CARTESIAN_POINT('Ctrl Pts',(28.7050253514017,10.5960464103352,58.3836102317404));
#112673=CARTESIAN_POINT('Ctrl Pts',(28.7707246265959,10.4921843560221,58.4116855396036));
#112674=CARTESIAN_POINT('',(20.1852098213545,19.2602427307108,66.2798693554263));
#112675=CARTESIAN_POINT('Ctrl Pts',(13.2726083411502,20.6713283131467,53.9604380084771));
#112676=CARTESIAN_POINT('Ctrl Pts',(13.6650705206071,20.6171872598987,54.4446995373014));
#112677=CARTESIAN_POINT('Ctrl Pts',(14.0456121743071,20.5589064465633,54.9370237517833));
#112678=CARTESIAN_POINT('Ctrl Pts',(14.4143958822179,20.4977644961702,55.4374033981323));
#112679=CARTESIAN_POINT('Ctrl Pts',(14.792876198402,20.4350149109242,55.9509397683671));
#112680=CARTESIAN_POINT('Ctrl Pts',(15.1589715900071,20.3692518224625,56.4729607208082));
#112681=CARTESIAN_POINT('Ctrl Pts',(15.5128201222323,20.301816719549,57.0034475857769));
#112682=CARTESIAN_POINT('Ctrl Pts',(15.8776473842055,20.2322893322172,57.550393673817));
#112683=CARTESIAN_POINT('Ctrl Pts',(16.2294557289051,20.1609845788745,58.1063392937893));
#112684=CARTESIAN_POINT('Ctrl Pts',(16.5683635307345,20.0893294000026,58.6712517682346));
#112685=CARTESIAN_POINT('Ctrl Pts',(16.7879003420604,20.0429127952516,59.0371892965194));
#112686=CARTESIAN_POINT('Ctrl Pts',(17.0020232495274,19.9963482605702,59.4068892038341));
#112687=CARTESIAN_POINT('Ctrl Pts',(17.2107580475794,19.9500144834406,59.7803395394369));
#112688=CARTESIAN_POINT('Ctrl Pts',(17.4689577772204,19.8927007588496,60.2422882733654));
#112689=CARTESIAN_POINT('Ctrl Pts',(17.7189332343118,19.8357394220478,60.7100397541429));
#112690=CARTESIAN_POINT('Ctrl Pts',(17.9609010912795,19.7797605046363,61.183494134282));
#112691=CARTESIAN_POINT('Ctrl Pts',(18.2082387691999,19.7225392868326,61.667455551523));
#112692=CARTESIAN_POINT('Ctrl Pts',(18.4472096766317,19.6663442139162,62.1573756648184));
#112693=CARTESIAN_POINT('Ctrl Pts',(18.6780286743746,19.6118176263714,62.6531899405673));
#112694=CARTESIAN_POINT('Ctrl Pts',(18.9120250296077,19.5565404486974,63.155829387633));
#112695=CARTESIAN_POINT('Ctrl Pts',(19.1376435950153,19.5029775403519,63.6645263330383));
#112696=CARTESIAN_POINT('Ctrl Pts',(19.3550892404964,19.4517734533484,64.1792577383865));
#112697=CARTESIAN_POINT('Ctrl Pts',(19.5780377759832,19.3992735461504,64.7070154349712));
#112698=CARTESIAN_POINT('Ctrl Pts',(19.7923945453953,19.3492528297393,65.2411168166477));
#112699=CARTESIAN_POINT('Ctrl Pts',(19.9983593229911,19.3023878519598,65.7815843256316));
#112700=CARTESIAN_POINT('Ctrl Pts',(20.0614280643745,19.2880372663985,65.9470815817552));
#112701=CARTESIAN_POINT('Ctrl Pts',(20.1237097797265,19.2739824855875,66.1131760904936));
#112702=CARTESIAN_POINT('Ctrl Pts',(20.1852098210872,19.2602427300862,66.2798693554734));
#112703=CARTESIAN_POINT('',(20.800313080212,19.9701890918763,80.5583314861626));
#112704=CARTESIAN_POINT('Ctrl Pts',(20.1852098218891,19.26024273196,66.279869355332));
#112705=CARTESIAN_POINT('Ctrl Pts',(20.3956147376191,19.2132888033458,66.85086198908));
#112706=CARTESIAN_POINT('Ctrl Pts',(20.583906319848,19.1756806736357,67.4339514479084));
#112707=CARTESIAN_POINT('Ctrl Pts',(20.8337679129635,19.1346807742746,68.3266260967489));
#112708=CARTESIAN_POINT('Ctrl Pts',(20.9116227172105,19.1235746354422,68.6271916025033));
#112709=CARTESIAN_POINT('Ctrl Pts',(21.0203010142702,19.1108571350284,69.0825429169022));
#112710=CARTESIAN_POINT('Ctrl Pts',(21.0551762471562,19.1072744149749,69.2350772354996));
#112711=CARTESIAN_POINT('Ctrl Pts',(21.1222298094364,19.1014326610879,69.5416461155132));
#112712=CARTESIAN_POINT('Ctrl Pts',(21.1548280750446,19.099151918798,69.6977888999547));
#112713=CARTESIAN_POINT('Ctrl Pts',(21.3068854151633,19.0912914655277,70.4611698530622));
#112714=CARTESIAN_POINT('Ctrl Pts',(21.4047375236733,19.0955470327253,71.0692966232455));
#112715=CARTESIAN_POINT('Ctrl Pts',(21.5157574614961,19.1175959029956,71.9776317061673));
#112716=CARTESIAN_POINT('Ctrl Pts',(21.5468008791318,19.1275486653768,72.2797681764848));
#112717=CARTESIAN_POINT('Ctrl Pts',(21.5843815989602,19.1462934155003,72.7320170222064));
#112718=CARTESIAN_POINT('Ctrl Pts',(21.5954108918719,19.1531771101233,72.8826073649739));
#112719=CARTESIAN_POINT('Ctrl Pts',(21.6144651576598,19.1681946363891,73.1834711088403));
#112720=CARTESIAN_POINT('Ctrl Pts',(21.622539704415,19.1763950000682,73.3348863784913));
#112721=CARTESIAN_POINT('Ctrl Pts',(21.6807506561845,19.2545151271669,74.6756524326983));
#112722=CARTESIAN_POINT('Ctrl Pts',(21.6393791641691,19.3636208894343,75.871367916597));
#112723=CARTESIAN_POINT('Ctrl Pts',(21.3604005439774,19.6406666743054,78.2839515090091));
#112724=CARTESIAN_POINT('Ctrl Pts',(21.128772128542,19.8020335869663,79.4438996858326));
#112725=CARTESIAN_POINT('Ctrl Pts',(20.8003130797391,19.9701890904,80.558331486246));
#112726=CARTESIAN_POINT('',(7.33390977237169,18.5189601985662,98.6155810279324));
#112727=CARTESIAN_POINT('Ctrl Pts',(7.33390977041688,18.5189602022785,98.615581028277));
#112728=CARTESIAN_POINT('Ctrl Pts',(7.40300811544448,18.5587169582139,98.5792660235925));
#112729=CARTESIAN_POINT('Ctrl Pts',(7.47743835222588,18.6010470589897,98.5393831952295));
#112730=CARTESIAN_POINT('Ctrl Pts',(7.5571859506456,18.645686168729,98.4956928813854));
#112731=CARTESIAN_POINT('Ctrl Pts',(7.63681402113335,18.6902583721215,98.4520680518063));
#112732=CARTESIAN_POINT('Ctrl Pts',(7.7217435913383,18.737132513752,98.4046472585255));
#112733=CARTESIAN_POINT('Ctrl Pts',(7.81195440394735,18.7860124926477,98.3531522464439));
#112734=CARTESIAN_POINT('Ctrl Pts',(7.89967363447421,18.8335424285046,98.303079503442));
#112735=CARTESIAN_POINT('Ctrl Pts',(7.99238644327563,18.8829686485955,98.249154440664));
#112736=CARTESIAN_POINT('Ctrl Pts',(8.0900680016121,18.9339911668916,98.191083469747));
#112737=CARTESIAN_POINT('Ctrl Pts',(8.19007101100508,18.9862262608367,98.1316324131815));
#112738=CARTESIAN_POINT('Ctrl Pts',(8.29528185234498,19.0401343561057,98.0678363631022));
#112739=CARTESIAN_POINT('Ctrl Pts',(8.40566612380089,19.0953664082598,97.9993377021124));
#112740=CARTESIAN_POINT('Ctrl Pts',(8.51545955489577,19.1503028265776,97.9312056855101));
#112741=CARTESIAN_POINT('Ctrl Pts',(8.63037125665938,19.2065488445754,97.8584213946183));
#112742=CARTESIAN_POINT('Ctrl Pts',(8.75035847762832,19.2637368556886,97.7805882331736));
#112743=CARTESIAN_POINT('Ctrl Pts',(8.78001842642022,19.2778733067826,97.7613484544362));
#112744=CARTESIAN_POINT('Ctrl Pts',(8.80998846475636,19.2920672107585,97.7417999486203));
#112745=CARTESIAN_POINT('Ctrl Pts',(8.84026785415954,19.3063128108983,97.7219362865122));
#112746=CARTESIAN_POINT('Ctrl Pts',(8.88625532412443,19.3279486206511,97.6917679250429));
#112747=CARTESIAN_POINT('Ctrl Pts',(8.93295637404587,19.3497036940079,97.6608726489343));
#112748=CARTESIAN_POINT('Ctrl Pts',(8.98036824142804,19.3715575334906,97.629227137476));
#112749=CARTESIAN_POINT('Ctrl Pts',(9.00407417511912,19.382484453232,97.6134043817468));
#112750=CARTESIAN_POINT('Ctrl Pts',(9.02795781521243,19.393436059536,97.5973940668182));
#112751=CARTESIAN_POINT('Ctrl Pts',(9.05201878813381,19.404409753059,97.5811931647464));
#112752=CARTESIAN_POINT('Ctrl Pts',(9.07122333245306,19.4131685336909,97.5682622270464));
#112753=CARTESIAN_POINT('Ctrl Pts',(9.09148271476123,19.4223679925869,97.5545719375748));
#112754=CARTESIAN_POINT('Ctrl Pts',(9.11054142550903,19.4309848244041,97.5416478040445));
#112755=CARTESIAN_POINT('Ctrl Pts',(9.1153609758434,19.4331638414014,97.5383795603054));
#112756=CARTESIAN_POINT('Ctrl Pts',(9.12010376098745,19.4353057867906,97.535160499116));
#112757=CARTESIAN_POINT('Ctrl Pts',(9.12473333698127,19.4373944771995,97.5320156598431));
#112758=CARTESIAN_POINT('Ctrl Pts',(9.2329304762039,19.486208953356,97.4585180840177));
#112759=CARTESIAN_POINT('Ctrl Pts',(9.33875382586786,19.5327559178126,97.3853580022948));
#112760=CARTESIAN_POINT('Ctrl Pts',(9.44221015358314,19.5772068491388,97.3126744947735));
#112761=CARTESIAN_POINT('Ctrl Pts',(9.59241066674853,19.6417418354786,97.2071507402632));
#112762=CARTESIAN_POINT('Ctrl Pts',(9.7376200143331,19.7018600336085,97.1026331426659));
#112763=CARTESIAN_POINT('Ctrl Pts',(9.87781587225694,19.7580219968163,96.9995654049525));
#112764=CARTESIAN_POINT('Ctrl Pts',(10.0204767735848,19.8151714476646,96.8946854421794));
#112765=CARTESIAN_POINT('Ctrl Pts',(10.1579466148379,19.8682243189159,96.7913069061254));
#112766=CARTESIAN_POINT('Ctrl Pts',(10.2902269366158,19.9176255912408,96.689870740715));
#112767=CARTESIAN_POINT('Ctrl Pts',(10.3939715015546,19.9563699292942,96.6103165734123));
#112768=CARTESIAN_POINT('Ctrl Pts',(10.4945245822998,19.9928673785176,96.5319566228767));
#112769=CARTESIAN_POINT('Ctrl Pts',(10.5918957033378,20.027315787863,96.4549917215766));
#112770=CARTESIAN_POINT('Ctrl Pts',(10.6631576246075,20.0525271627396,96.3986642737818));
#112771=CARTESIAN_POINT('Ctrl Pts',(10.73271539479,20.076640728936,96.3430838227071));
#112772=CARTESIAN_POINT('Ctrl Pts',(10.8005748819127,20.0997291910529,96.2883254403981));
#112773=CARTESIAN_POINT('Ctrl Pts',(10.8345046254741,20.1112734221114,96.2609462492436));
#112774=CARTESIAN_POINT('Ctrl Pts',(10.8680098181274,20.1225613096538,96.2337725716242));
#112775=CARTESIAN_POINT('Ctrl Pts',(10.9010913435032,20.1336015707345,96.2068134459687));
#112776=CARTESIAN_POINT('Ctrl Pts',(10.9176321061911,20.1391217012748,96.193333883141));
#112777=CARTESIAN_POINT('Ctrl Pts',(10.9340669532922,20.1445799211063,96.1799079580775));
#112778=CARTESIAN_POINT('Ctrl Pts',(10.9503960020745,20.1499772958843,96.1665367899462));
#112779=CARTESIAN_POINT('Ctrl Pts',(10.9585605264657,20.1526759832733,96.1598512058805));
#112780=CARTESIAN_POINT('Ctrl Pts',(10.9666986013493,20.1553594591464,96.1531793110346));
#112781=CARTESIAN_POINT('Ctrl Pts',(10.9748102418903,20.1580278552853,96.1465212440585));
#112782=CARTESIAN_POINT('Ctrl Pts',(10.9829218824312,20.1606962514242,96.1398631770824));
#112783=CARTESIAN_POINT('Ctrl Pts',(10.9926014686587,20.1638715521178,96.1319071805507));
#112784=CARTESIAN_POINT('Ctrl Pts',(10.9990658759471,20.165987935302,96.1265886649839));
#112785=CARTESIAN_POINT('Ctrl Pts',(11.0818740054802,20.1930985001283,96.0584592439361));
#112786=CARTESIAN_POINT('Ctrl Pts',(11.1696312337331,20.2211666649735,95.9854307495776));
#112787=CARTESIAN_POINT('Ctrl Pts',(11.2622619314072,20.2499219836152,95.9071881388308));
#112788=CARTESIAN_POINT('Ctrl Pts',(11.3435991454559,20.2751714696509,95.8384848240785));
#112789=CARTESIAN_POINT('Ctrl Pts',(11.428693788411,20.3009503157172,95.7657607532074));
#112790=CARTESIAN_POINT('Ctrl Pts',(11.5174819094351,20.3270576395467,95.6887777177979));
#112791=CARTESIAN_POINT('Ctrl Pts',(11.6214331785391,20.3576235464909,95.5986475952322));
#112792=CARTESIAN_POINT('Ctrl Pts',(11.7304491331547,20.3886400129683,95.5026781603857));
#112793=CARTESIAN_POINT('Ctrl Pts',(11.8443765358371,20.4197639254504,95.4005049410484));
#112794=CARTESIAN_POINT('Ctrl Pts',(11.9559928176839,20.4502564611001,95.3004043982621));
#112795=CARTESIAN_POINT('Ctrl Pts',(12.0723236790256,20.4808519046811,95.1943487770492));
#112796=CARTESIAN_POINT('Ctrl Pts',(12.1931818716125,20.5112046304692,95.0819849448582));
#112797=CARTESIAN_POINT('Ctrl Pts',(12.3094842731162,20.5404131998328,94.9738567059176));
#112798=CARTESIAN_POINT('Ctrl Pts',(12.4299793180954,20.5693967541912,94.8598864746458));
#112799=CARTESIAN_POINT('Ctrl Pts',(12.5544558512573,20.5978293238787,94.7397559166034));
#112800=CARTESIAN_POINT('Ctrl Pts',(12.6759694988279,20.6255851198089,94.6224847979304));
#112801=CARTESIAN_POINT('Ctrl Pts',(12.8012776177519,20.6528156642883,94.4993427834358));
#112802=CARTESIAN_POINT('Ctrl Pts',(12.930137215551,20.6792033322693,94.370035537127));
#112803=CARTESIAN_POINT('Ctrl Pts',(13.0543738883018,20.7046443248505,94.245367275559));
#112804=CARTESIAN_POINT('Ctrl Pts',(13.1819119164582,20.7293016507751,94.114967928198));
#112805=CARTESIAN_POINT('Ctrl Pts',(13.3124870307784,20.7528798152625,93.9785799115993));
#112806=CARTESIAN_POINT('Ctrl Pts',(13.3813266858498,20.7653103057045,93.9066756742));
#112807=CARTESIAN_POINT('Ctrl Pts',(13.4510096790417,20.7774406823677,93.8331070550628));
#112808=CARTESIAN_POINT('Ctrl Pts',(13.5214915861578,20.789226618785,93.7578374459239));
#112809=CARTESIAN_POINT('Ctrl Pts',(13.6749060720465,20.8148804844387,93.5940018055224));
#112810=CARTESIAN_POINT('Ctrl Pts',(13.8321074502674,20.8389019522866,93.4221100941343));
#112811=CARTESIAN_POINT('Ctrl Pts',(13.992732783026,20.8608671652904,93.24164273448));
#112812=CARTESIAN_POINT('Ctrl Pts',(14.065572171761,20.8708278150904,93.1598055053326));
#112813=CARTESIAN_POINT('Ctrl Pts',(14.1391150943112,20.8803656645332,93.0762043821394));
#112814=CARTESIAN_POINT('Ctrl Pts',(14.2133248047303,20.8894415798287,92.9907888952405));
#112815=CARTESIAN_POINT('Ctrl Pts',(14.3109575206791,20.9013821500724,92.8784134941921));
#112816=CARTESIAN_POINT('Ctrl Pts',(14.4097445882159,20.9125230950735,92.7628977570874));
#112817=CARTESIAN_POINT('Ctrl Pts',(14.5095972235387,20.9227764232584,92.6441234712457));
#112818=CARTESIAN_POINT('Ctrl Pts',(14.5595235412001,20.9279030873509,92.5847363283249));
#112819=CARTESIAN_POINT('Ctrl Pts',(14.6097162484685,20.9328078761558,92.5245345486646));
#112820=CARTESIAN_POINT('Ctrl Pts',(14.6601635801387,20.9374799404975,92.4635029456918));
#112821=CARTESIAN_POINT('Ctrl Pts',(14.6853872459738,20.9398159726684,92.4329871442054));
#112822=CARTESIAN_POINT('Ctrl Pts',(14.710674567712,20.9420938259984,92.4022638869283));
#112823=CARTESIAN_POINT('Ctrl Pts',(14.7360240539024,20.9443121571214,92.3713312646967));
#112824=CARTESIAN_POINT('Ctrl Pts',(14.7486987969976,20.9454213226829,92.3558649535809));
#112825=CARTESIAN_POINT('Ctrl Pts',(14.7613890811952,20.9465156078426,92.3403463012285));
#112826=CARTESIAN_POINT('Ctrl Pts',(14.774094717722,20.9475948454575,92.3247750676269));
#112827=CARTESIAN_POINT('Ctrl Pts',(14.7804475359853,20.9481344642649,92.3169894508261));
#112828=CARTESIAN_POINT('Ctrl Pts',(14.7868041923303,20.9486703211959,92.3091906887131));
#112829=CARTESIAN_POINT('Ctrl Pts',(14.7931646630046,20.9492023954075,92.3013787511973));
#112830=CARTESIAN_POINT('Ctrl Pts',(14.7995251336789,20.9497344696191,92.2935668136815));
#112831=CARTESIAN_POINT('Ctrl Pts',(14.8071091475034,20.9503632205178,92.2842403644937));
#112832=CARTESIAN_POINT('Ctrl Pts',(14.8122574942145,20.9507872490788,92.2779033823244));
#112833=CARTESIAN_POINT('Ctrl Pts',(15.0054140661669,20.9666960267569,92.0401513774521));
#112834=CARTESIAN_POINT('Ctrl Pts',(15.1956957611478,20.9785834093345,91.7979202834243));
#112835=CARTESIAN_POINT('Ctrl Pts',(15.3829840419243,20.9866600873303,91.5512433302939));
#112836=CARTESIAN_POINT('Ctrl Pts',(15.8633605515616,21.0073759931469,90.9185405618053));
#112837=CARTESIAN_POINT('Ctrl Pts',(16.3240405690058,21.0030203136065,90.256589250856));
#112838=CARTESIAN_POINT('Ctrl Pts',(16.7623705722965,20.9778487372575,89.5701434912169));
#112839=CARTESIAN_POINT('Ctrl Pts',(16.8643593595663,20.9719919204158,89.410424170097));
#112840=CARTESIAN_POINT('Ctrl Pts',(16.9651383553155,20.9650082821789,89.24937879876));
#112841=CARTESIAN_POINT('Ctrl Pts',(17.0646744743569,20.9569516053128,89.0870673107852));
#112842=CARTESIAN_POINT('Ctrl Pts',(17.5374317754215,20.9186855683457,88.3161517705195));
#112843=CARTESIAN_POINT('Ctrl Pts',(17.9821471685851,20.8562122789627,87.5166739726371));
#112844=CARTESIAN_POINT('Ctrl Pts',(18.3957624236964,20.7754934985282,86.6957101104845));
#112845=CARTESIAN_POINT('Ctrl Pts',(18.4435021572208,20.7661768859983,86.6009539439071));
#112846=CARTESIAN_POINT('Ctrl Pts',(18.4908276334093,20.7566172155477,86.5059115415749));
#112847=CARTESIAN_POINT('Ctrl Pts',(18.537734193146,20.7468236567509,86.4105937818987));
#112848=CARTESIAN_POINT('Ctrl Pts',(18.9662594531666,20.6573524323955,85.5397972882066));
#112849=CARTESIAN_POINT('Ctrl Pts',(19.3598171159288,20.5483617098516,84.6460200651757));
#112850=CARTESIAN_POINT('Ctrl Pts',(19.7197007721944,20.4254862467279,83.7274864709089));
#112851=CARTESIAN_POINT('Ctrl Pts',(20.121198686996,20.2884023826359,82.7027405110613));
#112852=CARTESIAN_POINT('Ctrl Pts',(20.4807861174765,20.1340385981811,81.6471815928633));
#112853=CARTESIAN_POINT('Ctrl Pts',(20.8003130801046,19.9701890915409,80.5583314861816));
#112854=CARTESIAN_POINT('Ctrl Pts',(7.33390977334909,18.51896019671,98.61558102776));
#112855=CARTESIAN_POINT('Ctrl Pts',(6.63322704598623,18.1147877634574,98.9948595799931));
#112856=CARTESIAN_POINT('Ctrl Pts',(5.89295788622676,17.6398039918909,99.2724209778057));
#112857=CARTESIAN_POINT('Ctrl Pts',(4.74849242406141,16.801502773932,99.531723109432));
#112858=CARTESIAN_POINT('Ctrl Pts',(4.36140549410044,16.5011208865675,99.5919699821525));
#112859=CARTESIAN_POINT('Ctrl Pts',(3.77627559787738,16.0169956123106,99.642372183263));
#112860=CARTESIAN_POINT('Ctrl Pts',(3.58048761657308,15.8500313075335,99.6525106426868));
#112861=CARTESIAN_POINT('Ctrl Pts',(3.28622330212731,15.5909646268607,99.657630641654));
#112862=CARTESIAN_POINT('Ctrl Pts',(3.13894605544017,15.4592765754447,99.6576686311094));
#112863=CARTESIAN_POINT('Ctrl Pts',(2.96699089507222,15.3018219412834,99.6532778873175));
#112864=CARTESIAN_POINT('Ctrl Pts',(2.88099605374559,15.2221343132077,99.649970986995));
#112865=CARTESIAN_POINT('Ctrl Pts',(2.83799628675308,15.1820497226923,99.6480393075469));
#112866=CARTESIAN_POINT('Ctrl Pts',(2.8195675244896,15.1648189435875,99.6471517869677));
#112867=CARTESIAN_POINT('Ctrl Pts',(2.80728164201297,15.1533202673855,99.6465468450906));
#112868=CARTESIAN_POINT('Ctrl Pts',(2.80006760744145,15.1465607400022,99.6461826927322));
#112869=CARTESIAN_POINT('Ctrl Pts',(2.47039426792358,14.8373955143149,99.6292382431169));
#112870=CARTESIAN_POINT('Ctrl Pts',(2.13940644347902,14.5110408544986,99.5933956312336));
#112871=CARTESIAN_POINT('Ctrl Pts',(1.63792852770526,13.9860880137101,99.5100852681188));
#112872=CARTESIAN_POINT('Ctrl Pts',(1.46994338013475,13.8052029378049,99.4773895309509));
#112873=CARTESIAN_POINT('Ctrl Pts',(1.21736259553632,13.524741470774,99.4208454099032));
#112874=CARTESIAN_POINT('Ctrl Pts',(1.09092209996242,13.3822276363525,99.3906981037323));
#112875=CARTESIAN_POINT('Ctrl Pts',(0.943291600146698,13.2119084215627,
99.3522188066159));
#112876=CARTESIAN_POINT('Ctrl Pts',(0.869465991839432,13.1257286835316,
99.3321489851273));
#112877=CARTESIAN_POINT('Ctrl Pts',(0.83255296139824,13.0823829352355,99.3219061144348));
#112878=CARTESIAN_POINT('Ctrl Pts',(0.81673329746239,13.0637512650341,99.3174717049452));
#112879=CARTESIAN_POINT('Ctrl Pts',(0.806186929066697,13.051317937016,99.314505514109));
#112880=CARTESIAN_POINT('Ctrl Pts',(0.799877375459519,13.0438709028361,
99.3127240133116));
#112881=CARTESIAN_POINT('Ctrl Pts',(0.524492575138919,12.718570563598,99.2347520082104));
#112882=CARTESIAN_POINT('Ctrl Pts',(0.241494197014471,12.3680862536953,
99.1412693519639));
#112883=CARTESIAN_POINT('Ctrl Pts',(-0.193563578726575,11.7932354542952,
98.9747078038906));
#112884=CARTESIAN_POINT('Ctrl Pts',(-0.340328439984648,11.5934330443894,
98.9147951491503));
#112885=CARTESIAN_POINT('Ctrl Pts',(-0.562058097063683,11.2810031769473,
98.8181552773681));
#112886=CARTESIAN_POINT('Ctrl Pts',(-0.673317085489583,11.1216071368294,
98.7681423666626));
#112887=CARTESIAN_POINT('Ctrl Pts',(-0.803567088169475,10.9299858870827,
98.7067886060777));
#112888=CARTESIAN_POINT('Ctrl Pts',(-0.86877265525937,10.8327494392575,
98.6753548485219));
#112889=CARTESIAN_POINT('Ctrl Pts',(-0.90488651237819,10.7785259673729,
98.6577437530991));
#112890=CARTESIAN_POINT('Ctrl Pts',(-0.922365710419661,10.7521687743111,
98.649158549259));
#112891=CARTESIAN_POINT('Ctrl Pts',(-0.931688985831928,10.738081682025,
98.6445638924));
#112892=CARTESIAN_POINT('Ctrl Pts',(-0.933921641068739,10.7347067958116,
98.6434628273561));
#112893=CARTESIAN_POINT('Ctrl Pts',(-0.959163860730728,10.6965448724609,
98.6310111690001));
#112894=CARTESIAN_POINT('Ctrl Pts',(-1.10562671612739,10.481109110981,98.5580089322338));
#112895=CARTESIAN_POINT('Ctrl Pts',(-1.47832025232363,9.87531424826814,
98.3524972497975));
#112896=CARTESIAN_POINT('Ctrl Pts',(-1.62755303669153,9.62598937210525,
98.2679041093474));
#112897=CARTESIAN_POINT('Ctrl Pts',(-1.88050856857826,9.17685763766061,
98.1154000785185));
#112898=CARTESIAN_POINT('Ctrl Pts',(-1.96964332888882,9.01461246026334,
98.0602902103554));
#112899=CARTESIAN_POINT('Ctrl Pts',(-2.10919509042164,8.75187222534487,
97.9709702151545));
#112900=CARTESIAN_POINT('Ctrl Pts',(-2.18042989056037,8.61565858151007,
97.9246458046577));
#112901=CARTESIAN_POINT('Ctrl Pts',(-2.26575206205299,8.44813945470475,
97.8676283019775));
#112902=CARTESIAN_POINT('Ctrl Pts',(-2.30892174604868,8.36221323615283,
97.838368504093));
#112903=CARTESIAN_POINT('Ctrl Pts',(-2.33217846248433,8.31559886746861,
97.8224913580097));
#112904=CARTESIAN_POINT('Ctrl Pts',(-2.34306616694847,8.29368664839123,
97.8150268158695));
#112905=CARTESIAN_POINT('Ctrl Pts',(-2.34929602204302,8.28112642642193,
97.8107478154731));
#112906=CARTESIAN_POINT('Ctrl Pts',(-2.35141537312412,8.27685034503791,
97.8092910057185));
#112907=CARTESIAN_POINT('Ctrl Pts',(-2.60781128656009,7.75931157392258,
97.6329689188456));
#112908=CARTESIAN_POINT('Ctrl Pts',(-2.81988247376081,7.27975194019941,
97.4744733855343));
#112909=CARTESIAN_POINT('Ctrl Pts',(-3.08696094432641,6.62204013560463,
97.2649027297406));
#112910=CARTESIAN_POINT('Ctrl Pts',(-3.16746394030832,6.41303970283115,
97.1997380332611));
#112911=CARTESIAN_POINT('Ctrl Pts',(-3.27698929875688,6.11558188393791,
97.1093035669909));
#112912=CARTESIAN_POINT('Ctrl Pts',(-3.32894253061792,5.97086114834436,
97.0659140969878));
#112913=CARTESIAN_POINT('Ctrl Pts',(-3.38495455445906,5.80916015520684,
97.0185474333141));
#112914=CARTESIAN_POINT('Ctrl Pts',(-3.41184824305314,5.73010863336922,
96.9956843445836));
#112915=CARTESIAN_POINT('Ctrl Pts',(-3.42596262200767,5.68824330614735,
96.9836568490984));
#112916=CARTESIAN_POINT('Ctrl Pts',(-3.43247025515977,5.66883807128544,
96.9781041851881));
#112917=CARTESIAN_POINT('Ctrl Pts',(-3.43616965951519,5.65778171617176,
96.9749459908604));
#112918=CARTESIAN_POINT('Ctrl Pts',(-3.43672740741094,5.65611434503391,
96.9744698093448));
#112919=CARTESIAN_POINT('Ctrl Pts',(-3.60276935109794,5.15911377442937,
96.8326696635262));
#112920=CARTESIAN_POINT('Ctrl Pts',(-3.74098279039443,4.67976192410362,
96.7084340657658));
#112921=CARTESIAN_POINT('Ctrl Pts',(-3.91397760600031,3.98465723159937,
96.5477461043137));
#112922=CARTESIAN_POINT('Ctrl Pts',(-3.96592027330548,3.75693302543452,
96.4984607795777));
#112923=CARTESIAN_POINT('Ctrl Pts',(-4.03591904901806,3.42163371778403,
96.4310666045399));
#112924=CARTESIAN_POINT('Ctrl Pts',(-4.06893940480704,3.25555499975203,
96.3990029302307));
#112925=CARTESIAN_POINT('Ctrl Pts',(-4.10414338226531,3.06460755890891,
96.3644790924407));
#112926=CARTESIAN_POINT('Ctrl Pts',(-4.12093315304482,2.96984375547221,
96.347941244464));
#112927=CARTESIAN_POINT('Ctrl Pts',(-4.12795661551212,2.92938357525808,
96.3410090871936));
#112928=CARTESIAN_POINT('Ctrl Pts',(-4.13260087720269,2.90244417691176,
96.3364222397417));
#112929=CARTESIAN_POINT('Ctrl Pts',(-4.13456032116638,2.89101293526736,
96.3344859573235));
#112930=CARTESIAN_POINT('Ctrl Pts',(-4.30537073788798,1.88630577984655,
96.1655730269347));
#112931=CARTESIAN_POINT('Ctrl Pts',(-4.3822632519282,0.924422265265613,
96.0811302365448));
#112932=CARTESIAN_POINT('Ctrl Pts',(-4.38226888389591,-1.31660223688345E-7,
96.08109859282));
#112933=CARTESIAN_POINT('Origin',(6.43246351666909,-92.,72.98888938658));
#112934=CARTESIAN_POINT('',(16.0575353748791,-92.5,68.792701625727));
#112935=CARTESIAN_POINT('',(16.0575353748791,-92.5,77.185077147433));
#112936=CARTESIAN_POINT('Origin',(6.43246351666909,-92.5,72.98888938658));
#112937=CARTESIAN_POINT('Origin',(16.0575353748791,-92.,68.792701625727));
#112938=CARTESIAN_POINT('Origin',(16.0575353748791,-92.,77.185077147433));
#112939=CARTESIAN_POINT('Origin',(27.4324635166691,25.,72.98888938658));
#112940=CARTESIAN_POINT('',(-10.7897587056049,60.03337045294,84.7813330856));
#112941=CARTESIAN_POINT('',(-12.5675365956403,55.41742345328,72.9889053195275));
#112942=CARTESIAN_POINT('Ctrl Pts',(-10.7897587055637,60.03337045294,84.7813330855873));
#112943=CARTESIAN_POINT('Ctrl Pts',(-10.868172625638,59.7799388856398,84.5271742059778));
#112944=CARTESIAN_POINT('Ctrl Pts',(-10.9470443127566,59.5350540421005,
84.2625454327982));
#112945=CARTESIAN_POINT('Ctrl Pts',(-11.0257532130399,59.298715922322,83.9873240920612));
#112946=CARTESIAN_POINT('Ctrl Pts',(-11.1037577008792,59.0644929319882,
83.7145658696824));
#112947=CARTESIAN_POINT('Ctrl Pts',(-11.1816022537234,58.8386643706073,
83.4314035267827));
#112948=CARTESIAN_POINT('Ctrl Pts',(-11.2586336094918,58.6212302381791,
83.1377318414606));
#112949=CARTESIAN_POINT('Ctrl Pts',(-11.2788912404733,58.5640496216161,
83.0605023474235));
#112950=CARTESIAN_POINT('Ctrl Pts',(-11.2990923685216,58.507449546707,82.9825461391374));
#112951=CARTESIAN_POINT('Ctrl Pts',(-11.319224547268,58.4514300134518,82.9038615093504));
#112952=CARTESIAN_POINT('Ctrl Pts',(-11.3482132341978,58.3707664781265,
82.7905620931367));
#112953=CARTESIAN_POINT('Ctrl Pts',(-11.377059007869,58.2913066169089,82.675752374104));
#112954=CARTESIAN_POINT('Ctrl Pts',(-11.4057238500298,58.2130504297991,
82.5594276195734));
#112955=CARTESIAN_POINT('Ctrl Pts',(-11.4200562711102,58.1739223362441,
82.5012652423081));
#112956=CARTESIAN_POINT('Ctrl Pts',(-11.4343434459378,58.1350951612161,
82.4427241029007));
#112957=CARTESIAN_POINT('Ctrl Pts',(-11.4485805234591,58.096568904715,82.3838036677011));
#112958=CARTESIAN_POINT('Ctrl Pts',(-11.4606645752162,58.06386884553,82.3337935734635));
#112959=CARTESIAN_POINT('Ctrl Pts',(-11.4730195897738,58.0305659718623,
82.2822208527233));
#112960=CARTESIAN_POINT('Ctrl Pts',(-11.484860368321,57.9987472502754,82.2323682571557));
#112961=CARTESIAN_POINT('Ctrl Pts',(-11.4869700498907,57.9930780816277,
82.2234859778654));
#112962=CARTESIAN_POINT('Ctrl Pts',(-11.4890635377764,57.9874560271675,
82.2146583348573));
#112963=CARTESIAN_POINT('Ctrl Pts',(-11.491136558511,57.9818928907926,82.2059039350897));
#112964=CARTESIAN_POINT('Ctrl Pts',(-11.5941202893394,57.7055268470603,
81.7710019902227));
#112965=CARTESIAN_POINT('Ctrl Pts',(-11.6914739522762,57.452348325549,81.3273738179643));
#112966=CARTESIAN_POINT('Ctrl Pts',(-11.7824236113942,57.2223573262586,
80.875119635137));
#112967=CARTESIAN_POINT('Ctrl Pts',(-11.7883235253147,57.2074377860266,
80.8457818588909));
#112968=CARTESIAN_POINT('Ctrl Pts',(-11.7941964818091,57.192615821914,80.8164077994128));
#112969=CARTESIAN_POINT('Ctrl Pts',(-11.8000422660877,57.1778914339208,
80.7869974908546));
#112970=CARTESIAN_POINT('Ctrl Pts',(-11.8480227721674,57.0570379172761,
80.5456061870847));
#112971=CARTESIAN_POINT('Ctrl Pts',(-11.8941729321993,56.942757763715,80.3017725851317));
#112972=CARTESIAN_POINT('Ctrl Pts',(-11.9383729337204,56.8350509732375,
80.0555178044805));
#112973=CARTESIAN_POINT('Ctrl Pts',(-11.960472934481,56.7811975779987,79.9323904141548));
#112974=CARTESIAN_POINT('Ctrl Pts',(-11.9820853781408,56.7289875235308,
79.8086577260715));
#112975=CARTESIAN_POINT('Ctrl Pts',(-12.0031951051495,56.6784208098339,
79.6843228350869));
#112976=CARTESIAN_POINT('Ctrl Pts',(-12.0137499686538,56.6531374529854,
79.6221553895946));
#112977=CARTESIAN_POINT('Ctrl Pts',(-12.0241791520448,56.6282649313297,
79.5598373931977));
#112978=CARTESIAN_POINT('Ctrl Pts',(-12.0344807519995,56.6038032448667,
79.4973692470241));
#112979=CARTESIAN_POINT('Ctrl Pts',(-12.0442431275652,56.5806219748433,
79.438170917976));
#112980=CARTESIAN_POINT('Ctrl Pts',(-12.0540526293657,56.5574302292912,
79.3778303823676));
#112981=CARTESIAN_POINT('Ctrl Pts',(-12.0634478798237,56.5353067074411,
79.3192118870842));
#112982=CARTESIAN_POINT('Ctrl Pts',(-12.0639668260734,56.5340847156757,
79.3159740970514));
#112983=CARTESIAN_POINT('Ctrl Pts',(-12.0644845215157,56.5328659829544,
79.3127415628864));
#112984=CARTESIAN_POINT('Ctrl Pts',(-12.0650008929351,56.5316506910558,
79.3095147679841));
#112985=CARTESIAN_POINT('Ctrl Pts',(-12.1397505417616,56.3557256897246,
78.8424056741844));
#112986=CARTESIAN_POINT('Ctrl Pts',(-12.2072603484823,56.2006332465385,
78.3674356697261));
#112987=CARTESIAN_POINT('Ctrl Pts',(-12.2667800777976,56.0663733614975,
77.8848119786146));
#112988=CARTESIAN_POINT('Ctrl Pts',(-12.3253653812388,55.9342212802365,
77.4097652047641));
#112989=CARTESIAN_POINT('Ctrl Pts',(-12.376209304955,55.8222527731538,76.9273030816847));
#112990=CARTESIAN_POINT('Ctrl Pts',(-12.4185828867259,55.7304678402495,
76.4376718607956));
#112991=CARTESIAN_POINT('Ctrl Pts',(-12.4605719336758,55.6395158438418,
75.9524839804513));
#112992=CARTESIAN_POINT('Ctrl Pts',(-12.4942434699381,55.5683827571013,
75.4602563976354));
#112993=CARTESIAN_POINT('Ctrl Pts',(-12.5188778974991,55.5170685800279,
74.961278599836));
#112994=CARTESIAN_POINT('Ctrl Pts',(-12.5431986105029,55.4664078788389,
74.4686551854904));
#112995=CARTESIAN_POINT('Ctrl Pts',(-12.5587107041102,55.4350645216717,
73.9694523035646));
#112996=CARTESIAN_POINT('Ctrl Pts',(-12.5647147706704,55.4230385085262,
73.463998901091));
#112997=CARTESIAN_POINT('Ctrl Pts',(-12.5665887310681,55.4192850071033,
73.306239214448));
#112998=CARTESIAN_POINT('Ctrl Pts',(-12.5675364200079,55.4174133220213,
73.1478710057732));
#112999=CARTESIAN_POINT('Ctrl Pts',(-12.5675364833277,55.41742345328,72.9889053195274));
#113000=CARTESIAN_POINT('',(-10.7897587056049,60.03337045294,61.19644568756));
#113001=CARTESIAN_POINT('Ctrl Pts',(-12.5675367079528,55.4174234532799,
72.9889053195275));
#113002=CARTESIAN_POINT('Ctrl Pts',(-12.5675367177603,55.4174203621651,
72.982050838097));
#113003=CARTESIAN_POINT('Ctrl Pts',(-12.5675348841624,55.4174209999673,
72.975196614252));
#113004=CARTESIAN_POINT('Ctrl Pts',(-12.5675312063047,55.4174253640918,
72.9683426483062));
#113005=CARTESIAN_POINT('Ctrl Pts',(-12.5673418846505,55.4176500120605,
72.6155274331763));
#113006=CARTESIAN_POINT('Ctrl Pts',(-12.5622677006653,55.4277450225524,
72.2633971372145));
#113007=CARTESIAN_POINT('Ctrl Pts',(-12.5525370191446,55.4476997595703,
71.9120808674882));
#113008=CARTESIAN_POINT('Ctrl Pts',(-12.5474620952179,55.4581069208906,
71.7288559475002));
#113009=CARTESIAN_POINT('Ctrl Pts',(-12.5411201910958,55.4711966604094,
71.5458521388165));
#113010=CARTESIAN_POINT('Ctrl Pts',(-12.5335411140015,55.4869721096583,
71.3630859763134));
#113011=CARTESIAN_POINT('Ctrl Pts',(-12.5334665414226,55.4871273285483,
71.3612876908618));
#113012=CARTESIAN_POINT('Ctrl Pts',(-12.5333918499186,55.4872828063653,
71.3594894491793));
#113013=CARTESIAN_POINT('Ctrl Pts',(-12.5333170395134,55.4874385430894,
71.3576912509943));
#113014=CARTESIAN_POINT('Ctrl Pts',(-12.52530966692,55.5041079084492,71.1652201257191));
#113015=CARTESIAN_POINT('Ctrl Pts',(-12.5159419633816,55.5237395698145,
70.9732476647015));
#113016=CARTESIAN_POINT('Ctrl Pts',(-12.5052315297495,55.5463351816122,
70.781537963485));
#113017=CARTESIAN_POINT('Ctrl Pts',(-12.494586011557,55.5687938424586,70.5909902058433));
#113018=CARTESIAN_POINT('Ctrl Pts',(-12.4826139196493,55.5941806061267,
70.4007016562411));
#113019=CARTESIAN_POINT('Ctrl Pts',(-12.4693110004844,55.62254352577,70.2104401810274));
#113020=CARTESIAN_POINT('Ctrl Pts',(-12.4587206881529,55.6451229441618,
70.0589750460298));
#113021=CARTESIAN_POINT('Ctrl Pts',(-12.4472865330326,55.6695893954222,
69.9075269903875));
#113022=CARTESIAN_POINT('Ctrl Pts',(-12.4349969289486,55.6959886852669,
69.7559810535915));
#113023=CARTESIAN_POINT('Ctrl Pts',(-12.4348262620416,55.6963552947291,
69.7538765206772));
#113024=CARTESIAN_POINT('Ctrl Pts',(-12.434655430027,55.6967222772554,69.7517719689367));
#113025=CARTESIAN_POINT('Ctrl Pts',(-12.4344844328715,55.6970896329577,
69.7496673980763));
#113026=CARTESIAN_POINT('Ctrl Pts',(-12.4147573136269,55.7394696931722,
69.5068731819895));
#113027=CARTESIAN_POINT('Ctrl Pts',(-12.3930365100942,55.7865471590384,
69.2663150158759));
#113028=CARTESIAN_POINT('Ctrl Pts',(-12.369431751922,55.8382937182926,69.0280167934519));
#113029=CARTESIAN_POINT('Ctrl Pts',(-12.3456145013075,55.8905061053548,
68.7875733861069));
#113030=CARTESIAN_POINT('Ctrl Pts',(-12.3198790436771,55.9474720578215,
68.5494302363846));
#113031=CARTESIAN_POINT('Ctrl Pts',(-12.2923167664104,56.0092105053825,
68.3136166604113));
#113032=CARTESIAN_POINT('Ctrl Pts',(-12.2871240455808,56.0208420015589,
68.2691894871404));
#113033=CARTESIAN_POINT('Ctrl Pts',(-12.2818664270495,56.0326430296357,
68.2248450281788));
#113034=CARTESIAN_POINT('Ctrl Pts',(-12.2765444463086,56.0446139033485,
68.1805835236521));
#113035=CARTESIAN_POINT('Ctrl Pts',(-12.2761514642722,56.0454978483604,
68.1773151961197));
#113036=CARTESIAN_POINT('Ctrl Pts',(-12.2757581312882,56.0463827194888,
68.1740473209075));
#113037=CARTESIAN_POINT('Ctrl Pts',(-12.2753644474245,56.0472685174559,
68.1707798974206));
#113038=CARTESIAN_POINT('Ctrl Pts',(-12.2443292802395,56.117098374705,67.9132000382251));
#113039=CARTESIAN_POINT('Ctrl Pts',(-12.2111136956103,56.1926615310602,
67.6584279769369));
#113040=CARTESIAN_POINT('Ctrl Pts',(-12.1757902067591,56.2739580008499,
67.406503196972));
#113041=CARTESIAN_POINT('Ctrl Pts',(-12.1581284623335,56.3146062357447,
67.2805408069895));
#113042=CARTESIAN_POINT('Ctrl Pts',(-12.1399397377143,56.3566878012821,
67.1552903360582));
#113043=CARTESIAN_POINT('Ctrl Pts',(-12.1212330098288,56.4002027038148,
67.0307566887872));
#113044=CARTESIAN_POINT('Ctrl Pts',(-12.1118796458861,56.4219601550811,
66.9684898651518));
#113045=CARTESIAN_POINT('Ctrl Pts',(-12.1023967812998,56.4440759405653,
66.9064022535711));
#113046=CARTESIAN_POINT('Ctrl Pts',(-12.0927855383316,56.4665500603436,
66.84449448797));
#113047=CARTESIAN_POINT('Ctrl Pts',(-12.0879799168475,56.4777871202328,
66.8135406051694));
#113048=CARTESIAN_POINT('Ctrl Pts',(-12.0831422008074,56.4891137636837,
66.7826316842441));
#113049=CARTESIAN_POINT('Ctrl Pts',(-12.0782725304343,56.5005299906145,
66.7517678045529));
#113050=CARTESIAN_POINT('Ctrl Pts',(-12.0741631291214,56.5101638784021,
66.7257224959376));
#113051=CARTESIAN_POINT('Ctrl Pts',(-12.0701688778298,56.5195377148765,
66.7005734698854));
#113052=CARTESIAN_POINT('Ctrl Pts',(-12.0659408536375,56.5294710194743,
66.6741328100669));
#113053=CARTESIAN_POINT('Ctrl Pts',(-12.0651586384838,56.5313087528999,
66.6692410961496));
#113054=CARTESIAN_POINT('Ctrl Pts',(-12.0643683768756,56.5331657640086,
66.6643052146056));
#113055=CARTESIAN_POINT('Ctrl Pts',(-12.0635677966548,56.535047421687,66.6593113694085));
#113056=CARTESIAN_POINT('Ctrl Pts',(-12.0630538197315,56.536255456309,66.6561052932107));
#113057=CARTESIAN_POINT('Ctrl Pts',(-12.0625394985148,56.5374644904417,
66.652899713093));
#113058=CARTESIAN_POINT('Ctrl Pts',(-12.0620248331215,56.5386745244904,
66.6496946288546));
#113059=CARTESIAN_POINT('Ctrl Pts',(-12.0160725489409,56.6467133186074,
66.3635262879531));
#113060=CARTESIAN_POINT('Ctrl Pts',(-11.967379099974,56.7627198108511,66.0813107384538));
#113061=CARTESIAN_POINT('Ctrl Pts',(-11.9163040906976,56.8866775804625,
65.8030527981967));
#113062=CARTESIAN_POINT('Ctrl Pts',(-11.8771617699855,56.9816750134855,
65.589804446556));
#113063=CARTESIAN_POINT('Ctrl Pts',(-11.8366199972925,57.0813432649774,
65.3788805106926));
#113064=CARTESIAN_POINT('Ctrl Pts',(-11.7948293248868,57.1856921089343,
65.170285466387));
#113065=CARTESIAN_POINT('Ctrl Pts',(-11.7942686561782,57.1870920656284,
65.1674869300781));
#113066=CARTESIAN_POINT('Ctrl Pts',(-11.7937077625437,57.1884928650177,
65.1646888129909));
#113067=CARTESIAN_POINT('Ctrl Pts',(-11.7931466444446,57.1898945067013,
65.1618911157007));
#113068=CARTESIAN_POINT('Ctrl Pts',(-11.7543525232861,57.2868000554267,
64.9684662238414));
#113069=CARTESIAN_POINT('Ctrl Pts',(-11.7144860248049,57.3877303365134,
64.7770433401785));
#113070=CARTESIAN_POINT('Ctrl Pts',(-11.6736515325127,57.4926792079085,
64.5876187494813));
#113071=CARTESIAN_POINT('Ctrl Pts',(-11.6631346852652,57.5197085937856,
64.5388327998231));
#113072=CARTESIAN_POINT('Ctrl Pts',(-11.6525535566606,57.5470047844004,
64.4901794771697));
#113073=CARTESIAN_POINT('Ctrl Pts',(-11.6419097870471,57.5745681821331,
64.4416588980482));
#113074=CARTESIAN_POINT('Ctrl Pts',(-11.6159242509573,57.6418610391336,
64.3232014994337));
#113075=CARTESIAN_POINT('Ctrl Pts',(-11.5895653660488,57.7107441790474,
64.2055345618778));
#113076=CARTESIAN_POINT('Ctrl Pts',(-11.5628547265451,57.7812175829487,
64.0886576456412));
#113077=CARTESIAN_POINT('Ctrl Pts',(-11.5476899162953,57.8212284481947,
64.0223014561138));
#113078=CARTESIAN_POINT('Ctrl Pts',(-11.5325098453544,57.861491635489,63.9566240152157));
#113079=CARTESIAN_POINT('Ctrl Pts',(-11.5171516660184,57.9024467648906,
63.8909009575293));
#113080=CARTESIAN_POINT('Ctrl Pts',(-11.5064596477077,57.9309588029324,
63.8451460460357));
#113081=CARTESIAN_POINT('Ctrl Pts',(-11.4956810919766,57.959807135689,63.7993694871288));
#113082=CARTESIAN_POINT('Ctrl Pts',(-11.4847584588285,57.9891528879259,
63.7533340900277));
#113083=CARTESIAN_POINT('Ctrl Pts',(-11.4837358338686,57.9919003663313,
63.7490240536585));
#113084=CARTESIAN_POINT('Ctrl Pts',(-11.4827119445604,57.9946522124987,
63.7447117530293));
#113085=CARTESIAN_POINT('Ctrl Pts',(-11.4816867427005,57.9974085638167,
63.7403969958321));
#113086=CARTESIAN_POINT('Ctrl Pts',(-11.4356078701281,58.1212959328434,
63.5464652884868));
#113087=CARTESIAN_POINT('Ctrl Pts',(-11.3889411870607,58.2488419536169,
63.3562493137595));
#113088=CARTESIAN_POINT('Ctrl Pts',(-11.3418218316508,58.3799615459157,
63.1697081560175));
#113089=CARTESIAN_POINT('Ctrl Pts',(-11.2938772096396,58.5133776174288,
62.9798998443447));
#113090=CARTESIAN_POINT('Ctrl Pts',(-11.245463670129,58.6504936180663,62.7938957316933));
#113091=CARTESIAN_POINT('Ctrl Pts',(-11.196706025114,58.7912696725781,62.611664155393));
#113092=CARTESIAN_POINT('Ctrl Pts',(-11.1477507289715,58.9326163975128,
62.4286938584979));
#113093=CARTESIAN_POINT('Ctrl Pts',(-11.0984482456183,59.0776530871168,
62.2495262909455));
#113094=CARTESIAN_POINT('Ctrl Pts',(-11.0489114884965,59.226386964476,62.0741478009945));
#113095=CARTESIAN_POINT('Ctrl Pts',(-10.9995158025983,59.3746972761584,
61.8992687554883));
#113096=CARTESIAN_POINT('Ctrl Pts',(-10.949886889216,59.5266839527353,61.728156812183));
#113097=CARTESIAN_POINT('Ctrl Pts',(-10.9001276897382,59.6823984335242,
61.560823247083));
#113098=CARTESIAN_POINT('Ctrl Pts',(-10.8633960277559,59.7973450511166,
61.437299556669));
#113099=CARTESIAN_POINT('Ctrl Pts',(-10.8265931653708,59.9143239540159,
61.3158352677684));
#113100=CARTESIAN_POINT('Ctrl Pts',(-10.7897587056886,60.03337045294,61.1964456875342));
#113101=CARTESIAN_POINT('',(-9.38953228746991,65.4601089375,57.36388938658));
#113102=CARTESIAN_POINT('Ctrl Pts',(-10.7897587055637,60.03337045294,61.1964456875727));
#113103=CARTESIAN_POINT('Ctrl Pts',(-10.6961215374564,60.3360244277033,
60.8929445016431));
#113104=CARTESIAN_POINT('Ctrl Pts',(-10.6017811001726,60.6488111261909,
60.5999839999674));
#113105=CARTESIAN_POINT('Ctrl Pts',(-10.5074126423797,60.9717305484028,
60.3174333914687));
#113106=CARTESIAN_POINT('Ctrl Pts',(-10.4809076023769,61.0624281438025,
60.2380740869275));
#113107=CARTESIAN_POINT('Ctrl Pts',(-10.4544000522521,61.1539250752782,
60.1595358809919));
#113108=CARTESIAN_POINT('Ctrl Pts',(-10.4279042524337,61.2462213428298,
60.081815652062));
#113109=CARTESIAN_POINT('Ctrl Pts',(-10.3674885729892,61.4566751412635,
59.9045981130723));
#113110=CARTESIAN_POINT('Ctrl Pts',(-10.3071345414077,61.6712849314232,
59.7316336177837));
#113111=CARTESIAN_POINT('Ctrl Pts',(-10.2470052704755,61.890050713309,59.5628835799898));
#113112=CARTESIAN_POINT('Ctrl Pts',(-10.2169406350094,61.9994336042519,
59.4785085610928));
#113113=CARTESIAN_POINT('Ctrl Pts',(-10.1869320857492,62.1098554931263,
59.3951871939623));
#113114=CARTESIAN_POINT('Ctrl Pts',(-10.156999204859,62.2213163799322,59.3129143826965));
#113115=CARTESIAN_POINT('Ctrl Pts',(-10.1270663239688,62.3327772667381,
59.2306415714307));
#113116=CARTESIAN_POINT('Ctrl Pts',(-10.0974532818734,62.4443457418673,
59.150075118638));
#113117=CARTESIAN_POINT('Ctrl Pts',(-10.067446726607,62.5588160341445,59.0692366701422));
#113118=CARTESIAN_POINT('Ctrl Pts',(-9.97973504987513,62.8934222954267,
58.8329391078582));
#113119=CARTESIAN_POINT('Ctrl Pts',(-9.89342052728445,63.2348821549413,
58.6072400191336));
#113120=CARTESIAN_POINT('Ctrl Pts',(-9.80904661013946,63.5831956126882,
58.3919745250479));
#113121=CARTESIAN_POINT('Ctrl Pts',(-9.724205933447,63.9334359530241,58.1755181744985));
#113122=CARTESIAN_POINT('Ctrl Pts',(-9.64132737070179,64.2906059300402,
57.9696108949634));
#113123=CARTESIAN_POINT('Ctrl Pts',(-9.56091064477735,64.6547055437366,
57.7740851436321));
#113124=CARTESIAN_POINT('Ctrl Pts',(-9.50242514788926,64.9195080034116,
57.6318831254627));
#113125=CARTESIAN_POINT('Ctrl Pts',(-9.44524070271336,65.1879758013327,
57.4951722686513));
#113126=CARTESIAN_POINT('Ctrl Pts',(-9.38953228746956,65.4601089375,57.3638893865801));
#113127=CARTESIAN_POINT('',(-9.38953228747191,-65.46010893749,57.36388938658));
#113128=CARTESIAN_POINT('',(-9.38953228747191,-65.46010893749,57.36388938658));
#113129=CARTESIAN_POINT('',(-10.7897587056049,-60.03337045294,61.19644568756));
#113130=CARTESIAN_POINT('Ctrl Pts',(-9.38953228746987,-65.46010893749,57.3638893865809));
#113131=CARTESIAN_POINT('Ctrl Pts',(-9.46407446179315,-65.0959614287623,
57.5395560509113));
#113132=CARTESIAN_POINT('Ctrl Pts',(-9.54149305329802,-64.737710655496,
57.72548653469));
#113133=CARTESIAN_POINT('Ctrl Pts',(-9.62133689772822,-64.3853566176911,
57.92184339707));
#113134=CARTESIAN_POINT('Ctrl Pts',(-9.65220875720963,-64.2491178829401,
57.997765360834));
#113135=CARTESIAN_POINT('Ctrl Pts',(-9.68344264578583,-64.1137607131964,
58.0752461350595));
#113136=CARTESIAN_POINT('Ctrl Pts',(-9.71501039923335,-63.9792851084599,
58.1542953015588));
#113137=CARTESIAN_POINT('Ctrl Pts',(-9.79705218697199,-63.6297949542694,
58.3597370650858));
#113138=CARTESIAN_POINT('Ctrl Pts',(-9.88157720980486,-63.2854296652719,
58.5763549087011));
#113139=CARTESIAN_POINT('Ctrl Pts',(-9.9675636085802,-62.9479926546559,
58.803052399267));
#113140=CARTESIAN_POINT('Ctrl Pts',(-10.000231858517,-62.8197924188312,
58.8891800937317));
#113141=CARTESIAN_POINT('Ctrl Pts',(-10.0331114014216,-62.6925922234125,
58.9767623509528));
#113142=CARTESIAN_POINT('Ctrl Pts',(-10.0661477385087,-62.5664909655025,
59.0657376624532));
#113143=CARTESIAN_POINT('Ctrl Pts',(-10.1635313447246,-62.194773144266,
59.3280166395464));
#113144=CARTESIAN_POINT('Ctrl Pts',(-10.2616480241468,-61.834854396424,
59.6006923739533));
#113145=CARTESIAN_POINT('Ctrl Pts',(-10.359861054366,-61.4867347219765,
59.8839207289473));
#113146=CARTESIAN_POINT('Ctrl Pts',(-10.4570476923973,-61.1422531321451,
60.1641891572358));
#113147=CARTESIAN_POINT('Ctrl Pts',(-10.554328628233,-60.8093252878649,
60.4547910987241));
#113148=CARTESIAN_POINT('Ctrl Pts',(-10.651037906848,-60.4879511891359,
60.755863623304));
#113149=CARTESIAN_POINT('Ctrl Pts',(-10.6974363335145,-60.3337648197827,
60.9003098610704));
#113150=CARTESIAN_POINT('Ctrl Pts',(-10.7437024522593,-60.1822379077174,
61.047165996827));
#113151=CARTESIAN_POINT('Ctrl Pts',(-10.7897587055637,-60.03337045294,61.1964456875727));
#113152=CARTESIAN_POINT('',(-12.5675365956403,-55.41742345328,72.9888734536679));
#113153=CARTESIAN_POINT('Ctrl Pts',(-10.7897587055637,-60.03337045294,61.1964456875727));
#113154=CARTESIAN_POINT('Ctrl Pts',(-10.8681726256022,-59.7799388857426,
61.4506045670663));
#113155=CARTESIAN_POINT('Ctrl Pts',(-10.9470443126877,-59.5350540422957,
61.7152333401302));
#113156=CARTESIAN_POINT('Ctrl Pts',(-11.0257532129406,-59.2987159225995,
61.9904546807518));
#113157=CARTESIAN_POINT('Ctrl Pts',(-11.1037577007278,-59.0644929324136,
62.2632129029387));
#113158=CARTESIAN_POINT('Ctrl Pts',(-11.1816022535226,-58.8386643711656,
62.5463752456409));
#113159=CARTESIAN_POINT('Ctrl Pts',(-11.2586336092453,-58.6212302388556,
62.8400469307598));
#113160=CARTESIAN_POINT('Ctrl Pts',(-11.2788912403012,-58.5640496220798,
62.9172764250728));
#113161=CARTESIAN_POINT('Ctrl Pts',(-11.2990923684237,-58.5074495469618,
62.9952326336407));
#113162=CARTESIAN_POINT('Ctrl Pts',(-11.3192245472439,-58.4514300135017,
63.0739172637152));
#113163=CARTESIAN_POINT('Ctrl Pts',(-11.3482132341742,-58.3707664781753,
63.18721667993));
#113164=CARTESIAN_POINT('Ctrl Pts',(-11.3770590078463,-58.291306616956,
63.3020263989648));
#113165=CARTESIAN_POINT('Ctrl Pts',(-11.4057238500081,-58.2130504298437,
63.4183511534986));
#113166=CARTESIAN_POINT('Ctrl Pts',(-11.4200562710891,-58.1739223362876,
63.4765135307655));
#113167=CARTESIAN_POINT('Ctrl Pts',(-11.4343434459173,-58.1350951612583,
63.5350546701748));
#113168=CARTESIAN_POINT('Ctrl Pts',(-11.4485805234392,-58.0965689047557,
63.5939751053765));
#113169=CARTESIAN_POINT('Ctrl Pts',(-11.4606645751704,-58.0638688456409,
63.6439851995063));
#113170=CARTESIAN_POINT('Ctrl Pts',(-11.4730195897036,-58.030565972039,
63.6955579201435));
#113171=CARTESIAN_POINT('Ctrl Pts',(-11.4848603682263,-57.9987472505176,
63.7454105156055));
#113172=CARTESIAN_POINT('Ctrl Pts',(-11.4869700498222,-57.9930780817996,
63.7542927950056));
#113173=CARTESIAN_POINT('Ctrl Pts',(-11.4890635377336,-57.9874560272703,
63.7631204381219));
#113174=CARTESIAN_POINT('Ctrl Pts',(-11.4911365584932,-57.9818928908282,
63.7718748379952));
#113175=CARTESIAN_POINT('Ctrl Pts',(-11.5941202890719,-57.7055268477676,
64.2067767818039));
#113176=CARTESIAN_POINT('Ctrl Pts',(-11.6914739517999,-57.4523483267938,
64.6504049530184));
#113177=CARTESIAN_POINT('Ctrl Pts',(-11.7824236107497,-57.222357327907,
65.1026591348182));
#113178=CARTESIAN_POINT('Ctrl Pts',(-11.7883235248732,-57.2074377871601,
65.1319969120616));
#113179=CARTESIAN_POINT('Ctrl Pts',(-11.7941964815689,-57.1926158225392,
65.1613709725395));
#113180=CARTESIAN_POINT('Ctrl Pts',(-11.800042266047,-57.1778914340443,
65.1907812821003));
#113181=CARTESIAN_POINT('Ctrl Pts',(-11.8480227721297,-57.0570379173963,
65.4321725858791));
#113182=CARTESIAN_POINT('Ctrl Pts',(-11.8941729321676,-56.942757763823,
65.6760061878564));
#113183=CARTESIAN_POINT('Ctrl Pts',(-11.9383729336968,-56.8350509733243,
65.9222609685475));
#113184=CARTESIAN_POINT('Ctrl Pts',(-11.9604729344613,-56.7811975780749,
66.0453883588931));
#113185=CARTESIAN_POINT('Ctrl Pts',(-11.9820853781256,-56.7289875235943,
66.1691210470003));
#113186=CARTESIAN_POINT('Ctrl Pts',(-12.0031951051392,-56.6784208098823,
66.2934559380126));
#113187=CARTESIAN_POINT('Ctrl Pts',(-12.013749968646,-56.6531374530263,
66.3556233835188));
#113188=CARTESIAN_POINT('Ctrl Pts',(-12.0241791520395,-56.6282649313624,
66.4179413799305));
#113189=CARTESIAN_POINT('Ctrl Pts',(-12.0344807519969,-56.6038032448907,
66.4804095261199));
#113190=CARTESIAN_POINT('Ctrl Pts',(-12.0442431275156,-56.5806219749766,
66.539607854883));
#113191=CARTESIAN_POINT('Ctrl Pts',(-12.054052629272,-56.5574302295258,
66.5999483902158));
#113192=CARTESIAN_POINT('Ctrl Pts',(-12.0634478796864,-56.5353067077742,
66.6585668852194));
#113193=CARTESIAN_POINT('Ctrl Pts',(-12.0639668259839,-56.534084715896,
66.6618046755502));
#113194=CARTESIAN_POINT('Ctrl Pts',(-12.0644845214739,-56.5328659830625,
66.6650372100122));
#113195=CARTESIAN_POINT('Ctrl Pts',(-12.0650008929406,-56.5316506910522,
66.6682640052103));
#113196=CARTESIAN_POINT('Ctrl Pts',(-12.1397505417374,-56.3557256897672,
67.1353730988268));
#113197=CARTESIAN_POINT('Ctrl Pts',(-12.2072603484355,-56.2006332466164,
67.6103431031051));
#113198=CARTESIAN_POINT('Ctrl Pts',(-12.2667800777353,-56.0663733615999,
68.0929667940404));
#113199=CARTESIAN_POINT('Ctrl Pts',(-12.3253653811598,-55.9342212803662,
68.5680135677053));
#113200=CARTESIAN_POINT('Ctrl Pts',(-12.3762093048664,-55.8222527732994,
69.0504756906023));
#113201=CARTESIAN_POINT('Ctrl Pts',(-12.4185828866349,-55.7304678403994,
69.5401069113127));
#113202=CARTESIAN_POINT('Ctrl Pts',(-12.4605719335821,-55.6395158439964,
70.0252947914776));
#113203=CARTESIAN_POINT('Ctrl Pts',(-12.4942434698488,-55.568382757249,
70.5175223741176));
#113204=CARTESIAN_POINT('Ctrl Pts',(-12.5188778974211,-55.5170685801572,
71.0165001717449));
#113205=CARTESIAN_POINT('Ctrl Pts',(-12.5431986104359,-55.4664078789505,
71.5091235859169));
#113206=CARTESIAN_POINT('Ctrl Pts',(-12.558710704061,-55.435064521754,72.0083264676726));
#113207=CARTESIAN_POINT('Ctrl Pts',(-12.5647147706456,-55.4230385085677,
72.5137798699802));
#113208=CARTESIAN_POINT('Ctrl Pts',(-12.5665887310599,-55.4192850071141,
72.6715395573251));
#113209=CARTESIAN_POINT('Ctrl Pts',(-12.5675364200081,-55.4174133220182,
72.829907766708));
#113210=CARTESIAN_POINT('Ctrl Pts',(-12.5675364833277,-55.41742345328,72.988873453668));
#113211=CARTESIAN_POINT('',(-10.7897587055989,-60.03337045296,84.78133308562));
#113212=CARTESIAN_POINT('Ctrl Pts',(-12.5675367079528,-55.4174234532799,
72.9888734536678));
#113213=CARTESIAN_POINT('Ctrl Pts',(-12.5675367177603,-55.417420362165,
72.9957279350907));
#113214=CARTESIAN_POINT('Ctrl Pts',(-12.5675348841625,-55.4174209999673,
73.0025821589281));
#113215=CARTESIAN_POINT('Ctrl Pts',(-12.5675312063047,-55.4174253640918,
73.0094361248664));
#113216=CARTESIAN_POINT('Ctrl Pts',(-12.5673418846506,-55.4176500120595,
73.3622513396429));
#113217=CARTESIAN_POINT('Ctrl Pts',(-12.5622677006751,-55.4277450225353,
73.7143816352725));
#113218=CARTESIAN_POINT('Ctrl Pts',(-12.5525370191716,-55.4476997595217,
74.0656979046879));
#113219=CARTESIAN_POINT('Ctrl Pts',(-12.5474620952415,-55.458106920851,
74.2489228249614));
#113220=CARTESIAN_POINT('Ctrl Pts',(-12.5411201911119,-55.4711966603877,
74.4319266339354));
#113221=CARTESIAN_POINT('Ctrl Pts',(-12.5335411140059,-55.4869721096635,
74.6146927967335));
#113222=CARTESIAN_POINT('Ctrl Pts',(-12.5334665414252,-55.4871273285572,
74.6164910822281));
#113223=CARTESIAN_POINT('Ctrl Pts',(-12.5333918499194,-55.487282806378,
74.6182893239537));
#113224=CARTESIAN_POINT('Ctrl Pts',(-12.5333170395124,-55.4874385431059,
74.6200875221817));
#113225=CARTESIAN_POINT('Ctrl Pts',(-12.5253096668512,-55.5041079086092,
74.8125586490817));
#113226=CARTESIAN_POINT('Ctrl Pts',(-12.5159419632214,-55.5237395701696,
75.0045311117337));
#113227=CARTESIAN_POINT('Ctrl Pts',(-12.5052315294745,-55.5463351822132,
75.1962408145872));
#113228=CARTESIAN_POINT('Ctrl Pts',(-12.494586011168,-55.5687938433041,
75.3867885738564));
#113229=CARTESIAN_POINT('Ctrl Pts',(-12.4826139191233,-55.5941806072669,
75.5770771250886));
#113230=CARTESIAN_POINT('Ctrl Pts',(-12.4693109997989,-55.6225435272547,
75.7673386019281));
#113231=CARTESIAN_POINT('Ctrl Pts',(-12.4587206876582,-55.6451229452431,
75.9188037336736));
#113232=CARTESIAN_POINT('Ctrl Pts',(-12.4472865327652,-55.6695893960182,
76.0702517860621));
#113233=CARTESIAN_POINT('Ctrl Pts',(-12.4349969289462,-55.6959886852914,
76.2217977195888));
#113234=CARTESIAN_POINT('Ctrl Pts',(-12.4348262620392,-55.6963552947537,
76.2239022525037));
#113235=CARTESIAN_POINT('Ctrl Pts',(-12.4346554300246,-55.69672227728,76.2260068042449));
#113236=CARTESIAN_POINT('Ctrl Pts',(-12.434484432869,-55.6970896329825,
76.2281113751059));
#113237=CARTESIAN_POINT('Ctrl Pts',(-12.4147573136306,-55.73946969318,76.4709055911142));
#113238=CARTESIAN_POINT('Ctrl Pts',(-12.3930365101054,-55.786547159027,
76.7114637571515));
#113239=CARTESIAN_POINT('Ctrl Pts',(-12.3694317519418,-55.8382937182597,
76.9497619795014));
#113240=CARTESIAN_POINT('Ctrl Pts',(-12.3456145013358,-55.8905061053007,
77.1902053867733));
#113241=CARTESIAN_POINT('Ctrl Pts',(-12.3198790437151,-55.9474720577438,
77.4283485364247));
#113242=CARTESIAN_POINT('Ctrl Pts',(-12.292316766459,-56.0092105052791,
77.6641621123292));
#113243=CARTESIAN_POINT('Ctrl Pts',(-12.2871240456124,-56.020842001493,
77.7085892857489));
#113244=CARTESIAN_POINT('Ctrl Pts',(-12.2818664270638,-56.0326430296083,
77.7529337448585));
#113245=CARTESIAN_POINT('Ctrl Pts',(-12.2765444463052,-56.0446139033609,
77.7971952495328));
#113246=CARTESIAN_POINT('Ctrl Pts',(-12.2761514642688,-56.0454978483726,
77.800463577065));
#113247=CARTESIAN_POINT('Ctrl Pts',(-12.2757581312848,-56.046382719501,
77.8037314522769));
#113248=CARTESIAN_POINT('Ctrl Pts',(-12.2753644474211,-56.0472685174681,
77.8069988757635));
#113249=CARTESIAN_POINT('Ctrl Pts',(-12.2443292802359,-56.1170983747168,
78.064578734961));
#113250=CARTESIAN_POINT('Ctrl Pts',(-12.2111136956062,-56.1926615310725,
78.3193507962519));
#113251=CARTESIAN_POINT('Ctrl Pts',(-12.1757902067544,-56.2739580008635,
78.5712755762204));
#113252=CARTESIAN_POINT('Ctrl Pts',(-12.1581284623285,-56.314606235759,
78.6972379662047));
#113253=CARTESIAN_POINT('Ctrl Pts',(-12.139939737709,-56.3566878012973,
78.822488437138));
#113254=CARTESIAN_POINT('Ctrl Pts',(-12.121233009823,-56.4002027038311,
78.9470220844111));
#113255=CARTESIAN_POINT('Ctrl Pts',(-12.1118796458801,-56.421960155098,
79.0092889080477));
#113256=CARTESIAN_POINT('Ctrl Pts',(-12.1023967812936,-56.4440759405827,
79.0713765196295));
#113257=CARTESIAN_POINT('Ctrl Pts',(-12.0927855383251,-56.4665500603618,
79.1332842852319));
#113258=CARTESIAN_POINT('Ctrl Pts',(-12.0879799168409,-56.4777871202513,
79.1642381680331));
#113259=CARTESIAN_POINT('Ctrl Pts',(-12.0831422008006,-56.4891137637026,
79.195147088959));
#113260=CARTESIAN_POINT('Ctrl Pts',(-12.0782725304274,-56.5005299906337,
79.2260109686509));
#113261=CARTESIAN_POINT('Ctrl Pts',(-12.0741631291138,-56.5101638784231,
79.2520562772707));
#113262=CARTESIAN_POINT('Ctrl Pts',(-12.0701688778214,-56.5195377148995,
79.2772053033278));
#113263=CARTESIAN_POINT('Ctrl Pts',(-12.0659408536283,-56.5294710194992,
79.303645963151));
#113264=CARTESIAN_POINT('Ctrl Pts',(-12.0651586384752,-56.5313087529233,
79.3085376770643));
#113265=CARTESIAN_POINT('Ctrl Pts',(-12.0643683768676,-56.5331657640305,
79.3134735586042));
#113266=CARTESIAN_POINT('Ctrl Pts',(-12.0635677966475,-56.5350474217073,
79.3184674037971));
#113267=CARTESIAN_POINT('Ctrl Pts',(-12.0630538197257,-56.5362554563258,
79.3216734799854));
#113268=CARTESIAN_POINT('Ctrl Pts',(-12.0625394985106,-56.5374644904549,
79.3248790600936));
#113269=CARTESIAN_POINT('Ctrl Pts',(-12.0620248331187,-56.5386745245,79.3280841443224));
#113270=CARTESIAN_POINT('Ctrl Pts',(-12.016072548911,-56.646713318681,79.6142524853919));
#113271=CARTESIAN_POINT('Ctrl Pts',(-11.9673790999134,-56.7627198109995,
79.8964680350565));
#113272=CARTESIAN_POINT('Ctrl Pts',(-11.9163040906032,-56.8866775806963,
80.1747259754764));
#113273=CARTESIAN_POINT('Ctrl Pts',(-11.8771617699198,-56.9816750136521,
80.387974326944));
#113274=CARTESIAN_POINT('Ctrl Pts',(-11.8366199972576,-57.08134326507,80.5988982626393));
#113275=CARTESIAN_POINT('Ctrl Pts',(-11.7948293248845,-57.185692108946,
80.8074933067817));
#113276=CARTESIAN_POINT('Ctrl Pts',(-11.7942686561726,-57.1870920656483,
80.8102918431072));
#113277=CARTESIAN_POINT('Ctrl Pts',(-11.7937077625348,-57.1884928650459,
80.8130899602107));
#113278=CARTESIAN_POINT('Ctrl Pts',(-11.7931466444324,-57.1898945067378,
80.8158876575174));
#113279=CARTESIAN_POINT('Ctrl Pts',(-11.7543525232763,-57.2868000554576,
81.0093125493625));
#113280=CARTESIAN_POINT('Ctrl Pts',(-11.7144860247975,-57.3877303365387,
81.2007354330128));
#113281=CARTESIAN_POINT('Ctrl Pts',(-11.6736515325075,-57.4926792079279,
81.3901600236987));
#113282=CARTESIAN_POINT('Ctrl Pts',(-11.6631346852557,-57.5197085938161,
81.4389459733767));
#113283=CARTESIAN_POINT('Ctrl Pts',(-11.6525535566467,-57.5470047844422,
81.4875992960499));
#113284=CARTESIAN_POINT('Ctrl Pts',(-11.6419097870288,-57.5745681821866,
81.5361198751912));
#113285=CARTESIAN_POINT('Ctrl Pts',(-11.6159242509377,-57.6418610391903,
81.65457727381));
#113286=CARTESIAN_POINT('Ctrl Pts',(-11.5895653660279,-57.7107441791077,
81.7722442113706));
#113287=CARTESIAN_POINT('Ctrl Pts',(-11.5628547265227,-57.7812175830128,
81.8891211276125));
#113288=CARTESIAN_POINT('Ctrl Pts',(-11.5476899162457,-57.8212284483305,
81.9554773172582));
#113289=CARTESIAN_POINT('Ctrl Pts',(-11.5325098452768,-57.8614916356994,
82.0211547582754));
#113290=CARTESIAN_POINT('Ctrl Pts',(-11.5171516659124,-57.9024467651775,
82.0868778160803));
#113291=CARTESIAN_POINT('Ctrl Pts',(-11.5064596476346,-57.930958803132,
82.1326327274308));
#113292=CARTESIAN_POINT('Ctrl Pts',(-11.495681091937,-57.9598071357988,
82.1784092861939));
#113293=CARTESIAN_POINT('Ctrl Pts',(-11.4847584588241,-57.989152887941,
82.2244446831469));
#113294=CARTESIAN_POINT('Ctrl Pts',(-11.4837358338566,-57.9919003663668,
82.2287547195481));
#113295=CARTESIAN_POINT('Ctrl Pts',(-11.4827119445408,-57.9946522125546,
82.2330670202093));
#113296=CARTESIAN_POINT('Ctrl Pts',(-11.4816867426733,-57.9974085638931,
82.2373817774385));
#113297=CARTESIAN_POINT('Ctrl Pts',(-11.43560787011,-58.1212959328948,82.4313134847434));
#113298=CARTESIAN_POINT('Ctrl Pts',(-11.3889411870521,-58.2488419536418,
82.6215294594314));
#113299=CARTESIAN_POINT('Ctrl Pts',(-11.341821831652,-58.3799615459125,
82.8080706171353));
#113300=CARTESIAN_POINT('Ctrl Pts',(-11.2938772096503,-58.5133776173983,
82.9978789287711));
#113301=CARTESIAN_POINT('Ctrl Pts',(-11.2454636701495,-58.6504936180069,
83.1838830413866));
#113302=CARTESIAN_POINT('Ctrl Pts',(-11.1967060251446,-58.7912696724882,
83.366114617652));
#113303=CARTESIAN_POINT('Ctrl Pts',(-11.1477507290122,-58.9326163973922,
83.549084914512));
#113304=CARTESIAN_POINT('Ctrl Pts',(-11.0984482456694,-59.0776530869639,
83.7282524820302));
#113305=CARTESIAN_POINT('Ctrl Pts',(-11.0489114885581,-59.2263869642892,
83.9036309719482));
#113306=CARTESIAN_POINT('Ctrl Pts',(-10.9995158026708,-59.3746972759362,
84.0785100174197));
#113307=CARTESIAN_POINT('Ctrl Pts',(-10.9498868892997,-59.5266839524761,
84.2496219606914));
#113308=CARTESIAN_POINT('Ctrl Pts',(-10.9001276898329,-59.6823984332261,
84.416955525759));
#113309=CARTESIAN_POINT('Ctrl Pts',(-10.863396027817,-59.7973450509208,
84.5404792162896));
#113310=CARTESIAN_POINT('Ctrl Pts',(-10.8265931653981,-59.9143239539261,
84.661943505303));
#113311=CARTESIAN_POINT('Ctrl Pts',(-10.7897587056822,-60.03337045296,84.7813330856457));
#113312=CARTESIAN_POINT('',(-9.38953228746991,-65.4601089375,88.61388938658));
#113313=CARTESIAN_POINT('Ctrl Pts',(-10.7897587055989,-60.03337045296,84.78133308562));
#113314=CARTESIAN_POINT('Ctrl Pts',(-10.670470502179,-60.4185374401732,
85.1679756114817));
#113315=CARTESIAN_POINT('Ctrl Pts',(-10.549981394999,-60.8207041658133,
85.5377156681126));
#113316=CARTESIAN_POINT('Ctrl Pts',(-10.3694938731286,-61.449453861914,
86.0673758482434));
#113317=CARTESIAN_POINT('Ctrl Pts',(-10.2793086657354,-61.7702036118744,
86.325969517694));
#113318=CARTESIAN_POINT('Ctrl Pts',(-10.1895683919245,-62.1005157147001,
86.5752922699324));
#113319=CARTESIAN_POINT('Ctrl Pts',(-10.1298782561999,-62.3228487505539,
86.7394569667994));
#113320=CARTESIAN_POINT('Ctrl Pts',(-10.1003989068031,-62.4339433710822,
86.8197126563052));
#113321=CARTESIAN_POINT('Ctrl Pts',(-9.83051728469071,-63.4637761676075,
87.54725601639));
#113322=CARTESIAN_POINT('Ctrl Pts',(-9.60025786520268,-64.4343560676532,
88.1172918608766));
#113323=CARTESIAN_POINT('Ctrl Pts',(-9.38953228746991,-65.4601089375,88.61388938658));
#113324=CARTESIAN_POINT('',(-9.38953228746991,65.4601089375,88.61388938658));
#113325=CARTESIAN_POINT('',(-9.38953228746991,65.4601089375,88.61388938658));
#113326=CARTESIAN_POINT('Ctrl Pts',(-9.38953228746955,65.4601089375,88.6138893865798));
#113327=CARTESIAN_POINT('Ctrl Pts',(-9.4673250436269,65.0800846589239,88.4305623759675));
#113328=CARTESIAN_POINT('Ctrl Pts',(-9.54819413567023,64.706647013074,88.2361905377287));
#113329=CARTESIAN_POINT('Ctrl Pts',(-9.63163220313212,64.3397959999503,
88.0305916995967));
#113330=CARTESIAN_POINT('Ctrl Pts',(-9.715070270594,63.9729449868266,87.8249928614648));
#113331=CARTESIAN_POINT('Ctrl Pts',(-9.80107740201692,63.6126806064291,
87.6081667119018));
#113332=CARTESIAN_POINT('Ctrl Pts',(-9.88908572874933,63.2590028587578,
87.3799269420104));
#113333=CARTESIAN_POINT('Ctrl Pts',(-9.93149413019431,63.088576849512,87.2699454874521));
#113334=CARTESIAN_POINT('Ctrl Pts',(-9.97461011732333,62.9187650612967,
87.1566690415153));
#113335=CARTESIAN_POINT('Ctrl Pts',(-10.0178349665076,62.7515519635204,
87.0414743274715));
#113336=CARTESIAN_POINT('Ctrl Pts',(-10.0344118943353,62.6874249739302,
86.9972966265224));
#113337=CARTESIAN_POINT('Ctrl Pts',(-10.0510053294605,62.6236801887277,
86.9528369978398));
#113338=CARTESIAN_POINT('Ctrl Pts',(-10.0675834133922,62.5604295403834,
86.9081738596842));
#113339=CARTESIAN_POINT('Ctrl Pts',(-10.1642608210937,62.1915745663972,
86.647714542764));
#113340=CARTESIAN_POINT('Ctrl Pts',(-10.2617150056454,61.8342111001938,
86.3768550872122));
#113341=CARTESIAN_POINT('Ctrl Pts',(-10.3593126521196,61.4883391417732,
86.0954394287602));
#113342=CARTESIAN_POINT('Ctrl Pts',(-10.455900523795,61.1460456793497,85.8169353819112));
#113343=CARTESIAN_POINT('Ctrl Pts',(-10.5526288561325,60.8150071655915,
85.5280921336091));
#113344=CARTESIAN_POINT('Ctrl Pts',(-10.6488346943094,60.4952236004985,
85.2287720071987));
#113345=CARTESIAN_POINT('Ctrl Pts',(-10.6959629091748,60.3385716877694,
85.0821444895936));
#113346=CARTESIAN_POINT('Ctrl Pts',(-10.742964994564,60.1846206385832,84.9330030588417));
#113347=CARTESIAN_POINT('Ctrl Pts',(-10.7897587055637,60.03337045294,84.7813330855873));
#113348=CARTESIAN_POINT('Origin',(24.4068933420691,-10.33199109902,60.67496896178));
#113349=CARTESIAN_POINT('',(25.579982351165,-11.2436243723453,60.4681262431048));
#113350=CARTESIAN_POINT('',(25.4229139949212,-10.8757227763334,59.7147318914574));
#113351=CARTESIAN_POINT('Origin',(24.4069013928191,-10.33197941375,60.67497222926));
#113352=CARTESIAN_POINT('',(23.4739859593054,-11.4524032074963,60.3223210887327));
#113353=CARTESIAN_POINT('Origin',(24.4068933420691,-10.33199109902,60.67496896178));
#113354=CARTESIAN_POINT('',(24.9372779666099,-10.3319811032157,59.2718682957262));
#113355=CARTESIAN_POINT('Origin',(24.4069013928191,-10.33197941375,60.67497222926));
#113356=CARTESIAN_POINT('',(22.9296817484535,-10.3319903259816,60.9354414318888));
#113357=CARTESIAN_POINT('Origin',(24.4068932609991,-10.33199110019,60.67496850203));
#113358=CARTESIAN_POINT('Origin',(24.4068933430391,-10.33198915989,60.67496896729));
#113359=CARTESIAN_POINT('Origin',(71.6139524734691,1.4210854715202E-14,
50.72762564822));
#113360=CARTESIAN_POINT('Origin',(72.5315042041368,1.25011112572802E-13,
55.931320096872));
#113361=CARTESIAN_POINT('',(82.4056897430765,1.53742691743921E-14,57.2222894375664));
#113362=CARTESIAN_POINT('',(80.9696261270861,1.53742691743921E-14,49.0779679603843));
#113363=CARTESIAN_POINT('',(81.8983892080091,3.04138126515101,57.22463037752));
#113364=CARTESIAN_POINT('Ctrl Pts',(82.4056897430765,1.31838984174237E-14,
57.2222894375664));
#113365=CARTESIAN_POINT('Ctrl Pts',(82.4056897430765,0.630938140511888,
57.2222894375664));
#113366=CARTESIAN_POINT('Ctrl Pts',(82.3346727961054,1.31739466653436,57.2050618631517));
#113367=CARTESIAN_POINT('Ctrl Pts',(82.1105250320151,2.34612040996873,57.2005733737953));
#113368=CARTESIAN_POINT('Ctrl Pts',(82.0116225514947,2.70113410021125,57.2046642839492));
#113369=CARTESIAN_POINT('Ctrl Pts',(81.8983892080076,3.04138126515041,57.2246303775219));
#113370=CARTESIAN_POINT('',(81.8983892080091,-3.04138126515099,57.22463037752));
#113371=CARTESIAN_POINT('Origin',(73.0351194308991,1.4210854715202E-14,
58.78746397652));
#113372=CARTESIAN_POINT('Ctrl Pts',(81.8983892080076,-3.04138126515039,
57.2246303775219));
#113373=CARTESIAN_POINT('Ctrl Pts',(82.0116225514947,-2.70113410021123,
57.2046642839493));
#113374=CARTESIAN_POINT('Ctrl Pts',(82.1105250320151,-2.34612040996872,
57.2005733737953));
#113375=CARTESIAN_POINT('Ctrl Pts',(82.3346727961054,-1.31739466653435,
57.2050618631517));
#113376=CARTESIAN_POINT('Ctrl Pts',(82.4056897430765,-0.630938140511861,
57.2222894375664));
#113377=CARTESIAN_POINT('Ctrl Pts',(82.4056897430765,1.36696209906972E-14,
57.2222894375664));
#113378=CARTESIAN_POINT('Origin',(74.1638325857391,1.4210854715202E-14,
65.188714371101));
#113379=CARTESIAN_POINT('',(82.1915345300951,-0.411812550483981,63.2655006193781));
#113380=CARTESIAN_POINT('Origin',(74.0770084969191,1.4210854715202E-14,
64.696310494688));
#113381=CARTESIAN_POINT('',(81.7865781657935,-0.386854671015844,63.8446186582614));
#113382=CARTESIAN_POINT('Origin',(82.2783682032164,-0.411813036887835,63.7579028058202));
#113383=CARTESIAN_POINT('',(81.7960926715764,1.51599559845412E-14,63.8429409941838));
#113384=CARTESIAN_POINT('Origin',(74.1638325857391,1.4210854715202E-14,
65.188714371101));
#113385=CARTESIAN_POINT('Origin',(74.1638325857391,1.4210854715202E-14,
65.188714371101));
#113386=CARTESIAN_POINT('Origin',(71.6139524734691,1.4210854715202E-14,
50.72762564822));
#113387=CARTESIAN_POINT('',(82.0565649380767,1.51599559845412E-14,65.3201526237018));
#113388=CARTESIAN_POINT('',(79.2462125593138,1.51599559845412E-14,49.3818522713015));
#113389=CARTESIAN_POINT('Origin',(74.4243048522391,1.4210854715202E-14,
66.665926000619));
#113390=CARTESIAN_POINT('Origin',(71.6139524734691,1.4210854715202E-14,
50.72762564822));
#113391=CARTESIAN_POINT('',(80.8255552468114,1.50068751346478E-14,65.5372128457854));
#113392=CARTESIAN_POINT('Origin',(74.4243048522391,1.4210854715202E-14,
66.665926000619));
#113393=CARTESIAN_POINT('',(81.0860275133185,1.50068751346486E-14,67.0144244753021));
#113394=CARTESIAN_POINT('',(78.0152028680485,1.50068751346478E-14,49.5989124933851));
#113395=CARTESIAN_POINT('',(69.2683344771676,3.46410161513628,69.0982026073056));
#113396=CARTESIAN_POINT('Origin',(74.6847771187391,1.4210854715202E-14,
68.143137630137));
#113397=CARTESIAN_POINT('',(69.268334477169,-3.46410161513855,69.0982026073053));
#113398=CARTESIAN_POINT('Ctrl Pts',(69.2683344771665,-3.4641016151401,69.0982026073051));
#113399=CARTESIAN_POINT('Ctrl Pts',(68.9648321493424,-2.97479325737662,
69.1517182564088));
#113400=CARTESIAN_POINT('Ctrl Pts',(68.7289781639998,-2.41648059182673,
69.2912781361514));
#113401=CARTESIAN_POINT('Ctrl Pts',(68.4194117007815,-1.22911622864477,
69.5454817189857));
#113402=CARTESIAN_POINT('Ctrl Pts',(68.3498544259377,-0.596312598658473,
69.6480138742419));
#113403=CARTESIAN_POINT('Ctrl Pts',(68.3498544259377,0.5963125986585,69.6480138742419));
#113404=CARTESIAN_POINT('Ctrl Pts',(68.4194117007815,1.2291162286448,69.5454817189857));
#113405=CARTESIAN_POINT('Ctrl Pts',(68.7289781639996,2.41648059182585,69.2912781361516));
#113406=CARTESIAN_POINT('Ctrl Pts',(68.9648321493417,2.97479325737492,69.1517182564092));
#113407=CARTESIAN_POINT('Ctrl Pts',(69.2683344771651,3.46410161513784,69.0982026073054));
#113408=CARTESIAN_POINT('Origin',(74.6847771187391,1.4210854715202E-14,
68.143137630137));
#113409=CARTESIAN_POINT('Origin',(113.044794833869,1.4210854715202E-14,
71.158082873799));
#113410=CARTESIAN_POINT('',(118.579168886261,-8.01332830629138,69.4281578533551));
#113411=CARTESIAN_POINT('',(118.579167675758,8.01332909152356,69.4281576180553));
#113412=CARTESIAN_POINT('Origin',(113.570314823169,1.4210854715202E-14,
68.454530393505));
#113413=CARTESIAN_POINT('',(113.836120912569,9.49997724965368,66.9781228011004));
#113414=CARTESIAN_POINT('Ctrl Pts',(113.836120912568,9.49997724965366,66.9781228011068));
#113415=CARTESIAN_POINT('Ctrl Pts',(114.686038635719,9.50187211507081,67.1433308953068));
#113416=CARTESIAN_POINT('Ctrl Pts',(115.610633133812,9.38050971532904,67.4594549710188));
#113417=CARTESIAN_POINT('Ctrl Pts',(117.387516977032,8.79824955495792,68.2752003940439));
#113418=CARTESIAN_POINT('Ctrl Pts',(118.027127690967,8.42218281811796,68.6679459525273));
#113419=CARTESIAN_POINT('Ctrl Pts',(118.418563176045,8.156345641126,69.0448344935117));
#113420=CARTESIAN_POINT('Ctrl Pts',(118.489716706812,8.10440527523949,69.1261923172504));
#113421=CARTESIAN_POINT('Ctrl Pts',(118.553353478955,8.05159245557175,69.2438470494525));
#113422=CARTESIAN_POINT('Ctrl Pts',(118.56938447916,8.03708381445878,69.2821462693244));
#113423=CARTESIAN_POINT('Ctrl Pts',(118.581302967088,8.02269597530884,69.3399573591882));
#113424=CARTESIAN_POINT('Ctrl Pts',(118.583467017461,8.01916164376496,69.3579848864792));
#113425=CARTESIAN_POINT('Ctrl Pts',(118.583973829246,8.01451405680058,69.3936861214022));
#113426=CARTESIAN_POINT('Ctrl Pts',(118.582509524538,8.01332909160475,69.4109653817901));
#113427=CARTESIAN_POINT('Ctrl Pts',(118.579167675665,8.01332909160488,69.4281576180372));
#113428=CARTESIAN_POINT('',(104.531073144128,1.53742691743937E-14,65.1693957133202));
#113429=CARTESIAN_POINT('Origin',(113.856529692569,1.4210854715202E-14,
66.982089885856));
#113430=CARTESIAN_POINT('',(105.008097926387,1.5374269174392E-14,62.7153282005846));
#113431=CARTESIAN_POINT('',(103.719338285428,1.5374269174392E-14,69.3453887012632));
#113432=CARTESIAN_POINT('Origin',(114.333554474769,1.4210854715202E-14,
64.528022373109));
#113433=CARTESIAN_POINT('',(113.83612107687,-9.49997725001998,66.9781228330329));
#113434=CARTESIAN_POINT('Origin',(113.856529692569,1.4210854715202E-14,
66.982089885856));
#113435=CARTESIAN_POINT('Ctrl Pts',(118.579168886168,-8.01332830637214,
69.428157853337));
#113436=CARTESIAN_POINT('Ctrl Pts',(118.583697953965,-8.01332830637242,
69.4048579356841));
#113437=CARTESIAN_POINT('Ctrl Pts',(118.584755128007,-8.01550606099109,
69.3815157842115));
#113438=CARTESIAN_POINT('Ctrl Pts',(118.58079181303,-8.02388189771212,69.3327838467339));
#113439=CARTESIAN_POINT('Ctrl Pts',(118.575268672964,-8.03030115604168,
69.3081184208139));
#113440=CARTESIAN_POINT('Ctrl Pts',(118.550114989685,-8.05509816333799,
69.2312409077683));
#113441=CARTESIAN_POINT('Ctrl Pts',(118.519917693981,-8.07983477899803,
69.1790179082443));
#113442=CARTESIAN_POINT('Ctrl Pts',(118.365671255634,-8.19683130407594,
68.9686926024889));
#113443=CARTESIAN_POINT('Ctrl Pts',(118.148405235818,-8.34221746197395,
68.7907241087155));
#113444=CARTESIAN_POINT('Ctrl Pts',(117.411981582031,-8.75017745982984,
68.3043581295628));
#113445=CARTESIAN_POINT('Ctrl Pts',(116.685780703193,-9.08337727457682,
67.9164630081501));
#113446=CARTESIAN_POINT('Ctrl Pts',(115.095330683893,-9.4415653031523,67.2939793018252));
#113447=CARTESIAN_POINT('Ctrl Pts',(114.445102020103,-9.50133494336816,
67.0964973277519));
#113448=CARTESIAN_POINT('Ctrl Pts',(113.83612107687,-9.49997725001994,66.9781228330337));
#113449=CARTESIAN_POINT('Origin',(113.044794833869,1.4210854715202E-14,
71.158082873799));
#113450=CARTESIAN_POINT('',(101.08158990599,1.58641278940509E-14,61.9520885489905));
#113451=CARTESIAN_POINT('Origin',(114.333554474769,1.4210854715202E-14,
64.528022373109));
#113452=CARTESIAN_POINT('',(102.016642645058,1.58641278940509E-14,57.1416832303295));
#113453=CARTESIAN_POINT('',(99.7928302650323,1.58641278940509E-14,68.5821490496692));
#113454=CARTESIAN_POINT('',(115.268607213821,13.5000000002585,59.71761705473));
#113455=CARTESIAN_POINT('Origin',(115.268607213895,1.4210854715202E-14,
59.7176170544594));
#113456=CARTESIAN_POINT('Origin',(115.268607213895,1.4210854715202E-14,
59.7176170544594));
#113457=CARTESIAN_POINT('Origin',(115.325809116069,6.8389738316912E-14,
59.42334024732));
#113458=CARTESIAN_POINT('',(115.383008995803,14.0995393124789,59.1290738447923));
#113459=CARTESIAN_POINT('',(115.325809116069,13.7997749560101,59.42334024732));
#113460=CARTESIAN_POINT('Origin',(115.383008995752,2.51354492775102E-13,
59.1290738450566));
#113461=CARTESIAN_POINT('Origin',(113.044794833869,1.4210854715202E-14,
71.158082873799));
#113462=CARTESIAN_POINT('',(101.149417421836,1.59865925739657E-14,56.3623301080323));
#113463=CARTESIAN_POINT('Origin',(115.383008995769,1.4210854715202E-14,
59.12907384506));
#113464=CARTESIAN_POINT('',(102.198871764054,1.59865925739657E-14,50.9633824994358));
#113465=CARTESIAN_POINT('',(98.8112032599333,1.59865925739657E-14,68.3913391367707));
#113466=CARTESIAN_POINT('Origin',(116.432463337969,1.4210854715202E-14,
53.73012623646));
#113467=CARTESIAN_POINT('Origin',(71.6139524734691,1.4210854715202E-14,
50.72762564822));
#113468=CARTESIAN_POINT('',(84.0425654467451,1.50987236445838E-14,79.4627064438384));
#113469=CARTESIAN_POINT('Origin',(76.9027092374091,1.4210854715202E-14,
80.721655731923));
#113470=CARTESIAN_POINT('',(84.4766854941234,2.43409355081298E-8,81.924725896327));
#113471=CARTESIAN_POINT('',(78.7538086828077,1.50987236445838E-14,49.4686763601349));
#113472=CARTESIAN_POINT('',(84.4100541385791,0.934521241357814,81.895304371373));
#113473=CARTESIAN_POINT('Origin',(76.7759739330123,0.0982566280424606,78.5297174321831));
#113474=CARTESIAN_POINT('',(70.2495245506391,0.934521077365814,84.39218780804));
#113475=CARTESIAN_POINT('Ctrl Pts',(70.2495245506391,0.934521077365814,
84.39218780804));
#113476=CARTESIAN_POINT('Ctrl Pts',(70.2969934017684,1.35358127369409,84.3467359130793));
#113477=CARTESIAN_POINT('Ctrl Pts',(70.4869050838629,2.32787641859955,84.1880974727865));
#113478=CARTESIAN_POINT('Ctrl Pts',(71.0685341933312,3.76636998723846,83.7654733575445));
#113479=CARTESIAN_POINT('Ctrl Pts',(72.0301843466196,5.12897761292657,83.1528274066478));
#113480=CARTESIAN_POINT('Ctrl Pts',(73.2668101124888,6.19715034366626,82.4884313637663));
#113481=CARTESIAN_POINT('Ctrl Pts',(74.6880725700381,6.91163507431541,81.8874154360421));
#113482=CARTESIAN_POINT('Ctrl Pts',(76.21258020475,7.26357978151313,81.4299948820006));
#113483=CARTESIAN_POINT('Ctrl Pts',(77.7886661372182,7.26412555002382,81.1517875118529));
#113484=CARTESIAN_POINT('Ctrl Pts',(79.3787551980435,6.91301445740564,81.0596077375714));
#113485=CARTESIAN_POINT('Ctrl Pts',(80.9222078782584,6.19827430998822,81.1380989555079));
#113486=CARTESIAN_POINT('Ctrl Pts',(82.3132368783365,5.12885137030863,81.3397449855469));
#113487=CARTESIAN_POINT('Ctrl Pts',(83.4269049429719,3.7650811278669,81.5867141627659));
#113488=CARTESIAN_POINT('Ctrl Pts',(84.1174814320447,2.3269000879036,81.7848112655805));
#113489=CARTESIAN_POINT('Ctrl Pts',(84.3499684922177,1.35312292207528,81.868858277333));
#113490=CARTESIAN_POINT('Ctrl Pts',(84.4100541385791,0.934521241357814,
81.895304371373));
#113491=CARTESIAN_POINT('',(70.1969737837932,-2.46875951473559E-8,84.4426243475923));
#113492=CARTESIAN_POINT('Origin',(77.2332453430234,0.0370024116887719,77.698216590392));
#113493=CARTESIAN_POINT('',(70.2495210701591,-0.934521544955186,84.39218841976));
#113494=CARTESIAN_POINT('Origin',(76.207146622872,-0.102456625673098,78.6809209731816));
#113495=CARTESIAN_POINT('',(84.4100566843091,-0.934521571518686,81.895303921756));
#113496=CARTESIAN_POINT('Ctrl Pts',(84.4100566843091,-0.934521571518686,
81.895303921756));
#113497=CARTESIAN_POINT('Ctrl Pts',(84.3485694403728,-1.36293966038387,
81.868236180679));
#113498=CARTESIAN_POINT('Ctrl Pts',(84.1118115437881,-2.3450231478546,81.7828932767119));
#113499=CARTESIAN_POINT('Ctrl Pts',(83.4124450771603,-3.78704013149007,
81.5830498021844));
#113500=CARTESIAN_POINT('Ctrl Pts',(82.2982972025616,-5.14249136537986,
81.3370657981871));
#113501=CARTESIAN_POINT('Ctrl Pts',(80.9114749651663,-6.20390890762343,
81.1372668611484));
#113502=CARTESIAN_POINT('Ctrl Pts',(79.3752681809786,-6.91362667787633,
81.0598653963965));
#113503=CARTESIAN_POINT('Ctrl Pts',(77.7914654251769,-7.26346845250041,
81.1516464342562));
#113504=CARTESIAN_POINT('Ctrl Pts',(76.2200481462661,-7.26409591671058,
81.4283837861607));
#113505=CARTESIAN_POINT('Ctrl Pts',(74.698991450041,-6.91521469606571,81.8835971817274));
#113506=CARTESIAN_POINT('Ctrl Pts',(73.2794043860132,-6.2052646895131,82.4824234380684));
#113507=CARTESIAN_POINT('Ctrl Pts',(72.0428187684898,-5.14252677561984,
83.1454232256136));
#113508=CARTESIAN_POINT('Ctrl Pts',(71.0795152379404,-3.78584032635307,
83.758011848655));
#113509=CARTESIAN_POINT('Ctrl Pts',(70.4910989582979,-2.34409180177857,
84.1847388290923));
#113510=CARTESIAN_POINT('Ctrl Pts',(70.2979924693142,-1.36249704964592,
84.3457715729416));
#113511=CARTESIAN_POINT('Ctrl Pts',(70.2495210701591,-0.934521544955186,
84.39218841976));
#113512=CARTESIAN_POINT('Origin',(76.0757054979363,-0.0613886712863647,
78.2217740086092));
#113513=CARTESIAN_POINT('Origin',(76.8158851485791,1.4210854715202E-14,
80.229251855417));
#113514=CARTESIAN_POINT('',(83.2171355431526,1.50068751346478E-14,79.1005387005832));
#113515=CARTESIAN_POINT('',(83.2046721647582,-0.405417357723799,79.1027363304649));
#113516=CARTESIAN_POINT('Origin',(76.8158851485791,1.4210854715202E-14,
80.229251855417));
#113517=CARTESIAN_POINT('Origin',(76.8158851485791,1.4210854715202E-14,
80.229251855417));
#113518=CARTESIAN_POINT('',(83.7829335152822,-0.436602807422093,79.508486558344));
#113519=CARTESIAN_POINT('Origin',(83.6961173198489,-0.436603308317939,79.016081290084));
#113520=CARTESIAN_POINT('Origin',(76.9027092373991,1.4210854715202E-14,
80.72165573186));
#113521=CARTESIAN_POINT('Origin',(71.6139524734691,1.4210854715202E-14,
50.72762564822));
#113522=CARTESIAN_POINT('',(83.0434873654856,1.50068751346478E-14,78.1157309475707));
#113523=CARTESIAN_POINT('Origin',(76.6422369709091,1.4210854715202E-14,
79.244444102405));
#113524=CARTESIAN_POINT('',(78.0152028680485,1.50068751346478E-14,49.5989124933851));
#113525=CARTESIAN_POINT('Origin',(76.5901687245791,3.1641356201812E-14,
78.949150403589));
#113526=CARTESIAN_POINT('',(76.5380973908943,5.50000000026545,78.6538391955389));
#113527=CARTESIAN_POINT('',(81.9545400325016,1.4884410454733E-14,77.6987742186408));
#113528=CARTESIAN_POINT('Origin',(76.5380973909344,1.4210854715202E-14,
78.6538391958088));
#113529=CARTESIAN_POINT('',(76.6422369709602,6.09968496682694,79.2444441026693));
#113530=CARTESIAN_POINT('',(76.5901687245791,5.79985137262403,78.949150403589));
#113531=CARTESIAN_POINT('Origin',(76.6422369709134,3.1641356201812E-14,
79.2444441024043));
#113532=CARTESIAN_POINT('Origin',(76.5380973909344,1.4210854715202E-14,
78.6538391958088));
#113533=CARTESIAN_POINT('Origin',(71.6139524734691,1.4210854715202E-14,
50.72762564822));
#113534=CARTESIAN_POINT('',(70.6108044793244,-6.69216074262907E-7,76.7117291756247));
#113535=CARTESIAN_POINT('',(81.443689908106,1.4884410454733E-14,74.8015991956061));
#113536=CARTESIAN_POINT('Origin',(76.0272472665391,1.4210854715202E-14,
75.756664172774));
#113537=CARTESIAN_POINT('Origin',(76.0272472665391,1.4210854715202E-14,
75.756664172774));
#113538=CARTESIAN_POINT('',(77.0303951150363,1.4884410454733E-14,49.772560671052));
#113539=CARTESIAN_POINT('Origin',(77.1089102519491,1.4210854715202E-14,
81.89107979688));
#113540=CARTESIAN_POINT('',(85.978205710623,0.538566788587397,77.5711572248142));
#113541=CARTESIAN_POINT('',(85.9781969325309,-0.538566277248559,77.5711587732182));
#113542=CARTESIAN_POINT('Origin',(76.9466693241,0.0139589647788434,66.7387412315728));
#113543=CARTESIAN_POINT('',(83.8031819186193,-5.65795202609479,75.9086537965711));
#113544=CARTESIAN_POINT('Ctrl Pts',(85.978196932531,-0.538566277248559,
77.5711587732182));
#113545=CARTESIAN_POINT('Ctrl Pts',(85.9662144643982,-0.701937597578064,
77.5567675886209));
#113546=CARTESIAN_POINT('Ctrl Pts',(85.9493237206406,-0.865436116456894,
77.5389549030835));
#113547=CARTESIAN_POINT('Ctrl Pts',(85.9275097219851,-1.02884991082947,
77.5177470062622));
#113548=CARTESIAN_POINT('Ctrl Pts',(85.9061196526422,-1.18908795101694,
77.4969512598799));
#113549=CARTESIAN_POINT('Ctrl Pts',(85.8799956734439,-1.34924507627592,
77.4728908186415));
#113550=CARTESIAN_POINT('Ctrl Pts',(85.8490864021384,-1.50909866089878,
77.4455664203364));
#113551=CARTESIAN_POINT('Ctrl Pts',(85.8368899917902,-1.57217487820617,
77.4347845558611));
#113552=CARTESIAN_POINT('Ctrl Pts',(85.8239481131521,-1.63520353641687,
77.4234942417378));
#113553=CARTESIAN_POINT('Ctrl Pts',(85.8102560443249,-1.69816965667799,
77.411694547642));
#113554=CARTESIAN_POINT('Ctrl Pts',(85.8027877437963,-1.73251435032291,
77.4052584376016));
#113555=CARTESIAN_POINT('Ctrl Pts',(85.7950962355473,-1.76684042190365,
77.3986707699566));
#113556=CARTESIAN_POINT('Ctrl Pts',(85.7871816196228,-1.80114691080217,
77.391932216887));
#113557=CARTESIAN_POINT('Ctrl Pts',(85.7463561667131,-1.97810786006311,
77.357173173157));
#113558=CARTESIAN_POINT('Ctrl Pts',(85.6995993200506,-2.15452400245472,
77.3183956868117));
#113559=CARTESIAN_POINT('Ctrl Pts',(85.6469330932711,-2.33010254807959,
77.2755957751522));
#113560=CARTESIAN_POINT('Ctrl Pts',(85.6372258054953,-2.36246468172528,
77.2677070182644));
#113561=CARTESIAN_POINT('Ctrl Pts',(85.6273177557924,-2.39479821740101,
77.2596816108375));
#113562=CARTESIAN_POINT('Ctrl Pts',(85.6172090817812,-2.42710112678368,
77.2515195341207));
#113563=CARTESIAN_POINT('Ctrl Pts',(85.5847327845844,-2.53088119569059,
77.225297100901));
#113564=CARTESIAN_POINT('Ctrl Pts',(85.5501853982468,-2.63434715539312,
77.1976640345017));
#113565=CARTESIAN_POINT('Ctrl Pts',(85.5135688065919,-2.73743563372485,
77.1686200026685));
#113566=CARTESIAN_POINT('Ctrl Pts',(85.4952605107644,-2.78897987289072,
77.1540979867519));
#113567=CARTESIAN_POINT('Ctrl Pts',(85.4764348763288,-2.84042973404583,
77.1392232360841));
#113568=CARTESIAN_POINT('Ctrl Pts',(85.4570919373216,-2.89177709254335,
77.123995744836));
#113569=CARTESIAN_POINT('Ctrl Pts',(85.4474204678179,-2.91745077179212,
77.1163819992119));
#113570=CARTESIAN_POINT('Ctrl Pts',(85.4376196696253,-2.94309882414378,
77.1086800688932));
#113571=CARTESIAN_POINT('Ctrl Pts',(85.4276895322232,-2.96872022216433,
77.1008899557592));
#113572=CARTESIAN_POINT('Ctrl Pts',(85.4210724538229,-2.98579337962055,
77.0956989108353));
#113573=CARTESIAN_POINT('Ctrl Pts',(85.4147180597581,-3.00203887736141,
77.0907195487122));
#113574=CARTESIAN_POINT('Ctrl Pts',(85.407988054798,-3.01908814644679,77.085451494958));
#113575=CARTESIAN_POINT('Ctrl Pts',(85.4046184553818,-3.02762442650873,
77.0828138697319));
#113576=CARTESIAN_POINT('Ctrl Pts',(85.4011541048568,-3.03636190537531,
77.0801034885673));
#113577=CARTESIAN_POINT('Ctrl Pts',(85.3975110815366,-3.04550341715496,
77.0772550716083));
#113578=CARTESIAN_POINT('Ctrl Pts',(85.3695874993951,-3.11557262413956,
77.0554221054331));
#113579=CARTESIAN_POINT('Ctrl Pts',(85.3405734858181,-3.18574621766199,
77.0328615317925));
#113580=CARTESIAN_POINT('Ctrl Pts',(85.3104477713276,-3.25598520087038,
77.0095630573215));
#113581=CARTESIAN_POINT('Ctrl Pts',(85.2480342703271,-3.40150410134786,
76.9612940159294));
#113582=CARTESIAN_POINT('Ctrl Pts',(85.1808476668105,-3.54730551159,76.9098558683555));
#113583=CARTESIAN_POINT('Ctrl Pts',(85.108723733047,-3.69312705963221,76.8552039801537));
#113584=CARTESIAN_POINT('Ctrl Pts',(85.0382641434063,-3.83558360491052,
76.8018132481892));
#113585=CARTESIAN_POINT('Ctrl Pts',(84.9630922540674,-3.97805940335467,
76.7453552101207));
#113586=CARTESIAN_POINT('Ctrl Pts',(84.8830768863397,-4.12027618953755,
76.6858154420667));
#113587=CARTESIAN_POINT('Ctrl Pts',(84.805813877074,-4.25760102076219,76.6283237153962));
#113588=CARTESIAN_POINT('Ctrl Pts',(84.7240347343763,-4.3946843146335,76.5679585237037));
#113589=CARTESIAN_POINT('Ctrl Pts',(84.6376444659376,-4.53124394110661,
76.5047344232751));
#113590=CARTESIAN_POINT('Ctrl Pts',(84.5694971390091,-4.63896641585609,
76.4548612891879));
#113591=CARTESIAN_POINT('Ctrl Pts',(84.498480915318,-4.74636245394866,76.4032096693207));
#113592=CARTESIAN_POINT('Ctrl Pts',(84.42456079498,-4.85327902986735,76.3498001953486));
#113593=CARTESIAN_POINT('Ctrl Pts',(84.3281244473085,-4.99276262432044,
76.2801220809546));
#113594=CARTESIAN_POINT('Ctrl Pts',(84.226745450638,-5.13142992615831,76.2074506944152));
#113595=CARTESIAN_POINT('Ctrl Pts',(84.1202967047771,-5.26902674736115,
76.1318569723351));
#113596=CARTESIAN_POINT('Ctrl Pts',(84.0191960638591,-5.39971054921692,
76.0600611640343));
#113597=CARTESIAN_POINT('Ctrl Pts',(83.9135222658985,-5.52942861474292,
75.9856293087662));
#113598=CARTESIAN_POINT('Ctrl Pts',(83.8031865951727,-5.6579465788927,75.9086570590228));
#113599=CARTESIAN_POINT('',(83.8031578769549,5.65797623157721,75.9086520659686));
#113600=CARTESIAN_POINT('Origin',(76.2877195330491,1.4210854715202E-14,
77.233875802293));
#113601=CARTESIAN_POINT('Ctrl Pts',(83.8031631996716,5.65797003185228,75.9086557791601));
#113602=CARTESIAN_POINT('Ctrl Pts',(83.9146383767883,5.52812731488565,75.9864222198002));
#113603=CARTESIAN_POINT('Ctrl Pts',(84.0213782518127,5.39701190664906,76.0615222181351));
#113604=CARTESIAN_POINT('Ctrl Pts',(84.1234507304318,5.26489792169313,76.1339017634367));
#113605=CARTESIAN_POINT('Ctrl Pts',(84.2274634112329,5.13027270309868,76.2076571051687));
#113606=CARTESIAN_POINT('Ctrl Pts',(84.3266296801952,4.994610790924,76.2785877161089));
#113607=CARTESIAN_POINT('Ctrl Pts',(84.4210534082592,4.85818561965194,76.3466763826821));
#113608=CARTESIAN_POINT('Ctrl Pts',(84.4310223939351,4.8437822423851,76.3538649882972));
#113609=CARTESIAN_POINT('Ctrl Pts',(84.4409385446514,4.82937034077388,76.3610219510471));
#113610=CARTESIAN_POINT('Ctrl Pts',(84.4508020021065,4.81495022461278,76.3681472750928));
#113611=CARTESIAN_POINT('Ctrl Pts',(84.5395416903718,4.68521512728899,76.4322524874367));
#113612=CARTESIAN_POINT('Ctrl Pts',(84.6240136534749,4.55481766585984,76.4937943659752));
#113613=CARTESIAN_POINT('Ctrl Pts',(84.7042816981499,4.42405601459424,76.5527860260094));
#113614=CARTESIAN_POINT('Ctrl Pts',(84.7164642319641,4.40420990716007,76.5617393759512));
#113615=CARTESIAN_POINT('Ctrl Pts',(84.7285499856946,4.38435535298269,76.5706340353276));
#113616=CARTESIAN_POINT('Ctrl Pts',(84.7405392429994,4.36449333269502,76.5794701069808));
#113617=CARTESIAN_POINT('Ctrl Pts',(84.8272353310484,4.22086813424354,76.6433650444714));
#113618=CARTESIAN_POINT('Ctrl Pts',(84.9089044311266,4.07680745468572,76.7041670189899));
#113619=CARTESIAN_POINT('Ctrl Pts',(84.9856720925189,3.93260490356097,76.7618449210903));
#113620=CARTESIAN_POINT('Ctrl Pts',(85.0260284014314,3.8567984690074,76.7921658556136));
#113621=CARTESIAN_POINT('Ctrl Pts',(85.0650305614148,3.7809521898354,76.8216239761702));
#113622=CARTESIAN_POINT('Ctrl Pts',(85.1026991261737,3.70510470472398,76.8502180733543));
#113623=CARTESIAN_POINT('Ctrl Pts',(85.1573608628283,3.59504064245878,76.8917116375544));
#113624=CARTESIAN_POINT('Ctrl Pts',(85.2092130179194,3.48497576389758,76.9313826789799));
#113625=CARTESIAN_POINT('Ctrl Pts',(85.2583185901418,3.37502563477719,76.9692200894284));
#113626=CARTESIAN_POINT('Ctrl Pts',(85.2814644688194,3.32320071483382,76.987054727578));
#113627=CARTESIAN_POINT('Ctrl Pts',(85.3040001456757,3.27140131321668,77.0044819961335));
#113628=CARTESIAN_POINT('Ctrl Pts',(85.3259325406226,3.21963888336876,77.0215006470104));
#113629=CARTESIAN_POINT('Ctrl Pts',(85.3272656872237,3.21649253717243,77.0225351148205));
#113630=CARTESIAN_POINT('Ctrl Pts',(85.3285966049385,3.21334632746294,77.0235680730266));
#113631=CARTESIAN_POINT('Ctrl Pts',(85.3299252954779,3.21020025792908,77.0245995217025));
#113632=CARTESIAN_POINT('Ctrl Pts',(85.3415191835484,3.1827482840084,77.0335997366838));
#113633=CARTESIAN_POINT('Ctrl Pts',(85.3529435118309,3.15530692758353,77.0424849792601));
#113634=CARTESIAN_POINT('Ctrl Pts',(85.3641995909304,3.12787797423294,77.051255018393));
#113635=CARTESIAN_POINT('Ctrl Pts',(85.371631741544,3.10976721731019,77.0570456894736));
#113636=CARTESIAN_POINT('Ctrl Pts',(85.3793140484198,3.09086332054833,77.0630385222237));
#113637=CARTESIAN_POINT('Ctrl Pts',(85.3866042826731,3.07274766257864,77.0687323546987));
#113638=CARTESIAN_POINT('Ctrl Pts',(85.3903551935305,3.06342694450479,77.0716618981549));
#113639=CARTESIAN_POINT('Ctrl Pts',(85.394003006187,3.05431525216176,77.0745127386788));
#113640=CARTESIAN_POINT('Ctrl Pts',(85.3974643703546,3.04563007803897,77.0772192980654));
#113641=CARTESIAN_POINT('Ctrl Pts',(85.4649143560354,2.87638614939062,77.1299607557767));
#113642=CARTESIAN_POINT('Ctrl Pts',(85.5266941417952,2.7059554568368,77.1788836210702));
#113643=CARTESIAN_POINT('Ctrl Pts',(85.5828053059658,2.5346255676035,77.2239545594196));
#113644=CARTESIAN_POINT('Ctrl Pts',(85.6402207568679,2.35931316785643,77.2700731578513));
#113645=CARTESIAN_POINT('Ctrl Pts',(85.6917014501738,2.18305900250801,77.3121590342264));
#113646=CARTESIAN_POINT('Ctrl Pts',(85.7372343351277,2.00611866949535,77.3501710657188));
#113647=CARTESIAN_POINT('Ctrl Pts',(85.7663710211512,1.89289380063139,77.3744951257435));
#113648=CARTESIAN_POINT('Ctrl Pts',(85.793071895714,1.77938691442686,77.3971509120166));
#113649=CARTESIAN_POINT('Ctrl Pts',(85.8173291550407,1.66565496084234,77.418125491269));
#113650=CARTESIAN_POINT('Ctrl Pts',(85.8528280677087,1.49921568452159,77.4488204163263));
#113651=CARTESIAN_POINT('Ctrl Pts',(85.8830952727907,1.33229650434879,77.4759159598019));
#113652=CARTESIAN_POINT('Ctrl Pts',(85.9081981255997,1.16521709143556,77.4994608635661));
#113653=CARTESIAN_POINT('Ctrl Pts',(85.9337966630433,0.994838503788336,
77.5234706884732));
#113654=CARTESIAN_POINT('Ctrl Pts',(85.9540251498616,0.824292838675683,
77.54378844342));
#113655=CARTESIAN_POINT('Ctrl Pts',(85.9689234471876,0.653880651746717,
77.5604450953023));
#113656=CARTESIAN_POINT('Ctrl Pts',(85.9722845858547,0.61543471538934,77.5642029285285));
#113657=CARTESIAN_POINT('Ctrl Pts',(85.9753742950457,0.576995436892595,
77.5677743312878));
#113658=CARTESIAN_POINT('Ctrl Pts',(85.9781927942916,0.538566041923533,
77.5711595027625));
#113659=CARTESIAN_POINT('Origin',(27.4324635166691,25.,72.98888938658));
#113660=CARTESIAN_POINT('',(-7.08815755044579,5.,58.3404518883124));
#113661=CARTESIAN_POINT('',(-8.23395173885291,5.,84.57149802283));
#113662=CARTESIAN_POINT('Origin',(27.4324635166691,5.,72.98888938658));
#113663=CARTESIAN_POINT('',(-8.23395173885291,-5.,84.57149802283));
#113664=CARTESIAN_POINT('',(-8.23395173890591,5.,84.57149802267));
#113665=CARTESIAN_POINT('',(-7.08815755044587,-5.,58.3404518883126));
#113666=CARTESIAN_POINT('Origin',(27.4324635166691,-5.,72.98888938658));
#113667=CARTESIAN_POINT('',(-7.08815755167191,-5.,58.3404518912));
#113668=CARTESIAN_POINT('Origin',(20.5162416486691,1.37771738462078E-14,
116.353388269));
#113669=CARTESIAN_POINT('Ctrl Pts',(20.8449496767831,16.375,118.217584317867));
#113670=CARTESIAN_POINT('Ctrl Pts',(20.560377721845,16.3749999994318,118.271191799454));
#113671=CARTESIAN_POINT('Ctrl Pts',(20.2758436122818,16.3673196851251,118.324851280152));
#113672=CARTESIAN_POINT('Ctrl Pts',(19.3903453687992,16.3194739703247,118.491914823905));
#113673=CARTESIAN_POINT('Ctrl Pts',(18.7913279623376,16.2526679348737,118.605012536406));
#113674=CARTESIAN_POINT('Ctrl Pts',(17.5039222623931,16.034160127074,118.847913184993));
#113675=CARTESIAN_POINT('Ctrl Pts',(16.8187606642767,15.8703432356303,118.977067391609));
#113676=CARTESIAN_POINT('Ctrl Pts',(15.7576475272096,15.5407174414681,119.177219354591));
#113677=CARTESIAN_POINT('Ctrl Pts',(15.3735955108468,15.4050337240163,119.249698536666));
#113678=CARTESIAN_POINT('Ctrl Pts',(14.6265437499547,15.1083739087842,119.39098027536));
#113679=CARTESIAN_POINT('Ctrl Pts',(14.2635181721422,14.9482691083237,119.459816635334));
#113680=CARTESIAN_POINT('Ctrl Pts',(13.3665414482046,14.5120054500825,119.630222584242));
#113681=CARTESIAN_POINT('Ctrl Pts',(12.8412688288321,14.2188161913186,119.730266696678));
#113682=CARTESIAN_POINT('Ctrl Pts',(11.7784055359248,13.5444528029723,119.932919961903));
#113683=CARTESIAN_POINT('Ctrl Pts',(11.2451441103364,13.1582815993812,120.034719152112));
#113684=CARTESIAN_POINT('Ctrl Pts',(10.3987038222404,12.462464869475,120.196770206009));
#113685=CARTESIAN_POINT('Ctrl Pts',(10.0721152976126,12.1709707006107,120.259433153701));
#113686=CARTESIAN_POINT('Ctrl Pts',(9.45411172552166,11.5725544403491,120.378549735947));
#113687=CARTESIAN_POINT('Ctrl Pts',(9.16210718307875,11.2667712606362,120.435142432012));
#113688=CARTESIAN_POINT('Ctrl Pts',(8.47984509519864,10.4939970519773,120.568028493558));
#113689=CARTESIAN_POINT('Ctrl Pts',(8.10301362456274,10.0156082338631,120.641951418667));
#113690=CARTESIAN_POINT('Ctrl Pts',(7.34591246341852,8.93528959929101,120.791338336788));
#113691=CARTESIAN_POINT('Ctrl Pts',(6.97625508631526,8.32719027346426,120.864852016916));
#113692=CARTESIAN_POINT('Ctrl Pts',(6.45599262264532,7.33083168892778,120.969636114732));
#113693=CARTESIAN_POINT('Ctrl Pts',(6.27881899880134,6.95798344802511,121.005644436317));
#113694=CARTESIAN_POINT('Ctrl Pts',(5.95755041512535,6.21060783612537,121.071849577373));
#113695=CARTESIAN_POINT('Ctrl Pts',(5.81274808411848,5.83671191490872,121.102199809476));
#113696=CARTESIAN_POINT('Ctrl Pts',(5.48278908801904,4.88292384939799,121.172622486078));
#113697=CARTESIAN_POINT('Ctrl Pts',(5.31570887041526,4.29718792996188,121.209512719585));
#113698=CARTESIAN_POINT('Ctrl Pts',(5.03383788936494,3.05296609408649,121.274485762568));
#113699=CARTESIAN_POINT('Ctrl Pts',(4.92578521641382,2.39401992697441,121.301332717164));
#113700=CARTESIAN_POINT('Ctrl Pts',(4.81261148165586,1.2915016417281,121.334101978111));
#113701=CARTESIAN_POINT('Ctrl Pts',(4.78505336113655,0.85116335348093,121.344027614717));
#113702=CARTESIAN_POINT('Ctrl Pts',(4.76536842121233,-0.0168249872455496,
121.357643273541));
#113703=CARTESIAN_POINT('Ctrl Pts',(4.7721643660596,-0.444100963069227,
121.361559172694));
#113704=CARTESIAN_POINT('Ctrl Pts',(4.8287501723439,-1.48218942359855,121.364170012791));
#113705=CARTESIAN_POINT('Ctrl Pts',(4.89585438918724,-2.0914232995622,121.359808433127));
#113706=CARTESIAN_POINT('Ctrl Pts',(5.11402913302341,-3.4023682566261,121.337245585004));
#113707=CARTESIAN_POINT('Ctrl Pts',(5.27721183480348,-4.10075146847743,
121.316827709394));
#113708=CARTESIAN_POINT('Ctrl Pts',(5.60446279919227,-5.18060140277138,
121.272175811282));
#113709=CARTESIAN_POINT('Ctrl Pts',(5.7386430530597,-5.57038133211787,121.253264839852));
#113710=CARTESIAN_POINT('Ctrl Pts',(6.03249489152454,-6.33050202809045,
121.211006773134));
#113711=CARTESIAN_POINT('Ctrl Pts',(6.19145203607718,-6.70081947829591,
121.187815822064));
#113712=CARTESIAN_POINT('Ctrl Pts',(6.62359354871342,-7.61392061452341,
121.123866996895));
#113713=CARTESIAN_POINT('Ctrl Pts',(6.91342082458287,-8.1479497402729,121.080178706915));
#113714=CARTESIAN_POINT('Ctrl Pts',(7.57820509716986,-9.22626204269762,
120.978151358745));
#113715=CARTESIAN_POINT('Ctrl Pts',(7.95779022242495,-9.76633340359109,
120.918951563827));
#113716=CARTESIAN_POINT('Ctrl Pts',(8.6436636687758,-10.6268782169619,120.810792977168));
#113717=CARTESIAN_POINT('Ctrl Pts',(8.93249980583699,-10.9606327551128,
120.764957268814));
#113718=CARTESIAN_POINT('Ctrl Pts',(9.5236526191515,-11.5902362641935,120.670869569245));
#113719=CARTESIAN_POINT('Ctrl Pts',(9.82469433091606,-11.8868426097135,
120.622876156179));
#113720=CARTESIAN_POINT('Ctrl Pts',(10.5873244522212,-12.5818566432385,
120.500983008873));
#113721=CARTESIAN_POINT('Ctrl Pts',(11.0602699688564,-12.9664901615787,
120.425078437679));
#113722=CARTESIAN_POINT('Ctrl Pts',(12.1248222765698,-13.7369140406902,
120.253231628986));
#113723=CARTESIAN_POINT('Ctrl Pts',(12.7222049932059,-14.1123415385586,
120.156194743627));
#113724=CARTESIAN_POINT('Ctrl Pts',(13.7048000340426,-14.6434851446472,
119.995979681164));
#113725=CARTESIAN_POINT('Ctrl Pts',(14.0751201110258,-14.8256257622507,
119.935480783136));
#113726=CARTESIAN_POINT('Ctrl Pts',(14.813050602275,-15.15392143503,119.8149240473));
#113727=CARTESIAN_POINT('Ctrl Pts',(15.1798936674267,-15.3011443639482,
119.755027934311));
#113728=CARTESIAN_POINT('Ctrl Pts',(16.1203776478522,-15.6387948805931,
119.601426904445));
#113729=CARTESIAN_POINT('Ctrl Pts',(16.6999012936228,-15.8105439418231,
119.506691369404));
#113730=CARTESIAN_POINT('Ctrl Pts',(17.936785303593,-16.1021212889422,119.303982023674));
#113731=CARTESIAN_POINT('Ctrl Pts',(18.5947437481837,-16.2143268134127,
119.195850610668));
#113732=CARTESIAN_POINT('Ctrl Pts',(19.687203546909,-16.3308560109771,119.016084384859));
#113733=CARTESIAN_POINT('Ctrl Pts',(20.1184051367867,-16.3592035165354,
118.94508023839));
#113734=CARTESIAN_POINT('Ctrl Pts',(20.9746338980482,-16.380630176759,118.804246552665));
#113735=CARTESIAN_POINT('Ctrl Pts',(21.3993127608701,-16.3742972727923,
118.734517544012));
#113736=CARTESIAN_POINT('Ctrl Pts',(22.4247777142537,-16.3180078925996,
118.566303953469));
#113737=CARTESIAN_POINT('Ctrl Pts',(23.0240182250927,-16.2509343747199,
118.46808654998));
#113738=CARTESIAN_POINT('Ctrl Pts',(24.3244196987897,-16.0302753659217,
118.254778504253));
#113739=CARTESIAN_POINT('Ctrl Pts',(25.0220284027002,-15.8629945222672,
118.140225379743));
#113740=CARTESIAN_POINT('Ctrl Pts',(26.0886546236702,-15.5300690963237,
117.965220170735));
#113741=CARTESIAN_POINT('Ctrl Pts',(26.4664124402663,-15.3964168081272,
117.903278978449));
#113742=CARTESIAN_POINT('Ctrl Pts',(27.2168327898064,-15.0988355234507,
117.7805254849));
#113743=CARTESIAN_POINT('Ctrl Pts',(27.5890792034858,-14.9346004754354,
117.719823710413));
#113744=CARTESIAN_POINT('Ctrl Pts',(28.4920465230995,-14.4945467777078,
117.57289640398));
#113745=CARTESIAN_POINT('Ctrl Pts',(29.0145808915519,-14.2028410042795,
117.488114142301));
#113746=CARTESIAN_POINT('Ctrl Pts',(30.1677040854385,-13.4721703757075,
117.301251244048));
#113747=CARTESIAN_POINT('Ctrl Pts',(30.7858698634633,-13.0157853524169,
117.201229394986));
#113748=CARTESIAN_POINT('Ctrl Pts',(31.6508239602556,-12.276882594101,117.061942375504));
#113749=CARTESIAN_POINT('Ctrl Pts',(31.9235781977717,-12.0272962337938,
117.018139934069));
#113750=CARTESIAN_POINT('Ctrl Pts',(32.6685048727935,-11.2975278642344,
116.899101386167));
#113751=CARTESIAN_POINT('Ctrl Pts',(33.1200888948291,-10.7967905266924,
116.827755373074));
#113752=CARTESIAN_POINT('Ctrl Pts',(33.8995146291264,-9.81706586470456,
116.705574216279));
#113753=CARTESIAN_POINT('Ctrl Pts',(34.2352669512445,-9.34590300807752,
116.653342387818));
#113754=CARTESIAN_POINT('Ctrl Pts',(34.8931481542072,-8.31112175338087,
116.551834947782));
#113755=CARTESIAN_POINT('Ctrl Pts',(35.2082625859149,-7.744104661659,116.503744836743));
#113756=CARTESIAN_POINT('Ctrl Pts',(35.6897396189397,-6.74306729907632,
116.431728658734));
#113757=CARTESIAN_POINT('Ctrl Pts',(35.8726183337573,-6.31807756200283,
116.404892093368));
#113758=CARTESIAN_POINT('Ctrl Pts',(36.2794399424667,-5.25178640577539,
116.346872057103));
#113759=CARTESIAN_POINT('Ctrl Pts',(36.4822775238642,-4.60316262806885,
116.319429213635));
#113760=CARTESIAN_POINT('Ctrl Pts',(36.8951991037712,-2.92793855495885,
116.267347054293));
#113761=CARTESIAN_POINT('Ctrl Pts',(37.049006831098,-1.89034145061715,116.252247993329));
#113762=CARTESIAN_POINT('Ctrl Pts',(37.1267103121608,-0.420910239128301,
116.255589744507));
#113763=CARTESIAN_POINT('Ctrl Pts',(37.1328878516839,0.00402868902685441,
116.259479566599));
#113764=CARTESIAN_POINT('Ctrl Pts',(37.1066528453196,1.10928849771526,116.277385483572));
#113765=CARTESIAN_POINT('Ctrl Pts',(37.048743919782,1.78810410530278,116.295943789864));
#113766=CARTESIAN_POINT('Ctrl Pts',(36.8573145214258,3.08469646862634,116.345460736456));
#113767=CARTESIAN_POINT('Ctrl Pts',(36.7298396643764,3.7022014920466,116.375366743719));
#113768=CARTESIAN_POINT('Ctrl Pts',(36.4339114898637,4.81193811867991,116.440901050943));
#113769=CARTESIAN_POINT('Ctrl Pts',(36.2767924596985,5.3064543030832,116.474563704631));
#113770=CARTESIAN_POINT('Ctrl Pts',(35.94950740758,6.19025495266907,116.543289610683));
#113771=CARTESIAN_POINT('Ctrl Pts',(35.7870277847551,6.58200030310312,116.577005611126));
#113772=CARTESIAN_POINT('Ctrl Pts',(35.3498426650777,7.53095447632581,116.666765889529));
#113773=CARTESIAN_POINT('Ctrl Pts',(35.0584583250972,8.07946459542988,116.725750167534));
#113774=CARTESIAN_POINT('Ctrl Pts',(34.3446687704117,9.25671145535685,116.86817565282));
#113775=CARTESIAN_POINT('Ctrl Pts',(33.9084059099991,9.87507715868073,116.953951655212));
#113776=CARTESIAN_POINT('Ctrl Pts',(33.0537009768897,10.923666116097,117.120393299594));
#113777=CARTESIAN_POINT('Ctrl Pts',(32.6511232386463,11.3654519807241,117.198308385746));
#113778=CARTESIAN_POINT('Ctrl Pts',(31.9558880781184,12.0486275219986,117.332670334456));
#113779=CARTESIAN_POINT('Ctrl Pts',(31.6772079410402,12.3039234612902,117.386448701375));
#113780=CARTESIAN_POINT('Ctrl Pts',(30.8181950144664,13.0371387092337,117.551776378099));
#113781=CARTESIAN_POINT('Ctrl Pts',(30.2136188341809,13.4840967544494,117.667527990713));
#113782=CARTESIAN_POINT('Ctrl Pts',(29.0761869599664,14.2075608565754,117.884105131791));
#113783=CARTESIAN_POINT('Ctrl Pts',(28.5545753434907,14.4996912570987,117.983034196769));
#113784=CARTESIAN_POINT('Ctrl Pts',(27.6563439774672,14.9385818707944,118.153161433088));
#113785=CARTESIAN_POINT('Ctrl Pts',(27.2880615584285,15.1015661154573,118.222872926722));
#113786=CARTESIAN_POINT('Ctrl Pts',(26.5412221153119,15.3987943846171,118.364333736677));
#113787=CARTESIAN_POINT('Ctrl Pts',(26.1629504867174,15.533003030054,118.435990930457));
#113788=CARTESIAN_POINT('Ctrl Pts',(25.1012520068866,15.8650022450366,118.636906660495));
#113789=CARTESIAN_POINT('Ctrl Pts',(24.4092489289208,16.0313210680016,118.767601207822));
#113790=CARTESIAN_POINT('Ctrl Pts',(23.1164101485355,16.2513860974161,119.011190980202));
#113791=CARTESIAN_POINT('Ctrl Pts',(22.5190413259115,16.3183899512091,119.123531240596));
#113792=CARTESIAN_POINT('Ctrl Pts',(21.6309411126748,16.3670889161068,119.290604045939));
#113793=CARTESIAN_POINT('Ctrl Pts',(21.3421435866636,16.37500000057,119.344946631207));
#113794=CARTESIAN_POINT('Ctrl Pts',(21.0533274903535,16.375,119.399353621412));
#113795=CARTESIAN_POINT('Ctrl Pts',(21.0210448803799,16.375,119.216269433269));
#113796=CARTESIAN_POINT('Ctrl Pts',(21.2091318775354,16.3749999995409,119.180837725885));
#113797=CARTESIAN_POINT('Ctrl Pts',(21.3972151118309,16.3716448489046,119.145380652092));
#113798=CARTESIAN_POINT('Ctrl Pts',(22.129344463814,16.3455117717536,119.007303069283));
#113799=CARTESIAN_POINT('Ctrl Pts',(22.6721403186664,16.2980016429559,118.904821018823));
#113800=CARTESIAN_POINT('Ctrl Pts',(23.8478536836665,16.133620224497,118.682943650173));
#113801=CARTESIAN_POINT('Ctrl Pts',(24.4783842341807,16.0059662313511,118.564026140583));
#113802=CARTESIAN_POINT('Ctrl Pts',(25.677290186071,15.6863267000636,118.337952311273));
#113803=CARTESIAN_POINT('Ctrl Pts',(26.2459811391878,15.4997572265107,118.230729148814));
#113804=CARTESIAN_POINT('Ctrl Pts',(27.2265273202302,15.1155688019718,118.045336237119));
#113805=CARTESIAN_POINT('Ctrl Pts',(27.6428128347225,14.9315226080182,117.966394393069));
#113806=CARTESIAN_POINT('Ctrl Pts',(28.6151484541191,14.4508997439625,117.781617308589));
#113807=CARTESIAN_POINT('Ctrl Pts',(29.1628753749719,14.1386251308742,117.677270394425));
#113808=CARTESIAN_POINT('Ctrl Pts',(30.2121066950332,13.4554895657411,117.477160345643));
#113809=CARTESIAN_POINT('Ctrl Pts',(30.7132868775911,13.0860987775049,117.381461820497));
#113810=CARTESIAN_POINT('Ctrl Pts',(31.6902754071368,12.2746616878511,117.194364546538));
#113811=CARTESIAN_POINT('Ctrl Pts',(32.163404786753,11.8310500365806,117.103433365788));
#113812=CARTESIAN_POINT('Ctrl Pts',(32.8735132979374,11.080184408507,116.96574152817));
#113813=CARTESIAN_POINT('Ctrl Pts',(33.1280659380327,10.7910743327432,116.916135028231));
#113814=CARTESIAN_POINT('Ctrl Pts',(33.844073207513,9.91714487357266,116.77606015033));
#113815=CARTESIAN_POINT('Ctrl Pts',(34.2763750258454,9.30891627341975,116.6908063204));
#113816=CARTESIAN_POINT('Ctrl Pts',(34.9813230114452,8.15805333104755,116.550588458271));
#113817=CARTESIAN_POINT('Ctrl Pts',(35.2681430841832,7.62601541255148,116.493046851121));
#113818=CARTESIAN_POINT('Ctrl Pts',(35.6975270948211,6.71231056108483,116.405597429031));
#113819=CARTESIAN_POINT('Ctrl Pts',(35.856320222466,6.33922267043306,116.37284567988));
#113820=CARTESIAN_POINT('Ctrl Pts',(36.1471447701724,5.57924034963549,116.311793432552));
#113821=CARTESIAN_POINT('Ctrl Pts',(36.2788944480832,5.19254204154739,116.283582673026));
#113822=CARTESIAN_POINT('Ctrl Pts',(36.6027999168374,4.11232940312022,116.212765649901));
#113823=CARTESIAN_POINT('Ctrl Pts',(36.7643736529417,3.41025680340466,116.175628119676));
#113824=CARTESIAN_POINT('Ctrl Pts',(36.9779681886653,2.09643819954386,116.122359176686));
#113825=CARTESIAN_POINT('Ctrl Pts',(37.0426989224839,1.48813747162239,116.10393213763));
#113826=CARTESIAN_POINT('Ctrl Pts',(37.0955271601667,0.449603788305685,
116.082575680149));
#113827=CARTESIAN_POINT('Ctrl Pts',(37.1007337682424,0.0209528223131461,
116.076641323096));
#113828=CARTESIAN_POINT('Ctrl Pts',(37.0776801789711,-0.846849150257792,
116.070285431662));
#113829=CARTESIAN_POINT('Ctrl Pts',(37.0485748538665,-1.28563078188508,
116.070058690432));
#113830=CARTESIAN_POINT('Ctrl Pts',(36.9311891574028,-2.39022465940462,
116.077284079822));
#113831=CARTESIAN_POINT('Ctrl Pts',(36.8199178219872,-3.05274998811974,
116.088858437463));
#113832=CARTESIAN_POINT('Ctrl Pts',(36.5316502460197,-4.30112393281202,
116.124657868899));
#113833=CARTESIAN_POINT('Ctrl Pts',(36.3617472251379,-4.88750193079068,
116.147608578871));
#113834=CARTESIAN_POINT('Ctrl Pts',(36.0274823548541,-5.84086906357453,
116.19482981852));
#113835=CARTESIAN_POINT('Ctrl Pts',(35.8813462638261,-6.21375293713925,
116.215908008467));
#113836=CARTESIAN_POINT('Ctrl Pts',(35.5566013349731,-6.9612282755069,116.263389976612));
#113837=CARTESIAN_POINT('Ctrl Pts',(35.3771346186739,-7.33511832637184,
116.289979693107));
#113838=CARTESIAN_POINT('Ctrl Pts',(34.8520486261734,-8.33107956937099,
116.368880244316));
#113839=CARTESIAN_POINT('Ctrl Pts',(34.4801094096761,-8.93786897760451,
116.425908415246));
#113840=CARTESIAN_POINT('Ctrl Pts',(33.7181280802402,-10.0172495988322,
116.544727350233));
#113841=CARTESIAN_POINT('Ctrl Pts',(33.3385187776704,-10.4958789408354,
116.604630085464));
#113842=CARTESIAN_POINT('Ctrl Pts',(32.6520278465918,-11.2684074249856,
116.71364372183));
#113843=CARTESIAN_POINT('Ctrl Pts',(32.3586408904443,-11.573757717665,116.760388703545));
#113844=CARTESIAN_POINT('Ctrl Pts',(31.7369943050775,-12.1722093244503,
116.85957407915));
#113845=CARTESIAN_POINT('Ctrl Pts',(31.4080817467552,-12.4640999378746,
116.912172552455));
#113846=CARTESIAN_POINT('Ctrl Pts',(30.557667792781,-13.1592229908957,117.048700775769));
#113847=CARTESIAN_POINT('Ctrl Pts',(30.0229043823789,-13.5444910972657,
117.13503518517));
#113848=CARTESIAN_POINT('Ctrl Pts',(28.9564262533286,-14.2179993513951,
117.308152610967));
#113849=CARTESIAN_POINT('Ctrl Pts',(28.4289654111353,-14.5111092739633,
117.39416536399));
#113850=CARTESIAN_POINT('Ctrl Pts',(27.5278176717548,-14.9475578246718,
117.54133721563));
#113851=CARTESIAN_POINT('Ctrl Pts',(27.1627938609599,-15.1078657553674,
117.600988772271));
#113852=CARTESIAN_POINT('Ctrl Pts',(26.4124904929182,-15.4045530984644,
117.723512644894));
#113853=CARTESIAN_POINT('Ctrl Pts',(26.0272117649698,-15.5401223337483,
117.786421458838));
#113854=CARTESIAN_POINT('Ctrl Pts',(24.9614860358582,-15.8699271201329,
117.960645185498));
#113855=CARTESIAN_POINT('Ctrl Pts',(24.2729033574866,-16.0339360814211,
118.073471036143));
#113856=CARTESIAN_POINT('Ctrl Pts',(22.9797149815855,-16.2525640843145,
118.285930997449));
#113857=CARTESIAN_POINT('Ctrl Pts',(22.3783601715876,-16.319386137466,118.384941140902));
#113858=CARTESIAN_POINT('Ctrl Pts',(21.354059431856,-16.374571109063,118.553516692846));
#113859=CARTESIAN_POINT('Ctrl Pts',(20.9326788300833,-16.3805558020248,
118.622818971033));
#113860=CARTESIAN_POINT('Ctrl Pts',(20.0760515029751,-16.3587761243772,
118.763440921684));
#113861=CARTESIAN_POINT('Ctrl Pts',(19.6411834765693,-16.3298663047228,
118.834737885319));
#113862=CARTESIAN_POINT('Ctrl Pts',(18.5535127541741,-16.2126655967384,
119.013080985069));
#113863=CARTESIAN_POINT('Ctrl Pts',(17.9038907796058,-16.1016925093283,
119.119633324013));
#113864=CARTESIAN_POINT('Ctrl Pts',(16.6767957492659,-15.8130571197902,
119.321032664589));
#113865=CARTESIAN_POINT('Ctrl Pts',(16.098882022775,-15.642177621903,119.415935800281));
#113866=CARTESIAN_POINT('Ctrl Pts',(15.1574942497523,-15.3050402551196,
119.57020555807));
#113867=CARTESIAN_POINT('Ctrl Pts',(14.7882864778266,-15.1571115096946,
119.630603712903));
#113868=CARTESIAN_POINT('Ctrl Pts',(14.0506074722251,-14.8292576329358,
119.750900076669));
#113869=CARTESIAN_POINT('Ctrl Pts',(13.6827534072311,-14.6486388375962,
119.810725334464));
#113870=CARTESIAN_POINT('Ctrl Pts',(12.6991201429727,-14.1181338292149,
119.970476404401));
#113871=CARTESIAN_POINT('Ctrl Pts',(12.0985491030648,-13.7412107925646,
120.067797018619));
#113872=CARTESIAN_POINT('Ctrl Pts',(11.0318055770103,-12.9695729735432,
120.240338423157));
#113873=CARTESIAN_POINT('Ctrl Pts',(10.5595268380952,-12.5856856666768,
120.316586053339));
#113874=CARTESIAN_POINT('Ctrl Pts',(9.79638608059639,-11.8907127291724,
120.43911324634));
#113875=CARTESIAN_POINT('Ctrl Pts',(9.4943180599465,-11.5932547346191,120.487381865253));
#113876=CARTESIAN_POINT('Ctrl Pts',(8.9032160382818,-10.9639781252492,120.581183417368));
#113877=CARTESIAN_POINT('Ctrl Pts',(8.61529972165134,-10.6315678888641,
120.626562914325));
#113878=CARTESIAN_POINT('Ctrl Pts',(7.92763484426373,-9.76975584838192,
120.734381748345));
#113879=CARTESIAN_POINT('Ctrl Pts',(7.54580325266375,-9.22669885034435,
120.793728572479));
#113880=CARTESIAN_POINT('Ctrl Pts',(6.8789726410338,-8.14450419205229,120.896353041296));
#113881=CARTESIAN_POINT('Ctrl Pts',(6.58902724562507,-7.60978860165946,
120.940481819028));
#113882=CARTESIAN_POINT('Ctrl Pts',(6.15741770612613,-6.69685673131263,
121.004862979586));
#113883=CARTESIAN_POINT('Ctrl Pts',(5.998978099082,-6.32746337152405,121.028093649019));
#113884=CARTESIAN_POINT('Ctrl Pts',(5.70515824532934,-5.56721695848674,
121.070126277436));
#113885=CARTESIAN_POINT('Ctrl Pts',(5.57065440452245,-5.17632983917947,
121.088809869634));
#113886=CARTESIAN_POINT('Ctrl Pts',(5.24372883810874,-4.096592838739,121.132764719218));
#113887=CARTESIAN_POINT('Ctrl Pts',(5.08096720098151,-3.39950969154844,
121.152882509476));
#113888=CARTESIAN_POINT('Ctrl Pts',(4.8631397704427,-2.08955413269141,121.175733358692));
#113889=CARTESIAN_POINT('Ctrl Pts',(4.79615003176477,-1.47997189837179,
121.180518731692));
#113890=CARTESIAN_POINT('Ctrl Pts',(4.7398276134997,-0.442035720120334,
121.178414324204));
#113891=CARTESIAN_POINT('Ctrl Pts',(4.73310555264194,-0.0152697929301527,
121.174603797263));
#113892=CARTESIAN_POINT('Ctrl Pts',(4.75279931713012,0.85280667069366,121.160706016147));
#113893=CARTESIAN_POINT('Ctrl Pts',(4.78039298773773,1.29373913838167,121.150454881641));
#113894=CARTESIAN_POINT('Ctrl Pts',(4.89356839464253,2.39547527162674,121.117061045922));
#113895=CARTESIAN_POINT('Ctrl Pts',(5.00139648645773,3.05307143673042,121.090062567205));
#113896=CARTESIAN_POINT('Ctrl Pts',(5.28286697461074,4.29573612649765,121.025470220113));
#113897=CARTESIAN_POINT('Ctrl Pts',(5.44989054252997,4.88123512615391,120.989022181531));
#113898=CARTESIAN_POINT('Ctrl Pts',(5.77986510507261,5.83518844406934,120.919115881787));
#113899=CARTESIAN_POINT('Ctrl Pts',(5.92479484405015,6.20945808579371,120.88885565206));
#113900=CARTESIAN_POINT('Ctrl Pts',(6.24596853150438,6.9568071761554,120.822448097083));
#113901=CARTESIAN_POINT('Ctrl Pts',(6.42287468611648,7.32927828513093,120.786220060535));
#113902=CARTESIAN_POINT('Ctrl Pts',(6.94293518901919,8.32577943534677,120.680828775043));
#113903=CARTESIAN_POINT('Ctrl Pts',(7.31277227877049,8.93435801135389,120.607037047274));
#113904=CARTESIAN_POINT('Ctrl Pts',(8.07011615192993,10.0150244357185,120.457940327377));
#113905=CARTESIAN_POINT('Ctrl Pts',(8.44691841369944,10.4933269043719,120.384472763636));
#113906=CARTESIAN_POINT('Ctrl Pts',(9.12927267228777,11.26619396452,120.252119903972));
#113907=CARTESIAN_POINT('Ctrl Pts',(9.42141679712077,11.5721294771388,120.195611852136));
#113908=CARTESIAN_POINT('Ctrl Pts',(10.0393301143943,12.1705347454964,120.076231654595));
#113909=CARTESIAN_POINT('Ctrl Pts',(10.3656781195924,12.4618892800762,120.013301191211));
#113910=CARTESIAN_POINT('Ctrl Pts',(11.2121872463817,13.1579485499713,119.85060195608));
#113911=CARTESIAN_POINT('Ctrl Pts',(11.7458328819303,13.5444399087714,119.748522308693));
#113912=CARTESIAN_POINT('Ctrl Pts',(12.8092948086128,14.2191076742046,119.546045978058));
#113913=CARTESIAN_POINT('Ctrl Pts',(13.3347384211048,14.5123247839378,119.446399145257));
#113914=CARTESIAN_POINT('Ctrl Pts',(14.2317845745067,14.9485252410783,119.276502684149));
#113915=CARTESIAN_POINT('Ctrl Pts',(14.5946974353486,15.1085564130321,119.207805648761));
#113916=CARTESIAN_POINT('Ctrl Pts',(15.3417325317689,15.4052068819475,119.066307326217));
#113917=CARTESIAN_POINT('Ctrl Pts',(15.7258986236758,15.5409317215388,118.993534403211));
#113918=CARTESIAN_POINT('Ctrl Pts',(16.7868834627811,15.870491784824,118.79276342403));
#113919=CARTESIAN_POINT('Ctrl Pts',(17.4718174756613,16.0342406736939,118.663410835333));
#113920=CARTESIAN_POINT('Ctrl Pts',(18.7591419880857,16.2527058726663,118.420863675022));
#113921=CARTESIAN_POINT('Ctrl Pts',(19.358286584221,16.319506023589,118.308191325544));
#113922=CARTESIAN_POINT('Ctrl Pts',(20.2437951232121,16.3673265956352,118.141604753093));
#113923=CARTESIAN_POINT('Ctrl Pts',(20.5282226470002,16.3750000005693,118.088083586325));
#113924=CARTESIAN_POINT('Ctrl Pts',(20.8126670602263,16.375,118.034500130964));
#113925=CARTESIAN_POINT('Origin',(21.9054270700043,1.38313839548321E-14,
124.231850293098));
#113926=CARTESIAN_POINT('',(37.957553020665,1.18719490761447E-14,123.127652630566));
#113927=CARTESIAN_POINT('',(22.2006289720379,16.,125.906023473218));
#113928=CARTESIAN_POINT('Origin',(22.2006289720381,1.38313839548321E-14,
125.906023473218));
#113929=CARTESIAN_POINT('',(22.6000197806719,16.,128.171081305147));
#113930=CARTESIAN_POINT('',(21.9054270700043,16.,124.231850293098));
#113931=CARTESIAN_POINT('Origin',(22.6000197806719,1.38313839548321E-14,
128.171081305147));
#113932=CARTESIAN_POINT('Origin',(22.2006289720381,1.38313839548321E-14,
125.906023473218));
#113933=CARTESIAN_POINT('Origin',(21.9054270700043,1.38313839548321E-14,
124.231850293098));
#113934=CARTESIAN_POINT('',(38.0316540255793,1.18260248212283E-14,121.388361383802));
#113935=CARTESIAN_POINT('Origin',(20.5162416486691,1.37771738462078E-14,
116.353388269));
#113936=CARTESIAN_POINT('',(3.90398359427627,-1.84682113605508,119.460277231561));
#113937=CARTESIAN_POINT('Origin',(20.5466300797608,1.37771738462078E-14,
116.525729625777));
#113938=CARTESIAN_POINT('',(36.9907122711205,-3.93403322697978E-8,113.998798303651));
#113939=CARTESIAN_POINT('Ctrl Pts',(3.90398359410123,-1.84682113607734,
119.460277231708));
#113940=CARTESIAN_POINT('Ctrl Pts',(4.09253341241264,-3.46976715541364,
119.43913879994));
#113941=CARTESIAN_POINT('Ctrl Pts',(4.51057950486753,-5.0605456459531,119.376649209939));
#113942=CARTESIAN_POINT('Ctrl Pts',(5.79266958034729,-8.0927115867017,119.17455671751));
#113943=CARTESIAN_POINT('Ctrl Pts',(6.65971736290921,-9.5201420067015,119.034171523839));
#113944=CARTESIAN_POINT('Ctrl Pts',(9.14067745054749,-12.5154238059216,
118.624373321083));
#113945=CARTESIAN_POINT('Ctrl Pts',(10.8833818913406,-13.924253160688,118.334038478557));
#113946=CARTESIAN_POINT('Ctrl Pts',(14.8090149381498,-15.9767847332362,
117.67364111434));
#113947=CARTESIAN_POINT('Ctrl Pts',(16.9465567801897,-16.5926464636835,
117.313655965925));
#113948=CARTESIAN_POINT('Ctrl Pts',(21.3360110729831,-16.9482149073978,
116.571441632361));
#113949=CARTESIAN_POINT('Ctrl Pts',(23.5360492708532,-16.6801796399091,
116.200471262066));
#113950=CARTESIAN_POINT('Ctrl Pts',(27.7085953562218,-15.2935300241975,
115.496533117316));
#113951=CARTESIAN_POINT('Ctrl Pts',(29.6310311157987,-14.1880688975949,
115.174475049015));
#113952=CARTESIAN_POINT('Ctrl Pts',(32.943669339213,-11.2838229294257,114.622135650669));
#113953=CARTESIAN_POINT('Ctrl Pts',(34.293178901759,-9.51652058353961,114.401130878503));
#113954=CARTESIAN_POINT('Ctrl Pts',(36.2394244838757,-5.55274054743395,
114.089754684589));
#113955=CARTESIAN_POINT('Ctrl Pts',(36.8110750825502,-3.40072162936504,
114.005863757635));
#113956=CARTESIAN_POINT('Ctrl Pts',(36.9812100412032,-0.799638676443703,
113.994632996858));
#113957=CARTESIAN_POINT('Ctrl Pts',(36.9930711830864,-0.399432342122534,
113.995429427058));
#113958=CARTESIAN_POINT('Ctrl Pts',(36.9907122708882,-3.93444676838328E-8,
113.998798303983));
#113959=CARTESIAN_POINT('',(37.4303148066539,1.16738429686722E-14,113.370980817571));
#113960=CARTESIAN_POINT('',(37.4303148066539,1.16738429686722E-14,113.370980817571));
#113961=CARTESIAN_POINT('Origin',(20.5162416486691,1.37771738462078E-14,
116.353388269));
#113962=CARTESIAN_POINT('Ctrl Pts',(36.9907122708882,-3.93444688880656E-8,
113.998798303983));
#113963=CARTESIAN_POINT('Ctrl Pts',(36.9800850306418,1.79950019091975,114.013975581234));
#113964=CARTESIAN_POINT('Ctrl Pts',(36.6819302639181,3.58330630250089,114.080237606053));
#113965=CARTESIAN_POINT('Ctrl Pts',(35.7530800713107,6.33618653414545,114.265066091959));
#113966=CARTESIAN_POINT('Ctrl Pts',(35.2956795589072,7.34652123993085,114.354154457965));
#113967=CARTESIAN_POINT('Ctrl Pts',(34.2285725062847,9.19089883267023,114.558491993484));
#113968=CARTESIAN_POINT('Ctrl Pts',(33.6338727138396,10.0291239704148,114.670864685681));
#113969=CARTESIAN_POINT('Ctrl Pts',(31.5459638144946,12.4575613900211,115.062384361103));
#113970=CARTESIAN_POINT('Ctrl Pts',(29.8207162508918,13.7996252076585,115.383524865064));
#113971=CARTESIAN_POINT('Ctrl Pts',(26.9146848459564,15.2482131474179,115.919866461799));
#113972=CARTESIAN_POINT('Ctrl Pts',(25.895397765369,15.6324963399188,116.108011822642));
#113973=CARTESIAN_POINT('Ctrl Pts',(23.870374682289,16.1689827911728,116.481257071023));
#113974=CARTESIAN_POINT('Ctrl Pts',(22.8723592822232,16.3346562272248,116.664754987268));
#113975=CARTESIAN_POINT('Ctrl Pts',(20.1524185690243,16.5243507431533,117.164544345951));
#113976=CARTESIAN_POINT('Ctrl Pts',(18.4322580304876,16.3641488207914,117.4815548212));
#113977=CARTESIAN_POINT('Ctrl Pts',(15.9758638057878,15.7279853791109,117.933720990333));
#113978=CARTESIAN_POINT('Ctrl Pts',(15.1949824542152,15.4599369840143,118.07740759597));
#113979=CARTESIAN_POINT('Ctrl Pts',(13.63561352332,14.7849825795089,118.365310419915));
#113980=CARTESIAN_POINT('Ctrl Pts',(12.8618917558936,14.3714704128383,118.508675853693));
#113981=CARTESIAN_POINT('Ctrl Pts',(12.125260423911,13.8967357377783,118.645285943585));
#113982=CARTESIAN_POINT('Ctrl Pts',(17.9811304324852,16.7992135487842,116.978096432152));
#113983=CARTESIAN_POINT('Ctrl Pts',(17.0503538967826,16.626385888926,117.167878519795));
#113984=CARTESIAN_POINT('Ctrl Pts',(16.1385226671129,16.3728037819194,117.355201872128));
#113985=CARTESIAN_POINT('Ctrl Pts',(14.3473992740267,15.7021557934855,117.72511490003));
#113986=CARTESIAN_POINT('Ctrl Pts',(13.4658015096741,15.2811885701607,117.90700169916));
#113987=CARTESIAN_POINT('Ctrl Pts',(10.5304702170588,13.5432870163047,118.516688678144));
#113988=CARTESIAN_POINT('Ctrl Pts',(9.15175218320397,12.097625298113,118.817226349984));
#113989=CARTESIAN_POINT('Ctrl Pts',(7.70060472672751,10.3365673810277,119.134906706266));
#113990=CARTESIAN_POINT('Ctrl Pts',(7.14965557029621,9.53339680556488,119.258265584443));
#113991=CARTESIAN_POINT('Ctrl Pts',(6.33485406962454,8.08283642086701,119.44871952037));
#113992=CARTESIAN_POINT('Ctrl Pts',(6.03619407286761,7.46301526240171,119.521139481765));
#113993=CARTESIAN_POINT('Ctrl Pts',(5.36573584063663,5.81988748793478,119.689551381307));
#113994=CARTESIAN_POINT('Ctrl Pts',(5.04916200526517,4.76612292289117,119.77442607934));
#113995=CARTESIAN_POINT('Ctrl Pts',(4.64336725291272,2.67058753533681,119.905000730856));
#113996=CARTESIAN_POINT('Ctrl Pts',(4.54325447090625,1.63745668755726,119.952553699906));
#113997=CARTESIAN_POINT('Ctrl Pts',(4.53968745365174,0.597925404677087,
119.982827119854));
#113998=CARTESIAN_POINT('Origin',(20.412052742069,1.37771738462078E-14,
115.762503617193));
#113999=CARTESIAN_POINT('Ctrl Pts',(3.85199197861135,1.50203116532297E-8,
119.744830291073));
#114000=CARTESIAN_POINT('Ctrl Pts',(3.85271799321469,-0.37210160825748,
119.748947726387));
#114001=CARTESIAN_POINT('Ctrl Pts',(3.86545935605242,-0.744122030987361,
119.750852528501));
#114002=CARTESIAN_POINT('Ctrl Pts',(3.9298097134233,-1.70942059371102,119.750262875271));
#114003=CARTESIAN_POINT('Ctrl Pts',(4.00009513845879,-2.3009195849853,119.74445746699));
#114004=CARTESIAN_POINT('Ctrl Pts',(4.22677607963365,-3.62113055601483,
119.719625040996));
#114005=CARTESIAN_POINT('Ctrl Pts',(4.40009631645244,-4.34564743104804,
119.69769156195));
#114006=CARTESIAN_POINT('Ctrl Pts',(4.73873631394887,-5.4419393116626,119.651410533643));
#114007=CARTESIAN_POINT('Ctrl Pts',(4.87132594088532,-5.82309122877746,
119.63276466704));
#114008=CARTESIAN_POINT('Ctrl Pts',(5.28797586353499,-6.89751614828942,
119.572610144393));
#114009=CARTESIAN_POINT('Ctrl Pts',(5.60395796881511,-7.57704252247497,
119.525142407087));
#114010=CARTESIAN_POINT('Ctrl Pts',(6.29193951357836,-8.83402061782267,
119.419845430246));
#114011=CARTESIAN_POINT('Ctrl Pts',(6.65631953289691,-9.4140855358866,119.363347348149));
#114012=CARTESIAN_POINT('Ctrl Pts',(7.52516386874132,-10.6283481506271,
119.227472650152));
#114013=CARTESIAN_POINT('Ctrl Pts',(8.0419455767051,-11.2514241803914,119.145991033838));
#114014=CARTESIAN_POINT('Ctrl Pts',(9.08935198284955,-12.3450437351211,
118.978848345114));
#114015=CARTESIAN_POINT('Ctrl Pts',(9.60911156584989,-12.823841024795,118.895017827169));
#114016=CARTESIAN_POINT('Ctrl Pts',(10.6964592721647,-13.7060623220113,
118.718992292532));
#114017=CARTESIAN_POINT('Ctrl Pts',(11.262180675743,-14.109662558594,118.627127092461));
#114018=CARTESIAN_POINT('Ctrl Pts',(12.533969198827,-14.9027933258467,118.420336055715));
#114019=CARTESIAN_POINT('Ctrl Pts',(13.2463513125027,-15.2786458153057,
118.304355644959));
#114020=CARTESIAN_POINT('Ctrl Pts',(14.408983687951,-15.7884938562373,118.114134007312));
#114021=CARTESIAN_POINT('Ctrl Pts',(14.8429858589734,-15.9575118233424,
118.042872723305));
#114022=CARTESIAN_POINT('Ctrl Pts',(15.834430410622,-16.2964541964434,117.879851808611));
#114023=CARTESIAN_POINT('Ctrl Pts',(16.3947999294395,-16.4556862701782,
117.787577779365));
#114024=CARTESIAN_POINT('Ctrl Pts',(17.7647960824515,-16.7681638955507,
117.5621158453));
#114025=CARTESIAN_POINT('Ctrl Pts',(18.5796111634086,-16.8911468539739,
117.428162113254));
#114026=CARTESIAN_POINT('Ctrl Pts',(19.742825576758,-16.9789270540022,117.236892774666));
#114027=CARTESIAN_POINT('Ctrl Pts',(20.0863305029633,-16.9941127917336,
117.180394982505));
#114028=CARTESIAN_POINT('Ctrl Pts',(20.8687595384806,-17.0043128978382,
117.051551265545));
#114029=CARTESIAN_POINT('Ctrl Pts',(21.3075047500614,-16.9925873117754,
116.979157735974));
#114030=CARTESIAN_POINT('Ctrl Pts',(22.3314933276495,-16.9244202093205,
116.810165704712));
#114031=CARTESIAN_POINT('Ctrl Pts',(22.9152707581049,-16.8542132352159,
116.713819192822));
#114032=CARTESIAN_POINT('Ctrl Pts',(24.2166311841858,-16.626969122988,116.499475361948));
#114033=CARTESIAN_POINT('Ctrl Pts',(24.9301381832088,-16.4529756777154,
116.382273419367));
#114034=CARTESIAN_POINT('Ctrl Pts',(26.0117157534911,-16.111944864853,116.204986476976));
#114035=CARTESIAN_POINT('Ctrl Pts',(26.3889193678127,-15.9778624640433,
116.143221441321));
#114036=CARTESIAN_POINT('Ctrl Pts',(27.4525780934676,-15.5559612318494,
115.96902314246));
#114037=CARTESIAN_POINT('Ctrl Pts',(28.1253461728596,-15.2354433406124,
115.8586704274));
#114038=CARTESIAN_POINT('Ctrl Pts',(29.3671431107902,-14.5384840938646,
115.655739420418));
#114039=CARTESIAN_POINT('Ctrl Pts',(29.9389426923638,-14.1701502984732,
115.56265904247));
#114040=CARTESIAN_POINT('Ctrl Pts',(31.1382177033198,-13.2902733853208,
115.368530305677));
#114041=CARTESIAN_POINT('Ctrl Pts',(31.7545545940983,-12.7659684716934,
115.269514531316));
#114042=CARTESIAN_POINT('Ctrl Pts',(32.8030425974044,-11.7355072922184,
115.101672402844));
#114043=CARTESIAN_POINT('Ctrl Pts',(33.2473503334598,-11.2444095111543,
115.030665807847));
#114044=CARTESIAN_POINT('Ctrl Pts',(34.1157035321844,-10.1638523206168,
114.89303802056));
#114045=CARTESIAN_POINT('Ctrl Pts',(34.5331004292285,-9.57060514800458,
114.827612323976));
#114046=CARTESIAN_POINT('Ctrl Pts',(35.3429169625275,-8.2481290840788,114.702756888522));
#114047=CARTESIAN_POINT('Ctrl Pts',(35.7228201630239,-7.51321099309242,
114.645587234829));
#114048=CARTESIAN_POINT('Ctrl Pts',(36.2345314732538,-6.31885114286027,
114.570346560497));
#114049=CARTESIAN_POINT('Ctrl Pts',(36.4026661867263,-5.87679790201272,
114.545991015855));
#114050=CARTESIAN_POINT('Ctrl Pts',(36.7386620439605,-4.8703271861914,114.498562365834));
#114051=CARTESIAN_POINT('Ctrl Pts',(36.8962420959419,-4.30302893979826,
114.477304368902));
#114052=CARTESIAN_POINT('Ctrl Pts',(37.207245462913,-2.91072959494826,114.438617875259));
#114053=CARTESIAN_POINT('Ctrl Pts',(37.3301644725751,-2.08034584037984,
114.426721472385));
#114054=CARTESIAN_POINT('Ctrl Pts',(37.4178422211624,-0.90001140238114,
114.425114777429));
#114055=CARTESIAN_POINT('Ctrl Pts',(37.4330817608476,-0.555049444777654,
114.426461153991));
#114056=CARTESIAN_POINT('Ctrl Pts',(37.4472678076631,0.449246104619875,
114.435507171637));
#114057=CARTESIAN_POINT('Ctrl Pts',(37.4187635225561,1.108284042432,114.447795564935));
#114058=CARTESIAN_POINT('Ctrl Pts',(37.2802795982228,2.4817911040431,114.48756930671));
#114059=CARTESIAN_POINT('Ctrl Pts',(37.1629618698992,3.19418405315069,114.516367827871));
#114060=CARTESIAN_POINT('Ctrl Pts',(36.8166970857841,4.70042200423587,114.59526874833));
#114061=CARTESIAN_POINT('Ctrl Pts',(36.5745791108977,5.48923154181531,114.647748596065));
#114062=CARTESIAN_POINT('Ctrl Pts',(36.1067888181912,6.69578234672308,114.745176264061));
#114063=CARTESIAN_POINT('Ctrl Pts',(35.9186866220005,7.12721727996997,114.783620197467));
#114064=CARTESIAN_POINT('Ctrl Pts',(35.4566150813895,8.07790602254515,114.876901575129));
#114065=CARTESIAN_POINT('Ctrl Pts',(35.1732364169441,8.59175099873082,114.93340010801));
#114066=CARTESIAN_POINT('Ctrl Pts',(34.4256662182454,9.79592859903436,115.081344438067));
#114067=CARTESIAN_POINT('Ctrl Pts',(33.9364866331835,10.4683694410871,115.17734737897));
#114068=CARTESIAN_POINT('Ctrl Pts',(33.1782298465971,11.364102886918,115.324893274146));
#114069=CARTESIAN_POINT('Ctrl Pts',(32.9479882125162,11.6198018402333,115.369544650871));
#114070=CARTESIAN_POINT('Ctrl Pts',(32.4018327708539,12.1901923961905,115.475007335694));
#114071=CARTESIAN_POINT('Ctrl Pts',(32.0809814011665,12.4996467427407,115.53660638392));
#114072=CARTESIAN_POINT('Ctrl Pts',(31.3098433945328,13.1863187617331,115.684175017861));
#114073=CARTESIAN_POINT('Ctrl Pts',(30.8514325589148,13.5532197783405,115.771572094959));
#114074=CARTESIAN_POINT('Ctrl Pts',(29.7518229927019,14.3421697557263,115.980939691737));
#114075=CARTESIAN_POINT('Ctrl Pts',(29.0991589453022,14.7453853766348,116.105033475238));
#114076=CARTESIAN_POINT('Ctrl Pts',(28.0871520018169,15.277780253951,116.297041181183));
#114077=CARTESIAN_POINT('Ctrl Pts',(27.7468654774369,15.4422015372312,116.361529641027));
#114078=CARTESIAN_POINT('Ctrl Pts',(26.7683612233073,15.8743439342201,116.54657308316));
#114079=CARTESIAN_POINT('Ctrl Pts',(26.1188324460879,16.1137232616475,116.668838755098));
#114080=CARTESIAN_POINT('Ctrl Pts',(24.7922172442306,16.5100104461845,116.918422555183));
#114081=CARTESIAN_POINT('Ctrl Pts',(24.1163405762553,16.6662611877686,117.04553556975));
#114082=CARTESIAN_POINT('Ctrl Pts',(22.6337691523531,16.9116792603534,117.324602149443));
#114083=CARTESIAN_POINT('Ctrl Pts',(21.8262668366208,16.9846848324341,117.47676301644));
#114084=CARTESIAN_POINT('Ctrl Pts',(20.3085977417149,17.0093357039595,117.762159566835));
#114085=CARTESIAN_POINT('Ctrl Pts',(19.6004264523002,16.9750187446062,117.894949973447));
#114086=CARTESIAN_POINT('Ctrl Pts',(18.2159800951321,16.8178077503574,118.154839084414));
#114087=CARTESIAN_POINT('Ctrl Pts',(17.54073749996,16.6980293030593,118.281752438149));
#114088=CARTESIAN_POINT('Ctrl Pts',(16.0974956406338,16.3478780427604,118.55365975145));
#114089=CARTESIAN_POINT('Ctrl Pts',(15.3346814310107,16.1028393572611,118.697800747025));
#114090=CARTESIAN_POINT('Ctrl Pts',(13.9745337524518,15.5540667308777,118.954773074378));
#114091=CARTESIAN_POINT('Ctrl Pts',(13.3721674714921,15.2676722999989,119.06844030748));
#114092=CARTESIAN_POINT('Ctrl Pts',(12.1701191348142,14.604589514317,119.295882779618));
#114093=CARTESIAN_POINT('Ctrl Pts',(11.5738563299225,14.2242624331316,119.409072544891));
#114094=CARTESIAN_POINT('Ctrl Pts',(10.3375441029528,13.3202174924989,119.644955350538));
#114095=CARTESIAN_POINT('Ctrl Pts',(9.70830067517231,12.7844092305938,119.765808959591));
#114096=CARTESIAN_POINT('Ctrl Pts',(8.61944759326335,11.7091674408892,119.975589220271));
#114097=CARTESIAN_POINT('Ctrl Pts',(8.14956662736872,11.1831025683743,120.066253985677));
#114098=CARTESIAN_POINT('Ctrl Pts',(7.28355580932695,10.0819854007779,120.234654862375));
#114099=CARTESIAN_POINT('Ctrl Pts',(6.88731422728817,9.50877753106153,120.312411527511));
#114100=CARTESIAN_POINT('Ctrl Pts',(6.10903212580853,8.22015947760868,120.467106658173));
#114101=CARTESIAN_POINT('Ctrl Pts',(5.74046962270476,7.49834933045992,120.5417275053));
#114102=CARTESIAN_POINT('Ctrl Pts',(5.24083623071057,6.32021024263145,120.6446099079));
#114103=CARTESIAN_POINT('Ctrl Pts',(5.07527966788584,5.88040718534626,120.67906723405));
#114104=CARTESIAN_POINT('Ctrl Pts',(4.74350280728304,4.87570126780782,120.749366118117));
#114105=CARTESIAN_POINT('Ctrl Pts',(4.5878104871605,4.30782722835296,120.783353049156));
#114106=CARTESIAN_POINT('Ctrl Pts',(4.28282875510673,2.91945271640569,120.85323538363));
#114107=CARTESIAN_POINT('Ctrl Pts',(4.16337497561081,2.09370822520031,120.884019039261));
#114108=CARTESIAN_POINT('Ctrl Pts',(4.07930582718988,0.914935586217559,
120.912679619261));
#114109=CARTESIAN_POINT('Ctrl Pts',(4.06505102882361,0.566869786360458,
120.919264141611));
#114110=CARTESIAN_POINT('Ctrl Pts',(4.06054612858338,0.145722462032777,
120.92490224283));
#114111=CARTESIAN_POINT('Ctrl Pts',(4.06022763391727,0.0728596834798867,
120.925793376835));
#114112=CARTESIAN_POINT('Ctrl Pts',(4.06036979181167,1.50326513895498E-8,
120.926599594688));
#114113=CARTESIAN_POINT('Ctrl Pts',(4.00959443610706,-1.25170851643402E-8,
120.638638242996));
#114114=CARTESIAN_POINT('Ctrl Pts',(4.00941930028957,0.0897616374665513,
120.637644998799));
#114115=CARTESIAN_POINT('Ctrl Pts',(4.00994522096334,0.179531815916759,
120.63653358753));
#114116=CARTESIAN_POINT('Ctrl Pts',(4.02241319275843,1.09160129606617,120.624027713017));
#114117=CARTESIAN_POINT('Ctrl Pts',(4.09245406774986,1.91187325198813,120.602698061528));
#114118=CARTESIAN_POINT('Ctrl Pts',(4.32997148817351,3.41615195095139,120.543651401598));
#114119=CARTESIAN_POINT('Ctrl Pts',(4.48139080798906,4.10102192532192,120.508870155708));
#114120=CARTESIAN_POINT('Ctrl Pts',(4.86894595447833,5.45566394986278,120.424051461169));
#114121=CARTESIAN_POINT('Ctrl Pts',(5.10569304281492,6.1238361677535,120.373942172049));
#114122=CARTESIAN_POINT('Ctrl Pts',(5.53393200045323,7.12952847586363,120.286047843403));
#114123=CARTESIAN_POINT('Ctrl Pts',(5.69680707063255,7.4787675842911,120.253036441261));
#114124=CARTESIAN_POINT('Ctrl Pts',(6.21907007830176,8.5063951264318,120.148079606928));
#114125=CARTESIAN_POINT('Ctrl Pts',(6.61229879522507,9.16583718027728,120.070125792049));
#114126=CARTESIAN_POINT('Ctrl Pts',(7.38379765576326,10.2808484071456,119.918385020826));
#114127=CARTESIAN_POINT('Ctrl Pts',(7.74417176915716,10.7476537005959,119.847880703483));
#114128=CARTESIAN_POINT('Ctrl Pts',(8.41822736444313,11.5323419487485,119.716829141124));
#114129=CARTESIAN_POINT('Ctrl Pts',(8.72169523896559,11.8585311948728,119.658091568323));
#114130=CARTESIAN_POINT('Ctrl Pts',(9.28165636666735,12.4144326952983,119.550341446819));
#114131=CARTESIAN_POINT('Ctrl Pts',(9.53302405607704,12.6490968913906,119.502156238616));
#114132=CARTESIAN_POINT('Ctrl Pts',(10.4128789185094,13.4212897305271,119.333874211133));
#114133=CARTESIAN_POINT('Ctrl Pts',(11.0732209728882,13.9194267380072,119.208147069428));
#114134=CARTESIAN_POINT('Ctrl Pts',(12.2560288088416,14.6811166886917,118.983209706228));
#114135=CARTESIAN_POINT('Ctrl Pts',(12.7609433941091,14.9700149254131,118.887279820164));
#114136=CARTESIAN_POINT('Ctrl Pts',(13.6949513007292,15.4411687009317,118.710186284678));
#114137=CARTESIAN_POINT('Ctrl Pts',(14.1187151926111,15.6330014728069,118.629978501912));
#114138=CARTESIAN_POINT('Ctrl Pts',(15.2925990160622,16.1058440253134,118.408471012262));
#114139=CARTESIAN_POINT('Ctrl Pts',(16.055611923457,16.3504407701573,118.265042740636));
#114140=CARTESIAN_POINT('Ctrl Pts',(17.5028474371416,16.7007056529506,117.992792844911));
#114141=CARTESIAN_POINT('Ctrl Pts',(18.1820204468462,16.8205536260093,117.864958416257));
#114142=CARTESIAN_POINT('Ctrl Pts',(19.5598323485553,16.9752682547864,117.605528693718));
#114143=CARTESIAN_POINT('Ctrl Pts',(20.2572667455539,17.0088668144535,117.474177393979));
#114144=CARTESIAN_POINT('Ctrl Pts',(21.7741415562458,16.9852600946745,117.189265334446));
#114145=CARTESIAN_POINT('Ctrl Pts',(22.5915224717932,16.9111999146883,117.036039392438));
#114146=CARTESIAN_POINT('Ctrl Pts',(24.093168110406,16.6609389494782,116.753811883417));
#114147=CARTESIAN_POINT('Ctrl Pts',(24.7782503198109,16.5011163161582,116.62477315557));
#114148=CARTESIAN_POINT('Ctrl Pts',(26.0904043329047,16.104997532903,116.377133536012));
#114149=CARTESIAN_POINT('Ctrl Pts',(26.7174905868263,15.873336267133,116.258576530814));
#114150=CARTESIAN_POINT('Ctrl Pts',(28.0734795149186,15.2767865408782,116.002484637455));
#114151=CARTESIAN_POINT('Ctrl Pts',(28.7932354201816,14.8947128644818,115.86655500571));
#114152=CARTESIAN_POINT('Ctrl Pts',(30.0811344098328,14.0845853304245,115.622083128316));
#114153=CARTESIAN_POINT('Ctrl Pts',(30.6554519075947,13.6701016283902,115.512550630566));
#114154=CARTESIAN_POINT('Ctrl Pts',(31.7157604337614,12.7973756534496,115.309356867423));
#114155=CARTESIAN_POINT('Ctrl Pts',(32.2040772124031,12.3441134431078,115.215330091604));
#114156=CARTESIAN_POINT('Ctrl Pts',(32.9043392884413,11.612143294737,115.080290415224));
#114157=CARTESIAN_POINT('Ctrl Pts',(33.1362928032818,11.3542166814392,115.035501283874));
#114158=CARTESIAN_POINT('Ctrl Pts',(33.8929474327213,10.4587984692788,114.888957473996));
#114159=CARTESIAN_POINT('Ctrl Pts',(34.3793648001977,9.78944551919494,114.793937144242));
#114160=CARTESIAN_POINT('Ctrl Pts',(35.1247318148005,8.58818303815335,114.646169202786));
#114161=CARTESIAN_POINT('Ctrl Pts',(35.4081786357093,8.07378631833508,114.589283864809));
#114162=CARTESIAN_POINT('Ctrl Pts',(35.8692721662685,7.12416271301863,114.495592266303));
#114163=CARTESIAN_POINT('Ctrl Pts',(36.0565242320879,6.69443153578555,114.457108069221));
#114164=CARTESIAN_POINT('Ctrl Pts',(36.5191404407503,5.50143785511238,114.36103444054));
#114165=CARTESIAN_POINT('Ctrl Pts',(36.7585332602379,4.72505075855716,114.30993383552));
#114166=CARTESIAN_POINT('Ctrl Pts',(37.1005710479695,3.25254145824192,114.232560306386));
#114167=CARTESIAN_POINT('Ctrl Pts',(37.2172154447346,2.56156820931256,114.203915819025));
#114168=CARTESIAN_POINT('Ctrl Pts',(37.3668078416288,1.15951241881491,114.161052857355));
#114169=CARTESIAN_POINT('Ctrl Pts',(37.3984771000427,0.449654850245953,
114.147091391248));
#114170=CARTESIAN_POINT('Ctrl Pts',(37.3722207529235,-1.09396235525398,
114.134271572704));
#114171=CARTESIAN_POINT('Ctrl Pts',(37.297702358504,-1.92563455369374,114.138310420694));
#114172=CARTESIAN_POINT('Ctrl Pts',(37.0481456529654,-3.45388030596479,
114.164862247004));
#114173=CARTESIAN_POINT('Ctrl Pts',(36.8892313015764,-4.15126057687536,
114.184639028468));
#114174=CARTESIAN_POINT('Ctrl Pts',(36.4963490562346,-5.48605687675346,
114.237647904344));
#114175=CARTESIAN_POINT('Ctrl Pts',(36.2670725075451,-6.12351678490518,
114.270099446789));
#114176=CARTESIAN_POINT('Ctrl Pts',(35.6816057623652,-7.49201423894137,
114.356478426261));
#114177=CARTESIAN_POINT('Ctrl Pts',(35.309918173823,-8.21444541962333,114.413124686832));
#114178=CARTESIAN_POINT('Ctrl Pts',(34.5272657296374,-9.50155972380706,
114.534094029113));
#114179=CARTESIAN_POINT('Ctrl Pts',(34.130121517857,-10.072849712436,114.596078870479));
#114180=CARTESIAN_POINT('Ctrl Pts',(33.2567246534963,-11.1781883092315,
114.733542630841));
#114181=CARTESIAN_POINT('Ctrl Pts',(32.7794288768618,-11.7096249860511,
114.809234167398));
#114182=CARTESIAN_POINT('Ctrl Pts',(31.6935580895123,-12.7750858369867,
114.983400478659));
#114183=CARTESIAN_POINT('Ctrl Pts',(31.0773355552952,-13.2985586939205,
115.083171767844));
#114184=CARTESIAN_POINT('Ctrl Pts',(29.8743613895649,-14.1798125471617,
115.278357715051));
#114185=CARTESIAN_POINT('Ctrl Pts',(29.298425482713,-14.5498604120333,115.371968236492));
#114186=CARTESIAN_POINT('Ctrl Pts',(28.0625214018881,-15.2409386847464,
115.573199682369));
#114187=CARTESIAN_POINT('Ctrl Pts',(27.4008044647638,-15.5557999556707,
115.6811530664));
#114188=CARTESIAN_POINT('Ctrl Pts',(26.3541034903535,-15.9718380084046,
115.852858291872));
#114189=CARTESIAN_POINT('Ctrl Pts',(25.9822179651935,-16.1045424611203,
115.914001383399));
#114190=CARTESIAN_POINT('Ctrl Pts',(24.8988200925056,-16.4481814905653,
116.092242525465));
#114191=CARTESIAN_POINT('Ctrl Pts',(24.1776960641974,-16.6247725812183,
116.210989886834));
#114192=CARTESIAN_POINT('Ctrl Pts',(22.8690593008678,-16.8535855084627,
116.426244432939));
#114193=CARTESIAN_POINT('Ctrl Pts',(22.2858720973622,-16.9238823077358,
116.522099685318));
#114194=CARTESIAN_POINT('Ctrl Pts',(21.2608407091994,-16.9924661098353,
116.690663287622));
#114195=CARTESIAN_POINT('Ctrl Pts',(20.8204508694921,-17.0043221651928,
116.763123114258));
#114196=CARTESIAN_POINT('Ctrl Pts',(20.036746452358,-16.9941460515523,116.892321026314));
#114197=CARTESIAN_POINT('Ctrl Pts',(19.6935856990506,-16.979001773077,116.948957606962));
#114198=CARTESIAN_POINT('Ctrl Pts',(18.5303243083283,-16.8913361586865,
117.140937191185));
#114199=CARTESIAN_POINT('Ctrl Pts',(17.7151179108909,-16.7683375808488,
117.275402802738));
#114200=CARTESIAN_POINT('Ctrl Pts',(16.3446787257858,-16.4558041489712,
117.500684601443));
#114201=CARTESIAN_POINT('Ctrl Pts',(15.7843002396079,-16.2966055065796,
117.592592357442));
#114202=CARTESIAN_POINT('Ctrl Pts',(14.7926010507014,-15.9576504725585,
117.755058380267));
#114203=CARTESIAN_POINT('Ctrl Pts',(14.3583603041696,-15.7885620302798,
117.82614752501));
#114204=CARTESIAN_POINT('Ctrl Pts',(13.1827235176851,-15.2729862389073,
118.018773325584));
#114205=CARTESIAN_POINT('Ctrl Pts',(12.4584699152919,-14.8896318770529,
118.137441055054));
#114206=CARTESIAN_POINT('Ctrl Pts',(11.1567694101241,-14.0732459290973,
118.349467910793));
#114207=CARTESIAN_POINT('Ctrl Pts',(10.5735987631925,-13.6531402431575,
118.44393147152));
#114208=CARTESIAN_POINT('Ctrl Pts',(9.51717859125105,-12.7842820492166,
118.614085566742));
#114209=CARTESIAN_POINT('Ctrl Pts',(9.03963203754324,-12.3429421777055,
118.690583911227));
#114210=CARTESIAN_POINT('Ctrl Pts',(8.35137225178435,-11.6289947435209,
118.800645361808));
#114211=CARTESIAN_POINT('Ctrl Pts',(8.12178136911124,-11.3759359997991,
118.837304741581));
#114212=CARTESIAN_POINT('Ctrl Pts',(7.34610584542342,-10.4672517649577,
118.960731741905));
#114213=CARTESIAN_POINT('Ctrl Pts',(6.84144120640024,-9.77700645242168,
119.04018367225));
#114214=CARTESIAN_POINT('Ctrl Pts',(6.07626521479113,-8.54633206248309,
119.158377721677));
#114215=CARTESIAN_POINT('Ctrl Pts',(5.7887332234669,-8.02512483548903,119.202085921422));
#114216=CARTESIAN_POINT('Ctrl Pts',(5.33194267538356,-7.08433436660324,
119.2703842278));
#114217=CARTESIAN_POINT('Ctrl Pts',(5.15110109479715,-6.67117922278847,
119.297027606815));
#114218=CARTESIAN_POINT('Ctrl Pts',(4.84876516523162,-5.89891988503616,
119.340953402027));
#114219=CARTESIAN_POINT('Ctrl Pts',(4.72248360426319,-5.54204249120961,
119.359012018623));
#114220=CARTESIAN_POINT('Ctrl Pts',(4.42063356141633,-4.59024170670288,
119.401126195762));
#114221=CARTESIAN_POINT('Ctrl Pts',(4.26521846397487,-3.9893706433944,119.421616823222));
#114222=CARTESIAN_POINT('Ctrl Pts',(4.04000962269131,-2.87370222757645,
119.448350331979));
#114223=CARTESIAN_POINT('Ctrl Pts',(3.9604302776283,-2.36168632455117,119.456378260556));
#114224=CARTESIAN_POINT('Ctrl Pts',(3.90398359427621,-1.84682113605508,
119.46027723156));
#114225=CARTESIAN_POINT('Origin',(-15.0675364833309,-75.,72.98888938658));
#114226=CARTESIAN_POINT('',(-15.5675364832709,-84.9916953137207,73.3961602849894));
#114227=CARTESIAN_POINT('Origin',(-15.5675364832709,-75.,72.98888938658));
#114228=CARTESIAN_POINT('',(-15.0675364833309,-84.4921179126434,73.3757970402573));
#114229=CARTESIAN_POINT('Origin',(-15.0675364833309,-84.9917030659404,73.3961606009772));
#114230=CARTESIAN_POINT('',(-15.0675364833309,-65.5,72.98888938658));
#114231=CARTESIAN_POINT('Origin',(-15.0675364833309,-75.,72.98888938658));
#114232=CARTESIAN_POINT('Origin',(-15.0675364833309,-75.,72.98888938658));
#114233=CARTESIAN_POINT('Origin',(-15.9175364833309,-75.,72.98888938658));
#114234=CARTESIAN_POINT('',(-13.5675364833309,-65.5,72.98888938658));
#114235=CARTESIAN_POINT('',(-15.9175364833309,-65.5,72.98888938658));
#114236=CARTESIAN_POINT('Origin',(-13.5675364833309,-75.,72.98888938658));
#114237=CARTESIAN_POINT('Origin',(-13.2677182305224,-75.,72.98888938658));
#114238=CARTESIAN_POINT('',(-13.2266934083678,-66.3412177685878,72.9890206473583));
#114239=CARTESIAN_POINT('',(-13.5675364833309,-80.6547445743814,66.0025908482903));
#114240=CARTESIAN_POINT('Ctrl Pts',(-13.2266934083678,-66.3412177685878,
72.9890206473583));
#114241=CARTESIAN_POINT('Ctrl Pts',(-13.2407667008042,-66.3271326547269,
72.1690325463416));
#114242=CARTESIAN_POINT('Ctrl Pts',(-13.2550858955079,-66.4295793336072,
71.3495943325524));
#114243=CARTESIAN_POINT('Ctrl Pts',(-13.2840611221687,-66.8589654028222,
69.7699075933991));
#114244=CARTESIAN_POINT('Ctrl Pts',(-13.2977088950612,-67.1832493356237,
69.0176462295908));
#114245=CARTESIAN_POINT('Ctrl Pts',(-13.3212649090564,-67.8955624618356,
67.8450674617599));
#114246=CARTESIAN_POINT('Ctrl Pts',(-13.3310562007338,-68.2300949998944,
67.3967683499587));
#114247=CARTESIAN_POINT('Ctrl Pts',(-13.3606234486437,-69.3599797236658,
66.1502763569408));
#114248=CARTESIAN_POINT('Ctrl Pts',(-13.3788394562794,-70.2685176026843,
65.4723217468462));
#114249=CARTESIAN_POINT('Ctrl Pts',(-13.4083143132994,-71.7995141325709,
64.7275913681621));
#114250=CARTESIAN_POINT('Ctrl Pts',(-13.4186276870038,-72.3482377586366,
64.5246133683743));
#114251=CARTESIAN_POINT('Ctrl Pts',(-13.4386174214408,-73.4695109564809,
64.232333269707));
#114252=CARTESIAN_POINT('Ctrl Pts',(-13.4484368516908,-74.0392487572431,
64.1418028503483));
#114253=CARTESIAN_POINT('Ctrl Pts',(-13.4742869329458,-75.5285911817388,
64.051052323433));
#114254=CARTESIAN_POINT('Ctrl Pts',(-13.4928531712087,-76.5958501455569,
64.1271300649806));
#114255=CARTESIAN_POINT('Ctrl Pts',(-13.5251748522153,-78.7941276658468,
64.7998965188398));
#114256=CARTESIAN_POINT('Ctrl Pts',(-13.5399964381131,-79.784891548598,
65.3190823617296));
#114257=CARTESIAN_POINT('Ctrl Pts',(-13.5590282940972,-80.6565021394416,
66.0000474243114));
#114258=CARTESIAN_POINT('Ctrl Pts',(-12.9675119086199,-76.1752581060379,
81.3058749742284));
#114259=CARTESIAN_POINT('Ctrl Pts',(-12.9761555362729,-75.7054160823964,
81.3809966173537));
#114260=CARTESIAN_POINT('Ctrl Pts',(-12.984944367006,-75.2297319433566,
81.4162357955362));
#114261=CARTESIAN_POINT('Ctrl Pts',(-13.0018977558637,-74.2930269577767,
81.4058301185759));
#114262=CARTESIAN_POINT('Ctrl Pts',(-13.0099327739343,-73.8336256353453,
81.3626055539312));
#114263=CARTESIAN_POINT('Ctrl Pts',(-13.034703878876,-72.4494579405428,
81.1175572774556));
#114264=CARTESIAN_POINT('Ctrl Pts',(-13.0521103372511,-71.5497303411989,
80.7973636804612));
#114265=CARTESIAN_POINT('Ctrl Pts',(-13.0786991340095,-70.2436949188266,
80.067967843619));
#114266=CARTESIAN_POINT('Ctrl Pts',(-13.0881440974825,-69.7906308676622,
79.7534393148135));
#114267=CARTESIAN_POINT('Ctrl Pts',(-13.1078514587778,-68.9366818033151,
79.0296821594344));
#114268=CARTESIAN_POINT('Ctrl Pts',(-13.1181095048179,-68.5395865522349,
78.6185751098584));
#114269=CARTESIAN_POINT('Ctrl Pts',(-13.14503423917,-67.6118538973413,77.4433982113719));
#114270=CARTESIAN_POINT('Ctrl Pts',(-13.1606202152678,-67.1609530319177,
76.6272467528462));
#114271=CARTESIAN_POINT('Ctrl Pts',(-13.1935425350349,-66.5290168126367,
74.8691112225869));
#114272=CARTESIAN_POINT('Ctrl Pts',(-13.2104360376322,-66.3574887953517,
73.9362652681327));
#114273=CARTESIAN_POINT('Ctrl Pts',(-13.2266934083678,-66.3412177685878,
72.9890206473583));
#114274=CARTESIAN_POINT('',(-13.2736619003202,-83.7052176583754,72.9888947630294));
#114275=CARTESIAN_POINT('Ctrl Pts',(-13.2736619003202,-83.7052176583754,
72.9888947630294));
#114276=CARTESIAN_POINT('Ctrl Pts',(-13.2229688258284,-83.6545977325295,
72.2041789688224));
#114277=CARTESIAN_POINT('Ctrl Pts',(-13.1720553132674,-83.4982142737105,
71.4337103090239));
#114278=CARTESIAN_POINT('Ctrl Pts',(-13.0702284178419,-82.9868581475011,
69.9759204830989));
#114279=CARTESIAN_POINT('Ctrl Pts',(-13.0193150349773,-82.6340458634663,
69.2881849289806));
#114280=CARTESIAN_POINT('Ctrl Pts',(-12.9679003706341,-82.2015397612608,
68.6647904662762));
#114281=CARTESIAN_POINT('',(-13.5669824724428,-82.8099251083261,77.459681895839));
#114282=CARTESIAN_POINT('Ctrl Pts',(-13.5669824724428,-82.8099251083261,
77.459681895839));
#114283=CARTESIAN_POINT('Ctrl Pts',(-13.5187525677101,-83.1543720959849,
76.7599043053519));
#114284=CARTESIAN_POINT('Ctrl Pts',(-13.4698907813316,-83.4052651158459,
76.0216902016215));
#114285=CARTESIAN_POINT('Ctrl Pts',(-13.3719801094319,-83.7042558727909,
74.5139171860312));
#114286=CARTESIAN_POINT('Ctrl Pts',(-13.3229312239106,-83.753373874782,
73.7448830644764));
#114287=CARTESIAN_POINT('Ctrl Pts',(-13.2736619003202,-83.7052176583754,
72.9888947630294));
#114288=CARTESIAN_POINT('Origin',(-13.5675364833309,-75.,72.98888938658));
#114289=CARTESIAN_POINT('Origin',(-15.9175364833309,-75.,72.98888938658));
#114290=CARTESIAN_POINT('',(-11.126080082656,-83.3999999999947,72.9888988113144));
#114291=CARTESIAN_POINT('Ctrl Pts',(-11.8763230992193,-66.6,72.98888938658));
#114292=CARTESIAN_POINT('Ctrl Pts',(-11.8631868209786,-66.6,73.4447625248225));
#114293=CARTESIAN_POINT('Ctrl Pts',(-11.8499323085124,-66.6371108146397,
73.9000553019549));
#114294=CARTESIAN_POINT('Ctrl Pts',(-11.8215505215453,-66.7982238465426,
74.8810309345825));
#114295=CARTESIAN_POINT('Ctrl Pts',(-11.8066118707031,-66.9361797585604,
75.4022143669236));
#114296=CARTESIAN_POINT('Ctrl Pts',(-11.7608748863597,-67.5043835959706,
76.9361908756775));
#114297=CARTESIAN_POINT('Ctrl Pts',(-11.7286576515623,-68.0839240829853,
77.8810612875392));
#114298=CARTESIAN_POINT('Ctrl Pts',(-11.6830410476023,-69.1896027373828,
79.0783996027313));
#114299=CARTESIAN_POINT('Ctrl Pts',(-11.6683360173514,-69.5866997778602,
79.4339675737516));
#114300=CARTESIAN_POINT('Ctrl Pts',(-11.6388063150206,-70.412644761118,
80.0430072438156));
#114301=CARTESIAN_POINT('Ctrl Pts',(-11.6244218669597,-70.8356745762694,
80.3007161607582));
#114302=CARTESIAN_POINT('Ctrl Pts',(-11.5952332387126,-71.7533765643096,
80.754166157821));
#114303=CARTESIAN_POINT('Ctrl Pts',(-11.5805467836055,-72.2489414458553,
80.9432445269332));
#114304=CARTESIAN_POINT('Ctrl Pts',(-11.5350826929847,-73.8155100562091,
81.3769013847141));
#114305=CARTESIAN_POINT('Ctrl Pts',(-11.5029132423661,-74.9191184248915,
81.4597345425669));
#114306=CARTESIAN_POINT('Ctrl Pts',(-11.4573495157567,-76.5357040014433,
81.2644397908755));
#114307=CARTESIAN_POINT('Ctrl Pts',(-11.4426237633509,-77.0566866345932,
81.1505780668194));
#114308=CARTESIAN_POINT('Ctrl Pts',(-11.412347381053,-78.0581362354934,
80.8296613001395));
#114309=CARTESIAN_POINT('Ctrl Pts',(-11.3972392495797,-78.5371113108017,
80.6255613125404));
#114310=CARTESIAN_POINT('Ctrl Pts',(-11.3676835224782,-79.4510244581362,
80.1315843948107));
#114311=CARTESIAN_POINT('Ctrl Pts',(-11.3532974583416,-79.8840076862191,
79.8428064851497));
#114312=CARTESIAN_POINT('Ctrl Pts',(-11.3082195679676,-81.1349701187117,
78.8293990833468));
#114313=CARTESIAN_POINT('Ctrl Pts',(-11.2762215280228,-81.8406359595486,
77.9843984850121));
#114314=CARTESIAN_POINT('Ctrl Pts',(-11.2359873168664,-82.5324799639801,
76.7229153250283));
#114315=CARTESIAN_POINT('Ctrl Pts',(-11.2263351879566,-82.6807503593282,
76.4075549821276));
#114316=CARTESIAN_POINT('Ctrl Pts',(-11.1865296948425,-83.199466595355,
75.0987856006205));
#114317=CARTESIAN_POINT('Ctrl Pts',(-11.1556542565268,-83.3999988110041,
74.0486126652872));
#114318=CARTESIAN_POINT('Ctrl Pts',(-11.126080082656,-83.3999999999947,
72.9888988113141));
#114319=CARTESIAN_POINT('',(-10.4867014633236,-67.603277897842,69.0114834762033));
#114320=CARTESIAN_POINT('Ctrl Pts',(-11.126080082656,-83.3999999999947,
72.9888988113144));
#114321=CARTESIAN_POINT('Ctrl Pts',(-11.1145413077361,-83.400000463896,
72.5754367246302));
#114322=CARTESIAN_POINT('Ctrl Pts',(-11.1030084942769,-83.3694748842814,
72.1625474232924));
#114323=CARTESIAN_POINT('Ctrl Pts',(-11.0793359541153,-83.2483598295159,
71.3479290463103));
#114324=CARTESIAN_POINT('Ctrl Pts',(-11.0674086818258,-83.1584221870653,
70.9472376975009));
#114325=CARTESIAN_POINT('Ctrl Pts',(-11.0345838926802,-82.8268542747668,
69.8521348082208));
#114326=CARTESIAN_POINT('Ctrl Pts',(-11.014410632469,-82.5229520442308,
69.1804710740507));
#114327=CARTESIAN_POINT('Ctrl Pts',(-10.9795609202248,-81.8709899141359,
68.1307930177543));
#114328=CARTESIAN_POINT('Ctrl Pts',(-10.9649269598758,-81.5687066565817,
67.7292622960216));
#114329=CARTESIAN_POINT('Ctrl Pts',(-10.9187102026195,-80.4937138906786,
66.5396188829876));
#114330=CARTESIAN_POINT('Ctrl Pts',(-10.8890682820479,-79.6013444988769,
65.8754091418893));
#114331=CARTESIAN_POINT('Ctrl Pts',(-10.8411103417265,-78.1075663202381,
65.1653414135114));
#114332=CARTESIAN_POINT('Ctrl Pts',(-10.8250822942596,-77.5867180388744,
64.9780354390374));
#114333=CARTESIAN_POINT('Ctrl Pts',(-10.7937856070089,-76.5139839988153,
64.7078973259577));
#114334=CARTESIAN_POINT('Ctrl Pts',(-10.7785899986975,-75.9646383727142,
64.6260880741254));
#114335=CARTESIAN_POINT('Ctrl Pts',(-10.7503632792826,-74.9562112953451,
64.5766577258682));
#114336=CARTESIAN_POINT('Ctrl Pts',(-10.7374549491415,-74.5001098436499,
64.5914093172152));
#114337=CARTESIAN_POINT('Ctrl Pts',(-10.7021819967178,-73.2498417520493,
64.7341073150666));
#114338=CARTESIAN_POINT('Ctrl Pts',(-10.6806528480035,-72.4694504792138,
64.9390080019671));
#114339=CARTESIAN_POINT('Ctrl Pts',(-10.6450022581522,-71.3823104846934,
65.3984426740841));
#114340=CARTESIAN_POINT('Ctrl Pts',(-10.6327525993254,-71.044869025316,
65.568684875407));
#114341=CARTESIAN_POINT('Ctrl Pts',(-10.5965655968264,-70.1050628211244,
66.1251860093398));
#114342=CARTESIAN_POINT('Ctrl Pts',(-10.5724815457644,-69.5389935191861,
66.566396987944));
#114343=CARTESIAN_POINT('Ctrl Pts',(-10.543113335062,-68.8576878872331,
67.2533980030717));
#114344=CARTESIAN_POINT('Ctrl Pts',(-10.5357245337686,-68.6879271709305,
67.4407721722845));
#114345=CARTESIAN_POINT('Ctrl Pts',(-10.5208890369568,-68.3512272796966,
67.8478997193744));
#114346=CARTESIAN_POINT('Ctrl Pts',(-10.5135077658083,-68.1861425191738,
68.0687970134825));
#114347=CARTESIAN_POINT('Ctrl Pts',(-10.4992635891988,-67.8770180063945,
68.5279098299338));
#114348=CARTESIAN_POINT('Ctrl Pts',(-10.4924139281037,-67.733356462548,
68.765962978087));
#114349=CARTESIAN_POINT('Ctrl Pts',(-10.4857110114799,-67.6017555331481,
69.0107015065655));
#114350=CARTESIAN_POINT('Ctrl Pts',(-10.493482781736,-67.6016578275035,
69.0108832153103));
#114351=CARTESIAN_POINT('Ctrl Pts',(-10.4734285229243,-67.2741720795565,
69.61994502055));
#114352=CARTESIAN_POINT('Ctrl Pts',(-10.4540474308237,-67.0231417279012,
70.2671297790049));
#114353=CARTESIAN_POINT('Ctrl Pts',(-10.4253085028645,-66.7701553475053,
71.27181739424));
#114354=CARTESIAN_POINT('Ctrl Pts',(-10.415775127276,-66.7066657642059,
71.6107443794165));
#114355=CARTESIAN_POINT('Ctrl Pts',(-10.3960457754692,-66.6214302894955,
72.2963768901155));
#114356=CARTESIAN_POINT('Ctrl Pts',(-10.3859052190887,-66.600000722933,
72.6424592454741));
#114357=CARTESIAN_POINT('Ctrl Pts',(-10.375811919862,-66.6000000000183,
72.9888718569527));
#114358=CARTESIAN_POINT('Ctrl Pts',(-10.8470411184476,-66.6,72.98888938658));
#114359=CARTESIAN_POINT('Ctrl Pts',(-10.8664020390562,-66.6,72.2994004757708));
#114360=CARTESIAN_POINT('Ctrl Pts',(-10.8868168182513,-66.6848932300671,
71.6119769486083));
#114361=CARTESIAN_POINT('Ctrl Pts',(-10.9317844969506,-67.0668102088584,
70.0917430958867));
#114362=CARTESIAN_POINT('Ctrl Pts',(-10.9552891277897,-67.4123212964733,
69.2799741823665));
#114363=CARTESIAN_POINT('Ctrl Pts',(-10.9944756820166,-68.1382837038421,
68.1186106133782));
#114364=CARTESIAN_POINT('Ctrl Pts',(-11.0089562329978,-68.4357035076209,
67.7245961283561));
#114365=CARTESIAN_POINT('Ctrl Pts',(-11.0553589070755,-69.5146785268516,
66.5298471320123));
#114366=CARTESIAN_POINT('Ctrl Pts',(-11.0850904667867,-70.4213205268241,
65.8584153852941));
#114367=CARTESIAN_POINT('Ctrl Pts',(-11.1329935679342,-71.9148752194113,
65.1578197079955));
#114368=CARTESIAN_POINT('Ctrl Pts',(-11.1484859650805,-72.4174783128085,
64.9780062826356));
#114369=CARTESIAN_POINT('Ctrl Pts',(-11.185933772976,-73.6985502883669,
64.6528906424635));
#114370=CARTESIAN_POINT('Ctrl Pts',(-11.2071539018874,-74.4869117255284,
64.5675243442591));
#114371=CARTESIAN_POINT('Ctrl Pts',(-11.2490784262655,-75.9408195094156,
64.6152465065459));
#114372=CARTESIAN_POINT('Ctrl Pts',(-11.2685950087625,-76.6011304134222,
64.7160749359359));
#114373=CARTESIAN_POINT('Ctrl Pts',(-11.3098734880201,-78.0075842524421,
65.1057089617123));
#114374=CARTESIAN_POINT('Ctrl Pts',(-11.3312503612692,-78.738651161473,
65.4249889856119));
#114375=CARTESIAN_POINT('Ctrl Pts',(-11.3763508683028,-80.0670110840061,
66.2454139502382));
#114376=CARTESIAN_POINT('Ctrl Pts',(-11.3987245609227,-80.6616947373075,
66.7363422965288));
#114377=CARTESIAN_POINT('Ctrl Pts',(-11.4339822674988,-81.5141144062874,
67.6627512081687));
#114378=CARTESIAN_POINT('Ctrl Pts',(-11.4474218230183,-81.8144462479833,
68.0528236096077));
#114379=CARTESIAN_POINT('Ctrl Pts',(-11.47559604091,-82.3515738740102,68.8936705988461));
#114380=CARTESIAN_POINT('Ctrl Pts',(-11.4904764804107,-82.5850359761253,
69.3442130163506));
#114381=CARTESIAN_POINT('Ctrl Pts',(-11.5369186379525,-83.1914900094629,
70.8291880812308));
#114382=CARTESIAN_POINT('Ctrl Pts',(-11.5661250213123,-83.4033109990622,
71.9168916413994));
#114383=CARTESIAN_POINT('Ctrl Pts',(-11.6191785733491,-83.3977024566762,
73.7544760260515));
#114384=CARTESIAN_POINT('Ctrl Pts',(-11.6407895058686,-83.2976786974849,
74.4909279410523));
#114385=CARTESIAN_POINT('Ctrl Pts',(-11.6744017058846,-82.9818552469437,
75.6457821548017));
#114386=CARTESIAN_POINT('Ctrl Pts',(-11.6869510695521,-82.8254210531336,
76.0762625537984));
#114387=CARTESIAN_POINT('Ctrl Pts',(-11.7202337039545,-82.3299737799591,
77.1560894029684));
#114388=CARTESIAN_POINT('Ctrl Pts',(-11.7418620756503,-81.9398414717581,
77.7776918925204));
#114389=CARTESIAN_POINT('Ctrl Pts',(-11.7872345369775,-80.9307048601188,
78.9984197023975));
#114390=CARTESIAN_POINT('Ctrl Pts',(-11.8101222335905,-80.2902003889862,
79.5692736077059));
#114391=CARTESIAN_POINT('Ctrl Pts',(-11.8482492964135,-79.1717122804874,
80.2955831476102));
#114392=CARTESIAN_POINT('Ctrl Pts',(-11.8623691819322,-78.7469382818944,
80.5222429012281));
#114393=CARTESIAN_POINT('Ctrl Pts',(-11.9084582056147,-77.2786902849668,
81.15063602866));
#114394=CARTESIAN_POINT('Ctrl Pts',(-11.9381487200623,-76.1749276675997,
81.3809138810878));
#114395=CARTESIAN_POINT('Ctrl Pts',(-11.9859193414545,-74.5285305330077,
81.3923749598895));
#114396=CARTESIAN_POINT('Ctrl Pts',(-12.0013614799584,-73.9994141424513,
81.3459043724441));
#114397=CARTESIAN_POINT('Ctrl Pts',(-12.0387800059918,-72.7029438625803,
81.107076853382));
#114398=CARTESIAN_POINT('Ctrl Pts',(-12.059962771865,-71.9516445122256,
80.8558430660798));
#114399=CARTESIAN_POINT('Ctrl Pts',(-12.0982159586963,-70.7615118930262,
80.2613730281013));
#114400=CARTESIAN_POINT('Ctrl Pts',(-12.1141384355232,-70.3011839779977,
79.9727953493084));
#114401=CARTESIAN_POINT('Ctrl Pts',(-12.1538537839071,-69.2025439911863,
79.125963032737));
#114402=CARTESIAN_POINT('Ctrl Pts',(-12.1765336606602,-68.6149100195654,
78.5120005903277));
#114403=CARTESIAN_POINT('Ctrl Pts',(-12.2143675660734,-67.8535751690471,
77.4293358979771));
#114404=CARTESIAN_POINT('Ctrl Pts',(-12.2284252541423,-67.612283742812,
77.0151290640062));
#114405=CARTESIAN_POINT('Ctrl Pts',(-12.2600783049814,-67.1431213608927,
76.0239401130097));
#114406=CARTESIAN_POINT('Ctrl Pts',(-12.2773381972661,-66.9411455127516,
75.4377574575907));
#114407=CARTESIAN_POINT('Ctrl Pts',(-12.3030381220826,-66.7377227431684,
74.5346543764784));
#114408=CARTESIAN_POINT('Ctrl Pts',(-12.3115670151115,-66.6866649432039,
74.2310937593356));
#114409=CARTESIAN_POINT('Ctrl Pts',(-12.3292273729659,-66.6174842077814,
73.6144624987546));
#114410=CARTESIAN_POINT('Ctrl Pts',(-12.3383399852619,-66.6000004824736,
73.3018086558167));
#114411=CARTESIAN_POINT('Ctrl Pts',(-12.3474397125752,-66.60000000001,72.9889023383631));
#114412=CARTESIAN_POINT('Origin',(-15.5675364833309,-75.,72.98888938658));
#114413=CARTESIAN_POINT('',(-8.69331175948402,-74.9999999935748,84.9888491626601));
#114414=CARTESIAN_POINT('',(-10.0948640593367,-81.4411229981149,83.1137069660509));
#114415=CARTESIAN_POINT('Ctrl Pts',(-8.69331176731091,-74.99999999459,84.98885921934));
#114416=CARTESIAN_POINT('Ctrl Pts',(-8.69350218303866,-75.3399348100396,
84.98888938658));
#114417=CARTESIAN_POINT('Ctrl Pts',(-8.70999107237271,-75.6865565005233,
84.9744403650337));
#114418=CARTESIAN_POINT('Ctrl Pts',(-8.75917211678321,-76.2144573664476,
84.9285833243014));
#114419=CARTESIAN_POINT('Ctrl Pts',(-8.77964041665495,-76.3917477453332,
84.9092679071993));
#114420=CARTESIAN_POINT('Ctrl Pts',(-8.81645479406493,-76.6593680378655,
84.8739469876302));
#114421=CARTESIAN_POINT('Ctrl Pts',(-8.83638996467051,-76.7935989129425,
84.8546997132077));
#114422=CARTESIAN_POINT('Ctrl Pts',(-8.86232163203638,-76.9508673416978,
84.8294029000445));
#114423=CARTESIAN_POINT('Ctrl Pts',(-8.87692983821257,-77.0352867737512,
84.8150813510417));
#114424=CARTESIAN_POINT('Ctrl Pts',(-8.8839419779519,-77.0747270242531,
84.808187280968));
#114425=CARTESIAN_POINT('Ctrl Pts',(-8.88799666438019,-77.0972749617629,
84.8041960057921));
#114426=CARTESIAN_POINT('Ctrl Pts',(-8.88930142930253,-77.1044975230504,
84.8029110191365));
#114427=CARTESIAN_POINT('Ctrl Pts',(-8.93704494657942,-77.3680116340577,
84.7558764741991));
#114428=CARTESIAN_POINT('Ctrl Pts',(-8.996315423307,-77.646861748394,84.6973356957918));
#114429=CARTESIAN_POINT('Ctrl Pts',(-9.10361335105004,-78.091735186163,
84.584775362276));
#114430=CARTESIAN_POINT('Ctrl Pts',(-9.14244469573966,-78.2444478463605,
84.5431227555126));
#114431=CARTESIAN_POINT('Ctrl Pts',(-9.205289765937,-78.4797206212988,84.4735849437371));
#114432=CARTESIAN_POINT('Ctrl Pts',(-9.2378618143264,-78.5989066168308,
84.4370507663802));
#114433=CARTESIAN_POINT('Ctrl Pts',(-9.27787418570615,-78.740560111277,
84.3911450412213));
#114434=CARTESIAN_POINT('Ctrl Pts',(-9.29838328346071,-78.8120228871968,
84.3673470633219));
#114435=CARTESIAN_POINT('Ctrl Pts',(-9.3095050087037,-78.85047486607,84.3543684906706));
#114436=CARTESIAN_POINT('Ctrl Pts',(-9.31473181782181,-78.868464671978,
84.348248857627));
#114437=CARTESIAN_POINT('Ctrl Pts',(-9.31772754646189,-78.8787556642023,
84.3447364218093));
#114438=CARTESIAN_POINT('Ctrl Pts',(-9.31880032699569,-78.8824378399766,
84.343477834413));
#114439=CARTESIAN_POINT('Ctrl Pts',(-9.34657670740517,-78.9777339923983,
84.3108797837443));
#114440=CARTESIAN_POINT('Ctrl Pts',(-9.37891343386388,-79.0868515499015,
84.2722906472581));
#114441=CARTESIAN_POINT('Ctrl Pts',(-9.43490003601987,-79.2726635673985,
84.202663101968));
#114442=CARTESIAN_POINT('Ctrl Pts',(-9.45480915548319,-79.3382869048505,
84.1774909725898));
#114443=CARTESIAN_POINT('Ctrl Pts',(-9.48654321279514,-79.4421181774566,
84.1364887145665));
#114444=CARTESIAN_POINT('Ctrl Pts',(-9.49743296158528,-79.4776277277984,
84.1222802870086));
#114445=CARTESIAN_POINT('Ctrl Pts',(-9.5198359185379,-79.550419763444,84.0927275962692));
#114446=CARTESIAN_POINT('Ctrl Pts',(-9.53095928417824,-79.5864443608939,
84.0779088489564));
#114447=CARTESIAN_POINT('Ctrl Pts',(-9.59203318603208,-79.7835095778662,
83.9955795484352));
#114448=CARTESIAN_POINT('Ctrl Pts',(-9.63384205469713,-79.9173749817685,
83.9357786815125));
#114449=CARTESIAN_POINT('Ctrl Pts',(-9.68597997846769,-80.0839679014012,
83.8588944861294));
#114450=CARTESIAN_POINT('Ctrl Pts',(-9.70159672318671,-80.1337954519072,
83.8353887160939));
#114451=CARTESIAN_POINT('Ctrl Pts',(-9.72237799545848,-80.2001344713731,
83.8036571761089));
#114452=CARTESIAN_POINT('Ctrl Pts',(-9.73210767039267,-80.231203008154,
83.7886719432529));
#114453=CARTESIAN_POINT('Ctrl Pts',(-9.74230227571295,-80.2638018139171,
83.7727923316102));
#114454=CARTESIAN_POINT('Ctrl Pts',(-9.74711040784735,-80.2791925024508,
83.7652601401528));
#114455=CARTESIAN_POINT('Ctrl Pts',(-9.74910907079229,-80.285594124668,
83.7621201130671));
#114456=CARTESIAN_POINT('Ctrl Pts',(-9.75042774273054,-80.2898187121123,
83.7600464056674));
#114457=CARTESIAN_POINT('Ctrl Pts',(-9.75062835462383,-80.2904612028244,
83.7597313046068));
#114458=CARTESIAN_POINT('Ctrl Pts',(-9.89219342166761,-80.7442018423511,
83.5366773477816));
#114459=CARTESIAN_POINT('Ctrl Pts',(-10.0065728498921,-81.1239733380417,
83.3154687974507));
#114460=CARTESIAN_POINT('Ctrl Pts',(-10.0948640443048,-81.4411228740412,
83.1137067644422));
#114461=CARTESIAN_POINT('',(-10.7325093222838,-83.7451128513012,81.2061270357565));
#114462=CARTESIAN_POINT('Ctrl Pts',(-10.0948643816744,-81.4411242764804,
83.113706293064));
#114463=CARTESIAN_POINT('Ctrl Pts',(-10.1145889408639,-81.5120136748696,
83.0686084401552));
#114464=CARTESIAN_POINT('Ctrl Pts',(-10.134262787638,-81.5824703733078,
83.0227400344558));
#114465=CARTESIAN_POINT('Ctrl Pts',(-10.1538554911333,-81.6524782418569,
82.9761078803152));
#114466=CARTESIAN_POINT('Ctrl Pts',(-10.1630137060671,-81.6852020110595,
82.9543106183625));
#114467=CARTESIAN_POINT('Ctrl Pts',(-10.1721541893806,-81.7178277160856,
82.932346488473));
#114468=CARTESIAN_POINT('Ctrl Pts',(-10.1812743580122,-81.7503538579739,
82.9102160961475));
#114469=CARTESIAN_POINT('Ctrl Pts',(-10.2036036374808,-81.8299889328943,
82.8560333573243));
#114470=CARTESIAN_POINT('Ctrl Pts',(-10.2258097210356,-81.9090267401245,
82.8008544982978));
#114471=CARTESIAN_POINT('Ctrl Pts',(-10.2478613443576,-81.9874661349763,
82.7446731589146));
#114472=CARTESIAN_POINT('Ctrl Pts',(-10.2540851768928,-82.009604807064,
82.7288165826063));
#114473=CARTESIAN_POINT('Ctrl Pts',(-10.2602967017504,-82.0316958025345,
82.7128801399322));
#114474=CARTESIAN_POINT('Ctrl Pts',(-10.2664952398757,-82.0537390094448,
82.6968637096431));
#114475=CARTESIAN_POINT('Ctrl Pts',(-10.2912298513789,-82.1417000977185,
82.6329518367372));
#114476=CARTESIAN_POINT('Ctrl Pts',(-10.3157575691505,-82.2289010075233,
82.5677659776206));
#114477=CARTESIAN_POINT('Ctrl Pts',(-10.34003159336,-82.315327383666,82.5013015554146));
#114478=CARTESIAN_POINT('Ctrl Pts',(-10.3433937280341,-82.3272980859061,
82.4920957337281));
#114479=CARTESIAN_POINT('Ctrl Pts',(-10.346750994044,-82.339253926429,82.4828653808484));
#114480=CARTESIAN_POINT('Ctrl Pts',(-10.3501032905936,-82.3511948681523,
82.4736104792522));
#114481=CARTESIAN_POINT('Ctrl Pts',(-10.3776585818149,-82.4493473202934,
82.397536807088));
#114482=CARTESIAN_POINT('Ctrl Pts',(-10.4048769457379,-82.5464932440241,
82.3198049543937));
#114483=CARTESIAN_POINT('Ctrl Pts',(-10.4317048924259,-82.6426167536869,
82.2403978649875));
#114484=CARTESIAN_POINT('Ctrl Pts',(-10.4585328391139,-82.7387402633496,
82.1609907755813));
#114485=CARTESIAN_POINT('Ctrl Pts',(-10.4849703685669,-82.8338413739666,
82.0799084732329));
#114486=CARTESIAN_POINT('Ctrl Pts',(-10.5109756445671,-82.9278970790637,
81.9971327232997));
#114487=CARTESIAN_POINT('Ctrl Pts',(-10.5129329729522,-82.9349763310343,
81.990902475063));
#114488=CARTESIAN_POINT('Ctrl Pts',(-10.5148878555447,-82.9420496564716,
81.9846626334909));
#114489=CARTESIAN_POINT('Ctrl Pts',(-10.5168402781798,-82.9491170406922,
81.9784131934004));
#114490=CARTESIAN_POINT('Ctrl Pts',(-10.5408279532213,-83.0359476853625,
81.9016318985182));
#114491=CARTESIAN_POINT('Ctrl Pts',(-10.5644444159327,-83.1218817349016,
81.8234018722818));
#114492=CARTESIAN_POINT('Ctrl Pts',(-10.5876709688431,-83.2068866485923,
81.7437172531352));
#114493=CARTESIAN_POINT('Ctrl Pts',(-10.5920344468021,-83.222856175742,
81.728747228067));
#114494=CARTESIAN_POINT('Ctrl Pts',(-10.596384183008,-83.2387929057976,
81.7137258573887));
#114495=CARTESIAN_POINT('Ctrl Pts',(-10.6007198219405,-83.2546967030312,
81.6986530080038));
#114496=CARTESIAN_POINT('Ctrl Pts',(-10.6213409618985,-83.3303382483097,
81.6269636119132));
#114497=CARTESIAN_POINT('Ctrl Pts',(-10.6416433017889,-83.4052350699339,
81.5541098256993));
#114498=CARTESIAN_POINT('Ctrl Pts',(-10.6615921031911,-83.4793719471172,
81.4800761056022));
#114499=CARTESIAN_POINT('Ctrl Pts',(-10.6681626972362,-83.5037906234037,
81.4556914064616));
#114500=CARTESIAN_POINT('Ctrl Pts',(-10.6746950042282,-83.5281267213735,
81.4311787890362));
#114501=CARTESIAN_POINT('Ctrl Pts',(-10.6811897503772,-83.552378548331,
81.4065387716961));
#114502=CARTESIAN_POINT('Ctrl Pts',(-10.6985593874023,-83.617237962661,
81.3406411757519));
#114503=CARTESIAN_POINT('Ctrl Pts',(-10.7156603688218,-83.6814945969358,
81.2738323243309));
#114504=CARTESIAN_POINT('Ctrl Pts',(-10.7325093222788,-83.7451129887462,
81.2061271649026));
#114505=CARTESIAN_POINT('',(-10.728449721964,-86.9999997812556,72.9890778951916));
#114506=CARTESIAN_POINT('Ctrl Pts',(-10.7325093222941,-83.7451125764117,
81.2061267774639));
#114507=CARTESIAN_POINT('Ctrl Pts',(-10.7510222432914,-83.8147824396805,
81.1319806227714));
#114508=CARTESIAN_POINT('Ctrl Pts',(-10.7684192693147,-83.8853352697393,
81.0550084029296));
#114509=CARTESIAN_POINT('Ctrl Pts',(-10.784678148295,-83.9565893449822,
80.9750967182059));
#114510=CARTESIAN_POINT('Ctrl Pts',(-10.8005806758881,-84.0262817203942,
80.8969364850883));
#114511=CARTESIAN_POINT('Ctrl Pts',(-10.8153942348733,-84.0966443465624,
80.8159644628949));
#114512=CARTESIAN_POINT('Ctrl Pts',(-10.829129701094,-84.167505760494,80.7320688051));
#114513=CARTESIAN_POINT('Ctrl Pts',(-10.8366818581569,-84.2064674177918,
80.6859405430965));
#114514=CARTESIAN_POINT('Ctrl Pts',(-10.8439087777216,-84.2455793597819,
80.6389285660367));
#114515=CARTESIAN_POINT('Ctrl Pts',(-10.8508177380832,-84.2848092060794,
80.59101538589));
#114516=CARTESIAN_POINT('Ctrl Pts',(-10.8639725022384,-84.3595034218339,
80.499787972246));
#114517=CARTESIAN_POINT('Ctrl Pts',(-10.8759730630549,-84.4346271026063,
80.4052926427323));
#114518=CARTESIAN_POINT('Ctrl Pts',(-10.8868017876358,-84.5099482633126,
80.3074184901472));
#114519=CARTESIAN_POINT('Ctrl Pts',(-10.8919626453418,-84.5458455464829,
80.2607726852041));
#114520=CARTESIAN_POINT('Ctrl Pts',(-10.8968578239527,-84.5817871757456,
80.2133596100936));
#114521=CARTESIAN_POINT('Ctrl Pts',(-10.9014882826352,-84.6177451464455,
80.1651683767535));
#114522=CARTESIAN_POINT('Ctrl Pts',(-10.9104447521555,-84.687296888652,
80.071954433568));
#114523=CARTESIAN_POINT('Ctrl Pts',(-10.918410184324,-84.7569111066675,
79.9758285647734));
#114524=CARTESIAN_POINT('Ctrl Pts',(-10.9253427541375,-84.8263886683429,
79.8767099737823));
#114525=CARTESIAN_POINT('Ctrl Pts',(-10.9290250056511,-84.8632918461719,
79.8240628903024));
#114526=CARTESIAN_POINT('Ctrl Pts',(-10.9324235557544,-84.9001588458681,
79.7705676777781));
#114527=CARTESIAN_POINT('Ctrl Pts',(-10.9355433881164,-84.9369547938558,
79.7162164675029));
#114528=CARTESIAN_POINT('Ctrl Pts',(-10.9431567626755,-85.0267485076795,
79.5835823790142));
#114529=CARTESIAN_POINT('Ctrl Pts',(-10.9491098324278,-85.1161220781421,
79.4458496824301));
#114530=CARTESIAN_POINT('Ctrl Pts',(-10.9533490201889,-85.2045892224903,
79.3028708304583));
#114531=CARTESIAN_POINT('Ctrl Pts',(-10.9537936745096,-85.213868664729,
79.2878735791283));
#114532=CARTESIAN_POINT('Ctrl Pts',(-10.9542194866345,-85.2231380919539,
79.2728186248596));
#114533=CARTESIAN_POINT('Ctrl Pts',(-10.9546264050554,-85.2323969126946,
79.257705809322));
#114534=CARTESIAN_POINT('Ctrl Pts',(-10.9566325283981,-85.2780432522572,
79.1831990520264));
#114535=CARTESIAN_POINT('Ctrl Pts',(-10.9581789632201,-85.3234320314642,
79.1072859065619));
#114536=CARTESIAN_POINT('Ctrl Pts',(-10.9592926858649,-85.3684954136484,
79.029941852874));
#114537=CARTESIAN_POINT('Ctrl Pts',(-10.9604160766467,-85.4139499874387,
78.9519263816601));
#114538=CARTESIAN_POINT('Ctrl Pts',(-10.9610809172281,-85.4590688918478,
78.8724629550289));
#114539=CARTESIAN_POINT('Ctrl Pts',(-10.9612894216802,-85.5037788116888,
78.7915296637231));
#114540=CARTESIAN_POINT('Ctrl Pts',(-10.9614870058926,-85.5461470882778,
78.7148351833147));
#114541=CARTESIAN_POINT('Ctrl Pts',(-10.9612749276812,-85.5881481125788,
78.6368206735561));
#114542=CARTESIAN_POINT('Ctrl Pts',(-10.960650954875,-85.6297120799806,
78.5574804832683));
#114543=CARTESIAN_POINT('Ctrl Pts',(-10.9600140200044,-85.672139474149,
78.4764921239476));
#114544=CARTESIAN_POINT('Ctrl Pts',(-10.9589490660722,-85.7141130952747,
78.3941194696662));
#114545=CARTESIAN_POINT('Ctrl Pts',(-10.9574560783488,-85.7555582591477,
78.3103522147957));
#114546=CARTESIAN_POINT('Ctrl Pts',(-10.9574460434946,-85.7558368255226,
78.3097891879347));
#114547=CARTESIAN_POINT('Ctrl Pts',(-10.9574359893214,-85.7561153680064,
78.3092260980831));
#114548=CARTESIAN_POINT('Ctrl Pts',(-10.9574259158265,-85.7563938865775,
78.3086629452375));
#114549=CARTESIAN_POINT('Ctrl Pts',(-10.956671510735,-85.7772521716685,
78.2664883693699));
#114550=CARTESIAN_POINT('Ctrl Pts',(-10.9558086563518,-85.7979763919999,
78.2239604082909));
#114551=CARTESIAN_POINT('Ctrl Pts',(-10.9548373526965,-85.8185569657927,
78.1810781497251));
#114552=CARTESIAN_POINT('Ctrl Pts',(-10.9543517008688,-85.8288472526891,
78.1596370204423));
#114553=CARTESIAN_POINT('Ctrl Pts',(-10.9538389367222,-85.8391016262828,
78.138107315856));
#114554=CARTESIAN_POINT('Ctrl Pts',(-10.953299060256,-85.8493188733959,
78.116488926769));
#114555=CARTESIAN_POINT('Ctrl Pts',(-10.953029122023,-85.8544274969525,
78.1056797322255));
#114556=CARTESIAN_POINT('Ctrl Pts',(-10.95275240571,-85.8595268387752,78.0948483664995));
#114557=CARTESIAN_POINT('Ctrl Pts',(-10.9524689113171,-85.8646167459357,
78.0839948168531));
#114558=CARTESIAN_POINT('Ctrl Pts',(-10.9521854169241,-85.8697066530963,
78.0731412672067));
#114559=CARTESIAN_POINT('Ctrl Pts',(-10.9518650103282,-85.8753015385961,
78.0611599992563));
#114560=CARTESIAN_POINT('Ctrl Pts',(-10.9515980938983,-85.8798580098567,
78.0513676035743));
#114561=CARTESIAN_POINT('Ctrl Pts',(-10.9493307066674,-85.9185640751157,
77.968183691148));
#114562=CARTESIAN_POINT('Ctrl Pts',(-10.9466840767295,-85.9568853712228,
77.8833334794079));
#114563=CARTESIAN_POINT('Ctrl Pts',(-10.9436635797958,-85.9947243643778,
77.7968032951168));
#114564=CARTESIAN_POINT('Ctrl Pts',(-10.9409949187626,-86.0281557661588,
77.7203523878379));
#114565=CARTESIAN_POINT('Ctrl Pts',(-10.9380346094849,-86.061210580883,
77.6425901674792));
#114566=CARTESIAN_POINT('Ctrl Pts',(-10.934777888651,-86.0938213085787,
77.5635061522729));
#114567=CARTESIAN_POINT('Ctrl Pts',(-10.9313064850056,-86.1285817331826,
77.4792089242683));
#114568=CARTESIAN_POINT('Ctrl Pts',(-10.9275010633154,-86.1628371480715,
77.3934109785441));
#114569=CARTESIAN_POINT('Ctrl Pts',(-10.9233616235826,-86.1965015630842,
77.306104556324));
#114570=CARTESIAN_POINT('Ctrl Pts',(-10.9221879091295,-86.206046915356,
77.2813493198119));
#114571=CARTESIAN_POINT('Ctrl Pts',(-10.9209875019718,-86.2155447536471,
77.2564727659167));
#114572=CARTESIAN_POINT('Ctrl Pts',(-10.9197600577454,-86.2249930310364,
77.2314748551298));
#114573=CARTESIAN_POINT('Ctrl Pts',(-10.9188230353986,-86.2322057799839,
77.2123916246859));
#114574=CARTESIAN_POINT('Ctrl Pts',(-10.9178702559755,-86.2393896458739,
77.1932376718965));
#114575=CARTESIAN_POINT('Ctrl Pts',(-10.9169019504432,-86.2465437460638,
77.1740128936221));
#114576=CARTESIAN_POINT('Ctrl Pts',(-10.9157835859962,-86.2548065216399,
77.1518088394203));
#114577=CARTESIAN_POINT('Ctrl Pts',(-10.9146443454205,-86.2630295774941,
77.1295103433876));
#114578=CARTESIAN_POINT('Ctrl Pts',(-10.9134842287163,-86.2712115153925,
77.1071173363896));
#114579=CARTESIAN_POINT('Ctrl Pts',(-10.9129041703643,-86.2753024843418,
77.0959208328907));
#114580=CARTESIAN_POINT('Ctrl Pts',(-10.9123188929802,-86.2793831737303,
77.0847007016266));
#114581=CARTESIAN_POINT('Ctrl Pts',(-10.911728396564,-86.2834534078366,
77.0734569352409));
#114582=CARTESIAN_POINT('Ctrl Pts',(-10.911433148356,-86.2854885248897,
77.0678350520481));
#114583=CARTESIAN_POINT('Ctrl Pts',(-10.9111365953899,-86.287521028118,
77.0622072600734));
#114584=CARTESIAN_POINT('Ctrl Pts',(-10.9108387376659,-86.289550895496,
77.056573558484));
#114585=CARTESIAN_POINT('Ctrl Pts',(-10.9105408799419,-86.291580762874,
77.0509398568946));
#114586=CARTESIAN_POINT('Ctrl Pts',(-10.9101335854462,-86.2943365970394,
77.0432685379285));
#114587=CARTESIAN_POINT('Ctrl Pts',(-10.9099412502199,-86.2956325680269,
77.0396547240619));
#114588=CARTESIAN_POINT('Ctrl Pts',(-10.907803220588,-86.3100387921298,
76.9994829818475));
#114589=CARTESIAN_POINT('Ctrl Pts',(-10.9052699371439,-86.326228168735,
76.95367723549));
#114590=CARTESIAN_POINT('Ctrl Pts',(-10.9023364899602,-86.3439953687665,
76.9021729235994));
#114591=CARTESIAN_POINT('Ctrl Pts',(-10.8994201604487,-86.3616588910807,
76.8509691570665));
#114592=CARTESIAN_POINT('Ctrl Pts',(-10.896107836887,-86.3808818716695,
76.7941329967364));
#114593=CARTESIAN_POINT('Ctrl Pts',(-10.8923984096102,-86.4014134015565,
76.7315870902248));
#114594=CARTESIAN_POINT('Ctrl Pts',(-10.8898341614871,-86.4156064111637,
76.6883504363129));
#114595=CARTESIAN_POINT('Ctrl Pts',(-10.8870802112116,-86.4304237153378,
76.6423849924677));
#114596=CARTESIAN_POINT('Ctrl Pts',(-10.8841392492642,-86.4457685531813,
76.5936618749884));
#114597=CARTESIAN_POINT('Ctrl Pts',(-10.8832950114274,-86.4501734699867,
76.5796753290774));
#114598=CARTESIAN_POINT('Ctrl Pts',(-10.8824353843272,-86.4546217860028,
76.5654615226593));
#114599=CARTESIAN_POINT('Ctrl Pts',(-10.8815605246739,-86.4591110286805,
76.5510197661022));
#114600=CARTESIAN_POINT('Ctrl Pts',(-10.8773404009239,-86.4807661130926,
76.4813560210649));
#114601=CARTESIAN_POINT('Ctrl Pts',(-10.8727620467592,-86.5033764055256,
76.4063902509679));
#114602=CARTESIAN_POINT('Ctrl Pts',(-10.8678183023178,-86.5266369525449,
76.3260472126269));
#114603=CARTESIAN_POINT('Ctrl Pts',(-10.8652847021162,-86.5385576590697,
76.2848725239761));
#114604=CARTESIAN_POINT('Ctrl Pts',(-10.8626555235647,-86.5506484475054,
76.242285489306));
#114605=CARTESIAN_POINT('Ctrl Pts',(-10.8599327538662,-86.5628637872285,
76.1982758449494));
#114606=CARTESIAN_POINT('Ctrl Pts',(-10.8559149361761,-86.5808891854308,
76.1333336180234));
#114607=CARTESIAN_POINT('Ctrl Pts',(-10.8516905238557,-86.5991864130687,
76.0652937708498));
#114608=CARTESIAN_POINT('Ctrl Pts',(-10.847259516825,-86.6175965484567,
75.9941250065181));
#114609=CARTESIAN_POINT('Ctrl Pts',(-10.8450440133097,-86.6268016161507,
75.9585406243523));
#114610=CARTESIAN_POINT('Ctrl Pts',(-10.8427768611176,-86.6360346768941,
75.922174040174));
#114611=CARTESIAN_POINT('Ctrl Pts',(-10.8404580602521,-86.6452744508845,
75.8850215613659));
#114612=CARTESIAN_POINT('Ctrl Pts',(-10.8399932126182,-86.6471267389101,
75.8775736420024));
#114613=CARTESIAN_POINT('Ctrl Pts',(-10.8395262919422,-86.648979293872,
75.8700941390403));
#114614=CARTESIAN_POINT('Ctrl Pts',(-10.83905729361,-86.6508319396637,75.8625830239116));
#114615=CARTESIAN_POINT('Ctrl Pts',(-10.8383565390388,-86.6536000731901,
75.8513602798226));
#114616=CARTESIAN_POINT('Ctrl Pts',(-10.8376511456282,-86.6563684098304,
75.8400669618679));
#114617=CARTESIAN_POINT('Ctrl Pts',(-10.8369411224503,-86.6591363571076,
75.8287029780982));
#114618=CARTESIAN_POINT('Ctrl Pts',(-10.8358316521156,-86.6634615051979,
75.8109458072505));
#114619=CARTESIAN_POINT('Ctrl Pts',(-10.8346490644395,-86.6680217558641,
75.792028396447));
#114620=CARTESIAN_POINT('Ctrl Pts',(-10.8335669198333,-86.67215187099,75.7747240707307));
#114621=CARTESIAN_POINT('Ctrl Pts',(-10.833493031196,-86.6724338745012,
75.7735425345117));
#114622=CARTESIAN_POINT('Ctrl Pts',(-10.833419610159,-86.67271389208,75.7723685240432));
#114623=CARTESIAN_POINT('Ctrl Pts',(-10.8333467116477,-86.6729917202779,
75.771202924429));
#114624=CARTESIAN_POINT('Ctrl Pts',(-10.82650931042,-86.6990501791833,75.6618773416835));
#114625=CARTESIAN_POINT('Ctrl Pts',(-10.8200333262671,-86.7226942142122,
75.5558789242882));
#114626=CARTESIAN_POINT('Ctrl Pts',(-10.8139542169689,-86.7442167453786,
75.4533141127769));
#114627=CARTESIAN_POINT('Ctrl Pts',(-10.8076212434149,-86.7666380597528,
75.3464661837463));
#114628=CARTESIAN_POINT('Ctrl Pts',(-10.8017186737899,-86.7867571708465,
75.2433446321614));
#114629=CARTESIAN_POINT('Ctrl Pts',(-10.7962391680734,-86.8048850275004,
75.1440468283543));
#114630=CARTESIAN_POINT('Ctrl Pts',(-10.7947405931986,-86.8098427649171,
75.1168901464188));
#114631=CARTESIAN_POINT('Ctrl Pts',(-10.7932734134942,-86.814651444266,
75.0900193350083));
#114632=CARTESIAN_POINT('Ctrl Pts',(-10.7918369460471,-86.8193171491601,
75.0634361046744));
#114633=CARTESIAN_POINT('Ctrl Pts',(-10.7901112142961,-86.824922396319,
75.0314997564292));
#114634=CARTESIAN_POINT('Ctrl Pts',(-10.7884297963389,-86.8303212963133,
74.9999784843577));
#114635=CARTESIAN_POINT('Ctrl Pts',(-10.7867896150128,-86.8355242020625,
74.9688754749133));
#114636=CARTESIAN_POINT('Ctrl Pts',(-10.7811928432361,-86.8532780171989,
74.8627430353731));
#114637=CARTESIAN_POINT('Ctrl Pts',(-10.7761184458931,-86.8687532514872,
74.7614793995783));
#114638=CARTESIAN_POINT('Ctrl Pts',(-10.77156743064,-86.8823386801257,74.6651789381298));
#114639=CARTESIAN_POINT('Ctrl Pts',(-10.7709185994682,-86.8842755335735,
74.6514495310024));
#114640=CARTESIAN_POINT('Ctrl Pts',(-10.7702803824442,-86.8861739133072,
74.6378209491359));
#114641=CARTESIAN_POINT('Ctrl Pts',(-10.7696527601112,-86.8880348839046,
74.6242934129354));
#114642=CARTESIAN_POINT('Ctrl Pts',(-10.7671378225696,-86.8954919557344,
74.5700873930946));
#114643=CARTESIAN_POINT('Ctrl Pts',(-10.7647934875938,-86.9023486428634,
74.5175042618523));
#114644=CARTESIAN_POINT('Ctrl Pts',(-10.7626197553063,-86.9086708213643,
74.4665573115567));
#114645=CARTESIAN_POINT('Ctrl Pts',(-10.7615328891625,-86.9118319106148,
74.4410838364088));
#114646=CARTESIAN_POINT('Ctrl Pts',(-10.7604886736913,-86.9148593057109,
74.4160193984485));
#114647=CARTESIAN_POINT('Ctrl Pts',(-10.7594871088829,-86.9177608650203,
74.3913654171809));
#114648=CARTESIAN_POINT('Ctrl Pts',(-10.7589863264787,-86.919211644675,
74.379038426547));
#114649=CARTESIAN_POINT('Ctrl Pts',(-10.7584962067405,-86.9206309612238,
74.3668140495618));
#114650=CARTESIAN_POINT('Ctrl Pts',(-10.7580167496668,-86.9220197725852,
74.3546924568402));
#114651=CARTESIAN_POINT('Ctrl Pts',(-10.7577770211299,-86.9227141782659,
74.3486316604794));
#114652=CARTESIAN_POINT('Ctrl Pts',(-10.7575399582592,-86.9234009573923,
74.3425965601559));
#114653=CARTESIAN_POINT('Ctrl Pts',(-10.7573055610544,-86.9240802282338,
74.336587176387));
#114654=CARTESIAN_POINT('Ctrl Pts',(-10.7570711638495,-86.9247594990753,
74.3305777926182));
#114655=CARTESIAN_POINT('Ctrl Pts',(-10.7568941569512,-86.9252725409332,
74.3260174959602));
#114656=CARTESIAN_POINT('Ctrl Pts',(-10.7566103664373,-86.9260956331663,
74.3186361949689));
#114657=CARTESIAN_POINT('Ctrl Pts',(-10.7557717398522,-86.9285279450123,
74.2968237842595));
#114658=CARTESIAN_POINT('Ctrl Pts',(-10.7549515907162,-86.9308930137454,
74.275070955312));
#114659=CARTESIAN_POINT('Ctrl Pts',(-10.754150066911,-86.933191857729,74.2533782531655));
#114660=CARTESIAN_POINT('Ctrl Pts',(-10.7479305549346,-86.9510299900418,
74.085051348921));
#114661=CARTESIAN_POINT('Ctrl Pts',(-10.7428350444671,-86.9648824251588,
73.9203479344601));
#114662=CARTESIAN_POINT('Ctrl Pts',(-10.7388723178175,-86.9752360679132,
73.7594344127732));
#114663=CARTESIAN_POINT('Ctrl Pts',(-10.7365822146096,-86.9812195516561,
73.6664407231237));
#114664=CARTESIAN_POINT('Ctrl Pts',(-10.73466985067,-86.9860341006921,73.5747120535647));
#114665=CARTESIAN_POINT('Ctrl Pts',(-10.7331325040884,-86.9897703599552,
73.4842749393781));
#114666=CARTESIAN_POINT('Ctrl Pts',(-10.7305698086316,-86.9959985551799,
73.3335198758081));
#114667=CARTESIAN_POINT('Ctrl Pts',(-10.7290511142392,-86.9992315626732,
73.1863560058278));
#114668=CARTESIAN_POINT('Ctrl Pts',(-10.7285784258043,-86.9998778669969,
73.0429165819694));
#114669=CARTESIAN_POINT('Ctrl Pts',(-10.728519092563,-86.9999589930147,
73.0249116440121));
#114670=CARTESIAN_POINT('Ctrl Pts',(-10.7284762009538,-86.9999993368467,
73.0069653406822));
#114671=CARTESIAN_POINT('Ctrl Pts',(-10.7284497219417,-86.9999996839437,
72.9890778951898));
#114672=CARTESIAN_POINT('',(-10.7325538919673,-83.7450248445335,64.7715579422181));
#114673=CARTESIAN_POINT('Ctrl Pts',(-10.7284497219764,-86.9999998242331,
72.9890778951925));
#114674=CARTESIAN_POINT('Ctrl Pts',(-10.7284888747654,-87.0000012631274,
72.8882010561864));
#114675=CARTESIAN_POINT('Ctrl Pts',(-10.7291051326801,-86.9987315794751,
72.7849150495473));
#114676=CARTESIAN_POINT('Ctrl Pts',(-10.7302920457223,-86.996004952873,
72.6792651291966));
#114677=CARTESIAN_POINT('Ctrl Pts',(-10.7319888110209,-86.992107072206,
72.5282320608291));
#114678=CARTESIAN_POINT('Ctrl Pts',(-10.7348512590662,-86.9852332530932,
72.3723668347754));
#114679=CARTESIAN_POINT('Ctrl Pts',(-10.7389002092034,-86.9748130428885,
72.2117979770313));
#114680=CARTESIAN_POINT('Ctrl Pts',(-10.7395319821845,-86.9731871381373,
72.1867438117535));
#114681=CARTESIAN_POINT('Ctrl Pts',(-10.7401926355456,-86.9714748188675,
72.1615752029785));
#114682=CARTESIAN_POINT('Ctrl Pts',(-10.7408822399634,-86.9696738375772,
72.1362927230114));
#114683=CARTESIAN_POINT('Ctrl Pts',(-10.7426464435455,-86.9650664169143,
72.071612972457));
#114684=CARTESIAN_POINT('Ctrl Pts',(-10.7446002347412,-86.9598787695624,
72.00618781155));
#114685=CARTESIAN_POINT('Ctrl Pts',(-10.7467361926647,-86.9540740543932,
71.9400335061946));
#114686=CARTESIAN_POINT('Ctrl Pts',(-10.7509385308377,-86.9426537095119,
71.8098798362008));
#114687=CARTESIAN_POINT('Ctrl Pts',(-10.7558549933362,-86.9288446840852,
71.676888006109));
#114688=CARTESIAN_POINT('Ctrl Pts',(-10.7615098162251,-86.9123520250915,
71.5411743141284));
#114689=CARTESIAN_POINT('Ctrl Pts',(-10.7639724035918,-86.9051697287615,
71.482073113272));
#114690=CARTESIAN_POINT('Ctrl Pts',(-10.7665748213442,-86.8974782983634,
71.4224562468907));
#114691=CARTESIAN_POINT('Ctrl Pts',(-10.7693103288981,-86.889252545791,
71.3623303350626));
#114692=CARTESIAN_POINT('Ctrl Pts',(-10.7738188465192,-86.875695299215,
71.2632340146852));
#114693=CARTESIAN_POINT('Ctrl Pts',(-10.7787004449165,-86.8606874728627,
71.1627601820488));
#114694=CARTESIAN_POINT('Ctrl Pts',(-10.7839551238006,-86.8441164950172,
71.0609588802453));
#114695=CARTESIAN_POINT('Ctrl Pts',(-10.7865824632427,-86.8358310060945,
71.0100582293435));
#114696=CARTESIAN_POINT('Ctrl Pts',(-10.7893030728237,-86.8271546776825,
70.958825719308));
#114697=CARTESIAN_POINT('Ctrl Pts',(-10.7921169525352,-86.8180732504146,
70.907268334575));
#114698=CARTESIAN_POINT('Ctrl Pts',(-10.7924606326094,-86.8169640681049,
70.9009712474106));
#114699=CARTESIAN_POINT('Ctrl Pts',(-10.7928057051129,-86.8158488425891,
70.8946693145837));
#114700=CARTESIAN_POINT('Ctrl Pts',(-10.7931521683829,-86.8147275475862,
70.8883625482581));
#114701=CARTESIAN_POINT('Ctrl Pts',(-10.7942240386725,-86.8112585426332,
70.8688509981639));
#114702=CARTESIAN_POINT('Ctrl Pts',(-10.7953092216315,-86.8077314450951,
70.849293184582));
#114703=CARTESIAN_POINT('Ctrl Pts',(-10.7964077247073,-86.8041454871649,
70.8296894990121));
#114704=CARTESIAN_POINT('Ctrl Pts',(-10.7971345121707,-86.801772959199,
70.8167193824761));
#114705=CARTESIAN_POINT('Ctrl Pts',(-10.7978671290185,-86.7993746656645,
70.8037291852011));
#114706=CARTESIAN_POINT('Ctrl Pts',(-10.7986055752513,-86.7969503833673,
70.7907190216704));
#114707=CARTESIAN_POINT('Ctrl Pts',(-10.7992908472177,-86.7947006695452,
70.7786456980492));
#114708=CARTESIAN_POINT('Ctrl Pts',(-10.7998987965539,-86.7927000493644,
70.7679895228104));
#114709=CARTESIAN_POINT('Ctrl Pts',(-10.8006586536161,-86.7901926376231,
70.7547573980053));
#114710=CARTESIAN_POINT('Ctrl Pts',(-10.800717615377,-86.7899980728568,
70.7537306399234));
#114711=CARTESIAN_POINT('Ctrl Pts',(-10.800777495232,-86.789800431358,70.7526883773526));
#114712=CARTESIAN_POINT('Ctrl Pts',(-10.8008384021056,-86.7895993463446,
70.7516287476968));
#114713=CARTESIAN_POINT('Ctrl Pts',(-10.8119753799017,-86.7528304367686,
70.5578727519031));
#114714=CARTESIAN_POINT('Ctrl Pts',(-10.823335768474,-86.7112853942037,
70.3650224851882));
#114715=CARTESIAN_POINT('Ctrl Pts',(-10.8349247208416,-86.6650136200905,
70.1733140719098));
#114716=CARTESIAN_POINT('Ctrl Pts',(-10.8374182920251,-86.6550574170725,
70.1320645646358));
#114717=CARTESIAN_POINT('Ctrl Pts',(-10.8399224267147,-86.6448823906394,
70.0908679706403));
#114718=CARTESIAN_POINT('Ctrl Pts',(-10.8424365917833,-86.6344890661378,
70.0497263415853));
#114719=CARTESIAN_POINT('Ctrl Pts',(-10.8495360058733,-86.6051407487454,
69.9335520041667));
#114720=CARTESIAN_POINT('Ctrl Pts',(-10.8567186108653,-86.5740520420787,
69.8178173284099));
#114721=CARTESIAN_POINT('Ctrl Pts',(-10.8639844065654,-86.5412369311502,
69.7025742433079));
#114722=CARTESIAN_POINT('Ctrl Pts',(-10.8676173044154,-86.5248293756859,
69.644952700757));
#114723=CARTESIAN_POINT('Ctrl Pts',(-10.8712709999796,-86.5079902361993,
69.5874540509201));
#114724=CARTESIAN_POINT('Ctrl Pts',(-10.8749454933449,-86.4907214240387,
69.5300847389974));
#114725=CARTESIAN_POINT('Ctrl Pts',(-10.8767827400276,-86.4820870179584,
69.5014000830361));
#114726=CARTESIAN_POINT('Ctrl Pts',(-10.8786251861658,-86.4733451959164,
69.4727477609269));
#114727=CARTESIAN_POINT('Ctrl Pts',(-10.8804728317814,-86.4644962125682,
69.4441285732381));
#114728=CARTESIAN_POINT('Ctrl Pts',(-10.8807324272481,-86.4632529243844,
69.4401075578871));
#114729=CARTESIAN_POINT('Ctrl Pts',(-10.8809947516596,-86.4619951972876,
69.4360473607439));
#114730=CARTESIAN_POINT('Ctrl Pts',(-10.8812586851527,-86.4607281333618,
69.4319648057151));
#114731=CARTESIAN_POINT('Ctrl Pts',(-10.8826244528261,-86.4541715007429,
69.4108389470075));
#114732=CARTESIAN_POINT('Ctrl Pts',(-10.8840327498243,-86.4473607879374,
69.3891157686244));
#114733=CARTESIAN_POINT('Ctrl Pts',(-10.8853325786385,-86.4410332420026,
69.3691163789735));
#114734=CARTESIAN_POINT('Ctrl Pts',(-10.8855693856182,-86.4398804694023,
69.3654728260624));
#114735=CARTESIAN_POINT('Ctrl Pts',(-10.8858026112128,-86.4387438659352,
69.3618864423125));
#114736=CARTESIAN_POINT('Ctrl Pts',(-10.8860313670693,-86.4376280585935,
69.3583712056871));
#114737=CARTESIAN_POINT('Ctrl Pts',(-10.8956823808273,-86.3905531020374,
69.2100663816831));
#114738=CARTESIAN_POINT('Ctrl Pts',(-10.904504945182,-86.3398056888968,
69.0601907694884));
#114739=CARTESIAN_POINT('Ctrl Pts',(-10.9125092853346,-86.2851319634432,
68.9089620111517));
#114740=CARTESIAN_POINT('Ctrl Pts',(-10.9157955212498,-86.2626852961636,
68.8468740229391));
#114741=CARTESIAN_POINT('Ctrl Pts',(-10.9189433001879,-86.2395768797012,
68.784558218495));
#114742=CARTESIAN_POINT('Ctrl Pts',(-10.9219509878368,-86.2157892384658,
68.722030682055));
#114743=CARTESIAN_POINT('Ctrl Pts',(-10.9221051116491,-86.2145702814525,
68.7188265653326));
#114744=CARTESIAN_POINT('Ctrl Pts',(-10.9222588672882,-86.2133495408695,
68.7156218927447));
#114745=CARTESIAN_POINT('Ctrl Pts',(-10.9224122547845,-86.2121270144323,
68.712416666541));
#114746=CARTESIAN_POINT('Ctrl Pts',(-10.9276310461364,-86.1705322915913,
68.6033634047605));
#114747=CARTESIAN_POINT('Ctrl Pts',(-10.9324274924053,-86.1268703731123,
68.4936690105705));
#114748=CARTESIAN_POINT('Ctrl Pts',(-10.9368015932311,-86.0810510568632,
68.3834248233145));
#114749=CARTESIAN_POINT('Ctrl Pts',(-10.938988643644,-86.0581413987386,
68.3283027296865));
#114750=CARTESIAN_POINT('Ctrl Pts',(-10.9410701077568,-86.0346923515679,
68.2730432024122));
#114751=CARTESIAN_POINT('Ctrl Pts',(-10.9430459856038,-86.0106927200718,
68.2176584839966));
#114752=CARTESIAN_POINT('Ctrl Pts',(-10.9440339245274,-85.9986929043237,
68.1899661247888));
#114753=CARTESIAN_POINT('Ctrl Pts',(-10.9449954668838,-85.9865554403056,
68.1622424687455));
#114754=CARTESIAN_POINT('Ctrl Pts',(-10.9459306126711,-85.9742789254811,
68.1344890742454));
#114755=CARTESIAN_POINT('Ctrl Pts',(-10.9463981855648,-85.9681406680688,
68.1206123769953));
#114756=CARTESIAN_POINT('Ctrl Pts',(-10.946859159316,-85.9619676478248,
68.1067282451965));
#114757=CARTESIAN_POINT('Ctrl Pts',(-10.9473135339246,-85.9557596898088,
68.0928368765541));
#114758=CARTESIAN_POINT('Ctrl Pts',(-10.9475407212289,-85.9526557108008,
68.0858911922329));
#114759=CARTESIAN_POINT('Ctrl Pts',(-10.9477662587475,-85.9495429973423,
68.0789436987048));
#114760=CARTESIAN_POINT('Ctrl Pts',(-10.9479901464804,-85.946421527598,
68.0719944208737));
#114761=CARTESIAN_POINT('Ctrl Pts',(-10.94816823117,-85.943938649401,68.066466829122));
#114762=CARTESIAN_POINT('Ctrl Pts',(-10.9483711709324,-85.9410850462583,
68.0601277871563));
#114763=CARTESIAN_POINT('Ctrl Pts',(-10.9485371095389,-85.9387319835289,
68.0549110128396));
#114764=CARTESIAN_POINT('Ctrl Pts',(-10.9485797886327,-85.9381267802728,
68.053569268413));
#114765=CARTESIAN_POINT('Ctrl Pts',(-10.9486200425959,-85.9375547496877,
68.0523017345745));
#114766=CARTESIAN_POINT('Ctrl Pts',(-10.9486568603221,-85.9370308276724,
68.0511412594396));
#114767=CARTESIAN_POINT('Ctrl Pts',(-10.9535290566002,-85.8676987107813,
67.8975722255995));
#114768=CARTESIAN_POINT('Ctrl Pts',(-10.9571237516371,-85.796390348302,
67.7482490038176));
#114769=CARTESIAN_POINT('Ctrl Pts',(-10.9593857595805,-85.7235058471837,
67.6031289566081));
#114770=CARTESIAN_POINT('Ctrl Pts',(-10.9602457587846,-85.6957956823561,
67.547955355002));
#114771=CARTESIAN_POINT('Ctrl Pts',(-10.9609134980145,-85.6678573736214,
67.4933890699717));
#114772=CARTESIAN_POINT('Ctrl Pts',(-10.9613872778227,-85.6397117577135,
67.4394269159064));
#114773=CARTESIAN_POINT('Ctrl Pts',(-10.9626755897398,-85.5631776130193,
67.2926919032226));
#114774=CARTESIAN_POINT('Ctrl Pts',(-10.9625276751357,-85.4851133229949,
67.1504256856112));
#114775=CARTESIAN_POINT('Ctrl Pts',(-10.9609574725558,-85.4059328878418,
67.0125566511054));
#114776=CARTESIAN_POINT('Ctrl Pts',(-10.9604607636164,-85.3808854000432,
66.9689439461118));
#114777=CARTESIAN_POINT('Ctrl Pts',(-10.9598219500033,-85.3557259460709,
66.9257710771614));
#114778=CARTESIAN_POINT('Ctrl Pts',(-10.9590420630014,-85.3304668763377,
66.8830352992811));
#114779=CARTESIAN_POINT('Ctrl Pts',(-10.9566133192741,-85.2518044457246,
66.7499464643508));
#114780=CARTESIAN_POINT('Ctrl Pts',(-10.9528135993784,-85.1721785314414,
66.6210980796646));
#114781=CARTESIAN_POINT('Ctrl Pts',(-10.9476408198054,-85.0919519597182,
66.496393328091));
#114782=CARTESIAN_POINT('Ctrl Pts',(-10.9461366559269,-85.0686233199461,
66.4601311251219));
#114783=CARTESIAN_POINT('Ctrl Pts',(-10.9445166201651,-85.0452436680095,
66.4242191730408));
#114784=CARTESIAN_POINT('Ctrl Pts',(-10.9427812044943,-85.0218213848203,
66.3886548154653));
#114785=CARTESIAN_POINT('Ctrl Pts',(-10.9388414051909,-84.9686473259792,
66.3079154090165));
#114786=CARTESIAN_POINT('Ctrl Pts',(-10.9343065299015,-84.9152540838332,
66.2289677825578));
#114787=CARTESIAN_POINT('Ctrl Pts',(-10.9291847863793,-84.8617440602333,
66.151785527885));
#114788=CARTESIAN_POINT('Ctrl Pts',(-10.9246671423073,-84.8145454373701,
66.083706766469));
#114789=CARTESIAN_POINT('Ctrl Pts',(-10.9196756195247,-84.7672558795174,
66.017001426963));
#114790=CARTESIAN_POINT('Ctrl Pts',(-10.9142209171807,-84.71993740355,65.9516443212193));
#114791=CARTESIAN_POINT('Ctrl Pts',(-10.9052079494621,-84.6417516714083,
65.8436528219419));
#114792=CARTESIAN_POINT('Ctrl Pts',(-10.8949278585239,-84.5634888687763,
65.7393427125517));
#114793=CARTESIAN_POINT('Ctrl Pts',(-10.8833752888633,-84.4854095252617,
65.6385828033828));
#114794=CARTESIAN_POINT('Ctrl Pts',(-10.8806126706233,-84.4667380586618,
65.6144876305245));
#114795=CARTESIAN_POINT('Ctrl Pts',(-10.8777774550046,-84.4480769262614,
65.590595431077));
#114796=CARTESIAN_POINT('Ctrl Pts',(-10.8748698783256,-84.4294294000177,
65.5669043282896));
#114797=CARTESIAN_POINT('Ctrl Pts',(-10.8628804971574,-84.3525363978144,
65.4692141577535));
#114798=CARTESIAN_POINT('Ctrl Pts',(-10.8496579766825,-84.2758777732863,
65.3749443449109));
#114799=CARTESIAN_POINT('Ctrl Pts',(-10.8352182645738,-84.1996939182158,
65.283979980599));
#114800=CARTESIAN_POINT('Ctrl Pts',(-10.832318642333,-84.1843955245298,
65.2657135295859));
#114801=CARTESIAN_POINT('Ctrl Pts',(-10.8293700476068,-84.1691161545344,
65.2475803268386));
#114802=CARTESIAN_POINT('Ctrl Pts',(-10.8263727699115,-84.153857575543,
65.2295793819169));
#114803=CARTESIAN_POINT('Ctrl Pts',(-10.8122899682069,-84.0821646714902,
65.1450013869506));
#114804=CARTESIAN_POINT('Ctrl Pts',(-10.7971290892607,-84.0109333643218,
65.0633439925102));
#114805=CARTESIAN_POINT('Ctrl Pts',(-10.7808637979447,-83.9403515843494,
64.9845085897367));
#114806=CARTESIAN_POINT('Ctrl Pts',(-10.7774480386293,-83.9255292016602,
64.9679529218317));
#114807=CARTESIAN_POINT('Ctrl Pts',(-10.7739837140888,-83.91073535137,64.9515216712212));
#114808=CARTESIAN_POINT('Ctrl Pts',(-10.7704707982537,-83.8959715976633,
64.9352138692215));
#114809=CARTESIAN_POINT('Ctrl Pts',(-10.758408522074,-83.8452773928997,
64.8792178759091));
#114810=CARTESIAN_POINT('Ctrl Pts',(-10.7457724178086,-83.7949388097837,
64.8246776374892));
#114811=CARTESIAN_POINT('Ctrl Pts',(-10.7325538919668,-83.7450247454837,
64.7715580352908));
#114812=CARTESIAN_POINT('',(-10.0948919410771,-81.441165552193,62.8640987085368));
#114813=CARTESIAN_POINT('Ctrl Pts',(-10.7325538919677,-83.7450249101666,
64.7715578805454));
#114814=CARTESIAN_POINT('Ctrl Pts',(-10.716052847459,-83.6827202146583,
64.7052522272387));
#114815=CARTESIAN_POINT('Ctrl Pts',(-10.6992857379384,-83.6198066549952,
64.6398096456013));
#114816=CARTESIAN_POINT('Ctrl Pts',(-10.682265385291,-83.5563142176879,
64.5752405343746));
#114817=CARTESIAN_POINT('Ctrl Pts',(-10.675408278814,-83.530734582993,64.5492271326563));
#114818=CARTESIAN_POINT('Ctrl Pts',(-10.6685100674777,-83.5050609864359,
64.5233554972818));
#114819=CARTESIAN_POINT('Ctrl Pts',(-10.6615717516232,-83.4792951642798,
64.4976259928887));
#114820=CARTESIAN_POINT('Ctrl Pts',(-10.6419708779072,-83.4065062286275,
64.4249396556047));
#114821=CARTESIAN_POINT('Ctrl Pts',(-10.6220493826656,-83.332982544654,
64.3533885661189));
#114822=CARTESIAN_POINT('Ctrl Pts',(-10.6018193908424,-83.2587410840879,
64.2829606190104));
#114823=CARTESIAN_POINT('Ctrl Pts',(-10.5971136829087,-83.2414717429507,
64.2665783410361));
#114824=CARTESIAN_POINT('Ctrl Pts',(-10.5923912784162,-83.224163554349,
64.250256840545));
#114825=CARTESIAN_POINT('Ctrl Pts',(-10.5876523724971,-83.2068167290645,
64.2339959799492));
#114826=CARTESIAN_POINT('Ctrl Pts',(-10.5648061772901,-83.1231879414425,
64.1556026119974));
#114827=CARTESIAN_POINT('Ctrl Pts',(-10.5415758864884,-83.0386612172355,
64.0786183411402));
#114828=CARTESIAN_POINT('Ctrl Pts',(-10.5179870208428,-82.9532664129503,
64.003036429589));
#114829=CARTESIAN_POINT('Ctrl Pts',(-10.5156479561116,-82.9447986901722,
63.995541750265));
#114830=CARTESIAN_POINT('Ctrl Pts',(-10.5133053645548,-82.9363224295946,
63.9880608612116));
#114831=CARTESIAN_POINT('Ctrl Pts',(-10.5109592781889,-82.9278376552467,
63.9805937523783));
#114832=CARTESIAN_POINT('Ctrl Pts',(-10.4849535148002,-82.8337861159219,
63.8978227732952));
#114833=CARTESIAN_POINT('Ctrl Pts',(-10.4585177019786,-82.7386893008579,
63.8167450927115));
#114834=CARTESIAN_POINT('Ctrl Pts',(-10.4316909758191,-82.6425707375081,
63.7373428936201));
#114835=CARTESIAN_POINT('Ctrl Pts',(-10.4048642496596,-82.5464521741583,
63.6579406945286));
#114836=CARTESIAN_POINT('Ctrl Pts',(-10.3776466101622,-82.4493118573151,
63.5802139880668));
#114837=CARTESIAN_POINT('Ctrl Pts',(-10.3500932814054,-82.3511651955188,
63.5041452967892));
#114838=CARTESIAN_POINT('Ctrl Pts',(-10.347150821168,-82.3406839700988,
63.4960218101001));
#114839=CARTESIAN_POINT('Ctrl Pts',(-10.3442045436766,-82.3301912664879,
63.4879172374884));
#114840=CARTESIAN_POINT('Ctrl Pts',(-10.3412545142997,-82.3196871110276,
63.479831568023));
#114841=CARTESIAN_POINT('Ctrl Pts',(-10.316580337161,-82.2318298867721,
63.4122026683785));
#114842=CARTESIAN_POINT('Ctrl Pts',(-10.2916437834906,-82.143171673775,
63.3458960280496));
#114843=CARTESIAN_POINT('Ctrl Pts',(-10.2664918373664,-82.0537284697427,
63.2809074057432));
#114844=CARTESIAN_POINT('Ctrl Pts',(-10.2607110531259,-82.0331713382295,
63.2659707800927));
#114845=CARTESIAN_POINT('Ctrl Pts',(-10.2549189010341,-82.0125726968343,
63.2511037585608));
#114846=CARTESIAN_POINT('Ctrl Pts',(-10.2491160027292,-81.9919326250545,
63.2363062330404));
#114847=CARTESIAN_POINT('Ctrl Pts',(-10.2266520827284,-81.9120317036672,
63.17902271504));
#114848=CARTESIAN_POINT('Ctrl Pts',(-10.204027171449,-81.8315100262574,
63.1227805141884));
#114849=CARTESIAN_POINT('Ctrl Pts',(-10.1812787454196,-81.7503678787914,
63.0675722165488));
#114850=CARTESIAN_POINT('Ctrl Pts',(-10.1725838287424,-81.7193536798173,
63.0464704687951));
#114851=CARTESIAN_POINT('Ctrl Pts',(-10.1638710839087,-81.6882489050877,
63.0255198497883));
#114852=CARTESIAN_POINT('Ctrl Pts',(-10.1551422412299,-81.6570549439541,
63.0047209448188));
#114853=CARTESIAN_POINT('Ctrl Pts',(-10.135134576849,-81.585554250444,62.9570470978457));
#114854=CARTESIAN_POINT('Ctrl Pts',(-10.1150423492291,-81.5135849718596,
62.9101703633017));
#114855=CARTESIAN_POINT('Ctrl Pts',(-10.0948919410775,-81.4411655389391,
62.8640987293704));
#114856=CARTESIAN_POINT('',(-8.69365830054091,-75.00000003516,60.98889557741));
#114857=CARTESIAN_POINT('Ctrl Pts',(-10.0948919410769,-81.44116555882,62.86409869812));
#114858=CARTESIAN_POINT('Ctrl Pts',(-10.0518048744405,-81.2863646276699,
62.7656178172554));
#114859=CARTESIAN_POINT('Ctrl Pts',(-10.0025424805627,-81.116825889132,
62.6627172439813));
#114860=CARTESIAN_POINT('Ctrl Pts',(-9.91938589888409,-80.8390231510282,
62.5047510738291));
#114861=CARTESIAN_POINT('Ctrl Pts',(-9.89012320651422,-80.7425066983133,
62.4514990831448));
#114862=CARTESIAN_POINT('Ctrl Pts',(-9.8439134202439,-80.5916925981988,
62.3711580712742));
#114863=CARTESIAN_POINT('Ctrl Pts',(-9.82022959017987,-80.5147758129416,
62.3308723952113));
#114864=CARTESIAN_POINT('Ctrl Pts',(-9.79158531547964,-80.4223627831845,
62.2837716277709));
#114865=CARTESIAN_POINT('Ctrl Pts',(-9.77700989322315,-80.3754828784744,
62.260209105959));
#114866=CARTESIAN_POINT('Ctrl Pts',(-9.7696588608683,-80.3518740598891,
62.2484264570357));
#114867=CARTESIAN_POINT('Ctrl Pts',(-9.76649484959624,-80.341719754058,
62.2433766307136));
#114868=CARTESIAN_POINT('Ctrl Pts',(-9.76438249345169,-80.3349421572503,
62.2400100730806));
#114869=CARTESIAN_POINT('Ctrl Pts',(-9.76289144897654,-80.3301595361113,
62.2376380948878));
#114870=CARTESIAN_POINT('Ctrl Pts',(-9.74223890670972,-80.2639262891045,
62.2048169668438));
#114871=CARTESIAN_POINT('Ctrl Pts',(-9.71522129820358,-80.1778496550703,
62.1627985636355));
#114872=CARTESIAN_POINT('Ctrl Pts',(-9.66420853416412,-80.0148712661353,
62.0868410206361));
#114873=CARTESIAN_POINT('Ctrl Pts',(-9.64545655427094,-79.9548962970397,
62.0593795841153));
#114874=CARTESIAN_POINT('Ctrl Pts',(-9.6147069966111,-79.8562873318557,
62.0153863538377));
#114875=CARTESIAN_POINT('Ctrl Pts',(-9.60402021275448,-79.82197637176,62.0002559306572));
#114876=CARTESIAN_POINT('Ctrl Pts',(-9.58177278243454,-79.7504407061777,
61.9691419096399));
#114877=CARTESIAN_POINT('Ctrl Pts',(-9.57055025010918,-79.7143065643979,
61.9536195698955));
#114878=CARTESIAN_POINT('Ctrl Pts',(-9.50887179058622,-79.5153650542099,
61.8694766597471));
#114879=CARTESIAN_POINT('Ctrl Pts',(-9.46580516087099,-79.3743754823427,
61.8138362640074));
#114880=CARTESIAN_POINT('Ctrl Pts',(-9.41061942315287,-79.1916364045872,
61.7445829366495));
#114881=CARTESIAN_POINT('Ctrl Pts',(-9.39379321172261,-79.1355075403693,
61.723875018136));
#114882=CARTESIAN_POINT('Ctrl Pts',(-9.37090744629091,-79.0586241662255,
61.6960459575867));
#114883=CARTESIAN_POINT('Ctrl Pts',(-9.36005295150348,-79.0220094527361,
61.6829405002834));
#114884=CARTESIAN_POINT('Ctrl Pts',(-9.34841905312621,-78.9825136859927,
61.6690033648935));
#114885=CARTESIAN_POINT('Ctrl Pts',(-9.34285952365626,-78.9635738264959,
61.6623657291019));
#114886=CARTESIAN_POINT('Ctrl Pts',(-9.34014411385095,-78.9543062283972,
61.6591287630642));
#114887=CARTESIAN_POINT('Ctrl Pts',(-9.33899415713361,-78.9503777913378,
61.6577589392433));
#114888=CARTESIAN_POINT('Ctrl Pts',(-9.33823058384251,-78.9477684793878,
61.6568495904088));
#114889=CARTESIAN_POINT('Ctrl Pts',(-9.33816091406803,-78.9475306640759,
61.656766554339));
#114890=CARTESIAN_POINT('Ctrl Pts',(-9.29335597623239,-78.7943239964564,
61.6034329332589));
#114891=CARTESIAN_POINT('Ctrl Pts',(-9.25256248254764,-78.6504854818397,
61.5567280406397));
#114892=CARTESIAN_POINT('Ctrl Pts',(-9.19635544814298,-78.445849160099,
61.4940552038252));
#114893=CARTESIAN_POINT('Ctrl Pts',(-9.16949773247126,-78.3463089295506,
61.4645666950856));
#114894=CARTESIAN_POINT('Ctrl Pts',(-9.14034388353282,-78.2351486053617,
61.4331267605316));
#114895=CARTESIAN_POINT('Ctrl Pts',(-9.12631199723324,-78.1808229019596,
61.4181153888453));
#114896=CARTESIAN_POINT('Ctrl Pts',(-9.11943231362586,-78.1539751249433,
61.410782870149));
#114897=CARTESIAN_POINT('Ctrl Pts',(-9.11651307626751,-78.1425366028503,
61.407677047469));
#114898=CARTESIAN_POINT('Ctrl Pts',(-9.11457340657824,-78.1349259754488,
61.4056146047108));
#114899=CARTESIAN_POINT('Ctrl Pts',(-9.11392192730972,-78.1323679828658,
61.4049221056818));
#114900=CARTESIAN_POINT('Ctrl Pts',(-9.07173282663215,-77.9663764800442,
61.3601144269983));
#114901=CARTESIAN_POINT('Ctrl Pts',(-9.0341765477646,-77.8090390324268,
61.3212393125679));
#114902=CARTESIAN_POINT('Ctrl Pts',(-8.98287367578384,-77.5788683170903,
61.2690076535193));
#114903=CARTESIAN_POINT('Ctrl Pts',(-8.9584801263736,-77.4652406052022,
61.2444124341212));
#114904=CARTESIAN_POINT('Ctrl Pts',(-8.93222228691025,-77.3353009481976,
61.2182124618105));
#114905=CARTESIAN_POINT('Ctrl Pts',(-8.91964369255738,-77.2709961531179,
61.2057156191777));
#114906=CARTESIAN_POINT('Ctrl Pts',(-8.91349197672566,-77.2390110591143,
61.1996154368605));
#114907=CARTESIAN_POINT('Ctrl Pts',(-8.91088500880021,-77.2253391220203,
61.1970325667274));
#114908=CARTESIAN_POINT('Ctrl Pts',(-8.90915358167585,-77.2162325005146,
61.1953176217769));
#114909=CARTESIAN_POINT('Ctrl Pts',(-8.90853926942428,-77.2129958721295,
61.1947092630006));
#114910=CARTESIAN_POINT('Ctrl Pts',(-8.76569916465401,-76.4573161571757,
61.0533061035506));
#114911=CARTESIAN_POINT('Ctrl Pts',(-8.69444127090419,-75.7170145006195,
60.9888893886809));
#114912=CARTESIAN_POINT('Ctrl Pts',(-8.69365830054091,-75.00000003516,60.98889557741));
#114913=CARTESIAN_POINT('',(-8.56753648333091,-75.,60.98888938658));
#114914=CARTESIAN_POINT('',(-15.5675364833309,-75.,60.98888938658));
#114915=CARTESIAN_POINT('Origin',(-8.56753648333091,-75.,72.98888938658));
#114916=CARTESIAN_POINT('',(-10.094867738972,-68.5588861609101,62.8640661515342));
#114917=CARTESIAN_POINT('Ctrl Pts',(-8.69365830112879,-75.0000000361644,
60.9889038049696));
#114918=CARTESIAN_POINT('Ctrl Pts',(-8.69384525821713,-74.8245766453446,
60.9889252073937));
#114919=CARTESIAN_POINT('Ctrl Pts',(-8.69827073512056,-74.647732721061,
60.9928047893908));
#114920=CARTESIAN_POINT('Ctrl Pts',(-8.706920554905,-74.4696329007517,61.0006933496487));
#114921=CARTESIAN_POINT('Ctrl Pts',(-8.71504876833194,-74.3022729572094,
61.0081062094544));
#114922=CARTESIAN_POINT('Ctrl Pts',(-8.72690760767029,-74.1338036400519,
61.0190593571933));
#114923=CARTESIAN_POINT('Ctrl Pts',(-8.7425079218425,-73.9643922544561,
61.0337105002916));
#114924=CARTESIAN_POINT('Ctrl Pts',(-8.74350903028094,-73.9535207318819,
61.034650698215));
#114925=CARTESIAN_POINT('Ctrl Pts',(-8.74452555346398,-73.9426453420439,
61.0356061359183));
#114926=CARTESIAN_POINT('Ctrl Pts',(-8.74555749710937,-73.9317661343774,
61.0365768596762));
#114927=CARTESIAN_POINT('Ctrl Pts',(-8.75602275042763,-73.8214367916468,
61.0464212635574));
#114928=CARTESIAN_POINT('Ctrl Pts',(-8.76806128725323,-73.7107058345274,
61.0578380832004));
#114929=CARTESIAN_POINT('Ctrl Pts',(-8.7816935928635,-73.5996352672253,
61.0708786774647));
#114930=CARTESIAN_POINT('Ctrl Pts',(-8.7903528098044,-73.5290834350178,
61.0791620403823));
#114931=CARTESIAN_POINT('Ctrl Pts',(-8.79965520013409,-73.4583948049494,
61.0881006865537));
#114932=CARTESIAN_POINT('Ctrl Pts',(-8.80959015964689,-73.3875752183467,
61.0977035441218));
#114933=CARTESIAN_POINT('Ctrl Pts',(-8.82237800036828,-73.2964193769703,
61.1100639179001));
#114934=CARTESIAN_POINT('Ctrl Pts',(-8.83622370490817,-73.2050527888017,
61.1235239289185));
#114935=CARTESIAN_POINT('Ctrl Pts',(-8.8511272719821,-73.1135030831726,
61.1381012595064));
#114936=CARTESIAN_POINT('Ctrl Pts',(-8.85857905551907,-73.067728230358,
61.1453899248004));
#114937=CARTESIAN_POINT('Ctrl Pts',(-8.86629530475195,-73.0219075951315,
61.1529579327023));
#114938=CARTESIAN_POINT('Ctrl Pts',(-8.87427601982463,-72.9760447470789,
61.1608075542463));
#114939=CARTESIAN_POINT('Ctrl Pts',(-8.87826637736097,-72.9531133230526,
61.1647323650183));
#114940=CARTESIAN_POINT('Ctrl Pts',(-8.88232285135977,-72.9301713457549,
61.1687275800761));
#114941=CARTESIAN_POINT('Ctrl Pts',(-8.88644544184757,-72.907219264802,
61.1727934881509));
#114942=CARTESIAN_POINT('Ctrl Pts',(-8.88953738471342,-72.8900052040874,
61.175842919207));
#114943=CARTESIAN_POINT('Ctrl Pts',(-8.89266651810446,-72.8727854600641,
61.1789321151613));
#114944=CARTESIAN_POINT('Ctrl Pts',(-8.89583284203163,-72.8555602239495,
61.1820611989636));
#114945=CARTESIAN_POINT('Ctrl Pts',(-8.89688828334068,-72.849818478578,
61.1831042268977));
#114946=CARTESIAN_POINT('Ctrl Pts',(-8.89817259108541,-72.8428627810642,
61.1843739259477));
#114947=CARTESIAN_POINT('Ctrl Pts',(-8.89901156280451,-72.8383331643582,
61.1852035833048));
#114948=CARTESIAN_POINT('Ctrl Pts',(-8.9225926824401,-72.7110184634967,
61.2085229025959));
#114949=CARTESIAN_POINT('Ctrl Pts',(-8.948694109248,-72.5807530056447,61.234507052742));
#114950=CARTESIAN_POINT('Ctrl Pts',(-8.97731851831312,-72.4476737333343,
61.2634710838465));
#114951=CARTESIAN_POINT('Ctrl Pts',(-8.9812829872012,-72.429242308828,61.2674825902474));
#114952=CARTESIAN_POINT('Ctrl Pts',(-8.98529579245517,-72.410756960309,
61.2715512808838));
#114953=CARTESIAN_POINT('Ctrl Pts',(-8.98935688116652,-72.3922181029307,
61.2756780155713));
#114954=CARTESIAN_POINT('Ctrl Pts',(-9.00017444305544,-72.3428359664415,
61.2866704392916));
#114955=CARTESIAN_POINT('Ctrl Pts',(-9.01133391949106,-72.2930733728004,
61.2980748567245));
#114956=CARTESIAN_POINT('Ctrl Pts',(-9.02283815818018,-72.2429398737176,
61.3099074330183));
#114957=CARTESIAN_POINT('Ctrl Pts',(-9.02908502354944,-72.2157171058559,
61.3163325875267));
#114958=CARTESIAN_POINT('Ctrl Pts',(-9.03543353648351,-72.1883849945047,
61.3228839886947));
#114959=CARTESIAN_POINT('Ctrl Pts',(-9.04188256206101,-72.1609442733638,
61.3295644679222));
#114960=CARTESIAN_POINT('Ctrl Pts',(-9.05104534349893,-72.1219564716734,
61.3390560989177));
#114961=CARTESIAN_POINT('Ctrl Pts',(-9.0604123756522,-72.0827501093837,
61.3488081304238));
#114962=CARTESIAN_POINT('Ctrl Pts',(-9.06998365852324,-72.0433292790635,
61.3588282522153));
#114963=CARTESIAN_POINT('Ctrl Pts',(-9.07476929995877,-72.0236188639035,
61.363838313111));
#114964=CARTESIAN_POINT('Ctrl Pts',(-9.07960600407186,-72.0038548320136,
61.3689153973613));
#114965=CARTESIAN_POINT('Ctrl Pts',(-9.08449377085193,-71.9840377054465,
61.3740604684296));
#114966=CARTESIAN_POINT('Ctrl Pts',(-9.08693765424197,-71.974129142163,
61.3766330039637));
#114967=CARTESIAN_POINT('Ctrl Pts',(-9.08939430329864,-71.9642073052274,
61.3792225362478));
#114968=CARTESIAN_POINT('Ctrl Pts',(-9.09186371802004,-71.9542722609874,
61.3818291857182));
#114969=CARTESIAN_POINT('Ctrl Pts',(-9.09309842538075,-71.9493047388673,
61.3831325104534));
#114970=CARTESIAN_POINT('Ctrl Pts',(-9.09433632415762,-71.9443339149221,
61.3844401144878));
#114971=CARTESIAN_POINT('Ctrl Pts',(-9.09557741435042,-71.9393597975172,
61.3857520128741));
#114972=CARTESIAN_POINT('Ctrl Pts',(-9.09681850454321,-71.9343856801124,
61.3870639112604));
#114973=CARTESIAN_POINT('Ctrl Pts',(-9.09837281773138,-71.9281704284257,
61.388708285338));
#114974=CARTESIAN_POINT('Ctrl Pts',(-9.09931025917626,-71.9244275733127,
61.3897006061457));
#114975=CARTESIAN_POINT('Ctrl Pts',(-9.11922873284419,-71.8449005144027,
61.4107851399981));
#114976=CARTESIAN_POINT('Ctrl Pts',(-9.14074565379796,-71.7615529692762,
61.4337570806931));
#114977=CARTESIAN_POINT('Ctrl Pts',(-9.16387259792112,-71.6744787276342,
61.458871924867));
#114978=CARTESIAN_POINT('Ctrl Pts',(-9.17557588230001,-71.6304152055975,
61.4715811769815));
#114979=CARTESIAN_POINT('Ctrl Pts',(-9.18769082592326,-71.5853975145052,
61.4848395475597));
#114980=CARTESIAN_POINT('Ctrl Pts',(-9.20021431489938,-71.5394388953521,
61.4986823135457));
#114981=CARTESIAN_POINT('Ctrl Pts',(-9.21884993753997,-71.4710500074589,
61.5192810910676));
#114982=CARTESIAN_POINT('Ctrl Pts',(-9.23839470040588,-71.4005780245766,
61.5411734447155));
#114983=CARTESIAN_POINT('Ctrl Pts',(-9.25884860323448,-71.3280737128276,
61.5644799762425));
#114984=CARTESIAN_POINT('Ctrl Pts',(-9.26907555464878,-71.2918215569531,
61.576133242006));
#114985=CARTESIAN_POINT('Ctrl Pts',(-9.27952979104853,-71.2550613542374,
61.5881401626345));
#114986=CARTESIAN_POINT('Ctrl Pts',(-9.29021131242184,-71.2178001815926,
61.6005162820495));
#114987=CARTESIAN_POINT('Ctrl Pts',(-9.2955520731085,-71.1991695952702,
61.606704341757));
#114988=CARTESIAN_POINT('Ctrl Pts',(-9.30094965503958,-71.1804137683667,
61.612984707645));
#114989=CARTESIAN_POINT('Ctrl Pts',(-9.30640405821832,-71.1615336159611,
61.6193593546832));
#114990=CARTESIAN_POINT('Ctrl Pts',(-9.30913125980769,-71.1520935397583,
61.6225466782022));
#114991=CARTESIAN_POINT('Ctrl Pts',(-9.31187266670901,-71.1426223823034,
61.6257575724023));
#114992=CARTESIAN_POINT('Ctrl Pts',(-9.31462827892278,-71.1331202606396,
61.6289922858397));
#114993=CARTESIAN_POINT('Ctrl Pts',(-9.31600608502967,-71.1283691998077,
61.6306096425584));
#114994=CARTESIAN_POINT('Ctrl Pts',(-9.31738744246467,-71.123610397931,
61.6322329541106));
#114995=CARTESIAN_POINT('Ctrl Pts',(-9.31877235122784,-71.1188438698163,
61.6338622516649));
#114996=CARTESIAN_POINT('Ctrl Pts',(-9.32015725999101,-71.1140773417016,
61.6354915492193));
#114997=CARTESIAN_POINT('Ctrl Pts',(-9.32207922785804,-71.1074703323387,
61.637755884187));
#114998=CARTESIAN_POINT('Ctrl Pts',(-9.32293773150189,-71.1045211216348,
61.6387681335848));
#114999=CARTESIAN_POINT('Ctrl Pts',(-9.32540804075955,-71.0960348879923,
61.6416808399853));
#115000=CARTESIAN_POINT('Ctrl Pts',(-9.32791662688662,-71.087431771361,
61.6446442765875));
#115001=CARTESIAN_POINT('Ctrl Pts',(-9.33046351585559,-71.0787120910557,
61.6476592445136));
#115002=CARTESIAN_POINT('Ctrl Pts',(-9.34717384114147,-71.0215016291683,
61.6674406701609));
#115003=CARTESIAN_POINT('Ctrl Pts',(-9.36553468648594,-70.9592718360005,
61.6894370377311));
#115004=CARTESIAN_POINT('Ctrl Pts',(-9.38555146037108,-70.8921230086149,
61.713900599354));
#115005=CARTESIAN_POINT('Ctrl Pts',(-9.39641198312577,-70.8556899963845,
61.7271738205629));
#115006=CARTESIAN_POINT('Ctrl Pts',(-9.4077596439782,-70.8178092287548,
61.7411740572641));
#115007=CARTESIAN_POINT('Ctrl Pts',(-9.41959197261567,-70.7784990529737,
61.7559466688392));
#115008=CARTESIAN_POINT('Ctrl Pts',(-9.43807399470082,-70.717096808393,
61.7790213941744));
#115009=CARTESIAN_POINT('Ctrl Pts',(-9.457742507847,-70.6522072039607,61.8039793522644));
#115010=CARTESIAN_POINT('Ctrl Pts',(-9.47859751201244,-70.5839139312709,
61.8310082703903));
#115011=CARTESIAN_POINT('Ctrl Pts',(-9.48902501409516,-70.549767294926,
61.8445227294532));
#115012=CARTESIAN_POINT('Ctrl Pts',(-9.49974913892252,-70.5147699709371,
61.8585552215054));
#115013=CARTESIAN_POINT('Ctrl Pts',(-9.51076988645421,-70.478933866873,
61.8731309024725));
#115014=CARTESIAN_POINT('Ctrl Pts',(-9.51628026022006,-70.4610158148409,
61.8804187429561));
#115015=CARTESIAN_POINT('Ctrl Pts',(-9.52186478966094,-70.442888076038,
61.8878424007396));
#115016=CARTESIAN_POINT('Ctrl Pts',(-9.5275234747752,-70.424552245374,61.8954051157619));
#115017=CARTESIAN_POINT('Ctrl Pts',(-9.53249846447252,-70.4084317921585,
61.9020540860722));
#115018=CARTESIAN_POINT('Ctrl Pts',(-9.53721923892211,-70.3931570372304,
61.9083908527476));
#115019=CARTESIAN_POINT('Ctrl Pts',(-9.54250747549523,-70.3760742064197,
61.9155244139028));
#115020=CARTESIAN_POINT('Ctrl Pts',(-9.54323421933363,-70.3737265727875,
61.9165047542382));
#115021=CARTESIAN_POINT('Ctrl Pts',(-9.54397168194754,-70.3713448258,61.9175002152205));
#115022=CARTESIAN_POINT('Ctrl Pts',(-9.54472199713705,-70.3689221118314,
61.9185137476522));
#115023=CARTESIAN_POINT('Ctrl Pts',(-9.56686698111811,-70.2974175457824,
61.9484273889841));
#115024=CARTESIAN_POINT('Ctrl Pts',(-9.587521094413,-70.2309884594451,61.9770285730077));
#115025=CARTESIAN_POINT('Ctrl Pts',(-9.60666602037937,-70.1695285933851,
62.0040558945936));
#115026=CARTESIAN_POINT('Ctrl Pts',(-9.61672698109021,-70.1372304639063,
62.0182591785902));
#115027=CARTESIAN_POINT('Ctrl Pts',(-9.62637177798907,-70.1063049602051,
62.0320284265364));
#115028=CARTESIAN_POINT('Ctrl Pts',(-9.63560123225895,-70.0767385813395,
62.0453297677685));
#115029=CARTESIAN_POINT('Ctrl Pts',(-9.64820959587144,-70.0363479315196,
62.0635007388664));
#115030=CARTESIAN_POINT('Ctrl Pts',(-9.66004264588526,-69.9984935808949,
62.0807981351448));
#115031=CARTESIAN_POINT('Ctrl Pts',(-9.67110723157983,-69.9631454708437,
62.097144337565));
#115032=CARTESIAN_POINT('Ctrl Pts',(-9.68741261949328,-69.9110545329359,
62.1212330091818));
#115033=CARTESIAN_POINT('Ctrl Pts',(-9.70203866039361,-69.8644019000139,
62.1432555275304));
#115034=CARTESIAN_POINT('Ctrl Pts',(-9.7149849350291,-69.8230959229707,
62.1630072776116));
#115035=CARTESIAN_POINT('Ctrl Pts',(-9.7157652165445,-69.8206063812863,
62.1641977301487));
#115036=CARTESIAN_POINT('Ctrl Pts',(-9.71653940047268,-69.8181362679303,
62.1653799476744));
#115037=CARTESIAN_POINT('Ctrl Pts',(-9.71730748819526,-69.815685565258,
62.1665538906621));
#115038=CARTESIAN_POINT('Ctrl Pts',(-9.72406351089009,-69.7941294299548,
62.1768797756291));
#115039=CARTESIAN_POINT('Ctrl Pts',(-9.73034752354787,-69.774074824194,
62.1865652270092));
#115040=CARTESIAN_POINT('Ctrl Pts',(-9.73615952618739,-69.7555102227944,
62.1955855670669));
#115041=CARTESIAN_POINT('Ctrl Pts',(-9.73906552750716,-69.7462279220946,
62.2000957370957));
#115042=CARTESIAN_POINT('Ctrl Pts',(-9.74185352632141,-69.7373181496336,
62.2044396850447));
#115043=CARTESIAN_POINT('Ctrl Pts',(-9.74452352263516,-69.7287795988378,
62.2086146753113));
#115044=CARTESIAN_POINT('Ctrl Pts',(-9.74585852079203,-69.7245103234399,
62.2107021704445));
#115045=CARTESIAN_POINT('Ctrl Pts',(-9.74716401832364,-69.7203338551499,
62.212747429656));
#115046=CARTESIAN_POINT('Ctrl Pts',(-9.74844001523034,-69.7162500405712,
62.2147501321042));
#115047=CARTESIAN_POINT('Ctrl Pts',(-9.74907801368369,-69.7142081332818,
62.2157514833284));
#115048=CARTESIAN_POINT('Ctrl Pts',(-9.74970863698081,-69.7121893895273,
62.2167421955798));
#115049=CARTESIAN_POINT('Ctrl Pts',(-9.75033188512175,-69.7101937906893,
62.2177222301046));
#115050=CARTESIAN_POINT('Ctrl Pts',(-9.7509551332627,-69.7081981918514,
62.2187022646294));
#115051=CARTESIAN_POINT('Ctrl Pts',(-9.75108437475398,-69.7077846654699,
62.2189049711921));
#115052=CARTESIAN_POINT('Ctrl Pts',(-9.75217950407609,-69.7042764107142,
62.2206302626284));
#115053=CARTESIAN_POINT('Ctrl Pts',(-9.78388530258222,-69.6027066543888,
62.2705802927656));
#115054=CARTESIAN_POINT('Ctrl Pts',(-9.81434516651739,-69.5047221369212,
62.3205516446024));
#115055=CARTESIAN_POINT('Ctrl Pts',(-9.84346562989802,-69.4102197139354,
62.3703005384937));
#115056=CARTESIAN_POINT('Ctrl Pts',(-9.86510654357278,-69.3399901042222,
62.4072714995682));
#115057=CARTESIAN_POINT('Ctrl Pts',(-9.88600896198795,-69.2716836485838,
62.4441198786041));
#115058=CARTESIAN_POINT('Ctrl Pts',(-9.90615231348221,-69.2052596148448,
62.480750451818));
#115059=CARTESIAN_POINT('Ctrl Pts',(-9.93783413302433,-69.1007867196179,
62.5383636653202));
#115060=CARTESIAN_POINT('Ctrl Pts',(-9.96763719432755,-69.0009707238969,
62.5954366889229));
#115061=CARTESIAN_POINT('Ctrl Pts',(-9.99559863800527,-68.9056769114017,
62.6516169537898));
#115062=CARTESIAN_POINT('Ctrl Pts',(-10.0249484751374,-68.8056513938114,
62.7105867853512));
#115063=CARTESIAN_POINT('Ctrl Pts',(-10.0522697332514,-68.7106081000212,
62.7685727517803));
#115064=CARTESIAN_POINT('Ctrl Pts',(-10.0776526495244,-68.6203935392705,
62.8251989857031));
#115065=CARTESIAN_POINT('Ctrl Pts',(-10.0834929971886,-68.5996360977893,
62.8382280990432));
#115066=CARTESIAN_POINT('Ctrl Pts',(-10.0892308978382,-68.5791343120549,
62.8511853626773));
#115067=CARTESIAN_POINT('Ctrl Pts',(-10.0948677389681,-68.558886345915,
62.8640664423475));
#115068=CARTESIAN_POINT('',(-10.0948705696752,-68.5588302431943,83.1136771106412));
#115069=CARTESIAN_POINT('Ctrl Pts',(-10.094867738974,-68.5588860050051,
62.8640659064653));
#115070=CARTESIAN_POINT('Ctrl Pts',(-10.1443275500759,-68.3811321371765,
62.9771476730743));
#115071=CARTESIAN_POINT('Ctrl Pts',(-10.192135551363,-68.2091735334229,
63.093117860736));
#115072=CARTESIAN_POINT('Ctrl Pts',(-10.2382917428353,-68.0429516821774,
63.2113907952489));
#115073=CARTESIAN_POINT('Ctrl Pts',(-10.2849968592397,-67.8747529928199,
63.331070322474));
#115074=CARTESIAN_POINT('Ctrl Pts',(-10.3300106430149,-67.7124280221737,
63.4531075205968));
#115075=CARTESIAN_POINT('Ctrl Pts',(-10.373333094161,-67.5558738575396,
63.5769296557302));
#115076=CARTESIAN_POINT('Ctrl Pts',(-10.4175331184007,-67.3961484106037,
63.7032600278475));
#115077=CARTESIAN_POINT('Ctrl Pts',(-10.4599725941102,-67.242429666187,
63.8314481853243));
#115078=CARTESIAN_POINT('Ctrl Pts',(-10.5006515212892,-67.0945688096429,
63.9609240734804));
#115079=CARTESIAN_POINT('Ctrl Pts',(-10.5377636714851,-66.959672569828,
64.0790473609223));
#115080=CARTESIAN_POINT('Ctrl Pts',(-10.5734104720686,-66.8296513193455,
64.1982428928792));
#115081=CARTESIAN_POINT('Ctrl Pts',(-10.6075919230397,-66.7043672961587,
64.3181063744779));
#115082=CARTESIAN_POINT('Ctrl Pts',(-10.6461222346423,-66.5631435530154,
64.4532199277225));
#115083=CARTESIAN_POINT('Ctrl Pts',(-10.6827906078484,-66.4279393536557,
64.5891814235258));
#115084=CARTESIAN_POINT('Ctrl Pts',(-10.717597042658,-66.2985272376477,
64.725453553584));
#115085=CARTESIAN_POINT('Ctrl Pts',(-10.7531375112871,-66.1663859461206,
64.8645995301782));
#115086=CARTESIAN_POINT('Ctrl Pts',(-10.7867366804925,-66.0402832831347,
65.0040692609461));
#115087=CARTESIAN_POINT('Ctrl Pts',(-10.8183945502742,-65.9199491500656,
65.1433379998));
#115088=CARTESIAN_POINT('Ctrl Pts',(-10.8430359460974,-65.8262852041199,
65.2517399909494));
#115089=CARTESIAN_POINT('Ctrl Pts',(-10.8665011999206,-65.736115520797,
65.3600211773868));
#115090=CARTESIAN_POINT('Ctrl Pts',(-10.888790311744,-65.6493033632878,
65.4679537793447));
#115091=CARTESIAN_POINT('Ctrl Pts',(-10.9019518551797,-65.5980414740365,
65.5316871232325));
#115092=CARTESIAN_POINT('Ctrl Pts',(-10.9147033004037,-65.5479501463495,
65.5952992464033));
#115093=CARTESIAN_POINT('Ctrl Pts',(-10.927044647416,-65.4990001414469,
65.6587460259236));
#115094=CARTESIAN_POINT('Ctrl Pts',(-10.9332153209221,-65.4745251389956,
65.6904694156838));
#115095=CARTESIAN_POINT('Ctrl Pts',(-10.9392834698753,-65.4503354754091,
65.7221514757892));
#115096=CARTESIAN_POINT('Ctrl Pts',(-10.9452490942756,-65.4264274089262,
65.7537869102193));
#115097=CARTESIAN_POINT('Ctrl Pts',(-10.9482319064758,-65.4144733756847,
65.7696046274344));
#115098=CARTESIAN_POINT('Ctrl Pts',(-10.9511890875377,-65.4025897422853,
65.7854106886726));
#115099=CARTESIAN_POINT('Ctrl Pts',(-10.9541206374614,-65.3907760409084,
65.8012044391147));
#115100=CARTESIAN_POINT('Ctrl Pts',(-10.9555864124233,-65.3848691902199,
65.8091013143357));
#115101=CARTESIAN_POINT('Ctrl Pts',(-10.9570457796006,-65.378979822572,
65.8169951118837));
#115102=CARTESIAN_POINT('Ctrl Pts',(-10.9584987389933,-65.3731078792483,
65.8248857506646));
#115103=CARTESIAN_POINT('Ctrl Pts',(-10.9595884585378,-65.3687039217556,
65.8308037297502));
#115104=CARTESIAN_POINT('Ctrl Pts',(-10.9606745737036,-65.3643097654482,
65.8367199320315));
#115105=CARTESIAN_POINT('Ctrl Pts',(-10.9617570844905,-65.359925385512,
65.8426343234645));
#115106=CARTESIAN_POINT('Ctrl Pts',(-10.9621179214195,-65.3584639255333,
65.8446057872755));
#115107=CARTESIAN_POINT('Ctrl Pts',(-10.9621766445903,-65.3582264482039,
65.8449252842859));
#115108=CARTESIAN_POINT('Ctrl Pts',(-10.9628383938178,-65.3555442634409,
65.8485481100336));
#115109=CARTESIAN_POINT('Ctrl Pts',(-10.9998963505593,-65.2053419167105,
66.0514263519079));
#115110=CARTESIAN_POINT('Ctrl Pts',(-11.0349672381504,-65.0601785208779,
66.2608881377162));
#115111=CARTESIAN_POINT('Ctrl Pts',(-11.0680510565911,-64.9207073657571,
66.4767576316708));
#115112=CARTESIAN_POINT('Ctrl Pts',(-11.0993629451878,-64.7887061193043,
66.6810654130789));
#115113=CARTESIAN_POINT('Ctrl Pts',(-11.1288949147412,-64.6618040411431,
66.8911126211767));
#115114=CARTESIAN_POINT('Ctrl Pts',(-11.1566469652512,-64.5405622102097,
67.106699222916));
#115115=CARTESIAN_POINT('Ctrl Pts',(-11.1841387787951,-64.4204572900871,
67.3202642225704));
#115116=CARTESIAN_POINT('Ctrl Pts',(-11.2098838981534,-64.3059072327915,
67.5392652961144));
#115117=CARTESIAN_POINT('Ctrl Pts',(-11.2338823233261,-64.1974604243281,
67.7634574698823));
#115118=CARTESIAN_POINT('Ctrl Pts',(-11.2576587098004,-64.0900169895454,
67.9855753684387));
#115119=CARTESIAN_POINT('Ctrl Pts',(-11.2797205741621,-63.9885646684362,
68.2127888114342));
#115120=CARTESIAN_POINT('Ctrl Pts',(-11.300067916411,-63.8936355732867,
68.4448087071646));
#115121=CARTESIAN_POINT('Ctrl Pts',(-11.3202294713136,-63.7995732559436,
68.6747100775266));
#115122=CARTESIAN_POINT('Ctrl Pts',(-11.3387076710504,-63.7119158685469,
68.9093305624892));
#115123=CARTESIAN_POINT('Ctrl Pts',(-11.3555025156215,-63.6311757184616,
69.1483380647638));
#115124=CARTESIAN_POINT('Ctrl Pts',(-11.3720713949053,-63.5515218821634,
69.3841298541042));
#115125=CARTESIAN_POINT('Ctrl Pts',(-11.3870019115129,-63.4786006761391,
69.6241913779256));
#115126=CARTESIAN_POINT('Ctrl Pts',(-11.4002940654443,-63.4128946261226,
69.8681540478078));
#115127=CARTESIAN_POINT('Ctrl Pts',(-11.4134848783109,-63.3476895273517,
70.110256715402));
#115128=CARTESIAN_POINT('Ctrl Pts',(-11.4250622154367,-63.289590271564,
70.3562012670786));
#115129=CARTESIAN_POINT('Ctrl Pts',(-11.4350260768217,-63.2390549508833,
70.6055783385509));
#115130=CARTESIAN_POINT('Ctrl Pts',(-11.4448755988908,-63.1890995433278,
70.8520937078527));
#115131=CARTESIAN_POINT('Ctrl Pts',(-11.4531484633147,-63.1465357405352,
71.1019632110204));
#115132=CARTESIAN_POINT('Ctrl Pts',(-11.4598446700932,-63.1117886989206,
71.3547437196065));
#115133=CARTESIAN_POINT('Ctrl Pts',(-11.4641055045612,-63.0896789586643,
71.5155893952958));
#115134=CARTESIAN_POINT('Ctrl Pts',(-11.4677279741092,-63.070733747897,
71.6776127373646));
#115135=CARTESIAN_POINT('Ctrl Pts',(-11.4707120787369,-63.0550580966133,
71.8406895238746));
#115136=CARTESIAN_POINT('Ctrl Pts',(-11.4737205646426,-63.0392543692532,
72.0050987102059));
#115137=CARTESIAN_POINT('Ctrl Pts',(-11.4760802116421,-63.0267738882719,
72.1705786358204));
#115138=CARTESIAN_POINT('Ctrl Pts',(-11.4777910197354,-63.0177200726439,
72.3369938869189));
#115139=CARTESIAN_POINT('Ctrl Pts',(-11.478646423782,-63.0131931648298,
72.4202015124681));
#115140=CARTESIAN_POINT('Ctrl Pts',(-11.4793396181021,-63.0095228482124,
72.5036429658301));
#115141=CARTESIAN_POINT('Ctrl Pts',(-11.4798706026955,-63.0067216199527,
72.5873004192394));
#115142=CARTESIAN_POINT('Ctrl Pts',(-11.4801360949923,-63.0053210058228,
72.629129145944));
#115143=CARTESIAN_POINT('Ctrl Pts',(-11.4803610348574,-63.0041376585083,
72.6710118723181));
#115144=CARTESIAN_POINT('Ctrl Pts',(-11.4805454222909,-63.0031731096894,
72.7129463418755));
#115145=CARTESIAN_POINT('Ctrl Pts',(-11.4806885551879,-63.0024243674126,
72.7454984632382));
#115146=CARTESIAN_POINT('Ctrl Pts',(-11.4808055767655,-63.001818854722,
72.7774000278934));
#115147=CARTESIAN_POINT('Ctrl Pts',(-11.4809003880803,-63.0013299265603,
72.8102375779043));
#115148=CARTESIAN_POINT('Ctrl Pts',(-11.4809277151094,-63.0011890050454,
72.8197021938854));
#115149=CARTESIAN_POINT('Ctrl Pts',(-11.4809531970458,-63.001058095518,
72.8292445713027));
#115150=CARTESIAN_POINT('Ctrl Pts',(-11.4809769272963,-63.0009373700998,
72.8389027080638));
#115151=CARTESIAN_POINT('Ctrl Pts',(-11.4816147494037,-62.9976925101056,
73.098494284336));
#115152=CARTESIAN_POINT('Ctrl Pts',(-11.480706716154,-63.0028956745713,
73.3564745512392));
#115153=CARTESIAN_POINT('Ctrl Pts',(-11.4782528275472,-63.0162050441979,
73.6123141673606));
#115154=CARTESIAN_POINT('Ctrl Pts',(-11.4757031884669,-63.0300337440175,
73.878136618204));
#115155=CARTESIAN_POINT('Ctrl Pts',(-11.4714847021596,-63.0526134452692,
74.1416477523053));
#115156=CARTESIAN_POINT('Ctrl Pts',(-11.4655973686252,-63.0835298833964,
74.402303678319));
#115157=CARTESIAN_POINT('Ctrl Pts',(-11.4598014315056,-63.1139663671286,
74.6589131175824));
#115158=CARTESIAN_POINT('Ctrl Pts',(-11.4523880601533,-63.1524823556258,
74.9127554294561));
#115159=CARTESIAN_POINT('Ctrl Pts',(-11.4433572545684,-63.1986578291045,
75.1633601188373));
#115160=CARTESIAN_POINT('Ctrl Pts',(-11.4342487987822,-63.2452303363555,
75.4161195998789));
#115161=CARTESIAN_POINT('Ctrl Pts',(-11.4234949745895,-63.299594321962,
75.6655854918157));
#115162=CARTESIAN_POINT('Ctrl Pts',(-11.4110957819905,-63.3612984860316,
75.9113245131054));
#115163=CARTESIAN_POINT('Ctrl Pts',(-11.398588636057,-63.423539876232,76.1592030565097));
#115164=CARTESIAN_POINT('Ctrl Pts',(-11.3844073462561,-63.4932495223862,
76.4032895248276));
#115165=CARTESIAN_POINT('Ctrl Pts',(-11.3685519125877,-63.5699480453472,
76.6431899097907));
#115166=CARTESIAN_POINT('Ctrl Pts',(-11.3524740491355,-63.6477225424026,
76.8864557650327));
#115167=CARTESIAN_POINT('Ctrl Pts',(-11.3346747404995,-63.7326830920559,
77.1254172171987));
#115168=CARTESIAN_POINT('Ctrl Pts',(-11.3151539866796,-63.8243176890293,
77.359715954205));
#115169=CARTESIAN_POINT('Ctrl Pts',(-11.2954837390822,-63.9166540417941,
77.5958089970854));
#115170=CARTESIAN_POINT('Ctrl Pts',(-11.2740655790092,-64.0157667566476,
77.8271676705252));
#115171=CARTESIAN_POINT('Ctrl Pts',(-11.2508995064605,-64.1211241869361,
78.0534783179675));
#115172=CARTESIAN_POINT('Ctrl Pts',(-11.2274340048623,-64.2278433964014,
78.2827141043994));
#115173=CARTESIAN_POINT('Ctrl Pts',(-11.2021751140965,-64.340969500323,
78.5067705421234));
#115174=CARTESIAN_POINT('Ctrl Pts',(-11.1751228341631,-64.4599465123221,
78.7253754605533));
#115175=CARTESIAN_POINT('Ctrl Pts',(-11.1504541131106,-64.5684405367777,
78.9247192410678));
#115176=CARTESIAN_POINT('Ctrl Pts',(-11.1242941090657,-64.6817996566903,
79.1195305579161));
#115177=CARTESIAN_POINT('Ctrl Pts',(-11.0966428220287,-64.7996028657007,
79.3096407899006));
#115178=CARTESIAN_POINT('Ctrl Pts',(-11.0779169478987,-64.8793809990325,
79.438386344138));
#115179=CARTESIAN_POINT('Ctrl Pts',(-11.0585071407615,-64.961197299292,
79.5649766295904));
#115180=CARTESIAN_POINT('Ctrl Pts',(-11.0384134006173,-65.0449218093244,
79.6893683409186));
#115181=CARTESIAN_POINT('Ctrl Pts',(-11.0283665305452,-65.0867840643406,
79.7515641965827));
#115182=CARTESIAN_POINT('Ctrl Pts',(-11.0181486772213,-65.1291233283142,
79.8132104383628));
#115183=CARTESIAN_POINT('Ctrl Pts',(-11.0077598406456,-65.1719235132878,
79.8743024149563));
#115184=CARTESIAN_POINT('Ctrl Pts',(-11.0025654223577,-65.1933236057745,
79.904848403253));
#115185=CARTESIAN_POINT('Ctrl Pts',(-10.9973282582569,-65.2148389261161,
79.935255826801));
#115186=CARTESIAN_POINT('Ctrl Pts',(-10.9920483483432,-65.236467460282,
79.9655241301987));
#115187=CARTESIAN_POINT('Ctrl Pts',(-10.9894083933863,-65.2472817273649,
79.9806582818975));
#115188=CARTESIAN_POINT('Ctrl Pts',(-10.9867577519762,-65.2581242977531,
79.9957576536675));
#115189=CARTESIAN_POINT('Ctrl Pts',(-10.9840964241129,-65.2689949201948,
80.0108221786826));
#115190=CARTESIAN_POINT('Ctrl Pts',(-10.9821004282154,-65.2771478870261,
80.0221205724439));
#115191=CARTESIAN_POINT('Ctrl Pts',(-10.9800984211879,-65.2853166331253,
80.0333993649144));
#115192=CARTESIAN_POINT('Ctrl Pts',(-10.9780904030305,-65.2935010525828,
80.0446585284801));
#115193=CARTESIAN_POINT('Ctrl Pts',(-10.9774210636447,-65.296229192402,
80.0484115830019));
#115194=CARTESIAN_POINT('Ctrl Pts',(-10.9764432355883,-65.3002128087954,
80.053882998953));
#115195=CARTESIAN_POINT('Ctrl Pts',(-10.9760803811631,-65.3016906925888,
80.0559111480989));
#115196=CARTESIAN_POINT('Ctrl Pts',(-10.9506866377528,-65.4051178502617,
80.1978476808771));
#115197=CARTESIAN_POINT('Ctrl Pts',(-10.9232759588804,-65.5140065031049,
80.340734749093));
#115198=CARTESIAN_POINT('Ctrl Pts',(-10.8938483445461,-65.6286728917096,
80.4841030746226));
#115199=CARTESIAN_POINT('Ctrl Pts',(-10.8648132081499,-65.7418099674972,
80.625559287802));
#115200=CARTESIAN_POINT('Ctrl Pts',(-10.8338145775144,-65.8605720396774,
80.7674840000695));
#115201=CARTESIAN_POINT('Ctrl Pts',(-10.8008524526395,-65.9852439685844,
80.9093801348895));
#115202=CARTESIAN_POINT('Ctrl Pts',(-10.7685610860177,-66.1073789031209,
81.0483887737158));
#115203=CARTESIAN_POINT('Ctrl Pts',(-10.7343853237954,-66.2351859267227,
81.1873698930677));
#115204=CARTESIAN_POINT('Ctrl Pts',(-10.6983251659726,-66.3689098151028,
81.3258122133891));
#115205=CARTESIAN_POINT('Ctrl Pts',(-10.6720325297249,-66.4664122601025,
81.4267550208881));
#115206=CARTESIAN_POINT('Ctrl Pts',(-10.6447380840791,-66.5670598666787,
81.5274104787523));
#115207=CARTESIAN_POINT('Ctrl Pts',(-10.6164418290353,-66.6709380618347,
81.6275656295125));
#115208=CARTESIAN_POINT('Ctrl Pts',(-10.5788107064715,-66.8090854275401,
81.7607617272937));
#115209=CARTESIAN_POINT('Ctrl Pts',(-10.5394077560457,-66.9529478270377,
81.893074375948));
#115210=CARTESIAN_POINT('Ctrl Pts',(-10.498232977758,-67.1027000784011,
82.0239684647239));
#115211=CARTESIAN_POINT('Ctrl Pts',(-10.4575611058947,-67.2506232641955,
82.1532638204671));
#115212=CARTESIAN_POINT('Ctrl Pts',(-10.415160423859,-67.4042936052472,
82.2811749400427));
#115213=CARTESIAN_POINT('Ctrl Pts',(-10.371030931651,-67.5638460348357,
82.4071490032168));
#115214=CARTESIAN_POINT('Ctrl Pts',(-10.3277609374189,-67.7202909056594,
82.5306695042285));
#115215=CARTESIAN_POINT('Ctrl Pts',(-10.2828288203227,-67.8823912045507,
82.6523274841528));
#115216=CARTESIAN_POINT('Ctrl Pts',(-10.2362345803624,-68.0502377910592,
82.771568224157));
#115217=CARTESIAN_POINT('Ctrl Pts',(-10.1907005843092,-68.2142650573938,
82.888095661655));
#115218=CARTESIAN_POINT('Ctrl Pts',(-10.1435792474133,-68.3837802585928,
83.0023143992325));
#115219=CARTESIAN_POINT('Ctrl Pts',(-10.0948705696749,-68.5588301155626,
83.1136773112635));
#115220=CARTESIAN_POINT('Ctrl Pts',(-10.0948705696749,-68.55883030701,83.11367701033));
#115221=CARTESIAN_POINT('Ctrl Pts',(-10.0502938077784,-68.718948701588,
83.2155412734439));
#115222=CARTESIAN_POINT('Ctrl Pts',(-9.99901505528794,-68.8951734040083,
83.3223532112927));
#115223=CARTESIAN_POINT('Ctrl Pts',(-9.91204394066144,-69.1852539436349,
83.4865593135653));
#115224=CARTESIAN_POINT('Ctrl Pts',(-9.8813780714708,-69.2862378191267,
83.5419522481948));
#115225=CARTESIAN_POINT('Ctrl Pts',(-9.83286602121212,-69.4443386154877,
83.6255326581122));
#115226=CARTESIAN_POINT('Ctrl Pts',(-9.8079816844646,-69.5250451157206,
83.6674449107169));
#115227=CARTESIAN_POINT('Ctrl Pts',(-9.77785041292734,-69.6221403905299,
83.7164402392164));
#115228=CARTESIAN_POINT('Ctrl Pts',(-9.76250989082578,-69.6714272090312,
83.7409472746058));
#115229=CARTESIAN_POINT('Ctrl Pts',(-9.75477090819175,-69.6962560014835,
83.7532012372322));
#115230=CARTESIAN_POINT('Ctrl Pts',(-9.75143947529504,-69.7069366999104,
83.7584528258423));
#115231=CARTESIAN_POINT('Ctrl Pts',(-9.74921524757422,-69.714066014065,
83.7619538376723));
#115232=CARTESIAN_POINT('Ctrl Pts',(-9.74760316095839,-69.7192316813361,
83.7644863914133));
#115233=CARTESIAN_POINT('Ctrl Pts',(-9.72724051790498,-69.7844701446807,
83.7964427918803));
#115234=CARTESIAN_POINT('Ctrl Pts',(-9.69988686319735,-69.871555510311,
83.8385058175468));
#115235=CARTESIAN_POINT('Ctrl Pts',(-9.64744428897033,-70.0391065537308,
83.9156142440336));
#115236=CARTESIAN_POINT('Ctrl Pts',(-9.62806141553372,-70.1011166189966,
83.9436375961161));
#115237=CARTESIAN_POINT('Ctrl Pts',(-9.59613408233741,-70.2035640260259,
83.9886890950437));
#115238=CARTESIAN_POINT('Ctrl Pts',(-9.57945715997892,-70.2571461972045,
84.0119674793892));
#115239=CARTESIAN_POINT('Ctrl Pts',(-9.5617103539799,-70.3143052101089,
84.0362741519362));
#115240=CARTESIAN_POINT('Ctrl Pts',(-9.54964139806043,-70.353210584381,
84.0526949680574));
#115241=CARTESIAN_POINT('Ctrl Pts',(-9.54306984809565,-70.3744133871288,
84.0615750413791));
#115242=CARTESIAN_POINT('Ctrl Pts',(-9.49038354358189,-70.5445482096079,
84.1323077681235));
#115243=CARTESIAN_POINT('Ctrl Pts',(-9.44837032070452,-70.682363037354,
84.1860064293701));
#115244=CARTESIAN_POINT('Ctrl Pts',(-9.39257905809074,-70.8678500066756,
84.2551971750906));
#115245=CARTESIAN_POINT('Ctrl Pts',(-9.3751867325032,-70.9261439148029,
84.2763632109177));
#115246=CARTESIAN_POINT('Ctrl Pts',(-9.35090538704745,-71.0081767458892,
84.3055226886024));
#115247=CARTESIAN_POINT('Ctrl Pts',(-9.33921650005097,-71.0478414726449,
84.3194545615856));
#115248=CARTESIAN_POINT('Ctrl Pts',(-9.32637009025168,-71.0917316627996,
84.3346257467507));
#115249=CARTESIAN_POINT('Ctrl Pts',(-9.32014454160952,-71.1130781654726,
84.3419466755683));
#115250=CARTESIAN_POINT('Ctrl Pts',(-9.31751880424662,-71.1220981592162,
84.3450281366084));
#115251=CARTESIAN_POINT('Ctrl Pts',(-9.3157777248741,-71.1280829053576,
84.3470700511436));
#115252=CARTESIAN_POINT('Ctrl Pts',(-9.31544127521446,-71.1292389848438,
84.3474647690699));
#115253=CARTESIAN_POINT('Ctrl Pts',(-9.26955439872479,-71.2871697016937,
84.4012099517279));
#115254=CARTESIAN_POINT('Ctrl Pts',(-9.22873605973666,-71.4324726572279,
84.4472137338849));
#115255=CARTESIAN_POINT('Ctrl Pts',(-9.1730255903936,-71.6380168485605,
84.5085326682448));
#115256=CARTESIAN_POINT('Ctrl Pts',(-9.14654961550685,-71.7376891690263,
84.5372682003853));
#115257=CARTESIAN_POINT('Ctrl Pts',(-9.11807468276234,-71.848434346492,
84.567725331802));
#115258=CARTESIAN_POINT('Ctrl Pts',(-9.10444064254594,-71.90240961628,84.5822224138533));
#115259=CARTESIAN_POINT('Ctrl Pts',(-9.0977744789767,-71.9290463969955,
84.5892924535069));
#115260=CARTESIAN_POINT('Ctrl Pts',(-9.09494987813394,-71.9403868187052,
84.5922846825071));
#115261=CARTESIAN_POINT('Ctrl Pts',(-9.09307399455015,-71.9479303399745,
84.5942711555288));
#115262=CARTESIAN_POINT('Ctrl Pts',(-9.09244019876047,-71.9504811837714,
84.5949421765475));
#115263=CARTESIAN_POINT('Ctrl Pts',(-9.05180689196814,-72.1144096422424,
84.637939790309));
#115264=CARTESIAN_POINT('Ctrl Pts',(-9.01546444294639,-72.2711841971463,
84.6755717545402));
#115265=CARTESIAN_POINT('Ctrl Pts',(-8.96554008757908,-72.5027421373977,
84.7264337754863));
#115266=CARTESIAN_POINT('Ctrl Pts',(-8.94172523943675,-72.6176208899744,
84.7504682609118));
#115267=CARTESIAN_POINT('Ctrl Pts',(-8.91594907663469,-72.7500075021818,
84.7761749791267));
#115268=CARTESIAN_POINT('Ctrl Pts',(-8.90356295190799,-72.815783810216,
84.7884586800507));
#115269=CARTESIAN_POINT('Ctrl Pts',(-8.8983621748839,-72.8438835247074,
84.7936025209064));
#115270=CARTESIAN_POINT('Ctrl Pts',(-8.89491889289996,-72.8625965537548,
84.797005110384));
#115271=CARTESIAN_POINT('Ctrl Pts',(-8.89356984042164,-72.8699597621748,
84.7983373347971));
#115272=CARTESIAN_POINT('Ctrl Pts',(-8.75977543568638,-73.6057342558853,
84.9303191698575));
#115273=CARTESIAN_POINT('Ctrl Pts',(-8.693708869803,-74.3160938546077,84.98888938658));
#115274=CARTESIAN_POINT('Ctrl Pts',(-8.69331176731091,-74.99999999459,84.98885921934));
#115275=CARTESIAN_POINT('Origin',(27.4324635166691,25.,72.98888938658));
#115276=CARTESIAN_POINT('',(-8.23395173818595,-10.,84.5714980248889));
#115277=CARTESIAN_POINT('',(-7.08815755488265,-10.,58.3404518987683));
#115278=CARTESIAN_POINT('Origin',(27.4324635166691,-10.,72.98888938658));
#115279=CARTESIAN_POINT('',(-8.23395173885291,-22.5,84.57149802283));
#115280=CARTESIAN_POINT('',(-8.23395173707291,-10.,84.57149802832));
#115281=CARTESIAN_POINT('',(-7.08815755056573,-22.5,87.637326884565));
#115282=CARTESIAN_POINT('Origin',(27.4324635166691,-22.5,72.98888938658));
#115283=CARTESIAN_POINT('',(-7.08838231939817,-64.8259873690431,87.6374222559034));
#115284=CARTESIAN_POINT('',(-7.08815755142093,25.,87.63732688255));
#115285=CARTESIAN_POINT('',(-10.0675288996373,-56.3106244902745,72.9888900918571));
#115286=CARTESIAN_POINT('Ctrl Pts',(-7.08827439219835,-64.8259873732546,
87.6373764712027));
#115287=CARTESIAN_POINT('Ctrl Pts',(-7.14208955312506,-64.5902694889972,
87.5106518782322));
#115288=CARTESIAN_POINT('Ctrl Pts',(-7.19693271715934,-64.3590102276896,
87.3795061726048));
#115289=CARTESIAN_POINT('Ctrl Pts',(-7.25261931495788,-64.1321728080882,
87.2440051558485));
#115290=CARTESIAN_POINT('Ctrl Pts',(-7.30862354726613,-63.9040415153574,
87.1077312457799));
#115291=CARTESIAN_POINT('Ctrl Pts',(-7.36548116596207,-63.6803822131273,
86.9670520486309));
#115292=CARTESIAN_POINT('Ctrl Pts',(-7.42302254145316,-63.4611762104035,
86.8219885103422));
#115293=CARTESIAN_POINT('Ctrl Pts',(-7.4806154753667,-63.2417737939584,
86.6767949917199));
#115294=CARTESIAN_POINT('Ctrl Pts',(-7.53889369791152,-63.0268322400467,
86.5272091019534));
#115295=CARTESIAN_POINT('Ctrl Pts',(-7.59770061678909,-62.8163579553965,
86.3732083557253));
#115296=CARTESIAN_POINT('Ctrl Pts',(-7.61918115792911,-62.7394775199539,
86.3169561420728));
#115297=CARTESIAN_POINT('Ctrl Pts',(-7.64073234701225,-62.6631933984299,
86.2601144748895));
#115298=CARTESIAN_POINT('Ctrl Pts',(-7.6623468788977,-62.5875069082207,
86.2026808795064));
#115299=CARTESIAN_POINT('Ctrl Pts',(-7.72171944494865,-62.3796050594585,
86.044917576859));
#115300=CARTESIAN_POINT('Ctrl Pts',(-7.78156955763312,-62.1762098056603,
85.8826908973321));
#115301=CARTESIAN_POINT('Ctrl Pts',(-7.84171474168083,-61.9772731854025,
85.7159708650554));
#115302=CARTESIAN_POINT('Ctrl Pts',(-7.90063733995764,-61.7823803981647,
85.5526397913863));
#115303=CARTESIAN_POINT('Ctrl Pts',(-7.95984346167794,-61.5917666858401,
85.3849958682327));
#115304=CARTESIAN_POINT('Ctrl Pts',(-8.01916413597774,-61.4054240949616,
85.2129748040599));
#115305=CARTESIAN_POINT('Ctrl Pts',(-8.08033107846091,-61.2132818667592,
85.0355998388838));
#115306=CARTESIAN_POINT('Ctrl Pts',(-8.14162016396233,-61.0256802340243,
84.8535710238742));
#115307=CARTESIAN_POINT('Ctrl Pts',(-8.20284384296533,-60.8426558696489,
84.6667810946507));
#115308=CARTESIAN_POINT('Ctrl Pts',(-8.26406752196834,-60.6596315052735,
84.4799911654272));
#115309=CARTESIAN_POINT('Ctrl Pts',(-8.32522614611897,-60.4811840784473,
84.28843993731));
#115310=CARTESIAN_POINT('Ctrl Pts',(-8.38612459115579,-60.307401135805,
84.0919856472692));
#115311=CARTESIAN_POINT('Ctrl Pts',(-8.40695694934915,-60.2479528443613,
84.0247818601072));
#115312=CARTESIAN_POINT('Ctrl Pts',(-8.42775877187844,-60.1890508569645,
83.9570040220028));
#115313=CARTESIAN_POINT('Ctrl Pts',(-8.44852208912459,-60.1306987436672,
83.8886487292554));
#115314=CARTESIAN_POINT('Ctrl Pts',(-8.46296549103274,-60.0901077815126,
83.8410993442512));
#115315=CARTESIAN_POINT('Ctrl Pts',(-8.4773880041915,-60.0497767660536,
83.7932779384106));
#115316=CARTESIAN_POINT('Ctrl Pts',(-8.49178675063624,-60.0097056972605,
83.7451840627535));
#115317=CARTESIAN_POINT('Ctrl Pts',(-8.49538643724743,-59.9996879300622,
83.7331605938392));
#115318=CARTESIAN_POINT('Ctrl Pts',(-8.49884248469713,-59.9900827858179,
83.7215930957605));
#115319=CARTESIAN_POINT('Ctrl Pts',(-8.50162619849312,-59.9823533344902,
83.712263964152));
#115320=CARTESIAN_POINT('Ctrl Pts',(-8.50440991228911,-59.9746238831625,
83.7029348325435));
#115321=CARTESIAN_POINT('Ctrl Pts',(-8.50719220167007,-59.9669062119242,
83.6935972057491));
#115322=CARTESIAN_POINT('Ctrl Pts',(-8.5099730494076,-59.9592003207754,
83.6842510817912));
#115323=CARTESIAN_POINT('Ctrl Pts',(-8.51553474488267,-59.9437885384776,
83.6655588338753));
#115324=CARTESIAN_POINT('Ctrl Pts',(-8.52109067384868,-59.9284238765374,
83.6468325973273));
#115325=CARTESIAN_POINT('Ctrl Pts',(-8.52664069770649,-59.9131063349545,
83.6280723560549));
#115326=CARTESIAN_POINT('Ctrl Pts',(-8.54884079313775,-59.8518361686228,
83.5530313909652));
#115327=CARTESIAN_POINT('Ctrl Pts',(-8.5709464276222,-59.7913199280025,
83.4774463572037));
#115328=CARTESIAN_POINT('Ctrl Pts',(-8.59294854414954,-59.7315576131294,
83.4013162397247));
#115329=CARTESIAN_POINT('Ctrl Pts',(-8.63695277720424,-59.6120329833831,
83.2490560047667));
#115330=CARTESIAN_POINT('Ctrl Pts',(-8.68054321499461,-59.4955240566604,
83.0946155134775));
#115331=CARTESIAN_POINT('Ctrl Pts',(-8.72364395735391,-59.3820308335148,
82.937986299838));
#115332=CARTESIAN_POINT('Ctrl Pts',(-8.77931417365709,-59.2354395699865,
82.7356792924547));
#115333=CARTESIAN_POINT('Ctrl Pts',(-8.83416874073783,-59.0938841685608,
82.5297174962948));
#115334=CARTESIAN_POINT('Ctrl Pts',(-8.88802887219702,-58.9573534873692,
82.3200954780129));
#115335=CARTESIAN_POINT('Ctrl Pts',(-8.91756743410084,-58.8824758391183,
82.2051322798983));
#115336=CARTESIAN_POINT('Ctrl Pts',(-8.94680683515967,-58.8091101854314,
82.0890675858819));
#115337=CARTESIAN_POINT('Ctrl Pts',(-8.97571685333632,-58.7372599362983,
81.9718964272046));
#115338=CARTESIAN_POINT('Ctrl Pts',(-8.9810958478393,-58.723891487591,81.9500955755213));
#115339=CARTESIAN_POINT('Ctrl Pts',(-8.98646348068979,-58.7105757369594,
81.9282562377321));
#115340=CARTESIAN_POINT('Ctrl Pts',(-8.99181954156358,-58.6973126643615,
81.9063784200908));
#115341=CARTESIAN_POINT('Ctrl Pts',(-9.04421400583836,-58.5675696312296,
81.692363575631));
#115342=CARTESIAN_POINT('Ctrl Pts',(-9.09550157275799,-58.4428643549359,
81.4746692484697));
#115343=CARTESIAN_POINT('Ctrl Pts',(-9.14550683304999,-58.3231561767416,
81.2533245862162));
#115344=CARTESIAN_POINT('Ctrl Pts',(-9.19551814217404,-58.2034335181774,
81.0319531492457));
#115345=CARTESIAN_POINT('Ctrl Pts',(-9.24424716833884,-58.0887087970384,
80.8069302641477));
#115346=CARTESIAN_POINT('Ctrl Pts',(-9.29150993392781,-57.9789829137176,
80.5782535255859));
#115347=CARTESIAN_POINT('Ctrl Pts',(-9.33877269951677,-57.8692570303968,
80.349576787024));
#115348=CARTESIAN_POINT('Ctrl Pts',(-9.38456956736444,-57.7645295954233,
80.1172459456955));
#115349=CARTESIAN_POINT('Ctrl Pts',(-9.4287028391648,-57.6648487671302,
79.8812306242836));
#115350=CARTESIAN_POINT('Ctrl Pts',(-9.43407045269604,-57.6527253024305,
79.8525257723405));
#115351=CARTESIAN_POINT('Ctrl Pts',(-9.43941336419247,-57.6406759877037,
79.8237667794555));
#115352=CARTESIAN_POINT('Ctrl Pts',(-9.44473119037857,-57.6287008573064,
79.7949536339167));
#115353=CARTESIAN_POINT('Ctrl Pts',(-9.4563678165064,-57.6024965192201,
79.7319038480703));
#115354=CARTESIAN_POINT('Ctrl Pts',(-9.46788432996337,-57.5766473867214,
79.6685947689743));
#115355=CARTESIAN_POINT('Ctrl Pts',(-9.4792774035311,-57.5511533674906,
79.6050267292126));
#115356=CARTESIAN_POINT('Ctrl Pts',(-9.48135235335323,-57.5465102998975,
79.5934494764184));
#115357=CARTESIAN_POINT('Ctrl Pts',(-9.48342320871521,-57.541879012395,
79.5818636331032));
#115358=CARTESIAN_POINT('Ctrl Pts',(-9.48548994915482,-57.537259504983,
79.5702692013485));
#115359=CARTESIAN_POINT('Ctrl Pts',(-9.48755668959442,-57.5326399975709,
79.5586747695938));
#115360=CARTESIAN_POINT('Ctrl Pts',(-9.48889802164019,-57.5296438207682,
79.5511269172421));
#115361=CARTESIAN_POINT('Ctrl Pts',(-9.49042437195825,-57.5262355074984,
79.5425266149269));
#115362=CARTESIAN_POINT('Ctrl Pts',(-9.49347707259439,-57.5194188809588,
79.5253260102966));
#115363=CARTESIAN_POINT('Ctrl Pts',(-9.49652001932305,-57.5126304293838,
79.5081104005636));
#115364=CARTESIAN_POINT('Ctrl Pts',(-9.49955316118484,-57.5058701527735,
79.4908797944758));
#115365=CARTESIAN_POINT('Ctrl Pts',(-9.50561944490843,-57.492349599553,
79.4564185823002));
#115366=CARTESIAN_POINT('Ctrl Pts',(-9.51164650964414,-57.4789417461908,
79.4218973848201));
#115367=CARTESIAN_POINT('Ctrl Pts',(-9.51763394201365,-57.4656465926865,
79.3873162705839));
#115368=CARTESIAN_POINT('Ctrl Pts',(-9.54158367149169,-57.4124659786691,
79.2489918136391));
#115369=CARTESIAN_POINT('Ctrl Pts',(-9.5648994423365,-57.3610885623673,
79.1097087217166));
#115370=CARTESIAN_POINT('Ctrl Pts',(-9.58755352231721,-57.3115143438162,
78.9694712267336));
#115371=CARTESIAN_POINT('Ctrl Pts',(-9.62609916515577,-57.2271644110935,
78.7308588267249));
#115372=CARTESIAN_POINT('Ctrl Pts',(-9.66273029453766,-57.1480362853527,
78.48948291296));
#115373=CARTESIAN_POINT('Ctrl Pts',(-9.69729491697327,-57.0741259973634,
78.2453693959728));
#115374=CARTESIAN_POINT('Ctrl Pts',(-9.70335899669416,-57.0611590430911,
78.202541680128));
#115375=CARTESIAN_POINT('Ctrl Pts',(-9.70935942942061,-57.0483528046862,
78.159629649545));
#115376=CARTESIAN_POINT('Ctrl Pts',(-9.71529534017754,-57.0357074057499,
78.1166333803834));
#115377=CARTESIAN_POINT('Ctrl Pts',(-9.72742678734184,-57.0098635217449,
78.0287602655483));
#115378=CARTESIAN_POINT('Ctrl Pts',(-9.73928886456698,-56.9846922496317,
77.9405345025405));
#115379=CARTESIAN_POINT('Ctrl Pts',(-9.75087363454091,-56.9601929819792,
77.8519582094545));
#115380=CARTESIAN_POINT('Ctrl Pts',(-9.78311100811269,-56.8920179517175,
77.6054736390878));
#115381=CARTESIAN_POINT('Ctrl Pts',(-9.81320230114342,-56.8290436401664,
77.3562760559548));
#115382=CARTESIAN_POINT('Ctrl Pts',(-9.84101052750768,-56.7712538627715,
77.1044066262465));
#115383=CARTESIAN_POINT('Ctrl Pts',(-9.86872917611775,-56.7136502417465,
76.8533485355128));
#115384=CARTESIAN_POINT('Ctrl Pts',(-9.89417981525409,-56.661197513563,
76.5996355006453));
#115385=CARTESIAN_POINT('Ctrl Pts',(-9.91720607264976,-56.6139237675165,
76.3432915265767));
#115386=CARTESIAN_POINT('Ctrl Pts',(-9.92060784437707,-56.6069398061206,
76.3054206877135));
#115387=CARTESIAN_POINT('Ctrl Pts',(-9.92395664213361,-56.6000685445888,
76.2674925987102));
#115388=CARTESIAN_POINT('Ctrl Pts',(-9.9272519106857,-56.5933099829211,
76.2295073886416));
#115389=CARTESIAN_POINT('Ctrl Pts',(-9.92950591356342,-56.5886870463661,
76.2035250532258));
#115390=CARTESIAN_POINT('Ctrl Pts',(-9.93150317406151,-56.5845931209331,
76.1802069722421));
#115391=CARTESIAN_POINT('Ctrl Pts',(-9.93346399982777,-56.5805746185882,
76.157082382999));
#115392=CARTESIAN_POINT('Ctrl Pts',(-9.93436982855763,-56.5787182196476,
76.1463996810155));
#115393=CARTESIAN_POINT('Ctrl Pts',(-9.93526760888132,-56.5768786059676,
76.135758163069));
#115394=CARTESIAN_POINT('Ctrl Pts',(-9.93617772172492,-56.5750144321809,
76.124913722644));
#115395=CARTESIAN_POINT('Ctrl Pts',(-9.93748512336717,-56.5723364962664,
76.1093353915387));
#115396=CARTESIAN_POINT('Ctrl Pts',(-9.93878300849999,-56.5696788927295,
76.0937531901985));
#115397=CARTESIAN_POINT('Ctrl Pts',(-9.9400713590507,-56.5670416263439,
76.0781671294405));
#115398=CARTESIAN_POINT('Ctrl Pts',(-9.94445949385756,-56.5580590707693,
76.0250808512716));
#115399=CARTESIAN_POINT('Ctrl Pts',(-9.94873702206621,-56.5493124387524,
75.9719498006223));
#115400=CARTESIAN_POINT('Ctrl Pts',(-9.95290366859442,-56.5408017072184,
75.9187744460697));
#115401=CARTESIAN_POINT('Ctrl Pts',(-9.96368360542344,-56.5187827652024,
75.7811993100327));
#115402=CARTESIAN_POINT('Ctrl Pts',(-9.97372148030912,-56.4983429057096,
75.6433276363244));
#115403=CARTESIAN_POINT('Ctrl Pts',(-9.98301121954607,-56.4794821288461,
75.5051674707858));
#115404=CARTESIAN_POINT('Ctrl Pts',(-10.00159069802,-56.4417605751189,75.2288471397085));
#115405=CARTESIAN_POINT('Ctrl Pts',(-10.0171796586205,-56.4103553524075,
74.9513729078636));
#115406=CARTESIAN_POINT('Ctrl Pts',(-10.0297059689885,-56.3852664608848,
74.672808313959));
#115407=CARTESIAN_POINT('Ctrl Pts',(-10.0349411749523,-56.374780890061,
74.5563859213738));
#115408=CARTESIAN_POINT('Ctrl Pts',(-10.0396410471935,-56.3653997046156,
74.4397728123101));
#115409=CARTESIAN_POINT('Ctrl Pts',(-10.0437985795037,-56.3571233343035,
74.3229742968176));
#115410=CARTESIAN_POINT('Ctrl Pts',(-10.0532545573527,-56.338299385744,
74.0573253269758));
#115411=CARTESIAN_POINT('Ctrl Pts',(-10.0599068555642,-56.3251877634295,
73.7907175155284));
#115412=CARTESIAN_POINT('Ctrl Pts',(-10.0637172608622,-56.3177898385427,
73.5232108702605));
#115413=CARTESIAN_POINT('Ctrl Pts',(-10.0662486708131,-56.3128750908428,
73.345495133801));
#115414=CARTESIAN_POINT('Ctrl Pts',(-10.0675252675775,-56.3104829476421,
73.1673825891876));
#115415=CARTESIAN_POINT('Ctrl Pts',(-10.0675288996373,-56.3106244902745,
72.9888900918571));
#115416=CARTESIAN_POINT('',(-7.08825603872491,-64.825987319,58.34041012264));
#115417=CARTESIAN_POINT('Ctrl Pts',(-10.0675326914397,-56.3106244903022,
72.9888900919343));
#115418=CARTESIAN_POINT('Ctrl Pts',(-10.0675364861884,-56.3106236438183,
72.8373894080529));
#115419=CARTESIAN_POINT('Ctrl Pts',(-10.0665997793874,-56.3125565421587,
72.6820441351514));
#115420=CARTESIAN_POINT('Ctrl Pts',(-10.0627950071674,-56.3200932749138,
72.3728615295497));
#115421=CARTESIAN_POINT('Ctrl Pts',(-10.0599294447923,-56.3257673245125,
72.2179451440282));
#115422=CARTESIAN_POINT('Ctrl Pts',(-10.0484874118121,-56.3485897944341,
71.7544431528985));
#115423=CARTESIAN_POINT('Ctrl Pts',(-10.0141911002797,-56.4173278124564,
70.8296920351912));
#115424=CARTESIAN_POINT('Ctrl Pts',(-9.94612028955057,-56.5553450650161,
69.9125366186336));
#115425=CARTESIAN_POINT('Ctrl Pts',(-9.82621684669285,-56.8009496102399,
68.6978275958031));
#115426=CARTESIAN_POINT('Ctrl Pts',(-9.75383725762295,-56.9508618239222,
68.1137141942851));
#115427=CARTESIAN_POINT('Ctrl Pts',(-9.58475593550578,-57.3152540454977,
66.9627992394608));
#115428=CARTESIAN_POINT('Ctrl Pts',(-9.48823107615905,-57.5285692202934,
66.3988547901617));
#115429=CARTESIAN_POINT('Ctrl Pts',(-9.36773885117348,-57.8035577389473,
65.7777835756058));
#115430=CARTESIAN_POINT('Ctrl Pts',(-9.35418547529567,-57.8345982541729,
65.7089611577416));
#115431=CARTESIAN_POINT('Ctrl Pts',(-9.33875494628785,-57.8700658485987,
65.631745287302));
#115432=CARTESIAN_POINT('Ctrl Pts',(-9.33693933149597,-57.8742404593784,
65.6226733259747));
#115433=CARTESIAN_POINT('Ctrl Pts',(-9.33254286197359,-57.8843567207882,
65.6007616913834));
#115434=CARTESIAN_POINT('Ctrl Pts',(-9.32593778198101,-57.8995651499525,
65.5679186925187));
#115435=CARTESIAN_POINT('Ctrl Pts',(-9.31045372056789,-57.9352897440166,
65.4914562102728));
#115436=CARTESIAN_POINT('Ctrl Pts',(-9.26134090855832,-58.0490646698304,
65.2522216414933));
#115437=CARTESIAN_POINT('Ctrl Pts',(-9.141804444225,-58.3297867322916,64.6952379674525));
#115438=CARTESIAN_POINT('Ctrl Pts',(-9.02454771227377,-58.6150552440629,
64.19989351254));
#115439=CARTESIAN_POINT('Ctrl Pts',(-8.78268079338333,-59.2204462064251,
63.2342091003427));
#115440=CARTESIAN_POINT('Ctrl Pts',(-8.61166284917084,-59.6705120997594,
62.6237793667378));
#115441=CARTESIAN_POINT('Ctrl Pts',(-8.42446623526063,-60.1980835247549,
62.0101821405832));
#115442=CARTESIAN_POINT('Ctrl Pts',(-8.41343432384315,-60.2292986689213,
61.9742166981781));
#115443=CARTESIAN_POINT('Ctrl Pts',(-8.39962032684187,-60.2685445127935,
61.9294203517137));
#115444=CARTESIAN_POINT('Ctrl Pts',(-8.39591465393794,-60.2790823039808,
61.9174185017987));
#115445=CARTESIAN_POINT('Ctrl Pts',(-8.38867784863578,-60.2996915603767,
61.8940265584313));
#115446=CARTESIAN_POINT('Ctrl Pts',(-8.37781951720245,-60.3306539737948,
61.8589894052093));
#115447=CARTESIAN_POINT('Ctrl Pts',(-8.33797279171314,-60.444716640061,
61.7310779500568));
#115448=CARTESIAN_POINT('Ctrl Pts',(-8.24355473748462,-60.7185251372143,
61.4331346970249));
#115449=CARTESIAN_POINT('Ctrl Pts',(-8.15608967698741,-60.9805889765312,
61.1678034254881));
#115450=CARTESIAN_POINT('Ctrl Pts',(-7.98128295927112,-61.5171400341676,
60.6499539622089));
#115451=CARTESIAN_POINT('Ctrl Pts',(-7.86491848259896,-61.8914052445958,
60.3218068716169));
#115452=CARTESIAN_POINT('Ctrl Pts',(-7.52031758516955,-63.063894391892,
59.3876499202851));
#115453=CARTESIAN_POINT('Ctrl Pts',(-7.29670946703427,-63.9118118447716,
58.8319269483214));
#115454=CARTESIAN_POINT('Ctrl Pts',(-7.08825603872491,-64.825987319,58.34041012264));
#115455=CARTESIAN_POINT('',(-7.08815756005477,25.,58.3404519109566));
#115456=CARTESIAN_POINT('Origin',(6.43246351666909,-92.5,72.98888938658));
#115457=CARTESIAN_POINT('',(14.224188353942,-89.,69.5919754841955));
#115458=CARTESIAN_POINT('',(14.2241883540028,-89.,76.3858032888256));
#115459=CARTESIAN_POINT('Origin',(6.43246351666909,-89.,72.98888938658));
#115460=CARTESIAN_POINT('',(14.2241130800822,-26.6269674540304,76.3859511531206));
#115461=CARTESIAN_POINT('',(14.2241160297191,-26.62696745403,76.385952439033));
#115462=CARTESIAN_POINT('',(14.9324318700046,-25.5800517253112,72.9888915205226));
#115463=CARTESIAN_POINT('Ctrl Pts',(14.9324318700046,-25.5800517253112,
72.9888915205226));
#115464=CARTESIAN_POINT('Ctrl Pts',(14.9324322830594,-25.5815074595943,
72.9978095054497));
#115465=CARTESIAN_POINT('Ctrl Pts',(14.932422196367,-25.5836894834383,73.011062863635));
#115466=CARTESIAN_POINT('Ctrl Pts',(14.9323408487722,-25.5866504441077,
73.0286517844855));
#115467=CARTESIAN_POINT('Ctrl Pts',(14.9322592991564,-25.5896187581116,
73.0462843861658));
#115468=CARTESIAN_POINT('Ctrl Pts',(14.9321061543371,-25.5933699393119,
73.0682741904377));
#115469=CARTESIAN_POINT('Ctrl Pts',(14.9317800569268,-25.5979909573379,
73.0946204833495));
#115470=CARTESIAN_POINT('Ctrl Pts',(14.9314522032137,-25.6026368633467,
73.1211086727178));
#115471=CARTESIAN_POINT('Ctrl Pts',(14.9309495708688,-25.6081620793749,
73.152000526072));
#115472=CARTESIAN_POINT('Ctrl Pts',(14.9301281339321,-25.6146882494659,
73.1872928876012));
#115473=CARTESIAN_POINT('Ctrl Pts',(14.9294390067672,-25.6201632419956,
73.2169006687399));
#115474=CARTESIAN_POINT('Ctrl Pts',(14.9285247921834,-25.626343334206,73.2496055449496));
#115475=CARTESIAN_POINT('Ctrl Pts',(14.9272780733121,-25.6333174822889,
73.2854032475674));
#115476=CARTESIAN_POINT('Ctrl Pts',(14.9257812819554,-25.6416905364001,
73.3283814145796));
#115477=CARTESIAN_POINT('Ctrl Pts',(14.9238063101476,-25.6512075171394,
73.3758179348384));
#115478=CARTESIAN_POINT('Ctrl Pts',(14.9211282881862,-25.6620501269969,
73.4276988568622));
#115479=CARTESIAN_POINT('Ctrl Pts',(14.9209004886526,-25.6629724276743,
73.432111983421));
#115480=CARTESIAN_POINT('Ctrl Pts',(14.9206675765875,-25.663904337248,73.4365572627827));
#115481=CARTESIAN_POINT('Ctrl Pts',(14.9204293993517,-25.6648459769638,
73.4410346832428));
#115482=CARTESIAN_POINT('Ctrl Pts',(14.9175353168443,-25.6762878052311,
73.4954396484616));
#115483=CARTESIAN_POINT('Ctrl Pts',(14.9138678415203,-25.6891646855909,
73.5545910535414));
#115484=CARTESIAN_POINT('Ctrl Pts',(14.9091275338572,-25.7036970772543,
73.6184639971648));
#115485=CARTESIAN_POINT('Ctrl Pts',(14.9057789676978,-25.7139627980468,
73.6635840173669));
#115486=CARTESIAN_POINT('Ctrl Pts',(14.9018940489071,-25.7250551143502,
73.71105991217));
#115487=CARTESIAN_POINT('Ctrl Pts',(14.8973527386311,-25.7370561031237,
73.7608788972865));
#115488=CARTESIAN_POINT('Ctrl Pts',(14.8958761541438,-25.7409581650348,
73.7770772929306));
#115489=CARTESIAN_POINT('Ctrl Pts',(14.8943300819425,-25.7449563112392,
73.7935233685791));
#115490=CARTESIAN_POINT('Ctrl Pts',(14.8927101227617,-25.7490534109817,
73.8102165937442));
#115491=CARTESIAN_POINT('Ctrl Pts',(14.8919001431713,-25.751101960853,73.8185632063267));
#115492=CARTESIAN_POINT('Ctrl Pts',(14.8910716896904,-25.753175249109,73.8269716060774));
#115493=CARTESIAN_POINT('Ctrl Pts',(14.890224199929,-25.7552736361177,73.8354417213194));
#115494=CARTESIAN_POINT('Ctrl Pts',(14.8893767101676,-25.7573720231265,
73.8439118365614));
#115495=CARTESIAN_POINT('Ctrl Pts',(14.8887607019875,-25.758878463585,73.849958788021));
#115496=CARTESIAN_POINT('Ctrl Pts',(14.8882268814574,-25.7601790630543,
73.8551710985703));
#115497=CARTESIAN_POINT('Ctrl Pts',(14.8860915993371,-25.7653814609316,
73.8760203407674));
#115498=CARTESIAN_POINT('Ctrl Pts',(14.8838992970071,-25.7705918971331,
73.8966649244407));
#115499=CARTESIAN_POINT('Ctrl Pts',(14.8816544011347,-25.7758047260644,
73.9171044047801));
#115500=CARTESIAN_POINT('Ctrl Pts',(14.8722952428081,-25.7975374451164,
74.00231830488));
#115501=CARTESIAN_POINT('Ctrl Pts',(14.8620235677878,-25.8193217618782,
74.0839701106493));
#115502=CARTESIAN_POINT('Ctrl Pts',(14.8511411867226,-25.8408864029058,
74.1620634102641));
#115503=CARTESIAN_POINT('Ctrl Pts',(14.84114150854,-25.8607018705969,74.2338223258621));
#115504=CARTESIAN_POINT('Ctrl Pts',(14.8306258959872,-25.8803326345716,
74.3025768350749));
#115505=CARTESIAN_POINT('Ctrl Pts',(14.8198094672081,-25.899601248361,74.3683365258879));
#115506=CARTESIAN_POINT('Ctrl Pts',(14.8085156384223,-25.9197203125662,
74.4369986235374));
#115507=CARTESIAN_POINT('Ctrl Pts',(14.7968940012334,-25.9394446013637,
74.5023957862849));
#115508=CARTESIAN_POINT('Ctrl Pts',(14.7851682425416,-25.9586045066459,
74.5645445447822));
#115509=CARTESIAN_POINT('Ctrl Pts',(14.7793053631958,-25.968184459287,74.5956189240309));
#115510=CARTESIAN_POINT('Ctrl Pts',(14.7734161154646,-25.9776238048017,
74.6258812797001));
#115511=CARTESIAN_POINT('Ctrl Pts',(14.7675264323988,-25.9869041150831,
74.6553340710032));
#115512=CARTESIAN_POINT('Ctrl Pts',(14.7645815908659,-25.9915442702239,
74.6700604666547));
#115513=CARTESIAN_POINT('Ctrl Pts',(14.7616366208883,-25.9961446665606,
74.6845844672437));
#115514=CARTESIAN_POINT('Ctrl Pts',(14.7586946352575,-26.0007032008082,
74.6989064097336));
#115515=CARTESIAN_POINT('Ctrl Pts',(14.7563545752567,-26.0043290661229,
74.7102981053299));
#115516=CARTESIAN_POINT('Ctrl Pts',(14.7534682637949,-26.008774456286,74.7242134413493));
#115517=CARTESIAN_POINT('Ctrl Pts',(14.750526882187,-26.0132657974865,74.7381970253182));
#115518=CARTESIAN_POINT('Ctrl Pts',(14.7497702806568,-26.0144210898212,
74.7417939747926));
#115519=CARTESIAN_POINT('Ctrl Pts',(14.7490102658137,-26.0155792891444,
74.7453954749945));
#115520=CARTESIAN_POINT('Ctrl Pts',(14.7482557038702,-26.0167269386934,
74.7489598144109));
#115521=CARTESIAN_POINT('Ctrl Pts',(14.726595823022,-26.0496704931656,74.8512750288573));
#115522=CARTESIAN_POINT('Ctrl Pts',(14.7030251667799,-26.0836746568982,
74.9532932583679));
#115523=CARTESIAN_POINT('Ctrl Pts',(14.6775434815947,-26.1186225857099,
75.0549628614383));
#115524=CARTESIAN_POINT('Ctrl Pts',(14.5807327523832,-26.2513977317848,
75.4412288536748));
#115525=CARTESIAN_POINT('Ctrl Pts',(14.4563370759543,-26.3977958659517,
75.822466523226));
#115526=CARTESIAN_POINT('Ctrl Pts',(14.3044197355888,-26.5490345935639,
76.1954372265989));
#115527=CARTESIAN_POINT('Ctrl Pts',(14.2784528993981,-26.5748854362402,
76.2591881396619));
#115528=CARTESIAN_POINT('Ctrl Pts',(14.2516820244083,-26.6008776840374,
76.322697408171));
#115529=CARTESIAN_POINT('Ctrl Pts',(14.2241074907228,-26.6269674540316,
76.3859487164399));
#115530=CARTESIAN_POINT('',(14.2241195978544,-25.6803288454663,69.5918555673368));
#115531=CARTESIAN_POINT('Ctrl Pts',(14.2241026265127,-25.6803288453497,
69.5918629655995));
#115532=CARTESIAN_POINT('Ctrl Pts',(14.2338993117142,-25.6750456877715,
69.61433611693));
#115533=CARTESIAN_POINT('Ctrl Pts',(14.2453110648062,-25.6689449086916,
69.6407711517479));
#115534=CARTESIAN_POINT('Ctrl Pts',(14.2582172700314,-25.6621326199402,
69.671216979588));
#115535=CARTESIAN_POINT('Ctrl Pts',(14.2711080763947,-25.6553284591778,
69.7016264814059));
#115536=CARTESIAN_POINT('Ctrl Pts',(14.2854898165465,-25.6478143058882,
69.7360373571018));
#115537=CARTESIAN_POINT('Ctrl Pts',(14.3012054317066,-25.6397313603784,
69.7745096285445));
#115538=CARTESIAN_POINT('Ctrl Pts',(14.3169210468667,-25.6316484148687,
69.8129818999871));
#115539=CARTESIAN_POINT('Ctrl Pts',(14.3339706033377,-25.6229964426334,
69.8555157476333));
#115540=CARTESIAN_POINT('Ctrl Pts',(14.3521592952607,-25.6139552487866,
69.9021800432174));
#115541=CARTESIAN_POINT('Ctrl Pts',(14.3697195313874,-25.6052264463257,
69.9472319937706));
#115542=CARTESIAN_POINT('Ctrl Pts',(14.3883414175576,-25.5961348293546,
69.9961341361763));
#115543=CARTESIAN_POINT('Ctrl Pts',(14.4078153200047,-25.5868797326659,
70.0489536868223));
#115544=CARTESIAN_POINT('Ctrl Pts',(14.4269162706787,-25.5778018836928,
70.1007616710847));
#115545=CARTESIAN_POINT('Ctrl Pts',(14.4468368816831,-25.5685666230943,
70.1563386573105));
#115546=CARTESIAN_POINT('Ctrl Pts',(14.4673467945466,-25.5594001158797,
70.2157500959955));
#115547=CARTESIAN_POINT('Ctrl Pts',(14.4746780481005,-25.55612355449,70.2369866718843));
#115548=CARTESIAN_POINT('Ctrl Pts',(14.4820842922524,-25.5528561464829,
70.2587131799805));
#115549=CARTESIAN_POINT('Ctrl Pts',(14.4895539796186,-25.5496094889563,
70.280932595363));
#115550=CARTESIAN_POINT('Ctrl Pts',(14.4978326632631,-25.5460112057556,
70.3055584601015));
#115551=CARTESIAN_POINT('Ctrl Pts',(14.5061892901608,-25.5424383921229,
70.330789784142));
#115552=CARTESIAN_POINT('Ctrl Pts',(14.5146073477813,-25.5389078583163,
70.3566305615356));
#115553=CARTESIAN_POINT('Ctrl Pts',(14.5188163765916,-25.5371425914131,
70.3695509502323));
#115554=CARTESIAN_POINT('Ctrl Pts',(14.5230407515599,-25.5353878944688,
70.3826237059942));
#115555=CARTESIAN_POINT('Ctrl Pts',(14.5272783273136,-25.5336459975768,
70.3958493129143));
#115556=CARTESIAN_POINT('Ctrl Pts',(14.5306261334141,-25.532269849189,70.406297920822));
#115557=CARTESIAN_POINT('Ctrl Pts',(14.5330136918787,-25.5312977314843,
70.4138070161427));
#115558=CARTESIAN_POINT('Ctrl Pts',(14.5353086196189,-25.5303666064219,
70.4210470939523));
#115559=CARTESIAN_POINT('Ctrl Pts',(14.5359185584858,-25.5301191348542,
70.4229713396609));
#115560=CARTESIAN_POINT('Ctrl Pts',(14.5365217515845,-25.529874753799,70.4248766451319));
#115561=CARTESIAN_POINT('Ctrl Pts',(14.5371340949548,-25.529627025719,70.4268132660522));
#115562=CARTESIAN_POINT('Ctrl Pts',(14.5469741685572,-25.5256461505121,
70.4579338649191));
#115563=CARTESIAN_POINT('Ctrl Pts',(14.5565890539903,-25.5218518761061,
70.4889666874341));
#115564=CARTESIAN_POINT('Ctrl Pts',(14.5659829572459,-25.5182420787809,
70.5199083042194));
#115565=CARTESIAN_POINT('Ctrl Pts',(14.6088329330693,-25.5017761088953,
70.6610474553376));
#115566=CARTESIAN_POINT('Ctrl Pts',(14.6470859696426,-25.4891475731015,
70.8002848510483));
#115567=CARTESIAN_POINT('Ctrl Pts',(14.6811698955704,-25.4799462604506,
70.9373334188642));
#115568=CARTESIAN_POINT('Ctrl Pts',(14.6927625606021,-25.4768166991542,
70.9839465391702));
#115569=CARTESIAN_POINT('Ctrl Pts',(14.7038728251073,-25.4740836902524,
71.0303068799569));
#115570=CARTESIAN_POINT('Ctrl Pts',(14.7145171831541,-25.471731357348,71.0764044326882));
#115571=CARTESIAN_POINT('Ctrl Pts',(14.7226506902966,-25.4699339059286,
71.1116282360168));
#115572=CARTESIAN_POINT('Ctrl Pts',(14.730419914814,-25.4683758830105,71.1462827098248));
#115573=CARTESIAN_POINT('Ctrl Pts',(14.7380228251446,-25.467013237196,71.181215845594));
#115574=CARTESIAN_POINT('Ctrl Pts',(14.7456257354751,-25.4656505913816,
71.2161489813631));
#115575=CARTESIAN_POINT('Ctrl Pts',(14.7530624440847,-25.4644832094774,
71.2513608443164));
#115576=CARTESIAN_POINT('Ctrl Pts',(14.7604873173191,-25.4635097754476,
71.2877085029335));
#115577=CARTESIAN_POINT('Ctrl Pts',(14.8052502089818,-25.4576411605043,
71.5068403659952));
#115578=CARTESIAN_POINT('Ctrl Pts',(14.8413639787243,-25.4600534562162,
71.7277141970178));
#115579=CARTESIAN_POINT('Ctrl Pts',(14.8687019433517,-25.4708912995428,
71.9497116025528));
#115580=CARTESIAN_POINT('Ctrl Pts',(14.8776406202561,-25.4744349422813,
72.0222979530274));
#115581=CARTESIAN_POINT('Ctrl Pts',(14.885641027309,-25.4788793646732,72.0950044205385));
#115582=CARTESIAN_POINT('Ctrl Pts',(14.8927019369333,-25.4842038600896,
72.1678085493355));
#115583=CARTESIAN_POINT('Ctrl Pts',(14.9070299012433,-25.4950083009269,
72.315542342079));
#115584=CARTESIAN_POINT('Ctrl Pts',(14.917489429708,-25.5094365505709,72.463678333871));
#115585=CARTESIAN_POINT('Ctrl Pts',(14.924069381774,-25.5273157376696,72.6120282867966));
#115586=CARTESIAN_POINT('Ctrl Pts',(14.9273593578071,-25.5362553312189,
72.6862032632594));
#115587=CARTESIAN_POINT('Ctrl Pts',(14.9296794223991,-25.5460576591347,
72.7604317306291));
#115588=CARTESIAN_POINT('Ctrl Pts',(14.9310280814812,-25.5567011269805,
72.8346900293723));
#115589=CARTESIAN_POINT('Ctrl Pts',(14.9317024110222,-25.5620228609035,
72.8718191787439));
#115590=CARTESIAN_POINT('Ctrl Pts',(14.9321338882588,-25.5675548798091,
72.9089557860247));
#115591=CARTESIAN_POINT('Ctrl Pts',(14.9323223207997,-25.5732944842521,
72.946096887067));
#115592=CARTESIAN_POINT('Ctrl Pts',(14.9323694289349,-25.5747293853629,
72.9553821623276));
#115593=CARTESIAN_POINT('Ctrl Pts',(14.9323992627362,-25.5761790818121,
72.9646677473044));
#115594=CARTESIAN_POINT('Ctrl Pts',(14.9324139020858,-25.5772981979159,
72.9717911886955));
#115595=CARTESIAN_POINT('Ctrl Pts',(14.9324212217606,-25.5778577559678,
72.975352909391));
#115596=CARTESIAN_POINT('Ctrl Pts',(14.9324226631454,-25.5780789378129,
72.976752333311));
#115597=CARTESIAN_POINT('Ctrl Pts',(14.9324232811651,-25.5781482284294,
72.9771871753668));
#115598=CARTESIAN_POINT('Ctrl Pts',(14.9324238991848,-25.5782175190459,
72.9776220174227));
#115599=CARTESIAN_POINT('Ctrl Pts',(14.9324245829475,-25.5782981840234,
72.9781259632307));
#115600=CARTESIAN_POINT('Ctrl Pts',(14.9324252956337,-25.578390236186,72.9786990130744));
#115601=CARTESIAN_POINT('Ctrl Pts',(14.9324281463782,-25.5787584448367,
72.9809912124489));
#115602=CARTESIAN_POINT('Ctrl Pts',(14.9324316612965,-25.5793088484383,
72.9843890844908));
#115603=CARTESIAN_POINT('Ctrl Pts',(14.9324318700046,-25.5800517252917,
72.988891520403));
#115604=CARTESIAN_POINT('',(14.2241252549691,-25.68032884552,69.591853101251));
#115605=CARTESIAN_POINT('Origin',(-15.5675364832709,-75.,72.98888938658));
#115606=CARTESIAN_POINT('',(-18.5675364832709,-75.,62.73888938658));
#115607=CARTESIAN_POINT('Origin',(-18.5675364832709,-75.,72.98888938658));
#115608=CARTESIAN_POINT('',(-15.5675364833309,-75.,62.73888938658));
#115609=CARTESIAN_POINT('',(-15.5675364832709,-75.,62.73888938658));
#115610=CARTESIAN_POINT('Origin',(-15.5675364833309,-75.,72.98888938658));
#115611=CARTESIAN_POINT('Origin',(-18.5675364832709,-75.,72.98888938658));
#115612=CARTESIAN_POINT('',(-20.0675364832709,-75.,84.7388893856825));
#115613=CARTESIAN_POINT('',(-20.0675364832709,-75.,61.23888938658));
#115614=CARTESIAN_POINT('Origin',(-20.0675364832709,-75.,72.98888938658));
#115615=CARTESIAN_POINT('',(-18.5675364832709,-75.,61.23888938658));
#115616=CARTESIAN_POINT('',(-18.5675364832709,-75.,61.23888938658));
#115617=CARTESIAN_POINT('Origin',(-18.5675364832709,-75.,72.98888938658));
#115618=CARTESIAN_POINT('Origin',(-20.0675364832709,-75.,72.98888938658));
#115619=CARTESIAN_POINT('Origin',(-20.5675364832709,-75.,72.98888938658));
#115620=CARTESIAN_POINT('',(-20.5675364832709,-75.,84.23888938658));
#115621=CARTESIAN_POINT('',(-20.5675364832709,-75.,84.23888938658));
#115622=CARTESIAN_POINT('Origin',(-20.5675364832709,-75.,72.98888938658));
#115623=CARTESIAN_POINT('Origin',(-20.5675364832709,-75.,72.98888938658));
#115624=CARTESIAN_POINT('',(-20.3675364832709,-75.,65.23888938658));
#115625=CARTESIAN_POINT('',(-20.3675364832709,-75.,80.73888938658));
#115626=CARTESIAN_POINT('Origin',(-20.3675364832709,-75.,72.98888938658));
#115627=CARTESIAN_POINT('',(-18.0675364832709,-75.,80.73888938658));
#115628=CARTESIAN_POINT('',(-20.5675364832709,-75.,80.73888938658));
#115629=CARTESIAN_POINT('',(-18.0675364832709,-75.,65.23888938658));
#115630=CARTESIAN_POINT('Origin',(-18.0675364832709,-75.,72.98888938658));
#115631=CARTESIAN_POINT('Origin',(-18.0675364832709,-75.,72.98888938658));
#115632=CARTESIAN_POINT('Origin',(-20.3675364832709,-75.,72.98888938658));
#115633=CARTESIAN_POINT('Origin',(-18.0675364832709,-75.,72.98888938658));
#115634=CARTESIAN_POINT('',(-17.0930718951698,-78.0310889133651,78.2388893867872));
#115635=CARTESIAN_POINT('',(-17.0930718951698,-71.9689110866348,78.2388893867871));
#115636=CARTESIAN_POINT('Ctrl Pts',(-17.0930718944527,-78.0310889135721,
78.23888938658));
#115637=CARTESIAN_POINT('Ctrl Pts',(-16.2180718918697,-75.,78.23888938658));
#115638=CARTESIAN_POINT('Ctrl Pts',(-17.0930718944527,-71.9689110864278,
78.23888938658));
#115639=CARTESIAN_POINT('',(-17.0930718951697,-81.0621778267302,72.98888938658));
#115640=CARTESIAN_POINT('Ctrl Pts',(-17.0930718945656,-81.0621778268498,
72.9888893859586));
#115641=CARTESIAN_POINT('Ctrl Pts',(-16.2180718917851,-79.5466333698683,
75.61388938658));
#115642=CARTESIAN_POINT('Ctrl Pts',(-17.0930718945656,-78.0310889128867,
78.2388893872014));
#115643=CARTESIAN_POINT('',(-17.0930718951697,-78.0310889133651,67.7388893863729));
#115644=CARTESIAN_POINT('Ctrl Pts',(-17.0930718945656,-78.0310889128867,
67.7388893859586));
#115645=CARTESIAN_POINT('Ctrl Pts',(-16.2180718917851,-79.5466333698682,
70.36388938658));
#115646=CARTESIAN_POINT('Ctrl Pts',(-17.0930718945656,-81.0621778268498,
72.9888893872014));
#115647=CARTESIAN_POINT('',(-16.6241608063082,-75.,67.73888938658));
#115648=CARTESIAN_POINT('Ctrl Pts',(-17.0930718944527,-78.0310889135721,
67.73888938658));
#115649=CARTESIAN_POINT('Ctrl Pts',(-16.6241608063082,-76.4067332603947,
67.73888938658));
#115650=CARTESIAN_POINT('Ctrl Pts',(-16.6241608063082,-75.,67.73888938658));
#115651=CARTESIAN_POINT('',(-18.0675364832709,-75.,65.23888938658));
#115652=CARTESIAN_POINT('',(-17.0930718951697,-71.9689110866349,67.7388893863728));
#115653=CARTESIAN_POINT('Ctrl Pts',(-16.6241608063082,-75.,67.73888938658));
#115654=CARTESIAN_POINT('Ctrl Pts',(-16.6241608063082,-73.5932667396054,
67.73888938658));
#115655=CARTESIAN_POINT('Ctrl Pts',(-17.0930718944527,-71.968911086428,
67.73888938658));
#115656=CARTESIAN_POINT('',(-17.0930718951698,-68.9378221732697,72.98888938658));
#115657=CARTESIAN_POINT('Ctrl Pts',(-17.0930718945656,-68.9378221731502,
72.9888893872015));
#115658=CARTESIAN_POINT('Ctrl Pts',(-16.2180718917851,-70.4533666301317,
70.36388938658));
#115659=CARTESIAN_POINT('Ctrl Pts',(-17.0930718945656,-71.9689110871133,
67.7388893859586));
#115660=CARTESIAN_POINT('Ctrl Pts',(-17.0930718945656,-71.9689110871132,
78.2388893872014));
#115661=CARTESIAN_POINT('Ctrl Pts',(-16.2180718917851,-70.4533666301317,
75.61388938658));
#115662=CARTESIAN_POINT('Ctrl Pts',(-17.0930718945656,-68.9378221731501,
72.9888893859586));
#115663=CARTESIAN_POINT('Origin',(-20.5675364832709,-75.,72.98888938658));
#115664=CARTESIAN_POINT('',(-20.5675364832709,-75.,65.03888938658));
#115665=CARTESIAN_POINT('',(-20.5675364832709,-75.,65.03888938658));
#115666=CARTESIAN_POINT('Origin',(-20.5675364832709,-75.,72.98888938658));
#115667=CARTESIAN_POINT('Origin',(-15.0675364833309,75.,72.98888938658));
#115668=CARTESIAN_POINT('',(-15.0675364833309,84.4840963577871,72.4394203008163));
#115669=CARTESIAN_POINT('',(-15.0675364833309,65.5,72.98888938658));
#115670=CARTESIAN_POINT('Origin',(-15.0675364833309,75.,72.98888938658));
#115671=CARTESIAN_POINT('Origin',(-15.0675364833309,75.,72.98888938658));
#115672=CARTESIAN_POINT('',(-15.5675364832709,84.9832593239864,72.4105008752498));
#115673=CARTESIAN_POINT('Origin',(-15.0675364833309,84.9832593239864,72.4105008752498));
#115674=CARTESIAN_POINT('Origin',(-15.5675364832709,75.,72.98888938658));
#115675=CARTESIAN_POINT('Origin',(-15.9175364833309,75.,72.98888938658));
#115676=CARTESIAN_POINT('',(-13.5675364833309,65.5,72.98888938658));
#115677=CARTESIAN_POINT('Origin',(-13.5675364833309,75.,72.98888938658));
#115678=CARTESIAN_POINT('',(-15.9175364833309,65.5,72.98888938658));
#115679=CARTESIAN_POINT('Origin',(-13.2677182305225,75.,72.98888938658));
#115680=CARTESIAN_POINT('',(-13.22669566117,66.3412155148882,72.9888893865797));
#115681=CARTESIAN_POINT('Ctrl Pts',(-13.22669566117,66.3412155148882,72.9888893865797));
#115682=CARTESIAN_POINT('Ctrl Pts',(-13.2104605534334,66.357449920082,73.9348371888089));
#115683=CARTESIAN_POINT('Ctrl Pts',(-13.1935918113208,66.5285128660429,
74.8664087689662));
#115684=CARTESIAN_POINT('Ctrl Pts',(-13.1607289900761,67.1584349638421,
76.6215069908932));
#115685=CARTESIAN_POINT('Ctrl Pts',(-13.1451833963657,67.6075512811205,
77.4360748130446));
#115686=CARTESIAN_POINT('Ctrl Pts',(-13.1183032532819,68.5324033671701,
78.610611579631));
#115687=CARTESIAN_POINT('Ctrl Pts',(-13.1080428039918,68.928953991022,79.0221823155135));
#115688=CARTESIAN_POINT('Ctrl Pts',(-13.0883350900634,69.7818215132367,
79.7468724686923));
#115689=CARTESIAN_POINT('Ctrl Pts',(-13.0788920662947,70.2343312777093,
80.0618859789133));
#115690=CARTESIAN_POINT('Ctrl Pts',(-13.0522833578858,71.5410395253665,
80.7939570097886));
#115691=CARTESIAN_POINT('Ctrl Pts',(-13.03483318715,72.4423882065013,81.1156940890532));
#115692=CARTESIAN_POINT('Ctrl Pts',(-13.0100115445559,73.8291489133028,
81.3621080239062));
#115693=CARTESIAN_POINT('Ctrl Pts',(-13.0019625279167,74.2894034272058,
81.4056373417021));
#115694=CARTESIAN_POINT('Ctrl Pts',(-12.9849785040465,75.227891744384,81.4163718781257));
#115695=CARTESIAN_POINT('Ctrl Pts',(-12.9761722647469,75.7045067720495,
81.3811420042793));
#115696=CARTESIAN_POINT('Ctrl Pts',(-12.9675119086199,76.1752581060379,
81.3058749742284));
#115697=CARTESIAN_POINT('',(-13.5675364833309,80.654580018939,66.0024639308014));
#115698=CARTESIAN_POINT('Ctrl Pts',(-13.5590247159961,80.6563382683147,
65.9999193993703));
#115699=CARTESIAN_POINT('Ctrl Pts',(-13.5400068999588,79.7853367243258,
65.319462092606));
#115700=CARTESIAN_POINT('Ctrl Pts',(-13.5251921994605,78.7953578411616,
64.8005562641523));
#115701=CARTESIAN_POINT('Ctrl Pts',(-13.492890683205,76.5983471916873,64.1275891133102));
#115702=CARTESIAN_POINT('Ctrl Pts',(-13.4743351779794,75.5313749841502,
64.0511778965532));
#115703=CARTESIAN_POINT('Ctrl Pts',(-13.4484851075557,74.0420263880311,
64.1414492774393));
#115704=CARTESIAN_POINT('Ctrl Pts',(-13.4386640566306,73.4721998577258,
64.2318124979119));
#115705=CARTESIAN_POINT('Ctrl Pts',(-13.4186751669976,72.3508272271238,
64.5237563092107));
#115706=CARTESIAN_POINT('Ctrl Pts',(-13.4083630346961,71.8020941955304,
64.7265441047799));
#115707=CARTESIAN_POINT('Ctrl Pts',(-13.378889434965,70.2710191495859,65.4707072119258));
#115708=CARTESIAN_POINT('Ctrl Pts',(-13.3606766606445,69.3623365579809,
66.1482847756555));
#115709=CARTESIAN_POINT('Ctrl Pts',(-13.3311112102964,68.2320374767698,
67.3943249844395));
#115710=CARTESIAN_POINT('Ctrl Pts',(-13.3213178770165,67.897308892087,67.8425591305012));
#115711=CARTESIAN_POINT('Ctrl Pts',(-13.2977592138052,67.184560519637,69.0149548811999));
#115712=CARTESIAN_POINT('Ctrl Pts',(-13.2841131442571,66.86000923957,69.7671246312326));
#115713=CARTESIAN_POINT('Ctrl Pts',(-13.2551217230953,66.4298369296489,
71.3475877782227));
#115714=CARTESIAN_POINT('Ctrl Pts',(-13.2407852022714,66.3271265834845,
72.1679542467925));
#115715=CARTESIAN_POINT('Ctrl Pts',(-13.22669566117,66.3412155148882,72.9888893865797));
#115716=CARTESIAN_POINT('',(-13.5677219667119,82.8053136859618,77.4672764703467));
#115717=CARTESIAN_POINT('Origin',(-13.5675364833309,75.,72.98888938658));
#115718=CARTESIAN_POINT('',(-13.2736619003203,83.7052176583754,72.9888947630299));
#115719=CARTESIAN_POINT('Ctrl Pts',(-13.2736619003203,83.7052176583754,
72.9888947630299));
#115720=CARTESIAN_POINT('Ctrl Pts',(-13.3229312239107,83.753373874782,73.7448830644767));
#115721=CARTESIAN_POINT('Ctrl Pts',(-13.371980109432,83.7042558727909,74.5139171860313));
#115722=CARTESIAN_POINT('Ctrl Pts',(-13.470077354358,83.4046953760079,76.0245633284111));
#115723=CARTESIAN_POINT('Ctrl Pts',(-13.5191257137627,83.1524546020321,
76.7655416665762));
#115724=CARTESIAN_POINT('Ctrl Pts',(-13.5676947124535,82.8052754641751,
77.4672501945017));
#115725=CARTESIAN_POINT('Ctrl Pts',(-12.9679003706342,82.2015397612608,
68.6647904662762));
#115726=CARTESIAN_POINT('Ctrl Pts',(-13.0193150349774,82.6340458634664,
69.2881849289807));
#115727=CARTESIAN_POINT('Ctrl Pts',(-13.0702284178419,82.9868581475013,
69.9759204830991));
#115728=CARTESIAN_POINT('Ctrl Pts',(-13.1720553132675,83.4982142737106,
71.4337103090243));
#115729=CARTESIAN_POINT('Ctrl Pts',(-13.2229688258284,83.6545977325296,
72.2041789688228));
#115730=CARTESIAN_POINT('Ctrl Pts',(-13.2736619003203,83.7052176583754,
72.9888947630299));
#115731=CARTESIAN_POINT('Origin',(-15.9175364833309,75.,72.98888938658));
#115732=CARTESIAN_POINT('',(-8.59968985140647,83.3999999997258,72.98882151283));
#115733=CARTESIAN_POINT('Ctrl Pts',(-9.34771011126149,66.6,72.98888938658));
#115734=CARTESIAN_POINT('Ctrl Pts',(-9.34482801228272,66.6,73.0851880451777));
#115735=CARTESIAN_POINT('Ctrl Pts',(-9.34195702478471,66.6016559635923,
73.1815258398187));
#115736=CARTESIAN_POINT('Ctrl Pts',(-9.30786458115699,66.6413112039165,
74.3335679385027));
#115737=CARTESIAN_POINT('Ctrl Pts',(-9.28193074981338,66.8764288734639,
75.3728643345099));
#115738=CARTESIAN_POINT('Ctrl Pts',(-9.22587128847865,67.679423604765,77.2176616875703));
#115739=CARTESIAN_POINT('Ctrl Pts',(-9.19621563570561,68.2075392243034,
78.0223270669282));
#115740=CARTESIAN_POINT('Ctrl Pts',(-9.13661313794164,69.5837355649427,
79.4966046033503));
#115741=CARTESIAN_POINT('Ctrl Pts',(-9.11063836871128,70.4483040656611,
80.1280967594261));
#115742=CARTESIAN_POINT('Ctrl Pts',(-9.06544015277399,71.9032877835412,
80.816474494744));
#115743=CARTESIAN_POINT('Ctrl Pts',(-9.0492530382319,72.4207379848354,81.0018836652407));
#115744=CARTESIAN_POINT('Ctrl Pts',(-9.01641236916751,73.4770724783752,
81.2673682415297));
#115745=CARTESIAN_POINT('Ctrl Pts',(-8.99989317304966,74.0131508282444,
81.3482387615376));
#115746=CARTESIAN_POINT('Ctrl Pts',(-8.96482585598902,75.2614006272828,
81.414712312213));
#115747=CARTESIAN_POINT('Ctrl Pts',(-8.94677685625615,75.9714458658481,
81.3626105564356));
#115748=CARTESIAN_POINT('Ctrl Pts',(-8.89744367046157,77.738984272286,81.0048289169403));
#115749=CARTESIAN_POINT('Ctrl Pts',(-8.8636309510077,78.7585842810629,80.5803202299836));
#115750=CARTESIAN_POINT('Ctrl Pts',(-8.80454412642285,80.4315045504105,
79.4620643314559));
#115751=CARTESIAN_POINT('Ctrl Pts',(-8.78167961117171,81.1060256594941,
78.8300902543004));
#115752=CARTESIAN_POINT('Ctrl Pts',(-8.73113802125434,82.2232693318652,
77.3736308124975));
#115753=CARTESIAN_POINT('Ctrl Pts',(-8.70335941293635,82.6586024229665,
76.5591999956128));
#115754=CARTESIAN_POINT('Ctrl Pts',(-8.64831230121883,83.2492253893665,
74.8205244935375));
#115755=CARTESIAN_POINT('Ctrl Pts',(-8.62456332243574,83.400007425365,73.9078125751677));
#115756=CARTESIAN_POINT('Ctrl Pts',(-8.59968985140647,83.3999999997258,
72.9888215128297));
#115757=CARTESIAN_POINT('',(-8.57006447465355,83.3346137605936,71.9543844308784));
#115758=CARTESIAN_POINT('Ctrl Pts',(-8.57089042794284,83.336032673353,71.9542110458426));
#115759=CARTESIAN_POINT('Ctrl Pts',(-8.57495963766164,83.3535848314682,
72.0956224949622));
#115760=CARTESIAN_POINT('Ctrl Pts',(-8.57897898148748,83.3675359712116,
72.2374588562827));
#115761=CARTESIAN_POINT('Ctrl Pts',(-8.58861924885021,83.3926174828801,
72.5823258349277));
#115762=CARTESIAN_POINT('Ctrl Pts',(-8.5941877887613,83.3999983571592,72.7855388109754));
#115763=CARTESIAN_POINT('Ctrl Pts',(-8.59968985140647,83.3999999997258,
72.98882151283));
#115764=CARTESIAN_POINT('',(-8.56753648333115,72.6784966214631,81.0617217311459));
#115765=CARTESIAN_POINT('Origin',(-8.56753648333091,75.,72.98888938658));
#115766=CARTESIAN_POINT('Ctrl Pts',(-8.56753648333163,72.6784966214636,
81.0617217311443));
#115767=CARTESIAN_POINT('Ctrl Pts',(-8.59656065877325,71.6765852906451,
80.7736022161819));
#115768=CARTESIAN_POINT('Ctrl Pts',(-8.62742781849965,70.7370700765324,
80.3014901279046));
#115769=CARTESIAN_POINT('Ctrl Pts',(-8.66662311789324,69.6339116236681,
79.4606631122048));
#115770=CARTESIAN_POINT('Ctrl Pts',(-8.67610817330382,69.3729450473901,
79.2350896258631));
#115771=CARTESIAN_POINT('Ctrl Pts',(-8.71654432300731,68.3297664008052,
78.2148070440606));
#115772=CARTESIAN_POINT('Ctrl Pts',(-8.74937209339453,67.6960196716305,
77.2846877425061));
#115773=CARTESIAN_POINT('Ctrl Pts',(-8.79628814797203,67.0522382181187,
75.7609558810951));
#115774=CARTESIAN_POINT('Ctrl Pts',(-8.81096863053585,66.8905908306959,
75.2447202116387));
#115775=CARTESIAN_POINT('Ctrl Pts',(-8.84234325928866,66.6600179277575,
74.1476246372836));
#115776=CARTESIAN_POINT('Ctrl Pts',(-8.85902939320876,66.6,73.5686245783471));
#115777=CARTESIAN_POINT('Ctrl Pts',(-8.87591635085981,66.6,72.98888938658));
#115778=CARTESIAN_POINT('Origin',(-15.5675364833309,75.,72.98888938658));
#115779=CARTESIAN_POINT('',(-8.69331175948402,75.0000000064252,84.9888491626591));
#115780=CARTESIAN_POINT('',(-10.0948603023692,68.5588728119111,83.113703237526));
#115781=CARTESIAN_POINT('Ctrl Pts',(-8.69331176731091,75.00000000541,84.98885921934));
#115782=CARTESIAN_POINT('Ctrl Pts',(-8.69350218314475,74.6600650057603,
84.98888938658));
#115783=CARTESIAN_POINT('Ctrl Pts',(-8.70999108976109,74.3134431213811,
84.9744403493725));
#115784=CARTESIAN_POINT('Ctrl Pts',(-8.75917218585936,73.7855419536267,
84.9285832566471));
#115785=CARTESIAN_POINT('Ctrl Pts',(-8.77964050725442,73.6082514723118,
84.909267817465));
#115786=CARTESIAN_POINT('Ctrl Pts',(-8.81645492339044,73.3406310239618,
84.8739468570477));
#115787=CARTESIAN_POINT('Ctrl Pts',(-8.83639011496931,73.2064000704339,
84.8546995602693));
#115788=CARTESIAN_POINT('Ctrl Pts',(-8.862321809622,73.0491315493374,84.829402717515));
#115789=CARTESIAN_POINT('Ctrl Pts',(-8.87693003117094,72.9647120676162,
84.815081151703));
#115790=CARTESIAN_POINT('Ctrl Pts',(-8.8839421782897,72.9252717938844,84.8081870735222));
#115791=CARTESIAN_POINT('Ctrl Pts',(-8.88799686898513,72.9027238430882,
84.8041957936489));
#115792=CARTESIAN_POINT('Ctrl Pts',(-8.88930163845279,72.8955012600355,
84.8029108023554));
#115793=CARTESIAN_POINT('Ctrl Pts',(-8.93704499978251,72.6319881317605,
84.7558764051637));
#115794=CARTESIAN_POINT('Ctrl Pts',(-8.99631542872801,72.3531384263844,
84.6973357387733));
#115795=CARTESIAN_POINT('Ctrl Pts',(-9.10361344344678,71.9082647950302,
84.5847753581377));
#115796=CARTESIAN_POINT('Ctrl Pts',(-9.14244484356978,71.7555519361259,
84.5431226993059));
#115797=CARTESIAN_POINT('Ctrl Pts',(-9.20529003657942,71.5202786694363,
84.4735847300639));
#115798=CARTESIAN_POINT('Ctrl Pts',(-9.23786215629052,71.4010923796508,
84.4370504540915));
#115799=CARTESIAN_POINT('Ctrl Pts',(-9.27787462823113,71.2594384594255,
84.3911445732516));
#115800=CARTESIAN_POINT('Ctrl Pts',(-9.2983837806042,71.1879754503105,84.3673465065967));
#115801=CARTESIAN_POINT('Ctrl Pts',(-9.30950553626907,71.149523341116,84.3543678833721));
#115802=CARTESIAN_POINT('Ctrl Pts',(-9.31473235990037,71.1315334729288,
84.3482482258899));
#115803=CARTESIAN_POINT('Ctrl Pts',(-9.31772809691117,71.1212424447593,
84.3447357758996));
#115804=CARTESIAN_POINT('Ctrl Pts',(-9.31880084972148,71.1175603615012,
84.3434772194659));
#115805=CARTESIAN_POINT('Ctrl Pts',(-9.34657930546541,71.0222570215131,
84.3108766922396));
#115806=CARTESIAN_POINT('Ctrl Pts',(-9.37891704962667,70.913135968742,84.2722861271594));
#115807=CARTESIAN_POINT('Ctrl Pts',(-9.43490363978099,70.7273239494605,
84.2026583458093));
#115808=CARTESIAN_POINT('Ctrl Pts',(-9.45481249881782,70.6617014838166,
84.1774864582193));
#115809=CARTESIAN_POINT('Ctrl Pts',(-9.48654578085119,70.55787279937,84.1364851159369));
#115810=CARTESIAN_POINT('Ctrl Pts',(-9.49743520710866,70.5223643250653,
84.1222770859608));
#115811=CARTESIAN_POINT('Ctrl Pts',(-9.51983739078298,70.449574862264,84.0927253889727));
#115812=CARTESIAN_POINT('Ctrl Pts',(-9.53095785234192,70.4135596763115,
84.0779105446965));
#115813=CARTESIAN_POINT('Ctrl Pts',(-9.59204144661402,70.2164634050565,
83.9955682249674));
#115814=CARTESIAN_POINT('Ctrl Pts',(-9.63385426088831,70.0825860012239,
83.9357611550359));
#115815=CARTESIAN_POINT('Ctrl Pts',(-9.68599239058464,69.9159933359892,
83.8588763565762));
#115816=CARTESIAN_POINT('Ctrl Pts',(-9.70160825186424,69.8661689165978,
83.8353718207634));
#115817=CARTESIAN_POINT('Ctrl Pts',(-9.72238677085485,69.7998390819442,
83.8036444519207));
#115818=CARTESIAN_POINT('Ctrl Pts',(-9.73211471211796,69.7687762601497,
83.7886618832566));
#115819=CARTESIAN_POINT('Ctrl Pts',(-9.74230667001859,69.7361860747107,
83.7727864150422));
#115820=CARTESIAN_POINT('Ctrl Pts',(-9.74711332224232,69.7208001835745,
83.7652565559044));
#115821=CARTESIAN_POINT('Ctrl Pts',(-9.74911131746822,69.7144007217004,
83.7621175843978));
#115822=CARTESIAN_POINT('Ctrl Pts',(-9.75042953682232,69.7101775976573,
83.7600445931811));
#115823=CARTESIAN_POINT('Ctrl Pts',(-9.7506298848693,69.7095359546722,83.7597299081517));
#115824=CARTESIAN_POINT('Ctrl Pts',(-9.89216934436306,69.2558786469672,
83.536716801684));
#115825=CARTESIAN_POINT('Ctrl Pts',(-10.0065470818248,68.8761013310119,
83.3155165038809));
#115826=CARTESIAN_POINT('Ctrl Pts',(-10.0948603023669,68.55887270828,83.11370340042));
#115827=CARTESIAN_POINT('',(-11.4810890049562,63.0000050909298,72.9889042778823));
#115828=CARTESIAN_POINT('Ctrl Pts',(-10.0948603023724,68.558873019173,83.1137029117378));
#115829=CARTESIAN_POINT('Ctrl Pts',(-10.133102456483,68.4213962033965,83.026242433531));
#115830=CARTESIAN_POINT('Ctrl Pts',(-10.1701648695647,68.2886100604876,
82.9378350766575));
#115831=CARTESIAN_POINT('Ctrl Pts',(-10.2059877970713,68.1603864864389,
82.8488901634555));
#115832=CARTESIAN_POINT('Ctrl Pts',(-10.2427052753644,68.0289609825926,
82.7577241659478));
#115833=CARTESIAN_POINT('Ctrl Pts',(-10.2781207464655,67.9023287183454,
82.6659935513413));
#115834=CARTESIAN_POINT('Ctrl Pts',(-10.3122145517979,67.7803371412517,
82.5741097836734));
#115835=CARTESIAN_POINT('Ctrl Pts',(-10.3353371804666,67.6976017026478,
82.5117936467752));
#115836=CARTESIAN_POINT('Ctrl Pts',(-10.3578528237975,67.6170005007825,
82.4494064462423));
#115837=CARTESIAN_POINT('Ctrl Pts',(-10.3797659715751,67.5384825179955,
82.3870688292528));
#115838=CARTESIAN_POINT('Ctrl Pts',(-10.4068308106687,67.441505278958,82.3100758937589));
#115839=CARTESIAN_POINT('Ctrl Pts',(-10.4329770164788,67.347706085323,82.2331590847956));
#115840=CARTESIAN_POINT('Ctrl Pts',(-10.4582672655742,67.2569866678418,
82.1565373005544));
#115841=CARTESIAN_POINT('Ctrl Pts',(-10.4929960292256,67.132410069311,82.0513196799045));
#115842=CARTESIAN_POINT('Ctrl Pts',(-10.5260204794163,67.0136339528322,
81.9466545403682));
#115843=CARTESIAN_POINT('Ctrl Pts',(-10.5573359267471,66.9003753871923,
81.8430489324138));
#115844=CARTESIAN_POINT('Ctrl Pts',(-10.5735475602532,66.8417427788768,
81.7894135451373));
#115845=CARTESIAN_POINT('Ctrl Pts',(-10.5893015019345,66.7845887376899,
81.7360612971428));
#115846=CARTESIAN_POINT('Ctrl Pts',(-10.6045989629336,66.7288733548622,
81.6830574812477));
#115847=CARTESIAN_POINT('Ctrl Pts',(-10.6270224795161,66.6472039320208,
81.605362761534));
#115848=CARTESIAN_POINT('Ctrl Pts',(-10.6484634459094,66.5686253077469,
81.5284170018002));
#115849=CARTESIAN_POINT('Ctrl Pts',(-10.6689218629804,66.4930090465584,
81.4524110711747));
#115850=CARTESIAN_POINT('Ctrl Pts',(-10.679151071516,66.4552009159641,81.4144081058619));
#115851=CARTESIAN_POINT('Ctrl Pts',(-10.6891346427481,66.4181333499334,
81.3766398443326));
#115852=CARTESIAN_POINT('Ctrl Pts',(-10.6988725767297,66.381790184475,81.3391286570921));
#115853=CARTESIAN_POINT('Ctrl Pts',(-10.7024765937321,66.3683395504414,
81.325245737281));
#115854=CARTESIAN_POINT('Ctrl Pts',(-10.706046974037,66.3549881473234,81.3113980276785));
#115855=CARTESIAN_POINT('Ctrl Pts',(-10.709583694381,66.3417351446778,81.297586618752));
#115856=CARTESIAN_POINT('Ctrl Pts',(-10.7108250243624,66.3370835613104,
81.2927390440732));
#115857=CARTESIAN_POINT('Ctrl Pts',(-10.7120622078409,66.3324440998453,
81.287895941108));
#115858=CARTESIAN_POINT('Ctrl Pts',(-10.7132952497367,66.3278167251015,
81.2830573588835));
#115859=CARTESIAN_POINT('Ctrl Pts',(-10.715668323907,66.3189110232607,81.2737451736792));
#115860=CARTESIAN_POINT('Ctrl Pts',(-10.7180260457432,66.3100500875175,
81.2644497305875));
#115861=CARTESIAN_POINT('Ctrl Pts',(-10.7203684152401,66.3012336595681,
81.2551713679032));
#115862=CARTESIAN_POINT('Ctrl Pts',(-10.7221251923627,66.2946213386061,
81.2482125958899));
#115863=CARTESIAN_POINT('Ctrl Pts',(-10.7238733337944,66.2880340533221,
81.2412634315616));
#115864=CARTESIAN_POINT('Ctrl Pts',(-10.7256128395322,66.2814716949002,
81.2343240161859));
#115865=CARTESIAN_POINT('Ctrl Pts',(-10.7261926747782,66.2792842420929,
81.2320108777274));
#115866=CARTESIAN_POINT('Ctrl Pts',(-10.7265389790354,66.2779776304599,
81.2306288274579));
#115867=CARTESIAN_POINT('Ctrl Pts',(-10.7273494667053,66.27491764138,81.2273878556018));
#115868=CARTESIAN_POINT('Ctrl Pts',(-10.7793655551984,66.0785313560826,
81.0193863212973));
#115869=CARTESIAN_POINT('Ctrl Pts',(-10.8286358129281,65.8881034723919,
80.8027848089594));
#115870=CARTESIAN_POINT('Ctrl Pts',(-10.8751613041746,65.7044664115946,
80.5778594555792));
#115871=CARTESIAN_POINT('Ctrl Pts',(-10.9198306168304,65.5281557254704,
80.3619077124559));
#115872=CARTESIAN_POINT('Ctrl Pts',(-10.9619698078079,65.3581048515807,
80.1382831909005));
#115873=CARTESIAN_POINT('Ctrl Pts',(-11.0015776921892,65.1950899867055,
79.9072521474355));
#115874=CARTESIAN_POINT('Ctrl Pts',(-11.0029937456614,65.1892619105779,
79.8989923699595));
#115875=CARTESIAN_POINT('Ctrl Pts',(-11.0044065633973,65.1834428321696,
79.890723127841));
#115876=CARTESIAN_POINT('Ctrl Pts',(-11.0058161517136,65.1776327838717,
79.8824444393747));
#115877=CARTESIAN_POINT('Ctrl Pts',(-11.0435518881779,65.0220934332085,
79.6608177398417));
#115878=CARTESIAN_POINT('Ctrl Pts',(-11.0789695059325,64.873026151247,79.4324241836466));
#115879=CARTESIAN_POINT('Ctrl Pts',(-11.1120688318277,64.7310579934169,
79.1976100654547));
#115880=CARTESIAN_POINT('Ctrl Pts',(-11.1148890648589,64.7189615752194,
79.1776026932682));
#115881=CARTESIAN_POINT('Ctrl Pts',(-11.117692469965,64.7069167213773,79.1575487267407));
#115882=CARTESIAN_POINT('Ctrl Pts',(-11.1204790485698,64.6949238339657,
79.1374483905087));
#115883=CARTESIAN_POINT('Ctrl Pts',(-11.1382245102557,64.6185508496559,
79.0094456326251));
#115884=CARTESIAN_POINT('Ctrl Pts',(-11.1552874613776,64.5442849053233,
78.8795620147912));
#115885=CARTESIAN_POINT('Ctrl Pts',(-11.1716678992142,64.4722319657888,
78.7478570972825));
#115886=CARTESIAN_POINT('Ctrl Pts',(-11.1798581181324,64.4362054960215,
78.6820046385282));
#115887=CARTESIAN_POINT('Ctrl Pts',(-11.1878777087469,64.4007323054803,
78.6156968418008));
#115888=CARTESIAN_POINT('Ctrl Pts',(-11.1957266710059,64.3658260660908,
78.5489415654864));
#115889=CARTESIAN_POINT('Ctrl Pts',(-11.1996511521354,64.3483729463961,
78.5155639273292));
#115890=CARTESIAN_POINT('Ctrl Pts',(-11.2035329761818,64.3310615664533,
78.4820744193169));
#115891=CARTESIAN_POINT('Ctrl Pts',(-11.2073721431682,64.3138936541916,
78.4484740371538));
#115892=CARTESIAN_POINT('Ctrl Pts',(-11.2092917266615,64.3053096980607,
78.4316738460722));
#115893=CARTESIAN_POINT('Ctrl Pts',(-11.21120064589,64.2967616089859,78.4148459364674));
#115894=CARTESIAN_POINT('Ctrl Pts',(-11.2130989008581,64.2882496045795,
78.3979904344908));
#115895=CARTESIAN_POINT('Ctrl Pts',(-11.2145225920841,64.2818656012747,
78.3853488080083));
#115896=CARTESIAN_POINT('Ctrl Pts',(-11.2159402846636,64.2755018956071,
78.3726916608183));
#115897=CARTESIAN_POINT('Ctrl Pts',(-11.2173519785987,64.2691585797592,
78.3600190465254));
#115898=CARTESIAN_POINT('Ctrl Pts',(-11.2178225432437,64.2670441411433,
78.3557948417611));
#115899=CARTESIAN_POINT('Ctrl Pts',(-11.2184210608201,64.2643536295815,
78.3504100947542));
#115900=CARTESIAN_POINT('Ctrl Pts',(-11.2187616729857,64.2628220639561,
78.3473412785494));
#115901=CARTESIAN_POINT('Ctrl Pts',(-11.2191016706038,64.2612932616486,
78.3442779992375));
#115902=CARTESIAN_POINT('Ctrl Pts',(-11.2194413371642,64.2597656118155,
78.3412137409868));
#115903=CARTESIAN_POINT('Ctrl Pts',(-11.2197806726984,64.2582391159477,
78.3381485044332));
#115904=CARTESIAN_POINT('Ctrl Pts',(-11.2452797298039,64.143531985737,78.1078141184037));
#115905=CARTESIAN_POINT('Ctrl Pts',(-11.2689091762991,64.0353380185579,
77.8719524167333));
#115906=CARTESIAN_POINT('Ctrl Pts',(-11.2906711856469,63.9342181600986,
77.6308953725145));
#115907=CARTESIAN_POINT('Ctrl Pts',(-11.3121098637698,63.8346007000241,
77.3934198573781));
#115908=CARTESIAN_POINT('Ctrl Pts',(-11.331736163075,63.7418486954108,77.1509021497749));
#115909=CARTESIAN_POINT('Ctrl Pts',(-11.349557324713,63.6565317893308,76.9036976654529));
#115910=CARTESIAN_POINT('Ctrl Pts',(-11.3522702568957,63.6435439165455,
76.8660654945054));
#115911=CARTESIAN_POINT('Ctrl Pts',(-11.3549413665753,63.630728410555,76.82832478512));
#115912=CARTESIAN_POINT('Ctrl Pts',(-11.357570690475,63.6180873502402,76.7904768718687));
#115913=CARTESIAN_POINT('Ctrl Pts',(-11.3745287988962,63.5365574666819,
76.5463726683083));
#115914=CARTESIAN_POINT('Ctrl Pts',(-11.3897484533509,63.4622819653971,
76.2978054605891));
#115915=CARTESIAN_POINT('Ctrl Pts',(-11.4032166767484,63.3957559838242,
76.0452199248016));
#115916=CARTESIAN_POINT('Ctrl Pts',(-11.4073561755882,63.3753090239386,
75.9675870031096));
#115917=CARTESIAN_POINT('Ctrl Pts',(-11.4113302485379,63.3555943162169,
75.8895748038605));
#115918=CARTESIAN_POINT('Ctrl Pts',(-11.4151385858384,63.3366267390366,
75.8111970970855));
#115919=CARTESIAN_POINT('Ctrl Pts',(-11.4225524542904,63.2997016688621,
75.6586155472498));
#115920=CARTESIAN_POINT('Ctrl Pts',(-11.4293373885995,63.2656083264762,
75.5046503952037));
#115921=CARTESIAN_POINT('Ctrl Pts',(-11.4354993489759,63.2344585032999,
75.34940560247));
#115922=CARTESIAN_POINT('Ctrl Pts',(-11.4459029018496,63.1818666635891,
75.0872978784816));
#115923=CARTESIAN_POINT('Ctrl Pts',(-11.4545307022797,63.1376642995191,
74.8215401834039));
#115924=CARTESIAN_POINT('Ctrl Pts',(-11.4613769255451,63.1023184811442,
74.5526099866829));
#115925=CARTESIAN_POINT('Ctrl Pts',(-11.4656979782655,63.0800096637533,
74.3828723790852));
#115926=CARTESIAN_POINT('Ctrl Pts',(-11.4693093299393,63.0612294271659,
74.2118718404528));
#115927=CARTESIAN_POINT('Ctrl Pts',(-11.4722096451391,63.046100307838,74.0397378739752));
#115928=CARTESIAN_POINT('Ctrl Pts',(-11.4764452699417,63.0240057185764,
73.7883531631491));
#115929=CARTESIAN_POINT('Ctrl Pts',(-11.4791643413329,63.0096976470856,
73.5345483639279));
#115930=CARTESIAN_POINT('Ctrl Pts',(-11.4803701594022,63.0035133775259,
73.2789208597845));
#115931=CARTESIAN_POINT('Ctrl Pts',(-11.4808250032522,63.0011806234832,
73.1824961991291));
#115932=CARTESIAN_POINT('Ctrl Pts',(-11.4810645445765,63.0000039177617,
73.0858126969849));
#115933=CARTESIAN_POINT('Ctrl Pts',(-11.4810890049761,63.000001907456,72.9889042779483));
#115934=CARTESIAN_POINT('',(-10.0948866959807,68.5588359045711,62.8641001495972));
#115935=CARTESIAN_POINT('Ctrl Pts',(-11.4810890049462,63.0000066826667,
72.9889042778822));
#115936=CARTESIAN_POINT('Ctrl Pts',(-11.4810244535258,63.0000209039102,
72.7386008713444));
#115937=CARTESIAN_POINT('Ctrl Pts',(-11.4795275015916,63.0078785296247,
72.4899373152444));
#115938=CARTESIAN_POINT('Ctrl Pts',(-11.47660614196,63.023222893841,72.2434339617198));
#115939=CARTESIAN_POINT('Ctrl Pts',(-11.4736219335098,63.0388973698158,
71.9916274457857));
#115940=CARTESIAN_POINT('Ctrl Pts',(-11.4691513830198,63.0623841707853,
71.7420749690625));
#115941=CARTESIAN_POINT('Ctrl Pts',(-11.4632023050969,63.0933255526803,
71.4952817751537));
#115942=CARTESIAN_POINT('Ctrl Pts',(-11.4617464824254,63.1008973420957,
71.4348880248103));
#115943=CARTESIAN_POINT('Ctrl Pts',(-11.4602021144584,63.1089156523144,
71.3746592912387));
#115944=CARTESIAN_POINT('Ctrl Pts',(-11.4585693081243,63.1173754402577,
71.3146025538948));
#115945=CARTESIAN_POINT('Ctrl Pts',(-11.4515256738386,63.1538694513121,
71.0555285379512));
#115946=CARTESIAN_POINT('Ctrl Pts',(-11.4428362393565,63.1985761183067,
70.7996584347455));
#115947=CARTESIAN_POINT('Ctrl Pts',(-11.4324898914039,63.2510013435756,
70.5473945000403));
#115948=CARTESIAN_POINT('Ctrl Pts',(-11.4234647054344,63.2967322052971,
70.3273430447311));
#115949=CARTESIAN_POINT('Ctrl Pts',(-11.4131787609363,63.3483368706343,
70.1100348172557));
#115950=CARTESIAN_POINT('Ctrl Pts',(-11.4016248773891,63.4055085587195,
69.8957124157511));
#115951=CARTESIAN_POINT('Ctrl Pts',(-11.3908685226147,63.4587338623659,
69.6961840253826));
#115952=CARTESIAN_POINT('Ctrl Pts',(-11.3790120736584,63.5167729773594,
69.4992875261014));
#115953=CARTESIAN_POINT('Ctrl Pts',(-11.3660704530696,63.579377814658,69.3052223934151));
#115954=CARTESIAN_POINT('Ctrl Pts',(-11.3498974798454,63.6576142573346,
69.0627017467036));
#115955=CARTESIAN_POINT('Ctrl Pts',(-11.3320293496765,63.7429795757764,
68.8246039756175));
#115956=CARTESIAN_POINT('Ctrl Pts',(-11.3124495579103,63.8348996525675,
68.5912730209228));
#115957=CARTESIAN_POINT('Ctrl Pts',(-11.3093161883228,63.8496096952754,
68.5539328833982));
#115958=CARTESIAN_POINT('Ctrl Pts',(-11.3061389972225,63.8644876721369,
68.516714739936));
#115959=CARTESIAN_POINT('Ctrl Pts',(-11.3029179326569,63.8795313071419,
68.4796199057335));
#115960=CARTESIAN_POINT('Ctrl Pts',(-11.2831903810548,63.9716667113824,
68.2524309621477));
#115961=CARTESIAN_POINT('Ctrl Pts',(-11.2618246134247,64.0700160665622,
68.0298633002975));
#115962=CARTESIAN_POINT('Ctrl Pts',(-11.2388206575932,64.1740820572025,
67.8121857422244));
#115963=CARTESIAN_POINT('Ctrl Pts',(-11.2273186796775,64.2261150525226,
67.7033469631879));
#115964=CARTESIAN_POINT('Ctrl Pts',(-11.2154071551784,64.2795777051529,
67.5957302111428));
#115965=CARTESIAN_POINT('Ctrl Pts',(-11.2030860857381,64.3344106010308,
67.4893664567818));
#115966=CARTESIAN_POINT('Ctrl Pts',(-11.1969255510179,64.3618270489698,
67.4361845796012));
#115967=CARTESIAN_POINT('Ctrl Pts',(-11.1906626300008,64.3895860653485,
67.3833159637608));
#115968=CARTESIAN_POINT('Ctrl Pts',(-11.1842973224823,64.4176803955192,
67.3307643015798));
#115969=CARTESIAN_POINT('Ctrl Pts',(-11.1811146687231,64.4317275606045,
67.3044884704894));
#115970=CARTESIAN_POINT('Ctrl Pts',(-11.1779064183332,64.4458585544738,
67.2782918787736));
#115971=CARTESIAN_POINT('Ctrl Pts',(-11.174672571257,64.4600724756541,67.2521749866161));
#115972=CARTESIAN_POINT('Ctrl Pts',(-11.1730556477189,64.4671794362442,
67.2391165405373));
#115973=CARTESIAN_POINT('Ctrl Pts',(-11.1714323250089,64.4743071286741,
67.2260780194078));
#115974=CARTESIAN_POINT('Ctrl Pts',(-11.1698026031183,64.4814554407902,
67.213059480252));
#115975=CARTESIAN_POINT('Ctrl Pts',(-11.168987742173,64.4850295968483,67.2065502106741));
#115976=CARTESIAN_POINT('Ctrl Pts',(-11.1681712814325,64.4886089078284,
67.2000459365936));
#115977=CARTESIAN_POINT('Ctrl Pts',(-11.1673532208957,64.4921933597455,
67.1935466651054));
#115978=CARTESIAN_POINT('Ctrl Pts',(-11.1665624051131,64.4956584347858,
67.1872638458808));
#115979=CARTESIAN_POINT('Ctrl Pts',(-11.1659133956055,64.4985010255737,
67.1821184487777));
#115980=CARTESIAN_POINT('Ctrl Pts',(-11.1649906082438,64.5025403038718,
67.174825409623));
#115981=CARTESIAN_POINT('Ctrl Pts',(-11.1649588168765,64.5026794628862,
67.1745741538129));
#115982=CARTESIAN_POINT('Ctrl Pts',(-11.164926699816,64.5028200447192,67.1743203504369));
#115983=CARTESIAN_POINT('Ctrl Pts',(-11.1648942398947,64.502962124333,67.1740638655116));
#115984=CARTESIAN_POINT('Ctrl Pts',(-11.133705344973,64.6394783563636,66.9276220667889));
#115985=CARTESIAN_POINT('Ctrl Pts',(-11.1001630834324,64.7836965504124,
66.6878447959721));
#115986=CARTESIAN_POINT('Ctrl Pts',(-11.0642655908435,64.9348380776373,
66.455054390543));
#115987=CARTESIAN_POINT('Ctrl Pts',(-11.0283680982545,65.0859796048621,
66.222263985114));
#115988=CARTESIAN_POINT('Ctrl Pts',(-10.9901154073647,65.2440446410345,
65.9964602437078));
#115989=CARTESIAN_POINT('Ctrl Pts',(-10.9495093621566,65.4083044678963,
65.7779331134484));
#115990=CARTESIAN_POINT('Ctrl Pts',(-10.9164961960038,65.5418495331351,
65.600268127283));
#115991=CARTESIAN_POINT('Ctrl Pts',(-10.8819326095739,65.6794935075489,
65.4274080152561));
#115992=CARTESIAN_POINT('Ctrl Pts',(-10.8458035256173,65.8208659609748,
65.2594975392633));
#115993=CARTESIAN_POINT('Ctrl Pts',(-10.8374939995453,65.8533809865151,
65.2208788884364));
#115994=CARTESIAN_POINT('Ctrl Pts',(-10.8291016705225,65.8860933193816,
65.1825220121138));
#115995=CARTESIAN_POINT('Ctrl Pts',(-10.8206283362097,65.9189985771524,
65.1444274192187));
#115996=CARTESIAN_POINT('Ctrl Pts',(-10.7979710152082,66.0069857803518,
65.0425641635285));
#115997=CARTESIAN_POINT('Ctrl Pts',(-10.7747251214092,66.0963494876869,
64.942579704158));
#115998=CARTESIAN_POINT('Ctrl Pts',(-10.7508906568507,66.1869974467674,
64.8444930011935));
#115999=CARTESIAN_POINT('Ctrl Pts',(-10.7389734245714,66.2323214263077,
64.7954496497112));
#116000=CARTESIAN_POINT('Ctrl Pts',(-10.7269090494873,66.2779664681663,
64.7468807246663));
#116001=CARTESIAN_POINT('Ctrl Pts',(-10.7146975314213,66.3239213020834,
64.6987882485336));
#116002=CARTESIAN_POINT('Ctrl Pts',(-10.7085917723883,66.346898719042,64.6747420104673));
#116003=CARTESIAN_POINT('Ctrl Pts',(-10.7024492276056,66.3699535839574,
64.6508148841806));
#116004=CARTESIAN_POINT('Ctrl Pts',(-10.6962698970365,66.3930844949761,
64.6270071118253));
#116005=CARTESIAN_POINT('Ctrl Pts',(-10.693180231752,66.4046499504855,64.6151032256477));
#116006=CARTESIAN_POINT('Ctrl Pts',(-10.6900813700207,66.4162344175122,
64.6032291779221));
#116007=CARTESIAN_POINT('Ctrl Pts',(-10.6869733118381,66.4278377216821,
64.5913849977991));
#116008=CARTESIAN_POINT('Ctrl Pts',(-10.6846422682011,66.4365401998095,
64.5825018627067));
#116009=CARTESIAN_POINT('Ctrl Pts',(-10.6823060515603,66.4452532738292,
64.5736355281385));
#116010=CARTESIAN_POINT('Ctrl Pts',(-10.6799646619137,66.4539768703599,
64.564786006148));
#116011=CARTESIAN_POINT('Ctrl Pts',(-10.6791841986982,66.4568847358701,
64.5618361654845));
#116012=CARTESIAN_POINT('Ctrl Pts',(-10.678163888481,66.4606846596497,64.5579863129423));
#116013=CARTESIAN_POINT('Ctrl Pts',(-10.6776215479318,66.4627039716936,
64.5559420887767));
#116014=CARTESIAN_POINT('Ctrl Pts',(-10.652920616734,66.5546736537245,64.4628377827436));
#116015=CARTESIAN_POINT('Ctrl Pts',(-10.6266237018721,66.6518339313718,
64.3675198611269));
#116016=CARTESIAN_POINT('Ctrl Pts',(-10.5986163301073,66.7544884150816,
64.2704343258768));
#116017=CARTESIAN_POINT('Ctrl Pts',(-10.5712573585473,66.8547663391904,
64.1755964231955));
#116018=CARTESIAN_POINT('Ctrl Pts',(-10.542266066329,66.9602873558472,64.0790717461688));
#116019=CARTESIAN_POINT('Ctrl Pts',(-10.5115377512955,67.0713326407731,
63.9813254725246));
#116020=CARTESIAN_POINT('Ctrl Pts',(-10.4965124517656,67.1256307259617,
63.9335302374838));
#116021=CARTESIAN_POINT('Ctrl Pts',(-10.4810718844178,67.1812495720263,
63.8854436899028));
#116022=CARTESIAN_POINT('Ctrl Pts',(-10.4652041499233,67.2382215142498,
63.8371247472103));
#116023=CARTESIAN_POINT('Ctrl Pts',(-10.4356119623104,67.3444701033932,
63.7470133820432));
#116024=CARTESIAN_POINT('Ctrl Pts',(-10.4045313128674,67.4554250840708,
63.656091786564));
#116025=CARTESIAN_POINT('Ctrl Pts',(-10.3719812538623,67.5712962804336,
63.5647574873318));
#116026=CARTESIAN_POINT('Ctrl Pts',(-10.3401570523442,67.6845835805459,
63.4754599181993));
#116027=CARTESIAN_POINT('Ctrl Pts',(-10.3069279981041,67.8025704642133,
63.385767843356));
#116028=CARTESIAN_POINT('Ctrl Pts',(-10.2723471316926,67.9254453728009,
63.2960856483857));
#116029=CARTESIAN_POINT('Ctrl Pts',(-10.2388925685195,68.0443182299126,
63.2093244139668));
#116030=CARTESIAN_POINT('Ctrl Pts',(-10.2041726718904,68.1677660318666,
63.1225724811793));
#116031=CARTESIAN_POINT('Ctrl Pts',(-10.1682715444886,68.2959498272669,
63.0362266371425));
#116032=CARTESIAN_POINT('Ctrl Pts',(-10.1443231826302,68.381456666154,62.9786284036718));
#116033=CARTESIAN_POINT('Ctrl Pts',(-10.1198499387848,68.4690707061841,
62.9212114915483));
#116034=CARTESIAN_POINT('Ctrl Pts',(-10.0948866960176,68.5588367757668,
62.8641015189355));
#116035=CARTESIAN_POINT('',(-8.69365830054191,74.99999996484,60.98889557741));
#116036=CARTESIAN_POINT('Ctrl Pts',(-10.0948866959449,68.55883546897,62.86409946493));
#116037=CARTESIAN_POINT('Ctrl Pts',(-10.0517874763325,68.713679379568,62.7655898290921));
#116038=CARTESIAN_POINT('Ctrl Pts',(-10.0025194376179,68.8832413055288,
62.6626774372055));
#116039=CARTESIAN_POINT('Ctrl Pts',(-9.91936415089262,69.161045298009,62.5047129513255));
#116040=CARTESIAN_POINT('Ctrl Pts',(-9.89010351720865,69.2575565756358,
62.4514647396401));
#116041=CARTESIAN_POINT('Ctrl Pts',(-9.84389925951936,69.4083541324548,
62.3711334956229));
#116042=CARTESIAN_POINT('Ctrl Pts',(-9.82021880388388,69.4852604507093,
62.3308537265188));
#116043=CARTESIAN_POINT('Ctrl Pts',(-9.79157953375854,69.5776573407017,
62.2837614623395));
#116044=CARTESIAN_POINT('Ctrl Pts',(-9.77700688072487,69.6245281826994,
62.2602035713135));
#116045=CARTESIAN_POINT('Ctrl Pts',(-9.76965729971529,69.6481322203813,
62.2484233295547));
#116046=CARTESIAN_POINT('Ctrl Pts',(-9.76649392474845,69.6582844236361,
62.2433745542121));
#116047=CARTESIAN_POINT('Ctrl Pts',(-9.76438199598519,69.6650606067955,
62.2400087014928));
#116048=CARTESIAN_POINT('Ctrl Pts',(-9.76289125250944,69.6698422307222,
62.237637219044));
#116049=CARTESIAN_POINT('Ctrl Pts',(-9.74224303814605,69.736061144494,62.2048232038921));
#116050=CARTESIAN_POINT('Ctrl Pts',(-9.7152274917603,69.822130672148,62.1628079730791));
#116051=CARTESIAN_POINT('Ctrl Pts',(-9.66421461894981,69.9851088712327,
62.0868501574437));
#116052=CARTESIAN_POINT('Ctrl Pts',(-9.645462069141,70.0450855257516,62.0593877994143));
#116053=CARTESIAN_POINT('Ctrl Pts',(-9.61471085611982,70.1436997066793,
62.0153920835851));
#116054=CARTESIAN_POINT('Ctrl Pts',(-9.60402338706143,70.1780128534713,
62.0002606485247));
#116055=CARTESIAN_POINT('Ctrl Pts',(-9.58177431950867,70.2495538013399,
61.9691442671256));
#116056=CARTESIAN_POINT('Ctrl Pts',(-9.57054973139168,70.2856945972867,
61.9536190736345));
#116057=CARTESIAN_POINT('Ctrl Pts',(-9.50887136344287,70.4846360990521,
61.869476191664));
#116058=CARTESIAN_POINT('Ctrl Pts',(-9.4658047898713,70.6256256598509,61.8138358171528));
#116059=CARTESIAN_POINT('Ctrl Pts',(-9.41061911069516,70.8083647148666,
61.7445825194025));
#116060=CARTESIAN_POINT('Ctrl Pts',(-9.39379291449998,70.8644935704817,
61.7238746103894));
#116061=CARTESIAN_POINT('Ctrl Pts',(-9.37090716550251,70.9413769302308,
61.6960455635373));
#116062=CARTESIAN_POINT('Ctrl Pts',(-9.36005267732761,70.9779916361502,
61.6829401129446));
#116063=CARTESIAN_POINT('Ctrl Pts',(-9.34841878385691,71.0174873934192,
61.6690029851454));
#116064=CARTESIAN_POINT('Ctrl Pts',(-9.34285925613824,71.0364272480192,
61.6623653530905));
#116065=CARTESIAN_POINT('Ctrl Pts',(-9.34014384703307,71.0456948436297,
61.6591283889064));
#116066=CARTESIAN_POINT('Ctrl Pts',(-9.33899389057818,71.0496232796143,
61.6577585658768));
#116067=CARTESIAN_POINT('Ctrl Pts',(-9.33823031745369,71.0522325908458,
61.6568492175692));
#116068=CARTESIAN_POINT('Ctrl Pts',(-9.33816064917692,71.0524704010327,
61.6567661833087));
#116069=CARTESIAN_POINT('Ctrl Pts',(-9.29335562400464,71.2056773548895,
61.6034324787957));
#116070=CARTESIAN_POINT('Ctrl Pts',(-9.25256208948599,71.3495159998227,
61.5567275679463));
#116071=CARTESIAN_POINT('Ctrl Pts',(-9.19635506156912,71.5541522804732,
61.4940547720857));
#116072=CARTESIAN_POINT('Ctrl Pts',(-9.16949736607596,71.6536924314009,
61.4645663009794));
#116073=CARTESIAN_POINT('Ctrl Pts',(-9.14034357031482,71.7648525579011,
61.4331264352157));
#116074=CARTESIAN_POINT('Ctrl Pts',(-9.12631171801281,71.8191781361214,
61.4181151035729));
#116075=CARTESIAN_POINT('Ctrl Pts',(-9.11943205325644,71.846025843946,61.4107826062409));
#116076=CARTESIAN_POINT('Ctrl Pts',(-9.116512824374,71.8574643349694,61.4076767929975));
#116077=CARTESIAN_POINT('Ctrl Pts',(-9.11457316042354,71.8650749413428,
61.4056143565919));
#116078=CARTESIAN_POINT('Ctrl Pts',(-9.11392168583116,71.8676329160552,
61.4049218626105));
#116079=CARTESIAN_POINT('Ctrl Pts',(-9.07173262458759,72.0336242990951,
61.3601142300229));
#116080=CARTESIAN_POINT('Ctrl Pts',(-9.03417637446264,72.1909616694013,
61.3212391441379));
#116081=CARTESIAN_POINT('Ctrl Pts',(-8.98287353135119,72.421132329324,61.2690075114148));
#116082=CARTESIAN_POINT('Ctrl Pts',(-8.95847999281444,72.5347600286294,
61.244412301046));
#116083=CARTESIAN_POINT('Ctrl Pts',(-8.93222215980482,72.6646996977874,
61.2182123336129));
#116084=CARTESIAN_POINT('Ctrl Pts',(-8.91964356712081,72.7290045056888,
61.2057154921927));
#116085=CARTESIAN_POINT('Ctrl Pts',(-8.91349185173401,72.7609896077938,
61.1996153101984));
#116086=CARTESIAN_POINT('Ctrl Pts',(-8.91088488391578,72.7746615487225,
61.1970324401455));
#116087=CARTESIAN_POINT('Ctrl Pts',(-8.90915345684435,72.7837681728654,
61.1953174952357));
#116088=CARTESIAN_POINT('Ctrl Pts',(-8.90853914396999,72.787004805579,61.1947091358399));
#116089=CARTESIAN_POINT('Ctrl Pts',(-8.76569912277902,73.5426843179641,
61.0533060591291));
#116090=CARTESIAN_POINT('Ctrl Pts',(-8.69444127063165,74.2829857452934,
60.9888893886809));
#116091=CARTESIAN_POINT('Ctrl Pts',(-8.69365830054191,74.99999996484,60.98889557741));
#116092=CARTESIAN_POINT('',(-8.56753648333091,75.,60.98888938658));
#116093=CARTESIAN_POINT('',(-15.5675364833309,75.,60.98888938658));
#116094=CARTESIAN_POINT('Origin',(-8.56753648333091,75.,72.98888938658));
#116095=CARTESIAN_POINT('',(-10.0948723726626,81.4411120680386,62.8640650186986));
#116096=CARTESIAN_POINT('Ctrl Pts',(-8.69365830112979,74.9999999638356,
60.9889038049687));
#116097=CARTESIAN_POINT('Ctrl Pts',(-8.69384525819957,75.1754233378247,
60.9889252073905));
#116098=CARTESIAN_POINT('Ctrl Pts',(-8.6982707338728,75.3522672414099,60.9928047886458));
#116099=CARTESIAN_POINT('Ctrl Pts',(-8.70692055121058,75.5303670372353,
61.0006933469007));
#116100=CARTESIAN_POINT('Ctrl Pts',(-8.71504876408759,75.6977269937859,
61.0081062064195));
#116101=CARTESIAN_POINT('Ctrl Pts',(-8.72690760340725,75.8661963210868,
61.0190593542814));
#116102=CARTESIAN_POINT('Ctrl Pts',(-8.74250791810455,76.0356077139438,
61.0337104975575));
#116103=CARTESIAN_POINT('Ctrl Pts',(-8.74350902300405,76.046479198187,61.034650692137));
#116104=CARTESIAN_POINT('Ctrl Pts',(-8.74452554254038,76.0573545496545,
61.0356061263879));
#116105=CARTESIAN_POINT('Ctrl Pts',(-8.74555748243123,76.0682337189115,
61.0365768465842));
#116106=CARTESIAN_POINT('Ctrl Pts',(-8.75602273934144,76.1785631114021,
61.0464212535427));
#116107=CARTESIAN_POINT('Ctrl Pts',(-8.76806128130061,76.2892941174044,
61.0578380775563));
#116108=CARTESIAN_POINT('Ctrl Pts',(-8.7816935935759,76.4003647326638,61.0708786774501));
#116109=CARTESIAN_POINT('Ctrl Pts',(-8.7903528007498,76.4709164812624,61.0791620305506));
#116110=CARTESIAN_POINT('Ctrl Pts',(-8.79965517985068,76.5416050269056,
61.0881006652942));
#116111=CARTESIAN_POINT('Ctrl Pts',(-8.80959012670336,76.6124245282971,
61.0977035097661));
#116112=CARTESIAN_POINT('Ctrl Pts',(-8.82237796377352,76.7035803501261,
61.1100638789093));
#116113=CARTESIAN_POINT('Ctrl Pts',(-8.83622366435869,76.794946917876,61.1235238847051));
#116114=CARTESIAN_POINT('Ctrl Pts',(-8.85112722717444,76.8864966022424,
61.1381012094152));
#116115=CARTESIAN_POINT('Ctrl Pts',(-8.85857900858232,76.9322714444256,
61.1453898717702));
#116116=CARTESIAN_POINT('Ctrl Pts',(-8.86629525561024,76.9780920688098,
61.1529578765693));
#116117=CARTESIAN_POINT('Ctrl Pts',(-8.87427596840209,77.023954905813,61.160807494838));
#116118=CARTESIAN_POINT('Ctrl Pts',(-8.87826632479801,77.0468863243146,
61.1647323039724));
#116119=CARTESIAN_POINT('Ctrl Pts',(-8.88232279763742,77.0698282960359,
61.1687275173494));
#116120=CARTESIAN_POINT('Ctrl Pts',(-8.88644538694687,77.0927803713609,
61.1727934236992));
#116121=CARTESIAN_POINT('Ctrl Pts',(-8.88953732892895,77.1099944278547,
61.1758428534616));
#116122=CARTESIAN_POINT('Ctrl Pts',(-8.89266646142556,77.1272141676282,
61.1789320480973));
#116123=CARTESIAN_POINT('Ctrl Pts',(-8.89583278444763,77.1444393994645,
61.1820611305557));
#116124=CARTESIAN_POINT('Ctrl Pts',(-8.89688822545498,77.1501811434099,
61.1831041580418));
#116125=CARTESIAN_POINT('Ctrl Pts',(-8.89817253250436,77.1571368374197,
61.1843738562206));
#116126=CARTESIAN_POINT('Ctrl Pts',(-8.89901150431184,77.1616664547679,
61.1852035135444));
#116127=CARTESIAN_POINT('Ctrl Pts',(-8.92259264299848,77.2889812631243,
61.208522848285));
#116128=CARTESIAN_POINT('Ctrl Pts',(-8.94869408539285,77.4192468165972,
61.2345070151699));
#116129=CARTESIAN_POINT('Ctrl Pts',(-8.97731850656541,77.5523261726857,
61.2634710633927));
#116130=CARTESIAN_POINT('Ctrl Pts',(-8.98128295423502,77.5707575023513,
61.2674825489975));
#116131=CARTESIAN_POINT('Ctrl Pts',(-8.98529573764546,77.5892427551795,
61.2715512181843));
#116132=CARTESIAN_POINT('Ctrl Pts',(-8.98935680388911,77.6077815160241,
61.2756779307514));
#116133=CARTESIAN_POINT('Ctrl Pts',(-9.00017439012048,77.6571637797025,
61.2866703811001));
#116134=CARTESIAN_POINT('Ctrl Pts',(-9.01133389180735,77.7069265004623,
61.2980748268113));
#116135=CARTESIAN_POINT('Ctrl Pts',(-9.02283815665349,77.7570601265521,
61.309907433083));
#116136=CARTESIAN_POINT('Ctrl Pts',(-9.02908498811848,77.7842827537343,
61.3163325543888));
#116137=CARTESIAN_POINT('Ctrl Pts',(-9.03543346584944,77.8116147226887,
61.3228839209108));
#116138=CARTESIAN_POINT('Ctrl Pts',(-9.04188245493954,77.8390552997318,
61.3295643639931));
#116139=CARTESIAN_POINT('Ctrl Pts',(-9.05104523026728,77.878043091275,61.3390559910058));
#116140=CARTESIAN_POINT('Ctrl Pts',(-9.06041225574227,77.9172494421727,
61.3488080181036));
#116141=CARTESIAN_POINT('Ctrl Pts',(-9.06998353136695,77.9566702598686,
61.3588281350206));
#116142=CARTESIAN_POINT('Ctrl Pts',(-9.07476916917929,77.9763806687166,
61.3638381934791));
#116143=CARTESIAN_POINT('Ctrl Pts',(-9.07960586952718,77.9961446939862,
61.3689152751757));
#116144=CARTESIAN_POINT('Ctrl Pts',(-9.08449363240003,78.0159618136268,
61.3740603435686));
#116145=CARTESIAN_POINT('Ctrl Pts',(-9.08693751383645,78.0258703734471,
61.376632877765));
#116146=CARTESIAN_POINT('Ctrl Pts',(-9.08939416090401,78.0357922068428,
61.3792224086809));
#116147=CARTESIAN_POINT('Ctrl Pts',(-9.09186357360078,78.0457272474666,
61.3818290567522));
#116148=CARTESIAN_POINT('Ctrl Pts',(-9.09309827994918,78.0506947677785,
61.3831323807878));
#116149=CARTESIAN_POINT('Ctrl Pts',(-9.09433617770486,78.0556655898965,
61.3844399841149));
#116150=CARTESIAN_POINT('Ctrl Pts',(-9.09557726686759,78.060639705455,61.3857518817859));
#116151=CARTESIAN_POINT('Ctrl Pts',(-9.09681835603032,78.0656138210136,
61.387063779457));
#116152=CARTESIAN_POINT('Ctrl Pts',(-9.09837266160549,78.0718290451585,
61.3887081459466));
#116153=CARTESIAN_POINT('Ctrl Pts',(-9.09931010857661,78.0755719240635,
61.3897004728883));
#116154=CARTESIAN_POINT('Ctrl Pts',(-9.11922887776139,78.1551001995736,
61.4107853255961));
#116155=CARTESIAN_POINT('Ctrl Pts',(-9.1407460830329,78.2384488549837,61.4337575836913));
#116156=CARTESIAN_POINT('Ctrl Pts',(-9.16387330016365,78.3255241006586,
61.4588727406335));
#116157=CARTESIAN_POINT('Ctrl Pts',(-9.17557641127034,78.3695869582439,
61.4715818128273));
#116158=CARTESIAN_POINT('Ctrl Pts',(-9.18769115678514,78.4146039068995,
61.4848399730603));
#116159=CARTESIAN_POINT('Ctrl Pts',(-9.20021442302084,78.4605617067419,
61.4986824948998));
#116160=CARTESIAN_POINT('Ctrl Pts',(-9.21885004348183,78.5289505838102,
61.5192812730754));
#116161=CARTESIAN_POINT('Ctrl Pts',(-9.2383947815182,78.5994224592807,61.541173598283));
#116162=CARTESIAN_POINT('Ctrl Pts',(-9.25884863686747,78.6719265687999,
61.5644800667747));
#116163=CARTESIAN_POINT('Ctrl Pts',(-9.2690755645421,78.7081786235595,61.5761333010206));
#116164=CARTESIAN_POINT('Ctrl Pts',(-9.27952977153974,78.7449387014591,
61.5881401814723));
#116165=CARTESIAN_POINT('Ctrl Pts',(-9.29021125784852,78.7821997258525,
61.6005162513103));
#116166=CARTESIAN_POINT('Ctrl Pts',(-9.29555200100291,78.8008302380492,
61.6067042862293));
#116167=CARTESIAN_POINT('Ctrl Pts',(-9.30094956398611,78.8195859849683,
61.6129846249781));
#116168=CARTESIAN_POINT('Ctrl Pts',(-9.30640394680137,78.8384660515663,
61.6193592424304));
#116169=CARTESIAN_POINT('Ctrl Pts',(-9.309131138209,78.8479060848653,61.6225465511565));
#116170=CARTESIAN_POINT('Ctrl Pts',(-9.31187253457468,78.8573771979606,
61.625757429952));
#116171=CARTESIAN_POINT('Ctrl Pts',(-9.31462813589891,78.8668792738138,
61.6289921273608));
#116172=CARTESIAN_POINT('Ctrl Pts',(-9.31600593656103,78.8716303117403,
61.6306094760651));
#116173=CARTESIAN_POINT('Ctrl Pts',(-9.31738728846278,78.8763890903488,
61.632232779447));
#116174=CARTESIAN_POINT('Ctrl Pts',(-9.31877219160423,78.8811555948331,
61.6338620686736));
#116175=CARTESIAN_POINT('Ctrl Pts',(-9.32015709474568,78.8859220993175,
61.6354913579001));
#116176=CARTESIAN_POINT('Ctrl Pts',(-9.32207911460549,78.8925292812147,
61.6377557517266));
#116177=CARTESIAN_POINT('Ctrl Pts',(-9.32293755474769,78.8954782710375,
61.6387679251359));
#116178=CARTESIAN_POINT('Ctrl Pts',(-9.32540791029129,78.9039646558167,
61.6416806829042));
#116179=CARTESIAN_POINT('Ctrl Pts',(-9.32791655809782,78.9125679742487,
61.6446441886323));
#116180=CARTESIAN_POINT('Ctrl Pts',(-9.33046352415257,78.9212879068898,
61.6476592438058));
#116181=CARTESIAN_POINT('Ctrl Pts',(-9.34717122788578,78.9784893175131,
61.667437539823));
#116182=CARTESIAN_POINT('Ctrl Pts',(-9.3655294968389,79.0407103562356,61.6894307270498));
#116183=CARTESIAN_POINT('Ctrl Pts',(-9.38554373915658,79.1078507385285,
61.7138910349835));
#116184=CARTESIAN_POINT('Ctrl Pts',(-9.39640552175165,79.1442880027646,
61.7271657092263));
#116185=CARTESIAN_POINT('Ctrl Pts',(-9.40775469220893,79.1821738158082,
61.7411677299387));
#116186=CARTESIAN_POINT('Ctrl Pts',(-9.41958877910638,79.2214898186444,
61.7559424868357));
#116187=CARTESIAN_POINT('Ctrl Pts',(-9.43807081163282,79.2828920754915,
61.7790171473404));
#116188=CARTESIAN_POINT('Ctrl Pts',(-9.45773959183724,79.3477825665806,
61.8039753638204));
#116189=CARTESIAN_POINT('Ctrl Pts',(-9.47859511967813,79.4160775816128,
61.8310049113892));
#116190=CARTESIAN_POINT('Ctrl Pts',(-9.48902288359857,79.4502250891288,
61.8445196851735));
#116191=CARTESIAN_POINT('Ctrl Pts',(-9.49974733441796,79.4852234981225,
61.8585525848617));
#116192=CARTESIAN_POINT('Ctrl Pts',(-9.51076847209598,79.5210608981225,
61.8731287732406));
#116193=CARTESIAN_POINT('Ctrl Pts',(-9.51627904093499,79.5389795981225,
61.8804168674301));
#116194=CARTESIAN_POINT('Ctrl Pts',(-9.52186378148761,79.5571080376222,
61.8878408038733));
#116195=CARTESIAN_POINT('Ctrl Pts',(-9.52752269375218,79.5754446213074,
61.8954038234184));
#116196=CARTESIAN_POINT('Ctrl Pts',(-9.53250202705314,79.591579164043,61.9020585996927));
#116197=CARTESIAN_POINT('Ctrl Pts',(-9.53722776857092,79.6068699851859,
61.9084020592662));
#116198=CARTESIAN_POINT('Ctrl Pts',(-9.54252091927987,79.6239686624488,
61.915542315475));
#116199=CARTESIAN_POINT('Ctrl Pts',(-9.54324332801525,79.6263022883924,
61.9165168170038));
#116200=CARTESIAN_POINT('Ctrl Pts',(-9.543976307386,79.6286695552575,61.9175062316699));
#116201=CARTESIAN_POINT('Ctrl Pts',(-9.54472194568067,79.631077170464,61.9185134474129));
#116202=CARTESIAN_POINT('Ctrl Pts',(-9.5668688246071,79.7025879322633,61.9484296752574));
#116203=CARTESIAN_POINT('Ctrl Pts',(-9.58752489475418,79.7690234373903,
61.9770336810328));
#116204=CARTESIAN_POINT('Ctrl Pts',(-9.60667184392161,79.8304899452595,
62.0040640470899));
#116205=CARTESIAN_POINT('Ctrl Pts',(-9.61673055756171,79.8627809382373,
62.0182642577541));
#116206=CARTESIAN_POINT('Ctrl Pts',(-9.62637339967271,79.8937002699575,
62.0320307794531));
#116207=CARTESIAN_POINT('Ctrl Pts',(-9.63560119149857,79.9232614284828,
62.0453297721826));
#116208=CARTESIAN_POINT('Ctrl Pts',(-9.64820426117206,79.963635263042,62.0634931784579));
#116209=CARTESIAN_POINT('Ctrl Pts',(-9.66003293470919,80.0014757893863,
62.0807841343321));
#116210=CARTESIAN_POINT('Ctrl Pts',(-9.67109405079398,80.0368130179988,
62.0971251414243));
#116211=CARTESIAN_POINT('Ctrl Pts',(-9.68740373782591,80.0889179895793,
62.1212200618118));
#116212=CARTESIAN_POINT('Ctrl Pts',(-9.70203412279025,80.1355847671629,
62.1432491475576));
#116213=CARTESIAN_POINT('Ctrl Pts',(-9.71498478797446,80.1769050203069,
62.1630077286355));
#116214=CARTESIAN_POINT('Ctrl Pts',(-9.71576166184407,80.1793837057255,
62.1641929901739));
#116215=CARTESIAN_POINT('Ctrl Pts',(-9.71653249553801,80.1818431456697,
62.1653700949537));
#116216=CARTESIAN_POINT('Ctrl Pts',(-9.71729729042005,80.1842833575417,
62.16653900399));
#116217=CARTESIAN_POINT('Ctrl Pts',(-9.72405434070977,80.2058429086365,
62.1768664490702));
#116218=CARTESIAN_POINT('Ctrl Pts',(-9.73033964617562,80.2259017641078,
62.1865538905201));
#116219=CARTESIAN_POINT('Ctrl Pts',(-9.7361532068364,80.2444714445637,62.1955766594361));
#116220=CARTESIAN_POINT('Ctrl Pts',(-9.73905998716679,80.2537562847916,
62.2000880438941));
#116221=CARTESIAN_POINT('Ctrl Pts',(-9.74184883129493,80.2626688041486,
62.2044333159049));
#116222=CARTESIAN_POINT('Ctrl Pts',(-9.74451973922586,80.2712103088226,
62.2086097405811));
#116223=CARTESIAN_POINT('Ctrl Pts',(-9.74585519319132,80.2754810611597,
62.2106979529192));
#116224=CARTESIAN_POINT('Ctrl Pts',(-9.74716116310733,80.2796590581362,
62.2127439569184));
#116225=CARTESIAN_POINT('Ctrl Pts',(-9.74843764897426,80.283744453113,62.2147474318027));
#116226=CARTESIAN_POINT('Ctrl Pts',(-9.74907589190773,80.2857871506015,
62.2157491692448));
#116227=CARTESIAN_POINT('Ctrl Pts',(-9.74970676382892,80.287806697483,62.2167402746261));
#116228=CARTESIAN_POINT('Ctrl Pts',(-9.75033026473789,80.2898031123722,
62.2177207091992));
#116229=CARTESIAN_POINT('Ctrl Pts',(-9.75095376564686,80.2917995272614,
62.2187011437723));
#116230=CARTESIAN_POINT('Ctrl Pts',(-9.7510833222648,80.2922140646321,62.2189043469225));
#116231=CARTESIAN_POINT('Ctrl Pts',(-9.75217865442817,80.2957229792706,
62.2206299626292));
#116232=CARTESIAN_POINT('Ctrl Pts',(-9.78387650612535,80.3972675696231,
62.270567609481));
#116233=CARTESIAN_POINT('Ctrl Pts',(-9.81432835451053,80.4952254170197,
62.3205249514219));
#116234=CARTESIAN_POINT('Ctrl Pts',(-9.8434407469923,80.5896997430749,62.3702581386498));
#116235=CARTESIAN_POINT('Ctrl Pts',(-9.8650914418614,80.6599596781753,62.407244382986));
#116236=CARTESIAN_POINT('Ctrl Pts',(-9.88600253165974,80.7282928637747,
62.44410692794));
#116237=CARTESIAN_POINT('Ctrl Pts',(-9.90615340852189,80.794740148219,62.4807503211802));
#116238=CARTESIAN_POINT('Ctrl Pts',(-9.93782589210618,80.8991797981746,
62.5383451980092));
#116239=CARTESIAN_POINT('Ctrl Pts',(-9.96761929950232,80.9989601739828,
62.5953972789563));
#116240=CARTESIAN_POINT('Ctrl Pts',(-9.99557073594596,81.0942161190798,
62.6515538909901));
#116241=CARTESIAN_POINT('Ctrl Pts',(-10.0249108575926,81.1942045766444,
62.7105004797159));
#116242=CARTESIAN_POINT('Ctrl Pts',(-10.0522219028098,81.2892080666935,
62.76846016398));
#116243=CARTESIAN_POINT('Ctrl Pts',(-10.0775940451767,81.3793801999264,
62.8250569690241));
#116244=CARTESIAN_POINT('Ctrl Pts',(-10.0834563564733,81.4002147478192,
62.8381338343814));
#116245=CARTESIAN_POINT('Ctrl Pts',(-10.0892153309249,81.4207913544346,
62.8511380792578));
#116246=CARTESIAN_POINT('Ctrl Pts',(-10.0948723726601,81.4411118802155,
62.8640653139415));
#116247=CARTESIAN_POINT('',(-10.7325524156118,83.7450179064977,64.7715505688173));
#116248=CARTESIAN_POINT('Ctrl Pts',(-10.0948723726639,81.4411122211604,
62.8640647780043));
#116249=CARTESIAN_POINT('Ctrl Pts',(-10.1238158396739,81.5451332595941,
62.9302398682223));
#116250=CARTESIAN_POINT('Ctrl Pts',(-10.1526418118159,81.6482221786327,
62.9980739436566));
#116251=CARTESIAN_POINT('Ctrl Pts',(-10.1812698397242,81.7503263490054,
63.0675440049332));
#116252=CARTESIAN_POINT('Ctrl Pts',(-10.2098978676326,81.8524305193781,
63.1370140662099));
#116253=CARTESIAN_POINT('Ctrl Pts',(-10.2383279513072,81.9535503248741,
63.2081195517163));
#116254=CARTESIAN_POINT('Ctrl Pts',(-10.2664843011526,82.0536858471839,
63.2808764091866));
#116255=CARTESIAN_POINT('Ctrl Pts',(-10.2946406509979,82.1538213694936,
63.353633266657));
#116256=CARTESIAN_POINT('Ctrl Pts',(-10.3225232670139,82.252972511183,63.4280416176109));
#116257=CARTESIAN_POINT('Ctrl Pts',(-10.3500718066949,82.3511229877178,
63.5041125932418));
#116258=CARTESIAN_POINT('Ctrl Pts',(-10.3776203463759,82.4492734642527,
63.5801835688728));
#116259=CARTESIAN_POINT('Ctrl Pts',(-10.4048348097219,82.5464232578521,
63.6579171984223));
#116260=CARTESIAN_POINT('Ctrl Pts',(-10.4316631941731,82.6425496669633,
63.7373254870007));
#116261=CARTESIAN_POINT('Ctrl Pts',(-10.4584915786242,82.7386760760745,
63.8167337755791));
#116262=CARTESIAN_POINT('Ctrl Pts',(-10.4849338841806,82.8337791084527,
63.8978167095015));
#116263=CARTESIAN_POINT('Ctrl Pts',(-10.5109460339877,82.9278331310342,
63.9805897775263));
#116264=CARTESIAN_POINT('Ctrl Pts',(-10.5369581837949,83.0218871536157,
64.0633628455512));
#116265=CARTESIAN_POINT('Ctrl Pts',(-10.5625401778529,83.1148920931469,
64.1478261377776));
#116266=CARTESIAN_POINT('Ctrl Pts',(-10.5876554908367,83.2068100073309,
64.2339896439459));
#116267=CARTESIAN_POINT('Ctrl Pts',(-10.6127708038206,83.2987279215148,
64.3201531501143));
#116268=CARTESIAN_POINT('Ctrl Pts',(-10.6374194357302,83.3895589867901,
64.408016670944));
#116269=CARTESIAN_POINT('Ctrl Pts',(-10.6615778397041,83.4792788066254,
64.4976096880002));
#116270=CARTESIAN_POINT('Ctrl Pts',(-10.6857362436779,83.5689986264608,
64.5872027050565));
#116271=CARTESIAN_POINT('Ctrl Pts',(-10.7094044197159,83.6576065909718,
64.678525829176));
#116272=CARTESIAN_POINT('Ctrl Pts',(-10.7325524156119,83.745018045238,64.7715504384495));
#116273=CARTESIAN_POINT('',(-10.7325548086171,83.7450176039532,81.2062285734056));
#116274=CARTESIAN_POINT('Ctrl Pts',(-10.7325524156115,83.7450176952948,
64.7715507672746));
#116275=CARTESIAN_POINT('Ctrl Pts',(-10.7501562547286,83.8114962912959,
64.8422991787488));
#116276=CARTESIAN_POINT('Ctrl Pts',(-10.7667240350834,83.8787704405261,
64.9156125289802));
#116277=CARTESIAN_POINT('Ctrl Pts',(-10.7822782455101,83.9466666344631,
64.9915677571402));
#116278=CARTESIAN_POINT('Ctrl Pts',(-10.7837981649509,83.9533012846502,
64.9989899164616));
#116279=CARTESIAN_POINT('Ctrl Pts',(-10.7853084365357,83.9599418483979,
65.0064372924184));
#116280=CARTESIAN_POINT('Ctrl Pts',(-10.7868091014514,83.9665881465513,
65.013909950191));
#116281=CARTESIAN_POINT('Ctrl Pts',(-10.8032614660996,84.0394540606112,
65.0958355614857));
#116282=CARTESIAN_POINT('Ctrl Pts',(-10.8185561237797,84.1130118947079,
65.1808006373549));
#116283=CARTESIAN_POINT('Ctrl Pts',(-10.832689957148,84.1870643803022,65.2689256223875));
#116284=CARTESIAN_POINT('Ctrl Pts',(-10.8388533377215,84.2193566565192,
65.3073545331184));
#116285=CARTESIAN_POINT('Ctrl Pts',(-10.8447964533634,84.2517425768332,
65.3463842196399));
#116286=CARTESIAN_POINT('Ctrl Pts',(-10.8505214018681,84.2842037635522,
65.3860241055826));
#116287=CARTESIAN_POINT('Ctrl Pts',(-10.8640271490599,84.3607830692007,
65.4795387071206));
#116288=CARTESIAN_POINT('Ctrl Pts',(-10.8763166551811,84.4377836100341,
65.5764500611726));
#116289=CARTESIAN_POINT('Ctrl Pts',(-10.8873758646346,84.5149629273589,
65.6768811296746));
#116290=CARTESIAN_POINT('Ctrl Pts',(-10.8922499094149,84.5489776053826,
65.7211433825304));
#116291=CARTESIAN_POINT('Ctrl Pts',(-10.8968854238649,84.5830265448267,
65.7660891430358));
#116292=CARTESIAN_POINT('Ctrl Pts',(-10.9012834140875,84.617086714057,65.8117281677846));
#116293=CARTESIAN_POINT('Ctrl Pts',(-10.9116143286586,84.6970943268044,
65.9189346057086));
#116294=CARTESIAN_POINT('Ctrl Pts',(-10.920632708015,84.77716637353,66.0299671776509));
#116295=CARTESIAN_POINT('Ctrl Pts',(-10.9283128382425,84.8570095906465,
66.1449612477235));
#116296=CARTESIAN_POINT('Ctrl Pts',(-10.9306986035121,84.8818121875772,
66.1806831496261));
#116297=CARTESIAN_POINT('Ctrl Pts',(-10.9329554612622,84.9065924256239,
66.2167872334362));
#116298=CARTESIAN_POINT('Ctrl Pts',(-10.9350832924956,84.9313407463341,
66.2532772859761));
#116299=CARTESIAN_POINT('Ctrl Pts',(-10.9358584453185,84.9403563723677,
66.2665703360984));
#116300=CARTESIAN_POINT('Ctrl Pts',(-10.9366167445909,84.9493676639085,
66.2799144663096));
#116301=CARTESIAN_POINT('Ctrl Pts',(-10.9373582249864,84.9583741277226,
66.2933098234466));
#116302=CARTESIAN_POINT('Ctrl Pts',(-10.9440570613183,85.0397421954264,
66.4143289435964));
#116303=CARTESIAN_POINT('Ctrl Pts',(-10.9493806507756,85.1207191934572,
66.5395306431455));
#116304=CARTESIAN_POINT('Ctrl Pts',(-10.9533178722974,85.200945015527,66.6690229320925));
#116305=CARTESIAN_POINT('Ctrl Pts',(-10.95495748534,85.2343541857984,66.7229485861856));
#116306=CARTESIAN_POINT('Ctrl Pts',(-10.956357038406,85.2676326509186,66.7776181129226));
#116307=CARTESIAN_POINT('Ctrl Pts',(-10.9575173777474,85.3007524839038,
66.8330383629357));
#116308=CARTESIAN_POINT('Ctrl Pts',(-10.9600931298752,85.3742727699435,
66.9560617077453));
#116309=CARTESIAN_POINT('Ctrl Pts',(-10.9614887331737,85.4470130418676,
67.0827853050045));
#116310=CARTESIAN_POINT('Ctrl Pts',(-10.9617079988126,85.5186654928951,
67.2132797997646));
#116311=CARTESIAN_POINT('Ctrl Pts',(-10.9618285298819,85.5580530895288,
67.2850130684641));
#116312=CARTESIAN_POINT('Ctrl Pts',(-10.9615938364338,85.5971114297609,
67.357885402198));
#116313=CARTESIAN_POINT('Ctrl Pts',(-10.9610019761566,85.6357852055068,
67.4319049822405));
#116314=CARTESIAN_POINT('Ctrl Pts',(-10.960166156352,85.6903999666699,67.5364347729694));
#116315=CARTESIAN_POINT('Ctrl Pts',(-10.9586176011902,85.7442481188906,
67.6432527692208));
#116316=CARTESIAN_POINT('Ctrl Pts',(-10.9563601692076,85.7971735499566,
67.7523800120814));
#116317=CARTESIAN_POINT('Ctrl Pts',(-10.9544321874464,85.8423750295958,
67.8455811962171));
#116318=CARTESIAN_POINT('Ctrl Pts',(-10.9519858673571,85.886903029062,67.9404660981445));
#116319=CARTESIAN_POINT('Ctrl Pts',(-10.9490212087671,85.930654905422,68.0370430779914));
#116320=CARTESIAN_POINT('Ctrl Pts',(-10.9485794522018,85.937174266096,68.0514337788437));
#116321=CARTESIAN_POINT('Ctrl Pts',(-10.9481262039085,85.9436763919122,
68.0658620559854));
#116322=CARTESIAN_POINT('Ctrl Pts',(-10.9476614373451,85.9501609285741,
68.080327917286));
#116323=CARTESIAN_POINT('Ctrl Pts',(-10.9465666637759,85.9654354769264,
68.1144027493692));
#116324=CARTESIAN_POINT('Ctrl Pts',(-10.9454079726398,85.9806124352409,
68.1486861231865));
#116325=CARTESIAN_POINT('Ctrl Pts',(-10.9441854670397,85.9956873076151,
68.1831782342848));
#116326=CARTESIAN_POINT('Ctrl Pts',(-10.9433147177819,86.0064246276983,
68.2077457946603));
#116327=CARTESIAN_POINT('Ctrl Pts',(-10.9424115723738,86.0171101545612,
68.2324192477099));
#116328=CARTESIAN_POINT('Ctrl Pts',(-10.941476030815,86.0277422448405,68.2571986441174));
#116329=CARTESIAN_POINT('Ctrl Pts',(-10.9410082600356,86.0330582899801,
68.2695883423211));
#116330=CARTESIAN_POINT('Ctrl Pts',(-10.9405323902186,86.0383609758636,
68.2820045264164));
#116331=CARTESIAN_POINT('Ctrl Pts',(-10.9400484213637,86.043650095586,68.2944472011266));
#116332=CARTESIAN_POINT('Ctrl Pts',(-10.9396261812646,86.0482646041711,
68.3053028505135));
#116333=CARTESIAN_POINT('Ctrl Pts',(-10.9391360171996,86.053523683442,68.317730587338));
#116334=CARTESIAN_POINT('Ctrl Pts',(-10.9387395065561,86.0577128820342,
68.3276685659382));
#116335=CARTESIAN_POINT('Ctrl Pts',(-10.9386815392793,86.0583253156173,
68.3291214337621));
#116336=CARTESIAN_POINT('Ctrl Pts',(-10.9386255999408,86.0589149648276,
68.3305210536576));
#116337=CARTESIAN_POINT('Ctrl Pts',(-10.9385722176855,86.059476548673,68.3318547014369));
#116338=CARTESIAN_POINT('Ctrl Pts',(-10.9349831434126,86.0972337794337,
68.4215204697137));
#116339=CARTESIAN_POINT('Ctrl Pts',(-10.9308041525169,86.1359710144443,
68.5165530785467));
#116340=CARTESIAN_POINT('Ctrl Pts',(-10.926022556049,86.1752952890009,68.6170738907957));
#116341=CARTESIAN_POINT('Ctrl Pts',(-10.9237789724588,86.1937467199572,
68.6642394862912));
#116342=CARTESIAN_POINT('Ctrl Pts',(-10.9214030150662,86.2123267369797,
68.7126133546548));
#116343=CARTESIAN_POINT('Ctrl Pts',(-10.9188952104483,86.230991194323,68.7622078211464));
#116344=CARTESIAN_POINT('Ctrl Pts',(-10.9167755798745,86.2467666475405,
68.8041257388006));
#116345=CARTESIAN_POINT('Ctrl Pts',(-10.91456175562,86.2626023824771,68.846915631229));
#116346=CARTESIAN_POINT('Ctrl Pts',(-10.9122560350931,86.2784706480888,
68.8905849692834));
#116347=CARTESIAN_POINT('Ctrl Pts',(-10.9068322158739,86.315798070468,68.993309732435));
#116348=CARTESIAN_POINT('Ctrl Pts',(-10.9008895022725,86.3533075084191,
69.100900201655));
#116349=CARTESIAN_POINT('Ctrl Pts',(-10.8944278943129,86.3906100147042,
69.2134425579111));
#116350=CARTESIAN_POINT('Ctrl Pts',(-10.8911970903331,86.4092612678467,
69.2697137360391));
#116351=CARTESIAN_POINT('Ctrl Pts',(-10.8878365627587,86.4278602099881,
69.327222722184));
#116352=CARTESIAN_POINT('Ctrl Pts',(-10.8843463115825,86.446354708905,69.3859790953269));
#116353=CARTESIAN_POINT('Ctrl Pts',(-10.8828959388797,86.4540400917119,
69.410395286432));
#116354=CARTESIAN_POINT('Ctrl Pts',(-10.8814231734589,86.4617074161907,
69.4350268841941));
#116355=CARTESIAN_POINT('Ctrl Pts',(-10.8799279934186,86.4693528151707,
69.4598745093374));
#116356=CARTESIAN_POINT('Ctrl Pts',(-10.8796241345346,86.4709065560845,
69.4649241832518));
#116357=CARTESIAN_POINT('Ctrl Pts',(-10.8793193502041,86.4724593912341,
69.4699827791575));
#116358=CARTESIAN_POINT('Ctrl Pts',(-10.8790136421172,86.4740112879634,
69.4750503022557));
#116359=CARTESIAN_POINT('Ctrl Pts',(-10.8781086484231,86.4786053985345,
69.4900517910762));
#116360=CARTESIAN_POINT('Ctrl Pts',(-10.8771955470043,86.483191286066,69.5051315140166));
#116361=CARTESIAN_POINT('Ctrl Pts',(-10.8762743378606,86.4877680971712,
69.5202896029158));
#116362=CARTESIAN_POINT('Ctrl Pts',(-10.8758137332888,86.4900565027238,
69.5278686473654));
#116363=CARTESIAN_POINT('Ctrl Pts',(-10.8753511017858,86.4923426390575,
69.5354672833387));
#116364=CARTESIAN_POINT('Ctrl Pts',(-10.8748864433516,86.4946263986312,
69.5430855268734));
#116365=CARTESIAN_POINT('Ctrl Pts',(-10.8744217849174,86.4969101582049,
69.550703770408));
#116366=CARTESIAN_POINT('Ctrl Pts',(-10.8738819795741,86.4995470533043,
69.5595362016483));
#116367=CARTESIAN_POINT('Ctrl Pts',(-10.8734863872555,86.5014704390232,
69.5659990961329));
#116368=CARTESIAN_POINT('Ctrl Pts',(-10.861496809166,86.5597642485571,69.7618759483011));
#116369=CARTESIAN_POINT('Ctrl Pts',(-10.8494413886398,86.6130533604805,
69.9592421054953));
#116370=CARTESIAN_POINT('Ctrl Pts',(-10.8373200119521,86.6612678630307,
70.1578404613565));
#116371=CARTESIAN_POINT('Ctrl Pts',(-10.8366432775534,86.663959670507,70.1689281737838));
#116372=CARTESIAN_POINT('Ctrl Pts',(-10.8359663362774,86.6666356621964,
70.1800197255885));
#116373=CARTESIAN_POINT('Ctrl Pts',(-10.8352891930952,86.6692958268583,
70.19111506744));
#116374=CARTESIAN_POINT('Ctrl Pts',(-10.8288862721828,86.6944497741948,
70.2960302437859));
#116375=CARTESIAN_POINT('Ctrl Pts',(-10.8224649904436,86.718188651506,70.4012846876382));
#116376=CARTESIAN_POINT('Ctrl Pts',(-10.8160253477116,86.7405039769241,
70.5068400814735));
#116377=CARTESIAN_POINT('Ctrl Pts',(-10.8126527026787,86.7521912202326,
70.5621227872892));
#116378=CARTESIAN_POINT('Ctrl Pts',(-10.8092384943889,86.7636043511571,
70.6180593279552));
#116379=CARTESIAN_POINT('Ctrl Pts',(-10.8058408027958,86.7745539441851,
70.6737478244563));
#116380=CARTESIAN_POINT('Ctrl Pts',(-10.8027510283912,86.7845112258722,
70.7243895282146));
#116381=CARTESIAN_POINT('Ctrl Pts',(-10.799675022111,86.7940858244824,70.7748258842997));
#116382=CARTESIAN_POINT('Ctrl Pts',(-10.7966513366151,86.8031715694856,
70.8243706394832));
#116383=CARTESIAN_POINT('Ctrl Pts',(-10.795628375841,86.8062454211655,70.8411324161896));
#116384=CARTESIAN_POINT('Ctrl Pts',(-10.7946164566296,86.8092803959527,
70.857883432425));
#116385=CARTESIAN_POINT('Ctrl Pts',(-10.7936156928137,86.8122766857533,
70.8746235236739));
#116386=CARTESIAN_POINT('Ctrl Pts',(-10.7832031496532,86.8434518705211,
71.0487974095269));
#116387=CARTESIAN_POINT('Ctrl Pts',(-10.7740019632466,86.8704392100341,
71.2217865823219));
#116388=CARTESIAN_POINT('Ctrl Pts',(-10.766068932557,86.8934600952167,71.3933899853205));
#116389=CARTESIAN_POINT('Ctrl Pts',(-10.7630545361072,86.9022075811753,
71.4585959209859));
#116390=CARTESIAN_POINT('Ctrl Pts',(-10.7602227798109,86.9103823632979,
71.5236020369678));
#116391=CARTESIAN_POINT('Ctrl Pts',(-10.7575751102966,86.9179965202485,
71.5883983800714));
#116392=CARTESIAN_POINT('Ctrl Pts',(-10.7512353234622,86.9362284527947,
71.7435518086617));
#116393=CARTESIAN_POINT('Ctrl Pts',(-10.7459521425721,86.9512463597118,
71.8975006171607));
#116394=CARTESIAN_POINT('Ctrl Pts',(-10.7416545618065,86.9632218800474,
72.0501051761386));
#116395=CARTESIAN_POINT('Ctrl Pts',(-10.7396275911568,86.9688701806982,
72.1220817087337));
#116396=CARTESIAN_POINT('Ctrl Pts',(-10.7378248801488,86.9738416376222,
72.193759898553));
#116397=CARTESIAN_POINT('Ctrl Pts',(-10.7362536744843,86.9781538748905,
72.2651275589387));
#116398=CARTESIAN_POINT('Ctrl Pts',(-10.7334570248527,86.9858293925143,
72.3921576134045));
#116399=CARTESIAN_POINT('Ctrl Pts',(-10.731393790858,86.9914166271671,72.518203273173));
#116400=CARTESIAN_POINT('Ctrl Pts',(-10.7300469114455,86.9950190418003,
72.643195786795));
#116401=CARTESIAN_POINT('Ctrl Pts',(-10.7290772139338,86.9976126314517,
72.7331852307752));
#116402=CARTESIAN_POINT('Ctrl Pts',(-10.7284825825092,86.9991773308193,
72.822629261593));
#116403=CARTESIAN_POINT('Ctrl Pts',(-10.7282633821769,86.9997504820953,
72.9115048423941));
#116404=CARTESIAN_POINT('Ctrl Pts',(-10.7282448252273,86.999799003643,72.9190288258855));
#116405=CARTESIAN_POINT('Ctrl Pts',(-10.7282289586258,86.9998404182714,
72.9265487366744));
#116406=CARTESIAN_POINT('Ctrl Pts',(-10.7282157704445,86.9998747499382,
72.9340645613803));
#116407=CARTESIAN_POINT('Ctrl Pts',(-10.7281312849499,87.0000946838152,
72.9822120771066));
#116408=CARTESIAN_POINT('Ctrl Pts',(-10.7281571517953,87.0000239499403,
73.0301918431451));
#116409=CARTESIAN_POINT('Ctrl Pts',(-10.728293370978,86.9996687874899,73.0780004629468));
#116410=CARTESIAN_POINT('Ctrl Pts',(-10.7283614805694,86.9994912062647,
73.1019047728476));
#116411=CARTESIAN_POINT('Ctrl Pts',(-10.7284571782452,86.9992425162455,
73.1257662963088));
#116412=CARTESIAN_POINT('Ctrl Pts',(-10.7285804640057,86.9989234877188,
73.1495846162313));
#116413=CARTESIAN_POINT('Ctrl Pts',(-10.728642106886,86.9987639734554,73.1614937761926));
#116414=CARTESIAN_POINT('Ctrl Pts',(-10.7287106467875,86.9985868744688,
73.1733921352721));
#116415=CARTESIAN_POINT('Ctrl Pts',(-10.7287860837103,86.9983922864601,
73.1852796422712));
#116416=CARTESIAN_POINT('Ctrl Pts',(-10.7288545066269,86.9982157909377,
73.1960618676091));
#116417=CARTESIAN_POINT('Ctrl Pts',(-10.7289413385066,86.9979921653486,
73.2085723766105));
#116418=CARTESIAN_POINT('Ctrl Pts',(-10.7290119709596,86.9978104599079,
73.2180840633153));
#116419=CARTESIAN_POINT('Ctrl Pts',(-10.7290192114644,86.997791833355,73.219059102563));
#116420=CARTESIAN_POINT('Ctrl Pts',(-10.7290262654236,86.9977736896406,
73.2200026305993));
#116421=CARTESIAN_POINT('Ctrl Pts',(-10.7290330855424,86.9977561506881,
73.2209095561051));
#116422=CARTESIAN_POINT('Ctrl Pts',(-10.7298120572208,86.9957529088541,
73.3244956231166));
#116423=CARTESIAN_POINT('Ctrl Pts',(-10.7312749998046,86.9923257875855,
73.4324657801859));
#116424=CARTESIAN_POINT('Ctrl Pts',(-10.7334586988057,86.9871180640138,
73.544768708703));
#116425=CARTESIAN_POINT('Ctrl Pts',(-10.7357270800446,86.9817083887606,
73.6614266620112));
#116426=CARTESIAN_POINT('Ctrl Pts',(-10.7387751755121,86.9743773859167,
73.7827603223291));
#116427=CARTESIAN_POINT('Ctrl Pts',(-10.7425955242636,86.9646968342411,
73.9086881881113));
#116428=CARTESIAN_POINT('Ctrl Pts',(-10.7453217724827,86.9577886725832,
73.998551873902));
#116429=CARTESIAN_POINT('Ctrl Pts',(-10.7484409799655,86.9496833232534,
74.0907545682361));
#116430=CARTESIAN_POINT('Ctrl Pts',(-10.7519438181274,86.9402147372432,
74.1852559325971));
#116431=CARTESIAN_POINT('Ctrl Pts',(-10.7530457951687,86.9372359629136,
74.2149856343677));
#116432=CARTESIAN_POINT('Ctrl Pts',(-10.7541856980251,86.9341222035809,
74.2449427618101));
#116433=CARTESIAN_POINT('Ctrl Pts',(-10.7553625082042,86.9308681814672,
74.2751259708024));
#116434=CARTESIAN_POINT('Ctrl Pts',(-10.7600481078438,86.9179119332007,
74.3953037494167));
#116435=CARTESIAN_POINT('Ctrl Pts',(-10.7653388979247,86.902733708385,74.519066681511));
#116436=CARTESIAN_POINT('Ctrl Pts',(-10.7712469033839,86.8849886449845,
74.6463126737205));
#116437=CARTESIAN_POINT('Ctrl Pts',(-10.7743570859573,86.8756470173687,
74.7132994546634));
#116438=CARTESIAN_POINT('Ctrl Pts',(-10.777637739596,86.8655937143387,74.7812510227291));
#116439=CARTESIAN_POINT('Ctrl Pts',(-10.7810863610267,86.8547763442664,
74.850148998758));
#116440=CARTESIAN_POINT('Ctrl Pts',(-10.7817163187627,86.8528003413629,
74.8627345532661));
#116441=CARTESIAN_POINT('Ctrl Pts',(-10.7823518727809,86.8507988391756,
74.8753516807464));
#116442=CARTESIAN_POINT('Ctrl Pts',(-10.7829929716454,86.8487715159117,
74.888000270938));
#116443=CARTESIAN_POINT('Ctrl Pts',(-10.7884017017479,86.831667688448,74.9947120658207));
#116444=CARTESIAN_POINT('Ctrl Pts',(-10.794212258259,86.8127265612355,75.103664440251));
#116445=CARTESIAN_POINT('Ctrl Pts',(-10.8004246409436,86.7917515545281,
75.2147801090942));
#116446=CARTESIAN_POINT('Ctrl Pts',(-10.8035308322859,86.7812640511744,
75.2703379435157));
#116447=CARTESIAN_POINT('Ctrl Pts',(-10.806737480238,86.7702679332875,75.3264365751154));
#116448=CARTESIAN_POINT('Ctrl Pts',(-10.8100445847874,86.7587380138097,
75.3830648877445));
#116449=CARTESIAN_POINT('Ctrl Pts',(-10.8116981370622,86.7529730540708,
75.411379044059));
#116450=CARTESIAN_POINT('Ctrl Pts',(-10.8133768034894,86.747074635108,75.4398256190323));
#116451=CARTESIAN_POINT('Ctrl Pts',(-10.8150805840696,86.7410395639213,
75.4684031694774));
#116452=CARTESIAN_POINT('Ctrl Pts',(-10.8159324743596,86.738022028328,75.4826919447));
#116453=CARTESIAN_POINT('Ctrl Pts',(-10.8167906431878,86.7349703291177,
75.4970134636656));
#116454=CARTESIAN_POINT('Ctrl Pts',(-10.8176550905538,86.7318840647869,
75.5113675406235));
#116455=CARTESIAN_POINT('Ctrl Pts',(-10.8179225350347,86.7309292300633,
75.515808434091));
#116456=CARTESIAN_POINT('Ctrl Pts',(-10.8181905804556,86.7299710868356,
75.5202524439623));
#116457=CARTESIAN_POINT('Ctrl Pts',(-10.8184592268714,86.7290096232093,
75.5246995645498));
#116458=CARTESIAN_POINT('Ctrl Pts',(-10.8186247466155,86.7284172415357,
75.527439546245));
#116459=CARTESIAN_POINT('Ctrl Pts',(-10.8187904945019,86.7278235994056,
75.530180708798));
#116460=CARTESIAN_POINT('Ctrl Pts',(-10.8189564705061,86.7272286940407,
75.5329230509585));
#116461=CARTESIAN_POINT('Ctrl Pts',(-10.8193918334579,86.7256682289784,
75.5401163448538));
#116462=CARTESIAN_POINT('Ctrl Pts',(-10.8196988436352,86.7245665827455,
75.545181674583));
#116463=CARTESIAN_POINT('Ctrl Pts',(-10.8202672682649,86.7225211743997,
75.5545272568814));
#116464=CARTESIAN_POINT('Ctrl Pts',(-10.8275417622956,86.6963447738284,
75.6741286588835));
#116465=CARTESIAN_POINT('Ctrl Pts',(-10.8345942233826,86.6691746593892,
75.7895144494221));
#116466=CARTESIAN_POINT('Ctrl Pts',(-10.8413435140449,86.641359333253,75.9007191351649));
#116467=CARTESIAN_POINT('Ctrl Pts',(-10.8473523085855,86.6165957561314,
75.9997230367618));
#116468=CARTESIAN_POINT('Ctrl Pts',(-10.8531217396086,86.5913204207394,
76.0954131499708));
#116469=CARTESIAN_POINT('Ctrl Pts',(-10.8586241561333,86.5657622751962,
76.1878199247765));
#116470=CARTESIAN_POINT('Ctrl Pts',(-10.8652247671061,86.5351031320437,
76.2986696158165));
#116471=CARTESIAN_POINT('Ctrl Pts',(-10.8714407767674,86.5040378671458,
76.4047944775482));
#116472=CARTESIAN_POINT('Ctrl Pts',(-10.8772777948961,86.4729322436842,
76.5062569106158));
#116473=CARTESIAN_POINT('Ctrl Pts',(-10.8833283429498,86.4406887136234,
76.6114310446336));
#116474=CARTESIAN_POINT('Ctrl Pts',(-10.8889720238455,86.4084019813046,
76.7115955374519));
#116475=CARTESIAN_POINT('Ctrl Pts',(-10.8942558342815,86.376442466493,76.8068279872566));
#116476=CARTESIAN_POINT('Ctrl Pts',(-10.8952324396605,86.3705353972565,
76.824429777455));
#116477=CARTESIAN_POINT('Ctrl Pts',(-10.896196850492,86.3646394044195,76.8418630967093));
#116478=CARTESIAN_POINT('Ctrl Pts',(-10.8971494929465,86.3587566888011,
76.8591284569882));
#116479=CARTESIAN_POINT('Ctrl Pts',(-10.9005529294257,86.3377399381437,
76.920811155172));
#116480=CARTESIAN_POINT('Ctrl Pts',(-10.9038058355024,86.3168931915867,
76.9803500170193));
#116481=CARTESIAN_POINT('Ctrl Pts',(-10.9069337564245,86.2963127364398,
77.0377685506294));
#116482=CARTESIAN_POINT('Ctrl Pts',(-10.9120682687526,86.2625297210428,
77.1320216267242));
#116483=CARTESIAN_POINT('Ctrl Pts',(-10.9167765779744,86.2294653974887,
77.2205664752667));
#116484=CARTESIAN_POINT('Ctrl Pts',(-10.9210486754665,86.197501551463,77.3035187659328));
#116485=CARTESIAN_POINT('Ctrl Pts',(-10.9252227188449,86.1662713466046,
77.3845671175261));
#116486=CARTESIAN_POINT('Ctrl Pts',(-10.9289809732627,86.1360914017084,
77.4602769639134));
#116487=CARTESIAN_POINT('Ctrl Pts',(-10.9323304910036,86.1072728402612,
77.5307522283811));
#116488=CARTESIAN_POINT('Ctrl Pts',(-10.9326964170239,86.1041244880745,
77.53845146602));
#116489=CARTESIAN_POINT('Ctrl Pts',(-10.9330574760382,86.1009923411827,
77.5460882227403));
#116490=CARTESIAN_POINT('Ctrl Pts',(-10.93341369061,86.0978767752278,77.5536626280678));
#116491=CARTESIAN_POINT('Ctrl Pts',(-10.936890719826,86.067465571677,77.6275967978205));
#116492=CARTESIAN_POINT('Ctrl Pts',(-10.9398996029891,86.0386383539991,
77.6955923112921));
#116493=CARTESIAN_POINT('Ctrl Pts',(-10.9424403395056,86.0117111061841,
77.7577689141376));
#116494=CARTESIAN_POINT('Ctrl Pts',(-10.9437107077639,85.9982474822766,
77.7888572155604));
#116495=CARTESIAN_POINT('Ctrl Pts',(-10.9448640393378,85.9852579622718,
77.8184906332928));
#116496=CARTESIAN_POINT('Ctrl Pts',(-10.9459003341546,85.9727768087027,
77.8466830224824));
#116497=CARTESIAN_POINT('Ctrl Pts',(-10.9464184815629,85.9665362319182,
77.8607792170771));
#116498=CARTESIAN_POINT('Ctrl Pts',(-10.9469073697786,85.9604226970262,
77.8745151324323));
#116499=CARTESIAN_POINT('Ctrl Pts',(-10.9473669988077,85.9544401629786,
77.8878924275129));
#116500=CARTESIAN_POINT('Ctrl Pts',(-10.9475968133222,85.9514488959548,
77.8945810750531));
#116501=CARTESIAN_POINT('Ctrl Pts',(-10.9478193130394,85.9484903760411,
77.9011800661612));
#116502=CARTESIAN_POINT('Ctrl Pts',(-10.9480344979591,85.9455650791476,
77.9076896009303));
#116503=CARTESIAN_POINT('Ctrl Pts',(-10.948142090419,85.9441024307008,77.9109443683149));
#116504=CARTESIAN_POINT('Ctrl Pts',(-10.9482478541794,85.9426480878169,
77.9141767715282));
#116505=CARTESIAN_POINT('Ctrl Pts',(-10.9483517892405,85.9412021087518,
77.9173868352419));
#116506=CARTESIAN_POINT('Ctrl Pts',(-10.9484037567711,85.9404791192192,
77.9189918670988));
#116507=CARTESIAN_POINT('Ctrl Pts',(-10.9484552671268,85.9397582206293,
77.9205913140754));
#116508=CARTESIAN_POINT('Ctrl Pts',(-10.9485063203077,85.9390394201873,
77.922185179234));
#116509=CARTESIAN_POINT('Ctrl Pts',(-10.9485573734885,85.9383206197453,
77.9237790443926));
#116510=CARTESIAN_POINT('Ctrl Pts',(-10.948568260266,85.9381698679242,77.9241138486253));
#116511=CARTESIAN_POINT('Ctrl Pts',(-10.9486581083257,85.9368893204608,
77.9269500323));
#116512=CARTESIAN_POINT('Ctrl Pts',(-10.951395910894,85.8978691552357,78.0133727216242));
#116513=CARTESIAN_POINT('Ctrl Pts',(-10.9537314325388,85.8582240439881,
78.0984489820115));
#116514=CARTESIAN_POINT('Ctrl Pts',(-10.9556525073569,85.8180244885345,
78.1821875838237));
#116515=CARTESIAN_POINT('Ctrl Pts',(-10.9591130519213,85.7456106752817,
78.3330308308512));
#116516=CARTESIAN_POINT('Ctrl Pts',(-10.9612268328035,85.6713997206963,
78.4795321797455));
#116517=CARTESIAN_POINT('Ctrl Pts',(-10.9619612599143,85.5957953551927,
78.621749827295));
#116518=CARTESIAN_POINT('Ctrl Pts',(-10.9622618887243,85.5648476272331,
78.679964892498));
#116519=CARTESIAN_POINT('Ctrl Pts',(-10.9623318059689,85.5336660407217,
78.737462455626));
#116520=CARTESIAN_POINT('Ctrl Pts',(-10.9621704102873,85.5022767295138,
78.7942475578633));
#116521=CARTESIAN_POINT('Ctrl Pts',(-10.9617720353596,85.4247981101503,
78.9344109176964));
#116522=CARTESIAN_POINT('Ctrl Pts',(-10.9599623479946,85.3460566132439,
79.0702318537373));
#116523=CARTESIAN_POINT('Ctrl Pts',(-10.9567596072908,85.2664470382299,
79.2017831826618));
#116524=CARTESIAN_POINT('Ctrl Pts',(-10.9555382395348,85.2360878624529,
79.251950388275));
#116525=CARTESIAN_POINT('Ctrl Pts',(-10.9541145859146,85.2056020553527,
79.3014969164829));
#116526=CARTESIAN_POINT('Ctrl Pts',(-10.9524907355255,85.1750101072347,
79.3504276719218));
#116527=CARTESIAN_POINT('Ctrl Pts',(-10.9482417584689,85.0949630249782,
79.4784601917986));
#116528=CARTESIAN_POINT('Ctrl Pts',(-10.942619355958,85.0141917592843,79.6022756610076));
#116529=CARTESIAN_POINT('Ctrl Pts',(-10.9356304201028,84.9330452710067,
79.721987764502));
#116530=CARTESIAN_POINT('Ctrl Pts',(-10.9335818511937,84.9092599371,79.7570772972067));
#116531=CARTESIAN_POINT('Ctrl Pts',(-10.931416110014,84.8854421357569,79.7918143835424));
#116532=CARTESIAN_POINT('Ctrl Pts',(-10.9291339382821,84.8616000941366,
79.8262021308764));
#116533=CARTESIAN_POINT('Ctrl Pts',(-10.9286955685532,84.8570204084039,
79.8328074828154));
#116534=CARTESIAN_POINT('Ctrl Pts',(-10.9282527382848,84.8524398377061,
79.8393999309981));
#116535=CARTESIAN_POINT('Ctrl Pts',(-10.9278054549261,84.8478584363307,
79.8459795023192));
#116536=CARTESIAN_POINT('Ctrl Pts',(-10.9200712462639,84.7686390477297,
79.9597502843571));
#116537=CARTESIAN_POINT('Ctrl Pts',(-10.9110030852049,84.6891747323319,
80.0696694873031));
#116538=CARTESIAN_POINT('Ctrl Pts',(-10.9006326689777,84.6097646350222,
80.175850627459));
#116539=CARTESIAN_POINT('Ctrl Pts',(-10.8970713501343,84.5824943047176,
80.2123144382621));
#116540=CARTESIAN_POINT('Ctrl Pts',(-10.8933567088875,84.5552300138256,
80.2483375603649));
#116541=CARTESIAN_POINT('Ctrl Pts',(-10.8894907894036,84.5279827932135,
80.2839250246018));
#116542=CARTESIAN_POINT('Ctrl Pts',(-10.8786864366559,84.4518330999468,
80.3833837739681));
#116543=CARTESIAN_POINT('Ctrl Pts',(-10.866697330589,84.3758192380347,80.4794390140921));
#116544=CARTESIAN_POINT('Ctrl Pts',(-10.8535044037148,84.3001723967285,
80.5722125416248));
#116545=CARTESIAN_POINT('Ctrl Pts',(-10.8489469098624,84.2740402110887,
80.6042611374695));
#116546=CARTESIAN_POINT('Ctrl Pts',(-10.844246106719,84.2479515284257,80.635918193433));
#116547=CARTESIAN_POINT('Ctrl Pts',(-10.8394022657455,84.2219149668464,
80.6671889838823));
#116548=CARTESIAN_POINT('Ctrl Pts',(-10.8255735235187,84.1475828612858,
80.7564643549623));
#116549=CARTESIAN_POINT('Ctrl Pts',(-10.8105760714285,84.0736782582328,
80.8425905963213));
#116550=CARTESIAN_POINT('Ctrl Pts',(-10.7944085851747,84.0004093351753,
80.9256789089337));
#116551=CARTESIAN_POINT('Ctrl Pts',(-10.7896138356913,83.978680160617,80.9503201943951));
#116552=CARTESIAN_POINT('Ctrl Pts',(-10.7847164308873,83.9570066589367,
80.9746943605333));
#116553=CARTESIAN_POINT('Ctrl Pts',(-10.7797169475032,83.9353936757825,
80.9988044841311));
#116554=CARTESIAN_POINT('Ctrl Pts',(-10.7649032283752,83.8713533265372,
81.0702439853112));
#116555=CARTESIAN_POINT('Ctrl Pts',(-10.7491908635468,83.8078463452034,
81.1393644748102));
#116556=CARTESIAN_POINT('Ctrl Pts',(-10.7325548086161,83.7450174768963,
81.2062284540156));
#116557=CARTESIAN_POINT('',(-10.0948776383655,81.4411710637376,83.1136760388969));
#116558=CARTESIAN_POINT('Ctrl Pts',(-10.7325548086179,83.7450177191935,
81.2062286816919));
#116559=CARTESIAN_POINT('Ctrl Pts',(-10.7094056412749,83.6576110466643,
81.2992481947719));
#116560=CARTESIAN_POINT('Ctrl Pts',(-10.6857306659004,83.5690067944165,
81.3905677640237));
#116561=CARTESIAN_POINT('Ctrl Pts',(-10.6615694462013,83.4792858039514,
81.4801620977175));
#116562=CARTESIAN_POINT('Ctrl Pts',(-10.6374082265022,83.3895648134863,
81.5697564314113));
#116563=CARTESIAN_POINT('Ctrl Pts',(-10.6127607624786,83.2987275812377,
81.657626026861));
#116564=CARTESIAN_POINT('Ctrl Pts',(-10.5876490343607,83.2068057061495,
81.7437931611233));
#116565=CARTESIAN_POINT('Ctrl Pts',(-10.5625373062429,83.1148838310612,
81.8299602953855));
#116566=CARTESIAN_POINT('Ctrl Pts',(-10.5369613140309,83.0218771946117,
81.9144248336993));
#116567=CARTESIAN_POINT('Ctrl Pts',(-10.5109555987824,82.9278254887252,
81.997195721309));
#116568=CARTESIAN_POINT('Ctrl Pts',(-10.4849498835339,82.8337737828386,
82.0799666089187));
#116569=CARTESIAN_POINT('Ctrl Pts',(-10.4585144452489,82.7386771162062,
82.1610439757537));
#116570=CARTESIAN_POINT('Ctrl Pts',(-10.4316882718126,82.6425589685798,
82.2404456022542));
#116571=CARTESIAN_POINT('Ctrl Pts',(-10.4048620983762,82.5464408209533,
82.3198472287548));
#116572=CARTESIAN_POINT('Ctrl Pts',(-10.3776451897886,82.4493012237793,
82.3975731462497));
#116573=CARTESIAN_POINT('Ctrl Pts',(-10.3500918160521,82.351155775502,82.4736407678395));
#116574=CARTESIAN_POINT('Ctrl Pts',(-10.3225384423156,82.2530103272247,
82.5497083894292));
#116575=CARTESIAN_POINT('Ctrl Pts',(-10.2946486034302,82.1538589465135,
82.6241176161567));
#116576=CARTESIAN_POINT('Ctrl Pts',(-10.2664905900852,82.0537231169019,
82.6968752842873));
#116577=CARTESIAN_POINT('Ctrl Pts',(-10.2383325767402,81.9535872872904,
82.7696329524178));
#116578=CARTESIAN_POINT('Ctrl Pts',(-10.2099063889356,81.8524671189661,
82.8407392030616));
#116579=CARTESIAN_POINT('Ctrl Pts',(-10.181277888407,81.7503663349919,82.9102075622766));
#116580=CARTESIAN_POINT('Ctrl Pts',(-10.1526494167491,81.6482656539822,
82.9796758514356));
#116581=CARTESIAN_POINT('Ctrl Pts',(-10.1238186327753,81.5451840202451,
83.0475057597329));
#116582=CARTESIAN_POINT('Ctrl Pts',(-10.0948776413094,81.4411712996156,
83.1136764109577));
#116583=CARTESIAN_POINT('Ctrl Pts',(-10.0948775537519,81.44117080392,83.11367632661));
#116584=CARTESIAN_POINT('Ctrl Pts',(-10.0503152587603,81.2811042916383,
83.2155075847456));
#116585=CARTESIAN_POINT('Ctrl Pts',(-9.99904314712063,81.1049072372153,
83.3223055647842));
#116586=CARTESIAN_POINT('Ctrl Pts',(-9.912070254689,80.8148282663644,83.4865137751945));
#116587=CARTESIAN_POINT('Ctrl Pts',(-9.88140183638311,80.7138382560085,
83.5419112301925));
#116588=CARTESIAN_POINT('Ctrl Pts',(-9.83288302768125,80.5557177866961,
83.625503240927));
#116589=CARTESIAN_POINT('Ctrl Pts',(-9.80799457801955,80.4749988320776,
83.6674224966469));
#116590=CARTESIAN_POINT('Ctrl Pts',(-9.77785722412043,80.377884338857,83.7164278765081));
#116591=CARTESIAN_POINT('Ctrl Pts',(-9.7625133398474,80.3285867257644,83.7409403779417));
#116592=CARTESIAN_POINT('Ctrl Pts',(-9.75477259588003,80.3037522380146,
83.7531971798874));
#116593=CARTESIAN_POINT('Ctrl Pts',(-9.75144039093026,80.2930690347116,
83.7584500077144));
#116594=CARTESIAN_POINT('Ctrl Pts',(-9.74921564468608,80.28593803639,83.7619518506129));
#116595=CARTESIAN_POINT('Ctrl Pts',(-9.74760337617057,80.2807717678712,
83.76448470132));
#116596=CARTESIAN_POINT('Ctrl Pts',(-9.72722943538018,80.2154968625108,
83.7964589701507));
#116597=CARTESIAN_POINT('Ctrl Pts',(-9.69987038258628,80.1283934374761,
83.8385299499183));
#116598=CARTESIAN_POINT('Ctrl Pts',(-9.64742804717243,79.9608419184596,
83.9156376385006));
#116599=CARTESIAN_POINT('Ctrl Pts',(-9.62804664266397,79.8988361406045,
83.9436586549674));
#116600=CARTESIAN_POINT('Ctrl Pts',(-9.59612359684555,79.7964020015627,
83.98870389199));
#116601=CARTESIAN_POINT('Ctrl Pts',(-9.57944933917239,79.7428281743368,
84.0119784579149));
#116602=CARTESIAN_POINT('Ctrl Pts',(-9.56170597935333,79.6856801076756,
84.0362803711258));
#116603=CARTESIAN_POINT('Ctrl Pts',(-9.54963949455265,79.6467826136689,
84.052697816691));
#116604=CARTESIAN_POINT('Ctrl Pts',(-9.54307101057707,79.6255896711592,
84.0615737659991));
#116605=CARTESIAN_POINT('Ctrl Pts',(-9.49038169671332,79.4554449164131,
84.1323106572381));
#116606=CARTESIAN_POINT('Ctrl Pts',(-9.44836711016332,79.3176255198826,
84.1860108422029));
#116607=CARTESIAN_POINT('Ctrl Pts',(-9.39257576899831,79.1321384223008,
84.2552014191141));
#116608=CARTESIAN_POINT('Ctrl Pts',(-9.37518374505331,79.0738455902002,
84.2763669865997));
#116609=CARTESIAN_POINT('Ctrl Pts',(-9.3509033438008,78.9918160771606,84.305525217164));
#116610=CARTESIAN_POINT('Ctrl Pts',(-9.33921505184079,78.9521534352811,
84.3194563301342));
#116611=CARTESIAN_POINT('Ctrl Pts',(-9.32636955138672,78.9082664269095,
84.3346264026876));
#116612=CARTESIAN_POINT('Ctrl Pts',(-9.32014451120116,78.8869217029075,
84.3419467200815));
#116613=CARTESIAN_POINT('Ctrl Pts',(-9.31751900327339,78.8779025117332,
84.3450279074121));
#116614=CARTESIAN_POINT('Ctrl Pts',(-9.31577807941876,78.8719183095939,
84.3470696368959));
#116615=CARTESIAN_POINT('Ctrl Pts',(-9.31544178421389,78.8707627633681,
84.347464173305));
#116616=CARTESIAN_POINT('Ctrl Pts',(-9.26955506958364,78.7128328443911,
84.4012091119334));
#116617=CARTESIAN_POINT('Ctrl Pts',(-9.22873679430673,78.5675302623779,
84.4472128255647));
#116618=CARTESIAN_POINT('Ctrl Pts',(-9.17302628066541,78.3619860064613,
84.5085318351849));
#116619=CARTESIAN_POINT('Ctrl Pts',(-9.14655024866327,78.2623134976708,
84.5372674497077));
#116620=CARTESIAN_POINT('Ctrl Pts',(-9.11807518809318,78.1515678237594,
84.567724741971));
#116621=CARTESIAN_POINT('Ctrl Pts',(-9.10444106866622,78.0975922362132,
84.5822219191351));
#116622=CARTESIAN_POINT('Ctrl Pts',(-9.09777486166728,78.0709552791927,
84.5892920098368));
#116623=CARTESIAN_POINT('Ctrl Pts',(-9.09495024139227,78.0596147781854,
84.5922842614441));
#116624=CARTESIAN_POINT('Ctrl Pts',(-9.09307434467153,78.05207120322,84.5942707496973));
#116625=CARTESIAN_POINT('Ctrl Pts',(-9.09244053606258,78.0495203074527,
84.594941784726));
#116626=CARTESIAN_POINT('Ctrl Pts',(-9.05180720977179,77.885591750876,84.6379394466845));
#116627=CARTESIAN_POINT('Ctrl Pts',(-9.01546474124791,77.7288171154016,
84.6755714490163));
#116628=CARTESIAN_POINT('Ctrl Pts',(-8.96554035573562,77.4972590772881,
84.7264335172893));
#116629=CARTESIAN_POINT('Ctrl Pts',(-8.94172549229785,77.3823802815235,
84.7504680239201));
#116630=CARTESIAN_POINT('Ctrl Pts',(-8.91594931126095,77.2499936291791,
84.7761747632328));
#116631=CARTESIAN_POINT('Ctrl Pts',(-8.90356317731929,77.1842173036598,
84.7884584738757));
#116632=CARTESIAN_POINT('Ctrl Pts',(-8.89836239632504,77.1561175822305,
84.7936023187275));
#116633=CARTESIAN_POINT('Ctrl Pts',(-8.89491911168967,77.1374045486816,
84.7970049108324));
#116634=CARTESIAN_POINT('Ctrl Pts',(-8.89357005880115,77.1300413420178,
84.7983371356429));
#116635=CARTESIAN_POINT('Ctrl Pts',(-8.75977550793369,76.3942664536245,
84.9303191121072));
#116636=CARTESIAN_POINT('Ctrl Pts',(-8.69370887000654,75.6839064820694,
84.98888938658));
#116637=CARTESIAN_POINT('Ctrl Pts',(-8.69331176731091,75.00000000541,84.98885921934));
#116638=CARTESIAN_POINT('Origin',(27.4324635166691,25.,72.98888938658));
#116639=CARTESIAN_POINT('',(-7.08826202869291,64.825987357,58.34040756172));
#116640=CARTESIAN_POINT('',(-10.067463384623,56.310682064485,72.9888891145402));
#116641=CARTESIAN_POINT('Ctrl Pts',(-7.08826202869291,64.825987357,58.34040756172));
#116642=CARTESIAN_POINT('Ctrl Pts',(-7.24267999369472,64.1486336869958,
58.7046006729965));
#116643=CARTESIAN_POINT('Ctrl Pts',(-7.40664860408434,63.505158727736,59.1068827930799));
#116644=CARTESIAN_POINT('Ctrl Pts',(-7.66100278224209,62.5907643549632,
59.7694119675106));
#116645=CARTESIAN_POINT('Ctrl Pts',(-7.74717579931205,62.2944359083917,
60.0001063446241));
#116646=CARTESIAN_POINT('Ctrl Pts',(-7.87768758671566,61.8626477550637,
60.3611577658764));
#116647=CARTESIAN_POINT('Ctrl Pts',(-7.9432553932647,61.649929807532,60.5454358170881));
#116648=CARTESIAN_POINT('Ctrl Pts',(-8.00912491301031,61.4419760536987,
60.7353844945309));
#116649=CARTESIAN_POINT('Ctrl Pts',(-8.05308578013046,61.3043989275207,
60.8632816219083));
#116650=CARTESIAN_POINT('Ctrl Pts',(-8.07558635098398,61.2346134642867,
60.9293321247506));
#116651=CARTESIAN_POINT('Ctrl Pts',(-8.26928846854225,60.6387810788844,
61.5030451637313));
#116652=CARTESIAN_POINT('Ctrl Pts',(-8.43901295569384,60.1518492983687,
62.041887135517));
#116653=CARTESIAN_POINT('Ctrl Pts',(-8.68450790024914,59.4854971373579,
62.8942474257412));
#116654=CARTESIAN_POINT('Ctrl Pts',(-8.76481806882766,59.2740540019814,
63.1857138175993));
#116655=CARTESIAN_POINT('Ctrl Pts',(-8.92142008072934,58.8725162344827,
63.7834240098156));
#116656=CARTESIAN_POINT('Ctrl Pts',(-8.99797239407982,58.6817880507017,
64.0907755449453));
#116657=CARTESIAN_POINT('Ctrl Pts',(-9.2185027435778,58.1454275641928,65.0284224069521));
#116658=CARTESIAN_POINT('Ctrl Pts',(-9.35433664401844,57.830887894101,65.677944992921));
#116659=CARTESIAN_POINT('Ctrl Pts',(-9.53607045987608,57.4236293703346,
66.68852121302));
#116660=CARTESIAN_POINT('Ctrl Pts',(-9.59297517919348,57.2986350259743,
67.0314238232507));
#116661=CARTESIAN_POINT('Ctrl Pts',(-9.6721357626539,57.1272812547768,67.55475293626));
#116662=CARTESIAN_POINT('Ctrl Pts',(-9.71016660933379,57.0456388055137,
67.8186607659407));
#116663=CARTESIAN_POINT('Ctrl Pts',(-9.74574171923844,56.9700480107542,
68.0859115726082));
#116664=CARTESIAN_POINT('Ctrl Pts',(-9.76889793333612,56.9209989596931,
68.2648188670356));
#116665=CARTESIAN_POINT('Ctrl Pts',(-9.78005219265401,56.8974491471374,
68.3534662981843));
#116666=CARTESIAN_POINT('Ctrl Pts',(-9.96966609619479,56.4982548013989,
69.9067322790409));
#116667=CARTESIAN_POINT('Ctrl Pts',(-10.0675364833309,56.3104931139281,
71.424806576562));
#116668=CARTESIAN_POINT('Ctrl Pts',(-10.0674651278229,56.31068206442,72.9888891141279));
#116669=CARTESIAN_POINT('',(-7.0883818064374,64.8259873343748,87.637422020082));
#116670=CARTESIAN_POINT('Ctrl Pts',(-10.0674651278229,56.31068206442,72.9888891141279));
#116671=CARTESIAN_POINT('Ctrl Pts',(-10.0675364833309,56.3105869691024,
73.724381242214));
#116672=CARTESIAN_POINT('Ctrl Pts',(-10.045894923569,56.3529537458112,74.4525676988862));
#116673=CARTESIAN_POINT('Ctrl Pts',(-9.98293498174587,56.4801967189142,
75.5320924062045));
#116674=CARTESIAN_POINT('Ctrl Pts',(-9.94383162901423,56.5597414074757,
76.0686695361057));
#116675=CARTESIAN_POINT('Ctrl Pts',(-9.88530911783133,56.680409147648,76.6887457170077));
#116676=CARTESIAN_POINT('Ctrl Pts',(-9.8528778023235,56.7477094186136,76.997259346543));
#116677=CARTESIAN_POINT('Ctrl Pts',(-9.83587656653315,56.7831011543162,
77.1511298884427));
#116678=CARTESIAN_POINT('Ctrl Pts',(-9.82842272910424,56.798642241093,77.2169910887884));
#116679=CARTESIAN_POINT('Ctrl Pts',(-9.8234163439587,56.8090858989546,77.2608799805709));
#116680=CARTESIAN_POINT('Ctrl Pts',(-9.82103027562739,56.8140658122574,
77.2816438526153));
#116681=CARTESIAN_POINT('Ctrl Pts',(-9.73272175794122,56.9984745832181,
78.0438490465314));
#116682=CARTESIAN_POINT('Ctrl Pts',(-9.62773423677328,57.2214589055245,
78.7577383351392));
#116683=CARTESIAN_POINT('Ctrl Pts',(-9.44733341207722,57.6221809328644,
79.7898119286563));
#116684=CARTESIAN_POINT('Ctrl Pts',(-9.38337611636343,57.7667958659578,
80.1273831484367));
#116685=CARTESIAN_POINT('Ctrl Pts',(-9.28243301353116,58.0002796515679,
80.6239996048413));
#116686=CARTESIAN_POINT('Ctrl Pts',(-9.2307092849391,58.1211618908655,80.8698732871114));
#116687=CARTESIAN_POINT('Ctrl Pts',(-9.17724028826713,58.2482546499019,
81.1120885623046));
#116688=CARTESIAN_POINT('Ctrl Pts',(-9.14122097838372,58.3343632714237,
81.272752011587));
#116689=CARTESIAN_POINT('Ctrl Pts',(-9.12343746339077,58.3771094829852,
81.350890758788));
#116690=CARTESIAN_POINT('Ctrl Pts',(-9.02949491806345,58.6042723990177,
81.7574127347759));
#116691=CARTESIAN_POINT('Ctrl Pts',(-8.95228473824977,58.7944286240105,
82.0717518718014));
#116692=CARTESIAN_POINT('Ctrl Pts',(-8.83457068817163,59.0923017997501,
82.5270655282608));
#116693=CARTESIAN_POINT('Ctrl Pts',(-8.77523768283496,59.2443980971824,
82.7506742777178));
#116694=CARTESIAN_POINT('Ctrl Pts',(-8.71540134802023,59.4012339589587,
82.9682394673107));
#116695=CARTESIAN_POINT('Ctrl Pts',(-8.67542120793468,59.5068444366637,
83.1119434230033));
#116696=CARTESIAN_POINT('Ctrl Pts',(-8.65577194947727,59.5591419591804,
83.181771430353));
#116697=CARTESIAN_POINT('Ctrl Pts',(-8.55350454907456,59.8336060090282,
83.5411136575106));
#116698=CARTESIAN_POINT('Ctrl Pts',(-8.4695959972588,60.0660422041825,83.8228958350763));
#116699=CARTESIAN_POINT('Ctrl Pts',(-8.34112301080695,60.4339939298278,
84.2370625817306));
#116700=CARTESIAN_POINT('Ctrl Pts',(-8.29786343947522,60.559860743862,84.3737006135942));
#116701=CARTESIAN_POINT('Ctrl Pts',(-8.21055983276111,60.8180268495683,
84.6441490396162));
#116702=CARTESIAN_POINT('Ctrl Pts',(-8.16692619209731,60.9490733898373,
84.7767354767832));
#116703=CARTESIAN_POINT('Ctrl Pts',(-7.7636854370743,62.1799879268859,85.9793603608846));
#116704=CARTESIAN_POINT('Ctrl Pts',(-7.40740356864993,63.426703148092,86.8849892493009));
#116705=CARTESIAN_POINT('Ctrl Pts',(-7.08824925985691,64.82598733535,87.63736578702));
#116706=CARTESIAN_POINT('',(-7.08815755253877,22.5,87.6373268799153));
#116707=CARTESIAN_POINT('',(-7.08815755536701,25.,87.6373268732506));
#116708=CARTESIAN_POINT('',(-8.23395173885291,22.5,84.57149802283));
#116709=CARTESIAN_POINT('Origin',(27.4324635166691,22.5,72.98888938658));
#116710=CARTESIAN_POINT('',(-8.23395173818611,10.,84.5714980248862));
#116711=CARTESIAN_POINT('',(-8.23395173885291,22.5,84.57149802283));
#116712=CARTESIAN_POINT('',(-7.08815755056573,10.,58.340451888595));
#116713=CARTESIAN_POINT('Origin',(27.4324635166691,10.,72.98888938658));
#116714=CARTESIAN_POINT('',(-7.08815755142092,25.,58.34045189061));
#116715=CARTESIAN_POINT('Origin',(6.43246351666909,-92.5,72.98888938658));
#116716=CARTESIAN_POINT('',(14.9324629260191,25.5800360490065,72.98888938658));
#116717=CARTESIAN_POINT('',(14.2241913549675,25.6803058095512,69.5919860434059));
#116718=CARTESIAN_POINT('Ctrl Pts',(14.9324629260191,25.5800360490065,72.98888938658));
#116719=CARTESIAN_POINT('Ctrl Pts',(14.9324626931148,25.556144234287,72.8429202738032));
#116720=CARTESIAN_POINT('Ctrl Pts',(14.9228631443724,25.5035388027324,72.4703017419395));
#116721=CARTESIAN_POINT('Ctrl Pts',(14.8679915267049,25.4553343707258,71.8723531717214));
#116722=CARTESIAN_POINT('Ctrl Pts',(14.7503488053081,25.4533873314043,71.1936658431954));
#116723=CARTESIAN_POINT('Ctrl Pts',(14.572743094615,25.5073301307937,70.5070039054373));
#116724=CARTESIAN_POINT('Ctrl Pts',(14.3852859030436,25.5948194038957,69.973693869023));
#116725=CARTESIAN_POINT('Ctrl Pts',(14.2575749161567,25.6622795837767,69.6685609430364));
#116726=CARTESIAN_POINT('Ctrl Pts',(14.2241960818191,25.68030397154,69.591995772582));
#116727=CARTESIAN_POINT('',(14.2241493853463,26.6269447605316,76.3858806723372));
#116728=CARTESIAN_POINT('Ctrl Pts',(14.2241515060895,26.6269447605405,76.3858815969566));
#116729=CARTESIAN_POINT('Ctrl Pts',(14.301420357292,26.5533368797724,76.2086481732271));
#116730=CARTESIAN_POINT('Ctrl Pts',(14.3723588782976,26.4805897804971,76.0294311309084));
#116731=CARTESIAN_POINT('Ctrl Pts',(14.4369615507881,26.4097165788527,75.8486116146905));
#116732=CARTESIAN_POINT('Ctrl Pts',(14.5194755009863,26.3191935771651,75.6176593648704));
#116733=CARTESIAN_POINT('Ctrl Pts',(14.5916532948012,26.2317276051259,75.3840929064488));
#116734=CARTESIAN_POINT('Ctrl Pts',(14.6535466657325,26.149138675707,75.148470794251));
#116735=CARTESIAN_POINT('Ctrl Pts',(14.7063523690853,26.0786760972192,74.9474445587614));
#116736=CARTESIAN_POINT('Ctrl Pts',(14.7516720122209,26.0117635317123,74.7449220071315));
#116737=CARTESIAN_POINT('Ctrl Pts',(14.7894951923039,25.949445299615,74.5413138042756));
#116738=CARTESIAN_POINT('Ctrl Pts',(14.8275519301444,25.8867422530599,74.3364483228102));
#116739=CARTESIAN_POINT('Ctrl Pts',(14.8580193379202,25.8286904550241,74.1304837409515));
#116740=CARTESIAN_POINT('Ctrl Pts',(14.8808863595751,25.7762233263775,73.9238500636511));
#116741=CARTESIAN_POINT('Ctrl Pts',(14.9059012075637,25.7188281278553,73.6978079447862));
#116742=CARTESIAN_POINT('Ctrl Pts',(14.9218208569589,25.6681159683744,73.4709651355588));
#116743=CARTESIAN_POINT('Ctrl Pts',(14.9286358566856,25.6250936747152,73.2439493185516));
#116744=CARTESIAN_POINT('Ctrl Pts',(14.931187773495,25.608983723318,73.1589419080368));
#116745=CARTESIAN_POINT('Ctrl Pts',(14.932463061676,25.593952023497,73.0739102388527));
#116746=CARTESIAN_POINT('Ctrl Pts',(14.9324629260191,25.5800360490065,72.98888938658));
#116747=CARTESIAN_POINT('',(14.2241883540074,89.,76.3858032888143));
#116748=CARTESIAN_POINT('',(14.2241883532291,89.,76.385803290591));
#116749=CARTESIAN_POINT('',(14.2241883539424,89.,69.591975484192));
#116750=CARTESIAN_POINT('Origin',(6.43246351666909,89.,72.98888938658));
#116751=CARTESIAN_POINT('',(14.2241883529691,89.,69.591975481954));
#116752=CARTESIAN_POINT('Origin',(-15.5675364832709,75.,72.98888938658));
#116753=CARTESIAN_POINT('',(-18.5675364832709,75.,62.73888938658));
#116754=CARTESIAN_POINT('Origin',(-18.5675364832709,75.,72.98888938658));
#116755=CARTESIAN_POINT('',(-15.5675364833309,75.,62.73888938658));
#116756=CARTESIAN_POINT('',(-15.5675364832709,75.,62.73888938658));
#116757=CARTESIAN_POINT('Origin',(-15.5675364833309,75.,72.98888938658));
#116758=CARTESIAN_POINT('Origin',(-18.5675364832709,75.,72.98888938658));
#116759=CARTESIAN_POINT('',(-20.0675364832709,75.,84.7388893856825));
#116760=CARTESIAN_POINT('',(-20.0675364832709,75.,61.23888938658));
#116761=CARTESIAN_POINT('Origin',(-20.0675364832709,75.,72.98888938658));
#116762=CARTESIAN_POINT('',(-18.5675364832709,75.,61.23888938658));
#116763=CARTESIAN_POINT('',(-18.5675364832709,75.,61.23888938658));
#116764=CARTESIAN_POINT('Origin',(-18.5675364832709,75.,72.98888938658));
#116765=CARTESIAN_POINT('Origin',(-20.0675364832709,75.,72.98888938658));
#116766=CARTESIAN_POINT('Origin',(-20.5675364832709,75.,72.98888938658));
#116767=CARTESIAN_POINT('',(-20.5675364832709,75.,84.23888938658));
#116768=CARTESIAN_POINT('',(-20.5675364832709,75.,84.23888938658));
#116769=CARTESIAN_POINT('Origin',(-20.5675364832709,75.,72.98888938658));
#116770=CARTESIAN_POINT('Origin',(-20.5675364832709,75.,72.98888938658));
#116771=CARTESIAN_POINT('',(-20.3675364832709,75.,65.23888938658));
#116772=CARTESIAN_POINT('',(-20.3675364832709,75.,80.73888938658));
#116773=CARTESIAN_POINT('Origin',(-20.3675364832709,75.,72.98888938658));
#116774=CARTESIAN_POINT('',(-18.0675364832709,75.,80.73888938658));
#116775=CARTESIAN_POINT('',(-20.5675364832709,75.,80.73888938658));
#116776=CARTESIAN_POINT('',(-18.0675364832709,75.,65.23888938658));
#116777=CARTESIAN_POINT('Origin',(-18.0675364832709,75.,72.98888938658));
#116778=CARTESIAN_POINT('Origin',(-18.0675364832709,75.,72.98888938658));
#116779=CARTESIAN_POINT('Origin',(-20.3675364832709,75.,72.98888938658));
#116780=CARTESIAN_POINT('Origin',(-18.0675364832709,75.,72.98888938658));
#116781=CARTESIAN_POINT('',(-17.0930718951697,71.9689110866349,78.2388893867872));
#116782=CARTESIAN_POINT('',(-17.0930718951698,78.0310889133652,78.2388893867871));
#116783=CARTESIAN_POINT('Ctrl Pts',(-17.0930718944527,71.9689110864279,
78.23888938658));
#116784=CARTESIAN_POINT('Ctrl Pts',(-16.2180718918697,75.,78.23888938658));
#116785=CARTESIAN_POINT('Ctrl Pts',(-17.0930718944527,78.0310889135722,
78.23888938658));
#116786=CARTESIAN_POINT('',(-17.0930718951698,68.9378221732697,72.98888938658));
#116787=CARTESIAN_POINT('Ctrl Pts',(-17.0930718945656,68.9378221731502,
72.9888893859585));
#116788=CARTESIAN_POINT('Ctrl Pts',(-16.2180718917851,70.4533666301317,
75.61388938658));
#116789=CARTESIAN_POINT('Ctrl Pts',(-17.0930718945656,71.9689110871133,
78.2388893872015));
#116790=CARTESIAN_POINT('',(-17.0930718951698,71.9689110866349,67.7388893863728));
#116791=CARTESIAN_POINT('Ctrl Pts',(-17.0930718945656,71.9689110871132,
67.7388893859585));
#116792=CARTESIAN_POINT('Ctrl Pts',(-16.2180718917851,70.4533666301317,
70.36388938658));
#116793=CARTESIAN_POINT('Ctrl Pts',(-17.0930718945656,68.9378221731501,
72.9888893872014));
#116794=CARTESIAN_POINT('',(-16.6241608063082,75.,67.73888938658));
#116795=CARTESIAN_POINT('Ctrl Pts',(-17.0930718944527,71.9689110864279,
67.73888938658));
#116796=CARTESIAN_POINT('Ctrl Pts',(-16.6241608063082,73.5932667396053,
67.73888938658));
#116797=CARTESIAN_POINT('Ctrl Pts',(-16.6241608063082,75.,67.73888938658));
#116798=CARTESIAN_POINT('',(-18.0675364832709,75.,65.23888938658));
#116799=CARTESIAN_POINT('',(-17.0930718951698,78.0310889133651,67.7388893863728));
#116800=CARTESIAN_POINT('Ctrl Pts',(-16.6241608063082,75.,67.73888938658));
#116801=CARTESIAN_POINT('Ctrl Pts',(-16.6241608063082,76.4067332603946,
67.73888938658));
#116802=CARTESIAN_POINT('Ctrl Pts',(-17.0930718944527,78.0310889135721,
67.73888938658));
#116803=CARTESIAN_POINT('',(-17.0930718951697,81.0621778267303,72.98888938658));
#116804=CARTESIAN_POINT('Ctrl Pts',(-17.0930718945656,81.0621778268498,
72.9888893872014));
#116805=CARTESIAN_POINT('Ctrl Pts',(-16.2180718917851,79.5466333698683,
70.36388938658));
#116806=CARTESIAN_POINT('Ctrl Pts',(-17.0930718945656,78.0310889128867,
67.7388893859585));
#116807=CARTESIAN_POINT('Ctrl Pts',(-17.0930718945656,78.0310889128868,
78.2388893872014));
#116808=CARTESIAN_POINT('Ctrl Pts',(-16.2180718917851,79.5466333698683,
75.61388938658));
#116809=CARTESIAN_POINT('Ctrl Pts',(-17.0930718945656,81.0621778268498,
72.9888893859586));
#116810=CARTESIAN_POINT('Origin',(-20.5675364832709,75.,72.98888938658));
#116811=CARTESIAN_POINT('',(-20.5675364832709,75.,65.03888938658));
#116812=CARTESIAN_POINT('',(-20.5675364832709,75.,65.03888938658));
#116813=CARTESIAN_POINT('Origin',(-20.5675364832709,75.,72.98888938658));
#116814=CARTESIAN_POINT('Origin',(-15.5675364832709,75.,72.98888938658));
#116815=CARTESIAN_POINT('',(-15.5675364832709,68.9378221735089,72.98888938658));
#116816=CARTESIAN_POINT('',(-15.5675364832709,71.9689110867545,78.23888938658));
#116817=CARTESIAN_POINT('',(-15.5675364832709,71.9689110867545,78.23888938658));
#116818=CARTESIAN_POINT('',(-15.5675364832709,78.0310889132456,78.23888938658));
#116819=CARTESIAN_POINT('',(-15.5675364832709,78.0310889132456,78.23888938658));
#116820=CARTESIAN_POINT('',(-15.5675364832709,81.0621778264911,72.98888938658));
#116821=CARTESIAN_POINT('',(-15.5675364832709,81.0621778264911,72.98888938658));
#116822=CARTESIAN_POINT('',(-15.5675364832709,78.0310889132455,67.73888938658));
#116823=CARTESIAN_POINT('',(-15.5675364832709,78.0310889132455,67.73888938658));
#116824=CARTESIAN_POINT('',(-15.5675364832709,71.9689110867545,67.73888938658));
#116825=CARTESIAN_POINT('',(-15.5675364832709,71.9689110867545,67.73888938658));
#116826=CARTESIAN_POINT('',(-15.5675364832709,68.9378221735089,72.98888938658));
#116827=CARTESIAN_POINT('Origin',(-25.5675364832709,71.9689110867545,78.23888938658));
#116828=CARTESIAN_POINT('',(-25.5675364832709,68.9378221735089,72.98888938658));
#116829=CARTESIAN_POINT('',(-25.5675364832709,71.9689110867545,78.23888938658));
#116830=CARTESIAN_POINT('Origin',(-25.5675364832709,78.0310889132456,78.23888938658));
#116831=CARTESIAN_POINT('',(-25.5675364832709,78.0310889132456,78.23888938658));
#116832=CARTESIAN_POINT('Origin',(-25.5675364832709,81.0621778264911,72.98888938658));
#116833=CARTESIAN_POINT('',(-25.5675364832709,81.0621778264911,72.98888938658));
#116834=CARTESIAN_POINT('Origin',(-25.5675364832709,78.0310889132455,67.73888938658));
#116835=CARTESIAN_POINT('',(-25.5675364832709,78.0310889132455,67.73888938658));
#116836=CARTESIAN_POINT('Origin',(-25.5675364832709,71.9689110867545,67.73888938658));
#116837=CARTESIAN_POINT('',(-25.5675364832709,71.9689110867545,67.73888938658));
#116838=CARTESIAN_POINT('Origin',(-25.5675364832709,68.9378221735089,72.98888938658));
#116839=CARTESIAN_POINT('Origin',(-18.5675364832709,75.,72.98888938658));
#116840=CARTESIAN_POINT('Origin',(-20.5675364832709,75.,72.98888938658));
#116841=CARTESIAN_POINT('Origin',(22.4176035807091,15.,81.066383761497));
#116842=CARTESIAN_POINT('',(21.1895064189465,15.000000374545,65.4633429305526));
#116843=CARTESIAN_POINT('',(19.9598072485171,15.0000009014414,58.489372381727));
#116844=CARTESIAN_POINT('',(23.5337568174491,15.,78.758247596214));
#116845=CARTESIAN_POINT('',(20.4074539076363,16.323529159868,65.6012398886274));
#116846=CARTESIAN_POINT('Origin',(19.7122947894285,15.,65.7238151970529));
#116847=CARTESIAN_POINT('',(19.1777534373736,16.323529923502,58.6272689137465));
#116848=CARTESIAN_POINT('',(22.7517036150791,16.32352940976,78.896144732003));
#116849=CARTESIAN_POINT('Origin',(18.4825956513191,15.,58.74984483153));
#116850=CARTESIAN_POINT('Ctrl Pts',(12.7032824634691,21.12789835764,82.238037292941));
#116851=CARTESIAN_POINT('Ctrl Pts',(12.7138554120091,21.14828359132,82.237040898622));
#116852=CARTESIAN_POINT('Ctrl Pts',(12.8158373280291,21.35262796258,82.223214955634));
#116853=CARTESIAN_POINT('Ctrl Pts',(12.9542723631091,21.78746324258,82.119828041772));
#116854=CARTESIAN_POINT('Ctrl Pts',(12.9927499413291,22.43374057185,81.82237309057));
#116855=CARTESIAN_POINT('Ctrl Pts',(12.9040637925191,22.89144264331,81.525965837519));
#116856=CARTESIAN_POINT('Ctrl Pts',(12.8188596948191,23.13940046188,81.341229725473));
#116857=CARTESIAN_POINT('Ctrl Pts',(12.8039698070391,23.17979419886,81.3104543621581));
#116858=CARTESIAN_POINT('Ctrl Pts',(12.2574243304591,21.44258358145,82.137599709054));
#116859=CARTESIAN_POINT('Ctrl Pts',(12.2648149716791,21.4590752496,82.1384735189879));
#116860=CARTESIAN_POINT('Ctrl Pts',(12.3361831962091,21.62530550758,82.144718783879));
#116861=CARTESIAN_POINT('Ctrl Pts',(12.4361287210991,21.99868109559,82.108019885141));
#116862=CARTESIAN_POINT('Ctrl Pts',(12.4736490564891,22.61131241278,81.933979041512));
#116863=CARTESIAN_POINT('Ctrl Pts',(12.4198055527491,23.08419677334,81.721137563021));
#116864=CARTESIAN_POINT('Ctrl Pts',(12.3623243256291,23.35151971112,81.5753002657141));
#116865=CARTESIAN_POINT('Ctrl Pts',(12.3521479900591,23.39541857132,81.550693031506));
#116866=CARTESIAN_POINT('Ctrl Pts',(11.8797380580991,21.71775544054,82.436832824221));
#116867=CARTESIAN_POINT('Ctrl Pts',(11.8879752712991,21.73377171117,82.439230205427));
#116868=CARTESIAN_POINT('Ctrl Pts',(11.9685429834291,21.89572596927,82.461081441199));
#116869=CARTESIAN_POINT('Ctrl Pts',(12.1037386879891,22.27116764255,82.462282033507));
#116870=CARTESIAN_POINT('Ctrl Pts',(12.2280447882491,22.92210242598,82.328679396874));
#116871=CARTESIAN_POINT('Ctrl Pts',(12.2548992725691,23.44220679821,82.11473481512));
#116872=CARTESIAN_POINT('Ctrl Pts',(12.2436859938191,23.73958274288,81.954178203878));
#116873=CARTESIAN_POINT('Ctrl Pts',(12.2410687116591,23.78853957945,81.926787648707));
#116874=CARTESIAN_POINT('Ctrl Pts',(11.7737606800391,21.80512243469,82.974478406183));
#116875=CARTESIAN_POINT('Ctrl Pts',(11.7864171226091,21.82433766992,82.977231665452));
#116876=CARTESIAN_POINT('Ctrl Pts',(11.9110398512391,22.01815839942,83.00181349883));
#116877=CARTESIAN_POINT('Ctrl Pts',(12.1362289260491,22.45807851148,82.99170083158));
#116878=CARTESIAN_POINT('Ctrl Pts',(12.3882945132591,23.19862430865,82.793768148027));
#116879=CARTESIAN_POINT('Ctrl Pts',(12.4982137765991,23.77253931309,82.494646053088));
#116880=CARTESIAN_POINT('Ctrl Pts',(12.5268794937091,24.09446043562,82.273684311624));
#116881=CARTESIAN_POINT('Ctrl Pts',(12.5305931541991,24.1473023328,82.236058931096));
#116882=CARTESIAN_POINT('',(12.5172885372655,21.4321684423365,82.2239071870765));
#116883=CARTESIAN_POINT('',(12.6211114714367,23.194984440251,81.5466523813612));
#116884=CARTESIAN_POINT('Ctrl Pts',(12.5172885372655,21.4321684423365,82.2239071870765));
#116885=CARTESIAN_POINT('Ctrl Pts',(12.5342731760867,21.4730660932803,82.2209158140286));
#116886=CARTESIAN_POINT('Ctrl Pts',(12.5505055162535,21.5160946454251,82.216479391709));
#116887=CARTESIAN_POINT('Ctrl Pts',(12.5658342343901,21.5611251493771,82.210418068523));
#116888=CARTESIAN_POINT('Ctrl Pts',(12.5804334410794,21.6040125994993,82.2046452107266));
#116889=CARTESIAN_POINT('Ctrl Pts',(12.5942131719627,21.6487162279354,82.1973985931567));
#116890=CARTESIAN_POINT('Ctrl Pts',(12.6070526543159,21.6950838572293,82.1885421434366));
#116891=CARTESIAN_POINT('Ctrl Pts',(12.6170577467715,21.731215564511,82.181640806152));
#116892=CARTESIAN_POINT('Ctrl Pts',(12.6264921283407,21.7683570037951,82.1737622916675));
#116893=CARTESIAN_POINT('Ctrl Pts',(12.6353019488066,21.8064159145208,82.1648503782335));
#116894=CARTESIAN_POINT('Ctrl Pts',(12.6419587616857,21.8351737136229,82.1581164226036));
#116895=CARTESIAN_POINT('Ctrl Pts',(12.64825458311,21.8644643485648,82.1507925482019));
#116896=CARTESIAN_POINT('Ctrl Pts',(12.6541492093415,21.894240056901,82.1428653077459));
#116897=CARTESIAN_POINT('Ctrl Pts',(12.6624164044795,21.9360003961519,82.1317473774173));
#116898=CARTESIAN_POINT('Ctrl Pts',(12.6698938329058,21.9787150737606,82.1194418905041));
#116899=CARTESIAN_POINT('Ctrl Pts',(12.6764904514613,22.0222859506516,82.1059172229102));
#116900=CARTESIAN_POINT('Ctrl Pts',(12.6821405015729,22.059604712647,82.0943332501509));
#116901=CARTESIAN_POINT('Ctrl Pts',(12.6871406011452,22.0975462801781,82.081857873438));
#116902=CARTESIAN_POINT('Ctrl Pts',(12.6914248518296,22.1360375972392,82.0684949110168));
#116903=CARTESIAN_POINT('Ctrl Pts',(12.6935669771719,22.1552832557698,82.0618134298062));
#116904=CARTESIAN_POINT('Ctrl Pts',(12.6955301256819,22.1746663379845,82.0549103304341));
#116905=CARTESIAN_POINT('Ctrl Pts',(12.697306057862,22.1941777204868,82.0477877712179));
#116906=CARTESIAN_POINT('Ctrl Pts',(12.6981940239521,22.2039334117379,82.0442264916098));
#116907=CARTESIAN_POINT('Ctrl Pts',(12.6990351936357,22.2137211822264,82.0406103594189));
#116908=CARTESIAN_POINT('Ctrl Pts',(12.699828535949,22.2235398957011,82.03693975532));
#116909=CARTESIAN_POINT('Ctrl Pts',(12.7002252071056,22.2284492524385,82.0351044532705));
#116910=CARTESIAN_POINT('Ctrl Pts',(12.7006099219181,22.2333663451915,82.0332555340571));
#116911=CARTESIAN_POINT('Ctrl Pts',(12.7009825534323,22.2382910332833,82.0313930508635));
#116912=CARTESIAN_POINT('Ctrl Pts',(12.7011688691894,22.2407533773292,82.0304618092667));
#116913=CARTESIAN_POINT('Ctrl Pts',(12.7013521641543,22.2432176202277,82.0295271767241));
#116914=CARTESIAN_POINT('Ctrl Pts',(12.701532422489,22.2456837444361,82.0285891603029));
#116915=CARTESIAN_POINT('Ctrl Pts',(12.7017126808237,22.2481498686444,82.0276511438817));
#116916=CARTESIAN_POINT('Ctrl Pts',(12.7019711143474,22.2517695268232,82.0262692122548));
#116917=CARTESIAN_POINT('Ctrl Pts',(12.7020640718486,22.2530877435032,82.0257649667038));
#116918=CARTESIAN_POINT('Ctrl Pts',(12.7037070878608,22.2763871124193,82.0168524690137));
#116919=CARTESIAN_POINT('Ctrl Pts',(12.7051346969877,22.3029829310185,82.0065495121645));
#116920=CARTESIAN_POINT('Ctrl Pts',(12.7061815011432,22.3327077677197,81.9946690642417));
#116921=CARTESIAN_POINT('Ctrl Pts',(12.7072104468936,22.3619255007986,81.9829912959245));
#116922=CARTESIAN_POINT('Ctrl Pts',(12.7078707303876,22.3941672419834,81.9697884885638));
#116923=CARTESIAN_POINT('Ctrl Pts',(12.707973025637,22.4292409366076,81.954868550681));
#116924=CARTESIAN_POINT('Ctrl Pts',(12.7080548403087,22.4572925111177,81.9429357402461));
#116925=CARTESIAN_POINT('Ctrl Pts',(12.7077790066496,22.4871551917192,81.9299040392018));
#116926=CARTESIAN_POINT('Ctrl Pts',(12.7070379455413,22.5187090825413,81.9156747183529));
#116927=CARTESIAN_POINT('Ctrl Pts',(12.7062349330901,22.5529008204859,81.9002558525042));
#116928=CARTESIAN_POINT('Ctrl Pts',(12.7048861036379,22.5890768462464,81.8834317772353));
#116929=CARTESIAN_POINT('Ctrl Pts',(12.702834427738,22.6271006413617,81.8650511210193));
#116930=CARTESIAN_POINT('Ctrl Pts',(12.7006542075314,22.667506753477,81.8455188556689));
#116931=CARTESIAN_POINT('Ctrl Pts',(12.6977134308586,22.7099757493514,81.8242030713352));
#116932=CARTESIAN_POINT('Ctrl Pts',(12.6936892868462,22.7542534992715,81.8011037562274));
#116933=CARTESIAN_POINT('Ctrl Pts',(12.6899832884161,22.7950306859686,81.7798306543551));
#116934=CARTESIAN_POINT('Ctrl Pts',(12.6853581107381,22.8373416451533,81.7570449391417));
#116935=CARTESIAN_POINT('Ctrl Pts',(12.6795926657466,22.8809919056613,81.732779052393));
#116936=CARTESIAN_POINT('Ctrl Pts',(12.673998690671,22.9233439651614,81.7092348566094));
#116937=CARTESIAN_POINT('Ctrl Pts',(12.6673308978515,22.9669565596022,81.6842972397914));
#116938=CARTESIAN_POINT('Ctrl Pts',(12.6594231085505,23.0116601500446,81.6580274464931));
#116939=CARTESIAN_POINT('Ctrl Pts',(12.6517293215199,23.0551539624462,81.6324685719097));
#116940=CARTESIAN_POINT('Ctrl Pts',(12.64286152633,23.0996802668986,81.6056488217044));
#116941=CARTESIAN_POINT('Ctrl Pts',(12.6327052588187,23.145094629419,81.5776535648036));
#116942=CARTESIAN_POINT('Ctrl Pts',(12.6290120242389,23.1616091505153,81.5674733435029));
#116943=CARTESIAN_POINT('Ctrl Pts',(12.6251488006487,23.1782412365338,81.5571379482193));
#116944=CARTESIAN_POINT('Ctrl Pts',(12.6211114714367,23.194984440251,81.5466523813612));
#116945=CARTESIAN_POINT('',(11.9367286423891,21.85927935059,82.709938120253));
#116946=CARTESIAN_POINT('Ctrl Pts',(12.5172885370886,21.4321684424534,82.2239071871077));
#116947=CARTESIAN_POINT('Ctrl Pts',(12.4901986054513,21.4500656883045,82.2286841217066));
#116948=CARTESIAN_POINT('Ctrl Pts',(12.463084003402,21.4681677807312,82.2351093103302));
#116949=CARTESIAN_POINT('Ctrl Pts',(12.436158321932,21.486342887008,82.2432343641709));
#116950=CARTESIAN_POINT('Ctrl Pts',(12.4095744841301,21.5042872453645,82.2512562637717));
#116951=CARTESIAN_POINT('Ctrl Pts',(12.3831754932965,21.5223023630035,82.2609354122807));
#116952=CARTESIAN_POINT('Ctrl Pts',(12.3571761792444,21.5402500104206,82.2722728721136));
#116953=CARTESIAN_POINT('Ctrl Pts',(12.331333296169,21.5580896716037,82.2835421174578));
#116954=CARTESIAN_POINT('Ctrl Pts',(12.3058860226616,21.5758622159077,82.2964498591008));
#116955=CARTESIAN_POINT('Ctrl Pts',(12.2810439524597,21.5934270741106,82.3109460939382));
#116956=CARTESIAN_POINT('Ctrl Pts',(12.2563091655433,21.6109160764899,82.3253797251484));
#116957=CARTESIAN_POINT('Ctrl Pts',(12.2321750779958,21.6281987093121,82.3413879941782));
#116958=CARTESIAN_POINT('Ctrl Pts',(12.2088363986967,21.6451383982326,82.358871396183));
#116959=CARTESIAN_POINT('Ctrl Pts',(12.1976321134016,21.6532706967677,82.3672647170509));
#116960=CARTESIAN_POINT('Ctrl Pts',(12.1866108985648,21.661324033758,82.3759972842875));
#116961=CARTESIAN_POINT('Ctrl Pts',(12.1757925791577,21.6692839648808,82.385054228068));
#116962=CARTESIAN_POINT('Ctrl Pts',(12.1532704744542,21.6858553375157,82.4039094151299));
#116963=CARTESIAN_POINT('Ctrl Pts',(12.1316297125416,21.7020208130826,82.4241729741317));
#116964=CARTESIAN_POINT('Ctrl Pts',(12.1110283811666,21.7176603411047,82.4456798235158));
#116965=CARTESIAN_POINT('Ctrl Pts',(12.0903040996834,21.7333932068644,82.4673150271996));
#116966=CARTESIAN_POINT('Ctrl Pts',(12.0706321574346,21.7485934559033,82.4902077461713));
#116967=CARTESIAN_POINT('Ctrl Pts',(12.0521383030712,21.7631575075447,82.5141551663165));
#116968=CARTESIAN_POINT('Ctrl Pts',(12.0335582924248,21.7777894079174,82.5382141489662));
#116969=CARTESIAN_POINT('Ctrl Pts',(12.016167631061,21.7917789116451,82.5633368727513));
#116970=CARTESIAN_POINT('Ctrl Pts',(12.0000529277821,21.8050445217185,82.5892938730034));
#116971=CARTESIAN_POINT('Ctrl Pts',(11.9837508572241,21.8184643723773,82.6155526779137));
#116972=CARTESIAN_POINT('Ctrl Pts',(11.9687546780973,21.831143241998,82.6426644005985));
#116973=CARTESIAN_POINT('Ctrl Pts',(11.9551095463526,21.8430239972692,82.6703799767414));
#116974=CARTESIAN_POINT('Ctrl Pts',(11.9486802243942,21.8486219791852,82.6834390197483));
#116975=CARTESIAN_POINT('Ctrl Pts',(11.9425502049782,21.8540431752193,82.6966320435008));
#116976=CARTESIAN_POINT('Ctrl Pts',(11.9367208468594,21.8592837631663,82.709932965079));
#116977=CARTESIAN_POINT('Ctrl Pts',(11.9367286423891,21.85927935059,82.709938120253));
#116978=CARTESIAN_POINT('Ctrl Pts',(12.0071900742098,21.9487713614003,82.6799677853506));
#116979=CARTESIAN_POINT('Ctrl Pts',(12.0805141882767,22.0494537651696,82.6349778443183));
#116980=CARTESIAN_POINT('Ctrl Pts',(12.1883057397716,22.213950793166,82.5387148842099));
#116981=CARTESIAN_POINT('Ctrl Pts',(12.2238600590811,22.2709879989896,82.5018176720259));
#116982=CARTESIAN_POINT('Ctrl Pts',(12.2757972429648,22.3591664953451,82.4387235891574));
#116983=CARTESIAN_POINT('Ctrl Pts',(12.3014185157823,22.4039115576769,82.405247458691));
#116984=CARTESIAN_POINT('Ctrl Pts',(12.3305204624122,22.4570972242989,82.3627454175667));
#116985=CARTESIAN_POINT('Ctrl Pts',(12.3428035577651,22.4800826633257,82.3437861552096));
#116986=CARTESIAN_POINT('Ctrl Pts',(12.3509480101634,22.4954467029582,82.3309807498732));
#116987=CARTESIAN_POINT('Ctrl Pts',(12.3542990499949,22.5018085230508,82.325635432429));
#116988=CARTESIAN_POINT('Ctrl Pts',(12.4346388523314,22.6558582457957,82.1945792914));
#116989=CARTESIAN_POINT('Ctrl Pts',(12.4898962985337,22.7845944228403,82.0626293863271));
#116990=CARTESIAN_POINT('Ctrl Pts',(12.5733519052877,23.0108494673222,81.8009014666782));
#116991=CARTESIAN_POINT('Ctrl Pts',(12.6014038389502,23.1090913488287,81.6707965042619));
#116992=CARTESIAN_POINT('Ctrl Pts',(12.6211132020991,23.19498548026,81.546653375664));
#116993=CARTESIAN_POINT('Ctrl Pts',(19.8429432353291,17.66670903096,80.88967894675));
#116994=CARTESIAN_POINT('Ctrl Pts',(20.0692982204291,17.57364273498,80.504253529771));
#116995=CARTESIAN_POINT('Ctrl Pts',(20.5023128070991,17.38259467766,79.684876559745));
#116996=CARTESIAN_POINT('Ctrl Pts',(21.0289682966291,17.11506095695,78.40607475062));
#116997=CARTESIAN_POINT('Ctrl Pts',(21.4337450075691,16.87634404777,77.091691432304));
#116998=CARTESIAN_POINT('Ctrl Pts',(21.7264515133391,16.6689476013,75.737023720658));
#116999=CARTESIAN_POINT('Ctrl Pts',(21.9058894958591,16.49221282193,74.267914636433));
#117000=CARTESIAN_POINT('Ctrl Pts',(21.9436945982691,16.36324862353,72.7108971134944));
#117001=CARTESIAN_POINT('Ctrl Pts',(21.8274598255191,16.29549033631,71.134112925171));
#117002=CARTESIAN_POINT('Ctrl Pts',(21.5557051837891,16.29308032823,69.560465808041));
#117003=CARTESIAN_POINT('Ctrl Pts',(21.1189566322091,16.35954526088,67.982905962895));
#117004=CARTESIAN_POINT('Ctrl Pts',(20.6097838163291,16.47512090179,66.682075896747));
#117005=CARTESIAN_POINT('Ctrl Pts',(20.2389056685491,16.57078829643,65.920640579465));
#117006=CARTESIAN_POINT('Ctrl Pts',(20.1031948314991,16.60676833735,65.660578297905));
#117007=CARTESIAN_POINT('Ctrl Pts',(15.9217651634291,18.86023850409,78.8653534140521));
#117008=CARTESIAN_POINT('Ctrl Pts',(16.0904271054691,18.7673148555,78.591765890084));
#117009=CARTESIAN_POINT('Ctrl Pts',(16.4154187039391,18.57712863705,78.005939013225));
#117010=CARTESIAN_POINT('Ctrl Pts',(16.8157392045791,18.31228006428,77.079624029397));
#117011=CARTESIAN_POINT('Ctrl Pts',(17.1269628424391,18.07701240892,76.117836928949));
#117012=CARTESIAN_POINT('Ctrl Pts',(17.3548149996891,17.87334248467,75.11896421969));
#117013=CARTESIAN_POINT('Ctrl Pts',(17.4975479419891,17.70032472588,74.028850771698));
#117014=CARTESIAN_POINT('Ctrl Pts',(17.5323952584791,17.57438021074,72.868074785256));
#117015=CARTESIAN_POINT('Ctrl Pts',(17.4489288771991,17.50830697097,71.6894403714931));
#117016=CARTESIAN_POINT('Ctrl Pts',(17.2457919781591,17.50595826264,70.512431280761));
#117017=CARTESIAN_POINT('Ctrl Pts',(16.9161419351691,17.57076519201,69.334239814392));
#117018=CARTESIAN_POINT('Ctrl Pts',(16.5309101724491,17.68362893957,68.366455266264));
#117019=CARTESIAN_POINT('Ctrl Pts',(16.2506832159191,17.77725583824,67.8027331628201));
#117020=CARTESIAN_POINT('Ctrl Pts',(16.1482365562791,17.81250084465,67.610590819165));
#117021=CARTESIAN_POINT('Ctrl Pts',(13.7245240389691,22.48149564395,77.145847903068));
#117022=CARTESIAN_POINT('Ctrl Pts',(13.8434718950791,22.38900479815,76.936687900911));
#117023=CARTESIAN_POINT('Ctrl Pts',(14.0698770466191,22.2014334629,76.494081975836));
#117024=CARTESIAN_POINT('Ctrl Pts',(14.3427852808591,21.94473182854,75.809156314966));
#117025=CARTESIAN_POINT('Ctrl Pts',(14.5508108918891,21.71992946569,75.109894854898));
#117026=CARTESIAN_POINT('Ctrl Pts',(14.6998789996491,21.52756608686,74.392905753835));
#117027=CARTESIAN_POINT('Ctrl Pts',(14.7897760814891,21.3658260448,73.6186841310744));
#117028=CARTESIAN_POINT('Ctrl Pts',(14.8063911950091,21.24904347311,72.8007794935411));
#117029=CARTESIAN_POINT('Ctrl Pts',(14.7437806796791,21.18808279255,71.974011411747));
#117030=CARTESIAN_POINT('Ctrl Pts',(14.6012904929691,21.18592007224,71.149238564271));
#117031=CARTESIAN_POINT('Ctrl Pts',(14.3738366030991,21.24569649639,70.321565846831));
#117032=CARTESIAN_POINT('Ctrl Pts',(14.1091114755891,21.35033215796,69.63726307722));
#117033=CARTESIAN_POINT('Ctrl Pts',(13.9161056624891,21.43776804022,69.235362518137));
#117034=CARTESIAN_POINT('Ctrl Pts',(13.8454360114391,21.47078289727,69.0979054154141));
#117035=CARTESIAN_POINT('Ctrl Pts',(14.1931489316191,26.97809399155,76.468292357438));
#117036=CARTESIAN_POINT('Ctrl Pts',(14.2916734495191,26.88614056693,76.248530254187));
#117037=CARTESIAN_POINT('Ctrl Pts',(14.4711914398691,26.70181619234,75.797419155646));
#117038=CARTESIAN_POINT('Ctrl Pts',(14.6702301335491,26.45523079894,75.13930481074));
#117039=CARTESIAN_POINT('Ctrl Pts',(14.8096524336191,26.2434234307,74.49995704091));
#117040=CARTESIAN_POINT('Ctrl Pts',(14.8997805017791,26.06509964957,73.870100268841));
#117041=CARTESIAN_POINT('Ctrl Pts',(14.9433609581991,25.91736340798,73.2132478891327));
#117042=CARTESIAN_POINT('Ctrl Pts',(14.9342853630891,25.81195743237,72.5378598662094));
#117043=CARTESIAN_POINT('Ctrl Pts',(14.8716775461091,25.75734513428,71.865834093289));
#117044=CARTESIAN_POINT('Ctrl Pts',(14.7558645741991,25.75541335958,71.197896549204));
#117045=CARTESIAN_POINT('Ctrl Pts',(14.5818943027391,25.8089432896,70.521630061898));
#117046=CARTESIAN_POINT('Ctrl Pts',(14.3825817446091,25.90336194739,69.949720331184));
#117047=CARTESIAN_POINT('Ctrl Pts',(14.2359764423691,25.98311030206,69.604378827809));
#117048=CARTESIAN_POINT('Ctrl Pts',(14.1819742353591,26.0133559313,69.484929408113));
#117049=CARTESIAN_POINT('',(15.6158099654941,20.1981134279197,68.3761656716912));
#117050=CARTESIAN_POINT('Origin',(22.9325826401891,25.68032358419,65.795421779755));
#117051=CARTESIAN_POINT('',(15.9984184148119,20.3875458432315,78.383019919252));
#117052=CARTESIAN_POINT('Ctrl Pts',(15.6158091070711,20.1981127933161,68.3761659747572));
#117053=CARTESIAN_POINT('Ctrl Pts',(16.2185010787615,20.1430815615197,69.9680357680762));
#117054=CARTESIAN_POINT('Ctrl Pts',(16.560638794584,20.1332273419861,71.64811321169));
#117055=CARTESIAN_POINT('Ctrl Pts',(16.7005936251506,20.218545920064,75.1663223132348));
#117056=CARTESIAN_POINT('Ctrl Pts',(16.4573509577271,20.3124614378109,76.8746944962966));
#117057=CARTESIAN_POINT('Ctrl Pts',(15.9984175514895,20.387544970039,78.3830197000386));
#117058=CARTESIAN_POINT('Origin',(22.9324069483482,26.6270131840282,80.1828101714809));
#117059=CARTESIAN_POINT('Origin',(17.7894674803291,1.4210854715202E-14,
100.88908350184));
#117060=CARTESIAN_POINT('',(18.9921123831974,17.0122606549803,65.8508016863977));
#117061=CARTESIAN_POINT('Origin',(11.8338327653321,1.4210854715202E-14,
67.1130006183879));
#117062=CARTESIAN_POINT('',(15.2821042656531,17.8079467178956,57.8022951133291));
#117063=CARTESIAN_POINT('Ctrl Pts',(18.9921123831974,17.0122606549803,65.8508016863977));
#117064=CARTESIAN_POINT('Ctrl Pts',(18.8584828352797,17.0408671426352,65.4783085652489));
#117065=CARTESIAN_POINT('Ctrl Pts',(18.7209892451032,17.0708101915551,65.1082362936578));
#117066=CARTESIAN_POINT('Ctrl Pts',(18.5796489012198,17.101896657633,64.7405625793287));
#117067=CARTESIAN_POINT('Ctrl Pts',(18.4320707453025,17.1343550712161,64.3566622204565));
#117068=CARTESIAN_POINT('Ctrl Pts',(18.2802986847668,17.1680604374422,63.9753763743597));
#117069=CARTESIAN_POINT('Ctrl Pts',(18.1243308189613,17.2027999736258,63.596735420507));
#117070=CARTESIAN_POINT('Ctrl Pts',(17.9683629531559,17.2375395098094,63.2180944666542));
#117071=CARTESIAN_POINT('Ctrl Pts',(17.8081990244202,17.2733136613848,62.842098371325));
#117072=CARTESIAN_POINT('Ctrl Pts',(17.6438191240194,17.3099101632158,62.4688350059709));
#117073=CARTESIAN_POINT('Ctrl Pts',(17.4791788661025,17.3465646293981,62.09498043742));
#117074=CARTESIAN_POINT('Ctrl Pts',(17.3103091873621,17.3840443729146,61.7238679103735));
#117075=CARTESIAN_POINT('Ctrl Pts',(17.1371257413606,17.422108587588,61.3554290200356));
#117076=CARTESIAN_POINT('Ctrl Pts',(16.9636788689392,17.4602307010967,60.986429703513));
#117077=CARTESIAN_POINT('Ctrl Pts',(16.7859049271392,17.4989395052665,60.620112265243));
#117078=CARTESIAN_POINT('Ctrl Pts',(16.6037058990406,17.5379817897613,60.2564573874014));
#117079=CARTESIAN_POINT('Ctrl Pts',(16.422299248806,17.5768542805842,59.8943840332285));
#117080=CARTESIAN_POINT('Ctrl Pts',(16.2365057539938,17.6160577681685,59.5349502630608));
#117081=CARTESIAN_POINT('Ctrl Pts',(16.0462180137517,17.65532478812,59.1781841243065));
#117082=CARTESIAN_POINT('Ctrl Pts',(15.8632233084799,17.6930868464312,58.8350915302737));
#117083=CARTESIAN_POINT('Ctrl Pts',(15.6760720768127,17.730907883019,58.4944663422677));
#117084=CARTESIAN_POINT('Ctrl Pts',(15.4846614635924,17.7685293574614,58.1563733471083));
#117085=CARTESIAN_POINT('Ctrl Pts',(15.4176654200366,17.7816973312637,58.0380366851618));
#117086=CARTESIAN_POINT('Ctrl Pts',(15.3501475082489,17.7948406501483,57.9200105893426));
#117087=CARTESIAN_POINT('Ctrl Pts',(15.2821042656531,17.8079467178956,57.8022951133291));
#117088=CARTESIAN_POINT('Ctrl Pts',(19.1777532421465,16.3235298342272,58.6272695410447));
#117089=CARTESIAN_POINT('Ctrl Pts',(18.9453611592213,16.4404319258409,58.5715817835269));
#117090=CARTESIAN_POINT('Ctrl Pts',(18.7156139825874,16.5504510635377,58.5177831660704));
#117091=CARTESIAN_POINT('Ctrl Pts',(18.4889489462576,16.6540581469211,58.4658115211243));
#117092=CARTESIAN_POINT('Ctrl Pts',(18.2590018284741,16.7591654479487,58.4130873332418));
#117093=CARTESIAN_POINT('Ctrl Pts',(18.0322266560163,16.8576739887225,58.3622434270875));
#117094=CARTESIAN_POINT('Ctrl Pts',(17.8090267987014,16.9500767735686,58.3132242642099));
#117095=CARTESIAN_POINT('Ctrl Pts',(17.5806932957228,17.0446048427291,58.2630776498368));
#117096=CARTESIAN_POINT('Ctrl Pts',(17.3561014070839,17.1327433971003,58.2148406933092));
#117097=CARTESIAN_POINT('Ctrl Pts',(17.135628872468,17.2150165121611,58.1684634758667));
#117098=CARTESIAN_POINT('Ctrl Pts',(16.9124418330387,17.2983025913412,58.1215152522433));
#117099=CARTESIAN_POINT('Ctrl Pts',(16.6934760271185,17.3755782319407,58.0764728766697));
#117100=CARTESIAN_POINT('Ctrl Pts',(16.4790704722335,17.4473782663621,58.0332938821258));
#117101=CARTESIAN_POINT('Ctrl Pts',(16.2603714273099,17.5206161027693,57.9892502244296));
#117102=CARTESIAN_POINT('Ctrl Pts',(16.0464169541269,17.5881571707185,57.9471453496133));
#117103=CARTESIAN_POINT('Ctrl Pts',(15.8375146169777,17.6505548979763,57.9069433976324));
#117104=CARTESIAN_POINT('Ctrl Pts',(15.6481633096011,17.7071128637455,57.8705039194027));
#117105=CARTESIAN_POINT('Ctrl Pts',(15.4629619198439,17.7594451174825,57.8356279892979));
#117106=CARTESIAN_POINT('Ctrl Pts',(15.2821054022649,17.807950818201,57.8022949128784));
#117107=CARTESIAN_POINT('Origin',(18.4825956495891,15.00000121252,58.74984482171));
#117108=CARTESIAN_POINT('',(18.87832452956,15.0000021622099,57.3029855895947));
#117109=CARTESIAN_POINT('Origin',(18.4825952511691,15.00000123316,58.74984256216));
#117110=CARTESIAN_POINT('Origin',(18.4825924316391,15.00000208393,58.74984406621));
#117111=CARTESIAN_POINT('Origin',(24.2283495281091,17.,82.697478608263));
#117112=CARTESIAN_POINT('',(21.1895064189391,9.5,65.4633429305539));
#117113=CARTESIAN_POINT('',(21.1895064189391,17.,65.4633429305539));
#117114=CARTESIAN_POINT('',(19.9598075156051,9.54868022077971,58.4893745818179));
#117115=CARTESIAN_POINT('',(19.9598072163191,15.00000057102,58.48937219914));
#117116=CARTESIAN_POINT('',(20.0012895471991,9.5,58.72463018868));
#117117=CARTESIAN_POINT('Origin',(19.9938181733183,9.83076353882643,58.6822579212327));
#117118=CARTESIAN_POINT('',(24.2283495281091,9.5,82.697478608263));
#117119=CARTESIAN_POINT('Ctrl Pts',(18.5989684124291,9.99292997789002,57.25761225601));
#117120=CARTESIAN_POINT('Ctrl Pts',(18.6222625186891,9.92394001275902,57.26454489492));
#117121=CARTESIAN_POINT('Ctrl Pts',(18.6746819394891,9.75907899964801,57.29185528042));
#117122=CARTESIAN_POINT('Ctrl Pts',(18.7402509692591,9.51839895443402,57.3713825578401));
#117123=CARTESIAN_POINT('Ctrl Pts',(18.7909229819691,9.28449495434002,57.49585505039));
#117124=CARTESIAN_POINT('Ctrl Pts',(18.8206195909491,9.09361539184202,57.63791449765));
#117125=CARTESIAN_POINT('Ctrl Pts',(18.8336214569991,8.94122220603702,57.78727492797));
#117126=CARTESIAN_POINT('Ctrl Pts',(18.8336610801191,8.82264484939901,57.93631838649));
#117127=CARTESIAN_POINT('Ctrl Pts',(18.8241401371591,8.73276899790502,58.07983530743));
#117128=CARTESIAN_POINT('Ctrl Pts',(18.8079424561291,8.66610608857702,58.21541004732));
#117129=CARTESIAN_POINT('Ctrl Pts',(18.7872031755891,8.61777448570702,58.34273076413));
#117130=CARTESIAN_POINT('Ctrl Pts',(18.7709241463591,8.59460757857502,58.4247208402));
#117131=CARTESIAN_POINT('Ctrl Pts',(18.7624724636291,8.58514829630202,58.46435199577));
#117132=CARTESIAN_POINT('Ctrl Pts',(19.1654129070991,10.56056596522,57.24431313358));
#117133=CARTESIAN_POINT('Ctrl Pts',(19.1935754232291,10.48544979949,57.22567128383));
#117134=CARTESIAN_POINT('Ctrl Pts',(19.2603011303891,10.29996486048,57.19274799569));
#117135=CARTESIAN_POINT('Ctrl Pts',(19.3536368863391,10.00561091375,57.18966955586));
#117136=CARTESIAN_POINT('Ctrl Pts',(19.4379237982291,9.69047600408601,57.24547446787));
#117137=CARTESIAN_POINT('Ctrl Pts',(19.5003292194691,9.40799131016201,57.34649268402));
#117138=CARTESIAN_POINT('Ctrl Pts',(19.5434774508091,9.16014843910101,57.48118063348));
#117139=CARTESIAN_POINT('Ctrl Pts',(19.5697672879791,8.94773680058601,57.63993508744));
#117140=CARTESIAN_POINT('Ctrl Pts',(19.5814446261691,8.77008394202101,57.81469108227));
#117141=CARTESIAN_POINT('Ctrl Pts',(19.5805345073391,8.62473681342901,57.99968336702));
#117142=CARTESIAN_POINT('Ctrl Pts',(19.5684896165591,8.50880607634101,58.1914376917));
#117143=CARTESIAN_POINT('Ctrl Pts',(19.5532261047991,8.44806080916502,58.32574241798));
#117144=CARTESIAN_POINT('Ctrl Pts',(19.5439231135291,8.42241936143501,58.39293424589));
#117145=CARTESIAN_POINT('Ctrl Pts',(19.4392357106891,10.92141167485,57.90603676144));
#117146=CARTESIAN_POINT('Ctrl Pts',(19.4699542803791,10.87379705862,57.87087569833));
#117147=CARTESIAN_POINT('Ctrl Pts',(19.5462693720491,10.75026038072,57.79424981718));
#117148=CARTESIAN_POINT('Ctrl Pts',(19.6642017406291,10.53149760247,57.71309988849));
#117149=CARTESIAN_POINT('Ctrl Pts',(19.7840987440191,10.27151168125,57.6793926310801));
#117150=CARTESIAN_POINT('Ctrl Pts',(19.8855888519391,10.01808188889,57.69883695166));
#117151=CARTESIAN_POINT('Ctrl Pts',(19.9685932208391,9.77937666711901,57.763832807));
#117152=CARTESIAN_POINT('Ctrl Pts',(20.0333327084191,9.56174852794401,57.86707398515));
#117153=CARTESIAN_POINT('Ctrl Pts',(20.0802536347391,9.369648419902,58.00118585982));
#117154=CARTESIAN_POINT('Ctrl Pts',(20.1101332724391,9.2050307565,58.15955190861));
#117155=CARTESIAN_POINT('Ctrl Pts',(20.1236001164291,9.068480502455,58.33700345402));
#117156=CARTESIAN_POINT('Ctrl Pts',(20.1217629015091,8.99459062150501,58.46851211914));
#117157=CARTESIAN_POINT('Ctrl Pts',(20.1180160422391,8.963053782842,58.5356858368));
#117158=CARTESIAN_POINT('Ctrl Pts',(19.1716240193791,10.74757975927,58.64149899143));
#117159=CARTESIAN_POINT('Ctrl Pts',(19.2002636935791,10.73610478672,58.6138843975));
#117160=CARTESIAN_POINT('Ctrl Pts',(19.2727377436391,10.70079842939,58.54979795779));
#117161=CARTESIAN_POINT('Ctrl Pts',(19.3897465656791,10.6182049493,58.46605148569));
#117162=CARTESIAN_POINT('Ctrl Pts',(19.5148912603391,10.4996360383,58.40332391661));
#117163=CARTESIAN_POINT('Ctrl Pts',(19.6263270987591,10.36952005018,58.37478490362));
#117164=CARTESIAN_POINT('Ctrl Pts',(19.7226815576091,10.23623676329,58.37839571799));
#117165=CARTESIAN_POINT('Ctrl Pts',(19.8031323356991,10.10674994874,58.41134223997));
#117166=CARTESIAN_POINT('Ctrl Pts',(19.8673175928291,9.98666003797102,58.46985863138));
#117167=CARTESIAN_POINT('Ctrl Pts',(19.9155116515791,9.87969595699702,58.54974895378));
#117168=CARTESIAN_POINT('Ctrl Pts',(19.9481259915791,9.78824200696503,58.64715774711));
#117169=CARTESIAN_POINT('Ctrl Pts',(19.9599258661791,9.73758529007002,58.72330031862));
#117170=CARTESIAN_POINT('Ctrl Pts',(19.9630939247691,9.71579676191702,58.76289359955));
#117171=CARTESIAN_POINT('',(18.8782362963603,10.0000000055723,57.3029603857805));
#117172=CARTESIAN_POINT('Ctrl Pts',(18.8783268084662,9.99999999999988,57.3029850932652));
#117173=CARTESIAN_POINT('Ctrl Pts',(18.9208387324483,9.98511016261138,57.3146419262317));
#117174=CARTESIAN_POINT('Ctrl Pts',(18.9623037038507,9.97062352280902,57.3279940735751));
#117175=CARTESIAN_POINT('Ctrl Pts',(19.002593961926,9.95647282485062,57.3428781052431));
#117176=CARTESIAN_POINT('Ctrl Pts',(19.0432887126542,9.9421800614493,57.3579115646324));
#117177=CARTESIAN_POINT('Ctrl Pts',(19.082784869332,9.92822962541205,57.3745069335272));
#117178=CARTESIAN_POINT('Ctrl Pts',(19.1209943308262,9.91457522331445,57.3924755789189));
#117179=CARTESIAN_POINT('Ctrl Pts',(19.1317186250454,9.91074282631757,57.3975188596239));
#117180=CARTESIAN_POINT('Ctrl Pts',(19.1423418240855,9.90693390618994,57.4026702453094));
#117181=CARTESIAN_POINT('Ctrl Pts',(19.1528625920286,9.90314781642201,57.4079254265304));
#117182=CARTESIAN_POINT('Ctrl Pts',(19.1910683050448,9.88939879544672,57.4270093894752));
#117183=CARTESIAN_POINT('Ctrl Pts',(19.2279196888839,9.87594969708246,57.4474595822681));
#117184=CARTESIAN_POINT('Ctrl Pts',(19.2633601514774,9.86288426186219,57.4690647053599));
#117185=CARTESIAN_POINT('Ctrl Pts',(19.2879038683567,9.8538360068597,57.4840269825285));
#117186=CARTESIAN_POINT('Ctrl Pts',(19.3117719511216,9.84497216265779,57.4995438337743));
#117187=CARTESIAN_POINT('Ctrl Pts',(19.3349570005266,9.83632379875053,57.5155533891061));
#117188=CARTESIAN_POINT('Ctrl Pts',(19.3504611502475,9.83054052322165,57.5262591908706));
#117189=CARTESIAN_POINT('Ctrl Pts',(19.3656621190298,9.82483923989344,57.5371869700974));
#117190=CARTESIAN_POINT('Ctrl Pts',(19.3805545544829,9.81921869377156,57.5483160349634));
#117191=CARTESIAN_POINT('Ctrl Pts',(19.4145014659596,9.8064068080158,57.5736844430398));
#117192=CARTESIAN_POINT('Ctrl Pts',(19.4468420661731,9.79401353306645,57.6000969576853));
#117193=CARTESIAN_POINT('Ctrl Pts',(19.4775552412542,9.78202389464304,57.6273208358166));
#117194=CARTESIAN_POINT('Ctrl Pts',(19.5077497374716,9.7702367351889,57.6540849617362));
#117195=CARTESIAN_POINT('Ctrl Pts',(19.5363719187633,9.75884011241947,57.6816332563403));
#117196=CARTESIAN_POINT('Ctrl Pts',(19.563444322055,9.74782565388447,57.7097684917865));
#117197=CARTESIAN_POINT('Ctrl Pts',(19.5924501923908,9.73602456062194,57.7399131000219));
#117198=CARTESIAN_POINT('Ctrl Pts',(19.6196776011776,9.72466241231091,57.7707303908133));
#117199=CARTESIAN_POINT('Ctrl Pts',(19.645181703832,9.71377420667168,57.8020131219249));
#117200=CARTESIAN_POINT('Ctrl Pts',(19.6509595334378,9.71130753698532,57.8091000715193));
#117201=CARTESIAN_POINT('Ctrl Pts',(19.6566490582282,9.70886518326726,57.816211069799));
#117202=CARTESIAN_POINT('Ctrl Pts',(19.6622511520499,9.70644752473145,57.823343979969));
#117203=CARTESIAN_POINT('Ctrl Pts',(19.6773116371737,9.69994797089116,57.8425198615096));
#117204=CARTESIAN_POINT('Ctrl Pts',(19.6917339583362,9.69361877354101,57.8618463008517));
#117205=CARTESIAN_POINT('Ctrl Pts',(19.7055337051702,9.68745455567342,57.8812762234864));
#117206=CARTESIAN_POINT('Ctrl Pts',(19.7284229573522,9.67723014076388,57.913504090013));
#117207=CARTESIAN_POINT('Ctrl Pts',(19.7495978658298,9.6674605475487,57.9460143695294));
#117208=CARTESIAN_POINT('Ctrl Pts',(19.7691396514823,9.65815512299354,57.9786127487493));
#117209=CARTESIAN_POINT('Ctrl Pts',(19.7845013999463,9.65084015219668,58.0042382525192));
#117210=CARTESIAN_POINT('Ctrl Pts',(19.7988547861705,9.64381178723341,58.0299190632408));
#117211=CARTESIAN_POINT('Ctrl Pts',(19.8122520110905,9.63706604159557,58.055577334875));
#117212=CARTESIAN_POINT('Ctrl Pts',(19.8293686065232,9.6284475254727,58.0883589189483));
#117213=CARTESIAN_POINT('Ctrl Pts',(19.8449239825892,9.62029165568125,58.1211021915863));
#117214=CARTESIAN_POINT('Ctrl Pts',(19.8590233443336,9.61261841013919,58.1536519928569));
#117215=CARTESIAN_POINT('Ctrl Pts',(19.8695982291186,9.60686327816901,58.1780651829325));
#117216=CARTESIAN_POINT('Ctrl Pts',(19.8793545690103,9.60137903712872,58.202370450052));
#117217=CARTESIAN_POINT('Ctrl Pts',(19.8883433273238,9.59616278333,58.2265163526361));
#117218=CARTESIAN_POINT('Ctrl Pts',(19.9001508647372,9.58931076776362,58.2582341537162));
#117219=CARTESIAN_POINT('Ctrl Pts',(19.9106335214388,9.58292271136002,58.2896751695036));
#117220=CARTESIAN_POINT('Ctrl Pts',(19.9199000760921,9.57700602057025,58.3207104461368));
#117221=CARTESIAN_POINT('Ctrl Pts',(19.9269921362974,9.57247774346322,58.3444629689037));
#117222=CARTESIAN_POINT('Ctrl Pts',(19.9333722047035,9.56822479168832,58.3679787526273));
#117223=CARTESIAN_POINT('Ctrl Pts',(19.9390931750267,9.56423707813824,58.3912149749821));
#117224=CARTESIAN_POINT('Ctrl Pts',(19.9463972232821,9.55914590469158,58.4208810071001));
#117225=CARTESIAN_POINT('Ctrl Pts',(19.9526268159925,9.55448824756716,58.4500894277211));
#117226=CARTESIAN_POINT('Ctrl Pts',(19.9578906509278,9.55024207996741,58.4787308390512));
#117227=CARTESIAN_POINT('Ctrl Pts',(19.9585443021874,9.54971480036342,58.4822874655076));
#117228=CARTESIAN_POINT('Ctrl Pts',(19.9591830680236,9.54919382674418,58.4858354008373));
#117229=CARTESIAN_POINT('Ctrl Pts',(19.9598071616935,9.54867908433721,58.4893744789377));
#117230=CARTESIAN_POINT('',(19.0913779940088,8.6460405135737,58.2486549879977));
#117231=CARTESIAN_POINT('Ctrl Pts',(19.0913780598671,8.64604000277229,58.2486547535097));
#117232=CARTESIAN_POINT('Ctrl Pts',(19.0954302009912,8.66285126361277,58.213171559027));
#117233=CARTESIAN_POINT('Ctrl Pts',(19.0988408317573,8.68159370027269,58.176982504357));
#117234=CARTESIAN_POINT('Ctrl Pts',(19.1015351597539,8.70248101758052,58.1403385759788));
#117235=CARTESIAN_POINT('Ctrl Pts',(19.1041640143191,8.72286076330142,58.1045851122115));
#117236=CARTESIAN_POINT('Ctrl Pts',(19.1061109304425,8.74528295029375,58.0683986435903));
#117237=CARTESIAN_POINT('Ctrl Pts',(19.1072942385465,8.76992764012634,58.0320567084334));
#117238=CARTESIAN_POINT('Ctrl Pts',(19.1084368662561,8.79372508172332,57.9969641556242));
#117239=CARTESIAN_POINT('Ctrl Pts',(19.1088674197003,8.81959529261079,57.9617268250813));
#117240=CARTESIAN_POINT('Ctrl Pts',(19.1085015617408,8.8476758943756,57.9266348400689));
#117241=CARTESIAN_POINT('Ctrl Pts',(19.1081426901077,8.87522027642978,57.8922129622787));
#117242=CARTESIAN_POINT('Ctrl Pts',(19.1070174722854,8.90489192584823,57.8579310879301));
#117243=CARTESIAN_POINT('Ctrl Pts',(19.1050366211492,8.93678978933392,57.8241001163336));
#117244=CARTESIAN_POINT('Ctrl Pts',(19.1031111812215,8.96779536004109,57.7912155131877));
#117245=CARTESIAN_POINT('Ctrl Pts',(19.1003772169515,9.00090472545617,57.7587572142995));
#117246=CARTESIAN_POINT('Ctrl Pts',(19.096744615821,9.03617293713031,57.727042886517));
#117247=CARTESIAN_POINT('Ctrl Pts',(19.0943428289093,9.05949141503571,57.7060741496127));
#117248=CARTESIAN_POINT('Ctrl Pts',(19.0915480345517,9.08375290262299,57.685431298777));
#117249=CARTESIAN_POINT('Ctrl Pts',(19.0883324721565,9.10896303915117,57.665213240763));
#117250=CARTESIAN_POINT('Ctrl Pts',(19.0836454651811,9.14570935946355,57.6357433791046));
#117251=CARTESIAN_POINT('Ctrl Pts',(19.0780646694153,9.18447336932474,57.6071751849723));
#117252=CARTESIAN_POINT('Ctrl Pts',(19.0714997588372,9.2252361160707,57.5798340720463));
#117253=CARTESIAN_POINT('Ctrl Pts',(19.0650441419727,9.26532023788887,57.5529481384756));
#117254=CARTESIAN_POINT('Ctrl Pts',(19.057636789312,9.30733741658159,57.5272491409521));
#117255=CARTESIAN_POINT('Ctrl Pts',(19.0491882101566,9.35122280768896,57.5030640999627));
#117256=CARTESIAN_POINT('Ctrl Pts',(19.0409254270953,9.39414309755229,57.4794109219136));
#117257=CARTESIAN_POINT('Ctrl Pts',(19.0316665837391,9.43885053921676,57.457206268645));
#117258=CARTESIAN_POINT('Ctrl Pts',(19.021326269496,9.48523556076868,57.4367671620351));
#117259=CARTESIAN_POINT('Ctrl Pts',(19.0198671000966,9.49178116493962,57.4338829055015));
#117260=CARTESIAN_POINT('Ctrl Pts',(19.0183863940477,9.4983600912586,57.4310338190697));
#117261=CARTESIAN_POINT('Ctrl Pts',(19.0168839108807,9.50497194766504,57.4282208040115));
#117262=CARTESIAN_POINT('Ctrl Pts',(19.0065288051913,9.5505408255026,57.4088335197662));
#117263=CARTESIAN_POINT('Ctrl Pts',(18.9951392061905,9.59767797885603,57.3911594931486));
#117264=CARTESIAN_POINT('Ctrl Pts',(18.9826423348366,9.64622838184959,57.3754959660479));
#117265=CARTESIAN_POINT('Ctrl Pts',(18.970337340225,9.6940333428125,57.3600729364658));
#117266=CARTESIAN_POINT('Ctrl Pts',(18.9569586843622,9.74320860365135,57.3465995994608));
#117267=CARTESIAN_POINT('Ctrl Pts',(18.9424390835605,9.79355619944309,57.3353571391542));
#117268=CARTESIAN_POINT('Ctrl Pts',(18.9282301475949,9.84282654608677,57.3243552252052));
#117269=CARTESIAN_POINT('Ctrl Pts',(18.9129284431077,9.89321958803115,57.3154902019306));
#117270=CARTESIAN_POINT('Ctrl Pts',(18.8964748979544,9.9445008817099,57.309016397297));
#117271=CARTESIAN_POINT('Ctrl Pts',(18.8905744661776,9.96289094731345,57.3066948160073));
#117272=CARTESIAN_POINT('Ctrl Pts',(18.8845259520051,9.98139478071069,57.3046806302731));
#117273=CARTESIAN_POINT('Ctrl Pts',(18.8783268084,10.,57.3029850935068));
#117274=CARTESIAN_POINT('Origin',(18.9749992656191,9.54868042581501,58.66301925565));
#117275=CARTESIAN_POINT('Ctrl Pts',(18.5706725300191,8.81765680955601,58.08301260777));
#117276=CARTESIAN_POINT('Ctrl Pts',(18.5857598980191,8.75765050426302,58.16857732362));
#117277=CARTESIAN_POINT('Ctrl Pts',(18.6277718770991,8.62602790954801,58.40683909675));
#117278=CARTESIAN_POINT('Ctrl Pts',(18.6885460064291,8.54234388419301,58.75150631155));
#117279=CARTESIAN_POINT('Ctrl Pts',(18.7326364903191,8.543692731993,59.00155587124));
#117280=CARTESIAN_POINT('Ctrl Pts',(18.7479295693691,8.55159287998601,59.0882872324));
#117281=CARTESIAN_POINT('Ctrl Pts',(19.4066515538591,8.59303798548101,57.77801712375));
#117282=CARTESIAN_POINT('Ctrl Pts',(19.4244719901391,8.52216007648402,57.87908184005));
#117283=CARTESIAN_POINT('Ctrl Pts',(19.4740138287791,8.36702838946302,58.16004756881));
#117284=CARTESIAN_POINT('Ctrl Pts',(19.5454018805591,8.26883637037401,58.56490932905));
#117285=CARTESIAN_POINT('Ctrl Pts',(19.5971457817591,8.27039928348501,58.85836357521));
#117286=CARTESIAN_POINT('Ctrl Pts',(19.6150981880091,8.27967362318701,58.96017673036));
#117287=CARTESIAN_POINT('Ctrl Pts',(20.1098257338891,9.12697886077701,58.02863494815));
#117288=CARTESIAN_POINT('Ctrl Pts',(20.1211494000291,9.08194381522401,58.09285465006));
#117289=CARTESIAN_POINT('Ctrl Pts',(20.1527920273191,8.98269553590501,58.27230890692));
#117290=CARTESIAN_POINT('Ctrl Pts',(20.1989497491491,8.91899043439601,58.53408235561));
#117291=CARTESIAN_POINT('Ctrl Pts',(20.2325007301691,8.92004449336401,58.72435942426));
#117292=CARTESIAN_POINT('Ctrl Pts',(20.2441316560191,8.92605224520602,58.79032168259));
#117293=CARTESIAN_POINT('Ctrl Pts',(19.9274540441491,9.84790099344701,58.5665821712));
#117294=CARTESIAN_POINT('Ctrl Pts',(19.9300058300991,9.83775874799601,58.58105406848));
#117295=CARTESIAN_POINT('Ctrl Pts',(19.9374811043791,9.81396373949001,58.62344845562));
#117296=CARTESIAN_POINT('Ctrl Pts',(19.9495730632891,9.79682256166901,58.69202536232));
#117297=CARTESIAN_POINT('Ctrl Pts',(19.9585601282791,9.79718957038302,58.74299354062));
#117298=CARTESIAN_POINT('Ctrl Pts',(19.9616558485791,9.79878680488901,58.76055024285));
#117299=CARTESIAN_POINT('',(19.0165386378691,8.5,58.89829442788));
#117300=CARTESIAN_POINT('Ctrl Pts',(19.0165386378691,8.5,58.89829442788));
#117301=CARTESIAN_POINT('Ctrl Pts',(19.032697313698,8.50000152435189,58.758360191488));
#117302=CARTESIAN_POINT('Ctrl Pts',(19.0473582025624,8.51918644290929,58.632939395879));
#117303=CARTESIAN_POINT('Ctrl Pts',(19.0723610486273,8.5742843133173,58.416069360015));
#117304=CARTESIAN_POINT('Ctrl Pts',(19.0827530892467,8.61013548696591,58.3244461106695));
#117305=CARTESIAN_POINT('Ctrl Pts',(19.0913779610791,8.64604076897401,58.24865510524));
#117306=CARTESIAN_POINT('Ctrl Pts',(19.0165386356542,8.50002857532344,58.8982944240715));
#117307=CARTESIAN_POINT('Ctrl Pts',(19.0471525139605,8.50003022814292,58.8928916452605));
#117308=CARTESIAN_POINT('Ctrl Pts',(19.0783619071455,8.50148345605102,58.8873852580101));
#117309=CARTESIAN_POINT('Ctrl Pts',(19.1099794394775,8.5045453023276,58.8818079404131));
#117310=CARTESIAN_POINT('Ctrl Pts',(19.1410879060831,8.50755785060767,58.8763204217671));
#117311=CARTESIAN_POINT('Ctrl Pts',(19.1725911301666,8.51212836874123,58.8707642981432));
#117312=CARTESIAN_POINT('Ctrl Pts',(19.2042713121879,8.51837713746225,58.8651776049256));
#117313=CARTESIAN_POINT('Ctrl Pts',(19.2352952562048,8.52449646628568,58.859706637066));
#117314=CARTESIAN_POINT('Ctrl Pts',(19.2664883366558,8.53222581446347,58.8542064515618));
#117315=CARTESIAN_POINT('Ctrl Pts',(19.297614759377,8.54164019590478,58.8487182728915));
#117316=CARTESIAN_POINT('Ctrl Pts',(19.3248593796421,8.54988050188843,58.8439145296166));
#117317=CARTESIAN_POINT('Ctrl Pts',(19.3520521700985,8.55941143136103,58.8391201186967));
#117318=CARTESIAN_POINT('Ctrl Pts',(19.3790206125476,8.57025382158666,58.8343652312728));
#117319=CARTESIAN_POINT('Ctrl Pts',(19.409325475612,8.58243758606239,58.8290220894677));
#117320=CARTESIAN_POINT('Ctrl Pts',(19.4393468014256,8.59627864031572,58.8237288999887));
#117321=CARTESIAN_POINT('Ctrl Pts',(19.468829263876,8.61175911113363,58.8185306779929));
#117322=CARTESIAN_POINT('Ctrl Pts',(19.4978600974361,8.62700244341984,58.8134120852762));
#117323=CARTESIAN_POINT('Ctrl Pts',(19.5263676033458,8.643835338317,58.8083857221369));
#117324=CARTESIAN_POINT('Ctrl Pts',(19.5541087839704,8.66218968833763,58.8034944312797));
#117325=CARTESIAN_POINT('Ctrl Pts',(19.5817057332889,8.68044861084528,58.7986285711091));
#117326=CARTESIAN_POINT('Ctrl Pts',(19.6085434726281,8.70021302554924,58.7938965291188));
#117327=CARTESIAN_POINT('Ctrl Pts',(19.6343960913359,8.7213663065163,58.7893381365852));
#117328=CARTESIAN_POINT('Ctrl Pts',(19.6601785398842,8.74246217244482,58.7847921166137));
#117329=CARTESIAN_POINT('Ctrl Pts',(19.6849804499355,8.76493896360552,58.780418938428));
#117330=CARTESIAN_POINT('Ctrl Pts',(19.7086029926765,8.7886360079756,58.7762536596547));
#117331=CARTESIAN_POINT('Ctrl Pts',(19.7331398265837,8.81325022703638,58.7719271671786));
#117332=CARTESIAN_POINT('Ctrl Pts',(19.7564032709207,8.83918055026988,58.7678251484334));
#117333=CARTESIAN_POINT('Ctrl Pts',(19.7782114202349,8.86620434281197,58.763979678758));
#117334=CARTESIAN_POINT('Ctrl Pts',(19.7993118639889,8.89235117472967,58.7602590000601));
#117335=CARTESIAN_POINT('Ctrl Pts',(19.8190497488021,8.91952067586753,58.756778522324));
#117336=CARTESIAN_POINT('Ctrl Pts',(19.8373056309835,8.94748353013081,58.7535593088364));
#117337=CARTESIAN_POINT('Ctrl Pts',(19.8564799622845,8.97685318898586,58.7501781374787));
#117338=CARTESIAN_POINT('Ctrl Pts',(19.8740187726101,9.00709715222103,58.7470852943527));
#117339=CARTESIAN_POINT('Ctrl Pts',(19.8898418485087,9.03793256084594,58.744294927503));
#117340=CARTESIAN_POINT('Ctrl Pts',(19.9056649244073,9.06876796947085,58.7415045606532));
#117341=CARTESIAN_POINT('Ctrl Pts',(19.9197724007878,9.10019375962582,58.739016646318));
#117342=CARTESIAN_POINT('Ctrl Pts',(19.9321441024897,9.13192558069005,58.7368347476417));
#117343=CARTESIAN_POINT('Ctrl Pts',(19.9443565817857,9.16324901679515,58.7346809297554));
#117344=CARTESIAN_POINT('Ctrl Pts',(19.9548782145085,9.19486980610647,58.7328253088665));
#117345=CARTESIAN_POINT('Ctrl Pts',(19.963742894296,9.22652726318772,58.7312616983276));
#117346=CARTESIAN_POINT('Ctrl Pts',(19.9727144348331,9.25856634032482,58.7296792389867));
#117347=CARTESIAN_POINT('Ctrl Pts',(19.9799893524906,9.29064224036267,58.7283957810469));
#117348=CARTESIAN_POINT('Ctrl Pts',(19.9856502178946,9.32251004117483,58.7273966395878));
#117349=CARTESIAN_POINT('Ctrl Pts',(19.9914529813404,9.35517665598586,58.7263724531566));
#117350=CARTESIAN_POINT('Ctrl Pts',(19.9955603937584,9.38762397511958,58.725646904131));
#117351=CARTESIAN_POINT('Ctrl Pts',(19.9981021899527,9.41962530702886,58.725197077525));
#117352=CARTESIAN_POINT('Ctrl Pts',(20.0002586629659,9.44677540222559,58.7248154423103));
#117353=CARTESIAN_POINT('Ctrl Pts',(20.0012891940811,9.47360506846782,58.7246320997432));
#117354=CARTESIAN_POINT('Ctrl Pts',(20.0012895469767,9.5,58.7246301887192));
#117355=CARTESIAN_POINT('Origin',(17.6260947381591,9.5,51.01300153266));
#117356=CARTESIAN_POINT('',(20.2047121520095,8.50000000009378,65.6369887302606));
#117357=CARTESIAN_POINT('',(17.6261082242393,8.50000000009378,51.0129991547002));
#117358=CARTESIAN_POINT('Origin',(20.2046986659293,9.5,65.6369911082204));
#117359=CARTESIAN_POINT('Origin',(11.833832765324,1.4210854715202E-14,67.1130006183894));
#117360=CARTESIAN_POINT('',(-6.53751764820717,8.5,70.352365368344));
#117361=CARTESIAN_POINT('',(14.8833738632635,20.2647763420359,66.5752842440434));
#117362=CARTESIAN_POINT('Origin',(11.833832765324,1.4210854715202E-14,67.1130006183894));
#117363=CARTESIAN_POINT('Ctrl Pts',(14.8833738632635,20.2647763420359,66.5752842440434));
#117364=CARTESIAN_POINT('Ctrl Pts',(15.4158628606723,19.5539773651717,66.4813920668699));
#117365=CARTESIAN_POINT('Ctrl Pts',(16.038207564819,18.9155234339931,66.3716559042235));
#117366=CARTESIAN_POINT('Ctrl Pts',(17.4246863278478,17.8184518326642,66.1271822901222));
#117367=CARTESIAN_POINT('Ctrl Pts',(18.1846649332837,17.362577725361,65.9931775572271));
#117368=CARTESIAN_POINT('Ctrl Pts',(18.9921125713384,17.0122606549179,65.8508027531287));
#117369=CARTESIAN_POINT('',(13.0648424565899,8.5,66.8959403963056));
#117370=CARTESIAN_POINT('Ctrl Pts',(9.05563024203908,19.74193612938,82.8694660886069));
#117371=CARTESIAN_POINT('Ctrl Pts',(9.2912870723891,19.69133710775,82.83982404191));
#117372=CARTESIAN_POINT('Ctrl Pts',(9.83390957824909,19.60771562075,82.7775183021509));
#117373=CARTESIAN_POINT('Ctrl Pts',(10.6924944126191,19.60610480474,82.6968208510499));
#117374=CARTESIAN_POINT('Ctrl Pts',(11.5835752842391,19.781355271,82.6295254022679));
#117375=CARTESIAN_POINT('Ctrl Pts',(12.3817632835191,20.13187242782,82.5800473343639));
#117376=CARTESIAN_POINT('Ctrl Pts',(13.0117456051291,20.6231476854,82.5470281941081));
#117377=CARTESIAN_POINT('Ctrl Pts',(13.3279861775891,21.03846780615,82.531891260602));
#117378=CARTESIAN_POINT('Ctrl Pts',(13.4400188950291,21.23364550312,82.5267141025));
#117379=CARTESIAN_POINT('Ctrl Pts',(9.04014179690909,20.62748100547,82.628890445775));
#117380=CARTESIAN_POINT('Ctrl Pts',(9.23810271641909,20.56703465702,82.565394916618));
#117381=CARTESIAN_POINT('Ctrl Pts',(9.69456866260909,20.45181847571,82.4295851276741));
#117382=CARTESIAN_POINT('Ctrl Pts',(10.4233163549891,20.36853097734,82.247768026541));
#117383=CARTESIAN_POINT('Ctrl Pts',(11.1933906349991,20.42297948124,82.0910063111319));
#117384=CARTESIAN_POINT('Ctrl Pts',(11.8996157831891,20.6330481663,81.9727340922851));
#117385=CARTESIAN_POINT('Ctrl Pts',(12.4721764120891,20.9837092188,81.892563066293));
#117386=CARTESIAN_POINT('Ctrl Pts',(12.7663175887191,21.30635661408,81.856049847967));
#117387=CARTESIAN_POINT('Ctrl Pts',(12.8712405032191,21.46181296005,81.843530263153));
#117388=CARTESIAN_POINT('Ctrl Pts',(9.1754164244991,21.25111488499,83.28851033235));
#117389=CARTESIAN_POINT('Ctrl Pts',(9.34795109475909,21.22160961919,83.2009960512001));
#117390=CARTESIAN_POINT('Ctrl Pts',(9.73650325255911,21.16897699452,83.0088184827001));
#117391=CARTESIAN_POINT('Ctrl Pts',(10.3245724089391,21.14747847135,82.736721724997));
#117392=CARTESIAN_POINT('Ctrl Pts',(10.9117626573691,21.21052731484,82.487715195758));
#117393=CARTESIAN_POINT('Ctrl Pts',(11.4233081317791,21.36219444676,82.2900975756531));
#117394=CARTESIAN_POINT('Ctrl Pts',(11.8193955837191,21.58897637511,82.150986996173));
#117395=CARTESIAN_POINT('Ctrl Pts',(12.0160830794091,21.78731661116,82.086898923722));
#117396=CARTESIAN_POINT('Ctrl Pts',(12.0855867709291,21.88149337789,82.0647837904481));
#117397=CARTESIAN_POINT('Ctrl Pts',(9.31664801360909,20.94526249146,84.14222888187));
#117398=CARTESIAN_POINT('Ctrl Pts',(9.50324388522909,20.95436551881,84.06624169837));
#117399=CARTESIAN_POINT('Ctrl Pts',(9.9148240365791,20.99150149227,83.89517208715));
#117400=CARTESIAN_POINT('Ctrl Pts',(10.5019640432991,21.10911496024,83.6402764497801));
#117401=CARTESIAN_POINT('Ctrl Pts',(11.0401629057291,21.30096012362,83.39499096567));
#117402=CARTESIAN_POINT('Ctrl Pts',(11.4627087352791,21.538789162,83.19241279179));
#117403=CARTESIAN_POINT('Ctrl Pts',(11.7521790465591,21.79103472492,83.04566744004));
#117404=CARTESIAN_POINT('Ctrl Pts',(11.8803788675091,21.9664992403,82.977323729301));
#117405=CARTESIAN_POINT('Ctrl Pts',(11.9240687861891,22.04343555306,82.953631578989));
#117406=CARTESIAN_POINT('',(9.2477991596469,20.0000000010953,82.8003500634525));
#117407=CARTESIAN_POINT('',(9.42147268300909,20.99999557355,83.78518826663));
#117408=CARTESIAN_POINT('Origin',(9.42146753586009,19.9999823863366,83.7851933307501));
#117409=CARTESIAN_POINT('Ctrl Pts',(9.42147268300909,20.99999557355,83.78518826663));
#117410=CARTESIAN_POINT('Ctrl Pts',(9.55304779465049,20.9999809750948,83.7291788487243));
#117411=CARTESIAN_POINT('Ctrl Pts',(9.90914050500111,21.0105650864534,83.5772223250782));
#117412=CARTESIAN_POINT('Ctrl Pts',(10.4545613751438,21.0771645183637,83.343573390357));
#117413=CARTESIAN_POINT('Ctrl Pts',(11.0175584794691,21.2301198695261,83.1023167131314));
#117414=CARTESIAN_POINT('Ctrl Pts',(11.4774912323362,21.4455062539072,82.9056378798363));
#117415=CARTESIAN_POINT('Ctrl Pts',(11.7701254599278,21.6678362651009,82.7808538677759));
#117416=CARTESIAN_POINT('Ctrl Pts',(11.9020761286329,21.8153229542896,82.7246877181993));
#117417=CARTESIAN_POINT('Ctrl Pts',(11.9367286423891,21.85927935059,82.709938120253));
#117418=CARTESIAN_POINT('Ctrl Pts',(9.24780017804999,20.0000000009406,82.8003558393504));
#117419=CARTESIAN_POINT('Ctrl Pts',(9.41381134930932,20.0000101594718,82.7710848429586));
#117420=CARTESIAN_POINT('Ctrl Pts',(9.57682815077475,20.0068943525989,82.7423593667788));
#117421=CARTESIAN_POINT('Ctrl Pts',(9.73685811767206,20.0206313648514,82.714153161567));
#117422=CARTESIAN_POINT('Ctrl Pts',(9.75787737369477,20.0224356630283,82.7104483963892));
#117423=CARTESIAN_POINT('Ctrl Pts',(9.77884511234476,20.0243582057448,82.706752604443));
#117424=CARTESIAN_POINT('Ctrl Pts',(9.79976062639953,20.0264001910967,82.7030658937577));
#117425=CARTESIAN_POINT('Ctrl Pts',(9.90991246820188,20.0371543349761,82.6836497813391));
#117426=CARTESIAN_POINT('Ctrl Pts',(10.0186334701653,20.0511934060788,82.6644820073428));
#117427=CARTESIAN_POINT('Ctrl Pts',(10.1259182750038,20.0685190477532,82.6455641010232));
#117428=CARTESIAN_POINT('Ctrl Pts',(10.1502333775788,20.0724457431983,82.6412765336146));
#117429=CARTESIAN_POINT('Ctrl Pts',(10.1744749114995,20.076541190263,82.6370017847766));
#117430=CARTESIAN_POINT('Ctrl Pts',(10.1986431558949,20.0808053197147,82.6327398452152));
#117431=CARTESIAN_POINT('Ctrl Pts',(10.2225046454665,20.0850153268124,82.6285320002127));
#117432=CARTESIAN_POINT('Ctrl Pts',(10.2467930053505,20.0894810818087,82.6242487629126));
#117433=CARTESIAN_POINT('Ctrl Pts',(10.2706890022724,20.0940576724294,82.6200346565755));
#117434=CARTESIAN_POINT('Ctrl Pts',(10.2904577504564,20.0978438073128,82.6165483987194));
#117435=CARTESIAN_POINT('Ctrl Pts',(10.3099580439718,20.1017048020977,82.613109442041));
#117436=CARTESIAN_POINT('Ctrl Pts',(10.3287297773731,20.1055318013188,82.6097989607847));
#117437=CARTESIAN_POINT('Ctrl Pts',(10.4121350942416,20.1225356696282,82.5950900507299));
#117438=CARTESIAN_POINT('Ctrl Pts',(10.4940463096557,20.1415290275566,82.5806445104727));
#117439=CARTESIAN_POINT('Ctrl Pts',(10.5745125079426,20.1624361396842,82.5664572751468));
#117440=CARTESIAN_POINT('Ctrl Pts',(10.6687093560787,20.1869108148641,82.5498491480088));
#117441=CARTESIAN_POINT('Ctrl Pts',(10.7609229035475,20.2140105162765,82.5335947896854));
#117442=CARTESIAN_POINT('Ctrl Pts',(10.8511148020616,20.2437803092907,82.5176937523984));
#117443=CARTESIAN_POINT('Ctrl Pts',(10.9136822460994,20.2644320517324,82.5066629694014));
#117444=CARTESIAN_POINT('Ctrl Pts',(10.975278171351,20.2863680756695,82.4958022140613));
#117445=CARTESIAN_POINT('Ctrl Pts',(11.0359035648296,20.3095996373692,82.4851115273486));
#117446=CARTESIAN_POINT('Ctrl Pts',(11.0675766555811,20.3217367192056,82.4795262920038));
#117447=CARTESIAN_POINT('Ctrl Pts',(11.0993314772997,20.3343588413361,82.4739263564523));
#117448=CARTESIAN_POINT('Ctrl Pts',(11.1307220159251,20.3473028790355,82.4683906090922));
#117449=CARTESIAN_POINT('Ctrl Pts',(11.1619517472033,20.3601806070615,82.4628832202403));
#117450=CARTESIAN_POINT('Ctrl Pts',(11.1928207334175,20.3733769581208,82.4574394030529));
#117451=CARTESIAN_POINT('Ctrl Pts',(11.2229069821298,20.3866822567242,82.4521339013917));
#117452=CARTESIAN_POINT('Ctrl Pts',(11.2334477503644,20.3913437906434,82.4502751098915));
#117453=CARTESIAN_POINT('Ctrl Pts',(11.2438926075315,20.3960182581678,82.4484332669831));
#117454=CARTESIAN_POINT('Ctrl Pts',(11.2542239598114,20.4006952414998,82.4466114892795));
#117455=CARTESIAN_POINT('Ctrl Pts',(11.2700155143389,20.407844047901,82.4438268875));
#117456=CARTESIAN_POINT('Ctrl Pts',(11.2857053529294,20.4150750395933,82.4410603493937));
#117457=CARTESIAN_POINT('Ctrl Pts',(11.3012948100236,20.4223871806256,82.4383117024514));
#117458=CARTESIAN_POINT('Ctrl Pts',(11.3716798206214,20.4554008462678,82.4259018062634));
#117459=CARTESIAN_POINT('Ctrl Pts',(11.4400135594739,20.4900689328506,82.4138566940165));
#117460=CARTESIAN_POINT('Ctrl Pts',(11.5062760631553,20.5263935357958,82.4021735431031));
#117461=CARTESIAN_POINT('Ctrl Pts',(11.5544472188273,20.5528005987044,82.3936801893944));
#117462=CARTESIAN_POINT('Ctrl Pts',(11.6015252661522,20.5800829070673,82.3853780955072));
#117463=CARTESIAN_POINT('Ctrl Pts',(11.647519334929,20.6082432514823,82.3772659700509));
#117464=CARTESIAN_POINT('Ctrl Pts',(11.6951740296187,20.6374203312917,82.3688609545306));
#117465=CARTESIAN_POINT('Ctrl Pts',(11.741809545569,20.6676409430077,82.3606344338639));
#117466=CARTESIAN_POINT('Ctrl Pts',(11.7872463267942,20.6987950811283,82.3526204474684));
#117467=CARTESIAN_POINT('Ctrl Pts',(11.8263526434061,20.7256086791928,82.3457230070941));
#117468=CARTESIAN_POINT('Ctrl Pts',(11.8645714129522,20.7531131352691,82.338982978887));
#117469=CARTESIAN_POINT('Ctrl Pts',(11.9018088960741,20.7812154666837,82.3324193291663));
#117470=CARTESIAN_POINT('Ctrl Pts',(11.9332265859284,20.8049257246964,82.3268815029238));
#117471=CARTESIAN_POINT('Ctrl Pts',(11.9639454805571,20.8290611782182,82.3214692070529));
#117472=CARTESIAN_POINT('Ctrl Pts',(11.9938802796988,20.8535531845223,82.3161950225982));
#117473=CARTESIAN_POINT('Ctrl Pts',(12.0432245216299,20.8939255778271,82.3075011064474));
#117474=CARTESIAN_POINT('Ctrl Pts',(12.0904669901627,20.935294926462,82.2991770861494));
#117475=CARTESIAN_POINT('Ctrl Pts',(12.1356130952059,20.9776340615505,82.2912177691209));
#117476=CARTESIAN_POINT('Ctrl Pts',(12.1835950663075,21.0226327420422,82.2827584852184));
#117477=CARTESIAN_POINT('Ctrl Pts',(12.2292104629269,21.0687261422084,82.2747110466225));
#117478=CARTESIAN_POINT('Ctrl Pts',(12.2725058106192,21.1159255274227,82.2670693314398));
#117479=CARTESIAN_POINT('Ctrl Pts',(12.3043664816712,21.1506591458444,82.2614458594807));
#117480=CARTESIAN_POINT('Ctrl Pts',(12.3349716875747,21.1859926223862,82.2560420928028));
#117481=CARTESIAN_POINT('Ctrl Pts',(12.3643457345344,21.2219474207367,82.2508562354651));
#117482=CARTESIAN_POINT('Ctrl Pts',(12.4000777563314,21.2656845891333,82.2445479059497));
#117483=CARTESIAN_POINT('Ctrl Pts',(12.4339866756333,21.3103385304835,82.238562052063));
#117484=CARTESIAN_POINT('Ctrl Pts',(12.4659848864984,21.3558676724476,82.232913638037));
#117485=CARTESIAN_POINT('Ctrl Pts',(12.4836712988028,21.3810330537258,82.2297915828773));
#117486=CARTESIAN_POINT('Ctrl Pts',(12.5007742972253,21.4064667735531,82.226772634051));
#117487=CARTESIAN_POINT('Ctrl Pts',(12.5172801388854,21.4321684410533,82.2238595693975));
#117488=CARTESIAN_POINT('Origin',(-7.20566857569291,10.,84.1784376645));
#117489=CARTESIAN_POINT('',(-4.19330934979995,8.50000005802184,83.6470312449829));
#117490=CARTESIAN_POINT('',(-3.1851014235548,10.,84.9926431156514));
#117491=CARTESIAN_POINT('Ctrl Pts',(-4.19330934571277,8.50000001959754,
83.6470312442563));
#117492=CARTESIAN_POINT('Ctrl Pts',(-4.19329531627948,8.50000000653218,
83.6471108434094));
#117493=CARTESIAN_POINT('Ctrl Pts',(-4.19328128427642,8.5,83.6471904399934));
#117494=CARTESIAN_POINT('Ctrl Pts',(-4.15980554940295,8.5,83.8370407665797));
#117495=CARTESIAN_POINT('Ctrl Pts',(-4.10685468483148,8.53950345297412,
84.0345242483906));
#117496=CARTESIAN_POINT('Ctrl Pts',(-3.97184256650876,8.6947907400348,84.3859356237976));
#117497=CARTESIAN_POINT('Ctrl Pts',(-3.88961764476103,8.81043822068695,
84.5398608579619));
#117498=CARTESIAN_POINT('Ctrl Pts',(-3.71525661408043,9.07833587624806,
84.7811467125873));
#117499=CARTESIAN_POINT('Ctrl Pts',(-3.61058564106113,9.25135231079439,
84.879888801679));
#117500=CARTESIAN_POINT('Ctrl Pts',(-3.3954856573262,9.62155435638349,84.9943545575053));
#117501=CARTESIAN_POINT('Ctrl Pts',(-3.2849218663493,9.8186103084606,85.0102441529475));
#117502=CARTESIAN_POINT('Ctrl Pts',(-3.18510142355393,10.,84.9926431156565));
#117503=CARTESIAN_POINT('',(-6.8072945652419,8.50000000000004,84.1081934943927));
#117504=CARTESIAN_POINT('',(-6.80729512863291,8.5,84.10819367738));
#117505=CARTESIAN_POINT('',(-6.54682286425215,10.,85.5854053072757));
#117506=CARTESIAN_POINT('Origin',(-6.80729512863291,10.,84.10819367738));
#117507=CARTESIAN_POINT('',(-6.94519630919256,10.,85.6556492940183));
#117508=CARTESIAN_POINT('Origin',(11.833832765324,1.4210854715202E-14,67.1130006183894));
#117509=CARTESIAN_POINT('',(-6.53751764820717,8.5,70.352365368344));
#117510=CARTESIAN_POINT('',(13.3597592683937,20.4707111483689,82.0753376302183));
#117511=CARTESIAN_POINT('Origin',(14.4385554303262,1.4210854715202E-14,
81.8851169135651));
#117512=CARTESIAN_POINT('',(15.1826200703325,20.4790215093801,80.7654567789229));
#117513=CARTESIAN_POINT('Ctrl Pts',(13.3597592422362,20.4707111483689,82.0753374818706));
#117514=CARTESIAN_POINT('Ctrl Pts',(13.5489200678292,20.4809897643711,82.0419835619616));
#117515=CARTESIAN_POINT('Ctrl Pts',(13.7352332109664,20.4885496274001,81.9876000411839));
#117516=CARTESIAN_POINT('Ctrl Pts',(14.0953296708824,20.4982351765127,81.841707426555));
#117517=CARTESIAN_POINT('Ctrl Pts',(14.2709193683375,20.5002927571102,81.7485872067569));
#117518=CARTESIAN_POINT('Ctrl Pts',(14.6067578621981,20.4996156846239,81.5206315743113));
#117519=CARTESIAN_POINT('Ctrl Pts',(14.7693220761259,20.4964642438232,81.3803787318923));
#117520=CARTESIAN_POINT('Ctrl Pts',(15.0202379695866,20.4881014789292,81.0852130979036));
#117521=CARTESIAN_POINT('Ctrl Pts',(15.1191031310536,20.4831599384662,80.9316197555286));
#117522=CARTESIAN_POINT('Ctrl Pts',(15.1826197616608,20.4790215522793,80.7654566598632));
#117523=CARTESIAN_POINT('Ctrl Pts',(15.9984193009007,20.3875466887266,78.3830201467867));
#117524=CARTESIAN_POINT('Ctrl Pts',(15.8770688204797,20.4073988582131,78.7818268437993));
#117525=CARTESIAN_POINT('Ctrl Pts',(15.7502010071011,20.4250600452808,79.1746414174431));
#117526=CARTESIAN_POINT('Ctrl Pts',(15.6182044599264,20.4401531721352,79.5610824354396));
#117527=CARTESIAN_POINT('Ctrl Pts',(15.549503107267,20.4480088187635,79.7622166410514));
#117528=CARTESIAN_POINT('Ctrl Pts',(15.4794122215352,20.4551693893405,79.9616248643147));
#117529=CARTESIAN_POINT('Ctrl Pts',(15.4079854932393,20.4615855988943,80.1592571638601));
#117530=CARTESIAN_POINT('Ctrl Pts',(15.3342663988258,20.4682077299811,80.3632322652954));
#117531=CARTESIAN_POINT('Ctrl Pts',(15.2591243512077,20.4740369355328,80.5653156100083));
#117532=CARTESIAN_POINT('Ctrl Pts',(15.1826202858407,20.4790215304872,80.7654568607777));
#117533=CARTESIAN_POINT('Ctrl Pts',(14.8833738632635,20.2647763420359,66.5752842440434));
#117534=CARTESIAN_POINT('Ctrl Pts',(15.0733159401335,20.2477695588669,67.0115691027874));
#117535=CARTESIAN_POINT('Ctrl Pts',(15.2555091649434,20.23108766834,67.4513545027359));
#117536=CARTESIAN_POINT('Ctrl Pts',(15.4297724903522,20.2151317187521,67.8942334785676));
#117537=CARTESIAN_POINT('Ctrl Pts',(15.4928256588264,20.2093584260918,68.0544790300126));
#117538=CARTESIAN_POINT('Ctrl Pts',(15.5548406861411,20.2036796842702,68.2151295830088));
#117539=CARTESIAN_POINT('Ctrl Pts',(15.6158090592685,20.1981127976809,68.3761658484978));
#117540=CARTESIAN_POINT('Ctrl Pts',(12.6103939613991,23.39573848791,81.293275948705));
#117541=CARTESIAN_POINT('Ctrl Pts',(12.6301344989091,23.36712060978,81.286688115074));
#117542=CARTESIAN_POINT('Ctrl Pts',(12.8623544188791,23.03339800576,81.2092658486509));
#117543=CARTESIAN_POINT('Ctrl Pts',(13.3195155352191,22.43787252879,81.0584942952861));
#117544=CARTESIAN_POINT('Ctrl Pts',(14.0054384121691,21.66395729877,80.8371498110769));
#117545=CARTESIAN_POINT('Ctrl Pts',(14.6750728316091,20.99216918735,80.625783923235));
#117546=CARTESIAN_POINT('Ctrl Pts',(15.3162005729891,20.41109563502,80.4277322359629));
#117547=CARTESIAN_POINT('Ctrl Pts',(15.9201036787491,19.91127773927,80.245012905101));
#117548=CARTESIAN_POINT('Ctrl Pts',(16.4827047066491,19.4827933493,80.0780860889519));
#117549=CARTESIAN_POINT('Ctrl Pts',(17.0027455733291,19.11617373137,79.926546278835));
#117550=CARTESIAN_POINT('Ctrl Pts',(17.4804240494591,18.80293987069,79.789629873945));
#117551=CARTESIAN_POINT('Ctrl Pts',(17.9170466493591,18.53549113312,79.666341537588));
#117552=CARTESIAN_POINT('Ctrl Pts',(18.2457112148691,18.34670706214,79.574782208674));
#117553=CARTESIAN_POINT('Ctrl Pts',(18.4288583779791,18.24601358153,79.524208507212));
#117554=CARTESIAN_POINT('Ctrl Pts',(18.4788029562491,18.2188868654,79.510449919603));
#117555=CARTESIAN_POINT('Ctrl Pts',(12.4260057050691,23.15454775929,82.3416317744899));
#117556=CARTESIAN_POINT('Ctrl Pts',(12.4484290189691,23.12610953721,82.335556515214));
#117557=CARTESIAN_POINT('Ctrl Pts',(12.7119653073691,22.79485591383,82.264081173276));
#117558=CARTESIAN_POINT('Ctrl Pts',(13.2254892213291,22.21157537144,82.123130223133));
#117559=CARTESIAN_POINT('Ctrl Pts',(13.9832319374791,21.46817083564,81.911502389663));
#117560=CARTESIAN_POINT('Ctrl Pts',(14.7127953478491,20.83289001182,81.705550703378));
#117561=CARTESIAN_POINT('Ctrl Pts',(15.4031177402791,20.29055202507,81.509530462387));
#117562=CARTESIAN_POINT('Ctrl Pts',(16.0467726803191,19.82929174299,81.326377521192));
#117563=CARTESIAN_POINT('Ctrl Pts',(16.6411046175391,19.43781087338,81.1573453210401));
#117564=CARTESIAN_POINT('Ctrl Pts',(17.1862122875291,19.10591070303,81.0026466246689));
#117565=CARTESIAN_POINT('Ctrl Pts',(17.6834900333091,18.82474934939,80.861975064868));
#117566=CARTESIAN_POINT('Ctrl Pts',(18.1352802572891,18.58660771731,80.734659490498));
#117567=CARTESIAN_POINT('Ctrl Pts',(18.4735435632491,18.41979202888,80.639728546379));
#117568=CARTESIAN_POINT('Ctrl Pts',(18.6613901681291,18.33128071504,80.587171652487));
#117569=CARTESIAN_POINT('Ctrl Pts',(18.7125685143091,18.30747099738,80.572865027715));
#117570=CARTESIAN_POINT('Ctrl Pts',(11.5978097779391,22.5674100597,82.742358165064));
#117571=CARTESIAN_POINT('Ctrl Pts',(11.6227733666891,22.53672166376,82.73823514027));
#117572=CARTESIAN_POINT('Ctrl Pts',(11.9160671669291,22.17956444248,82.6896285494211));
#117573=CARTESIAN_POINT('Ctrl Pts',(12.4854557092891,21.55712977634,82.591528127515));
#117574=CARTESIAN_POINT('Ctrl Pts',(13.3211227504391,20.77626353478,82.4380379028789));
#117575=CARTESIAN_POINT('Ctrl Pts',(14.1224813937691,20.11780076625,82.283329059817));
#117576=CARTESIAN_POINT('Ctrl Pts',(14.8783020667991,19.56212479249,82.131672635088));
#117577=CARTESIAN_POINT('Ctrl Pts',(15.5811274847591,19.09431145646,81.9864168604));
#117578=CARTESIAN_POINT('Ctrl Pts',(16.2285628910291,18.7009157217,81.849546008323));
#117579=CARTESIAN_POINT('Ctrl Pts',(16.8211097747291,18.37024197503,81.722081374855));
#117580=CARTESIAN_POINT('Ctrl Pts',(17.3606117917191,18.09238223453,81.6044624197011));
#117581=CARTESIAN_POINT('Ctrl Pts',(17.8498880368591,17.8588580807,81.496683301038));
#117582=CARTESIAN_POINT('Ctrl Pts',(18.2156163347991,17.69650125828,81.415469693152));
#117583=CARTESIAN_POINT('Ctrl Pts',(18.4184926455491,17.61080394924,81.370213465902));
#117584=CARTESIAN_POINT('Ctrl Pts',(18.4737491950091,17.58778530033,81.357872779003));
#117585=CARTESIAN_POINT('Ctrl Pts',(10.7887911682091,22.10433914807,82.174666798942));
#117586=CARTESIAN_POINT('Ctrl Pts',(10.8141189968491,22.07077205096,82.172372871705));
#117587=CARTESIAN_POINT('Ctrl Pts',(11.1117900557491,21.6800749259,82.145250032619));
#117588=CARTESIAN_POINT('Ctrl Pts',(11.6918244678991,20.99843062262,82.088727484073));
#117589=CARTESIAN_POINT('Ctrl Pts',(12.5491405664491,20.14211901076,81.9952556772969));
#117590=CARTESIAN_POINT('Ctrl Pts',(13.3766873742891,19.41934260798,81.896597547713));
#117591=CARTESIAN_POINT('Ctrl Pts',(14.1618774648791,18.80893238109,81.7961233164201));
#117592=CARTESIAN_POINT('Ctrl Pts',(14.8959250259991,18.29470115512,81.696758155871));
#117593=CARTESIAN_POINT('Ctrl Pts',(15.5753262268891,17.86200505198,81.600569675382));
#117594=CARTESIAN_POINT('Ctrl Pts',(16.1997088336891,17.49808293197,81.5089307213659));
#117595=CARTESIAN_POINT('Ctrl Pts',(16.7702588729991,17.19211091299,81.422718126577));
#117596=CARTESIAN_POINT('Ctrl Pts',(17.2893313360391,16.93481823995,81.3423998907959));
#117597=CARTESIAN_POINT('Ctrl Pts',(17.6784046821991,16.75584136857,81.2810116085869));
#117598=CARTESIAN_POINT('Ctrl Pts',(17.8946094266191,16.66133724348,81.2464955986819));
#117599=CARTESIAN_POINT('Ctrl Pts',(17.9535239433391,16.63595046951,81.2370610578369));
#117600=CARTESIAN_POINT('Ctrl Pts',(12.5172852744664,21.43216844352,82.2238886792731));
#117601=CARTESIAN_POINT('Ctrl Pts',(12.7388749288692,21.15829039737,82.184816444556));
#117602=CARTESIAN_POINT('Ctrl Pts',(12.9611536694374,20.90216875751,82.1456227053559));
#117603=CARTESIAN_POINT('Ctrl Pts',(13.181766647766,20.66173879788,82.1067226849821));
#117604=CARTESIAN_POINT('Ctrl Pts',(13.2412317619777,20.5969321164344,82.0962373809357));
#117605=CARTESIAN_POINT('Ctrl Pts',(13.3005758510999,20.5332655058573,82.0857734168779));
#117606=CARTESIAN_POINT('Ctrl Pts',(13.3597592946233,20.4707111483689,82.0753377789735));
#117607=CARTESIAN_POINT('Ctrl Pts',(12.6211132020991,23.19498548026,81.546653375664));
#117608=CARTESIAN_POINT('Ctrl Pts',(12.8357939683531,22.9022256951466,81.4798426388965));
#117609=CARTESIAN_POINT('Ctrl Pts',(13.2793186839497,22.3474956363199,81.342352295626));
#117610=CARTESIAN_POINT('Ctrl Pts',(13.9768208390301,21.5902063508969,81.1283687718575));
#117611=CARTESIAN_POINT('Ctrl Pts',(14.6131840765691,20.9760939162043,80.9356018413964));
#117612=CARTESIAN_POINT('Ctrl Pts',(15.0160011538732,20.6207817077894,80.8150471263846));
#117613=CARTESIAN_POINT('Ctrl Pts',(15.182620190286,20.4790216117855,80.7654568892173));
#117614=CARTESIAN_POINT('Origin',(-6.70435958676991,20.,86.62860989379));
#117615=CARTESIAN_POINT('',(-6.1121826461617,20.00000000008,85.5087648635416));
#117616=CARTESIAN_POINT('',(-5.93853418691238,20.9999970776591,86.4935742132893));
#117617=CARTESIAN_POINT('Origin',(-5.93853418697242,20.,86.4935742132939));
#117618=CARTESIAN_POINT('',(-5.93853418690691,20.99999766213,86.49357421329));
#117619=CARTESIAN_POINT('',(-8.75366715310791,20.00000000008,85.97453149762));
#117620=CARTESIAN_POINT('Ctrl Pts',(0.957715876419088,23.49481230627,90.05041057889));
#117621=CARTESIAN_POINT('Ctrl Pts',(1.41501551649909,23.49481230627,89.9030012875299));
#117622=CARTESIAN_POINT('Ctrl Pts',(2.31555886405909,23.49481230627,89.60436039102));
#117623=CARTESIAN_POINT('Ctrl Pts',(3.60119053426909,23.49481230627,89.1258337619599));
#117624=CARTESIAN_POINT('Ctrl Pts',(4.77329563338909,23.49481230627,88.61996295293));
#117625=CARTESIAN_POINT('Ctrl Pts',(5.85230040977909,23.49481230627,88.07694753354));
#117626=CARTESIAN_POINT('Ctrl Pts',(6.88449642105908,23.49481230627,87.4679726818399));
#117627=CARTESIAN_POINT('Ctrl Pts',(7.88241911249909,23.49481230627,86.77324032414));
#117628=CARTESIAN_POINT('Ctrl Pts',(8.82724414092909,23.49481230627,85.99908763589));
#117629=CARTESIAN_POINT('Ctrl Pts',(9.71652793426909,23.49481230627,85.14645307785));
#117630=CARTESIAN_POINT('Ctrl Pts',(10.5558228444891,23.49481230627,84.20870787798));
#117631=CARTESIAN_POINT('Ctrl Pts',(11.3451188799491,23.49481230627,83.18434038658));
#117632=CARTESIAN_POINT('Ctrl Pts',(11.9952966407791,23.49481230627,82.206938842754));
#117633=CARTESIAN_POINT('Ctrl Pts',(12.3726190997991,23.49481230627,81.5679157537));
#117634=CARTESIAN_POINT('Ctrl Pts',(12.5199395434791,23.49481230627,81.306465323002));
#117635=CARTESIAN_POINT('Ctrl Pts',(1.31223816379909,22.19079499982,91.1502067021801));
#117636=CARTESIAN_POINT('Ctrl Pts',(1.77575274979909,22.19079499982,91.00079655301));
#117637=CARTESIAN_POINT('Ctrl Pts',(2.69548452203909,22.19079499982,90.69589495095));
#117638=CARTESIAN_POINT('Ctrl Pts',(4.02863623059909,22.19079499982,90.1999352359901));
#117639=CARTESIAN_POINT('Ctrl Pts',(5.26015181865909,22.19079499982,89.6686560663001));
#117640=CARTESIAN_POINT('Ctrl Pts',(6.4052033873591,22.19079499982,89.0925893293601));
#117641=CARTESIAN_POINT('Ctrl Pts',(7.50852137763909,22.19079499982,88.44181096938));
#117642=CARTESIAN_POINT('Ctrl Pts',(8.57970895306909,22.19079499982,87.6961548951001));
#117643=CARTESIAN_POINT('Ctrl Pts',(9.5949459237791,22.19079499982,86.86429832097));
#117644=CARTESIAN_POINT('Ctrl Pts',(10.5489790579091,22.19079499982,85.94949099884));
#117645=CARTESIAN_POINT('Ctrl Pts',(11.4462119670491,22.19079499982,84.94685287882));
#117646=CARTESIAN_POINT('Ctrl Pts',(12.2859883987391,22.19079499982,83.85676531586));
#117647=CARTESIAN_POINT('Ctrl Pts',(12.9740777733391,22.19079499982,82.822164502385));
#117648=CARTESIAN_POINT('Ctrl Pts',(13.3716617553591,22.19079499982,82.14877575625));
#117649=CARTESIAN_POINT('Ctrl Pts',(13.5266438736891,22.19079499982,81.8737270015279));
#117650=CARTESIAN_POINT('Ctrl Pts',(1.04499173760909,20.68183692524,90.3211570374501));
#117651=CARTESIAN_POINT('Ctrl Pts',(1.50382136543909,20.68183692524,90.1732551773701));
#117652=CARTESIAN_POINT('Ctrl Pts',(2.40908849580909,20.68183692524,89.87307302805));
#117653=CARTESIAN_POINT('Ctrl Pts',(3.70641859067909,20.68183692524,89.39025474333));
#117654=CARTESIAN_POINT('Ctrl Pts',(4.89314929098909,20.68183692524,88.8781289352801));
#117655=CARTESIAN_POINT('Ctrl Pts',(5.98841338556909,20.68183692524,88.3269769831401));
#117656=CARTESIAN_POINT('Ctrl Pts',(7.03811811826909,20.68183692524,87.7077109951301));
#117657=CARTESIAN_POINT('Ctrl Pts',(8.05407706883909,20.68183692524,87.00044229944));
#117658=CARTESIAN_POINT('Ctrl Pts',(9.01623602272909,20.68183692524,86.21208413945));
#117659=CARTESIAN_POINT('Ctrl Pts',(9.9214597292391,20.68183692524,85.3441439667299));
#117660=CARTESIAN_POINT('Ctrl Pts',(10.7750177448491,20.68183692524,84.39042350749));
#117661=CARTESIAN_POINT('Ctrl Pts',(11.5767409822491,20.68183692524,83.34987712961));
#117662=CARTESIAN_POINT('Ctrl Pts',(12.2362517775791,20.68183692524,82.358394339851));
#117663=CARTESIAN_POINT('Ctrl Pts',(12.6185621934391,20.68183692524,81.710911155554));
#117664=CARTESIAN_POINT('Ctrl Pts',(12.7677687787691,20.68183692524,81.446113106153));
#117665=CARTESIAN_POINT('Ctrl Pts',(0.521235740009087,21.03030703444,88.69636549059));
#117666=CARTESIAN_POINT('Ctrl Pts',(0.970883673709088,21.03030703444,88.55141961189));
#117667=CARTESIAN_POINT('Ctrl Pts',(1.84780264977909,21.03030703444,88.26048675999));
#117668=CARTESIAN_POINT('Ctrl Pts',(3.07492868137909,21.03030703444,87.80342336748));
#117669=CARTESIAN_POINT('Ctrl Pts',(4.17388887751909,21.03030703444,87.3288347799701));
#117670=CARTESIAN_POINT('Ctrl Pts',(5.17157827841909,21.03030703444,86.82651142453));
#117671=CARTESIAN_POINT('Ctrl Pts',(6.11621045464909,21.03030703444,86.2690041438399));
#117672=CARTESIAN_POINT('Ctrl Pts',(7.02393101296908,21.03030703444,85.63696795942));
#117673=CARTESIAN_POINT('Ctrl Pts',(7.8820663881191,21.03030703444,84.93385904153));
#117674=CARTESIAN_POINT('Ctrl Pts',(8.69163220008909,21.03030703444,84.15777023963));
#117675=CARTESIAN_POINT('Ctrl Pts',(9.45959510503909,21.03030703444,83.29991979292));
#117676=CARTESIAN_POINT('Ctrl Pts',(10.1867407736191,21.03030703444,82.356465425506));
#117677=CARTESIAN_POINT('Ctrl Pts',(10.7902425793991,21.03030703444,81.449486379538));
#117678=CARTESIAN_POINT('Ctrl Pts',(11.1426194915691,21.03030703444,80.852773540713));
#117679=CARTESIAN_POINT('Ctrl Pts',(11.2805070479191,21.03030703444,80.6080650710599));
#117680=CARTESIAN_POINT('',(0.756634314019088,21.00000000035,88.9355837865));
#117681=CARTESIAN_POINT('Ctrl Pts',(0.756634314019086,21.000000000506,88.9355837865));
#117682=CARTESIAN_POINT('Ctrl Pts',(0.93994744103186,21.000000000506,88.8761073500416));
#117683=CARTESIAN_POINT('Ctrl Pts',(1.11959860663145,21.0000000005717,88.8170344284642));
#117684=CARTESIAN_POINT('Ctrl Pts',(1.29567538370028,21.0000000005633,88.7581145497408));
#117685=CARTESIAN_POINT('Ctrl Pts',(1.48070951214041,21.0000000005545,88.6961973077917));
#117686=CARTESIAN_POINT('Ctrl Pts',(1.66179643777212,21.0000000004149,88.6344492947818));
#117687=CARTESIAN_POINT('Ctrl Pts',(1.8390552467172,21.0000000002067,88.5726343848086));
#117688=CARTESIAN_POINT('Ctrl Pts',(1.87867901386347,21.0000000001602,88.5588165124359));
#117689=CARTESIAN_POINT('Ctrl Pts',(1.91811155806819,21.0000000001135,88.5449954954783));
#117690=CARTESIAN_POINT('Ctrl Pts',(1.95735431199024,21.0000000000752,88.531169025967));
#117691=CARTESIAN_POINT('Ctrl Pts',(2.00286697124637,21.0000000000307,88.5151334695217));
#117692=CARTESIAN_POINT('Ctrl Pts',(2.04812434624247,20.9999999999972,88.4990905761022));
#117693=CARTESIAN_POINT('Ctrl Pts',(2.09312837856909,20.9999999999972,88.483037093));
#117694=CARTESIAN_POINT('Ctrl Pts',(2.24351527878013,20.9999999999972,88.4293922652698));
#117695=CARTESIAN_POINT('Ctrl Pts',(2.39108406144822,21.0000000003555,88.3756366703905));
#117696=CARTESIAN_POINT('Ctrl Pts',(2.5354704698584,21.0000000005385,88.3218406192587));
#117697=CARTESIAN_POINT('Ctrl Pts',(2.67828857452791,21.0000000007195,88.2686288928506));
#117698=CARTESIAN_POINT('Ctrl Pts',(2.81799304255477,21.000000000706,88.2153775179761));
#117699=CARTESIAN_POINT('Ctrl Pts',(2.95425406246973,21.0000000004912,88.1622002390388));
#117700=CARTESIAN_POINT('Ctrl Pts',(3.04816581560319,21.0000000003433,88.1255502015227));
#117701=CARTESIAN_POINT('Ctrl Pts',(3.14044239566545,21.0000000001096,88.0889363184504));
#117702=CARTESIAN_POINT('Ctrl Pts',(3.23098221778327,21.0000000000248,88.052408776881));
#117703=CARTESIAN_POINT('Ctrl Pts',(3.2494640903951,21.0000000000075,88.0449524184045));
#117704=CARTESIAN_POINT('Ctrl Pts',(3.26787361139831,20.9999999999972,88.0374996931925));
#117705=CARTESIAN_POINT('Ctrl Pts',(3.28620992071076,20.9999999999972,88.03005113008));
#117706=CARTESIAN_POINT('Ctrl Pts',(3.47134091295659,20.9999999999972,87.954847344175));
#117707=CARTESIAN_POINT('Ctrl Pts',(3.64897689064145,20.9999999997563,87.8799868520678));
#117708=CARTESIAN_POINT('Ctrl Pts',(3.82034472080339,21.000000000393,87.8052335230894));
#117709=CARTESIAN_POINT('Ctrl Pts',(3.97819715652474,21.0000000009796,87.7363758206468));
#117710=CARTESIAN_POINT('Ctrl Pts',(4.13073188522359,21.0000000007529,87.6676097819603));
#117711=CARTESIAN_POINT('Ctrl Pts',(4.27889814688429,21.0000000000916,87.5987088186199));
#117712=CARTESIAN_POINT('Ctrl Pts',(4.2915842068743,21.000000000035,87.5928094880671));
#117713=CARTESIAN_POINT('Ctrl Pts',(4.30423823260115,20.9999999999972,87.586909137677));
#117714=CARTESIAN_POINT('Ctrl Pts',(4.31686081404071,20.9999999999972,87.5810076073234));
#117715=CARTESIAN_POINT('Ctrl Pts',(4.31910810196864,20.9999999999972,87.579956915911));
#117716=CARTESIAN_POINT('Ctrl Pts',(4.32135438131283,20.9999999999984,87.5789061686031));
#117717=CARTESIAN_POINT('Ctrl Pts',(4.32359966125888,21.0000000000008,87.5778553613796));
#117718=CARTESIAN_POINT('Ctrl Pts',(4.42088083646353,21.000000000105,87.5323270691057));
#117719=CARTESIAN_POINT('Ctrl Pts',(4.51628790649546,21.0000000025738,87.4866900145638));
#117720=CARTESIAN_POINT('Ctrl Pts',(4.61055451505413,21.0000000047615,87.4406063796447));
#117721=CARTESIAN_POINT('Ctrl Pts',(4.70337776390992,21.0000000069156,87.3952283526033));
#117722=CARTESIAN_POINT('Ctrl Pts',(4.79509535721351,21.0000000085217,87.3494173844181));
#117723=CARTESIAN_POINT('Ctrl Pts',(4.88638328488241,21.0000000077554,87.3028072525664));
#117724=CARTESIAN_POINT('Ctrl Pts',(4.97507500508643,21.000000007011,87.2575227020411));
#117725=CARTESIAN_POINT('Ctrl Pts',(5.06336126825696,21.0000000036719,87.211483844095));
#117726=CARTESIAN_POINT('Ctrl Pts',(5.15183690010692,21.0000000013663,87.1643125760065));
#117727=CARTESIAN_POINT('Ctrl Pts',(5.18170994870006,21.0000000005878,87.1483855964039));
#117728=CARTESIAN_POINT('Ctrl Pts',(5.21160436110771,20.9999999999972,87.1323291520711));
#117729=CARTESIAN_POINT('Ctrl Pts',(5.24154231686215,20.9999999999972,87.1161275298069));
#117730=CARTESIAN_POINT('Ctrl Pts',(5.26025608299938,20.9999999999972,87.1060001392601));
#117731=CARTESIAN_POINT('Ctrl Pts',(5.27898824498872,21.0000000002298,87.0958185962174));
#117732=CARTESIAN_POINT('Ctrl Pts',(5.2977362483153,21.0000000005657,87.0855832092499));
#117733=CARTESIAN_POINT('Ctrl Pts',(5.41724408030014,21.0000000027072,87.0203384530646));
#117734=CARTESIAN_POINT('Ctrl Pts',(5.5373939734491,21.0000000060343,86.9529020405239));
#117735=CARTESIAN_POINT('Ctrl Pts',(5.65753673683337,21.0000000050463,86.8834118691035));
#117736=CARTESIAN_POINT('Ctrl Pts',(5.77345936830357,21.0000000040931,86.8163626078292));
#117737=CARTESIAN_POINT('Ctrl Pts',(5.8893751368828,21.0000000014303,86.7474012834568));
#117738=CARTESIAN_POINT('Ctrl Pts',(6.00472156171291,21.0000000005319,86.676695723562));
#117739=CARTESIAN_POINT('Ctrl Pts',(6.05642031158837,21.0000000001292,86.6450051959952));
#117740=CARTESIAN_POINT('Ctrl Pts',(6.10800499045389,20.9999999999972,86.6129648797915));
#117741=CARTESIAN_POINT('Ctrl Pts',(6.15942655135603,20.9999999999972,86.5805929331082));
#117742=CARTESIAN_POINT('Ctrl Pts',(6.19537674171716,20.9999999999972,86.5579608382202));
#117743=CARTESIAN_POINT('Ctrl Pts',(6.23124719525267,21.0000000000476,86.5351662312197));
#117744=CARTESIAN_POINT('Ctrl Pts',(6.2670292769119,21.0000000000872,86.512212433455));
#117745=CARTESIAN_POINT('Ctrl Pts',(6.40028191327865,21.0000000002348,86.4267323852033));
#117746=CARTESIAN_POINT('Ctrl Pts',(6.53230650202812,21.0000000000892,86.3390413814324));
#117747=CARTESIAN_POINT('Ctrl Pts',(6.66269166437902,21.0000000000251,86.2493922214948));
#117748=CARTESIAN_POINT('Ctrl Pts',(6.79307682672993,20.9999999999609,86.1597430615573));
#117749=CARTESIAN_POINT('Ctrl Pts',(6.92182230893109,20.9999999999972,86.0681357906987));
#117750=CARTESIAN_POINT('Ctrl Pts',(7.0485510816308,20.9999999999972,85.9748650028717));
#117751=CARTESIAN_POINT('Ctrl Pts',(7.09916077095027,20.9999999999972,85.9376169060587));
#117752=CARTESIAN_POINT('Ctrl Pts',(7.14944610400102,21.0000000000191,85.9001003667346));
#117753=CARTESIAN_POINT('Ctrl Pts',(7.1994227681535,21.0000000000378,85.8623048375778));
#117754=CARTESIAN_POINT('Ctrl Pts',(7.32807752282551,21.0000000000858,85.7650079368374));
#117755=CARTESIAN_POINT('Ctrl Pts',(7.45468888847659,21.0000000000897,85.6658652185241));
#117756=CARTESIAN_POINT('Ctrl Pts',(7.57952991246622,21.0000000000568,85.5647153018767));
#117757=CARTESIAN_POINT('Ctrl Pts',(7.68167013643052,21.0000000000299,85.4819582496661));
#117758=CARTESIAN_POINT('Ctrl Pts',(7.78262481832806,20.9999999999972,85.3978567469911));
#117759=CARTESIAN_POINT('Ctrl Pts',(7.88252783227743,20.9999999999972,85.3123017409167));
#117760=CARTESIAN_POINT('Ctrl Pts',(7.94500648545622,20.9999999999972,85.2587962325149));
#117761=CARTESIAN_POINT('Ctrl Pts',(8.00707501935217,21.0000000000007,85.2047245834137));
#117762=CARTESIAN_POINT('Ctrl Pts',(8.06876006198254,20.9999999999989,85.1500566565699));
#117763=CARTESIAN_POINT('Ctrl Pts',(8.19199549949309,20.9999999999952,85.0408401334858));
#117764=CARTESIAN_POINT('Ctrl Pts',(8.31370272600517,21.0000000000204,84.9292458792537));
#117765=CARTESIAN_POINT('Ctrl Pts',(8.4340961907889,21.0000000000293,84.8150402865715));
#117766=CARTESIAN_POINT('Ctrl Pts',(8.51332555497591,21.0000000000352,84.7398830800648));
#117767=CARTESIAN_POINT('Ctrl Pts',(8.59198518630918,20.9999999999972,84.6635942037091));
#117768=CARTESIAN_POINT('Ctrl Pts',(8.67012689091576,20.9999999999972,84.5860990407983));
#117769=CARTESIAN_POINT('Ctrl Pts',(8.74384121285911,20.9999999999972,84.5129946285434));
#117770=CARTESIAN_POINT('Ctrl Pts',(8.8171026280427,21.0000000000352,84.4388238577954));
#117771=CARTESIAN_POINT('Ctrl Pts',(8.88988045449224,21.0000000000318,84.3635930688318));
#117772=CARTESIAN_POINT('Ctrl Pts',(9.0701638994232,21.0000000000234,84.1772332053831));
#117773=CARTESIAN_POINT('Ctrl Pts',(9.24747949353293,21.0000000000373,83.9843643404513));
#117774=CARTESIAN_POINT('Ctrl Pts',(9.42147268297582,21.0000000000345,83.7851882666207));
#117775=CARTESIAN_POINT('',(1.21030572547832,22.7988981836224,90.3337691724699));
#117776=CARTESIAN_POINT('Origin',(0.756612526612343,22.5000005075418,88.9355510391788));
#117777=CARTESIAN_POINT('Ctrl Pts',(12.6211182849899,23.194988543039,81.5466562879185));
#117778=CARTESIAN_POINT('Ctrl Pts',(12.4932187937712,23.2005913915118,81.7639926710847));
#117779=CARTESIAN_POINT('Ctrl Pts',(12.3627405816846,23.2058937154176,81.9773859230737));
#117780=CARTESIAN_POINT('Ctrl Pts',(12.2297445484923,23.2108375253335,82.1867818886298));
#117781=CARTESIAN_POINT('Ctrl Pts',(12.0799119016713,23.2164071961522,82.4226863062268));
#117782=CARTESIAN_POINT('Ctrl Pts',(11.9268841365456,23.2215219023617,82.6535157173191));
#117783=CARTESIAN_POINT('Ctrl Pts',(11.770784498812,23.2261014255578,82.8791446435673));
#117784=CARTESIAN_POINT('Ctrl Pts',(11.6733482848867,23.2289599293204,83.0199805138157));
#117785=CARTESIAN_POINT('Ctrl Pts',(11.5747152411408,23.2316099698021,83.1587912947737));
#117786=CARTESIAN_POINT('Ctrl Pts',(11.4749149002699,23.2340322162995,83.2955566725622));
#117787=CARTESIAN_POINT('Ctrl Pts',(11.3162265942549,23.2378837281286,83.5130215222145));
#117788=CARTESIAN_POINT('Ctrl Pts',(11.1545882040806,23.2411594814845,83.725312223375));
#117789=CARTESIAN_POINT('Ctrl Pts',(10.9901795614978,23.2437806622171,83.9323201856936));
#117790=CARTESIAN_POINT('Ctrl Pts',(10.8850257656668,23.2454571379745,84.0647199954788));
#117791=CARTESIAN_POINT('Ctrl Pts',(10.7787384305381,23.246865819069,84.1949598703842));
#117792=CARTESIAN_POINT('Ctrl Pts',(10.6713609019886,23.2479852956996,84.3230218260961));
#117793=CARTESIAN_POINT('Ctrl Pts',(10.5941883156074,23.248789867272,84.4150603789743));
#117794=CARTESIAN_POINT('Ctrl Pts',(10.5164525980134,23.2494450421076,84.5059741148954));
#117795=CARTESIAN_POINT('Ctrl Pts',(10.4381795739186,23.24994255375,84.5957555369526));
#117796=CARTESIAN_POINT('Ctrl Pts',(10.2676153414658,23.2510266781007,84.7913976437804));
#117797=CARTESIAN_POINT('Ctrl Pts',(10.0944510855359,23.2513968052464,84.9816931937978));
#117798=CARTESIAN_POINT('Ctrl Pts',(9.918759213001,23.2510526136532,85.1666740707244));
#117799=CARTESIAN_POINT('Ctrl Pts',(9.88699239518467,23.2509903804293,85.2001204318568));
#117800=CARTESIAN_POINT('Ctrl Pts',(9.85514281024508,23.2509047730507,85.2333930675873));
#117801=CARTESIAN_POINT('Ctrl Pts',(9.82321071099612,23.2507957610793,85.2664921901425));
#117802=CARTESIAN_POINT('Ctrl Pts',(9.65324116957873,23.2502155075031,85.4426736130474));
#117803=CARTESIAN_POINT('Ctrl Pts',(9.48093802884081,23.2489727089887,85.613939274566));
#117804=CARTESIAN_POINT('Ctrl Pts',(9.30643613027418,23.2470585771029,85.7803407810742));
#117805=CARTESIAN_POINT('Ctrl Pts',(9.27598738730181,23.2467245812536,85.8093760909677));
#117806=CARTESIAN_POINT('Ctrl Pts',(9.24547157334416,23.2463701281518,85.8382632907172));
#117807=CARTESIAN_POINT('Ctrl Pts',(9.2148892476124,23.2459951489363,85.8670026333113));
#117808=CARTESIAN_POINT('Ctrl Pts',(9.12168396549575,23.2448523305685,85.9545910841644));
#117809=CARTESIAN_POINT('Ctrl Pts',(9.02785809547641,23.2435191969874,86.0408090358809));
#117810=CARTESIAN_POINT('Ctrl Pts',(8.93341171656685,23.2419982707098,86.1256702646693));
#117811=CARTESIAN_POINT('Ctrl Pts',(8.81461189297349,23.2400851664112,86.2324133619313));
#117812=CARTESIAN_POINT('Ctrl Pts',(8.6948307292937,23.2378749655979,86.337010199082));
#117813=CARTESIAN_POINT('Ctrl Pts',(8.57409648579421,23.2353716487655,86.4395061305676));
#117814=CARTESIAN_POINT('Ctrl Pts',(8.46573723845031,23.2331249164388,86.5314964530284));
#117815=CARTESIAN_POINT('Ctrl Pts',(8.35660744053645,23.2306439797656,86.6217952727136));
#117816=CARTESIAN_POINT('Ctrl Pts',(8.24671423456762,23.2279295907953,86.7104347179882));
#117817=CARTESIAN_POINT('Ctrl Pts',(8.19176763158321,23.2265723963101,86.7547544406254));
#117818=CARTESIAN_POINT('Ctrl Pts',(8.13663010537614,23.2251567756296,86.7986592337719));
#117819=CARTESIAN_POINT('Ctrl Pts',(8.08130107438259,23.2236822322506,86.8421534874745));
#117820=CARTESIAN_POINT('Ctrl Pts',(8.05363655888582,23.2229449605611,86.8639006143258));
#117821=CARTESIAN_POINT('Ctrl Pts',(8.02592416291969,23.2221929539408,86.8855450991431));
#117822=CARTESIAN_POINT('Ctrl Pts',(7.99816380423124,23.2214261205358,86.9070874391833));
#117823=CARTESIAN_POINT('Ctrl Pts',(7.99636893047286,23.221376540155,86.9084802807264));
#117824=CARTESIAN_POINT('Ctrl Pts',(7.9945738562225,23.2213268977379,86.9098726952744));
#117825=CARTESIAN_POINT('Ctrl Pts',(7.99277858143012,23.2212771933182,86.911264682935));
#117826=CARTESIAN_POINT('Ctrl Pts',(7.9806905755884,23.2209425218144,86.920637262021));
#117827=CARTESIAN_POINT('Ctrl Pts',(7.96859347796431,23.2206050393413,86.9299904876475));
#117828=CARTESIAN_POINT('Ctrl Pts',(7.95648730188297,23.2202647561823,86.9393244303098));
#117829=CARTESIAN_POINT('Ctrl Pts',(7.94953522715104,23.2200693456797,86.9446845263877));
#117830=CARTESIAN_POINT('Ctrl Pts',(7.9425801585374,23.2198730116799,86.9500382634073));
#117831=CARTESIAN_POINT('Ctrl Pts',(7.93562209831243,23.2196757561466,86.9553856546025));
#117832=CARTESIAN_POINT('Ctrl Pts',(7.92866403808747,23.2194785006134,86.9607330457977));
#117833=CARTESIAN_POINT('Ctrl Pts',(7.92337482480999,23.2193281201649,86.9647934011114));
#117834=CARTESIAN_POINT('Ctrl Pts',(7.91473894495999,23.2190812268188,86.9714088038817));
#117835=CARTESIAN_POINT('Ctrl Pts',(7.75412374001771,23.2144893582334,87.0944459801958));
#117836=CARTESIAN_POINT('Ctrl Pts',(7.59313440095865,23.2092503649804,87.213320286633));
#117837=CARTESIAN_POINT('Ctrl Pts',(7.43187198895906,23.2034201191061,87.3282788054784));
#117838=CARTESIAN_POINT('Ctrl Pts',(7.28392337804805,23.1980712174763,87.4337463658644));
#117839=CARTESIAN_POINT('Ctrl Pts',(7.13574410135277,23.1922245520801,87.5359175245917));
#117840=CARTESIAN_POINT('Ctrl Pts',(6.98738482421358,23.1859233657266,87.6349560317578));
#117841=CARTESIAN_POINT('Ctrl Pts',(6.82499126114028,23.1790261084519,87.7433632467989));
#117842=CARTESIAN_POINT('Ctrl Pts',(6.66238224676357,23.1715841250771,87.8480182462217));
#117843=CARTESIAN_POINT('Ctrl Pts',(6.49962387552277,23.1636562178235,87.9492019279517));
#117844=CARTESIAN_POINT('Ctrl Pts',(6.33000192396702,23.1553939878082,88.0546525627166));
#117845=CARTESIAN_POINT('Ctrl Pts',(6.1602174231917,23.1466038280092,88.1563328656577));
#117846=CARTESIAN_POINT('Ctrl Pts',(5.99031550141526,23.1373568935397,88.2545137117141));
#117847=CARTESIAN_POINT('Ctrl Pts',(5.97629193379932,23.1365936590253,88.2626174795754));
#117848=CARTESIAN_POINT('Ctrl Pts',(5.96226755183385,23.1358273159182,88.27069738153));
#117849=CARTESIAN_POINT('Ctrl Pts',(5.94824237341941,23.1350579060704,88.2787535565813));
#117850=CARTESIAN_POINT('Ctrl Pts',(5.77104788922942,23.1253371612015,88.3805354905128));
#117851=CARTESIAN_POINT('Ctrl Pts',(5.59372812088921,23.1151261986145,88.4785346318076));
#117852=CARTESIAN_POINT('Ctrl Pts',(5.41629450000383,23.1045139189269,88.5731175903428));
#117853=CARTESIAN_POINT('Ctrl Pts',(5.24819748102698,23.0944600600745,88.6627235697307));
#117854=CARTESIAN_POINT('Ctrl Pts',(5.07999774069339,23.084046009247,88.7492625038068));
#117855=CARTESIAN_POINT('Ctrl Pts',(4.9116901409163,23.073355125837,88.8330064906868));
#117856=CARTESIAN_POINT('Ctrl Pts',(4.7973680441979,23.0660933966648,88.8898891756063));
#117857=CARTESIAN_POINT('Ctrl Pts',(4.68299588668316,23.0587041056104,88.9454816003795));
#117858=CARTESIAN_POINT('Ctrl Pts',(4.56855907778642,23.0512155486768,88.9998818145646));
#117859=CARTESIAN_POINT('Ctrl Pts',(4.33172366852101,23.0357174282444,89.1124670667651));
#117860=CARTESIAN_POINT('Ctrl Pts',(4.0945289701563,23.0197040987167,89.2200241428719));
#117861=CARTESIAN_POINT('Ctrl Pts',(3.85733585746382,23.0031940856782,89.3232234871173));
#117862=CARTESIAN_POINT('Ctrl Pts',(3.82513871686922,23.0009529784007,89.337232004305));
#117863=CARTESIAN_POINT('Ctrl Pts',(3.79294157723204,22.9987027283982,89.3511601537571));
#117864=CARTESIAN_POINT('Ctrl Pts',(3.76074531545843,22.9964433907818,89.3650095465169));
#117865=CARTESIAN_POINT('Ctrl Pts',(3.50417118157362,22.9784385802809,89.4753762709885));
#117866=CARTESIAN_POINT('Ctrl Pts',(3.24765436648079,22.9598558973906,89.5807460605779));
#117867=CARTESIAN_POINT('Ctrl Pts',(2.99145622685065,22.9407283360055,89.6820323373258));
#117868=CARTESIAN_POINT('Ctrl Pts',(2.80669244682127,22.926934010452,89.7550775022285));
#117869=CARTESIAN_POINT('Ctrl Pts',(2.62209396769549,22.9128564807424,89.8259975035371));
#117870=CARTESIAN_POINT('Ctrl Pts',(2.4377532614348,22.898511215253,89.8951196997858));
#117871=CARTESIAN_POINT('Ctrl Pts',(2.13718806689121,22.8751214409591,90.0078225682093));
#117872=CARTESIAN_POINT('Ctrl Pts',(1.83730931686889,22.851018863972,90.1157480463776));
#117873=CARTESIAN_POINT('Ctrl Pts',(1.53825824495239,22.8262860812645,90.220267935109));
#117874=CARTESIAN_POINT('Ctrl Pts',(1.4288217069242,22.8172352188216,90.2585165683761));
#117875=CARTESIAN_POINT('Ctrl Pts',(1.3194957728693,22.8081001505928,90.2963086713995));
#117876=CARTESIAN_POINT('Ctrl Pts',(1.2102865960548,22.7988855800353,90.3337102128107));
#117877=CARTESIAN_POINT('Ctrl Pts',(-1.18612654204091,23.08684060709,90.8056390119699));
#117878=CARTESIAN_POINT('Ctrl Pts',(-1.02638895989091,23.08684060709,90.77605244985));
#117879=CARTESIAN_POINT('Ctrl Pts',(-0.683862091540912,23.08684060709,90.71121995565));
#117880=CARTESIAN_POINT('Ctrl Pts',(-0.161822890870914,23.08684060709,90.60439269897));
#117881=CARTESIAN_POINT('Ctrl Pts',(0.363860643519087,23.08684060709,90.48319011439));
#117882=CARTESIAN_POINT('Ctrl Pts',(0.845214580869085,23.08684060709,90.3551094761801));
#117883=CARTESIAN_POINT('Ctrl Pts',(1.17290328465909,23.08684060709,90.25335018102));
#117884=CARTESIAN_POINT('Ctrl Pts',(1.33589618381909,23.08684060709,90.19751377573));
#117885=CARTESIAN_POINT('Ctrl Pts',(1.35880646243909,23.08684060709,90.1895581012301));
#117886=CARTESIAN_POINT('Ctrl Pts',(-1.08807919910092,21.82055786604,91.33494523279));
#117887=CARTESIAN_POINT('Ctrl Pts',(-0.926943055190917,21.82055786604,91.30509987628));
#117888=CARTESIAN_POINT('Ctrl Pts',(-0.580391297820914,21.82055786604,91.23951081764));
#117889=CARTESIAN_POINT('Ctrl Pts',(-0.0482616351409153,21.82055786604,
91.13064340811));
#117890=CARTESIAN_POINT('Ctrl Pts',(0.492565115739089,21.82055786604,91.00598854667));
#117891=CARTESIAN_POINT('Ctrl Pts',(0.993006855569089,21.82055786604,90.87289106935));
#117892=CARTESIAN_POINT('Ctrl Pts',(1.33813198802909,21.82055786604,90.76576936584));
#117893=CARTESIAN_POINT('Ctrl Pts',(1.51105882888909,21.82055786604,90.7065309896001));
#117894=CARTESIAN_POINT('Ctrl Pts',(1.53539056153909,21.82055786604,90.69808194737));
#117895=CARTESIAN_POINT('Ctrl Pts',(-1.24665752627091,20.75508697312,90.47886395057));
#117896=CARTESIAN_POINT('Ctrl Pts',(-1.08778336701091,20.75508697312,90.4494371590201));
#117897=CARTESIAN_POINT('Ctrl Pts',(-0.747741323710916,20.75508697312,90.3850717411299));
#117898=CARTESIAN_POINT('Ctrl Pts',(-0.231931619720914,20.75508697312,90.27950400312));
#117899=CARTESIAN_POINT('Ctrl Pts',(0.284403024929085,20.75508697312,90.16043273296));
#117900=CARTESIAN_POINT('Ctrl Pts',(0.753972823749085,20.75508697312,90.03544931493));
#117901=CARTESIAN_POINT('Ctrl Pts',(1.07089688918909,20.75508697312,89.93700058226));
#117902=CARTESIAN_POINT('Ctrl Pts',(1.22775692180909,20.75508697312,89.8832644342999));
#117903=CARTESIAN_POINT('Ctrl Pts',(1.24978964464909,20.75508697312,89.87561334769));
#117904=CARTESIAN_POINT('Ctrl Pts',(-1.49220764661091,21.03031426069,89.1532675363799));
#117905=CARTESIAN_POINT('Ctrl Pts',(-1.33683605048091,21.03031426069,89.1244888704399));
#117906=CARTESIAN_POINT('Ctrl Pts',(-1.00687395381091,21.03031426069,89.06201819526));
#117907=CARTESIAN_POINT('Ctrl Pts',(-0.516334839390912,21.03031426069,88.96155982342));
#117908=CARTESIAN_POINT('Ctrl Pts',(-0.0379249208809143,21.03031426069,
88.85113444793));
#117909=CARTESIAN_POINT('Ctrl Pts',(0.383841316339086,21.03031426069,88.7387152199099));
#117910=CARTESIAN_POINT('Ctrl Pts',(0.657097526779088,21.03031426069,88.65369612211));
#117911=CARTESIAN_POINT('Ctrl Pts',(0.789078959859088,21.03031426069,88.6084798825201));
#117912=CARTESIAN_POINT('Ctrl Pts',(0.807551788049085,21.03031426069,88.60206438782));
#117913=CARTESIAN_POINT('',(-1.28513099060542,21.0000000000039,89.419838384476));
#117914=CARTESIAN_POINT('Ctrl Pts',(-1.28513097334713,21.,89.4198384761759));
#117915=CARTESIAN_POINT('Ctrl Pts',(-1.13188223424533,21.,89.3909954656273));
#117916=CARTESIAN_POINT('Ctrl Pts',(-0.828434316537085,21.,89.3323920366554));
#117917=CARTESIAN_POINT('Ctrl Pts',(-0.374817752490913,20.99999999999,89.23726971619));
#117918=CARTESIAN_POINT('Ctrl Pts',(0.0523864881590876,21.00000000004,89.1373009151));
#117919=CARTESIAN_POINT('Ctrl Pts',(0.441186856229087,20.99999999984,89.03383812529));
#117920=CARTESIAN_POINT('Ctrl Pts',(0.657536503429089,21.00000000035,88.96773970165));
#117921=CARTESIAN_POINT('Ctrl Pts',(0.756634314019088,21.00000000035,88.9355837865));
#117922=CARTESIAN_POINT('',(-1.00773525083376,22.4999925247862,90.8939704740664));
#117923=CARTESIAN_POINT('Origin',(-1.28513134966091,22.5,89.41983613899));
#117924=CARTESIAN_POINT('Ctrl Pts',(-1.00769979882528,22.4999592529598,
90.8939685470445));
#117925=CARTESIAN_POINT('Ctrl Pts',(-0.957084251150433,22.5061488705642,
90.8844393268669));
#117926=CARTESIAN_POINT('Ctrl Pts',(-0.906738505136563,22.5123434672732,
90.8748395747033));
#117927=CARTESIAN_POINT('Ctrl Pts',(-0.856658827927557,22.5185434703929,
90.8651548009734));
#117928=CARTESIAN_POINT('Ctrl Pts',(-0.731233690259289,22.5340714507668,
90.840899171823));
#117929=CARTESIAN_POINT('Ctrl Pts',(-0.607474509670458,22.5496351877152,
90.816110119547));
#117930=CARTESIAN_POINT('Ctrl Pts',(-0.485314354543676,22.565250802786,
90.7905920608092));
#117931=CARTESIAN_POINT('Ctrl Pts',(-0.366271594539289,22.5804679242382,
90.7657251953494));
#117932=CARTESIAN_POINT('Ctrl Pts',(-0.248747016584948,22.5957338562364,
90.7401660636045));
#117933=CARTESIAN_POINT('Ctrl Pts',(-0.132722430427957,22.6110410435462,
90.7137342806339));
#117934=CARTESIAN_POINT('Ctrl Pts',(-0.0187383588171168,22.6260790246524,
90.6877673511863));
#117935=CARTESIAN_POINT('Ctrl Pts',(0.0937983147043079,22.6411564272297,
90.6609582147743));
#117936=CARTESIAN_POINT('Ctrl Pts',(0.204857809483684,22.6562502661615,
90.6331362234104));
#117937=CARTESIAN_POINT('Ctrl Pts',(0.312787937670032,22.6709188001213,
90.6060981831215));
#117938=CARTESIAN_POINT('Ctrl Pts',(0.419323130664292,22.6856024750495,
90.5781035934115));
#117939=CARTESIAN_POINT('Ctrl Pts',(0.52438798738615,22.7002708090524,90.5489958293737));
#117940=CARTESIAN_POINT('Ctrl Pts',(0.577140084527384,22.7076356444918,
90.5343810890694));
#117941=CARTESIAN_POINT('Ctrl Pts',(0.629520735811119,22.7149964976842,
90.5194857203461));
#117942=CARTESIAN_POINT('Ctrl Pts',(0.6815154128319,22.7223490422761,90.504289854534));
#117943=CARTESIAN_POINT('Ctrl Pts',(0.79287133060566,22.7380958340233,90.471745184948));
#117944=CARTESIAN_POINT('Ctrl Pts',(0.902459500416484,22.7538032895651,
90.437822278412));
#117945=CARTESIAN_POINT('Ctrl Pts',(1.01020021045901,22.7694829094358,90.4023270529812));
#117946=CARTESIAN_POINT('Ctrl Pts',(1.07763762528111,22.7792971479819,90.3801097663061));
#117947=CARTESIAN_POINT('Ctrl Pts',(1.14435030260074,22.7891007041396,90.3572764595547));
#117948=CARTESIAN_POINT('Ctrl Pts',(1.21030897714296,22.7989003259575,90.3337791942256));
#117949=CARTESIAN_POINT('Ctrl Pts',(8.45816176827909,16.26511926842,98.7964653589499));
#117950=CARTESIAN_POINT('Ctrl Pts',(8.71225114275908,16.41477280571,98.6494070076199));
#117951=CARTESIAN_POINT('Ctrl Pts',(9.27881268981909,16.73006084598,98.30341626023));
#117952=CARTESIAN_POINT('Ctrl Pts',(10.1626398113191,17.16069654247,97.6962496853799));
#117953=CARTESIAN_POINT('Ctrl Pts',(11.1008309226691,17.54981639277,96.96627400869));
#117954=CARTESIAN_POINT('Ctrl Pts',(12.0284701745891,17.86984908755,96.1523318668001));
#117955=CARTESIAN_POINT('Ctrl Pts',(12.9325147810891,18.12067756051,95.26102236673));
#117956=CARTESIAN_POINT('Ctrl Pts',(13.8034582743191,18.30536666785,94.2997004316301));
#117957=CARTESIAN_POINT('Ctrl Pts',(14.6483615697391,18.43072561429,93.2588424428));
#117958=CARTESIAN_POINT('Ctrl Pts',(15.4901719996691,18.50141397362,92.10037160054));
#117959=CARTESIAN_POINT('Ctrl Pts',(16.3530907398691,18.51438369082,90.76409474325));
#117960=CARTESIAN_POINT('Ctrl Pts',(17.2403956363891,18.45914837749,89.19684938304));
#117961=CARTESIAN_POINT('Ctrl Pts',(18.1343401599191,18.32423291388,87.36260202144));
#117962=CARTESIAN_POINT('Ctrl Pts',(19.0033848293491,18.10320054974,85.24319884147));
#117963=CARTESIAN_POINT('Ctrl Pts',(19.7639909942691,17.81526535809,82.9702592037509));
#117964=CARTESIAN_POINT('Ctrl Pts',(20.1883444225591,17.59455708305,81.382235884647));
#117965=CARTESIAN_POINT('Ctrl Pts',(20.3703684052891,17.48632437673,80.615759308313));
#117966=CARTESIAN_POINT('Ctrl Pts',(6.31418014116909,15.43220418763,92.79563719768));
#117967=CARTESIAN_POINT('Ctrl Pts',(6.49200941171909,15.56346847277,92.67838236751));
#117968=CARTESIAN_POINT('Ctrl Pts',(6.88387432291909,15.84414338516,92.4035075448201));
#117969=CARTESIAN_POINT('Ctrl Pts',(7.48196966441909,16.24577547329,91.9242120499101));
#117970=CARTESIAN_POINT('Ctrl Pts',(8.10612356461909,16.6365848729,91.3501649846601));
#117971=CARTESIAN_POINT('Ctrl Pts',(8.71750994518909,16.99297183984,90.71045662041));
#117972=CARTESIAN_POINT('Ctrl Pts',(9.3124519476191,17.31472032014,90.0082381109));
#117973=CARTESIAN_POINT('Ctrl Pts',(9.88895414563909,17.60257331209,89.2471181028301));
#117974=CARTESIAN_POINT('Ctrl Pts',(10.4549508437891,17.8618188302,88.41744323317));
#117975=CARTESIAN_POINT('Ctrl Pts',(11.0287137839791,18.10025681166,87.4864837035));
#117976=CARTESIAN_POINT('Ctrl Pts',(11.6304101411391,18.32271215478,86.40251363781));
#117977=CARTESIAN_POINT('Ctrl Pts',(12.2670974264291,18.52555248364,85.11784149556));
#117978=CARTESIAN_POINT('Ctrl Pts',(12.9309003101591,18.69913435731,83.5979370835401));
#117979=CARTESIAN_POINT('Ctrl Pts',(13.6016889453491,18.83244677012,81.8239640921051));
#117980=CARTESIAN_POINT('Ctrl Pts',(14.2139669773891,18.91249476228,79.9062655709491));
#117981=CARTESIAN_POINT('Ctrl Pts',(14.5696327416291,18.93553052461,78.560927762134));
#117982=CARTESIAN_POINT('Ctrl Pts',(14.7249351849991,18.94108956235,77.911474252923));
#117983=CARTESIAN_POINT('Ctrl Pts',(2.54935064044909,19.22183178223,89.2228044174901));
#117984=CARTESIAN_POINT('Ctrl Pts',(2.74816966526909,19.38069675838,89.11271227861));
#117985=CARTESIAN_POINT('Ctrl Pts',(3.18450270870909,19.72231812323,88.8567707992701));
#117986=CARTESIAN_POINT('Ctrl Pts',(3.84607183220909,20.21957457743,88.41774917846));
#117987=CARTESIAN_POINT('Ctrl Pts',(4.53420387286909,20.71569136082,87.89920721743));
#117988=CARTESIAN_POINT('Ctrl Pts',(5.20913049307909,21.18237918094,87.3269794904301));
#117989=CARTESIAN_POINT('Ctrl Pts',(5.86983667115909,21.61932357701,86.70255461879));
#117990=CARTESIAN_POINT('Ctrl Pts',(6.5166169471191,22.02651478544,86.02752892074));
#117991=CARTESIAN_POINT('Ctrl Pts',(7.16026643121909,22.41003287152,85.29176070735));
#117992=CARTESIAN_POINT('Ctrl Pts',(7.82357909374909,22.78105285215,84.46472655768));
#117993=CARTESIAN_POINT('Ctrl Pts',(8.5330095959891,23.14891805727,83.49874325701));
#117994=CARTESIAN_POINT('Ctrl Pts',(9.30144695145909,23.51183300341,82.349167312438));
#117995=CARTESIAN_POINT('Ctrl Pts',(10.1247389211891,23.8583235636,80.982966536629));
#117996=CARTESIAN_POINT('Ctrl Pts',(10.9831261496691,24.1725563834,79.382122199941));
#117997=CARTESIAN_POINT('Ctrl Pts',(11.7956651902091,24.42485648488,77.6476829007421));
#117998=CARTESIAN_POINT('Ctrl Pts',(12.2871279910191,24.55396132786,76.431541471836));
#117999=CARTESIAN_POINT('Ctrl Pts',(12.5064116716291,24.60764795684,75.845400513527));
#118000=CARTESIAN_POINT('Ctrl Pts',(-0.111615554140913,24.89134380645,90.66372486418));
#118001=CARTESIAN_POINT('Ctrl Pts',(0.19025221778909,25.10382403371,90.53297074905));
#118002=CARTESIAN_POINT('Ctrl Pts',(0.85803534504909,25.557842799,90.23007744772));
#118003=CARTESIAN_POINT('Ctrl Pts',(1.88634608190909,26.20614559666,89.71458517922));
#118004=CARTESIAN_POINT('Ctrl Pts',(2.97016886586909,26.83497373368,89.11095423698));
#118005=CARTESIAN_POINT('Ctrl Pts',(4.04244300886909,27.40608121153,88.4506164042799));
#118006=CARTESIAN_POINT('Ctrl Pts',(5.09618479047909,27.91912696323,87.73638641167));
#118007=CARTESIAN_POINT('Ctrl Pts',(6.1271003298391,28.37546235392,86.9710385745999));
#118008=CARTESIAN_POINT('Ctrl Pts',(7.14876251537909,28.78369951161,86.14393771161));
#118009=CARTESIAN_POINT('Ctrl Pts',(8.19441250288909,29.15618061071,85.2220293390399));
#118010=CARTESIAN_POINT('Ctrl Pts',(9.30256349945909,29.50014277728,84.1543224935201));
#118011=CARTESIAN_POINT('Ctrl Pts',(10.4897674388291,29.80928089036,82.894592873641));
#118012=CARTESIAN_POINT('Ctrl Pts',(11.7467525600991,30.0679526902,81.410216850361));
#118013=CARTESIAN_POINT('Ctrl Pts',(13.0428227217091,30.25874444737,79.684901641459));
#118014=CARTESIAN_POINT('Ctrl Pts',(14.2592774845091,30.36290197067,77.829109904896));
#118015=CARTESIAN_POINT('Ctrl Pts',(14.9927419533391,30.38363581186,76.53517273404));
#118016=CARTESIAN_POINT('Ctrl Pts',(15.3204046577991,30.3849546111,75.912812767194));
#118017=CARTESIAN_POINT('',(0.214734006960575,24.6920295183809,90.5121348736941));
#118018=CARTESIAN_POINT('Origin',(4.08666499754585,24.6942623759682,99.1828508702515));
#118019=CARTESIAN_POINT('Ctrl Pts',(0.214734710864216,24.6920295184668,
90.5121364516904));
#118020=CARTESIAN_POINT('Ctrl Pts',(0.448085072341334,24.8703386629935,
90.408088292175));
#118021=CARTESIAN_POINT('Ctrl Pts',(0.682365291824861,25.0409638010153,
90.2997216953764));
#118022=CARTESIAN_POINT('Ctrl Pts',(0.916972181677289,25.2039041524456,
90.1870952943443));
#118023=CARTESIAN_POINT('Ctrl Pts',(1.18245519028357,25.3882887404188,90.0596463698336));
#118024=CARTESIAN_POINT('Ctrl Pts',(1.44835601157772,25.5628320122888,89.9267421084685));
#118025=CARTESIAN_POINT('Ctrl Pts',(1.7139478183002,25.7276223328341,89.788483032972));
#118026=CARTESIAN_POINT('Ctrl Pts',(1.80455090592196,25.7838383435456,89.741317801159));
#118027=CARTESIAN_POINT('Ctrl Pts',(1.89511814408961,25.8389196837459,89.6935296954762));
#118028=CARTESIAN_POINT('Ctrl Pts',(1.98562111022021,25.8928708578754,89.645123576841));
#118029=CARTESIAN_POINT('Ctrl Pts',(1.99510975164078,25.8985272840393,89.6400485133162));
#118030=CARTESIAN_POINT('Ctrl Pts',(2.00459768683022,25.9041712877118,89.6349666568877));
#118031=CARTESIAN_POINT('Ctrl Pts',(2.01408488454097,25.9098028720523,89.6298780152039));
#118032=CARTESIAN_POINT('Ctrl Pts',(2.27638611268886,26.0655044326133,89.4891876866217));
#118033=CARTESIAN_POINT('Ctrl Pts',(2.5381215790732,26.2117095514659,89.3433083869172));
#118034=CARTESIAN_POINT('Ctrl Pts',(2.79864368999521,26.3485037793546,89.1924156666076));
#118035=CARTESIAN_POINT('Ctrl Pts',(2.83590914671666,26.3680710220776,89.1708317552905));
#118036=CARTESIAN_POINT('Ctrl Pts',(2.87314982374135,26.3874457695934,89.1491453083512));
#118037=CARTESIAN_POINT('Ctrl Pts',(2.91036387529036,26.4066283314947,89.1273568819364));
#118038=CARTESIAN_POINT('Ctrl Pts',(2.95962816543374,26.4320223763747,89.0985131705966));
#118039=CARTESIAN_POINT('Ctrl Pts',(3.00884579357381,26.4570796201783,89.0694907422277));
#118040=CARTESIAN_POINT('Ctrl Pts',(3.05801251725147,26.4818008189935,89.0402909133547));
#118041=CARTESIAN_POINT('Ctrl Pts',(3.15723971555294,26.5316925976924,88.9813604621628));
#118042=CARTESIAN_POINT('Ctrl Pts',(3.25625952770616,26.5802156066599,88.9217074232645));
#118043=CARTESIAN_POINT('Ctrl Pts',(3.35503904348991,26.6273747875817,88.8613446270082));
#118044=CARTESIAN_POINT('Ctrl Pts',(3.42890125067334,26.6626379812125,88.8162084535023));
#118045=CARTESIAN_POINT('Ctrl Pts',(3.50262907322627,26.6971386911426,88.7706754717244));
#118046=CARTESIAN_POINT('Ctrl Pts',(3.57620910916385,26.7308791747741,88.724751175111));
#118047=CARTESIAN_POINT('Ctrl Pts',(3.61299912713264,26.7477494165898,88.7017890268044));
#118048=CARTESIAN_POINT('Ctrl Pts',(3.64975220037152,26.7644296018314,88.6787290532671));
#118049=CARTESIAN_POINT('Ctrl Pts',(3.68646667213144,26.7809200510704,88.6555719581755));
#118050=CARTESIAN_POINT('Ctrl Pts',(3.71420411411316,26.7933784321145,88.6380769881874));
#118051=CARTESIAN_POINT('Ctrl Pts',(3.74287781855371,26.8061518366951,88.6199185032941));
#118052=CARTESIAN_POINT('Ctrl Pts',(3.77031481493722,26.8182802241769,88.6024743503514));
#118053=CARTESIAN_POINT('Ctrl Pts',(3.77919460759156,26.8222054922552,88.5968286718305));
#118054=CARTESIAN_POINT('Ctrl Pts',(3.78794498704772,26.8260634946765,88.5912580810618));
#118055=CARTESIAN_POINT('Ctrl Pts',(3.79649264115169,26.8298225071378,88.5858100219609));
#118056=CARTESIAN_POINT('Ctrl Pts',(3.90574097342447,26.877866781906,88.516177890892));
#118057=CARTESIAN_POINT('Ctrl Pts',(4.01538651343084,26.924563711977,88.4452071775689));
#118058=CARTESIAN_POINT('Ctrl Pts',(4.12536961495221,26.9698843234981,88.3728825083693));
#118059=CARTESIAN_POINT('Ctrl Pts',(4.38795683492624,27.0780883404992,88.2002056738561));
#118060=CARTESIAN_POINT('Ctrl Pts',(4.65246842891141,27.1784438479384,88.0198092728228));
#118061=CARTESIAN_POINT('Ctrl Pts',(4.91808261803891,27.2705546094886,87.8315435610201));
#118062=CARTESIAN_POINT('Ctrl Pts',(5.00364879866118,27.3002275952803,87.7708947758253));
#118063=CARTESIAN_POINT('Ctrl Pts',(5.08932938844843,27.3290453301415,87.7094295101056));
#118064=CARTESIAN_POINT('Ctrl Pts',(5.17509696863496,27.3569956224824,87.6471432192937));
#118065=CARTESIAN_POINT('Ctrl Pts',(5.44404841356497,27.4446426272707,87.4518248032119));
#118066=CARTESIAN_POINT('Ctrl Pts',(5.71385425895366,27.5237565399761,87.2484310772638));
#118067=CARTESIAN_POINT('Ctrl Pts',(5.98365442899377,27.5939687504165,87.0368916265424));
#118068=CARTESIAN_POINT('Ctrl Pts',(6.05136012798605,27.6115883345144,86.9838063139075));
#118069=CARTESIAN_POINT('Ctrl Pts',(6.11906554879761,27.628647551287,86.9302081419426));
#118070=CARTESIAN_POINT('Ctrl Pts',(6.18675729780204,27.6451410027722,86.8760962144203));
#118071=CARTESIAN_POINT('Ctrl Pts',(6.24335188846402,27.658930573128,86.8308552148436));
#118072=CARTESIAN_POINT('Ctrl Pts',(6.29993692536935,27.672324676065,86.7852550990612));
#118073=CARTESIAN_POINT('Ctrl Pts',(6.35650433239512,27.68532020831,86.7392959497498));
#118074=CARTESIAN_POINT('Ctrl Pts',(6.49958850185862,27.7181916980208,86.6230447893338));
#118075=CARTESIAN_POINT('Ctrl Pts',(6.64255971585015,27.7485128921454,86.5044963583867));
#118076=CARTESIAN_POINT('Ctrl Pts',(6.7852886742244,27.7762356542623,86.3836534502605));
#118077=CARTESIAN_POINT('Ctrl Pts',(6.85665315341153,27.7900970353207,86.3232319961974));
#118078=CARTESIAN_POINT('Ctrl Pts',(6.92795709856489,27.8033088083776,86.2622369578808));
#118079=CARTESIAN_POINT('Ctrl Pts',(6.99918458829304,27.8158652735421,86.2006688566683));
#118080=CARTESIAN_POINT('Ctrl Pts',(7.03479833315711,27.8221435061243,86.169884806062));
#118081=CARTESIAN_POINT('Ctrl Pts',(7.07039296614475,27.8282579117335,86.1389574921));
#118082=CARTESIAN_POINT('Ctrl Pts',(7.1059665142924,27.834207785269,86.1078869900565));
#118083=CARTESIAN_POINT('Ctrl Pts',(7.12375328836623,27.8371827220367,86.0923517390348));
#118084=CARTESIAN_POINT('Ctrl Pts',(7.1415347913618,27.8401165257861,86.0767806911431));
#118085=CARTESIAN_POINT('Ctrl Pts',(7.15931077778746,27.8430091094421,86.0611738564153));
#118086=CARTESIAN_POINT('Ctrl Pts',(7.16020518693599,27.8431546514797,86.0603885894025));
#118087=CARTESIAN_POINT('Ctrl Pts',(7.16110281836779,27.8433006095559,86.0596003904142));
#118088=CARTESIAN_POINT('Ctrl Pts',(7.16200318248296,27.8434469037773,86.0588096872644));
#118089=CARTESIAN_POINT('Ctrl Pts',(7.17899715712277,27.8462081425327,86.0438855148673));
#118090=CARTESIAN_POINT('Ctrl Pts',(7.19696213785824,27.8490860148214,86.0280666995787));
#118091=CARTESIAN_POINT('Ctrl Pts',(7.2126219330494,27.8515631175667,86.014246018903));
#118092=CARTESIAN_POINT('Ctrl Pts',(7.3955209150022,27.8804945029882,85.8528270223818));
#118093=CARTESIAN_POINT('Ctrl Pts',(7.58290941906807,27.9057765944473,85.6831190222835));
#118094=CARTESIAN_POINT('Ctrl Pts',(7.77409387939456,27.9268419894547,85.5047753250708));
#118095=CARTESIAN_POINT('Ctrl Pts',(7.89515415183026,27.9401808479279,85.3918459764464));
#118096=CARTESIAN_POINT('Ctrl Pts',(8.01773533519229,27.9518288665838,85.2754541736625));
#118097=CARTESIAN_POINT('Ctrl Pts',(8.14165068493019,27.9616413427991,85.1555130160333));
#118098=CARTESIAN_POINT('Ctrl Pts',(8.33529254401225,27.9769752472796,84.9680816058579));
#118099=CARTESIAN_POINT('Ctrl Pts',(8.532195054996,27.9878261331155,84.7719813593696));
#118100=CARTESIAN_POINT('Ctrl Pts',(8.73159286517084,27.9936606308062,84.5669176085115));
#118101=CARTESIAN_POINT('Ctrl Pts',(8.87368832939101,27.9978184280114,84.4207844646853));
#118102=CARTESIAN_POINT('Ctrl Pts',(9.01704988471146,27.9994288667593,84.2700997131144));
#118103=CARTESIAN_POINT('Ctrl Pts',(9.16138571517198,27.9983013850854,84.1147624618979));
#118104=CARTESIAN_POINT('Ctrl Pts',(9.35575610573425,27.9967830576361,83.9055769665743));
#118105=CARTESIAN_POINT('Ctrl Pts',(9.55189495406335,27.9902984775844,83.6879527320489));
#118106=CARTESIAN_POINT('Ctrl Pts',(9.74904736009992,27.9784210280426,83.4616906788339));
#118107=CARTESIAN_POINT('Ctrl Pts',(9.75943215812474,27.9777953957359,83.4497725604069));
#118108=CARTESIAN_POINT('Ctrl Pts',(9.76981975905456,27.9771548047027,83.4378304824439));
#118109=CARTESIAN_POINT('Ctrl Pts',(9.78021004950441,27.9764991939486,83.4258644180379));
#118110=CARTESIAN_POINT('Ctrl Pts',(9.93003295121258,27.9670456078297,83.2533196273041));
#118111=CARTESIAN_POINT('Ctrl Pts',(10.0804161000811,27.9544685945203,83.0757866926596));
#118112=CARTESIAN_POINT('Ctrl Pts',(10.2310127297883,27.9385884831185,82.8931903393292));
#118113=CARTESIAN_POINT('Ctrl Pts',(10.2319927570955,27.9384851412121,82.8920020696262));
#118114=CARTESIAN_POINT('Ctrl Pts',(10.2329727934239,27.938381659436,82.8908135854978));
#118115=CARTESIAN_POINT('Ctrl Pts',(10.233952838676,27.9382780377418,82.8896248869249));
#118116=CARTESIAN_POINT('Ctrl Pts',(10.3082724870422,27.930420106831,82.799482457522));
#118117=CARTESIAN_POINT('Ctrl Pts',(10.3826435118955,27.9217575070292,82.7081067746664));
#118118=CARTESIAN_POINT('Ctrl Pts',(10.4570232118485,27.9122715604355,82.615491198011));
#118119=CARTESIAN_POINT('Ctrl Pts',(10.494703480398,27.9074660420573,82.5685727538327));
#118120=CARTESIAN_POINT('Ctrl Pts',(10.5323859748428,27.902449222046,82.5213361058194));
#118121=CARTESIAN_POINT('Ctrl Pts',(10.5700650950581,27.8972187339656,82.4737804394676));
#118122=CARTESIAN_POINT('Ctrl Pts',(10.5889046551658,27.8946034899254,82.4500026062917));
#118123=CARTESIAN_POINT('Ctrl Pts',(10.6077433716528,27.8919348288679,82.4261450184844));
#118124=CARTESIAN_POINT('Ctrl Pts',(10.6265805403487,27.8892124574999,82.4022075787539));
#118125=CARTESIAN_POINT('Ctrl Pts',(10.6359991246967,27.8878512718159,82.3902388588887));
#118126=CARTESIAN_POINT('Ctrl Pts',(10.6454173220933,27.8864766585542,82.3782501760398));
#118127=CARTESIAN_POINT('Ctrl Pts',(10.6548350442347,27.8850885813009,82.3662415183625));
#118128=CARTESIAN_POINT('Ctrl Pts',(10.6595439053054,27.8843945426743,82.3602371895238));
#118129=CARTESIAN_POINT('Ctrl Pts',(10.6642526475621,27.8836971380498,82.3542278669779));
#118130=CARTESIAN_POINT('Ctrl Pts',(10.6689612599484,27.8829963628918,82.348213549265));
#118131=CARTESIAN_POINT('Ctrl Pts',(10.6736698723347,27.8822955877338,82.3421992315521));
#118132=CARTESIAN_POINT('Ctrl Pts',(10.6795441809366,27.8814162537848,82.3346882475515));
#118133=CARTESIAN_POINT('Ctrl Pts',(10.6830866964339,27.8808839212869,82.3301556091715));
#118134=CARTESIAN_POINT('Ctrl Pts',(10.7537849753811,27.8702601169703,82.2396973647956));
#118135=CARTESIAN_POINT('Ctrl Pts',(10.8291598045365,27.8581390422069,82.1420941961379));
#118136=CARTESIAN_POINT('Ctrl Pts',(10.9088955347453,27.8442893594117,82.0371953640855));
#118137=CARTESIAN_POINT('Ctrl Pts',(10.9894121916854,27.8303040336935,81.9312691594636));
#118138=CARTESIAN_POINT('Ctrl Pts',(11.0743757019637,27.8145558305146,81.8179034621183));
#118139=CARTESIAN_POINT('Ctrl Pts',(11.1634132907465,27.7967856191051,81.6969321954422));
#118140=CARTESIAN_POINT('Ctrl Pts',(11.2188687161481,27.7857177695973,81.6215874657993));
#118141=CARTESIAN_POINT('Ctrl Pts',(11.2759036035297,27.7738651429691,81.5432921853156));
#118142=CARTESIAN_POINT('Ctrl Pts',(11.3344183799878,27.7611617527346,81.4620047494625));
#118143=CARTESIAN_POINT('Ctrl Pts',(11.4301282618082,27.7403834117471,81.3290466942514));
#118144=CARTESIAN_POINT('Ctrl Pts',(11.5298000370535,27.7173292049529,81.1880834873095));
#118145=CARTESIAN_POINT('Ctrl Pts',(11.6329585192826,27.6917064185804,81.0389322040532));
#118146=CARTESIAN_POINT('Ctrl Pts',(11.7358149219911,27.6661586635467,80.8902176812761));
#118147=CARTESIAN_POINT('Ctrl Pts',(11.8421376498616,27.6380569513037,80.7333626172256));
#118148=CARTESIAN_POINT('Ctrl Pts',(11.9514044066712,27.6071058859235,80.5681872211007));
#118149=CARTESIAN_POINT('Ctrl Pts',(12.0492938537255,27.579377574365,80.4202105750855));
#118150=CARTESIAN_POINT('Ctrl Pts',(12.1495455023141,27.5493621274191,80.2655559235485));
#118151=CARTESIAN_POINT('Ctrl Pts',(12.2517485599061,27.5168474912581,80.1040985739415));
#118152=CARTESIAN_POINT('Ctrl Pts',(12.296333474959,27.5026633530789,80.0336646516451));
#118153=CARTESIAN_POINT('Ctrl Pts',(12.3412893211916,27.4880036350616,79.9619362240762));
#118154=CARTESIAN_POINT('Ctrl Pts',(12.3865799860944,27.4728509251013,79.888903372782));
#118155=CARTESIAN_POINT('Ctrl Pts',(12.4004630852323,27.4682061141885,79.8665163683735));
#118156=CARTESIAN_POINT('Ctrl Pts',(12.4143776401482,27.4635149835819,79.8440067925359));
#118157=CARTESIAN_POINT('Ctrl Pts',(12.4283225849059,27.4587770342044,79.8213743700025));
#118158=CARTESIAN_POINT('Ctrl Pts',(12.4371238517049,27.4557867063633,79.8070900546119));
#118159=CARTESIAN_POINT('Ctrl Pts',(12.4459372238459,27.4527777286304,79.7927568042114));
#118160=CARTESIAN_POINT('Ctrl Pts',(12.4547624356809,27.4497499808059,79.7783745484681));
#118161=CARTESIAN_POINT('Ctrl Pts',(12.4661664835309,27.4458374876313,79.7597896197714));
#118162=CARTESIAN_POINT('Ctrl Pts',(12.4775903008183,27.4418936486109,79.7411228625664));
#118163=CARTESIAN_POINT('Ctrl Pts',(12.489033314005,27.4379182106952,79.7223741203786));
#118164=CARTESIAN_POINT('Ctrl Pts',(12.4947548205984,27.4359304917374,79.7129997492847));
#118165=CARTESIAN_POINT('Ctrl Pts',(12.500481126124,27.4339348730558,79.70360488192));
#118166=CARTESIAN_POINT('Ctrl Pts',(12.5062121581154,27.4319313223091,79.694189499433));
#118167=CARTESIAN_POINT('Ctrl Pts',(12.5119431901068,27.4299277715624,79.6847741169461));
#118168=CARTESIAN_POINT('Ctrl Pts',(12.5166768585406,27.4282688187441,79.676989005964));
#118169=CARTESIAN_POINT('Ctrl Pts',(12.5234193609175,27.4258968418557,79.6658817875526));
#118170=CARTESIAN_POINT('Ctrl Pts',(12.6277194954064,27.389204602886,79.4940636243047));
#118171=CARTESIAN_POINT('Ctrl Pts',(12.7267772690378,27.3524203174733,79.3266390217625));
#118172=CARTESIAN_POINT('Ctrl Pts',(12.8209630720956,27.3158288233724,79.1637887314953));
#118173=CARTESIAN_POINT('Ctrl Pts',(12.9170176284925,27.2785113124562,78.9977073064514));
#118174=CARTESIAN_POINT('Ctrl Pts',(13.0080050168062,27.2413940893072,78.8363833821447));
#118175=CARTESIAN_POINT('Ctrl Pts',(13.0942922600167,27.2047381959935,78.6799821906079));
#118176=CARTESIAN_POINT('Ctrl Pts',(13.1831069669234,27.1670086046897,78.518999808168));
#118177=CARTESIAN_POINT('Ctrl Pts',(13.2669422569155,27.1297675963549,78.3632326678671));
#118178=CARTESIAN_POINT('Ctrl Pts',(13.3461699531508,27.0932597216902,78.2128348956482));
#118179=CARTESIAN_POINT('Ctrl Pts',(13.391271668521,27.0724769922895,78.1272184024616));
#118180=CARTESIAN_POINT('Ctrl Pts',(13.4348797008029,27.0519311347474,78.043341470321));
#118181=CARTESIAN_POINT('Ctrl Pts',(13.477058519881,27.03166203572,77.9612291258042));
#118182=CARTESIAN_POINT('Ctrl Pts',(13.5102451213573,27.0157141612559,77.8966225362097));
#118183=CARTESIAN_POINT('Ctrl Pts',(13.5425468915552,26.9999375445627,77.8331082976471));
#118184=CARTESIAN_POINT('Ctrl Pts',(13.573994157241,26.984350213617,77.7706978590314));
#118185=CARTESIAN_POINT('Ctrl Pts',(13.647200350837,26.9480644144555,77.6254123929643));
#118186=CARTESIAN_POINT('Ctrl Pts',(13.7157782150303,26.9128067215343,77.4861101507085));
#118187=CARTESIAN_POINT('Ctrl Pts',(13.7800855430065,26.878778616932,77.3529178756503));
#118188=CARTESIAN_POINT('Ctrl Pts',(13.8454410221642,26.8441958850552,77.2175546871853));
#118189=CARTESIAN_POINT('Ctrl Pts',(13.9063856804312,26.8108829197527,77.0885020861424));
#118190=CARTESIAN_POINT('Ctrl Pts',(13.9632588799502,26.7790170672471,76.965870056256));
#118191=CARTESIAN_POINT('Ctrl Pts',(14.021432781162,26.7464224361841,76.840433406791));
#118192=CARTESIAN_POINT('Ctrl Pts',(14.0753469777581,26.7153416801476,76.7217142165492));
#118193=CARTESIAN_POINT('Ctrl Pts',(14.1253256651883,26.685932309831,76.6098087379326));
#118194=CARTESIAN_POINT('Ctrl Pts',(14.1601432684105,26.6654443010547,76.5318498968105));
#118195=CARTESIAN_POINT('Ctrl Pts',(14.1930500706757,26.6457667714177,76.457197435002));
#118196=CARTESIAN_POINT('Ctrl Pts',(14.224144487831,26.6269447605154,76.3858785370778));
#118197=CARTESIAN_POINT('Origin',(-10.9843331791359,89.,65.395787724084));
#118198=CARTESIAN_POINT('',(12.8491777742141,90.5,75.7863477566628));
#118199=CARTESIAN_POINT('Origin',(12.8491780888091,89.,75.786347893815));
#118200=CARTESIAN_POINT('',(0.214666887831327,89.,90.5121648016016));
#118201=CARTESIAN_POINT('Origin',(-10.9843331791359,89.,65.395787724084));
#118202=CARTESIAN_POINT('',(-0.396188735614809,90.4999999999959,89.1421781913432));
#118203=CARTESIAN_POINT('Origin',(-0.396187662550911,89.,89.14218059794));
#118204=CARTESIAN_POINT('Origin',(-10.9843331791359,90.5,65.395787724084));
#118205=CARTESIAN_POINT('Origin',(6.43246351666909,89.,72.98888938658));
#118206=CARTESIAN_POINT('',(12.8491777735034,90.5,70.191431016807));
#118207=CARTESIAN_POINT('Origin',(12.8491780888091,89.,70.191430879345));
#118208=CARTESIAN_POINT('Origin',(6.43246351666909,90.5,72.98888938658));
#118209=CARTESIAN_POINT('Origin',(-10.9843331791359,89.,80.581991049076));
#118210=CARTESIAN_POINT('',(-0.396188735973519,90.4999999999959,56.8356005826213));
#118211=CARTESIAN_POINT('',(0.214666887829776,89.,55.4656139715578));
#118212=CARTESIAN_POINT('Origin',(-0.396187662550911,89.,56.83559817522));
#118213=CARTESIAN_POINT('Origin',(-10.9843331791359,89.,80.581991049076));
#118214=CARTESIAN_POINT('Origin',(-10.9843331791359,90.5,80.581991049076));
#118215=CARTESIAN_POINT('Ctrl Pts',(20.8483779149991,16.41007210111,65.906087946997));
#118216=CARTESIAN_POINT('Ctrl Pts',(20.1925712483991,16.57554287881,64.475654366764));
#118217=CARTESIAN_POINT('Ctrl Pts',(18.6376319248691,16.98964070821,61.61992743409));
#118218=CARTESIAN_POINT('Ctrl Pts',(16.6713472851791,17.48480467007,58.95952934426));
#118219=CARTESIAN_POINT('Ctrl Pts',(15.5130979896291,17.74010536827,57.61807705647));
#118220=CARTESIAN_POINT('Ctrl Pts',(15.3837024999291,17.76815938829,57.47076094755));
#118221=CARTESIAN_POINT('Ctrl Pts',(16.5559173247791,17.39873241323,67.856902903292));
#118222=CARTESIAN_POINT('Ctrl Pts',(15.9859836856991,17.56285104948,66.616102235752));
#118223=CARTESIAN_POINT('Ctrl Pts',(14.6351635728291,17.97417903959,64.140742823463));
#118224=CARTESIAN_POINT('Ctrl Pts',(12.9298166594891,18.46868755045,61.83930771341));
#118225=CARTESIAN_POINT('Ctrl Pts',(11.9267347229591,18.72463122147,60.6803866708301));
#118226=CARTESIAN_POINT('Ctrl Pts',(11.8146919425591,18.75276856151,60.55313564187));
#118227=CARTESIAN_POINT('Ctrl Pts',(13.9709992217891,21.16901952499,69.377261511201));
#118228=CARTESIAN_POINT('Ctrl Pts',(13.4841936868091,21.32798172742,68.290595666228));
#118229=CARTESIAN_POINT('Ctrl Pts',(12.3245021055191,21.72874684849,66.102133407878));
#118230=CARTESIAN_POINT('Ctrl Pts',(10.8279137708991,22.22075577646,64.01412309014));
#118231=CARTESIAN_POINT('Ctrl Pts',(9.93074736335909,22.47915144446,62.94493798825));
#118232=CARTESIAN_POINT('Ctrl Pts',(9.83032735308908,22.50760652801,62.8273104973501));
#118233=CARTESIAN_POINT('Ctrl Pts',(14.3007957475191,25.96018691159,69.757147250502));
#118234=CARTESIAN_POINT('Ctrl Pts',(13.8555520737491,26.11259647311,68.717136258303));
#118235=CARTESIAN_POINT('Ctrl Pts',(12.7847401829791,26.49993861813,66.5881181087229));
#118236=CARTESIAN_POINT('Ctrl Pts',(11.3472397804891,26.98877115137,64.46832374737));
#118237=CARTESIAN_POINT('Ctrl Pts',(10.4572738893891,27.25028274335,63.354172063168));
#118238=CARTESIAN_POINT('Ctrl Pts',(10.3573188072491,27.27914160579,63.2312323188751));
#118239=CARTESIAN_POINT('',(10.4221245511888,26.952572131543,63.31891762201));
#118240=CARTESIAN_POINT('Ctrl Pts',(14.22419092811,25.6803054598776,69.5919861772058));
#118241=CARTESIAN_POINT('Ctrl Pts',(14.1934725897366,25.6908438843884,69.5215276352073));
#118242=CARTESIAN_POINT('Ctrl Pts',(14.1589619430435,25.7027345557711,69.4431671438523));
#118243=CARTESIAN_POINT('Ctrl Pts',(14.1204327313001,25.7160784589078,69.3570002391341));
#118244=CARTESIAN_POINT('Ctrl Pts',(14.0817643578833,25.7294705582002,69.2705221126153));
#118245=CARTESIAN_POINT('Ctrl Pts',(14.039048314131,25.7443267224897,69.176180926378));
#118246=CARTESIAN_POINT('Ctrl Pts',(13.9920105642602,25.760760407159,69.074097146258));
#118247=CARTESIAN_POINT('Ctrl Pts',(13.9678857806148,25.769188937185,69.0217402814876));
#118248=CARTESIAN_POINT('Ctrl Pts',(13.9426234552543,25.7780325843239,68.9673471478871));
#118249=CARTESIAN_POINT('Ctrl Pts',(13.9161820562462,25.7873073621252,68.9109366361141));
#118250=CARTESIAN_POINT('Ctrl Pts',(13.8646942311264,25.8053676068691,68.8010916704903));
#118251=CARTESIAN_POINT('Ctrl Pts',(13.8087383000022,25.8250626495538,68.683595516882));
#118252=CARTESIAN_POINT('Ctrl Pts',(13.7479745393579,25.8465122969549,68.5586086826413));
#118253=CARTESIAN_POINT('Ctrl Pts',(13.7324012602,25.8520096747221,68.5265755293268));
#118254=CARTESIAN_POINT('Ctrl Pts',(13.7165119540592,25.8576223016977,68.4940504934647));
#118255=CARTESIAN_POINT('Ctrl Pts',(13.7003004465873,25.8633521726573,68.4610365899567));
#118256=CARTESIAN_POINT('Ctrl Pts',(13.6605676941403,25.8773955023592,68.3801228774186));
#118257=CARTESIAN_POINT('Ctrl Pts',(13.6188999657739,25.8921431903905,68.2962722386112));
#118258=CARTESIAN_POINT('Ctrl Pts',(13.5752017215861,25.9076239016636,68.2095325118103));
#118259=CARTESIAN_POINT('Ctrl Pts',(13.5533525994922,25.9153642573001,68.1661626484099));
#118260=CARTESIAN_POINT('Ctrl Pts',(13.5309957354795,25.9232878687553,68.1220705701642));
#118261=CARTESIAN_POINT('Ctrl Pts',(13.5081185883337,25.9313981582767,68.0772627600019));
#118262=CARTESIAN_POINT('Ctrl Pts',(13.4966800147608,25.9354533030373,68.0548588549208));
#118263=CARTESIAN_POINT('Ctrl Pts',(13.4851113633025,25.939555117315,68.0322760204064));
#118264=CARTESIAN_POINT('Ctrl Pts',(13.4734110270797,25.9437040194584,68.0095150949663));
#118265=CARTESIAN_POINT('Ctrl Pts',(13.4624685152899,25.9475841994596,67.9882283823253));
#118266=CARTESIAN_POINT('Ctrl Pts',(13.4506285380081,25.9517830008408,67.9652732993136));
#118267=CARTESIAN_POINT('Ctrl Pts',(13.4400845638854,25.9555223814671,67.9448944647072));
#118268=CARTESIAN_POINT('Ctrl Pts',(13.439354340207,25.9557813525385,67.943483127066));
#118269=CARTESIAN_POINT('Ctrl Pts',(13.4386303503209,25.9560381137129,67.9420841374378));
#118270=CARTESIAN_POINT('Ctrl Pts',(13.4379133304858,25.9562924038131,67.9406989021384));
#118271=CARTESIAN_POINT('Ctrl Pts',(13.3607550418609,25.9836564849563,67.7916341485257));
#118272=CARTESIAN_POINT('Ctrl Pts',(13.2857009269469,26.0102700616628,67.6499684523326));
#118273=CARTESIAN_POINT('Ctrl Pts',(13.2131177177402,26.035965285323,67.5155491144957));
#118274=CARTESIAN_POINT('Ctrl Pts',(13.139430690727,26.06205127216,67.3790855785548));
#118275=CARTESIAN_POINT('Ctrl Pts',(13.0682903286398,26.087191078862,67.2500902843998));
#118276=CARTESIAN_POINT('Ctrl Pts',(13.0000406297685,26.1112452964015,67.1284103791098));
#118277=CARTESIAN_POINT('Ctrl Pts',(12.9304855521089,26.135759587258,67.004403161466));
#118278=CARTESIAN_POINT('Ctrl Pts',(12.8639328391001,26.1591466630811,66.8879936409601));
#118279=CARTESIAN_POINT('Ctrl Pts',(12.8007048462081,26.1812916013322,66.7790301998885));
#118280=CARTESIAN_POINT('Ctrl Pts',(12.7825538915208,26.1876487819474,66.7477499015427));
#118281=CARTESIAN_POINT('Ctrl Pts',(12.7646766648217,26.193903784652,66.7170833086437));
#118282=CARTESIAN_POINT('Ctrl Pts',(12.7470801615792,26.2000543217691,66.6870270209143));
#118283=CARTESIAN_POINT('Ctrl Pts',(12.7413586970835,26.202054155444,66.6772542847777));
#118284=CARTESIAN_POINT('Ctrl Pts',(12.7356669087703,26.204042946285,66.6675460714649));
#118285=CARTESIAN_POINT('Ctrl Pts',(12.730005029151,26.2060206160786,66.6579022642968));
#118286=CARTESIAN_POINT('Ctrl Pts',(12.6963581285086,26.2177733313468,66.6005919286103));
#118287=CARTESIAN_POINT('Ctrl Pts',(12.6637677778018,26.2291330895811,66.5455560250034));
#118288=CARTESIAN_POINT('Ctrl Pts',(12.6322805997689,26.2400850348388,66.4927709300283));
#118289=CARTESIAN_POINT('Ctrl Pts',(12.6165370107524,26.2455610074676,66.4663783825407));
#118290=CARTESIAN_POINT('Ctrl Pts',(12.6010691618075,26.2509350268608,66.4405485689667));
#118291=CARTESIAN_POINT('Ctrl Pts',(12.5858825271088,26.2562055126126,66.4152786705119));
#118292=CARTESIAN_POINT('Ctrl Pts',(12.5782892097594,26.2588407554886,66.4026437212844));
#118293=CARTESIAN_POINT('Ctrl Pts',(12.5707661926246,26.2614501149547,66.3901487528226));
#118294=CARTESIAN_POINT('Ctrl Pts',(12.563314139175,26.2640333993445,66.3777934235363));
#118295=CARTESIAN_POINT('Ctrl Pts',(12.5595881124501,26.2653250415394,66.3716157588932));
#118296=CARTESIAN_POINT('Ctrl Pts',(12.555879826438,26.2666101649652,66.3654730041698));
#118297=CARTESIAN_POINT('Ctrl Pts',(12.5521893627096,26.2678887465314,66.35936511724));
#118298=CARTESIAN_POINT('Ctrl Pts',(12.5503441308454,26.2685280373144,66.3563111737751));
#118299=CARTESIAN_POINT('Ctrl Pts',(12.5485033545391,26.2691656926326,66.3532659472665));
#118300=CARTESIAN_POINT('Ctrl Pts',(12.5466670439017,26.2698017096539,66.3502294324841));
#118301=CARTESIAN_POINT('Ctrl Pts',(12.5448307332644,26.2704377266752,66.3471929177017));
#118302=CARTESIAN_POINT('Ctrl Pts',(12.5436494615672,26.2708468404772,66.3452399622795));
#118303=CARTESIAN_POINT('Ctrl Pts',(12.5411715190533,26.2717048430112,66.3411460181136));
#118304=CARTESIAN_POINT('Ctrl Pts',(11.962278170298,26.4721501549424,65.3847246990396));
#118305=CARTESIAN_POINT('Ctrl Pts',(11.3231338036213,26.6855355653743,64.460421737533));
#118306=CARTESIAN_POINT('Ctrl Pts',(10.6245339352504,26.893097015685,63.5729680868371));
#118307=CARTESIAN_POINT('Ctrl Pts',(10.5576059451875,26.9129820332934,63.4879473306014));
#118308=CARTESIAN_POINT('Ctrl Pts',(10.4901322849598,26.9328135924601,63.4032648117697));
#118309=CARTESIAN_POINT('Ctrl Pts',(10.4221147584861,26.9525719251785,63.3189269730742));
#118310=CARTESIAN_POINT('Origin',(17.8170756838691,26.95256493355,57.35532384706));
#118311=CARTESIAN_POINT('Ctrl Pts',(15.6451955709591,17.70734006941,57.66551497159));
#118312=CARTESIAN_POINT('Ctrl Pts',(15.4053160301991,17.76750394009,57.5702232381));
#118313=CARTESIAN_POINT('Ctrl Pts',(14.8524063434191,17.89090859263,57.35645087848));
#118314=CARTESIAN_POINT('Ctrl Pts',(13.9432808889591,18.03861939721,57.02808486809));
#118315=CARTESIAN_POINT('Ctrl Pts',(12.9188376719691,18.13614112929,56.68942936417));
#118316=CARTESIAN_POINT('Ctrl Pts',(11.8651204328191,18.16653625119,56.3745849123));
#118317=CARTESIAN_POINT('Ctrl Pts',(10.8194002598291,18.13134446021,56.09433316092));
#118318=CARTESIAN_POINT('Ctrl Pts',(9.75348782079909,18.03185317263,55.8398643760501));
#118319=CARTESIAN_POINT('Ctrl Pts',(8.60334640165909,17.85384778506,55.5992400384));
#118320=CARTESIAN_POINT('Ctrl Pts',(7.32308763312909,17.56641516118,55.37248137399));
#118321=CARTESIAN_POINT('Ctrl Pts',(6.08206864086909,17.18674270191,55.19570687228));
#118322=CARTESIAN_POINT('Ctrl Pts',(5.28049439426909,16.87792525594,55.10601469316));
#118323=CARTESIAN_POINT('Ctrl Pts',(4.94559772960909,16.736925875,55.07276081499));
#118324=CARTESIAN_POINT('Ctrl Pts',(12.0373027887591,18.6574860008,60.7132364091101));
#118325=CARTESIAN_POINT('Ctrl Pts',(11.8364311238391,18.77666302266,60.6457111203401));
#118326=CARTESIAN_POINT('Ctrl Pts',(11.3704473225491,19.03747034031,60.48554158426));
#118327=CARTESIAN_POINT('Ctrl Pts',(10.5891293699691,19.41263661724,60.205607251));
#118328=CARTESIAN_POINT('Ctrl Pts',(9.68271453490909,19.76202380549,59.87027563324));
#118329=CARTESIAN_POINT('Ctrl Pts',(8.71691702481909,20.03893729113,59.50718051343));
#118330=CARTESIAN_POINT('Ctrl Pts',(7.72171670189909,20.22883548888,59.13283164616));
#118331=CARTESIAN_POINT('Ctrl Pts',(6.66769425441909,20.33228659359,58.7406236989601));
#118332=CARTESIAN_POINT('Ctrl Pts',(5.48364232856909,20.33573846041,58.30895983799));
#118333=CARTESIAN_POINT('Ctrl Pts',(4.10481591372909,20.19187673024,57.82159800215));
#118334=CARTESIAN_POINT('Ctrl Pts',(2.69831955594909,19.86874669915,57.3431750580601));
#118335=CARTESIAN_POINT('Ctrl Pts',(1.74651831724909,19.53037562758,57.0299445529801));
#118336=CARTESIAN_POINT('Ctrl Pts',(1.34062365781909,19.36074341708,56.8973330406101));
#118337=CARTESIAN_POINT('Ctrl Pts',(10.0358374714891,22.38383994892,63.019033831034));
#118338=CARTESIAN_POINT('Ctrl Pts',(9.84598787858909,22.55213797617,62.881678099));
#118339=CARTESIAN_POINT('Ctrl Pts',(9.39884778054908,22.91846423345,62.55638442729));
#118340=CARTESIAN_POINT('Ctrl Pts',(8.62363209760909,23.43709896161,61.99154664531));
#118341=CARTESIAN_POINT('Ctrl Pts',(7.69183910901909,23.90734852226,61.32157759184));
#118342=CARTESIAN_POINT('Ctrl Pts',(6.6663237622691,24.26349060744,60.60358414559));
#118343=CARTESIAN_POINT('Ctrl Pts',(5.58132317884909,24.48664443975,59.87044986124));
#118344=CARTESIAN_POINT('Ctrl Pts',(4.40709163424909,24.57682141001,59.10837536092));
#118345=CARTESIAN_POINT('Ctrl Pts',(3.06417177756909,24.51032471516,58.27536784085));
#118346=CARTESIAN_POINT('Ctrl Pts',(1.47641806860909,24.21374904793,57.34023061635));
#118347=CARTESIAN_POINT('Ctrl Pts',(-0.16335550177091,23.64851785533,56.42568615944));
#118348=CARTESIAN_POINT('Ctrl Pts',(-1.27954381589091,23.08548524468,55.82771633623));
#118349=CARTESIAN_POINT('Ctrl Pts',(-1.75618235438091,22.80589742487,55.57457975359));
#118350=CARTESIAN_POINT('Ctrl Pts',(10.5754944201391,27.14617507505,63.506087747273));
#118351=CARTESIAN_POINT('Ctrl Pts',(10.3635337299691,27.33076219475,63.233915867281));
#118352=CARTESIAN_POINT('Ctrl Pts',(9.85835504468908,27.72144576791,62.60188493816));
#118353=CARTESIAN_POINT('Ctrl Pts',(8.96468660719909,28.23256140694,61.5518599865));
#118354=CARTESIAN_POINT('Ctrl Pts',(7.87596066045909,28.63622689438,60.36556961314));
#118355=CARTESIAN_POINT('Ctrl Pts',(6.67097845427909,28.86730764335,59.15176956186));
#118356=CARTESIAN_POINT('Ctrl Pts',(5.39779469245909,28.91635220029,57.96271623088));
#118357=CARTESIAN_POINT('Ctrl Pts',(4.02739324090909,28.78323759979,56.77137740692));
#118358=CARTESIAN_POINT('Ctrl Pts',(2.47484018625909,28.42805287238,55.51415168585));
#118359=CARTESIAN_POINT('Ctrl Pts',(0.665369677529091,27.75379664694,54.15318031056));
#118360=CARTESIAN_POINT('Ctrl Pts',(-1.16653927068091,26.7608832154,52.87171230437));
#118361=CARTESIAN_POINT('Ctrl Pts',(-2.38450511710091,25.88299926927,52.06077692591));
#118362=CARTESIAN_POINT('Ctrl Pts',(-2.89859565635591,25.46348290666,51.72223367689));
#118363=CARTESIAN_POINT('',(0.214722992422839,21.3110521316348,55.4657680174377));
#118364=CARTESIAN_POINT('Ctrl Pts',(10.4221245511888,26.952572131543,63.31891762201));
#118365=CARTESIAN_POINT('Ctrl Pts',(10.2814066492482,26.993572523789,63.1444235191351));
#118366=CARTESIAN_POINT('Ctrl Pts',(10.1346923009253,27.0285147217768,62.9668635799751));
#118367=CARTESIAN_POINT('Ctrl Pts',(9.98184065432509,27.0565650645596,62.786777213206));
#118368=CARTESIAN_POINT('Ctrl Pts',(9.96268076478778,27.0600811632157,62.7642034629637));
#118369=CARTESIAN_POINT('Ctrl Pts',(9.94342447433925,27.0634889599087,62.7415900735869));
#118370=CARTESIAN_POINT('Ctrl Pts',(9.92407153256859,27.0667868020637,62.7189381553192));
#118371=CARTESIAN_POINT('Ctrl Pts',(9.90528602597828,27.0699879503061,62.6969503994038));
#118372=CARTESIAN_POINT('Ctrl Pts',(9.88640945302957,27.0730854973525,62.6749263412792));
#118373=CARTESIAN_POINT('Ctrl Pts',(9.8674415908049,27.0760779304426,62.6528670059662));
#118374=CARTESIAN_POINT('Ctrl Pts',(9.79869381173847,27.086923808935,62.5729143843959));
#118375=CARTESIAN_POINT('Ctrl Pts',(9.72874671454407,27.0963888624975,62.4924982081541));
#118376=CARTESIAN_POINT('Ctrl Pts',(9.65759474141652,27.1044036647129,62.4116697829035));
#118377=CARTESIAN_POINT('Ctrl Pts',(9.61220315905006,27.109516728187,62.3601050832748));
#118378=CARTESIAN_POINT('Ctrl Pts',(9.56632112929409,27.1140395147692,62.3083725197215));
#118379=CARTESIAN_POINT('Ctrl Pts',(9.5199475857354,27.11795403698,62.2564859095843));
#118380=CARTESIAN_POINT('Ctrl Pts',(9.49676081395605,27.1199112980854,62.2305426045156));
#118381=CARTESIAN_POINT('Ctrl Pts',(9.47345116346099,27.121716493098,62.2045607880786));
#118382=CARTESIAN_POINT('Ctrl Pts',(9.45001849613942,27.1233673617675,62.1785421858642));
#118383=CARTESIAN_POINT('Ctrl Pts',(9.43830216247863,27.1241927961022,62.1655328847569));
#118384=CARTESIAN_POINT('Ctrl Pts',(9.42655507458789,27.1249796488512,62.1525143872246));
#118385=CARTESIAN_POINT('Ctrl Pts',(9.41477721697565,27.1257276380715,62.1394869111806));
#118386=CARTESIAN_POINT('Ctrl Pts',(9.40594382376647,27.1262886299868,62.1297163041475));
#118387=CARTESIAN_POINT('Ctrl Pts',(9.39709312258736,27.1268277611672,62.119940646703));
#118388=CARTESIAN_POINT('Ctrl Pts',(9.38822510715136,27.1273449126714,62.1101600311071));
#118389=CARTESIAN_POINT('Ctrl Pts',(9.38526910200603,27.1275172965062,62.1068998259085));
#118390=CARTESIAN_POINT('Ctrl Pts',(9.38137384331691,27.1277402806879,62.1026062763353));
#118391=CARTESIAN_POINT('Ctrl Pts',(9.37935132008672,27.1278547332123,62.100377766239));
#118392=CARTESIAN_POINT('Ctrl Pts',(9.33983231774599,27.1300910732023,62.0568338927249));
#118393=CARTESIAN_POINT('Ctrl Pts',(9.29613981450071,27.1319600387806,62.0089688918052));
#118394=CARTESIAN_POINT('Ctrl Pts',(9.24818733537905,27.1332027091348,61.956876784848));
#118395=CARTESIAN_POINT('Ctrl Pts',(9.20000809183754,27.1344512560031,61.9045383374173));
#118396=CARTESIAN_POINT('Ctrl Pts',(9.14752838831708,27.1350675138919,61.847932585123));
#118397=CARTESIAN_POINT('Ctrl Pts',(9.09064900126491,27.1347427847506,61.7871776110701));
#118398=CARTESIAN_POINT('Ctrl Pts',(9.06506963794882,27.1345967500425,61.7598553483823));
#118399=CARTESIAN_POINT('Ctrl Pts',(9.03860033203933,27.1342597963946,61.7316942581623));
#118400=CARTESIAN_POINT('Ctrl Pts',(9.01123138962838,27.1337008833808,61.7027066707963));
#118401=CARTESIAN_POINT('Ctrl Pts',(8.98852386077562,27.13323716311,61.67865618077));
#118402=CARTESIAN_POINT('Ctrl Pts',(8.96519703880106,27.1326206187768,61.6540367698852));
#118403=CARTESIAN_POINT('Ctrl Pts',(8.94124519193602,27.1318325819045,61.6288560163335));
#118404=CARTESIAN_POINT('Ctrl Pts',(8.93903805036325,27.1317599650015,61.626535632093));
#118405=CARTESIAN_POINT('Ctrl Pts',(8.93682560129779,27.1316858912838,61.6242104815798));
#118406=CARTESIAN_POINT('Ctrl Pts',(8.93460784034833,27.1316103457679,61.6218805709601));
#118407=CARTESIAN_POINT('Ctrl Pts',(8.91452314150809,27.1309261832415,61.6007802115493));
#118408=CARTESIAN_POINT('Ctrl Pts',(8.89452126022697,27.1301435289572,61.5798314489841));
#118409=CARTESIAN_POINT('Ctrl Pts',(8.87341065881786,27.1292010067377,61.5577961809475));
#118410=CARTESIAN_POINT('Ctrl Pts',(8.86689381231496,27.1289100499567,61.5509938896881));
#118411=CARTESIAN_POINT('Ctrl Pts',(8.86027120104815,27.1286035315052,61.5440881800932));
#118412=CARTESIAN_POINT('Ctrl Pts',(8.8535074709814,27.1282787291607,61.5370429720019));
#118413=CARTESIAN_POINT('Ctrl Pts',(8.76572859058654,27.1240634831555,61.4456111034465));
#118414=CARTESIAN_POINT('Ctrl Pts',(8.68104973639839,27.1180728992385,61.3586725401621));
#118415=CARTESIAN_POINT('Ctrl Pts',(8.59964480291943,27.1107438490325,61.2760963895947));
#118416=CARTESIAN_POINT('Ctrl Pts',(8.57468192486981,27.1084963908172,61.2507743570308));
#118417=CARTESIAN_POINT('Ctrl Pts',(8.55002670460079,27.1061227585507,61.2258625402158));
#118418=CARTESIAN_POINT('Ctrl Pts',(8.52568363313075,27.1036347301996,61.201357175705));
#118419=CARTESIAN_POINT('Ctrl Pts',(8.47382023755181,27.0983339365531,61.1491480115904));
#118420=CARTESIAN_POINT('Ctrl Pts',(8.42337401150025,27.0925143842389,61.0987837393931));
#118421=CARTESIAN_POINT('Ctrl Pts',(8.37438496064367,27.0862842171409,61.0502283048172));
#118422=CARTESIAN_POINT('Ctrl Pts',(8.34989043521538,27.0831691335919,61.0259505875293));
#118423=CARTESIAN_POINT('Ctrl Pts',(8.32576016401583,27.0799513963409,61.0021251196712));
#118424=CARTESIAN_POINT('Ctrl Pts',(8.30199870177388,27.0766436642737,60.9787474266291));
#118425=CARTESIAN_POINT('Ctrl Pts',(8.2901179706529,27.0749897982401,60.9670585801081));
#118426=CARTESIAN_POINT('Ctrl Pts',(8.27832943929354,27.0733134335021,60.9554816797772));
#118427=CARTESIAN_POINT('Ctrl Pts',(8.26663365856629,27.071616129553,60.9440161775303));
#118428=CARTESIAN_POINT('Ctrl Pts',(8.26078576820267,27.0707674775785,60.9382834264068));
#118429=CARTESIAN_POINT('Ctrl Pts',(8.25496106534509,27.0699135908012,60.9325785249595));
#118430=CARTESIAN_POINT('Ctrl Pts',(8.24915961727369,27.0690546611449,60.9269014049513));
#118431=CARTESIAN_POINT('Ctrl Pts',(8.24335816920229,27.0681957314886,60.9212242849432));
#118432=CARTESIAN_POINT('Ctrl Pts',(8.2386130797743,27.0674877290304,60.9165841299647));
#118433=CARTESIAN_POINT('Ctrl Pts',(8.23182510390789,27.0664629345651,60.9099533214476));
#118434=CARTESIAN_POINT('Ctrl Pts',(8.11648638367961,27.0490500143582,60.7972851294147));
#118435=CARTESIAN_POINT('Ctrl Pts',(8.00223494191034,27.0286870805438,60.6876598283109));
#118436=CARTESIAN_POINT('Ctrl Pts',(7.88922788442964,27.0056723798554,60.5810237234782));
#118437=CARTESIAN_POINT('Ctrl Pts',(7.75397942678112,26.9781280579278,60.453400112796));
#118438=CARTESIAN_POINT('Ctrl Pts',(7.62051474582978,26.9467864738024,60.3300581414355));
#118439=CARTESIAN_POINT('Ctrl Pts',(7.48909721297415,26.912148066346,60.2108850727485));
#118440=CARTESIAN_POINT('Ctrl Pts',(7.42012718180227,26.8939692739878,60.148341132959));
#118441=CARTESIAN_POINT('Ctrl Pts',(7.35172031310869,26.8748818989521,60.0869451782984));
#118442=CARTESIAN_POINT('Ctrl Pts',(7.28391041918654,26.8549548660802,60.0266793543247));
#118443=CARTESIAN_POINT('Ctrl Pts',(7.23308109372499,26.84001784759,59.9815049556671));
#118444=CARTESIAN_POINT('Ctrl Pts',(7.18258713569114,26.8246089951325,59.9369655314101));
#118445=CARTESIAN_POINT('Ctrl Pts',(7.13244179464783,26.8087565024949,59.8930532223584));
#118446=CARTESIAN_POINT('Ctrl Pts',(7.10736912412617,26.8008302561761,59.8710970678326));
#118447=CARTESIAN_POINT('Ctrl Pts',(7.08238360440521,26.7927930998124,59.8492976960571));
#118448=CARTESIAN_POINT('Ctrl Pts',(7.05748680242125,26.7846484759186,59.8276540880368));
#118449=CARTESIAN_POINT('Ctrl Pts',(7.03864287135314,26.778483960037,59.811272439588));
#118450=CARTESIAN_POINT('Ctrl Pts',(7.01912796897405,26.7720165488119,59.7943551656028));
#118451=CARTESIAN_POINT('Ctrl Pts',(7.00058154509988,26.7657948074645,59.778321121133));
#118452=CARTESIAN_POINT('Ctrl Pts',(6.99462423665639,26.7637963180245,59.7731708156536));
#118453=CARTESIAN_POINT('Ctrl Pts',(6.98876691844394,26.7618235394718,59.7681114531265));
#118454=CARTESIAN_POINT('Ctrl Pts',(6.98306410141104,26.759895640288,59.7631895502394));
#118455=CARTESIAN_POINT('Ctrl Pts',(6.92582299967832,26.7405446646773,59.713786747685));
#118456=CARTESIAN_POINT('Ctrl Pts',(6.86780102036232,26.7202464698308,59.6641221341678));
#118457=CARTESIAN_POINT('Ctrl Pts',(6.80900131236983,26.6989614566225,59.6142241745268));
#118458=CARTESIAN_POINT('Ctrl Pts',(6.6750357626757,26.6504670237069,59.5005398073734));
#118459=CARTESIAN_POINT('Ctrl Pts',(6.53703097285645,26.5968507260649,59.3856427811481));
#118460=CARTESIAN_POINT('Ctrl Pts',(6.39506530351964,26.5376331238691,59.2698754606097));
#118461=CARTESIAN_POINT('Ctrl Pts',(6.29292692206693,26.49502852749,59.1865856990769));
#118462=CARTESIAN_POINT('Ctrl Pts',(6.18873892527997,26.4495243827305,59.1028459007061));
#118463=CARTESIAN_POINT('Ctrl Pts',(6.08254064887584,26.4009401198577,59.0187902614544));
#118464=CARTESIAN_POINT('Ctrl Pts',(6.02944151067378,26.3766479884214,58.9767624418286));
#118465=CARTESIAN_POINT('Ctrl Pts',(5.97583981231385,26.3515858274571,58.9346556496021));
#118466=CARTESIAN_POINT('Ctrl Pts',(5.92174144205499,26.3257309408639,58.8924872877607));
#118467=CARTESIAN_POINT('Ctrl Pts',(5.89469225692556,26.3128034975672,58.87140310684));
#118468=CARTESIAN_POINT('Ctrl Pts',(5.86751890463645,26.2996778728634,58.8503035324909));
#118469=CARTESIAN_POINT('Ctrl Pts',(5.84022215204843,26.2863512303691,58.829190754269));
#118470=CARTESIAN_POINT('Ctrl Pts',(5.82657377575442,26.2796879091219,58.818634365158));
#118471=CARTESIAN_POINT('Ctrl Pts',(5.81289454943385,26.2729743334271,58.8080746750166));
#118472=CARTESIAN_POINT('Ctrl Pts',(5.79918457251528,26.2662101484786,58.7975119596882));
#118473=CARTESIAN_POINT('Ctrl Pts',(5.78763485513043,26.2605117855304,58.788613594827));
#118474=CARTESIAN_POINT('Ctrl Pts',(5.77492168842818,26.2542098195369,58.7788360061934));
#118475=CARTESIAN_POINT('Ctrl Pts',(5.76393033383615,26.2487384151678,58.7703961828101));
#118476=CARTESIAN_POINT('Ctrl Pts',(5.76187451049826,26.2477150435079,58.7688175979565));
#118477=CARTESIAN_POINT('Ctrl Pts',(5.75987893234084,26.2467208583818,58.7672857384051));
#118478=CARTESIAN_POINT('Ctrl Pts',(5.75796249058962,26.245765411025,58.7658150144878));
#118479=CARTESIAN_POINT('Ctrl Pts',(5.75464223830328,26.2441100900276,58.7632669722914));
#118480=CARTESIAN_POINT('Ctrl Pts',(5.75132049304372,26.2424518611636,58.7607189918301));
#118481=CARTESIAN_POINT('Ctrl Pts',(5.74799725649708,26.2407907204187,58.758171076555));
#118482=CARTESIAN_POINT('Ctrl Pts',(5.58044261383318,26.1570374756447,58.6297074455561));
#118483=CARTESIAN_POINT('Ctrl Pts',(5.40909309321754,26.0658809328938,58.5014082207791));
#118484=CARTESIAN_POINT('Ctrl Pts',(5.23422053837367,25.9668212156878,58.3736999585156));
#118485=CARTESIAN_POINT('Ctrl Pts',(5.05984397712084,25.86804246301,58.2463539170686));
#118486=CARTESIAN_POINT('Ctrl Pts',(4.88196434708753,25.761404800653,58.1195955448284));
#118487=CARTESIAN_POINT('Ctrl Pts',(4.70089759350769,25.6464293458342,57.9938628415067));
#118488=CARTESIAN_POINT('Ctrl Pts',(4.52764611784975,25.5364165090325,57.8735570650002));
#118489=CARTESIAN_POINT('Ctrl Pts',(4.35147646196849,25.4187699381707,57.7541905673983));
#118490=CARTESIAN_POINT('Ctrl Pts',(4.17274238471399,25.2930685727607,57.6361260281792));
#118491=CARTESIAN_POINT('Ctrl Pts',(3.99912209081811,25.1709636650629,57.5214394484695));
#118492=CARTESIAN_POINT('Ctrl Pts',(3.82308218514099,25.0412577714307,57.4079813739881));
#118493=CARTESIAN_POINT('Ctrl Pts',(3.64498832129322,24.9035899436578,57.29609430042));
#118494=CARTESIAN_POINT('Ctrl Pts',(3.61989910262178,24.8841957985682,57.2803320546323));
#118495=CARTESIAN_POINT('Ctrl Pts',(3.59476918753824,24.8646436889377,57.2646010042274));
#118496=CARTESIAN_POINT('Ctrl Pts',(3.56959966427412,24.8449326566351,57.2489021238195));
#118497=CARTESIAN_POINT('Ctrl Pts',(3.5618666053648,24.8388766589763,57.2440788156571));
#118498=CARTESIAN_POINT('Ctrl Pts',(3.55412980772363,24.8328056597867,57.239258544239));
#118499=CARTESIAN_POINT('Ctrl Pts',(3.54638930684746,24.826719625658,57.2344413338674));
#118500=CARTESIAN_POINT('Ctrl Pts',(3.49031332815,24.7826294142349,57.1995431030552));
#118501=CARTESIAN_POINT('Ctrl Pts',(3.4340429523821,24.7377501024215,57.1648055170815));
#118502=CARTESIAN_POINT('Ctrl Pts',(3.37759196808357,24.6920691766732,57.1302378655454));
#118503=CARTESIAN_POINT('Ctrl Pts',(3.34936647593431,24.669228713799,57.1129540397773));
#118504=CARTESIAN_POINT('Ctrl Pts',(3.32109583321996,24.646187847441,57.0957126950519));
#118505=CARTESIAN_POINT('Ctrl Pts',(3.29278181910187,24.6229450529,57.0785150056188));
#118506=CARTESIAN_POINT('Ctrl Pts',(3.27862481204283,24.6113236556295,57.0699161609022));
#118507=CARTESIAN_POINT('Ctrl Pts',(3.26445696223054,24.5996517763133,57.0613282298503));
#118508=CARTESIAN_POINT('Ctrl Pts',(3.25027849397554,24.587929225742,57.0527513591214));
#118509=CARTESIAN_POINT('Ctrl Pts',(3.24318925984804,24.5820679504564,57.0484629237569));
#118510=CARTESIAN_POINT('Ctrl Pts',(3.23609737111571,24.576194007357,57.0441772534636));
#118511=CARTESIAN_POINT('Ctrl Pts',(3.22900285601976,24.5703073729452,57.0398943666173));
#118512=CARTESIAN_POINT('Ctrl Pts',(3.22190834092382,24.5644207385335,57.035611479771));
#118513=CARTESIAN_POINT('Ctrl Pts',(3.21632152231737,24.5597790772393,57.0322412838866));
#118514=CARTESIAN_POINT('Ctrl Pts',(3.20771145995645,24.5526093723229,57.0270540747882));
#118515=CARTESIAN_POINT('Ctrl Pts',(3.01702554634636,24.3938228647475,56.9121736401804));
#118516=CARTESIAN_POINT('Ctrl Pts',(2.82881053842557,24.2294935613802,56.8019286901944));
#118517=CARTESIAN_POINT('Ctrl Pts',(2.64342884833907,24.0599839636375,56.6961523244788));
#118518=CARTESIAN_POINT('Ctrl Pts',(2.53066793462781,23.9568774642017,56.6318124231565));
#118519=CARTESIAN_POINT('Ctrl Pts',(2.41895457083286,23.8518549938012,56.5691261814459));
#118520=CARTESIAN_POINT('Ctrl Pts',(2.30836409397114,23.7450044702533,56.5080591013602));
#118521=CARTESIAN_POINT('Ctrl Pts',(2.14640352322155,23.5885210887742,56.4186259112216));
#118522=CARTESIAN_POINT('Ctrl Pts',(1.98685270757876,23.4281143258072,56.3326643026614));
#118523=CARTESIAN_POINT('Ctrl Pts',(1.82994511721138,23.2639864925265,56.2500260357267));
#118524=CARTESIAN_POINT('Ctrl Pts',(1.67088138732323,23.0976033030393,56.1662521982765));
#118525=CARTESIAN_POINT('Ctrl Pts',(1.51453385646949,22.9273959923632,56.0858937160226));
#118526=CARTESIAN_POINT('Ctrl Pts',(1.36112026579838,22.7536190886725,56.0088149386751));
#118527=CARTESIAN_POINT('Ctrl Pts',(1.23542781254438,22.6112428803573,55.9456639454923));
#118528=CARTESIAN_POINT('Ctrl Pts',(1.11170426995191,22.466471375799,55.8847148596342));
#118529=CARTESIAN_POINT('Ctrl Pts',(0.990058160464487,22.319466349336,55.8259018516421));
#118530=CARTESIAN_POINT('Ctrl Pts',(0.868248809376559,22.1722640511649,
55.767009920209));
#118531=CARTESIAN_POINT('Ctrl Pts',(0.74852275231373,22.0228197708775,55.7102593206989));
#118532=CARTESIAN_POINT('Ctrl Pts',(0.631054499834477,21.8711790855951,
55.6555578594923));
#118533=CARTESIAN_POINT('Ctrl Pts',(0.512649166714672,21.7183287155893,
55.6004200277836));
#118534=CARTESIAN_POINT('Ctrl Pts',(0.396537737896709,21.5632467730203,
55.5473641780413));
#118535=CARTESIAN_POINT('Ctrl Pts',(0.282886631224853,21.4060296276657,
55.4963092820682));
#118536=CARTESIAN_POINT('Ctrl Pts',(0.260062346259937,21.3744560774204,
55.4860560471577));
#118537=CARTESIAN_POINT('Ctrl Pts',(0.237337252860129,21.3427965692195,
55.4758835564763));
#118538=CARTESIAN_POINT('Ctrl Pts',(0.214712643454674,21.3110521213042,
55.465791216911));
#118539=CARTESIAN_POINT('',(4.86118877219909,16.96274263543,55.19970909287));
#118540=CARTESIAN_POINT('Ctrl Pts',(4.86118877219909,16.96274263543,55.19970909287));
#118541=CARTESIAN_POINT('Ctrl Pts',(3.21558079015593,18.2032496927606,55.9931907979944));
#118542=CARTESIAN_POINT('Ctrl Pts',(1.60457389977557,19.7107791425907,56.0853779332709));
#118543=CARTESIAN_POINT('Ctrl Pts',(0.214754169499088,21.31105212978,55.4656980988));
#118544=CARTESIAN_POINT('Ctrl Pts',(15.2821022274612,17.8079499022762,57.8022939269451));
#118545=CARTESIAN_POINT('Ctrl Pts',(15.092084226211,17.8569950920321,57.7280471206653));
#118546=CARTESIAN_POINT('Ctrl Pts',(14.8978323790944,17.9029043539499,57.6536660080466));
#118547=CARTESIAN_POINT('Ctrl Pts',(14.6993937859133,17.9453287930748,57.5793905280265));
#118548=CARTESIAN_POINT('Ctrl Pts',(14.4630225436543,17.9958629014725,57.4909168737826));
#118549=CARTESIAN_POINT('Ctrl Pts',(14.2207098803036,18.0414524117732,57.4025925276253));
#118550=CARTESIAN_POINT('Ctrl Pts',(13.9725790603985,18.0815246521105,57.3148176057679));
#118551=CARTESIAN_POINT('Ctrl Pts',(13.9004739636052,18.0931693674641,57.2893108217296));
#118552=CARTESIAN_POINT('Ctrl Pts',(13.8278777812175,18.1043481499142,57.263850679352));
#118553=CARTESIAN_POINT('Ctrl Pts',(13.7547940963012,18.115046875106,57.2384476074277));
#118554=CARTESIAN_POINT('Ctrl Pts',(13.5410615600471,18.1463351944148,57.1641565669957));
#118555=CARTESIAN_POINT('Ctrl Pts',(13.3231571973339,18.173517895102,57.0903522859025));
#118556=CARTESIAN_POINT('Ctrl Pts',(13.1012753400396,18.1962394952848,57.0172914311508));
#118557=CARTESIAN_POINT('Ctrl Pts',(12.9720833719076,18.2094692756847,56.9747513346604));
#118558=CARTESIAN_POINT('Ctrl Pts',(12.8415273351186,18.2211892081843,56.9324614523191));
#118559=CARTESIAN_POINT('Ctrl Pts',(12.7096497119619,18.231329974947,56.8904801232899));
#118560=CARTESIAN_POINT('Ctrl Pts',(12.4444257808021,18.2517244434051,56.8060499307075));
#118561=CARTESIAN_POINT('Ctrl Pts',(12.1738535015571,18.2657306505299,56.7228668117145));
#118562=CARTESIAN_POINT('Ctrl Pts',(11.8982362092349,18.2728269465582,56.641337813959));
#118563=CARTESIAN_POINT('Ctrl Pts',(11.816782613109,18.2749241256786,56.6172434256868));
#118564=CARTESIAN_POINT('Ctrl Pts',(11.7348914914288,18.2764174198421,56.5932935716011));
#118565=CARTESIAN_POINT('Ctrl Pts',(11.6525706270574,18.2772939817353,56.5694993585778));
#118566=CARTESIAN_POINT('Ctrl Pts',(11.5263631906892,18.2786378528207,56.5330200692871));
#118567=CARTESIAN_POINT('Ctrl Pts',(11.3991455032489,18.2785321023952,56.4969065926259));
#118568=CARTESIAN_POINT('Ctrl Pts',(11.2709602716692,18.276929295604,56.4611958066604));
#118569=CARTESIAN_POINT('Ctrl Pts',(11.1650621990578,18.2756051637375,56.4316939415971));
#118570=CARTESIAN_POINT('Ctrl Pts',(11.0585025136665,18.2732596241015,56.4024671445837));
#118571=CARTESIAN_POINT('Ctrl Pts',(10.9513041961047,18.2698666163817,56.3735365751458));
#118572=CARTESIAN_POINT('Ctrl Pts',(10.8977050373239,18.2681701125217,56.3590712904268));
#118573=CARTESIAN_POINT('Ctrl Pts',(10.8439462208197,18.2662117444404,56.344680060825));
#118574=CARTESIAN_POINT('Ctrl Pts',(10.7900307491872,18.2639882578872,56.3303655288327));
#118575=CARTESIAN_POINT('Ctrl Pts',(10.7630730133709,18.2628765146106,56.3232082628366));
#118576=CARTESIAN_POINT('Ctrl Pts',(10.736076113812,18.2616984918937,56.316070171194));
#118577=CARTESIAN_POINT('Ctrl Pts',(10.7090404294249,18.2604537834562,56.3089515838742));
#118578=CARTESIAN_POINT('Ctrl Pts',(10.6853842055862,18.2593646635733,56.3027228199694));
#118579=CARTESIAN_POINT('Ctrl Pts',(10.6616982871151,18.258224487445,56.2965089890576));
#118580=CARTESIAN_POINT('Ctrl Pts',(10.6379829303447,18.2570329830165,56.2903103121946));
#118581=CARTESIAN_POINT('Ctrl Pts',(10.6345950222346,18.2568627680981,56.2894247869284));
#118582=CARTESIAN_POINT('Ctrl Pts',(10.6299498050268,18.2566276114753,56.288211440762));
#118583=CARTESIAN_POINT('Ctrl Pts',(10.6278174044834,18.2565191949143,56.2876546648398));
#118584=CARTESIAN_POINT('Ctrl Pts',(10.624434478532,18.2563471985231,56.2867713731327));
#118585=CARTESIAN_POINT('Ctrl Pts',(10.6210431006008,18.2561738055463,56.2858864140547));
#118586=CARTESIAN_POINT('Ctrl Pts',(10.6176432727053,18.2559990005717,56.2849997937491));
#118587=CARTESIAN_POINT('Ctrl Pts',(10.5197768751936,18.2509671184732,56.259477815007));
#118588=CARTESIAN_POINT('Ctrl Pts',(10.4149081209611,18.2447691498421,56.2325775734398));
#118589=CARTESIAN_POINT('Ctrl Pts',(10.3030846392931,18.2370134649294,56.204453451112));
#118590=CARTESIAN_POINT('Ctrl Pts',(10.1918637896328,18.2292995764615,56.1764808935188));
#118591=CARTESIAN_POINT('Ctrl Pts',(10.0737626481988,18.2200446326264,56.1472975810232));
#118592=CARTESIAN_POINT('Ctrl Pts',(9.9488378237052,18.2088174848259,56.1170763702377));
#118593=CARTESIAN_POINT('Ctrl Pts',(9.83465594272455,18.198555818587,56.0894540405128));
#118594=CARTESIAN_POINT('Ctrl Pts',(9.71477342786885,18.1866460127634,56.0609648476129));
#118595=CARTESIAN_POINT('Ctrl Pts',(9.58924430789209,18.1727259445411,56.0317566527638));
#118596=CARTESIAN_POINT('Ctrl Pts',(9.45494599459543,18.1578334504045,56.0005080364794));
#118597=CARTESIAN_POINT('Ctrl Pts',(9.31418394076855,18.1406405777714,55.9684363423956));
#118598=CARTESIAN_POINT('Ctrl Pts',(9.1670458181545,18.120660125274,55.9357383746402));
#118599=CARTESIAN_POINT('Ctrl Pts',(9.02222235037387,18.1009939886732,55.9035547841771));
#118600=CARTESIAN_POINT('Ctrl Pts',(8.87122151575632,18.078627145095,55.8707644658192));
#118601=CARTESIAN_POINT('Ctrl Pts',(8.71415143451219,18.0530552455148,55.8375736497027));
#118602=CARTESIAN_POINT('Ctrl Pts',(8.63126405316597,18.0395607099836,55.8200585391809));
#118603=CARTESIAN_POINT('Ctrl Pts',(8.54668696617735,18.0251729808728,55.8024322121376));
#118604=CARTESIAN_POINT('Ctrl Pts',(8.46043936686297,18.0098135712464,55.7847271238998));
#118605=CARTESIAN_POINT('Ctrl Pts',(8.42076900727369,18.002748872544,55.7765835092075));
#118606=CARTESIAN_POINT('Ctrl Pts',(8.38074526108865,17.9954785609053,55.7684232534171));
#118607=CARTESIAN_POINT('Ctrl Pts',(8.3403705785985,17.987994825621,55.7602495303123));
#118608=CARTESIAN_POINT('Ctrl Pts',(8.1788518450135,17.9580561766696,55.7275505882243));
#118609=CARTESIAN_POINT('Ctrl Pts',(8.01173044245365,17.9247086739793,55.6946404784799));
#118610=CARTESIAN_POINT('Ctrl Pts',(7.83920340169692,17.8874645237823,55.6617567079231));
#118611=CARTESIAN_POINT('Ctrl Pts',(7.67027183132816,17.850996543156,55.629558236452));
#118612=CARTESIAN_POINT('Ctrl Pts',(7.49615737387537,17.8107924659674,55.5973851070223));
#118613=CARTESIAN_POINT('Ctrl Pts',(7.31708859833298,17.7663712540038,55.565469020871));
#118614=CARTESIAN_POINT('Ctrl Pts',(7.26721682661411,17.753999669199,55.5565801916607));
#118615=CARTESIAN_POINT('Ctrl Pts',(7.21696104451305,17.7413008471286,55.5477113488666));
#118616=CARTESIAN_POINT('Ctrl Pts',(7.1663268426109,17.7282640937974,55.5388676077781));
#118617=CARTESIAN_POINT('Ctrl Pts',(7.02456228981143,17.6917640713517,55.514107091104));
#118618=CARTESIAN_POINT('Ctrl Pts',(6.87983029660342,17.6526158128162,55.4895432732945));
#118619=CARTESIAN_POINT('Ctrl Pts',(6.73225177878659,17.6105711023872,55.4652840000943));
#118620=CARTESIAN_POINT('Ctrl Pts',(6.53967588068064,17.5557067631104,55.4336279610377));
#118621=CARTESIAN_POINT('Ctrl Pts',(6.34235173618997,17.4959262820899,55.4024975297025));
#118622=CARTESIAN_POINT('Ctrl Pts',(6.14052458838782,17.430705751096,55.3721629295414));
#118623=CARTESIAN_POINT('Ctrl Pts',(6.0112340933984,17.388925471151,55.3527305810549));
#118624=CARTESIAN_POINT('Ctrl Pts',(5.88009655935121,17.344912249901,55.3336246860117));
#118625=CARTESIAN_POINT('Ctrl Pts',(5.74718567469591,17.2985221805562,55.3149141909974));
#118626=CARTESIAN_POINT('Ctrl Pts',(5.57957686810175,17.2400214476715,55.2913191051001));
#118627=CARTESIAN_POINT('Ctrl Pts',(5.40914470359067,17.1777406306088,55.2683529979293));
#118628=CARTESIAN_POINT('Ctrl Pts',(5.23620340618366,17.1114219519761,55.2461528140407));
#118629=CARTESIAN_POINT('Ctrl Pts',(5.11243895042099,17.0639613668473,55.2302653787202));
#118630=CARTESIAN_POINT('Ctrl Pts',(4.98739047852652,17.0144327233601,55.2147701156798));
#118631=CARTESIAN_POINT('Ctrl Pts',(4.86118934214646,16.9627394489676,55.199715256373));
#118632=CARTESIAN_POINT('Ctrl Pts',(29.5338632414891,-0.462029067073086,
63.010868215388));
#118633=CARTESIAN_POINT('Ctrl Pts',(29.5346219246491,-0.433752793220286,
63.011230106753));
#118634=CARTESIAN_POINT('Ctrl Pts',(29.5608039722791,0.641998223276014,
63.023714156154));
#118635=CARTESIAN_POINT('Ctrl Pts',(29.4078372281691,2.83176758612401,62.95026782851));
#118636=CARTESIAN_POINT('Ctrl Pts',(28.5737667388991,6.01426195252202,62.55847749973));
#118637=CARTESIAN_POINT('Ctrl Pts',(27.1713456340891,8.95881369369201,61.93185808602));
#118638=CARTESIAN_POINT('Ctrl Pts',(25.3938118350091,11.44424088043,61.19592371053));
#118639=CARTESIAN_POINT('Ctrl Pts',(23.4862351945491,13.39803722808,60.47438298443));
#118640=CARTESIAN_POINT('Ctrl Pts',(21.5959186421791,14.88576337841,59.82526804813));
#118641=CARTESIAN_POINT('Ctrl Pts',(19.7728932383691,16.01167021338,59.25919610008));
#118642=CARTESIAN_POINT('Ctrl Pts',(17.9890179586191,16.88023517151,58.75958030935));
#118643=CARTESIAN_POINT('Ctrl Pts',(16.1694318501091,17.56205741783,58.30367386163));
#118644=CARTESIAN_POINT('Ctrl Pts',(14.2545233152291,18.07545203247,57.8825033362001));
#118645=CARTESIAN_POINT('Ctrl Pts',(12.2750306503891,18.39974030706,57.50985034058));
#118646=CARTESIAN_POINT('Ctrl Pts',(10.2979506383991,18.52298246441,57.20011317475));
#118647=CARTESIAN_POINT('Ctrl Pts',(8.29553577903909,18.45025449476,56.94745644735));
#118648=CARTESIAN_POINT('Ctrl Pts',(6.18046749893909,18.15452185092,56.74590079812));
#118649=CARTESIAN_POINT('Ctrl Pts',(3.8630583959391,17.55006605826,56.60308243839));
#118650=CARTESIAN_POINT('Ctrl Pts',(1.35289501732909,16.52026706539,56.54071687939));
#118651=CARTESIAN_POINT('Ctrl Pts',(-1.22835397511091,14.96025853102,56.57780430316));
#118652=CARTESIAN_POINT('Ctrl Pts',(-2.82698452737391,13.56768331313,56.66360640014));
#118653=CARTESIAN_POINT('Ctrl Pts',(-3.58348738863291,12.77819820572,56.71617340988));
#118654=CARTESIAN_POINT('Ctrl Pts',(30.0860529662091,-0.465286448929386,
62.05420413572));
#118655=CARTESIAN_POINT('Ctrl Pts',(30.0868281149291,-0.436810905979286,
62.05457485453));
#118656=CARTESIAN_POINT('Ctrl Pts',(30.1135782153191,0.646521910559514,
62.06736342767));
#118657=CARTESIAN_POINT('Ctrl Pts',(29.9572832439191,2.85177150159601,61.99211983581));
#118658=CARTESIAN_POINT('Ctrl Pts',(29.1052651413891,6.05572682568202,61.59085102028));
#118659=CARTESIAN_POINT('Ctrl Pts',(27.6732347629591,9.01845477515302,60.9493802108601));
#118660=CARTESIAN_POINT('Ctrl Pts',(25.8588487868591,11.51786388819,60.196375469));
#118661=CARTESIAN_POINT('Ctrl Pts',(23.9121691835891,13.48193550668,59.45836886149));
#118662=CARTESIAN_POINT('Ctrl Pts',(21.9833029704391,14.97718508481,58.7946079262));
#118663=CARTESIAN_POINT('Ctrl Pts',(20.1231372976191,16.10868985698,58.2158677272001));
#118664=CARTESIAN_POINT('Ctrl Pts',(18.3028628908391,16.98156509667,57.70514405855));
#118665=CARTESIAN_POINT('Ctrl Pts',(16.4460310900391,17.66679861647,57.23916702843));
#118666=CARTESIAN_POINT('Ctrl Pts',(14.4917463634591,18.18280526933,56.80876811987));
#118667=CARTESIAN_POINT('Ctrl Pts',(12.4713202820591,18.50878353077,56.42804576509));
#118668=CARTESIAN_POINT('Ctrl Pts',(10.4531101100391,18.6326885709,56.11172577456));
#118669=CARTESIAN_POINT('Ctrl Pts',(8.40879716453909,18.55957000061,55.85386194703));
#118670=CARTESIAN_POINT('Ctrl Pts',(6.24923249066909,18.26219087574,55.6483878136801));
#118671=CARTESIAN_POINT('Ctrl Pts',(3.88282255928909,17.6542832528,55.50319038629));
#118672=CARTESIAN_POINT('Ctrl Pts',(1.31936572697909,16.61847639235,55.44054243506));
#118673=CARTESIAN_POINT('Ctrl Pts',(-1.31681310253091,15.04922855625,55.47988027154));
#118674=CARTESIAN_POINT('Ctrl Pts',(-2.94946644714391,13.64834848308,55.5686612246301));
#118675=CARTESIAN_POINT('Ctrl Pts',(-3.72205763400691,12.85415388889,55.6229400250801));
#118676=CARTESIAN_POINT('Ctrl Pts',(29.6438402590691,-0.440906405366586,
61.0422837596));
#118677=CARTESIAN_POINT('Ctrl Pts',(29.6445863481391,-0.413922302316986,
61.04263099393));
#118678=CARTESIAN_POINT('Ctrl Pts',(29.6703352983091,0.612664138304914,
61.0546093697601));
#118679=CARTESIAN_POINT('Ctrl Pts',(29.5199825989191,2.70205115803401,60.98418855492));
#118680=CARTESIAN_POINT('Ctrl Pts',(28.6983885856991,5.74538083047302,60.60757066705));
#118681=CARTESIAN_POINT('Ctrl Pts',(27.3118968411491,8.57206800556001,60.00247848032));
#118682=CARTESIAN_POINT('Ctrl Pts',(25.5485386075391,10.96682866558,59.28852217894));
#118683=CARTESIAN_POINT('Ctrl Pts',(23.6522177073491,12.85399448613,58.58612492656));
#118684=CARTESIAN_POINT('Ctrl Pts',(21.7712823376891,14.29293457848,57.95274708762));
#118685=CARTESIAN_POINT('Ctrl Pts',(19.9569744205691,15.3825412991,57.399474373));
#118686=CARTESIAN_POINT('Ctrl Pts',(18.1821311163691,16.22315601275,56.9105053048901));
#118687=CARTESIAN_POINT('Ctrl Pts',(16.3728054944391,16.88285767912,56.46373198555));
#118688=CARTESIAN_POINT('Ctrl Pts',(14.4702883739891,17.37931439633,56.0503330424501));
#118689=CARTESIAN_POINT('Ctrl Pts',(12.5056416128591,17.69264386349,55.6837038022));
#118690=CARTESIAN_POINT('Ctrl Pts',(10.5455810396291,17.81158752306,55.37787002278));
#118691=CARTESIAN_POINT('Ctrl Pts',(8.56254414565909,17.74139242357,55.12695247192));
#118692=CARTESIAN_POINT('Ctrl Pts',(6.4700871073191,17.45633647142,54.9246919594001));
#118693=CARTESIAN_POINT('Ctrl Pts',(4.17965284087909,16.87426425135,54.77784196221));
#118694=CARTESIAN_POINT('Ctrl Pts',(1.70063539712909,15.88342358762,54.70699356138));
#118695=CARTESIAN_POINT('Ctrl Pts',(-0.847455673380912,14.38332778486,54.73062029495));
#118696=CARTESIAN_POINT('Ctrl Pts',(-2.42552047959091,13.04460583201,54.80507482908));
#118697=CARTESIAN_POINT('Ctrl Pts',(-3.17239712901691,12.28565963609,54.85169577897));
#118698=CARTESIAN_POINT('Ctrl Pts',(28.5669936237991,-0.408723671234686,
60.79836945316));
#118699=CARTESIAN_POINT('Ctrl Pts',(28.5676887698891,-0.383708334716086,
60.79867999721));
#118700=CARTESIAN_POINT('Ctrl Pts',(28.5916818669991,0.567970383760914,
60.80939260235));
#118701=CARTESIAN_POINT('Ctrl Pts',(28.4517075181491,2.50441369284601,60.74649096621));
#118702=CARTESIAN_POINT('Ctrl Pts',(27.6841573416491,5.33571041184002,60.40859830391));
#118703=CARTESIAN_POINT('Ctrl Pts',(26.3813035283791,7.98281775714401,59.8615184069));
#118704=CARTESIAN_POINT('Ctrl Pts',(24.7153386034591,10.23943783787,59.21096093285));
#118705=CARTESIAN_POINT('Ctrl Pts',(22.9178680255491,12.02508460897,58.5672777695));
#118706=CARTESIAN_POINT('Ctrl Pts',(21.1323491770191,13.38969369344,57.98459351753));
#118707=CARTESIAN_POINT('Ctrl Pts',(19.4095888040891,14.4239931358,57.47420458465));
#118708=CARTESIAN_POINT('Ctrl Pts',(17.7250457055691,15.22202253043,57.02215382759));
#118709=CARTESIAN_POINT('Ctrl Pts',(16.0093287990591,15.84802102278,56.60823505731));
#118710=CARTESIAN_POINT('Ctrl Pts',(14.2076068025491,16.3186709616,56.22423386201));
#118711=CARTESIAN_POINT('Ctrl Pts',(12.3500720308091,16.61530346173,55.88239455409));
#118712=CARTESIAN_POINT('Ctrl Pts',(10.5001323733591,16.72769787988,55.59558481383));
#118713=CARTESIAN_POINT('Ctrl Pts',(8.63169365612909,16.66136189094,55.35811567321));
#118714=CARTESIAN_POINT('Ctrl Pts',(6.66335190121909,16.39257307097,55.16358639907));
#118715=CARTESIAN_POINT('Ctrl Pts',(4.51205869883909,15.8446047236,55.01715480186));
#118716=CARTESIAN_POINT('Ctrl Pts',(2.18651660771909,14.91312142525,54.93685948768));
#118717=CARTESIAN_POINT('Ctrl Pts',(-0.202134170110909,13.50430936028,54.93959559631));
#118718=CARTESIAN_POINT('Ctrl Pts',(-1.68141039720091,12.24763887117,54.99407390047));
#118719=CARTESIAN_POINT('Ctrl Pts',(-2.38169007766091,11.53522211755,55.02989751292));
#118720=CARTESIAN_POINT('',(-2.29964905112222,12.0405998988806,54.9957533296306));
#118721=CARTESIAN_POINT('Ctrl Pts',(4.86118859572189,16.9627436220233,55.1997071844704));
#118722=CARTESIAN_POINT('Ctrl Pts',(4.68019380908066,16.8884238711505,55.1780230937973));
#118723=CARTESIAN_POINT('Ctrl Pts',(4.49747300369887,16.8105144441383,55.1576454460921));
#118724=CARTESIAN_POINT('Ctrl Pts',(4.31324259250774,16.728823982826,55.1386016985526));
#118725=CARTESIAN_POINT('Ctrl Pts',(4.08125567542773,16.6259575876845,55.1146213998996));
#118726=CARTESIAN_POINT('Ctrl Pts',(3.8468734963356,16.5170959661948,55.0927569037346));
#118727=CARTESIAN_POINT('Ctrl Pts',(3.61057048418905,16.4018815131822,55.0730204256337));
#118728=CARTESIAN_POINT('Ctrl Pts',(3.37819526251966,16.2885821361869,55.0536120040821));
#118729=CARTESIAN_POINT('Ctrl Pts',(3.14396235812309,16.1691393004344,55.036261253206));
#118730=CARTESIAN_POINT('Ctrl Pts',(2.90836790423341,16.0431949807409,55.0209649897225));
#118731=CARTESIAN_POINT('Ctrl Pts',(2.87714666293793,16.0265046982236,55.0189379117279));
#118732=CARTESIAN_POINT('Ctrl Pts',(2.8459015783102,16.0097002122994,55.016946895061));
#118733=CARTESIAN_POINT('Ctrl Pts',(2.81463386825826,15.9927806666211,55.0149919150382));
#118734=CARTESIAN_POINT('Ctrl Pts',(2.58345076949164,15.8676831461077,55.0005374398324));
#118735=CARTESIAN_POINT('Ctrl Pts',(2.35102690793354,15.7362970187507,54.9880538400737));
#118736=CARTESIAN_POINT('Ctrl Pts',(2.11788131495968,15.5982672566783,54.9775249063338));
#118737=CARTESIAN_POINT('Ctrl Pts',(2.07828347526746,15.5748240497037,54.9757366545163));
#118738=CARTESIAN_POINT('Ctrl Pts',(2.03866493000065,15.5511891631188,54.974004762886));
#118739=CARTESIAN_POINT('Ctrl Pts',(1.99902836376755,15.5273608138029,54.9723291226172));
#118740=CARTESIAN_POINT('Ctrl Pts',(1.76453865798392,15.3863924315389,54.9624160440894));
#118741=CARTESIAN_POINT('Ctrl Pts',(1.52941429199146,15.2386535900276,54.9544729303309));
#118742=CARTESIAN_POINT('Ctrl Pts',(1.29420737288338,15.083814302669,54.9484358207017));
#118743=CARTESIAN_POINT('Ctrl Pts',(1.27342059356983,15.0701301384973,54.9479022816969));
#118744=CARTESIAN_POINT('Ctrl Pts',(1.25263320162065,15.056390512645,54.9473836198031));
#118745=CARTESIAN_POINT('Ctrl Pts',(1.23184559706263,15.0425951949651,54.9468797853324));
#118746=CARTESIAN_POINT('Ctrl Pts',(1.14353560697248,14.9839898677281,54.9447393935912));
#118747=CARTESIAN_POINT('Ctrl Pts',(1.05522169704458,14.9243794649775,54.9428666185128));
#118748=CARTESIAN_POINT('Ctrl Pts',(0.966935191652489,14.8637462740514,
54.9412574715373));
#118749=CARTESIAN_POINT('Ctrl Pts',(0.922791938956445,14.8334296785884,
54.9404528980496));
#118750=CARTESIAN_POINT('Ctrl Pts',(0.87865553714637,14.8028573865017,54.9397142291387));
#118751=CARTESIAN_POINT('Ctrl Pts',(0.834530021960648,14.7720271720485,
54.9390409369179));
#118752=CARTESIAN_POINT('Ctrl Pts',(0.812467264367783,14.7566120648218,
54.9387042908075));
#118753=CARTESIAN_POINT('Ctrl Pts',(0.790407228415868,14.7411324770304,
54.9383839887219));
#118754=CARTESIAN_POINT('Ctrl Pts',(0.768350422076952,14.7255881303148,
54.9380799633647));
#118755=CARTESIAN_POINT('Ctrl Pts',(0.75180781732276,14.7139298702781,54.9378519443468));
#118756=CARTESIAN_POINT('Ctrl Pts',(0.735267029224624,14.7022351833486,
54.9376330809763));
#118757=CARTESIAN_POINT('Ctrl Pts',(0.718728273521809,14.6905039519781,
54.9374233444669));
#118758=CARTESIAN_POINT('Ctrl Pts',(0.713215354954205,14.6865935415213,
54.9373534322972));
#118759=CARTESIAN_POINT('Ctrl Pts',(0.706358237698069,14.6817233852973,
54.9372679778407));
#118760=CARTESIAN_POINT('Ctrl Pts',(0.702190203405758,14.6787605347623,
54.9372166491539));
#118761=CARTESIAN_POINT('Ctrl Pts',(0.414311150449465,14.4741214780138,
54.9336714638866));
#118762=CARTESIAN_POINT('Ctrl Pts',(0.130361881835239,14.2607100262735,
54.9329242570408));
#118763=CARTESIAN_POINT('Ctrl Pts',(-0.148954082189152,14.0384416901636,
54.9346480764321));
#118764=CARTESIAN_POINT('Ctrl Pts',(-0.223061625545815,13.9794699073921,
54.9351054366862));
#118765=CARTESIAN_POINT('Ctrl Pts',(-0.296842775194991,13.9198745072161,
54.9357367725867));
#118766=CARTESIAN_POINT('Ctrl Pts',(-0.370283853487526,13.8596536078829,
54.9365360485735));
#118767=CARTESIAN_POINT('Ctrl Pts',(-0.640247022236335,13.6382866946122,
54.9394741192435));
#118768=CARTESIAN_POINT('Ctrl Pts',(-0.905618976193242,13.4084677122387,
54.9446812477808));
#118769=CARTESIAN_POINT('Ctrl Pts',(-1.16567793374027,13.1703272706806,
54.9518066483159));
#118770=CARTESIAN_POINT('Ctrl Pts',(-1.41754491008076,12.9396883666207,
54.9587075953355));
#118771=CARTESIAN_POINT('Ctrl Pts',(-1.66442842803035,12.7012435830281,
54.9674079551425));
#118772=CARTESIAN_POINT('Ctrl Pts',(-1.90562432250537,12.4551152970694,
54.9775911038724));
#118773=CARTESIAN_POINT('Ctrl Pts',(-2.03874091225642,12.3192765086878,
54.9832112079575));
#118774=CARTESIAN_POINT('Ctrl Pts',(-2.17012420063582,12.1810974577443,
54.9892829940561));
#118775=CARTESIAN_POINT('Ctrl Pts',(-2.29964905112222,12.0405998988806,
54.9957533296306));
#118776=CARTESIAN_POINT('Ctrl Pts',(18.8783242222685,15.00000216221,57.3029867131023));
#118777=CARTESIAN_POINT('Ctrl Pts',(18.6127767826748,15.1297977097545,57.2303573983608));
#118778=CARTESIAN_POINT('Ctrl Pts',(18.3456529579163,15.2531803415356,57.1590406458946));
#118779=CARTESIAN_POINT('Ctrl Pts',(18.0769627299134,15.3701589810481,57.0890865260526));
#118780=CARTESIAN_POINT('Ctrl Pts',(17.9957291190046,15.4055253483233,57.0679371683146));
#118781=CARTESIAN_POINT('Ctrl Pts',(17.9143522632205,15.4403060098944,57.0469124191582));
#118782=CARTESIAN_POINT('Ctrl Pts',(17.832832288681,15.4745003070782,57.0260138163773));
#118783=CARTESIAN_POINT('Ctrl Pts',(17.8156701817998,15.4816991094124,57.0216141087397));
#118784=CARTESIAN_POINT('Ctrl Pts',(17.7985017315288,15.488871921816,57.0172199923451));
#118785=CARTESIAN_POINT('Ctrl Pts',(17.7813269427055,15.496018733811,57.0128314769495));
#118786=CARTESIAN_POINT('Ctrl Pts',(17.597031111528,15.5727083321772,56.9657400628558));
#118787=CARTESIAN_POINT('Ctrl Pts',(17.4120056425813,15.6464079374915,56.9192934226056));
#118788=CARTESIAN_POINT('Ctrl Pts',(17.2262544323235,15.7171175514224,56.8735045150547));
#118789=CARTESIAN_POINT('Ctrl Pts',(17.1333788271946,15.7524723583878,56.8506100612793));
#118790=CARTESIAN_POINT('Ctrl Pts',(17.0403217757781,15.7870796675443,56.8278800786812));
#118791=CARTESIAN_POINT('Ctrl Pts',(16.9470837154508,15.8209394790412,56.8053164191352));
#118792=CARTESIAN_POINT('Ctrl Pts',(16.9004646852872,15.8378693847897,56.7940345893622));
#118793=CARTESIAN_POINT('Ctrl Pts',(16.8538004022893,15.8546124161202,56.7827943427494));
#118794=CARTESIAN_POINT('Ctrl Pts',(16.807090919087,15.8711685730292,56.7715959255905));
#118795=CARTESIAN_POINT('Ctrl Pts',(16.7691902434841,15.8846024517454,56.7625093858366));
#118796=CARTESIAN_POINT('Ctrl Pts',(16.7320664876038,15.8976320223834,56.7536425910697));
#118797=CARTESIAN_POINT('Ctrl Pts',(16.6937562393354,15.9109424860321,56.7445276971792));
#118798=CARTESIAN_POINT('Ctrl Pts',(16.6848522395858,15.9140360803144,56.7424092297563));
#118799=CARTESIAN_POINT('Ctrl Pts',(16.6758840662253,15.917144647716,56.7402774022098));
#118800=CARTESIAN_POINT('Ctrl Pts',(16.6668269197058,15.9202764204705,56.7381264185738));
#118801=CARTESIAN_POINT('Ctrl Pts',(16.4836225612769,15.9836246744713,56.6946171768736));
#118802=CARTESIAN_POINT('Ctrl Pts',(16.2992644068695,16.0442560768477,56.6516427589442));
#118803=CARTESIAN_POINT('Ctrl Pts',(16.11368872958,16.1022137938751,56.6092177628598));
#118804=CARTESIAN_POINT('Ctrl Pts',(15.8774529239984,16.1759933331533,56.5552112072963));
#118805=CARTESIAN_POINT('Ctrl Pts',(15.6392447884627,16.2454417113728,56.5020946551783));
#118806=CARTESIAN_POINT('Ctrl Pts',(15.3989232603713,16.3106085166983,56.4498915487045));
#118807=CARTESIAN_POINT('Ctrl Pts',(15.1618975210043,16.3748816192254,56.3984043598226));
#118808=CARTESIAN_POINT('Ctrl Pts',(14.9228156990975,16.4349899187113,56.3478055828261));
#118809=CARTESIAN_POINT('Ctrl Pts',(14.6815204260846,16.4909365220136,56.2981269141177));
#118810=CARTESIAN_POINT('Ctrl Pts',(14.5535595378906,16.5206054706034,56.271781903323));
#118811=CARTESIAN_POINT('Ctrl Pts',(14.4249758180904,16.5491032729303,56.2456958206221));
#118812=CARTESIAN_POINT('Ctrl Pts',(14.2957435954912,16.576424990075,56.2198747060703));
#118813=CARTESIAN_POINT('Ctrl Pts',(14.2878336666268,16.5780972729989,56.2182942706711));
#118814=CARTESIAN_POINT('Ctrl Pts',(14.279922746965,16.5797646169782,56.216715115788));
#118815=CARTESIAN_POINT('Ctrl Pts',(14.2720108369673,16.5814270232247,56.215137242614));
#118816=CARTESIAN_POINT('Ctrl Pts',(13.9886158069621,16.6409724007936,56.1586197372808));
#118817=CARTESIAN_POINT('Ctrl Pts',(13.7039524089762,16.6941863964793,56.1037459715631));
#118818=CARTESIAN_POINT('Ctrl Pts',(13.4180554492033,16.741109133657,56.050550191522));
#118819=CARTESIAN_POINT('Ctrl Pts',(13.1340559574864,16.7877204495626,55.9977074662787));
#118820=CARTESIAN_POINT('Ctrl Pts',(12.8488388845799,16.8281239109499,55.9465203811792));
#118821=CARTESIAN_POINT('Ctrl Pts',(12.5624151426491,16.8623139613762,55.8970317856168));
#118822=CARTESIAN_POINT('Ctrl Pts',(12.4972314222718,16.8700948620504,55.8857692738108));
#118823=CARTESIAN_POINT('Ctrl Pts',(12.4319851226791,16.8775537685843,55.8745947731496));
#118824=CARTESIAN_POINT('Ctrl Pts',(12.3666762308545,16.8846902730156,55.8635088691272));
#118825=CARTESIAN_POINT('Ctrl Pts',(12.1858178738426,16.904453224586,55.8328089394323));
#118826=CARTESIAN_POINT('Ctrl Pts',(12.0044796821691,16.9217442788938,55.8027883025021));
#118827=CARTESIAN_POINT('Ctrl Pts',(11.8226672654872,16.9365537724192,55.7734537879868));
#118828=CARTESIAN_POINT('Ctrl Pts',(11.7183577198391,16.9450502853037,55.7566239699977));
#118829=CARTESIAN_POINT('Ctrl Pts',(11.6138924170508,16.9527331913848,55.7400200906268));
#118830=CARTESIAN_POINT('Ctrl Pts',(11.5092722772993,16.9596024906979,55.7236437786283));
#118831=CARTESIAN_POINT('Ctrl Pts',(11.4536892865923,16.9632520384885,55.7149433085297));
#118832=CARTESIAN_POINT('Ctrl Pts',(11.400122252971,16.9665326225997,55.7066281879219));
#118833=CARTESIAN_POINT('Ctrl Pts',(11.3470814439974,16.9695624093708,55.6984575201622));
#118834=CARTESIAN_POINT('Ctrl Pts',(11.3002870915886,16.9722353872653,55.6912490873732));
#118835=CARTESIAN_POINT('Ctrl Pts',(11.2539021857595,16.9747123402,55.6841533134244));
#118836=CARTESIAN_POINT('Ctrl Pts',(11.2069005490931,16.9770423115579,55.6770138507463));
#118837=CARTESIAN_POINT('Ctrl Pts',(11.0063457496235,16.9869842406395,55.6465499433747));
#118838=CARTESIAN_POINT('Ctrl Pts',(10.8051909091927,16.9937263467392,55.6169182014827));
#118839=CARTESIAN_POINT('Ctrl Pts',(10.6034419396794,16.9972686283256,55.58813544389));
#118840=CARTESIAN_POINT('Ctrl Pts',(10.5630955412427,16.9979770250258,55.5823793767896));
#118841=CARTESIAN_POINT('Ctrl Pts',(10.5227253892399,16.9985574497193,55.576657276456));
#118842=CARTESIAN_POINT('Ctrl Pts',(10.4823315117015,16.9990098854209,55.5709692927393));
#118843=CARTESIAN_POINT('Ctrl Pts',(10.320739004239,17.0008198186072,55.5482149644305));
#118844=CARTESIAN_POINT('Ctrl Pts',(10.1587669981462,17.0005819416682,55.5260065254767));
#118845=CARTESIAN_POINT('Ctrl Pts',(9.99641916947968,16.9982960003329,55.5043489511402));
#118846=CARTESIAN_POINT('Ctrl Pts',(9.89495391115787,16.9968673170544,55.4908132519397));
#118847=CARTESIAN_POINT('Ctrl Pts',(9.7933418469281,16.994638677846,55.4774927539923));
#118848=CARTESIAN_POINT('Ctrl Pts',(9.69158385139753,16.9916100826178,55.4643889746107));
#118849=CARTESIAN_POINT('Ctrl Pts',(9.64070485363225,16.9900957850037,55.45783708492));
#118850=CARTESIAN_POINT('Ctrl Pts',(9.58978937249366,16.9883814983837,55.4513393785284));
#118851=CARTESIAN_POINT('Ctrl Pts',(9.5388375149835,16.986467222751,55.4448960676726));
#118852=CARTESIAN_POINT('Ctrl Pts',(9.50095971915006,16.9850441432966,55.4401060869926));
#118853=CARTESIAN_POINT('Ctrl Pts',(9.46399488492687,16.98354948681,55.4354629744234));
#118854=CARTESIAN_POINT('Ctrl Pts',(9.42586210998851,16.9818974962683,55.430706000245));
#118855=CARTESIAN_POINT('Ctrl Pts',(9.41270003863564,16.981327288162,55.4290640627343));
#118856=CARTESIAN_POINT('Ctrl Pts',(9.39939882519323,16.9807379061749,55.427408684632));
#118857=CARTESIAN_POINT('Ctrl Pts',(9.38587291883542,16.9801244288179,55.4257295494624));
#118858=CARTESIAN_POINT('Ctrl Pts',(9.14440294537702,16.9691723818947,55.395752946482));
#118859=CARTESIAN_POINT('Ctrl Pts',(8.90351586532162,16.9536344281327,55.3671722628587));
#118860=CARTESIAN_POINT('Ctrl Pts',(8.66322315413537,16.9335124031959,55.3399705237772));
#118861=CARTESIAN_POINT('Ctrl Pts',(8.48386964246388,16.9184934048395,55.3196672553021));
#118862=CARTESIAN_POINT('Ctrl Pts',(8.30484714506715,16.9009200618216,55.3001323488735));
#118863=CARTESIAN_POINT('Ctrl Pts',(8.12616603302871,16.8807920330551,55.2813536914305));
#118864=CARTESIAN_POINT('Ctrl Pts',(7.91712955232603,16.8572445397087,55.2593848083213));
#118865=CARTESIAN_POINT('Ctrl Pts',(7.70855805259612,16.8302009995561,55.238450604365));
#118866=CARTESIAN_POINT('Ctrl Pts',(7.50046210261416,16.7996614123033,55.2185354391638));
#118867=CARTESIAN_POINT('Ctrl Pts',(7.39641412762318,16.7843916186769,55.2085778565632));
#118868=CARTESIAN_POINT('Ctrl Pts',(7.29248503207262,16.768247813263,55.1988751062129));
#118869=CARTESIAN_POINT('Ctrl Pts',(7.18867608397116,16.7512299960567,55.1894256651067));
#118870=CARTESIAN_POINT('Ctrl Pts',(7.13677160992043,16.7427210874536,55.1847009445537));
#118871=CARTESIAN_POINT('Ctrl Pts',(7.08489717240314,16.7339936759037,55.1800395558109));
#118872=CARTESIAN_POINT('Ctrl Pts',(7.0330529264252,16.7250477614135,55.1754413353781));
#118873=CARTESIAN_POINT('Ctrl Pts',(6.98768921119449,16.7172200862346,55.1714178924994));
#118874=CARTESIAN_POINT('Ctrl Pts',(6.94234861133948,16.7092251197422,55.1674428131252));
#118875=CARTESIAN_POINT('Ctrl Pts',(6.89703122952768,16.7010628619411,55.1635159990321));
#118876=CARTESIAN_POINT('Ctrl Pts',(6.89055731784029,16.6998968251124,55.1629550255902));
#118877=CARTESIAN_POINT('Ctrl Pts',(6.88523427686265,16.6989358196951,55.1624943851822));
#118878=CARTESIAN_POINT('Ctrl Pts',(6.87761091625737,16.6975545091299,55.1618360335067));
#118879=CARTESIAN_POINT('Ctrl Pts',(6.81796790451055,16.6867475269429,55.1566852766753));
#118880=CARTESIAN_POINT('Ctrl Pts',(6.75841106823449,16.675656026884,55.1516220895054));
#118881=CARTESIAN_POINT('Ctrl Pts',(6.69894050187817,16.6642799974611,55.1466458983541));
#118882=CARTESIAN_POINT('Ctrl Pts',(6.4278669534886,16.612426772392,55.1239638578846));
#118883=CARTESIAN_POINT('Ctrl Pts',(6.15858533275166,16.5546660050314,55.1030880538125));
#118884=CARTESIAN_POINT('Ctrl Pts',(5.89111960752089,16.4910081648164,55.0839395476397));
#118885=CARTESIAN_POINT('Ctrl Pts',(5.73725476114619,16.4543877574847,55.0729239980472));
#118886=CARTESIAN_POINT('Ctrl Pts',(5.58399094712087,16.4158148823987,55.0624803584915));
#118887=CARTESIAN_POINT('Ctrl Pts',(5.43133401166316,16.3752841611111,55.0525958371668));
#118888=CARTESIAN_POINT('Ctrl Pts',(5.1932133509905,16.3120626500699,55.0371775481697));
#118889=CARTESIAN_POINT('Ctrl Pts',(4.95656700803464,16.2440862458202,55.0231190695121));
#118890=CARTESIAN_POINT('Ctrl Pts',(4.72141062423708,16.1713549480517,55.0103787866828));
#118891=CARTESIAN_POINT('Ctrl Pts',(4.65556535494333,16.1509897263626,55.0068114272081));
#118892=CARTESIAN_POINT('Ctrl Pts',(4.58983691459802,16.1302518486424,55.003347472626));
#118893=CARTESIAN_POINT('Ctrl Pts',(4.52422559886721,16.1091410100962,54.9999861303057));
#118894=CARTESIAN_POINT('Ctrl Pts',(4.4726764875169,16.0925547710489,54.9973452107078));
#118895=CARTESIAN_POINT('Ctrl Pts',(4.42119967559925,16.0757383052224,54.994767633101));
#118896=CARTESIAN_POINT('Ctrl Pts',(4.36979535037543,16.0586918314921,54.9922527529268));
#118897=CARTESIAN_POINT('Ctrl Pts',(4.31137967123683,16.0393202837569,54.9893948526881));
#118898=CARTESIAN_POINT('Ctrl Pts',(4.25305758892359,16.0196515551977,54.9866179184494));
#118899=CARTESIAN_POINT('Ctrl Pts',(4.19482934568938,15.9996856457891,54.9839210346576));
#118900=CARTESIAN_POINT('Ctrl Pts',(4.14387963285945,15.9822154750566,54.9815612613397));
#118901=CARTESIAN_POINT('Ctrl Pts',(4.09300176550862,15.9645177752357,54.9792627771575));
#118902=CARTESIAN_POINT('Ctrl Pts',(4.04219590177801,15.9465925463056,54.9770249897373));
#118903=CARTESIAN_POINT('Ctrl Pts',(4.03493792124507,15.9440317993156,54.9767053058201));
#118904=CARTESIAN_POINT('Ctrl Pts',(4.02898435525666,15.9419279656044,54.976443828588));
#118905=CARTESIAN_POINT('Ctrl Pts',(4.02042636895411,15.9388963749819,54.976069652515));
#118906=CARTESIAN_POINT('Ctrl Pts',(3.76622253922922,15.8488469265306,54.9649552399189));
#118907=CARTESIAN_POINT('Ctrl Pts',(3.51477256686552,15.7533796106994,54.9553998714821));
#118908=CARTESIAN_POINT('Ctrl Pts',(3.26608481102119,15.6525216252025,54.947305074222));
#118909=CARTESIAN_POINT('Ctrl Pts',(3.01662939797749,15.5513523080985,54.9391852896866));
#118910=CARTESIAN_POINT('Ctrl Pts',(2.76995287456916,15.4447588538453,54.9325352163513));
#118911=CARTESIAN_POINT('Ctrl Pts',(2.52608079000258,15.3327212238872,54.9272690335963));
#118912=CARTESIAN_POINT('Ctrl Pts',(2.48924126768141,15.3157967252223,54.9264735195977));
#118913=CARTESIAN_POINT('Ctrl Pts',(2.45246577929163,15.2987479080524,54.9257096084919));
#118914=CARTESIAN_POINT('Ctrl Pts',(2.41575445572796,15.2815746123853,54.9249770288859));
#118915=CARTESIAN_POINT('Ctrl Pts',(2.33630193044391,15.2444072870004,54.9233915426102));
#118916=CARTESIAN_POINT('Ctrl Pts',(2.25714875042345,15.2066591154509,54.9219527803405));
#118917=CARTESIAN_POINT('Ctrl Pts',(2.17829605290603,15.168329539463,54.9206580947122));
#118918=CARTESIAN_POINT('Ctrl Pts',(1.99811405393256,15.080744715624,54.9176996791868));
#118919=CARTESIAN_POINT('Ctrl Pts',(1.81950057314376,14.9901250853999,54.9154933218064));
#118920=CARTESIAN_POINT('Ctrl Pts',(1.64246035550463,14.8964714583744,54.9139967485022));
#118921=CARTESIAN_POINT('Ctrl Pts',(1.51520136375156,14.8291519176044,54.912920990619));
#118922=CARTESIAN_POINT('Ctrl Pts',(1.3887556138919,14.7602645360824,54.9122120483486));
#118923=CARTESIAN_POINT('Ctrl Pts',(1.26312512636562,14.6898093136131,54.9118552464249));
#118924=CARTESIAN_POINT('Ctrl Pts',(1.20030988260248,14.6545817023784,54.9116768454631));
#118925=CARTESIAN_POINT('Ctrl Pts',(1.13769845398559,14.6189621309022,54.9115864926887));
#118926=CARTESIAN_POINT('Ctrl Pts',(1.07529108426283,14.5829505991502,54.9115824312511));
#118927=CARTESIAN_POINT('Ctrl Pts',(1.04408739940145,14.5649448332741,54.9115804005323));
#118928=CARTESIAN_POINT('Ctrl Pts',(1.0129347292531,14.5468410773292,54.9115999434474));
#118929=CARTESIAN_POINT('Ctrl Pts',(0.981833103304978,14.5286393313122,
54.9116408451671));
#118930=CARTESIAN_POINT('Ctrl Pts',(0.958506883843886,14.5149880217994,
54.9116715214569));
#118931=CARTESIAN_POINT('Ctrl Pts',(0.935209376744892,14.5012815928711,
54.9117142121395));
#118932=CARTESIAN_POINT('Ctrl Pts',(0.911940594245692,14.4875200445262,
54.9117688277537));
#118933=CARTESIAN_POINT('Ctrl Pts',(0.904184333412627,14.4829328617446,
54.9117870329584));
#118934=CARTESIAN_POINT('Ctrl Pts',(0.897758611058758,14.4791273142993,
54.9118029917875));
#118935=CARTESIAN_POINT('Ctrl Pts',(0.888681387048689,14.4737401230426,
54.911827415081));
#118936=CARTESIAN_POINT('Ctrl Pts',(0.665558682792343,14.3413202686666,
54.9124277518466));
#118937=CARTESIAN_POINT('Ctrl Pts',(0.446148520268852,14.2044010760549,
54.9141197456218));
#118938=CARTESIAN_POINT('Ctrl Pts',(0.230394363731208,14.0630045829432,
54.9167998817626));
#118939=CARTESIAN_POINT('Ctrl Pts',(0.0610584854176204,13.9520287401795,
54.9189034018741));
#118940=CARTESIAN_POINT('Ctrl Pts',(-0.106024987154981,13.8382939133016,
54.9216158988433));
#118941=CARTESIAN_POINT('Ctrl Pts',(-0.270873407103883,13.7217912087955,
54.9248921647364));
#118942=CARTESIAN_POINT('Ctrl Pts',(-0.480997690549446,13.5732908633788,
54.9290682619254));
#118943=CARTESIAN_POINT('Ctrl Pts',(-0.687491725483667,13.4202947474371,
54.9341601219953));
#118944=CARTESIAN_POINT('Ctrl Pts',(-0.890361482265292,13.2628389385424,
54.9400609774921));
#118945=CARTESIAN_POINT('Ctrl Pts',(-1.09332741816922,13.105308480958,54.9459646305429));
#118946=CARTESIAN_POINT('Ctrl Pts',(-1.2926659920302,12.943313812555,54.9526782096502));
#118947=CARTESIAN_POINT('Ctrl Pts',(-1.48835062831574,12.7768509970127,
54.9601021061303));
#118948=CARTESIAN_POINT('Ctrl Pts',(-1.68291599205989,12.6113403117047,
54.9674835395757));
#118949=CARTESIAN_POINT('Ctrl Pts',(-1.87386942063507,12.4414121400208,
54.9755673514226));
#118950=CARTESIAN_POINT('Ctrl Pts',(-2.06114762481944,12.2670275136822,
54.9842604084735));
#118951=CARTESIAN_POINT('Ctrl Pts',(-2.14132463669145,12.1923704636686,
54.9879820553219));
#118952=CARTESIAN_POINT('Ctrl Pts',(-2.22082754382691,12.1168962028275,
54.9918154127102));
#118953=CARTESIAN_POINT('Ctrl Pts',(-2.29964905112222,12.0405998988806,
54.9957533296306));
#118954=CARTESIAN_POINT('Origin',(18.4825952511691,16.31176789041,58.74984256216));
#118955=CARTESIAN_POINT('',(18.8783254659891,15.00000123934,57.30298584572));
#118956=CARTESIAN_POINT('Origin',(1.07038457110909,10.,122.41156512159));
#118957=CARTESIAN_POINT('',(-2.29973550275167,9.99999999999999,54.9957487971692));
#118958=CARTESIAN_POINT('Origin',(1.07038457110909,10.,122.41156512159));
#118959=CARTESIAN_POINT('',(-2.22484390946911,8.5000000000004,56.4938787766214));
#118960=CARTESIAN_POINT('Origin',(-2.22484394585091,10.,56.49387804884));
#118961=CARTESIAN_POINT('Origin',(1.07038457110909,8.5,122.41156512159));
#118962=CARTESIAN_POINT('Origin',(16.1036855657591,8.5,84.13007607401));
#118963=CARTESIAN_POINT('',(-5.70733149090974,8.50000000000053,58.926389902638));
#118964=CARTESIAN_POINT('Origin',(-2.02513312664091,8.50000000000101,60.48888938658));
#118965=CARTESIAN_POINT('Origin',(27.4324635166691,8.5,72.98888938658));
#118966=CARTESIAN_POINT('Origin',(-6.80729512863291,10.,84.10819367738));
#118967=CARTESIAN_POINT('Origin',(-6.80729512863291,10.,84.10819367738));
#118968=CARTESIAN_POINT('Origin',(-6.80729512863291,10.,84.10819367738));
#118969=CARTESIAN_POINT('Origin',(-8.75366715310791,111.0724296188,85.97453149762));
#118970=CARTESIAN_POINT('',(-6.54676185926042,20.0375488868139,85.5853826642543));
#118971=CARTESIAN_POINT('',(-6.54675958911291,20.03754888577,85.5853955666));
#118972=CARTESIAN_POINT('Ctrl Pts',(-6.54675958911291,20.03754888577,85.5853955666));
#118973=CARTESIAN_POINT('Ctrl Pts',(-6.40319215776023,20.012661527608,85.5600793384597));
#118974=CARTESIAN_POINT('Ctrl Pts',(-6.25833300218533,20.000145232378,85.5345367609292));
#118975=CARTESIAN_POINT('Ctrl Pts',(-6.11218320925691,20.00000000008,85.50876167007));
#118976=CARTESIAN_POINT('Ctrl Pts',(-6.75849120365391,19.73404260182,85.68410573154));
#118977=CARTESIAN_POINT('Ctrl Pts',(-6.63053349123792,19.71244938409,85.65842703201));
#118978=CARTESIAN_POINT('Ctrl Pts',(-6.35597941290291,19.68586616255,85.6033939864201));
#118979=CARTESIAN_POINT('Ctrl Pts',(-6.08345357859991,19.70033953338,85.5491449197301));
#118980=CARTESIAN_POINT('Ctrl Pts',(-5.94102950564791,19.71905670448,85.5209003835101));
#118981=CARTESIAN_POINT('Ctrl Pts',(-6.62106101297492,20.57404799423,85.3408528354601));
#118982=CARTESIAN_POINT('Ctrl Pts',(-6.52824231671291,20.56394872862,85.3292460691401));
#118983=CARTESIAN_POINT('Ctrl Pts',(-6.33031752895692,20.55653875518,85.3049678702));
#118984=CARTESIAN_POINT('Ctrl Pts',(-6.13666228963791,20.57814865479,85.28260809697));
#118985=CARTESIAN_POINT('Ctrl Pts',(-6.03628168416291,20.5971517614,85.27142548283));
#118986=CARTESIAN_POINT('Ctrl Pts',(-6.36266993702292,21.23542234314,85.92234121122));
#118987=CARTESIAN_POINT('Ctrl Pts',(-6.29925055569891,21.22679739812,85.92211116805));
#118988=CARTESIAN_POINT('Ctrl Pts',(-6.16331617101391,21.21744860275,85.92215843362));
#118989=CARTESIAN_POINT('Ctrl Pts',(-6.02869814368591,21.22697975827,85.92360048863));
#118990=CARTESIAN_POINT('Ctrl Pts',(-5.95843846253591,21.23704574569,85.92475783753));
#118991=CARTESIAN_POINT('Ctrl Pts',(-6.25992640685391,21.01016240069,86.8060857876899));
#118992=CARTESIAN_POINT('Ctrl Pts',(-6.18869458337992,20.99141388005,86.8023584409401));
#118993=CARTESIAN_POINT('Ctrl Pts',(-6.03375079962092,20.9610897075,86.79426130529));
#118994=CARTESIAN_POINT('Ctrl Pts',(-5.87513708666991,20.95225717825,86.7859377939401));
#118995=CARTESIAN_POINT('Ctrl Pts',(-5.79083124578291,20.95373020502,86.7815031789699));
#118996=CARTESIAN_POINT('',(-6.21291509723754,21.0225564527532,86.5058292049926));
#118997=CARTESIAN_POINT('Origin',(-6.37308545636947,20.0375750950329,86.5701674523326));
#118998=CARTESIAN_POINT('Origin',(-5.93751316552096,22.6785117147427,86.5230655023542));
#118999=CARTESIAN_POINT('Origin',(156.848906078169,21.,64.897742657285));
#119000=CARTESIAN_POINT('',(-5.70733054567061,21.0000000000039,87.0513884694204));
#119001=CARTESIAN_POINT('Origin',(27.4324635166691,21.,72.98888938658));
#119002=CARTESIAN_POINT('Origin',(-2.02513312664091,21.00000000001,85.48888938658));
#119003=CARTESIAN_POINT('Ctrl Pts',(-8.35462806748892,22.42643511175,84.29934907621));
#119004=CARTESIAN_POINT('Ctrl Pts',(-8.35090947121791,22.37969257573,84.32927895922));
#119005=CARTESIAN_POINT('Ctrl Pts',(-8.33351057093391,22.20164105692,84.44276426472));
#119006=CARTESIAN_POINT('Ctrl Pts',(-8.28365361158691,21.90483406201,84.6285915005799));
#119007=CARTESIAN_POINT('Ctrl Pts',(-8.18724379590092,21.54970983089,84.84428475201));
#119008=CARTESIAN_POINT('Ctrl Pts',(-8.07006104322492,21.23582300564,85.0284324468699));
#119009=CARTESIAN_POINT('Ctrl Pts',(-7.93917357924691,20.96122182353,85.18316506841));
#119010=CARTESIAN_POINT('Ctrl Pts',(-7.79858230655091,20.72092123751,85.31219748715));
#119011=CARTESIAN_POINT('Ctrl Pts',(-7.6482694193289,20.5075413273,85.4200547810799));
#119012=CARTESIAN_POINT('Ctrl Pts',(-7.4836205707029,20.31265218618,85.51083397843));
#119013=CARTESIAN_POINT('Ctrl Pts',(-7.29258471097291,20.12666462895,85.58725205448));
#119014=CARTESIAN_POINT('Ctrl Pts',(-7.05745176478091,19.9467868938,85.6450057031999));
#119015=CARTESIAN_POINT('Ctrl Pts',(-6.76628674550091,19.79030673,85.6657564249));
#119016=CARTESIAN_POINT('Ctrl Pts',(-6.54310988125591,19.72773437946,85.6357518205));
#119017=CARTESIAN_POINT('Ctrl Pts',(-6.42976359251691,19.71267560486,85.60686271593));
#119018=CARTESIAN_POINT('Ctrl Pts',(-7.94697006594592,23.04092220471,84.80596115758));
#119019=CARTESIAN_POINT('Ctrl Pts',(-7.93335072749191,22.99384694058,84.82825711759));
#119020=CARTESIAN_POINT('Ctrl Pts',(-7.87927599267992,22.8151897012,84.91112157838));
#119021=CARTESIAN_POINT('Ctrl Pts',(-7.77554997450592,22.52107215757,85.0361032601));
#119022=CARTESIAN_POINT('Ctrl Pts',(-7.63029827947891,22.17542681458,85.16338885188));
#119023=CARTESIAN_POINT('Ctrl Pts',(-7.48571075372192,21.87555618959,85.25742491269));
#119024=CARTESIAN_POINT('Ctrl Pts',(-7.34661185907992,21.61836861234,85.32424726386));
#119025=CARTESIAN_POINT('Ctrl Pts',(-7.21476913077092,21.3981324291,85.36956564192));
#119026=CARTESIAN_POINT('Ctrl Pts',(-7.08904716940091,21.20725692061,85.39810235033));
#119027=CARTESIAN_POINT('Ctrl Pts',(-6.96603251958891,21.03773902674,85.4130071847901));
#119028=CARTESIAN_POINT('Ctrl Pts',(-6.83949966896591,20.88136131406,85.41536453852));
#119029=CARTESIAN_POINT('Ctrl Pts',(-6.70427653768091,20.7367020702,85.40328206329));
#119030=CARTESIAN_POINT('Ctrl Pts',(-6.56371790810491,20.6183554452,85.37415966696));
#119031=CARTESIAN_POINT('Ctrl Pts',(-6.47361817696992,20.57431207621,85.34615928593));
#119032=CARTESIAN_POINT('Ctrl Pts',(-6.42908978116191,20.56370269296,85.33103245456));
#119033=CARTESIAN_POINT('Ctrl Pts',(-8.4348349802069,23.50406104764,85.39579476813));
#119034=CARTESIAN_POINT('Ctrl Pts',(-8.40969820765591,23.45673500638,85.42776643184));
#119035=CARTESIAN_POINT('Ctrl Pts',(-8.31090848053591,23.27762123549,85.54572550045));
#119036=CARTESIAN_POINT('Ctrl Pts',(-8.12775601955191,22.98553073094,85.71799464822));
#119037=CARTESIAN_POINT('Ctrl Pts',(-7.8815186557559,22.64702962472,85.88325981061));
#119038=CARTESIAN_POINT('Ctrl Pts',(-7.64457453124492,22.35772300805,85.9958072564301));
#119039=CARTESIAN_POINT('Ctrl Pts',(-7.42361387635791,22.11366006255,86.06659135295));
#119040=CARTESIAN_POINT('Ctrl Pts',(-7.22054442786891,21.90854641711,86.10532035578));
#119041=CARTESIAN_POINT('Ctrl Pts',(-7.03315811824792,21.73463247331,86.11946431853));
#119042=CARTESIAN_POINT('Ctrl Pts',(-6.85657254671691,21.58423688521,86.11359046581));
#119043=CARTESIAN_POINT('Ctrl Pts',(-6.68328271986891,21.45017610857,86.08876818199));
#119044=CARTESIAN_POINT('Ctrl Pts',(-6.51001739351891,21.33206103707,86.0429626720599));
#119045=CARTESIAN_POINT('Ctrl Pts',(-6.34791600768991,21.24245565535,85.97816203645));
#119046=CARTESIAN_POINT('Ctrl Pts',(-6.25807374458691,21.21237757737,85.93509102818));
#119047=CARTESIAN_POINT('Ctrl Pts',(-6.21484666490891,21.20512169981,85.91670410992));
#119048=CARTESIAN_POINT('Ctrl Pts',(-9.31121502261391,23.33454012732,85.4558723699601));
#119049=CARTESIAN_POINT('Ctrl Pts',(-9.28491347993491,23.28730587704,85.5047740045099));
#119050=CARTESIAN_POINT('Ctrl Pts',(-9.17983912464392,23.10835920862,85.68707148129));
#119051=CARTESIAN_POINT('Ctrl Pts',(-8.97424581930491,22.81552675479,85.96561818075));
#119052=CARTESIAN_POINT('Ctrl Pts',(-8.6798271479399,22.4744106712,86.2557803286799));
#119053=CARTESIAN_POINT('Ctrl Pts',(-8.38155509163591,22.1812373514,86.4762244427199));
#119054=CARTESIAN_POINT('Ctrl Pts',(-8.09015620392992,21.93237044768,86.63872510375));
#119055=CARTESIAN_POINT('Ctrl Pts',(-7.80990628928392,21.72172155819,86.75483732633));
#119056=CARTESIAN_POINT('Ctrl Pts',(-7.53868429503691,21.54159923843,86.83447387236));
#119057=CARTESIAN_POINT('Ctrl Pts',(-7.26899562207991,21.38420438667,86.8845110107599));
#119058=CARTESIAN_POINT('Ctrl Pts',(-6.98628046299991,21.24197502821,86.90763628799));
#119059=CARTESIAN_POINT('Ctrl Pts',(-6.67655582865691,21.11414409591,86.89926709383));
#119060=CARTESIAN_POINT('Ctrl Pts',(-6.34315059286091,21.01401866802,86.85006128191));
#119061=CARTESIAN_POINT('Ctrl Pts',(-6.12047856213391,20.97882892856,86.79050676521));
#119062=CARTESIAN_POINT('Ctrl Pts',(-6.00968384453291,20.97034558027,86.75522540636));
#119063=CARTESIAN_POINT('Ctrl Pts',(-8.23395173885521,22.5,84.5714980228307));
#119064=CARTESIAN_POINT('Ctrl Pts',(-8.22142766674582,22.4758562186449,
84.6100482185526));
#119065=CARTESIAN_POINT('Ctrl Pts',(-8.20731320283664,22.4496738732414,
84.6514255097405));
#119066=CARTESIAN_POINT('Ctrl Pts',(-8.1912618489509,22.4215351161334,84.6955546689892));
#119067=CARTESIAN_POINT('Ctrl Pts',(-8.17628816671385,22.3952855666885,
84.7367210411645));
#119068=CARTESIAN_POINT('Ctrl Pts',(-8.15962851767868,22.3673340632109,
84.7802824882887));
#119069=CARTESIAN_POINT('Ctrl Pts',(-8.14097429954895,22.33774180324,84.8261449122856));
#119070=CARTESIAN_POINT('Ctrl Pts',(-8.12603890112914,22.3140489210331,
84.8628644129437));
#119071=CARTESIAN_POINT('Ctrl Pts',(-8.10982451010508,22.2893043566117,
84.9010584792541));
#119072=CARTESIAN_POINT('Ctrl Pts',(-8.09216019510566,22.2635324072133,
84.9406592830494));
#119073=CARTESIAN_POINT('Ctrl Pts',(-8.07270453650607,22.2351469165246,
84.9842760164997));
#119074=CARTESIAN_POINT('Ctrl Pts',(-8.05149008683296,22.2055140674626,
85.0296011650061));
#119075=CARTESIAN_POINT('Ctrl Pts',(-8.02827282937339,22.1746900474528,
85.0764886326811));
#119076=CARTESIAN_POINT('Ctrl Pts',(-8.00665737524525,22.1459926359809,
85.1201412436097));
#119077=CARTESIAN_POINT('Ctrl Pts',(-7.98330611454984,22.116262884349,85.1651482272115));
#119078=CARTESIAN_POINT('Ctrl Pts',(-7.95800680800294,22.0855457664435,
85.2113489761293));
#119079=CARTESIAN_POINT('Ctrl Pts',(-7.94921119087629,22.0748665801256,
85.2274112384562));
#119080=CARTESIAN_POINT('Ctrl Pts',(-7.94017995739716,22.0640680393239,
85.2436173769373));
#119081=CARTESIAN_POINT('Ctrl Pts',(-7.93090361526843,22.053151982212,85.2599592296446));
#119082=CARTESIAN_POINT('Ctrl Pts',(-7.906206213193,22.0240889908057,85.303467899481));
#119083=CARTESIAN_POINT('Ctrl Pts',(-7.8797728759181,21.9941928412466,85.3479419904631));
#119084=CARTESIAN_POINT('Ctrl Pts',(-7.85140570019092,21.9635035437492,
85.3931920714271));
#119085=CARTESIAN_POINT('Ctrl Pts',(-7.82485750363657,21.9347821260828,
85.4355405961829));
#119086=CARTESIAN_POINT('Ctrl Pts',(-7.7966159059768,21.9053659437477,85.4785689025909));
#119087=CARTESIAN_POINT('Ctrl Pts',(-7.76649755550958,21.8752897319992,
85.5220796372438));
#119088=CARTESIAN_POINT('Ctrl Pts',(-7.76443396327619,21.873229026947,85.525060823554));
#119089=CARTESIAN_POINT('Ctrl Pts',(-7.76236155050475,21.8711652245217,
85.5280442567256));
#119090=CARTESIAN_POINT('Ctrl Pts',(-7.76028025348173,21.869098336431,85.5310298651969));
#119091=CARTESIAN_POINT('Ctrl Pts',(-7.73211084979391,21.841123951054,85.571438710909));
#119092=CARTESIAN_POINT('Ctrl Pts',(-7.70231553838991,21.8125833290727,
85.6122494955127));
#119093=CARTESIAN_POINT('Ctrl Pts',(-7.67073246783274,21.7835331002349,
85.6532530028498));
#119094=CARTESIAN_POINT('Ctrl Pts',(-7.65172373904734,21.7660487989498,
85.6779315580527));
#119095=CARTESIAN_POINT('Ctrl Pts',(-7.63206708837751,21.7483801122145,
85.702679152938));
#119096=CARTESIAN_POINT('Ctrl Pts',(-7.61172320807623,21.7305417927462,
85.7274421778844));
#119097=CARTESIAN_POINT('Ctrl Pts',(-7.60387233078295,21.7236578327941,
85.736998440868));
#119098=CARTESIAN_POINT('Ctrl Pts',(-7.59591906966474,21.7167486318406,
85.7465569330663));
#119099=CARTESIAN_POINT('Ctrl Pts',(-7.58786101727019,21.7098151309467,
85.7561143014515));
#119100=CARTESIAN_POINT('Ctrl Pts',(-7.58287821376429,21.7055277087669,
85.7620242268733));
#119101=CARTESIAN_POINT('Ctrl Pts',(-7.57785533858723,21.7012309955984,
85.7679337194716));
#119102=CARTESIAN_POINT('Ctrl Pts',(-7.57279185930897,21.6969253210417,
85.7738419360785));
#119103=CARTESIAN_POINT('Ctrl Pts',(-7.56616586015563,21.6912909746961,
85.7815733468504));
#119104=CARTESIAN_POINT('Ctrl Pts',(-7.55947028595343,21.6856412267916,
85.7893025976754));
#119105=CARTESIAN_POINT('Ctrl Pts',(-7.55270397316235,21.6799769114545,
85.7970277121451));
#119106=CARTESIAN_POINT('Ctrl Pts',(-7.5493208167668,21.677144753786,85.80089026938));
#119107=CARTESIAN_POINT('Ctrl Pts',(-7.54591997503914,21.6743089546902,
85.8047517922779));
#119108=CARTESIAN_POINT('Ctrl Pts',(-7.54250128881515,21.6714696081392,
85.8086120319138));
#119109=CARTESIAN_POINT('Ctrl Pts',(-7.54079194570317,21.6700499348637,
85.8105421517318));
#119110=CARTESIAN_POINT('Ctrl Pts',(-7.53907814141567,21.6686293747617,
85.8124719507154));
#119111=CARTESIAN_POINT('Ctrl Pts',(-7.53735985637281,21.6672079404422,
85.8144013971823));
#119112=CARTESIAN_POINT('Ctrl Pts',(-7.53564157132995,21.6657865061226,
85.8163308436492));
#119113=CARTESIAN_POINT('Ctrl Pts',(-7.53325512565926,21.6638173628125,
85.8190010194744));
#119114=CARTESIAN_POINT('Ctrl Pts',(-7.53219153923514,21.662941027586,85.8201886471735));
#119115=CARTESIAN_POINT('Ctrl Pts',(-7.5082070923888,21.6431791961245,85.8469702915965));
#119116=CARTESIAN_POINT('Ctrl Pts',(-7.48262569868808,21.6226690970833,
85.8745392519396));
#119117=CARTESIAN_POINT('Ctrl Pts',(-7.45529229994458,21.6014761715685,
85.9027111175446));
#119118=CARTESIAN_POINT('Ctrl Pts',(-7.44255729541833,21.5916020975505,
85.9158367752558));
#119119=CARTESIAN_POINT('Ctrl Pts',(-7.42944167748955,21.5815800239868,
85.9290927323526));
#119120=CARTESIAN_POINT('Ctrl Pts',(-7.41592801790452,21.5714178742797,
85.9424570368911));
#119121=CARTESIAN_POINT('Ctrl Pts',(-7.38929896106609,21.5513930645344,
85.968791785293));
#119122=CARTESIAN_POINT('Ctrl Pts',(-7.36112512444487,21.530822813742,85.9955496136367));
#119123=CARTESIAN_POINT('Ctrl Pts',(-7.33127204040911,21.5097958253814,
86.0225360407876));
#119124=CARTESIAN_POINT('Ctrl Pts',(-7.30339328044189,21.4901594501031,
86.047737729297));
#119125=CARTESIAN_POINT('Ctrl Pts',(-7.27405020128941,21.4701247211595,
86.0731388693538));
#119126=CARTESIAN_POINT('Ctrl Pts',(-7.24311923952744,21.4497833014211,
86.0985477000223));
#119127=CARTESIAN_POINT('Ctrl Pts',(-7.21216793008562,21.4294285002463,
86.1239732456819));
#119128=CARTESIAN_POINT('Ctrl Pts',(-7.17962619705669,21.4087658566656,
86.1494066116004));
#119129=CARTESIAN_POINT('Ctrl Pts',(-7.14537550743067,21.3879312712363,
86.174626888892));
#119130=CARTESIAN_POINT('Ctrl Pts',(-7.13907688309786,21.3840998381124,
86.179264840827));
#119131=CARTESIAN_POINT('Ctrl Pts',(-7.13272043120045,21.3802626745631,
86.1838954779573));
#119132=CARTESIAN_POINT('Ctrl Pts',(-7.12630536519258,21.3764207432868,
86.1885172729001));
#119133=CARTESIAN_POINT('Ctrl Pts',(-7.10844112800482,21.3657219957613,
86.2013877314412));
#119134=CARTESIAN_POINT('Ctrl Pts',(-7.0912092503863,21.3556240801419,86.2133797962381));
#119135=CARTESIAN_POINT('Ctrl Pts',(-7.07430698339713,21.3459028412265,
86.2247499007996));
#119136=CARTESIAN_POINT('Ctrl Pts',(-7.07122130368359,21.3441281307849,
86.2268256283342));
#119137=CARTESIAN_POINT('Ctrl Pts',(-7.06814652587917,21.342366022409,86.2288805256242));
#119138=CARTESIAN_POINT('Ctrl Pts',(-7.06508069946555,21.3406152175656,
86.2309160183396));
#119139=CARTESIAN_POINT('Ctrl Pts',(-7.04789054710154,21.3307984184523,
86.2423290682622));
#119140=CARTESIAN_POINT('Ctrl Pts',(-7.03098420424403,21.3213352771548,
86.2531353338268));
#119141=CARTESIAN_POINT('Ctrl Pts',(-7.01400310668316,21.312011519002,86.2635653853502));
#119142=CARTESIAN_POINT('Ctrl Pts',(-6.9970220091223,21.3026877608493,86.2739954368736));
#119143=CARTESIAN_POINT('Ctrl Pts',(-6.97996598709154,21.2935030330653,
86.2840493949244));
#119144=CARTESIAN_POINT('Ctrl Pts',(-6.96244875624373,21.2842670815851,
86.2939168179826));
#119145=CARTESIAN_POINT('Ctrl Pts',(-6.93266456847538,21.26856338301,86.31069419471));
#119146=CARTESIAN_POINT('Ctrl Pts',(-6.90228320749175,21.2531257985842,
86.3265648508905));
#119147=CARTESIAN_POINT('Ctrl Pts',(-6.87132227451052,21.2380561271013,
86.3414757926713));
#119148=CARTESIAN_POINT('Ctrl Pts',(-6.82196897998102,21.2140343078747,
86.365244588717));
#119149=CARTESIAN_POINT('Ctrl Pts',(-6.77114060472277,21.1909468139287,
86.3865756596193));
#119150=CARTESIAN_POINT('Ctrl Pts',(-6.7189898404278,21.169247598944,86.4053578137257));
#119151=CARTESIAN_POINT('Ctrl Pts',(-6.69360340937748,21.1586846545173,
86.4145007642968));
#119152=CARTESIAN_POINT('Ctrl Pts',(-6.66790423558804,21.1484509219892,
86.4230393996217));
#119153=CARTESIAN_POINT('Ctrl Pts',(-6.64191335523892,21.1386003907898,
86.43095830036));
#119154=CARTESIAN_POINT('Ctrl Pts',(-6.59340489783472,21.1202157086753,
86.4457378558807));
#119155=CARTESIAN_POINT('Ctrl Pts',(-6.54387772623071,21.1031655777177,
86.4583594906108));
#119156=CARTESIAN_POINT('Ctrl Pts',(-6.49343465793604,21.0877698814451,
86.4688980397014));
#119157=CARTESIAN_POINT('Ctrl Pts',(-6.45258501756962,21.0753021891103,
86.4774323330125));
#119158=CARTESIAN_POINT('Ctrl Pts',(-6.41113526624891,21.0639193972677,
86.484600503558));
#119159=CARTESIAN_POINT('Ctrl Pts',(-6.36916128441197,21.0537978031306,
86.4904298740942));
#119160=CARTESIAN_POINT('Ctrl Pts',(-6.32275972737502,21.0426085447591,
86.4968741487993));
#119161=CARTESIAN_POINT('Ctrl Pts',(-6.27571569550032,21.0329606922833,
86.5016818168602));
#119162=CARTESIAN_POINT('Ctrl Pts',(-6.22791363557178,21.024996082316,86.5048800287462));
#119163=CARTESIAN_POINT('Ctrl Pts',(-6.22292237448476,21.0241644560668,
86.5052139706424));
#119164=CARTESIAN_POINT('Ctrl Pts',(-6.21792289450644,21.023351190184,86.505530354876));
#119165=CARTESIAN_POINT('Ctrl Pts',(-6.21291509723754,21.0225564527532,
86.5058292049926));
#119166=CARTESIAN_POINT('Ctrl Pts',(-8.23395173885521,22.5,84.5714980228307));
#119167=CARTESIAN_POINT('Ctrl Pts',(-8.21760659462262,22.4147034792435,
84.621797380569));
#119168=CARTESIAN_POINT('Ctrl Pts',(-8.19943848710039,22.3338593791439,
84.6687450527327));
#119169=CARTESIAN_POINT('Ctrl Pts',(-8.18020402924739,22.2574714230342,
84.7124495350668));
#119170=CARTESIAN_POINT('Ctrl Pts',(-8.16709282862747,22.2054014439813,
84.7422407691245));
#119171=CARTESIAN_POINT('Ctrl Pts',(-8.15348570968668,22.155401258526,84.7705256576035));
#119172=CARTESIAN_POINT('Ctrl Pts',(-8.1396129664063,22.1074638808062,84.7973449949855));
#119173=CARTESIAN_POINT('Ctrl Pts',(-8.12311399437653,22.0504515481914,
84.8292414619193));
#119174=CARTESIAN_POINT('Ctrl Pts',(-8.1062398891631,21.9963593206321,84.8590634254539));
#119175=CARTESIAN_POINT('Ctrl Pts',(-8.08935621921663,21.9452011132389,
84.8868623392333));
#119176=CARTESIAN_POINT('Ctrl Pts',(-8.07167595547547,21.8916291942128,
84.9159728423939));
#119177=CARTESIAN_POINT('Ctrl Pts',(-8.05396691424662,21.841263506198,84.9428994902048));
#119178=CARTESIAN_POINT('Ctrl Pts',(-8.03656426649347,21.7941099687286,
84.9677854423284));
#119179=CARTESIAN_POINT('Ctrl Pts',(-8.03184007172358,21.7813094743294,
84.974541085868));
#119180=CARTESIAN_POINT('Ctrl Pts',(-8.02713820360347,21.7687455339146,
84.9811463777592));
#119181=CARTESIAN_POINT('Ctrl Pts',(-8.02246480578853,21.7564179432622,
84.9876042296749));
#119182=CARTESIAN_POINT('Ctrl Pts',(-8.0190828900531,21.7474970521979,84.9922774699757));
#119183=CARTESIAN_POINT('Ctrl Pts',(-8.01571587757638,21.7386999287141,
84.9968734997127));
#119184=CARTESIAN_POINT('Ctrl Pts',(-8.01236595424368,21.7300264779375,
85.001393387132));
#119185=CARTESIAN_POINT('Ctrl Pts',(-7.99985006379615,21.6976209722166,
85.0182804648816));
#119186=CARTESIAN_POINT('Ctrl Pts',(-7.98757294713772,21.6669439334479,
85.034105627324));
#119187=CARTESIAN_POINT('Ctrl Pts',(-7.97563821227694,21.6379953616346,
85.0489286136373));
#119188=CARTESIAN_POINT('Ctrl Pts',(-7.96967084484655,21.623521075728,85.0563401067939));
#119189=CARTESIAN_POINT('Ctrl Pts',(-7.9637888644607,21.6094789065459,85.063501084823));
#119190=CARTESIAN_POINT('Ctrl Pts',(-7.95800396907429,21.5958688540644,
85.0704190837983));
#119191=CARTESIAN_POINT('Ctrl Pts',(-7.95511152138109,21.5890638278237,
85.0738780832859));
#119192=CARTESIAN_POINT('Ctrl Pts',(-7.95224333724095,21.5823668307585,
85.0772763315146));
#119193=CARTESIAN_POINT('Ctrl Pts',(-7.94940079325356,21.5757778628675,
85.0806147757484));
#119194=CARTESIAN_POINT('Ctrl Pts',(-7.94715518130021,21.5705725731264,
85.0832521492807));
#119195=CARTESIAN_POINT('Ctrl Pts',(-7.94539568124722,21.5665142395513,
85.0853058853073));
#119196=CARTESIAN_POINT('Ctrl Pts',(-7.94300939935868,21.5610441974117,
85.0880715302674));
#119197=CARTESIAN_POINT('Ctrl Pts',(-7.94237507422545,21.5595901423709,
85.0888066982776));
#119198=CARTESIAN_POINT('Ctrl Pts',(-7.94169623917092,21.5580363940842,
85.0895920510289));
#119199=CARTESIAN_POINT('Ctrl Pts',(-7.94095142577195,21.5563350467186,
85.0904516160242));
#119200=CARTESIAN_POINT('Ctrl Pts',(-7.92481966153642,21.5194859048771,
85.109068762102));
#119201=CARTESIAN_POINT('Ctrl Pts',(-7.90841653112025,21.4834288245106,
85.1270711143947));
#119202=CARTESIAN_POINT('Ctrl Pts',(-7.89179152635374,21.4481629112508,
85.144469492258));
#119203=CARTESIAN_POINT('Ctrl Pts',(-7.86346596351681,21.3880771033924,
85.1741127225818));
#119204=CARTESIAN_POINT('Ctrl Pts',(-7.83449617097394,21.3302906458657,
85.2020005238258));
#119205=CARTESIAN_POINT('Ctrl Pts',(-7.80511118203973,21.2748094023012,
85.2281791540894));
#119206=CARTESIAN_POINT('Ctrl Pts',(-7.79107260695249,21.2483034333707,
85.2406859026016));
#119207=CARTESIAN_POINT('Ctrl Pts',(-7.77693928027529,21.2223229817798,
85.2528030566652));
#119208=CARTESIAN_POINT('Ctrl Pts',(-7.76273610728766,21.1968654811886,
85.2645382455123));
#119209=CARTESIAN_POINT('Ctrl Pts',(-7.76002406525863,21.1920044679757,
85.2667790353273));
#119210=CARTESIAN_POINT('Ctrl Pts',(-7.75730945440262,21.1871625853629,
85.2690059210676));
#119211=CARTESIAN_POINT('Ctrl Pts',(-7.75459243225009,21.1823398204644,
85.2712189735255));
#119212=CARTESIAN_POINT('Ctrl Pts',(-7.72656223953097,21.1325857066023,
85.2940499566427));
#119213=CARTESIAN_POINT('Ctrl Pts',(-7.69827563591021,21.0848691356955,
85.3154067867001));
#119214=CARTESIAN_POINT('Ctrl Pts',(-7.66989477041555,21.03918914901,85.3353556251637));
#119215=CARTESIAN_POINT('Ctrl Pts',(-7.65432883088826,21.0141352298303,
85.3462968846268));
#119216=CARTESIAN_POINT('Ctrl Pts',(-7.63873440030209,20.9896940454143,
85.3568150785505));
#119217=CARTESIAN_POINT('Ctrl Pts',(-7.62313693229151,20.9658655957017,
85.3669241648387));
#119218=CARTESIAN_POINT('Ctrl Pts',(-7.62011930331171,20.9612555256347,
85.368879961236));
#119219=CARTESIAN_POINT('Ctrl Pts',(-7.61710156474831,20.9566684038422,
85.370820445469));
#119220=CARTESIAN_POINT('Ctrl Pts',(-7.61408388714227,20.9521042062413,
85.3727457322644));
#119221=CARTESIAN_POINT('Ctrl Pts',(-7.60930270507376,20.944872731387,85.3757961398642));
#119222=CARTESIAN_POINT('Ctrl Pts',(-7.60452167614984,20.9376988048727,
85.3788083963661));
#119223=CARTESIAN_POINT('Ctrl Pts',(-7.59974145817027,20.9305824721789,
85.381782858467));
#119224=CARTESIAN_POINT('Ctrl Pts',(-7.59584281462332,20.9247785434349,
85.38420876614));
#119225=CARTESIAN_POINT('Ctrl Pts',(-7.5919447078127,20.919012910613,85.3866095361309));
#119226=CARTESIAN_POINT('Ctrl Pts',(-7.58804748868746,20.9132855737127,
85.3889853720183));
#119227=CARTESIAN_POINT('Ctrl Pts',(-7.58609887912484,20.9104219052625,
85.390173289962));
#119228=CARTESIAN_POINT('Ctrl Pts',(-7.58415049153295,20.9075678107926,
85.3913549744375));
#119229=CARTESIAN_POINT('Ctrl Pts',(-7.5822023694505,20.904723290303,85.3925304516039));
#119230=CARTESIAN_POINT('Ctrl Pts',(-7.58025424736805,20.9018787698134,
85.3937059287704));
#119231=CARTESIAN_POINT('Ctrl Pts',(-7.57893328365522,20.8999532776846,
85.3945008138175));
#119232=CARTESIAN_POINT('Ctrl Pts',(-7.57635884326463,20.8962184507747,
85.396038287666));
#119233=CARTESIAN_POINT('Ctrl Pts',(-7.54126018515817,20.8452996517695,
85.4169994523349));
#119234=CARTESIAN_POINT('Ctrl Pts',(-7.50558531703489,20.7965597621204,
85.436354179377));
#119235=CARTESIAN_POINT('Ctrl Pts',(-7.46947393676564,20.7499909550496,
85.4541206031617));
#119236=CARTESIAN_POINT('Ctrl Pts',(-7.43569965747034,20.7064360456351,
85.4707371975569));
#119237=CARTESIAN_POINT('Ctrl Pts',(-7.40154379163175,20.6647807397546,
85.4859642826928));
#119238=CARTESIAN_POINT('Ctrl Pts',(-7.36712038208436,20.6250355889639,
85.499811424579));
#119239=CARTESIAN_POINT('Ctrl Pts',(-7.35051750899141,20.6058659685424,
85.5064900872233));
#119240=CARTESIAN_POINT('Ctrl Pts',(-7.33385233478653,20.5871400356242,
85.5128482195878));
#119241=CARTESIAN_POINT('Ctrl Pts',(-7.31713719799185,20.5688555431679,
85.5188893576003));
#119242=CARTESIAN_POINT('Ctrl Pts',(-7.28333834177506,20.5318833700342,
85.5311048457282));
#119243=CARTESIAN_POINT('Ctrl Pts',(-7.24933600575288,20.4967193018425,
85.5420222251503));
#119244=CARTESIAN_POINT('Ctrl Pts',(-7.21523874947433,20.4633745956437,
85.5516581337858));
#119245=CARTESIAN_POINT('Ctrl Pts',(-7.19291786555609,20.4415463491046,
85.5579660312993));
#119246=CARTESIAN_POINT('Ctrl Pts',(-7.17055608797526,20.4204967554895,
85.5637254316562));
#119247=CARTESIAN_POINT('Ctrl Pts',(-7.14818109510134,20.4002191741198,
85.5689472100749));
#119248=CARTESIAN_POINT('Ctrl Pts',(-7.11825287463554,20.3730963978505,
85.5759317278631));
#119249=CARTESIAN_POINT('Ctrl Pts',(-7.08830176189899,20.3473563759075,
85.5819536290381));
#119250=CARTESIAN_POINT('Ctrl Pts',(-7.05840633710034,20.3230076680704,
85.5870306408997));
#119251=CARTESIAN_POINT('Ctrl Pts',(-7.01998447469757,20.2917144950011,
85.5935556611153));
#119252=CARTESIAN_POINT('Ctrl Pts',(-6.98168418706005,20.2627155071484,
85.5985165424507));
#119253=CARTESIAN_POINT('Ctrl Pts',(-6.94356148768183,20.2359899576851,
85.6019927183458));
#119254=CARTESIAN_POINT('Ctrl Pts',(-6.90863319582898,20.2115038167033,
85.6051776157476));
#119255=CARTESIAN_POINT('Ctrl Pts',(-6.87385512777084,20.1889265390783,
85.6071162886427));
#119256=CARTESIAN_POINT('Ctrl Pts',(-6.83932345299749,20.1682889367351,
85.6078564420343));
#119257=CARTESIAN_POINT('Ctrl Pts',(-6.80072505024667,20.1452208842216,
85.6086837618471));
#119258=CARTESIAN_POINT('Ctrl Pts',(-6.76243438098927,20.124575521933,85.6080140932172));
#119259=CARTESIAN_POINT('Ctrl Pts',(-6.72453642013718,20.1063527673125,
85.6059151707774));
#119260=CARTESIAN_POINT('Ctrl Pts',(-6.71391650835035,20.1012463171967,
85.6053270026898));
#119261=CARTESIAN_POINT('Ctrl Pts',(-6.70332717263078,20.0963299095061,
85.6046265848816));
#119262=CARTESIAN_POINT('Ctrl Pts',(-6.69276971843498,20.0916031601899,
85.6038153499371));
#119263=CARTESIAN_POINT('Ctrl Pts',(-6.65757504863047,20.0758459162232,
85.6011109909621));
#119264=CARTESIAN_POINT('Ctrl Pts',(-6.62273893243763,20.0621968271072,
85.5971767052845));
#119265=CARTESIAN_POINT('Ctrl Pts',(-6.58841052103251,20.0506322793736,
85.5921113489862));
#119266=CARTESIAN_POINT('Ctrl Pts',(-6.57444222050592,20.0459266413441,
85.5900502451904));
#119267=CARTESIAN_POINT('Ctrl Pts',(-6.56055738483732,20.0415660736729,
85.5878016471825));
#119268=CARTESIAN_POINT('Ctrl Pts',(-6.54676386035728,20.0375488864052,
85.5853713237095));
#119269=CARTESIAN_POINT('Origin',(-2.02513312664091,22.5,85.48888938658));
#119270=CARTESIAN_POINT('Origin',(-5.70733270705591,22.5,87.05138938658));
#119271=CARTESIAN_POINT('Origin',(-2.02513312664091,22.5,85.48888938658));
#119272=CARTESIAN_POINT('Ctrl Pts',(-1.86852584115091,-0.200657301970986,
95.96514097396));
#119273=CARTESIAN_POINT('Ctrl Pts',(-1.87679361636091,0.397260618019714,
95.95539499753));
#119274=CARTESIAN_POINT('Ctrl Pts',(-1.81764502158091,1.61545674784001,
96.02675082903));
#119275=CARTESIAN_POINT('Ctrl Pts',(-1.51056034305091,3.37210791261202,
96.3812545342701));
#119276=CARTESIAN_POINT('Ctrl Pts',(-1.03549752546091,4.99180633572701,
96.87949059878));
#119277=CARTESIAN_POINT('Ctrl Pts',(-0.47565565201091,6.40141962980201,
97.39996719591));
#119278=CARTESIAN_POINT('Ctrl Pts',(0.128959222729088,7.63825880799903,
97.89143667163));
#119279=CARTESIAN_POINT('Ctrl Pts',(0.78047764573909,8.77397550221601,98.34798763131));
#119280=CARTESIAN_POINT('Ctrl Pts',(1.50402784399909,9.87146117248002,98.77288024243));
#119281=CARTESIAN_POINT('Ctrl Pts',(2.31936621098909,10.95615772036,99.1532466824299));
#119282=CARTESIAN_POINT('Ctrl Pts',(3.21879357943909,12.01000937004,99.45696306809));
#119283=CARTESIAN_POINT('Ctrl Pts',(4.1912683517691,13.0170795927,99.65335362598));
#119284=CARTESIAN_POINT('Ctrl Pts',(5.2757469215191,14.01086777604,99.7165874722901));
#119285=CARTESIAN_POINT('Ctrl Pts',(6.5351502248891,15.02007613619,99.5796055175001));
#119286=CARTESIAN_POINT('Ctrl Pts',(7.73731890968909,15.84006914657,99.1892695249101));
#119287=CARTESIAN_POINT('Ctrl Pts',(8.5044225018091,16.29480837482,98.77493643233));
#119288=CARTESIAN_POINT('Ctrl Pts',(8.76798669870909,16.44357118509,98.6108142135001));
#119289=CARTESIAN_POINT('Ctrl Pts',(-2.76633335145391,-0.277061106735686,
89.62464525754));
#119290=CARTESIAN_POINT('Ctrl Pts',(-2.78010061236391,0.548141406161314,
89.61313564381));
#119291=CARTESIAN_POINT('Ctrl Pts',(-2.67974655644691,2.23539163023501,
89.69951614818));
#119292=CARTESIAN_POINT('Ctrl Pts',(-2.18690829439091,4.52753916756702,
90.11267233159));
#119293=CARTESIAN_POINT('Ctrl Pts',(-1.49193309304091,6.44657897676101,
90.65739218289));
#119294=CARTESIAN_POINT('Ctrl Pts',(-0.744560214060911,7.96637647141302,
91.1950322953901));
#119295=CARTESIAN_POINT('Ctrl Pts',(-0.000714101840911076,9.19387013708703,
91.67997579193));
#119296=CARTESIAN_POINT('Ctrl Pts',(0.743218764159092,10.2409288401,92.11363373692));
#119297=CARTESIAN_POINT('Ctrl Pts',(1.51015059767909,11.1834522333,92.50353807267));
#119298=CARTESIAN_POINT('Ctrl Pts',(2.30766423261909,12.04981733614,92.84138179648));
#119299=CARTESIAN_POINT('Ctrl Pts',(3.11198293474909,12.83069438562,93.10362209738));
#119300=CARTESIAN_POINT('Ctrl Pts',(3.89792431306909,13.52231896489,93.27156799052));
#119301=CARTESIAN_POINT('Ctrl Pts',(4.67814510883909,14.15587807635,93.33468615681));
#119302=CARTESIAN_POINT('Ctrl Pts',(5.4599957395091,14.75400852768,93.25754212455));
#119303=CARTESIAN_POINT('Ctrl Pts',(6.06740744298909,15.2155704877,93.02226348412));
#119304=CARTESIAN_POINT('Ctrl Pts',(6.38629556221909,15.47756556229,92.7840149103));
#119305=CARTESIAN_POINT('Ctrl Pts',(6.48862860801909,15.56565674012,92.69092482342));
#119306=CARTESIAN_POINT('Ctrl Pts',(-8.21314323670391,-0.382376649944286,
86.25787732271));
#119307=CARTESIAN_POINT('Ctrl Pts',(-8.23233050746892,0.756384491850314,
86.2455034223201));
#119308=CARTESIAN_POINT('Ctrl Pts',(-8.09201734092391,3.08654305365901,
86.33967991873));
#119309=CARTESIAN_POINT('Ctrl Pts',(-7.41007493507491,6.21008628532401,
86.78035394901));
#119310=CARTESIAN_POINT('Ctrl Pts',(-6.46595117430891,8.76366891642203,
87.33791220527));
#119311=CARTESIAN_POINT('Ctrl Pts',(-5.47046355413091,10.73360469488,87.86524851897));
#119312=CARTESIAN_POINT('Ctrl Pts',(-4.49835120662891,12.28405501304,88.3219438496));
#119313=CARTESIAN_POINT('Ctrl Pts',(-3.54419140703191,13.57328011442,88.71413997378));
#119314=CARTESIAN_POINT('Ctrl Pts',(-2.58024571757991,14.70275906295,89.05110200106));
#119315=CARTESIAN_POINT('Ctrl Pts',(-1.60151740187091,15.70963613843,89.32658646923));
#119316=CARTESIAN_POINT('Ctrl Pts',(-0.643241151590912,16.5857007526,89.52289696124));
#119317=CARTESIAN_POINT('Ctrl Pts',(0.258320540729089,17.33121239699,89.6296159923701));
#119318=CARTESIAN_POINT('Ctrl Pts',(1.10917349098909,17.98470665617,89.644481026));
#119319=CARTESIAN_POINT('Ctrl Pts',(1.89817703664909,18.57234274478,89.5498507959201));
#119320=CARTESIAN_POINT('Ctrl Pts',(2.42972632590909,19.00878869518,89.36136454575));
#119321=CARTESIAN_POINT('Ctrl Pts',(2.66092298708909,19.26095009207,89.20319983242));
#119322=CARTESIAN_POINT('Ctrl Pts',(2.72918498241909,19.3474423808,89.14448415142));
#119323=CARTESIAN_POINT('Ctrl Pts',(-14.2862958551049,-0.440758245828086,
88.2895013269199));
#119324=CARTESIAN_POINT('Ctrl Pts',(-14.3069203009679,0.872018283434913,
88.2777849287));
#119325=CARTESIAN_POINT('Ctrl Pts',(-14.1566719512549,3.55593252096201,
88.36691425296));
#119326=CARTESIAN_POINT('Ctrl Pts',(-13.4184630337948,7.20801986586801,
88.78415381662));
#119327=CARTESIAN_POINT('Ctrl Pts',(-12.3753852541951,10.27436448968,89.3116591898701));
#119328=CARTESIAN_POINT('Ctrl Pts',(-11.2498853426949,12.71021402121,89.8086449352));
#119329=CARTESIAN_POINT('Ctrl Pts',(-10.1248635377679,14.68333765206,90.23571355337));
#119330=CARTESIAN_POINT('Ctrl Pts',(-8.99406462449291,16.37115120725,90.59773884278));
#119331=CARTESIAN_POINT('Ctrl Pts',(-7.82135743268891,17.89486271208,90.90193228787));
#119332=CARTESIAN_POINT('Ctrl Pts',(-6.59288141698792,19.29990188201,91.1401305760401));
#119333=CARTESIAN_POINT('Ctrl Pts',(-5.34245787553691,20.5707644631,91.2935385755));
#119334=CARTESIAN_POINT('Ctrl Pts',(-4.10638909157991,21.70068773103,91.3503426401699));
#119335=CARTESIAN_POINT('Ctrl Pts',(-2.86088161342491,22.73992455031,91.30356781784));
#119336=CARTESIAN_POINT('Ctrl Pts',(-1.58517092003091,23.72520760639,91.1267204027899));
#119337=CARTESIAN_POINT('Ctrl Pts',(-0.555955217310912,24.48794052554,90.8430628426899));
#119338=CARTESIAN_POINT('Ctrl Pts',(0.0112272501190876,24.92026069551,90.6113068883499));
#119339=CARTESIAN_POINT('Ctrl Pts',(0.19711543522909,25.06537831943,90.52555227838));
#119340=CARTESIAN_POINT('Ctrl Pts',(-1.00773525083376,22.4999925247862,
90.8939704740664));
#119341=CARTESIAN_POINT('Ctrl Pts',(-0.913881385337355,22.6929489369076,
90.8763043702935));
#119342=CARTESIAN_POINT('Ctrl Pts',(-0.821284198747461,22.877174794995,
90.856339427234));
#119343=CARTESIAN_POINT('Ctrl Pts',(-0.730256985160353,23.0529605945689,
90.8342888831775));
#119344=CARTESIAN_POINT('Ctrl Pts',(-0.637872403585209,23.2313676543977,
90.8119095286318));
#119345=CARTESIAN_POINT('Ctrl Pts',(-0.547105332201889,23.4010810682236,
90.7873821522087));
#119346=CARTESIAN_POINT('Ctrl Pts',(-0.458254687202534,23.5624045216343,
90.7609754970322));
#119347=CARTESIAN_POINT('Ctrl Pts',(-0.36847061103016,23.7254227780524,
90.7342914235531));
#119348=CARTESIAN_POINT('Ctrl Pts',(-0.280643724697561,23.8798738645884,
90.7056887345579));
#119349=CARTESIAN_POINT('Ctrl Pts',(-0.195048516452712,24.0260711389505,
90.6754865677338));
#119350=CARTESIAN_POINT('Ctrl Pts',(-0.107589728737015,24.1754514213897,
90.6446268391229));
#119351=CARTESIAN_POINT('Ctrl Pts',(-0.0224611347238633,24.3162145750682,
90.6120976040466));
#119352=CARTESIAN_POINT('Ctrl Pts',(0.0600841858518275,24.4486948738206,
90.5782772436489));
#119353=CARTESIAN_POINT('Ctrl Pts',(0.112701886340464,24.5331431336587,
90.5567187884704));
#119354=CARTESIAN_POINT('Ctrl Pts',(0.164270749100463,24.6142258216448,
90.5346364601734));
#119355=CARTESIAN_POINT('Ctrl Pts',(0.214734006960575,24.6920295183809,
90.5121348736941));
#119356=CARTESIAN_POINT('Origin',(-10.9843331791359,-92.5,65.395787724084));
#119357=CARTESIAN_POINT('',(0.214666888280743,89.,90.5121648014016));
#119358=CARTESIAN_POINT('Origin',(-2.02513312664091,89.,85.48888938658));
#119359=CARTESIAN_POINT('',(-7.08815755064843,89.,87.6373268843701));
#119360=CARTESIAN_POINT('Origin',(-2.02513312664091,89.,85.48888938658));
#119361=CARTESIAN_POINT('',(-5.70733025617244,90.4999999999959,87.051388346575));
#119362=CARTESIAN_POINT('Origin',(-5.70733270705591,89.,87.05138938658));
#119363=CARTESIAN_POINT('Origin',(-2.02513312664091,90.49999999999,85.48888938658));
#119364=CARTESIAN_POINT('Origin',(-2.27593483123091,90.5,69.192338555332));
#119365=CARTESIAN_POINT('',(-5.7073302546465,90.4999999999959,58.9263904272322));
#119366=CARTESIAN_POINT('Origin',(27.4324635166691,90.5,72.98888938658));
#119367=CARTESIAN_POINT('Origin',(-2.02513312664091,90.49999999999,60.48888938658));
#119368=CARTESIAN_POINT('Origin',(-2.02513312664091,89.,60.48888938658));
#119369=CARTESIAN_POINT('',(-7.08815755380101,89.,58.3404518962193));
#119370=CARTESIAN_POINT('Origin',(-5.70733270705591,89.,58.92638938658));
#119371=CARTESIAN_POINT('Origin',(-2.02513312664091,89.,60.48888938658));
#119372=CARTESIAN_POINT('Origin',(-10.9843331791359,-92.5,80.581991049076));
#119373=CARTESIAN_POINT('',(0.214770984780106,21.31105212978,55.4656603870195));
#119374=CARTESIAN_POINT('Ctrl Pts',(5.21275554925909,16.84790218393,55.1007357528));
#119375=CARTESIAN_POINT('Ctrl Pts',(5.08987221057909,16.79738018542,55.08711855268));
#119376=CARTESIAN_POINT('Ctrl Pts',(4.53992236271909,16.56567500218,55.02943324933));
#119377=CARTESIAN_POINT('Ctrl Pts',(3.59664713182909,16.12384541239,54.9543844059));
#119378=CARTESIAN_POINT('Ctrl Pts',(2.42419774846909,15.48152670993,54.8998706626));
#119379=CARTESIAN_POINT('Ctrl Pts',(1.37116655289909,14.81743214788,54.87937490558));
#119380=CARTESIAN_POINT('Ctrl Pts',(0.421859436239088,14.13775868448,54.88216912445));
#119381=CARTESIAN_POINT('Ctrl Pts',(-0.446505860180913,13.43742265295,54.90142155045));
#119382=CARTESIAN_POINT('Ctrl Pts',(-1.26178821829091,12.69950859659,54.93347110475));
#119383=CARTESIAN_POINT('Ctrl Pts',(-1.81779397457091,12.13439310831,54.96399549816));
#119384=CARTESIAN_POINT('Ctrl Pts',(-2.10763051195091,11.81847011659,54.9822761899501));
#119385=CARTESIAN_POINT('Ctrl Pts',(-2.14449596917091,11.77792717693,54.9846401213));
#119386=CARTESIAN_POINT('Ctrl Pts',(3.41542118564909,18.16535552692,56.05233703107));
#119387=CARTESIAN_POINT('Ctrl Pts',(3.29153510574909,18.12260617231,56.02604874878));
#119388=CARTESIAN_POINT('Ctrl Pts',(2.73528597745909,17.92273095754,55.9107434192));
#119389=CARTESIAN_POINT('Ctrl Pts',(1.76818306694909,17.51347174676,55.73169222743));
#119390=CARTESIAN_POINT('Ctrl Pts',(0.548997708799087,16.87566838021,55.5460284887601));
#119391=CARTESIAN_POINT('Ctrl Pts',(-0.557108605230912,16.18769292699,55.40933909873));
#119392=CARTESIAN_POINT('Ctrl Pts',(-1.55941549777091,15.46717855553,55.3104586032101));
#119393=CARTESIAN_POINT('Ctrl Pts',(-2.48080341267091,14.7114503467,55.23984281602));
#119394=CARTESIAN_POINT('Ctrl Pts',(-3.34714675340591,13.90828499752,55.1905881852));
#119395=CARTESIAN_POINT('Ctrl Pts',(-3.93855870358191,13.28946121546,55.16788012438));
#119396=CARTESIAN_POINT('Ctrl Pts',(-4.24409608839291,12.94795249993,55.15906941751));
#119397=CARTESIAN_POINT('Ctrl Pts',(-4.28290610423791,12.90420804222,55.1579968414401));
#119398=CARTESIAN_POINT('Ctrl Pts',(1.65053628828909,19.82150258154,56.17061479967));
#119399=CARTESIAN_POINT('Ctrl Pts',(1.52396188714909,19.77706403619,56.12774489951));
#119400=CARTESIAN_POINT('Ctrl Pts',(0.954443363319088,19.56713881503,55.93839722755));
#119401=CARTESIAN_POINT('Ctrl Pts',(-0.0439950975309107,19.12236569434,
55.63472119012));
#119402=CARTESIAN_POINT('Ctrl Pts',(-1.31089293764091,18.41257410019,55.30270839141));
#119403=CARTESIAN_POINT('Ctrl Pts',(-2.46454089411091,17.63895669212,55.04252121858));
#119404=CARTESIAN_POINT('Ctrl Pts',(-3.50973548507091,16.82817478502,54.83934772625));
#119405=CARTESIAN_POINT('Ctrl Pts',(-4.47093084477291,15.97725182874,54.67900864002));
#119406=CARTESIAN_POINT('Ctrl Pts',(-5.37247266060192,15.07666324399,54.55030739518));
#119407=CARTESIAN_POINT('Ctrl Pts',(-5.98639287753791,14.38579398253,54.47647799956));
#119408=CARTESIAN_POINT('Ctrl Pts',(-6.30055887152191,14.01004943148,54.4418538746401));
#119409=CARTESIAN_POINT('Ctrl Pts',(-6.34040880614791,13.96201778839,54.43751017046));
#119410=CARTESIAN_POINT('Ctrl Pts',(0.161630205399088,21.58781829589,55.43924838639));
#119411=CARTESIAN_POINT('Ctrl Pts',(0.0310528536290871,21.53246180977,55.37817436325));
#119412=CARTESIAN_POINT('Ctrl Pts',(-0.556874190470912,21.27199336722,55.1085788369));
#119413=CARTESIAN_POINT('Ctrl Pts',(-1.58983220620091,20.72852246885,54.67685193629));
#119414=CARTESIAN_POINT('Ctrl Pts',(-2.89883538253791,19.88017244876,54.20348512935));
#119415=CARTESIAN_POINT('Ctrl Pts',(-4.08793142591791,18.97096941006,53.82953698486));
#119416=CARTESIAN_POINT('Ctrl Pts',(-5.15998373732991,18.03294899289,53.53384318326));
#119417=CARTESIAN_POINT('Ctrl Pts',(-6.14227849942291,17.06016425825,53.29630626823));
#119418=CARTESIAN_POINT('Ctrl Pts',(-7.05829938720391,16.04342353451,53.1009784983001));
#119419=CARTESIAN_POINT('Ctrl Pts',(-7.67872411882791,15.27211287311,52.98519291411));
#119420=CARTESIAN_POINT('Ctrl Pts',(-7.99325585674391,14.85820643969,52.92959524119));
#119421=CARTESIAN_POINT('Ctrl Pts',(-8.03309757611691,14.80539351529,52.92259715796));
#119422=CARTESIAN_POINT('Ctrl Pts',(0.214764603391513,21.3110521291418,
55.4656747003203));
#119423=CARTESIAN_POINT('Ctrl Pts',(0.180854938597129,21.2147111573871,
55.4505468232702));
#119424=CARTESIAN_POINT('Ctrl Pts',(0.147018940254829,21.1178106894989,
55.4358631290332));
#119425=CARTESIAN_POINT('Ctrl Pts',(0.113269006376136,21.0203699849487,
55.4216182940488));
#119426=CARTESIAN_POINT('Ctrl Pts',(0.0414294124360488,20.8129591890258,
55.3912969557997));
#119427=CARTESIAN_POINT('Ctrl Pts',(-0.0300191465661176,20.6031023493503,
55.3629607110215));
#119428=CARTESIAN_POINT('Ctrl Pts',(-0.10098994563944,20.3909832464082,
55.3364624582132));
#119429=CARTESIAN_POINT('Ctrl Pts',(-0.175487023028061,20.1683247243989,
55.3086476045564));
#119430=CARTESIAN_POINT('Ctrl Pts',(-0.249457389675094,19.9431739149331,
55.2828585215437));
#119431=CARTESIAN_POINT('Ctrl Pts',(-0.322817933803376,19.7157137436041,
55.2589715907221));
#119432=CARTESIAN_POINT('Ctrl Pts',(-0.350917171761308,19.6285898331142,
55.2498221963001));
#119433=CARTESIAN_POINT('Ctrl Pts',(-0.378927138419568,19.5411267856233,
55.240952285874));
#119434=CARTESIAN_POINT('Ctrl Pts',(-0.406843922230958,19.4533336453778,
55.2323562594312));
#119435=CARTESIAN_POINT('Ctrl Pts',(-0.473595533320854,19.2434121302915,
55.2118023654759));
#119436=CARTESIAN_POINT('Ctrl Pts',(-0.539816199718292,19.0316029376036,
55.1928122593711));
#119437=CARTESIAN_POINT('Ctrl Pts',(-0.605437038356976,18.8179768810558,
55.1752806605715));
#119438=CARTESIAN_POINT('Ctrl Pts',(-0.689037512667965,18.5458188284756,
55.1529455303677));
#119439=CARTESIAN_POINT('Ctrl Pts',(-0.77166554544613,18.2707117621105,
55.1329772781823));
#119440=CARTESIAN_POINT('Ctrl Pts',(-0.853135974721628,17.9928053600222,
55.115210672658));
#119441=CARTESIAN_POINT('Ctrl Pts',(-0.917278510361073,17.7740066933293,
55.1012228351301));
#119442=CARTESIAN_POINT('Ctrl Pts',(-0.980699436725039,17.5534772495342,
55.0886003290476));
#119443=CARTESIAN_POINT('Ctrl Pts',(-1.04330728897502,17.331346469236,55.0772416027675));
#119444=CARTESIAN_POINT('Ctrl Pts',(-1.10591514122499,17.1092156889378,
55.0658828764875));
#119445=CARTESIAN_POINT('Ctrl Pts',(-1.16770970176269,16.8854836897017,
55.0557884827401));
#119446=CARTESIAN_POINT('Ctrl Pts',(-1.22862268601253,16.6602282693306,
55.0468703568845));
#119447=CARTESIAN_POINT('Ctrl Pts',(-1.24405012706333,16.603177793772,55.0446116617538));
#119448=CARTESIAN_POINT('Ctrl Pts',(-1.25942117156684,16.5460293014174,
55.0424284610014));
#119449=CARTESIAN_POINT('Ctrl Pts',(-1.27473433959933,16.4887822934079,
55.0403191528466));
#119450=CARTESIAN_POINT('Ctrl Pts',(-1.28995091842717,16.4318963761251,
55.0382231493454));
#119451=CARTESIAN_POINT('Ctrl Pts',(-1.30511034814177,16.3749131821594,
55.0362001097604));
#119452=CARTESIAN_POINT('Ctrl Pts',(-1.32021095540953,16.317832398685,55.0342485000666));
#119453=CARTESIAN_POINT('Ctrl Pts',(-1.32776125904341,16.2892920069477,
55.0332726952197));
#119454=CARTESIAN_POINT('Ctrl Pts',(-1.3352968570784,16.2607272178333,55.0323147479457));
#119455=CARTESIAN_POINT('Ctrl Pts',(-1.34281751604111,16.2321380119861,
55.0313744699216));
#119456=CARTESIAN_POINT('Ctrl Pts',(-1.34657784552247,16.2178434090626,
55.0309043309095));
#119457=CARTESIAN_POINT('Ctrl Pts',(-1.35033444023579,16.2035427019558,
55.0304386092098));
#119458=CARTESIAN_POINT('Ctrl Pts',(-1.35408727034747,16.1892358887999,
55.0299772813598));
#119459=CARTESIAN_POINT('Ctrl Pts',(-1.35596368540331,16.1820824822219,
55.0297466174348));
#119460=CARTESIAN_POINT('Ctrl Pts',(-1.35783915930872,16.1749275491317,
55.0295170519722));
#119461=CARTESIAN_POINT('Ctrl Pts',(-1.35971368824907,16.1677710893663,
55.0292885820492));
#119462=CARTESIAN_POINT('Ctrl Pts',(-1.36158821718942,16.1606146296009,
55.0290601121261));
#119463=CARTESIAN_POINT('Ctrl Pts',(-1.36390932142334,16.1517456707088,
55.0287786611796));
#119464=CARTESIAN_POINT('Ctrl Pts',(-1.36533443633472,16.146297129903,55.0286064559783));
#119465=CARTESIAN_POINT('Ctrl Pts',(-1.42768981805868,15.9078982197032,
55.0210716803769));
#119466=CARTESIAN_POINT('Ctrl Pts',(-1.4884755321976,15.6700343355104,55.0148090280403));
#119467=CARTESIAN_POINT('Ctrl Pts',(-1.54768204110244,15.4328191754794,
55.0096521710442));
#119468=CARTESIAN_POINT('Ctrl Pts',(-1.59598853326158,15.2392757208825,
55.0054446999966));
#119469=CARTESIAN_POINT('Ctrl Pts',(-1.64323935791373,15.0461703467149,
55.0019734168841));
#119470=CARTESIAN_POINT('Ctrl Pts',(-1.68944051522512,14.8535968995406,
54.9991481034072));
#119471=CARTESIAN_POINT('Ctrl Pts',(-1.7356416725365,14.6610234523662,54.9963227899303));
#119472=CARTESIAN_POINT('Ctrl Pts',(-1.78079333866968,14.4689815333594,
54.9941437027382));
#119473=CARTESIAN_POINT('Ctrl Pts',(-1.82492463553365,14.2775166933926,
54.9925345386017));
#119474=CARTESIAN_POINT('Ctrl Pts',(-1.84080564612811,14.2086164940318,
54.9919554676358));
#119475=CARTESIAN_POINT('Ctrl Pts',(-1.85655476412944,14.1397905502665,
54.9914503172646));
#119476=CARTESIAN_POINT('Ctrl Pts',(-1.87217181097862,14.0710412448739,
54.9910155527655));
#119477=CARTESIAN_POINT('Ctrl Pts',(-1.94160339402295,13.7653897889553,
54.9890826401148));
#119478=CARTESIAN_POINT('Ctrl Pts',(-2.00842718663851,13.4612560904928,
54.9885384899925));
#119479=CARTESIAN_POINT('Ctrl Pts',(-2.07260302534106,13.1588273555174,
54.9890942440626));
#119480=CARTESIAN_POINT('Ctrl Pts',(-2.09829868771968,13.0377365084847,
54.9893167650181));
#119481=CARTESIAN_POINT('Ctrl Pts',(-2.12356740923878,12.9169225119993,
54.9897158412855));
#119482=CARTESIAN_POINT('Ctrl Pts',(-2.14841466004433,12.7963954402831,
54.9902741273346));
#119483=CARTESIAN_POINT('Ctrl Pts',(-2.17450028860511,12.6698613440601,
54.9908602381531));
#119484=CARTESIAN_POINT('Ctrl Pts',(-2.2001213545838,12.5436435262945,54.9916218281353));
#119485=CARTESIAN_POINT('Ctrl Pts',(-2.2253115642739,12.417699967537,54.9925407754541));
#119486=CARTESIAN_POINT('Ctrl Pts',(-2.25050177396401,12.2917564087794,
54.9934597227729));
#119487=CARTESIAN_POINT('Ctrl Pts',(-2.27526132344878,12.1660867047988,
54.9945360459858));
#119488=CARTESIAN_POINT('Ctrl Pts',(-2.29964905129997,12.0405998990293,
54.995753327958));
#119489=CARTESIAN_POINT('Origin',(1.07038457110909,25.,122.41156512159));
#119490=CARTESIAN_POINT('',(-2.29973550185091,10.,54.99574879712));
#119491=CARTESIAN_POINT('Origin',(-2.02513312664091,10.,60.48888938658));
#119492=CARTESIAN_POINT('Origin',(-5.70733270705591,10.,58.92638938658));
#119493=CARTESIAN_POINT('Origin',(-2.02513312664091,10.,60.48888938658));
#119494=CARTESIAN_POINT('Origin',(27.4324635166691,10.,72.98888938658));
#119495=CARTESIAN_POINT('Origin',(-6.80729512863291,91.08441266238,84.10819367738));
#119496=CARTESIAN_POINT('Origin',(27.4324635166691,22.5,72.98888938658));
#119497=CARTESIAN_POINT('Origin',(-2.02513312664091,-92.5,85.48888938658));
#119498=CARTESIAN_POINT('',(-7.08838232372406,85.1740126527982,87.6374222456928));
#119499=CARTESIAN_POINT('Ctrl Pts',(-7.0883818064374,64.8259873343748,87.637422020082));
#119500=CARTESIAN_POINT('Ctrl Pts',(-7.06379466657136,65.03820054502,87.6953798859809));
#119501=CARTESIAN_POINT('Ctrl Pts',(-7.03897737033209,65.2515735354143,
87.7510159589579));
#119502=CARTESIAN_POINT('Ctrl Pts',(-7.01415562444538,65.4660641629207,
87.8044130368114));
#119503=CARTESIAN_POINT('Ctrl Pts',(-6.98858405264758,65.6870342149981,
87.8594231564201));
#119504=CARTESIAN_POINT('Ctrl Pts',(-6.96300721566767,65.9091904325734,
87.9120570715152));
#119505=CARTESIAN_POINT('Ctrl Pts',(-6.93763343777821,66.1325240456197,
87.9623874104707));
#119506=CARTESIAN_POINT('Ctrl Pts',(-6.91119723122836,66.3652088885995,
88.0148251374087));
#119507=CARTESIAN_POINT('Ctrl Pts',(-6.88498087704221,66.5991717001637,
88.064762513918));
#119508=CARTESIAN_POINT('Ctrl Pts',(-6.85918743756997,66.8344433770868,
88.1122603178858));
#119509=CARTESIAN_POINT('Ctrl Pts',(-6.85102495572795,66.9088964484926,
88.1272912703434));
#119510=CARTESIAN_POINT('Ctrl Pts',(-6.84290462584899,66.9834808964798,
88.1420777481535));
#119511=CARTESIAN_POINT('Ctrl Pts',(-6.83483238691541,67.0581985226156,
88.1566212148313));
#119512=CARTESIAN_POINT('Ctrl Pts',(-6.82950733941523,67.107487810451,88.1662151641078));
#119513=CARTESIAN_POINT('Ctrl Pts',(-6.82420321472302,67.1568350591063,
88.175703359103));
#119514=CARTESIAN_POINT('Ctrl Pts',(-6.81892161009561,67.2062392427801,
88.1850867777694));
#119515=CARTESIAN_POINT('Ctrl Pts',(-6.79460045638261,67.4337395632247,
88.2282962915135));
#119516=CARTESIAN_POINT('Ctrl Pts',(-6.77075805880709,67.6624482893294,
88.2692850297369));
#119517=CARTESIAN_POINT('Ctrl Pts',(-6.74754274177323,67.8923491571023,
88.3081363926079));
#119518=CARTESIAN_POINT('Ctrl Pts',(-6.72950180658429,68.0710082143671,
88.3383283093729));
#119519=CARTESIAN_POINT('Ctrl Pts',(-6.7118393390258,68.2503882255433,88.3672287815631));
#119520=CARTESIAN_POINT('Ctrl Pts',(-6.6946249460294,68.4304987288456,88.3948638281204));
#119521=CARTESIAN_POINT('Ctrl Pts',(-6.67494189379613,68.6364382844837,
88.4264619254201));
#119522=CARTESIAN_POINT('Ctrl Pts',(-6.65584162687453,68.8433259942116,
88.4564106873118));
#119523=CARTESIAN_POINT('Ctrl Pts',(-6.63741314843917,69.0511618587221,
88.4847590086765));
#119524=CARTESIAN_POINT('Ctrl Pts',(-6.62819890922149,69.1550797909774,
88.4989331693589));
#119525=CARTESIAN_POINT('Ctrl Pts',(-6.61915252166941,69.25923476194,88.5127071591024));
#119526=CARTESIAN_POINT('Ctrl Pts',(-6.61028438410816,69.3636267717451,
88.5260871339677));
#119527=CARTESIAN_POINT('Ctrl Pts',(-6.60585031532754,69.4158227766476,
88.5327771214003));
#119528=CARTESIAN_POINT('Ctrl Pts',(-6.60146080436318,69.4680780412606,
88.53936860247));
#119529=CARTESIAN_POINT('Ctrl Pts',(-6.59711712217367,69.5203925655962,
88.5458623381286));
#119530=CARTESIAN_POINT('Ctrl Pts',(-6.59494528107892,69.546549827764,88.5491092059579));
#119531=CARTESIAN_POINT('Ctrl Pts',(-6.5927848969414,69.5727219048623,88.5523316373004));
#119532=CARTESIAN_POINT('Ctrl Pts',(-6.5906361265566,69.5989087968919,88.555529727633));
#119533=CARTESIAN_POINT('Ctrl Pts',(-6.58848735617179,69.6250956889215,
88.5587278179656));
#119534=CARTESIAN_POINT('Ctrl Pts',(-6.58644313922851,69.6501509912735,
88.5617638446549));
#119535=CARTESIAN_POINT('Ctrl Pts',(-6.58422481242837,69.6775139177743,
88.5650510709359));
#119536=CARTESIAN_POINT('Ctrl Pts',(-6.56410003276806,69.9257518539767,
88.5948729639929));
#119537=CARTESIAN_POINT('Ctrl Pts',(-6.54513276355699,70.1744087231534,
88.6223706242821));
#119538=CARTESIAN_POINT('Ctrl Pts',(-6.52746288468714,70.4235233797567,
88.6476244002884));
#119539=CARTESIAN_POINT('Ctrl Pts',(-6.51570354940074,70.5893096193416,
88.6644308323808));
#119540=CARTESIAN_POINT('Ctrl Pts',(-6.50451897291542,70.7552995617695,
88.6802428581044));
#119541=CARTESIAN_POINT('Ctrl Pts',(-6.49395412391555,70.9215145754299,
88.6950770967392));
#119542=CARTESIAN_POINT('Ctrl Pts',(-6.47849417436243,71.1647433926325,
88.7167846082195));
#119543=CARTESIAN_POINT('Ctrl Pts',(-6.46435935369875,71.4084526956892,
88.7363996338555));
#119544=CARTESIAN_POINT('Ctrl Pts',(-6.45152719394054,71.6525968740843,
88.7540050221084));
#119545=CARTESIAN_POINT('Ctrl Pts',(-6.43849859227522,71.9004785486544,
88.7718799235304));
#119546=CARTESIAN_POINT('Ctrl Pts',(-6.42681257394867,72.1488090208903,
88.7876831470584));
#119547=CARTESIAN_POINT('Ctrl Pts',(-6.41648044535944,72.397570219193,88.801473345101));
#119548=CARTESIAN_POINT('Ctrl Pts',(-6.40604941678005,72.6487125802786,
88.8153955440609));
#119549=CARTESIAN_POINT('Ctrl Pts',(-6.39699804956997,72.9002945114833,
88.8272659517491));
#119550=CARTESIAN_POINT('Ctrl Pts',(-6.38937723579345,73.1523192932256,
88.8371172189261));
#119551=CARTESIAN_POINT('Ctrl Pts',(-6.38177776433586,73.4036382719624,
88.8469408973322));
#119552=CARTESIAN_POINT('Ctrl Pts',(-6.37560062815082,73.6553982145796,
88.8547566569079));
#119553=CARTESIAN_POINT('Ctrl Pts',(-6.37093868730099,73.9076153300843,
88.8605704111973));
#119554=CARTESIAN_POINT('Ctrl Pts',(-6.36634677417501,74.1560438538663,
88.8662968361977));
#119555=CARTESIAN_POINT('Ctrl Pts',(-6.36322473582904,74.4049164792301,
88.8700808561546));
#119556=CARTESIAN_POINT('Ctrl Pts',(-6.36170502115568,74.6542527439161,
88.8719037070657));
#119557=CARTESIAN_POINT('Ctrl Pts',(-6.36100385159357,74.7692921013646,
88.8727447383446));
#119558=CARTESIAN_POINT('Ctrl Pts',(-6.36064440344129,74.8844301613427,
88.8731679528114));
#119559=CARTESIAN_POINT('Ctrl Pts',(-6.36064303502608,74.9996686417215,
88.8731697877771));
#119560=CARTESIAN_POINT('Ctrl Pts',(-6.36064303474299,74.9996924816059,
88.8731697881567));
#119561=CARTESIAN_POINT('Ctrl Pts',(-6.3606430344747,74.9997163214862,88.8731697885189));
#119562=CARTESIAN_POINT('Ctrl Pts',(-6.36064303422121,74.9997401613624,
88.8731697888638));
#119563=CARTESIAN_POINT('Ctrl Pts',(-6.36064037275879,75.2500455466579,
88.8731734100344));
#119564=CARTESIAN_POINT('Ctrl Pts',(-6.36226542360875,75.4998974699238,
88.8712654838432));
#119565=CARTESIAN_POINT('Ctrl Pts',(-6.3654009159308,75.7493144063505,88.86742892387));
#119566=CARTESIAN_POINT('Ctrl Pts',(-6.36856862205069,76.0012938324725,
88.8635529473859));
#119567=CARTESIAN_POINT('Ctrl Pts',(-6.37327830216265,76.2528298495998,
88.8577085595702));
#119568=CARTESIAN_POINT('Ctrl Pts',(-6.37945537706228,76.503929709642,88.8498538555591));
#119569=CARTESIAN_POINT('Ctrl Pts',(-6.38565350919478,76.7558855522182,
88.8419723753902));
#119570=CARTESIAN_POINT('Ctrl Pts',(-6.39332941744835,77.0074028106557,
88.8320668995079));
#119571=CARTESIAN_POINT('Ctrl Pts',(-6.40244884291788,77.258468608758,88.8200700124218));
#119572=CARTESIAN_POINT('Ctrl Pts',(-6.40753815588165,77.3985818675713,
88.8133748633496));
#119573=CARTESIAN_POINT('Ctrl Pts',(-6.41307774881445,77.5385541127024,
88.8060279003157));
#119574=CARTESIAN_POINT('Ctrl Pts',(-6.41906658906012,77.6783794171587,
88.7980139264912));
#119575=CARTESIAN_POINT('Ctrl Pts',(-6.42961407071633,77.9246382541503,
88.7838998011448));
#119576=CARTESIAN_POINT('Ctrl Pts',(-6.44153211992909,78.170458717253,88.7677456921256));
#119577=CARTESIAN_POINT('Ctrl Pts',(-6.45477301806723,78.4158477603694,
88.7495427829172));
#119578=CARTESIAN_POINT('Ctrl Pts',(-6.46538522170445,78.6125201060613,
88.7349536683953));
#119579=CARTESIAN_POINT('Ctrl Pts',(-6.47684792880327,78.8089152817468,
88.7190479852231));
#119580=CARTESIAN_POINT('Ctrl Pts',(-6.48915462984713,79.0050284462474,
88.7018073908017));
#119581=CARTESIAN_POINT('Ctrl Pts',(-6.49071151880142,79.0298382160235,
88.6996263277431));
#119582=CARTESIAN_POINT('Ctrl Pts',(-6.49228179757586,79.0546436053862,
88.6974240762827));
#119583=CARTESIAN_POINT('Ctrl Pts',(-6.49386552851074,79.0794444862278,
88.6952005063406));
#119584=CARTESIAN_POINT('Ctrl Pts',(-6.50635116928276,79.2749668961259,
88.6776705743827));
#119585=CARTESIAN_POINT('Ctrl Pts',(-6.51967251742695,79.4702103739657,
88.658816297229));
#119586=CARTESIAN_POINT('Ctrl Pts',(-6.53376695262603,79.6651764666531,
88.6385971265922));
#119587=CARTESIAN_POINT('Ctrl Pts',(-6.54170806880242,79.7750246706158,
88.6272051991578));
#119588=CARTESIAN_POINT('Ctrl Pts',(-6.54989472187858,79.8847846386297,
88.6153797943906));
#119589=CARTESIAN_POINT('Ctrl Pts',(-6.55831553553021,79.9944563692783,
88.6031135000803));
#119590=CARTESIAN_POINT('Ctrl Pts',(-6.56252594235602,80.0492922346025,
88.5969803529252));
#119591=CARTESIAN_POINT('Ctrl Pts',(-6.56679488603044,80.1041060406106,
88.5907369818051));
#119592=CARTESIAN_POINT('Ctrl Pts',(-6.57112091400058,80.1588977872398,
88.584382459583));
#119593=CARTESIAN_POINT('Ctrl Pts',(-6.57328392798565,80.1862936605544,
88.5812051984719));
#119594=CARTESIAN_POINT('Ctrl Pts',(-6.57546121277668,80.2136840190252,
88.5780001494511));
#119595=CARTESIAN_POINT('Ctrl Pts',(-6.57765258443277,80.2410688626487,
88.5747671967393));
#119596=CARTESIAN_POINT('Ctrl Pts',(-6.57984395608886,80.2684537062723,
88.5715342440275));
#119597=CARTESIAN_POINT('Ctrl Pts',(-6.58214377145534,80.2969968411338,
88.5681335599459));
#119598=CARTESIAN_POINT('Ctrl Pts',(-6.584268774623,80.3232068489765,88.5649845114387));
#119599=CARTESIAN_POINT('Ctrl Pts',(-6.60448466570381,80.5725517308274,
88.5350265223882));
#119600=CARTESIAN_POINT('Ctrl Pts',(-6.62580884323505,80.8205332639971,
88.5028111501408));
#119601=CARTESIAN_POINT('Ctrl Pts',(-6.64805940844237,81.0671975548834,
88.4683166923041));
#119602=CARTESIAN_POINT('Ctrl Pts',(-6.66995048632655,81.3098766577614,
88.4343795380772));
#119603=CARTESIAN_POINT('Ctrl Pts',(-6.69273887743609,81.5512810694582,
88.3982363328307));
#119604=CARTESIAN_POINT('Ctrl Pts',(-6.7162618961127,81.7914169235885,88.3598360359073));
#119605=CARTESIAN_POINT('Ctrl Pts',(-6.73899066478621,82.023444638814,88.3227323173004));
#119606=CARTESIAN_POINT('Ctrl Pts',(-6.76240583176186,82.2542881886803,
88.2835212815749));
#119607=CARTESIAN_POINT('Ctrl Pts',(-6.78636214031899,82.4839140899401,
88.2421290564647));
#119608=CARTESIAN_POINT('Ctrl Pts',(-6.80235074803454,82.6371680208544,
88.2145035962156));
#119609=CARTESIAN_POINT('Ctrl Pts',(-6.81858041995665,82.7898787767762,
88.1859060023952));
#119610=CARTESIAN_POINT('Ctrl Pts',(-6.83500657856313,82.9420255751848,
88.1563072065959));
#119611=CARTESIAN_POINT('Ctrl Pts',(-6.85992974853696,83.1728756849734,
88.1113973870575));
#119612=CARTESIAN_POINT('Ctrl Pts',(-6.88530658635467,83.4024289215281,
88.0641834221432));
#119613=CARTESIAN_POINT('Ctrl Pts',(-6.91096134814823,83.6307464515349,
88.014605662357));
#119614=CARTESIAN_POINT('Ctrl Pts',(-6.93592464561993,83.8529102145597,
87.9663641555568));
#119615=CARTESIAN_POINT('Ctrl Pts',(-6.96115166965242,84.0739039790992,
87.9158844277155));
#119616=CARTESIAN_POINT('Ctrl Pts',(-6.98645600059154,84.2937475202454,
87.8630911193911));
#119617=CARTESIAN_POINT('Ctrl Pts',(-7.01070139620015,84.5043910515804,
87.8125071047854));
#119618=CARTESIAN_POINT('Ctrl Pts',(-7.03501818894437,84.713978522577,87.7597989460343));
#119619=CARTESIAN_POINT('Ctrl Pts',(-7.05921250535445,84.9224941290667,
87.7048834370974));
#119620=CARTESIAN_POINT('Ctrl Pts',(-7.06896083979781,85.0065088965959,
87.6827569699482));
#119621=CARTESIAN_POINT('Ctrl Pts',(-7.07868890741303,85.0903492738633,
87.6602719689559));
#119622=CARTESIAN_POINT('Ctrl Pts',(-7.08838232372406,85.1740126527982,
87.6374222456928));
#119623=CARTESIAN_POINT('',(-7.08815755158633,25.,87.6373268821602));
#119624=CARTESIAN_POINT('Origin',(27.4324635166691,25.,72.98888938658));
#119625=CARTESIAN_POINT('',(-8.15022843086022,88.9999999999406,84.8262046973771));
#119626=CARTESIAN_POINT('Ctrl Pts',(-7.08815755274652,85.1740126534065,
87.6373268794261));
#119627=CARTESIAN_POINT('Ctrl Pts',(-7.17036726380078,85.5345012501752,
87.4435908386425));
#119628=CARTESIAN_POINT('Ctrl Pts',(-7.25522061315342,85.8855446623315,
87.2391013265329));
#119629=CARTESIAN_POINT('Ctrl Pts',(-7.34216730501181,86.2271428898753,
87.0236694424198));
#119630=CARTESIAN_POINT('Ctrl Pts',(-7.38564065101201,86.3979420039261,
86.9159535001874));
#119631=CARTESIAN_POINT('Ctrl Pts',(-7.42963643207846,86.5663798218163,
86.8055018223152));
#119632=CARTESIAN_POINT('Ctrl Pts',(-7.47408022130472,86.7324563435456,
86.69229058004));
#119633=CARTESIAN_POINT('Ctrl Pts',(-7.49630211591786,86.8154946044102,
86.6356849589023));
#119634=CARTESIAN_POINT('Ctrl Pts',(-7.51863596096647,86.8979425412346,
86.5783894265339));
#119635=CARTESIAN_POINT('Ctrl Pts',(-7.54107208032303,86.9798001540188,
86.5204010481027));
#119636=CARTESIAN_POINT('Ctrl Pts',(-7.56219127703993,87.0568530079322,
86.4658163870069));
#119637=CARTESIAN_POINT('Ctrl Pts',(-7.58374961926499,87.1346233889664,
86.409704963375));
#119638=CARTESIAN_POINT('Ctrl Pts',(-7.60475461115699,87.2096079961757,
86.3546421099823));
#119639=CARTESIAN_POINT('Ctrl Pts',(-7.60606441236483,87.214283786083,86.3512085741708));
#119640=CARTESIAN_POINT('Ctrl Pts',(-7.60737207769441,87.2189487439171,
86.3477791216078));
#119641=CARTESIAN_POINT('Ctrl Pts',(-7.60867737276574,87.2236020202508,
86.3443543791131));
#119642=CARTESIAN_POINT('Ctrl Pts',(-7.69897653199269,87.5455115637841,
86.1074337206083));
#119643=CARTESIAN_POINT('Ctrl Pts',(-7.79034517661201,87.8565795431264,
85.8604972245752));
#119644=CARTESIAN_POINT('Ctrl Pts',(-7.88218584960569,88.1568059583733,
85.6033866075186));
#119645=CARTESIAN_POINT('Ctrl Pts',(-7.97128639647277,88.448074923533,85.3539470527077));
#119646=CARTESIAN_POINT('Ctrl Pts',(-8.06083103308143,88.7291396040179,
85.0949311765289));
#119647=CARTESIAN_POINT('Ctrl Pts',(-8.15022843086787,88.9999999999152,
84.8262046973541));
#119648=CARTESIAN_POINT('Origin',(27.4324635166691,89.,72.98888938658));
#119649=CARTESIAN_POINT('Origin',(27.4324635166691,89.,72.98888938658));
#119650=CARTESIAN_POINT('',(-8.15023280835573,89.,61.1515872344397));
#119651=CARTESIAN_POINT('Ctrl Pts',(-8.15022843089586,89.,84.82620469727));
#119652=CARTESIAN_POINT('Ctrl Pts',(-8.23099022828455,89.040788968413,84.5834366301713));
#119653=CARTESIAN_POINT('Ctrl Pts',(-8.3072115088959,89.0804132599216,84.3407528351496));
#119654=CARTESIAN_POINT('Ctrl Pts',(-8.37920382923813,89.1187594637775,
84.0984057817494));
#119655=CARTESIAN_POINT('Ctrl Pts',(-8.4538662110039,89.1585278570998,83.8470705263394));
#119656=CARTESIAN_POINT('Ctrl Pts',(-8.52398061097728,89.1969217770695,
83.5960976664654));
#119657=CARTESIAN_POINT('Ctrl Pts',(-8.58989600097626,89.2338606648925,
83.3457359072875));
#119658=CARTESIAN_POINT('Ctrl Pts',(-8.65741525486121,89.2716983556834,
83.0892823054612));
#119659=CARTESIAN_POINT('Ctrl Pts',(-8.7205291465347,89.3080096915148,82.8334699848971));
#119660=CARTESIAN_POINT('Ctrl Pts',(-8.77960675471714,89.3427512305223,
82.5785301532357));
#119661=CARTESIAN_POINT('Ctrl Pts',(-8.84016030158506,89.3783607190456,
82.3172211476758));
#119662=CARTESIAN_POINT('Ctrl Pts',(-8.89647381090144,89.4123214017868,
82.0568287849466));
#119663=CARTESIAN_POINT('Ctrl Pts',(-8.94893137920165,89.4446254527761,
81.7975638237655));
#119664=CARTESIAN_POINT('Ctrl Pts',(-9.00272174432682,89.4777502573381,
81.5317116812056));
#119665=CARTESIAN_POINT('Ctrl Pts',(-9.05245813981911,89.5091336420425,
81.2670449049156));
#119666=CARTESIAN_POINT('Ctrl Pts',(-9.09853431394997,89.5388008973398,
81.0037513160143));
#119667=CARTESIAN_POINT('Ctrl Pts',(-9.14578370419498,89.5692235561105,
80.7337536053606));
#119668=CARTESIAN_POINT('Ctrl Pts',(-9.18918444346121,89.5978420867409,
80.4651997864143));
#119669=CARTESIAN_POINT('Ctrl Pts',(-9.22913424351228,89.6247112734543,
80.1982527545268));
#119670=CARTESIAN_POINT('Ctrl Pts',(-9.27008186582461,89.6522515692249,
79.9246382126481));
#119671=CARTESIAN_POINT('Ctrl Pts',(-9.30740428114443,89.6779545858764,
79.6527115481155));
#119672=CARTESIAN_POINT('Ctrl Pts',(-9.34149710551561,89.7018997176548,
79.382609315175));
#119673=CARTESIAN_POINT('Ctrl Pts',(-9.37682272870595,89.7267107070066,
79.1027401673497));
#119674=CARTESIAN_POINT('Ctrl Pts',(-9.40868125352791,89.7496349422738,
78.8248296112862));
#119675=CARTESIAN_POINT('Ctrl Pts',(-9.43747375244598,89.7707738252341,
78.548990948235));
#119676=CARTESIAN_POINT('Ctrl Pts',(-9.46681260492824,89.79231383017,78.2679180942535));
#119677=CARTESIAN_POINT('Ctrl Pts',(-9.49296806742673,89.8120006729132,
77.9889961971702));
#119678=CARTESIAN_POINT('Ctrl Pts',(-9.51632189397733,89.8299460219586,
77.7123096368855));
#119679=CARTESIAN_POINT('Ctrl Pts',(-9.54005451876946,89.8481824439315,
77.4311352303687));
#119680=CARTESIAN_POINT('Ctrl Pts',(-9.56089390164509,89.864620967278,77.1522689208994));
#119681=CARTESIAN_POINT('Ctrl Pts',(-9.57919626952247,89.8793745450462,
76.8757679999358));
#119682=CARTESIAN_POINT('Ctrl Pts',(-9.59773862113798,89.8943215742174,
76.5956415522067));
#119683=CARTESIAN_POINT('Ctrl Pts',(-9.61367694107309,89.9075396619312,
76.3179425767034));
#119684=CARTESIAN_POINT('Ctrl Pts',(-9.62733674672953,89.9191340964769,
76.042704161449));
#119685=CARTESIAN_POINT('Ctrl Pts',(-9.64118935864556,89.9308921848559,
75.763580794192));
#119686=CARTESIAN_POINT('Ctrl Pts',(-9.65269862180367,89.9409808739967,
75.4869875985512));
#119687=CARTESIAN_POINT('Ctrl Pts',(-9.66215898432848,89.9494907165252,
75.2129373093804));
#119688=CARTESIAN_POINT('Ctrl Pts',(-9.67166871289319,89.9580449650925,
74.9374569716806));
#119689=CARTESIAN_POINT('Ctrl Pts',(-9.6791079897816,89.9650041387877,74.6645458048206));
#119690=CARTESIAN_POINT('Ctrl Pts',(-9.68473211235737,89.9704355901593,
74.394200121574));
#119691=CARTESIAN_POINT('Ctrl Pts',(-9.69038567099905,89.9758954691761,
74.122439477461));
#119692=CARTESIAN_POINT('Ctrl Pts',(-9.69420494935699,89.9798117901643,
73.853270926103));
#119693=CARTESIAN_POINT('Ctrl Pts',(-9.69640658254741,89.9822244493205,
73.5866789427521));
#119694=CARTESIAN_POINT('Ctrl Pts',(-9.69765753916908,89.9835953098073,
73.4352027530279));
#119695=CARTESIAN_POINT('Ctrl Pts',(-9.69838547816114,89.9844801812682,
73.2845582091729));
#119696=CARTESIAN_POINT('Ctrl Pts',(-9.69862415412181,89.9848820179164,
73.1347413557224));
#119697=CARTESIAN_POINT('Ctrl Pts',(-9.69880899985258,89.9851932255835,
73.0187137269644));
#119698=CARTESIAN_POINT('Ctrl Pts',(-9.69870030258848,89.9852146484256,
72.9031825241757));
#119699=CARTESIAN_POINT('Ctrl Pts',(-9.69831197418757,89.9849463301446,
72.7881457028777));
#119700=CARTESIAN_POINT('Ctrl Pts',(-9.69811780998711,89.9848121710041,
72.7306272922287));
#119701=CARTESIAN_POINT('Ctrl Pts',(-9.69785371532275,89.9846055568432,
72.6732324771218));
#119702=CARTESIAN_POINT('Ctrl Pts',(-9.69752128278207,89.9843263864972,
72.6159609876627));
#119703=CARTESIAN_POINT('Ctrl Pts',(-9.69723837411871,89.9840888053348,
72.5672214734792));
#119704=CARTESIAN_POINT('Ctrl Pts',(-9.6968968822444,89.9837889265374,72.5172614285427));
#119705=CARTESIAN_POINT('Ctrl Pts',(-9.69652059962177,89.98345152985,72.4694248344562));
#119706=CARTESIAN_POINT('Ctrl Pts',(-9.69645473039663,89.9833924677062,
72.4610509176282));
#119707=CARTESIAN_POINT('Ctrl Pts',(-9.69638792490953,89.9833322559799,
72.4527420703728));
#119708=CARTESIAN_POINT('Ctrl Pts',(-9.6963204727055,89.9832710277394,72.4445162301548));
#119709=CARTESIAN_POINT('Ctrl Pts',(-9.69415092230604,89.9813016665379,
72.1799381457496));
#119710=CARTESIAN_POINT('Ctrl Pts',(-9.69042915325381,89.9778218956941,
71.9131805112186));
#119711=CARTESIAN_POINT('Ctrl Pts',(-9.68497059678481,89.9727958742029,
71.6442252251322));
#119712=CARTESIAN_POINT('Ctrl Pts',(-9.67950014414439,89.9677588991906,
71.3746837880731));
#119713=CARTESIAN_POINT('Ctrl Pts',(-9.67228544970801,89.9611687731311,
71.1029347875081));
#119714=CARTESIAN_POINT('Ctrl Pts',(-9.66309824485758,89.9529598432053,
70.8289704889018));
#119715=CARTESIAN_POINT('Ctrl Pts',(-9.65404878935528,89.9448739947568,
70.5591139035943));
#119716=CARTESIAN_POINT('Ctrl Pts',(-9.64308557086269,89.9352172001176,
70.2871076504854));
#119717=CARTESIAN_POINT('Ctrl Pts',(-9.62994819833856,89.9239017139816,
70.0129590830614));
#119718=CARTESIAN_POINT('Ctrl Pts',(-9.61651086337457,89.9123278640956,
69.7325509479028));
#119719=CARTESIAN_POINT('Ctrl Pts',(-9.60079931872581,89.8990184010136,
69.4499010640564));
#119720=CARTESIAN_POINT('Ctrl Pts',(-9.58248695867312,89.8838576197446,
69.1650389459225));
#119721=CARTESIAN_POINT('Ctrl Pts',(-9.56417459862044,89.8686968384756,
68.8801768277886));
#119722=CARTESIAN_POINT('Ctrl Pts',(-9.54326161077761,89.8516841940021,
68.5931019996591));
#119723=CARTESIAN_POINT('Ctrl Pts',(-9.51937003839826,89.8326890010658,
68.3038725446563));
#119724=CARTESIAN_POINT('Ctrl Pts',(-9.51325248701204,89.8278251910564,
68.2298139592566));
#119725=CARTESIAN_POINT('Ctrl Pts',(-9.50688313067602,89.82278018902,68.1549359143919));
#119726=CARTESIAN_POINT('Ctrl Pts',(-9.50041457050318,89.8176926172772,
68.0811433185792));
#119727=CARTESIAN_POINT('Ctrl Pts',(-9.49643999587079,89.8145665841186,
68.035801825026));
#119728=CARTESIAN_POINT('Ctrl Pts',(-9.49242901214205,89.8114245665556,
67.9908700903788));
#119729=CARTESIAN_POINT('Ctrl Pts',(-9.48842673027931,89.8082995552444,
67.946789497296));
#119730=CARTESIAN_POINT('Ctrl Pts',(-9.47791079514489,89.8000886352317,
67.8309684048684));
#119731=CARTESIAN_POINT('Ctrl Pts',(-9.46686551069631,89.7915572195587,
67.7146039273164));
#119732=CARTESIAN_POINT('Ctrl Pts',(-9.45525766962326,89.7826964392123,
67.5977024306567));
#119733=CARTESIAN_POINT('Ctrl Pts',(-9.43204198747717,89.7649748785196,
67.3638994373374));
#119734=CARTESIAN_POINT('Ctrl Pts',(-9.40657713178295,89.7459365233459,
67.1279482182838));
#119735=CARTESIAN_POINT('Ctrl Pts',(-9.37857876259766,89.7255146874016,
66.8899176101877));
#119736=CARTESIAN_POINT('Ctrl Pts',(-9.34777506896367,89.7030466652926,
66.6280372885596));
#119737=CARTESIAN_POINT('Ctrl Pts',(-9.31390519847322,89.6789034791376,
66.3636392431617));
#119738=CARTESIAN_POINT('Ctrl Pts',(-9.27655786722363,89.6530046963734,
66.09684619365));
#119739=CARTESIAN_POINT('Ctrl Pts',(-9.23993781998643,89.6276102540804,
65.8352485439977));
#119740=CARTESIAN_POINT('Ctrl Pts',(-9.19997422560453,89.6005274408591,
65.5713480466599));
#119741=CARTESIAN_POINT('Ctrl Pts',(-9.1562484296008,89.5716957264074,65.3052953170558));
#119742=CARTESIAN_POINT('Ctrl Pts',(-9.11386252192325,89.5437475013635,
65.0473952336954));
#119743=CARTESIAN_POINT('Ctrl Pts',(-9.06794113880673,89.5141554994056,
64.7874727033319));
#119744=CARTESIAN_POINT('Ctrl Pts',(-9.01807743618613,89.4828855884678,
64.5257001931378));
#119745=CARTESIAN_POINT('Ctrl Pts',(-8.98110727649462,89.4597013173416,
64.3316156988844));
#119746=CARTESIAN_POINT('Ctrl Pts',(-8.94196943300685,89.4355950611352,
64.136514953116));
#119747=CARTESIAN_POINT('Ctrl Pts',(-8.90049023128382,89.4105628602268,
63.9404818633314));
#119748=CARTESIAN_POINT('Ctrl Pts',(-8.87374043729102,89.3944196802795,
63.8140608004931));
#119749=CARTESIAN_POINT('Ctrl Pts',(-8.84601675892349,89.3778915875108,
63.6872522230383));
#119750=CARTESIAN_POINT('Ctrl Pts',(-8.81727136207657,89.3609798242451,
63.5600813823535));
#119751=CARTESIAN_POINT('Ctrl Pts',(-8.80289866365312,89.3525239426123,
63.4964959620111));
#119752=CARTESIAN_POINT('Ctrl Pts',(-8.78827052166063,89.3439721398952,
63.4328199795232));
#119753=CARTESIAN_POINT('Ctrl Pts',(-8.77338087736314,89.3353248110982,
63.3690568457531));
#119754=CARTESIAN_POINT('Ctrl Pts',(-8.76139824326063,89.3283657612467,
63.317742637977));
#119755=CARTESIAN_POINT('Ctrl Pts',(-8.7498000098866,89.3216673898715,63.2687267767439));
#119756=CARTESIAN_POINT('Ctrl Pts',(-8.73810400382164,89.3149473055847,
63.219886471355));
#119757=CARTESIAN_POINT('Ctrl Pts',(-8.7352665301426,89.3133170001472,63.2080377188622));
#119758=CARTESIAN_POINT('Ctrl Pts',(-8.73242306773881,89.3116853999522,
63.19619935055));
#119759=CARTESIAN_POINT('Ctrl Pts',(-8.72956628736566,89.3100484417968,
63.1843411558216));
#119760=CARTESIAN_POINT('Ctrl Pts',(-8.67103681448578,89.2765105825837,
62.9413914725765));
#119761=CARTESIAN_POINT('Ctrl Pts',(-8.61029041858642,89.2425921176504,
62.7040929500362));
#119762=CARTESIAN_POINT('Ctrl Pts',(-8.54759953967446,89.2083683446713,
62.4724949310574));
#119763=CARTESIAN_POINT('Ctrl Pts',(-8.46136277254382,89.1612905625131,
62.1539116733774));
#119764=CARTESIAN_POINT('Ctrl Pts',(-8.37144770856337,89.1136344577483,
61.8461167293845));
#119765=CARTESIAN_POINT('Ctrl Pts',(-8.27854025383427,89.0656082931277,
61.5491975618905));
#119766=CARTESIAN_POINT('Ctrl Pts',(-8.23636727388946,89.0438080351906,
61.4144186452527));
#119767=CARTESIAN_POINT('Ctrl Pts',(-8.19357735405081,89.0219317507927,
61.2818800821673));
#119768=CARTESIAN_POINT('Ctrl Pts',(-8.15023280835573,89.,61.1515872344397));
#119769=CARTESIAN_POINT('Origin',(27.4324635166691,89.,72.98888938658));
#119770=CARTESIAN_POINT('Origin',(27.4324635166691,25.,72.98888938658));
#119771=CARTESIAN_POINT('',(-7.08823084473591,85.17401267208,58.34042080741));
#119772=CARTESIAN_POINT('Ctrl Pts',(-8.15023171813679,88.9999966970448,
61.1515839572636));
#119773=CARTESIAN_POINT('Ctrl Pts',(-8.06825403899497,88.7516349867913,
60.9051607496867));
#119774=CARTESIAN_POINT('Ctrl Pts',(-7.98615707526439,88.4947314647135,
60.6669181708804));
#119775=CARTESIAN_POINT('Ctrl Pts',(-7.90440000894433,88.2292835455461,
60.4367550592167));
#119776=CARTESIAN_POINT('Ctrl Pts',(-7.86352129457012,88.0965589975983,
60.3216729932293));
#119777=CARTESIAN_POINT('Ctrl Pts',(-7.82272705501043,87.9616983314395,
60.2086106683171));
#119778=CARTESIAN_POINT('Ctrl Pts',(-7.78207158303099,87.8247015470696,
60.0975544009398));
#119779=CARTESIAN_POINT('Ctrl Pts',(-7.76174384704127,87.7562031548847,
60.0420262672512));
#119780=CARTESIAN_POINT('Ctrl Pts',(-7.74145077759651,87.687170733147,59.9869996572717));
#119781=CARTESIAN_POINT('Ctrl Pts',(-7.72119896745376,87.6176042818565,
59.9324728049764));
#119782=CARTESIAN_POINT('Ctrl Pts',(-7.71107306238239,87.5828210562113,
59.9052093788288));
#119783=CARTESIAN_POINT('Ctrl Pts',(-7.7009574705316,87.5479043231778,59.8780708926836));
#119784=CARTESIAN_POINT('Ctrl Pts',(-7.69085300541049,87.5128540827562,
59.8510571266594));
#119785=CARTESIAN_POINT('Ctrl Pts',(-7.68580077284993,87.4953289625454,
59.8375502436472));
#119786=CARTESIAN_POINT('Ctrl Pts',(-7.68075132187224,87.4777704654875,
59.8240745407027));
#119787=CARTESIAN_POINT('Ctrl Pts',(-7.67570475343219,87.4601785915826,
59.8106299902009));
#119788=CARTESIAN_POINT('Ctrl Pts',(-7.67191982710215,87.4469846861539,
59.8005465773246));
#119789=CARTESIAN_POINT('Ctrl Pts',(-7.66813652219137,87.4337720062488,
59.7904806877004));
#119790=CARTESIAN_POINT('Ctrl Pts',(-7.66435488111403,87.4205405518672,
59.7804323096526));
#119791=CARTESIAN_POINT('Ctrl Pts',(-7.66309433408825,87.4161300670734,
59.7770828503034));
#119792=CARTESIAN_POINT('Ctrl Pts',(-7.66213046872563,87.4127561859883,
59.774522489036));
#119793=CARTESIAN_POINT('Ctrl Pts',(-7.66057379620993,87.4073028393268,
59.7703897683601));
#119794=CARTESIAN_POINT('Ctrl Pts',(-7.57292901815406,87.1002650051115,
59.5377066685055));
#119795=CARTESIAN_POINT('Ctrl Pts',(-7.48650824070021,86.7842493410492,
59.3152773725034));
#119796=CARTESIAN_POINT('Ctrl Pts',(-7.4018625872353,86.45925584714,59.1029351562491));
#119797=CARTESIAN_POINT('Ctrl Pts',(-7.31672440178161,86.1323712969823,
58.8893573734914));
#119798=CARTESIAN_POINT('Ctrl Pts',(-7.23338203755186,85.7964041334929,
58.6859841080592));
#119799=CARTESIAN_POINT('Ctrl Pts',(-7.15234364504138,85.451354356672,58.4926445767232));
#119800=CARTESIAN_POINT('Ctrl Pts',(-7.13078249036753,85.3595500725821,
58.4412044702432));
#119801=CARTESIAN_POINT('Ctrl Pts',(-7.10938414421814,85.2671028443848,
58.3904746433863));
#119802=CARTESIAN_POINT('Ctrl Pts',(-7.08815755789147,85.17401267208,58.3404519058586));
#119803=CARTESIAN_POINT('',(-7.08815755789148,25.,58.3404519058586));
#119804=CARTESIAN_POINT('Origin',(-2.02513312664091,25.,60.48888938658));
#119805=CARTESIAN_POINT('',(-6.3608745026988,75.000000198958,57.1044283173089));
#119806=CARTESIAN_POINT('Ctrl Pts',(-7.08823084473591,85.17401267208,58.34042080741));
#119807=CARTESIAN_POINT('Ctrl Pts',(-6.99794733253354,84.395480762676,58.1278617890738));
#119808=CARTESIAN_POINT('Ctrl Pts',(-6.90526175250424,83.6014255566489,
57.9461672025321));
#119809=CARTESIAN_POINT('Ctrl Pts',(-6.77559318043826,82.3870578026733,
57.7156418039018));
#119810=CARTESIAN_POINT('Ctrl Pts',(-6.73388351299471,81.9783877271923,
57.6457886604248));
#119811=CARTESIAN_POINT('Ctrl Pts',(-6.67482258874527,81.3595613777372,
57.5509009776497));
#119812=CARTESIAN_POINT('Ctrl Pts',(-6.64616402539984,81.0486928939511,
57.5059302335453));
#119813=CARTESIAN_POINT('Ctrl Pts',(-6.61448392509546,80.6834662053486,
57.4576672877489));
#119814=CARTESIAN_POINT('Ctrl Pts',(-6.60130482845044,80.5263947407648,
57.4378709142691));
#119815=CARTESIAN_POINT('Ctrl Pts',(-6.59260961427136,80.4215591552874,
57.4248692009795));
#119816=CARTESIAN_POINT('Ctrl Pts',(-6.58847590583747,80.3711606040599,
57.4187159022452));
#119817=CARTESIAN_POINT('Ctrl Pts',(-6.44248206665566,78.5687353454011,
57.2023906778076));
#119818=CARTESIAN_POINT('Ctrl Pts',(-6.36088860509349,76.7965548568022,
57.1049235783142));
#119819=CARTESIAN_POINT('Ctrl Pts',(-6.36082055131841,75.0000001903814,
57.1044704220667));
#119820=CARTESIAN_POINT('Ctrl Pts',(-6.36082055131591,75.00000012423,57.10447042205));
#119821=CARTESIAN_POINT('Ctrl Pts',(-6.36078005892346,74.1015163751048,
57.1047845229305));
#119822=CARTESIAN_POINT('Ctrl Pts',(-6.38054795665555,73.2093627488455,
57.1296675067439));
#119823=CARTESIAN_POINT('Ctrl Pts',(-6.43768908071951,71.8806274937553,
57.2055446823194));
#119824=CARTESIAN_POINT('Ctrl Pts',(-6.46127736870379,71.4392982727752,
57.2372936872005));
#119825=CARTESIAN_POINT('Ctrl Pts',(-6.50284689574204,70.7796782373796,
57.2950449971091));
#119826=CARTESIAN_POINT('Ctrl Pts',(-6.52517432368794,70.4504616687004,
57.3264550703474));
#119827=CARTESIAN_POINT('Ctrl Pts',(-6.55374105031257,70.0674142076908,
57.3676560019655));
#119828=CARTESIAN_POINT('Ctrl Pts',(-6.56650106834364,69.9034735534973,
57.386304042184));
#119829=CARTESIAN_POINT('Ctrl Pts',(-6.57512008494194,69.7942292381198,
57.3989577885545));
#119830=CARTESIAN_POINT('Ctrl Pts',(-6.57964842000668,69.7376238449638,
57.4056364990831));
#119831=CARTESIAN_POINT('Ctrl Pts',(-6.72015827311288,68.0029873888583,
57.6138146305435));
#119832=CARTESIAN_POINT('Ctrl Pts',(-6.90771375469196,66.3832968065684,
57.9152166422413));
#119833=CARTESIAN_POINT('Ctrl Pts',(-7.08826202869291,64.825987357,58.34040756172));
#119834=CARTESIAN_POINT('Ctrl Pts',(-7.03188519117291,64.48864439232,87.78728731875));
#119835=CARTESIAN_POINT('Ctrl Pts',(-6.88609751213191,65.18356633688,88.1317453461401));
#119836=CARTESIAN_POINT('Ctrl Pts',(-6.48107502800391,67.06022719065,88.90591654349));
#119837=CARTESIAN_POINT('Ctrl Pts',(-5.85681573002291,70.58880890762,89.73590455514));
#119838=CARTESIAN_POINT('Ctrl Pts',(-5.56514360048791,75.000227314,90.0489960419));
#119839=CARTESIAN_POINT('Ctrl Pts',(-5.85684197554291,79.41149656929,89.73588726852));
#119840=CARTESIAN_POINT('Ctrl Pts',(-6.48119721579791,82.94037009471,88.9057205787));
#119841=CARTESIAN_POINT('Ctrl Pts',(-6.88619858540991,84.81690451187,88.13154376415));
#119842=CARTESIAN_POINT('Ctrl Pts',(-7.03199311061991,85.51186803899,87.78703386752));
#119843=CARTESIAN_POINT('Ctrl Pts',(-7.61748537101091,65.71636999684,86.17253031082));
#119844=CARTESIAN_POINT('Ctrl Pts',(-7.51830008809391,66.33734423762,86.47777868194));
#119845=CARTESIAN_POINT('Ctrl Pts',(-7.23957881195592,68.00723840045,87.16157842494));
#119846=CARTESIAN_POINT('Ctrl Pts',(-6.79943501286791,71.12056079708,87.89696611428));
#119847=CARTESIAN_POINT('Ctrl Pts',(-6.59060414049291,75.00020008,88.17713487981));
#119848=CARTESIAN_POINT('Ctrl Pts',(-6.79945418426991,78.87970714104,87.89695030624));
#119849=CARTESIAN_POINT('Ctrl Pts',(-7.23966394454191,81.99329091746,87.16140528946));
#119850=CARTESIAN_POINT('Ctrl Pts',(-7.51836939848791,83.66307480429,86.4776005098));
#119851=CARTESIAN_POINT('Ctrl Pts',(-7.61755877579091,84.28408768177,86.17230574268));
#119852=CARTESIAN_POINT('Ctrl Pts',(-8.94180860021491,66.85942373552,84.99045086646));
#119853=CARTESIAN_POINT('Ctrl Pts',(-8.87784689601391,67.42208270543,85.27891160191));
#119854=CARTESIAN_POINT('Ctrl Pts',(-8.69724452663791,68.91837287318,85.9195538233101));
#119855=CARTESIAN_POINT('Ctrl Pts',(-8.40920338350691,71.64461634376,86.6015220059799));
#119856=CARTESIAN_POINT('Ctrl Pts',(-8.27170246170191,75.00017346889,86.8622727040301));
#119857=CARTESIAN_POINT('Ctrl Pts',(-8.40921610499591,78.3556137306,86.60150734616));
#119858=CARTESIAN_POINT('Ctrl Pts',(-8.69729997195491,81.08209623368,85.91939262999));
#119859=CARTESIAN_POINT('Ctrl Pts',(-8.87789174106491,82.57829325392,85.27874430401));
#119860=CARTESIAN_POINT('Ctrl Pts',(-8.94185593213491,83.1409906991,84.99023863948));
#119861=CARTESIAN_POINT('Ctrl Pts',(-10.7849842451049,67.728030224,84.437303609));
#119862=CARTESIAN_POINT('Ctrl Pts',(-10.7390193110219,68.25768814305,84.73418589492));
#119863=CARTESIAN_POINT('Ctrl Pts',(-10.6120633653509,69.64235959775,85.38604975076));
#119864=CARTESIAN_POINT('Ctrl Pts',(-10.4188592067689,72.07396927714,86.06464821073));
#119865=CARTESIAN_POINT('Ctrl Pts',(-10.3293343809289,75.00015189878,86.32270937777));
#119866=CARTESIAN_POINT('Ctrl Pts',(-10.4188671733959,77.92622889483,86.06463417814));
#119867=CARTESIAN_POINT('Ctrl Pts',(-10.6121014201629,80.35806705098,85.38588762974));
#119868=CARTESIAN_POINT('Ctrl Pts',(-10.7390510501279,81.74266061082,84.73401513024));
#119869=CARTESIAN_POINT('Ctrl Pts',(-10.7850182747159,82.27235965491,84.43708513232));
#119870=CARTESIAN_POINT('',(-10.5124658720316,82.2724294924703,84.5902497248058));
#119871=CARTESIAN_POINT('Origin',(-13.9921841235194,85.1739455889546,90.5667900805245));
#119872=CARTESIAN_POINT('',(-10.5124533228377,67.7276214880894,84.5902767292648));
#119873=CARTESIAN_POINT('Ctrl Pts',(-7.0883818064374,64.8259873343747,87.637422020082));
#119874=CARTESIAN_POINT('Ctrl Pts',(-7.1363573875817,64.9120414131586,87.5243405857398));
#119875=CARTESIAN_POINT('Ctrl Pts',(-7.18874895534319,64.9985784645067,
87.4123798504516));
#119876=CARTESIAN_POINT('Ctrl Pts',(-7.24554630246499,65.0853673865831,
87.3018945690997));
#119877=CARTESIAN_POINT('Ctrl Pts',(-7.30203975256059,65.1716919402222,
87.1920004447321));
#119878=CARTESIAN_POINT('Ctrl Pts',(-7.36289203093885,65.258265410166,87.0835664700366));
#119879=CARTESIAN_POINT('Ctrl Pts',(-7.42804307835773,65.3448487590915,
86.97693850846));
#119880=CARTESIAN_POINT('Ctrl Pts',(-7.4929119982875,65.4310571709469,86.8707722843422));
#119881=CARTESIAN_POINT('Ctrl Pts',(-7.56204252324817,65.5172750897001,
86.7663969043445));
#119882=CARTESIAN_POINT('Ctrl Pts',(-7.63532522931996,65.6032591451936,
86.6641439642266));
#119883=CARTESIAN_POINT('Ctrl Pts',(-7.70836562802005,65.6889588966322,
86.5622291208097));
#119884=CARTESIAN_POINT('Ctrl Pts',(-7.78553069649791,65.7744260296269,
86.4624231268371));
#119885=CARTESIAN_POINT('Ctrl Pts',(-7.86666300528646,65.8594165712825,
86.3650381068938));
#119886=CARTESIAN_POINT('Ctrl Pts',(-7.94972480666814,65.9464283622167,
86.2653370715743));
#119887=CARTESIAN_POINT('Ctrl Pts',(-8.03694480940951,66.0329402845693,
86.1681740647751));
#119888=CARTESIAN_POINT('Ctrl Pts',(-8.12810281466341,66.1186922363791,
86.0738596015708));
#119889=CARTESIAN_POINT('Ctrl Pts',(-8.21684696864524,66.2021734884584,
85.9820425722051));
#119890=CARTESIAN_POINT('Ctrl Pts',(-8.3093228698759,66.2849342013616,85.8929254695088));
#119891=CARTESIAN_POINT('Ctrl Pts',(-8.40528331540584,66.3667405844881,
85.8067664771821));
#119892=CARTESIAN_POINT('Ctrl Pts',(-8.50125644712467,66.4485577826043,
85.7205960944409));
#119893=CARTESIAN_POINT('Ctrl Pts',(-8.60071471462732,66.5294201127503,
85.6373849072769));
#119894=CARTESIAN_POINT('Ctrl Pts',(-8.70337175913268,66.6091042380695,
85.5573582535216));
#119895=CARTESIAN_POINT('Ctrl Pts',(-8.80613614014928,66.6888716797949,
85.4772479252181));
#119896=CARTESIAN_POINT('Ctrl Pts',(-8.91210559832289,66.7674581872891,
85.4003290361888));
#119897=CARTESIAN_POINT('Ctrl Pts',(-9.02095916621875,66.8446544329877,
85.3267904997943));
#119898=CARTESIAN_POINT('Ctrl Pts',(-9.13482440844064,66.9254048335946,
85.2498662113115));
#119899=CARTESIAN_POINT('Ctrl Pts',(-9.25184515284972,67.0046335847733,
85.1766412400787));
#119900=CARTESIAN_POINT('Ctrl Pts',(-9.37162211306383,67.0821226882352,
85.1072847713051));
#119901=CARTESIAN_POINT('Ctrl Pts',(-9.48691984041536,67.1567139744701,
85.0405219881085));
#119902=CARTESIAN_POINT('Ctrl Pts',(-9.60477082817847,67.2296932391917,
84.9773435825922));
#119903=CARTESIAN_POINT('Ctrl Pts',(-9.72479786071144,67.3008886557696,
84.9178564386286));
#119904=CARTESIAN_POINT('Ctrl Pts',(-9.84523065795204,67.3723247563566,
84.8581681917711));
#119905=CARTESIAN_POINT('Ctrl Pts',(-9.96785372820824,67.4419647734391,
84.8021962284059));
#119906=CARTESIAN_POINT('Ctrl Pts',(-10.0922728788578,67.5096601064754,
84.7500042148469));
#119907=CARTESIAN_POINT('Ctrl Pts',(-10.2174394678376,67.5777621139378,
84.6974986618427));
#119908=CARTESIAN_POINT('Ctrl Pts',(-10.3444232654319,67.6438958867125,
84.6488185701164));
#119909=CARTESIAN_POINT('Ctrl Pts',(-10.4728174088399,67.7079374181744,
84.6039841038095));
#119910=CARTESIAN_POINT('Ctrl Pts',(-10.4860152695413,67.714520360269,84.5993754898554));
#119911=CARTESIAN_POINT('Ctrl Pts',(-10.4992280313844,67.7210812198742,
84.5948074711202));
#119912=CARTESIAN_POINT('Ctrl Pts',(-10.5124552525542,67.7276198791653,
84.5902800433982));
#119913=CARTESIAN_POINT('',(-9.07682641225642,74.9999993273739,86.7031084130398));
#119914=CARTESIAN_POINT('Ctrl Pts',(-9.07682655323991,74.99999932735,86.70310871249));
#119915=CARTESIAN_POINT('Ctrl Pts',(-9.07712526169529,74.2289612612945,
86.7030795502179));
#119916=CARTESIAN_POINT('Ctrl Pts',(-9.14270438815803,73.4895290149526,
86.6375361780761));
#119917=CARTESIAN_POINT('Ctrl Pts',(-9.3533357059732,72.1026301973661,86.4100844515529));
#119918=CARTESIAN_POINT('Ctrl Pts',(-9.49858983167106,71.4552329230801,
86.2491187506501));
#119919=CARTESIAN_POINT('Ctrl Pts',(-9.80521029864172,70.2481781832132,
85.8621722888973));
#119920=CARTESIAN_POINT('Ctrl Pts',(-9.96584170202329,69.6878707034077,
85.6360582877567));
#119921=CARTESIAN_POINT('Ctrl Pts',(-10.2616407451189,68.6483272973767,
85.140895052477));
#119922=CARTESIAN_POINT('Ctrl Pts',(-10.397197373174,68.1684971409187,84.8713728384291));
#119923=CARTESIAN_POINT('Ctrl Pts',(-10.5124537296469,67.72762114885,84.59027742783));
#119924=CARTESIAN_POINT('Ctrl Pts',(-10.5124660110345,82.2724296180547,
84.590249978775));
#119925=CARTESIAN_POINT('Ctrl Pts',(-10.4327317076632,81.9674479999995,
84.7846994560194));
#119926=CARTESIAN_POINT('Ctrl Pts',(-10.3563178345119,81.6928249029256,
84.9429181111852));
#119927=CARTESIAN_POINT('Ctrl Pts',(-10.2548252957151,81.3329087641512,
85.1382332495564));
#119928=CARTESIAN_POINT('Ctrl Pts',(-10.2231180616871,81.2215555837217,
85.1963100913213));
#119929=CARTESIAN_POINT('Ctrl Pts',(-10.1646866545284,81.0167060472492,
85.3001066634692));
#119930=CARTESIAN_POINT('Ctrl Pts',(-10.137530445106,80.9217074846821,85.3465427226686));
#119931=CARTESIAN_POINT('Ctrl Pts',(-10.0667221831868,80.6732715679706,
85.4650986193299));
#119932=CARTESIAN_POINT('Ctrl Pts',(-10.006574102531,80.4619738935322,85.5619003025072));
#119933=CARTESIAN_POINT('Ctrl Pts',(-9.89784633786381,80.0728164008409,
85.7232268450414));
#119934=CARTESIAN_POINT('Ctrl Pts',(-9.85855483704574,79.9310487048605,
85.7796419776147));
#119935=CARTESIAN_POINT('Ctrl Pts',(-9.79567450569929,79.699751948937,85.8664855704092));
#119936=CARTESIAN_POINT('Ctrl Pts',(-9.77406187507859,79.6195447847065,
85.8958006922035));
#119937=CARTESIAN_POINT('Ctrl Pts',(-9.7407926882298,79.4944941612481,85.9400809236713));
#119938=CARTESIAN_POINT('Ctrl Pts',(-9.72394611655148,79.4307838217257,
85.962297655564));
#119939=CARTESIAN_POINT('Ctrl Pts',(-9.70395555604986,79.3543637447838,
85.9882951610611));
#119940=CARTESIAN_POINT('Ctrl Pts',(-9.69388109680604,79.3156286336885,
86.0013061847912));
#119941=CARTESIAN_POINT('Ctrl Pts',(-9.68954704161508,79.2989151157696,
86.0068841881018));
#119942=CARTESIAN_POINT('Ctrl Pts',(-9.68665408161935,79.2877476867685,
86.0106031809924));
#119943=CARTESIAN_POINT('Ctrl Pts',(-9.68488954554205,79.2809281193058,
86.0128684664986));
#119944=CARTESIAN_POINT('Ctrl Pts',(-9.5386321981269,78.715198548132,86.2004537835104));
#119945=CARTESIAN_POINT('Ctrl Pts',(-9.38875542898227,78.0813549654087,
86.3702394608437));
#119946=CARTESIAN_POINT('Ctrl Pts',(-9.15798583588213,76.6544047057943,
86.6219716832798));
#119947=CARTESIAN_POINT('Ctrl Pts',(-9.07716136819869,75.8598507335324,
86.7030186537697));
#119948=CARTESIAN_POINT('Ctrl Pts',(-9.07682655323991,74.99999932735,86.70310871249));
#119949=CARTESIAN_POINT('Ctrl Pts',(-6.95501669863192,85.15292062438,87.96390315669));
#119950=CARTESIAN_POINT('Ctrl Pts',(-7.05577166295491,85.6220618517,87.73413944146));
#119951=CARTESIAN_POINT('Ctrl Pts',(-7.30568233571291,86.70369358379,87.14935422758));
#119952=CARTESIAN_POINT('Ctrl Pts',(-7.70041279880391,88.17329653931,86.15516126834));
#119953=CARTESIAN_POINT('Ctrl Pts',(-7.99020466768391,89.12453288443,85.35040692656));
#119954=CARTESIAN_POINT('Ctrl Pts',(-8.11816676495491,89.52580380127,84.97601340087));
#119955=CARTESIAN_POINT('Ctrl Pts',(-7.61083224231891,83.87335575514,86.20258040905));
#119956=CARTESIAN_POINT('Ctrl Pts',(-7.67997552099091,84.2850156158801,
86.00281171969));
#119957=CARTESIAN_POINT('Ctrl Pts',(-7.85160010872291,85.2354085891601,
85.49468691626));
#119958=CARTESIAN_POINT('Ctrl Pts',(-8.12329981631592,86.53242756658,84.63146474731));
#119959=CARTESIAN_POINT('Ctrl Pts',(-8.32333534303391,87.37732082528,83.93205479338));
#119960=CARTESIAN_POINT('Ctrl Pts',(-8.41178168001291,87.73490557796,83.60629776158));
#119961=CARTESIAN_POINT('Ctrl Pts',(-9.10619845304691,82.6941092224099,
84.9604499123));
#119962=CARTESIAN_POINT('Ctrl Pts',(-9.14942950263491,83.05174595081,84.78078660695));
#119963=CARTESIAN_POINT('Ctrl Pts',(-9.25676191996691,83.87817202196,84.32433369085));
#119964=CARTESIAN_POINT('Ctrl Pts',(-9.42681211112791,85.00969446553,83.55043534523));
#119965=CARTESIAN_POINT('Ctrl Pts',(-9.55212940395591,85.75040379967,82.923637684635));
#119966=CARTESIAN_POINT('Ctrl Pts',(-9.6075636437929,86.06468918842,82.6315536));
#119967=CARTESIAN_POINT('Ctrl Pts',(-11.1563479441029,81.83974872807,84.47405456341));
#119968=CARTESIAN_POINT('Ctrl Pts',(-11.1843007701189,82.15710835684,84.30077826739));
#119969=CARTESIAN_POINT('Ctrl Pts',(-11.2535782960269,82.89044679757,83.86116867218));
#119970=CARTESIAN_POINT('Ctrl Pts',(-11.3627176534689,83.89507618764,83.11793696059));
#119971=CARTESIAN_POINT('Ctrl Pts',(-11.4425836537559,84.5536008381701,
82.517191706728));
#119972=CARTESIAN_POINT('Ctrl Pts',(-11.4777960592089,84.8332193001001,
82.237404575152));
#119973=CARTESIAN_POINT('',(-11.2183641640957,84.8936549215229,82.398008587887));
#119974=CARTESIAN_POINT('Origin',(-15.2667795907663,89.0000989196622,87.1935200637487));
#119975=CARTESIAN_POINT('Ctrl Pts',(-11.2183640786879,84.89365483489,82.398008486721));
#119976=CARTESIAN_POINT('Ctrl Pts',(-11.1916877670009,84.79458413089,82.505356281463));
#119977=CARTESIAN_POINT('Ctrl Pts',(-11.1374110586199,84.59363295486,82.71600930826));
#119978=CARTESIAN_POINT('Ctrl Pts',(-11.0534777220769,84.28413888454,83.01989100238));
#119979=CARTESIAN_POINT('Ctrl Pts',(-10.9672488249899,83.96689130624,83.31172338868));
#119980=CARTESIAN_POINT('Ctrl Pts',(-10.8789840138769,83.64218959052,83.59155535029));
#119981=CARTESIAN_POINT('Ctrl Pts',(-10.7889745724689,83.31029580231,83.85945164347));
#119982=CARTESIAN_POINT('Ctrl Pts',(-10.6976034072729,82.97143399976,84.11547480699));
#119983=CARTESIAN_POINT('Ctrl Pts',(-10.6052905178419,82.6257943239,84.35970336408));
#119984=CARTESIAN_POINT('Ctrl Pts',(-10.5434121371829,82.39092339779,84.51470624232));
#119985=CARTESIAN_POINT('Ctrl Pts',(-10.5124662721409,82.27243061678,84.59024934201));
#119986=CARTESIAN_POINT('Ctrl Pts',(-8.05759391320591,89.09479728929,85.11444853606));
#119987=CARTESIAN_POINT('Ctrl Pts',(-8.14537547024391,89.40820525939,84.88191214513));
#119988=CARTESIAN_POINT('Ctrl Pts',(-8.30485040107691,90.04383584284,84.32400074789));
#119989=CARTESIAN_POINT('Ctrl Pts',(-8.44711181861191,90.8927881628099,
83.3107809761201));
#119990=CARTESIAN_POINT('Ctrl Pts',(-8.49152901544292,91.61200955648,82.169824637043));
#119991=CARTESIAN_POINT('Ctrl Pts',(-8.46019247365591,92.1812155164301,
81.000788275304));
#119992=CARTESIAN_POINT('Ctrl Pts',(-8.38144499566592,92.62910837717,79.824303302778));
#119993=CARTESIAN_POINT('Ctrl Pts',(-8.28032368080192,92.9778795319,78.655233108223));
#119994=CARTESIAN_POINT('Ctrl Pts',(-8.17567642246891,93.24688018349,77.491375495357));
#119995=CARTESIAN_POINT('Ctrl Pts',(-8.0792216397619,93.45170953512,76.301792744643));
#119996=CARTESIAN_POINT('Ctrl Pts',(-8.00171757232991,93.59651183087,75.055323443605));
#119997=CARTESIAN_POINT('Ctrl Pts',(-7.95626984505191,93.67512561334,73.7508838101839));
#119998=CARTESIAN_POINT('Ctrl Pts',(-7.95303968845091,93.68056164489,72.4254389675695));
#119999=CARTESIAN_POINT('Ctrl Pts',(-7.9922643335139,93.61318488753,71.123698735184));
#120000=CARTESIAN_POINT('Ctrl Pts',(-8.06589394090391,93.47774173659,69.859266094178));
#120001=CARTESIAN_POINT('Ctrl Pts',(-8.16449146505991,93.27322272629,68.611528925018));
#120002=CARTESIAN_POINT('Ctrl Pts',(-8.27702127703391,92.99001093203,67.360147933957));
#120003=CARTESIAN_POINT('Ctrl Pts',(-8.38089851070491,92.63191641036,66.161932842428));
#120004=CARTESIAN_POINT('Ctrl Pts',(-8.45501279011491,92.20760376093,65.048518071429));
#120005=CARTESIAN_POINT('Ctrl Pts',(-8.48706795306991,91.72614549686,64.034326581107));
#120006=CARTESIAN_POINT('Ctrl Pts',(-8.46914099990891,91.1781515568,63.102992965472));
#120007=CARTESIAN_POINT('Ctrl Pts',(-8.39597121741591,90.56662317277,62.26482137247));
#120008=CARTESIAN_POINT('Ctrl Pts',(-8.26891544260791,89.90502511908,61.53563424739));
#120009=CARTESIAN_POINT('Ctrl Pts',(-8.14307662048791,89.402762062,61.0959841259));
#120010=CARTESIAN_POINT('Ctrl Pts',(-8.06733038719591,89.1295723537,60.8891544567201));
#120011=CARTESIAN_POINT('Ctrl Pts',(-8.05741235095491,89.09421528998,60.8629107499701));
#120012=CARTESIAN_POINT('Ctrl Pts',(-8.43449075962691,87.3255218789,83.72838173066));
#120013=CARTESIAN_POINT('Ctrl Pts',(-8.48604994062191,87.6134946867,83.5184247158101));
#120014=CARTESIAN_POINT('Ctrl Pts',(-8.58295769954691,88.1972243351,83.01531841742));
#120015=CARTESIAN_POINT('Ctrl Pts',(-8.67270363534791,88.97328181171,82.100770985326));
#120016=CARTESIAN_POINT('Ctrl Pts',(-8.70161580970891,89.62442872423,81.072223265241));
#120017=CARTESIAN_POINT('Ctrl Pts',(-8.68122039286491,90.13306172578,80.022995701701));
#120018=CARTESIAN_POINT('Ctrl Pts',(-8.62854234137091,90.52766929495,78.973848658753));
#120019=CARTESIAN_POINT('Ctrl Pts',(-8.55957570510291,90.83104487852,77.938493180666));
#120020=CARTESIAN_POINT('Ctrl Pts',(-8.48707215371791,91.06266767612,76.914171416008));
#120021=CARTESIAN_POINT('Ctrl Pts',(-8.4193990100769,91.23770308926,75.872605345747));
#120022=CARTESIAN_POINT('Ctrl Pts',(-8.36449198774192,91.36077676341,74.785590258427));
#120023=CARTESIAN_POINT('Ctrl Pts',(-8.33208811649991,91.42737337254,73.651011260914));
#120024=CARTESIAN_POINT('Ctrl Pts',(-8.32977951489891,91.43197300079,72.4993099454986));
#120025=CARTESIAN_POINT('Ctrl Pts',(-8.35776326441891,91.3749128398,71.367369082459));
#120026=CARTESIAN_POINT('Ctrl Pts',(-8.40999132472892,91.25987022267,70.2652675785361));
#120027=CARTESIAN_POINT('Ctrl Pts',(-8.47928365007991,91.08527122531,69.173517146296));
#120028=CARTESIAN_POINT('Ctrl Pts',(-8.55733844158391,90.84161384012,68.0726655952461));
#120029=CARTESIAN_POINT('Ctrl Pts',(-8.62816744586991,90.53014063058,67.011431700305));
#120030=CARTESIAN_POINT('Ctrl Pts',(-8.67775615445391,90.1562527277,66.018533444014));
#120031=CARTESIAN_POINT('Ctrl Pts',(-8.69874863300591,89.72661187799,65.108917233721));
#120032=CARTESIAN_POINT('Ctrl Pts',(-8.68698486500291,89.23205723218,64.270218074132));
#120033=CARTESIAN_POINT('Ctrl Pts',(-8.64030304788692,88.67534874195,63.513957909542));
#120034=CARTESIAN_POINT('Ctrl Pts',(-8.56108579733091,88.06966366952,62.85595626257));
#120035=CARTESIAN_POINT('Ctrl Pts',(-8.48488213662791,87.60848496498,62.4594052903301));
#120036=CARTESIAN_POINT('Ctrl Pts',(-8.44021087804591,87.35747749659,62.27270988017));
#120037=CARTESIAN_POINT('Ctrl Pts',(-8.43438199135791,87.32498891706,62.2490170251));
#120038=CARTESIAN_POINT('Ctrl Pts',(-9.6999844477539,85.6881588875,82.7738570047421));
#120039=CARTESIAN_POINT('Ctrl Pts',(-9.73052844606491,85.96801129276,82.5499001395251));
#120040=CARTESIAN_POINT('Ctrl Pts',(-9.78855454575391,86.53325677765,82.029291495388));
#120041=CARTESIAN_POINT('Ctrl Pts',(-9.84289992097791,87.28164187496,81.119418867505));
#120042=CARTESIAN_POINT('Ctrl Pts',(-9.86056579303691,87.90561991059,80.125117128897));
#120043=CARTESIAN_POINT('Ctrl Pts',(-9.84810420539291,88.38735477522,79.136154702713));
#120044=CARTESIAN_POINT('Ctrl Pts',(-9.8156728194649,88.7546501532,78.171273522151));
#120045=CARTESIAN_POINT('Ctrl Pts',(-9.77299215563892,89.03126880255,77.240847039094));
#120046=CARTESIAN_POINT('Ctrl Pts',(-9.72793680936391,89.23817877156,76.338821849754));
#120047=CARTESIAN_POINT('Ctrl Pts',(-9.68574655309991,89.39169056754,75.436996451304));
#120048=CARTESIAN_POINT('Ctrl Pts',(-9.65143069752991,89.4980030391201,
74.5083096496581));
#120049=CARTESIAN_POINT('Ctrl Pts',(-9.63114620088991,89.55493349031,73.5476360749947));
#120050=CARTESIAN_POINT('Ctrl Pts',(-9.62970017204091,89.55884994206,72.5758080726426));
#120051=CARTESIAN_POINT('Ctrl Pts',(-9.64722036840191,89.51012034927,71.618213001195));
#120052=CARTESIAN_POINT('Ctrl Pts',(-9.67987233041491,89.41094576649,70.6783078920771));
#120053=CARTESIAN_POINT('Ctrl Pts',(-9.72309053227491,89.2582139250901,
69.735130882087));
#120054=CARTESIAN_POINT('Ctrl Pts',(-9.77161007194191,89.0409437393701,
68.767148960646));
#120055=CARTESIAN_POINT('Ctrl Pts',(-9.81544045356291,88.75693664562,67.8132966510681));
#120056=CARTESIAN_POINT('Ctrl Pts',(-9.84597155572592,88.40888022177,66.900108010975));
#120057=CARTESIAN_POINT('Ctrl Pts',(-9.85882019495192,88.00260462959,66.045056833334));
#120058=CARTESIAN_POINT('Ctrl Pts',(-9.85161602892291,87.52992169388,65.23989706833));
#120059=CARTESIAN_POINT('Ctrl Pts',(-9.8232552816659,86.99445632834,64.498394809129));
#120060=CARTESIAN_POINT('Ctrl Pts',(-9.77545164269291,86.4097184428599,
63.837833742151));
#120061=CARTESIAN_POINT('Ctrl Pts',(-9.72987140316592,85.96304250074,63.427133769246));
#120062=CARTESIAN_POINT('Ctrl Pts',(-9.70337333602791,85.7192096835,63.228777314971));
#120063=CARTESIAN_POINT('Ctrl Pts',(-9.69991960746991,85.68763621062,63.203508570277));
#120064=CARTESIAN_POINT('Ctrl Pts',(-11.6120575244425,84.49584335857,82.433421016034));
#120065=CARTESIAN_POINT('Ctrl Pts',(-11.6408125507013,84.78644309534,82.161562454506));
#120066=CARTESIAN_POINT('Ctrl Pts',(-11.6910783687624,85.37015616451,81.554491230016));
#120067=CARTESIAN_POINT('Ctrl Pts',(-11.733908231978,86.14138350952,80.554401844931));
#120068=CARTESIAN_POINT('Ctrl Pts',(-11.746737304217,86.78429414385,79.509634128628));
#120069=CARTESIAN_POINT('Ctrl Pts',(-11.737684956696,87.27794978712,78.509867862637));
#120070=CARTESIAN_POINT('Ctrl Pts',(-11.7158054320425,87.64912935359,77.570065178083));
#120071=CARTESIAN_POINT('Ctrl Pts',(-11.6885150129063,87.92274679561,76.695714979443));
#120072=CARTESIAN_POINT('Ctrl Pts',(-11.6609630788506,88.12233512948,75.8753586663711));
#120073=CARTESIAN_POINT('Ctrl Pts',(-11.6360835214809,88.26670988172,75.078273434703));
#120074=CARTESIAN_POINT('Ctrl Pts',(-11.6164150273645,88.36443404092,74.276509733812));
#120075=CARTESIAN_POINT('Ctrl Pts',(-11.6050076721688,88.41589793954,73.460528085693));
#120076=CARTESIAN_POINT('Ctrl Pts',(-11.6042002723842,88.41941509469,72.6403035787583));
#120077=CARTESIAN_POINT('Ctrl Pts',(-11.6140353445887,88.3754368748,71.828258220239));
#120078=CARTESIAN_POINT('Ctrl Pts',(-11.632680458814,88.28456316836,71.0193957560081));
#120079=CARTESIAN_POINT('Ctrl Pts',(-11.6580421193584,88.1414636743,70.18896515103));
#120080=CARTESIAN_POINT('Ctrl Pts',(-11.6876146010148,87.93236709785,69.310782594631));
#120081=CARTESIAN_POINT('Ctrl Pts',(-11.7156592780194,87.65141820721,68.414176228036));
#120082=CARTESIAN_POINT('Ctrl Pts',(-11.7362453816865,87.29965989215,67.524646358954));
#120083=CARTESIAN_POINT('Ctrl Pts',(-11.7454264830685,86.88382894687,66.6637147582931));
#120084=CARTESIAN_POINT('Ctrl Pts',(-11.7403063415502,86.3972673145,65.8265851349111));
#120085=CARTESIAN_POINT('Ctrl Pts',(-11.7185959829517,85.84540569484,65.0298649044641));
#120086=CARTESIAN_POINT('Ctrl Pts',(-11.6797733935927,85.24264318848,64.2934889918351));
#120087=CARTESIAN_POINT('Ctrl Pts',(-11.6399483044843,84.78111485949,63.814097772889));
#120088=CARTESIAN_POINT('Ctrl Pts',(-11.6152461406276,84.5280769991699,
63.574515070347));
#120089=CARTESIAN_POINT('Ctrl Pts',(-11.6119993452045,84.49529024722,63.543845073383));
#120090=CARTESIAN_POINT('',(-11.2183629396496,84.893660453341,63.5797762185932));
#120091=CARTESIAN_POINT('Origin',(-15.2667666827029,88.99999891808,58.78411221242));
#120092=CARTESIAN_POINT('Ctrl Pts',(-11.2183626065601,84.8936601154805,
63.5797766131558));
#120093=CARTESIAN_POINT('Ctrl Pts',(-11.2440643838473,84.9878772718897,
63.6821529156428));
#120094=CARTESIAN_POINT('Ctrl Pts',(-11.2676805974612,85.0819208490858,
63.7873536467638));
#120095=CARTESIAN_POINT('Ctrl Pts',(-11.2893281573193,85.1755780930456,
63.8952945730814));
#120096=CARTESIAN_POINT('Ctrl Pts',(-11.3101899025391,85.265835543506,63.9993172028093));
#120097=CARTESIAN_POINT('Ctrl Pts',(-11.3292235684967,85.3557347030482,
64.1058853743975));
#120098=CARTESIAN_POINT('Ctrl Pts',(-11.3465346355939,85.4450809939655,
64.2149692606675));
#120099=CARTESIAN_POINT('Ctrl Pts',(-11.3652626521845,85.541740478283,64.3329819065866));
#120100=CARTESIAN_POINT('Ctrl Pts',(-11.3819749095474,85.6377537022209,
64.4539388724611));
#120101=CARTESIAN_POINT('Ctrl Pts',(-11.3968262427568,85.7329138232058,
64.5778551626002));
#120102=CARTESIAN_POINT('Ctrl Pts',(-11.4114570696226,85.8266610467739,
64.6999315958282));
#120103=CARTESIAN_POINT('Ctrl Pts',(-11.4242819467732,85.9195807517229,
64.8248806703207));
#120104=CARTESIAN_POINT('Ctrl Pts',(-11.4354420007458,86.0114518154075,
64.9527597856336));
#120105=CARTESIAN_POINT('Ctrl Pts',(-11.4469451661489,86.1061474184867,
65.0845704935991));
#120106=CARTESIAN_POINT('Ctrl Pts',(-11.4566796664678,86.1997293488902,
65.2194944701745));
#120107=CARTESIAN_POINT('Ctrl Pts',(-11.4648120393461,86.2919781405238,
65.3576488543686));
#120108=CARTESIAN_POINT('Ctrl Pts',(-11.466005961,86.3055212762758,65.3779314352756));
#120109=CARTESIAN_POINT('Ctrl Pts',(-11.4671653338274,86.3190356153124,
65.3982837068906));
#120110=CARTESIAN_POINT('Ctrl Pts',(-11.4682906666504,86.3325203963996,
65.418706104327));
#120111=CARTESIAN_POINT('Ctrl Pts',(-11.4743280332397,86.4048657196134,
65.5282714679603));
#120112=CARTESIAN_POINT('Ctrl Pts',(-11.4793359570297,86.476365120929,65.639798478805));
#120113=CARTESIAN_POINT('Ctrl Pts',(-11.4833397084349,86.546884348317,65.7532644534786));
#120114=CARTESIAN_POINT('Ctrl Pts',(-11.489870811182,86.6619185432754,65.938355350461));
#120115=CARTESIAN_POINT('Ctrl Pts',(-11.4937301361174,86.7743463826138,
66.1286040586217));
#120116=CARTESIAN_POINT('Ctrl Pts',(-11.4950660406149,86.8836703778639,
66.3240036328811));
#120117=CARTESIAN_POINT('Ctrl Pts',(-11.4954880319227,86.9182041157297,
66.3857272980393));
#120118=CARTESIAN_POINT('Ctrl Pts',(-11.4956581731352,86.9524278291927,
66.4479651528052));
#120119=CARTESIAN_POINT('Ctrl Pts',(-11.4955809788701,86.986324955698,66.5107175960102));
#120120=CARTESIAN_POINT('Ctrl Pts',(-11.4955462526203,87.0015737579076,
66.5389471155376));
#120121=CARTESIAN_POINT('Ctrl Pts',(-11.4954613695831,87.0167564257236,
66.567280552291));
#120122=CARTESIAN_POINT('Ctrl Pts',(-11.4953266861444,87.0318711487173,
66.5957173402037));
#120123=CARTESIAN_POINT('Ctrl Pts',(-11.4945472651005,87.1193409467324,
66.7602827176819));
#120124=CARTESIAN_POINT('Ctrl Pts',(-11.4920997209308,87.2045347935397,
66.9283086756899));
#120125=CARTESIAN_POINT('Ctrl Pts',(-11.4880865957529,87.2871590215378,
67.0997481823419));
#120126=CARTESIAN_POINT('Ctrl Pts',(-11.4857333004814,87.3356098413936,
67.2002802521017));
#120127=CARTESIAN_POINT('Ctrl Pts',(-11.4828419519049,87.3831763334808,
67.3019850253048));
#120128=CARTESIAN_POINT('Ctrl Pts',(-11.4794366396737,87.4297960762833,
67.4048490959103));
#120129=CARTESIAN_POINT('Ctrl Pts',(-11.478966455102,87.4362330436778,67.4190519342089));
#120130=CARTESIAN_POINT('Ctrl Pts',(-11.4784864812005,87.4426519655538,
67.4332768940122));
#120131=CARTESIAN_POINT('Ctrl Pts',(-11.4779967813246,87.4490526655553,
67.4475239062325));
#120132=CARTESIAN_POINT('Ctrl Pts',(-11.4767131552796,87.4658305036402,
67.4848688941509));
#120133=CARTESIAN_POINT('Ctrl Pts',(-11.4753627008147,87.4824831362804,
67.5223654019056));
#120134=CARTESIAN_POINT('Ctrl Pts',(-11.4739470005395,87.4990076744605,
67.5600128068845));
#120135=CARTESIAN_POINT('Ctrl Pts',(-11.4729691074825,87.5104219769358,
67.5860177011308));
#120136=CARTESIAN_POINT('Ctrl Pts',(-11.4719600740534,87.5217751589472,
67.6120945670384));
#120137=CARTESIAN_POINT('Ctrl Pts',(-11.4709204375023,87.533066255857,67.6382431522244));
#120138=CARTESIAN_POINT('Ctrl Pts',(-11.4704006192268,87.5387118043119,
67.6513174448174));
#120139=CARTESIAN_POINT('Ctrl Pts',(-11.4698731502832,87.5443418316278,
67.6644096671619));
#120140=CARTESIAN_POINT('Ctrl Pts',(-11.4693380985937,87.5499562175845,
67.6775197862553));
#120141=CARTESIAN_POINT('Ctrl Pts',(-11.4688030469042,87.5555706035413,
67.6906299053486));
#120142=CARTESIAN_POINT('Ctrl Pts',(-11.4683098506388,87.5606676415093,
67.7025765857496));
#120143=CARTESIAN_POINT('Ctrl Pts',(-11.4677102641549,87.5667523313235,
67.7169038004129));
#120144=CARTESIAN_POINT('Ctrl Pts',(-11.4593814924172,87.6512739039688,
67.915921129471));
#120145=CARTESIAN_POINT('Ctrl Pts',(-11.4496490888984,87.7310058292564,
68.116671032636));
#120146=CARTESIAN_POINT('Ctrl Pts',(-11.4388614406095,87.805888027071,68.3188814889115));
#120147=CARTESIAN_POINT('Ctrl Pts',(-11.4271990263813,87.8868423913448,
68.5374891074784));
#120148=CARTESIAN_POINT('Ctrl Pts',(-11.4143038178399,87.962128492374,68.7578051176865));
#120149=CARTESIAN_POINT('Ctrl Pts',(-11.4007134055397,88.0316981308213,
68.9795300453518));
#120150=CARTESIAN_POINT('Ctrl Pts',(-11.3979153008475,88.0460216941891,
69.0251805780055));
#120151=CARTESIAN_POINT('Ctrl Pts',(-11.3950876782912,88.0601031022114,
69.0708907961833));
#120152=CARTESIAN_POINT('Ctrl Pts',(-11.3922351522357,88.0739421860231,
69.1166580085631));
#120153=CARTESIAN_POINT('Ctrl Pts',(-11.3893241231477,88.0880650983972,
69.1633638699369));
#120154=CARTESIAN_POINT('Ctrl Pts',(-11.3863878696309,88.1019350238038,
69.2101286604569));
#120155=CARTESIAN_POINT('Ctrl Pts',(-11.3834311287561,88.1155522298085,
69.2569504871902));
#120156=CARTESIAN_POINT('Ctrl Pts',(-11.3713946747561,88.170985857788,69.447555206216));
#120157=CARTESIAN_POINT('Ctrl Pts',(-11.359019694,88.2222305320539,69.6391061576776));
#120158=CARTESIAN_POINT('Ctrl Pts',(-11.3466852494264,88.2692734167392,
69.8314251207791));
#120159=CARTESIAN_POINT('Ctrl Pts',(-11.3401069893598,88.294362534283,69.933993513501));
#120160=CARTESIAN_POINT('Ctrl Pts',(-11.3335399652676,88.3182570085292,
70.0367810142898));
#120161=CARTESIAN_POINT('Ctrl Pts',(-11.3270416342221,88.3409564268637,
70.1397668321956));
#120162=CARTESIAN_POINT('Ctrl Pts',(-11.3259511143649,88.3447657382495,
70.1570494357827));
#120163=CARTESIAN_POINT('Ctrl Pts',(-11.3248625266058,88.3485413950261,
70.1743376210178));
#120164=CARTESIAN_POINT('Ctrl Pts',(-11.3237761609902,88.3522833731834,
70.1916311965887));
#120165=CARTESIAN_POINT('Ctrl Pts',(-11.3199961900763,88.3653034544452,
70.2518035839664));
#120166=CARTESIAN_POINT('Ctrl Pts',(-11.316243007293,88.3779160421096,70.3120420658397));
#120167=CARTESIAN_POINT('Ctrl Pts',(-11.3125281520359,88.390121082633,70.3723422790808));
#120168=CARTESIAN_POINT('Ctrl Pts',(-11.3106707244074,88.3962236028947,
70.4024923857013));
#120169=CARTESIAN_POINT('Ctrl Pts',(-11.3088228770383,88.4022242340392,
70.4326579255869));
#120170=CARTESIAN_POINT('Ctrl Pts',(-11.3069860431439,88.4081229551823,
70.4628383562181));
#120171=CARTESIAN_POINT('Ctrl Pts',(-11.305608417723,88.4125469960397,70.4854736791915));
#120172=CARTESIAN_POINT('Ctrl Pts',(-11.3042369872504,88.4169137123298,
70.5081173782386));
#120173=CARTESIAN_POINT('Ctrl Pts',(-11.3028723541656,88.4212230917365,
70.5307692252172));
#120174=CARTESIAN_POINT('Ctrl Pts',(-11.3024174764707,88.4226595515387,
70.5383198408768));
#120175=CARTESIAN_POINT('Ctrl Pts',(-11.3018522650191,88.4244385126321,
70.5477220291572));
#120176=CARTESIAN_POINT('Ctrl Pts',(-11.3015100091043,88.4255133582408,
70.5534237797669));
#120177=CARTESIAN_POINT('Ctrl Pts',(-11.2940999934808,88.4487843154625,
70.6768695969599));
#120178=CARTESIAN_POINT('Ctrl Pts',(-11.2868138826341,88.4710863076103,
70.8051376168955));
#120179=CARTESIAN_POINT('Ctrl Pts',(-11.2798279157889,88.4920244103432,
70.9382902197918));
#120180=CARTESIAN_POINT('Ctrl Pts',(-11.2792804769337,88.4936651755006,
70.9487244102354));
#120181=CARTESIAN_POINT('Ctrl Pts',(-11.2787348981785,88.4952975498514,
70.9591885819396));
#120182=CARTESIAN_POINT('Ctrl Pts',(-11.2781912731431,88.4969213353755,
70.9696827577816));
#120183=CARTESIAN_POINT('Ctrl Pts',(-11.2716782339142,88.5163755145074,
71.0954109242402));
#120184=CARTESIAN_POINT('Ctrl Pts',(-11.2654434724911,88.5345988950427,
71.2254493003095));
#120185=CARTESIAN_POINT('Ctrl Pts',(-11.2596545734534,88.5512377649264,
71.3597739094034));
#120186=CARTESIAN_POINT('Ctrl Pts',(-11.2538656744158,88.5678766348101,
71.4940985184973));
#120187=CARTESIAN_POINT('Ctrl Pts',(-11.2485224827647,88.5829310285231,
71.6327098498418));
#120188=CARTESIAN_POINT('Ctrl Pts',(-11.2438200976684,88.5960223610397,
71.7755378131299));
#120189=CARTESIAN_POINT('Ctrl Pts',(-11.2436977938004,88.5963628522098,
71.7792526114736));
#120190=CARTESIAN_POINT('Ctrl Pts',(-11.2435759269761,88.5967020137289,
71.7829702735955));
#120191=CARTESIAN_POINT('Ctrl Pts',(-11.24345450108,88.5970398387411,71.7866908005161));
#120192=CARTESIAN_POINT('Ctrl Pts',(-11.2393869943549,88.6083562510806,
71.9113204615367));
#120193=CARTESIAN_POINT('Ctrl Pts',(-11.2358131384022,88.618174848028,72.0391681835653));
#120194=CARTESIAN_POINT('Ctrl Pts',(-11.2328618753785,88.6262364573018,
72.1702168260346));
#120195=CARTESIAN_POINT('Ctrl Pts',(-11.230568415286,88.6325012256408,72.2720562179402));
#120196=CARTESIAN_POINT('Ctrl Pts',(-11.2286511898399,88.6377045122625,
72.3758279368693));
#120197=CARTESIAN_POINT('Ctrl Pts',(-11.2271765482226,88.6417149897169,
72.4815052446917));
#120198=CARTESIAN_POINT('Ctrl Pts',(-11.2265151028858,88.6435138753438,
72.5289064312825));
#120199=CARTESIAN_POINT('Ctrl Pts',(-11.2259411261284,88.6450737693633,
72.5766912940998));
#120200=CARTESIAN_POINT('Ctrl Pts',(-11.2254612012353,88.6463821040866,
72.6248588574509));
#120201=CARTESIAN_POINT('Ctrl Pts',(-11.2246971786375,88.6484649243536,
72.7015398285955));
#120202=CARTESIAN_POINT('Ctrl Pts',(-11.2241715349995,88.6499103101457,
72.7791910010726));
#120203=CARTESIAN_POINT('Ctrl Pts',(-11.2239031859301,88.6506695009302,
72.8578011864478));
#120204=CARTESIAN_POINT('Ctrl Pts',(-11.2236847289416,88.6512875412042,
72.9217959839446));
#120205=CARTESIAN_POINT('Ctrl Pts',(-11.2236380328797,88.6514499822571,
72.9864269822321));
#120206=CARTESIAN_POINT('Ctrl Pts',(-11.2237716537321,88.6511304616044,
73.0516886702974));
#120207=CARTESIAN_POINT('Ctrl Pts',(-11.2238384641583,88.650970701278,73.08431951433));
#120208=CARTESIAN_POINT('Ctrl Pts',(-11.2239503458186,88.6506904384363,
73.1171080311107));
#120209=CARTESIAN_POINT('Ctrl Pts',(-11.2241082420675,88.6502863510213,
73.1500534666971));
#120210=CARTESIAN_POINT('Ctrl Pts',(-11.224187190192,88.6500843073138,73.1665261844903));
#120211=CARTESIAN_POINT('Ctrl Pts',(-11.2242776414149,88.6498513066299,
73.1830381320236));
#120212=CARTESIAN_POINT('Ctrl Pts',(-11.2243797195615,88.6495869224374,
73.199589213211));
#120213=CARTESIAN_POINT('Ctrl Pts',(-11.2244562781714,88.6493886342931,
73.2120025241015));
#120214=CARTESIAN_POINT('Ctrl Pts',(-11.2245393768795,88.6491726928545,
73.2244378476724));
#120215=CARTESIAN_POINT('Ctrl Pts',(-11.2246290659167,88.6489389176174,
73.2368951425909));
#120216=CARTESIAN_POINT('Ctrl Pts',(-11.2246589622624,88.6488609925384,
73.2410475742304));
#120217=CARTESIAN_POINT('Ctrl Pts',(-11.2246989706019,88.648756593375,73.2464457864442));
#120218=CARTESIAN_POINT('Ctrl Pts',(-11.2247209535766,88.6486991910242,
73.249359759689));
#120219=CARTESIAN_POINT('Ctrl Pts',(-11.225283848485,88.647229349411,73.3239748072662));
#120220=CARTESIAN_POINT('Ctrl Pts',(-11.2261056322508,88.6450963337197,
73.3999366369867));
#120221=CARTESIAN_POINT('Ctrl Pts',(-11.2272066924712,88.6422313440667,
73.477242239284));
#120222=CARTESIAN_POINT('Ctrl Pts',(-11.2289107443734,88.6377973531025,
73.5968839775064));
#120223=CARTESIAN_POINT('Ctrl Pts',(-11.2312844404146,88.6316110674878,
73.7197465262424));
#120224=CARTESIAN_POINT('Ctrl Pts',(-11.2343707142876,88.6234126405493,
73.8457961686285));
#120225=CARTESIAN_POINT('Ctrl Pts',(-11.2373579946079,88.6154771816569,
73.9678027148938));
#120226=CARTESIAN_POINT('Ctrl Pts',(-11.2410129804589,88.6056565218842,
74.0927953458536));
#120227=CARTESIAN_POINT('Ctrl Pts',(-11.2453674480413,88.593694657795,74.2206993317718));
#120228=CARTESIAN_POINT('Ctrl Pts',(-11.2465166159642,88.590537856131,74.2544538964924));
#120229=CARTESIAN_POINT('Ctrl Pts',(-11.2477144554566,88.5872318178545,
74.2884109730504));
#120230=CARTESIAN_POINT('Ctrl Pts',(-11.2489614488936,88.583771599319,74.3225686294004));
#120231=CARTESIAN_POINT('Ctrl Pts',(-11.2507210899968,88.5788888609015,
74.3707687356094));
#120232=CARTESIAN_POINT('Ctrl Pts',(-11.2525786286889,88.5736991271919,
74.4193682627737));
#120233=CARTESIAN_POINT('Ctrl Pts',(-11.2545339242869,88.5681887007774,
74.4683632121842));
#120234=CARTESIAN_POINT('Ctrl Pts',(-11.2597788893554,88.5534073070655,
74.5997892730114));
#120235=CARTESIAN_POINT('Ctrl Pts',(-11.2657233837533,88.5363226200422,
74.7340741379433));
#120236=CARTESIAN_POINT('Ctrl Pts',(-11.2723313215113,88.5166659063121,
74.8711490314704));
#120237=CARTESIAN_POINT('Ctrl Pts',(-11.2766411116037,88.5038455207116,
74.960551208014));
#120238=CARTESIAN_POINT('Ctrl Pts',(-11.2812327478108,88.4899305955625,
75.0511394324114));
#120239=CARTESIAN_POINT('Ctrl Pts',(-11.2860912678808,88.4748414623636,
75.1428849073909));
#120240=CARTESIAN_POINT('Ctrl Pts',(-11.2862257893454,88.4744236782919,
75.1454251327036));
#120241=CARTESIAN_POINT('Ctrl Pts',(-11.2863605151317,88.4740049937973,
75.1479662446589));
#120242=CARTESIAN_POINT('Ctrl Pts',(-11.2864954448362,88.473585407131,75.1505082428964));
#120243=CARTESIAN_POINT('Ctrl Pts',(-11.2927354812477,88.4541809617887,
75.2680669496431));
#120244=CARTESIAN_POINT('Ctrl Pts',(-11.2994101983583,88.4328491779489,
75.3875253915086));
#120245=CARTESIAN_POINT('Ctrl Pts',(-11.3064600273543,88.4094230288148,
75.5088220006582));
#120246=CARTESIAN_POINT('Ctrl Pts',(-11.3099849418523,88.3977099542478,
75.569470305233));
#120247=CARTESIAN_POINT('Ctrl Pts',(-11.3136033503414,88.3854731719582,
75.6305780279337));
#120248=CARTESIAN_POINT('Ctrl Pts',(-11.3173060099884,88.3726910795556,
75.6921366923697));
#120249=CARTESIAN_POINT('Ctrl Pts',(-11.3191573398119,88.3663000333544,
75.7229160245877));
#120250=CARTESIAN_POINT('Ctrl Pts',(-11.3210297220361,88.3597726445926,
75.7538080897276));
#120251=CARTESIAN_POINT('Ctrl Pts',(-11.3229218713195,88.3531061736548,
75.7848117696022));
#120252=CARTESIAN_POINT('Ctrl Pts',(-11.3238679459612,88.349772938186,75.8003136095394));
#120253=CARTESIAN_POINT('Ctrl Pts',(-11.3248189616925,88.3464049311971,
75.8158433529954));
#120254=CARTESIAN_POINT('Ctrl Pts',(-11.3257747517608,88.343001805872,75.8314008579735));
#120255=CARTESIAN_POINT('Ctrl Pts',(-11.3262526467949,88.3413002432095,
75.8391796104625));
#120256=CARTESIAN_POINT('Ctrl Pts',(-11.3267317353696,88.3395899009004,
75.8469653033204));
#120257=CARTESIAN_POINT('Ctrl Pts',(-11.3272119959038,88.3378707356376,
75.8547579182132));
#120258=CARTESIAN_POINT('Ctrl Pts',(-11.3275721913045,88.3365813616905,
75.8606023793827));
#120259=CARTESIAN_POINT('Ctrl Pts',(-11.3279330459287,88.3352870248267,
75.8664507341958));
#120260=CARTESIAN_POINT('Ctrl Pts',(-11.3282945501904,88.333987707079,75.8723029743145));
#120261=CARTESIAN_POINT('Ctrl Pts',(-11.328415051611,88.3335546011631,75.8742537210207));
#120262=CARTESIAN_POINT('Ctrl Pts',(-11.328446700373,88.3334409900833,75.8747664148878));
#120263=CARTESIAN_POINT('Ctrl Pts',(-11.3286562706676,88.3326867283402,
75.8781565092706));
#120264=CARTESIAN_POINT('Ctrl Pts',(-11.3299318021828,88.3280959793215,
75.8987900262188));
#120265=CARTESIAN_POINT('Ctrl Pts',(-11.3312032512804,88.3234824888511,
75.919300324912));
#120266=CARTESIAN_POINT('Ctrl Pts',(-11.3324701252167,88.3188478348224,
75.9396874271587));
#120267=CARTESIAN_POINT('Ctrl Pts',(-11.3417138987592,88.2850309797587,
76.0884423671338));
#120268=CARTESIAN_POINT('Ctrl Pts',(-11.3507102095,88.2500896582609,76.2306380982602));
#120269=CARTESIAN_POINT('Ctrl Pts',(-11.3593111082457,88.2146061164511,
76.3663372416437));
#120270=CARTESIAN_POINT('Ctrl Pts',(-11.3678698694557,88.1792964156612,
76.5013715675851));
#120271=CARTESIAN_POINT('Ctrl Pts',(-11.3760375905093,88.1434498786598,
76.6299731632938));
#120272=CARTESIAN_POINT('Ctrl Pts',(-11.3837111937169,88.1076119442604,
76.752204866115));
#120273=CARTESIAN_POINT('Ctrl Pts',(-11.3894955324291,88.0805974185279,
76.844342751195));
#120274=CARTESIAN_POINT('Ctrl Pts',(-11.3950002586896,88.0535870781357,
76.9328614131808));
#120275=CARTESIAN_POINT('Ctrl Pts',(-11.4002002457319,88.0268001149174,
77.0177900264554));
#120276=CARTESIAN_POINT('Ctrl Pts',(-11.4074220590762,87.9895980129032,
77.1357400497272));
#120277=CARTESIAN_POINT('Ctrl Pts',(-11.4140599832157,87.9528283661577,
77.246756436065));
#120278=CARTESIAN_POINT('Ctrl Pts',(-11.4201245213447,87.9169885962003,
77.3509667338731));
#120279=CARTESIAN_POINT('Ctrl Pts',(-11.4256842951077,87.8841318462804,
77.4465033876583));
#120280=CARTESIAN_POINT('Ctrl Pts',(-11.4307626968668,87.8520562688905,
77.536319548865));
#120281=CARTESIAN_POINT('Ctrl Pts',(-11.4353816424501,87.8211137905606,
77.620495962014));
#120282=CARTESIAN_POINT('Ctrl Pts',(-11.4396640130432,87.7924260398857,
77.6985385779736));
#120283=CARTESIAN_POINT('Ctrl Pts',(-11.4435520003413,87.7647119833415,
77.7717331729491));
#120284=CARTESIAN_POINT('Ctrl Pts',(-11.4470732780468,87.7382271402767,
77.8401291250943));
#120285=CARTESIAN_POINT('Ctrl Pts',(-11.4510911140927,87.7080074967171,
77.9181700366335));
#120286=CARTESIAN_POINT('Ctrl Pts',(-11.454635220842,87.6793846231229,77.9899704189875));
#120287=CARTESIAN_POINT('Ctrl Pts',(-11.4577639818982,87.6526652121703,
78.0556405133578));
#120288=CARTESIAN_POINT('Ctrl Pts',(-11.4608616360046,87.6262114524958,
78.1206576987048));
#120289=CARTESIAN_POINT('Ctrl Pts',(-11.4635523479143,87.6016234909309,
78.1796659293152));
#120290=CARTESIAN_POINT('Ctrl Pts',(-11.4658912623909,87.5791543275422,
78.2327480152614));
#120291=CARTESIAN_POINT('Ctrl Pts',(-11.4679294546614,87.5595741010736,
78.2790051564945));
#120292=CARTESIAN_POINT('Ctrl Pts',(-11.469700537194,87.5416022097708,78.3207617484193));
#120293=CARTESIAN_POINT('Ctrl Pts',(-11.4712385085672,87.5253779368081,
78.3580569175926));
#120294=CARTESIAN_POINT('Ctrl Pts',(-11.4729736282064,87.50707391949,78.4001328506095));
#120295=CARTESIAN_POINT('Ctrl Pts',(-11.4744132374809,87.4909913920126,
78.4365382864589));
#120296=CARTESIAN_POINT('Ctrl Pts',(-11.4755981275821,87.4772798964043,
78.4673325524168));
#120297=CARTESIAN_POINT('Ctrl Pts',(-11.4761496383669,87.4708978381051,
78.4816658393345));
#120298=CARTESIAN_POINT('Ctrl Pts',(-11.4766458711987,87.4650288268202,
78.4947831205361));
#120299=CARTESIAN_POINT('Ctrl Pts',(-11.4770904055706,87.4596846443869,
78.5066884459327));
#120300=CARTESIAN_POINT('Ctrl Pts',(-11.4777902013847,87.4512717145153,
78.5254300717866));
#120301=CARTESIAN_POINT('Ctrl Pts',(-11.4783617801018,87.444159905083,78.5411694292968));
#120302=CARTESIAN_POINT('Ctrl Pts',(-11.4788156162087,87.4383839488606,
78.5539203953817));
#120303=CARTESIAN_POINT('Ctrl Pts',(-11.478862614163,87.437785807545,78.5552408485389));
#120304=CARTESIAN_POINT('Ctrl Pts',(-11.4789083435246,87.4372019824694,
78.5565292493966));
#120305=CARTESIAN_POINT('Ctrl Pts',(-11.4789528140825,87.436632503541,78.5577856107489));
#120306=CARTESIAN_POINT('Ctrl Pts',(-11.4791230586672,87.4344523936397,
78.5625952809352));
#120307=CARTESIAN_POINT('Ctrl Pts',(-11.4792748598656,87.4324825592293,
78.5669354103097));
#120308=CARTESIAN_POINT('Ctrl Pts',(-11.4794087272775,87.4307244748754,
78.5708065929922));
#120309=CARTESIAN_POINT('Ctrl Pts',(-11.4794931451181,87.429615813083,78.5732477911756));
#120310=CARTESIAN_POINT('Ctrl Pts',(-11.479570424627,87.4285913534853,78.5755025046763));
#120311=CARTESIAN_POINT('Ctrl Pts',(-11.4796406605466,87.427651407994,78.5775708598944));
#120312=CARTESIAN_POINT('Ctrl Pts',(-11.4796757785065,87.4271814352483,
78.5786050375034));
#120313=CARTESIAN_POINT('Ctrl Pts',(-11.4797091350718,87.4267325904039,
78.5795926252744));
#120314=CARTESIAN_POINT('Ctrl Pts',(-11.4797407407133,87.4263049075492,
78.5805336370791));
#120315=CARTESIAN_POINT('Ctrl Pts',(-11.4797644449444,87.4259841454082,
78.5812393959326));
#120316=CARTESIAN_POINT('Ctrl Pts',(-11.4797871642159,87.4256752867183,
78.581918955712));
#120317=CARTESIAN_POINT('Ctrl Pts',(-11.4798088218001,87.4253793424745,
78.5825701418522));
#120318=CARTESIAN_POINT('Ctrl Pts',(-11.4798160409948,87.4252806943932,
78.582787203899));
#120319=CARTESIAN_POINT('Ctrl Pts',(-11.4798231963261,87.4251831259764,
78.5830021359438));
#120320=CARTESIAN_POINT('Ctrl Pts',(-11.479872260988,87.42451004271,78.584482751014));
#120321=CARTESIAN_POINT('Ctrl Pts',(-11.4874249839525,87.3208995980584,
78.8123998504856));
#120322=CARTESIAN_POINT('Ctrl Pts',(-11.4924355150551,87.2125152025755,
79.0349269405381));
#120323=CARTESIAN_POINT('Ctrl Pts',(-11.4946370187129,87.0998930412592,
79.2520671402321));
#120324=CARTESIAN_POINT('Ctrl Pts',(-11.495653919499,87.0478715222575,79.3523667872323));
#120325=CARTESIAN_POINT('Ctrl Pts',(-11.4960714579233,86.9949456985302,
79.4515163260804));
#120326=CARTESIAN_POINT('Ctrl Pts',(-11.4958632283546,86.9411677295198,
79.5495124210284));
#120327=CARTESIAN_POINT('Ctrl Pts',(-11.4953780111862,86.8158541440381,
79.7778632168492));
#120328=CARTESIAN_POINT('Ctrl Pts',(-11.4914957997757,86.685916172962,79.9999533966771));
#120329=CARTESIAN_POINT('Ctrl Pts',(-11.4839750065312,86.5521807765044,
80.2155247870291));
#120330=CARTESIAN_POINT('Ctrl Pts',(-11.4796020617359,86.4744206936407,
80.3408681861652));
#120331=CARTESIAN_POINT('Ctrl Pts',(-11.4739987782135,86.3953761413322,
80.4640069290554));
#120332=CARTESIAN_POINT('Ctrl Pts',(-11.4671164242811,86.3152043383839,
80.5848843774298));
#120333=CARTESIAN_POINT('Ctrl Pts',(-11.4653349240774,86.2944518335455,
80.6161735556695));
#120334=CARTESIAN_POINT('Ctrl Pts',(-11.4634677184249,86.2736237791093,
80.647311198389));
#120335=CARTESIAN_POINT('Ctrl Pts',(-11.4615142713744,86.2527237865284,
80.6782958810632));
#120336=CARTESIAN_POINT('Ctrl Pts',(-11.4531193396924,86.1629061434915,
80.8114524435487));
#120337=CARTESIAN_POINT('Ctrl Pts',(-11.4432055498831,86.0717204867096,
80.9417551760528));
#120338=CARTESIAN_POINT('Ctrl Pts',(-11.4316032617844,85.9793810212328,
81.069299429788));
#120339=CARTESIAN_POINT('Ctrl Pts',(-11.4201568371083,85.8882820304799,
81.1951302728799));
#120340=CARTESIAN_POINT('Ctrl Pts',(-11.4070668735547,85.7960595052786,
81.3182766347454));
#120341=CARTESIAN_POINT('Ctrl Pts',(-11.3921616073703,85.7028924985339,
81.4387882806349));
#120342=CARTESIAN_POINT('Ctrl Pts',(-11.383513739806,85.6488380505474,81.5087077802744));
#120343=CARTESIAN_POINT('Ctrl Pts',(-11.374254648862,85.5944652161075,81.5777395744793));
#120344=CARTESIAN_POINT('Ctrl Pts',(-11.3643496044752,85.5398057770639,
81.6458860450783));
#120345=CARTESIAN_POINT('Ctrl Pts',(-11.3478951255173,85.4490043071802,
81.7590924702823));
#120346=CARTESIAN_POINT('Ctrl Pts',(-11.3296580331722,85.3574121697646,
81.869858575104));
#120347=CARTESIAN_POINT('Ctrl Pts',(-11.3095049384425,85.265214975612,81.9781604293505));
#120348=CARTESIAN_POINT('Ctrl Pts',(-11.2900334836182,85.1761361753112,
82.0827991804025));
#120349=CARTESIAN_POINT('Ctrl Pts',(-11.2687732012478,85.0864920261908,
82.1851377113581));
#120350=CARTESIAN_POINT('Ctrl Pts',(-11.2456039676521,84.9964467274536,
82.2851060442717));
#120351=CARTESIAN_POINT('Ctrl Pts',(-11.2368017735046,84.9622377322241,
82.3230848868289));
#120352=CARTESIAN_POINT('Ctrl Pts',(-11.2277240798479,84.9279708452815,
82.3607211144414));
#120353=CARTESIAN_POINT('Ctrl Pts',(-11.2183644203191,84.8936551814217,
82.3980088913849));
#120354=CARTESIAN_POINT('Ctrl Pts',(-8.11806431796091,89.5255017784999,
61.00149777281));
#120355=CARTESIAN_POINT('Ctrl Pts',(-8.07086318655591,89.37752140552,60.86342605855));
#120356=CARTESIAN_POINT('Ctrl Pts',(-7.93861582162591,88.95570109335,60.48379909532));
#120357=CARTESIAN_POINT('Ctrl Pts',(-7.71230074227791,88.19557981969,59.86550662082));
#120358=CARTESIAN_POINT('Ctrl Pts',(-7.43411667443291,87.18478569849,59.14981124117));
#120359=CARTESIAN_POINT('Ctrl Pts',(-7.17722923208391,86.15427442674,58.52679204685));
#120360=CARTESIAN_POINT('Ctrl Pts',(-7.01884060245691,85.45023623237,58.15949863958));
#120361=CARTESIAN_POINT('Ctrl Pts',(-6.9550272838599,85.15303793274,58.01394630623));
#120362=CARTESIAN_POINT('Ctrl Pts',(-8.41171488046691,87.73463689348,62.37124535609));
#120363=CARTESIAN_POINT('Ctrl Pts',(-8.37908848527591,87.6027656137199,
62.25111048357));
#120364=CARTESIAN_POINT('Ctrl Pts',(-8.28772302885891,87.22733283713,61.92093632006));
#120365=CARTESIAN_POINT('Ctrl Pts',(-8.13158722580592,86.55302576817,61.38366585189));
#120366=CARTESIAN_POINT('Ctrl Pts',(-7.93999671396091,85.65985867277,60.76212250409));
#120367=CARTESIAN_POINT('Ctrl Pts',(-7.76337792118091,84.7525457800201,
60.22102525981));
#120368=CARTESIAN_POINT('Ctrl Pts',(-7.65463361368691,84.13424336598,59.90180878916));
#120369=CARTESIAN_POINT('Ctrl Pts',(-7.61084293435091,83.8734594803,59.77525700745));
#120370=CARTESIAN_POINT('Ctrl Pts',(-9.60752426142491,86.06445447859,63.346010094274));
#120371=CARTESIAN_POINT('Ctrl Pts',(-9.58707518654291,85.94854941245,63.238292826413));
#120372=CARTESIAN_POINT('Ctrl Pts',(-9.52982036816891,85.61888897018,62.94230156249));
#120373=CARTESIAN_POINT('Ctrl Pts',(-9.43202271378591,85.02829664499,62.46078605318));
#120374=CARTESIAN_POINT('Ctrl Pts',(-9.31208721147991,84.24836667598,61.90361036938));
#120375=CARTESIAN_POINT('Ctrl Pts',(-9.2015883596909,83.45823035843,61.41806587424));
#120376=CARTESIAN_POINT('Ctrl Pts',(-9.13358660596391,82.92076056578,61.13119207966));
#120377=CARTESIAN_POINT('Ctrl Pts',(-9.10620724839091,82.69420059489,61.01737706409));
#120378=CARTESIAN_POINT('Ctrl Pts',(-11.4777715891229,84.83301140937,63.740165181442));
#120379=CARTESIAN_POINT('Ctrl Pts',(-11.4647834620949,84.72988919255,63.636981566655));
#120380=CARTESIAN_POINT('Ctrl Pts',(-11.4283722400189,84.43666934708,63.353393769986));
#120381=CARTESIAN_POINT('Ctrl Pts',(-11.3659621319769,83.91175030367,62.89174862045));
#120382=CARTESIAN_POINT('Ctrl Pts',(-11.2890976560299,83.21910354186,62.35689854292));
#120383=CARTESIAN_POINT('Ctrl Pts',(-11.2179786564239,82.51780777718,61.88995855165));
#120384=CARTESIAN_POINT('Ctrl Pts',(-11.1740589850739,82.04087429545,61.61353407859));
#120385=CARTESIAN_POINT('Ctrl Pts',(-11.1563543840809,81.83983039734,61.50376655049));
#120386=CARTESIAN_POINT('',(-10.512461378761,82.2723685552168,61.3874899937114));
#120387=CARTESIAN_POINT('Ctrl Pts',(-7.08823084473591,85.17401267208,58.34042080741));
#120388=CARTESIAN_POINT('Ctrl Pts',(-7.69416668359522,84.0874238004884,
59.7681360479894));
#120389=CARTESIAN_POINT('Ctrl Pts',(-8.88950038744297,83.0746581634291,
60.8319656797966));
#120390=CARTESIAN_POINT('Ctrl Pts',(-10.5124612559679,82.2723684529,61.38749020456));
#120391=CARTESIAN_POINT('Ctrl Pts',(-10.5124593301194,82.2723668470766,
61.3874935123221));
#120392=CARTESIAN_POINT('Ctrl Pts',(-10.543406490679,82.3908668412531,61.463039940396));
#120393=CARTESIAN_POINT('Ctrl Pts',(-10.5743387198586,82.5083084983807,
61.5405397185248));
#120394=CARTESIAN_POINT('Ctrl Pts',(-10.6051932668095,82.6246361406724,
61.6199953153426));
#120395=CARTESIAN_POINT('Ctrl Pts',(-10.6136794284811,82.656630620479,61.6418485949057));
#120396=CARTESIAN_POINT('Ctrl Pts',(-10.6221596942608,82.6885410365736,
61.6638499155315));
#120397=CARTESIAN_POINT('Ctrl Pts',(-10.630632339241,82.7203668208188,61.6859993897178));
#120398=CARTESIAN_POINT('Ctrl Pts',(-10.6529650963324,82.8042553244039,
61.744382436318));
#120399=CARTESIAN_POINT('Ctrl Pts',(-10.6752448489044,82.8875557846347,
61.8037947274344));
#120400=CARTESIAN_POINT('Ctrl Pts',(-10.6974393984954,82.9702651978949,
61.864241507277));
#120401=CARTESIAN_POINT('Ctrl Pts',(-10.7280541596352,83.0843530698112,
61.9476207044518));
#120402=CARTESIAN_POINT('Ctrl Pts',(-10.7585068118979,83.1973152513338,
62.0329678195663));
#120403=CARTESIAN_POINT('Ctrl Pts',(-10.7887320955408,83.3091128864989,
62.120290979857));
#120404=CARTESIAN_POINT('Ctrl Pts',(-10.805119581979,83.3697271143666,62.1676356837782));
#120405=CARTESIAN_POINT('Ctrl Pts',(-10.821440176059,83.4299988418,62.2155610749663));
#120406=CARTESIAN_POINT('Ctrl Pts',(-10.8376847347992,83.4899230304163,
62.2640698043313));
#120407=CARTESIAN_POINT('Ctrl Pts',(-10.8514018420793,83.5405237599943,
62.3050311782514));
#120408=CARTESIAN_POINT('Ctrl Pts',(-10.8650647364673,83.5908766852467,
62.3464084936124));
#120409=CARTESIAN_POINT('Ctrl Pts',(-10.8786677705792,83.6409782943706,
62.388202788185));
#120410=CARTESIAN_POINT('Ctrl Pts',(-10.9083802716627,83.7504130060041,
62.4794922029256));
#120411=CARTESIAN_POINT('Ctrl Pts',(-10.9378074291972,83.8586494099304,
62.5727717257789));
#120412=CARTESIAN_POINT('Ctrl Pts',(-10.9668956205255,83.9656424031755,
62.668049909996));
#120413=CARTESIAN_POINT('Ctrl Pts',(-10.9832012273164,84.0256181389489,
62.7214588205074));
#120414=CARTESIAN_POINT('Ctrl Pts',(-10.9994002846426,84.0852032442459,
62.7754957722232));
#120415=CARTESIAN_POINT('Ctrl Pts',(-11.0154847086497,84.1443887642205,
62.8301624013932));
#120416=CARTESIAN_POINT('Ctrl Pts',(-11.0280938996011,84.1907865415108,
62.8730176485303));
#120417=CARTESIAN_POINT('Ctrl Pts',(-11.0406326443985,84.2369387500661,
62.9162598687448));
#120418=CARTESIAN_POINT('Ctrl Pts',(-11.053097041941,84.28284136205,62.9598897456861));
#120419=CARTESIAN_POINT('Ctrl Pts',(-11.0814611634103,84.3872978556447,
63.0591743781783));
#120420=CARTESIAN_POINT('Ctrl Pts',(-11.1094404699311,84.4904615396237,
63.1604663878809));
#120421=CARTESIAN_POINT('Ctrl Pts',(-11.1369965900705,84.5922821735986,
63.2637770344675));
#120422=CARTESIAN_POINT('Ctrl Pts',(-11.1465313985047,84.6275135572145,
63.2995239835819));
#120423=CARTESIAN_POINT('Ctrl Pts',(-11.1560154863109,84.6625839225875,
63.3355123900509));
#120424=CARTESIAN_POINT('Ctrl Pts',(-11.1654475910058,84.6974913707312,
63.3717431191836));
#120425=CARTESIAN_POINT('Ctrl Pts',(-11.1832747870022,84.7634683652532,
63.440221187465));
#120426=CARTESIAN_POINT('Ctrl Pts',(-11.2009162748768,84.8288634066181,
63.5095649076378));
#120427=CARTESIAN_POINT('Ctrl Pts',(-11.2183629288857,84.8936604424237,
63.579776231348));
#120428=CARTESIAN_POINT('Ctrl Pts',(-7.03190132372392,85.51125736721,58.19041163275));
#120429=CARTESIAN_POINT('Ctrl Pts',(-6.87538499773691,84.764785848,57.82043934909));
#120430=CARTESIAN_POINT('Ctrl Pts',(-6.44219525692591,82.7628240863,57.00605633808));
#120431=CARTESIAN_POINT('Ctrl Pts',(-5.81802729707191,79.11947090448,56.20016572671));
#120432=CARTESIAN_POINT('Ctrl Pts',(-5.65466277323091,76.16634624041,56.0230347830401));
#120433=CARTESIAN_POINT('Ctrl Pts',(-5.66377280626991,74.75743685423,56.03448007748));
#120434=CARTESIAN_POINT('Ctrl Pts',(-7.61749008897591,84.28355049495,59.80517876415));
#120435=CARTESIAN_POINT('Ctrl Pts',(-7.51101338340191,83.61653066378,59.4773129480801));
#120436=CARTESIAN_POINT('Ctrl Pts',(-7.21262854088391,81.83570965308,58.75816327819));
#120437=CARTESIAN_POINT('Ctrl Pts',(-6.77170475316191,78.62276514827,58.0435574767001));
#120438=CARTESIAN_POINT('Ctrl Pts',(-6.65471902994991,76.02576985881,57.88508025476));
#120439=CARTESIAN_POINT('Ctrl Pts',(-6.66121106065891,74.78666667996,57.89523984334));
#120440=CARTESIAN_POINT('Ctrl Pts',(-8.94180740140891,83.14051916281,60.98727660285));
#120441=CARTESIAN_POINT('Ctrl Pts',(-8.87314584653491,82.53616876214,60.67745020954));
#120442=CARTESIAN_POINT('Ctrl Pts',(-8.67972691500492,80.94176301112,60.00417372484));
#120443=CARTESIAN_POINT('Ctrl Pts',(-8.39095356268692,78.1327640109401,
59.34163189448));
#120444=CARTESIAN_POINT('Ctrl Pts',(-8.31392121950591,75.88722716423,59.1942394639501));
#120445=CARTESIAN_POINT('Ctrl Pts',(-8.31818786704791,74.81548246347,59.20357187645));
#120446=CARTESIAN_POINT('Ctrl Pts',(-10.7849819612819,82.27193645786,61.5404460002401));
#120447=CARTESIAN_POINT('Ctrl Pts',(-10.7356327836559,81.7030684661301,
61.22159696902));
#120448=CARTESIAN_POINT('Ctrl Pts',(-10.5999136901219,80.22940267629,60.53721736543));
#120449=CARTESIAN_POINT('Ctrl Pts',(-10.4069360860469,77.73082049296,59.87887468695));
#120450=CARTESIAN_POINT('Ctrl Pts',(-10.3567983965849,75.77371986632,59.73315775232));
#120451=CARTESIAN_POINT('Ctrl Pts',(-10.3596017519129,74.83910003127,59.74225885137));
#120452=CARTESIAN_POINT('',(-9.07718749310076,74.9999295892969,59.2746757754477));
#120453=CARTESIAN_POINT('Origin',(-12.2732112378425,74.9974087405852,52.48990049032));
#120454=CARTESIAN_POINT('Ctrl Pts',(-9.07715892555296,74.9999296085943,
59.2747363757378));
#120455=CARTESIAN_POINT('Ctrl Pts',(-9.0773126974457,75.1671390338749,59.2747599925217));
#120456=CARTESIAN_POINT('Ctrl Pts',(-9.08051136250148,75.3329507230294,
59.2778799903799));
#120457=CARTESIAN_POINT('Ctrl Pts',(-9.08649604199268,75.4971005092912,
59.2839019342157));
#120458=CARTESIAN_POINT('Ctrl Pts',(-9.09252940111275,75.6625854966585,
59.28997286079));
#120459=CARTESIAN_POINT('Ctrl Pts',(-9.10139410251057,75.8263814458647,
59.2989929030652));
#120460=CARTESIAN_POINT('Ctrl Pts',(-9.11282405185339,75.988270808707,59.3107655533047));
#120461=CARTESIAN_POINT('Ctrl Pts',(-9.12433014853199,76.1512386928359,
59.3226166339837));
#120462=CARTESIAN_POINT('Ctrl Pts',(-9.13843563623841,76.3122745930102,
59.3372568966318));
#120463=CARTESIAN_POINT('Ctrl Pts',(-9.15487070829253,76.4712093978363,
59.3544920669801));
#120464=CARTESIAN_POINT('Ctrl Pts',(-9.17152592658787,76.6322731193941,
59.3719581008109));
#120465=CARTESIAN_POINT('Ctrl Pts',(-9.19057342413913,76.7911791731002,
59.3920887946037));
#120466=CARTESIAN_POINT('Ctrl Pts',(-9.21173623755204,76.9478043091153,
59.4146917667016));
#120467=CARTESIAN_POINT('Ctrl Pts',(-9.22410595925357,77.0393521249075,
59.4279032650512));
#120468=CARTESIAN_POINT('Ctrl Pts',(-9.23719844767898,77.1301216611817,
59.441959603078));
#120469=CARTESIAN_POINT('Ctrl Pts',(-9.25095924211316,77.220096231446,59.4568243459834));
#120470=CARTESIAN_POINT('Ctrl Pts',(-9.27408310622116,77.371290971395,59.4818033031643));
#120471=CARTESIAN_POINT('Ctrl Pts',(-9.29906497055013,77.5203598017278,
59.5090624155835));
#120472=CARTESIAN_POINT('Ctrl Pts',(-9.32559640764624,77.667196408224,59.5384134796225));
#120473=CARTESIAN_POINT('Ctrl Pts',(-9.3361603318799,77.7256617970431,59.5501000842931));
#120474=CARTESIAN_POINT('Ctrl Pts',(-9.34696997058316,77.7837738708436,
59.5621184464069));
#120475=CARTESIAN_POINT('Ctrl Pts',(-9.35800608221007,77.8415281464316,
59.5744571510943));
#120476=CARTESIAN_POINT('Ctrl Pts',(-9.38679503195127,77.9921867292233,
59.6066440626737));
#120477=CARTESIAN_POINT('Ctrl Pts',(-9.4171239637515,78.1404072099406,59.6410096038375));
#120478=CARTESIAN_POINT('Ctrl Pts',(-9.44860318915678,78.2862101560236,
59.6773564370463));
#120479=CARTESIAN_POINT('Ctrl Pts',(-9.48147161938259,78.4384475093367,
59.7153072867217));
#120480=CARTESIAN_POINT('Ctrl Pts',(-9.5155938823567,78.5880492817324,59.7554178387944));
#120481=CARTESIAN_POINT('Ctrl Pts',(-9.55054446592392,78.7350915048918,
59.7974850672691));
#120482=CARTESIAN_POINT('Ctrl Pts',(-9.58549504949114,78.8821337280512,
59.8395522957438));
#120483=CARTESIAN_POINT('Ctrl Pts',(-9.62127390794191,79.0266168736045,
59.8835761093334));
#120484=CARTESIAN_POINT('Ctrl Pts',(-9.65747512115821,79.1686640000084,
59.9293775568926));
#120485=CARTESIAN_POINT('Ctrl Pts',(-9.69746684112778,79.3255844012029,
59.9799747193148));
#120486=CARTESIAN_POINT('Ctrl Pts',(-9.73789118088399,79.4795137713661,
60.0327000453531));
#120487=CARTESIAN_POINT('Ctrl Pts',(-9.77838369612151,79.6304418625122,
60.0873581744602));
#120488=CARTESIAN_POINT('Ctrl Pts',(-9.81982019060805,79.7848884554185,
60.1432905178108));
#120489=CARTESIAN_POINT('Ctrl Pts',(-9.86132792820858,79.9361925289671,
60.2012468526367));
#120490=CARTESIAN_POINT('Ctrl Pts',(-9.90254234074071,80.0843919819349,
60.261023922613));
#120491=CARTESIAN_POINT('Ctrl Pts',(-9.94567186427043,80.2394778220858,
60.3235786549914));
#120492=CARTESIAN_POINT('Ctrl Pts',(-9.98847998753714,80.3911641286306,
60.3881273608188));
#120493=CARTESIAN_POINT('Ctrl Pts',(-10.0305797986512,80.5395425243068,
60.4544428473998));
#120494=CARTESIAN_POINT('Ctrl Pts',(-10.0464894045399,80.5956150276066,
60.4795036072442));
#120495=CARTESIAN_POINT('Ctrl Pts',(-10.0622981738445,80.6512155761922,
60.5048167286596));
#120496=CARTESIAN_POINT('Ctrl Pts',(-10.0779863609401,80.7063506214463,
60.530370087055));
#120497=CARTESIAN_POINT('Ctrl Pts',(-10.0913829565748,80.7534320274796,
60.5521908371166));
#120498=CARTESIAN_POINT('Ctrl Pts',(-10.1046916356889,80.8001740172076,
60.5741867658278));
#120499=CARTESIAN_POINT('Ctrl Pts',(-10.1179001771309,80.8465822591748,
60.596350058545));
#120500=CARTESIAN_POINT('Ctrl Pts',(-10.1645207022042,81.0103835855924,
60.6745770413171));
#120501=CARTESIAN_POINT('Ctrl Pts',(-10.2098646468677,81.170020639701,60.7548765032126));
#120502=CARTESIAN_POINT('Ctrl Pts',(-10.253655887701,81.3255210281248,60.8369308421171));
#120503=CARTESIAN_POINT('Ctrl Pts',(-10.297629569873,81.4816692561275,60.9193270325686));
#120504=CARTESIAN_POINT('Ctrl Pts',(-10.3400377339496,81.633646677204,61.0034930253945));
#120505=CARTESIAN_POINT('Ctrl Pts',(-10.3806383769278,81.781496485306,61.0890737373057));
#120506=CARTESIAN_POINT('Ctrl Pts',(-10.4213964104706,81.9299194410991,
61.1749862074252));
#120507=CARTESIAN_POINT('Ctrl Pts',(-10.460333076907,82.0741830516942,61.2623246295904));
#120508=CARTESIAN_POINT('Ctrl Pts',(-10.4972387190891,82.2143408245832,
61.3506921725723));
#120509=CARTESIAN_POINT('Ctrl Pts',(-10.5023528212912,82.2337628189614,
61.3629374721917));
#120510=CARTESIAN_POINT('Ctrl Pts',(-10.5074279753542,82.2531059827642,
61.3752024712711));
#120511=CARTESIAN_POINT('Ctrl Pts',(-10.5124636729889,82.2723704679908,
61.3874860534033));
#120512=CARTESIAN_POINT('Ctrl Pts',(-5.66390800190791,75.24262194042,56.03434062129));
#120513=CARTESIAN_POINT('Ctrl Pts',(-5.65535143044491,73.89532137167,56.02321678452));
#120514=CARTESIAN_POINT('Ctrl Pts',(-5.80770736214291,70.97306194622,56.19025779444));
#120515=CARTESIAN_POINT('Ctrl Pts',(-6.42570231125791,67.31182980722,56.97863787701));
#120516=CARTESIAN_POINT('Ctrl Pts',(-6.87092179892391,65.25676291415,57.80972125753));
#120517=CARTESIAN_POINT('Ctrl Pts',(-7.03202707322891,64.48823711687,58.19064865432));
#120518=CARTESIAN_POINT('Ctrl Pts',(-6.66130720700991,75.21338769677,57.89513939594));
#120519=CARTESIAN_POINT('Ctrl Pts',(-6.65520853313191,74.02846944445,57.88529563077));
#120520=CARTESIAN_POINT('Ctrl Pts',(-6.76428610217291,71.45857655335,58.0346520151801));
#120521=CARTESIAN_POINT('Ctrl Pts',(-7.20118402052992,68.23053169304,58.7339902498301));
#120522=CARTESIAN_POINT('Ctrl Pts',(-7.50797933384991,66.4027178495701,
59.46781536177));
#120523=CARTESIAN_POINT('Ctrl Pts',(-7.61757435664191,65.71599759142,59.8053935093701));
#120524=CARTESIAN_POINT('Ctrl Pts',(-8.31825584846591,75.18456566475,59.2035141051799));
#120525=CARTESIAN_POINT('Ctrl Pts',(-8.31424745200392,74.15969362865,59.19451697865));
#120526=CARTESIAN_POINT('Ctrl Pts',(-8.38606591942392,71.93755190537,59.33332163781));
#120527=CARTESIAN_POINT('Ctrl Pts',(-8.67229006571891,69.11718615321,59.98168191414));
#120528=CARTESIAN_POINT('Ctrl Pts',(-8.87119397702391,67.48125880356,60.6684860693));
#120529=CARTESIAN_POINT('Ctrl Pts',(-8.94186531869191,66.85906807835,60.98748833076));
#120530=CARTESIAN_POINT('Ctrl Pts',(-10.3596548680249,75.16094109459,59.74223855301));
#120531=CARTESIAN_POINT('Ctrl Pts',(-10.3570220852529,74.26720709964,59.73351406686));
#120532=CARTESIAN_POINT('Ctrl Pts',(-10.4037867479779,72.3304649169,59.8706517777));
#120533=CARTESIAN_POINT('Ctrl Pts',(-10.5947763722079,69.82458415487,60.51456172883));
#120534=CARTESIAN_POINT('Ctrl Pts',(-10.7342345947289,68.31331830637,61.21238901141));
#120535=CARTESIAN_POINT('Ctrl Pts',(-10.7850312275449,67.72766743019,61.54067285792));
#120536=CARTESIAN_POINT('',(-10.5124868003233,67.7275732983192,61.3875216938171));
#120537=CARTESIAN_POINT('Origin',(-13.9923414084008,64.825873417259,55.411082747836));
#120538=CARTESIAN_POINT('Ctrl Pts',(-10.5124868003233,67.7275732983192,
61.3875216938171));
#120539=CARTESIAN_POINT('Ctrl Pts',(-10.4762701075093,67.8661449558079,
61.2991658162155));
#120540=CARTESIAN_POINT('Ctrl Pts',(-10.4380003201166,68.0087788126902,
61.211774700065));
#120541=CARTESIAN_POINT('Ctrl Pts',(-10.3978879892869,68.1555292889392,
61.1257495553478));
#120542=CARTESIAN_POINT('Ctrl Pts',(-10.3579054434168,68.3018049484868,
61.0400027482313));
#120543=CARTESIAN_POINT('Ctrl Pts',(-10.3160920568659,68.4521709674743,
60.9556128504399));
#120544=CARTESIAN_POINT('Ctrl Pts',(-10.2726907444907,68.6066715326339,
60.8729398329561));
#120545=CARTESIAN_POINT('Ctrl Pts',(-10.2295860562707,68.7601161712075,
60.7908318401829));
#120546=CARTESIAN_POINT('Ctrl Pts',(-10.1849149375519,68.9176394274009,
60.7104170559603));
#120547=CARTESIAN_POINT('Ctrl Pts',(-10.1389518423473,69.0792695620243,
60.632015160386));
#120548=CARTESIAN_POINT('Ctrl Pts',(-10.1318974355681,69.1040765231818,
60.6199820529292));
#120549=CARTESIAN_POINT('Ctrl Pts',(-10.1248126674201,69.1289801903125,
60.6079963024182));
#120550=CARTESIAN_POINT('Ctrl Pts',(-10.1176986096817,69.1539806243396,
60.5960590019341));
#120551=CARTESIAN_POINT('Ctrl Pts',(-10.0996746444948,69.2173209807338,
60.5658150123203));
#120552=CARTESIAN_POINT('Ctrl Pts',(-10.0814630365437,69.2812783888663,
60.5358835999103));
#120553=CARTESIAN_POINT('Ctrl Pts',(-10.0630957245031,69.3458681631611,
60.5062844575174));
#120554=CARTESIAN_POINT('Ctrl Pts',(-10.0218973231987,69.4907448569128,
60.4398927425039));
#120555=CARTESIAN_POINT('Ctrl Pts',(-9.97991359072972,69.6388059609115,
60.3751724378893));
#120556=CARTESIAN_POINT('Ctrl Pts',(-9.93751542809077,69.7901601866326,
60.312340052335));
#120557=CARTESIAN_POINT('Ctrl Pts',(-9.89646721486002,69.9366953226874,
60.2515082379473));
#120558=CARTESIAN_POINT('Ctrl Pts',(-9.85503061526349,70.0863176266317,
60.1924459147403));
#120559=CARTESIAN_POINT('Ctrl Pts',(-9.81356881089885,70.2390859076572,
60.1353552330375));
#120560=CARTESIAN_POINT('Ctrl Pts',(-9.77350524883942,70.3867022885978,
60.0801898560245));
#120561=CARTESIAN_POINT('Ctrl Pts',(-9.73341830512795,70.5372562897347,
60.0268653562765));
#120562=CARTESIAN_POINT('Ctrl Pts',(-9.69365921584859,70.6907584294202,
59.9755704936241));
#120563=CARTESIAN_POINT('Ctrl Pts',(-9.6815232341654,70.7376131031394,59.9599133564795));
#120564=CARTESIAN_POINT('Ctrl Pts',(-9.66941796029569,70.7847421335854,
59.9444453679735));
#120565=CARTESIAN_POINT('Ctrl Pts',(-9.65735380374282,70.832144941498,59.9291720205939));
#120566=CARTESIAN_POINT('Ctrl Pts',(-9.62200662870135,70.9710320109257,
59.8844221302116));
#120567=CARTESIAN_POINT('Ctrl Pts',(-9.58703153567298,71.1122271274692,
59.8413601076449));
#120568=CARTESIAN_POINT('Ctrl Pts',(-9.55281926379787,71.2558507181445,
59.8001562974858));
#120569=CARTESIAN_POINT('Ctrl Pts',(-9.51916731788748,71.3971220526677,
59.7596273201692));
#120570=CARTESIAN_POINT('Ctrl Pts',(-9.48625349670778,71.54074326782,59.7208963190959));
#120571=CARTESIAN_POINT('Ctrl Pts',(-9.45446673383467,71.6867871682261,
59.6841468622814));
#120572=CARTESIAN_POINT('Ctrl Pts',(-9.42326249685992,71.8301546603858,
59.648070877957));
#120573=CARTESIAN_POINT('Ctrl Pts',(-9.3931445162145,71.9758570705251,59.6139046705913));
#120574=CARTESIAN_POINT('Ctrl Pts',(-9.3644957399514,72.1239188889196,59.5818403151953));
#120575=CARTESIAN_POINT('Ctrl Pts',(-9.35416809263895,72.1772939520209,
59.5702813798051));
#120576=CARTESIAN_POINT('Ctrl Pts',(-9.34403150850522,72.2309751908338,
59.5589957504543));
#120577=CARTESIAN_POINT('Ctrl Pts',(-9.33410436362879,72.2849622223357,
59.5479929451075));
#120578=CARTESIAN_POINT('Ctrl Pts',(-9.3074741014996,72.4297862194032,59.5184771483512));
#120579=CARTESIAN_POINT('Ctrl Pts',(-9.28235075410872,72.5768144578516,
59.4909958965004));
#120580=CARTESIAN_POINT('Ctrl Pts',(-9.25904207989478,72.7259503851478,
59.4657366079965));
#120581=CARTESIAN_POINT('Ctrl Pts',(-9.25620454146715,72.7441058117825,
59.4626616067705));
#120582=CARTESIAN_POINT('Ctrl Pts',(-9.25339390160451,72.7622924121674,
59.4596195469236));
#120583=CARTESIAN_POINT('Ctrl Pts',(-9.25061071951314,72.7805099599108,
59.4566107760049));
#120584=CARTESIAN_POINT('Ctrl Pts',(-9.22695251543498,72.9353666843967,
59.4310349731716));
#120585=CARTESIAN_POINT('Ctrl Pts',(-9.2052828960784,73.0925588459421,59.407856783846));
#120586=CARTESIAN_POINT('Ctrl Pts',(-9.18587503647428,73.2520001394406,
59.3872619276458));
#120587=CARTESIAN_POINT('Ctrl Pts',(-9.16679028054398,73.4087870409176,
59.3670099363382));
#120588=CARTESIAN_POINT('Ctrl Pts',(-9.14989271692039,73.5677489173827,
59.349256203791));
#120589=CARTESIAN_POINT('Ctrl Pts',(-9.13544671220291,73.7287551183742,
59.3341896287712));
#120590=CARTESIAN_POINT('Ctrl Pts',(-9.1211136461013,73.8885025756618,59.3192408439752));
#120591=CARTESIAN_POINT('Ctrl Pts',(-9.10919408187488,74.050262646377,59.3069375774147));
#120592=CARTESIAN_POINT('Ctrl Pts',(-9.0999490525663,74.2138576301041,59.2974733318929));
#120593=CARTESIAN_POINT('Ctrl Pts',(-9.09078225483746,74.3760682705711,
59.2880891729618));
#120594=CARTESIAN_POINT('Ctrl Pts',(-9.08424506901794,74.5400829676146,
59.28149640993));
#120595=CARTESIAN_POINT('Ctrl Pts',(-9.08059270014877,74.7056776060466,
59.2778893465346));
#120596=CARTESIAN_POINT('Ctrl Pts',(-9.07844102510663,74.8032323337834,
59.2757643617476));
#120597=CARTESIAN_POINT('Ctrl Pts',(-9.07729055840808,74.9013344250172,
59.2746756845705));
#120598=CARTESIAN_POINT('Ctrl Pts',(-9.07719325348408,74.9999295853934,
59.2746634979996));
#120599=CARTESIAN_POINT('Ctrl Pts',(-6.95350273443992,64.85427978905,58.01030135259));
#120600=CARTESIAN_POINT('Ctrl Pts',(-7.13804274350491,63.99524524915,58.4306382535));
#120601=CARTESIAN_POINT('Ctrl Pts',(-7.57336514742491,62.21958654223,59.46854577467));
#120602=CARTESIAN_POINT('Ctrl Pts',(-8.29958740449491,59.85356795294,61.46379788794));
#120603=CARTESIAN_POINT('Ctrl Pts',(-9.03398262523491,57.8394554497201,
63.966105684766));
#120604=CARTESIAN_POINT('Ctrl Pts',(-9.65355624003791,56.34001186882,66.835457200394));
#120605=CARTESIAN_POINT('Ctrl Pts',(-10.0603100074489,55.43622922579,69.955066301403));
#120606=CARTESIAN_POINT('Ctrl Pts',(-10.1459643513009,55.25249740592,72.1222089702131));
#120607=CARTESIAN_POINT('Ctrl Pts',(-10.1403726637939,55.26506242224,73.1850262950981));
#120608=CARTESIAN_POINT('Ctrl Pts',(-7.65862076439791,66.22813057212,59.90322577706));
#120609=CARTESIAN_POINT('Ctrl Pts',(-7.78097032738291,65.48218511246,60.2645947192301));
#120610=CARTESIAN_POINT('Ctrl Pts',(-8.06993590988691,63.93605519502,61.15578231356));
#120611=CARTESIAN_POINT('Ctrl Pts',(-8.55437878141292,61.85463455847,62.86927844546));
#120612=CARTESIAN_POINT('Ctrl Pts',(-9.04755438821391,60.05347845777,65.030787886569));
#120613=CARTESIAN_POINT('Ctrl Pts',(-9.46704764745591,58.68556152658,67.535143565041));
#120614=CARTESIAN_POINT('Ctrl Pts',(-9.74468998856591,57.84498149326,70.289989823668));
#120615=CARTESIAN_POINT('Ctrl Pts',(-9.80338789027092,57.6722837132601,
72.2180181904323));
#120616=CARTESIAN_POINT('Ctrl Pts',(-9.79958208940392,57.68401165871,73.1633534773191));
#120617=CARTESIAN_POINT('Ctrl Pts',(-9.31846800108191,67.47735678569,61.18858040015));
#120618=CARTESIAN_POINT('Ctrl Pts',(-9.39099275510391,66.8364283808701,
61.51211508092));
#120619=CARTESIAN_POINT('Ctrl Pts',(-9.56233860701091,65.50564909822,62.30810424059));
#120620=CARTESIAN_POINT('Ctrl Pts',(-9.84998217425491,63.7004966011401,
63.835139422207));
#120621=CARTESIAN_POINT('Ctrl Pts',(-10.1433419235899,62.1191058317,65.7671445554511));
#120622=CARTESIAN_POINT('Ctrl Pts',(-10.3934232529189,60.90047284578,68.021797610286));
#120623=CARTESIAN_POINT('Ctrl Pts',(-10.5592976252989,60.14127553959,70.5237615137681));
#120624=CARTESIAN_POINT('Ctrl Pts',(-10.5944027227179,59.98414788629,72.2848823047987));
#120625=CARTESIAN_POINT('Ctrl Pts',(-10.5921307252349,59.9947625292,73.1482290672144));
#120626=CARTESIAN_POINT('Ctrl Pts',(-11.5725330395007,68.33063207667,61.58719193961));
#120627=CARTESIAN_POINT('Ctrl Pts',(-11.618420347605,67.76383946612,61.90224348891));
#120628=CARTESIAN_POINT('Ctrl Pts',(-11.7264300397956,66.58745946769,62.67523238084));
#120629=CARTESIAN_POINT('Ctrl Pts',(-11.9049983137748,64.99024109106,64.151600128689));
#120630=CARTESIAN_POINT('Ctrl Pts',(-12.0833450737449,63.5876925334,66.015242312359));
#120631=CARTESIAN_POINT('Ctrl Pts',(-12.2314784131961,62.50367698227,68.189720251468));
#120632=CARTESIAN_POINT('Ctrl Pts',(-12.3272037779371,61.82636655584,70.605607204909));
#120633=CARTESIAN_POINT('Ctrl Pts',(-12.3472039606322,61.68596335411,72.308278726365));
#120634=CARTESIAN_POINT('Ctrl Pts',(-12.3458805480338,61.69543026713,73.1429380190955));
#120635=CARTESIAN_POINT('',(-12.1331989796159,61.4797180052465,72.9888456300652));
#120636=CARTESIAN_POINT('Origin',(-17.5675192547456,56.310652416732,72.9886930857116));
#120637=CARTESIAN_POINT('Ctrl Pts',(-12.1332079421933,61.4797094802272,
72.9888456275718));
#120638=CARTESIAN_POINT('Ctrl Pts',(-12.1331653467128,61.4797185453445,
72.8047456110304));
#120639=CARTESIAN_POINT('Ctrl Pts',(-12.1322831197896,61.4832907140384,
72.6175747076454));
#120640=CARTESIAN_POINT('Ctrl Pts',(-12.130481030127,61.4907627280311,72.4274543646988));
#120641=CARTESIAN_POINT('Ctrl Pts',(-12.1287809460169,61.4978117958562,
72.2480956009586));
#120642=CARTESIAN_POINT('Ctrl Pts',(-12.1262621768532,61.5083318721226,
72.066111858343));
#120643=CARTESIAN_POINT('Ctrl Pts',(-12.1228518473085,61.5226310275087,
71.881646620849));
#120644=CARTESIAN_POINT('Ctrl Pts',(-12.1195127607835,61.5366314683583,
71.7010349289953));
#120645=CARTESIAN_POINT('Ctrl Pts',(-12.1153189970978,61.5542547474794,
71.5180441111482));
#120646=CARTESIAN_POINT('Ctrl Pts',(-12.1101965797031,61.5758140946132,
71.3328517672573));
#120647=CARTESIAN_POINT('Ctrl Pts',(-12.1052203638473,61.5967581053765,
71.1529450929197));
#120648=CARTESIAN_POINT('Ctrl Pts',(-12.0993677620032,61.6214167411873,
70.9709606179531));
#120649=CARTESIAN_POINT('Ctrl Pts',(-12.0925653862056,61.6500998120332,
70.7871047536805));
#120650=CARTESIAN_POINT('Ctrl Pts',(-12.0907794318631,61.6576305125496,
70.7388336512086));
#120651=CARTESIAN_POINT('Ctrl Pts',(-12.0889279767352,61.6654387473065,
70.6904337965565));
#120652=CARTESIAN_POINT('Ctrl Pts',(-12.0870096244634,61.6735303884131,
70.641909464666));
#120653=CARTESIAN_POINT('Ctrl Pts',(-12.079323095454,61.7059522928846,70.4474802713318));
#120654=CARTESIAN_POINT('Ctrl Pts',(-12.070562765951,61.742923132194,70.2510489263372));
#120655=CARTESIAN_POINT('Ctrl Pts',(-12.060658636014,61.7847569874742,70.0528399176));
#120656=CARTESIAN_POINT('Ctrl Pts',(-12.0567749820864,61.8011610752028,
69.9751172705682));
#120657=CARTESIAN_POINT('Ctrl Pts',(-12.05271542204,61.8183130693951,69.8971218150545));
#120658=CARTESIAN_POINT('Ctrl Pts',(-12.0484756078765,61.8362325226126,
69.8188692114161));
#120659=CARTESIAN_POINT('Ctrl Pts',(-12.0380219491557,61.8804146120088,
69.6259300917068));
#120660=CARTESIAN_POINT('Ctrl Pts',(-12.0264752882927,61.9292585199403,
69.4314424213465));
#120661=CARTESIAN_POINT('Ctrl Pts',(-12.0137349078255,61.9830342790126,
69.2356607295991));
#120662=CARTESIAN_POINT('Ctrl Pts',(-12.0013924645638,62.0351303884588,
69.0459941471689));
#120663=CARTESIAN_POINT('Ctrl Pts',(-11.9879297021071,62.0918551359694,
68.8551130122815));
#120664=CARTESIAN_POINT('Ctrl Pts',(-11.9732513573392,62.1534679657069,
68.663294660096));
#120665=CARTESIAN_POINT('Ctrl Pts',(-11.9607095382935,62.2061126592121,
68.499396679716));
#120666=CARTESIAN_POINT('Ctrl Pts',(-11.9472801962284,62.2623262340416,
68.3348150750062));
#120667=CARTESIAN_POINT('Ctrl Pts',(-11.9329017126591,62.3222785805898,
68.1697519096999));
#120668=CARTESIAN_POINT('Ctrl Pts',(-11.9309069607861,62.3305958732299,
68.1468524115318));
#120669=CARTESIAN_POINT('Ctrl Pts',(-11.9288939379843,62.3389851359816,
68.1239436899144));
#120670=CARTESIAN_POINT('Ctrl Pts',(-11.9268625115437,62.3474467822139,
68.1010261931419));
#120671=CARTESIAN_POINT('Ctrl Pts',(-11.9083411270276,62.4245952333618,
67.8920775640391));
#120672=CARTESIAN_POINT('Ctrl Pts',(-11.888269059637,62.5077412898931,67.6823915702289));
#120673=CARTESIAN_POINT('Ctrl Pts',(-11.8665135228292,62.5971460438744,
67.4723866003536));
#120674=CARTESIAN_POINT('Ctrl Pts',(-11.8580218723687,62.6320426279955,
67.3904171773559));
#120675=CARTESIAN_POINT('Ctrl Pts',(-11.8492737462824,62.6678927592649,
67.3083997082421));
#120676=CARTESIAN_POINT('Ctrl Pts',(-11.8402612660364,62.704712083059,67.2263612479458));
#120677=CARTESIAN_POINT('Ctrl Pts',(-11.8242100767523,62.7702871433535,
67.0802510963719));
#120678=CARTESIAN_POINT('Ctrl Pts',(-11.8073196299173,62.8389358061581,
66.9340732660924));
#120679=CARTESIAN_POINT('Ctrl Pts',(-11.7895406122778,62.9107434320246,
66.7879889495863));
#120680=CARTESIAN_POINT('Ctrl Pts',(-11.780651103458,62.9466472449579,66.7149467913332));
#120681=CARTESIAN_POINT('Ctrl Pts',(-11.7715393875097,62.9833408625202,
66.641928037025));
#120682=CARTESIAN_POINT('Ctrl Pts',(-11.7621989800699,63.0208346945652,
66.5689541969016));
#120683=CARTESIAN_POINT('Ctrl Pts',(-11.75752877635,63.0395816105878,66.5324672768399));
#120684=CARTESIAN_POINT('Ctrl Pts',(-11.7528013955934,63.058528584409,66.495991587103));
#120685=CARTESIAN_POINT('Ctrl Pts',(-11.7480160038192,63.0776769209298,
66.459529867771));
#120686=CARTESIAN_POINT('Ctrl Pts',(-11.7447595858139,63.0907071994858,
66.4347179808998));
#120687=CARTESIAN_POINT('Ctrl Pts',(-11.7413647584787,63.104273765333,66.4090764859645));
#120688=CARTESIAN_POINT('Ctrl Pts',(-11.738058747514,63.117474192884,66.3843141959879));
#120689=CARTESIAN_POINT('Ctrl Pts',(-11.7365064885483,63.1236721402702,
66.3726876505715));
#120690=CARTESIAN_POINT('Ctrl Pts',(-11.7349738984648,63.129788732834,66.3612544971653));
#120691=CARTESIAN_POINT('Ctrl Pts',(-11.7334849449445,63.1357273297451,
66.3501893914605));
#120692=CARTESIAN_POINT('Ctrl Pts',(-11.7170783789754,63.2011638800877,
66.228264573638));
#120693=CARTESIAN_POINT('Ctrl Pts',(-11.7001633859446,63.2684475221823,
66.1073814441102));
#120694=CARTESIAN_POINT('Ctrl Pts',(-11.6827276781987,63.3375315176884,
65.9876235892416));
#120695=CARTESIAN_POINT('Ctrl Pts',(-11.6455787104538,63.484723656841,65.7324644209088));
#120696=CARTESIAN_POINT('Ctrl Pts',(-11.6060658609039,63.6400899127347,
65.4824168542107));
#120697=CARTESIAN_POINT('Ctrl Pts',(-11.5641140464249,63.8031665788657,
65.2380129164019));
#120698=CARTESIAN_POINT('Ctrl Pts',(-11.5362719517495,63.9113954131643,
65.0758097397329));
#120699=CARTESIAN_POINT('Ctrl Pts',(-11.5073555995864,64.0230198042498,
64.9160914069143));
#120700=CARTESIAN_POINT('Ctrl Pts',(-11.4773432659756,64.1379005967349,
64.7590012547552));
#120701=CARTESIAN_POINT('Ctrl Pts',(-11.4344204221028,64.3022000605408,
64.5343350837563));
#120702=CARTESIAN_POINT('Ctrl Pts',(-11.3892616495029,64.4731513924225,
64.3150645575879));
#120703=CARTESIAN_POINT('Ctrl Pts',(-11.3418451116646,64.6503209328055,
64.1016187216834));
#120704=CARTESIAN_POINT('Ctrl Pts',(-11.3359829404079,64.672224644771,64.075230121816));
#120705=CARTESIAN_POINT('Ctrl Pts',(-11.330086268261,64.6942233854544,64.0489304810118));
#120706=CARTESIAN_POINT('Ctrl Pts',(-11.3241550735596,64.7163164325531,
64.0227202842263));
#120707=CARTESIAN_POINT('Ctrl Pts',(-11.297202057071,64.8167134508116,63.903613780109));
#120708=CARTESIAN_POINT('Ctrl Pts',(-11.269540961379,64.9190583895597,63.7863595421992));
#120709=CARTESIAN_POINT('Ctrl Pts',(-11.2411950260713,65.0232761843867,
63.6710239744486));
#120710=CARTESIAN_POINT('Ctrl Pts',(-11.2270220584174,65.0753850818002,
63.6133561905732));
#120711=CARTESIAN_POINT('Ctrl Pts',(-11.2126779701479,65.1279620983969,
63.5561680134618));
#120712=CARTESIAN_POINT('Ctrl Pts',(-11.1981661560224,65.180997423307,63.4994671916645));
#120713=CARTESIAN_POINT('Ctrl Pts',(-11.1909102489597,65.2075150857621,
63.4711167807659));
#120714=CARTESIAN_POINT('Ctrl Pts',(-11.1836124156156,65.2341473198062,
63.4428882037445));
#120715=CARTESIAN_POINT('Ctrl Pts',(-11.1762731100198,65.260892870629,63.4147823938254));
#120716=CARTESIAN_POINT('Ctrl Pts',(-11.1726034572219,65.2742656460403,
63.4007294888658));
#120717=CARTESIAN_POINT('Ctrl Pts',(-11.1689234366739,65.2876667503186,
63.386707275337));
#120718=CARTESIAN_POINT('Ctrl Pts',(-11.1652331068892,65.3010960251005,
63.372715867342));
#120719=CARTESIAN_POINT('Ctrl Pts',(-11.1624653595506,65.3111679811869,
63.3622223113457));
#120720=CARTESIAN_POINT('Ctrl Pts',(-11.1596918132918,65.3212557831551,
63.3517460834332));
#120721=CARTESIAN_POINT('Ctrl Pts',(-11.1569124932258,65.3313593638241,
63.3412872311077));
#120722=CARTESIAN_POINT('Ctrl Pts',(-11.1559860532039,65.3347272240471,
63.3378009469992));
#120723=CARTESIAN_POINT('Ctrl Pts',(-11.1547187447784,65.3393332299145,
63.3330394727056));
#120724=CARTESIAN_POINT('Ctrl Pts',(-11.1541312495045,65.3414682015608,
63.3308341723723));
#120725=CARTESIAN_POINT('Ctrl Pts',(-11.1294971591335,65.4309890654857,
63.2383643770943));
#120726=CARTESIAN_POINT('Ctrl Pts',(-11.1033515358283,65.5265230289392,
63.1425216544724));
#120727=CARTESIAN_POINT('Ctrl Pts',(-11.07557230204,65.6283774805403,63.0438117051595));
#120728=CARTESIAN_POINT('Ctrl Pts',(-11.0477429559631,65.7304156722586,
62.9449236882476));
#120729=CARTESIAN_POINT('Ctrl Pts',(-11.0182738064181,65.8387973476537,
62.8431580967832));
#120730=CARTESIAN_POINT('Ctrl Pts',(-10.9870532157423,65.9538609854524,
62.7390650122299));
#120731=CARTESIAN_POINT('Ctrl Pts',(-10.9608634381172,66.050383537443,62.6517452441618));
#120732=CARTESIAN_POINT('Ctrl Pts',(-10.9334412612304,66.1516086733662,
62.5627883573703));
#120733=CARTESIAN_POINT('Ctrl Pts',(-10.9047293596841,66.2577508851825,
62.4725416655751));
#120734=CARTESIAN_POINT('Ctrl Pts',(-10.8975383262697,66.2843347110785,
62.4499389488866));
#120735=CARTESIAN_POINT('Ctrl Pts',(-10.8902664379593,66.3112270383585,
62.4272554276655));
#120736=CARTESIAN_POINT('Ctrl Pts',(-10.8829128118355,66.3384311136375,
62.4044967295375));
#120737=CARTESIAN_POINT('Ctrl Pts',(-10.8469819514119,66.4713540846117,
62.2932945019423));
#120738=CARTESIAN_POINT('Ctrl Pts',(-10.80907714389,66.6117098375458,62.1802881568853));
#120739=CARTESIAN_POINT('Ctrl Pts',(-10.7692527638807,66.7598505141739,
62.066267766513));
#120740=CARTESIAN_POINT('Ctrl Pts',(-10.7300594413498,66.9056437523284,
61.9540541442562));
#120741=CARTESIAN_POINT('Ctrl Pts',(-10.6890064797408,67.0589777669139,
61.8408584917643));
#120742=CARTESIAN_POINT('Ctrl Pts',(-10.646176795151,67.2201664659931,61.7274685250017));
#120743=CARTESIAN_POINT('Ctrl Pts',(-10.6058295911207,67.3720123969497,
61.6206508314378));
#120744=CARTESIAN_POINT('Ctrl Pts',(-10.5639055145783,67.530829139225,61.5136609766));
#120745=CARTESIAN_POINT('Ctrl Pts',(-10.5205053048556,67.6968536294708,
61.4071851455753));
#120746=CARTESIAN_POINT('Ctrl Pts',(-10.517834979129,67.7070687752127,61.4006339064762));
#120747=CARTESIAN_POINT('Ctrl Pts',(-10.5151590760853,67.7173111980251,
61.3940846217744));
#120748=CARTESIAN_POINT('Ctrl Pts',(-10.5124776235678,67.7275809493603,
61.3875374546355));
#120749=CARTESIAN_POINT('Ctrl Pts',(-10.1403245269799,55.26504566043,72.7925531866283));
#120750=CARTESIAN_POINT('Ctrl Pts',(-10.1450666807169,55.25428818104,73.6993150005103));
#120751=CARTESIAN_POINT('Ctrl Pts',(-10.0787320679299,55.39759073255,75.731249626262));
#120752=CARTESIAN_POINT('Ctrl Pts',(-9.7171468928169,56.19403365364,78.782525259709));
#120753=CARTESIAN_POINT('Ctrl Pts',(-9.09680907897791,57.67747381634,81.773917000605));
#120754=CARTESIAN_POINT('Ctrl Pts',(-8.34088152741291,59.72748177467,84.39459302725));
#120755=CARTESIAN_POINT('Ctrl Pts',(-7.59054532717091,62.15234847022,86.46774807429));
#120756=CARTESIAN_POINT('Ctrl Pts',(-7.14211997123491,63.97655318543,87.53799401565));
#120757=CARTESIAN_POINT('Ctrl Pts',(-6.95354550483591,64.85417809566,87.96744232501));
#120758=CARTESIAN_POINT('Ctrl Pts',(-9.79955613262591,57.68387140554,72.8142459416047));
#120759=CARTESIAN_POINT('Ctrl Pts',(-9.80277833012592,57.6738396029,73.6207885064451));
#120760=CARTESIAN_POINT('Ctrl Pts',(-9.75736005205691,57.8083505427,75.42855130615));
#120761=CARTESIAN_POINT('Ctrl Pts',(-9.51030405160591,58.55075850748,78.126834664904));
#120762=CARTESIAN_POINT('Ctrl Pts',(-9.08987811173791,59.90727613614,80.7409654777591));
#120763=CARTESIAN_POINT('Ctrl Pts',(-8.58195139340691,61.74310086763,83.00598344105));
#120764=CARTESIAN_POINT('Ctrl Pts',(-8.08130749399791,63.87735771982,84.78648432159));
#120765=CARTESIAN_POINT('Ctrl Pts',(-7.78363606475891,65.46586756939,85.70542531448));
#120766=CARTESIAN_POINT('Ctrl Pts',(-7.65860430020592,66.22796383846,86.07462806762));
#120767=CARTESIAN_POINT('Ctrl Pts',(-10.5920145387619,59.99452354804,72.8293845444182));
#120768=CARTESIAN_POINT('Ctrl Pts',(-10.5939373540449,59.98545191324,73.5659849178225));
#120769=CARTESIAN_POINT('Ctrl Pts',(-10.5667795569519,60.1077131188501,
75.2172706809381));
#120770=CARTESIAN_POINT('Ctrl Pts',(-10.4191341151519,60.77930377661,77.670484391766));
#120771=CARTESIAN_POINT('Ctrl Pts',(-10.1684208232389,61.98983684518,80.026094579785));
#120772=CARTESIAN_POINT('Ctrl Pts',(-9.86622817732191,63.60334211099,82.0513183903311));
#120773=CARTESIAN_POINT('Ctrl Pts',(-9.5689352031129,65.4550150481601,83.63801640698));
#120774=CARTESIAN_POINT('Ctrl Pts',(-9.39241919703993,66.8223326583,84.45875352908));
#120775=CARTESIAN_POINT('Ctrl Pts',(-9.31830056473391,67.47714606609,84.7893033349101));
#120776=CARTESIAN_POINT('Ctrl Pts',(-12.3455984679183,61.69518876569,72.8346812857541));
#120777=CARTESIAN_POINT('Ctrl Pts',(-12.3467246669001,61.68710326644,73.5468061433598));
#120778=CARTESIAN_POINT('Ctrl Pts',(-12.3312057972915,61.79631693786,75.143292386617));
#120779=CARTESIAN_POINT('Ctrl Pts',(-12.2462629200551,62.3956876081601,
77.512581805897));
#120780=CARTESIAN_POINT('Ctrl Pts',(-12.0982058935566,63.4728781259,79.784555602918));
#120781=CARTESIAN_POINT('Ctrl Pts',(-11.9148004897113,64.90420967114,81.737926201103));
#120782=CARTESIAN_POINT('Ctrl Pts',(-11.7303545528999,66.5426944707001,
83.27176157901));
#120783=CARTESIAN_POINT('Ctrl Pts',(-11.6190836714997,67.75135964745,84.06872322495));
#120784=CARTESIAN_POINT('Ctrl Pts',(-11.5721915986834,68.3304350105,84.39060710346));
#120785=CARTESIAN_POINT('Ctrl Pts',(-10.5124509203882,67.7276234911821,
84.5902726033587));
#120786=CARTESIAN_POINT('Ctrl Pts',(-10.5571607538673,67.5564137297223,
84.4811141924303));
#120787=CARTESIAN_POINT('Ctrl Pts',(-10.6024067360406,67.3854035451806,
84.3665684200013));
#120788=CARTESIAN_POINT('Ctrl Pts',(-10.647902702036,67.2149593627826,84.2464239157399));
#120789=CARTESIAN_POINT('Ctrl Pts',(-10.6923121599897,67.0485856286275,
84.1291486322367));
#120790=CARTESIAN_POINT('Ctrl Pts',(-10.7369598391845,66.8827510813303,
84.006538784529));
#120791=CARTESIAN_POINT('Ctrl Pts',(-10.7815416096712,66.7178284965059,
83.8784014638752));
#120792=CARTESIAN_POINT('Ctrl Pts',(-10.7952986086174,66.6669368472762,
83.8388609753309));
#120793=CARTESIAN_POINT('Ctrl Pts',(-10.8090490512996,66.6161322765244,
83.7987941851335));
#120794=CARTESIAN_POINT('Ctrl Pts',(-10.8227832369869,66.5654263988847,
83.7581955099901));
#120795=CARTESIAN_POINT('Ctrl Pts',(-10.8374969257521,66.5111042483657,
83.7147013936337));
#120796=CARTESIAN_POINT('Ctrl Pts',(-10.8521919416177,66.4568953654081,
83.6705968123089));
#120797=CARTESIAN_POINT('Ctrl Pts',(-10.866861219374,66.40281454008,83.6258763513473));
#120798=CARTESIAN_POINT('Ctrl Pts',(-10.912283231951,66.2353584478959,83.4874037302678));
#120799=CARTESIAN_POINT('Ctrl Pts',(-10.9574603156574,66.0691269645397,
83.3430250688872));
#120800=CARTESIAN_POINT('Ctrl Pts',(-11.0021668171137,65.904586381939,83.1925892385079));
#120801=CARTESIAN_POINT('Ctrl Pts',(-11.0156267029942,65.855047782577,83.1472971882851));
#120802=CARTESIAN_POINT('Ctrl Pts',(-11.0290437632254,65.8056627461838,
83.101456195675));
#120803=CARTESIAN_POINT('Ctrl Pts',(-11.0424113914877,65.7564447705378,
83.0550624239674));
#120804=CARTESIAN_POINT('Ctrl Pts',(-11.0712952412536,65.6500979611824,
82.9548179598197));
#120805=CARTESIAN_POINT('Ctrl Pts',(-11.0999486221246,65.5445305662594,
82.8519924828178));
#120806=CARTESIAN_POINT('Ctrl Pts',(-11.1283013959138,65.439884830871,82.7465497055479));
#120807=CARTESIAN_POINT('Ctrl Pts',(-11.1424777828084,65.3875619631768,
82.6938283169129));
#120808=CARTESIAN_POINT('Ctrl Pts',(-11.1565789783029,65.3354695501648,
82.6404525535991));
#120809=CARTESIAN_POINT('Ctrl Pts',(-11.1705957096327,65.283626287648,82.5864183268548));
#120810=CARTESIAN_POINT('Ctrl Pts',(-11.1776040752976,65.2577046563896,
82.5594012134826));
#120811=CARTESIAN_POINT('Ctrl Pts',(-11.184591322483,65.2318453151878,82.5322194811105));
#120812=CARTESIAN_POINT('Ctrl Pts',(-11.191556267829,65.2060506367561,82.5048726231623));
#120813=CARTESIAN_POINT('Ctrl Pts',(-11.1916810581474,65.2055884757517,
82.5043826518928));
#120814=CARTESIAN_POINT('Ctrl Pts',(-11.1918058413085,65.205126335507,82.5038926276147));
#120815=CARTESIAN_POINT('Ctrl Pts',(-11.1919306173052,65.2046642160358,
82.5034025503252));
#120816=CARTESIAN_POINT('Ctrl Pts',(-11.1952879143089,65.1922301553399,
82.4902162399814));
#120817=CARTESIAN_POINT('Ctrl Pts',(-11.1986400245594,65.1798111337265,
82.4769915511165));
#120818=CARTESIAN_POINT('Ctrl Pts',(-11.2019868941466,65.1674074115863,
82.4637284635117));
#120819=CARTESIAN_POINT('Ctrl Pts',(-11.2048825157721,65.156676044519,82.4522535965384));
#120820=CARTESIAN_POINT('Ctrl Pts',(-11.2075163566646,65.146911979336,82.4417781471476));
#120821=CARTESIAN_POINT('Ctrl Pts',(-11.2105337830348,65.1357230733704,
82.4297294168383));
#120822=CARTESIAN_POINT('Ctrl Pts',(-11.2111336336814,65.133498769724,82.4273341840208));
#120823=CARTESIAN_POINT('Ctrl Pts',(-11.2117486041085,65.131218265178,82.4248766638023));
#120824=CARTESIAN_POINT('Ctrl Pts',(-11.2123837019444,65.128862938698,82.4223364667047));
#120825=CARTESIAN_POINT('Ctrl Pts',(-11.2942472546863,64.8252634259213,
82.0949072938397));
#120826=CARTESIAN_POINT('Ctrl Pts',(-11.3705951712443,64.5372340599892,
81.7515706634562));
#120827=CARTESIAN_POINT('Ctrl Pts',(-11.4414053735863,64.2666193828729,
81.3941165105011));
#120828=CARTESIAN_POINT('Ctrl Pts',(-11.4735077597793,64.1439339987481,
81.2320617375315));
#120829=CARTESIAN_POINT('Ctrl Pts',(-11.5044718368254,64.0248281634478,
81.0671060031894));
#120830=CARTESIAN_POINT('Ctrl Pts',(-11.5342949433969,63.9094748506058,
80.899419378088));
#120831=CARTESIAN_POINT('Ctrl Pts',(-11.5371696397123,63.8983557627067,
80.8832557996171));
#120832=CARTESIAN_POINT('Ctrl Pts',(-11.5400337345991,63.8872715412271,
80.8670668490848));
#120833=CARTESIAN_POINT('Ctrl Pts',(-11.542887259983,63.876222305584,80.8508527026476));
#120834=CARTESIAN_POINT('Ctrl Pts',(-11.5917648555483,63.6869616548419,
80.5731230926512));
#120835=CARTESIAN_POINT('Ctrl Pts',(-11.6375414127317,63.5079663264096,
80.2880005124143));
#120836=CARTESIAN_POINT('Ctrl Pts',(-11.6803771649707,63.3398328677561,
79.9963738633194));
#120837=CARTESIAN_POINT('Ctrl Pts',(-11.7017950410903,63.2557661384293,
79.8505605387719));
#120838=CARTESIAN_POINT('Ctrl Pts',(-11.722477786309,63.1744148043336,79.7031212474435));
#120839=CARTESIAN_POINT('Ctrl Pts',(-11.7424453129458,63.0958527030976,
79.5541677673539));
#120840=CARTESIAN_POINT('Ctrl Pts',(-11.7524290762642,63.0565716524796,
79.479691027309));
#120841=CARTESIAN_POINT('Ctrl Pts',(-11.7622340395622,63.0179879053016,
79.4048357436953));
#120842=CARTESIAN_POINT('Ctrl Pts',(-11.7718627033941,62.9801106499541,
79.329615914249));
#120843=CARTESIAN_POINT('Ctrl Pts',(-11.77667703531,62.9611720222803,79.2920059995258));
#120844=CARTESIAN_POINT('Ctrl Pts',(-11.7814472926542,62.9424100172644,
79.2543049485313));
#120845=CARTESIAN_POINT('Ctrl Pts',(-11.7861737878643,62.9238257804744,
79.2165145132332));
#120846=CARTESIAN_POINT('Ctrl Pts',(-11.7903094711731,62.9075645732832,
79.1834478823473));
#120847=CARTESIAN_POINT('Ctrl Pts',(-11.7944116491156,62.8914394698721,
79.1503128166153));
#120848=CARTESIAN_POINT('Ctrl Pts',(-11.7984805310734,62.8754512364734,
79.1171104905557));
#120849=CARTESIAN_POINT('Ctrl Pts',(-11.7990617999246,62.8731672031307,
79.1123673011186));
#120850=CARTESIAN_POINT('Ctrl Pts',(-11.799770087722,62.8703842409647,79.1065776670679));
#120851=CARTESIAN_POINT('Ctrl Pts',(-11.8002222996932,62.8686075184584,
79.1028768077023));
#120852=CARTESIAN_POINT('Ctrl Pts',(-11.8006505385931,62.866924985178,79.0993721416518));
#120853=CARTESIAN_POINT('Ctrl Pts',(-11.8010783203329,62.8652438987129,
79.0958667426276));
#120854=CARTESIAN_POINT('Ctrl Pts',(-11.8015056452176,62.8635642598512,
79.0923606119149));
#120855=CARTESIAN_POINT('Ctrl Pts',(-11.8460771862884,62.6883718121375,
78.7266584151115));
#120856=CARTESIAN_POINT('Ctrl Pts',(-11.8856781389952,62.5289278991055,
78.3530004020439));
#120857=CARTESIAN_POINT('Ctrl Pts',(-11.9206224684312,62.3858328118145,
77.972949274693));
#120858=CARTESIAN_POINT('Ctrl Pts',(-11.9405131754483,62.3043814718452,
77.756619880263));
#120859=CARTESIAN_POINT('Ctrl Pts',(-11.9588952170532,62.2282272177574,
77.5382181271681));
#120860=CARTESIAN_POINT('Ctrl Pts',(-11.9758265504949,62.1574824052876,
77.3180248654247));
#120861=CARTESIAN_POINT('Ctrl Pts',(-12.0039576391837,62.0399412440611,
76.9521779463928));
#120862=CARTESIAN_POINT('Ctrl Pts',(-12.0280844055031,61.9373317689448,
76.5813885434241));
#120863=CARTESIAN_POINT('Ctrl Pts',(-12.0484148829352,61.8499598392947,
76.2068848559227));
#120864=CARTESIAN_POINT('Ctrl Pts',(-12.0498602892,61.8437480848044,76.180259314152));
#120865=CARTESIAN_POINT('Ctrl Pts',(-12.0512865041583,61.8376133587138,
76.1536149789424));
#120866=CARTESIAN_POINT('Ctrl Pts',(-12.0526936012417,61.8315557753413,
76.1269522832721));
#120867=CARTESIAN_POINT('Ctrl Pts',(-12.0606350094199,61.7973678414036,
75.9764727236643));
#120868=CARTESIAN_POINT('Ctrl Pts',(-12.0679674798593,61.7656370535321,
75.8254083877693));
#120869=CARTESIAN_POINT('Ctrl Pts',(-12.0747040815038,61.7363843803514,
75.6738365926947));
#120870=CARTESIAN_POINT('Ctrl Pts',(-12.0928359949156,61.6576492902919,
75.265873229416));
#120871=CARTESIAN_POINT('Ctrl Pts',(-12.1066523254737,61.5968632578809,
74.854233901312));
#120872=CARTESIAN_POINT('Ctrl Pts',(-12.1162912295882,61.554270718676,74.4406782018442));
#120873=CARTESIAN_POINT('Ctrl Pts',(-12.1182894866595,61.5454407892938,
74.354943289344));
#120874=CARTESIAN_POINT('Ctrl Pts',(-12.120108150671,61.5373929478406,74.2691259786376));
#120875=CARTESIAN_POINT('Ctrl Pts',(-12.121748363988,61.5301296357777,74.1832418854536));
#120876=CARTESIAN_POINT('Ctrl Pts',(-12.1293332128959,61.496541855458,73.7860875253132));
#120877=CARTESIAN_POINT('Ctrl Pts',(-12.1331032131001,61.4797272509038,
73.3875061697423));
#120878=CARTESIAN_POINT('Ctrl Pts',(-12.1331903843725,61.479726180876,72.9888456300909));
#120879=CARTESIAN_POINT('Ctrl Pts',(-8.78823419891791,75.1738592483,86.78284890083));
#120880=CARTESIAN_POINT('Ctrl Pts',(-8.78306415477291,74.72662405869,86.7884138386));
#120881=CARTESIAN_POINT('Ctrl Pts',(-8.81909035422792,73.69777888124,86.7513931292899));
#120882=CARTESIAN_POINT('Ctrl Pts',(-9.02657683818592,72.18719744924,86.52606621289));
#120883=CARTESIAN_POINT('Ctrl Pts',(-9.35664843890192,70.73345419047,86.13264231638));
#120884=CARTESIAN_POINT('Ctrl Pts',(-9.6889294640759,69.49596570738,85.65887409272));
#120885=CARTESIAN_POINT('Ctrl Pts',(-9.98045484259091,68.43292028954,85.1378870539701));
#120886=CARTESIAN_POINT('Ctrl Pts',(-10.1467259739209,67.78111503905,84.74996216346));
#120887=CARTESIAN_POINT('Ctrl Pts',(-10.2190769752779,67.475529743,84.5512406152801));
#120888=CARTESIAN_POINT('Ctrl Pts',(-10.2208450793799,67.46804721363,84.5463644091599));
#120889=CARTESIAN_POINT('Ctrl Pts',(-9.36200580714891,75.1655542348801,
86.72290591126));
#120890=CARTESIAN_POINT('Ctrl Pts',(-9.35704322401691,74.73927457895,86.72795887135));
#120891=CARTESIAN_POINT('Ctrl Pts',(-9.39143229199792,73.75929218439,86.69443228328));
#120892=CARTESIAN_POINT('Ctrl Pts',(-9.59050034197691,72.30758761571,86.4878381917));
#120893=CARTESIAN_POINT('Ctrl Pts',(-9.91209801261292,70.8899328487,86.11982386996));
#120894=CARTESIAN_POINT('Ctrl Pts',(-10.2428814797899,69.6573777794501,
85.6638478182801));
#120895=CARTESIAN_POINT('Ctrl Pts',(-10.5367862749579,68.58546080019,85.1527501978));
#120896=CARTESIAN_POINT('Ctrl Pts',(-10.7064479646429,67.92049428063,84.76549219756));
#120897=CARTESIAN_POINT('Ctrl Pts',(-10.7804323422959,67.60807376471,84.56605837982));
#120898=CARTESIAN_POINT('Ctrl Pts',(-10.7822404632969,67.60042346136,84.5611641469));
#120899=CARTESIAN_POINT('Ctrl Pts',(-9.69871563896591,75.1551813275201,
86.2544898819));
#120900=CARTESIAN_POINT('Ctrl Pts',(-9.69387480142491,74.75534324128,86.25906511331));
#120901=CARTESIAN_POINT('Ctrl Pts',(-9.72730314172991,73.8365765524401,
86.2287688187401));
#120902=CARTESIAN_POINT('Ctrl Pts',(-9.92143095164091,72.46713521092,86.04033581194));
#120903=CARTESIAN_POINT('Ctrl Pts',(-10.2380558150979,71.11646999816,85.69971076544));
#120904=CARTESIAN_POINT('Ctrl Pts',(-10.5679604613399,69.92567467496,85.2691364608701));
#120905=CARTESIAN_POINT('Ctrl Pts',(-10.8632615838429,68.88187046176,84.78024447802));
#120906=CARTESIAN_POINT('Ctrl Pts',(-11.0349129752099,68.22957034288,84.40555652065));
#120907=CARTESIAN_POINT('Ctrl Pts',(-11.1098558768639,67.9226946509401,
84.21193807214));
#120908=CARTESIAN_POINT('Ctrl Pts',(-11.1116874812229,67.91517987633,84.20718621096));
#120909=CARTESIAN_POINT('Ctrl Pts',(-9.5727563377929,75.14969073673,85.69145592532));
#120910=CARTESIAN_POINT('Ctrl Pts',(-9.56786995661691,74.76406348025,85.69590777195));
#120911=CARTESIAN_POINT('Ctrl Pts',(-9.60165769416891,73.87784875743,85.6664135335801));
#120912=CARTESIAN_POINT('Ctrl Pts',(-9.79763359144691,72.55893776929,85.48340130992));
#120913=CARTESIAN_POINT('Ctrl Pts',(-10.1161187252549,71.26127783041,85.1537934673599));
#120914=CARTESIAN_POINT('Ctrl Pts',(-10.4463521283689,70.12108809596,84.73921042658));
#120915=CARTESIAN_POINT('Ctrl Pts',(-10.7411309007689,69.12354444036,84.26996174735));
#120916=CARTESIAN_POINT('Ctrl Pts',(-10.9120379674689,68.50125146073,83.91132461735));
#120917=CARTESIAN_POINT('Ctrl Pts',(-10.9866222962459,68.20858541074,83.7261526762101));
#120918=CARTESIAN_POINT('Ctrl Pts',(-10.9884451157479,68.20141865861,83.7216081912601));
#120919=CARTESIAN_POINT('Ctrl Pts',(-9.44679703661891,75.14420014595,85.12842196873));
#120920=CARTESIAN_POINT('Ctrl Pts',(-9.44186511180891,74.7727837192299,
85.1327504306));
#120921=CARTESIAN_POINT('Ctrl Pts',(-9.47601224660891,73.91912096243,85.1040582484099));
#120922=CARTESIAN_POINT('Ctrl Pts',(-9.67383623125391,72.65074032767,84.9264668079));
#120923=CARTESIAN_POINT('Ctrl Pts',(-9.99418163541291,71.40608566265,84.6078761692801));
#120924=CARTESIAN_POINT('Ctrl Pts',(-10.3247437953979,70.31650151696,84.2092843923));
#120925=CARTESIAN_POINT('Ctrl Pts',(-10.6190002176949,69.36521841896,83.75967901667));
#120926=CARTESIAN_POINT('Ctrl Pts',(-10.7891629597279,68.77293257858,83.41709271406));
#120927=CARTESIAN_POINT('Ctrl Pts',(-10.8633887156269,68.49447617054,83.24036728027));
#120928=CARTESIAN_POINT('Ctrl Pts',(-10.8652027502739,68.4876574409,83.23603017156));
#120929=CARTESIAN_POINT('Ctrl Pts',(-8.94256573698691,75.14727075947,84.84802251596));
#120930=CARTESIAN_POINT('Ctrl Pts',(-8.93745149514391,74.76831266994,84.8526646090801));
#120931=CARTESIAN_POINT('Ctrl Pts',(-8.97303734339591,73.89672718439,84.8218088401));
#120932=CARTESIAN_POINT('Ctrl Pts',(-9.17825945971091,72.6132869262601,
84.63326576691));
#120933=CARTESIAN_POINT('Ctrl Pts',(-9.50605176559191,71.3721378685,84.3019383492));
#120934=CARTESIAN_POINT('Ctrl Pts',(-9.83792998165891,70.30809764094,83.89921264699));
#120935=CARTESIAN_POINT('Ctrl Pts',(-10.1300953692419,69.39022670154,83.45352654093));
#120936=CARTESIAN_POINT('Ctrl Pts',(-10.2972784838039,68.8251829068101,
83.11971723483));
#120937=CARTESIAN_POINT('Ctrl Pts',(-10.3700688263069,68.56008000191,82.948409991363));
#120938=CARTESIAN_POINT('Ctrl Pts',(-10.3718476940469,68.55358860125,82.944206314064));
#120939=CARTESIAN_POINT('Ctrl Pts',(-8.39791503440691,75.15684515891,85.03813500136));
#120940=CARTESIAN_POINT('Ctrl Pts',(-8.3926038609189,74.75364609168,85.0433175978499));
#120941=CARTESIAN_POINT('Ctrl Pts',(-8.4297437505259,73.82567203736,85.00878227787));
#120942=CARTESIAN_POINT('Ctrl Pts',(-8.6429570360019,72.47167265314,84.80025313287));
#120943=CARTESIAN_POINT('Ctrl Pts',(-8.9787931905259,71.18218065664,84.44096904022));
#120944=CARTESIAN_POINT('Ctrl Pts',(-9.31209295830991,70.1015073586001,
84.01675409817));
#120945=CARTESIAN_POINT('Ctrl Pts',(-9.60199969291491,69.18181286463,83.5566371800399));
#120946=CARTESIAN_POINT('Ctrl Pts',(-9.76596433175591,68.62299289916,83.21845014512));
#120947=CARTESIAN_POINT('Ctrl Pts',(-9.83720419749391,68.36144004473,83.04590239804));
#120948=CARTESIAN_POINT('Ctrl Pts',(-9.83894507933091,68.3550359577,83.04166880362));
#120949=CARTESIAN_POINT('Origin',(-10.0948681361921,68.0757882531393,83.873061985328));
#120950=CARTESIAN_POINT('Ctrl Pts',(-9.07682613028944,74.9999993274218,
86.7031078141393));
#120951=CARTESIAN_POINT('Ctrl Pts',(-9.1039999950439,75.0000092485729,86.6903141483864));
#120952=CARTESIAN_POINT('Ctrl Pts',(-9.13088724151182,75.0000188963107,
86.6759898162085));
#120953=CARTESIAN_POINT('Ctrl Pts',(-9.15724126370756,75.0000282223508,
86.660143135858));
#120954=CARTESIAN_POINT('Ctrl Pts',(-9.1832912253031,75.0000374407914,86.6444792872249));
#120955=CARTESIAN_POINT('Ctrl Pts',(-9.20881934010755,75.000046344709,86.6273278788693));
#120956=CARTESIAN_POINT('Ctrl Pts',(-9.23358406665593,75.0000548869962,
86.6087473498606));
#120957=CARTESIAN_POINT('Ctrl Pts',(-9.25813552876578,75.0000633557204,
86.5903268293252));
#120958=CARTESIAN_POINT('Ctrl Pts',(-9.28193582083955,75.0000714688075,
86.5705018011063));
#120959=CARTESIAN_POINT('Ctrl Pts',(-9.30475915361152,75.0000791829749,
86.5493793145271));
#120960=CARTESIAN_POINT('Ctrl Pts',(-9.3274531992086,75.0000868534439,86.5283764803511));
#120961=CARTESIAN_POINT('Ctrl Pts',(-9.3491805030452,75.000094129306,86.5060911919904));
#120962=CARTESIAN_POINT('Ctrl Pts',(-9.36974127645128,75.0001009736224,
86.4826751026743));
#120963=CARTESIAN_POINT('Ctrl Pts',(-9.39024645363451,75.0001077994319,
86.4593223303403));
#120964=CARTESIAN_POINT('Ctrl Pts',(-9.40959070386905,75.0001141958634,
86.4348454293696));
#120965=CARTESIAN_POINT('Ctrl Pts',(-9.42760939948391,75.0001201345612,
86.4094343008029));
#120966=CARTESIAN_POINT('Ctrl Pts',(-9.44563283269775,75.0001260748204,
86.384016490968));
#120967=CARTESIAN_POINT('Ctrl Pts',(-9.46232950021035,75.0001315569872,
86.3576647027745));
#120968=CARTESIAN_POINT('Ctrl Pts',(-9.47757741530337,75.0001365631105,
86.3305987120963));
#120969=CARTESIAN_POINT('Ctrl Pts',(-9.49293759605771,75.0001416060924,
86.3033334429381));
#120970=CARTESIAN_POINT('Ctrl Pts',(-9.50682728712193,75.0001461659229,
86.2753442715377));
#120971=CARTESIAN_POINT('Ctrl Pts',(-9.51917165228589,75.0001502362991,
86.2468739512454));
#120972=CARTESIAN_POINT('Ctrl Pts',(-9.53159872212886,75.000154333946,86.2182128857289));
#120973=CARTESIAN_POINT('Ctrl Pts',(-9.54245964807323,75.0001579355543,
86.1890651223823));
#120974=CARTESIAN_POINT('Ctrl Pts',(-9.55173123092228,75.0001610474391,
86.1596830567647));
#120975=CARTESIAN_POINT('Ctrl Pts',(-9.56108916788585,75.0001641883075,
86.1300273310505));
#120976=CARTESIAN_POINT('Ctrl Pts',(-9.56882823591791,75.0001668303455,
86.1001338087849));
#120977=CARTESIAN_POINT('Ctrl Pts',(-9.57497724561461,75.0001689925852,
86.0702529880198));
#120978=CARTESIAN_POINT('Ctrl Pts',(-9.58119948158406,75.0001711805742,
86.0400163276578));
#120979=CARTESIAN_POINT('Ctrl Pts',(-9.58579401693955,75.0001728773831,
86.0097934597345));
#120980=CARTESIAN_POINT('Ctrl Pts',(-9.5888392751087,75.0001741142058,85.9798218969514));
#120981=CARTESIAN_POINT('Ctrl Pts',(-9.59195555286792,75.000175379873,85.9491513562872));
#120982=CARTESIAN_POINT('Ctrl Pts',(-9.59345005338468,75.0001761639981,
85.9187446672596));
#120983=CARTESIAN_POINT('Ctrl Pts',(-9.59344934447128,75.0001765099556,
85.8888219184229));
#120984=CARTESIAN_POINT('Ctrl Pts',(-9.59344862496941,75.0001768610804,
85.8584522371007));
#120985=CARTESIAN_POINT('Ctrl Pts',(-9.59190851333747,75.0001767610487,
85.8285814699798));
#120986=CARTESIAN_POINT('Ctrl Pts',(-9.5889935805498,75.0001762626353,85.7993962358321));
#120987=CARTESIAN_POINT('Ctrl Pts',(-9.58600511872059,75.0001757516495,
85.769474805535));
#120988=CARTESIAN_POINT('Ctrl Pts',(-9.58157246622322,75.0001748221386,
85.7402741621901));
#120989=CARTESIAN_POINT('Ctrl Pts',(-9.57589365398664,75.0001735355896,
85.7119449365612));
#120990=CARTESIAN_POINT('Ctrl Pts',(-9.57457467685929,75.0001732367721,
85.7053651098151));
#120991=CARTESIAN_POINT('Ctrl Pts',(-9.57318852872199,75.0001729187054,
85.69883207632));
#120992=CARTESIAN_POINT('Ctrl Pts',(-9.57173776914894,75.000172582176,85.6923473348265));
#120993=CARTESIAN_POINT('Ctrl Pts',(-9.56551370280152,75.0001711383933,
85.6645264180797));
#120994=CARTESIAN_POINT('Ctrl Pts',(-9.55783270404159,75.000169375034,85.636404976219));
#120995=CARTESIAN_POINT('Ctrl Pts',(-9.54857347396362,75.0001672728027,
85.6081918997157));
#120996=CARTESIAN_POINT('Ctrl Pts',(-9.53951690601546,75.0001652165842,
85.5805963391533));
#120997=CARTESIAN_POINT('Ctrl Pts',(-9.52894976121176,75.0001628359852,
85.5529135806624));
#120998=CARTESIAN_POINT('Ctrl Pts',(-9.51679285414588,75.0001601213691,
85.525374443193));
#120999=CARTESIAN_POINT('Ctrl Pts',(-9.5048679062755,75.000157458549,85.4983607647188));
#121000=CARTESIAN_POINT('Ctrl Pts',(-9.49141274535669,75.0001544741896,
85.4714859248144));
#121001=CARTESIAN_POINT('Ctrl Pts',(-9.47639499416025,75.0001511698034,
85.4449939781286));
#121002=CARTESIAN_POINT('Ctrl Pts',(-9.46162100403104,75.0001479190524,
85.4189320362492));
#121003=CARTESIAN_POINT('Ctrl Pts',(-9.44533438718474,75.0001443584789,
85.3932414401996));
#121004=CARTESIAN_POINT('Ctrl Pts',(-9.42755231432626,75.0001405017234,
85.3681696172939));
#121005=CARTESIAN_POINT('Ctrl Pts',(-9.41000756113383,75.0001366964402,
85.3434324031083));
#121006=CARTESIAN_POINT('Ctrl Pts',(-9.39100687524647,75.0001326027845,
85.3192984171788));
#121007=CARTESIAN_POINT('Ctrl Pts',(-9.37061743520198,75.0001282469069,
85.2960079213212));
#121008=CARTESIAN_POINT('Ctrl Pts',(-9.34984201493385,75.0001238085708,
85.2722765270976));
#121009=CARTESIAN_POINT('Ctrl Pts',(-9.32762462572574,75.0001190979427,
85.2494218850684));
#121010=CARTESIAN_POINT('Ctrl Pts',(-9.30409180453489,75.0001141571469,
85.2276865690307));
#121011=CARTESIAN_POINT('Ctrl Pts',(-9.28144013241794,75.0001094013514,
85.2067650973444));
#121012=CARTESIAN_POINT('Ctrl Pts',(-9.25757030985385,75.0001044324524,
85.1868814238287));
#121013=CARTESIAN_POINT('Ctrl Pts',(-9.23264164306911,75.0000993002975,
85.1682285148038));
#121014=CARTESIAN_POINT('Ctrl Pts',(-9.20779321329462,75.0000941846614,
85.1496356432316));
#121015=CARTESIAN_POINT('Ctrl Pts',(-9.18189331394217,75.0000889069572,
85.1322663161795));
#121016=CARTESIAN_POINT('Ctrl Pts',(-9.15513836009448,75.0000835269521,
85.116277304706));
#121017=CARTESIAN_POINT('Ctrl Pts',(-9.12839924598676,75.0000781501322,
85.1002977592098));
#121018=CARTESIAN_POINT('Ctrl Pts',(-9.10080683593434,75.0000726713189,
85.0856974009567));
#121019=CARTESIAN_POINT('Ctrl Pts',(-9.07258596059583,75.0000671581359,
85.072589329158));
#121020=CARTESIAN_POINT('Ctrl Pts',(-9.04430746240215,75.0000616336957,
85.0594544926146));
#121021=CARTESIAN_POINT('Ctrl Pts',(-9.01539879073464,75.000056074964,85.0478183180827));
#121022=CARTESIAN_POINT('Ctrl Pts',(-8.98610290733461,75.0000505549175,
85.0377450762615));
#121023=CARTESIAN_POINT('Ctrl Pts',(-8.95654791083624,75.0000449860479,
85.0275827397076));
#121024=CARTESIAN_POINT('Ctrl Pts',(-8.92659973489031,75.0000394567854,
85.0190111633951));
#121025=CARTESIAN_POINT('Ctrl Pts',(-8.89651140594933,75.000034043637,85.012043351497));
#121026=CARTESIAN_POINT('Ctrl Pts',(-8.86622517470581,75.0000285948843,
85.0050297096686));
#121027=CARTESIAN_POINT('Ctrl Pts',(-8.83579781987906,75.0000232640081,
84.9996407568054));
#121028=CARTESIAN_POINT('Ctrl Pts',(-8.80547732474202,75.0000181270819,
84.9958377323157));
#121029=CARTESIAN_POINT('Ctrl Pts',(-8.77474583349593,75.0000129205244,
84.9919831576037));
#121030=CARTESIAN_POINT('Ctrl Pts',(-8.74412491066269,75.0000079134206,
84.9897573534682));
#121031=CARTESIAN_POINT('Ctrl Pts',(-8.71384962962853,75.000003179607,84.9890718459353));
#121032=CARTESIAN_POINT('Ctrl Pts',(-8.70698518555844,75.0000021062891,
84.9889164178779));
#121033=CARTESIAN_POINT('Ctrl Pts',(-8.70013839104306,75.0000010469921,
84.9888399980095));
#121034=CARTESIAN_POINT('Ctrl Pts',(-8.69331176399212,75.0000000025229,
84.9888412596806));
#121035=CARTESIAN_POINT('Ctrl Pts',(-10.2209988615099,82.53201492112,84.5463071490699));
#121036=CARTESIAN_POINT('Ctrl Pts',(-10.2196138809369,82.52615454987,84.5501263019201));
#121037=CARTESIAN_POINT('Ctrl Pts',(-10.1480248596239,82.22369804759,84.7469073932701));
#121038=CARTESIAN_POINT('Ctrl Pts',(-9.98388528962092,81.57953238398,85.13082175917));
#121039=CARTESIAN_POINT('Ctrl Pts',(-9.69703742856391,80.53299869942,85.6454591886499));
#121040=CARTESIAN_POINT('Ctrl Pts',(-9.37340190588592,79.32933774873,86.1104956637399));
#121041=CARTESIAN_POINT('Ctrl Pts',(-9.0509892783709,77.93165755883,86.49818447736));
#121042=CARTESIAN_POINT('Ctrl Pts',(-8.8275504427949,76.40669320108,86.74311300067));
#121043=CARTESIAN_POINT('Ctrl Pts',(-8.78224841483291,75.3376955241,86.7892411675));
#121044=CARTESIAN_POINT('Ctrl Pts',(-8.78824703447191,74.82597871997,86.7828639942501));
#121045=CARTESIAN_POINT('Ctrl Pts',(-10.7823191176949,82.39961247361,84.56103171051));
#121046=CARTESIAN_POINT('Ctrl Pts',(-10.7809027858309,82.39362068301,84.56486500648));
#121047=CARTESIAN_POINT('Ctrl Pts',(-10.7076964146739,82.08439452547,84.76235742167));
#121048=CARTESIAN_POINT('Ctrl Pts',(-10.5401996687189,81.42719321186,85.1456491656101));
#121049=CARTESIAN_POINT('Ctrl Pts',(-10.2509568608329,80.37172515551,85.6506696895));
#121050=CARTESIAN_POINT('Ctrl Pts',(-9.92861983620391,79.1723369897,86.09858813837));
#121051=CARTESIAN_POINT('Ctrl Pts',(-9.61403567648691,77.80751099573,86.46193062935));
#121052=CARTESIAN_POINT('Ctrl Pts',(-9.39940208414091,76.34053759145,86.68685818504));
#121053=CARTESIAN_POINT('Ctrl Pts',(-9.35621111575492,75.32201118481,86.7286338586));
#121054=CARTESIAN_POINT('Ctrl Pts',(-9.36195895042991,74.83428008366,86.72284269431));
#121055=CARTESIAN_POINT('Ctrl Pts',(-11.1116947646629,82.08488536259,84.20707377878));
#121056=CARTESIAN_POINT('Ctrl Pts',(-11.1102600362549,82.07899968205,84.21079560067));
#121057=CARTESIAN_POINT('Ctrl Pts',(-11.0361046246079,81.77525758485,84.40253403785));
#121058=CARTESIAN_POINT('Ctrl Pts',(-10.8666379301449,81.13055427193,84.77340994602));
#121059=CARTESIAN_POINT('Ctrl Pts',(-10.5759897976639,80.10263820646,85.2565886538999));
#121060=CARTESIAN_POINT('Ctrl Pts',(-10.2544147153149,78.94355025105,85.67978173207));
#121061=CARTESIAN_POINT('Ctrl Pts',(-9.94442420176891,77.64203064539,86.01654748314));
#121062=CARTESIAN_POINT('Ctrl Pts',(-9.7349574150989,76.25723670102,86.22195022949));
#121063=CARTESIAN_POINT('Ctrl Pts',(-9.69300518984691,75.30213041752,86.25970207899));
#121064=CARTESIAN_POINT('Ctrl Pts',(-9.69860586706891,74.84465461789,86.25445790009));
#121065=CARTESIAN_POINT('Ctrl Pts',(-10.9884710263669,81.7986750417,83.7215562525299));
#121066=CARTESIAN_POINT('Ctrl Pts',(-10.9870431803459,81.79306191555,83.72511566167));
#121067=CARTESIAN_POINT('Ctrl Pts',(-10.9132428171619,81.50338372185,83.90848951421));
#121068=CARTESIAN_POINT('Ctrl Pts',(-10.7445131062059,80.88833942085,84.2634739684799));
#121069=CARTESIAN_POINT('Ctrl Pts',(-10.4543907240389,79.90600412583,84.7272181823501));
#121070=CARTESIAN_POINT('Ctrl Pts',(-10.1325305891159,78.79624595759,85.13464252384));
#121071=CARTESIAN_POINT('Ctrl Pts',(-9.82082153244591,77.54607482409,85.46040536236));
#121072=CARTESIAN_POINT('Ctrl Pts',(-9.60942177618192,76.21259532136,85.65983948489));
#121073=CARTESIAN_POINT('Ctrl Pts',(-9.56700612091791,75.29137171221,85.69659181294));
#121074=CARTESIAN_POINT('Ctrl Pts',(-9.5726618516689,74.85015223226,85.69148916033));
#121075=CARTESIAN_POINT('Ctrl Pts',(-10.8652472880709,81.5124647208,83.2360387262901));
#121076=CARTESIAN_POINT('Ctrl Pts',(-10.8638263244369,81.50712414905,83.23943572267));
#121077=CARTESIAN_POINT('Ctrl Pts',(-10.7903810097159,81.23150985885,83.41444499058));
#121078=CARTESIAN_POINT('Ctrl Pts',(-10.6223882822669,80.64612456977,83.75353799095));
#121079=CARTESIAN_POINT('Ctrl Pts',(-10.3327916504149,79.7093700452,84.1978477107901));
#121080=CARTESIAN_POINT('Ctrl Pts',(-10.0106464629179,78.64894166412,84.58950331562));
#121081=CARTESIAN_POINT('Ctrl Pts',(-9.69721886312191,77.45011900279,84.90426324159));
#121082=CARTESIAN_POINT('Ctrl Pts',(-9.48388613726391,76.16795394169,85.0977287403));
#121083=CARTESIAN_POINT('Ctrl Pts',(-9.44100705198991,75.2806130069,85.1334815468801));
#121084=CARTESIAN_POINT('Ctrl Pts',(-9.4467178362679,74.85564984662,85.12852042057));
#121085=CARTESIAN_POINT('Ctrl Pts',(-10.3719740027499,81.44650872388,82.9442186851291));
#121086=CARTESIAN_POINT('Ctrl Pts',(-10.3705805897979,81.4414245616901,
82.947511133341));
#121087=CARTESIAN_POINT('Ctrl Pts',(-10.2985565590249,81.17903235171,83.11714879837));
#121088=CARTESIAN_POINT('Ctrl Pts',(-10.1335140283549,80.6205979707,83.4475207026201));
#121089=CARTESIAN_POINT('Ctrl Pts',(-9.84602201196492,79.71691760354,83.88782277379));
#121090=CARTESIAN_POINT('Ctrl Pts',(-9.5227357389799,78.68180165885,84.28323004135));
#121091=CARTESIAN_POINT('Ctrl Pts',(-9.20242869026491,77.4879702719599,
84.60993193468));
#121092=CARTESIAN_POINT('Ctrl Pts',(-8.98135815126292,76.19187815032,84.81498348546));
#121093=CARTESIAN_POINT('Ctrl Pts',(-8.93662392308091,75.28618381722,84.85343067092));
#121094=CARTESIAN_POINT('Ctrl Pts',(-8.94255509050291,74.8525875886,84.84811080075));
#121095=CARTESIAN_POINT('Ctrl Pts',(-9.83910397498791,81.64499218078,83.0415917172));
#121096=CARTESIAN_POINT('Ctrl Pts',(-9.8377403243039,81.63997650984,83.04490752058));
#121097=CARTESIAN_POINT('Ctrl Pts',(-9.76725166882992,81.38110684321,83.2157650996));
#121098=CARTESIAN_POINT('Ctrl Pts',(-9.60539615737491,80.82886035969,83.55042868746));
#121099=CARTESIAN_POINT('Ctrl Pts',(-9.32017770116691,79.92359055334,84.0048347525));
#121100=CARTESIAN_POINT('Ctrl Pts',(-8.9956587438369,78.87281242971,84.42100077467));
#121101=CARTESIAN_POINT('Ctrl Pts',(-8.6679200091869,77.63427137341,84.7745893727101));
#121102=CARTESIAN_POINT('Ctrl Pts',(-8.43849051617991,76.26834068187,85.00101994304));
#121103=CARTESIAN_POINT('Ctrl Pts',(-8.39175222638992,75.30435215535,85.0440503939699));
#121104=CARTESIAN_POINT('Ctrl Pts',(-8.39792146786892,74.84301692091,85.03811183887));
#121105=CARTESIAN_POINT('Origin',(-10.0948766030609,81.92425938485,83.87303403236));
#121106=CARTESIAN_POINT('Ctrl Pts',(-10.9000842015569,85.1489979884701,
82.322918391228));
#121107=CARTESIAN_POINT('Ctrl Pts',(-10.9000339342259,85.1487780176699,
82.323157570113));
#121108=CARTESIAN_POINT('Ctrl Pts',(-10.8749983963149,85.03922423422,82.442269255368));
#121109=CARTESIAN_POINT('Ctrl Pts',(-10.8237045453949,84.8169570122299,
82.675542262189));
#121110=CARTESIAN_POINT('Ctrl Pts',(-10.7429847377379,84.47338318276,83.01175597191));
#121111=CARTESIAN_POINT('Ctrl Pts',(-10.6588700927759,84.1207479250599,
83.33364079941));
#121112=CARTESIAN_POINT('Ctrl Pts',(-10.5716199860159,83.75941600244,83.64129586374));
#121113=CARTESIAN_POINT('Ctrl Pts',(-10.4815593551129,83.38967102889,83.93484316048));
#121114=CARTESIAN_POINT('Ctrl Pts',(-10.3891461035709,83.01172959405,84.2144031959899));
#121115=CARTESIAN_POINT('Ctrl Pts',(-10.2950438513529,82.62625525885,84.47973595617));
#121116=CARTESIAN_POINT('Ctrl Pts',(-10.2314871820529,82.36404301501,84.6474306810499));
#121117=CARTESIAN_POINT('Ctrl Pts',(-10.1996872471569,82.23194589096,84.72880451956));
#121118=CARTESIAN_POINT('Ctrl Pts',(-11.4502964565729,85.02149802074,82.3294407801081));
#121119=CARTESIAN_POINT('Ctrl Pts',(-11.4502456178769,85.0212755613401,
82.329679510253));
#121120=CARTESIAN_POINT('Ctrl Pts',(-11.4249255198359,84.91048240158,82.4485675977571));
#121121=CARTESIAN_POINT('Ctrl Pts',(-11.3730558256989,84.68574072168,82.681278953403));
#121122=CARTESIAN_POINT('Ctrl Pts',(-11.2914660795799,84.3385299168701,
83.01625977792));
#121123=CARTESIAN_POINT('Ctrl Pts',(-11.2065003700329,83.98243486936,83.33647585558));
#121124=CARTESIAN_POINT('Ctrl Pts',(-11.1184361131769,83.61789200861,83.64201291631));
#121125=CARTESIAN_POINT('Ctrl Pts',(-11.0276387921209,83.24534162635,83.93292036531));
#121126=CARTESIAN_POINT('Ctrl Pts',(-10.9346178603449,82.86519761575,84.20924596527));
#121127=CARTESIAN_POINT('Ctrl Pts',(-10.8400534714679,82.4781915141401,
84.4707996776401));
#121128=CARTESIAN_POINT('Ctrl Pts',(-10.7763071557859,82.21549634624,84.6356097280201));
#121129=CARTESIAN_POINT('Ctrl Pts',(-10.7444477634099,82.08331859002,84.71545483133));
#121130=CARTESIAN_POINT('Ctrl Pts',(-11.7566426228269,84.63945625565,82.047965337043));
#121131=CARTESIAN_POINT('Ctrl Pts',(-11.7565914660076,84.63923911138,82.048196506829));
#121132=CARTESIAN_POINT('Ctrl Pts',(-11.7311129311008,84.5310931103201,
82.163319446383));
#121133=CARTESIAN_POINT('Ctrl Pts',(-11.6789226200385,84.3117447011801,
82.388587120115));
#121134=CARTESIAN_POINT('Ctrl Pts',(-11.596848511184,83.97297677322,82.712600409691));
#121135=CARTESIAN_POINT('Ctrl Pts',(-11.5114089474649,83.62570147102,83.02204061675));
#121136=CARTESIAN_POINT('Ctrl Pts',(-11.4228913896159,83.27038454296,83.31698288365));
#121137=CARTESIAN_POINT('Ctrl Pts',(-11.3316838955729,82.90754607615,83.59743190417));
#121138=CARTESIAN_POINT('Ctrl Pts',(-11.2383246207169,82.5377047440001,
83.86339068861));
#121139=CARTESIAN_POINT('Ctrl Pts',(-11.1435029242409,82.16161019115,84.11470474701));
#121140=CARTESIAN_POINT('Ctrl Pts',(-11.0796510175969,81.9066530444801,
84.27276298195));
#121141=CARTESIAN_POINT('Ctrl Pts',(-11.0477585205939,81.7784653785301,
84.3492589645101));
#121142=CARTESIAN_POINT('Ctrl Pts',(-11.6201571429516,84.25100099088,81.661304594338));
#121143=CARTESIAN_POINT('Ctrl Pts',(-11.620106127865,84.2507935134,81.661526002444));
#121144=CARTESIAN_POINT('Ctrl Pts',(-11.594698180855,84.1474619307,81.771787630287));
#121145=CARTESIAN_POINT('Ctrl Pts',(-11.5426507132809,83.9378717021601,
81.9875641102349));
#121146=CARTESIAN_POINT('Ctrl Pts',(-11.4607924010889,83.61414302773,82.297998404337));
#121147=CARTESIAN_POINT('Ctrl Pts',(-11.3755639521849,83.28223876212,82.594554327183));
#121148=CARTESIAN_POINT('Ctrl Pts',(-11.2872483521549,82.9425925833399,
82.877306111483));
#121149=CARTESIAN_POINT('Ctrl Pts',(-11.1962236012409,82.59567566606,83.14627065778));
#121150=CARTESIAN_POINT('Ctrl Pts',(-11.1030150673529,82.24195088805,83.40146328096));
#121151=CARTESIAN_POINT('Ctrl Pts',(-11.0083080083519,81.88212437179,83.64272752465));
#121152=CARTESIAN_POINT('Ctrl Pts',(-10.9445031453299,81.63810050545,83.794551969));
#121153=CARTESIAN_POINT('Ctrl Pts',(-10.9126253973309,81.51538217035,83.8680536305499));
#121154=CARTESIAN_POINT('Ctrl Pts',(-11.4836716630759,83.86254572611,81.274643851633));
#121155=CARTESIAN_POINT('Ctrl Pts',(-11.4836207897219,83.8623479154201,
81.274855498059));
#121156=CARTESIAN_POINT('Ctrl Pts',(-11.4582834306089,83.76383075108,81.380255814191));
#121157=CARTESIAN_POINT('Ctrl Pts',(-11.4063788065229,83.5639987031501,
81.586541100355));
#121158=CARTESIAN_POINT('Ctrl Pts',(-11.3247362909949,83.25530928223,81.8833963989819));
#121159=CARTESIAN_POINT('Ctrl Pts',(-11.2397189569049,82.93877605322,82.1670680376131));
#121160=CARTESIAN_POINT('Ctrl Pts',(-11.1516053146929,82.61480062371,82.437629339314));
#121161=CARTESIAN_POINT('Ctrl Pts',(-11.0607633069079,82.28380525598,82.6951094113881));
#121162=CARTESIAN_POINT('Ctrl Pts',(-10.9677055139879,81.9461970320901,
82.939535873321));
#121163=CARTESIAN_POINT('Ctrl Pts',(-10.8731130924629,81.60263855244,83.17075030229));
#121164=CARTESIAN_POINT('Ctrl Pts',(-10.8093552730629,81.36954796641,83.3163409560501));
#121165=CARTESIAN_POINT('Ctrl Pts',(-10.7774922740679,81.25229896216,83.3868482966));
#121166=CARTESIAN_POINT('Ctrl Pts',(-10.9929990594039,83.71997069593,81.033926038262));
#121167=CARTESIAN_POINT('Ctrl Pts',(-10.9929486955869,83.7197806253201,
81.034132061698));
#121168=CARTESIAN_POINT('Ctrl Pts',(-10.9678651037399,83.62511827294,81.136732224696));
#121169=CARTESIAN_POINT('Ctrl Pts',(-10.9164740096379,83.4330715771,81.337643141076));
#121170=CARTESIAN_POINT('Ctrl Pts',(-10.8356072946589,83.13625009941,81.627127262995));
#121171=CARTESIAN_POINT('Ctrl Pts',(-10.7513489296249,82.83165602498,81.904174282366));
#121172=CARTESIAN_POINT('Ctrl Pts',(-10.6639613365779,82.51961833081,82.1688668813501));
#121173=CARTESIAN_POINT('Ctrl Pts',(-10.5737763001199,82.20041342654,82.421295364125));
#121174=CARTESIAN_POINT('Ctrl Pts',(-10.4812604290489,81.8742682608201,
82.661548720194));
#121175=CARTESIAN_POINT('Ctrl Pts',(-10.3870801353809,81.5417685492,82.889430322419));
#121176=CARTESIAN_POINT('Ctrl Pts',(-10.3234914403189,81.3157055610401,
83.03335392967));
#121177=CARTESIAN_POINT('Ctrl Pts',(-10.2916814647829,81.20185290992,83.1031664991001));
#121178=CARTESIAN_POINT('Ctrl Pts',(-10.4668211332059,83.9158754608199,
81.0954924412439));
#121179=CARTESIAN_POINT('Ctrl Pts',(-10.4667713157959,83.91568617653,81.095700632396));
#121180=CARTESIAN_POINT('Ctrl Pts',(-10.4419598539459,83.8214154083399,
81.19938044292));
#121181=CARTESIAN_POINT('Ctrl Pts',(-10.3911194491209,83.63012480945,81.402524356558));
#121182=CARTESIAN_POINT('Ctrl Pts',(-10.3110846720209,83.33429197876,81.695632548757));
#121183=CARTESIAN_POINT('Ctrl Pts',(-10.2276401954349,83.03045094066,81.976617168283));
#121184=CARTESIAN_POINT('Ctrl Pts',(-10.1410311888439,82.71886465341,82.245574446584));
#121185=CARTESIAN_POINT('Ctrl Pts',(-10.0515506624969,82.39966146212,82.502665128717));
#121186=CARTESIAN_POINT('Ctrl Pts',(-9.95961592701791,82.07288083721,82.748048781055));
#121187=CARTESIAN_POINT('Ctrl Pts',(-9.86587758299191,81.73904818185,82.981479147184));
#121188=CARTESIAN_POINT('Ctrl Pts',(-9.80247025019291,81.5115428283,83.12938516456));
#121189=CARTESIAN_POINT('Ctrl Pts',(-9.7707171349199,81.39680769081,83.20125375235));
#121190=CARTESIAN_POINT('Origin',(-10.7325649783137,84.400884996501,81.8225337390639));
#121191=CARTESIAN_POINT('Ctrl Pts',(-10.9119544098049,84.86842874797,63.380422745097));
#121192=CARTESIAN_POINT('Ctrl Pts',(-10.9167381083619,84.8874759227999,
63.39998682244));
#121193=CARTESIAN_POINT('Ctrl Pts',(-10.9504786885429,85.0241366108199,
63.541195794788));
#121194=CARTESIAN_POINT('Ctrl Pts',(-11.0074315439549,85.2867981542799,
63.824462601624));
#121195=CARTESIAN_POINT('Ctrl Pts',(-11.0713860526219,85.65704572501,64.256521960082));
#121196=CARTESIAN_POINT('Ctrl Pts',(-11.1222079779469,86.0440636034599,
64.750002833932));
#121197=CARTESIAN_POINT('Ctrl Pts',(-11.1583315157829,86.4400410225399,
65.3076455886));
#121198=CARTESIAN_POINT('Ctrl Pts',(-11.1784124764709,86.8363310607599,
65.93168374147));
#121199=CARTESIAN_POINT('Ctrl Pts',(-11.1813287703659,87.2214023399299,
66.619865386485));
#121200=CARTESIAN_POINT('Ctrl Pts',(-11.1670632946759,87.58130362105,67.362729524661));
#121201=CARTESIAN_POINT('Ctrl Pts',(-11.1377395816439,87.90221268558,68.143219650457));
#121202=CARTESIAN_POINT('Ctrl Pts',(-11.0978808367489,88.1743502388799,
68.941806401532));
#121203=CARTESIAN_POINT('Ctrl Pts',(-11.0531195238519,88.3963865257801,
69.752103612324));
#121204=CARTESIAN_POINT('Ctrl Pts',(-11.0097139579119,88.5673268808599,
70.566915779017));
#121205=CARTESIAN_POINT('Ctrl Pts',(-10.9743067365659,88.68604747705,71.372377743079));
#121206=CARTESIAN_POINT('Ctrl Pts',(-10.9517101510869,88.75478071011,72.1496973709892));
#121207=CARTESIAN_POINT('Ctrl Pts',(-10.9431768096399,88.7795591710799,
72.8954247448889));
#121208=CARTESIAN_POINT('Ctrl Pts',(-10.9481909246279,88.76504282562,73.6271941059289));
#121209=CARTESIAN_POINT('Ctrl Pts',(-10.9661875364359,88.7111874448201,
74.366562872615));
#121210=CARTESIAN_POINT('Ctrl Pts',(-10.9960850511939,88.6145104410999,
75.122691718376));
#121211=CARTESIAN_POINT('Ctrl Pts',(-11.0346951715699,88.4723543121901,
75.888569658041));
#121212=CARTESIAN_POINT('Ctrl Pts',(-11.0771783094979,88.2835627033099,
76.658382386414));
#121213=CARTESIAN_POINT('Ctrl Pts',(-11.1183051004929,88.0466951245799,
77.428862016883));
#121214=CARTESIAN_POINT('Ctrl Pts',(-11.1527080864609,87.7600489942401,
78.196068193518));
#121215=CARTESIAN_POINT('Ctrl Pts',(-11.1750828468669,87.42966285556,78.941086404059));
#121216=CARTESIAN_POINT('Ctrl Pts',(-11.1820923536469,87.0683400052,79.641730697645));
#121217=CARTESIAN_POINT('Ctrl Pts',(-11.1727457911329,86.69122473511,80.282286917317));
#121218=CARTESIAN_POINT('Ctrl Pts',(-11.1481220746969,86.31198160359,80.855947397552));
#121219=CARTESIAN_POINT('Ctrl Pts',(-11.1097562815799,85.9405639758301,
81.363318728113));
#121220=CARTESIAN_POINT('Ctrl Pts',(-11.0596843146889,85.58438097307,81.807939054316));
#121221=CARTESIAN_POINT('Ctrl Pts',(-10.9997169907709,85.2500946837,82.193255543295));
#121222=CARTESIAN_POINT('Ctrl Pts',(-10.9476481892759,85.0127333998599,
82.448325023705));
#121223=CARTESIAN_POINT('Ctrl Pts',(-10.9170561372289,84.88870678709,82.576527099225));
#121224=CARTESIAN_POINT('Ctrl Pts',(-10.9119974436429,84.86856730116,82.597213818352));
#121225=CARTESIAN_POINT('Ctrl Pts',(-11.4334076262239,84.7058852730001,
63.4021229260991));
#121226=CARTESIAN_POINT('Ctrl Pts',(-11.4384281336359,84.72577353141,63.422283368637));
#121227=CARTESIAN_POINT('Ctrl Pts',(-11.4738076598529,84.86833137268,63.5676916393111));
#121228=CARTESIAN_POINT('Ctrl Pts',(-11.5331240407119,85.14051214413,63.857962637228));
#121229=CARTESIAN_POINT('Ctrl Pts',(-11.5992378217001,85.5210751481201,
64.298195710351));
#121230=CARTESIAN_POINT('Ctrl Pts',(-11.6514593274787,85.91618297563,64.798734693346));
#121231=CARTESIAN_POINT('Ctrl Pts',(-11.6884177467697,86.31832604546,65.362584895379));
#121232=CARTESIAN_POINT('Ctrl Pts',(-11.7088853971653,86.7189526464401,
65.991987132611));
#121233=CARTESIAN_POINT('Ctrl Pts',(-11.7118379510303,87.10657313034,66.684546553909));
#121234=CARTESIAN_POINT('Ctrl Pts',(-11.6973592798139,87.46724901606,67.430425724164));
#121235=CARTESIAN_POINT('Ctrl Pts',(-11.6677063303148,87.7872078148999,
68.21187499679));
#121236=CARTESIAN_POINT('Ctrl Pts',(-11.6275693811737,88.0568714128401,
69.008438916133));
#121237=CARTESIAN_POINT('Ctrl Pts',(-11.582721209285,88.2753365204001,69.812913501992));
#121238=CARTESIAN_POINT('Ctrl Pts',(-11.5394764818229,88.44224391384,70.617568177949));
#121239=CARTESIAN_POINT('Ctrl Pts',(-11.5043921904999,88.55733668999,71.4088842175801));
#121240=CARTESIAN_POINT('Ctrl Pts',(-11.4820942729849,88.62361512615,72.1695141058363));
#121241=CARTESIAN_POINT('Ctrl Pts',(-11.4736921131039,88.64744151544,72.8976469313896));
#121242=CARTESIAN_POINT('Ctrl Pts',(-11.4786272848249,88.63348875016,73.612004070298));
#121243=CARTESIAN_POINT('Ctrl Pts',(-11.4963735631779,88.58160440959,74.334975761448));
#121244=CARTESIAN_POINT('Ctrl Pts',(-11.5259553584829,88.48805634354,75.076751346021));
#121245=CARTESIAN_POINT('Ctrl Pts',(-11.5643401913829,88.34964052366,75.83152869767));
#121246=CARTESIAN_POINT('Ctrl Pts',(-11.6067999626929,88.16450527128,76.594015687991));
#121247=CARTESIAN_POINT('Ctrl Pts',(-11.6481137161238,87.93058808465,77.360828340916));
#121248=CARTESIAN_POINT('Ctrl Pts',(-11.6828288814868,87.64568228453,78.127539128295));
#121249=CARTESIAN_POINT('Ctrl Pts',(-11.7054934028938,87.3154663606801,
78.874524071436));
#121250=CARTESIAN_POINT('Ctrl Pts',(-11.7126190573528,86.95265177104,79.578735256338));
#121251=CARTESIAN_POINT('Ctrl Pts',(-11.7031198632119,86.57247347689,80.2238099822379));
#121252=CARTESIAN_POINT('Ctrl Pts',(-11.6779789498894,86.1883870293801,
80.8030245735091));
#121253=CARTESIAN_POINT('Ctrl Pts',(-11.6386935480217,85.81075877209,81.316300792395));
#121254=CARTESIAN_POINT('Ctrl Pts',(-11.5871609929257,85.44651420014,81.767814318776));
#121255=CARTESIAN_POINT('Ctrl Pts',(-11.5251031442909,85.10253986725,82.16069340561));
#121256=CARTESIAN_POINT('Ctrl Pts',(-11.4708398731529,84.85643753722,82.422175114672));
#121257=CARTESIAN_POINT('Ctrl Pts',(-11.4387608790089,84.7270567674,82.554194043774));
#121258=CARTESIAN_POINT('Ctrl Pts',(-11.4334511980329,84.70602607796,82.575513314783));
#121259=CARTESIAN_POINT('Ctrl Pts',(-11.6998099956741,84.3301713905001,
63.6965256689001));
#121260=CARTESIAN_POINT('Ctrl Pts',(-11.7049514850605,84.34993837856,63.71642164007));
#121261=CARTESIAN_POINT('Ctrl Pts',(-11.7411683234158,84.49155421921,63.859866042207));
#121262=CARTESIAN_POINT('Ctrl Pts',(-11.8016921928089,84.76097528105,64.14545510258));
#121263=CARTESIAN_POINT('Ctrl Pts',(-11.8689091125722,85.1360255796801,
64.5772345678011));
#121264=CARTESIAN_POINT('Ctrl Pts',(-11.921845642321,85.52396286686,65.066927135476));
#121265=CARTESIAN_POINT('Ctrl Pts',(-11.9592305896123,85.91766516084,65.617595936977));
#121266=CARTESIAN_POINT('Ctrl Pts',(-11.9798957937884,86.30888526874,66.2314198083571));
#121267=CARTESIAN_POINT('Ctrl Pts',(-11.9828668723107,86.6864950662899,
66.905995485085));
#121268=CARTESIAN_POINT('Ctrl Pts',(-11.9682792828025,87.0369737321501,
67.63156738817));
#121269=CARTESIAN_POINT('Ctrl Pts',(-11.9384581314933,87.3469819707,68.3905258639001));
#121270=CARTESIAN_POINT('Ctrl Pts',(-11.898179052113,87.6073349610399,69.1625064764761));
#121271=CARTESIAN_POINT('Ctrl Pts',(-11.8532865053112,87.81739160382,69.940065705042));
#121272=CARTESIAN_POINT('Ctrl Pts',(-11.8101239477353,87.9771542765201,
70.715405132558));
#121273=CARTESIAN_POINT('Ctrl Pts',(-11.7752046363583,88.08685253399,71.475595648902));
#121274=CARTESIAN_POINT('Ctrl Pts',(-11.7530593036793,88.14982244754,72.204598786874));
#121275=CARTESIAN_POINT('Ctrl Pts',(-11.7447241624273,88.17242101204,72.9015623720751));
#121276=CARTESIAN_POINT('Ctrl Pts',(-11.749619003257,88.1591906022601,73.585256804372));
#121277=CARTESIAN_POINT('Ctrl Pts',(-11.7672373901261,88.10992352232,74.277872782123));
#121278=CARTESIAN_POINT('Ctrl Pts',(-11.7966578892543,88.0208597083,74.989867717288));
#121279=CARTESIAN_POINT('Ctrl Pts',(-11.8349276262727,87.88858761723,75.716278183036));
#121280=CARTESIAN_POINT('Ctrl Pts',(-11.8773754599393,87.71092602096,76.452256402395));
#121281=CARTESIAN_POINT('Ctrl Pts',(-11.9187847295823,87.48552957653,77.194453959513));
#121282=CARTESIAN_POINT('Ctrl Pts',(-11.9536593825615,87.20997814688,77.938304641709));
#121283=CARTESIAN_POINT('Ctrl Pts',(-11.9764719383746,86.88958404568,78.664370660746));
#121284=CARTESIAN_POINT('Ctrl Pts',(-11.9836569308835,86.5366335335601,
79.349806919033));
#121285=CARTESIAN_POINT('Ctrl Pts',(-11.9740797596092,86.16596285257,79.978374486369));
#121286=CARTESIAN_POINT('Ctrl Pts',(-11.9486746184099,85.79051571235,80.543594155305));
#121287=CARTESIAN_POINT('Ctrl Pts',(-11.9089194026789,85.42058120531,81.045011693211));
#121288=CARTESIAN_POINT('Ctrl Pts',(-11.8566406556977,85.06261365341,81.487031944037));
#121289=CARTESIAN_POINT('Ctrl Pts',(-11.7935147903732,84.72342073508,81.872514837236));
#121290=CARTESIAN_POINT('Ctrl Pts',(-11.7381303986936,84.47973974133,82.129835708481));
#121291=CARTESIAN_POINT('Ctrl Pts',(-11.7052917488689,84.35121274205,82.260073941226));
#121292=CARTESIAN_POINT('Ctrl Pts',(-11.6998538423245,84.33030929138,82.281114592639));
#121293=CARTESIAN_POINT('Ctrl Pts',(-11.5463481159819,83.97372753764,64.081494764462));
#121294=CARTESIAN_POINT('Ctrl Pts',(-11.5514199133399,83.99248592696,64.100429046463));
#121295=CARTESIAN_POINT('Ctrl Pts',(-11.5871544155405,84.12690339444,64.236961386833));
#121296=CARTESIAN_POINT('Ctrl Pts',(-11.6469827075615,84.38299314048,64.509078924552));
#121297=CARTESIAN_POINT('Ctrl Pts',(-11.7135641609422,84.74011310431,64.921007397318));
#121298=CARTESIAN_POINT('Ctrl Pts',(-11.7660887989998,85.1100555127999,
65.388659305653));
#121299=CARTESIAN_POINT('Ctrl Pts',(-11.803228043564,85.48593260363,65.914912709119));
#121300=CARTESIAN_POINT('Ctrl Pts',(-11.8237794462954,85.8598226158,66.501853529596));
#121301=CARTESIAN_POINT('Ctrl Pts',(-11.8267398536336,86.2210550814401,
67.147209825903));
#121302=CARTESIAN_POINT('Ctrl Pts',(-11.8122150068324,86.5566733499299,
67.84171552602));
#121303=CARTESIAN_POINT('Ctrl Pts',(-11.7824907486777,86.8538867813,68.568647494553));
#121304=CARTESIAN_POINT('Ctrl Pts',(-11.7422935438457,87.10385264418,69.308693118078));
#121305=CARTESIAN_POINT('Ctrl Pts',(-11.697426559345,87.30586554635,70.054895804105));
#121306=CARTESIAN_POINT('Ctrl Pts',(-11.6542166675608,87.4597919165999,
70.799898497466));
#121307=CARTESIAN_POINT('Ctrl Pts',(-11.6192023189939,87.56566634817,71.531240114491));
#121308=CARTESIAN_POINT('Ctrl Pts',(-11.596969089365,87.62652087531,72.2332458051846));
#121309=CARTESIAN_POINT('Ctrl Pts',(-11.5885953418317,87.6483754722201,
72.9047487270023));
#121310=CARTESIAN_POINT('Ctrl Pts',(-11.5935134153919,87.63557929833,73.5634998632841));
#121311=CARTESIAN_POINT('Ctrl Pts',(-11.6112054745317,87.5879564959899,
74.230581459377));
#121312=CARTESIAN_POINT('Ctrl Pts',(-11.640718888804,87.50195800566,74.91579255546));
#121313=CARTESIAN_POINT('Ctrl Pts',(-11.6790549271481,87.37443216287,75.614119392195));
#121314=CARTESIAN_POINT('Ctrl Pts',(-11.7215096375298,87.2034378446199,
76.320805814706));
#121315=CARTESIAN_POINT('Ctrl Pts',(-11.7628638847739,86.98686102094,77.03266861722));
#121316=CARTESIAN_POINT('Ctrl Pts',(-11.7976466644359,86.72249079514,77.7454371892611));
#121317=CARTESIAN_POINT('Ctrl Pts',(-11.8203739445878,86.4154937219899,
78.4406404007131));
#121318=CARTESIAN_POINT('Ctrl Pts',(-11.827524755236,86.0776605602099,79.096575274848));
#121319=CARTESIAN_POINT('Ctrl Pts',(-11.817992502922,85.72318611707,79.697822394072));
#121320=CARTESIAN_POINT('Ctrl Pts',(-11.7927395709794,85.36451608399,80.23815625388));
#121321=CARTESIAN_POINT('Ctrl Pts',(-11.753254992926,85.0114198651101,80.717288073687));
#121322=CARTESIAN_POINT('Ctrl Pts',(-11.7014060920064,84.67018455978,81.139301715589));
#121323=CARTESIAN_POINT('Ctrl Pts',(-11.6388954608823,84.34728442778,81.507005378146));
#121324=CARTESIAN_POINT('Ctrl Pts',(-11.5841568940353,84.11568916058,81.752166503278));
#121325=CARTESIAN_POINT('Ctrl Pts',(-11.5517558461319,83.99369566282,81.876128141433));
#121326=CARTESIAN_POINT('Ctrl Pts',(-11.5463918043089,83.97385917525,81.896151373524));
#121327=CARTESIAN_POINT('Ctrl Pts',(-11.3928862362889,83.6172836847901,
64.466463860024));
#121328=CARTESIAN_POINT('Ctrl Pts',(-11.3978883416199,83.63503347536,64.4844364528561));
#121329=CARTESIAN_POINT('Ctrl Pts',(-11.4331405076649,83.76225256968,64.61405673146));
#121330=CARTESIAN_POINT('Ctrl Pts',(-11.4922732223139,84.00501099991,64.8727027465231));
#121331=CARTESIAN_POINT('Ctrl Pts',(-11.5582192093119,84.34420062893,65.2647802268361));
#121332=CARTESIAN_POINT('Ctrl Pts',(-11.6103319556786,84.69614815874,65.710391475831));
#121333=CARTESIAN_POINT('Ctrl Pts',(-11.6472254975157,85.05420004642,66.21222948126));
#121334=CARTESIAN_POINT('Ctrl Pts',(-11.6676630988025,85.41075996287,66.7722872508351));
#121335=CARTESIAN_POINT('Ctrl Pts',(-11.6706128349566,85.75561509659,67.388424166722));
#121336=CARTESIAN_POINT('Ctrl Pts',(-11.6561507308623,86.0763729677001,
68.05186366387));
#121337=CARTESIAN_POINT('Ctrl Pts',(-11.6265233658621,86.3607915919,68.746769125207));
#121338=CARTESIAN_POINT('Ctrl Pts',(-11.5864080355784,86.6003703273101,
69.45487975968));
#121339=CARTESIAN_POINT('Ctrl Pts',(-11.5415666133789,86.79433948889,70.169725903168));
#121340=CARTESIAN_POINT('Ctrl Pts',(-11.4983093873859,86.94242955668,70.884391862373));
#121341=CARTESIAN_POINT('Ctrl Pts',(-11.4632000016299,87.04448016234,71.58688458008));
#121342=CARTESIAN_POINT('Ctrl Pts',(-11.4408788750509,87.1032193030901,
72.2618928234953));
#121343=CARTESIAN_POINT('Ctrl Pts',(-11.4324665212359,87.12432993239,72.9079350819296));
#121344=CARTESIAN_POINT('Ctrl Pts',(-11.4374078275269,87.1119679944,73.5417429221963));
#121345=CARTESIAN_POINT('Ctrl Pts',(-11.4551735589369,87.06598946966,74.183290136631));
#121346=CARTESIAN_POINT('Ctrl Pts',(-11.4847798883539,86.98305630301,74.841717393632));
#121347=CARTESIAN_POINT('Ctrl Pts',(-11.5231822280239,86.8602767085,75.5119606013541));
#121348=CARTESIAN_POINT('Ctrl Pts',(-11.5656438151199,86.69594966828,76.189355227018));
#121349=CARTESIAN_POINT('Ctrl Pts',(-11.6069430399654,86.48819246535,76.870883274928));
#121350=CARTESIAN_POINT('Ctrl Pts',(-11.6416339463103,86.2350034433901,
77.552569736814));
#121351=CARTESIAN_POINT('Ctrl Pts',(-11.6642759508009,85.9414033983,78.216910140681));
#121352=CARTESIAN_POINT('Ctrl Pts',(-11.6713925795885,85.61868758687,78.843343630664));
#121353=CARTESIAN_POINT('Ctrl Pts',(-11.6619052462348,85.28040938158,79.417270301776));
#121354=CARTESIAN_POINT('Ctrl Pts',(-11.6368045235489,84.9385164556401,
79.9327183524551));
#121355=CARTESIAN_POINT('Ctrl Pts',(-11.5975905831731,84.60225852491,80.3895644541621));
#121356=CARTESIAN_POINT('Ctrl Pts',(-11.5461715283149,84.27775546615,80.791571487141));
#121357=CARTESIAN_POINT('Ctrl Pts',(-11.4842761313909,83.97114812048,81.1414959190551));
#121358=CARTESIAN_POINT('Ctrl Pts',(-11.4301833893769,83.7516385798401,
81.374497298075));
#121359=CARTESIAN_POINT('Ctrl Pts',(-11.3982199433949,83.63617858359,81.49218234164));
#121360=CARTESIAN_POINT('Ctrl Pts',(-11.3929297662929,83.61740905912,81.511188154409));
#121361=CARTESIAN_POINT('Ctrl Pts',(-10.9145013594719,83.50062863623,64.703833009367));
#121362=CARTESIAN_POINT('Ctrl Pts',(-10.9192862146809,83.51710648279,64.720741657142));
#121363=CARTESIAN_POINT('Ctrl Pts',(-10.9530348000159,83.6353242016,64.842777920554));
#121364=CARTESIAN_POINT('Ctrl Pts',(-11.0099991996659,83.86242730732,65.087497166191));
#121365=CARTESIAN_POINT('Ctrl Pts',(-11.0739642549319,84.18236181444,65.460607352468));
#121366=CARTESIAN_POINT('Ctrl Pts',(-11.1247930162699,84.51662290047,65.886619447888));
#121367=CARTESIAN_POINT('Ctrl Pts',(-11.1609206319429,84.85849295892,66.367912971536));
#121368=CARTESIAN_POINT('Ctrl Pts',(-11.1810034813509,85.20052067337,66.906414565492));
#121369=CARTESIAN_POINT('Ctrl Pts',(-11.1839199523509,85.53276388586,67.500173427059));
#121370=CARTESIAN_POINT('Ctrl Pts',(-11.1696534353449,85.84319176642,68.1410073089521));
#121371=CARTESIAN_POINT('Ctrl Pts',(-11.1403281142129,86.1198870157801,
68.81416418141));
#121372=CARTESIAN_POINT('Ctrl Pts',(-11.1004680104759,86.3544282397101,
69.502745154234));
#121373=CARTESIAN_POINT('Ctrl Pts',(-11.0557062733309,86.54569475296,70.2011927159229));
#121374=CARTESIAN_POINT('Ctrl Pts',(-11.0123014929789,86.6928676434501,
70.9032686830991));
#121375=CARTESIAN_POINT('Ctrl Pts',(-10.9768958489299,86.7950307772,71.597036884302));
#121376=CARTESIAN_POINT('Ctrl Pts',(-10.9543007222439,86.85415637997,72.2663793166297));
#121377=CARTESIAN_POINT('Ctrl Pts',(-10.9457680215319,86.87546716438,72.9084210698479));
#121378=CARTESIAN_POINT('Ctrl Pts',(-10.9507817509339,86.86298269682,73.5384365296263));
#121379=CARTESIAN_POINT('Ctrl Pts',(-10.9687771400309,86.81665821225,74.175067882143));
#121380=CARTESIAN_POINT('Ctrl Pts',(-10.9986731127109,86.73347503727,74.826278291994));
#121381=CARTESIAN_POINT('Ctrl Pts',(-11.0372821327079,86.61110788032,75.4860954416901));
#121382=CARTESIAN_POINT('Ctrl Pts',(-11.0797651565069,86.44851693899,76.149537007965));
#121383=CARTESIAN_POINT('Ctrl Pts',(-11.1208928606869,86.24442185857,76.813777645638));
#121384=CARTESIAN_POINT('Ctrl Pts',(-11.1552973714429,85.99732347199,77.475389357107));
#121385=CARTESIAN_POINT('Ctrl Pts',(-11.1776735471369,85.71240740907,78.118016760138));
#121386=CARTESIAN_POINT('Ctrl Pts',(-11.1846836212209,85.4007096691001,
78.722473835778));
#121387=CARTESIAN_POINT('Ctrl Pts',(-11.1753363132029,85.07529630638,79.275168931218));
#121388=CARTESIAN_POINT('Ctrl Pts',(-11.1507100706079,84.7479389048601,
79.770236225873));
#121389=CARTESIAN_POINT('Ctrl Pts',(-11.1123397858179,84.4272465671801,
80.208156931037));
#121390=CARTESIAN_POINT('Ctrl Pts',(-11.0622606849319,84.11957935255,80.5920213789121));
#121391=CARTESIAN_POINT('Ctrl Pts',(-11.0022831502009,83.830696414,80.9247829028901));
#121392=CARTESIAN_POINT('Ctrl Pts',(-10.9502036301909,83.6254599932199,
81.145148417673));
#121393=CARTESIAN_POINT('Ctrl Pts',(-10.9196043154289,83.51817119103,81.255944067916));
#121394=CARTESIAN_POINT('Ctrl Pts',(-10.9145443959369,83.50074826293,81.2738231017611));
#121395=CARTESIAN_POINT('Ctrl Pts',(-10.4071527116419,83.69593260378,64.646750601693));
#121396=CARTESIAN_POINT('Ctrl Pts',(-10.4117071633399,83.71166206633,64.663151272416));
#121397=CARTESIAN_POINT('Ctrl Pts',(-10.4438611337989,83.82464422908,64.78162352002));
#121398=CARTESIAN_POINT('Ctrl Pts',(-10.4985259380069,84.04345337825,65.020576732323));
#121399=CARTESIAN_POINT('Ctrl Pts',(-10.5603901261999,84.35472041601,65.387337694065));
#121400=CARTESIAN_POINT('Ctrl Pts',(-10.6098571637469,84.6825454490501,
65.808317421142));
#121401=CARTESIAN_POINT('Ctrl Pts',(-10.6451724803229,85.0198881580799,
66.285647498717));
#121402=CARTESIAN_POINT('Ctrl Pts',(-10.6648790994309,85.3591721061099,
66.821255809763));
#121403=CARTESIAN_POINT('Ctrl Pts',(-10.6677602912409,85.6903713424199,
67.41332242683));
#121404=CARTESIAN_POINT('Ctrl Pts',(-10.6537012031249,86.00139042658,68.05399654853));
#121405=CARTESIAN_POINT('Ctrl Pts',(-10.6246962130819,86.28021190296,68.729137806898));
#121406=CARTESIAN_POINT('Ctrl Pts',(-10.5851067885619,86.5181817555,69.42267673283));
#121407=CARTESIAN_POINT('Ctrl Pts',(-10.5404295609959,86.71375874238,70.129828876235));
#121408=CARTESIAN_POINT('Ctrl Pts',(-10.4968682926189,86.86550100478,70.84485056109));
#121409=CARTESIAN_POINT('Ctrl Pts',(-10.4611484533439,86.97164340359,71.555416167859));
#121410=CARTESIAN_POINT('Ctrl Pts',(-10.4382627372379,87.0334182268699,
72.2439296553813));
#121411=CARTESIAN_POINT('Ctrl Pts',(-10.4296024032359,87.0557494604799,
72.9059060278074));
#121412=CARTESIAN_POINT('Ctrl Pts',(-10.4346929406019,87.0426615024399,
73.5556262297241));
#121413=CARTESIAN_POINT('Ctrl Pts',(-10.4529318919879,86.9942148532899,
74.211001504031));
#121414=CARTESIAN_POINT('Ctrl Pts',(-10.4831350443589,86.907621009,74.879026858038));
#121415=CARTESIAN_POINT('Ctrl Pts',(-10.5219632581269,86.7810773188199,
75.552525741454));
#121416=CARTESIAN_POINT('Ctrl Pts',(-10.5644690165089,86.61421723637,76.225985233305));
#121417=CARTESIAN_POINT('Ctrl Pts',(-10.6054148153219,86.40636115899,76.896680893526));
#121418=CARTESIAN_POINT('Ctrl Pts',(-10.6395155906909,86.1564947859499,
77.561644728154));
#121419=CARTESIAN_POINT('Ctrl Pts',(-10.6616098430089,85.87017719721,78.205141976549));
#121420=CARTESIAN_POINT('Ctrl Pts',(-10.6685069110429,85.55858177196,78.808743611411));
#121421=CARTESIAN_POINT('Ctrl Pts',(-10.6593081061829,85.2347428489799,
79.359431202932));
#121422=CARTESIAN_POINT('Ctrl Pts',(-10.6351850710339,84.9106867918599,
79.85123162298));
#121423=CARTESIAN_POINT('Ctrl Pts',(-10.5977095208839,84.59465748902,80.285295703793));
#121424=CARTESIAN_POINT('Ctrl Pts',(-10.5490515013679,84.29351399509,80.664105744214));
#121425=CARTESIAN_POINT('Ctrl Pts',(-10.4911079456309,84.01282164204,80.99093874636));
#121426=CARTESIAN_POINT('Ctrl Pts',(-10.4411635379779,83.81521547721,81.206009625821));
#121427=CARTESIAN_POINT('Ctrl Pts',(-10.4120109456419,83.71268034274,81.313565299678));
#121428=CARTESIAN_POINT('Ctrl Pts',(-10.4071952246869,83.69605055436,81.330905291903));
#121429=CARTESIAN_POINT('Origin',(-10.7325537287249,84.40089372352,64.155250052704));
#121430=CARTESIAN_POINT('Ctrl Pts',(-10.1996916360579,82.23193715457,61.24897010379));
#121431=CARTESIAN_POINT('Ctrl Pts',(-10.2310626160719,82.36225161932,61.32924567366));
#121432=CARTESIAN_POINT('Ctrl Pts',(-10.2941931732499,82.6227313586901,
61.49574862112));
#121433=CARTESIAN_POINT('Ctrl Pts',(-10.3879051058939,83.00658407806,61.75970657116));
#121434=CARTESIAN_POINT('Ctrl Pts',(-10.4803285035579,83.38463777582,62.03908119861));
#121435=CARTESIAN_POINT('Ctrl Pts',(-10.5704060709779,83.7545051675001,
62.33244822809));
#121436=CARTESIAN_POINT('Ctrl Pts',(-10.6577144882509,84.1159531733799,
62.6399145318601));
#121437=CARTESIAN_POINT('Ctrl Pts',(-10.7418927390509,84.46869818965,62.96159914678));
#121438=CARTESIAN_POINT('Ctrl Pts',(-10.8226586546719,84.81239048239,63.297613065143));
#121439=CARTESIAN_POINT('Ctrl Pts',(-10.8743262685519,85.03625004551,63.532334707995));
#121440=CARTESIAN_POINT('Ctrl Pts',(-10.8997056579209,85.14730307016,63.6530190115981));
#121441=CARTESIAN_POINT('Ctrl Pts',(-10.9000935484179,85.14900063192,63.654864808037));
#121442=CARTESIAN_POINT('Ctrl Pts',(-10.7444499634089,82.08330821913,61.26232339111));
#121443=CARTESIAN_POINT('Ctrl Pts',(-10.7758793664039,82.21370125987,61.34109026097));
#121444=CARTESIAN_POINT('Ctrl Pts',(-10.8391966950829,82.47465383373,61.5047240749901));
#121445=CARTESIAN_POINT('Ctrl Pts',(-10.9333652704749,82.86001665981,61.76490805656));
#121446=CARTESIAN_POINT('Ctrl Pts',(-11.0264060300299,83.24030836404,62.04107449498));
#121447=CARTESIAN_POINT('Ctrl Pts',(-11.1172082967379,83.61293379475,62.3317633769501));
#121448=CARTESIAN_POINT('Ctrl Pts',(-11.2053255419869,83.97757037,62.63708798503));
#121449=CARTESIAN_POINT('Ctrl Pts',(-11.2903576554999,84.33378428946,62.9571076));
#121450=CARTESIAN_POINT('Ctrl Pts',(-11.3719979235199,84.6811296404201,
63.291900810757));
#121451=CARTESIAN_POINT('Ctrl Pts',(-11.4242452127629,84.9074793665401,
63.526053666644));
#121452=CARTESIAN_POINT('Ctrl Pts',(-11.4499125748089,85.01978652385,63.646508605745));
#121453=CARTESIAN_POINT('Ctrl Pts',(-11.4503048673419,85.0215032608,63.648350908626));
#121454=CARTESIAN_POINT('Ctrl Pts',(-11.0477573137059,81.77845564567,61.6285201490101));
#121455=CARTESIAN_POINT('Ctrl Pts',(-11.0792192451059,81.9049119093501,
61.70398277631));
#121456=CARTESIAN_POINT('Ctrl Pts',(-11.1426405633259,82.15817371936,61.86090998634));
#121457=CARTESIAN_POINT('Ctrl Pts',(-11.2370633855929,82.53266234296,62.11089922386));
#121458=CARTESIAN_POINT('Ctrl Pts',(-11.3304478762849,82.90266797425,62.3767193705));
#121459=CARTESIAN_POINT('Ctrl Pts',(-11.4216536368169,83.2655510331,62.65693374751));
#121460=CARTESIAN_POINT('Ctrl Pts',(-11.5102212165679,83.62094552581,62.9516559917));
#121461=CARTESIAN_POINT('Ctrl Pts',(-11.5957287387605,83.9683415161201,
63.2609080093));
#121462=CARTESIAN_POINT('Ctrl Pts',(-11.6778558235873,84.3072494738502,
63.584746703615));
#121463=CARTESIAN_POINT('Ctrl Pts',(-11.730425861083,84.52816616381,63.81140761883));
#121464=CARTESIAN_POINT('Ctrl Pts',(-11.7562535588696,84.6377886984001,
63.9280461233941));
#121465=CARTESIAN_POINT('Ctrl Pts',(-11.7566483023413,84.63946440061,63.929830064275));
#121466=CARTESIAN_POINT('Ctrl Pts',(-10.9126225976289,81.5153741101001,
62.10972407656));
#121467=CARTESIAN_POINT('Ctrl Pts',(-10.9440700364139,81.63643508906,62.18223294764));
#121468=CARTESIAN_POINT('Ctrl Pts',(-11.0074450234219,81.8788375096601,
62.33297186689));
#121469=CARTESIAN_POINT('Ctrl Pts',(-11.1017545692409,82.23713016388,62.57296683459));
#121470=CARTESIAN_POINT('Ctrl Pts',(-11.1949859149149,82.5910062086201,
62.82802226324));
#121471=CARTESIAN_POINT('Ctrl Pts',(-11.2860119039269,82.93797392928,63.096768725873));
#121472=CARTESIAN_POINT('Ctrl Pts',(-11.3743788428919,83.2776982057901,
63.379313927409));
#121473=CARTESIAN_POINT('Ctrl Pts',(-11.4596745528199,83.6097164751,63.675689054981));
#121474=CARTESIAN_POINT('Ctrl Pts',(-11.5415847426359,83.93357647935,63.9859541283691));
#121475=CARTESIAN_POINT('Ctrl Pts',(-11.5940109837696,84.14466556495,64.203065790909));
#121476=CARTESIAN_POINT('Ctrl Pts',(-11.619767246015,84.2494083216699,64.314779476617));
#121477=CARTESIAN_POINT('Ctrl Pts',(-11.620160897502,84.2510094303001,64.31648809182));
#121478=CARTESIAN_POINT('Ctrl Pts',(-10.7774878815529,81.25229257453,62.59092800412));
#121479=CARTESIAN_POINT('Ctrl Pts',(-10.8089208277219,81.3679582687801,
62.6604831189601));
#121480=CARTESIAN_POINT('Ctrl Pts',(-10.8722494835169,81.59950129996,62.80503374744));
#121481=CARTESIAN_POINT('Ctrl Pts',(-10.9664457528889,81.9415979848,63.035034445325));
#121482=CARTESIAN_POINT('Ctrl Pts',(-11.0595239535449,82.27934444298,63.279325155982));
#121483=CARTESIAN_POINT('Ctrl Pts',(-11.1503701710379,82.6103968254701,
63.536603704234));
#121484=CARTESIAN_POINT('Ctrl Pts',(-11.2385364692169,82.9344508857701,
63.8069718631161));
#121485=CARTESIAN_POINT('Ctrl Pts',(-11.3236203668789,83.2510914340801,
64.090470100661));
#121486=CARTESIAN_POINT('Ctrl Pts',(-11.4053136616849,83.55990348484,64.387161553123));
#121487=CARTESIAN_POINT('Ctrl Pts',(-11.4575961064559,83.7611649660901,
64.5947239629891));
#121488=CARTESIAN_POINT('Ctrl Pts',(-11.4832809331599,83.8610279449301,
64.701512829841));
#121489=CARTESIAN_POINT('Ctrl Pts',(-11.4836734926629,83.86255445999,64.703146119366));
#121490=CARTESIAN_POINT('Ctrl Pts',(-10.2916779629739,81.20184743248,62.87460831108));
#121491=CARTESIAN_POINT('Ctrl Pts',(-10.3230588081249,81.3141634466501,
62.9434785522));
#121492=CARTESIAN_POINT('Ctrl Pts',(-10.3862209030019,81.53873138438,63.086378354437));
#121493=CARTESIAN_POINT('Ctrl Pts',(-10.4800099430289,81.86982923944,63.313076303186));
#121494=CARTESIAN_POINT('Ctrl Pts',(-10.5725375866489,82.19607838981,63.5531753043091));
#121495=CARTESIAN_POINT('Ctrl Pts',(-10.6627375247109,82.51537911082,63.805440673177));
#121496=CARTESIAN_POINT('Ctrl Pts',(-10.7501825183529,82.82751226324,64.069965817418));
#121497=CARTESIAN_POINT('Ctrl Pts',(-10.8345049499589,83.13220277182,64.3468411136921));
#121498=CARTESIAN_POINT('Ctrl Pts',(-10.9154185062159,83.42912960561,64.636155592722));
#121499=CARTESIAN_POINT('Ctrl Pts',(-10.9671840024129,83.6225517154301,
64.838313456043));
#121500=CARTESIAN_POINT('Ctrl Pts',(-10.9926120180209,83.7185090637701,
64.942267675345));
#121501=CARTESIAN_POINT('Ctrl Pts',(-10.9930006518329,83.7199758732201,
64.943857597795));
#121502=CARTESIAN_POINT('Ctrl Pts',(-9.77071511647392,81.39680163372,62.77652121756));
#121503=CARTESIAN_POINT('Ctrl Pts',(-9.80204009060491,81.50998911196,62.84742027707));
#121504=CARTESIAN_POINT('Ctrl Pts',(-9.86502357231191,81.73599641365,62.994278890954));
#121505=CARTESIAN_POINT('Ctrl Pts',(-9.95837591611191,82.06843606335,63.226510670207));
#121506=CARTESIAN_POINT('Ctrl Pts',(-10.0503131647039,82.39528741943,63.471713388376));
#121507=CARTESIAN_POINT('Ctrl Pts',(-10.1398200589239,82.71463258723,63.728676256591));
#121508=CARTESIAN_POINT('Ctrl Pts',(-10.2264915548459,83.02633649328,63.997487316694));
#121509=CARTESIAN_POINT('Ctrl Pts',(-10.3099974211469,83.33026591704,64.278295067199));
#121510=CARTESIAN_POINT('Ctrl Pts',(-10.3900748174189,83.62618944315,64.57122039344));
#121511=CARTESIAN_POINT('Ctrl Pts',(-10.4412859589379,83.8188519043601,
64.775628543979));
#121512=CARTESIAN_POINT('Ctrl Pts',(-10.4664385807459,83.91441438601,64.880679324874));
#121513=CARTESIAN_POINT('Ctrl Pts',(-10.4668230048079,83.91587515524,64.882286004762));
#121514=CARTESIAN_POINT('Origin',(-10.0948816704592,81.9241950980305,62.1047057712127));
#121515=CARTESIAN_POINT('Ctrl Pts',(-8.7885046972379,74.82640395806,59.1949076002999));
#121516=CARTESIAN_POINT('Ctrl Pts',(-8.78188852469191,75.41917609617,59.18747495118));
#121517=CARTESIAN_POINT('Ctrl Pts',(-8.83939730075691,76.54805897963,59.2464797348));
#121518=CARTESIAN_POINT('Ctrl Pts',(-9.08760907888691,78.10809237206,59.52130962476));
#121519=CARTESIAN_POINT('Ctrl Pts',(-9.4057436642799,79.44978989415,59.90923180518));
#121520=CARTESIAN_POINT('Ctrl Pts',(-9.71792425590291,80.60886585816,60.36713913228));
#121521=CARTESIAN_POINT('Ctrl Pts',(-9.9935632318369,81.61530137155,60.86767974539));
#121522=CARTESIAN_POINT('Ctrl Pts',(-10.1509566002329,82.23504579931,61.23828496981));
#121523=CARTESIAN_POINT('Ctrl Pts',(-10.2198405635139,82.52601067952,61.42758786454));
#121524=CARTESIAN_POINT('Ctrl Pts',(-10.2212128295729,82.53181579063,61.43137091566));
#121525=CARTESIAN_POINT('Ctrl Pts',(-9.36212373100291,74.83407745381,59.25507590285));
#121526=CARTESIAN_POINT('Ctrl Pts',(-9.35580368689491,75.39892771435,59.2482959049099));
#121527=CARTESIAN_POINT('Ctrl Pts',(-9.41070341492091,76.47682878814,59.30190722458));
#121528=CARTESIAN_POINT('Ctrl Pts',(-9.6491407943599,77.97728162386,59.55440424595));
#121529=CARTESIAN_POINT('Ctrl Pts',(-9.96067084052391,79.29224334994,59.91952962683));
#121530=CARTESIAN_POINT('Ctrl Pts',(-10.2718202607539,80.4478475221001,
60.36120446053));
#121531=CARTESIAN_POINT('Ctrl Pts',(-10.5499421585019,81.46357762313,60.85287618631));
#121532=CARTESIAN_POINT('Ctrl Pts',(-10.7105860042159,82.09595442055,61.22299843353));
#121533=CARTESIAN_POINT('Ctrl Pts',(-10.7810231783999,82.39342460616,61.41298176732));
#121534=CARTESIAN_POINT('Ctrl Pts',(-10.7824264415109,82.39935974081,61.41677874076));
#121535=CARTESIAN_POINT('Ctrl Pts',(-9.69865424998491,74.84406498959,59.72344078078));
#121536=CARTESIAN_POINT('Ctrl Pts',(-9.69250793835691,75.3737935536399,
59.71728021895));
#121537=CARTESIAN_POINT('Ctrl Pts',(-9.74587699142391,76.38610626559,59.76584842462));
#121538=CARTESIAN_POINT('Ctrl Pts',(-9.97857993167891,77.8023554124599,
59.99650618733));
#121539=CARTESIAN_POINT('Ctrl Pts',(-10.2862352301719,79.05940149627,60.33596972221));
#121540=CARTESIAN_POINT('Ctrl Pts',(-10.5967796833019,80.17658751631,60.75367197684));
#121541=CARTESIAN_POINT('Ctrl Pts',(-10.8763582603389,81.16624364348,61.22439153817));
#121542=CARTESIAN_POINT('Ctrl Pts',(-11.0389090944099,81.78665342459,61.58260102151));
#121543=CARTESIAN_POINT('Ctrl Pts',(-11.1102575055659,82.07884520387,61.76704808987));
#121544=CARTESIAN_POINT('Ctrl Pts',(-11.1116789540119,82.0846751666,61.7707346179));
#121545=CARTESIAN_POINT('Ctrl Pts',(-9.57270218658391,74.84967733165,60.28631102629));
#121546=CARTESIAN_POINT('Ctrl Pts',(-9.5664908527279,75.36060742374,60.28032181312));
#121547=CARTESIAN_POINT('Ctrl Pts',(-9.6204327859899,76.33665356348,60.32757492156));
#121548=CARTESIAN_POINT('Ctrl Pts',(-9.85528193411291,77.70047199869,60.55151405767));
#121549=CARTESIAN_POINT('Ctrl Pts',(-10.1643874204399,78.90721206905,60.87963793133));
#121550=CARTESIAN_POINT('Ctrl Pts',(-10.4751582924239,79.97676444833,61.28168335215));
#121551=CARTESIAN_POINT('Ctrl Pts',(-10.7541916833579,80.9224412974,61.73340035542));
#121552=CARTESIAN_POINT('Ctrl Pts',(-10.9160287957759,81.51429968327,62.07624595922));
#121553=CARTESIAN_POINT('Ctrl Pts',(-10.9870361615569,81.7929646003,62.25264801673));
#121554=CARTESIAN_POINT('Ctrl Pts',(-10.9884508038439,81.7985246354,62.25617370333));
#121555=CARTESIAN_POINT('Ctrl Pts',(-9.44675012318391,74.8552896737,60.8491812718));
#121556=CARTESIAN_POINT('Ctrl Pts',(-9.44047376709891,75.34742129385,60.84336340728));
#121557=CARTESIAN_POINT('Ctrl Pts',(-9.49498858055591,76.28720086137,60.8893014185));
#121558=CARTESIAN_POINT('Ctrl Pts',(-9.73198393654791,77.59858858492,61.1065219280101));
#121559=CARTESIAN_POINT('Ctrl Pts',(-10.0425396107069,78.75502264184,61.42330614045));
#121560=CARTESIAN_POINT('Ctrl Pts',(-10.3535369015469,79.77694138035,61.80969472745));
#121561=CARTESIAN_POINT('Ctrl Pts',(-10.6320251063769,80.67863895132,62.24240917267));
#121562=CARTESIAN_POINT('Ctrl Pts',(-10.7931484971409,81.24194594195,62.56989089692));
#121563=CARTESIAN_POINT('Ctrl Pts',(-10.8638148175489,81.50708399673,62.73824794359));
#121564=CARTESIAN_POINT('Ctrl Pts',(-10.8652226536749,81.5123741042,62.7416127887499));
#121565=CARTESIAN_POINT('Ctrl Pts',(-8.94267290203492,74.85276791002,61.1295699342099));
#121566=CARTESIAN_POINT('Ctrl Pts',(-8.93613631818291,75.35501471312,61.1233605687));
#121567=CARTESIAN_POINT('Ctrl Pts',(-8.99294387579391,76.31213933141,61.17259229662));
#121568=CARTESIAN_POINT('Ctrl Pts',(-9.23852864643191,77.63798521846,61.4027146666999));
#121569=CARTESIAN_POINT('Ctrl Pts',(-9.55488816876592,78.7854157547301,
61.73007623355));
#121570=CARTESIAN_POINT('Ctrl Pts',(-9.86679161853491,79.78238838433,62.11961002449));
#121571=CARTESIAN_POINT('Ctrl Pts',(-10.1430979147219,80.6516568541701,
62.54799863672));
#121572=CARTESIAN_POINT('Ctrl Pts',(-10.3013648947369,81.18895060113,62.86695544977));
#121573=CARTESIAN_POINT('Ctrl Pts',(-10.3706663053529,81.44137306437,63.030146951985));
#121574=CARTESIAN_POINT('Ctrl Pts',(-10.3720469023069,81.44640927474,63.033408284556));
#121575=CARTESIAN_POINT('Ctrl Pts',(-8.39808036489391,74.84380101246,60.93968441354));
#121576=CARTESIAN_POINT('Ctrl Pts',(-8.39126263741091,75.37830192689,60.9327829084));
#121577=CARTESIAN_POINT('Ctrl Pts',(-8.4505472189839,76.39476622932,60.98771117323));
#121578=CARTESIAN_POINT('Ctrl Pts',(-8.70541178033391,77.79227568178,61.2417147644));
#121579=CARTESIAN_POINT('Ctrl Pts',(-9.0280416363969,78.97803537179,61.59448643167));
#121580=CARTESIAN_POINT('Ctrl Pts',(-9.3409240778179,79.9894572848,62.00386093824));
#121581=CARTESIAN_POINT('Ctrl Pts',(-9.61487309398091,80.85956648621,62.44549770459));
#121582=CARTESIAN_POINT('Ctrl Pts',(-9.7700540786129,81.39080772377,62.76847820377));
#121583=CARTESIAN_POINT('Ctrl Pts',(-9.83788087451691,81.63984223761,62.93284329357));
#121584=CARTESIAN_POINT('Ctrl Pts',(-9.8392320429429,81.64481063107,62.9361277708));
#121585=CARTESIAN_POINT('Ctrl Pts',(-9.07717754188791,74.99992957401,59.27469685199));
#121586=CARTESIAN_POINT('Ctrl Pts',(-9.16720240147935,74.999881575874,59.3170480141486));
#121587=CARTESIAN_POINT('Ctrl Pts',(-9.2540427904884,74.9999918735864,59.3767114129878));
#121588=CARTESIAN_POINT('Ctrl Pts',(-9.40351821239664,75.0001891988783,
59.5255401835567));
#121589=CARTESIAN_POINT('Ctrl Pts',(-9.46580962876118,75.000275896729,59.6145335066942));
#121590=CARTESIAN_POINT('Ctrl Pts',(-9.5544246386494,75.0004147462713,59.8054548367023));
#121591=CARTESIAN_POINT('Ctrl Pts',(-9.58072200049164,75.0004668731721,
59.9070017703396));
#121592=CARTESIAN_POINT('Ctrl Pts',(-9.59905684910332,75.0005382403778,
60.1039339215822));
#121593=CARTESIAN_POINT('Ctrl Pts',(-9.59135343873588,75.000557729544,60.199126681737));
#121594=CARTESIAN_POINT('Ctrl Pts',(-9.55275050059052,75.0005744561138,
60.3716696675297));
#121595=CARTESIAN_POINT('Ctrl Pts',(-9.51915258821925,75.0005694408721,
60.4610758883646));
#121596=CARTESIAN_POINT('Ctrl Pts',(-9.418642837365,75.000528745341,60.6314235011406));
#121597=CARTESIAN_POINT('Ctrl Pts',(-9.35157790424357,75.0004929319658,
60.7120836753024));
#121598=CARTESIAN_POINT('Ctrl Pts',(-9.190050282834,75.0003967133209,60.8470403630041));
#121599=CARTESIAN_POINT('Ctrl Pts',(-9.09577378900069,75.0003364917561,
60.9010033430406));
#121600=CARTESIAN_POINT('Ctrl Pts',(-8.89712916494734,75.0002078724708,
60.9719435463236));
#121601=CARTESIAN_POINT('Ctrl Pts',(-8.79314519935575,75.0001398318208,
60.9889116321));
#121602=CARTESIAN_POINT('Ctrl Pts',(-8.69365830054191,74.99999996484,60.98889557741));
#121603=CARTESIAN_POINT('Ctrl Pts',(-10.2211075019859,67.46805497937,61.43143799722));
#121604=CARTESIAN_POINT('Ctrl Pts',(-10.2201352975039,67.47216669351,61.42875836433));
#121605=CARTESIAN_POINT('Ctrl Pts',(-10.1636464373649,67.71082606018,61.27340384402));
#121606=CARTESIAN_POINT('Ctrl Pts',(-10.0368070785259,68.21698868467,60.96586480023));
#121607=CARTESIAN_POINT('Ctrl Pts',(-9.8163009649119,69.03334101746,60.53842192908));
#121608=CARTESIAN_POINT('Ctrl Pts',(-9.5624403228119,69.96232137517,60.13185886181));
#121609=CARTESIAN_POINT('Ctrl Pts',(-9.2889829848119,71.02203085471,59.76217395547));
#121610=CARTESIAN_POINT('Ctrl Pts',(-9.02433492377792,72.23936277407,59.45104885171));
#121611=CARTESIAN_POINT('Ctrl Pts',(-8.8268115228959,73.64000933415,59.23360212871));
#121612=CARTESIAN_POINT('Ctrl Pts',(-8.78269423684091,74.64578270171,59.1882690656));
#121613=CARTESIAN_POINT('Ctrl Pts',(-8.78852660744491,75.17354115938,59.19489180673));
#121614=CARTESIAN_POINT('Ctrl Pts',(-10.7823632829819,67.60046014905,61.41677523848));
#121615=CARTESIAN_POINT('Ctrl Pts',(-10.7813689778119,67.60466446032,61.41408541359));
#121616=CARTESIAN_POINT('Ctrl Pts',(-10.7235979843399,67.84869045929,61.25815041502));
#121617=CARTESIAN_POINT('Ctrl Pts',(-10.5941274714749,68.3652544873801,
60.95074940909));
#121618=CARTESIAN_POINT('Ctrl Pts',(-10.3707860974499,69.19221319007,60.52861635201));
#121619=CARTESIAN_POINT('Ctrl Pts',(-10.1166516420119,70.12249423931,60.13360637521));
#121620=CARTESIAN_POINT('Ctrl Pts',(-9.8458315563439,71.1722927941801,59.7802070981001));
#121621=CARTESIAN_POINT('Ctrl Pts',(-9.58828414872691,72.3577590955501,
59.48963830056));
#121622=CARTESIAN_POINT('Ctrl Pts',(-9.39873529479691,73.70268390503,59.2901244165301));
#121623=CARTESIAN_POINT('Ctrl Pts',(-9.3566156200659,74.66287447499,59.24892709458));
#121624=CARTESIAN_POINT('Ctrl Pts',(-9.36218740473191,75.16597612265,59.25497557749));
#121625=CARTESIAN_POINT('Ctrl Pts',(-11.1116903071099,67.9151459000001,
61.77071136858));
#121626=CARTESIAN_POINT('Ctrl Pts',(-11.1106830339599,67.9192760147101,
61.76809958451));
#121627=CARTESIAN_POINT('Ctrl Pts',(-11.0521597254649,68.1589905993,61.61669524768));
#121628=CARTESIAN_POINT('Ctrl Pts',(-10.9211453351839,68.6658303921001,
61.31902498468));
#121629=CARTESIAN_POINT('Ctrl Pts',(-10.6961403206129,69.47345397702,60.91344584111));
#121630=CARTESIAN_POINT('Ctrl Pts',(-10.4418452002249,70.37535814882,60.53803008547));
#121631=CARTESIAN_POINT('Ctrl Pts',(-10.1725725702669,71.38604201504,60.20586917915));
#121632=CARTESIAN_POINT('Ctrl Pts',(-9.91919160001691,72.51445318339,59.93722926335));
#121633=CARTESIAN_POINT('Ctrl Pts',(-9.73432195636091,73.7824508557801,
59.75515226462));
#121634=CARTESIAN_POINT('Ctrl Pts',(-9.69337441635991,74.68410470834,59.71782522354));
#121635=CARTESIAN_POINT('Ctrl Pts',(-9.69879329749291,75.15605350359,59.723326013));
#121636=CARTESIAN_POINT('Ctrl Pts',(-10.9885018319529,68.2013323702401,
62.25617620429));
#121637=CARTESIAN_POINT('Ctrl Pts',(-10.9874994096209,68.20527119236,62.25367842127));
#121638=CARTESIAN_POINT('Ctrl Pts',(-10.9292575130169,68.43388414708,62.10888120075));
#121639=CARTESIAN_POINT('Ctrl Pts',(-10.7988206274369,68.91738746191,61.82401663069));
#121640=CARTESIAN_POINT('Ctrl Pts',(-10.5744379163129,69.68868530886,61.43514751277));
#121641=CARTESIAN_POINT('Ctrl Pts',(-10.3202028944559,70.55154216846,61.0742426913));
#121642=CARTESIAN_POINT('Ctrl Pts',(-10.0503514212949,71.52010701642,60.75404721078));
#121643=CARTESIAN_POINT('Ctrl Pts',(-9.7954119483149,72.60448967147,60.49402055406));
#121644=CARTESIAN_POINT('Ctrl Pts',(-9.60879199345991,73.82588143466,60.31720507579));
#121645=CARTESIAN_POINT('Ctrl Pts',(-9.56740600328791,74.6952531657101,
60.28089050002));
#121646=CARTESIAN_POINT('Ctrl Pts',(-9.57288207970592,75.15041957795,60.28623701169));
#121647=CARTESIAN_POINT('Ctrl Pts',(-10.8653133567959,68.4875188404901,
62.74164103999));
#121648=CARTESIAN_POINT('Ctrl Pts',(-10.8643157852829,68.49126637,62.73925725804));
#121649=CARTESIAN_POINT('Ctrl Pts',(-10.8063553005689,68.7087776948599,
62.60106715382));
#121650=CARTESIAN_POINT('Ctrl Pts',(-10.6764959196909,69.16894453172,62.32900827669));
#121651=CARTESIAN_POINT('Ctrl Pts',(-10.4527355120119,69.9039166407,61.95684918442));
#121652=CARTESIAN_POINT('Ctrl Pts',(-10.1985605886859,70.7277261881,61.6104552971401));
#121653=CARTESIAN_POINT('Ctrl Pts',(-9.92813027232292,71.65417201779,61.30222524241));
#121654=CARTESIAN_POINT('Ctrl Pts',(-9.67163229661291,72.69452615956,61.05081184478));
#121655=CARTESIAN_POINT('Ctrl Pts',(-9.48326203055891,73.86931201353,60.87925788696));
#121656=CARTESIAN_POINT('Ctrl Pts',(-9.44143759021592,74.7064016230801,
60.84395577649));
#121657=CARTESIAN_POINT('Ctrl Pts',(-9.44697086191892,75.14478565231,60.84914801039));
#121658=CARTESIAN_POINT('Ctrl Pts',(-10.3721223328469,68.5535152893101,
63.0334650724921));
#121659=CARTESIAN_POINT('Ctrl Pts',(-10.3711441818219,68.55708256,63.031154892722));
#121660=CARTESIAN_POINT('Ctrl Pts',(-10.3143103432349,68.76413802923,62.89722284264));
#121661=CARTESIAN_POINT('Ctrl Pts',(-10.1867630303869,69.20298716651,62.63246721916));
#121662=CARTESIAN_POINT('Ctrl Pts',(-9.96549404468091,69.90897428286,62.26598171184));
#121663=CARTESIAN_POINT('Ctrl Pts',(-9.71155972872991,70.7092203882,61.9192958937501));
#121664=CARTESIAN_POINT('Ctrl Pts',(-9.43881198558591,71.61875463628,61.60574375038));
#121665=CARTESIAN_POINT('Ctrl Pts',(-9.17607446874791,72.6575976508201,
61.34385873668));
#121666=CARTESIAN_POINT('Ctrl Pts',(-8.98069674707291,73.847315957,61.16186671212));
#121667=CARTESIAN_POINT('Ctrl Pts',(-8.93711695024591,74.70000094919,61.12404109137));
#121668=CARTESIAN_POINT('Ctrl Pts',(-8.94287920604192,75.1472140833999,
61.12957580005));
#121669=CARTESIAN_POINT('Ctrl Pts',(-9.83927335193191,68.35511659356,62.93618146194));
#121670=CARTESIAN_POINT('Ctrl Pts',(-9.83831618301491,68.35863537848,62.93385518594));
#121671=CARTESIAN_POINT('Ctrl Pts',(-9.78269958523491,68.56288420959,62.7989800378801));
#121672=CARTESIAN_POINT('Ctrl Pts',(-9.65765025599492,68.99671324753,62.53113343182));
#121673=CARTESIAN_POINT('Ctrl Pts',(-9.43907302986091,69.70047057283,62.15548484121));
#121674=CARTESIAN_POINT('Ctrl Pts',(-9.18539866875291,70.5084201503,61.79389976569));
#121675=CARTESIAN_POINT('Ctrl Pts',(-8.91014715234592,71.4375778106,61.4613028108201));
#121676=CARTESIAN_POINT('Ctrl Pts',(-8.64066836697291,72.5184392530701,
61.17687530567));
#121677=CARTESIAN_POINT('Ctrl Pts',(-8.4377197135399,73.77462645762,60.97573715526));
#121678=CARTESIAN_POINT('Ctrl Pts',(-8.39224341035191,74.68033838347,60.93354232265));
#121679=CARTESIAN_POINT('Ctrl Pts',(-8.39825306306791,75.15607828224,60.93968686544));
#121680=CARTESIAN_POINT('Origin',(-10.0948464627305,68.0757372670146,62.1047362602089));
#121681=CARTESIAN_POINT('Ctrl Pts',(-11.6237407641905,61.21249245617,73.1626298883762));
#121682=CARTESIAN_POINT('Ctrl Pts',(-11.6250359865815,61.20366449265,72.4606436349265));
#121683=CARTESIAN_POINT('Ctrl Pts',(-11.6091550238638,61.29933896423,70.962670779947));
#121684=CARTESIAN_POINT('Ctrl Pts',(-11.5165282050679,61.83819205569,68.625444675657));
#121685=CARTESIAN_POINT('Ctrl Pts',(-11.3260709964139,62.87321223361,66.244698162091));
#121686=CARTESIAN_POINT('Ctrl Pts',(-11.0228468995629,64.33705500443,64.127545184309));
#121687=CARTESIAN_POINT('Ctrl Pts',(-10.6320772268289,66.0053612858,62.46170707634));
#121688=CARTESIAN_POINT('Ctrl Pts',(-10.3400165566969,67.18512894546,61.6081075162));
#121689=CARTESIAN_POINT('Ctrl Pts',(-10.1997669692099,67.76783374115,61.24911703265));
#121690=CARTESIAN_POINT('Ctrl Pts',(-12.1814102453093,61.3021055231,73.1626457611423));
#121691=CARTESIAN_POINT('Ctrl Pts',(-12.1827146639685,61.29320969844,72.4598923200226));
#121692=CARTESIAN_POINT('Ctrl Pts',(-12.1667224102372,61.38959736518,70.961546111832));
#121693=CARTESIAN_POINT('Ctrl Pts',(-12.0733368718683,61.93301542577,68.621592685892));
#121694=CARTESIAN_POINT('Ctrl Pts',(-11.8811272628205,62.9779150684401,
66.2383521195351));
#121695=CARTESIAN_POINT('Ctrl Pts',(-11.574501834705,64.45859748606,64.119339944351));
#121696=CARTESIAN_POINT('Ctrl Pts',(-11.1791162023439,66.1463437687401,
62.45789631767));
#121697=CARTESIAN_POINT('Ctrl Pts',(-10.8850195894329,67.33344051896,61.61471183482));
#121698=CARTESIAN_POINT('Ctrl Pts',(-10.7445184442879,67.91647053246,61.26248407009));
#121699=CARTESIAN_POINT('Ctrl Pts',(-12.4918941626243,61.7739078301301,
73.1573469410713));
#121700=CARTESIAN_POINT('Ctrl Pts',(-12.4932037013295,61.76524338757,72.4756060823452));
#121701=CARTESIAN_POINT('Ctrl Pts',(-12.4771494860403,61.85911084582,71.022812237691));
#121702=CARTESIAN_POINT('Ctrl Pts',(-12.3833415285984,62.38864418025,68.752721416032));
#121703=CARTESIAN_POINT('Ctrl Pts',(-12.1901562661264,63.40750159366,66.4408047023301));
#121704=CARTESIAN_POINT('Ctrl Pts',(-11.8816371380848,64.85297076891,64.3854220064841));
#121705=CARTESIAN_POINT('Ctrl Pts',(-11.4836815583349,66.50072553144,62.77735083217));
#121706=CARTESIAN_POINT('Ctrl Pts',(-11.1884514290469,67.65591813368,61.96612394498));
#121707=CARTESIAN_POINT('Ctrl Pts',(-11.0478102285289,68.2213300947501,
61.6286814152101));
#121708=CARTESIAN_POINT('Ctrl Pts',(-12.3535426183118,62.32147807264,73.1501748512657));
#121709=CARTESIAN_POINT('Ctrl Pts',(-12.354849875526,62.31319397975,72.4975793093326));
#121710=CARTESIAN_POINT('Ctrl Pts',(-12.3388232702892,62.40294462491,71.106678664906));
#121711=CARTESIAN_POINT('Ctrl Pts',(-12.2452035426648,62.9091612469,68.933666728549));
#121712=CARTESIAN_POINT('Ctrl Pts',(-12.0524530310782,63.8829683759799,
66.720569091486));
#121713=CARTESIAN_POINT('Ctrl Pts',(-11.7447777351794,65.26404135376,64.752979132619));
#121714=CARTESIAN_POINT('Ctrl Pts',(-11.3479673232469,66.83834635544,63.212594590931));
#121715=CARTESIAN_POINT('Ctrl Pts',(-11.0532422885309,67.94312234868,62.43411232759));
#121716=CARTESIAN_POINT('Ctrl Pts',(-10.9126634966469,68.48441537841,62.10987498673));
#121717=CARTESIAN_POINT('Ctrl Pts',(-12.2151910739994,62.86904831516,73.1430027614602));
#121718=CARTESIAN_POINT('Ctrl Pts',(-12.2164960497225,62.86114457193,72.5195525363199));
#121719=CARTESIAN_POINT('Ctrl Pts',(-12.2004970545381,62.94677840401,71.190545092121));
#121720=CARTESIAN_POINT('Ctrl Pts',(-12.1070655567313,63.42967831355,69.114612041066));
#121721=CARTESIAN_POINT('Ctrl Pts',(-11.91474979603,64.35843515829,67.000333480642));
#121722=CARTESIAN_POINT('Ctrl Pts',(-11.607918332274,65.67511193861,65.120536258753));
#121723=CARTESIAN_POINT('Ctrl Pts',(-11.2122530881599,67.17596717943,63.647838349687));
#121724=CARTESIAN_POINT('Ctrl Pts',(-10.9180331480149,68.23032656369,62.90210071019));
#121725=CARTESIAN_POINT('Ctrl Pts',(-10.7775167647649,68.74750066206,62.59106855825));
#121726=CARTESIAN_POINT('Ctrl Pts',(-11.7178592045691,63.13675620992,73.1386154569617));
#121727=CARTESIAN_POINT('Ctrl Pts',(-11.7191559790235,63.12913475835,72.5335142827482));
#121728=CARTESIAN_POINT('Ctrl Pts',(-11.7032562336092,63.21172891812,71.242543117047));
#121729=CARTESIAN_POINT('Ctrl Pts',(-11.6105013649466,63.67702362726,69.227855437429));
#121730=CARTESIAN_POINT('Ctrl Pts',(-11.4197484019109,64.5709809274,67.175711181192));
#121731=CARTESIAN_POINT('Ctrl Pts',(-11.1159502589549,65.83590193446,65.350851231036));
#121732=CARTESIAN_POINT('Ctrl Pts',(-10.7244015460629,67.27755256816,63.9161937176));
#121733=CARTESIAN_POINT('Ctrl Pts',(-10.4319972678159,68.29572694252,63.182721088991));
#121734=CARTESIAN_POINT('Ctrl Pts',(-10.2917052246899,68.79794574581,62.87473770978));
#121735=CARTESIAN_POINT('Ctrl Pts',(-11.1845489919669,62.95073358981,73.1398623591238));
#121736=CARTESIAN_POINT('Ctrl Pts',(-11.1858369718499,62.94311303201,72.5303968172997));
#121737=CARTESIAN_POINT('Ctrl Pts',(-11.1700436562049,63.02571883533,71.228901597836));
#121738=CARTESIAN_POINT('Ctrl Pts',(-11.0780143658839,63.49055390038,69.199848762541));
#121739=CARTESIAN_POINT('Ctrl Pts',(-10.8889372575579,64.3825636456,67.1327996899));
#121740=CARTESIAN_POINT('Ctrl Pts',(-10.5883918740969,65.64198311034,65.294341452631));
#121741=CARTESIAN_POINT('Ctrl Pts',(-10.2012574935159,67.07712588928,63.843372013349));
#121742=CARTESIAN_POINT('Ctrl Pts',(-9.91080022709891,68.09684792052,63.093719029673));
#121743=CARTESIAN_POINT('Ctrl Pts',(-9.77074875347191,68.60298807605,62.77664792151));
#121744=CARTESIAN_POINT('Ctrl Pts',(-12.1332042595665,61.479712982889,72.9888456302782));
#121745=CARTESIAN_POINT('Ctrl Pts',(-12.154541208045,61.5021440298757,72.9888417288154));
#121746=CARTESIAN_POINT('Ctrl Pts',(-12.1748167181765,61.5257830744051,
72.9888400206132));
#121747=CARTESIAN_POINT('Ctrl Pts',(-12.1938447273005,61.5504617721141,
72.9888400652945));
#121748=CARTESIAN_POINT('Ctrl Pts',(-12.2128355979227,61.5750923024161,
72.9888401098885));
#121749=CARTESIAN_POINT('Ctrl Pts',(-12.2305831957688,61.60075779768,72.9888419004666));
#121750=CARTESIAN_POINT('Ctrl Pts',(-12.2469398266819,61.6272548217178,
72.9888449935941));
#121751=CARTESIAN_POINT('Ctrl Pts',(-12.2633575502906,61.6538508132404,
72.9888480982745));
#121752=CARTESIAN_POINT('Ctrl Pts',(-12.2783734354803,61.6812837707993,
72.9888525151648));
#121753=CARTESIAN_POINT('Ctrl Pts',(-12.2918840994421,61.7093222793794,
72.9888577913022));
#121754=CARTESIAN_POINT('Ctrl Pts',(-12.3054384234256,61.7374513950457,
72.9888630844895));
#121755=CARTESIAN_POINT('Ctrl Pts',(-12.3174775876023,61.7661890889953,
72.9888692423773));
#121756=CARTESIAN_POINT('Ctrl Pts',(-12.3279483638797,61.7952886248432,
72.9888758045281));
#121757=CARTESIAN_POINT('Ctrl Pts',(-12.3385368919628,61.8247154070003,
72.9888824404753));
#121758=CARTESIAN_POINT('Ctrl Pts',(-12.3475215770959,61.8545112926814,
72.9888894897106));
#121759=CARTESIAN_POINT('Ctrl Pts',(-12.3549010685653,61.8844216123198,
72.9888964746818));
#121760=CARTESIAN_POINT('Ctrl Pts',(-12.3610944269458,61.9095243351247,
72.9889023369326));
#121761=CARTESIAN_POINT('Ctrl Pts',(-12.366158217251,61.9347074358474,72.9889081538596));
#121762=CARTESIAN_POINT('Ctrl Pts',(-12.3701190895151,61.959827502654,72.9889136433191));
#121763=CARTESIAN_POINT('Ctrl Pts',(-12.3749397042919,61.9904001031244,
72.9889203243145));
#121764=CARTESIAN_POINT('Ctrl Pts',(-12.3781258301378,62.0208781607225,
72.9889265531504));
#121765=CARTESIAN_POINT('Ctrl Pts',(-12.3797689676216,62.0510265774712,
72.988932368569));
#121766=CARTESIAN_POINT('Ctrl Pts',(-12.3814487003365,62.0818464464216,
72.9889383135061));
#121767=CARTESIAN_POINT('Ctrl Pts',(-12.3815166075881,62.1123211758842,
72.9889438263104));
#121768=CARTESIAN_POINT('Ctrl Pts',(-12.3801113156889,62.1422366139128,
72.98894893607));
#121769=CARTESIAN_POINT('Ctrl Pts',(-12.3790019726615,62.1658519799483,
72.9889529697345));
#121770=CARTESIAN_POINT('Ctrl Pts',(-12.3769755570522,62.1891195437263,
72.9889567519603));
#121771=CARTESIAN_POINT('Ctrl Pts',(-12.374113173743,62.2119528798782,72.9889602925763));
#121772=CARTESIAN_POINT('Ctrl Pts',(-12.370364760107,62.241854112293,72.9889649291648));
#121773=CARTESIAN_POINT('Ctrl Pts',(-12.3651827094674,62.2710089869103,
72.9889692499398));
#121774=CARTESIAN_POINT('Ctrl Pts',(-12.358766718633,62.2992685082974,72.988973146793));
#121775=CARTESIAN_POINT('Ctrl Pts',(-12.3571501629764,62.3063887006933,
72.9889741286335));
#121776=CARTESIAN_POINT('Ctrl Pts',(-12.355455337204,62.3134523062013,72.9889750835445));
#121777=CARTESIAN_POINT('Ctrl Pts',(-12.3536855356837,62.3204574463092,
72.9889760097662));
#121778=CARTESIAN_POINT('Ctrl Pts',(-12.3466752021777,62.3482053987486,
72.9889796786091));
#121779=CARTESIAN_POINT('Ctrl Pts',(-12.338191440408,62.3762050445819,72.9889829510826));
#121780=CARTESIAN_POINT('Ctrl Pts',(-12.3281211515463,62.4042415517801,
72.9889858111758));
#121781=CARTESIAN_POINT('Ctrl Pts',(-12.3238100314073,62.416244062579,72.9889870355901));
#121782=CARTESIAN_POINT('Ctrl Pts',(-12.319208549409,62.4282528358705,72.9889881843647));
#121783=CARTESIAN_POINT('Ctrl Pts',(-12.314309904899,62.4402489088726,72.9889892558765));
#121784=CARTESIAN_POINT('Ctrl Pts',(-12.3032198131789,62.4674069419982,
72.9889916816831));
#121785=CARTESIAN_POINT('Ctrl Pts',(-12.2906036714925,62.4945015538455,
72.9889936107424));
#121786=CARTESIAN_POINT('Ctrl Pts',(-12.276412224394,62.521292316785,72.9889951016));
#121787=CARTESIAN_POINT('Ctrl Pts',(-12.2624553258617,62.5476402964769,
72.9889965678174));
#121788=CARTESIAN_POINT('Ctrl Pts',(-12.246974328998,62.5736936514737,72.9889976104105));
#121789=CARTESIAN_POINT('Ctrl Pts',(-12.2299687881257,62.5992042926995,
72.9889982713549));
#121790=CARTESIAN_POINT('Ctrl Pts',(-12.213285338897,62.6242317523302,72.9889989197807));
#121791=CARTESIAN_POINT('Ctrl Pts',(-12.1951343757566,62.6487360266731,
72.9889992010127));
#121792=CARTESIAN_POINT('Ctrl Pts',(-12.1755649618719,62.6724756656738,
72.9889991388274));
#121793=CARTESIAN_POINT('Ctrl Pts',(-12.1561793061432,62.6959923878149,
72.988999077226));
#121794=CARTESIAN_POINT('Ctrl Pts',(-12.1354017183969,62.7187578959313,
72.9889986787046));
#121795=CARTESIAN_POINT('Ctrl Pts',(-12.1133302921518,62.7405430183668,
72.9889979490452));
#121796=CARTESIAN_POINT('Ctrl Pts',(-12.0914627435291,62.7621269078182,
72.9889972261258));
#121797=CARTESIAN_POINT('Ctrl Pts',(-12.0683254188729,62.7827476021891,
72.9889961781443));
#121798=CARTESIAN_POINT('Ctrl Pts',(-12.0440613696876,62.8022004457818,
72.9889947931482));
#121799=CARTESIAN_POINT('Ctrl Pts',(-12.0265199799282,62.8162636348557,
72.9889937918826));
#121800=CARTESIAN_POINT('Ctrl Pts',(-12.0083907632135,62.8297168099659,
72.9889926141001));
#121801=CARTESIAN_POINT('Ctrl Pts',(-11.9897418060247,62.8424922777627,
72.9889912497166));
#121802=CARTESIAN_POINT('Ctrl Pts',(-11.9641069654802,62.8600534248304,
72.9889893742362));
#121803=CARTESIAN_POINT('Ctrl Pts',(-11.9374890967615,62.8763321193198,
72.9889872025664));
#121804=CARTESIAN_POINT('Ctrl Pts',(-11.9100952215728,62.8911856415241,
72.9889846305083));
#121805=CARTESIAN_POINT('Ctrl Pts',(-11.8826990290741,62.9060404202215,
72.9889820582326));
#121806=CARTESIAN_POINT('Ctrl Pts',(-11.8545274891427,62.9194693501063,
72.9889790853045));
#121807=CARTESIAN_POINT('Ctrl Pts',(-11.8258127212586,62.9313753840749,
72.9889755961807));
#121808=CARTESIAN_POINT('Ctrl Pts',(-11.7969005111399,62.943363283722,72.9889720830658));
#121809=CARTESIAN_POINT('Ctrl Pts',(-11.7674384630735,62.9538070397002,
72.9889680463902));
#121810=CARTESIAN_POINT('Ctrl Pts',(-11.7376762200055,62.9626590950443,
72.9889633600468));
#121811=CARTESIAN_POINT('Ctrl Pts',(-11.7077660056033,62.9715551608629,
72.988958650404));
#121812=CARTESIAN_POINT('Ctrl Pts',(-11.6775535187158,62.978843725931,72.9889532843411));
#121813=CARTESIAN_POINT('Ctrl Pts',(-11.6472912201003,62.9845296107777,
72.9889471295904));
#121814=CARTESIAN_POINT('Ctrl Pts',(-11.6166074832013,62.9902946782926,
72.9889408891275));
#121815=CARTESIAN_POINT('Ctrl Pts',(-11.5858734214282,62.9944123876513,
72.9889338375723));
#121816=CARTESIAN_POINT('Ctrl Pts',(-11.5553374658601,62.9969397578481,
72.9889258369577));
#121817=CARTESIAN_POINT('Ctrl Pts',(-11.5304153894896,62.9990024839651,
72.9889193072152));
#121818=CARTESIAN_POINT('Ctrl Pts',(-11.5056251349898,63.00000700811,72.988912145239));
#121819=CARTESIAN_POINT('Ctrl Pts',(-11.4810890049462,63.0000066826667,
72.9889042778822));
#121820=CARTESIAN_POINT('Ctrl Pts',(-10.1997576867849,67.76779559893,84.72864147799));
#121821=CARTESIAN_POINT('Ctrl Pts',(-10.3096071503739,67.31146422345,84.44751423884));
#121822=CARTESIAN_POINT('Ctrl Pts',(-10.5431181289799,66.36314644642,83.7842726899399));
#121823=CARTESIAN_POINT('Ctrl Pts',(-10.8727722357109,64.9897459741,82.539892806721));
#121824=CARTESIAN_POINT('Ctrl Pts',(-11.1574332348069,63.69898082881,80.98142837168));
#121825=CARTESIAN_POINT('Ctrl Pts',(-11.3672962669879,62.64696648581,79.225467208697));
#121826=CARTESIAN_POINT('Ctrl Pts',(-11.5032040207249,61.90938280311,77.447206492296));
#121827=CARTESIAN_POINT('Ctrl Pts',(-11.5810454885597,61.46365902169,75.7768267823979));
#121828=CARTESIAN_POINT('Ctrl Pts',(-11.6184127295029,61.24328748873,74.247983007362));
#121829=CARTESIAN_POINT('Ctrl Pts',(-11.6245351204064,61.20669260332,73.2770976585449));
#121830=CARTESIAN_POINT('Ctrl Pts',(-11.6236939394218,61.2124848047,72.8155267773184));
#121831=CARTESIAN_POINT('Ctrl Pts',(-11.6236928456892,61.21249233149,72.8149300730504));
#121832=CARTESIAN_POINT('Ctrl Pts',(-10.7445114810569,67.9164295402001,
84.71528553673));
#121833=CARTESIAN_POINT('Ctrl Pts',(-10.8545618554429,67.45983386763,84.43944843073));
#121834=CARTESIAN_POINT('Ctrl Pts',(-11.0894328441589,66.5068038019001,
83.78520548561));
#121835=CARTESIAN_POINT('Ctrl Pts',(-11.4226175304349,65.11912432056,82.54699405835));
#121836=CARTESIAN_POINT('Ctrl Pts',(-11.7106257883405,63.81306197145,80.989105717709));
#121837=CARTESIAN_POINT('Ctrl Pts',(-11.9227252329622,62.74954121041,79.231327320835));
#121838=CARTESIAN_POINT('Ctrl Pts',(-12.0598976401354,62.00485586623,77.450888058051));
#121839=CARTESIAN_POINT('Ctrl Pts',(-12.1383713127295,61.55537167225,75.779454975613));
#121840=CARTESIAN_POINT('Ctrl Pts',(-12.1760508898936,61.33310788978,74.248646493056));
#121841=CARTESIAN_POINT('Ctrl Pts',(-12.1822137575716,61.2962518831,73.2775160011898));
#121842=CARTESIAN_POINT('Ctrl Pts',(-12.1813663982192,61.30208713828,72.8155200043769));
#121843=CARTESIAN_POINT('Ctrl Pts',(-12.1813652964467,61.30209472109,72.8149227500128));
#121844=CARTESIAN_POINT('Ctrl Pts',(-11.0478118783009,68.22129063266,84.34909471137));
#121845=CARTESIAN_POINT('Ctrl Pts',(-11.1579741129899,67.77848669656,84.08483280083));
#121846=CARTESIAN_POINT('Ctrl Pts',(-11.3936023091109,66.8517673089299,
83.45593242299));
#121847=CARTESIAN_POINT('Ctrl Pts',(-11.7287527020768,65.49798356831,82.2592195154991));
#121848=CARTESIAN_POINT('Ctrl Pts',(-12.0186245999192,64.22271758572,80.749267626391));
#121849=CARTESIAN_POINT('Ctrl Pts',(-12.2319692029754,63.18483956493,79.044107978404));
#121850=CARTESIAN_POINT('Ctrl Pts',(-12.3698457261984,62.4586779496,77.316764725178));
#121851=CARTESIAN_POINT('Ctrl Pts',(-12.4486713889145,62.0206875690101,
75.6957671382841));
#121852=CARTESIAN_POINT('Ctrl Pts',(-12.4865248642707,61.80408781319,74.210555691052));
#121853=CARTESIAN_POINT('Ctrl Pts',(-12.4927102680409,61.76820235719,73.2689474092427));
#121854=CARTESIAN_POINT('Ctrl Pts',(-12.4918594687833,61.7738849678301,
72.8208124201688));
#121855=CARTESIAN_POINT('Ctrl Pts',(-12.4918583625345,61.77389235232,72.8202330845845));
#121856=CARTESIAN_POINT('Ctrl Pts',(-10.9126738311849,68.48438020148,83.8678996071999));
#121857=CARTESIAN_POINT('Ctrl Pts',(-11.0227862255739,68.06046669184,83.61398019171));
#121858=CARTESIAN_POINT('Ctrl Pts',(-11.2580770415569,67.17399290633,83.0103070625101));
#121859=CARTESIAN_POINT('Ctrl Pts',(-11.592351597347,65.88026532928,81.863470621288));
#121860=CARTESIAN_POINT('Ctrl Pts',(-11.8813931347155,64.66188791271,80.4176821685851));
#121861=CARTESIAN_POINT('Ctrl Pts',(-12.0941829469415,63.67014755444,78.785402860033));
#121862=CARTESIAN_POINT('Ctrl Pts',(-12.2317457453268,62.97610441922,77.131945812737));
#121863=CARTESIAN_POINT('Ctrl Pts',(-12.3104145758787,62.55739717061,75.58011615866));
#121864=CARTESIAN_POINT('Ctrl Pts',(-12.3481905694304,62.35033909216,74.158449502137));
#121865=CARTESIAN_POINT('Ctrl Pts',(-12.3543659320548,62.31602551352,73.2569569413241));
#121866=CARTESIAN_POINT('Ctrl Pts',(-12.353516665476,62.32145891959,72.8279667500161));
#121867=CARTESIAN_POINT('Ctrl Pts',(-12.3535155612216,62.32146598023,72.8274121643456));
#121868=CARTESIAN_POINT('Ctrl Pts',(-10.7775357840699,68.74746977031,83.38670450304));
#121869=CARTESIAN_POINT('Ctrl Pts',(-10.8875983381589,68.34244668712,83.14312758258));
#121870=CARTESIAN_POINT('Ctrl Pts',(-11.1225517740029,67.49621850373,82.564681702032));
#121871=CARTESIAN_POINT('Ctrl Pts',(-11.4559504926169,66.26254709025,81.467721727077));
#121872=CARTESIAN_POINT('Ctrl Pts',(-11.7441616695118,65.1010582397,80.086096710779));
#121873=CARTESIAN_POINT('Ctrl Pts',(-11.9563966909076,64.15545554395,78.526697741661));
#121874=CARTESIAN_POINT('Ctrl Pts',(-12.0936457644551,63.49353088885,76.9471269002951));
#121875=CARTESIAN_POINT('Ctrl Pts',(-12.1721577628428,63.09410677221,75.464465179036));
#121876=CARTESIAN_POINT('Ctrl Pts',(-12.2098562745902,62.89659037114,74.106343313221));
#121877=CARTESIAN_POINT('Ctrl Pts',(-12.2160215960688,62.8638486698501,
73.2449664734054));
#121878=CARTESIAN_POINT('Ctrl Pts',(-12.2151738621687,62.86903287134,72.8351210798634));
#121879=CARTESIAN_POINT('Ctrl Pts',(-12.2151727599088,62.86903960813,72.8345912441068));
#121880=CARTESIAN_POINT('Ctrl Pts',(-10.2917276399139,68.79791856628,83.10302775846));
#121881=CARTESIAN_POINT('Ctrl Pts',(-10.4016110229669,68.40461580073,82.861843474006));
#121882=CARTESIAN_POINT('Ctrl Pts',(-10.6353516100079,67.58642976082,82.292125137501));
#121883=CARTESIAN_POINT('Ctrl Pts',(-10.9656017791049,66.39997015062,81.2210262182501));
#121884=CARTESIAN_POINT('Ctrl Pts',(-11.2508278908059,65.28451454765,79.878119282303));
#121885=CARTESIAN_POINT('Ctrl Pts',(-11.4610684930919,64.37557932713,78.364528519757));
#121886=CARTESIAN_POINT('Ctrl Pts',(-11.5971897563413,63.73850785712,76.831647075385));
#121887=CARTESIAN_POINT('Ctrl Pts',(-11.6751379583426,63.35363234109,75.391963104124));
#121888=CARTESIAN_POINT('Ctrl Pts',(-11.7125579305342,63.16333821796,74.074063236392));
#121889=CARTESIAN_POINT('Ctrl Pts',(-11.7186871550696,63.13174883075,73.2373415999963));
#121890=CARTESIAN_POINT('Ctrl Pts',(-11.7178449310008,63.13674911897,72.8394907884618));
#121891=CARTESIAN_POINT('Ctrl Pts',(-11.7178438359108,63.1367556167101,
72.8389764593828));
#121892=CARTESIAN_POINT('Ctrl Pts',(-9.77076807637092,68.60296152033,83.20110941226));
#121893=CARTESIAN_POINT('Ctrl Pts',(-9.88045932418391,68.20659694811,82.952813955229));
#121894=CARTESIAN_POINT('Ctrl Pts',(-10.1128993048199,67.38603701235,82.369655164651));
#121895=CARTESIAN_POINT('Ctrl Pts',(-10.4397731061019,66.20328211146,81.283605864789));
#121896=CARTESIAN_POINT('Ctrl Pts',(-10.7217981634799,65.09310714263,79.928825352772));
#121897=CARTESIAN_POINT('Ctrl Pts',(-10.9299000372949,64.18755471981,78.404219526706));
#121898=CARTESIAN_POINT('Ctrl Pts',(-11.0648118857419,63.55192969764,76.860507224859));
#121899=CARTESIAN_POINT('Ctrl Pts',(-11.1421554969749,63.16741934538,75.409697985201));
#121900=CARTESIAN_POINT('Ctrl Pts',(-11.1792767754389,62.97733743511,74.082574270443));
#121901=CARTESIAN_POINT('Ctrl Pts',(-11.1853672911799,62.9457324032,73.2390344611633));
#121902=CARTESIAN_POINT('Ctrl Pts',(-11.1845309756149,62.95073351593,72.8382378734121));
#121903=CARTESIAN_POINT('Ctrl Pts',(-11.1845298882129,62.95074001469,72.8377197366249));
#121904=CARTESIAN_POINT('Origin',(-8.56753648333091,1.4210854715202E-14,
72.98888938658));
#121905=CARTESIAN_POINT('',(-8.56285234933876,73.333293028708,64.0807251311373));
#121906=CARTESIAN_POINT('',(-8.56795784296129,66.4424972638774,69.9758907965238));
#121907=CARTESIAN_POINT('Ctrl Pts',(-8.56753648333091,73.3335502589656,
64.0821442489851));
#121908=CARTESIAN_POINT('Ctrl Pts',(-8.56753648333091,72.5539028998352,
64.2258274700778));
#121909=CARTESIAN_POINT('Ctrl Pts',(-8.56753648333092,71.7917993992724,
64.4685834837518));
#121910=CARTESIAN_POINT('Ctrl Pts',(-8.56753648333092,70.5771863640527,
65.0448111485544));
#121911=CARTESIAN_POINT('Ctrl Pts',(-8.56753648333091,69.8608492258319,
65.440988650358));
#121912=CARTESIAN_POINT('Ctrl Pts',(-8.56753648333091,68.4965495909561,
66.6238377720524));
#121913=CARTESIAN_POINT('Ctrl Pts',(-8.56753648333093,67.9668494703072,
67.2198258127435));
#121914=CARTESIAN_POINT('Ctrl Pts',(-8.56753648333093,67.0735256632114,
68.5233977289405));
#121915=CARTESIAN_POINT('Ctrl Pts',(-8.56753648333091,66.7090578372287,
69.23213924102));
#121916=CARTESIAN_POINT('Ctrl Pts',(-8.56753648333091,66.4431946200656,
69.976105782015));
#121917=CARTESIAN_POINT('Ctrl Pts',(-8.56753648333091,66.4418053341428,
69.9756606261135));
#121918=CARTESIAN_POINT('Ctrl Pts',(-8.56753648333091,66.2607314661459,
70.5747391016418));
#121919=CARTESIAN_POINT('Ctrl Pts',(-8.56753648333067,66.1409893830732,
71.1924170733865));
#121920=CARTESIAN_POINT('Ctrl Pts',(-8.56753648333067,66.0348383656674,
72.4359711725211));
#121921=CARTESIAN_POINT('Ctrl Pts',(-8.5675364833307,66.0481767601204,73.060065741546));
#121922=CARTESIAN_POINT('Ctrl Pts',(-8.5675364833307,66.2227996979891,74.4574116220633));
#121923=CARTESIAN_POINT('Ctrl Pts',(-8.56753648333093,66.468768244879,75.6274791834595));
#121924=CARTESIAN_POINT('Ctrl Pts',(-8.56753648333093,67.7151076066531,
77.8553329362392));
#121925=CARTESIAN_POINT('Ctrl Pts',(-8.56753648333122,68.4456337803905,
78.7215971823619));
#121926=CARTESIAN_POINT('Ctrl Pts',(-8.56753648333122,69.8118531742968,
79.8204638981078));
#121927=CARTESIAN_POINT('Ctrl Pts',(-8.56753648333126,70.3493421759933,
80.1599025125624));
#121928=CARTESIAN_POINT('Ctrl Pts',(-8.56753648333126,71.4836677103505,
80.7090839391736));
#121929=CARTESIAN_POINT('Ctrl Pts',(-8.56753648333091,72.0732569766187,
80.9188351508686));
#121930=CARTESIAN_POINT('Ctrl Pts',(-8.56753648333091,72.6784966214632,
81.0617217311455));
#121931=CARTESIAN_POINT('Ctrl Pts',(-8.57006447465355,83.3346137605936,
71.9543844308784));
#121932=CARTESIAN_POINT('Ctrl Pts',(-8.56941033891195,83.3220909976787,
71.8009596765008));
#121933=CARTESIAN_POINT('Ctrl Pts',(-8.56886746936034,83.305681306695,71.6484246702876));
#121934=CARTESIAN_POINT('Ctrl Pts',(-8.5683903518647,83.2853788427609,71.4967593339514));
#121935=CARTESIAN_POINT('Ctrl Pts',(-8.56791227764618,83.2650356680335,
71.3447898760967));
#121936=CARTESIAN_POINT('Ctrl Pts',(-8.56750021944195,83.2407839104731,
71.1936931337831));
#121937=CARTESIAN_POINT('Ctrl Pts',(-8.56710838877179,83.2125673414922,
71.0434635951297));
#121938=CARTESIAN_POINT('Ctrl Pts',(-8.56671842313737,83.1844850777445,
70.8939491190778));
#121939=CARTESIAN_POINT('Ctrl Pts',(-8.56634849293726,83.1524754527888,
70.745293194284));
#121940=CARTESIAN_POINT('Ctrl Pts',(-8.56595346041612,83.1164361810017,
70.5975113327712));
#121941=CARTESIAN_POINT('Ctrl Pts',(-8.56561023543377,83.0851233706345,
70.469110697137));
#121942=CARTESIAN_POINT('Ctrl Pts',(-8.56524806059338,83.0507677873467,
70.3413700448385));
#121943=CARTESIAN_POINT('Ctrl Pts',(-8.56483733000771,83.0132750464447,
70.2143161908913));
#121944=CARTESIAN_POINT('Ctrl Pts',(-8.56435630198732,82.9693653412412,
70.0655167929924));
#121945=CARTESIAN_POINT('Ctrl Pts',(-8.56383104291083,82.9211785522005,
69.9176068560262));
#121946=CARTESIAN_POINT('Ctrl Pts',(-8.56332873364437,82.8687104849843,
69.7706206743157));
#121947=CARTESIAN_POINT('Ctrl Pts',(-8.56283735805838,82.8173844812751,
69.6268339158561));
#121948=CARTESIAN_POINT('Ctrl Pts',(-8.56236794406668,82.7619616214511,
69.4839306438142));
#121949=CARTESIAN_POINT('Ctrl Pts',(-8.56198338038889,82.702388237078,69.3419433580854));
#121950=CARTESIAN_POINT('Ctrl Pts',(-8.56184284085215,82.6806170290173,
69.2900538310404));
#121951=CARTESIAN_POINT('Ctrl Pts',(-8.56171363350844,82.6582910038869,
69.2382866788046));
#121952=CARTESIAN_POINT('Ctrl Pts',(-8.56159882782864,82.6354057978218,
69.1866437008642));
#121953=CARTESIAN_POINT('Ctrl Pts',(-8.56127799107733,82.5714506417676,
69.0423218754944));
#121954=CARTESIAN_POINT('Ctrl Pts',(-8.56106962884463,82.5031319272677,
68.8989691362582));
#121955=CARTESIAN_POINT('Ctrl Pts',(-8.56104073355965,82.4304725808081,
68.7565547922964));
#121956=CARTESIAN_POINT('Ctrl Pts',(-8.56103230042259,82.4092668295218,
68.7149909288044));
#121957=CARTESIAN_POINT('Ctrl Pts',(-8.56103815082216,82.3874931148553,
68.6731323533542));
#121958=CARTESIAN_POINT('Ctrl Pts',(-8.56105882880582,82.3655094434444,
68.6316745428395));
#121959=CARTESIAN_POINT('Ctrl Pts',(-8.56107193580283,82.351574820021,68.6053959942441));
#121960=CARTESIAN_POINT('Ctrl Pts',(-8.56109100025004,82.3375568159525,
68.5792780371855));
#121961=CARTESIAN_POINT('Ctrl Pts',(-8.56111616070234,82.323556420184,68.5534931793396));
#121962=CARTESIAN_POINT('Ctrl Pts',(-8.5612477274945,82.2503467998598,68.4186613014251));
#121963=CARTESIAN_POINT('Ctrl Pts',(-8.56147132827033,82.174042389154,68.2865956486264));
#121964=CARTESIAN_POINT('Ctrl Pts',(-8.56175811113411,82.0947707474585,
68.1572071661102));
#121965=CARTESIAN_POINT('Ctrl Pts',(-8.56204998515142,82.0140918246817,
68.0255216961757));
#121966=CARTESIAN_POINT('Ctrl Pts',(-8.56240730446691,81.9303390791557,
67.896609002754));
#121967=CARTESIAN_POINT('Ctrl Pts',(-8.56279965315277,81.8435974231482,
67.7703984890432));
#121968=CARTESIAN_POINT('Ctrl Pts',(-8.56319761464984,81.7556148695475,
67.6423824492459));
#121969=CARTESIAN_POINT('Ctrl Pts',(-8.5636316149234,81.6645569462095,67.5171461454029));
#121970=CARTESIAN_POINT('Ctrl Pts',(-8.56406991392175,81.5704666099132,
67.3946442191827));
#121971=CARTESIAN_POINT('Ctrl Pts',(-8.56451394760364,81.4751452000696,
67.2705394835052));
#121972=CARTESIAN_POINT('Ctrl Pts',(-8.56496239323484,81.3767111650124,
67.1492408053214));
#121973=CARTESIAN_POINT('Ctrl Pts',(-8.5653822485358,81.2751677791634,67.0307348194276));
#121974=CARTESIAN_POINT('Ctrl Pts',(-8.56580299955837,81.1734077600962,
66.9119760122114));
#121975=CARTESIAN_POINT('Ctrl Pts',(-8.56619503813103,81.0685247080004,
66.7960215218833));
#121976=CARTESIAN_POINT('Ctrl Pts',(-8.56652515030154,80.9604863334545,
66.6828963954045));
#121977=CARTESIAN_POINT('Ctrl Pts',(-8.56685368594238,80.8529639220205,
66.5703115250387));
#121978=CARTESIAN_POINT('Ctrl Pts',(-8.56712088525739,80.7423158404718,
66.4605287861003));
#121979=CARTESIAN_POINT('Ctrl Pts',(-8.56729400788887,80.6284811960154,
66.3536151977035));
#121980=CARTESIAN_POINT('Ctrl Pts',(-8.567412542533,80.5505402072772,66.2804129592374));
#121981=CARTESIAN_POINT('Ctrl Pts',(-8.56748697450439,80.4711047740473,
66.2085566378043));
#121982=CARTESIAN_POINT('Ctrl Pts',(-8.5675067948903,80.3901489224879,66.1380803177677));
#121983=CARTESIAN_POINT('Ctrl Pts',(-8.56752047565147,80.3342702087702,
66.0894349631041));
#121984=CARTESIAN_POINT('Ctrl Pts',(-8.56752614823847,80.2773606447956,
66.0411465497854));
#121985=CARTESIAN_POINT('Ctrl Pts',(-8.56752927539675,80.2199013837073,
65.9936363050754));
#121986=CARTESIAN_POINT('Ctrl Pts',(-8.56753240255504,80.162442122619,65.9461260603653));
#121987=CARTESIAN_POINT('Ctrl Pts',(-8.56753298428461,80.104433364226,65.8993941752881));
#121988=CARTESIAN_POINT('Ctrl Pts',(-8.56753648333091,80.04639670726,65.8538149462682));
#121989=CARTESIAN_POINT('Ctrl Pts',(-8.56754409353963,79.9201705773867,
65.7546829496551));
#121990=CARTESIAN_POINT('Ctrl Pts',(-8.56747490722444,79.7915654578427,
65.6594020033908));
#121991=CARTESIAN_POINT('Ctrl Pts',(-8.56735121852545,79.660643441596,65.5679332348105));
#121992=CARTESIAN_POINT('Ctrl Pts',(-8.56722776761322,79.5299731178824,
65.4766403114145));
#121993=CARTESIAN_POINT('Ctrl Pts',(-8.56705002367323,79.3969944738259,
65.389144513119));
#121994=CARTESIAN_POINT('Ctrl Pts',(-8.56684015251371,79.2617278672298,
65.3054383083156));
#121995=CARTESIAN_POINT('Ctrl Pts',(-8.56663265773141,79.127992888336,65.2226799112923));
#121996=CARTESIAN_POINT('Ctrl Pts',(-8.56639375916541,78.9920211157852,
65.1436254255641));
#121997=CARTESIAN_POINT('Ctrl Pts',(-8.56614487816521,78.8537968393649,
65.0683035613709));
#121998=CARTESIAN_POINT('Ctrl Pts',(-8.56593648593594,78.7380593379894,
65.0052353031283));
#121999=CARTESIAN_POINT('Ctrl Pts',(-8.56572109502871,78.6207419150425,
64.9447844778263));
#122000=CARTESIAN_POINT('Ctrl Pts',(-8.56551128067993,78.5018184917218,
64.8869904906993));
#122001=CARTESIAN_POINT('Ctrl Pts',(-8.5652590707752,78.358865135855,64.8175185214435));
#122002=CARTESIAN_POINT('Ctrl Pts',(-8.56501491873875,78.2135914960043,
64.7518844114023));
#122003=CARTESIAN_POINT('Ctrl Pts',(-8.56480066680265,78.0659885596718,
64.6900507575985));
#122004=CARTESIAN_POINT('Ctrl Pts',(-8.56464683650043,77.9600114342514,
64.6456549410436));
#122005=CARTESIAN_POINT('Ctrl Pts',(-8.56450841989892,77.8528329663568,
64.6032192090122));
#122006=CARTESIAN_POINT('Ctrl Pts',(-8.56439350140998,77.7444430632104,
64.5627448543925));
#122007=CARTESIAN_POINT('Ctrl Pts',(-8.56426217032434,77.6205729724613,
64.5164899742403));
#122008=CARTESIAN_POINT('Ctrl Pts',(-8.56415731154464,77.4948545122233,
64.4727108661274));
#122009=CARTESIAN_POINT('Ctrl Pts',(-8.56410423122616,77.3676660355867,
64.4315565945173));
#122010=CARTESIAN_POINT('Ctrl Pts',(-8.56405092899636,77.2399458258337,
64.3902302704566));
#122011=CARTESIAN_POINT('Ctrl Pts',(-8.56404983907014,77.1107436360798,
64.351550878493));
#122012=CARTESIAN_POINT('Ctrl Pts',(-8.56412658632163,76.9804597267701,
64.3156197196934));
#122013=CARTESIAN_POINT('Ctrl Pts',(-8.56414588941054,76.9476913626139,
64.3065824924385));
#122014=CARTESIAN_POINT('Ctrl Pts',(-8.56417011646539,76.9148546383835,
64.2977188696857));
#122015=CARTESIAN_POINT('Ctrl Pts',(-8.56419967519835,76.8819560504712,
64.2890299614086));
#122016=CARTESIAN_POINT('Ctrl Pts',(-8.56433878773446,76.7271251243546,
64.2481372726687));
#122017=CARTESIAN_POINT('Ctrl Pts',(-8.56449961980914,76.5721315732247,
64.2115987798294));
#122018=CARTESIAN_POINT('Ctrl Pts',(-8.56466401278212,76.4170095331184,
64.179271595885));
#122019=CARTESIAN_POINT('Ctrl Pts',(-8.56483069887061,76.2597236976112,
64.1464934804553));
#122020=CARTESIAN_POINT('Ctrl Pts',(-8.56500104589211,76.1023053158395,
64.1180449315697));
#122021=CARTESIAN_POINT('Ctrl Pts',(-8.56515612467349,75.9447685236109,
64.0938270945347));
#122022=CARTESIAN_POINT('Ctrl Pts',(-8.56531272843634,75.7856825788478,
64.0693711091719));
#122023=CARTESIAN_POINT('Ctrl Pts',(-8.56545376219935,75.6264754095279,
64.0492294120697));
#122024=CARTESIAN_POINT('Ctrl Pts',(-8.56555973285479,75.4671468724349,
64.0333515489916));
#122025=CARTESIAN_POINT('Ctrl Pts',(-8.56566623305092,75.3070221626365,
64.0173943434339));
#122026=CARTESIAN_POINT('Ctrl Pts',(-8.56573731883972,75.1467743786349,
64.0057436685047));
#122027=CARTESIAN_POINT('Ctrl Pts',(-8.56575320342664,74.9863959007504,
63.9984003217801));
#122028=CARTESIAN_POINT('Ctrl Pts',(-8.5657690510057,74.8263910722562,63.991074083567));
#122029=CARTESIAN_POINT('Ctrl Pts',(-8.5657299542985,74.6662556684931,63.9880351413726));
#122030=CARTESIAN_POINT('Ctrl Pts',(-8.56561626448623,74.5059820589448,
63.9893358949042));
#122031=CARTESIAN_POINT('Ctrl Pts',(-8.56550328681298,74.3467123835981,
63.9906285006754));
#122032=CARTESIAN_POINT('Ctrl Pts',(-8.56531664759201,74.1873057550039,
63.9962066299903));
#122033=CARTESIAN_POINT('Ctrl Pts',(-8.56503706492985,74.027761791215,64.0061723870185));
#122034=CARTESIAN_POINT('Ctrl Pts',(-8.56476171519069,73.8706333467147,
64.0159872610063));
#122035=CARTESIAN_POINT('Ctrl Pts',(-8.56439621506046,73.713371264694,64.0300579850534));
#122036=CARTESIAN_POINT('Ctrl Pts',(-8.56392214524518,73.5559887369095,
64.04853056409));
#122037=CARTESIAN_POINT('Ctrl Pts',(-8.56369817955241,73.4816362138653,
64.0572575992815));
#122038=CARTESIAN_POINT('Ctrl Pts',(-8.56344998198766,73.4072570453578,
64.066967792157));
#122039=CARTESIAN_POINT('Ctrl Pts',(-8.56317561036611,73.3328541209004,
64.077680326643));
#122040=CARTESIAN_POINT('Ctrl Pts',(-9.33949250599091,68.28843467669,68.385749441946));
#122041=CARTESIAN_POINT('Ctrl Pts',(-9.28372478921891,67.21314456544,69.953566173561));
#122042=CARTESIAN_POINT('Ctrl Pts',(-9.17218935567391,66.21224057553,73.8663634510705));
#122043=CARTESIAN_POINT('Ctrl Pts',(-9.00488620535791,68.84902572167,79.327681027565));
#122044=CARTESIAN_POINT('Ctrl Pts',(-8.83758305504191,74.3860768082,81.799718607153));
#122045=CARTESIAN_POINT('Ctrl Pts',(-8.67027990472591,80.21224973459,80.119224478064));
#122046=CARTESIAN_POINT('Ctrl Pts',(-8.50297675440891,83.58160767004,75.077818068246));
#122047=CARTESIAN_POINT('Ctrl Pts',(-8.33567360409291,82.90653225676,69.051693466476));
#122048=CARTESIAN_POINT('Ctrl Pts',(-8.16837045377691,78.50298784705,64.8818706633));
#122049=CARTESIAN_POINT('Ctrl Pts',(-8.05683502023291,74.47097197897,64.648120002453));
#122050=CARTESIAN_POINT('Ctrl Pts',(-8.00106730345991,72.65076867909,65.196898714115));
#122051=CARTESIAN_POINT('Ctrl Pts',(-9.57007551786691,67.95907438126,68.159857051868));
#122052=CARTESIAN_POINT('Ctrl Pts',(-9.51430780109491,66.83101597355,69.804612106664));
#122053=CARTESIAN_POINT('Ctrl Pts',(-9.40277236755091,65.78099407777,73.9094242130813));
#122054=CARTESIAN_POINT('Ctrl Pts',(-9.23546921723391,68.54717561549,79.638747997329));
#122055=CARTESIAN_POINT('Ctrl Pts',(-9.06816606691691,74.3559494215,82.232097221564));
#122056=CARTESIAN_POINT('Ctrl Pts',(-8.90086291659891,80.46803330067,80.469135290092));
#122057=CARTESIAN_POINT('Ctrl Pts',(-8.73355976628091,84.00273757062,75.180329201596));
#122058=CARTESIAN_POINT('Ctrl Pts',(-8.56625661596291,83.29453381444,68.858481309736));
#122059=CARTESIAN_POINT('Ctrl Pts',(-8.39895346564491,78.67489187492,64.484030524229));
#122060=CARTESIAN_POINT('Ctrl Pts',(-8.28741803209991,74.4450106992,64.238808890051));
#122061=CARTESIAN_POINT('Ctrl Pts',(-8.23165031532691,72.5354835728,64.814518117892));
#122062=CARTESIAN_POINT('Ctrl Pts',(-9.80065852974291,67.62971408584,67.93396466179));
#122063=CARTESIAN_POINT('Ctrl Pts',(-9.74489081297091,66.44888738166,69.655658039767));
#122064=CARTESIAN_POINT('Ctrl Pts',(-9.63335537942691,65.34974758001,73.9524849750929));
#122065=CARTESIAN_POINT('Ctrl Pts',(-9.46605222911191,68.24532550932,79.949814967102));
#122066=CARTESIAN_POINT('Ctrl Pts',(-9.29874907879591,74.32582203482,82.66447583598));
#122067=CARTESIAN_POINT('Ctrl Pts',(-9.13144592848091,80.72381686678,80.8190461021));
#122068=CARTESIAN_POINT('Ctrl Pts',(-8.96414277816591,84.42386747123,75.282840334888));
#122069=CARTESIAN_POINT('Ctrl Pts',(-8.79683962785091,83.68253537209,68.665269152917));
#122070=CARTESIAN_POINT('Ctrl Pts',(-8.62953647753691,78.84679590269,64.086190385108));
#122071=CARTESIAN_POINT('Ctrl Pts',(-8.51800104399391,74.41904941931,63.829497777655));
#122072=CARTESIAN_POINT('Ctrl Pts',(-8.46223332722191,72.4201984664,64.432137521706));
#122073=CARTESIAN_POINT('Ctrl Pts',(-10.0312415416199,67.30035379041,67.708072271712));
#122074=CARTESIAN_POINT('Ctrl Pts',(-9.97547382484791,66.06675878978,69.50670397287));
#122075=CARTESIAN_POINT('Ctrl Pts',(-9.86393839130291,64.91850108225,73.995545737104));
#122076=CARTESIAN_POINT('Ctrl Pts',(-9.69663524098691,67.94347540314,80.260881936865));
#122077=CARTESIAN_POINT('Ctrl Pts',(-9.52933209067091,74.29569464812,83.09685445039));
#122078=CARTESIAN_POINT('Ctrl Pts',(-9.36202894035391,80.97960043285,81.168956914128));
#122079=CARTESIAN_POINT('Ctrl Pts',(-9.19472579003791,84.84499737182,75.38535146824));
#122080=CARTESIAN_POINT('Ctrl Pts',(-9.02742263972191,84.07053692978,68.47205699618));
#122081=CARTESIAN_POINT('Ctrl Pts',(-8.86011948940491,79.01869993056,63.68835024604));
#122082=CARTESIAN_POINT('Ctrl Pts',(-8.74858405586091,74.39308813955,63.420186665253));
#122083=CARTESIAN_POINT('Ctrl Pts',(-8.69281633908891,72.30491336013,64.049756925482));
#122084=CARTESIAN_POINT('',(-9.85448379345391,67.0101053268475,68.6926900228996));
#122085=CARTESIAN_POINT('Ctrl Pts',(-9.85448379345391,67.0101053268475,
68.6926900228996));
#122086=CARTESIAN_POINT('Ctrl Pts',(-9.83968424671194,66.7566723975021,
69.1693478230976));
#122087=CARTESIAN_POINT('Ctrl Pts',(-9.82516107127357,66.5463438560124,
69.6690843869866));
#122088=CARTESIAN_POINT('Ctrl Pts',(-9.81076777080292,66.3808021984325,
70.1832779640609));
#122089=CARTESIAN_POINT('Ctrl Pts',(-9.79800752377682,66.2340427773993,
70.6391315103747));
#122090=CARTESIAN_POINT('Ctrl Pts',(-9.78534935256035,66.1224832757427,
71.1063467143764));
#122091=CARTESIAN_POINT('Ctrl Pts',(-9.77269118134386,66.0472619576907,
71.5789206748202));
#122092=CARTESIAN_POINT('Ctrl Pts',(-9.7641119086294,65.9962795376812,71.8992150376523));
#122093=CARTESIAN_POINT('Ctrl Pts',(-9.75553263591493,65.961974408791,72.2220322993447));
#122094=CARTESIAN_POINT('Ctrl Pts',(-9.74695336320047,65.9447185888639,
72.5456455219375));
#122095=CARTESIAN_POINT('Ctrl Pts',(-9.73851905287355,65.9277543373412,
72.8637907116387));
#122096=CARTESIAN_POINT('Ctrl Pts',(-9.73008474254663,65.9272680677149,
73.1827060455231));
#122097=CARTESIAN_POINT('Ctrl Pts',(-9.72165043221971,65.9436628520002,
73.500745147291));
#122098=CARTESIAN_POINT('Ctrl Pts',(-9.71348628550153,65.9595324867575,
73.8085969796649));
#122099=CARTESIAN_POINT('Ctrl Pts',(-9.70532213878336,65.991219138219,74.1156284875255));
#122100=CARTESIAN_POINT('Ctrl Pts',(-9.69715799206519,66.0391346213581,
74.4203302806321));
#122101=CARTESIAN_POINT('Ctrl Pts',(-9.69539938958562,66.0494558821544,
74.4859647366732));
#122102=CARTESIAN_POINT('Ctrl Pts',(-9.69364078710605,66.0605303262043,
74.551491012646));
#122103=CARTESIAN_POINT('Ctrl Pts',(-9.69188218462648,66.0723623568164,
74.6168938744211));
#122104=CARTESIAN_POINT('Ctrl Pts',(-9.68912429718818,66.0909176636431,
74.719460391308));
#122105=CARTESIAN_POINT('Ctrl Pts',(-9.68636640974989,66.1113251604818,
74.8216626934074));
#122106=CARTESIAN_POINT('Ctrl Pts',(-9.68360852231159,66.1335950524943,
74.9234405765911));
#122107=CARTESIAN_POINT('Ctrl Pts',(-9.6733601644373,66.2163503600525,75.3016489675757));
#122108=CARTESIAN_POINT('Ctrl Pts',(-9.66311180656301,66.3248188849568,
75.673995727457));
#122109=CARTESIAN_POINT('Ctrl Pts',(-9.65286344868873,66.456981133905,76.0379113155534));
#122110=CARTESIAN_POINT('Ctrl Pts',(-9.6420032438932,66.5970337264689,76.4235533728952));
#122111=CARTESIAN_POINT('Ctrl Pts',(-9.63114303909766,66.7636936492638,
76.7997282070751));
#122112=CARTESIAN_POINT('Ctrl Pts',(-9.62028283430213,66.9546167830891,
77.1633862403935));
#122113=CARTESIAN_POINT('Ctrl Pts',(-9.60912582522197,67.1507577562851,
77.5369828765709));
#122114=CARTESIAN_POINT('Ctrl Pts',(-9.5979688161418,67.3725067113742,77.8973701715073));
#122115=CARTESIAN_POINT('Ctrl Pts',(-9.58681180706164,67.6173784973787,
78.2412368390855));
#122116=CARTESIAN_POINT('Ctrl Pts',(-9.57549059509304,67.8658541752745,
78.5901643522403));
#122117=CARTESIAN_POINT('Ctrl Pts',(-9.56416938312445,68.1381389483182,
78.9220824577887));
#122118=CARTESIAN_POINT('Ctrl Pts',(-9.55284817115585,68.4316852140694,
79.2335109677848));
#122119=CARTESIAN_POINT('Ctrl Pts',(-9.54532017783458,68.626877595785,79.4405940742406));
#122120=CARTESIAN_POINT('Ctrl Pts',(-9.53779218451331,68.8314718067912,
79.6386171967666));
#122121=CARTESIAN_POINT('Ctrl Pts',(-9.53026419119205,69.0447283571958,
79.8265486021723));
#122122=CARTESIAN_POINT('Ctrl Pts',(-9.52194613970065,69.2803660486017,
80.0342032905206));
#122123=CARTESIAN_POINT('Ctrl Pts',(-9.51362808820925,69.5268279476083,
80.2297487085396));
#122124=CARTESIAN_POINT('Ctrl Pts',(-9.50531003671786,69.783037643129,80.4116123859453));
#122125=CARTESIAN_POINT('Ctrl Pts',(-9.49781673259709,70.0138437603079,
80.5754440050126));
#122126=CARTESIAN_POINT('Ctrl Pts',(-9.49032342847633,70.2525595800675,
80.7281723744406));
#122127=CARTESIAN_POINT('Ctrl Pts',(-9.48283012435557,70.4983698898005,
80.8686705606302));
#122128=CARTESIAN_POINT('Ctrl Pts',(-9.47469694729936,70.7651705880079,
81.021166256246));
#122129=CARTESIAN_POINT('Ctrl Pts',(-9.46656377024315,71.0403291308939,
81.1592526198816));
#122130=CARTESIAN_POINT('Ctrl Pts',(-9.45843059318694,71.3221041991271,
81.2826982415201));
#122131=CARTESIAN_POINT('Ctrl Pts',(-9.45012412633853,71.6098829166948,
81.4087740611703));
#122132=CARTESIAN_POINT('Ctrl Pts',(-9.44181765949011,71.9045622622991,
81.5195783413505));
#122133=CARTESIAN_POINT('Ctrl Pts',(-9.4335111926417,72.2042657814675,81.6149141880342));
#122134=CARTESIAN_POINT('Ctrl Pts',(-9.42521438877695,72.5036206529783,
81.7101391297152));
#122135=CARTESIAN_POINT('Ctrl Pts',(-9.4169175849122,72.8079870625739,81.7899315289484));
#122136=CARTESIAN_POINT('Ctrl Pts',(-9.40862078104745,73.1154877013141,
81.854146473293));
#122137=CARTESIAN_POINT('Ctrl Pts',(-9.40048676107778,73.4169551551642,
81.9171015157606));
#122138=CARTESIAN_POINT('Ctrl Pts',(-9.3923527411081,73.7214341968443,81.965084457809));
#122139=CARTESIAN_POINT('Ctrl Pts',(-9.38421872113843,74.0271621528231,
81.9980077408963));
#122140=CARTESIAN_POINT('Ctrl Pts',(-9.37902788001143,74.2222668185954,
82.0190182046673));
#122141=CARTESIAN_POINT('Ctrl Pts',(-9.37383703888443,74.4178802756318,
82.0338965468219));
#122142=CARTESIAN_POINT('Ctrl Pts',(-9.36864619775743,74.6135481804256,
82.0426305340964));
#122143=CARTESIAN_POINT('Ctrl Pts',(-9.36110373378891,74.8978601224783,
82.0553213066914));
#122144=CARTESIAN_POINT('Ctrl Pts',(-9.35356126982038,75.1831895074007,
82.0550770709536));
#122145=CARTESIAN_POINT('Ctrl Pts',(-9.34601880585185,75.4681029630233,
82.0416491691116));
#122146=CARTESIAN_POINT('Ctrl Pts',(-9.33843160312578,75.754706406701,82.0281416185437));
#122147=CARTESIAN_POINT('Ctrl Pts',(-9.33084440039971,76.0408881332488,
82.0012933809063));
#122148=CARTESIAN_POINT('Ctrl Pts',(-9.32325719767364,76.3251718586273,
81.9609015624754));
#122149=CARTESIAN_POINT('Ctrl Pts',(-9.31572904715047,76.6072429661492,
81.9208241189129));
#122150=CARTESIAN_POINT('Ctrl Pts',(-9.3082008966273,76.8874446469196,81.867413064794));
#122151=CARTESIAN_POINT('Ctrl Pts',(-9.30067274610414,77.1643306109711,
81.8005207374888));
#122152=CARTESIAN_POINT('Ctrl Pts',(-9.29451315298162,77.3908809269679,
81.7457888989115));
#122153=CARTESIAN_POINT('Ctrl Pts',(-9.28835355985909,77.6152112078615,
81.6820327358978));
#122154=CARTESIAN_POINT('Ctrl Pts',(-9.28219396673657,77.8365331068418,
81.6091970918653));
#122155=CARTESIAN_POINT('Ctrl Pts',(-9.27464830785804,78.1076580852023,
81.5199715678518));
#122156=CARTESIAN_POINT('Ctrl Pts',(-9.26710264897951,78.374267377385,81.4171194611954));
#122157=CARTESIAN_POINT('Ctrl Pts',(-9.25955699010099,78.6352651857245,
81.3016023574398));
#122158=CARTESIAN_POINT('Ctrl Pts',(-9.25196749606842,78.8977792140945,
81.1854141777557));
#122159=CARTESIAN_POINT('Ctrl Pts',(-9.24437800203584,79.1546157026713,
81.0564139756897));
#122160=CARTESIAN_POINT('Ctrl Pts',(-9.23678850800327,79.4046883212804,
80.9156244836224));
#122161=CARTESIAN_POINT('Ctrl Pts',(-9.22924654220847,79.6531948920309,
80.7757166677809));
#122162=CARTESIAN_POINT('Ctrl Pts',(-9.22170457641367,79.8950214601759,
80.6241673829361));
#122163=CARTESIAN_POINT('Ctrl Pts',(-9.21416261061888,80.1291394950741,
80.4620149282776));
#122164=CARTESIAN_POINT('Ctrl Pts',(-9.21178447518684,80.2029616800612,
80.4108849565559));
#122165=CARTESIAN_POINT('Ctrl Pts',(-9.20940633975481,80.2760177457059,
80.3587009664616));
#122166=CARTESIAN_POINT('Ctrl Pts',(-9.20702820432278,80.3482763680922,
80.3054960787968));
#122167=CARTESIAN_POINT('Ctrl Pts',(-9.19830930076526,80.6131965031266,
80.1104322157008));
#122168=CARTESIAN_POINT('Ctrl Pts',(-9.18959039720775,80.8682552155851,
79.9010102664133));
#122169=CARTESIAN_POINT('Ctrl Pts',(-9.18087149365024,81.111814081159,79.6785563218492));
#122170=CARTESIAN_POINT('Ctrl Pts',(-9.17186595779949,81.3633798980331,
79.4487892462418));
#122171=CARTESIAN_POINT('Ctrl Pts',(-9.16286042194875,81.6026765258506,
79.205119591945));
#122172=CARTESIAN_POINT('Ctrl Pts',(-9.15385488609801,81.8279139681047,
78.94906204399));
#122173=CARTESIAN_POINT('Ctrl Pts',(-9.14480155182367,82.0543468966522,
78.6916454267532));
#122174=CARTESIAN_POINT('Ctrl Pts',(-9.13574821754934,82.2665702022945,
78.4217097128373));
#122175=CARTESIAN_POINT('Ctrl Pts',(-9.12669488327501,82.4627926640579,
78.1408390221426));
#122176=CARTESIAN_POINT('Ctrl Pts',(-9.11777922382609,82.6560311541323,
77.8642395559641));
#122177=CARTESIAN_POINT('Ctrl Pts',(-9.10886356437717,82.8337511090989,
77.5770359114317));
#122178=CARTESIAN_POINT('Ctrl Pts',(-9.09994790492826,82.994278877925,77.2807741296127));
#122179=CARTESIAN_POINT('Ctrl Pts',(-9.09380383002873,83.1049038564554,
77.0766103672134));
#122180=CARTESIAN_POINT('Ctrl Pts',(-9.08765975512921,83.2073649566054,
76.8681455411797));
#122181=CARTESIAN_POINT('Ctrl Pts',(-9.08151568022969,83.3011273339562,
76.6558922479745));
#122182=CARTESIAN_POINT('Ctrl Pts',(-9.07246710832417,83.4392141293431,
76.3433001625654));
#122183=CARTESIAN_POINT('Ctrl Pts',(-9.06341853641865,83.5584317260117,
76.0224912178744));
#122184=CARTESIAN_POINT('Ctrl Pts',(-9.05436996451312,83.6587995041413,
75.6958576243948));
#122185=CARTESIAN_POINT('Ctrl Pts',(-9.05138337997155,83.6919270360617,
75.5880484749256));
#122186=CARTESIAN_POINT('Ctrl Pts',(-9.04839679542997,83.7230014791061,
75.479604834333));
#122187=CARTESIAN_POINT('Ctrl Pts',(-9.04541021088839,83.7520247722967,
75.3706127663605));
#122188=CARTESIAN_POINT('Ctrl Pts',(-9.03539106069585,83.8493897487475,
75.0049750676414));
#122189=CARTESIAN_POINT('Ctrl Pts',(-9.02537191050332,83.9237100286563,
74.6330371582655));
#122190=CARTESIAN_POINT('Ctrl Pts',(-9.01535276031078,83.9750640216069,
74.2577698789031));
#122191=CARTESIAN_POINT('Ctrl Pts',(-9.00513012247064,84.027461007528,73.874880969519));
#122192=CARTESIAN_POINT('Ctrl Pts',(-8.9949074846305,84.055949510843,73.4885250035023));
#122193=CARTESIAN_POINT('Ctrl Pts',(-8.98468484679035,84.0605617694674,
73.1018404298762));
#122194=CARTESIAN_POINT('Ctrl Pts',(-8.97452712867039,84.0651447375559,
72.7176115291115));
#122195=CARTESIAN_POINT('Ctrl Pts',(-8.96436941055043,84.0461536980524,
72.3330570424656));
#122196=CARTESIAN_POINT('Ctrl Pts',(-8.95421169243046,84.0035699263375,
71.951256065974));
#122197=CARTESIAN_POINT('Ctrl Pts',(-8.94427537112854,83.9619143071316,
71.5777767932672));
#122198=CARTESIAN_POINT('Ctrl Pts',(-8.93433904982663,83.8976830275582,
71.2069313198722));
#122199=CARTESIAN_POINT('Ctrl Pts',(-8.92440272852471,83.8108120961398,
70.8416174230802));
#122200=CARTESIAN_POINT('Ctrl Pts',(-8.91488179465382,83.7275727998039,
70.4915754560591));
#122201=CARTESIAN_POINT('Ctrl Pts',(-8.90536086078292,83.6235469010876,
70.14661155296));
#122202=CARTESIAN_POINT('Ctrl Pts',(-8.89583992691202,83.4986384743573,
69.8093014238666));
#122203=CARTESIAN_POINT('Ctrl Pts',(-8.89182402375937,83.4459524509587,
69.6670249592661));
#122204=CARTESIAN_POINT('Ctrl Pts',(-8.88780812060673,83.3895506839613,
69.526110587854));
#122205=CARTESIAN_POINT('Ctrl Pts',(-8.88379221745408,83.3294239020245,
69.3867535301559));
#122206=CARTESIAN_POINT('Ctrl Pts',(-8.88276827073607,83.3140931983973,
69.3512212485154));
#122207=CARTESIAN_POINT('Ctrl Pts',(-8.88174432401806,83.2985229335303,
69.3157962727063));
#122208=CARTESIAN_POINT('Ctrl Pts',(-8.88072037730005,83.2827131953649,
69.28048176021));
#122209=CARTESIAN_POINT('Ctrl Pts',(-8.87076384242528,83.1289842887371,
68.9370945809048));
#122210=CARTESIAN_POINT('Ctrl Pts',(-8.8608073075505,82.9526176762723,68.6041515378788));
#122211=CARTESIAN_POINT('Ctrl Pts',(-8.85085077267572,82.7559042186426,
68.2835569890274));
#122212=CARTESIAN_POINT('Ctrl Pts',(-8.84012772695439,82.5440466369946,
67.93828124314));
#122213=CARTESIAN_POINT('Ctrl Pts',(-8.82940468123306,82.3085887208393,
67.6073276606856));
#122214=CARTESIAN_POINT('Ctrl Pts',(-8.81868163551173,82.0523291916876,
67.2930844645106));
#122215=CARTESIAN_POINT('Ctrl Pts',(-8.80794383623225,81.7957170817522,
66.9784089093411));
#122216=CARTESIAN_POINT('Ctrl Pts',(-8.79720603695278,81.5182451844684,
66.6804889429592));
#122217=CARTESIAN_POINT('Ctrl Pts',(-8.7864682376733,81.2226714956049,66.4017442245413));
#122218=CARTESIAN_POINT('Ctrl Pts',(-8.77574164723827,80.9274063466398,
66.1232904787991));
#122219=CARTESIAN_POINT('Ctrl Pts',(-8.76501505680324,80.6140762722008,
65.8639711687019));
#122220=CARTESIAN_POINT('Ctrl Pts',(-8.75428846636821,80.285392018042,65.626231962766));
#122221=CARTESIAN_POINT('Ctrl Pts',(-8.74358371891872,79.9573770767891,
65.3889768746933));
#122222=CARTESIAN_POINT('Ctrl Pts',(-8.73287897146925,79.6140695273579,
65.1732133043622));
#122223=CARTESIAN_POINT('Ctrl Pts',(-8.72217422401977,79.2581386075932,
64.9814173392414));
#122224=CARTESIAN_POINT('Ctrl Pts',(-8.71420778820075,78.993256055091,64.8386834490966));
#122225=CARTESIAN_POINT('Ctrl Pts',(-8.70624135238174,78.7211837617792,
64.7091241008327));
#122226=CARTESIAN_POINT('Ctrl Pts',(-8.69827491656272,78.4431588341649,
64.5938933849846));
#122227=CARTESIAN_POINT('Ctrl Pts',(-8.69216431948956,78.2299018209231,
64.505506496419));
#122228=CARTESIAN_POINT('Ctrl Pts',(-8.6860537224164,78.01314340794,64.4255493009773));
#122229=CARTESIAN_POINT('Ctrl Pts',(-8.67994312534324,77.7934534819807,
64.354525331016));
#122230=CARTESIAN_POINT('Ctrl Pts',(-8.67205571477406,77.5098830512668,
64.2628493123501));
#122231=CARTESIAN_POINT('Ctrl Pts',(-8.66416830420487,77.221428261215,64.1860589478401));
#122232=CARTESIAN_POINT('Ctrl Pts',(-8.65628089363569,76.9297092055054,
64.1240228313856));
#122233=CARTESIAN_POINT('Ctrl Pts',(-8.65130900485802,76.7458218971689,
64.0849178971991));
#122234=CARTESIAN_POINT('Ctrl Pts',(-8.64633711608036,76.5606379014098,
64.0516745335715));
#122235=CARTESIAN_POINT('Ctrl Pts',(-8.6413652273027,76.374564889621,64.0242494098714));
#122236=CARTESIAN_POINT('Ctrl Pts',(-8.63215604425852,76.0299110765988,
63.9734512131585));
#122237=CARTESIAN_POINT('Ctrl Pts',(-8.62294686121434,75.6823641851788,
63.9426311069089));
#122238=CARTESIAN_POINT('Ctrl Pts',(-8.61394688716208,75.3342120447879,
63.9314140909321));
#122239=CARTESIAN_POINT('Ctrl Pts',(-8.60457468117178,74.9716606022213,
63.9197331478848));
#122240=CARTESIAN_POINT('Ctrl Pts',(-8.59542934748614,74.6084520064369,
63.929310146414));
#122241=CARTESIAN_POINT('Ctrl Pts',(-8.58674714167216,74.2471433794914,
63.9597728002335));
#122242=CARTESIAN_POINT('Ctrl Pts',(-8.57938389032876,73.9407228350195,
63.9856077299122));
#122243=CARTESIAN_POINT('Ctrl Pts',(-8.57235374311391,73.6356680467237,
64.0264655590552));
#122244=CARTESIAN_POINT('Ctrl Pts',(-8.56580081221051,73.3335318456389,
64.0821476424436));
#122245=CARTESIAN_POINT('',(-9.46541110279056,67.6020149116865,69.0109979579471));
#122246=CARTESIAN_POINT('Ctrl Pts',(-9.87756472937818,67.62520219141,67.700413019766));
#122247=CARTESIAN_POINT('Ctrl Pts',(-9.81096367927215,66.1498345501,69.757818081886));
#122248=CARTESIAN_POINT('Ctrl Pts',(-9.67776157906115,65.03881684527,75.159924360853));
#122249=CARTESIAN_POINT('Ctrl Pts',(-9.47795842874515,69.94095953137,81.84418107373));
#122250=CARTESIAN_POINT('Ctrl Pts',(-9.27815527842915,78.18756436805,82.675374708005));
#122251=CARTESIAN_POINT('Ctrl Pts',(-9.07835212811315,84.3279816375,77.109502645435));
#122252=CARTESIAN_POINT('Ctrl Pts',(-8.87854897779715,84.30727308569,68.821968198105));
#122253=CARTESIAN_POINT('Ctrl Pts',(-8.67874582748115,78.13920519194,63.285515123434));
#122254=CARTESIAN_POINT('Ctrl Pts',(-8.47894267716618,69.89662703841,64.163123294247));
#122255=CARTESIAN_POINT('Ctrl Pts',(-8.34574057695515,66.65138462743,68.622440986855));
#122256=CARTESIAN_POINT('Ctrl Pts',(-8.27913952685018,66.12404568677,71.098635427588));
#122257=CARTESIAN_POINT('Ctrl Pts',(-9.87845073280442,67.62520219141,67.700413019766));
#122258=CARTESIAN_POINT('Ctrl Pts',(-9.8118496826984,66.1498345501,69.757818081886));
#122259=CARTESIAN_POINT('Ctrl Pts',(-9.6786475824874,65.03881684527,75.159924360853));
#122260=CARTESIAN_POINT('Ctrl Pts',(-9.4788444321714,69.94095953137,81.84418107373));
#122261=CARTESIAN_POINT('Ctrl Pts',(-9.2790412818554,78.18756436805,82.675374708005));
#122262=CARTESIAN_POINT('Ctrl Pts',(-9.0792381315394,84.3279816375,77.109502645435));
#122263=CARTESIAN_POINT('Ctrl Pts',(-8.8794349812234,84.30727308569,68.821968198105));
#122264=CARTESIAN_POINT('Ctrl Pts',(-8.6796318309074,78.13920519194,63.285515123434));
#122265=CARTESIAN_POINT('Ctrl Pts',(-8.47982868059242,69.89662703841,64.163123294247));
#122266=CARTESIAN_POINT('Ctrl Pts',(-8.3466265803814,66.65138462743,68.622440986855));
#122267=CARTESIAN_POINT('Ctrl Pts',(-8.28002553027642,66.12404568677,71.098635427588));
#122268=CARTESIAN_POINT('Ctrl Pts',(-9.87933673623067,67.62520219141,67.700413019766));
#122269=CARTESIAN_POINT('Ctrl Pts',(-9.81273568612466,66.1498345501,69.757818081886));
#122270=CARTESIAN_POINT('Ctrl Pts',(-9.67953358591366,65.03881684527,75.159924360853));
#122271=CARTESIAN_POINT('Ctrl Pts',(-9.47973043559766,69.94095953137,81.84418107373));
#122272=CARTESIAN_POINT('Ctrl Pts',(-9.27992728528165,78.18756436805,82.675374708005));
#122273=CARTESIAN_POINT('Ctrl Pts',(-9.08012413496566,84.3279816375,77.109502645435));
#122274=CARTESIAN_POINT('Ctrl Pts',(-8.88032098464966,84.30727308569,68.821968198105));
#122275=CARTESIAN_POINT('Ctrl Pts',(-8.68051783433366,78.13920519194,63.285515123434));
#122276=CARTESIAN_POINT('Ctrl Pts',(-8.48071468401867,69.89662703841,64.163123294247));
#122277=CARTESIAN_POINT('Ctrl Pts',(-8.34751258380766,66.65138462743,68.622440986855));
#122278=CARTESIAN_POINT('Ctrl Pts',(-8.28091153370267,66.12404568677,71.098635427588));
#122279=CARTESIAN_POINT('Ctrl Pts',(-9.88022273965691,67.62520219141,67.700413019766));
#122280=CARTESIAN_POINT('Ctrl Pts',(-9.81362168955091,66.1498345501,69.757818081886));
#122281=CARTESIAN_POINT('Ctrl Pts',(-9.68041958933991,65.03881684527,75.159924360853));
#122282=CARTESIAN_POINT('Ctrl Pts',(-9.48061643902391,69.94095953137,81.84418107373));
#122283=CARTESIAN_POINT('Ctrl Pts',(-9.28081328870791,78.18756436805,82.675374708005));
#122284=CARTESIAN_POINT('Ctrl Pts',(-9.08101013839191,84.3279816375,77.109502645435));
#122285=CARTESIAN_POINT('Ctrl Pts',(-8.88120698807591,84.30727308569,68.821968198105));
#122286=CARTESIAN_POINT('Ctrl Pts',(-8.68140383775991,78.13920519194,63.285515123434));
#122287=CARTESIAN_POINT('Ctrl Pts',(-8.48160068744491,69.89662703841,64.163123294247));
#122288=CARTESIAN_POINT('Ctrl Pts',(-8.34839858723391,66.65138462743,68.622440986855));
#122289=CARTESIAN_POINT('Ctrl Pts',(-8.28179753712891,66.12404568677,71.098635427588));
#122290=CARTESIAN_POINT('Ctrl Pts',(-9.96688940632291,67.62520219141,67.700413019766));
#122291=CARTESIAN_POINT('Ctrl Pts',(-9.90028835621791,66.1498345501,69.757818081886));
#122292=CARTESIAN_POINT('Ctrl Pts',(-9.76708625600691,65.03881684527,75.159924360853));
#122293=CARTESIAN_POINT('Ctrl Pts',(-9.56728310569091,69.94095953137,81.84418107373));
#122294=CARTESIAN_POINT('Ctrl Pts',(-9.36747995537491,78.18756436805,82.675374708005));
#122295=CARTESIAN_POINT('Ctrl Pts',(-9.16767680505891,84.3279816375,77.109502645435));
#122296=CARTESIAN_POINT('Ctrl Pts',(-8.96787365474291,84.30727308569,68.821968198105));
#122297=CARTESIAN_POINT('Ctrl Pts',(-8.76807050442691,78.13920519194,63.285515123434));
#122298=CARTESIAN_POINT('Ctrl Pts',(-8.56826735411091,69.89662703841,64.163123294247));
#122299=CARTESIAN_POINT('Ctrl Pts',(-8.43506525390091,66.65138462743,68.622440986855));
#122300=CARTESIAN_POINT('Ctrl Pts',(-8.36846420379491,66.12404568677,71.098635427588));
#122301=CARTESIAN_POINT('Ctrl Pts',(-10.0535560729899,67.62520219141,67.700413019766));
#122302=CARTESIAN_POINT('Ctrl Pts',(-9.98695502288491,66.1498345501,69.757818081886));
#122303=CARTESIAN_POINT('Ctrl Pts',(-9.85375292267391,65.03881684527,75.159924360853));
#122304=CARTESIAN_POINT('Ctrl Pts',(-9.65394977235791,69.94095953137,81.84418107373));
#122305=CARTESIAN_POINT('Ctrl Pts',(-9.45414662204191,78.18756436805,82.675374708005));
#122306=CARTESIAN_POINT('Ctrl Pts',(-9.25434347172591,84.3279816375,77.109502645435));
#122307=CARTESIAN_POINT('Ctrl Pts',(-9.05454032140991,84.30727308569,68.821968198105));
#122308=CARTESIAN_POINT('Ctrl Pts',(-8.85473717109391,78.13920519194,63.285515123434));
#122309=CARTESIAN_POINT('Ctrl Pts',(-8.65493402077791,69.89662703841,64.163123294247));
#122310=CARTESIAN_POINT('Ctrl Pts',(-8.52173192056691,66.65138462743,68.622440986855));
#122311=CARTESIAN_POINT('Ctrl Pts',(-8.45513087046191,66.12404568677,71.098635427588));
#122312=CARTESIAN_POINT('Ctrl Pts',(-10.1402227396569,67.62520219141,67.700413019766));
#122313=CARTESIAN_POINT('Ctrl Pts',(-10.0736216895509,66.1498345501,69.757818081886));
#122314=CARTESIAN_POINT('Ctrl Pts',(-9.94041958933991,65.03881684527,75.159924360853));
#122315=CARTESIAN_POINT('Ctrl Pts',(-9.74061643902391,69.94095953137,81.84418107373));
#122316=CARTESIAN_POINT('Ctrl Pts',(-9.54081328870791,78.18756436805,82.675374708005));
#122317=CARTESIAN_POINT('Ctrl Pts',(-9.34101013839191,84.3279816375,77.109502645435));
#122318=CARTESIAN_POINT('Ctrl Pts',(-9.14120698807591,84.30727308569,68.821968198105));
#122319=CARTESIAN_POINT('Ctrl Pts',(-8.94140383775991,78.13920519194,63.285515123434));
#122320=CARTESIAN_POINT('Ctrl Pts',(-8.74160068744491,69.89662703841,64.163123294247));
#122321=CARTESIAN_POINT('Ctrl Pts',(-8.60839858723391,66.65138462743,68.622440986855));
#122322=CARTESIAN_POINT('Ctrl Pts',(-8.54179753712891,66.12404568677,71.098635427588));
#122323=CARTESIAN_POINT('Ctrl Pts',(-10.1421564156154,67.62520219141,67.700413019766));
#122324=CARTESIAN_POINT('Ctrl Pts',(-10.0755553655094,66.1498345501,69.757818081886));
#122325=CARTESIAN_POINT('Ctrl Pts',(-9.94235326529838,65.03881684527,75.159924360853));
#122326=CARTESIAN_POINT('Ctrl Pts',(-9.74255011498238,69.94095953137,81.84418107373));
#122327=CARTESIAN_POINT('Ctrl Pts',(-9.54274696466638,78.18756436805,82.675374708005));
#122328=CARTESIAN_POINT('Ctrl Pts',(-9.34294381435038,84.3279816375,77.109502645435));
#122329=CARTESIAN_POINT('Ctrl Pts',(-9.14314066403438,84.30727308569,68.821968198105));
#122330=CARTESIAN_POINT('Ctrl Pts',(-8.94333751371838,78.13920519194,63.285515123434));
#122331=CARTESIAN_POINT('Ctrl Pts',(-8.7435343634034,69.89662703841,64.163123294247));
#122332=CARTESIAN_POINT('Ctrl Pts',(-8.6103322631924,66.65138462743,68.622440986855));
#122333=CARTESIAN_POINT('Ctrl Pts',(-8.5437312130874,66.12404568677,71.098635427588));
#122334=CARTESIAN_POINT('Ctrl Pts',(-10.1440900915739,67.62520219141,67.700413019766));
#122335=CARTESIAN_POINT('Ctrl Pts',(-10.0774890414678,66.1498345501,69.757818081886));
#122336=CARTESIAN_POINT('Ctrl Pts',(-9.94428694125685,65.03881684527,75.159924360853));
#122337=CARTESIAN_POINT('Ctrl Pts',(-9.74448379094085,69.94095953137,81.84418107373));
#122338=CARTESIAN_POINT('Ctrl Pts',(-9.54468064062485,78.18756436805,82.675374708005));
#122339=CARTESIAN_POINT('Ctrl Pts',(-9.34487749030885,84.3279816375,77.109502645435));
#122340=CARTESIAN_POINT('Ctrl Pts',(-9.14507433999285,84.30727308569,68.821968198105));
#122341=CARTESIAN_POINT('Ctrl Pts',(-8.94527118967685,78.13920519194,63.285515123434));
#122342=CARTESIAN_POINT('Ctrl Pts',(-8.74546803936189,69.89662703841,64.163123294247));
#122343=CARTESIAN_POINT('Ctrl Pts',(-8.61226593915089,66.65138462743,68.622440986855));
#122344=CARTESIAN_POINT('Ctrl Pts',(-8.54566488904589,66.12404568677,71.098635427588));
#122345=CARTESIAN_POINT('Ctrl Pts',(-10.1460237675324,67.62520219141,67.700413019766));
#122346=CARTESIAN_POINT('Ctrl Pts',(-10.0794227174263,66.1498345501,69.757818081886));
#122347=CARTESIAN_POINT('Ctrl Pts',(-9.94622061721532,65.03881684527,75.159924360853));
#122348=CARTESIAN_POINT('Ctrl Pts',(-9.74641746689932,69.94095953137,81.84418107373));
#122349=CARTESIAN_POINT('Ctrl Pts',(-9.54661431658332,78.18756436805,82.675374708005));
#122350=CARTESIAN_POINT('Ctrl Pts',(-9.34681116626732,84.3279816375,77.109502645435));
#122351=CARTESIAN_POINT('Ctrl Pts',(-9.14700801595132,84.30727308569,68.821968198105));
#122352=CARTESIAN_POINT('Ctrl Pts',(-8.94720486563532,78.13920519194,63.285515123434));
#122353=CARTESIAN_POINT('Ctrl Pts',(-8.74740171532038,69.89662703841,64.163123294247));
#122354=CARTESIAN_POINT('Ctrl Pts',(-8.61419961510938,66.65138462743,68.622440986855));
#122355=CARTESIAN_POINT('Ctrl Pts',(-8.54759856500438,66.12404568677,71.098635427588));
#122356=CARTESIAN_POINT('',(-10.0985254849308,67.012152548955,68.6936268712446));
#122357=CARTESIAN_POINT('',(-9.85448379345391,67.0101053268475,68.6926900228996));
#122358=CARTESIAN_POINT('Ctrl Pts',(-10.1056201537506,67.0100609947306,
68.6927734040079));
#122359=CARTESIAN_POINT('Ctrl Pts',(-10.0858657783411,66.6267587441179,
69.4137083799558));
#122360=CARTESIAN_POINT('Ctrl Pts',(-10.0674517206336,66.3421922385653,
70.187160389714));
#122361=CARTESIAN_POINT('Ctrl Pts',(-10.0354771245178,66.0641744360156,
71.41530529054));
#122362=CARTESIAN_POINT('Ctrl Pts',(-10.0234229206655,65.9970171979819,
71.8541444907421));
#122363=CARTESIAN_POINT('Ctrl Pts',(-10.0022989220673,65.9387470053738,
72.5774629218321));
#122364=CARTESIAN_POINT('Ctrl Pts',(-9.99380990519663,65.9289357827518,
72.8605855183034));
#122365=CARTESIAN_POINT('Ctrl Pts',(-9.97011755037087,65.9384360540978,
73.6524999818985));
#122366=CARTESIAN_POINT('Ctrl Pts',(-9.95498934267005,65.9872704953509,
74.1608327726866));
#122367=CARTESIAN_POINT('Ctrl Pts',(-9.93289270928219,66.1395396585373,
74.9780926170575));
#122368=CARTESIAN_POINT('Ctrl Pts',(-9.92514464639115,66.2160738287241,
75.2894488228344));
#122369=CARTESIAN_POINT('Ctrl Pts',(-9.90675928447394,66.4481877519415,
76.0511949084095));
#122370=CARTESIAN_POINT('Ctrl Pts',(-9.89630776232476,66.6238583447981,
76.4950140682969));
#122371=CARTESIAN_POINT('Ctrl Pts',(-9.87665530166429,66.9867250370315,
77.2381296826608));
#122372=CARTESIAN_POINT('Ctrl Pts',(-9.86799181905648,67.1588289504397,
77.5448386454165));
#122373=CARTESIAN_POINT('Ctrl Pts',(-9.83474755552943,67.8577859554754,
78.6415461446342));
#122374=CARTESIAN_POINT('Ctrl Pts',(-9.80803618459269,68.4906818730782,
79.3663681222012));
#122375=CARTESIAN_POINT('Ctrl Pts',(-9.76845513375547,69.5268040522261,
80.2340080815034));
#122376=CARTESIAN_POINT('Ctrl Pts',(-9.75634104363941,69.8522607993321,
80.471575968419));
#122377=CARTESIAN_POINT('Ctrl Pts',(-9.73562568268234,70.4685501783667,
80.8586624789983));
#122378=CARTESIAN_POINT('Ctrl Pts',(-9.72704885670965,70.7519521275781,
81.0148065063888));
#122379=CARTESIAN_POINT('Ctrl Pts',(-9.70232993771758,71.6516208700326,
81.4468481791628));
#122380=CARTESIAN_POINT('Ctrl Pts',(-9.68780978107427,72.2924085246533,
81.6680928606966));
#122381=CARTESIAN_POINT('Ctrl Pts',(-9.66477679705922,73.2570983554498,
81.8880275039081));
#122382=CARTESIAN_POINT('Ctrl Pts',(-9.65716697850892,73.5685498652193,
81.9425296255044));
#122383=CARTESIAN_POINT('Ctrl Pts',(-9.63079350027746,74.5787643785797,
82.0672627216527));
#122384=CARTESIAN_POINT('Ctrl Pts',(-9.60979911610278,75.2860288566837,
82.0752133493487));
#122385=CARTESIAN_POINT('Ctrl Pts',(-9.57636424384008,76.408719975205,81.9587410683443));
#122386=CARTESIAN_POINT('Ctrl Pts',(-9.5638092569189,76.8300110796484,81.8849983390011));
#122387=CARTESIAN_POINT('Ctrl Pts',(-9.53999615768963,77.6650508781469,
81.6749819617454));
#122388=CARTESIAN_POINT('Ctrl Pts',(-9.52918351341566,78.0735305819472,
81.5388149512676));
#122389=CARTESIAN_POINT('Ctrl Pts',(-9.49784468673609,79.2748170163315,
81.0356105848816));
#122390=CARTESIAN_POINT('Ctrl Pts',(-9.47764772497503,80.0258135580735,
80.5810569454226));
#122391=CARTESIAN_POINT('Ctrl Pts',(-9.43962677527073,81.2030303086033,
79.6247405516389));
#122392=CARTESIAN_POINT('Ctrl Pts',(-9.42246712903821,81.6641786070497,
79.1635366659919));
#122393=CARTESIAN_POINT('Ctrl Pts',(-9.39387315677519,82.2894133043008,
78.3914213853036));
#122394=CARTESIAN_POINT('Ctrl Pts',(-9.38341740832812,82.4917721834501,
78.1107530810851));
#122395=CARTESIAN_POINT('Ctrl Pts',(-9.35973644735305,82.9139163017574,
77.4477969979189));
#122396=CARTESIAN_POINT('Ctrl Pts',(-9.34660691469877,83.1230928738138,
77.0589116166437));
#122397=CARTESIAN_POINT('Ctrl Pts',(-9.32459867969423,83.4586217794764,
76.2993696292396));
#122398=CARTESIAN_POINT('Ctrl Pts',(-9.31541138867127,83.5915616317143,
75.932183219999));
#122399=CARTESIAN_POINT('Ctrl Pts',(-9.28836179847158,83.9228722685685,
74.7883461178696));
#122400=CARTESIAN_POINT('Ctrl Pts',(-9.27067528707267,84.0422668468796,
73.9887398515901));
#122401=CARTESIAN_POINT('Ctrl Pts',(-9.23609197264821,84.0696989172094,
72.6868145105387));
#122402=CARTESIAN_POINT('Ctrl Pts',(-9.2218955699631,84.0401778552934,72.1848321359113));
#122403=CARTESIAN_POINT('Ctrl Pts',(-9.18306129567446,83.8528090878916,
70.8507049131391));
#122404=CARTESIAN_POINT('Ctrl Pts',(-9.15351833944773,83.6043238906748,
69.8915616477434));
#122405=CARTESIAN_POINT('Ctrl Pts',(-9.11312336352832,82.8859730463364,
68.4763625114011));
#122406=CARTESIAN_POINT('Ctrl Pts',(-9.1018164298601,82.6346820516927,68.0685004412505));
#122407=CARTESIAN_POINT('Ctrl Pts',(-9.07160828662411,81.8749572103008,
67.0276762953672));
#122408=CARTESIAN_POINT('Ctrl Pts',(-9.05281212830922,81.3090550776609,
66.4356804440943));
#122409=CARTESIAN_POINT('Ctrl Pts',(-9.02087352722843,80.3919244403997,
65.6954459142547));
#122410=CARTESIAN_POINT('Ctrl Pts',(-9.01014874711913,80.0922263287438,
65.4813487697423));
#122411=CARTESIAN_POINT('Ctrl Pts',(-8.97802486309619,79.1834863086863,
64.9109673589789));
#122412=CARTESIAN_POINT('Ctrl Pts',(-8.95607643694238,78.5430298334253,
64.604680300816));
#122413=CARTESIAN_POINT('Ctrl Pts',(-8.93114078948074,77.6373105266441,
64.3018784374812));
#122414=CARTESIAN_POINT('Ctrl Pts',(-8.92511398649856,77.3977461094428,
64.2333870070539));
#122415=CARTESIAN_POINT('Ctrl Pts',(-8.90618495150541,76.6077965411486,
64.0434804307023));
#122416=CARTESIAN_POINT('Ctrl Pts',(-8.89392940839807,76.0470459905734,
63.9647069748064));
#122417=CARTESIAN_POINT('Ctrl Pts',(-8.8621805569852,74.7288603894014,63.9009008652572));
#122418=CARTESIAN_POINT('Ctrl Pts',(-8.8423851688574,73.9685550763677,63.9568528698512));
#122419=CARTESIAN_POINT('Ctrl Pts',(-8.79712880032208,72.3679595129946,
64.2710478711938));
#122420=CARTESIAN_POINT('Ctrl Pts',(-8.77056908072397,71.5320945510507,
64.5602948838878));
#122421=CARTESIAN_POINT('Ctrl Pts',(-8.7356019826268,70.44819469651,65.1297891983091));
#122422=CARTESIAN_POINT('Ctrl Pts',(-8.72638528489723,70.1513073666477,
65.3098447556629));
#122423=CARTESIAN_POINT('Ctrl Pts',(-8.70755440340243,69.5281095573045,
65.7405384651327));
#122424=CARTESIAN_POINT('Ctrl Pts',(-8.69809474021031,69.2072887729914,
65.9972096785191));
#122425=CARTESIAN_POINT('Ctrl Pts',(-8.67461105541209,68.4536022927773,
66.6882193607657));
#122426=CARTESIAN_POINT('Ctrl Pts',(-8.66059211699792,68.0436150970389,
67.14774252102));
#122427=CARTESIAN_POINT('Ctrl Pts',(-8.62796634820956,67.3144144402831,
68.146245304326));
#122428=CARTESIAN_POINT('Ctrl Pts',(-8.60948912160607,66.9966010470373,
68.6871096557166));
#122429=CARTESIAN_POINT('Ctrl Pts',(-8.58347171193975,66.6287424326869,
69.4905465658079));
#122430=CARTESIAN_POINT('Ctrl Pts',(-8.57584088745256,66.530635313355,69.7314186039164));
#122431=CARTESIAN_POINT('Ctrl Pts',(-8.56837920259168,66.4431891936119,
69.9761209669341));
#122432=CARTESIAN_POINT('Ctrl Pts',(-9.99199816632791,67.59428425961,67.303209521688));
#122433=CARTESIAN_POINT('Ctrl Pts',(-9.95025389358791,66.60009764549,68.598158170228));
#122434=CARTESIAN_POINT('Ctrl Pts',(-9.86676534810891,65.30823381695,71.71969580549));
#122435=CARTESIAN_POINT('Ctrl Pts',(-9.74153252989091,65.975649193,76.744817636531));
#122436=CARTESIAN_POINT('Ctrl Pts',(-9.61629971167191,69.0702482942,80.759474381881));
#122437=CARTESIAN_POINT('Ctrl Pts',(-9.49106689345391,73.75942478415,82.684532165368));
#122438=CARTESIAN_POINT('Ctrl Pts',(-9.36583407523591,78.78224537899,82.00215805984));
#122439=CARTESIAN_POINT('Ctrl Pts',(-9.24060125701691,82.78791878897,78.895896207008));
#122440=CARTESIAN_POINT('Ctrl Pts',(-9.11536843879891,84.6992258503,74.201089045577));
#122441=CARTESIAN_POINT('Ctrl Pts',(-8.99013562057991,84.00216577159,69.180291345096));
#122442=CARTESIAN_POINT('Ctrl Pts',(-8.86490280236191,80.88419637879,65.183721669986));
#122443=CARTESIAN_POINT('Ctrl Pts',(-8.73966998414291,76.18381732287,63.28615857581));
#122444=CARTESIAN_POINT('Ctrl Pts',(-8.61443716592491,71.16508250412,63.997905008714));
#122445=CARTESIAN_POINT('Ctrl Pts',(-8.48920434770591,67.17764413613,67.127552977624));
#122446=CARTESIAN_POINT('Ctrl Pts',(-8.36397152948791,65.29387078721,71.833466448308));
#122447=CARTESIAN_POINT('Ctrl Pts',(-8.23873871126891,66.02018597587,76.850086687758));
#122448=CARTESIAN_POINT('Ctrl Pts',(-8.11350589305091,69.16190222137,80.828391821067));
#122449=CARTESIAN_POINT('Ctrl Pts',(-8.03001734757191,72.30180432462,82.07495675794));
#122450=CARTESIAN_POINT('Ctrl Pts',(-7.98827307483191,73.92349052215,82.263193053033));
#122451=CARTESIAN_POINT('Ctrl Pts',(-10.2225811782039,67.91107137654,67.546420332812));
#122452=CARTESIAN_POINT('Ctrl Pts',(-10.1808369054639,66.95941211861,68.78597621942));
#122453=CARTESIAN_POINT('Ctrl Pts',(-10.0973483599859,65.72280909565,71.77398686789));
#122454=CARTESIAN_POINT('Ctrl Pts',(-9.97211554176791,66.36167509171,76.584153937925));
#122455=CARTESIAN_POINT('Ctrl Pts',(-9.84688272354991,69.32389952966,80.42707960685));
#122456=CARTESIAN_POINT('Ctrl Pts',(-9.72164990533191,73.81249166652,82.269791061293));
#122457=CARTESIAN_POINT('Ctrl Pts',(-9.59641708711391,78.6204559381,81.616606210807));
#122458=CARTESIAN_POINT('Ctrl Pts',(-9.47118426889691,82.45478254308,78.643217907434));
#122459=CARTESIAN_POINT('Ctrl Pts',(-9.34595145067991,84.28433147665,74.149235956863));
#122460=CARTESIAN_POINT('Ctrl Pts',(-9.22071863246191,83.61708886061,69.343208048245));
#122461=CARTESIAN_POINT('Ctrl Pts',(-9.09548581424491,80.63249381933,65.517595756513));
#122462=CARTESIAN_POINT('Ctrl Pts',(-8.97025299602791,76.13317831779,63.701202877746));
#122463=CARTESIAN_POINT('Ctrl Pts',(-8.84502017781091,71.32912504901,64.382503624079));
#122464=CARTESIAN_POINT('Ctrl Pts',(-8.71978735959391,67.51225346334,67.37827767835));
#122465=CARTESIAN_POINT('Ctrl Pts',(-8.59455454137691,65.70906045929,71.88289085437));
#122466=CARTESIAN_POINT('Ctrl Pts',(-8.46932172315991,66.40430676786,76.684919997149));
#122467=CARTESIAN_POINT('Ctrl Pts',(-8.34408890494191,69.41163286577,80.493049031652));
#122468=CARTESIAN_POINT('Ctrl Pts',(-8.26060035946391,72.41722242321,81.686290869658));
#122469=CARTESIAN_POINT('Ctrl Pts',(-8.21885608672491,73.96953932369,81.866475163376));
#122470=CARTESIAN_POINT('Ctrl Pts',(-10.4531641900799,68.22785849346,67.789631143935));
#122471=CARTESIAN_POINT('Ctrl Pts',(-10.4114199173409,67.31872659173,68.973794268612));
#122472=CARTESIAN_POINT('Ctrl Pts',(-10.3279313718619,66.13738437435,71.82827793029));
#122473=CARTESIAN_POINT('Ctrl Pts',(-10.2026985536429,66.74770099042,76.423490239315));
#122474=CARTESIAN_POINT('Ctrl Pts',(-10.0774657354239,69.57755076511,80.09468483181));
#122475=CARTESIAN_POINT('Ctrl Pts',(-9.95223291720491,73.86555854886,81.855049957214));
#122476=CARTESIAN_POINT('Ctrl Pts',(-9.82700009898591,78.45866649718,81.231054361786));
#122477=CARTESIAN_POINT('Ctrl Pts',(-9.70176728076691,82.12164629715,78.390539607897));
#122478=CARTESIAN_POINT('Ctrl Pts',(-9.57653446254691,83.86943710299,74.097382868212));
#122479=CARTESIAN_POINT('Ctrl Pts',(-9.45130164432791,83.23201194965,69.506124751474));
#122480=CARTESIAN_POINT('Ctrl Pts',(-9.32606882610791,80.38079125995,65.851469843104));
#122481=CARTESIAN_POINT('Ctrl Pts',(-9.20083600788791,76.08253931283,64.116247179702));
#122482=CARTESIAN_POINT('Ctrl Pts',(-9.07560318966791,71.49316759404,64.76710223939));
#122483=CARTESIAN_POINT('Ctrl Pts',(-8.95037037144891,67.84686279065,67.629002378947));
#122484=CARTESIAN_POINT('Ctrl Pts',(-8.82513755322891,66.1242501314,71.932315260248));
#122485=CARTESIAN_POINT('Ctrl Pts',(-8.69990473500891,66.78842755977,76.519753306352));
#122486=CARTESIAN_POINT('Ctrl Pts',(-8.57467191678891,69.66136350999,80.1577062421));
#122487=CARTESIAN_POINT('Ctrl Pts',(-8.49118337130991,72.53264052159,81.29762498131));
#122488=CARTESIAN_POINT('Ctrl Pts',(-8.44943909856991,74.01558812501,81.469757273692));
#122489=CARTESIAN_POINT('Ctrl Pts',(-10.6837472019569,68.54464561039,68.032841955058));
#122490=CARTESIAN_POINT('Ctrl Pts',(-10.6420029292169,67.67804106486,69.161612317803));
#122491=CARTESIAN_POINT('Ctrl Pts',(-10.5585143837379,66.55195965305,71.882568992689));
#122492=CARTESIAN_POINT('Ctrl Pts',(-10.4332815655199,67.13372688913,76.262826540709));
#122493=CARTESIAN_POINT('Ctrl Pts',(-10.3080487473019,69.83120200056,79.762290056778));
#122494=CARTESIAN_POINT('Ctrl Pts',(-10.1828159290829,73.91862543122,81.440308853139));
#122495=CARTESIAN_POINT('Ctrl Pts',(-10.0575831108649,78.29687705629,80.845502512754));
#122496=CARTESIAN_POINT('Ctrl Pts',(-9.93235029264591,81.78851005125,78.137861308325));
#122497=CARTESIAN_POINT('Ctrl Pts',(-9.80711747442791,83.45454272935,74.0455297795));
#122498=CARTESIAN_POINT('Ctrl Pts',(-9.68188465620991,82.84693503866,69.669041454627));
#122499=CARTESIAN_POINT('Ctrl Pts',(-9.55665183799091,80.1290887005,66.185343929634));
#122500=CARTESIAN_POINT('Ctrl Pts',(-9.43141901977291,76.03190030776,64.531291481639));
#122501=CARTESIAN_POINT('Ctrl Pts',(-9.30618620155491,71.65721013894,65.151700854752));
#122502=CARTESIAN_POINT('Ctrl Pts',(-9.18095338333591,68.18147211787,67.879727079667));
#122503=CARTESIAN_POINT('Ctrl Pts',(-9.05572056511791,66.53943980348,71.981739666301));
#122504=CARTESIAN_POINT('Ctrl Pts',(-8.93048774689891,67.17254835176,76.354586615735));
#122505=CARTESIAN_POINT('Ctrl Pts',(-8.80525492868091,69.91109415439,79.822363452678));
#122506=CARTESIAN_POINT('Ctrl Pts',(-8.72176638320191,72.64805862017,80.908959093025));
#122507=CARTESIAN_POINT('Ctrl Pts',(-8.68002211046191,74.06163692655,81.073039384034));
#122508=CARTESIAN_POINT('',(-10.0976119119436,67.0107639369115,68.6928899475042));
#122509=CARTESIAN_POINT('Ctrl Pts',(-13.1454639400434,80.45858984268,79.025262748814));
#122510=CARTESIAN_POINT('Ctrl Pts',(-13.1047676696649,81.48759917444,78.094747098224));
#122511=CARTESIAN_POINT('Ctrl Pts',(-13.023375128908,83.05789139581,75.697173136178));
#122512=CARTESIAN_POINT('Ctrl Pts',(-12.9012863177725,83.35252030674,71.406833513058));
#122513=CARTESIAN_POINT('Ctrl Pts',(-12.779197506637,81.50958548889,67.521577101676));
#122514=CARTESIAN_POINT('Ctrl Pts',(-12.6571086955016,78.00102966728,65.03524813757));
#122515=CARTESIAN_POINT('Ctrl Pts',(-12.535019884366,73.72453794147,64.584146732116));
#122516=CARTESIAN_POINT('Ctrl Pts',(-12.4129310732305,69.77442198226,66.283678758148));
#122517=CARTESIAN_POINT('Ctrl Pts',(-12.2908422620949,67.16144589233,69.698967665193));
#122518=CARTESIAN_POINT('Ctrl Pts',(-12.1687534509593,66.5542301033,73.956094258219));
#122519=CARTESIAN_POINT('Ctrl Pts',(-12.0466646398237,68.10815086311,77.965728779761));
#122520=CARTESIAN_POINT('Ctrl Pts',(-11.9245758286881,71.42558498136,80.70187013362));
#122521=CARTESIAN_POINT('Ctrl Pts',(-11.8024870175525,75.65765439615,81.464383794463));
#122522=CARTESIAN_POINT('Ctrl Pts',(-11.6803982064169,79.72144063224,80.058154773716));
#122523=CARTESIAN_POINT('Ctrl Pts',(-11.5583093952809,82.57708616044,76.843014459137));
#122524=CARTESIAN_POINT('Ctrl Pts',(-11.4362205841459,83.49387722752,72.6416655369233));
#122525=CARTESIAN_POINT('Ctrl Pts',(-11.3141317730099,82.23722174699,68.52916561233));
#122526=CARTESIAN_POINT('Ctrl Pts',(-11.1920429618739,79.12867764146,65.557837261156));
#122527=CARTESIAN_POINT('Ctrl Pts',(-11.0699541507389,74.96367134257,64.48799561084));
#122528=CARTESIAN_POINT('Ctrl Pts',(-10.9478653396029,70.80796096272,65.593395929895));
#122529=CARTESIAN_POINT('Ctrl Pts',(-10.8257765284669,67.72492593816,68.59118405853));
#122530=CARTESIAN_POINT('Ctrl Pts',(-10.7036877173319,66.50346533712,72.714274237664));
#122531=CARTESIAN_POINT('Ctrl Pts',(-10.5815989061959,67.45613127848,76.907634016596));
#122532=CARTESIAN_POINT('Ctrl Pts',(-10.4595100950609,70.33915187332,80.09825008004));
#122533=CARTESIAN_POINT('Ctrl Pts',(-10.3374212839249,74.4148085262,81.46969511541));
#122534=CARTESIAN_POINT('Ctrl Pts',(-10.2153324727889,78.64020627051,80.671038351543));
#122535=CARTESIAN_POINT('Ctrl Pts',(-10.0932436616539,81.93413376206,77.906643386292));
#122536=CARTESIAN_POINT('Ctrl Pts',(-9.97115485051791,83.45372806371,73.8838737528785));
#122537=CARTESIAN_POINT('Ctrl Pts',(-9.84906603938191,82.81014898713,69.632093987784));
#122538=CARTESIAN_POINT('Ctrl Pts',(-9.72697722824691,80.16807974905,66.239256812192));
#122539=CARTESIAN_POINT('Ctrl Pts',(-9.60488841711091,76.20357708221,64.573569483865));
#122540=CARTESIAN_POINT('Ctrl Pts',(-9.48279960597591,71.93111689791,65.061124710008));
#122541=CARTESIAN_POINT('Ctrl Pts',(-9.36071079483991,68.44386550154,67.577649690078));
#122542=CARTESIAN_POINT('Ctrl Pts',(-9.27931825408291,67.23760922485,70.177481292106));
#122543=CARTESIAN_POINT('Ctrl Pts',(-9.23862198370491,66.9910877936,71.542745649207));
#122544=CARTESIAN_POINT('Ctrl Pts',(-13.3760469519197,80.72646219088,79.321488981906));
#122545=CARTESIAN_POINT('Ctrl Pts',(-13.3353506815413,81.80596865723,78.345309630701));
#122546=CARTESIAN_POINT('Ctrl Pts',(-13.2539581407843,83.45332068284,75.83007821761));
#122547=CARTESIAN_POINT('Ctrl Pts',(-13.1318693296489,83.76240807855,71.329196424715));
#122548=CARTESIAN_POINT('Ctrl Pts',(-13.0097805185134,81.82903391805,67.253276712327));
#122549=CARTESIAN_POINT('Ctrl Pts',(-12.8876917073779,78.14830082834,64.644934774693));
#122550=CARTESIAN_POINT('Ctrl Pts',(-12.7656028962424,73.66194649816,64.171696224628));
#122551=CARTESIAN_POINT('Ctrl Pts',(-12.6435140851068,69.51798435007,65.954630310129));
#122552=CARTESIAN_POINT('Ctrl Pts',(-12.5214252739713,66.77678026333,69.537519547239));
#122553=CARTESIAN_POINT('Ctrl Pts',(-12.3993364628357,66.13976624364,74.003558428952));
#122554=CARTESIAN_POINT('Ctrl Pts',(-12.2772476517001,67.76994340206,78.209959926145));
#122555=CARTESIAN_POINT('Ctrl Pts',(-12.1551588405645,71.2501757691,81.080373432798));
#122556=CARTESIAN_POINT('Ctrl Pts',(-12.0330700294289,75.68992782805,81.880306341227));
#122557=CARTESIAN_POINT('Ctrl Pts',(-11.9109812182932,79.95313845632,80.405068678906));
#122558=CARTESIAN_POINT('Ctrl Pts',(-11.7888924071576,82.94892063066,77.032150034994));
#122559=CARTESIAN_POINT('Ctrl Pts',(-11.666803596022,83.91070188439,72.624626032068));
#122560=CARTESIAN_POINT('Ctrl Pts',(-11.5447147848859,82.59237786598,68.310311161955));
#122561=CARTESIAN_POINT('Ctrl Pts',(-11.4226259737509,79.33128648485,65.193169198556));
#122562=CARTESIAN_POINT('Ctrl Pts',(-11.3005371626149,74.96188856657,64.070826627081));
#122563=CARTESIAN_POINT('Ctrl Pts',(-11.1784483514789,70.60224275103,65.23047285722));
#122564=CARTESIAN_POINT('Ctrl Pts',(-11.0563595403439,67.36791227191,68.375373073155));
#122565=CARTESIAN_POINT('Ctrl Pts',(-10.9342707292079,66.08651027048,72.7007978991383));
#122566=CARTESIAN_POINT('Ctrl Pts',(-10.8121819180729,67.08592690573,77.0999407032));
#122567=CARTESIAN_POINT('Ctrl Pts',(-10.6900931069369,70.11042753827,80.447131604038));
#122568=CARTESIAN_POINT('Ctrl Pts',(-10.5680042958009,74.38609110676,81.885878307519));
#122569=CARTESIAN_POINT('Ctrl Pts',(-10.4459154846659,78.8188440927,81.048028625887));
#122570=CARTESIAN_POINT('Ctrl Pts',(-10.3238266735299,82.27441627954,78.147975002984));
#122571=CARTESIAN_POINT('Ctrl Pts',(-10.2017378623939,83.86858245883,73.9277938074277));
#122572=CARTESIAN_POINT('Ctrl Pts',(-10.0796490512589,83.19342067618,69.46736414145));
#122573=CARTESIAN_POINT('Ctrl Pts',(-9.95756024012291,80.4216957374,65.908028421839));
#122574=CARTESIAN_POINT('Ctrl Pts',(-9.83547142898791,76.26264087496,64.160599913318));
#122575=CARTESIAN_POINT('Ctrl Pts',(-9.71338261785191,71.78051592832,64.672081202253));
#122576=CARTESIAN_POINT('Ctrl Pts',(-9.59129380671691,68.12213274751,67.312100981366));
#122577=CARTESIAN_POINT('Ctrl Pts',(-9.50990126595991,66.8566812005,70.039515533604));
#122578=CARTESIAN_POINT('Ctrl Pts',(-9.46920499558091,66.59806208898,71.471778251044));
#122579=CARTESIAN_POINT('Ctrl Pts',(-13.6066299637959,80.99433453906,79.617715215002));
#122580=CARTESIAN_POINT('Ctrl Pts',(-13.5659336934176,82.12433814002,78.595872163185));
#122581=CARTESIAN_POINT('Ctrl Pts',(-13.4845411526607,83.84874996986,75.962983299055));
#122582=CARTESIAN_POINT('Ctrl Pts',(-13.3624523415252,84.17229585037,71.251559336391));
#122583=CARTESIAN_POINT('Ctrl Pts',(-13.2403635303897,82.14848234721,66.984976322999));
#122584=CARTESIAN_POINT('Ctrl Pts',(-13.1182747192542,78.29557198944,64.254621411829));
#122585=CARTESIAN_POINT('Ctrl Pts',(-12.9961859081187,73.59935505488,63.759245717135));
#122586=CARTESIAN_POINT('Ctrl Pts',(-12.8740970969832,69.26154671793,65.625581862084));
#122587=CARTESIAN_POINT('Ctrl Pts',(-12.7520082858476,66.39211463435,69.376071429236));
#122588=CARTESIAN_POINT('Ctrl Pts',(-12.629919474712,65.72530238397,74.051022599625));
#122589=CARTESIAN_POINT('Ctrl Pts',(-12.5078306635765,67.43173594097,78.454191072474));
#122590=CARTESIAN_POINT('Ctrl Pts',(-12.3857418524408,71.07476655678,81.458876731945));
#122591=CARTESIAN_POINT('Ctrl Pts',(-12.2636530413052,75.72220125986,82.296228887996));
#122592=CARTESIAN_POINT('Ctrl Pts',(-12.1415642301696,80.18483628034,80.751982584142));
#122593=CARTESIAN_POINT('Ctrl Pts',(-12.0194754190339,83.32075510084,77.221285610932));
#122594=CARTESIAN_POINT('Ctrl Pts',(-11.8973866078983,84.32752654126,72.6075865273095));
#122595=CARTESIAN_POINT('Ctrl Pts',(-11.7752977967627,82.94753398501,68.091456711666));
#122596=CARTESIAN_POINT('Ctrl Pts',(-11.653208985627,79.53389532833,64.828501136008));
#122597=CARTESIAN_POINT('Ctrl Pts',(-11.5311201744909,74.96010579067,63.653657643322));
#122598=CARTESIAN_POINT('Ctrl Pts',(-11.4090313633559,70.39652453943,64.867549784492));
#122599=CARTESIAN_POINT('Ctrl Pts',(-11.2869425522199,67.01089860571,68.159562087686));
#122600=CARTESIAN_POINT('Ctrl Pts',(-11.1648537410839,65.66955520384,72.6873215605024));
#122601=CARTESIAN_POINT('Ctrl Pts',(-11.0427649299489,66.71572253294,77.292247389707));
#122602=CARTESIAN_POINT('Ctrl Pts',(-10.9206761188129,69.88170320312,80.796013127978));
#122603=CARTESIAN_POINT('Ctrl Pts',(-10.7985873076779,74.35737368722,82.302061499622));
#122604=CARTESIAN_POINT('Ctrl Pts',(-10.6764984965419,78.99748191481,81.425018900273));
#122605=CARTESIAN_POINT('Ctrl Pts',(-10.5544096854059,82.61469879698,78.389306619751));
#122606=CARTESIAN_POINT('Ctrl Pts',(-10.4323208742709,84.28343685395,73.9717138620569));
#122607=CARTESIAN_POINT('Ctrl Pts',(-10.3102320631349,83.57669236526,69.30263429518));
#122608=CARTESIAN_POINT('Ctrl Pts',(-10.1881432519999,80.67531172579,65.57680003152));
#122609=CARTESIAN_POINT('Ctrl Pts',(-10.0660544408639,76.32170466775,63.747630342775));
#122610=CARTESIAN_POINT('Ctrl Pts',(-9.94396562972891,71.62991495875,64.283037694485));
#122611=CARTESIAN_POINT('Ctrl Pts',(-9.82187681859291,67.80039999349,67.046552272646));
#122612=CARTESIAN_POINT('Ctrl Pts',(-9.74048427783591,66.47575317615,69.901549775107));
#122613=CARTESIAN_POINT('Ctrl Pts',(-9.69978800745791,66.20503638435,71.400810852893));
#122614=CARTESIAN_POINT('Ctrl Pts',(-13.8372129756729,81.26220688726,79.913941448094));
#122615=CARTESIAN_POINT('Ctrl Pts',(-13.7965167052939,82.44270762281,78.846434695661));
#122616=CARTESIAN_POINT('Ctrl Pts',(-13.7151241645369,84.24417925689,76.095888380488));
#122617=CARTESIAN_POINT('Ctrl Pts',(-13.5930353534019,84.58218362219,71.173922248048));
#122618=CARTESIAN_POINT('Ctrl Pts',(-13.4709465422661,82.46793077636,66.716675933649));
#122619=CARTESIAN_POINT('Ctrl Pts',(-13.3488577311306,78.4428431505,63.864308048952));
#122620=CARTESIAN_POINT('Ctrl Pts',(-13.2267689199951,73.53676361156,63.346795209648));
#122621=CARTESIAN_POINT('Ctrl Pts',(-13.1046801088595,69.00510908574,65.296533414067));
#122622=CARTESIAN_POINT('Ctrl Pts',(-12.982591297724,66.00744900535,69.214623311284));
#122623=CARTESIAN_POINT('Ctrl Pts',(-12.8605024865884,65.31083852431,74.098486770361));
#122624=CARTESIAN_POINT('Ctrl Pts',(-12.7384136754528,67.09352847992,78.698422218861));
#122625=CARTESIAN_POINT('Ctrl Pts',(-12.6163248643172,70.89935734453,81.837380031125));
#122626=CARTESIAN_POINT('Ctrl Pts',(-12.4942360531816,75.75447469176,82.71215143476));
#122627=CARTESIAN_POINT('Ctrl Pts',(-12.3721472420459,80.41653410443,81.098896489329));
#122628=CARTESIAN_POINT('Ctrl Pts',(-12.2500584309103,83.69258957107,77.410421186785));
#122629=CARTESIAN_POINT('Ctrl Pts',(-12.1279696197746,84.74435119813,72.5905470224495));
#122630=CARTESIAN_POINT('Ctrl Pts',(-12.005880808639,83.302690104,67.872602261286));
#122631=CARTESIAN_POINT('Ctrl Pts',(-11.8837919975033,79.73650417172,64.463833073406));
#122632=CARTESIAN_POINT('Ctrl Pts',(-11.7617031863677,74.95832301467,63.236488659563));
#122633=CARTESIAN_POINT('Ctrl Pts',(-11.639614375232,70.19080632774,64.50462671182));
#122634=CARTESIAN_POINT('Ctrl Pts',(-11.5175255640959,66.65388493945,67.943751102315));
#122635=CARTESIAN_POINT('Ctrl Pts',(-11.3954367529609,65.25260013719,72.6738452219821));
#122636=CARTESIAN_POINT('Ctrl Pts',(-11.2733479418249,66.34551816019,77.484554076315));
#122637=CARTESIAN_POINT('Ctrl Pts',(-11.1512591306899,69.65297886808,81.144894651979));
#122638=CARTESIAN_POINT('Ctrl Pts',(-11.0291703195539,74.32865626779,82.718244691732));
#122639=CARTESIAN_POINT('Ctrl Pts',(-10.9070815084179,79.176119737,81.802009174614));
#122640=CARTESIAN_POINT('Ctrl Pts',(-10.7849926972829,82.95498131447,78.63063823644));
#122641=CARTESIAN_POINT('Ctrl Pts',(-10.6629038861469,84.69829124907,74.015633916602));
#122642=CARTESIAN_POINT('Ctrl Pts',(-10.5408150750119,83.95996405431,69.137904448843));
#122643=CARTESIAN_POINT('Ctrl Pts',(-10.4187262638759,80.92892771414,65.245571641166));
#122644=CARTESIAN_POINT('Ctrl Pts',(-10.2966374527399,76.3807684605,63.334660772228));
#122645=CARTESIAN_POINT('Ctrl Pts',(-10.1745486416049,71.47931398915,63.89399418673));
#122646=CARTESIAN_POINT('Ctrl Pts',(-10.0524598304689,67.47866723947,66.781003563935));
#122647=CARTESIAN_POINT('Ctrl Pts',(-9.97106728971191,66.0948251518,69.763584016604));
#122648=CARTESIAN_POINT('Ctrl Pts',(-9.93037101933391,65.81201067972,71.32984345473));
#122649=CARTESIAN_POINT('',(-13.5671411043958,83.559062666398,76.0030398856965));
#122650=CARTESIAN_POINT('Ctrl Pts',(-13.5675364833309,83.5597121396993,
76.003284345909));
#122651=CARTESIAN_POINT('Ctrl Pts',(-13.5675364833309,83.4568123740149,
76.2576560644358));
#122652=CARTESIAN_POINT('Ctrl Pts',(-13.5675364833306,83.3421517896857,
76.5072491508691));
#122653=CARTESIAN_POINT('Ctrl Pts',(-13.5675364833306,83.0901412786061,
76.9958065667943));
#122654=CARTESIAN_POINT('Ctrl Pts',(-13.5675364833309,82.9527179931296,
77.2347267130182));
#122655=CARTESIAN_POINT('Ctrl Pts',(-13.5675364833309,82.8047338290467,
77.4669045928492));
#122656=CARTESIAN_POINT('Ctrl Pts',(-13.5667373703007,83.5584173721563,
76.0027980283233));
#122657=CARTESIAN_POINT('Ctrl Pts',(-13.564075594742,83.592340938489,75.9066576672772));
#122658=CARTESIAN_POINT('Ctrl Pts',(-13.5614443082188,83.6246588263767,
75.8099515860624));
#122659=CARTESIAN_POINT('Ctrl Pts',(-13.5528805561748,83.7255380217485,
75.4903852147587));
#122660=CARTESIAN_POINT('Ctrl Pts',(-13.5470489678549,83.7872128263381,
75.2653495867716));
#122661=CARTESIAN_POINT('Ctrl Pts',(-13.5345639614118,83.9002282736153,
74.7800787709895));
#122662=CARTESIAN_POINT('Ctrl Pts',(-13.5279027197026,83.9490273837395,
74.5191127785177));
#122663=CARTESIAN_POINT('Ctrl Pts',(-13.5172661848976,84.0062659030078,
74.1128779791592));
#122664=CARTESIAN_POINT('Ctrl Pts',(-13.5134514878214,84.0229649995657,
73.9689943804952));
#122665=CARTESIAN_POINT('Ctrl Pts',(-13.5006780599591,84.0667101876582,
73.4915677406669));
#122666=CARTESIAN_POINT('Ctrl Pts',(-13.49153011449,84.0786264963019,73.1566509078807));
#122667=CARTESIAN_POINT('Ctrl Pts',(-13.4729263825575,84.0655098046931,
72.4769062914134));
#122668=CARTESIAN_POINT('Ctrl Pts',(-13.4634705515801,84.0392880090477,
72.1320526846346));
#122669=CARTESIAN_POINT('Ctrl Pts',(-13.450356846143,83.9744742638213,71.6448625935257));
#122670=CARTESIAN_POINT('Ctrl Pts',(-13.4464988064657,83.9517277642667,
71.5003802332486));
#122671=CARTESIAN_POINT('Ctrl Pts',(-13.4330174124397,83.8587193348971,
70.989577291242));
#122672=CARTESIAN_POINT('Ctrl Pts',(-13.4237734591929,83.7694743897222,
70.6267028826339));
#122673=CARTESIAN_POINT('Ctrl Pts',(-13.4107623419622,83.6148428033846,
70.1325839685342));
#122674=CARTESIAN_POINT('Ctrl Pts',(-13.4071042783417,83.5682706710727,
69.9954701646365));
#122675=CARTESIAN_POINT('Ctrl Pts',(-13.3997705438625,83.4697062984198,
69.7269846099298));
#122676=CARTESIAN_POINT('Ctrl Pts',(-13.3960969783972,83.4179375018191,
69.5957494947586));
#122677=CARTESIAN_POINT('Ctrl Pts',(-13.3863600580663,83.2744249480845,
69.2556865489435));
#122678=CARTESIAN_POINT('Ctrl Pts',(-13.3802233403998,83.1777076411274,
69.0489260936027));
#122679=CARTESIAN_POINT('Ctrl Pts',(-13.3642353284874,82.9081485026537,
68.5250273260032));
#122680=CARTESIAN_POINT('Ctrl Pts',(-13.3543039465761,82.7237894033983,
68.2137929137039));
#122681=CARTESIAN_POINT('Ctrl Pts',(-13.3385997299704,82.3996390811858,
67.7335478280627));
#122682=CARTESIAN_POINT('Ctrl Pts',(-13.3327347574751,82.2710304442392,
67.5569360377424));
#122683=CARTESIAN_POINT('Ctrl Pts',(-13.3232860326794,82.0497101593525,
67.2747633743399));
#122684=CARTESIAN_POINT('Ctrl Pts',(-13.3196387460536,81.9605972793141,
67.1663678592388));
#122685=CARTESIAN_POINT('Ctrl Pts',(-13.3098868170892,81.7120551150842,
66.877862131313));
#122686=CARTESIAN_POINT('Ctrl Pts',(-13.303869318848,81.5478733964024,66.7018423740798));
#122687=CARTESIAN_POINT('Ctrl Pts',(-13.2918801304206,81.20810462183,66.3655714889457));
#122688=CARTESIAN_POINT('Ctrl Pts',(-13.2859052916122,81.0326107033414,
66.2050781705628));
#122689=CARTESIAN_POINT('Ctrl Pts',(-13.2758786417514,80.7359781736785,
65.9549353524514));
#122690=CARTESIAN_POINT('Ctrl Pts',(-13.2719337647068,80.6186701800267,
65.8609971690494));
#122691=CARTESIAN_POINT('Ctrl Pts',(-13.2578861871576,80.197661633211,65.5408500301459));
#122692=CARTESIAN_POINT('Ctrl Pts',(-13.2475391732826,79.881765707429,65.3307048056643));
#122693=CARTESIAN_POINT('Ctrl Pts',(-13.2278220192659,79.2566252411988,
64.968591485336));
#122694=CARTESIAN_POINT('Ctrl Pts',(-13.2184503864139,78.9494020070053,
64.8130212923133));
#122695=CARTESIAN_POINT('Ctrl Pts',(-13.2053810712702,78.4985829896546,
64.6157036183555));
#122696=CARTESIAN_POINT('Ctrl Pts',(-13.201486622264,78.3612636850413,64.5595283514857));
#122697=CARTESIAN_POINT('Ctrl Pts',(-13.1912751694299,77.9919679476251,
64.4188457528643));
#122698=CARTESIAN_POINT('Ctrl Pts',(-13.1850745512282,77.75771183689,64.3403094362059));
#122699=CARTESIAN_POINT('Ctrl Pts',(-13.1723425719473,77.2703020673871,
64.1988175121525));
#122700=CARTESIAN_POINT('Ctrl Pts',(-13.1658078920904,77.0167147743859,
64.1369466091538));
#122701=CARTESIAN_POINT('Ctrl Pts',(-13.1551134668004,76.6102158677895,
64.05657975247));
#122702=CARTESIAN_POINT('Ctrl Pts',(-13.1510897667258,76.4589428399496,
64.0307232111347));
#122703=CARTESIAN_POINT('Ctrl Pts',(-13.1366065118578,75.9186504014741,
63.9525508618867));
#122704=CARTESIAN_POINT('Ctrl Pts',(-13.1258877181829,75.5265270032235,
63.9217977227068));
#122705=CARTESIAN_POINT('Ctrl Pts',(-13.1061387660654,74.8021638102403,
63.9116218425384));
#122706=CARTESIAN_POINT('Ctrl Pts',(-13.0971038211258,74.4699675554139,
63.9250115406869));
#122707=CARTESIAN_POINT('Ctrl Pts',(-13.0841859521077,73.9860025382002,
63.9708955159304));
#122708=CARTESIAN_POINT('Ctrl Pts',(-13.0801346581054,73.8328673009898,
63.9893202487664));
#122709=CARTESIAN_POINT('Ctrl Pts',(-13.0698525264644,73.4393650210581,
64.0468018451389));
#122710=CARTESIAN_POINT('Ctrl Pts',(-13.0637306563078,73.1998390097788,
64.0916281188541));
#122711=CARTESIAN_POINT('Ctrl Pts',(-13.0512170732183,72.713993539085,64.2030395987611));
#122712=CARTESIAN_POINT('Ctrl Pts',(-13.0448210725716,72.4677631456297,
64.270579210745));
#122713=CARTESIAN_POINT('Ctrl Pts',(-13.0341661133012,72.074517734885,64.3969280041532));
#122714=CARTESIAN_POINT('Ctrl Pts',(-13.0300303888732,71.9256084093377,
64.4491851464445));
#122715=CARTESIAN_POINT('Ctrl Pts',(-13.0134987819331,71.343000767011,64.6710253275285));
#122716=CARTESIAN_POINT('Ctrl Pts',(-13.0007317281315,70.9207089899708,
64.870532135827));
#122717=CARTESIAN_POINT('Ctrl Pts',(-12.9822116127472,70.3287077799567,
65.2074302125292));
#122718=CARTESIAN_POINT('Ctrl Pts',(-12.9763751415612,70.1451578642584,
65.3206270535002));
#122719=CARTESIAN_POINT('Ctrl Pts',(-12.9659649315537,69.8210882501108,
65.5365946790075));
#122720=CARTESIAN_POINT('Ctrl Pts',(-12.9613645499335,69.6790895582943,
65.6371699567346));
#122721=CARTESIAN_POINT('Ctrl Pts',(-12.9474535762678,69.2517199479968,
65.9585632774538));
#122722=CARTESIAN_POINT('Ctrl Pts',(-12.9384722719713,68.9762093686211,
66.1924796443799));
#122723=CARTESIAN_POINT('Ctrl Pts',(-12.9258413535345,68.614300180949,66.5393319777033));
#122724=CARTESIAN_POINT('Ctrl Pts',(-12.9222826170324,68.5151523215405,
66.638924521861));
#122725=CARTESIAN_POINT('Ctrl Pts',(-12.9146013600048,68.3093468719787,
66.8557053345773));
#122726=CARTESIAN_POINT('Ctrl Pts',(-12.9104646050691,68.2033750057172,
66.9734888532676));
#122727=CARTESIAN_POINT('Ctrl Pts',(-12.8939450494719,67.7977178914268,
67.4490636836859));
#122728=CARTESIAN_POINT('Ctrl Pts',(-12.8811816764342,67.5225170413055,
67.8277526797481));
#122729=CARTESIAN_POINT('Ctrl Pts',(-12.8622355477249,67.1568637793898,
68.4211831175986));
#122730=CARTESIAN_POINT('Ctrl Pts',(-12.8559943911129,67.0434249301038,
68.621833338459));
#122731=CARTESIAN_POINT('Ctrl Pts',(-12.8449569971097,66.8539793764485,
68.9884793111014));
#122732=CARTESIAN_POINT('Ctrl Pts',(-12.8401301655231,66.7750908408301,
69.1530037799877));
#122733=CARTESIAN_POINT('Ctrl Pts',(-12.826085500755,66.5564523644054,69.6463250323456));
#122734=CARTESIAN_POINT('Ctrl Pts',(-12.8171801930435,66.4308640256927,
69.981386793575));
#122735=CARTESIAN_POINT('Ctrl Pts',(-12.8045916096158,66.2838228836075,
70.4584977964471));
#122736=CARTESIAN_POINT('Ctrl Pts',(-12.8009903537789,66.2452030472901,
70.5952639474852));
#122737=CARTESIAN_POINT('Ctrl Pts',(-12.7930893845086,66.1688548682222,
70.89279144699));
#122738=CARTESIAN_POINT('Ctrl Pts',(-12.7887744392789,66.1322896222929,
71.0537958023746));
#122739=CARTESIAN_POINT('Ctrl Pts',(-12.7728051907319,66.014833578395,71.6460170351442));
#122740=CARTESIAN_POINT('Ctrl Pts',(-12.7608427566072,65.9609842654104,
72.0825832165419));
#122741=CARTESIAN_POINT('Ctrl Pts',(-12.7422445472057,65.9260444425325,
72.7663239634917));
#122742=CARTESIAN_POINT('Ctrl Pts',(-12.7355782073821,65.9233786337209,
73.012451328927));
#122743=CARTESIAN_POINT('Ctrl Pts',(-12.7238859406409,65.9362073925439,
73.449313466967));
#122744=CARTESIAN_POINT('Ctrl Pts',(-12.7188252174585,65.9477872686935,
73.6401820146338));
#122745=CARTESIAN_POINT('Ctrl Pts',(-12.7047983993841,65.9972648248628,
74.1766531939995));
#122746=CARTESIAN_POINT('Ctrl Pts',(-12.6961131093045,66.0489467690798,
74.5209729009366));
#122747=CARTESIAN_POINT('Ctrl Pts',(-12.6836459088926,66.1505500222828,
75.0046507446182));
#122748=CARTESIAN_POINT('Ctrl Pts',(-12.6799271639989,66.1842224256447,
75.1474594584057));
#122749=CARTESIAN_POINT('Ctrl Pts',(-12.6717235174104,66.2650516639478,
75.4557902382051));
#122750=CARTESIAN_POINT('Ctrl Pts',(-12.6672247126425,66.3134879406318,
75.6208672876483));
#122751=CARTESIAN_POINT('Ctrl Pts',(-12.6531757084016,66.4774940861465,
76.1257904975992));
#122752=CARTESIAN_POINT('Ctrl Pts',(-12.6434503837016,66.6087951896857,
76.4605145900957));
#122753=CARTESIAN_POINT('Ctrl Pts',(-12.6258030342205,66.88135216578,77.0507839403595));
#122754=CARTESIAN_POINT('Ctrl Pts',(-12.6178868748013,67.0160770530749,
77.3093887965338));
#122755=CARTESIAN_POINT('Ctrl Pts',(-12.6044136729505,67.2691109372457,
77.7433825391018));
#122756=CARTESIAN_POINT('Ctrl Pts',(-12.5988062683593,67.3817507577389,
77.922110938651));
#122757=CARTESIAN_POINT('Ctrl Pts',(-12.5882906799113,67.60825280591,78.2553264648053));
#122758=CARTESIAN_POINT('Ctrl Pts',(-12.5833813940964,67.7210573086567,
78.41053531039));
#122759=CARTESIAN_POINT('Ctrl Pts',(-12.5725479478004,67.9836142033438,
78.7486768244862));
#122760=CARTESIAN_POINT('Ctrl Pts',(-12.5666345801389,68.1358541457552,
78.9296633685733));
#122761=CARTESIAN_POINT('Ctrl Pts',(-12.5560814553162,68.4153494079624,
79.2363296886019));
#122762=CARTESIAN_POINT('Ctrl Pts',(-12.5514812092673,68.5393340464195,
79.36438391965));
#122763=CARTESIAN_POINT('Ctrl Pts',(-12.540188094451,68.8482087290248,79.6649048815689));
#122764=CARTESIAN_POINT('Ctrl Pts',(-12.5334414053335,69.0367483922625,
79.8334355772062));
#122765=CARTESIAN_POINT('Ctrl Pts',(-12.5156481711702,69.5472316402805,
80.2528513826252));
#122766=CARTESIAN_POINT('Ctrl Pts',(-12.5045078689187,69.8799499965225,
80.4906817912754));
#122767=CARTESIAN_POINT('Ctrl Pts',(-12.4883226190392,70.3911116671256,
80.8069128989764));
#122768=CARTESIAN_POINT('Ctrl Pts',(-12.4831582287761,70.558496888027,80.9033038675062));
#122769=CARTESIAN_POINT('Ctrl Pts',(-12.4734907321598,70.8813099343359,
81.0758447716644));
#122770=CARTESIAN_POINT('Ctrl Pts',(-12.4689745525381,71.0361780777578,
81.1530610916338));
#122771=CARTESIAN_POINT('Ctrl Pts',(-12.4570631524985,71.4569675669917,
81.3480902085793));
#122772=CARTESIAN_POINT('Ctrl Pts',(-12.4497988475183,71.7266747493541,
81.4577271304391));
#122773=CARTESIAN_POINT('Ctrl Pts',(-12.4383211700839,72.1541234716692,
81.60765414121));
#122774=CARTESIAN_POINT('Ctrl Pts',(-12.4341804007932,72.3083041762663,
81.6570566756748));
#122775=CARTESIAN_POINT('Ctrl Pts',(-12.4244611698138,72.6675205969803,
81.7614196825632));
#122776=CARTESIAN_POINT('Ctrl Pts',(-12.4188637003036,72.8730226382521,
81.813274778027));
#122777=CARTESIAN_POINT('Ctrl Pts',(-12.4004787803361,73.5462611627678,
81.9582469171631));
#122778=CARTESIAN_POINT('Ctrl Pts',(-12.3874564595957,74.0203970767149,
82.021810566711));
#122779=CARTESIAN_POINT('Ctrl Pts',(-12.3671300994806,74.7733760226478,
82.0636494785414));
#122780=CARTESIAN_POINT('Ctrl Pts',(-12.3597133925574,75.0509543705473,
82.0664880196756));
#122781=CARTESIAN_POINT('Ctrl Pts',(-12.3476615880533,75.5102965307628,
82.0502835522977));
#122782=CARTESIAN_POINT('Ctrl Pts',(-12.342950076167,75.6923285086733,82.038400729389));
#122783=CARTESIAN_POINT('Ctrl Pts',(-12.3306517123437,76.1731961781591,
81.9924120218353));
#122784=CARTESIAN_POINT('Ctrl Pts',(-12.3231452386327,76.4711123378138,
81.9488889682233));
#122785=CARTESIAN_POINT('Ctrl Pts',(-12.3106304952259,76.9502484100407,
81.8538526155916));
#122786=CARTESIAN_POINT('Ctrl Pts',(-12.305741722965,77.1331624934673,81.8114969195186));
#122787=CARTESIAN_POINT('Ctrl Pts',(-12.2925180068898,77.6181233127046,
81.6831070298117));
#122788=CARTESIAN_POINT('Ctrl Pts',(-12.284077113479,77.9175165446415,81.5868332732924));
#122789=CARTESIAN_POINT('Ctrl Pts',(-12.2660745886364,78.5407379361755,
81.3503819297233));
#122790=CARTESIAN_POINT('Ctrl Pts',(-12.2565020320278,78.8631153856673,
81.2062563850034));
#122791=CARTESIAN_POINT('Ctrl Pts',(-12.2405850593187,79.3905705659937,
80.9330114673131));
#122792=CARTESIAN_POINT('Ctrl Pts',(-12.2341725776039,79.6006501278721,
80.813440125623));
#122793=CARTESIAN_POINT('Ctrl Pts',(-12.2216027796096,80.0097752838398,
80.5585650532214));
#122794=CARTESIAN_POINT('Ctrl Pts',(-12.2154774447836,80.2088643721971,
80.4233312735564));
#122795=CARTESIAN_POINT('Ctrl Pts',(-12.2046453730353,80.5532762949083,
80.1686665260884));
#122796=CARTESIAN_POINT('Ctrl Pts',(-12.1999090131954,80.7008184544443,
80.0522638025176));
#122797=CARTESIAN_POINT('Ctrl Pts',(-12.1901006111542,80.9939699950065,
79.8055145925463));
#122798=CARTESIAN_POINT('Ctrl Pts',(-12.1850200616843,81.1391421901178,
79.6748897334218));
#122799=CARTESIAN_POINT('Ctrl Pts',(-12.1711816510871,81.5180700576123,
79.3109742306788));
#122800=CARTESIAN_POINT('Ctrl Pts',(-12.1623088331986,81.7436892761096,
79.0690816217196));
#122801=CARTESIAN_POINT('Ctrl Pts',(-12.1438682207081,82.1821064845516,
78.5448370469674));
#122802=CARTESIAN_POINT('Ctrl Pts',(-12.1342946016636,82.3929714160391,
78.2608055499923));
#122803=CARTESIAN_POINT('Ctrl Pts',(-12.1182745618553,82.7215936081313,
77.7602519075173));
#122804=CARTESIAN_POINT('Ctrl Pts',(-12.1117624548681,82.8481742610244,
77.5494630099774));
#122805=CARTESIAN_POINT('Ctrl Pts',(-12.0978616409741,83.1042913307437,
77.0810631266478));
#122806=CARTESIAN_POINT('Ctrl Pts',(-12.0905739617319,83.230546547132,76.8216673697312));
#122807=CARTESIAN_POINT('Ctrl Pts',(-12.0787437540253,83.4145321503588,
76.3922532317014));
#122808=CARTESIAN_POINT('Ctrl Pts',(-12.0741938022211,83.4800754356876,
76.2256666843821));
#122809=CARTESIAN_POINT('Ctrl Pts',(-12.0638001481673,83.6158637370845,
75.8472566058139));
#122810=CARTESIAN_POINT('Ctrl Pts',(-12.0579463729973,83.6832187490197,
75.6348454886013));
#122811=CARTESIAN_POINT('Ctrl Pts',(-12.0385091783984,83.8785318879706,
74.9295902101342));
#122812=CARTESIAN_POINT('Ctrl Pts',(-12.0246654647559,83.9730142509582,
74.427433964592));
#122813=CARTESIAN_POINT('Ctrl Pts',(-12.0026284815655,84.0572939236343,
73.6119406926));
#122814=CARTESIAN_POINT('Ctrl Pts',(-11.9943351321064,84.073543915764,73.3012121215505));
#122815=CARTESIAN_POINT('Ctrl Pts',(-11.9773935617203,84.0743111601728,
72.6535079496331));
#122816=CARTESIAN_POINT('Ctrl Pts',(-11.9688665158948,84.0560336237962,
72.3165311780078));
#122817=CARTESIAN_POINT('Ctrl Pts',(-11.9541824810339,83.9921630770108,
71.7415416566964));
#122818=CARTESIAN_POINT('Ctrl Pts',(-11.9480006684834,83.9558518769487,
71.5034271347825));
#122819=CARTESIAN_POINT('Ctrl Pts',(-11.925413164715,83.7913448027552,70.6559352350277));
#122820=CARTESIAN_POINT('Ctrl Pts',(-11.9085088968384,83.6093139072469,
70.0575986845659));
#122821=CARTESIAN_POINT('Ctrl Pts',(-11.8826053899707,83.2370411383783,
69.16872447229));
#122822=CARTESIAN_POINT('Ctrl Pts',(-11.8734787558732,83.0874641788945,
68.8609537687649));
#122823=CARTESIAN_POINT('Ctrl Pts',(-11.8566200690561,82.7736384453366,
68.2979888438898));
#122824=CARTESIAN_POINT('Ctrl Pts',(-11.8489105905299,82.6129745364498,
68.0407856392821));
#122825=CARTESIAN_POINT('Ctrl Pts',(-11.8361173800603,82.3247164839222,
67.6274886742986));
#122826=CARTESIAN_POINT('Ctrl Pts',(-11.8309988914646,82.2044001390743,
67.4668056975292));
#122827=CARTESIAN_POINT('Ctrl Pts',(-11.8186884328572,81.9073280157545,
67.0969139690612));
#122828=CARTESIAN_POINT('Ctrl Pts',(-11.8114726770941,81.7265066892708,
66.8917785636207));
#122829=CARTESIAN_POINT('Ctrl Pts',(-11.7909036071631,81.1907842154379,
66.3365812720506));
#122830=CARTESIAN_POINT('Ctrl Pts',(-11.7773919869305,80.8152025653093,
66.0063841928442));
#122831=CARTESIAN_POINT('Ctrl Pts',(-11.7577359137786,80.2259325654831,
65.5677402313798));
#122832=CARTESIAN_POINT('Ctrl Pts',(-11.7514533924048,80.0309507826131,
65.4339767474056));
#122833=CARTESIAN_POINT('Ctrl Pts',(-11.7391261110203,79.6336498983422,
65.1835295377725));
#122834=CARTESIAN_POINT('Ctrl Pts',(-11.7330919905038,79.4314422155539,
65.0666522017275));
#122835=CARTESIAN_POINT('Ctrl Pts',(-11.7218739022591,79.0422033436105,
64.8613980133367));
#122836=CARTESIAN_POINT('Ctrl Pts',(-11.7166481683376,78.8560991917015,
64.7712967384883));
#122837=CARTESIAN_POINT('Ctrl Pts',(-11.7051089646206,78.4448254719931,
64.5896135664457));
#122838=CARTESIAN_POINT('Ctrl Pts',(-11.6987660691994,78.2185704367478,
64.50056777215));
#122839=CARTESIAN_POINT('Ctrl Pts',(-11.6848137035157,77.7193217761979,
64.3269818650027));
#122840=CARTESIAN_POINT('Ctrl Pts',(-11.6771777832053,77.4451071848254,
64.2459806907456));
#122841=CARTESIAN_POINT('Ctrl Pts',(-11.652910886625,76.5668494001514,64.0306567087294));
#122842=CARTESIAN_POINT('Ctrl Pts',(-11.6361730259508,75.9508490052193,
63.9442499692642));
#122843=CARTESIAN_POINT('Ctrl Pts',(-11.6138730333825,75.09755207763,63.912029666633));
#122844=CARTESIAN_POINT('Ctrl Pts',(-11.6078376954894,74.8621502508335,
63.912269520108));
#122845=CARTESIAN_POINT('Ctrl Pts',(-11.5935401925601,74.3012374350425,
63.9348905061263));
#122846=CARTESIAN_POINT('Ctrl Pts',(-11.5852322787154,73.9777561566445,
63.9657478053854));
#122847=CARTESIAN_POINT('Ctrl Pts',(-11.564688317689,73.2028988620542,64.0825377978221));
#122848=CARTESIAN_POINT('Ctrl Pts',(-11.5524127609735,72.7554314771851,
64.1853200226825));
#122849=CARTESIAN_POINT('Ctrl Pts',(-11.5268898277826,71.8470843832727,
64.4668238657377));
#122850=CARTESIAN_POINT('Ctrl Pts',(-11.5136411107232,71.387687790774,64.6508499734686));
#122851=CARTESIAN_POINT('Ctrl Pts',(-11.4937288130588,70.707457635515,64.9896193704598));
#122852=CARTESIAN_POINT('Ctrl Pts',(-11.4868639886907,70.473924993594,65.1190168069731));
#122853=CARTESIAN_POINT('Ctrl Pts',(-11.4716617689557,69.9660535818595,
65.4307895649784));
#122854=CARTESIAN_POINT('Ctrl Pts',(-11.4632483507889,69.6964232405937,
65.6176345534709));
#122855=CARTESIAN_POINT('Ctrl Pts',(-11.4470220115368,69.208284502858,65.9971295944645));
#122856=CARTESIAN_POINT('Ctrl Pts',(-11.43931922007,68.9881340287137,66.1859898710082));
#122857=CARTESIAN_POINT('Ctrl Pts',(-11.4120216262576,68.2452570433496,
66.8872342308817));
#122858=CARTESIAN_POINT('Ctrl Pts',(-11.3922149334269,67.7732110023256,
67.4537567647632));
#122859=CARTESIAN_POINT('Ctrl Pts',(-11.3669456680991,67.2454304508019,
68.2695544984007));
#122860=CARTESIAN_POINT('Ctrl Pts',(-11.3608242996976,67.123178986526,68.4760297071188));
#122861=CARTESIAN_POINT('Ctrl Pts',(-11.3475630061663,66.8771307302081,
68.9325669324535));
#122862=CARTESIAN_POINT('Ctrl Pts',(-11.3403681640615,66.7568349349563,
69.1834264553651));
#122863=CARTESIAN_POINT('Ctrl Pts',(-11.3248199603447,66.5257007577464,
69.7287292610446));
#122864=CARTESIAN_POINT('Ctrl Pts',(-11.3164608927144,66.4181790243786,
70.0245316235007));
#122865=CARTESIAN_POINT('Ctrl Pts',(-11.2895635086448,66.1233415939836,
70.9874007142824));
#122866=CARTESIAN_POINT('Ctrl Pts',(-11.2708832047889,65.9956993337317,
71.6730255604155));
#122867=CARTESIAN_POINT('Ctrl Pts',(-11.2459423296123,65.9287622245236,
72.6274682344808));
#122868=CARTESIAN_POINT('Ctrl Pts',(-11.2391899128312,65.9217943497886,
72.8916999445158));
#122869=CARTESIAN_POINT('Ctrl Pts',(-11.2247967392948,65.9319287012176,
73.4531286084572));
#122870=CARTESIAN_POINT('Ctrl Pts',(-11.2170835341397,65.9522349747787,
73.7494401143278));
#122871=CARTESIAN_POINT('Ctrl Pts',(-11.1997593434101,66.0294539077494,
74.4032547996756));
#122872=CARTESIAN_POINT('Ctrl Pts',(-11.1901116721686,66.0935069748745,
74.7601509818632));
#122873=CARTESIAN_POINT('Ctrl Pts',(-11.1636740994005,66.3256054618999,
75.7221353348087));
#122874=CARTESIAN_POINT('Ctrl Pts',(-11.1468391668825,66.5355387126056,
76.3173479064166));
#122875=CARTESIAN_POINT('Ctrl Pts',(-11.1230855295391,66.9259140697659,
77.1409425112817));
#122876=CARTESIAN_POINT('Ctrl Pts',(-11.1158407152713,67.0594948847545,
77.3916337481368));
#122877=CARTESIAN_POINT('Ctrl Pts',(-11.0991516044814,67.3913951984904,
77.948534407531));
#122878=CARTESIAN_POINT('Ctrl Pts',(-11.0896004548305,67.5971897626805,
78.2499532894295));
#122879=CARTESIAN_POINT('Ctrl Pts',(-11.066606918913,68.1292644930105,78.936850578795));
#122880=CARTESIAN_POINT('Ctrl Pts',(-11.053077156272,68.4716321676164,79.3101735682659));
#122881=CARTESIAN_POINT('Ctrl Pts',(-11.0284125191687,69.1515329753655,
79.9388802838722));
#122882=CARTESIAN_POINT('Ctrl Pts',(-11.0172503581122,69.4806030071237,
80.2036409696054));
#122883=CARTESIAN_POINT('Ctrl Pts',(-10.9985390390634,70.0712279150404,
80.614415278307));
#122884=CARTESIAN_POINT('Ctrl Pts',(-10.9909334047949,70.3245754877019,
80.7726454831127));
#122885=CARTESIAN_POINT('Ctrl Pts',(-10.9697548269484,71.0388286659262,
81.1699412959377));
#122886=CARTESIAN_POINT('Ctrl Pts',(-10.9560294121159,71.5135704359081,
81.3823050592927));
#122887=CARTESIAN_POINT('Ctrl Pts',(-10.9223429476978,72.708313125711,81.7995014839169));
#122888=CARTESIAN_POINT('Ctrl Pts',(-10.9023122329795,73.4443011087522,
81.9596064222288));
#122889=CARTESIAN_POINT('Ctrl Pts',(-10.8751584514562,74.4848368720807,
82.0540579166407));
#122890=CARTESIAN_POINT('Ctrl Pts',(-10.8675576584132,74.7822601659039,
82.0662707454521));
#122891=CARTESIAN_POINT('Ctrl Pts',(-10.8434722464501,75.7084594847752,
82.0575451759476));
#122892=CARTESIAN_POINT('Ctrl Pts',(-10.8267691213327,76.3355363323114,
81.9854855858357));
#122893=CARTESIAN_POINT('Ctrl Pts',(-10.7944474624907,77.5216341862379,
81.7244250653333));
#122894=CARTESIAN_POINT('Ctrl Pts',(-10.7788310631899,78.0826746872989,
81.5433290772843));
#122895=CARTESIAN_POINT('Ctrl Pts',(-10.7546809646044,78.9322314538102,
81.1746669638441));
#122896=CARTESIAN_POINT('Ctrl Pts',(-10.7459964850638,79.2354841414371,
81.0222032664891));
#122897=CARTESIAN_POINT('Ctrl Pts',(-10.7256878866019,79.9103259574314,
80.6328063119621));
#122898=CARTESIAN_POINT('Ctrl Pts',(-10.7140980827418,80.2741212462702,
80.3856733475756));
#122899=CARTESIAN_POINT('Ctrl Pts',(-10.6871684528069,81.0706736659949,
79.7565830065856));
#122900=CARTESIAN_POINT('Ctrl Pts',(-10.6717915993553,81.4893718767674,
79.3565348007192));
#122901=CARTESIAN_POINT('Ctrl Pts',(-10.640519778576,82.2659768611267,78.4594683542636));
#122902=CARTESIAN_POINT('Ctrl Pts',(-10.6249072747157,82.6176903657794,
77.9595190933445));
#122903=CARTESIAN_POINT('Ctrl Pts',(-10.5939779030133,83.1934066138114,
76.9294721098776));
#122904=CARTESIAN_POINT('Ctrl Pts',(-10.5789318808566,83.4231942328531,
76.4088603817057));
#122905=CARTESIAN_POINT('Ctrl Pts',(-10.5481810648341,83.7914428882741,
75.3100152504172));
#122906=CARTESIAN_POINT('Ctrl Pts',(-10.5324760203067,83.9253402123738,
74.7299845962427));
#122907=CARTESIAN_POINT('Ctrl Pts',(-10.506040976142,84.0550494842427,73.7246815616173));
#122908=CARTESIAN_POINT('Ctrl Pts',(-10.4952140429273,84.0791260026975,
73.3057698135278));
#122909=CARTESIAN_POINT('Ctrl Pts',(-10.4652701513313,84.0649528968915,
72.1657159863188));
#122910=CARTESIAN_POINT('Ctrl Pts',(-10.4461089964124,83.9699778210984,
71.4466320716153));
#122911=CARTESIAN_POINT('Ctrl Pts',(-10.3954812582148,83.4987543731218,
69.5913065933387));
#122912=CARTESIAN_POINT('Ctrl Pts',(-10.3651611426005,82.9832088330785,
68.5139509363784));
#122913=CARTESIAN_POINT('Ctrl Pts',(-10.3180635153095,81.9168420926899,
67.0873853839914));
#122914=CARTESIAN_POINT('Ctrl Pts',(-10.3024236418362,81.5179256481026,
66.6488212164598));
#122915=CARTESIAN_POINT('Ctrl Pts',(-10.26313876224,80.410269540294,65.6467307993475));
#122916=CARTESIAN_POINT('Ctrl Pts',(-10.2399332767544,79.6574681785045,
65.1498522254083));
#122917=CARTESIAN_POINT('Ctrl Pts',(-10.2006644622652,78.3096069450724,
64.5202404529412));
#122918=CARTESIAN_POINT('Ctrl Pts',(-10.1850172306535,77.749637921637,64.321816495378));
#122919=CARTESIAN_POINT('Ctrl Pts',(-10.1540168337345,76.6070822003054,
64.0382750241231));
#122920=CARTESIAN_POINT('Ctrl Pts',(-10.1388244678694,76.0279702794316,
63.9529979491404));
#122921=CARTESIAN_POINT('Ctrl Pts',(-10.0928504785718,74.2792924799251,
63.869769992767));
#122922=CARTESIAN_POINT('Ctrl Pts',(-10.0620175451159,73.1064692951876,
64.0387582366355));
#122923=CARTESIAN_POINT('Ctrl Pts',(-10.0163541915642,71.4644504576041,
64.610815205128));
#122924=CARTESIAN_POINT('Ctrl Pts',(-10.0013527294429,70.9424093499569,
64.8520339579409));
#122925=CARTESIAN_POINT('Ctrl Pts',(-9.96434722807135,69.7262383344997,
65.5590017814957));
#122926=CARTESIAN_POINT('Ctrl Pts',(-9.94233034594927,69.0618814918381,
66.0776427426821));
#122927=CARTESIAN_POINT('Ctrl Pts',(-9.89823651844638,67.8956325647864,
67.2795378045371));
#122928=CARTESIAN_POINT('Ctrl Pts',(-9.87641089052029,67.4023950609479,
67.9580324679594));
#122929=CARTESIAN_POINT('Ctrl Pts',(-9.85451302005563,67.0084395094767,
68.6917839432004));
#122930=CARTESIAN_POINT('Ctrl Pts',(-13.6367975371279,82.22637258748,78.478439844214));
#122931=CARTESIAN_POINT('Ctrl Pts',(-13.5965727996549,83.15132333764,77.260846746689));
#122932=CARTESIAN_POINT('Ctrl Pts',(-13.5161233247074,84.37134578258,74.349656820311));
#122933=CARTESIAN_POINT('Ctrl Pts',(-13.3954491122865,83.85839097116,69.641309155131));
#122934=CARTESIAN_POINT('Ctrl Pts',(-13.2747748998656,81.12957508313,65.770566029046));
#122935=CARTESIAN_POINT('Ctrl Pts',(-13.1541006874447,76.867728622,63.705144460549));
#122936=CARTESIAN_POINT('Ctrl Pts',(-13.0334264750238,72.13871802361,63.961747337343));
#122937=CARTESIAN_POINT('Ctrl Pts',(-12.9127522626029,68.12536086466,66.476164874831));
#122938=CARTESIAN_POINT('Ctrl Pts',(-12.7920780501819,65.83145073401,70.619512225841));
#122939=CARTESIAN_POINT('Ctrl Pts',(-12.6714038377609,65.83072989138,75.355475184308));
#122940=CARTESIAN_POINT('Ctrl Pts',(-12.5507296253399,68.12337819702,79.499520367104));
#122941=CARTESIAN_POINT('Ctrl Pts',(-12.4300554129189,72.13597072448,82.015161004986));
#122942=CARTESIAN_POINT('Ctrl Pts',(-12.3093812004979,76.86489906758,82.273198436157));
#122943=CARTESIAN_POINT('Ctrl Pts',(-12.1887069880768,81.12738874216,80.209093695038));
#122944=CARTESIAN_POINT('Ctrl Pts',(-12.0680327756558,83.857328421,76.339109722068));
#122945=CARTESIAN_POINT('Ctrl Pts',(-11.9473585632348,84.37192006169,71.631186395751));
#122946=CARTESIAN_POINT('Ctrl Pts',(-11.8266843508137,82.5424567304,67.262844545329));
#122947=CARTESIAN_POINT('Ctrl Pts',(-11.7060101383927,78.82651409889,64.326670680902));
#122948=CARTESIAN_POINT('Ctrl Pts',(-11.5853359259716,74.15350404259,63.557045046897));
#122949=CARTESIAN_POINT('Ctrl Pts',(-11.4646617135509,69.69221506849,65.146462327629));
#122950=CARTESIAN_POINT('Ctrl Pts',(-11.3439875011299,66.55848112866,68.697385897282));
#122951=CARTESIAN_POINT('Ctrl Pts',(-11.2233132887089,65.53609514649,73.3216775732696));
#122952=CARTESIAN_POINT('Ctrl Pts',(-11.1026390762869,66.88077088472,77.862734032643));
#122953=CARTESIAN_POINT('Ctrl Pts',(-10.9819648638659,70.25618517554,81.184770299059));
#122954=CARTESIAN_POINT('Ctrl Pts',(-10.8612906514449,74.81809728471,82.456896282854));
#122955=CARTESIAN_POINT('Ctrl Pts',(-10.7406164390239,79.42550594423,81.360934525046));
#122956=CARTESIAN_POINT('Ctrl Pts',(-10.6199422266029,82.92603048601,78.171001360235));
#122957=CARTESIAN_POINT('Ctrl Pts',(-10.4992680141819,84.44413839523,73.6849452599872));
#122958=CARTESIAN_POINT('Ctrl Pts',(-10.3785938017609,83.60012808368,69.02479742627));
#122959=CARTESIAN_POINT('Ctrl Pts',(-10.2579195893399,80.60510074462,65.356119528941));
#122960=CARTESIAN_POINT('Ctrl Pts',(-10.1372453769189,76.20814999546,63.596538435828));
#122961=CARTESIAN_POINT('Ctrl Pts',(-10.0165711644989,71.50904302936,64.186014661069));
#122962=CARTESIAN_POINT('Ctrl Pts',(-9.89589695207791,67.68300161261,66.977621268753));
#122963=CARTESIAN_POINT('Ctrl Pts',(-9.81544747712991,66.35255094703,69.840029796558));
#122964=CARTESIAN_POINT('Ctrl Pts',(-9.77522273965691,66.0753597154,71.343769089941));
#122965=CARTESIAN_POINT('Ctrl Pts',(-13.7234642037949,82.22637258748,78.478439844214));
#122966=CARTESIAN_POINT('Ctrl Pts',(-13.6832394663209,83.15132333764,77.260846746689));
#122967=CARTESIAN_POINT('Ctrl Pts',(-13.6027899913739,84.37134578258,74.349656820311));
#122968=CARTESIAN_POINT('Ctrl Pts',(-13.4821157789532,83.85839097116,69.641309155131));
#122969=CARTESIAN_POINT('Ctrl Pts',(-13.3614415665323,81.12957508313,65.770566029046));
#122970=CARTESIAN_POINT('Ctrl Pts',(-13.2407673541114,76.867728622,63.705144460549));
#122971=CARTESIAN_POINT('Ctrl Pts',(-13.1200931416905,72.13871802361,63.961747337343));
#122972=CARTESIAN_POINT('Ctrl Pts',(-12.9994189292695,68.12536086466,66.476164874831));
#122973=CARTESIAN_POINT('Ctrl Pts',(-12.8787447168486,65.83145073401,70.619512225841));
#122974=CARTESIAN_POINT('Ctrl Pts',(-12.7580705044276,65.83072989138,75.355475184308));
#122975=CARTESIAN_POINT('Ctrl Pts',(-12.6373962920066,68.12337819702,79.499520367104));
#122976=CARTESIAN_POINT('Ctrl Pts',(-12.5167220795856,72.13597072448,82.015161004986));
#122977=CARTESIAN_POINT('Ctrl Pts',(-12.3960478671645,76.86489906758,82.273198436157));
#122978=CARTESIAN_POINT('Ctrl Pts',(-12.2753736547435,81.12738874216,80.209093695038));
#122979=CARTESIAN_POINT('Ctrl Pts',(-12.1546994423225,83.857328421,76.339109722068));
#122980=CARTESIAN_POINT('Ctrl Pts',(-12.0340252299014,84.37192006169,71.631186395751));
#122981=CARTESIAN_POINT('Ctrl Pts',(-11.9133510174804,82.5424567304,67.262844545329));
#122982=CARTESIAN_POINT('Ctrl Pts',(-11.7926768050593,78.82651409889,64.326670680902));
#122983=CARTESIAN_POINT('Ctrl Pts',(-11.6720025926383,74.15350404259,63.557045046897));
#122984=CARTESIAN_POINT('Ctrl Pts',(-11.5513283802169,69.69221506849,65.146462327629));
#122985=CARTESIAN_POINT('Ctrl Pts',(-11.4306541677959,66.55848112866,68.697385897282));
#122986=CARTESIAN_POINT('Ctrl Pts',(-11.3099799553749,65.53609514649,73.3216775732696));
#122987=CARTESIAN_POINT('Ctrl Pts',(-11.1893057429539,66.88077088472,77.862734032643));
#122988=CARTESIAN_POINT('Ctrl Pts',(-11.0686315305329,70.25618517554,81.184770299059));
#122989=CARTESIAN_POINT('Ctrl Pts',(-10.9479573181119,74.81809728471,82.456896282854));
#122990=CARTESIAN_POINT('Ctrl Pts',(-10.8272831056909,79.42550594423,81.360934525046));
#122991=CARTESIAN_POINT('Ctrl Pts',(-10.7066088932699,82.92603048601,78.171001360235));
#122992=CARTESIAN_POINT('Ctrl Pts',(-10.5859346808489,84.44413839523,73.6849452599872));
#122993=CARTESIAN_POINT('Ctrl Pts',(-10.4652604684279,83.60012808368,69.02479742627));
#122994=CARTESIAN_POINT('Ctrl Pts',(-10.3445862560069,80.60510074462,65.356119528941));
#122995=CARTESIAN_POINT('Ctrl Pts',(-10.2239120435859,76.20814999546,63.596538435828));
#122996=CARTESIAN_POINT('Ctrl Pts',(-10.1032378311649,71.50904302936,64.186014661069));
#122997=CARTESIAN_POINT('Ctrl Pts',(-9.98256361874391,67.68300161261,66.977621268753));
#122998=CARTESIAN_POINT('Ctrl Pts',(-9.90211414379691,66.35255094703,69.840029796558));
#122999=CARTESIAN_POINT('Ctrl Pts',(-9.86188940632291,66.0753597154,71.343769089941));
#123000=CARTESIAN_POINT('Ctrl Pts',(-13.8101308704619,82.22637258748,78.478439844214));
#123001=CARTESIAN_POINT('Ctrl Pts',(-13.7699061329879,83.15132333764,77.260846746689));
#123002=CARTESIAN_POINT('Ctrl Pts',(-13.6894566580409,84.37134578258,74.349656820311));
#123003=CARTESIAN_POINT('Ctrl Pts',(-13.5687824456199,83.85839097116,69.641309155131));
#123004=CARTESIAN_POINT('Ctrl Pts',(-13.448108233199,81.12957508313,65.770566029046));
#123005=CARTESIAN_POINT('Ctrl Pts',(-13.3274340207781,76.867728622,63.705144460549));
#123006=CARTESIAN_POINT('Ctrl Pts',(-13.2067598083571,72.13871802361,63.961747337343));
#123007=CARTESIAN_POINT('Ctrl Pts',(-13.0860855959362,68.12536086466,66.476164874831));
#123008=CARTESIAN_POINT('Ctrl Pts',(-12.9654113835152,65.83145073401,70.619512225841));
#123009=CARTESIAN_POINT('Ctrl Pts',(-12.8447371710942,65.83072989138,75.355475184308));
#123010=CARTESIAN_POINT('Ctrl Pts',(-12.7240629586732,68.12337819702,79.499520367104));
#123011=CARTESIAN_POINT('Ctrl Pts',(-12.6033887462522,72.13597072448,82.015161004986));
#123012=CARTESIAN_POINT('Ctrl Pts',(-12.4827145338312,76.86489906758,82.273198436157));
#123013=CARTESIAN_POINT('Ctrl Pts',(-12.3620403214102,81.12738874216,80.209093695038));
#123014=CARTESIAN_POINT('Ctrl Pts',(-12.2413661089891,83.857328421,76.339109722068));
#123015=CARTESIAN_POINT('Ctrl Pts',(-12.1206918965681,84.37192006169,71.631186395751));
#123016=CARTESIAN_POINT('Ctrl Pts',(-12.000017684147,82.5424567304,67.262844545329));
#123017=CARTESIAN_POINT('Ctrl Pts',(-11.879343471726,78.82651409889,64.326670680902));
#123018=CARTESIAN_POINT('Ctrl Pts',(-11.7586692593049,74.15350404259,63.557045046897));
#123019=CARTESIAN_POINT('Ctrl Pts',(-11.6379950468839,69.69221506849,65.146462327629));
#123020=CARTESIAN_POINT('Ctrl Pts',(-11.5173208344629,66.55848112866,68.697385897282));
#123021=CARTESIAN_POINT('Ctrl Pts',(-11.3966466220419,65.53609514649,73.3216775732696));
#123022=CARTESIAN_POINT('Ctrl Pts',(-11.2759724096209,66.88077088472,77.862734032643));
#123023=CARTESIAN_POINT('Ctrl Pts',(-11.1552981971999,70.25618517554,81.184770299059));
#123024=CARTESIAN_POINT('Ctrl Pts',(-11.0346239847789,74.81809728471,82.456896282854));
#123025=CARTESIAN_POINT('Ctrl Pts',(-10.9139497723579,79.42550594423,81.360934525046));
#123026=CARTESIAN_POINT('Ctrl Pts',(-10.7932755599369,82.92603048601,78.171001360235));
#123027=CARTESIAN_POINT('Ctrl Pts',(-10.6726013475159,84.44413839523,73.6849452599872));
#123028=CARTESIAN_POINT('Ctrl Pts',(-10.5519271350949,83.60012808368,69.02479742627));
#123029=CARTESIAN_POINT('Ctrl Pts',(-10.4312529226739,80.60510074462,65.356119528941));
#123030=CARTESIAN_POINT('Ctrl Pts',(-10.3105787102529,76.20814999546,63.596538435828));
#123031=CARTESIAN_POINT('Ctrl Pts',(-10.1899044978319,71.50904302936,64.186014661069));
#123032=CARTESIAN_POINT('Ctrl Pts',(-10.0692302854109,67.68300161261,66.977621268753));
#123033=CARTESIAN_POINT('Ctrl Pts',(-9.98878081046391,66.35255094703,69.840029796558));
#123034=CARTESIAN_POINT('Ctrl Pts',(-9.94855607298991,66.0753597154,71.343769089941));
#123035=CARTESIAN_POINT('Ctrl Pts',(-13.8967975371279,82.22637258748,78.478439844214));
#123036=CARTESIAN_POINT('Ctrl Pts',(-13.8565727996549,83.15132333764,77.260846746689));
#123037=CARTESIAN_POINT('Ctrl Pts',(-13.7761233247069,84.37134578258,74.349656820311));
#123038=CARTESIAN_POINT('Ctrl Pts',(-13.6554491122869,83.85839097116,69.641309155131));
#123039=CARTESIAN_POINT('Ctrl Pts',(-13.5347748998656,81.12957508313,65.770566029046));
#123040=CARTESIAN_POINT('Ctrl Pts',(-13.4141006874447,76.867728622,63.705144460549));
#123041=CARTESIAN_POINT('Ctrl Pts',(-13.2934264750238,72.13871802361,63.961747337343));
#123042=CARTESIAN_POINT('Ctrl Pts',(-13.1727522626029,68.12536086466,66.476164874831));
#123043=CARTESIAN_POINT('Ctrl Pts',(-13.0520780501819,65.83145073401,70.619512225841));
#123044=CARTESIAN_POINT('Ctrl Pts',(-12.9314038377609,65.83072989138,75.355475184308));
#123045=CARTESIAN_POINT('Ctrl Pts',(-12.8107296253399,68.12337819702,79.499520367104));
#123046=CARTESIAN_POINT('Ctrl Pts',(-12.6900554129189,72.13597072448,82.015161004986));
#123047=CARTESIAN_POINT('Ctrl Pts',(-12.5693812004979,76.86489906758,82.273198436157));
#123048=CARTESIAN_POINT('Ctrl Pts',(-12.4487069880768,81.12738874216,80.209093695038));
#123049=CARTESIAN_POINT('Ctrl Pts',(-12.3280327756558,83.857328421,76.339109722068));
#123050=CARTESIAN_POINT('Ctrl Pts',(-12.2073585632348,84.37192006169,71.631186395751));
#123051=CARTESIAN_POINT('Ctrl Pts',(-12.0866843508137,82.5424567304,67.262844545329));
#123052=CARTESIAN_POINT('Ctrl Pts',(-11.9660101383927,78.82651409889,64.326670680902));
#123053=CARTESIAN_POINT('Ctrl Pts',(-11.8453359259716,74.15350404259,63.557045046897));
#123054=CARTESIAN_POINT('Ctrl Pts',(-11.7246617135505,69.69221506849,65.146462327629));
#123055=CARTESIAN_POINT('Ctrl Pts',(-11.6039875011295,66.55848112866,68.697385897282));
#123056=CARTESIAN_POINT('Ctrl Pts',(-11.4833132887089,65.53609514649,73.3216775732696));
#123057=CARTESIAN_POINT('Ctrl Pts',(-11.3626390762869,66.88077088472,77.862734032643));
#123058=CARTESIAN_POINT('Ctrl Pts',(-11.2419648638659,70.25618517554,81.184770299059));
#123059=CARTESIAN_POINT('Ctrl Pts',(-11.1212906514449,74.81809728471,82.456896282854));
#123060=CARTESIAN_POINT('Ctrl Pts',(-11.0006164390239,79.42550594423,81.360934525046));
#123061=CARTESIAN_POINT('Ctrl Pts',(-10.8799422266029,82.92603048601,78.171001360235));
#123062=CARTESIAN_POINT('Ctrl Pts',(-10.7592680141819,84.44413839523,73.6849452599872));
#123063=CARTESIAN_POINT('Ctrl Pts',(-10.6385938017609,83.60012808368,69.02479742627));
#123064=CARTESIAN_POINT('Ctrl Pts',(-10.5179195893399,80.60510074462,65.356119528941));
#123065=CARTESIAN_POINT('Ctrl Pts',(-10.3972453769189,76.20814999546,63.596538435828));
#123066=CARTESIAN_POINT('Ctrl Pts',(-10.2765711644989,71.50904302936,64.186014661069));
#123067=CARTESIAN_POINT('Ctrl Pts',(-10.1558969520779,67.68300161261,66.977621268753));
#123068=CARTESIAN_POINT('Ctrl Pts',(-10.0754474771299,66.35255094703,69.840029796558));
#123069=CARTESIAN_POINT('Ctrl Pts',(-10.0352227396569,66.0753597154,71.343769089941));
#123070=CARTESIAN_POINT('',(-13.5633022950147,81.8869258507955,67.0921386900969));
#123071=CARTESIAN_POINT('Ctrl Pts',(-13.5675364833309,81.8924678804059,
67.0873924564601));
#123072=CARTESIAN_POINT('Ctrl Pts',(-13.5675364833309,81.9977690181948,
67.2106037724578));
#123073=CARTESIAN_POINT('Ctrl Pts',(-13.5675364833309,82.0992425609522,
67.3359700547413));
#123074=CARTESIAN_POINT('Ctrl Pts',(-13.5675364833309,82.1969937123613,
67.4634099181992));
#123075=CARTESIAN_POINT('Ctrl Pts',(-13.5675364833309,82.2957238032808,
67.592126041995));
#123076=CARTESIAN_POINT('Ctrl Pts',(-13.5675364833309,82.3906568522104,
67.7229578489377));
#123077=CARTESIAN_POINT('Ctrl Pts',(-13.5675364833309,82.4818665253462,
67.8558621259143));
#123078=CARTESIAN_POINT('Ctrl Pts',(-13.5675364833309,82.5735780703432,
67.9894976950288));
#123079=CARTESIAN_POINT('Ctrl Pts',(-13.5675364833309,82.6615254275363,
68.1252289856858));
#123080=CARTESIAN_POINT('Ctrl Pts',(-13.5675364833309,82.7457443938265,
68.2630472884685));
#123081=CARTESIAN_POINT('Ctrl Pts',(-13.5675364833309,82.8298710462911,
68.4007145262914));
#123082=CARTESIAN_POINT('Ctrl Pts',(-13.5675364833309,82.9102777265511,
68.5404646023485));
#123083=CARTESIAN_POINT('Ctrl Pts',(-13.5675364833309,82.9869573381782,
68.6823179698962));
#123084=CARTESIAN_POINT('Ctrl Pts',(-13.5675364833309,83.0632243468457,
68.823408043029));
#123085=CARTESIAN_POINT('Ctrl Pts',(-13.5675364833309,83.135804521286,68.9665792259746));
#123086=CARTESIAN_POINT('Ctrl Pts',(-13.5675364833309,83.2046449902606,
69.111874551974));
#123087=CARTESIAN_POINT('Ctrl Pts',(-13.5675364833309,83.2725207161971,
69.2551336824574));
#123088=CARTESIAN_POINT('Ctrl Pts',(-13.5675364833309,83.336760991513,69.400458221822));
#123089=CARTESIAN_POINT('Ctrl Pts',(-13.5675364833309,83.3972675206113,
69.5479059599801));
#123090=CARTESIAN_POINT('Ctrl Pts',(-13.5675364833309,83.4288997535913,
69.6249902230389));
#123091=CARTESIAN_POINT('Ctrl Pts',(-13.5675364833309,83.4595107091917,
69.7026550175545));
#123092=CARTESIAN_POINT('Ctrl Pts',(-13.5675364833309,83.4890807917262,
69.7809099116504));
#123093=CARTESIAN_POINT('Ctrl Pts',(-13.5675364833309,83.5462497067958,
69.9322029420008));
#123094=CARTESIAN_POINT('Ctrl Pts',(-13.5675364833309,83.5995311272314,
70.0857015184292));
#123095=CARTESIAN_POINT('Ctrl Pts',(-13.5675364833309,83.6488530159178,
70.2414380131213));
#123096=CARTESIAN_POINT('Ctrl Pts',(-13.5675364833309,83.6976829222368,
70.3956210472426));
#123097=CARTESIAN_POINT('Ctrl Pts',(-13.5675364833309,83.742631951158,70.5519980279251));
#123098=CARTESIAN_POINT('Ctrl Pts',(-13.5675364833309,83.7835790887525,
70.7106003983674));
#123099=CARTESIAN_POINT('Ctrl Pts',(-13.5675364833309,83.8216452441033,
70.8580437320634));
#123100=CARTESIAN_POINT('Ctrl Pts',(-13.5675364833309,83.8562524416585,
71.0074106221777));
#123101=CARTESIAN_POINT('Ctrl Pts',(-13.5675364833309,83.8872622912965,
71.1587211275468));
#123102=CARTESIAN_POINT('Ctrl Pts',(-13.5675364833309,83.8940456959048,
71.1918203005962));
#123103=CARTESIAN_POINT('Ctrl Pts',(-13.5675364833309,83.9006568071547,
71.2250124483185));
#123104=CARTESIAN_POINT('Ctrl Pts',(-13.5675364833309,83.907093914309,71.2582977234034));
#123105=CARTESIAN_POINT('Ctrl Pts',(-13.5675364833309,83.910075144381,71.2737131981902));
#123106=CARTESIAN_POINT('Ctrl Pts',(-13.5675364833309,83.9130190507611,
71.289148647634));
#123107=CARTESIAN_POINT('Ctrl Pts',(-13.5675364833309,83.9159254565328,
71.3046040850435));
#123108=CARTESIAN_POINT('Ctrl Pts',(-13.5675364833309,83.9182590717436,
71.317013585527));
#123109=CARTESIAN_POINT('Ctrl Pts',(-13.5675364833309,83.9205689816703,
71.3294386553613));
#123110=CARTESIAN_POINT('Ctrl Pts',(-13.5675364833309,83.9228508036666,
71.3418555967155));
#123111=CARTESIAN_POINT('Ctrl Pts',(-13.5675364833309,83.9522228601566,
71.5016888805896));
#123112=CARTESIAN_POINT('Ctrl Pts',(-13.5675364833309,83.977099558419,71.6609852694542));
#123113=CARTESIAN_POINT('Ctrl Pts',(-13.5675364833309,83.9976830999355,
71.8196936146382));
#123114=CARTESIAN_POINT('Ctrl Pts',(-13.5675364833309,84.0186174256015,
71.9811066630849));
#123115=CARTESIAN_POINT('Ctrl Pts',(-13.5675364833309,84.0351110922124,
72.141911865271));
#123116=CARTESIAN_POINT('Ctrl Pts',(-13.5675364833309,84.0473295499119,
72.3020822045462));
#123117=CARTESIAN_POINT('Ctrl Pts',(-13.5675364833309,84.0601988915448,
72.4707849055154));
#123118=CARTESIAN_POINT('Ctrl Pts',(-13.5675364833309,84.0683258291414,
72.6387836571667));
#123119=CARTESIAN_POINT('Ctrl Pts',(-13.5675364833309,84.071847456582,72.8060705862103));
#123120=CARTESIAN_POINT('Ctrl Pts',(-13.5675364833309,84.0752820285138,
72.9692221406381));
#123121=CARTESIAN_POINT('Ctrl Pts',(-13.5675364833309,84.0743359159924,
73.1316972062282));
#123122=CARTESIAN_POINT('Ctrl Pts',(-13.5675364833309,84.0690840216172,
73.2935029730835));
#123123=CARTESIAN_POINT('Ctrl Pts',(-13.5675364833309,84.0636324489359,
73.4614606346904));
#123124=CARTESIAN_POINT('Ctrl Pts',(-13.5675364833309,84.0535418104486,
73.6286976277291));
#123125=CARTESIAN_POINT('Ctrl Pts',(-13.5675364833309,84.0388373131803,
73.7952298789199));
#123126=CARTESIAN_POINT('Ctrl Pts',(-13.5675364833309,84.0241328159119,
73.9617621301106));
#123127=CARTESIAN_POINT('Ctrl Pts',(-13.5675364833309,84.0048144863583,
74.1275901954544));
#123128=CARTESIAN_POINT('Ctrl Pts',(-13.5675364833309,83.9808477027752,
74.2927296910418));
#123129=CARTESIAN_POINT('Ctrl Pts',(-13.5675364833309,83.9577030737421,
74.4522042551125));
#123130=CARTESIAN_POINT('Ctrl Pts',(-13.5675364833309,83.9302230679344,
74.611037108983));
#123131=CARTESIAN_POINT('Ctrl Pts',(-13.5675364833309,83.8984368670594,
74.769252947345));
#123132=CARTESIAN_POINT('Ctrl Pts',(-13.5675364833309,83.8666355215599,
74.9275441680868));
#123133=CARTESIAN_POINT('Ctrl Pts',(-13.5675364833309,83.8305237251017,
75.0852182238534));
#123134=CARTESIAN_POINT('Ctrl Pts',(-13.5675364833309,83.7900804621859,
75.2422858250677));
#123135=CARTESIAN_POINT('Ctrl Pts',(-13.5675364833309,83.7498958119861,
75.3983490642201));
#123136=CARTESIAN_POINT('Ctrl Pts',(-13.5675364833309,83.7054347308817,
75.5538140031912));
#123137=CARTESIAN_POINT('Ctrl Pts',(-13.5675364833309,83.6566295892481,
75.7086709106651));
#123138=CARTESIAN_POINT('Ctrl Pts',(-13.5675364833309,83.6256590203533,
75.8069393791343));
#123139=CARTESIAN_POINT('Ctrl Pts',(-13.5675364833309,83.5929382246295,
75.9049625778693));
#123140=CARTESIAN_POINT('Ctrl Pts',(-13.5675364833309,83.558440477199,76.0027325471775));
#123141=CARTESIAN_POINT('Ctrl Pts',(-13.5590681066986,81.8921747150299,
67.0870494451112));
#123142=CARTESIAN_POINT('Ctrl Pts',(-13.5542716148093,81.7920287222896,
66.9698818089279));
#123143=CARTESIAN_POINT('Ctrl Pts',(-13.5495044344257,81.6889149671049,
66.8552469756093));
#123144=CARTESIAN_POINT('Ctrl Pts',(-13.5372447085138,81.4124470616348,
66.563205798704));
#123145=CARTESIAN_POINT('Ctrl Pts',(-13.529861101716,81.2345601511849,66.3900885153774));
#123146=CARTESIAN_POINT('Ctrl Pts',(-13.5199226290234,80.9740045601888,
66.156827913568));
#123147=CARTESIAN_POINT('Ctrl Pts',(-13.5170895307345,80.8970775777746,
66.0902902151318));
#123148=CARTESIAN_POINT('Ctrl Pts',(-13.5125120131832,80.7680020470132,
65.9824745318577));
#123149=CARTESIAN_POINT('Ctrl Pts',(-13.5107324021522,80.7165917930754,
65.9404996883744));
#123150=CARTESIAN_POINT('Ctrl Pts',(-13.5071900740137,80.6118804334446,
65.8569317744254));
#123151=CARTESIAN_POINT('Ctrl Pts',(-13.5054283118564,80.5585625821676,
65.8153609276827));
#123152=CARTESIAN_POINT('Ctrl Pts',(-13.5010903681271,80.4243331006755,
65.7131198731638));
#123153=CARTESIAN_POINT('Ctrl Pts',(-13.4985435658636,80.3428494857749,
65.6532011411002));
#123154=CARTESIAN_POINT('Ctrl Pts',(-13.4885613616639,80.0136753562677,
65.4195494435737));
#123155=CARTESIAN_POINT('Ctrl Pts',(-13.481492094847,79.7581702326144,65.2568101746283));
#123156=CARTESIAN_POINT('Ctrl Pts',(-13.4588390414386,78.8891870017602,
64.7620196695988));
#123157=CARTESIAN_POINT('Ctrl Pts',(-13.4441362070671,78.2434647223616,
64.4860491263886));
#123158=CARTESIAN_POINT('Ctrl Pts',(-13.4198273992042,77.217813969253,64.1813375254656));
#123159=CARTESIAN_POINT('Ctrl Pts',(-13.4109965907119,76.8543859453273,
64.0973701782848));
#123160=CARTESIAN_POINT('Ctrl Pts',(-13.3959694872772,76.2561904286052,
63.9984996318914));
#123161=CARTESIAN_POINT('Ctrl Pts',(-13.3900843911558,76.0255742570212,
63.9695480407988));
#123162=CARTESIAN_POINT('Ctrl Pts',(-13.3774389878636,75.5360882992717,
63.9270862755009));
#123163=CARTESIAN_POINT('Ctrl Pts',(-13.3706562147548,75.2770273815881,
63.9157442749326));
#123164=CARTESIAN_POINT('Ctrl Pts',(-13.347732045806,74.4106296861599,63.9145582499049));
#123165=CARTESIAN_POINT('Ctrl Pts',(-13.3312825573389,73.8030388329621,
63.9741128273904));
#123166=CARTESIAN_POINT('Ctrl Pts',(-13.3068741897951,72.9206303161106,
64.150906941191));
#123167=CARTESIAN_POINT('Ctrl Pts',(-13.2989021548328,72.6365043448969,
64.2222676715389));
#123168=CARTESIAN_POINT('Ctrl Pts',(-13.2841430096769,72.11390741135,64.3812599171973));
#123169=CARTESIAN_POINT('Ctrl Pts',(-13.2774143257934,71.8748867859194,
64.4653481326174));
#123170=CARTESIAN_POINT('Ctrl Pts',(-13.26220366846,71.3373124473978,64.6802439653337));
#123171=CARTESIAN_POINT('Ctrl Pts',(-13.2537603715575,71.0411819714063,
64.8176543050313));
#123172=CARTESIAN_POINT('Ctrl Pts',(-13.2347161766478,70.3900011803531,
65.1631713777577));
#123173=CARTESIAN_POINT('Ctrl Pts',(-13.2241240900908,70.0397173233626,
65.3804032542507));
#123174=CARTESIAN_POINT('Ctrl Pts',(-13.2051183934299,69.4482949212431,
65.8047240141437));
#123175=CARTESIAN_POINT('Ctrl Pts',(-13.1967624649786,69.2005327453609,
66.00270251492));
#123176=CARTESIAN_POINT('Ctrl Pts',(-13.1818819584551,68.7862115849624,
66.3710115826409));
#123177=CARTESIAN_POINT('Ctrl Pts',(-13.1754097133126,68.6148257190972,
66.535904073327));
#123178=CARTESIAN_POINT('Ctrl Pts',(-13.1624110166355,68.2799723187363,
66.8849633204276));
#123179=CARTESIAN_POINT('Ctrl Pts',(-13.1559150838736,68.1172195495557,
67.0694098321845));
#123180=CARTESIAN_POINT('Ctrl Pts',(-13.1354655682893,67.6240205700236,
67.6765416477148));
#123181=CARTESIAN_POINT('Ctrl Pts',(-13.1217679375107,67.322809964869,68.123242778279));
#123182=CARTESIAN_POINT('Ctrl Pts',(-13.1015177943972,66.9432140501511,
68.8085880289499));
#123183=CARTESIAN_POINT('Ctrl Pts',(-13.0950997382616,66.8323194547083,
69.0293555972505));
#123184=CARTESIAN_POINT('Ctrl Pts',(-13.0773000587725,66.5537365188385,
69.6448401820738));
#123185=CARTESIAN_POINT('Ctrl Pts',(-13.0655752232905,66.4044147511725,
70.047863266239));
#123186=CARTESIAN_POINT('Ctrl Pts',(-13.0486019735719,66.2296064977183,
70.6489567976515));
#123187=CARTESIAN_POINT('Ctrl Pts',(-13.043332694699,66.1809619688838,70.839625496625));
#123188=CARTESIAN_POINT('Ctrl Pts',(-13.0239654869984,66.0229808213967,
71.5572526921515));
#123189=CARTESIAN_POINT('Ctrl Pts',(-13.0103353904296,65.9546993289936,
72.0927051944972));
#123190=CARTESIAN_POINT('Ctrl Pts',(-12.9885990908377,65.9215169832869,
72.94027813103));
#123191=CARTESIAN_POINT('Ctrl Pts',(-12.9805888307732,65.9251310481666,
73.2512490738343));
#123192=CARTESIAN_POINT('Ctrl Pts',(-12.9675766122192,65.9559266866908,
73.74381766199));
#123193=CARTESIAN_POINT('Ctrl Pts',(-12.9626850690453,65.9728160711133,
73.9260876702788));
#123194=CARTESIAN_POINT('Ctrl Pts',(-12.9484343499011,66.0370404315548,
74.4475702119123));
#123195=CARTESIAN_POINT('Ctrl Pts',(-12.9389457038534,66.098081394884,74.7850890378309));
#123196=CARTESIAN_POINT('Ctrl Pts',(-12.925582513397,66.2141810184528,75.2668037068532));
#123197=CARTESIAN_POINT('Ctrl Pts',(-12.9215223251056,66.2538082057257,
75.4143612272045));
#123198=CARTESIAN_POINT('Ctrl Pts',(-12.9103588328681,66.3746781881217,
75.8224056279332));
#123199=CARTESIAN_POINT('Ctrl Pts',(-12.9033635871439,66.4640962439975,
76.0803740916759));
#123200=CARTESIAN_POINT('Ctrl Pts',(-12.8882860121754,66.6828685200793,
76.6303282834251));
#123201=CARTESIAN_POINT('Ctrl Pts',(-12.880219860982,66.8164302170816,76.9206510033425));
#123202=CARTESIAN_POINT('Ctrl Pts',(-12.8666140533297,67.0629123031222,
77.3903188047085));
#123203=CARTESIAN_POINT('Ctrl Pts',(-12.8611410249638,67.1675695463286,
77.5740349716444));
#123204=CARTESIAN_POINT('Ctrl Pts',(-12.8511834084674,67.3655746794775,
77.8952730849634));
#123205=CARTESIAN_POINT('Ctrl Pts',(-12.8467286199518,67.4565482303131,
78.0342668066983));
#123206=CARTESIAN_POINT('Ctrl Pts',(-12.833995788073,67.7239259088111,78.4194204642622));
#123207=CARTESIAN_POINT('Ctrl Pts',(-12.8256153163989,67.9089901421128,
78.6595736177276));
#123208=CARTESIAN_POINT('Ctrl Pts',(-12.812629429129,68.2185515999683,79.0218455084534));
#123209=CARTESIAN_POINT('Ctrl Pts',(-12.8079363573752,68.3352956683199,
79.1507091594142));
#123210=CARTESIAN_POINT('Ctrl Pts',(-12.7990549287592,68.5677928938533,
79.3926279738622));
#123211=CARTESIAN_POINT('Ctrl Pts',(-12.7948525605507,68.6828733112431,
79.5060229309362));
#123212=CARTESIAN_POINT('Ctrl Pts',(-12.7806824443328,69.085267748706,79.8817244083457));
#123213=CARTESIAN_POINT('Ctrl Pts',(-12.7709327824128,69.3868228250467,
80.1287660236168));
#123214=CARTESIAN_POINT('Ctrl Pts',(-12.7566803432005,69.8424642292089,
80.4559321600454));
#123215=CARTESIAN_POINT('Ctrl Pts',(-12.7522856836234,69.9849367350732,
80.552272782412));
#123216=CARTESIAN_POINT('Ctrl Pts',(-12.7440584346135,70.2528646125522,
80.7226820373419));
#123217=CARTESIAN_POINT('Ctrl Pts',(-12.7402422777692,70.3775937352692,
80.7979062825841));
#123218=CARTESIAN_POINT('Ctrl Pts',(-12.7276119703817,70.7894664750456,
81.0331177540324));
#123219=CARTESIAN_POINT('Ctrl Pts',(-12.7185610917208,71.0836724484624,
81.1807805316131));
#123220=CARTESIAN_POINT('Ctrl Pts',(-12.702293439271,71.6269553837915,81.4174559790179));
#123221=CARTESIAN_POINT('Ctrl Pts',(-12.6950675809478,71.8735050770989,
81.512293743389));
#123222=CARTESIAN_POINT('Ctrl Pts',(-12.6845676398191,72.2467370303841,
81.6371436992725));
#123223=CARTESIAN_POINT('Ctrl Pts',(-12.6811649282168,72.3703507424593,
81.6755062985264));
#123224=CARTESIAN_POINT('Ctrl Pts',(-12.6696724559748,72.7959008790564,
81.7974905154234));
#123225=CARTESIAN_POINT('Ctrl Pts',(-12.6617808167259,73.1014806864576,
81.8679574019711));
#123226=CARTESIAN_POINT('Ctrl Pts',(-12.646439637525,73.7008182023705,81.9739776539254));
#123227=CARTESIAN_POINT('Ctrl Pts',(-12.6389889782674,73.9942699533495,
82.011283164141));
#123228=CARTESIAN_POINT('Ctrl Pts',(-12.6278434068756,74.4232051779274,
82.0448901912824));
#123229=CARTESIAN_POINT('Ctrl Pts',(-12.6243059456231,74.5578259666299,
82.0524580466115));
#123230=CARTESIAN_POINT('Ctrl Pts',(-12.6148482026504,74.9128642445359,
82.0645788122341));
#123231=CARTESIAN_POINT('Ctrl Pts',(-12.6088559346375,75.1334576442571,
82.06416141907));
#123232=CARTESIAN_POINT('Ctrl Pts',(-12.5953156808615,75.6281410419969,
82.0453178066303));
#123233=CARTESIAN_POINT('Ctrl Pts',(-12.5877472401498,75.9020786960933,
82.0224912276371));
#123234=CARTESIAN_POINT('Ctrl Pts',(-12.5754682039387,76.3504212585025,
81.9644199628588));
#123235=CARTESIAN_POINT('Ctrl Pts',(-12.5706936698356,76.5257589578696,
81.9364229349427));
#123236=CARTESIAN_POINT('Ctrl Pts',(-12.5623439346404,76.8364716997386,
81.8772308815007));
#123237=CARTESIAN_POINT('Ctrl Pts',(-12.5587450920961,76.9720237602414,
81.8480940252307));
#123238=CARTESIAN_POINT('Ctrl Pts',(-12.5463814236343,77.4405981239887,
81.7359365737801));
#123239=CARTESIAN_POINT('Ctrl Pts',(-12.5378228793052,77.769782858668,81.6368484111675));
#123240=CARTESIAN_POINT('Ctrl Pts',(-12.5252668781339,78.2367696310233,
81.4670486765995));
#123241=CARTESIAN_POINT('Ctrl Pts',(-12.5213608271997,78.3798637588088,
81.4108881467845));
#123242=CARTESIAN_POINT('Ctrl Pts',(-12.5138496797056,78.6483701795652,
81.2976356180653));
#123243=CARTESIAN_POINT('Ctrl Pts',(-12.5102502760716,78.7740794318261,
81.2412427123319));
#123244=CARTESIAN_POINT('Ctrl Pts',(-12.4945868895627,79.307834183047,80.9872211680897));
#123245=CARTESIAN_POINT('Ctrl Pts',(-12.4820732174252,79.7028366912285,
80.7620305089869));
#123246=CARTESIAN_POINT('Ctrl Pts',(-12.4648059240783,80.227945570971,80.40821904971));
#123247=CARTESIAN_POINT('Ctrl Pts',(-12.4599257936274,80.3740861746635,
80.3033082210613));
#123248=CARTESIAN_POINT('Ctrl Pts',(-12.4511559708814,80.634188495179,80.1044868638146));
#123249=CARTESIAN_POINT('Ctrl Pts',(-12.4472457653971,80.7492164195056,
80.0119814787204));
#123250=CARTESIAN_POINT('Ctrl Pts',(-12.4332795506338,81.1582244220697,
79.6659256628228));
#123251=CARTESIAN_POINT('Ctrl Pts',(-12.4236150142218,81.4380023386033,
79.3958458132811));
#123252=CARTESIAN_POINT('Ctrl Pts',(-12.4100069435382,81.8010927749715,
78.9975352387134));
#123253=CARTESIAN_POINT('Ctrl Pts',(-12.4061747844966,81.9000221752958,
78.8834324251171));
#123254=CARTESIAN_POINT('Ctrl Pts',(-12.3984621213635,82.0906265432574,
78.6522776794879));
#123255=CARTESIAN_POINT('Ctrl Pts',(-12.3945765142021,82.1823911497242,
78.5352973120272));
#123256=CARTESIAN_POINT('Ctrl Pts',(-12.3827850493668,82.4487635846914,
78.1781950435444));
#123257=CARTESIAN_POINT('Ctrl Pts',(-12.3747418122683,82.6147305355668,
77.9315979227482));
#123258=CARTESIAN_POINT('Ctrl Pts',(-12.3588545103332,82.91685114776,77.4318820722629));
#123259=CARTESIAN_POINT('Ctrl Pts',(-12.351012514832,83.0538253470931,77.1792180890642));
#123260=CARTESIAN_POINT('Ctrl Pts',(-12.3379241347035,83.2647422152221,
76.741680778256));
#123261=CARTESIAN_POINT('Ctrl Pts',(-12.3326223872496,83.3451029286835,
76.5599022296358));
#123262=CARTESIAN_POINT('Ctrl Pts',(-12.3230759992552,83.4811363673166,
76.2221284152004));
#123263=CARTESIAN_POINT('Ctrl Pts',(-12.3188237233838,83.5385306234,76.0672737673675));
#123264=CARTESIAN_POINT('Ctrl Pts',(-12.3059762950662,83.7007336782974,
75.589358835331));
#123265=CARTESIAN_POINT('Ctrl Pts',(-12.2975196851177,83.7915195380404,
75.2617906469131));
#123266=CARTESIAN_POINT('Ctrl Pts',(-12.284416541049,83.9002990261761,74.7627277986276));
#123267=CARTESIAN_POINT('Ctrl Pts',(-12.2799483222741,83.9320801054606,
74.5942380095015));
#123268=CARTESIAN_POINT('Ctrl Pts',(-12.2676973283403,84.0053152103195,
74.1357483228414));
#123269=CARTESIAN_POINT('Ctrl Pts',(-12.2598136509086,84.03765462545,73.844267491681));
#123270=CARTESIAN_POINT('Ctrl Pts',(-12.243010956856,84.0765286814414,73.2241921333138));
#123271=CARTESIAN_POINT('Ctrl Pts',(-12.2340817631658,84.0794669516359,
72.8953261693159));
#123272=CARTESIAN_POINT('Ctrl Pts',(-12.2192024854395,84.0543085669752,
72.3413562601775));
#123273=CARTESIAN_POINT('Ctrl Pts',(-12.2131903613112,84.0355885901246,
72.1158209549323));
#123274=CARTESIAN_POINT('Ctrl Pts',(-12.1991156142519,83.9706342828342,
71.5807516670429));
#123275=CARTESIAN_POINT('Ctrl Pts',(-12.1912430531929,83.9166562606102,
71.2732499383507));
#123276=CARTESIAN_POINT('Ctrl Pts',(-12.1785628959082,83.8049388610954,
70.7861645488808));
#123277=CARTESIAN_POINT('Ctrl Pts',(-12.1737622640556,83.7571752478623,
70.6041849778724));
#123278=CARTESIAN_POINT('Ctrl Pts',(-12.1621925259686,83.6306908125787,
70.1765927133141));
#123279=CARTESIAN_POINT('Ctrl Pts',(-12.155381403236,83.5470588002038,69.9324277607096));
#123280=CARTESIAN_POINT('Ctrl Pts',(-12.135766427616,83.2795469543242,69.2470416383225));
#123281=CARTESIAN_POINT('Ctrl Pts',(-12.1228063212596,83.0709738936559,
68.8153488006643));
#123282=CARTESIAN_POINT('Ctrl Pts',(-12.1038849508357,82.7143540404618,
68.2049686009164));
#123283=CARTESIAN_POINT('Ctrl Pts',(-12.0977932247745,82.5913421194022,
68.0115833645262));
#123284=CARTESIAN_POINT('Ctrl Pts',(-12.0859684623677,82.3352464314142,
67.6411035413038));
#123285=CARTESIAN_POINT('Ctrl Pts',(-12.0802589120059,82.2029032967178,
67.4640614477432));
#123286=CARTESIAN_POINT('Ctrl Pts',(-12.0680022595118,81.901768283777,67.0911217221234));
#123287=CARTESIAN_POINT('Ctrl Pts',(-12.0614431166126,81.7312092381388,
66.8976311253861));
#123288=CARTESIAN_POINT('Ctrl Pts',(-12.0350907451483,81.0277197183915,
66.1648734460141));
#123289=CARTESIAN_POINT('Ctrl Pts',(-12.0146415565156,80.4340705962415,
65.6835536311353));
#123290=CARTESIAN_POINT('Ctrl Pts',(-11.9861207020082,79.5260624044424,
65.1177839484425));
#123291=CARTESIAN_POINT('Ctrl Pts',(-11.9778495822136,79.2529846788054,
64.9664801821875));
#123292=CARTESIAN_POINT('Ctrl Pts',(-11.9563975669566,78.516556851685,64.6073049986407));
#123293=CARTESIAN_POINT('Ctrl Pts',(-11.9435203999241,78.0439024990142,
64.4251713358605));
#123294=CARTESIAN_POINT('Ctrl Pts',(-11.8997917000753,76.4413545917399,
63.955826946439));
#123295=CARTESIAN_POINT('Ctrl Pts',(-11.8683582127767,75.2573169088765,
63.8422182709281));
#123296=CARTESIAN_POINT('Ctrl Pts',(-11.8230247640893,73.5295526399705,
64.0160172908243));
#123297=CARTESIAN_POINT('Ctrl Pts',(-11.8081872143295,72.9709249133046,
64.1266639140826));
#123298=CARTESIAN_POINT('Ctrl Pts',(-11.7711827409064,71.6199064620653,
64.5270034009169));
#123299=CARTESIAN_POINT('Ctrl Pts',(-11.738904698618,70.4680384568216,64.9838759366761));
#123300=CARTESIAN_POINT('Ctrl Pts',(-11.683963031582,68.8379068340988,66.3014728066721));
#123301=CARTESIAN_POINT('Ctrl Pts',(-11.6684195253985,68.4099673656422,
66.7237215655609));
#123302=CARTESIAN_POINT('Ctrl Pts',(-11.6445866614158,67.8269749097122,
67.4234734941558));
#123303=CARTESIAN_POINT('Ctrl Pts',(-11.6363748850356,67.6391360600916,
67.6738942448746));
#123304=CARTESIAN_POINT('Ctrl Pts',(-11.6139907705485,67.1672167477589,
68.3756301632476));
#123305=CARTESIAN_POINT('Ctrl Pts',(-11.5995675723112,66.9092625860644,
68.8432102479295));
#123306=CARTESIAN_POINT('Ctrl Pts',(-11.5761640350408,66.5517926648154,
69.6574927779121));
#123307=CARTESIAN_POINT('Ctrl Pts',(-11.5669860779528,66.4288090560081,
69.9894867289769));
#123308=CARTESIAN_POINT('Ctrl Pts',(-11.5416972747449,66.1432248448741,
70.9230510370065));
#123309=CARTESIAN_POINT('Ctrl Pts',(-11.5256205887917,66.0218137197234,
71.5374256873591));
#123310=CARTESIAN_POINT('Ctrl Pts',(-11.5015728944489,65.9379543872354,
72.4382896118954));
#123311=CARTESIAN_POINT('Ctrl Pts',(-11.4939376963333,65.9248703381677,
72.7202149910102));
#123312=CARTESIAN_POINT('Ctrl Pts',(-11.4799783985566,65.9253087201448,
73.2360564909682));
#123313=CARTESIAN_POINT('Ctrl Pts',(-11.4737305181669,65.9346898217129,
73.4691147765804));
#123314=CARTESIAN_POINT('Ctrl Pts',(-11.461462234947,65.9716054716059,73.9330051590798));
#123315=CARTESIAN_POINT('Ctrl Pts',(-11.4554357373374,65.9989288197087,
74.1632051665436));
#123316=CARTESIAN_POINT('Ctrl Pts',(-11.436431174078,66.1134062822752,74.8894375070278));
#123317=CARTESIAN_POINT('Ctrl Pts',(-11.4235929510636,66.2331522473532,
75.3804019438939));
#123318=CARTESIAN_POINT('Ctrl Pts',(-11.4039580363381,66.4715142352684,
76.0963920715314));
#123319=CARTESIAN_POINT('Ctrl Pts',(-11.3973588721539,66.5606049907156,
76.3313660082699));
#123320=CARTESIAN_POINT('Ctrl Pts',(-11.3855131280604,66.7346096341848,
76.7386951469584));
#123321=CARTESIAN_POINT('Ctrl Pts',(-11.380299463487,66.8155544511462,76.9127505942496));
#123322=CARTESIAN_POINT('Ctrl Pts',(-11.3676148063142,67.0251092041908,
77.3281676202458));
#123323=CARTESIAN_POINT('Ctrl Pts',(-11.360145787446,67.1594163536749,77.5668108127286));
#123324=CARTESIAN_POINT('Ctrl Pts',(-11.3470740162834,67.4204480446439,
77.9840353655374));
#123325=CARTESIAN_POINT('Ctrl Pts',(-11.341390207838,67.5427478377599,78.164464478255));
#123326=CARTESIAN_POINT('Ctrl Pts',(-11.3278575667772,67.8521077144758,
78.5871696700794));
#123327=CARTESIAN_POINT('Ctrl Pts',(-11.3200632355294,68.045343253798,78.824924085721));
#123328=CARTESIAN_POINT('Ctrl Pts',(-11.303856794792,68.4695769470887,79.2965611134832));
#123329=CARTESIAN_POINT('Ctrl Pts',(-11.295439055484,68.7023320071261,79.528916990291));
#123330=CARTESIAN_POINT('Ctrl Pts',(-11.2822070002329,69.0783193405568,
79.8659813912701));
#123331=CARTESIAN_POINT('Ctrl Pts',(-11.2775251264432,69.2132061360693,
79.9800526775385));
#123332=CARTESIAN_POINT('Ctrl Pts',(-11.2635480851696,69.6188891659272,
80.3034138395053));
#123333=CARTESIAN_POINT('Ctrl Pts',(-11.2540666495126,69.8984948524752,
80.5016572189363));
#123334=CARTESIAN_POINT('Ctrl Pts',(-11.2402553948987,70.3294348510951,
80.7715033277092));
#123335=CARTESIAN_POINT('Ctrl Pts',(-11.2357957702606,70.4726147436903,
80.8556940786965));
#123336=CARTESIAN_POINT('Ctrl Pts',(-11.226031295672,70.7966107214824,81.0341546158046));
#123337=CARTESIAN_POINT('Ctrl Pts',(-11.2207595596775,70.9781670271131,
81.1262131508542));
#123338=CARTESIAN_POINT('Ctrl Pts',(-11.2077292262514,71.4386085384673,
81.3404794186449));
#123339=CARTESIAN_POINT('Ctrl Pts',(-11.2000345207221,71.7210793827409,
81.4549782229865));
#123340=CARTESIAN_POINT('Ctrl Pts',(-11.1849992988541,72.2792537971876,
81.6494725518392));
#123341=CARTESIAN_POINT('Ctrl Pts',(-11.1776627778634,72.5544204164013,
81.7310975951903));
#123342=CARTESIAN_POINT('Ctrl Pts',(-11.1661861333091,72.9796903608049,
81.8358593485588));
#123343=CARTESIAN_POINT('Ctrl Pts',(-11.1621696184886,73.1274980702723,
81.8684154793323));
#123344=CARTESIAN_POINT('Ctrl Pts',(-11.1536965122738,73.4362445673246,
81.9284303650665));
#123345=CARTESIAN_POINT('Ctrl Pts',(-11.14923889819,73.5973034419281,81.9552859638776));
#123346=CARTESIAN_POINT('Ctrl Pts',(-11.1354479115498,74.095608384285,82.0246398185578));
#123347=CARTESIAN_POINT('Ctrl Pts',(-11.1260611004602,74.4348687842597,
82.0526069627284));
#123348=CARTESIAN_POINT('Ctrl Pts',(-11.1132847863632,74.9137958663528,
82.0645609659671));
#123349=CARTESIAN_POINT('Ctrl Pts',(-11.1096344325108,75.0528851330426,
82.0647569843448));
#123350=CARTESIAN_POINT('Ctrl Pts',(-11.097451488835,75.5222664236924,82.0545033550214));
#123351=CARTESIAN_POINT('Ctrl Pts',(-11.0891109015025,75.8522790135066,
82.0290056159743));
#123352=CARTESIAN_POINT('Ctrl Pts',(-11.0731591278899,76.4779139290216,
81.9463295571717));
#123353=CARTESIAN_POINT('Ctrl Pts',(-11.0655487002234,76.773957797436,81.8922289112971));
#123354=CARTESIAN_POINT('Ctrl Pts',(-11.0541089926271,77.2027813124686,
81.7919009598897));
#123355=CARTESIAN_POINT('Ctrl Pts',(-11.0504324152805,77.3382213250744,
81.7569309772833));
#123356=CARTESIAN_POINT('Ctrl Pts',(-11.0395110816555,77.7319107042377,
81.6456185433552));
#123357=CARTESIAN_POINT('Ctrl Pts',(-11.0321327395218,77.9878144579349,
81.560936713203));
#123358=CARTESIAN_POINT('Ctrl Pts',(-11.0160723366018,78.5345152964866,
81.3526799100089));
#123359=CARTESIAN_POINT('Ctrl Pts',(-11.0073864060271,78.8237214348501,
81.2249110123661));
#123360=CARTESIAN_POINT('Ctrl Pts',(-10.995523273993,79.2203641592331,81.0238803300764));
#123361=CARTESIAN_POINT('Ctrl Pts',(-10.9921389815689,79.3338722568417,
80.9632120031192));
#123362=CARTESIAN_POINT('Ctrl Pts',(-10.9851430172786,79.5687433371426,
80.8310605102586));
#123363=CARTESIAN_POINT('Ctrl Pts',(-10.9815399342954,79.6897131415036,
80.759182953659));
#123364=CARTESIAN_POINT('Ctrl Pts',(-10.970129390683,80.0701013964238,80.5209530187167));
#123365=CARTESIAN_POINT('Ctrl Pts',(-10.9624233072592,80.3228815115587,
80.3440073690476));
#123366=CARTESIAN_POINT('Ctrl Pts',(-10.9494508315752,80.7266720984723,
80.0298384114745));
#123367=CARTESIAN_POINT('Ctrl Pts',(-10.9442447135714,80.883087339794,79.8995387813573));
#123368=CARTESIAN_POINT('Ctrl Pts',(-10.9352272618405,81.1406594814284,
79.6700506114573));
#123369=CARTESIAN_POINT('Ctrl Pts',(-10.931468298786,81.2441438311538,79.5734655898293));
#123370=CARTESIAN_POINT('Ctrl Pts',(-10.9229822704551,81.470005458756,79.3526661384571));
#123371=CARTESIAN_POINT('Ctrl Pts',(-10.9182350454293,81.5912007312285,
79.2272356724659));
#123372=CARTESIAN_POINT('Ctrl Pts',(-10.9020030173533,81.9911897640813,
78.7888296477144));
#123373=CARTESIAN_POINT('Ctrl Pts',(-10.8904187287239,82.2523713314234,
78.4597671882362));
#123374=CARTESIAN_POINT('Ctrl Pts',(-10.8758390717496,82.5626442097709,
78.0067722268572));
#123375=CARTESIAN_POINT('Ctrl Pts',(-10.872443510504,82.6335816113649,77.8981809201727));
#123376=CARTESIAN_POINT('Ctrl Pts',(-10.8615128088464,82.8571960949351,
77.5389438864602));
#123377=CARTESIAN_POINT('Ctrl Pts',(-10.854151008882,82.9998691784603,77.2823937818435));
#123378=CARTESIAN_POINT('Ctrl Pts',(-10.8398330113968,83.2520152333316,
76.7724142411953));
#123379=CARTESIAN_POINT('Ctrl Pts',(-10.8328778790993,83.3629621935259,
76.5197172542601));
#123380=CARTESIAN_POINT('Ctrl Pts',(-10.8220340017719,83.5134344201952,
76.1302013555007));
#123381=CARTESIAN_POINT('Ctrl Pts',(-10.8182906544755,83.5614911438892,
75.9966613381224));
#123382=CARTESIAN_POINT('Ctrl Pts',(-10.8100790459964,83.6589444655758,
75.7047932533741));
#123383=CARTESIAN_POINT('Ctrl Pts',(-10.805596054612,83.707201183287,75.5460768921971));
#123384=CARTESIAN_POINT('Ctrl Pts',(-10.7905233374584,83.8539709219854,
75.0116408948854));
#123385=CARTESIAN_POINT('Ctrl Pts',(-10.7798132579853,83.9330152256115,
74.6305418036001));
#123386=CARTESIAN_POINT('Ctrl Pts',(-10.7648866957545,84.0103282714376,
74.0816038978186));
#123387=CARTESIAN_POINT('Ctrl Pts',(-10.7604640999119,84.0289311753907,
73.91663382697));
#123388=CARTESIAN_POINT('Ctrl Pts',(-10.7518282430458,84.0566969974354,
73.5881549578561));
#123389=CARTESIAN_POINT('Ctrl Pts',(-10.7476287681822,84.0659508983708,
73.4249268254314));
#123390=CARTESIAN_POINT('Ctrl Pts',(-10.7369089950463,84.0783125154229,
73.0034218628282));
#123391=CARTESIAN_POINT('Ctrl Pts',(-10.7304495321392,84.0747281652656,
72.7449048836405));
#123392=CARTESIAN_POINT('Ctrl Pts',(-10.7189021956243,84.0489699557529,
72.2887506864487));
#123393=CARTESIAN_POINT('Ctrl Pts',(-10.7138396085273,84.0312872964701,
72.0908628998149));
#123394=CARTESIAN_POINT('Ctrl Pts',(-10.7040256390475,83.9856008159391,
71.717068354512));
#123395=CARTESIAN_POINT('Ctrl Pts',(-10.6993074056721,83.9588552189296,
71.5410052129082));
#123396=CARTESIAN_POINT('Ctrl Pts',(-10.6883676563367,83.8857880556542,
71.1390987168748));
#123397=CARTESIAN_POINT('Ctrl Pts',(-10.6821126698903,83.8360159121452,
70.913866793063));
#123398=CARTESIAN_POINT('Ctrl Pts',(-10.6647578788761,83.6748783135999,
70.2963632020085));
#123399=CARTESIAN_POINT('Ctrl Pts',(-10.6536314488456,83.5455642563476,
69.9087429247327));
#123400=CARTESIAN_POINT('Ctrl Pts',(-10.6387704893156,83.3320061063279,
69.3894003495198));
#123401=CARTESIAN_POINT('Ctrl Pts',(-10.6347472808774,83.2698176549128,
69.2485817466867));
#123402=CARTESIAN_POINT('Ctrl Pts',(-10.6267493833386,83.1369122834732,
68.9676880493098));
#123403=CARTESIAN_POINT('Ctrl Pts',(-10.622775296033,83.0661878347582,68.8278812557266));
#123404=CARTESIAN_POINT('Ctrl Pts',(-10.6106636336823,82.8388717217479,
68.40621890752));
#123405=CARTESIAN_POINT('Ctrl Pts',(-10.60255735847,82.6706398329936,68.1306584318951));
#123406=CARTESIAN_POINT('Ctrl Pts',(-10.5885771942367,82.3668852831137,
67.6875722247586));
#123407=CARTESIAN_POINT('Ctrl Pts',(-10.5828885964537,82.2391850817937,
67.5146839739715));
#123408=CARTESIAN_POINT('Ctrl Pts',(-10.5692504803771,81.921960006923,67.1153221651725));
#123409=CARTESIAN_POINT('Ctrl Pts',(-10.5612512148942,81.727165806553,66.8929947304493));
#123410=CARTESIAN_POINT('Ctrl Pts',(-10.5435319075459,81.2722102448684,
66.4218138464385));
#123411=CARTESIAN_POINT('Ctrl Pts',(-10.5338183891719,81.0070363711832,
66.1777518799018));
#123412=CARTESIAN_POINT('Ctrl Pts',(-10.5194676891263,80.5855150542378,
65.8341332595257));
#123413=CARTESIAN_POINT('Ctrl Pts',(-10.5146683306702,80.4392027997058,
65.7221643306107));
#123414=CARTESIAN_POINT('Ctrl Pts',(-10.5047176744966,80.1239421895527,
65.4961505584553));
#123415=CARTESIAN_POINT('Ctrl Pts',(-10.499576210428,79.9545533087552,65.383294232073));
#123416=CARTESIAN_POINT('Ctrl Pts',(-10.4888830249124,79.5967004160453,
65.1619505119251));
#123417=CARTESIAN_POINT('Ctrl Pts',(-10.4833082953928,79.4077355140865,
65.0542964008141));
#123418=CARTESIAN_POINT('Ctrl Pts',(-10.4702868364309,78.9660838679099,
64.8231668544518));
#123419=CARTESIAN_POINT('Ctrl Pts',(-10.4628034926422,78.7109646074756,
64.7043176959357));
#123420=CARTESIAN_POINT('Ctrl Pts',(-10.4429926927163,78.0283863439525,
64.4236983412069));
#123421=CARTESIAN_POINT('Ctrl Pts',(-10.4305578883603,77.5927797074079,
64.2814987911854));
#123422=CARTESIAN_POINT('Ctrl Pts',(-10.4117972714492,76.9121080083537,
64.1147808037987));
#123423=CARTESIAN_POINT('Ctrl Pts',(-10.4053261437037,76.6728659880689,
64.0663019989242));
#123424=CARTESIAN_POINT('Ctrl Pts',(-10.3924704747258,76.1857043884102,
63.9881669547922));
#123425=CARTESIAN_POINT('Ctrl Pts',(-10.3861511257801,75.9386255716942,
63.959137783098));
#123426=CARTESIAN_POINT('Ctrl Pts',(-10.3713108958127,75.3523051671442,
63.9148915114114));
#123427=CARTESIAN_POINT('Ctrl Pts',(-10.362733387284,75.0128591344745,63.9085165958738));
#123428=CARTESIAN_POINT('Ctrl Pts',(-10.3401166534282,74.1289295276929,
63.9410628493276));
#123429=CARTESIAN_POINT('Ctrl Pts',(-10.3260052712222,73.5854220383952,
64.0099614259926));
#123430=CARTESIAN_POINT('Ctrl Pts',(-10.3026746214761,72.7193661825693,
64.1994590185667));
#123431=CARTESIAN_POINT('Ctrl Pts',(-10.2935997285093,72.3903230828583,
64.29100020586));
#123432=CARTESIAN_POINT('Ctrl Pts',(-10.2771851687998,71.8164515781705,
64.4864564148652));
#123433=CARTESIAN_POINT('Ctrl Pts',(-10.2699644152529,71.569986256241,64.5828222381821));
#123434=CARTESIAN_POINT('Ctrl Pts',(-10.2547777509193,71.0769910820738,
64.8014282605783));
#123435=CARTESIAN_POINT('Ctrl Pts',(-10.2467455153074,70.8317810443425,
64.9238945174778));
#123436=CARTESIAN_POINT('Ctrl Pts',(-10.2197265688772,70.0470125104654,
65.3610879081932));
#123437=CARTESIAN_POINT('Ctrl Pts',(-10.1998805061955,69.5325629390287,
65.7212544317407));
#123438=CARTESIAN_POINT('Ctrl Pts',(-10.1710850937717,68.8153166755438,
66.3412913225327));
#123439=CARTESIAN_POINT('Ctrl Pts',(-10.1614971478665,68.5817403100494,
66.565910497724));
#123440=CARTESIAN_POINT('Ctrl Pts',(-10.1496876337135,68.2943085028007,
66.8737771833284));
#123441=CARTESIAN_POINT('Ctrl Pts',(-10.1469980858286,68.2288702338781,
66.9461926427268));
#123442=CARTESIAN_POINT('Ctrl Pts',(-10.1426652596873,68.1232727188615,
67.0669657211208));
#123443=CARTESIAN_POINT('Ctrl Pts',(-10.1409904959236,68.082410690264,67.1147062631595));
#123444=CARTESIAN_POINT('Ctrl Pts',(-10.1377322385359,68.0027565016216,
67.209789323264));
#123445=CARTESIAN_POINT('Ctrl Pts',(-10.1361495029794,67.9639758520655,
67.2570649985359));
#123446=CARTESIAN_POINT('Ctrl Pts',(-10.1320253387701,67.8627351097104,
67.3831132172281));
#123447=CARTESIAN_POINT('Ctrl Pts',(-10.1295231532016,67.8011406699431,
67.4625170228407));
#123448=CARTESIAN_POINT('Ctrl Pts',(-10.1209819085711,67.5911480164043,
67.742829592026));
#123449=CARTESIAN_POINT('Ctrl Pts',(-10.1152119461978,67.4497532638925,
67.9489759575478));
#123450=CARTESIAN_POINT('Ctrl Pts',(-10.1050291723372,67.2082880174862,
68.334092729626));
#123451=CARTESIAN_POINT('Ctrl Pts',(-10.1005588812509,67.1053631655791,
68.5112665138926));
#123452=CARTESIAN_POINT('Ctrl Pts',(-10.0961244884418,67.0084911154305,
68.691687827272));
#123453=CARTESIAN_POINT('Ctrl Pts',(-13.4857787351653,83.53086080835,69.194683933252));
#123454=CARTESIAN_POINT('Ctrl Pts',(-13.4107459268847,82.33835458422,66.513462598172));
#123455=CARTESIAN_POINT('Ctrl Pts',(-13.2981967144638,78.53320802489,63.458709829566));
#123456=CARTESIAN_POINT('Ctrl Pts',(-13.1481310979025,72.48811911993,63.63322643035));
#123457=CARTESIAN_POINT('Ctrl Pts',(-13.0355818854816,68.51429278678,65.790797832361));
#123458=CARTESIAN_POINT('Ctrl Pts',(-12.9230326730606,65.95227475056,69.522686716285));
#123459=CARTESIAN_POINT('Ctrl Pts',(-12.8104834606397,65.36509547432,74.009771845382));
#123460=CARTESIAN_POINT('Ctrl Pts',(-12.6979342482187,66.87977327092,78.274405364341));
#123461=CARTESIAN_POINT('Ctrl Pts',(-12.5853850357977,70.16613638824,81.385801227635));
#123462=CARTESIAN_POINT('Ctrl Pts',(-12.4728358233767,74.50710712086,82.665227893767));
#123463=CARTESIAN_POINT('Ctrl Pts',(-12.3602866109557,78.95561877133,81.83352216413));
#123464=CARTESIAN_POINT('Ctrl Pts',(-12.2477373985346,82.54111542822,79.072147533527));
#123465=CARTESIAN_POINT('Ctrl Pts',(-12.1351881861136,84.48133587032,74.983562774911));
#123466=CARTESIAN_POINT('Ctrl Pts',(-12.0226389736926,84.35297372718,70.459791926131));
#123467=CARTESIAN_POINT('Ctrl Pts',(-11.9100897612715,82.18403440969,66.487804766612));
#123468=CARTESIAN_POINT('Ctrl Pts',(-11.7975405488505,78.44772440513,63.934186298037));
#123469=CARTESIAN_POINT('Ctrl Pts',(-11.6849913364294,73.95921002211,63.356070078148));
#123470=CARTESIAN_POINT('Ctrl Pts',(-11.5724421240084,69.69776911955,64.879586131319));
#123471=CARTESIAN_POINT('Ctrl Pts',(-11.4598929115869,66.59313798963,68.172342617968));
#123472=CARTESIAN_POINT('Ctrl Pts',(-11.3473436991659,65.32266693424,72.5159451614496));
#123473=CARTESIAN_POINT('Ctrl Pts',(-11.2347944867449,66.16353987442,76.962731892397));
#123474=CARTESIAN_POINT('Ctrl Pts',(-11.1222452743239,68.93230019525,80.542528950631));
#123475=CARTESIAN_POINT('Ctrl Pts',(-11.0096960619029,73.02487543835,82.474316725385));
#123476=CARTESIAN_POINT('Ctrl Pts',(-10.8971468494819,77.5483732915,82.336630496769));
#123477=CARTESIAN_POINT('Ctrl Pts',(-10.7845976370609,81.5158764696,80.159504403197));
#123478=CARTESIAN_POINT('Ctrl Pts',(-10.6720484246399,84.06180417873,76.417951402524));
#123479=CARTESIAN_POINT('Ctrl Pts',(-10.5594992122189,84.63060417684,71.928205926366));
#123480=CARTESIAN_POINT('Ctrl Pts',(-10.4469499997979,83.09853951678,67.670097151854));
#123481=CARTESIAN_POINT('Ctrl Pts',(-10.3344007873769,79.79852165914,64.571579248221));
#123482=CARTESIAN_POINT('Ctrl Pts',(-10.2218515749559,75.45555056223,63.312606598678));
#123483=CARTESIAN_POINT('Ctrl Pts',(-10.0717859583949,69.51269706816,64.433342187813));
#123484=CARTESIAN_POINT('Ctrl Pts',(-9.95923674597391,66.44785978885,68.230370929682));
#123485=CARTESIAN_POINT('Ctrl Pts',(-9.88420393769391,65.8555809379,71.104431594487));
#123486=CARTESIAN_POINT('Ctrl Pts',(-13.7163617470419,83.16594445251,69.356984978657));
#123487=CARTESIAN_POINT('Ctrl Pts',(-13.6413289387609,82.02444891012,66.790455647208));
#123488=CARTESIAN_POINT('Ctrl Pts',(-13.5287797263401,78.38207141327,63.866373073948));
#123489=CARTESIAN_POINT('Ctrl Pts',(-13.3787141097789,72.59556741124,64.033424547414));
#123490=CARTESIAN_POINT('Ctrl Pts',(-13.2661648973579,68.79172559158,66.09870361091));
#123491=CARTESIAN_POINT('Ctrl Pts',(-13.153615684937,66.33930051512,69.670957104856));
#123492=CARTESIAN_POINT('Ctrl Pts',(-13.041066472516,65.77723843707,73.9661025469177));
#123493=CARTESIAN_POINT('Ctrl Pts',(-12.928517260095,67.22712433115,78.048311975543));
#123494=CARTESIAN_POINT('Ctrl Pts',(-12.815968047674,70.37290988194,81.026614676792));
#123495=CARTESIAN_POINT('Ctrl Pts',(-12.703418835253,74.5281911213,82.251312549785));
#123496=CARTESIAN_POINT('Ctrl Pts',(-12.590869622832,78.78641310501,81.455183889208));
#123497=CARTESIAN_POINT('Ctrl Pts',(-12.478320410411,82.2185364502,78.811929902003));
#123498=CARTESIAN_POINT('Ctrl Pts',(-12.3657711979899,84.07576196493,74.898238566719));
#123499=CARTESIAN_POINT('Ctrl Pts',(-12.2532219855689,83.95289064466,70.567976674408));
#123500=CARTESIAN_POINT('Ctrl Pts',(-12.1406727731479,81.87672993999,66.765895355836));
#123501=CARTESIAN_POINT('Ctrl Pts',(-12.0281235607268,78.3002444434,64.321510546861));
#123502=CARTESIAN_POINT('Ctrl Pts',(-11.9155743483058,74.00373088522,63.768123843582));
#123503=CARTESIAN_POINT('Ctrl Pts',(-11.8030251358847,69.92457750553,65.2264699287));
#123504=CARTESIAN_POINT('Ctrl Pts',(-11.6904759234637,66.95275016922,68.378375365861));
#123505=CARTESIAN_POINT('Ctrl Pts',(-11.5779267110427,65.73662482149,72.5361758376591));
#123506=CARTESIAN_POINT('Ctrl Pts',(-11.4653774986219,66.54152855574,76.792746687058));
#123507=CARTESIAN_POINT('Ctrl Pts',(-11.3528282862009,69.19185230266,80.219414239796));
#123508=CARTESIAN_POINT('Ctrl Pts',(-11.2402790737799,73.10936342534,82.068567803219));
#123509=CARTESIAN_POINT('Ctrl Pts',(-11.1277298613589,77.4393639997,81.936771244833));
#123510=CARTESIAN_POINT('Ctrl Pts',(-11.0151806489379,81.23715314378,79.852773961851));
#123511=CARTESIAN_POINT('Ctrl Pts',(-10.9026314365169,83.67417617347,76.271269743701));
#123512=CARTESIAN_POINT('Ctrl Pts',(-10.7900822240959,84.21864516594,71.973577753657));
#123513=CARTESIAN_POINT('Ctrl Pts',(-10.6775330116749,82.75211614938,67.897613966809));
#123514=CARTESIAN_POINT('Ctrl Pts',(-10.5649837992539,79.59325995385,64.931638357232));
#123515=CARTESIAN_POINT('Ctrl Pts',(-10.4524345868329,75.43606391784,63.726519559207));
#123516=CARTESIAN_POINT('Ctrl Pts',(-10.3023689702719,69.7474221017,64.799314529419));
#123517=CARTESIAN_POINT('Ctrl Pts',(-10.1898197578509,66.81368639306,68.433921456821));
#123518=CARTESIAN_POINT('Ctrl Pts',(-10.1147869495699,66.24674287986,71.185041217093));
#123519=CARTESIAN_POINT('Ctrl Pts',(-13.9469447589179,82.80102809666,69.519286024043));
#123520=CARTESIAN_POINT('Ctrl Pts',(-13.8719119506369,81.710543236,67.067448696223));
#123521=CARTESIAN_POINT('Ctrl Pts',(-13.7593627382169,78.23093480162,64.274036318316));
#123522=CARTESIAN_POINT('Ctrl Pts',(-13.6092971216549,72.7030157025,64.433622664488));
#123523=CARTESIAN_POINT('Ctrl Pts',(-13.4967479092343,69.06915839634,66.406609389489));
#123524=CARTESIAN_POINT('Ctrl Pts',(-13.3841986968133,66.72632627966,69.819227493478));
#123525=CARTESIAN_POINT('Ctrl Pts',(-13.2716494843923,66.18938139983,73.9224332485153));
#123526=CARTESIAN_POINT('Ctrl Pts',(-13.1591002719714,67.57447539142,77.822218586803));
#123527=CARTESIAN_POINT('Ctrl Pts',(-13.0465510595504,70.57968337571,80.667428125987));
#123528=CARTESIAN_POINT('Ctrl Pts',(-12.9340018471294,74.54927512182,81.837397205809));
#123529=CARTESIAN_POINT('Ctrl Pts',(-12.8214526347083,78.61720743877,81.076845614251));
#123530=CARTESIAN_POINT('Ctrl Pts',(-12.7089034222873,81.89595747223,78.551712270407));
#123531=CARTESIAN_POINT('Ctrl Pts',(-12.5963542098663,83.67018805956,74.812914358431));
#123532=CARTESIAN_POINT('Ctrl Pts',(-12.4838049974453,83.55280756212,70.676161422585));
#123533=CARTESIAN_POINT('Ctrl Pts',(-12.3712557850242,81.56942547021,67.043985944979));
#123534=CARTESIAN_POINT('Ctrl Pts',(-12.2587065726032,78.15276448156,64.708834795646));
#123535=CARTESIAN_POINT('Ctrl Pts',(-12.1461573601821,74.04825174822,64.180177609028));
#123536=CARTESIAN_POINT('Ctrl Pts',(-12.0336081477611,70.15138589142,65.573353726144));
#123537=CARTESIAN_POINT('Ctrl Pts',(-11.92105893534,67.31236234875,68.584408113854));
#123538=CARTESIAN_POINT('Ctrl Pts',(-11.808509722919,66.15058270873,72.5564065139833));
#123539=CARTESIAN_POINT('Ctrl Pts',(-11.695960510498,66.9195172371,76.622761481822));
#123540=CARTESIAN_POINT('Ctrl Pts',(-11.5834112980769,69.45140441015,79.89629952903));
#123541=CARTESIAN_POINT('Ctrl Pts',(-11.4708620856559,73.19385141245,81.662818881074));
#123542=CARTESIAN_POINT('Ctrl Pts',(-11.3583128732349,77.330354708,81.53691199287));
#123543=CARTESIAN_POINT('Ctrl Pts',(-11.2457636608139,80.95842981803,79.54604352044));
#123544=CARTESIAN_POINT('Ctrl Pts',(-11.1332144483929,83.28654816823,76.124588084795));
#123545=CARTESIAN_POINT('Ctrl Pts',(-11.0206652359719,83.80668615503,72.0189495808697));
#123546=CARTESIAN_POINT('Ctrl Pts',(-10.9081160235509,82.40569278195,68.125130781709));
#123547=CARTESIAN_POINT('Ctrl Pts',(-10.7955668111299,79.38799824851,65.291697466218));
#123548=CARTESIAN_POINT('Ctrl Pts',(-10.6830175987089,75.4165772734,64.140432519737));
#123549=CARTESIAN_POINT('Ctrl Pts',(-10.5329519821479,69.98214713522,65.165286871043));
#123550=CARTESIAN_POINT('Ctrl Pts',(-10.4204027697269,67.17951299727,68.637471983962));
#123551=CARTESIAN_POINT('Ctrl Pts',(-10.3453699614459,66.63790482183,71.265650839687));
#123552=CARTESIAN_POINT('Ctrl Pts',(-14.1775277707939,82.43611174083,69.681587069447));
#123553=CARTESIAN_POINT('Ctrl Pts',(-14.1024949625139,81.3966375619,67.344441745258));
#123554=CARTESIAN_POINT('Ctrl Pts',(-13.9899457500929,78.07979819,64.681699562697));
#123555=CARTESIAN_POINT('Ctrl Pts',(-13.8398801335319,72.8104639938,64.833820781552));
#123556=CARTESIAN_POINT('Ctrl Pts',(-13.7273309211109,69.34659120114,66.714515168039));
#123557=CARTESIAN_POINT('Ctrl Pts',(-13.6147817086899,67.11335204423,69.967497882051));
#123558=CARTESIAN_POINT('Ctrl Pts',(-13.5022324962687,66.60152436258,73.878763950054));
#123559=CARTESIAN_POINT('Ctrl Pts',(-13.3896832838477,67.92182645165,77.596125198008));
#123560=CARTESIAN_POINT('Ctrl Pts',(-13.2771340714267,70.78645686942,80.308241575145));
#123561=CARTESIAN_POINT('Ctrl Pts',(-13.1645848590057,74.57035912226,81.423481861828));
#123562=CARTESIAN_POINT('Ctrl Pts',(-13.0520356465847,78.44800177245,80.698507339327));
#123563=CARTESIAN_POINT('Ctrl Pts',(-12.9394864341637,81.57337849421,78.29149463888));
#123564=CARTESIAN_POINT('Ctrl Pts',(-12.8269372217426,83.26461415418,74.727590150234));
#123565=CARTESIAN_POINT('Ctrl Pts',(-12.7143880093216,83.1527244796,70.784346170858));
#123566=CARTESIAN_POINT('Ctrl Pts',(-12.6018387969006,81.26212100051,67.322076534199));
#123567=CARTESIAN_POINT('Ctrl Pts',(-12.4892895844795,78.00528451983,65.096159044468));
#123568=CARTESIAN_POINT('Ctrl Pts',(-12.3767403720585,74.09277261133,64.592231374463));
#123569=CARTESIAN_POINT('Ctrl Pts',(-12.2641911596374,70.37819427741,65.920237523529));
#123570=CARTESIAN_POINT('Ctrl Pts',(-12.1516419472164,67.67197452834,68.790440861752));
#123571=CARTESIAN_POINT('Ctrl Pts',(-12.0390927347954,66.56454059598,72.5766371901982));
#123572=CARTESIAN_POINT('Ctrl Pts',(-11.9265435223743,67.29750591841,76.452776276488));
#123573=CARTESIAN_POINT('Ctrl Pts',(-11.8139943099533,69.71095651757,79.573184818198));
#123574=CARTESIAN_POINT('Ctrl Pts',(-11.7014450975323,73.27833939945,81.257069958908));
#123575=CARTESIAN_POINT('Ctrl Pts',(-11.5888958851113,77.22134541621,81.137052740933));
#123576=CARTESIAN_POINT('Ctrl Pts',(-11.4763466726899,80.67970649221,79.239313079091));
#123577=CARTESIAN_POINT('Ctrl Pts',(-11.3637974602689,82.89892016296,75.977906425967));
#123578=CARTESIAN_POINT('Ctrl Pts',(-11.2512482478479,83.39472714413,72.0643214081573));
#123579=CARTESIAN_POINT('Ctrl Pts',(-11.1386990354269,82.05926941456,68.352647596662));
#123580=CARTESIAN_POINT('Ctrl Pts',(-11.0261498230059,79.18273654321,65.651756575228));
#123581=CARTESIAN_POINT('Ctrl Pts',(-10.9136006105849,75.39709062901,64.554345480267));
#123582=CARTESIAN_POINT('Ctrl Pts',(-10.7635349940239,70.21687216876,65.53125921265));
#123583=CARTESIAN_POINT('Ctrl Pts',(-10.6509857816029,67.54533960148,68.841022511101));
#123584=CARTESIAN_POINT('Ctrl Pts',(-10.5759529733229,67.02906676379,71.346260462292));
#123585=CARTESIAN_POINT('Ctrl Pts',(-13.5675364833309,80.6475155947738,
66.0116637084142));
#123586=CARTESIAN_POINT('Ctrl Pts',(-13.5675364833309,80.8673931721485,
66.1731545541286));
#123587=CARTESIAN_POINT('Ctrl Pts',(-13.5675364833309,81.0802488986569,
66.3442606841591));
#123588=CARTESIAN_POINT('Ctrl Pts',(-13.5675364833309,81.4923702907423,
66.7063307057292));
#123589=CARTESIAN_POINT('Ctrl Pts',(-13.5675364833309,81.6915016168863,
66.8975231489235));
#123590=CARTESIAN_POINT('Ctrl Pts',(-13.5675364833309,81.881676986561,67.0972279350825));
#123591=CARTESIAN_POINT('Origin',(-13.5675364833309,75.,72.98888938658));
#123592=CARTESIAN_POINT('Origin',(-15.5675364832709,-75.,72.98888938658));
#123593=CARTESIAN_POINT('',(-15.5675364832709,-81.062177826491,72.98888938658));
#123594=CARTESIAN_POINT('',(-15.5675364832709,-78.0310889132455,78.23888938658));
#123595=CARTESIAN_POINT('',(-15.5675364832709,-78.0310889132455,78.23888938658));
#123596=CARTESIAN_POINT('',(-15.5675364832709,-71.9689110867544,78.23888938658));
#123597=CARTESIAN_POINT('',(-15.5675364832709,-71.9689110867544,78.23888938658));
#123598=CARTESIAN_POINT('',(-15.5675364832709,-68.9378221735089,72.98888938658));
#123599=CARTESIAN_POINT('',(-15.5675364832709,-68.9378221735089,72.98888938658));
#123600=CARTESIAN_POINT('',(-15.5675364832709,-71.9689110867545,67.73888938658));
#123601=CARTESIAN_POINT('',(-15.5675364832709,-71.9689110867545,67.73888938658));
#123602=CARTESIAN_POINT('',(-15.5675364832709,-78.0310889132455,67.73888938658));
#123603=CARTESIAN_POINT('',(-15.5675364832709,-78.0310889132455,67.73888938658));
#123604=CARTESIAN_POINT('',(-15.5675364832709,-81.062177826491,72.98888938658));
#123605=CARTESIAN_POINT('Origin',(-25.5675364832709,-78.0310889132455,78.23888938658));
#123606=CARTESIAN_POINT('',(-25.5675364832709,-81.062177826491,72.98888938658));
#123607=CARTESIAN_POINT('',(-25.5675364832709,-78.0310889132455,78.23888938658));
#123608=CARTESIAN_POINT('Origin',(-25.5675364832709,-71.9689110867544,78.23888938658));
#123609=CARTESIAN_POINT('',(-25.5675364832709,-71.9689110867544,78.23888938658));
#123610=CARTESIAN_POINT('Origin',(-25.5675364832709,-68.9378221735089,72.98888938658));
#123611=CARTESIAN_POINT('',(-25.5675364832709,-68.9378221735089,72.98888938658));
#123612=CARTESIAN_POINT('Origin',(-25.5675364832709,-71.9689110867545,67.73888938658));
#123613=CARTESIAN_POINT('',(-25.5675364832709,-71.9689110867545,67.73888938658));
#123614=CARTESIAN_POINT('Origin',(-25.5675364832709,-78.0310889132455,67.73888938658));
#123615=CARTESIAN_POINT('',(-25.5675364832709,-78.0310889132455,67.73888938658));
#123616=CARTESIAN_POINT('Origin',(-25.5675364832709,-81.062177826491,72.98888938658));
#123617=CARTESIAN_POINT('Origin',(-18.5675364832709,-75.,72.98888938658));
#123618=CARTESIAN_POINT('Origin',(-20.5675364832709,-75.,72.98888938658));
#123619=CARTESIAN_POINT('Ctrl Pts',(11.7737028196091,-21.80503453548,82.974463848657));
#123620=CARTESIAN_POINT('Ctrl Pts',(11.7842119497491,-21.8209908852,82.976752059407));
#123621=CARTESIAN_POINT('Ctrl Pts',(11.9074330236891,-22.0118587646,83.00150321689));
#123622=CARTESIAN_POINT('Ctrl Pts',(12.1327094234791,-22.44912871337,82.99331681448));
#123623=CARTESIAN_POINT('Ctrl Pts',(12.3872208177991,-23.19361457716,82.796143394484));
#123624=CARTESIAN_POINT('Ctrl Pts',(12.4980497482091,-23.77070951624,82.495844470338));
#123625=CARTESIAN_POINT('Ctrl Pts',(12.5268844558191,-24.09442226678,82.2737301581291));
#123626=CARTESIAN_POINT('Ctrl Pts',(12.5306001626891,-24.14726018536,82.236125320949));
#123627=CARTESIAN_POINT('Ctrl Pts',(11.8797038575791,-21.71767911338,82.436822495267));
#123628=CARTESIAN_POINT('Ctrl Pts',(11.8865435901191,-21.73097889939,82.438814682516));
#123629=CARTESIAN_POINT('Ctrl Pts',(11.9662971783691,-21.8903986298,82.4607304615951));
#123630=CARTESIAN_POINT('Ctrl Pts',(12.1018554065891,-22.26337977053,82.463312214956));
#123631=CARTESIAN_POINT('Ctrl Pts',(12.2277242566991,-22.91758315467,82.330367392035));
#123632=CARTESIAN_POINT('Ctrl Pts',(12.2549645866691,-23.44051817093,82.115603938798));
#123633=CARTESIAN_POINT('Ctrl Pts',(12.2436931578091,-23.7395527805,81.954214255122));
#123634=CARTESIAN_POINT('Ctrl Pts',(12.2410774442991,-23.78850636215,81.926839572217));
#123635=CARTESIAN_POINT('Ctrl Pts',(12.2573963950691,-21.44250482709,82.137598971116));
#123636=CARTESIAN_POINT('Ctrl Pts',(12.2635341762291,-21.45619889632,82.1383257760441));
#123637=CARTESIAN_POINT('Ctrl Pts',(12.3343464866891,-21.61991088389,82.1449108583021));
#123638=CARTESIAN_POINT('Ctrl Pts',(12.4352004835491,-21.99123106393,82.109689603077));
#123639=CARTESIAN_POINT('Ctrl Pts',(12.4740260820391,-22.60719182595,81.935724156804));
#123640=CARTESIAN_POINT('Ctrl Pts',(12.4201268319991,-23.08268362029,81.721934479734));
#123641=CARTESIAN_POINT('Ctrl Pts',(12.3623316865191,-23.35150381325,81.575321364862));
#123642=CARTESIAN_POINT('Ctrl Pts',(12.3521581962191,-23.39540043164,81.550724432541));
#123643=CARTESIAN_POINT('Ctrl Pts',(12.7032417518891,-21.12780322461,82.238044969419));
#123644=CARTESIAN_POINT('Ctrl Pts',(12.7120233098291,-21.14472994457,82.237218948315));
#123645=CARTESIAN_POINT('Ctrl Pts',(12.8132390090491,-21.34616149612,82.224239734821));
#123646=CARTESIAN_POINT('Ctrl Pts',(12.9531048408191,-21.77934365529,82.123016365173));
#123647=CARTESIAN_POINT('Ctrl Pts',(12.9933941281391,-22.42971061916,81.824887107694));
#123648=CARTESIAN_POINT('Ctrl Pts',(12.9045304751091,-22.89004306637,81.526984743628));
#123649=CARTESIAN_POINT('Ctrl Pts',(12.8188656848891,-23.13939512993,81.341237038185));
#123650=CARTESIAN_POINT('Ctrl Pts',(12.8039809507391,-23.17978735852,81.310468521703));
#123651=CARTESIAN_POINT('',(11.9367309803807,-21.8592780094232,82.7099370787206));
#123652=CARTESIAN_POINT('',(12.6211149266398,-23.1949866874293,81.5466536447308));
#123653=CARTESIAN_POINT('Ctrl Pts',(11.9367361538315,-21.8592750801367,
82.7099405001105));
#123654=CARTESIAN_POINT('Ctrl Pts',(11.9622030980227,-21.8915999880229,
82.6991156916996));
#123655=CARTESIAN_POINT('Ctrl Pts',(11.9881073830353,-21.9253909044623,
82.686248515633));
#123656=CARTESIAN_POINT('Ctrl Pts',(12.0142120213475,-21.96058406732,82.6711822410034));
#123657=CARTESIAN_POINT('Ctrl Pts',(12.0397543732084,-21.9950191795043,
82.6564404896249));
#123658=CARTESIAN_POINT('Ctrl Pts',(12.0654879223436,-22.0307968926114,
82.6395928765279));
#123659=CARTESIAN_POINT('Ctrl Pts',(12.091184141745,-22.0678087196869,82.6204972631129));
#123660=CARTESIAN_POINT('Ctrl Pts',(12.111834171334,-22.0975522127786,82.6051516211771));
#123661=CARTESIAN_POINT('Ctrl Pts',(12.1324598146958,-22.1280917768807,
82.5883541804234));
#123662=CARTESIAN_POINT('Ctrl Pts',(12.1529436620966,-22.159347265805,82.5700366962959));
#123663=CARTESIAN_POINT('Ctrl Pts',(12.1778034947841,-22.1972798968201,
82.5478060292853));
#123664=CARTESIAN_POINT('Ctrl Pts',(12.202453650089,-22.2362680889833,82.5233356680296));
#123665=CARTESIAN_POINT('Ctrl Pts',(12.2266946108567,-22.2761267814906,
82.496519371568));
#123666=CARTESIAN_POINT('Ctrl Pts',(12.2375690653905,-22.2940073244114,
82.4844896257411));
#123667=CARTESIAN_POINT('Ctrl Pts',(12.2483613802324,-22.3120624442134,
82.4719880522356));
#123668=CARTESIAN_POINT('Ctrl Pts',(12.2590548093192,-22.3302726084963,
82.4590065396343));
#123669=CARTESIAN_POINT('Ctrl Pts',(12.2656381470914,-22.3414835737899,
82.4510145586191));
#123670=CARTESIAN_POINT('Ctrl Pts',(12.2721840230251,-22.3527532703367,
82.4428406920455));
#123671=CARTESIAN_POINT('Ctrl Pts',(12.2786887204933,-22.364076830813,82.4344832478605));
#123672=CARTESIAN_POINT('Ctrl Pts',(12.2892432084479,-22.3824503805796,
82.4209225028125));
#123673=CARTESIAN_POINT('Ctrl Pts',(12.2996892145748,-22.4009658161235,
82.4068783698921));
#123674=CARTESIAN_POINT('Ctrl Pts',(12.3100118138469,-22.4196011341924,
82.3923445214752));
#123675=CARTESIAN_POINT('Ctrl Pts',(12.3183540060871,-22.4346612369525,
82.3805990149134));
#123676=CARTESIAN_POINT('Ctrl Pts',(12.3266156437967,-22.4497997587411,
82.3685336671056));
#123677=CARTESIAN_POINT('Ctrl Pts',(12.3347894358396,-22.4650042051673,
82.3561457565399));
#123678=CARTESIAN_POINT('Ctrl Pts',(12.3398113417301,-22.4743456832313,
82.3485347333192));
#123679=CARTESIAN_POINT('Ctrl Pts',(12.3446189812725,-22.4833743225494,
82.3410841813665));
#123680=CARTESIAN_POINT('Ctrl Pts',(12.3495471969363,-22.4927104514669,
82.3332749532429));
#123681=CARTESIAN_POINT('Ctrl Pts',(12.3526402805277,-22.4985700625578,
82.3283736670537));
#123682=CARTESIAN_POINT('Ctrl Pts',(12.3557800676704,-22.504550607999,82.3233305968092));
#123683=CARTESIAN_POINT('Ctrl Pts',(12.3590406769578,-22.5108028429602,
82.3180120668465));
#123684=CARTESIAN_POINT('Ctrl Pts',(12.3824229780028,-22.5556385246324,
82.2798721188351));
#123685=CARTESIAN_POINT('Ctrl Pts',(12.4041003709132,-22.5998921737425,
82.240400081111));
#123686=CARTESIAN_POINT('Ctrl Pts',(12.4241951999649,-22.6433365148074,
82.1997161277026));
#123687=CARTESIAN_POINT('Ctrl Pts',(12.4446093426681,-22.6874712011915,
82.1583856924713));
#123688=CARTESIAN_POINT('Ctrl Pts',(12.4633908163091,-22.7307703672997,
82.1158049661513));
#123689=CARTESIAN_POINT('Ctrl Pts',(12.4806936617776,-22.773042052157,82.0721100489682));
#123690=CARTESIAN_POINT('Ctrl Pts',(12.4984950964185,-22.8165318143765,
82.0271560433517));
#123691=CARTESIAN_POINT('Ctrl Pts',(12.5147320846937,-22.8589338308361,
81.9810231648695));
#123692=CARTESIAN_POINT('Ctrl Pts',(12.5295900954036,-22.900091637856,81.9338632672124));
#123693=CARTESIAN_POINT('Ctrl Pts',(12.5447043782732,-22.9419593380302,
81.8858899518606));
#123694=CARTESIAN_POINT('Ctrl Pts',(12.5583923685859,-22.982539647835,81.8368543167831));
#123695=CARTESIAN_POINT('Ctrl Pts',(12.5708573524237,-23.0217220410528,
81.7869130407606));
#123696=CARTESIAN_POINT('Ctrl Pts',(12.5836915758153,-23.0620651007883,
81.7354923970383));
#123697=CARTESIAN_POINT('Ctrl Pts',(12.595229903226,-23.1009263988723,81.6831120651281));
#123698=CARTESIAN_POINT('Ctrl Pts',(12.6056925681694,-23.1382400019589,
81.6299332280271));
#123699=CARTESIAN_POINT('Ctrl Pts',(12.6111132368744,-23.1575720441887,
81.6023814656797));
#123700=CARTESIAN_POINT('Ctrl Pts',(12.6162450821,-23.1764895136934,81.5746151666791));
#123701=CARTESIAN_POINT('Ctrl Pts',(12.6211177605568,-23.194988395035,81.5466552684072));
#123702=CARTESIAN_POINT('',(12.5172257454391,-21.43204530223,82.22390472213));
#123703=CARTESIAN_POINT('Ctrl Pts',(11.9367208753803,-21.8592837299615,
82.7099303959673));
#123704=CARTESIAN_POINT('Ctrl Pts',(11.9491160482679,-21.848141643132,82.6816498425584));
#123705=CARTESIAN_POINT('Ctrl Pts',(11.9628731595236,-21.8361810914248,
82.6538570180536));
#123706=CARTESIAN_POINT('Ctrl Pts',(11.9779676352564,-21.8234463126838,
82.6268031589723));
#123707=CARTESIAN_POINT('Ctrl Pts',(11.9928703653537,-21.8108733042677,
82.6000929659777));
#123708=CARTESIAN_POINT('Ctrl Pts',(12.0090767055389,-21.7975457050617,
82.5741039294356));
#123709=CARTESIAN_POINT('Ctrl Pts',(12.0265202200287,-21.7835329478403,
82.5490727877408));
#123710=CARTESIAN_POINT('Ctrl Pts',(12.0438587432357,-21.7696045324158,
82.5241923067215));
#123711=CARTESIAN_POINT('Ctrl Pts',(12.0624194312919,-21.7549993785506,
82.5002590484555));
#123712=CARTESIAN_POINT('Ctrl Pts',(12.0820955779931,-21.7398102759138,
82.4774879979392));
#123713=CARTESIAN_POINT('Ctrl Pts',(12.1016867174577,-21.7246867950505,
82.4548153256321));
#123714=CARTESIAN_POINT('Ctrl Pts',(12.1223833406148,-21.7089847118948,
82.433295570755));
#123715=CARTESIAN_POINT('Ctrl Pts',(12.1440427643665,-21.6928162797401,
82.413111864013));
#123716=CARTESIAN_POINT('Ctrl Pts',(12.1544146354514,-21.6850738348868,
82.4034466574616));
#123717=CARTESIAN_POINT('Ctrl Pts',(12.165006766415,-21.6772247283014,82.3940873195626));
#123718=CARTESIAN_POINT('Ctrl Pts',(12.175800879479,-21.6692826127025,82.3850508899748));
#123719=CARTESIAN_POINT('Ctrl Pts',(12.1983165878219,-21.6527159566566,
82.3662015772193));
#123720=CARTESIAN_POINT('Ctrl Pts',(12.221712471054,-21.6357439101918,82.3487602726554));
#123721=CARTESIAN_POINT('Ctrl Pts',(12.2458031684748,-21.6184980794134,
82.3328492103853));
#123722=CARTESIAN_POINT('Ctrl Pts',(12.2700378782506,-21.6011491543716,
82.3168430329964));
#123723=CARTESIAN_POINT('Ctrl Pts',(12.2949750489175,-21.5835236405448,
82.3023857528171));
#123724=CARTESIAN_POINT('Ctrl Pts',(12.3204084032296,-21.5657611169978,
82.289552276764));
#123725=CARTESIAN_POINT('Ctrl Pts',(12.3459603671866,-21.5479157570861,
82.2766589511913));
#123726=CARTESIAN_POINT('Ctrl Pts',(12.3720124086933,-21.5299325919223,
82.2654046417675));
#123727=CARTESIAN_POINT('Ctrl Pts',(12.3983485415761,-21.5119514677974,
82.2558129175903));
#123728=CARTESIAN_POINT('Ctrl Pts',(12.4249913690804,-21.4937609464128,
82.2461094940141));
#123729=CARTESIAN_POINT('Ctrl Pts',(12.4519242002296,-21.4755729740054,
82.2381074290571));
#123730=CARTESIAN_POINT('Ctrl Pts',(12.4789278146413,-21.4575233831369,
82.2317786261044));
#123731=CARTESIAN_POINT('Ctrl Pts',(12.4916861066886,-21.4489955635597,
82.2287884813353));
#123732=CARTESIAN_POINT('Ctrl Pts',(12.5044603332855,-21.4404984616105,
82.2261711119611));
#123733=CARTESIAN_POINT('Ctrl Pts',(12.5172284057885,-21.4320453006202,
82.2239198161667));
#123734=CARTESIAN_POINT('Ctrl Pts',(12.5172257454391,-21.43204530223,82.22390472213));
#123735=CARTESIAN_POINT('Ctrl Pts',(12.6340357992967,-21.713678275013,82.2033623527417));
#123736=CARTESIAN_POINT('Ctrl Pts',(12.692894450305,-22.0223140153352,82.1188254444615));
#123737=CARTESIAN_POINT('Ctrl Pts',(12.7189823415742,-22.623367521142,81.8782087798771));
#123738=CARTESIAN_POINT('Ctrl Pts',(12.6874951393621,-22.9152905983023,
81.7236169057246));
#123739=CARTESIAN_POINT('Ctrl Pts',(12.6211129829291,-23.19498551621,81.546652531098));
#123740=CARTESIAN_POINT('Origin',(18.2606283043191,-15.,57.49100545192));
#123741=CARTESIAN_POINT('',(19.1777592571107,-16.3235270075928,58.627271032273));
#123742=CARTESIAN_POINT('',(20.4074538435026,-16.3235291382987,65.6012398999359));
#123743=CARTESIAN_POINT('',(19.1777552349091,-16.32352916975,58.62727005114));
#123744=CARTESIAN_POINT('',(21.1895064189377,-15.0000003990606,65.4633429305542));
#123745=CARTESIAN_POINT('Origin',(19.7122947894255,-15.,65.7238151970535));
#123746=CARTESIAN_POINT('',(19.9598072782762,-15.0000003739637,58.4893725505111));
#123747=CARTESIAN_POINT('',(19.9598072256691,-15.00000060839,58.48937225217));
#123748=CARTESIAN_POINT('Origin',(18.4825957015691,-15.,58.74984511652));
#123749=CARTESIAN_POINT('Ctrl Pts',(12.5199362278991,-23.49480870114,81.306473853632));
#123750=CARTESIAN_POINT('Ctrl Pts',(12.3430034024391,-23.49480870114,81.620480433794));
#123751=CARTESIAN_POINT('Ctrl Pts',(11.9272160718391,-23.49480870114,82.318177658235));
#123752=CARTESIAN_POINT('Ctrl Pts',(11.2242863296091,-23.49480870114,83.3524350127001));
#123753=CARTESIAN_POINT('Ctrl Pts',(10.4115975050891,-23.49480870114,84.38086299568));
#123754=CARTESIAN_POINT('Ctrl Pts',(9.55586525979908,-23.49480870114,85.31060223946));
#123755=CARTESIAN_POINT('Ctrl Pts',(8.6576193448791,-23.49480870114,86.1471009819601));
#123756=CARTESIAN_POINT('Ctrl Pts',(7.70893043203909,-23.49480870114,86.90213314277));
#123757=CARTESIAN_POINT('Ctrl Pts',(6.71139644797909,-23.49480870114,87.57700589972));
#123758=CARTESIAN_POINT('Ctrl Pts',(5.68377226408909,-23.49480870114,88.16713174316));
#123759=CARTESIAN_POINT('Ctrl Pts',(4.61844145667909,-23.49480870114,88.69058723386));
#123760=CARTESIAN_POINT('Ctrl Pts',(3.47639771609909,-23.49480870114,89.1742936871701));
#123761=CARTESIAN_POINT('Ctrl Pts',(2.24422019413909,-23.49480870114,89.62822366128));
#123762=CARTESIAN_POINT('Ctrl Pts',(1.38880489860909,-23.49480870114,89.9114551536101));
#123763=CARTESIAN_POINT('Ctrl Pts',(0.957537393149087,-23.49480870114,90.05047159017));
#123764=CARTESIAN_POINT('Ctrl Pts',(13.5266301189791,-22.19079082182,81.873739112569));
#123765=CARTESIAN_POINT('Ctrl Pts',(13.3404943832391,-22.19079082182,82.2040797061641));
#123766=CARTESIAN_POINT('Ctrl Pts',(12.9022454213091,-22.19079082182,82.939551587252));
#123767=CARTESIAN_POINT('Ctrl Pts',(12.1577492774591,-22.19079082182,84.03519946655));
#123768=CARTESIAN_POINT('Ctrl Pts',(11.2923354682991,-22.19079082182,85.13056199279));
#123769=CARTESIAN_POINT('Ctrl Pts',(10.3768252729191,-22.19079082182,86.12540154234));
#123770=CARTESIAN_POINT('Ctrl Pts',(9.4127272028091,-22.19079082182,87.0233027811901));
#123771=CARTESIAN_POINT('Ctrl Pts',(8.39331680038909,-22.19079082182,87.83461537407));
#123772=CARTESIAN_POINT('Ctrl Pts',(7.32308119035909,-22.19079082182,88.5585788914901));
#123773=CARTESIAN_POINT('Ctrl Pts',(6.22576052973909,-22.19079082182,89.18856810325));
#123774=CARTESIAN_POINT('Ctrl Pts',(5.09676735478909,-22.19079082182,89.74312289588));
#123775=CARTESIAN_POINT('Ctrl Pts',(3.89863512110909,-22.19079082182,90.2503735744501));
#123776=CARTESIAN_POINT('Ctrl Pts',(2.62244286138909,-22.19079082182,90.7203026262499));
#123777=CARTESIAN_POINT('Ctrl Pts',(1.74918245929909,-22.19079082182,91.0093591043299));
#123778=CARTESIAN_POINT('Ctrl Pts',(1.31205504332909,-22.19079082182,91.1502619594));
#123779=CARTESIAN_POINT('Ctrl Pts',(12.7677580370791,-20.68183777369,81.446119781757));
#123780=CARTESIAN_POINT('Ctrl Pts',(12.5885596948691,-20.68183777369,81.7641473704861));
#123781=CARTESIAN_POINT('Ctrl Pts',(12.1672428958191,-20.68183777369,82.471143731272));
#123782=CARTESIAN_POINT('Ctrl Pts',(11.4540805884091,-20.68183777369,83.5205138335801));
#123783=CARTESIAN_POINT('Ctrl Pts',(10.6284122462891,-20.68183777369,84.56541935731));
#123784=CARTESIAN_POINT('Ctrl Pts',(9.75796422704909,-20.68183777369,85.51118460035));
#123785=CARTESIAN_POINT('Ctrl Pts',(8.8435072271191,-20.68183777369,86.3627990377701));
#123786=CARTESIAN_POINT('Ctrl Pts',(7.87740852601909,-20.68183777369,87.13168597471));
#123787=CARTESIAN_POINT('Ctrl Pts',(6.86197729568909,-20.68183777369,87.81864359795));
#123788=CARTESIAN_POINT('Ctrl Pts',(5.81719565499909,-20.68183777369,88.41858276414));
#123789=CARTESIAN_POINT('Ctrl Pts',(4.73619283124909,-20.68183777369,88.9496940927601));
#123790=CARTESIAN_POINT('Ctrl Pts',(3.58034156490909,-20.68183777369,89.43919652094));
#123791=CARTESIAN_POINT('Ctrl Pts',(2.33732876120909,-20.68183777369,89.89706505117));
#123792=CARTESIAN_POINT('Ctrl Pts',(1.47752046534909,-20.68183777369,90.1817305032401));
#123793=CARTESIAN_POINT('Ctrl Pts',(1.04481040258909,-20.68183777369,90.3212113268901));
#123794=CARTESIAN_POINT('Ctrl Pts',(11.2805063366991,-21.03030703232,80.6080634188521));
#123795=CARTESIAN_POINT('Ctrl Pts',(11.1149040280891,-21.03030703232,80.9019597503359));
#123796=CARTESIAN_POINT('Ctrl Pts',(10.7267711985491,-21.03030703232,81.5531492538179));
#123797=CARTESIAN_POINT('Ctrl Pts',(10.0750175298891,-21.03030703232,82.511823303176));
#123798=CARTESIAN_POINT('Ctrl Pts',(9.32724309746908,-21.03030703232,83.4578422496101));
#123799=CARTESIAN_POINT('Ctrl Pts',(8.54510877389908,-21.03030703232,84.30743074885));
#123800=CARTESIAN_POINT('Ctrl Pts',(7.72793927182908,-21.03030703232,85.06833144705));
#123801=CARTESIAN_POINT('Ctrl Pts',(6.86632184011909,-21.03030703232,85.7540717899401));
#123802=CARTESIAN_POINT('Ctrl Pts',(5.95829725822909,-21.03030703232,86.3685045695999));
#123803=CARTESIAN_POINT('Ctrl Pts',(5.01648257150909,-21.03030703232,86.9095510944));
#123804=CARTESIAN_POINT('Ctrl Pts',(4.02953213566909,-21.03030703232,87.3947174837801));
#123805=CARTESIAN_POINT('Ctrl Pts',(2.95654389997909,-21.03030703232,87.84943655887));
#123806=CARTESIAN_POINT('Ctrl Pts',(1.77855681476909,-21.03030703232,88.2836686533401));
#123807=CARTESIAN_POINT('Ctrl Pts',(0.945112208319089,-21.03030703232,88.5597284904799));
#123808=CARTESIAN_POINT('Ctrl Pts',(0.521059356999088,-21.03030703232,88.6964223903801));
#123809=CARTESIAN_POINT('',(1.21025704777005,-22.7988943080295,90.3337993035096));
#123810=CARTESIAN_POINT('Ctrl Pts',(1.21023413007473,-22.798879208848,90.3337286710351));
#123811=CARTESIAN_POINT('Ctrl Pts',(1.51039343408459,-22.8242058549175,
90.2309309413167));
#123812=CARTESIAN_POINT('Ctrl Pts',(1.81144147252023,-22.8489329406032,
90.1251809362156));
#123813=CARTESIAN_POINT('Ctrl Pts',(2.11324772692397,-22.8729680300164,
90.0151018754575));
#123814=CARTESIAN_POINT('Ctrl Pts',(2.19524318765021,-22.8794979418431,
89.9851953272284));
#123815=CARTESIAN_POINT('Ctrl Pts',(2.27729447866082,-22.8859768914643,
89.9549690246212));
#123816=CARTESIAN_POINT('Ctrl Pts',(2.35939866739142,-22.8924032818193,
89.9243947585409));
#123817=CARTESIAN_POINT('Ctrl Pts',(2.61750826452643,-22.9126058202183,
89.8282789376222));
#123818=CARTESIAN_POINT('Ctrl Pts',(2.87614185551581,-22.9322881533364,
89.7287273974561));
#123819=CARTESIAN_POINT('Ctrl Pts',(3.13505901007745,-22.9514075662278,
89.6248336129083));
#123820=CARTESIAN_POINT('Ctrl Pts',(3.29875079872078,-22.9634951812772,
89.5591502113957));
#123821=CARTESIAN_POINT('Ctrl Pts',(3.46255562440981,-22.9753580097105,
89.4917304938924));
#123822=CARTESIAN_POINT('Ctrl Pts',(3.62640905193442,-22.9869873315234,
89.422335216172));
#123823=CARTESIAN_POINT('Ctrl Pts',(3.86411883991196,-23.0038585295461,
89.3216602592743));
#123824=CARTESIAN_POINT('Ctrl Pts',(4.10193181500926,-23.0202380107857,
89.216829570639));
#123825=CARTESIAN_POINT('Ctrl Pts',(4.33950678287984,-23.0361047359754,
89.1071648584239));
#123826=CARTESIAN_POINT('Ctrl Pts',(4.41586782947864,-23.0412045987785,
89.0719165649073));
#123827=CARTESIAN_POINT('Ctrl Pts',(4.49220414898786,-23.0462515375288,
89.0361685057209));
#123828=CARTESIAN_POINT('Ctrl Pts',(4.56850399330538,-23.0512449880405,
88.9998970643313));
#123829=CARTESIAN_POINT('Ctrl Pts',(4.62986114399214,-23.0552605125574,
88.9707290848305));
#123830=CARTESIAN_POINT('Ctrl Pts',(4.69120662481904,-23.0592406305492,
88.9412176853075));
#123831=CARTESIAN_POINT('Ctrl Pts',(4.75254164044052,-23.0631825590175,
88.9113475912022));
#123832=CARTESIAN_POINT('Ctrl Pts',(4.93441452521425,-23.0748713129018,
88.822775669791));
#123833=CARTESIAN_POINT('Ctrl Pts',(5.11619655591822,-23.0862237242864,
88.7310530645164));
#123834=CARTESIAN_POINT('Ctrl Pts',(5.29786541494919,-23.0971723853635,
88.6358318752671));
#123835=CARTESIAN_POINT('Ctrl Pts',(5.45867598089911,-23.1068639769416,
88.5515434979674));
#123836=CARTESIAN_POINT('Ctrl Pts',(5.61939791126611,-23.1162393502448,
88.4645135318602));
#123837=CARTESIAN_POINT('Ctrl Pts',(5.78000322652552,-23.1252563837044,
88.3744691485403));
#123838=CARTESIAN_POINT('Ctrl Pts',(5.93597595541102,-23.1340133249855,
88.2870220539998));
#123839=CARTESIAN_POINT('Ctrl Pts',(6.09183893182038,-23.1424323589763,
88.1967316702881));
#123840=CARTESIAN_POINT('Ctrl Pts',(6.2475397577679,-23.1504782711739,88.1033934457889));
#123841=CARTESIAN_POINT('Ctrl Pts',(6.41231567943124,-23.1589931431401,
88.004614959068));
#123842=CARTESIAN_POINT('Ctrl Pts',(6.57693499166336,-23.1670818041468,
87.9024144337999));
#123843=CARTESIAN_POINT('Ctrl Pts',(6.74135405556885,-23.1746592334894,
87.7965118526924));
#123844=CARTESIAN_POINT('Ctrl Pts',(6.76510788714164,-23.1757539543574,
87.7812119719183));
#123845=CARTESIAN_POINT('Ctrl Pts',(6.7888574945791,-23.1768380148025,87.7658347455952));
#123846=CARTESIAN_POINT('Ctrl Pts',(6.81260269912841,-23.1779111680061,
87.7503792501723));
#123847=CARTESIAN_POINT('Ctrl Pts',(6.90290661273152,-23.1819924103465,
87.691601414822));
#123848=CARTESIAN_POINT('Ctrl Pts',(6.99314705828,-23.1859158714207,87.6316918366667));
#123849=CARTESIAN_POINT('Ctrl Pts',(7.0833163338459,-23.189668226085,87.570615127344));
#123850=CARTESIAN_POINT('Ctrl Pts',(7.22231302199292,-23.1954525120052,
87.4764648719994));
#123851=CARTESIAN_POINT('Ctrl Pts',(7.36114570487625,-23.2008334359504,
87.3795376940918));
#123852=CARTESIAN_POINT('Ctrl Pts',(7.49978323223744,-23.2057581195249,
87.2796812183491));
#123853=CARTESIAN_POINT('Ctrl Pts',(7.56910199591804,-23.2082204613121,
87.2297529804777));
#123854=CARTESIAN_POINT('Ctrl Pts',(7.63837141634081,-23.2105683901063,
87.1790924778903));
#123855=CARTESIAN_POINT('Ctrl Pts',(7.70758513080529,-23.2127935346573,
87.1276801626053));
#123856=CARTESIAN_POINT('Ctrl Pts',(7.74219198803752,-23.2139061069327,
87.1019740049629));
#123857=CARTESIAN_POINT('Ctrl Pts',(7.7767849042651,-23.21498797025,87.0760798768848));
#123858=CARTESIAN_POINT('Ctrl Pts',(7.81136296286751,-23.2160379809069,
87.0499952636164));
#123859=CARTESIAN_POINT('Ctrl Pts',(7.81422474291771,-23.2161248828231,
87.0478364256456));
#123860=CARTESIAN_POINT('Ctrl Pts',(7.81708642119755,-23.2162115663482,
87.0456762829635));
#123861=CARTESIAN_POINT('Ctrl Pts',(7.81994799711031,-23.2162980310548,
87.0435148340046));
#123862=CARTESIAN_POINT('Ctrl Pts',(7.83437421723199,-23.2167339303383,
87.0326182024236));
#123863=CARTESIAN_POINT('Ctrl Pts',(7.84879783586087,-23.2171642683021,
87.0216883716409));
#123864=CARTESIAN_POINT('Ctrl Pts',(7.86321881976802,-23.2175889901186,
87.010725206942));
#123865=CARTESIAN_POINT('Ctrl Pts',(7.87185958035186,-23.2178434748025,
87.0041563013795));
#123866=CARTESIAN_POINT('Ctrl Pts',(7.88049939494386,-23.2180959434931,
86.9975754281851));
#123867=CARTESIAN_POINT('Ctrl Pts',(7.88913825598689,-23.2183463846371,
86.9909825578367));
#123868=CARTESIAN_POINT('Ctrl Pts',(7.89777711702992,-23.2185968257811,
86.9843896874883));
#123869=CARTESIAN_POINT('Ctrl Pts',(7.9080894630654,-23.2188930037954,86.976502007423));
#123870=CARTESIAN_POINT('Ctrl Pts',(7.91505197072149,-23.2190916136997,
86.9711679255529));
#123871=CARTESIAN_POINT('Ctrl Pts',(8.09134263270587,-23.2241204155669,
86.8361089970165));
#123872=CARTESIAN_POINT('Ctrl Pts',(8.26579962669912,-23.2285515297506,
86.6969431825184));
#123873=CARTESIAN_POINT('Ctrl Pts',(8.43834390340455,-23.2323917796661,
86.5535726536806));
#123874=CARTESIAN_POINT('Ctrl Pts',(8.54726618800008,-23.2348160199957,
86.4630669246999));
#123875=CARTESIAN_POINT('Ctrl Pts',(8.6554255322555,-23.2370047142792,86.3708849085284));
#123876=CARTESIAN_POINT('Ctrl Pts',(8.76279353307567,-23.2389586523644,
86.2769955028744));
#123877=CARTESIAN_POINT('Ctrl Pts',(8.93583566793336,-23.2421077621092,
86.1256764592974));
#123878=CARTESIAN_POINT('Ctrl Pts',(9.10682452799498,-23.2446473763279,
85.9699232692661));
#123879=CARTESIAN_POINT('Ctrl Pts',(9.27571672569409,-23.2465765880523,
85.8096667102436));
#123880=CARTESIAN_POINT('Ctrl Pts',(9.40440547155385,-23.2480465661845,
85.6875579575756));
#123881=CARTESIAN_POINT('Ctrl Pts',(9.53187611599803,-23.2491620555429,
85.5628340870123));
#123882=CARTESIAN_POINT('Ctrl Pts',(9.65809042986943,-23.249920494709,85.4354575360454));
#123883=CARTESIAN_POINT('Ctrl Pts',(9.82840053416643,-23.2509439115427,
85.2635791411569));
#123884=CARTESIAN_POINT('Ctrl Pts',(9.99642459708762,-23.2513174795469,
85.0868705066055));
#123885=CARTESIAN_POINT('Ctrl Pts',(10.1621489201754,-23.2510291393295,
84.9052620331361));
#123886=CARTESIAN_POINT('Ctrl Pts',(10.2548830078338,-23.2508677932669,
84.803639677501));
#123887=CARTESIAN_POINT('Ctrl Pts',(10.3468961194323,-23.2504990718905,
84.7004829782548));
#123888=CARTESIAN_POINT('Ctrl Pts',(10.4381787520344,-23.2499199044464,
84.5957795828485));
#123889=CARTESIAN_POINT('Ctrl Pts',(10.4661094651373,-23.2497426904544,
84.5637423769241));
#123890=CARTESIAN_POINT('Ctrl Pts',(10.4939715105974,-23.2495454018335,
84.5315609605594));
#123891=CARTESIAN_POINT('Ctrl Pts',(10.5217636141367,-23.24932841804,84.4992356500257));
#123892=CARTESIAN_POINT('Ctrl Pts',(10.6908907477392,-23.2480079765346,
84.3025219645837));
#123893=CARTESIAN_POINT('Ctrl Pts',(10.857429405005,-23.2459586353402,84.1004758835953));
#123894=CARTESIAN_POINT('Ctrl Pts',(11.0212005082572,-23.2432622574743,
83.8931696662918));
#123895=CARTESIAN_POINT('Ctrl Pts',(11.1316471341769,-23.2414438302207,
83.7533631205783));
#123896=CARTESIAN_POINT('Ctrl Pts',(11.2408345983813,-23.2393309822942,
83.6111650785467));
#123897=CARTESIAN_POINT('Ctrl Pts',(11.3487029438601,-23.2369477669547,
83.4666101713744));
#123898=CARTESIAN_POINT('Ctrl Pts',(11.509949909774,-23.2333852181743,83.2505223090267));
#123899=CARTESIAN_POINT('Ctrl Pts',(11.6682489825816,-23.2292184719187,
83.0291657532378));
#123900=CARTESIAN_POINT('Ctrl Pts',(11.8234719698744,-23.2245265773938,
82.8026310036824));
#123901=CARTESIAN_POINT('Ctrl Pts',(11.9273300939928,-23.2213872784251,
82.651058903784));
#123902=CARTESIAN_POINT('Ctrl Pts',(12.0298109606654,-23.2180128492973,
82.4971696001478));
#123903=CARTESIAN_POINT('Ctrl Pts',(12.1308752870379,-23.2144271256202,
82.3410032958163));
#123904=CARTESIAN_POINT('Ctrl Pts',(12.2858032080798,-23.2089303421886,
82.1016060551149));
#123905=CARTESIAN_POINT('Ctrl Pts',(12.4374015621889,-23.2029367897955,
81.8568558748265));
#123906=CARTESIAN_POINT('Ctrl Pts',(12.58557409216,-23.1965347740778,81.6068413665939));
#123907=CARTESIAN_POINT('Ctrl Pts',(12.5974439769964,-23.1960219179545,
81.5868130697111));
#123908=CARTESIAN_POINT('Ctrl Pts',(12.6092918820148,-23.1955064427389,
81.5667510169829));
#123909=CARTESIAN_POINT('Ctrl Pts',(12.6211177605568,-23.194988395035,81.5466552684072));
#123910=CARTESIAN_POINT('',(0.756578721069087,-21.00000000034,88.93560161898));
#123911=CARTESIAN_POINT('Origin',(0.756570553373981,-22.5000441054858,88.9355484040727));
#123912=CARTESIAN_POINT('',(9.42148081258226,-20.999999610319,83.7851764430462));
#123913=CARTESIAN_POINT('Ctrl Pts',(9.42147697938284,-21.000000000085,83.7851937308496));
#123914=CARTESIAN_POINT('Ctrl Pts',(9.27399191800444,-21.0000000000907,
83.9540227648115));
#123915=CARTESIAN_POINT('Ctrl Pts',(9.12456523022954,-20.9999999999873,
84.1177960831894));
#123916=CARTESIAN_POINT('Ctrl Pts',(8.97356867507927,-21.0000000000114,
84.2763877180128));
#123917=CARTESIAN_POINT('Ctrl Pts',(8.89529364447174,-21.000000000024,84.3585999582691));
#123918=CARTESIAN_POINT('Ctrl Pts',(8.81659690184896,-21.0000000000025,
84.4394205773969));
#123919=CARTESIAN_POINT('Ctrl Pts',(8.7375311505406,-20.9999999999974,84.518837464166));
#123920=CARTESIAN_POINT('Ctrl Pts',(8.73449110473416,-20.9999999999972,
84.5218910109873));
#123921=CARTESIAN_POINT('Ctrl Pts',(8.73145051346632,-20.9999999999971,
84.5249424830282));
#123922=CARTESIAN_POINT('Ctrl Pts',(8.72840938028159,-20.9999999999971,
84.5279918800666));
#123923=CARTESIAN_POINT('Ctrl Pts',(8.61933714481441,-20.9999999999971,
84.6373605040659));
#123924=CARTESIAN_POINT('Ctrl Pts',(8.5095545037636,-21.0000000000552,84.7440439198219));
#123925=CARTESIAN_POINT('Ctrl Pts',(8.39886090767497,-21.0000000000394,
84.8483541764564));
#123926=CARTESIAN_POINT('Ctrl Pts',(8.28809191854098,-21.0000000000236,
84.9527354784648));
#123927=CARTESIAN_POINT('Ctrl Pts',(8.17641056141695,-20.9999999999989,
85.0547405710911));
#123928=CARTESIAN_POINT('Ctrl Pts',(8.0635768694174,-20.9999999999973,85.1546476180281));
#123929=CARTESIAN_POINT('Ctrl Pts',(8.04652410682795,-20.9999999999971,
85.1697467530669));
#123930=CARTESIAN_POINT('Ctrl Pts',(8.02944495413355,-20.9999999999971,
85.184797899742));
#123931=CARTESIAN_POINT('Ctrl Pts',(8.01233850907909,-20.9999999999971,
85.1998019455117));
#123932=CARTESIAN_POINT('Ctrl Pts',(7.97871884199685,-20.9999999999971,
85.2292897217305));
#123933=CARTESIAN_POINT('Ctrl Pts',(7.94499438200283,-20.9999999999966,
85.2585958705356));
#123934=CARTESIAN_POINT('Ctrl Pts',(7.91115741286785,-20.9999999999976,
85.2877267368321));
#123935=CARTESIAN_POINT('Ctrl Pts',(7.79875923544382,-21.0000000000009,
85.3844923858313));
#123936=CARTESIAN_POINT('Ctrl Pts',(7.68512207258091,-21.0000000000743,
85.4793270732401));
#123937=CARTESIAN_POINT('Ctrl Pts',(7.56996387602843,-21.0000000001119,
85.5724644706683));
#123938=CARTESIAN_POINT('Ctrl Pts',(7.46879379250766,-21.000000000145,85.6542885922576));
#123939=CARTESIAN_POINT('Ctrl Pts',(7.36644918188812,-20.9999999999971,
85.7348021831151));
#123940=CARTESIAN_POINT('Ctrl Pts',(7.26271916490076,-20.9999999999971,
85.8141369321334));
#123941=CARTESIAN_POINT('Ctrl Pts',(7.18897059090721,-20.9999999999971,
85.8705412862264));
#123942=CARTESIAN_POINT('Ctrl Pts',(7.11453057722115,-21.0000000000856,
85.9263626033712));
#123943=CARTESIAN_POINT('Ctrl Pts',(7.03944495771895,-21.0000000000741,
85.9815486371181));
#123944=CARTESIAN_POINT('Ctrl Pts',(6.89893946022772,-21.0000000000526,
86.0848166287467));
#123945=CARTESIAN_POINT('Ctrl Pts',(6.75617114718754,-21.0000000000048,
86.1858577156669));
#123946=CARTESIAN_POINT('Ctrl Pts',(6.61149924495893,-21.0000000000084,
86.2844218120254));
#123947=CARTESIAN_POINT('Ctrl Pts',(6.56370101073671,-21.0000000000097,
86.3169864613531));
#123948=CARTESIAN_POINT('Ctrl Pts',(6.51569527322402,-20.9999999999971,
86.3492810398185));
#123949=CARTESIAN_POINT('Ctrl Pts',(6.46749581550409,-20.9999999999971,
86.3812974551033));
#123950=CARTESIAN_POINT('Ctrl Pts',(6.34746269045993,-20.9999999999971,
86.4610292728694));
#123951=CARTESIAN_POINT('Ctrl Pts',(6.22623198433834,-21.0000000001373,
86.5390531423975));
#123952=CARTESIAN_POINT('Ctrl Pts',(6.10431565800804,-21.0000000001907,
86.615112577885));
#123953=CARTESIAN_POINT('Ctrl Pts',(5.9818449747345,-21.0000000002444,86.6915178577514));
#123954=CARTESIAN_POINT('Ctrl Pts',(5.85868278370828,-21.0000000001471,
86.7659410902819));
#123955=CARTESIAN_POINT('Ctrl Pts',(5.73538690640595,-21.0000000000453,
86.838212150071));
#123956=CARTESIAN_POINT('Ctrl Pts',(5.70324379362019,-21.0000000000188,
86.8570531435963));
#123957=CARTESIAN_POINT('Ctrl Pts',(5.67109173256492,-20.9999999999971,
86.8757481081935));
#123958=CARTESIAN_POINT('Ctrl Pts',(5.63894088385909,-20.9999999999971,
86.8942945284283));
#123959=CARTESIAN_POINT('Ctrl Pts',(5.50244658861362,-20.9999999999971,
86.9730321251381));
#123960=CARTESIAN_POINT('Ctrl Pts',(5.36594890838618,-20.9999999999385,
87.0490545898275));
#123961=CARTESIAN_POINT('Ctrl Pts',(5.22930121456414,-21.0000000000313,
87.1227204573118));
#123962=CARTESIAN_POINT('Ctrl Pts',(5.19957341189603,-21.0000000000515,
87.1387465190088));
#123963=CARTESIAN_POINT('Ctrl Pts',(5.16983838021216,-21.0000000000804,
87.1546608986856));
#123964=CARTESIAN_POINT('Ctrl Pts',(5.14009440103752,-21.0000000001088,
87.1704670447945));
#123965=CARTESIAN_POINT('Ctrl Pts',(5.02785242631964,-21.0000000002158,
87.2301131681836));
#123966=CARTESIAN_POINT('Ctrl Pts',(4.91548405719906,-20.9999999999971,
87.2882194114902));
#123967=CARTESIAN_POINT('Ctrl Pts',(4.80288878060909,-20.9999999999971,
87.3449847521551));
#123968=CARTESIAN_POINT('Ctrl Pts',(4.70564380844993,-20.9999999999971,
87.3940111779496));
#123969=CARTESIAN_POINT('Ctrl Pts',(4.60821980374707,-21.0000000005356,
87.4420125406706));
#123970=CARTESIAN_POINT('Ctrl Pts',(4.50998723134151,-21.0000000008011,
87.4893476966616));
#123971=CARTESIAN_POINT('Ctrl Pts',(4.40901116245255,-21.000000001074,87.5380048564524));
#123972=CARTESIAN_POINT('Ctrl Pts',(4.30718057840428,-21.0000000010355,
87.5859579974302));
#123973=CARTESIAN_POINT('Ctrl Pts',(4.20378538799987,-21.0000000007123,
87.6335491764987));
#123974=CARTESIAN_POINT('Ctrl Pts',(4.19363316767935,-21.0000000006805,
87.6382220837522));
#123975=CARTESIAN_POINT('Ctrl Pts',(4.18346584369122,-21.0000000006469,
87.6428914648658));
#123976=CARTESIAN_POINT('Ctrl Pts',(4.17328273148044,-21.0000000006121,
87.647557620073));
#123977=CARTESIAN_POINT('Ctrl Pts',(4.09799686416734,-21.0000000003543,
87.682055476379));
#123978=CARTESIAN_POINT('Ctrl Pts',(4.02184851305395,-20.9999999999971,
87.7163779316246));
#123979=CARTESIAN_POINT('Ctrl Pts',(3.94455679822576,-20.9999999999971,
87.7506447831067));
#123980=CARTESIAN_POINT('Ctrl Pts',(3.72588698588882,-20.9999999999971,
87.8475908270601));
#123981=CARTESIAN_POINT('Ctrl Pts',(3.49813393978502,-21.0000000001597,
87.9441897501269));
#123982=CARTESIAN_POINT('Ctrl Pts',(3.25999551214122,-21.000000000035,88.0406735965696));
#123983=CARTESIAN_POINT('Ctrl Pts',(3.20802281016991,-21.0000000000077,
88.0617307869014));
#123984=CARTESIAN_POINT('Ctrl Pts',(3.15555560316831,-20.9999999999999,
88.0827825845688));
#123985=CARTESIAN_POINT('Ctrl Pts',(3.10258068301365,-20.9999999999979,
88.1038316430887));
#123986=CARTESIAN_POINT('Ctrl Pts',(3.0677194107392,-20.9999999999966,88.117683423479));
#123987=CARTESIAN_POINT('Ctrl Pts',(3.03263827309266,-20.9999999999971,
88.1315340188204));
#123988=CARTESIAN_POINT('Ctrl Pts',(2.99733338629909,-20.9999999999971,
88.1453845195516));
#123989=CARTESIAN_POINT('Ctrl Pts',(2.84718752884044,-20.9999999999971,
88.2042884135275));
#123990=CARTESIAN_POINT('Ctrl Pts',(2.6930013806397,-21.0000000000004,88.2632001191942));
#123991=CARTESIAN_POINT('Ctrl Pts',(2.53487949972314,-21.0000000000036,
88.3221003830513));
#123992=CARTESIAN_POINT('Ctrl Pts',(2.37929265912228,-21.0000000000068,
88.3800563465837));
#123993=CARTESIAN_POINT('Ctrl Pts',(2.21989523490024,-21.0000000000046,
88.4380011683893));
#123994=CARTESIAN_POINT('Ctrl Pts',(2.05680785367107,-20.9999999999995,
88.4959626190292));
#123995=CARTESIAN_POINT('Ctrl Pts',(2.01608671892802,-20.9999999999982,
88.5104349590939));
#123996=CARTESIAN_POINT('Ctrl Pts',(1.97513564045399,-20.9999999999971,
88.5249085661768));
#123997=CARTESIAN_POINT('Ctrl Pts',(1.93395670865826,-20.9999999999971,
88.5393843373408));
#123998=CARTESIAN_POINT('Ctrl Pts',(1.91643441811195,-20.9999999999971,
88.5455440082491));
#123999=CARTESIAN_POINT('Ctrl Pts',(1.89887083619214,-20.9999999999973,
88.5517040899185));
#124000=CARTESIAN_POINT('Ctrl Pts',(1.88126597856944,-20.9999999999978,
88.5578647064176));
#124001=CARTESIAN_POINT('Ctrl Pts',(1.71400566050106,-21.0000000000031,
88.6163955220154));
#124002=CARTESIAN_POINT('Ctrl Pts',(1.54301816142452,-21.000000000055,88.6749706246985));
#124003=CARTESIAN_POINT('Ctrl Pts',(1.36830996496456,-21.0000000001698,
88.7337291107176));
#124004=CARTESIAN_POINT('Ctrl Pts',(1.19842766148794,-21.0000000002815,
88.7908645351338));
#124005=CARTESIAN_POINT('Ctrl Pts',(1.0250273328815,-21.0000000004429,88.8481732337227));
#124006=CARTESIAN_POINT('Ctrl Pts',(0.848131604814033,-21.0000000004876,
88.9058299251113));
#124007=CARTESIAN_POINT('Ctrl Pts',(0.81771720783072,-21.0000000004953,
88.915743072929));
#124008=CARTESIAN_POINT('Ctrl Pts',(0.787199523968459,-21.0000000004994,
88.9256666252834));
#124009=CARTESIAN_POINT('Ctrl Pts',(0.756578721069087,-21.0000000004994,
88.93560161898));
#124010=CARTESIAN_POINT('Ctrl Pts',(9.42148468716754,-20.9999998370474,
83.7851849075908));
#124011=CARTESIAN_POINT('Ctrl Pts',(9.4941219370757,-20.9999987247078,83.7542551887972));
#124012=CARTESIAN_POINT('Ctrl Pts',(9.56349342993131,-21.0011753932936,
83.7247364896096));
#124013=CARTESIAN_POINT('Ctrl Pts',(9.62942675509781,-21.0033031504389,
83.6966742681167));
#124014=CARTESIAN_POINT('Ctrl Pts',(9.70159869602387,-21.0056322361116,
83.6659567972971));
#124015=CARTESIAN_POINT('Ctrl Pts',(9.76965086116896,-21.0091004632847,
83.6369844447678));
#124016=CARTESIAN_POINT('Ctrl Pts',(9.83339225163773,-21.0133592125468,
83.6097967955185));
#124017=CARTESIAN_POINT('Ctrl Pts',(9.86821381453554,-21.0156857433019,
83.5949443357366));
#124018=CARTESIAN_POINT('Ctrl Pts',(9.9017494968727,-21.0182473659859,83.5806241620194));
#124019=CARTESIAN_POINT('Ctrl Pts',(9.93397208322834,-21.0209827456319,
83.5668406521577));
#124020=CARTESIAN_POINT('Ctrl Pts',(10.0012249953719,-21.0266918542982,
83.5380725958777));
#124021=CARTESIAN_POINT('Ctrl Pts',(10.0627624804275,-21.0331595220266,
83.5116677566652));
#124022=CARTESIAN_POINT('Ctrl Pts',(10.118432381711,-21.0398462117802,83.4877507581234));
#124023=CARTESIAN_POINT('Ctrl Pts',(10.1228137575912,-21.0403724728392,
83.4858684238975));
#124024=CARTESIAN_POINT('Ctrl Pts',(10.1271587990794,-21.0409000994819,
83.4840014909435));
#124025=CARTESIAN_POINT('Ctrl Pts',(10.1314674224592,-21.041428840755,83.4821500212401));
#124026=CARTESIAN_POINT('Ctrl Pts',(10.1609944869985,-21.045052313108,83.4694618699199));
#124027=CARTESIAN_POINT('Ctrl Pts',(10.1888130136579,-21.0487283218401,
83.4575006696735));
#124028=CARTESIAN_POINT('Ctrl Pts',(10.2149085149073,-21.0523803329437,
83.4462874670011));
#124029=CARTESIAN_POINT('Ctrl Pts',(10.227956265532,-21.0542063384956,83.4406808656649));
#124030=CARTESIAN_POINT('Ctrl Pts',(10.2405732483423,-21.0560263866187,
83.4352612547228));
#124031=CARTESIAN_POINT('Ctrl Pts',(10.2527582877196,-21.0578314278658,
83.4300313071825));
#124032=CARTESIAN_POINT('Ctrl Pts',(10.2588508074083,-21.0587339484893,
83.4274163334123));
#124033=CARTESIAN_POINT('Ctrl Pts',(10.2648353402489,-21.0596327218206,
83.4248487747094));
#124034=CARTESIAN_POINT('Ctrl Pts',(10.2707117489126,-21.0605266486678,
83.4223289593342));
#124035=CARTESIAN_POINT('Ctrl Pts',(10.2736499532444,-21.0609736120914,
83.4210690516466));
#124036=CARTESIAN_POINT('Ctrl Pts',(10.2765611264585,-21.0614193642047,
83.4198210797331));
#124037=CARTESIAN_POINT('Ctrl Pts',(10.2794452533187,-21.0618637701409,
83.4185850844988));
#124038=CARTESIAN_POINT('Ctrl Pts',(10.2823293801789,-21.0623081760772,
83.4173490892646));
#124039=CARTESIAN_POINT('Ctrl Pts',(10.2836807391676,-21.0625162915106,
83.4167699199381));
#124040=CARTESIAN_POINT('Ctrl Pts',(10.2880164799651,-21.063192816072,83.4149130695255));
#124041=CARTESIAN_POINT('Ctrl Pts',(10.3573883327262,-21.0740172090535,
83.3852034629241));
#124042=CARTESIAN_POINT('Ctrl Pts',(10.4244790085951,-21.0860937750086,
83.356489243626));
#124043=CARTESIAN_POINT('Ctrl Pts',(10.4891589927194,-21.0992619090558,
83.3288037272593));
#124044=CARTESIAN_POINT('Ctrl Pts',(10.5538389768437,-21.1124300431029,
83.3011182108926));
#124045=CARTESIAN_POINT('Ctrl Pts',(10.6161083609051,-21.126689375742,83.2744613038628));
#124046=CARTESIAN_POINT('Ctrl Pts',(10.6758773896147,-21.1418390982324,
83.2488498686012));
#124047=CARTESIAN_POINT('Ctrl Pts',(10.6944286648869,-21.146541310704,83.240900520989));
#124048=CARTESIAN_POINT('Ctrl Pts',(10.7127383054214,-21.1513290015203,
83.2330530884892));
#124049=CARTESIAN_POINT('Ctrl Pts',(10.7308053753453,-21.1561961057732,
83.2253085040455));
#124050=CARTESIAN_POINT('Ctrl Pts',(10.7709473075054,-21.1670099770626,
83.2081013650542));
#124051=CARTESIAN_POINT('Ctrl Pts',(10.8098908809428,-21.1782162765483,
83.191402349222));
#124052=CARTESIAN_POINT('Ctrl Pts',(10.8476102714308,-21.1897492289399,
83.1752272556387));
#124053=CARTESIAN_POINT('Ctrl Pts',(10.8749583331879,-21.1981110791757,
83.1634996679836));
#124054=CARTESIAN_POINT('Ctrl Pts',(10.9016637920612,-21.2066447958269,
83.1520473918412));
#124055=CARTESIAN_POINT('Ctrl Pts',(10.9277205287919,-21.2153245551945,
83.1408772706061));
#124056=CARTESIAN_POINT('Ctrl Pts',(10.9407488971573,-21.2196644348783,
83.1352922099885));
#124057=CARTESIAN_POINT('Ctrl Pts',(10.9536150958344,-21.2240407993215,
83.129777696196));
#124058=CARTESIAN_POINT('Ctrl Pts',(10.9663185903961,-21.2284503766631,
83.1243346726393));
#124059=CARTESIAN_POINT('Ctrl Pts',(10.9757077232876,-21.2317094883551,
83.1203117424717));
#124060=CARTESIAN_POINT('Ctrl Pts',(10.9844456080701,-21.2347871993304,
83.1165686325483));
#124061=CARTESIAN_POINT('Ctrl Pts',(10.9937795634143,-21.2381236045094,
83.1125716339291));
#124062=CARTESIAN_POINT('Ctrl Pts',(10.9970744474234,-21.2393013547414,
83.1111606943703));
#124063=CARTESIAN_POINT('Ctrl Pts',(11.000443387423,-21.2405117232215,83.1097182138103));
#124064=CARTESIAN_POINT('Ctrl Pts',(11.0039404737775,-21.2417753992659,
83.1082210540086));
#124065=CARTESIAN_POINT('Ctrl Pts',(11.0631942380401,-21.2631868128966,
83.082853549476));
#124066=CARTESIAN_POINT('Ctrl Pts',(11.1203932699226,-21.2859004072948,
83.0584395184106));
#124067=CARTESIAN_POINT('Ctrl Pts',(11.1754531134644,-21.3098087790778,
83.0349755843049));
#124068=CARTESIAN_POINT('Ctrl Pts',(11.1976469963221,-21.3194459223848,
83.0255175878519));
#124069=CARTESIAN_POINT('Ctrl Pts',(11.2194937986439,-21.3292768923882,
83.0162137952532));
#124070=CARTESIAN_POINT('Ctrl Pts',(11.2409899698962,-21.3392935161446,
83.0070633299919));
#124071=CARTESIAN_POINT('Ctrl Pts',(11.2895857629332,-21.3619378172754,
82.9863771291417));
#124072=CARTESIAN_POINT('Ctrl Pts',(11.3363860415459,-21.3855316806876,
82.9664757873883));
#124073=CARTESIAN_POINT('Ctrl Pts',(11.3812882123752,-21.4099625974059,
82.9473763273766));
#124074=CARTESIAN_POINT('Ctrl Pts',(11.4271082844229,-21.4348929369317,
82.9278864315065));
#124075=CARTESIAN_POINT('Ctrl Pts',(11.4709518791844,-21.4606946924684,
82.9092315100768));
#124076=CARTESIAN_POINT('Ctrl Pts',(11.5127604257083,-21.4872375191448,
82.8914122362505));
#124077=CARTESIAN_POINT('Ctrl Pts',(11.5296285630557,-21.4979465268285,
82.8842228459624));
#124078=CARTESIAN_POINT('Ctrl Pts',(11.5461659945948,-21.5087760641745,
82.8771692907715));
#124079=CARTESIAN_POINT('Ctrl Pts',(11.5623710988165,-21.5197172131263,
82.8702508527974));
#124080=CARTESIAN_POINT('Ctrl Pts',(11.5907328843161,-21.5388661501183,
82.8581423682649));
#124081=CARTESIAN_POINT('Ctrl Pts',(11.6180670866337,-21.5583481139389,
82.8464481889862));
#124082=CARTESIAN_POINT('Ctrl Pts',(11.6443762493541,-21.5781278394007,
82.8351789009517));
#124083=CARTESIAN_POINT('Ctrl Pts',(11.6824031463224,-21.6067171787951,
82.818890429154));
#124084=CARTESIAN_POINT('Ctrl Pts',(11.7182857209953,-21.6359274631247,
82.803491035106));
#124085=CARTESIAN_POINT('Ctrl Pts',(11.7519727657735,-21.6655985418644,
82.7890322234246));
#124086=CARTESIAN_POINT('Ctrl Pts',(11.7875315792775,-21.6969182483662,
82.7737700301556));
#124087=CARTESIAN_POINT('Ctrl Pts',(11.8206442207179,-21.7287515826067,
82.7595557971992));
#124088=CARTESIAN_POINT('Ctrl Pts',(11.8513026624327,-21.7609228338839,
82.7464223763073));
#124089=CARTESIAN_POINT('Ctrl Pts',(11.881683577325,-21.7928028640605,82.7334078419721));
#124090=CARTESIAN_POINT('Ctrl Pts',(11.9096550578661,-21.825015029524,82.7214543109823));
#124091=CARTESIAN_POINT('Ctrl Pts',(11.9352533773051,-21.8573962950116,
82.7105706050017));
#124092=CARTESIAN_POINT('Ctrl Pts',(11.9357484417354,-21.8580225397456,
82.710360117133));
#124093=CARTESIAN_POINT('Ctrl Pts',(11.9362426197884,-21.8586488478941,
82.7101500287686));
#124094=CARTESIAN_POINT('Ctrl Pts',(11.9367359116729,-21.8592752175941,
82.7099403399791));
#124095=CARTESIAN_POINT('Origin',(-6.52065461870091,-20.,86.59621775143));
#124096=CARTESIAN_POINT('',(-5.93853418689289,-20.99999960112,86.4935742132807));
#124097=CARTESIAN_POINT('',(-6.11218254686295,-20.0000000000124,85.5087654262472));
#124098=CARTESIAN_POINT('Origin',(-5.93853418689091,-20.,86.49357421328));
#124099=CARTESIAN_POINT('',(9.24780733902467,-20.0000000000007,82.8003857150944));
#124100=CARTESIAN_POINT('',(-6.11218263803291,-20.00000000001,85.50876490924));
#124101=CARTESIAN_POINT('Origin',(9.42145554646909,-19.99999972872,83.78519359989));
#124102=CARTESIAN_POINT('',(-5.93853418689091,-20.99999920224,86.49357421328));
#124103=CARTESIAN_POINT('Ctrl Pts',(9.31777244213909,-20.94531685512,84.14178879308));
#124104=CARTESIAN_POINT('Ctrl Pts',(9.36640017655909,-20.94770345583,84.1219806875601));
#124105=CARTESIAN_POINT('Ctrl Pts',(9.65757640544909,-20.96509256254,84.00275491356));
#124106=CARTESIAN_POINT('Ctrl Pts',(10.1549539983791,-21.02844485154,83.7926499217099));
#124107=CARTESIAN_POINT('Ctrl Pts',(10.7546658021091,-21.18754199612,83.5266079797999));
#124108=CARTESIAN_POINT('Ctrl Pts',(11.2403353151791,-21.40098020438,83.30037335394));
#124109=CARTESIAN_POINT('Ctrl Pts',(11.6099495725991,-21.65243696673,83.11889690529));
#124110=CARTESIAN_POINT('Ctrl Pts',(11.8190595633691,-21.87547143775,83.0102334421199));
#124111=CARTESIAN_POINT('Ctrl Pts',(11.9040610043191,-22.00823653322,82.964473853835));
#124112=CARTESIAN_POINT('Ctrl Pts',(11.9241977534391,-22.04372273473,82.9535566484859));
#124113=CARTESIAN_POINT('Ctrl Pts',(9.17645376799909,-21.25096624947,83.2879897269701));
#124114=CARTESIAN_POINT('Ctrl Pts',(9.22142272969909,-21.24328720155,83.2651886209901));
#124115=CARTESIAN_POINT('Ctrl Pts',(9.49214864496909,-21.19958401021,83.12878887307));
#124116=CARTESIAN_POINT('Ctrl Pts',(9.97085285597909,-21.15021821319,82.897289550365));
#124117=CARTESIAN_POINT('Ctrl Pts',(10.5934314779391,-21.16468088244,82.619908795121));
#124118=CARTESIAN_POINT('Ctrl Pts',(11.1469282254291,-21.2664360337,82.394534196853));
#124119=CARTESIAN_POINT('Ctrl Pts',(11.6180848277091,-21.4560997606,82.2199954501849));
#124120=CARTESIAN_POINT('Ctrl Pts',(11.9207663248691,-21.68120338254,82.117675714632));
#124121=CARTESIAN_POINT('Ctrl Pts',(12.0537280986091,-21.83843148824,82.074956833363));
#124122=CARTESIAN_POINT('Ctrl Pts',(12.0857902240491,-21.88190130568,82.0647465697241));
#124123=CARTESIAN_POINT('Ctrl Pts',(9.04133139198908,-20.62712475778,82.628500914342));
#124124=CARTESIAN_POINT('Ctrl Pts',(9.0929323218291,-20.61138663654,82.6119687700661));
#124125=CARTESIAN_POINT('Ctrl Pts',(9.40552780613909,-20.52047148252,82.5136949694449));
#124126=CARTESIAN_POINT('Ctrl Pts',(9.97906646707909,-20.40232051245,82.353473063821));
#124127=CARTESIAN_POINT('Ctrl Pts',(10.7708010393391,-20.37411518934,82.1731360077631));
#124128=CARTESIAN_POINT('Ctrl Pts',(11.5138296365191,-20.49600614651,82.034557857099));
#124129=CARTESIAN_POINT('Ctrl Pts',(12.1780168724191,-20.77496047938,81.932042963468));
#124130=CARTESIAN_POINT('Ctrl Pts',(12.6233299940891,-21.13270407263,81.8735317226859));
#124131=CARTESIAN_POINT('Ctrl Pts',(12.8231734110491,-21.39071629538,81.8493699294251));
#124132=CARTESIAN_POINT('Ctrl Pts',(12.8715846172591,-21.46248197016,81.84356917358));
#124133=CARTESIAN_POINT('Ctrl Pts',(9.05705447055909,-19.74161771142,82.869308315871));
#124134=CARTESIAN_POINT('Ctrl Pts',(9.11847855545909,-19.7284543691,82.8615961416661));
#124135=CARTESIAN_POINT('Ctrl Pts',(9.49044191549909,-19.65474822197,82.815934198766));
#124136=CARTESIAN_POINT('Ctrl Pts',(10.1708021213091,-19.58537985194,82.743358638735));
#124137=CARTESIAN_POINT('Ctrl Pts',(11.0968995137491,-19.66214931145,82.6645620454749));
#124138=CARTESIAN_POINT('Ctrl Pts',(11.9482698149491,-19.91443945991,82.605800745851));
#124139=CARTESIAN_POINT('Ctrl Pts',(12.6903357471891,-20.33818201501,82.563293973608));
#124140=CARTESIAN_POINT('Ctrl Pts',(13.1746527682191,-20.81714466972,82.539158789408));
#124141=CARTESIAN_POINT('Ctrl Pts',(13.3887020165791,-21.14437223204,82.529205012765));
#124142=CARTESIAN_POINT('Ctrl Pts',(13.4403842380291,-21.23445515355,82.526795931394));
#124143=CARTESIAN_POINT('Ctrl Pts',(9.2478073367568,-19.9999999999995,82.8003857022309));
#124144=CARTESIAN_POINT('Ctrl Pts',(9.44746232363843,-19.9999947893509,
82.7651858109517));
#124145=CARTESIAN_POINT('Ctrl Pts',(9.63275874640372,-20.0102049333749,
82.732512666375));
#124146=CARTESIAN_POINT('Ctrl Pts',(9.8878093209807,-20.0353935839062,82.6875380030807));
#124147=CARTESIAN_POINT('Ctrl Pts',(9.96902609894511,-20.0454254995066,
82.6732164866477));
#124148=CARTESIAN_POINT('Ctrl Pts',(10.0850995196626,-20.0622046672562,
82.6527499742875));
#124149=CARTESIAN_POINT('Ctrl Pts',(10.1228331636278,-20.0680856223673,
82.6460969388893));
#124150=CARTESIAN_POINT('Ctrl Pts',(10.1779943238935,-20.0772527547499,
82.6363715837551));
#124151=CARTESIAN_POINT('Ctrl Pts',(10.1961413085924,-20.0803664121402,
82.6331721758484));
#124152=CARTESIAN_POINT('Ctrl Pts',(10.2319541510883,-20.0866967255136,
82.6268581999328));
#124153=CARTESIAN_POINT('Ctrl Pts',(10.2510600419059,-20.0901829259522,
82.6234897459459));
#124154=CARTESIAN_POINT('Ctrl Pts',(10.3949250479738,-20.1171116810494,
82.59812551849));
#124155=CARTESIAN_POINT('Ctrl Pts',(10.5440152508577,-20.149477090711,82.5718364035666));
#124156=CARTESIAN_POINT('Ctrl Pts',(10.7965591891663,-20.2221388834674,
82.5272998102366));
#124157=CARTESIAN_POINT('Ctrl Pts',(10.8855418190081,-20.2504210618513,
82.5116080062251));
#124158=CARTESIAN_POINT('Ctrl Pts',(11.0254757509608,-20.3008841383642,
82.4869377685761));
#124159=CARTESIAN_POINT('Ctrl Pts',(11.0731867261691,-20.319054786091,82.4785267513243));
#124160=CARTESIAN_POINT('Ctrl Pts',(11.146183705256,-20.348647486402,82.4656568172526));
#124161=CARTESIAN_POINT('Ctrl Pts',(11.1830392891995,-20.3640284868325,
82.4591586062959));
#124162=CARTESIAN_POINT('Ctrl Pts',(11.226619501312,-20.3830693031182,82.4514740645984));
#124163=CARTESIAN_POINT('Ctrl Pts',(11.2454164624666,-20.3914727212221,
82.4481594349195));
#124164=CARTESIAN_POINT('Ctrl Pts',(11.2579738094765,-20.3971299277008,
82.4459450591596));
#124165=CARTESIAN_POINT('Ctrl Pts',(11.2657286922385,-20.4006553367271,
82.4445775325265));
#124166=CARTESIAN_POINT('Ctrl Pts',(11.3480297246391,-20.4383043456372,
82.4300640878185));
#124167=CARTESIAN_POINT('Ctrl Pts',(11.421888665082,-20.4753509528145,82.4170367346209));
#124168=CARTESIAN_POINT('Ctrl Pts',(11.5272732330714,-20.5327179132995,
82.3984528739781));
#124169=CARTESIAN_POINT('Ctrl Pts',(11.561502672334,-20.5521388404709,82.3924175625728));
#124170=CARTESIAN_POINT('Ctrl Pts',(11.6031750904849,-20.5767194020878,
82.3850720577672));
#124171=CARTESIAN_POINT('Ctrl Pts',(11.6123888516415,-20.58221902437,82.3834480849646));
#124172=CARTESIAN_POINT('Ctrl Pts',(11.6240309445655,-20.5892103236488,
82.3813961661963));
#124173=CARTESIAN_POINT('Ctrl Pts',(11.6419615202763,-20.6000380415341,
82.3782359971482));
#124174=CARTESIAN_POINT('Ctrl Pts',(11.6612775281911,-20.6119196074362,
82.3748318879259));
#124175=CARTESIAN_POINT('Ctrl Pts',(11.7017026635763,-20.6371825857324,
82.367707745307));
#124176=CARTESIAN_POINT('Ctrl Pts',(11.7310477696397,-20.6560203002695,
82.3625363705117));
#124177=CARTESIAN_POINT('Ctrl Pts',(11.7783737270488,-20.6877204153845,
82.354195088854));
#124178=CARTESIAN_POINT('Ctrl Pts',(11.7946994328715,-20.6988620468004,
82.3513174598515));
#124179=CARTESIAN_POINT('Ctrl Pts',(11.8283908526668,-20.7223825537064,
82.3453782383267));
#124180=CARTESIAN_POINT('Ctrl Pts',(11.8401311157668,-20.7307794729597,
82.3433083872193));
#124181=CARTESIAN_POINT('Ctrl Pts',(11.8792669632643,-20.759194418091,82.3364080799073));
#124182=CARTESIAN_POINT('Ctrl Pts',(11.9179182184663,-20.7883420314512,
82.3295918309551));
#124183=CARTESIAN_POINT('Ctrl Pts',(11.9620834760337,-20.8236468981876,
82.3218011143799));
#124184=CARTESIAN_POINT('Ctrl Pts',(11.9839243744912,-20.8416259125265,
82.3179480447014));
#124185=CARTESIAN_POINT('Ctrl Pts',(11.9932319197662,-20.8494013637813,
82.3163059961232));
#124186=CARTESIAN_POINT('Ctrl Pts',(11.9994250927753,-20.8546006075963,
82.3152133794341));
#124187=CARTESIAN_POINT('Ctrl Pts',(12.0039591773524,-20.8584317976343,
82.3144134551576));
#124188=CARTESIAN_POINT('Ctrl Pts',(12.0318603467978,-20.8820869136747,
82.3094909807558));
#124189=CARTESIAN_POINT('Ctrl Pts',(12.0824933910368,-20.9240074051633,
82.3005552708056));
#124190=CARTESIAN_POINT('Ctrl Pts',(12.1616638165423,-21.0000768353195,
82.2865925876594));
#124191=CARTESIAN_POINT('Ctrl Pts',(12.1707604794478,-21.0089379861606,
82.2849883614701));
#124192=CARTESIAN_POINT('Ctrl Pts',(12.1895177034974,-21.0275141712816,
82.2816805550659));
#124193=CARTESIAN_POINT('Ctrl Pts',(12.1938078445007,-21.0318455932408,
82.2809240187919));
#124194=CARTESIAN_POINT('Ctrl Pts',(12.2118934559253,-21.0501437800382,
82.2777347242169));
#124195=CARTESIAN_POINT('Ctrl Pts',(12.2236629025068,-21.0622900912216,
82.2756592661729));
#124196=CARTESIAN_POINT('Ctrl Pts',(12.2581217968457,-21.0985357629434,
82.2695825526892));
#124197=CARTESIAN_POINT('Ctrl Pts',(12.2809075638514,-21.1235159463043,
82.2655641269728));
#124198=CARTESIAN_POINT('Ctrl Pts',(12.3799394395816,-21.2359287811547,
82.2480979874625));
#124199=CARTESIAN_POINT('Ctrl Pts',(12.4526737390527,-21.3312614384013,
82.2352611547935));
#124200=CARTESIAN_POINT('Ctrl Pts',(12.5172257454391,-21.43204530223,82.22390472213));
#124201=CARTESIAN_POINT('Ctrl Pts',(10.7887201262991,-22.10443025328,82.17467014195));
#124202=CARTESIAN_POINT('Ctrl Pts',(10.8047337967191,-22.08320647671,82.173219921734));
#124203=CARTESIAN_POINT('Ctrl Pts',(11.0973679846591,-21.6977322454,82.146617864881));
#124204=CARTESIAN_POINT('Ctrl Pts',(11.6742414050491,-21.01672713982,82.090586401544));
#124205=CARTESIAN_POINT('Ctrl Pts',(12.5401712418891,-20.15025725843,81.996296778919));
#124206=CARTESIAN_POINT('Ctrl Pts',(13.3705524233291,-19.42440302238,81.897353491595));
#124207=CARTESIAN_POINT('Ctrl Pts',(14.1538154081591,-18.81497810678,81.7971741645661));
#124208=CARTESIAN_POINT('Ctrl Pts',(14.8829524524591,-18.30350003294,81.698540745942));
#124209=CARTESIAN_POINT('Ctrl Pts',(15.5555809773291,-17.87418996261,81.6034015345329));
#124210=CARTESIAN_POINT('Ctrl Pts',(16.1720623735391,-17.513706038,81.513033347234));
#124211=CARTESIAN_POINT('Ctrl Pts',(16.7343651483591,-17.21078913064,81.4281925355089));
#124212=CARTESIAN_POINT('Ctrl Pts',(17.2456693404391,-16.95583958766,81.349208818485));
#124213=CARTESIAN_POINT('Ctrl Pts',(17.6465406780691,-16.77007568858,81.2860730452739));
#124214=CARTESIAN_POINT('Ctrl Pts',(17.8774928558391,-16.66870970371,81.2492359042699));
#124215=CARTESIAN_POINT('Ctrl Pts',(17.9533920306691,-16.63600339584,81.237081512272));
#124216=CARTESIAN_POINT('Ctrl Pts',(11.5977514399991,-22.56749970211,82.742377900034));
#124217=CARTESIAN_POINT('Ctrl Pts',(11.6135348286791,-22.54809608191,82.73977119412));
#124218=CARTESIAN_POINT('Ctrl Pts',(11.9019007421091,-22.19570125639,82.692043649529));
#124219=CARTESIAN_POINT('Ctrl Pts',(12.4682941702191,-21.57382709283,82.59463865837));
#124220=CARTESIAN_POINT('Ctrl Pts',(13.3124318802591,-20.78368851256,82.4397023567349));
#124221=CARTESIAN_POINT('Ctrl Pts',(14.1165688943791,-20.12241917829,82.284501810265));
#124222=CARTESIAN_POINT('Ctrl Pts',(14.8705665392591,-19.56763806237,82.13324984309));
#124223=CARTESIAN_POINT('Ctrl Pts',(15.5687371062291,-19.10232611625,81.989006399952));
#124224=CARTESIAN_POINT('Ctrl Pts',(16.2097847874691,-18.71200397957,81.853549425408));
#124225=CARTESIAN_POINT('Ctrl Pts',(16.7949185413491,-18.38444768917,81.727752369711));
#124226=CARTESIAN_POINT('Ctrl Pts',(17.3267225057291,-18.10935418506,81.611888543045));
#124227=CARTESIAN_POINT('Ctrl Pts',(17.8087865331191,-17.87794738429,81.505773672536));
#124228=CARTESIAN_POINT('Ctrl Pts',(18.1857031536891,-17.70942521826,81.4221360479911));
#124229=CARTESIAN_POINT('Ctrl Pts',(18.4024472122491,-17.61750301323,81.373802591825));
#124230=CARTESIAN_POINT('Ctrl Pts',(18.4736338331591,-17.58784766122,81.357904139968));
#124231=CARTESIAN_POINT('Ctrl Pts',(12.4259640368191,-23.15463944465,82.3416426964909));
#124232=CARTESIAN_POINT('Ctrl Pts',(12.4401412767391,-23.13665861788,82.33780158716));
#124233=CARTESIAN_POINT('Ctrl Pts',(12.6992171930991,-22.80992651895,82.2675629739351));
#124234=CARTESIAN_POINT('Ctrl Pts',(13.2099574421591,-22.22741757786,82.127448594009));
#124235=CARTESIAN_POINT('Ctrl Pts',(13.9753360388591,-21.47531598229,81.913721537321));
#124236=CARTESIAN_POINT('Ctrl Pts',(14.7074100844491,-20.8373796579,81.707070463445));
#124237=CARTESIAN_POINT('Ctrl Pts',(15.3960509033691,-20.29596035334,81.511532543162));
#124238=CARTESIAN_POINT('Ctrl Pts',(16.0354203056491,-19.83722693452,81.329600240346));
#124239=CARTESIAN_POINT('Ctrl Pts',(16.6238567262691,-19.44888644012,81.162238962755));
#124240=CARTESIAN_POINT('Ctrl Pts',(17.1621028148391,-19.12021905677,81.0094715701341));
#124241=CARTESIAN_POINT('Ctrl Pts',(17.6522333898591,-18.84198037761,80.870794099851));
#124242=CARTESIAN_POINT('Ctrl Pts',(18.0973044970791,-18.60613730024,80.745333020243));
#124243=CARTESIAN_POINT('Ctrl Pts',(18.4458601500391,-18.43311625794,80.647472162088));
#124244=CARTESIAN_POINT('Ctrl Pts',(18.6465294124491,-18.33821558922,80.591313309216));
#124245=CARTESIAN_POINT('Ctrl Pts',(18.7124620135991,-18.30754110383,80.572882098526));
#124246=CARTESIAN_POINT('Ctrl Pts',(12.6103453412591,-23.3958239894,81.2932667992599));
#124247=CARTESIAN_POINT('Ctrl Pts',(12.6228263425391,-23.37772959822,81.289101551044));
#124248=CARTESIAN_POINT('Ctrl Pts',(12.8510381860091,-23.0486996543,81.212987170427));
#124249=CARTESIAN_POINT('Ctrl Pts',(13.3055043469091,-22.45427700608,81.063017870605));
#124250=CARTESIAN_POINT('Ctrl Pts',(13.9982062138891,-21.67146816858,80.839419997635));
#124251=CARTESIAN_POINT('Ctrl Pts',(14.6700873664091,-20.9969340879,80.627313039042));
#124252=CARTESIAN_POINT('Ctrl Pts',(15.3096002530191,-20.41689801836,80.4297282763071));
#124253=CARTESIAN_POINT('Ctrl Pts',(15.9094061513291,-19.91988918978,80.2481995028229));
#124254=CARTESIAN_POINT('Ctrl Pts',(16.4663180120191,-19.4949376737,80.082887870565));
#124255=CARTESIAN_POINT('Ctrl Pts',(16.9796715957291,-19.13200993825,79.933199351765));
#124256=CARTESIAN_POINT('Ctrl Pts',(17.4503151792491,-18.82217532617,79.798180712975));
#124257=CARTESIAN_POINT('Ctrl Pts',(17.8802547115591,-18.55746834489,79.676645672238));
#124258=CARTESIAN_POINT('Ctrl Pts',(18.2187470731791,-18.36180932168,79.582226384286));
#124259=CARTESIAN_POINT('Ctrl Pts',(18.4143432878591,-18.25389230802,79.52817755149));
#124260=CARTESIAN_POINT('Ctrl Pts',(18.4786864263191,-18.21894445124,79.510452443262));
#124261=CARTESIAN_POINT('',(15.1826284143117,-20.4790209964007,80.7654348671615));
#124262=CARTESIAN_POINT('',(13.3597754116033,-20.4707120255044,82.0753347888772));
#124263=CARTESIAN_POINT('Ctrl Pts',(15.1826281951692,-20.4790210042571,
80.7654347832022));
#124264=CARTESIAN_POINT('Ctrl Pts',(15.1191106435012,-20.4831595772132,
80.9316095253303));
#124265=CARTESIAN_POINT('Ctrl Pts',(15.0202333632624,-20.4881017533022,
81.0852214233996));
#124266=CARTESIAN_POINT('Ctrl Pts',(14.7692951009453,-20.496465001043,81.3804070169615));
#124267=CARTESIAN_POINT('Ctrl Pts',(14.6067129985061,-20.4996164325595,
81.5206692599665));
#124268=CARTESIAN_POINT('Ctrl Pts',(14.2708648919509,-20.5002922526295,
81.7486174057977));
#124269=CARTESIAN_POINT('Ctrl Pts',(14.0952875735918,-20.4982343136608,
81.8417267900461));
#124270=CARTESIAN_POINT('Ctrl Pts',(13.7352155159587,-20.4885488872977,
81.9876049764954));
#124271=CARTESIAN_POINT('Ctrl Pts',(13.5489239184334,-20.4809898307412,
82.041981658877));
#124272=CARTESIAN_POINT('Ctrl Pts',(13.359775386349,-20.470712025504,82.0753346456572));
#124273=CARTESIAN_POINT('Ctrl Pts',(12.6211112025166,-23.1949844434374,
81.546651511011));
#124274=CARTESIAN_POINT('Ctrl Pts',(12.7010796583489,-23.0859335125774,
81.5217614922825));
#124275=CARTESIAN_POINT('Ctrl Pts',(12.7873020478414,-22.9720163830221,
81.4948559993584));
#124276=CARTESIAN_POINT('Ctrl Pts',(12.8801975478467,-22.8535598950672,
81.4659316626286));
#124277=CARTESIAN_POINT('Ctrl Pts',(12.9693469700448,-22.7398802501308,
81.4381737205671));
#124278=CARTESIAN_POINT('Ctrl Pts',(13.0646433628694,-22.6220200826152,
81.4085560004937));
#124279=CARTESIAN_POINT('Ctrl Pts',(13.1664350211465,-22.5002998917991,
81.3770989552872));
#124280=CARTESIAN_POINT('Ctrl Pts',(13.2060171790742,-22.4529684316637,
81.3648667375164));
#124281=CARTESIAN_POINT('Ctrl Pts',(13.2465829275287,-22.4050546552067,
81.3523520386674));
#124282=CARTESIAN_POINT('Ctrl Pts',(13.2881527164378,-22.3565825378578,
81.3395481591552));
#124283=CARTESIAN_POINT('Ctrl Pts',(13.3557321339824,-22.2777821026487,
81.3187330734294));
#124284=CARTESIAN_POINT('Ctrl Pts',(13.4259653175262,-22.197505741631,81.2971535838656));
#124285=CARTESIAN_POINT('Ctrl Pts',(13.4989513338155,-22.115863929788,81.2747791284266));
#124286=CARTESIAN_POINT('Ctrl Pts',(13.5578921034289,-22.0499330642976,
81.256710357307));
#124287=CARTESIAN_POINT('Ctrl Pts',(13.6186279276438,-21.9831129698786,
81.2381219473619));
#124288=CARTESIAN_POINT('Ctrl Pts',(13.6812085868739,-21.9154695454829,
81.2189866650971));
#124289=CARTESIAN_POINT('Ctrl Pts',(13.712498916489,-21.881647833285,81.2094190239647));
#124290=CARTESIAN_POINT('Ctrl Pts',(13.7442504334845,-21.847620273801,81.1997146534683));
#124291=CARTESIAN_POINT('Ctrl Pts',(13.7764690753335,-21.8133956591303,
81.1898691502691));
#124292=CARTESIAN_POINT('Ctrl Pts',(13.7925783962579,-21.7962833517949,
81.1849463986695));
#124293=CARTESIAN_POINT('Ctrl Pts',(13.8088044961137,-21.7791217787972,
81.1799883628294));
#124294=CARTESIAN_POINT('Ctrl Pts',(13.8251480981321,-21.7619120485684,
81.1749944576721));
#124295=CARTESIAN_POINT('Ctrl Pts',(13.8333198991413,-21.7533071834539,
81.1724975050935));
#124296=CARTESIAN_POINT('Ctrl Pts',(13.8415210755324,-21.7446902788946,
81.1699915851153));
#124297=CARTESIAN_POINT('Ctrl Pts',(13.8497517162525,-21.7360614749796,
81.1674766209594));
#124298=CARTESIAN_POINT('Ctrl Pts',(13.8538670366125,-21.7317470730221,
81.1662191388814));
#124299=CARTESIAN_POINT('Ctrl Pts',(13.8579897230441,-21.7274296962161,
81.1649593957544));
#124300=CARTESIAN_POINT('Ctrl Pts',(13.8621197865673,-21.7231093621754,
81.1636973817387));
#124301=CARTESIAN_POINT('Ctrl Pts',(13.8662498500906,-21.7187890281346,
81.162435367723));
#124302=CARTESIAN_POINT('Ctrl Pts',(13.8718575245007,-21.7129311569294,
81.1607218127025));
#124303=CARTESIAN_POINT('Ctrl Pts',(13.8745321193775,-21.7101395059708,
81.1599045171018));
#124304=CARTESIAN_POINT('Ctrl Pts',(13.9127985873755,-21.6701982711336,
81.1482111514188));
#124305=CARTESIAN_POINT('Ctrl Pts',(13.9540072554889,-21.6275871585619,
81.1356238056198));
#124306=CARTESIAN_POINT('Ctrl Pts',(13.9982420814259,-21.5823867839551,
81.1221332886392));
#124307=CARTESIAN_POINT('Ctrl Pts',(14.0529431604893,-21.5264917010042,
81.1054508258889));
#124308=CARTESIAN_POINT('Ctrl Pts',(14.112271257553,-21.4666361954175,81.0873872566257));
#124309=CARTESIAN_POINT('Ctrl Pts',(14.1764050690305,-21.4029997983481,
81.0679228150623));
#124310=CARTESIAN_POINT('Ctrl Pts',(14.2344033461055,-21.3454513491875,
81.0503204919055));
#124311=CARTESIAN_POINT('Ctrl Pts',(14.2963323407058,-21.2848124726741,
81.0315700508687));
#124312=CARTESIAN_POINT('Ctrl Pts',(14.362335166225,-21.221246127599,81.0116327158677));
#124313=CARTESIAN_POINT('Ctrl Pts',(14.3953365789847,-21.1894629550614,
81.0016640483672));
#124314=CARTESIAN_POINT('Ctrl Pts',(14.4293565867576,-21.1569483381342,
80.9913983362014));
#124315=CARTESIAN_POINT('Ctrl Pts',(14.4644136947065,-21.1237252347141,
80.9808285409277));
#124316=CARTESIAN_POINT('Ctrl Pts',(14.4819422486809,-21.107113683004,80.9755436432908));
#124317=CARTESIAN_POINT('Ctrl Pts',(14.4997300874212,-21.0903250186968,
80.9701827288884));
#124318=CARTESIAN_POINT('Ctrl Pts',(14.5177795393016,-21.0733622970361,
80.9647447272958));
#124319=CARTESIAN_POINT('Ctrl Pts',(14.5268042652417,-21.0648809362057,
80.9620257264995));
#124320=CARTESIAN_POINT('Ctrl Pts',(14.5358943949757,-21.0563560614945,
80.9592874541226));
#124321=CARTESIAN_POINT('Ctrl Pts',(14.5450502210561,-21.0477880619624,
80.9565297708572));
#124322=CARTESIAN_POINT('Ctrl Pts',(14.5496281340964,-21.0435040621964,
80.9551509292245));
#124323=CARTESIAN_POINT('Ctrl Pts',(14.5542224712529,-21.0392092812524,
80.953767234882));
#124324=CARTESIAN_POINT('Ctrl Pts',(14.5588332691131,-21.0349037684304,
80.9523786696975));
#124325=CARTESIAN_POINT('Ctrl Pts',(14.5634440669733,-21.0305982556084,
80.9509901045129));
#124326=CARTESIAN_POINT('Ctrl Pts',(14.5671550748878,-21.0271357486057,
80.9498725694768));
#124327=CARTESIAN_POINT('Ctrl Pts',(14.5727150814534,-21.0219550838904,
80.9481983432867));
#124328=CARTESIAN_POINT('Ctrl Pts',(14.6124113807312,-20.9849671389,80.9362450149736));
#124329=CARTESIAN_POINT('Ctrl Pts',(14.6503266609049,-20.9499779898511,
80.9248393076686));
#124330=CARTESIAN_POINT('Ctrl Pts',(14.6864107610285,-20.9169365199115,
80.9139933493658));
#124331=CARTESIAN_POINT('Ctrl Pts',(14.7443878671627,-20.863848073672,80.8965669129716));
#124332=CARTESIAN_POINT('Ctrl Pts',(14.7976358817662,-20.8157860004258,
80.880585953442));
#124333=CARTESIAN_POINT('Ctrl Pts',(14.8459839415778,-20.7725674980799,
80.8660905655735));
#124334=CARTESIAN_POINT('Ctrl Pts',(14.8949868311436,-20.7287636410915,
80.8513988510827));
#124335=CARTESIAN_POINT('Ctrl Pts',(14.9389562888953,-20.6899353059313,
80.8382331285868));
#124336=CARTESIAN_POINT('Ctrl Pts',(14.977753356939,-20.655927835926,80.8266253191512));
#124337=CARTESIAN_POINT('Ctrl Pts',(15.0167645805568,-20.6217326484042,
80.8149534358764));
#124338=CARTESIAN_POINT('Ctrl Pts',(15.0505463171594,-20.5924116099799,
80.804856625578));
#124339=CARTESIAN_POINT('Ctrl Pts',(15.0789939351,-20.5678449536711,80.796358861458));
#124340=CARTESIAN_POINT('Ctrl Pts',(15.1076083817696,-20.5431342282155,
80.7878112628952));
#124341=CARTESIAN_POINT('Ctrl Pts',(15.1308260759889,-20.5232337366539,
80.78088145753));
#124342=CARTESIAN_POINT('Ctrl Pts',(15.1485754243984,-20.5080606018071,
80.7755864184812));
#124343=CARTESIAN_POINT('Ctrl Pts',(15.1641398050169,-20.4947552995232,
80.7709432056013));
#124344=CARTESIAN_POINT('Ctrl Pts',(15.1754998459937,-20.4850856751023,
80.7675569223367));
#124345=CARTESIAN_POINT('Ctrl Pts',(15.1826283063839,-20.4790208829906,
80.7654348287324));
#124346=CARTESIAN_POINT('Ctrl Pts',(12.5172248390746,-21.4320453024142,
82.2238995806392));
#124347=CARTESIAN_POINT('Ctrl Pts',(12.6294093254391,-21.2933908624356,
82.2041182404801));
#124348=CARTESIAN_POINT('Ctrl Pts',(12.7416585985438,-21.1594801400756,
82.1843245397865));
#124349=CARTESIAN_POINT('Ctrl Pts',(12.8535950144248,-21.0300306251832,
82.164587125004));
#124350=CARTESIAN_POINT('Ctrl Pts',(12.9612121273082,-20.9055761931985,
82.145611320053));
#124351=CARTESIAN_POINT('Ctrl Pts',(13.0685405940468,-20.785245355736,82.1266873294237));
#124352=CARTESIAN_POINT('Ctrl Pts',(13.175286560664,-20.6688012397128,82.1078652991768));
#124353=CARTESIAN_POINT('Ctrl Pts',(13.1820061662658,-20.6614711404209,
82.1066804617174));
#124354=CARTESIAN_POINT('Ctrl Pts',(13.1887234763875,-20.6541564475408,
82.1054960251714));
#124355=CARTESIAN_POINT('Ctrl Pts',(13.1954384320464,-20.6468571100375,
82.1043120005116));
#124356=CARTESIAN_POINT('Ctrl Pts',(13.2503880070708,-20.5871254432717,
82.0946229340191));
#124357=CARTESIAN_POINT('Ctrl Pts',(13.305175381437,-20.5284202730709,82.084962261829));
#124358=CARTESIAN_POINT('Ctrl Pts',(13.3597753863499,-20.4707120255048,
82.0753346456571));
#124359=CARTESIAN_POINT('Origin',(22.8854471965091,-9.5,80.840271512642));
#124360=CARTESIAN_POINT('',(21.1895064189391,-9.49999999533099,65.4633429305539));
#124361=CARTESIAN_POINT('',(20.0012895469927,-9.49999999792378,58.7246301887194));
#124362=CARTESIAN_POINT('',(24.2283495281091,-9.49999999533099,82.697478608263));
#124363=CARTESIAN_POINT('',(20.2047119979795,-8.50000000009162,65.6369887574203));
#124364=CARTESIAN_POINT('Origin',(20.2046986659336,-9.5,65.6369911082197));
#124365=CARTESIAN_POINT('',(19.0165457197942,-8.50000000044727,58.8982964289324));
#124366=CARTESIAN_POINT('Ctrl Pts',(20.2047119979795,-8.50000000009162,
65.6369887574203));
#124367=CARTESIAN_POINT('Ctrl Pts',(19.8086377232276,-8.50000000004136,
63.3907613048375));
#124368=CARTESIAN_POINT('Ctrl Pts',(19.4125634484756,-8.50000000001177,
61.1445338522548));
#124369=CARTESIAN_POINT('Ctrl Pts',(19.0165457198591,-8.5,58.89829642895));
#124370=CARTESIAN_POINT('Ctrl Pts',(20.0012895473071,-9.49999999792378,
58.7246301886641));
#124371=CARTESIAN_POINT('Ctrl Pts',(20.0012899795185,-9.46762591868316,
58.7246326402436));
#124372=CARTESIAN_POINT('Ctrl Pts',(19.9997391442553,-9.43457989065709,
58.7249081307818));
#124373=CARTESIAN_POINT('Ctrl Pts',(19.9964623697764,-9.40109896318049,
58.725487577709));
#124374=CARTESIAN_POINT('Ctrl Pts',(19.9932143516384,-9.36791185786638,
58.7260619395216));
#124375=CARTESIAN_POINT('Ctrl Pts',(19.9882701017658,-9.33429788673468,
58.7269350260154));
#124376=CARTESIAN_POINT('Ctrl Pts',(19.9814984743018,-9.3005197579655,58.728130076751));
#124377=CARTESIAN_POINT('Ctrl Pts',(19.9747974261233,-9.26709369171103,
58.7293126717177));
#124378=CARTESIAN_POINT('Ctrl Pts',(19.966306563625,-9.23350740803131,58.7308106127281));
#124379=CARTESIAN_POINT('Ctrl Pts',(19.9559429296749,-9.20003957605674,
58.7326386388117));
#124380=CARTESIAN_POINT('Ctrl Pts',(19.9488851771946,-9.17724760219227,
58.7338835453463));
#124381=CARTESIAN_POINT('Ctrl Pts',(19.9409598030488,-9.15451106970619,
58.7352813743508));
#124382=CARTESIAN_POINT('Ctrl Pts',(19.932153557986,-9.13192242870445,58.7368344972254));
#124383=CARTESIAN_POINT('Ctrl Pts',(19.9201566287579,-9.10114945730447,
58.738950348542));
#124384=CARTESIAN_POINT('Ctrl Pts',(19.9065243780912,-9.07065704605179,
58.7413544985239));
#124385=CARTESIAN_POINT('Ctrl Pts',(19.8912777345561,-9.04071403997275,
58.7440432534581));
#124386=CARTESIAN_POINT('Ctrl Pts',(19.8761507537896,-9.01100604056889,
58.7467109057897));
#124387=CARTESIAN_POINT('Ctrl Pts',(19.8594347467946,-8.98183953430048,
58.7496586911272));
#124388=CARTESIAN_POINT('Ctrl Pts',(19.8412003847823,-8.95346833657049,
58.7528741448684));
#124389=CARTESIAN_POINT('Ctrl Pts',(19.8227496569657,-8.92476049108652,
58.7561277526309));
#124390=CARTESIAN_POINT('Ctrl Pts',(19.8027444542824,-8.89686767177941,
58.7596553963031));
#124391=CARTESIAN_POINT('Ctrl Pts',(19.781307980834,-8.8700331238014,58.7634353481959));
#124392=CARTESIAN_POINT('Ctrl Pts',(19.7598715073857,-8.84319857582339,
58.7672153000887));
#124393=CARTESIAN_POINT('Ctrl Pts',(19.7370041494664,-8.81742294259417,
58.7712474920879));
#124394=CARTESIAN_POINT('Ctrl Pts',(19.7128747804019,-8.79291951777192,
58.7755021437878));
#124395=CARTESIAN_POINT('Ctrl Pts',(19.6888397304775,-8.76851187423399,
58.7797401645063));
#124396=CARTESIAN_POINT('Ctrl Pts',(19.6635614323748,-8.74537551707984,
58.7841973371116));
#124397=CARTESIAN_POINT('Ctrl Pts',(19.6372473957868,-8.72368004516574,
58.7888370761684));
#124398=CARTESIAN_POINT('Ctrl Pts',(19.61117460253,-8.70218347424117,58.7934342787599));
#124399=CARTESIAN_POINT('Ctrl Pts',(19.5840856193093,-8.68210179550079,
58.7982106020061));
#124400=CARTESIAN_POINT('Ctrl Pts',(19.5562104876184,-8.66355581926994,
58.8031254873951));
#124401=CARTESIAN_POINT('Ctrl Pts',(19.5279484762274,-8.64475244293768,
58.8081085866101));
#124402=CARTESIAN_POINT('Ctrl Pts',(19.4988789808644,-8.62752803875613,
58.813234008398));
#124403=CARTESIAN_POINT('Ctrl Pts',(19.4692613061491,-8.61195770978641,
58.8184560345373));
#124404=CARTESIAN_POINT('Ctrl Pts',(19.4396436314338,-8.59638738081669,
58.8236780606767));
#124405=CARTESIAN_POINT('Ctrl Pts',(19.409478491668,-8.58247119127859,58.8289965652168));
#124406=CARTESIAN_POINT('Ctrl Pts',(19.3790342951517,-8.57023085295102,
58.8343642247118));
#124407=CARTESIAN_POINT('Ctrl Pts',(19.3463554205598,-8.55709204401731,
58.8401258834697));
#124408=CARTESIAN_POINT('Ctrl Pts',(19.3133623206699,-8.54588566789205,
58.8459428927352));
#124409=CARTESIAN_POINT('Ctrl Pts',(19.2803417007415,-8.53656112194488,
58.8517651620618));
#124410=CARTESIAN_POINT('Ctrl Pts',(19.2471142663819,-8.5271781745906,58.8576238973702));
#124411=CARTESIAN_POINT('Ctrl Pts',(19.2138595521797,-8.51970040815207,
58.8634878555077));
#124412=CARTESIAN_POINT('Ctrl Pts',(19.1808509606665,-8.51402658730199,
58.8693093004204));
#124413=CARTESIAN_POINT('Ctrl Pts',(19.147412530532,-8.50827888182916,58.8752065523197));
#124414=CARTESIAN_POINT('Ctrl Pts',(19.1142272133837,-8.50438203527085,
58.8810600816113));
#124415=CARTESIAN_POINT('Ctrl Pts',(19.0815514632307,-8.50218500580683,
58.8868251594106));
#124416=CARTESIAN_POINT('Ctrl Pts',(19.0596311897744,-8.50071114563782,
58.8906926171205));
#124417=CARTESIAN_POINT('Ctrl Pts',(19.0379396363874,-8.50000130130795,
58.8945203748651));
#124418=CARTESIAN_POINT('Ctrl Pts',(19.016545719859,-8.50000000178909,58.89829642895));
#124419=CARTESIAN_POINT('Origin',(23.0888233837291,-10.,78.836701365196));
#124420=CARTESIAN_POINT('',(-3.18510217627065,-9.99999863269069,84.9926432467801));
#124421=CARTESIAN_POINT('',(-4.19326724970536,-8.5,83.6472700340011));
#124422=CARTESIAN_POINT('Ctrl Pts',(-3.18510142355444,-10.,84.9926431156534));
#124423=CARTESIAN_POINT('Ctrl Pts',(-3.28774654871392,-9.81347742952627,
85.0107420480117));
#124424=CARTESIAN_POINT('Ctrl Pts',(-3.40138324898531,-9.61104424048628,
84.9933696737421));
#124425=CARTESIAN_POINT('Ctrl Pts',(-3.6218722462137,-9.23231631838246,
84.8715546372826));
#124426=CARTESIAN_POINT('Ctrl Pts',(-3.72887381127769,-9.05615862658819,
84.7669564448341));
#124427=CARTESIAN_POINT('Ctrl Pts',(-3.90143678101031,-8.79358573018847,
84.5186556652058));
#124428=CARTESIAN_POINT('Ctrl Pts',(-3.98029199297708,-8.68400566943748,
84.3669625950309));
#124429=CARTESIAN_POINT('Ctrl Pts',(-4.10991781742065,-8.53714553683044,
84.0232533567387));
#124430=CARTESIAN_POINT('Ctrl Pts',(-4.16082961889395,-8.5,83.8312329798933));
#124431=CARTESIAN_POINT('Ctrl Pts',(-4.19326724970496,-8.5,83.6472700340034));
#124432=CARTESIAN_POINT('',(-6.54682286478236,-9.99999999999981,85.5854053073669));
#124433=CARTESIAN_POINT('',(-1.48527513867091,-9.99999794132199,84.6929178719));
#124434=CARTESIAN_POINT('',(-6.8072945644184,-8.50000000000003,84.1081934941563));
#124435=CARTESIAN_POINT('Origin',(-6.80729512863291,-10.,84.10819367738));
#124436=CARTESIAN_POINT('',(-2.24409325564091,-8.5,83.30357806876));
#124437=CARTESIAN_POINT('Ctrl Pts',(19.9312442464691,-9.83434173672299,
58.58808248603));
#124438=CARTESIAN_POINT('Ctrl Pts',(19.9318133015791,-9.83251988519099,
58.59130975793));
#124439=CARTESIAN_POINT('Ctrl Pts',(19.9372671952991,-9.81590682367799,
58.62224032621));
#124440=CARTESIAN_POINT('Ctrl Pts',(19.9474515848891,-9.79777453008298,
58.67999886974));
#124441=CARTESIAN_POINT('Ctrl Pts',(19.9576520930091,-9.79674919137799,
58.73784882602));
#124442=CARTESIAN_POINT('Ctrl Pts',(19.9616392603091,-9.79878222958499,
58.76046117542));
#124443=CARTESIAN_POINT('Ctrl Pts',(20.1262752009291,-9.06820471416898,
58.12191241983));
#124444=CARTESIAN_POINT('Ctrl Pts',(20.1286905848491,-9.06047995653799,
58.13561074275));
#124445=CARTESIAN_POINT('Ctrl Pts',(20.1516207901991,-8.99069547653899,
58.26565439945));
#124446=CARTESIAN_POINT('Ctrl Pts',(20.1910945955491,-8.92247834065099,
58.48952147411));
#124447=CARTESIAN_POINT('Ctrl Pts',(20.2290936722891,-8.91832092631999,
58.70502494718));
#124448=CARTESIAN_POINT('Ctrl Pts',(20.2440720102891,-8.926020544672,58.7899713231901));
#124449=CARTESIAN_POINT('Ctrl Pts',(19.4324748633591,-8.50077447479,57.9244548090799));
#124450=CARTESIAN_POINT('Ctrl Pts',(19.4362577086691,-8.48867780022699,
57.94590839094));
#124451=CARTESIAN_POINT('Ctrl Pts',(19.4721315355791,-8.37951254390298,
58.14935897332));
#124452=CARTESIAN_POINT('Ctrl Pts',(19.5332981970591,-8.27420066749899,
58.49625234851));
#124453=CARTESIAN_POINT('Ctrl Pts',(19.5918859517691,-8.267723518747,58.8285200166801));
#124454=CARTESIAN_POINT('Ctrl Pts',(19.6150047691491,-8.27962002203299,
58.95963334533));
#124455=CARTESIAN_POINT('Ctrl Pts',(18.5925509242691,-8.73948053367298,
58.2070864406));
#124456=CARTESIAN_POINT('Ctrl Pts',(18.5957585071091,-8.72922303331798,
58.22527754688));
#124457=CARTESIAN_POINT('Ctrl Pts',(18.6261872225791,-8.63662444767899,
58.3978473677));
#124458=CARTESIAN_POINT('Ctrl Pts',(18.6782281522391,-8.54691755440599,
58.69298614594));
#124459=CARTESIAN_POINT('Ctrl Pts',(18.7281546798291,-8.54141626950999,
58.97613355421));
#124460=CARTESIAN_POINT('Ctrl Pts',(18.7478489674291,-8.55154723089699,
59.08782540944));
#124461=CARTESIAN_POINT('',(19.0913785491043,-8.64603879443074,58.2486575231502));
#124462=CARTESIAN_POINT('Ctrl Pts',(19.0913788008791,-8.64603683958299,
58.24865662762));
#124463=CARTESIAN_POINT('Ctrl Pts',(19.0831160153987,-8.61192581016859,
58.3206480322238));
#124464=CARTESIAN_POINT('Ctrl Pts',(19.0729896736748,-8.57628931983382,
58.4100917669793));
#124465=CARTESIAN_POINT('Ctrl Pts',(19.04805521017,-8.52029418216068,58.6267491454393));
#124466=CARTESIAN_POINT('Ctrl Pts',(19.0331814385135,-8.4999991684141,58.7541918345667));
#124467=CARTESIAN_POINT('Ctrl Pts',(19.0165457198591,-8.5,58.89829642895));
#124468=CARTESIAN_POINT('',(19.9598076682562,-9.54867899952217,58.4893752699909));
#124469=CARTESIAN_POINT('Origin',(18.9749976915275,-9.54867463823461,58.6630340457145));
#124470=CARTESIAN_POINT('Origin',(19.9995178579382,-9.97190853039367,58.7145825449128));
#124471=CARTESIAN_POINT('Origin',(24.2283495281091,-1.25,82.697478608263));
#124472=CARTESIAN_POINT('',(21.1895064189391,-1.25,65.4633429305539));
#124473=CARTESIAN_POINT('',(19.9598077382391,-9.54867899952299,58.48937525765));
#124474=CARTESIAN_POINT('Ctrl Pts',(19.1714182688491,-10.74749523148,58.64157228471));
#124475=CARTESIAN_POINT('Ctrl Pts',(19.2001402692091,-10.7360962773,58.6139545222));
#124476=CARTESIAN_POINT('Ctrl Pts',(19.2671048399391,-10.70358813109,58.5547842577801));
#124477=CARTESIAN_POINT('Ctrl Pts',(19.3727076110191,-10.63072812626,58.47790542142));
#124478=CARTESIAN_POINT('Ctrl Pts',(19.4816021301791,-10.53268886688,58.41849876533));
#124479=CARTESIAN_POINT('Ctrl Pts',(19.5798624371291,-10.42553809768,58.38451859051));
#124480=CARTESIAN_POINT('Ctrl Pts',(19.6666859921691,-10.31512361264,58.37413803989));
#124481=CARTESIAN_POINT('Ctrl Pts',(19.7421160173891,-10.20561091184,58.3851490096));
#124482=CARTESIAN_POINT('Ctrl Pts',(19.8072433379691,-10.09866844348,58.41581498618));
#124483=CARTESIAN_POINT('Ctrl Pts',(19.8629533250291,-9.99480870780799,
58.46596105467));
#124484=CARTESIAN_POINT('Ctrl Pts',(19.9090928496691,-9.894926057294,58.53693056153));
#124485=CARTESIAN_POINT('Ctrl Pts',(19.9440264651791,-9.80174293293698,
58.63026741436));
#124486=CARTESIAN_POINT('Ctrl Pts',(19.9586138434991,-9.74464988774498,
58.71150611838));
#124487=CARTESIAN_POINT('Ctrl Pts',(19.9627402380791,-9.71822700826899,
58.75847349534));
#124488=CARTESIAN_POINT('Ctrl Pts',(19.9631169183391,-9.71562037545599,
58.76321536219));
#124489=CARTESIAN_POINT('Ctrl Pts',(19.4389951139891,-10.92142136616,57.90619534373));
#124490=CARTESIAN_POINT('Ctrl Pts',(19.4698150313491,-10.87387824357,57.8709868808));
#124491=CARTESIAN_POINT('Ctrl Pts',(19.5403451857891,-10.75993068367,57.8001893243101));
#124492=CARTESIAN_POINT('Ctrl Pts',(19.6471278826591,-10.56375960732,57.72415385788));
#124493=CARTESIAN_POINT('Ctrl Pts',(19.7525232043691,-10.34198300414,57.68551084602));
#124494=CARTESIAN_POINT('Ctrl Pts',(19.8436599230991,-10.12537489763,57.68693560855));
#124495=CARTESIAN_POINT('Ctrl Pts',(19.9206973644291,-9.91948599561099,
57.7224735366501));
#124496=CARTESIAN_POINT('Ctrl Pts',(19.9844091841491,-9.72750230791499,
57.78683436066));
#124497=CARTESIAN_POINT('Ctrl Pts',(20.0362321565991,-9.54902868193599,
57.87682821331));
#124498=CARTESIAN_POINT('Ctrl Pts',(20.0770494080691,-9.38266419984499,
57.9922002653601));
#124499=CARTESIAN_POINT('Ctrl Pts',(20.1064831635191,-9.22819950554099,
58.1349559086));
#124500=CARTESIAN_POINT('Ctrl Pts',(20.1226504432591,-9.08837963333299,
58.30711118863));
#124501=CARTESIAN_POINT('Ctrl Pts',(20.1225325579991,-9.00485278376398,
58.44835364564));
#124502=CARTESIAN_POINT('Ctrl Pts',(20.1184343085791,-8.96657204339798,
58.52818750154));
#124503=CARTESIAN_POINT('Ctrl Pts',(20.1179829255791,-8.96279955198799,
58.53623155663));
#124504=CARTESIAN_POINT('Ctrl Pts',(19.1652394686491,-10.56072968227,57.2444908451201));
#124505=CARTESIAN_POINT('Ctrl Pts',(19.1934686882291,-10.48562637282,57.22576151961));
#124506=CARTESIAN_POINT('Ctrl Pts',(19.2551219195491,-10.31444099589,57.1952629814201));
#124507=CARTESIAN_POINT('Ctrl Pts',(19.3403057354091,-10.04843890404,57.18919599896));
#124508=CARTESIAN_POINT('Ctrl Pts',(19.4162870129891,-9.77434356831699,
57.22757500333));
#124509=CARTESIAN_POINT('Ctrl Pts',(19.4752171934691,-9.526002199897,57.3005463023901));
#124510=CARTESIAN_POINT('Ctrl Pts',(19.5191579447891,-9.30450735442199,
57.39946609893));
#124511=CARTESIAN_POINT('Ctrl Pts',(19.5501871442691,-9.10911142993699,
57.5177279503601));
#124512=CARTESIAN_POINT('Ctrl Pts',(19.5703028373991,-8.93619395275799,
57.6522092200201));
#124513=CARTESIAN_POINT('Ctrl Pts',(19.5806370647691,-8.78210021717399,
57.80293835391));
#124514=CARTESIAN_POINT('Ctrl Pts',(19.5812333396291,-8.64489440002398,
57.9717607872401));
#124515=CARTESIAN_POINT('Ctrl Pts',(19.5712315886491,-8.52540487218098,
58.16008290365));
#124516=CARTESIAN_POINT('Ctrl Pts',(19.5558276663491,-8.45644720816198,
58.30540130949));
#124517=CARTESIAN_POINT('Ctrl Pts',(19.5449631456091,-8.425280107705,58.38543455065));
#124518=CARTESIAN_POINT('Ctrl Pts',(19.5438477623991,-8.42221325699699,
58.39347965143));
#124519=CARTESIAN_POINT('Ctrl Pts',(18.5989027611591,-9.99316710698298,
57.25772470602));
#124520=CARTESIAN_POINT('Ctrl Pts',(18.6222067375291,-9.92413049439999,
57.26457038522));
#124521=CARTESIAN_POINT('Ctrl Pts',(18.6706066640791,-9.77191874230598,
57.28967897792));
#124522=CARTESIAN_POINT('Ctrl Pts',(18.7310388805491,-9.55301850062899,
57.35912787143));
#124523=CARTESIAN_POINT('Ctrl Pts',(18.7784186996691,-9.34556310230998,
57.46080026331));
#124524=CARTESIAN_POINT('Ctrl Pts',(18.8093242582891,-9.17204736543399,
57.57644805921));
#124525=CARTESIAN_POINT('Ctrl Pts',(18.8269314570391,-9.02899558215699,
57.69862040094));
#124526=CARTESIAN_POINT('Ctrl Pts',(18.8340110856991,-8.91234674184498,
57.82235662252));
#124527=CARTESIAN_POINT('Ctrl Pts',(18.8328277769991,-8.817024057061,57.94606081245));
#124528=CARTESIAN_POINT('Ctrl Pts',(18.8247874658691,-8.73882659643499,
58.07015047993));
#124529=CARTESIAN_POINT('Ctrl Pts',(18.8106180795391,-8.67503808675099,
58.19563444819));
#124530=CARTESIAN_POINT('Ctrl Pts',(18.7908234139491,-8.62437257846199,
58.32278161578));
#124531=CARTESIAN_POINT('Ctrl Pts',(18.7734425263991,-8.59774862058898,
58.41254450536));
#124532=CARTESIAN_POINT('Ctrl Pts',(18.7634183625491,-8.58620276459499,
58.4599288642401));
#124533=CARTESIAN_POINT('Ctrl Pts',(18.7624063941091,-8.58507186480098,
58.46467291799));
#124534=CARTESIAN_POINT('',(18.8782773267445,-10.0000000019723,57.3029715768249));
#124535=CARTESIAN_POINT('Ctrl Pts',(18.8783268875783,-10.,57.302985115163));
#124536=CARTESIAN_POINT('Ctrl Pts',(18.8938428301929,-9.95326836354297,
57.3072289031713));
#124537=CARTESIAN_POINT('Ctrl Pts',(18.9083223436148,-9.90758142138574,
57.3134594588141));
#124538=CARTESIAN_POINT('Ctrl Pts',(18.9218376118847,-9.8631161205231,57.3213913093735));
#124539=CARTESIAN_POINT('Ctrl Pts',(18.9357793183205,-9.81724783594088,
57.3295734282767));
#124540=CARTESIAN_POINT('Ctrl Pts',(18.9486951127055,-9.77267940607304,
57.3395653884218));
#124541=CARTESIAN_POINT('Ctrl Pts',(18.9606650515343,-9.72954964117205,
57.3510561920399));
#124542=CARTESIAN_POINT('Ctrl Pts',(18.973479323177,-9.6833775987557,57.3633575313416));
#124543=CARTESIAN_POINT('Ctrl Pts',(18.9852097700432,-9.63885449218422,
57.3773759762135));
#124544=CARTESIAN_POINT('Ctrl Pts',(18.9959530202418,-9.59608710933202,
57.3927418875215));
#124545=CARTESIAN_POINT('Ctrl Pts',(19.0066962704403,-9.55331972647982,
57.4081077988295));
#124546=CARTESIAN_POINT('Ctrl Pts',(19.0164524568694,-9.51230744604947,
57.4248207583032));
#124547=CARTESIAN_POINT('Ctrl Pts',(19.0253143161839,-9.47310040316696,
57.4425306909256));
#124548=CARTESIAN_POINT('Ctrl Pts',(19.0342882072661,-9.43339770421921,
57.4604645128002));
#124549=CARTESIAN_POINT('Ctrl Pts',(19.042345123411,-9.39554564575364,57.4794203451349));
#124550=CARTESIAN_POINT('Ctrl Pts',(19.0495778675271,-9.35954753176827,
57.4990608309867));
#124551=CARTESIAN_POINT('Ctrl Pts',(19.0570664813153,-9.32227592801514,
57.5193961298439));
#124552=CARTESIAN_POINT('Ctrl Pts',(19.0636717003723,-9.28699131720336,
57.5404649911381));
#124553=CARTESIAN_POINT('Ctrl Pts',(19.0694884995562,-9.25365191702527,
57.5619262349102));
#124554=CARTESIAN_POINT('Ctrl Pts',(19.0740301794008,-9.22762095445684,
57.5786828901084));
#124555=CARTESIAN_POINT('Ctrl Pts',(19.0780910568302,-9.20277482937547,
57.5956794254871));
#124556=CARTESIAN_POINT('Ctrl Pts',(19.0817125082702,-9.17907826869883,
57.6127686736064));
#124557=CARTESIAN_POINT('Ctrl Pts',(19.0837152207405,-9.16597374462739,
57.6222192629302));
#124558=CARTESIAN_POINT('Ctrl Pts',(19.0855505911153,-9.15346508141529,
57.6315179556795));
#124559=CARTESIAN_POINT('Ctrl Pts',(19.0872733852832,-9.14119469554508,
57.6408911412512));
#124560=CARTESIAN_POINT('Ctrl Pts',(19.0890134403464,-9.12880137110741,
57.6503582379696));
#124561=CARTESIAN_POINT('Ctrl Pts',(19.0906385994655,-9.11665094506254,
57.6599015274696));
#124562=CARTESIAN_POINT('Ctrl Pts',(19.0921933332106,-9.10440424433379,
57.6697959537671));
#124563=CARTESIAN_POINT('Ctrl Pts',(19.0923631759237,-9.10306638639855,
57.6708768437986));
#124564=CARTESIAN_POINT('Ctrl Pts',(19.0925321668134,-9.10172741006866,
57.671961963764));
#124565=CARTESIAN_POINT('Ctrl Pts',(19.0927003554822,-9.10038689612429,
57.6730517011598));
#124566=CARTESIAN_POINT('Ctrl Pts',(19.0980544282457,-9.05771333644073,
57.7077421077707));
#124567=CARTESIAN_POINT('Ctrl Pts',(19.1021295422428,-9.01730565368886,
57.7440102458586));
#124568=CARTESIAN_POINT('Ctrl Pts',(19.1050219213473,-8.97924705484321,
57.7815126843629));
#124569=CARTESIAN_POINT('Ctrl Pts',(19.1079843594873,-8.94026660286906,
57.8199235047129));
#124570=CARTESIAN_POINT('Ctrl Pts',(19.1097062135066,-8.90375023790228,
57.8596286926656));
#124571=CARTESIAN_POINT('Ctrl Pts',(19.110288386314,-8.86973433764281,57.9002739713109));
#124572=CARTESIAN_POINT('Ctrl Pts',(19.1108784273267,-8.83525870431884,
57.9414685806624));
#124573=CARTESIAN_POINT('Ctrl Pts',(19.1102978994856,-8.8033512522251,57.9836284817762));
#124574=CARTESIAN_POINT('Ctrl Pts',(19.1086472825267,-8.77400002787252,
58.0264061375439));
#124575=CARTESIAN_POINT('Ctrl Pts',(19.1069602796114,-8.74400178946377,
58.0701267776396));
#124576=CARTESIAN_POINT('Ctrl Pts',(19.104155613855,-8.71667339410396,58.114492336582));
#124577=CARTESIAN_POINT('Ctrl Pts',(19.1003338768725,-8.69195530435059,
58.1591597238884));
#124578=CARTESIAN_POINT('Ctrl Pts',(19.0977902289464,-8.67550359194224,
58.1888891656587));
#124579=CARTESIAN_POINT('Ctrl Pts',(19.0947958862835,-8.66020725328719,
58.2187529102463));
#124580=CARTESIAN_POINT('Ctrl Pts',(19.0913785491043,-8.64603879443074,
58.2486575231502));
#124581=CARTESIAN_POINT('Ctrl Pts',(19.9598074414544,-9.54867899952064,
58.4893753099853));
#124582=CARTESIAN_POINT('Ctrl Pts',(19.9542411823548,-9.55326652103831,
58.4578102133941));
#124583=CARTESIAN_POINT('Ctrl Pts',(19.9476045455276,-9.55822494497135,
58.4260920838297));
#124584=CARTESIAN_POINT('Ctrl Pts',(19.9398484081562,-9.56355305469618,
58.3942993779954));
#124585=CARTESIAN_POINT('Ctrl Pts',(19.9372948498576,-9.56530723182746,
58.383832244172));
#124586=CARTESIAN_POINT('Ctrl Pts',(19.9346200002808,-9.56710131672924,
58.3733574086514));
#124587=CARTESIAN_POINT('Ctrl Pts',(19.931822301245,-9.56893477895819,58.3628787978499));
#124588=CARTESIAN_POINT('Ctrl Pts',(19.9230863039181,-9.57465988409868,
58.3301586536235));
#124589=CARTESIAN_POINT('Ctrl Pts',(19.9131513284052,-9.58077050467405,
58.2973984067014));
#124590=CARTESIAN_POINT('Ctrl Pts',(19.9019681612585,-9.58727342913176,
58.2646820321185));
#124591=CARTESIAN_POINT('Ctrl Pts',(19.8956843679744,-9.59092740590757,
58.2462987841365));
#124592=CARTESIAN_POINT('Ctrl Pts',(19.8890067452488,-9.59470485515314,
58.2279302044197));
#124593=CARTESIAN_POINT('Ctrl Pts',(19.8819290491294,-9.59860407484053,
58.2095973349305));
#124594=CARTESIAN_POINT('Ctrl Pts',(19.874816160293,-9.60252268277692,58.1911733081669));
#124595=CARTESIAN_POINT('Ctrl Pts',(19.8672991829115,-9.60656426155635,
58.1727853912745));
#124596=CARTESIAN_POINT('Ctrl Pts',(19.8593707036486,-9.61073258786585,
58.1544516284897));
#124597=CARTESIAN_POINT('Ctrl Pts',(19.8458919321712,-9.61781893013978,
58.1232834068547));
#124598=CARTESIAN_POINT('Ctrl Pts',(19.8312239210235,-9.62526905939209,
58.0922727289796));
#124599=CARTESIAN_POINT('Ctrl Pts',(19.8153419026997,-9.63307328270873,
58.061521164123));
#124600=CARTESIAN_POINT('Ctrl Pts',(19.8029377456224,-9.63916852891185,
58.0375036096107));
#124601=CARTESIAN_POINT('Ctrl Pts',(19.7897933314337,-9.64547947752553,
58.0136448082272));
#124602=CARTESIAN_POINT('Ctrl Pts',(19.7758983977501,-9.65201328479347,
57.9899949949436));
#124603=CARTESIAN_POINT('Ctrl Pts',(19.7616084921664,-9.65873281948774,
57.9656729214027));
#124604=CARTESIAN_POINT('Ctrl Pts',(19.7465252268148,-9.66568418437979,
57.9415725405707));
#124605=CARTESIAN_POINT('Ctrl Pts',(19.7306431945115,-9.67286709491166,
57.9177510229782));
#124606=CARTESIAN_POINT('Ctrl Pts',(19.7289172210685,-9.67364769481126,
57.9151622291796));
#124607=CARTESIAN_POINT('Ctrl Pts',(19.7271818233574,-9.67443102682133,
57.9125767380664));
#124608=CARTESIAN_POINT('Ctrl Pts',(19.7254369924547,-9.67521710892549,
57.909994624528));
#124609=CARTESIAN_POINT('Ctrl Pts',(19.7172273866166,-9.67891570471584,
57.8978455192213));
#124610=CARTESIAN_POINT('Ctrl Pts',(19.7086434471657,-9.68274570879777,
57.8855333625138));
#124611=CARTESIAN_POINT('Ctrl Pts',(19.6999083684738,-9.68661195124135,
57.8734007870112));
#124612=CARTESIAN_POINT('Ctrl Pts',(19.6910441422571,-9.69053535580778,
57.8610888322324));
#124613=CARTESIAN_POINT('Ctrl Pts',(19.6820244432216,-9.69449595062049,
57.8489619683201));
#124614=CARTESIAN_POINT('Ctrl Pts',(19.6731171416485,-9.69837585202093,
57.8373408913688));
#124615=CARTESIAN_POINT('Ctrl Pts',(19.6717701967348,-9.69896256320545,
57.835583574592));
#124616=CARTESIAN_POINT('Ctrl Pts',(19.6704258816302,-9.69954739803375,
57.8338377535858));
#124617=CARTESIAN_POINT('Ctrl Pts',(19.669085184134,-9.70012991688436,57.832104463319));
#124618=CARTESIAN_POINT('Ctrl Pts',(19.6545934277506,-9.70642643141944,
57.813369125661));
#124619=CARTESIAN_POINT('Ctrl Pts',(19.6392416893483,-9.71304394409325,
57.7944386211372));
#124620=CARTESIAN_POINT('Ctrl Pts',(19.6229683979434,-9.71997398145692,
57.7753944714038));
#124621=CARTESIAN_POINT('Ctrl Pts',(19.6011612990038,-9.72926060987679,
57.7498742710262));
#124622=CARTESIAN_POINT('Ctrl Pts',(19.5776981983314,-9.73910833703785,
57.7241483916085));
#124623=CARTESIAN_POINT('Ctrl Pts',(19.5524383006595,-9.74951075760174,
57.6984455580634));
#124624=CARTESIAN_POINT('Ctrl Pts',(19.5320199393966,-9.75791935782019,
57.677669157952));
#124625=CARTESIAN_POINT('Ctrl Pts',(19.5104276008589,-9.76669025045359,
57.6569084037166));
#124626=CARTESIAN_POINT('Ctrl Pts',(19.4876002219506,-9.7758198446224,57.6363054400513));
#124627=CARTESIAN_POINT('Ctrl Pts',(19.4614826753149,-9.78626531023744,
57.6127329192411));
#124628=CARTESIAN_POINT('Ctrl Pts',(19.4337470744814,-9.79717991205959,
57.5893665362372));
#124629=CARTESIAN_POINT('Ctrl Pts',(19.4043265244434,-9.80858109390736,
57.5664510660148));
#124630=CARTESIAN_POINT('Ctrl Pts',(19.3908862087655,-9.81378954456305,
57.5559824937652));
#124631=CARTESIAN_POINT('Ctrl Pts',(19.3770947553912,-9.81909963101177,
57.5456084732102));
#124632=CARTESIAN_POINT('Ctrl Pts',(19.3629486740691,-9.82451356155939,
57.5353545818722));
#124633=CARTESIAN_POINT('Ctrl Pts',(19.3490675385454,-9.82982609313166,
57.5252927384494));
#124634=CARTESIAN_POINT('Ctrl Pts',(19.3348478695568,-9.83525106947039,
57.5153486013066));
#124635=CARTESIAN_POINT('Ctrl Pts',(19.3202822274548,-9.84078167951122,
57.5055433568592));
#124636=CARTESIAN_POINT('Ctrl Pts',(19.2897062331762,-9.85239145955266,
57.4849603234422));
#124637=CARTESIAN_POINT('Ctrl Pts',(19.2576029146744,-9.86446624259593,
57.4649867936472));
#124638=CARTESIAN_POINT('Ctrl Pts',(19.2239336798893,-9.87694380377314,
57.4458454060012));
#124639=CARTESIAN_POINT('Ctrl Pts',(19.1927256677699,-9.88850925463423,
57.4281032547034));
#124640=CARTESIAN_POINT('Ctrl Pts',(19.1601720310806,-9.90042058302751,
57.4110763933475));
#124641=CARTESIAN_POINT('Ctrl Pts',(19.1262789226855,-9.91263776729008,
57.3949732486323));
#124642=CARTESIAN_POINT('Ctrl Pts',(19.1236059396619,-9.91360127661915,
57.3937032726847));
#124643=CARTESIAN_POINT('Ctrl Pts',(19.1209246469674,-9.91456669436537,
57.3924390573872));
#124644=CARTESIAN_POINT('Ctrl Pts',(19.1182350589379,-9.91553400419153,
57.3911807128345));
#124645=CARTESIAN_POINT('Ctrl Pts',(19.0841674648025,-9.92778640797961,
57.3752419255427));
#124646=CARTESIAN_POINT('Ctrl Pts',(19.0487653579397,-9.94034008511723,
57.3602447619451));
#124647=CARTESIAN_POINT('Ctrl Pts',(19.0120652193687,-9.95324402795822,
57.3464036888154));
#124648=CARTESIAN_POINT('Ctrl Pts',(18.9756752032899,-9.96603893025964,
57.3326795751376));
#124649=CARTESIAN_POINT('Ctrl Pts',(18.9380089288395,-9.97917838906926,
57.3200930197138));
#124650=CARTESIAN_POINT('Ctrl Pts',(18.8991462603499,-9.99273593367285,
57.3088485005585));
#124651=CARTESIAN_POINT('Ctrl Pts',(18.8922438986108,-9.99514387632795,
57.3068513721623));
#124652=CARTESIAN_POINT('Ctrl Pts',(18.8853039100555,-9.99756506874135,
57.3048965453963));
#124653=CARTESIAN_POINT('Ctrl Pts',(18.8783268876145,-9.99999999999996,
57.3029851150307));
#124654=CARTESIAN_POINT('Origin',(18.4825957014091,-15.00000011529,58.74984511558));
#124655=CARTESIAN_POINT('',(18.8783357567019,-14.999996024641,57.302989036439));
#124656=CARTESIAN_POINT('Origin',(18.4825952511691,-15.00000013862,58.74984256216));
#124657=CARTESIAN_POINT('Origin',(18.4826085813491,-14.99999405365,58.74984854358));
#124658=CARTESIAN_POINT('Origin',(17.7894674803291,1.4210854715202E-14,
100.88908350184));
#124659=CARTESIAN_POINT('',(15.282105101301,-17.8079464603878,57.8022959605294));
#124660=CARTESIAN_POINT('',(18.9921129410137,-17.0122601925885,65.8508014704009));
#124661=CARTESIAN_POINT('Ctrl Pts',(15.282105101301,-17.8079464603878,57.8022959605294));
#124662=CARTESIAN_POINT('Ctrl Pts',(15.3505394572593,-17.7947650778713,
57.9206881482452));
#124663=CARTESIAN_POINT('Ctrl Pts',(15.4184424259051,-17.7815460140866,
58.0393944742722));
#124664=CARTESIAN_POINT('Ctrl Pts',(15.4858175145022,-17.7683020806319,
58.1584148517074));
#124665=CARTESIAN_POINT('Ctrl Pts',(15.684876581833,-17.7291730034586,58.5100594405155));
#124666=CARTESIAN_POINT('Ctrl Pts',(15.8793283335588,-17.6898288245895,
58.8644420115123));
#124667=CARTESIAN_POINT('Ctrl Pts',(16.0692882733122,-17.6505598703399,
59.2214906008568));
#124668=CARTESIAN_POINT('Ctrl Pts',(16.2599229789274,-17.6111514269444,
59.5798074797121));
#124669=CARTESIAN_POINT('Ctrl Pts',(16.4460340568941,-17.5718183397561,
59.9408092387024));
#124670=CARTESIAN_POINT('Ctrl Pts',(16.6277296627721,-17.532830229838,60.3044694396092));
#124671=CARTESIAN_POINT('Ctrl Pts',(16.80927596144,-17.4938741581515,60.6678308050557));
#124672=CARTESIAN_POINT('Ctrl Pts',(16.9864141980048,-17.4552620670934,
61.0338461524315));
#124673=CARTESIAN_POINT('Ctrl Pts',(17.1592414060169,-17.4172454697713,
61.4025367311538));
#124674=CARTESIAN_POINT('Ctrl Pts',(17.3247218718306,-17.3808449266747,
61.7555545771854));
#124675=CARTESIAN_POINT('Ctrl Pts',(17.4862500986103,-17.3449898813006,
62.1110252596489));
#124676=CARTESIAN_POINT('Ctrl Pts',(17.6438998504956,-17.3098916204539,
62.4690096849072));
#124677=CARTESIAN_POINT('Ctrl Pts',(17.8025545590757,-17.2745696216578,
62.8292761235559));
#124678=CARTESIAN_POINT('Ctrl Pts',(17.957281269496,-17.240013832677,63.1920878397201));
#124679=CARTESIAN_POINT('Ctrl Pts',(18.1080982043483,-17.2064151462286,
63.5573650366903));
#124680=CARTESIAN_POINT('Ctrl Pts',(18.2637636032691,-17.1717363289306,
63.9343851680085));
#124681=CARTESIAN_POINT('Ctrl Pts',(18.4152641332005,-17.1380767231858,
64.3140315907342));
#124682=CARTESIAN_POINT('Ctrl Pts',(18.5626024828262,-17.1056465582174,
64.6962722974421));
#124683=CARTESIAN_POINT('Ctrl Pts',(18.7099408324519,-17.0732163932491,
65.0785130041501));
#124684=CARTESIAN_POINT('Ctrl Pts',(18.8531172838998,-17.042015217014,65.4633480320533));
#124685=CARTESIAN_POINT('Ctrl Pts',(18.9921129410137,-17.0122601925885,
65.8508014704009));
#124686=CARTESIAN_POINT('Origin',(11.8338327653321,1.4210854715202E-14,
67.1130006183879));
#124687=CARTESIAN_POINT('Ctrl Pts',(15.2821062552024,-17.8079506230211,
57.8022957570331));
#124688=CARTESIAN_POINT('Ctrl Pts',(15.4823121359235,-17.7542554209139,
57.8391951328845));
#124689=CARTESIAN_POINT('Ctrl Pts',(15.6878488274998,-17.6958698358612,
57.8779860861533));
#124690=CARTESIAN_POINT('Ctrl Pts',(15.8984493855906,-17.632250897153,57.9186971735126));
#124691=CARTESIAN_POINT('Ctrl Pts',(16.1060975495705,-17.5695238277811,
57.9588375350598));
#124692=CARTESIAN_POINT('Ctrl Pts',(16.3186688001434,-17.5017088209382,
58.0008445354996));
#124693=CARTESIAN_POINT('Ctrl Pts',(16.5358605764418,-17.4282679911826,
58.0447537793855));
#124694=CARTESIAN_POINT('Ctrl Pts',(16.7482639330329,-17.3564463089037,
58.0876949576643));
#124695=CARTESIAN_POINT('Ctrl Pts',(16.9650864343223,-17.2792438249526,
58.132455407181));
#124696=CARTESIAN_POINT('Ctrl Pts',(17.1859979209596,-17.1961450662185,
58.1790767468365));
#124697=CARTESIAN_POINT('Ctrl Pts',(17.4041564194499,-17.1140818801533,
58.2251170936362));
#124698=CARTESIAN_POINT('Ctrl Pts',(17.626302786287,-17.0262681635225,58.2729722104596));
#124699=CARTESIAN_POINT('Ctrl Pts',(17.8520704187426,-16.9321996968654,
58.3226907549545));
#124700=CARTESIAN_POINT('Ctrl Pts',(18.0732551795446,-16.8400407320471,
58.3714000595255));
#124701=CARTESIAN_POINT('Ctrl Pts',(18.2979157487183,-16.7418780652835,
58.4218978960706));
#124702=CARTESIAN_POINT('Ctrl Pts',(18.5256588509806,-16.6372345008744,
58.4742385791027));
#124703=CARTESIAN_POINT('Ctrl Pts',(18.7404075568062,-16.5385616110849,
58.5235928463957));
#124704=CARTESIAN_POINT('Ctrl Pts',(18.957896824941,-16.4341260375928,58.5745857071687));
#124705=CARTESIAN_POINT('Ctrl Pts',(19.1777550979457,-16.323528908982,58.6272700752903));
#124706=CARTESIAN_POINT('Origin',(11.833832765324,1.4210854715202E-14,67.1130006183894));
#124707=CARTESIAN_POINT('',(14.883373594419,-20.2647763837508,66.5752842914479));
#124708=CARTESIAN_POINT('Ctrl Pts',(18.9921131492666,-17.012260192524,65.8508026512244));
#124709=CARTESIAN_POINT('Ctrl Pts',(18.1865537652697,-17.3617579185958,
65.9928445051859));
#124710=CARTESIAN_POINT('Ctrl Pts',(17.4282361956689,-17.8163218667055,
66.1265563526508));
#124711=CARTESIAN_POINT('Ctrl Pts',(16.0411085625388,-18.9125487124957,
66.3711443800578));
#124712=CARTESIAN_POINT('Ctrl Pts',(15.4171051316011,-19.5523187044817,
66.4811730209878));
#124713=CARTESIAN_POINT('Ctrl Pts',(14.883373594419,-20.2647763837508,66.575284291448));
#124714=CARTESIAN_POINT('',(-6.53751764820717,-8.5,70.352365368344));
#124715=CARTESIAN_POINT('Origin',(11.833832765324,1.4210854715202E-14,67.1130006183894));
#124716=CARTESIAN_POINT('',(-12.1462360205204,-8.5,71.3413337445779));
#124717=CARTESIAN_POINT('Origin',(11.833832765324,1.4210854715202E-14,67.1130006183894));
#124718=CARTESIAN_POINT('',(15.6158353372468,-20.1981065744412,68.3761083647154));
#124719=CARTESIAN_POINT('Ctrl Pts',(15.6157934551793,-20.1981142180028,
68.3761244855819));
#124720=CARTESIAN_POINT('Ctrl Pts',(15.5010475555325,-20.2085914269983,
68.07304656518));
#124721=CARTESIAN_POINT('Ctrl Pts',(15.3826186459966,-20.2194631831356,
67.7713940591794));
#124722=CARTESIAN_POINT('Ctrl Pts',(15.1384505677303,-20.2417654565994,
67.1710527205433));
#124723=CARTESIAN_POINT('Ctrl Pts',(15.0127177613177,-20.2531953410346,
66.8723797468496));
#124724=CARTESIAN_POINT('Ctrl Pts',(14.8833735944191,-20.2647763837508,
66.5752842914479));
#124725=CARTESIAN_POINT('',(15.9984098127276,-20.3875455450126,78.3830072931938));
#124726=CARTESIAN_POINT('Ctrl Pts',(15.9983959512983,-20.3875469025234,
78.3830030094886));
#124727=CARTESIAN_POINT('Ctrl Pts',(16.4328372437242,-20.3164621615951,
76.9546891450724));
#124728=CARTESIAN_POINT('Ctrl Pts',(16.7037780449221,-20.2204258112703,
75.2444468274443));
#124729=CARTESIAN_POINT('Ctrl Pts',(16.5602362046653,-20.1331659697557,
71.6438394681868));
#124730=CARTESIAN_POINT('Ctrl Pts',(16.217560034564,-20.1431511202205,69.965049899536));
#124731=CARTESIAN_POINT('Ctrl Pts',(15.615877218811,-20.198098930694,68.3760922412998));
#124732=CARTESIAN_POINT('Ctrl Pts',(15.1826286361355,-20.4790209859242,
80.7654349522145));
#124733=CARTESIAN_POINT('Ctrl Pts',(15.3308715299447,-20.4693621419826,
80.3776179869579));
#124734=CARTESIAN_POINT('Ctrl Pts',(15.4722327090839,-20.4566516001834,
79.9871295969088));
#124735=CARTESIAN_POINT('Ctrl Pts',(15.7443617489847,-20.4259089142243,
79.1929667922874));
#124736=CARTESIAN_POINT('Ctrl Pts',(15.874915709885,-20.4077502433841,78.7889060427433));
#124737=CARTESIAN_POINT('Ctrl Pts',(15.9984236741293,-20.387544187533,78.3830115786004));
#124738=CARTESIAN_POINT('Origin',(14.4385554303262,1.4210854715202E-14,
81.8851169135651));
#124739=CARTESIAN_POINT('',(-6.53751764820717,-8.5,70.352365368344));
#124740=CARTESIAN_POINT('Ctrl Pts',(20.1035333418991,-16.60682578431,65.661400313719));
#124741=CARTESIAN_POINT('Ctrl Pts',(20.4910764161291,-16.50426328115,66.404263622412));
#124742=CARTESIAN_POINT('Ctrl Pts',(21.2622024424291,-16.31712154271,68.2147622085249));
#124743=CARTESIAN_POINT('Ctrl Pts',(21.9472426402291,-16.25946392932,71.32939250689));
#124744=CARTESIAN_POINT('Ctrl Pts',(21.9575487565991,-16.51641000933,74.855943101759));
#124745=CARTESIAN_POINT('Ctrl Pts',(21.2210210639291,-17.03764923711,78.150815900789));
#124746=CARTESIAN_POINT('Ctrl Pts',(20.3317361244091,-17.46566964773,80.057299005597));
#124747=CARTESIAN_POINT('Ctrl Pts',(19.8425295031191,-17.6668669887,80.890276924625));
#124748=CARTESIAN_POINT('Ctrl Pts',(16.1484715971691,-17.81257432064,67.611225517012));
#124749=CARTESIAN_POINT('Ctrl Pts',(16.4410317598291,-17.71210035932,68.160095145162));
#124750=CARTESIAN_POINT('Ctrl Pts',(17.0247629322891,-17.52936000758,69.505370284895));
#124751=CARTESIAN_POINT('Ctrl Pts',(17.5404653675491,-17.47323219871,71.836115329147));
#124752=CARTESIAN_POINT('Ctrl Pts',(17.5346243142291,-17.72370055013,74.470228345905));
#124753=CARTESIAN_POINT('Ctrl Pts',(16.9597507724791,-18.2350065912,76.900867930413));
#124754=CARTESIAN_POINT('Ctrl Pts',(16.2859520423791,-18.65955113028,78.274474857878));
#124755=CARTESIAN_POINT('Ctrl Pts',(15.9214324846391,-18.86042280821,78.865755836276));
#124756=CARTESIAN_POINT('Ctrl Pts',(13.8455860593191,-21.47087538256,69.098352900055));
#124757=CARTESIAN_POINT('Ctrl Pts',(14.0473884300291,-21.37673816115,69.4909848960241));
#124758=CARTESIAN_POINT('Ctrl Pts',(14.4481518263091,-21.20735183567,70.444214760764));
#124759=CARTESIAN_POINT('Ctrl Pts',(14.8055693836991,-21.15586552985,72.0760640565359));
#124760=CARTESIAN_POINT('Ctrl Pts',(14.8175681434991,-21.38668013034,73.9261073698239));
#124761=CARTESIAN_POINT('Ctrl Pts',(14.4432251927491,-21.86784838863,75.6694251557751));
#124762=CARTESIAN_POINT('Ctrl Pts',(13.9813565266591,-22.2818469605,76.694122020234));
#124763=CARTESIAN_POINT('Ctrl Pts',(13.7242846805491,-22.48173056057,77.146151574849));
#124764=CARTESIAN_POINT('Ctrl Pts',(14.1821041658691,-26.01344642904,69.485263605966));
#124765=CARTESIAN_POINT('Ctrl Pts',(14.3362809575091,-25.92717763912,69.826391761791));
#124766=CARTESIAN_POINT('Ctrl Pts',(14.6369403842691,-25.77437322202,70.628820996858));
#124767=CARTESIAN_POINT('Ctrl Pts',(14.9149813289091,-25.72865034491,71.94637471107));
#124768=CARTESIAN_POINT('Ctrl Pts',(14.9711591085391,-25.93506056796,73.456840206672));
#124769=CARTESIAN_POINT('Ctrl Pts',(14.7502574305891,-26.37880625846,74.9843966174541));
#124770=CARTESIAN_POINT('Ctrl Pts',(14.4059100677191,-26.77970973387,75.993724308785));
#124771=CARTESIAN_POINT('Ctrl Pts',(14.1929846615191,-26.97836642181,76.46864385711));
#124772=CARTESIAN_POINT('Origin',(22.9322443087252,-26.6270894131141,80.1832188051537));
#124773=CARTESIAN_POINT('Origin',(22.9323739056077,-25.6803623351439,65.7952890379436));
#124774=CARTESIAN_POINT('Ctrl Pts',(20.3703076195591,-17.48636025246,80.6160118299));
#124775=CARTESIAN_POINT('Ctrl Pts',(20.1881103583291,-17.59469264276,81.383197007755));
#124776=CARTESIAN_POINT('Ctrl Pts',(19.7633142133291,-17.81559800981,82.9726719728399));
#124777=CARTESIAN_POINT('Ctrl Pts',(19.0018167096191,-18.10372872761,85.2475673257499));
#124778=CARTESIAN_POINT('Ctrl Pts',(18.1317679720991,-18.32477803286,87.36843783982));
#124779=CARTESIAN_POINT('Ctrl Pts',(17.2370610827991,-18.45951303147,89.2032198305499));
#124780=CARTESIAN_POINT('Ctrl Pts',(16.3494952333791,-18.51446227549,90.7700178089799));
#124781=CARTESIAN_POINT('Ctrl Pts',(15.4867758268391,-18.50123398135,92.10529605495));
#124782=CARTESIAN_POINT('Ctrl Pts',(14.6453959780491,-18.43037008788,93.26267617499));
#124783=CARTESIAN_POINT('Ctrl Pts',(13.8009845953991,-18.30490819777,94.3025568640399));
#124784=CARTESIAN_POINT('Ctrl Pts',(12.9307100320291,-18.12021817286,95.2628709280001));
#124785=CARTESIAN_POINT('Ctrl Pts',(12.0275979803391,-17.86955305763,96.15310194351));
#124786=CARTESIAN_POINT('Ctrl Pts',(11.1010176724691,-17.54986176095,96.96608256951));
#124787=CARTESIAN_POINT('Ctrl Pts',(10.1635981391591,-17.16111541643,97.6955323958101));
#124788=CARTESIAN_POINT('Ctrl Pts',(9.27968364505908,-16.73052720888,98.30286534269));
#124789=CARTESIAN_POINT('Ctrl Pts',(8.71271538374908,-16.41504543997,98.64913661867));
#124790=CARTESIAN_POINT('Ctrl Pts',(8.45819912877909,-16.26514131694,98.79644286584));
#124791=CARTESIAN_POINT('Ctrl Pts',(14.7248846521991,-18.94108804276,77.911688731006));
#124792=CARTESIAN_POINT('Ctrl Pts',(14.5694350031491,-18.93552267139,78.561742613804));
#124793=CARTESIAN_POINT('Ctrl Pts',(14.2134049487491,-18.91245218656,79.908309787637));
#124794=CARTESIAN_POINT('Ctrl Pts',(13.6004443439491,-18.832257487,81.827642780919));
#124795=CARTESIAN_POINT('Ctrl Pts',(12.9289464995691,-18.69869734538,83.60280410874));
#124796=CARTESIAN_POINT('Ctrl Pts',(12.2646619608891,-18.52485132822,85.12309497776));
#124797=CARTESIAN_POINT('Ctrl Pts',(11.6278705382591,-18.32183553005,86.4073429830001));
#124798=CARTESIAN_POINT('Ctrl Pts',(11.0263774792591,-18.09933417041,87.4904580833699));
#124799=CARTESIAN_POINT('Ctrl Pts',(10.4529512601791,-17.86094059021,88.4205103504401));
#124800=CARTESIAN_POINT('Ctrl Pts',(9.88731078157909,-17.60178133109,89.249386304));
#124801=CARTESIAN_POINT('Ctrl Pts',(9.31126387016909,-17.31409529898,90.0096973799401));
#124802=CARTESIAN_POINT('Ctrl Pts',(8.71693645522909,-16.9926399648,90.7110627126001));
#124803=CARTESIAN_POINT('Ctrl Pts',(8.10624510203909,-16.63664836235,91.35001588189));
#124804=CARTESIAN_POINT('Ctrl Pts',(7.48260991328909,-16.24618559887,91.92364883475));
#124805=CARTESIAN_POINT('Ctrl Pts',(6.88447228887909,-15.84456366131,92.40307208249));
#124806=CARTESIAN_POINT('Ctrl Pts',(6.49233429628909,-15.56370842049,92.67816808986));
#124807=CARTESIAN_POINT('Ctrl Pts',(6.31420645011909,-15.43222415467,92.79562051845));
#124808=CARTESIAN_POINT('Ctrl Pts',(12.5063401363191,-24.60762905604,75.845594438731));
#124809=CARTESIAN_POINT('Ctrl Pts',(12.2868497584891,-24.55389093248,76.4322774261809));
#124810=CARTESIAN_POINT('Ctrl Pts',(11.7948949593591,-24.42464703364,77.649532278307));
#124811=CARTESIAN_POINT('Ctrl Pts',(10.9814946228591,-24.17202064863,79.385448634424));
#124812=CARTESIAN_POINT('Ctrl Pts',(10.1222707621991,-23.85736527914,80.987352988331));
#124813=CARTESIAN_POINT('Ctrl Pts',(9.29846527963909,-23.5105055521,82.353880287081));
#124814=CARTESIAN_POINT('Ctrl Pts',(8.52998276490909,-23.14741348718,83.50305548649));
#124815=CARTESIAN_POINT('Ctrl Pts',(7.82085548590909,-22.77957706661,84.4682620618799));
#124816=CARTESIAN_POINT('Ctrl Pts',(7.15797738393909,-22.40870352106,85.2944825448601));
#124817=CARTESIAN_POINT('Ctrl Pts',(6.5147643722091,-22.02537234206,86.0295402695));
#124818=CARTESIAN_POINT('Ctrl Pts',(5.86851416204909,-21.61846160989,86.7038509520601));
#124819=CARTESIAN_POINT('Ctrl Pts',(5.20849832309909,-21.1819420503,87.32752168855));
#124820=CARTESIAN_POINT('Ctrl Pts',(4.53433886995909,-20.71577757791,87.89907590832));
#124821=CARTESIAN_POINT('Ctrl Pts',(3.84677854591909,-20.22008924508,88.41723900531));
#124822=CARTESIAN_POINT('Ctrl Pts',(3.18516755758909,-19.72283039656,88.85636793195));
#124823=CARTESIAN_POINT('Ctrl Pts',(2.74853368799909,-19.38098595465,89.11251172142));
#124824=CARTESIAN_POINT('Ctrl Pts',(2.54938093874909,-19.22185467038,89.22278927536));
#124825=CARTESIAN_POINT('Ctrl Pts',(15.3202955475791,-30.38495224307,75.913018023323));
#124826=CARTESIAN_POINT('Ctrl Pts',(14.9923241307591,-30.38363031797,76.535953769073));
#124827=CARTESIAN_POINT('Ctrl Pts',(14.2581262150091,-30.36285605286,77.831078640661));
#124828=CARTESIAN_POINT('Ctrl Pts',(13.0403732440191,-30.25848525137,79.688467729779));
#124829=CARTESIAN_POINT('Ctrl Pts',(11.7430089211191,-30.06731245317,81.414958143033));
#124830=CARTESIAN_POINT('Ctrl Pts',(10.4851888796891,-29.80822108623,82.899732333371));
#124831=CARTESIAN_POINT('Ctrl Pts',(9.29785820693909,-29.4987931119,84.15906778619));
#124832=CARTESIAN_POINT('Ctrl Pts',(8.19013397563909,-29.15474260213,85.2259540885799));
#124833=CARTESIAN_POINT('Ctrl Pts',(7.14513725765909,-28.78231819477,86.14698476448));
#124834=CARTESIAN_POINT('Ctrl Pts',(6.12414964407909,-28.37420716695,86.97330959057));
#124835=CARTESIAN_POINT('Ctrl Pts',(5.09407323602909,-27.91812922517,87.73786331633));
#124836=CARTESIAN_POINT('Ctrl Pts',(4.04143642525909,-27.40554656753,88.4512402521699));
#124837=CARTESIAN_POINT('Ctrl Pts',(2.97038542110909,-26.83507178681,89.11080249674));
#124838=CARTESIAN_POINT('Ctrl Pts',(1.88745485450909,-26.20680336296,89.71398781054));
#124839=CARTESIAN_POINT('Ctrl Pts',(0.859057681899087,-25.55851947637,90.2295998987501));
#124840=CARTESIAN_POINT('Ctrl Pts',(0.190804675379086,-25.10420966072,90.53273076058));
#124841=CARTESIAN_POINT('Ctrl Pts',(-0.111569990190912,-24.89137338738,
90.6637050372499));
#124842=CARTESIAN_POINT('',(0.214736886699964,-24.69203306784,90.5121335896162));
#124843=CARTESIAN_POINT('Ctrl Pts',(14.2241127701603,-26.6269674540423,
76.3859510179931));
#124844=CARTESIAN_POINT('Ctrl Pts',(14.1795412520668,-26.6539472170917,
76.4881804929476));
#124845=CARTESIAN_POINT('Ctrl Pts',(14.1312457138014,-26.6826870736875,
76.5972642426185));
#124846=CARTESIAN_POINT('Ctrl Pts',(14.0789302636491,-26.7130501592952,
76.7131194761497));
#124847=CARTESIAN_POINT('Ctrl Pts',(14.0273555139025,-26.7429833537376,
76.8273343908414));
#124848=CARTESIAN_POINT('Ctrl Pts',(13.9718738149409,-26.7744943394918,
76.9481305583616));
#124849=CARTESIAN_POINT('Ctrl Pts',(13.9121646105711,-26.8074240326092,
77.0754103633617));
#124850=CARTESIAN_POINT('Ctrl Pts',(13.853945332469,-26.8395320297204,77.1995141500777));
#124851=CARTESIAN_POINT('Ctrl Pts',(13.7917067792004,-26.8729889715799,
77.3297821645709));
#124852=CARTESIAN_POINT('Ctrl Pts',(13.7251177195424,-26.9076180913397,
77.4661043804653));
#124853=CARTESIAN_POINT('Ctrl Pts',(13.6768759464196,-26.9327058482096,
77.564865730221));
#124854=CARTESIAN_POINT('Ctrl Pts',(13.6263500841447,-26.9584082502522,
77.6668042823383));
#124855=CARTESIAN_POINT('Ctrl Pts',(13.5734030099601,-26.9846472826072,
77.7718708996449));
#124856=CARTESIAN_POINT('Ctrl Pts',(13.5418538420831,-27.0002821340026,
77.8344761407981));
#124857=CARTESIAN_POINT('Ctrl Pts',(13.5094448380976,-27.0161073377719,
77.8981918866019));
#124858=CARTESIAN_POINT('Ctrl Pts',(13.4761453842481,-27.0321046935293,
77.9630065865777));
#124859=CARTESIAN_POINT('Ctrl Pts',(13.401736918055,-27.0678511868629,78.1078366619823));
#124860=CARTESIAN_POINT('Ctrl Pts',(13.3228842458205,-27.1044596343681,
78.2581554643632));
#124861=CARTESIAN_POINT('Ctrl Pts',(13.2392274815457,-27.1417034896578,
78.4138206406379));
#124862=CARTESIAN_POINT('Ctrl Pts',(13.157955967163,-27.1778854355779,78.5650474388788));
#124863=CARTESIAN_POINT('Ctrl Pts',(13.0721503004761,-27.2146672208158,
78.7213201750395));
#124864=CARTESIAN_POINT('Ctrl Pts',(12.9814542693971,-27.2518065680707,
78.8824858105204));
#124865=CARTESIAN_POINT('Ctrl Pts',(12.932154265861,-27.2719945512626,78.9700912581302));
#124866=CARTESIAN_POINT('Ctrl Pts',(12.8814088429243,-27.292287566873,79.0591420216869));
#124867=CARTESIAN_POINT('Ctrl Pts',(12.8291575446481,-27.3126419570784,
79.1496104415529));
#124868=CARTESIAN_POINT('Ctrl Pts',(12.7805568352331,-27.3315742675917,
79.2337581953925));
#124869=CARTESIAN_POINT('Ctrl Pts',(12.7306532976543,-27.3505596547148,
79.3191324189104));
#124870=CARTESIAN_POINT('Ctrl Pts',(12.6793964907654,-27.3695601212508,
79.4057090153605));
#124871=CARTESIAN_POINT('Ctrl Pts',(12.653768087321,-27.3790603545189,79.4489973135856));
#124872=CARTESIAN_POINT('Ctrl Pts',(12.6278013340391,-27.38856435764,79.4925861857176));
#124873=CARTESIAN_POINT('Ctrl Pts',(12.6014897686547,-27.3980670555022,
79.5364724335371));
#124874=CARTESIAN_POINT('Ctrl Pts',(12.5883339859625,-27.4028184044332,
79.5584155574468));
#124875=CARTESIAN_POINT('Ctrl Pts',(12.5750919981576,-27.4075694270496,
79.5804330240537));
#124876=CARTESIAN_POINT('Ctrl Pts',(12.5617629862613,-27.4123194787753,
79.6025244237642));
#124877=CARTESIAN_POINT('Ctrl Pts',(12.5550984803131,-27.4146945046381,
79.6135701236194));
#124878=CARTESIAN_POINT('Ctrl Pts',(12.5484122182105,-27.4170692877783,
79.624634306671));
#124879=CARTESIAN_POINT('Ctrl Pts',(12.5417040969433,-27.4194437464173,
79.6357169209848));
#124880=CARTESIAN_POINT('Ctrl Pts',(12.5349959756761,-27.4218182050562,
79.6467995352986));
#124881=CARTESIAN_POINT('Ctrl Pts',(12.5272565546748,-27.4245472203708,
79.6595629761372));
#124882=CARTESIAN_POINT('Ctrl Pts',(12.5215140521559,-27.4265660666789,
79.6690200053765));
#124883=CARTESIAN_POINT('Ctrl Pts',(12.4895955835732,-27.4377873908745,
79.7215848740324));
#124884=CARTESIAN_POINT('Ctrl Pts',(12.457820218365,-27.4487628534799,79.773516535532));
#124885=CARTESIAN_POINT('Ctrl Pts',(12.4262002963281,-27.459497966512,79.8248182666612));
#124886=CARTESIAN_POINT('Ctrl Pts',(12.3102039383348,-27.4988792784873,
80.0130165159416));
#124887=CARTESIAN_POINT('Ctrl Pts',(12.1963034536775,-27.5350256110503,
80.1927364770569));
#124888=CARTESIAN_POINT('Ctrl Pts',(12.0850861408458,-27.568225675283,80.3641442765277));
#124889=CARTESIAN_POINT('Ctrl Pts',(11.9732291346555,-27.6016166977403,
80.5365379695448));
#124890=CARTESIAN_POINT('Ctrl Pts',(11.8640862653525,-27.6320278504697,
80.7005239682551));
#124891=CARTESIAN_POINT('Ctrl Pts',(11.7582030352789,-27.6597560315795,
80.8562805060204));
#124892=CARTESIAN_POINT('Ctrl Pts',(11.6520919177104,-27.687543890749,81.0123722712543));
#124893=CARTESIAN_POINT('Ctrl Pts',(11.549254468362,-27.7126376176627,81.1601994727069));
#124894=CARTESIAN_POINT('Ctrl Pts',(11.4501877554424,-27.7353332633818,
81.2999452956347));
#124895=CARTESIAN_POINT('Ctrl Pts',(11.4098317685165,-27.7445786007401,
81.3568723949279));
#124896=CARTESIAN_POINT('Ctrl Pts',(11.3701009140853,-27.7534259261453,
81.4124584548637));
#124897=CARTESIAN_POINT('Ctrl Pts',(11.3310263390456,-27.7618948858452,
81.466715831748));
#124898=CARTESIAN_POINT('Ctrl Pts',(11.2369289677487,-27.782289396715,81.5973756414347));
#124899=CARTESIAN_POINT('Ctrl Pts',(11.1466408422166,-27.8004908673477,
81.7203306552685));
#124900=CARTESIAN_POINT('Ctrl Pts',(11.0605649669356,-27.8167694213073,
81.8357518458604));
#124901=CARTESIAN_POINT('Ctrl Pts',(10.9902945781751,-27.830058862878,81.9299790832555));
#124902=CARTESIAN_POINT('Ctrl Pts',(10.9228306223314,-27.8420665444725,
82.0191852159257));
#124903=CARTESIAN_POINT('Ctrl Pts',(10.8583685231998,-27.8529305219237,
82.1034591713792));
#124904=CARTESIAN_POINT('Ctrl Pts',(10.8270363034821,-27.8582110283468,
82.1444210718496));
#124905=CARTESIAN_POINT('Ctrl Pts',(10.7964129542786,-27.8632212016962,
82.1842176753842));
#124906=CARTESIAN_POINT('Ctrl Pts',(10.7665191005272,-27.8679760853578,
82.2228587759127));
#124907=CARTESIAN_POINT('Ctrl Pts',(10.7515721736515,-27.8703535271885,
82.2421793261769));
#124908=CARTESIAN_POINT('Ctrl Pts',(10.7368076068207,-27.8726671465973,
82.2612109899799));
#124909=CARTESIAN_POINT('Ctrl Pts',(10.7222278619699,-27.8749187597034,
82.2799549691001));
#124910=CARTESIAN_POINT('Ctrl Pts',(10.7149379895445,-27.8760445662565,
82.2893269586601));
#124911=CARTESIAN_POINT('Ctrl Pts',(10.7076943217371,-27.8771548712339,
82.2986270263737));
#124912=CARTESIAN_POINT('Ctrl Pts',(10.7004971602225,-27.8782498996363,
82.3078553194231));
#124913=CARTESIAN_POINT('Ctrl Pts',(10.6968985794652,-27.8787974138375,
82.3124694659478));
#124914=CARTESIAN_POINT('Ctrl Pts',(10.6933116252264,-27.8793411088949,
82.3170656687637));
#124915=CARTESIAN_POINT('Ctrl Pts',(10.6897363347735,-27.8798810126956,
82.3216439461571));
#124916=CARTESIAN_POINT('Ctrl Pts',(10.6861610443206,-27.8804209164962,
82.3262222235505));
#124917=CARTESIAN_POINT('Ctrl Pts',(10.6837523045838,-27.8807839390271,
82.3293056274602));
#124918=CARTESIAN_POINT('Ctrl Pts',(10.6790454917869,-27.881489378141,82.335325020227));
#124919=CARTESIAN_POINT('Ctrl Pts',(10.5292564252777,-27.9039391909764,
82.5268854800133));
#124920=CARTESIAN_POINT('Ctrl Pts',(10.3793236309,-27.9229735484718,82.7133951355727));
#124921=CARTESIAN_POINT('Ctrl Pts',(10.2295971511516,-27.9387427501686,
82.8949065634546));
#124922=CARTESIAN_POINT('Ctrl Pts',(10.0307485928665,-27.9596854920803,
83.1359680363966));
#124923=CARTESIAN_POINT('Ctrl Pts',(9.83226532157518,-27.9748691529642,
83.3682129997933));
#124924=CARTESIAN_POINT('Ctrl Pts',(9.63493943597387,-27.9847086285095,
83.5918178861406));
#124925=CARTESIAN_POINT('Ctrl Pts',(9.47468391907635,-27.992699623886,83.7734155337742));
#124926=CARTESIAN_POINT('Ctrl Pts',(9.3151911459906,-27.9971661307136,83.9493151099293));
#124927=CARTESIAN_POINT('Ctrl Pts',(9.15686623641873,-27.9983390449081,
84.1196252339744));
#124928=CARTESIAN_POINT('Ctrl Pts',(8.95410134268431,-27.9998411826489,
84.3377394542653));
#124929=CARTESIAN_POINT('Ctrl Pts',(8.753253301804,-27.9959415990584,84.5466860940465));
#124930=CARTESIAN_POINT('Ctrl Pts',(8.55512279127164,-27.9871686188701,
84.7467468079522));
#124931=CARTESIAN_POINT('Ctrl Pts',(8.41451149554765,-27.9809425201823,
84.8887279502314));
#124932=CARTESIAN_POINT('Ctrl Pts',(8.27526800369909,-27.9722620931865,
85.0262340307359));
#124933=CARTESIAN_POINT('Ctrl Pts',(8.13766371803501,-27.9613185539669,
85.1593713327432));
#124934=CARTESIAN_POINT('Ctrl Pts',(7.95933531701222,-27.9471362642138,
85.3319107421728));
#124935=CARTESIAN_POINT('Ctrl Pts',(7.78376096012283,-27.9291534161313,
85.4971131132777));
#124936=CARTESIAN_POINT('Ctrl Pts',(7.61149075125023,-27.907799918818,85.6552372156831));
#124937=CARTESIAN_POINT('Ctrl Pts',(7.54331604267503,-27.899349424296,85.717813703346));
#124938=CARTESIAN_POINT('Ctrl Pts',(7.47565842835141,-27.8903710309361,
85.779281690035));
#124939=CARTESIAN_POINT('Ctrl Pts',(7.40855047216036,-27.8808912939398,
85.8396573807588));
#124940=CARTESIAN_POINT('Ctrl Pts',(7.37499649406485,-27.8761514254417,
85.8698452261206));
#124941=CARTESIAN_POINT('Ctrl Pts',(7.34157992495571,-27.8712862210344,
85.8997599913057));
#124942=CARTESIAN_POINT('Ctrl Pts',(7.30830474045628,-27.8662989906185,
85.9294037186682));
#124943=CARTESIAN_POINT('Ctrl Pts',(7.29166714820657,-27.8638053754106,
85.9442255823494));
#124944=CARTESIAN_POINT('Ctrl Pts',(7.27506490174535,-27.8612812537005,
85.9589796861728));
#124945=CARTESIAN_POINT('Ctrl Pts',(7.25849849392102,-27.8587270387572,
85.9736662847182));
#124946=CARTESIAN_POINT('Ctrl Pts',(7.2430603299745,-27.8563467768762,85.9873526625114));
#124947=CARTESIAN_POINT('Ctrl Pts',(7.22880377733608,-27.8541223276371,
85.999964745298));
#124948=CARTESIAN_POINT('Ctrl Pts',(7.21251286320198,-27.8515454028678,
86.0143422730012));
#124949=CARTESIAN_POINT('Ctrl Pts',(7.21132229907794,-27.8513570773904,
86.015393004012));
#124950=CARTESIAN_POINT('Ctrl Pts',(7.21012085734284,-27.8511668541592,
86.0164531517114));
#124951=CARTESIAN_POINT('Ctrl Pts',(7.20890727669436,-27.8509745272833,
86.0175238184091));
#124952=CARTESIAN_POINT('Ctrl Pts',(7.19212008865412,-27.8483141128838,
86.0323341099262));
#124953=CARTESIAN_POINT('Ctrl Pts',(7.17532881181902,-27.8456172063041,
86.0471115463409));
#124954=CARTESIAN_POINT('Ctrl Pts',(7.158533668051,-27.842883885024,86.0618561108206));
#124955=CARTESIAN_POINT('Ctrl Pts',(6.88863339131123,-27.7989590350725,
86.29880329558));
#124956=CARTESIAN_POINT('Ctrl Pts',(6.61773200244552,-27.7456271040454,
86.5272593346919));
#124957=CARTESIAN_POINT('Ctrl Pts',(6.34672839360205,-27.6832456329547,
86.7472348456383));
#124958=CARTESIAN_POINT('Ctrl Pts',(6.29242554817431,-27.6707458312117,
86.7913128423107));
#124959=CARTESIAN_POINT('Ctrl Pts',(6.2381186830817,-27.657882802054,86.8350504199427));
#124960=CARTESIAN_POINT('Ctrl Pts',(6.18381514071596,-27.6446596060459,
86.8784477931218));
#124961=CARTESIAN_POINT('Ctrl Pts',(5.91249637583059,-27.5785920706245,
87.0952756680128));
#124962=CARTESIAN_POINT('Ctrl Pts',(5.64125923124188,-27.5035299731285,
87.3036091507583));
#124963=CARTESIAN_POINT('Ctrl Pts',(5.37099723920783,-27.4198773606199,
87.5035499473392));
#124964=CARTESIAN_POINT('Ctrl Pts',(5.30487001435339,-27.3994093877638,
87.5524711068169));
#124965=CARTESIAN_POINT('Ctrl Pts',(5.23880123116859,-27.378427332939,87.6008899271453));
#124966=CARTESIAN_POINT('Ctrl Pts',(5.17280406231213,-27.3569375245363,
87.6488081242018));
#124967=CARTESIAN_POINT('Ctrl Pts',(4.99448569078833,-27.2988740090079,
87.7782787517077));
#124968=CARTESIAN_POINT('Ctrl Pts',(4.81669010245746,-27.2371030146491,
87.9040944119933));
#124969=CARTESIAN_POINT('Ctrl Pts',(4.63967111765496,-27.1717492493324,
88.0263075399396));
#124970=CARTESIAN_POINT('Ctrl Pts',(4.49833896028284,-27.1195707293002,
88.1238826393061));
#124971=CARTESIAN_POINT('Ctrl Pts',(4.35750189809531,-27.0651085905577,
88.2191613816254));
#124972=CARTESIAN_POINT('Ctrl Pts',(4.21728870287524,-27.0084307638643,
88.3121724045632));
#124973=CARTESIAN_POINT('Ctrl Pts',(4.18619065250119,-26.9958601216588,
88.3328014293289));
#124974=CARTESIAN_POINT('Ctrl Pts',(4.15512327995206,-26.9831804716333,
88.3533189145229));
#124975=CARTESIAN_POINT('Ctrl Pts',(4.12408798694208,-26.9703925946575,
88.3737251833332));
#124976=CARTESIAN_POINT('Ctrl Pts',(4.08515816083398,-26.9543518301381,
88.3993222510343));
#124977=CARTESIAN_POINT('Ctrl Pts',(4.04627881053809,-26.938140774818,88.4247443251059));
#124978=CARTESIAN_POINT('Ctrl Pts',(4.00745267935975,-26.9217608738289,
88.4499921950428));
#124979=CARTESIAN_POINT('Ctrl Pts',(3.97256330064477,-26.9070418031521,
88.4726800722337));
#124980=CARTESIAN_POINT('Ctrl Pts',(3.93771690956971,-26.8921864059705,
88.4952272722382));
#124981=CARTESIAN_POINT('Ctrl Pts',(3.90291546573732,-26.8771956934937,
88.5176343908025));
#124982=CARTESIAN_POINT('Ctrl Pts',(3.88551474382113,-26.8697003372553,
88.5288379500847));
#124983=CARTESIAN_POINT('Ctrl Pts',(3.86812525873783,-26.8621711521931,
88.5400064890187));
#124984=CARTESIAN_POINT('Ctrl Pts',(3.85074725861327,-26.8546082721214,
88.5511400802268));
#124985=CARTESIAN_POINT('Ctrl Pts',(3.8333692584887,-26.8470453920496,88.5622736714349));
#124986=CARTESIAN_POINT('Ctrl Pts',(3.81691551857993,-26.8398501240272,
88.5727904156976));
#124987=CARTESIAN_POINT('Ctrl Pts',(3.79864795992528,-26.8318186793894,
88.584436084294));
#124988=CARTESIAN_POINT('Ctrl Pts',(3.55361646487997,-26.7240890739074,
88.7406450031161));
#124989=CARTESIAN_POINT('Ctrl Pts',(3.30660909204321,-26.6077717064107,
88.8926491666568));
#124990=CARTESIAN_POINT('Ctrl Pts',(3.05812708824525,-26.4827613689761,
89.0402227961973));
#124991=CARTESIAN_POINT('Ctrl Pts',(2.79976957900169,-26.3527827028528,
89.1936614950784));
#124992=CARTESIAN_POINT('Ctrl Pts',(2.53981823571299,-26.2134059636382,
89.3423100176492));
#124993=CARTESIAN_POINT('Ctrl Pts',(2.27889797695919,-26.064512216502,89.4859651894051));
#124994=CARTESIAN_POINT('Ctrl Pts',(2.18168862608131,-26.0090398488981,
89.5394858553102));
#124995=CARTESIAN_POINT('Ctrl Pts',(2.08434511443063,-25.9522468182292,
89.592313669351));
#124996=CARTESIAN_POINT('Ctrl Pts',(1.98690080831514,-25.8941281785326,
89.6444390289528));
#124997=CARTESIAN_POINT('Ctrl Pts',(1.72144171495565,-25.7358005961816,
89.7864396368133));
#124998=CARTESIAN_POINT('Ctrl Pts',(1.45523313112368,-25.5676326544185,
89.9232247222671));
#124999=CARTESIAN_POINT('Ctrl Pts',(1.18899435962219,-25.3894973442791,
90.0546604194468));
#125000=CARTESIAN_POINT('Ctrl Pts',(1.09880780979761,-25.3291552350784,
90.099183356454));
#125001=CARTESIAN_POINT('Ctrl Pts',(1.00861796167179,-25.2676697047823,
90.1430927451011));
#125002=CARTESIAN_POINT('Ctrl Pts',(0.918453200391034,-25.2050367529372,
90.1863842595382));
#125003=CARTESIAN_POINT('Ctrl Pts',(0.683510322579977,-25.0418336817674,
90.2991892272681));
#125004=CARTESIAN_POINT('Ctrl Pts',(0.448737285098761,-24.8708383520767,
90.4077974543601));
#125005=CARTESIAN_POINT('Ctrl Pts',(0.214737593717178,-24.6920330679193,
90.5121351745855));
#125006=CARTESIAN_POINT('Origin',(4.0920067733132,-24.696099145329,99.1931566746257));
#125007=CARTESIAN_POINT('Ctrl Pts',(1.36163900653909,-23.0868350636,90.18857710052));
#125008=CARTESIAN_POINT('Ctrl Pts',(1.33629755400909,-23.0868350636,90.1973864042999));
#125009=CARTESIAN_POINT('Ctrl Pts',(1.18340487400909,-23.0868350636,90.24974235902));
#125010=CARTESIAN_POINT('Ctrl Pts',(0.88596103596909,-23.0868350636,90.3426923710499));
#125011=CARTESIAN_POINT('Ctrl Pts',(0.460669337409092,-23.0868350636,90.4582699612699));
#125012=CARTESIAN_POINT('Ctrl Pts',(0.0027641290990888,-23.0868350636,90.5675700300099));
#125013=CARTESIAN_POINT('Ctrl Pts',(-0.472046391840912,-23.0868350636,90.6688291289299));
#125014=CARTESIAN_POINT('Ctrl Pts',(-0.870003116440913,-23.0868350636,90.74660632017));
#125015=CARTESIAN_POINT('Ctrl Pts',(-1.10812696320091,-23.0868350636,90.7911946280099));
#125016=CARTESIAN_POINT('Ctrl Pts',(-1.18647142001091,-23.0868350636,90.80570636327));
#125017=CARTESIAN_POINT('Ctrl Pts',(1.53839445242909,-21.82055408281,90.69703431954));
#125018=CARTESIAN_POINT('Ctrl Pts',(1.51147927430909,-21.82055408281,90.7063904444401));
#125019=CARTESIAN_POINT('Ctrl Pts',(1.34927535701909,-21.82055408281,90.76193375724));
#125020=CARTESIAN_POINT('Ctrl Pts',(1.03585658491909,-21.82055408281,90.8598359761601));
#125021=CARTESIAN_POINT('Ctrl Pts',(0.592965254849087,-21.82055408281,90.98015107536));
#125022=CARTESIAN_POINT('Ctrl Pts',(0.120694188719086,-21.82055408281,91.09284990719));
#125023=CARTESIAN_POINT('Ctrl Pts',(-0.364876444990915,-21.82055408281,
91.19638270328));
#125024=CARTESIAN_POINT('Ctrl Pts',(-0.768844937710913,-21.82055408281,
91.27532498826));
#125025=CARTESIAN_POINT('Ctrl Pts',(-1.00940150886091,-21.82055408281,91.3203684735299));
#125026=CARTESIAN_POINT('Ctrl Pts',(-1.08843051722092,-21.82055408281,91.33500702056));
#125027=CARTESIAN_POINT('Ctrl Pts',(1.25251305092909,-20.75508811698,89.87466383106));
#125028=CARTESIAN_POINT('Ctrl Pts',(1.22814319113909,-20.75508811698,89.88313553631));
#125029=CARTESIAN_POINT('Ctrl Pts',(1.08099911855909,-20.75508811698,89.93352366767));
#125030=CARTESIAN_POINT('Ctrl Pts',(0.793417946619087,-20.75508811698,90.0234162672001));
#125031=CARTESIAN_POINT('Ctrl Pts',(0.378991976119086,-20.75508811698,90.1360689959401));
#125032=CARTESIAN_POINT('Ctrl Pts',(-0.0700439837509129,-20.75508811698,
90.24327072329));
#125033=CARTESIAN_POINT('Ctrl Pts',(-0.538211384980914,-20.75508811698,
90.34312607832));
#125034=CARTESIAN_POINT('Ctrl Pts',(-0.932456541100915,-20.75508811698,
90.42018395951));
#125035=CARTESIAN_POINT('Ctrl Pts',(-1.16907846314091,-20.75508811698,90.46449124816));
#125036=CARTESIAN_POINT('Ctrl Pts',(-1.24700028889091,-20.75508811698,90.47892469189));
#125037=CARTESIAN_POINT('Ctrl Pts',(0.809841866079087,-21.03031417726,88.60126963119));
#125038=CARTESIAN_POINT('Ctrl Pts',(0.78941328779909,-21.03031417726,88.60837186262));
#125039=CARTESIAN_POINT('Ctrl Pts',(0.665588533179087,-21.03031417726,88.6507774870499));
#125040=CARTESIAN_POINT('Ctrl Pts',(0.418015424089088,-21.03031417726,88.72826764384));
#125041=CARTESIAN_POINT('Ctrl Pts',(0.0476664532790877,-21.03031417726,
88.8290556252));
#125042=CARTESIAN_POINT('Ctrl Pts',(-0.36539125839091,-21.03031417726,88.9277453971099));
#125043=CARTESIAN_POINT('Ctrl Pts',(-0.80661073819091,-21.03031417726,89.02190644259));
#125044=CARTESIAN_POINT('Ctrl Pts',(-1.18579985743091,-21.03031417726,89.09604643108));
#125045=CARTESIAN_POINT('Ctrl Pts',(-1.41632919778091,-21.03031417726,89.13921376088));
#125046=CARTESIAN_POINT('Ctrl Pts',(-1.49253661387091,-21.03031417726,89.15332961377));
#125047=CARTESIAN_POINT('',(-1.00776358327158,-22.5000393642437,90.8939758070015));
#125048=CARTESIAN_POINT('',(-1.28514186019175,-21.0000000000091,89.4198403356738));
#125049=CARTESIAN_POINT('Origin',(-1.28514465536091,-22.5,89.4198456395));
#125050=CARTESIAN_POINT('Ctrl Pts',(0.756578721069087,-21.00000000034,88.93560161898));
#125051=CARTESIAN_POINT('Ctrl Pts',(0.653003740499087,-21.00000000034,88.96920956699));
#125052=CARTESIAN_POINT('Ctrl Pts',(0.429939155889087,-20.99999999984,89.03708519515));
#125053=CARTESIAN_POINT('Ctrl Pts',(0.0394814676090878,-21.00000000004,
89.14048085679));
#125054=CARTESIAN_POINT('Ctrl Pts',(-0.384836251440913,-20.99999999999,
89.23943098501));
#125055=CARTESIAN_POINT('Ctrl Pts',(-0.831136955090912,-21.,89.33289755051));
#125056=CARTESIAN_POINT('Ctrl Pts',(-1.13262274867091,-21.,89.39113259042));
#125057=CARTESIAN_POINT('Ctrl Pts',(-1.28513819680091,-21.00000000001,89.41983964605));
#125058=CARTESIAN_POINT('Ctrl Pts',(1.21025704777005,-22.7988943080295,
90.3337993035096));
#125059=CARTESIAN_POINT('Ctrl Pts',(1.11883424343817,-22.7853130337259,
90.3663681552013));
#125060=CARTESIAN_POINT('Ctrl Pts',(1.02596857595066,-22.7717048756296,
90.3976542109587));
#125061=CARTESIAN_POINT('Ctrl Pts',(0.931813726174482,-22.7580801782437,
90.4277751577328));
#125062=CARTESIAN_POINT('Ctrl Pts',(0.840202022289285,-22.7448234873202,
90.4570825302491));
#125063=CARTESIAN_POINT('Ctrl Pts',(0.747372442868353,-22.7315511422234,
90.485287389861));
#125064=CARTESIAN_POINT('Ctrl Pts',(0.653326688054345,-22.7182727250757,
90.5125156428743));
#125065=CARTESIAN_POINT('Ctrl Pts',(0.602522516857858,-22.7110996317305,
90.5272245346281));
#125066=CARTESIAN_POINT('Ctrl Pts',(0.551363182508309,-22.7039247670197,
90.5416492614627));
#125067=CARTESIAN_POINT('Ctrl Pts',(0.499847108697976,-22.696749642616,
90.5558157707814));
#125068=CARTESIAN_POINT('Ctrl Pts',(0.395200362092091,-22.6821745135387,
90.5845927912591));
#125069=CARTESIAN_POINT('Ctrl Pts',(0.289081810103877,-22.6675983181277,
90.6123016588467));
#125070=CARTESIAN_POINT('Ctrl Pts',(0.181529294844612,-22.653033691233,
90.6390726080421));
#125071=CARTESIAN_POINT('Ctrl Pts',(0.133050478942922,-22.6464687507088,
90.6511394938274));
#125072=CARTESIAN_POINT('Ctrl Pts',(0.0842802116893185,-22.6399061596043,
90.6630165007185));
#125073=CARTESIAN_POINT('Ctrl Pts',(0.0352214027325707,-22.6333470682069,
90.6747190033485));
#125074=CARTESIAN_POINT('Ctrl Pts',(-0.0778601668898635,-22.6182282268349,
90.7016935140235));
#125075=CARTESIAN_POINT('Ctrl Pts',(-0.192474304323062,-22.60312799504,
90.7277376446242));
#125076=CARTESIAN_POINT('Ctrl Pts',(-0.30858246594518,-22.58806032326,90.7530081683137));
#125077=CARTESIAN_POINT('Ctrl Pts',(-0.35395508725891,-22.5821721948442,
90.7628833561192));
#125078=CARTESIAN_POINT('Ctrl Pts',(-0.39955594211883,-22.576289036217,
90.7726409553093));
#125079=CARTESIAN_POINT('Ctrl Pts',(-0.445383055984327,-22.5704116694695,
90.782292479886));
#125080=CARTESIAN_POINT('Ctrl Pts',(-0.566668934225101,-22.5548566513245,
90.8078361708562));
#125081=CARTESIAN_POINT('Ctrl Pts',(-0.689539096038413,-22.5393422305868,
90.832633381094));
#125082=CARTESIAN_POINT('Ctrl Pts',(-0.813956921433526,-22.5238833956251,
90.856869529174));
#125083=CARTESIAN_POINT('Ctrl Pts',(-0.852043593115456,-22.5191511511103,
90.8642886768069));
#125084=CARTESIAN_POINT('Ctrl Pts',(-0.890275349954781,-22.5144241126308,
90.8716556097766));
#125085=CARTESIAN_POINT('Ctrl Pts',(-0.928651288068415,-22.5097027021494,
90.8789766224509));
#125086=CARTESIAN_POINT('Ctrl Pts',(-0.954936548950239,-22.5064688136157,
90.8839910856152));
#125087=CARTESIAN_POINT('Ctrl Pts',(-0.981289452544953,-22.5032375653443,
90.8889840167774));
#125088=CARTESIAN_POINT('Ctrl Pts',(-1.00770989807145,-22.500009091799,
90.8939570738426));
#125089=CARTESIAN_POINT('Ctrl Pts',(-6.25976359311891,-21.0101086723,86.80605952089));
#125090=CARTESIAN_POINT('Ctrl Pts',(-6.20991132790791,-20.99698855152,86.80345236223));
#125091=CARTESIAN_POINT('Ctrl Pts',(-6.05600621273991,-20.963809122,86.7954056045899));
#125092=CARTESIAN_POINT('Ctrl Pts',(-5.89752936873391,-20.95187439198,86.78709081339));
#125093=CARTESIAN_POINT('Ctrl Pts',(-5.79082527707091,-20.95374691807,86.7814767506699));
#125094=CARTESIAN_POINT('Ctrl Pts',(-6.36253180399691,-21.23537119951,85.92231661493));
#125095=CARTESIAN_POINT('Ctrl Pts',(-6.31814829585091,-21.22933598386,85.92215256487));
#125096=CARTESIAN_POINT('Ctrl Pts',(-6.18252552805991,-21.21729456478,85.92204034661));
#125097=CARTESIAN_POINT('Ctrl Pts',(-6.04735840947691,-21.22429001182,85.92328042834));
#125098=CARTESIAN_POINT('Ctrl Pts',(-5.95842995311291,-21.23703750146,85.9247493404201));
#125099=CARTESIAN_POINT('Ctrl Pts',(-6.62085321050291,-20.57398746247,85.34080893105));
#125100=CARTESIAN_POINT('Ctrl Pts',(-6.55589593677591,-20.56692097113,85.33267979129));
#125101=CARTESIAN_POINT('Ctrl Pts',(-6.35811797501791,-20.55529791815,85.3082833307501));
#125102=CARTESIAN_POINT('Ctrl Pts',(-6.16331684750191,-20.57308609787,85.2855875247701));
#125103=CARTESIAN_POINT('Ctrl Pts',(-6.03626442425791,-20.59714856909,85.2714418523801));
#125104=CARTESIAN_POINT('Ctrl Pts',(-6.75819841819991,-19.73395935219,85.68403218053));
#125105=CARTESIAN_POINT('Ctrl Pts',(-6.66864877990991,-19.71884937032,85.6660562680899));
#125106=CARTESIAN_POINT('Ctrl Pts',(-6.39481433463891,-19.68647718414,85.61115271986));
#125107=CARTESIAN_POINT('Ctrl Pts',(-6.12127282288791,-19.69536718519,85.55665329315));
#125108=CARTESIAN_POINT('Ctrl Pts',(-5.94100799531891,-19.71907212904,85.52091066777));
#125109=CARTESIAN_POINT('',(-6.21291707614173,-21.0225426194874,86.5058300720823));
#125110=CARTESIAN_POINT('',(-6.5468225705719,-20.0375665162624,85.5854070569733));
#125111=CARTESIAN_POINT('Origin',(-6.37317299992691,-20.0375768096,86.57021276289));
#125112=CARTESIAN_POINT('Origin',(-6.11241447398738,-22.6085115286827,85.5088316030536));
#125113=CARTESIAN_POINT('Origin',(-5.9375029357236,-22.6813923363259,86.5223306616674));
#125114=CARTESIAN_POINT('Origin',(155.459720656869,-21.,57.01928063319));
#125115=CARTESIAN_POINT('',(-5.70733054565492,-21.0000000000039,87.0513884694139));
#125116=CARTESIAN_POINT('Origin',(-2.02513312664091,-21.00000000001,85.48888938658));
#125117=CARTESIAN_POINT('Origin',(27.4324635166691,-21.,72.98888938658));
#125118=CARTESIAN_POINT('Ctrl Pts',(-9.31134522286991,-23.33493700796,85.4554385022599));
#125119=CARTESIAN_POINT('Ctrl Pts',(-9.28499288372891,-23.28758267006,85.50448598234));
#125120=CARTESIAN_POINT('Ctrl Pts',(-9.19047003471491,-23.12655314471,85.66856307458));
#125121=CARTESIAN_POINT('Ctrl Pts',(-9.0098363850229,-22.86492193384,85.9192200995));
#125122=CARTESIAN_POINT('Ctrl Pts',(-8.75884674055692,-22.5625884577,86.18264969547));
#125123=CARTESIAN_POINT('Ctrl Pts',(-8.49981345722091,-22.29401394629,86.39371900856));
#125124=CARTESIAN_POINT('Ctrl Pts',(-8.23984516015692,-22.05730715509,86.5593464839501));
#125125=CARTESIAN_POINT('Ctrl Pts',(-7.98398752470691,-21.85037332061,86.6857732052299));
#125126=CARTESIAN_POINT('Ctrl Pts',(-7.73566246859491,-21.67095709777,86.77861968057));
#125127=CARTESIAN_POINT('Ctrl Pts',(-7.4973815228969,-21.51699185038,86.84277779335));
#125128=CARTESIAN_POINT('Ctrl Pts',(-7.27102440704691,-21.386549034,86.88261210473));
#125129=CARTESIAN_POINT('Ctrl Pts',(-7.05796092602491,-21.2777684576,86.90210334931));
#125130=CARTESIAN_POINT('Ctrl Pts',(-6.85943856171691,-21.18897387943,86.9049046154299));
#125131=CARTESIAN_POINT('Ctrl Pts',(-6.67670949594691,-21.11854136463,86.8945490446601));
#125132=CARTESIAN_POINT('Ctrl Pts',(-6.51034314219591,-21.06450784875,86.87448931141));
#125133=CARTESIAN_POINT('Ctrl Pts',(-6.35927469654491,-21.02446132003,86.84768246284));
#125134=CARTESIAN_POINT('Ctrl Pts',(-6.22090131047091,-20.99596779402,86.81617682313));
#125135=CARTESIAN_POINT('Ctrl Pts',(-6.10579036137791,-20.97909200866,86.78485289377));
#125136=CARTESIAN_POINT('Ctrl Pts',(-6.03665598268991,-20.97241818335,86.7637314788699));
#125137=CARTESIAN_POINT('Ctrl Pts',(-6.00965782959991,-20.97035997432,86.7551449868199));
#125138=CARTESIAN_POINT('Ctrl Pts',(-8.4350370823869,-23.50439686796,85.39546316836));
#125139=CARTESIAN_POINT('Ctrl Pts',(-8.40984591433391,-23.45695203024,85.4275369102899));
#125140=CARTESIAN_POINT('Ctrl Pts',(-8.32096735149791,-23.295774178,85.53371911941));
#125141=CARTESIAN_POINT('Ctrl Pts',(-8.15928441830591,-23.0347138024,85.68952154615));
#125142=CARTESIAN_POINT('Ctrl Pts',(-7.94691404596691,-22.73437091822,85.84244627094));
#125143=CARTESIAN_POINT('Ctrl Pts',(-7.73767036549491,-22.46881609534,85.95482781482));
#125144=CARTESIAN_POINT('Ctrl Pts',(-7.53628477743691,-22.23597796783,86.0332540986199));
#125145=CARTESIAN_POINT('Ctrl Pts',(-7.34594773687791,-22.03361870056,86.08348958725));
#125146=CARTESIAN_POINT('Ctrl Pts',(-7.16868354027591,-21.85935874251,86.11059919866));
#125147=CARTESIAN_POINT('Ctrl Pts',(-7.0058965082479,-21.71100809099,86.11900317502));
#125148=CARTESIAN_POINT('Ctrl Pts',(-6.85853254906791,-21.58650051732,86.11268429546));
#125149=CARTESIAN_POINT('Ctrl Pts',(-6.7271147517219,-21.48381351961,86.09531628731));
#125150=CARTESIAN_POINT('Ctrl Pts',(-6.61192983251291,-21.40106859032,86.07035403811));
#125151=CARTESIAN_POINT('Ctrl Pts',(-6.51295284246591,-21.33639303747,86.0411390717));
#125152=CARTESIAN_POINT('Ctrl Pts',(-6.42933637844591,-21.28756622125,86.01071140893));
#125153=CARTESIAN_POINT('Ctrl Pts',(-6.35905177532891,-21.25197480454,85.98135155073));
#125154=CARTESIAN_POINT('Ctrl Pts',(-6.29925123788791,-21.22705685392,85.95440275155));
#125155=CARTESIAN_POINT('Ctrl Pts',(-6.25250368986091,-21.21251241075,85.93304888243));
#125156=CARTESIAN_POINT('Ctrl Pts',(-6.22536410282091,-21.20680909012,85.92116194032));
#125157=CARTESIAN_POINT('Ctrl Pts',(-6.21483774804991,-21.20505475476,85.91669105491));
#125158=CARTESIAN_POINT('Ctrl Pts',(-7.94712863324292,-23.04130212549,84.80577059714));
#125159=CARTESIAN_POINT('Ctrl Pts',(-7.93348145948992,-22.99410460291,84.82813589426));
#125160=CARTESIAN_POINT('Ctrl Pts',(-7.88483370393191,-22.83333209387,84.90272578354));
#125161=CARTESIAN_POINT('Ctrl Pts',(-7.79354048754991,-22.57071175704,85.01536177068));
#125162=CARTESIAN_POINT('Ctrl Pts',(-7.66920664452491,-22.26492904381,85.13152091435));
#125163=CARTESIAN_POINT('Ctrl Pts',(-7.54292338971691,-21.99112210811,85.2225126459599));
#125164=CARTESIAN_POINT('Ctrl Pts',(-7.41794917868591,-21.74771181434,85.29191458303));
#125165=CARTESIAN_POINT('Ctrl Pts',(-7.29656245333991,-21.53285130916,85.3429175053));
#125166=CARTESIAN_POINT('Ctrl Pts',(-7.18027985650291,-21.34450046779,85.3783690288999));
#125167=CARTESIAN_POINT('Ctrl Pts',(-7.07019785162091,-21.18080641974,85.40075005732));
#125168=CARTESIAN_POINT('Ctrl Pts',(-6.96711552884591,-21.04007919563,85.41228205909));
#125169=CARTESIAN_POINT('Ctrl Pts',(-6.8715811492079,-20.9207398517,85.41499958511));
#125170=CARTESIAN_POINT('Ctrl Pts',(-6.78405515274891,-20.82146262628,85.41078684325));
#125171=CARTESIAN_POINT('Ctrl Pts',(-6.70493563279891,-20.74105462321,85.40146619008));
#125172=CARTESIAN_POINT('Ctrl Pts',(-6.63423230918392,-20.6779990968,85.3887722936999));
#125173=CARTESIAN_POINT('Ctrl Pts',(-6.57118663989192,-20.63023288573,85.37412460379));
#125174=CARTESIAN_POINT('Ctrl Pts',(-6.51437698962792,-20.59554371159,85.35845791767));
#125175=CARTESIAN_POINT('Ctrl Pts',(-6.46773244924391,-20.57462824752,85.34399614184));
#125176=CARTESIAN_POINT('Ctrl Pts',(-6.4399101321309,-20.56627276126,85.33475936856));
#125177=CARTESIAN_POINT('Ctrl Pts',(-6.42905981978291,-20.56368800922,85.33107841599));
#125178=CARTESIAN_POINT('Ctrl Pts',(-8.35461977250192,-22.42686803145,84.29912753498));
#125179=CARTESIAN_POINT('Ctrl Pts',(-8.35090371515592,-22.37999864658,84.3291380087));
#125180=CARTESIAN_POINT('Ctrl Pts',(-8.3352682829919,-22.2197639469,84.4312666422201));
#125181=CARTESIAN_POINT('Ctrl Pts',(-8.29265977640492,-21.95507385353,84.5972798544901));
#125182=CARTESIAN_POINT('Ctrl Pts',(-8.21429839509991,-21.64207357524,84.7886168945501));
#125183=CARTESIAN_POINT('Ctrl Pts',(-8.11793979130091,-21.35731773644,84.95774354849));
#125184=CARTESIAN_POINT('Ctrl Pts',(-8.00780433526691,-21.0998802927,85.1056754455199));
#125185=CARTESIAN_POINT('Ctrl Pts',(-7.8871493623079,-20.86843314535,85.2336070050299));
#125186=CARTESIAN_POINT('Ctrl Pts',(-7.7584013469319,-20.66138652028,85.34281089274));
#125187=CARTESIAN_POINT('Ctrl Pts',(-7.6234681520699,-20.47733485406,85.43437619933));
#125188=CARTESIAN_POINT('Ctrl Pts',(-7.48394160578191,-20.31508739811,85.50921378337));
#125189=CARTESIAN_POINT('Ctrl Pts',(-7.34124087217191,-20.17365372159,85.5680901662));
#125190=CARTESIAN_POINT('Ctrl Pts',(-7.19695408294091,-20.05244144602,85.61157853619));
#125191=CARTESIAN_POINT('Ctrl Pts',(-7.05316295123591,-19.95115962835,85.64023314414));
#125192=CARTESIAN_POINT('Ctrl Pts',(-6.91211759795191,-19.86922544959,85.6549470362799));
#125193=CARTESIAN_POINT('Ctrl Pts',(-6.77524376654791,-19.80530572163,85.6569888494899));
#125194=CARTESIAN_POINT('Ctrl Pts',(-6.64273512392691,-19.75765208834,85.64760597632));
#125195=CARTESIAN_POINT('Ctrl Pts',(-6.52782615951691,-19.72828355387,85.6297965517001));
#125196=CARTESIAN_POINT('Ctrl Pts',(-6.45735303533591,-19.71640917432,85.61387177559));
#125197=CARTESIAN_POINT('Ctrl Pts',(-6.42971964328091,-19.71272262543,85.6068342398));
#125198=CARTESIAN_POINT('Ctrl Pts',(-8.23395173885433,-22.5,84.5714980228305));
#125199=CARTESIAN_POINT('Ctrl Pts',(-8.21609487741167,-22.4068116375628,
84.6264627209876));
#125200=CARTESIAN_POINT('Ctrl Pts',(-8.19563729693556,-22.316592985688,
84.6786894498294));
#125201=CARTESIAN_POINT('Ctrl Pts',(-8.17316811952911,-22.2295003482217,
84.7281880289493));
#125202=CARTESIAN_POINT('Ctrl Pts',(-8.16832056716124,-22.2107107809253,
84.7388669670376));
#125203=CARTESIAN_POINT('Ctrl Pts',(-8.16337943807854,-22.1920665946948,
84.7494190677838));
#125204=CARTESIAN_POINT('Ctrl Pts',(-8.1583507236139,-22.1735691653645,
84.7598446655152));
#125205=CARTESIAN_POINT('Ctrl Pts',(-8.15717124053408,-22.1692306002961,
84.7622899855285));
#125206=CARTESIAN_POINT('Ctrl Pts',(-8.15598693964693,-22.1649001132339,
84.7647283456416));
#125207=CARTESIAN_POINT('Ctrl Pts',(-8.15479788384955,-22.1605776812017,
84.7671597802231));
#125208=CARTESIAN_POINT('Ctrl Pts',(-8.13546187554057,-22.09028780761,84.8066989165476));
#125209=CARTESIAN_POINT('Ctrl Pts',(-8.11487172341013,-22.0221309939227,
84.8444053993864));
#125210=CARTESIAN_POINT('Ctrl Pts',(-8.09327142289032,-21.9560751966656,
84.8803769914104));
#125211=CARTESIAN_POINT('Ctrl Pts',(-8.08428709169013,-21.9286002474302,
84.8953388525311));
#125212=CARTESIAN_POINT('Ctrl Pts',(-8.07512753850495,-21.9014883623869,
84.9100007460101));
#125213=CARTESIAN_POINT('Ctrl Pts',(-8.06580839124876,-21.8747356121368,
84.9243703323895));
#125214=CARTESIAN_POINT('Ctrl Pts',(-8.0630516692208,-21.8668218090929,
84.9286210384053));
#125215=CARTESIAN_POINT('Ctrl Pts',(-8.06028098400575,-21.8589394443409,
84.9328461531074));
#125216=CARTESIAN_POINT('Ctrl Pts',(-8.05749675602641,-21.8510884665214,
84.9370458299792));
#125217=CARTESIAN_POINT('Ctrl Pts',(-8.0321399670793,-21.7795872859154,
84.9752935312716));
#125218=CARTESIAN_POINT('Ctrl Pts',(-8.00566235701005,-21.7106926989649,
85.0114295529073));
#125219=CARTESIAN_POINT('Ctrl Pts',(-7.97833258524892,-21.6443451374452,
85.0455700289277));
#125220=CARTESIAN_POINT('Ctrl Pts',(-7.97262937400217,-21.6304996446119,
85.0526945065308));
#125221=CARTESIAN_POINT('Ctrl Pts',(-7.96688894881453,-21.6167649379167,
85.0597321527015));
#125222=CARTESIAN_POINT('Ctrl Pts',(-7.96111358632208,-21.6031402786599,
85.0666841259067));
#125223=CARTESIAN_POINT('Ctrl Pts',(-7.95655569992873,-21.5923877676058,
85.0721705874267));
#125224=CARTESIAN_POINT('Ctrl Pts',(-7.95197608277586,-21.5817039214224,
85.0776036540415));
#125225=CARTESIAN_POINT('Ctrl Pts',(-7.94737578754198,-21.5710882773315,
85.0829839580058));
#125226=CARTESIAN_POINT('Ctrl Pts',(-7.9189919510701,-21.5055897189562,
85.1161804508671));
#125227=CARTESIAN_POINT('Ctrl Pts',(-7.88982332230086,-21.442690854516,
85.1473666462622));
#125228=CARTESIAN_POINT('Ctrl Pts',(-7.86008135930843,-21.382298961433,
85.1766706697932));
#125229=CARTESIAN_POINT('Ctrl Pts',(-7.85605227772784,-21.3741177978663,
85.18064042463));
#125230=CARTESIAN_POINT('Ctrl Pts',(-7.85201262971751,-21.3659825840344,
85.1845756664998));
#125231=CARTESIAN_POINT('Ctrl Pts',(-7.84796289870774,-21.3578930384239,
85.1884767380341));
#125232=CARTESIAN_POINT('Ctrl Pts',(-7.84150175753707,-21.3449865772121,
85.1947007005242));
#125233=CARTESIAN_POINT('Ctrl Pts',(-7.83501500635689,-21.3321966058346,
85.2008376333083));
#125234=CARTESIAN_POINT('Ctrl Pts',(-7.82850443275156,-21.3195216462603,
85.2068890661026));
#125235=CARTESIAN_POINT('Ctrl Pts',(-7.79757970098214,-21.2593165477873,
85.2356329137769));
#125236=CARTESIAN_POINT('Ctrl Pts',(-7.76612012353127,-21.2017094488401,
85.2624463516647));
#125237=CARTESIAN_POINT('Ctrl Pts',(-7.73428116833124,-21.1465576100225,
85.2874725851855));
#125238=CARTESIAN_POINT('Ctrl Pts',(-7.7325816659029,-21.1436137105318,
85.288808437583));
#125239=CARTESIAN_POINT('Ctrl Pts',(-7.7308810746105,-21.1406767981643,
85.2901392012988));
#125240=CARTESIAN_POINT('Ctrl Pts',(-7.72917941540612,-21.1377468484969,
85.2914648991735));
#125241=CARTESIAN_POINT('Ctrl Pts',(-7.7207908080919,-21.1233031824875,
85.2980001436337));
#125242=CARTESIAN_POINT('Ctrl Pts',(-7.71237638460782,-21.1090291814494,
85.3044121822821));
#125243=CARTESIAN_POINT('Ctrl Pts',(-7.70393847386822,-21.094921727032,
85.3107038484261));
#125244=CARTESIAN_POINT('Ctrl Pts',(-7.67184699656642,-21.0412675622518,
85.3346326226784));
#125245=CARTESIAN_POINT('Ctrl Pts',(-7.63941827929952,-20.9900251945777,
85.3568192087859));
#125246=CARTESIAN_POINT('Ctrl Pts',(-7.60675049093118,-20.9410460703631,
85.3773953104988));
#125247=CARTESIAN_POINT('Ctrl Pts',(-7.59644995709495,-20.9256023825152,
85.3838831948184));
#125248=CARTESIAN_POINT('Ctrl Pts',(-7.58612566976997,-20.9103839950355,
85.3902108619718));
#125249=CARTESIAN_POINT('Ctrl Pts',(-7.57578194958231,-20.89538828511,85.3963815542268));
#125250=CARTESIAN_POINT('Ctrl Pts',(-7.54469546302359,-20.8503209469976,
85.4149266364955));
#125251=CARTESIAN_POINT('Ctrl Pts',(-7.51343434563313,-20.807267573974,
85.4320523721681));
#125252=CARTESIAN_POINT('Ctrl Pts',(-7.48210528888147,-20.7661744671713,
85.4478328690123));
#125253=CARTESIAN_POINT('Ctrl Pts',(-7.46993905493201,-20.7502164906821,
85.4539610208417));
#125254=CARTESIAN_POINT('Ctrl Pts',(-7.4577626784941,-20.7345546856784,
85.4598863994543));
#125255=CARTESIAN_POINT('Ctrl Pts',(-7.44558104050676,-20.7191833921662,
85.4656144281874));
#125256=CARTESIAN_POINT('Ctrl Pts',(-7.41595632336812,-20.6818017015572,
85.4795445114125));
#125257=CARTESIAN_POINT('Ctrl Pts',(-7.38630150114422,-20.6461400595536,
85.4923065228914));
#125258=CARTESIAN_POINT('Ctrl Pts',(-7.3566796152423,-20.6121347464711,
85.5039653794934));
#125259=CARTESIAN_POINT('Ctrl Pts',(-7.34275950248185,-20.5961547445857,
85.5094441865853));
#125260=CARTESIAN_POINT('Ctrl Pts',(-7.32884685141897,-20.5805413456455,
85.514679426976));
#125261=CARTESIAN_POINT('Ctrl Pts',(-7.31494462205447,-20.5652838484883,
85.5196794165379));
#125262=CARTESIAN_POINT('Ctrl Pts',(-7.28709819590326,-20.5347227955304,
85.5296944894045));
#125263=CARTESIAN_POINT('Ctrl Pts',(-7.25929464945993,-20.5055906815646,
85.5387654561346));
#125264=CARTESIAN_POINT('Ctrl Pts',(-7.23155263669677,-20.477820081468,
85.5469457005477));
#125265=CARTESIAN_POINT('Ctrl Pts',(-7.21598901700505,-20.462240423921,
85.5515349210241));
#125266=CARTESIAN_POINT('Ctrl Pts',(-7.20044538808841,-20.4470894585749,
85.5558434744203));
#125267=CARTESIAN_POINT('Ctrl Pts',(-7.184933585593,-20.4323636783849,85.5598786279935));
#125268=CARTESIAN_POINT('Ctrl Pts',(-7.15899174990591,-20.4077363811918,
85.5666269920859));
#125269=CARTESIAN_POINT('Ctrl Pts',(-7.13313936171369,-20.3842994707439,
85.5726100926947));
#125270=CARTESIAN_POINT('Ctrl Pts',(-7.10743707658413,-20.3620447045031,
85.5778590282367));
#125271=CARTESIAN_POINT('Ctrl Pts',(-7.09034758997357,-20.3472474781951,
85.5813490530812));
#125272=CARTESIAN_POINT('Ctrl Pts',(-7.07332502324638,-20.3329726384921,
85.5845144972691));
#125273=CARTESIAN_POINT('Ctrl Pts',(-7.05639340493283,-20.3192185126292,
85.5873657595805));
#125274=CARTESIAN_POINT('Ctrl Pts',(-7.03263357576654,-20.2999176002897,
85.5913668836416));
#125275=CARTESIAN_POINT('Ctrl Pts',(-7.00905319070198,-20.2816430035672,
85.5947488602904));
#125276=CARTESIAN_POINT('Ctrl Pts',(-6.9857261746476,-20.2643903645038,
85.5975435664691));
#125277=CARTESIAN_POINT('Ctrl Pts',(-6.96742649372553,-20.2508559377606,
85.5997359699561));
#125278=CARTESIAN_POINT('Ctrl Pts',(-6.94928267677856,-20.237951007443,
85.6015674054324));
#125279=CARTESIAN_POINT('Ctrl Pts',(-6.93131002919188,-20.2256539965921,
85.6030583215737));
#125280=CARTESIAN_POINT('Ctrl Pts',(-6.91004642120851,-20.2111052876811,
85.6048222384486));
#125281=CARTESIAN_POINT('Ctrl Pts',(-6.88902273918636,-20.1974077367977,
85.606109504425));
#125282=CARTESIAN_POINT('Ctrl Pts',(-6.86826729763053,-20.1845277817933,
85.6069539388812));
#125283=CARTESIAN_POINT('Ctrl Pts',(-6.84914188148638,-20.172659352075,
85.6077320558072));
#125284=CARTESIAN_POINT('Ctrl Pts',(-6.83024405342614,-20.1614855334301,
85.6081344160708));
#125285=CARTESIAN_POINT('Ctrl Pts',(-6.81157466760304,-20.1509669364568,
85.6081875725525));
#125286=CARTESIAN_POINT('Ctrl Pts',(-6.79285868093349,-20.140422083905,
85.6082408617186));
#125287=CARTESIAN_POINT('Ctrl Pts',(-6.77437236819119,-20.1305356928375,
85.6079432628828));
#125288=CARTESIAN_POINT('Ctrl Pts',(-6.75611755799409,-20.1212710245048,
85.6073201220557));
#125289=CARTESIAN_POINT('Ctrl Pts',(-6.73638327829304,-20.111255496858,
85.6066464784931));
#125290=CARTESIAN_POINT('Ctrl Pts',(-6.71691930222018,-20.1019677281025,
85.6055929164435));
#125291=CARTESIAN_POINT('Ctrl Pts',(-6.69768443571138,-20.0933512015893,
85.6041834821669));
#125292=CARTESIAN_POINT('Ctrl Pts',(-6.68137792897692,-20.0860464746472,
85.6029886233665));
#125293=CARTESIAN_POINT('Ctrl Pts',(-6.6652359218369,-20.0792242508093,
85.6015378792598));
#125294=CARTESIAN_POINT('Ctrl Pts',(-6.64923350344088,-20.072855918317,
85.599842182004));
#125295=CARTESIAN_POINT('Ctrl Pts',(-6.62896111745131,-20.0647883068349,
85.5976940173679));
#125296=CARTESIAN_POINT('Ctrl Pts',(-6.60891363092771,-20.0574444366806,
85.5951518701932));
#125297=CARTESIAN_POINT('Ctrl Pts',(-6.58913563150429,-20.0508103664085,
85.5922443617696));
#125298=CARTESIAN_POINT('Ctrl Pts',(-6.57488563962315,-20.0460305377973,
85.5901495102861));
#125299=CARTESIAN_POINT('Ctrl Pts',(-6.56077545734654,-20.0416189903231,
85.5878650765649));
#125300=CARTESIAN_POINT('Ctrl Pts',(-6.54682296816177,-20.0375665177092,
85.5854047998161));
#125301=CARTESIAN_POINT('Ctrl Pts',(-8.23395173885433,-22.5,84.5714980228305));
#125302=CARTESIAN_POINT('Ctrl Pts',(-8.21516313921569,-22.4637909993162,
84.6293396005463));
#125303=CARTESIAN_POINT('Ctrl Pts',(-8.19537632053088,-22.4283109296505,
84.6855617234812));
#125304=CARTESIAN_POINT('Ctrl Pts',(-8.17476407227142,-22.393589005892,
84.7401422899255));
#125305=CARTESIAN_POINT('Ctrl Pts',(-8.15671077006665,-22.3631777002037,
84.7879468500163));
#125306=CARTESIAN_POINT('Ctrl Pts',(-8.13802383025153,-22.3333487538864,
84.8344926324756));
#125307=CARTESIAN_POINT('Ctrl Pts',(-8.11881620643752,-22.3041412702589,
84.8797910935868));
#125308=CARTESIAN_POINT('Ctrl Pts',(-8.11710382636405,-22.3015373920569,
84.88382949953));
#125309=CARTESIAN_POINT('Ctrl Pts',(-8.11538731317498,-22.2989384496591,
84.8878579869973));
#125310=CARTESIAN_POINT('Ctrl Pts',(-8.11366673296642,-22.2963444085858,
84.8918765846372));
#125311=CARTESIAN_POINT('Ctrl Pts',(-8.0897968412713,-22.2603568509209,
84.9476272494163));
#125312=CARTESIAN_POINT('Ctrl Pts',(-8.06514684457484,-22.2253110021173,
85.0014709552372));
#125313=CARTESIAN_POINT('Ctrl Pts',(-8.03987636784091,-22.1911816240943,
85.0534715425807));
#125314=CARTESIAN_POINT('Ctrl Pts',(-8.02320821822501,-22.1686702332261,
85.0877706014818));
#125315=CARTESIAN_POINT('Ctrl Pts',(-8.0062694224247,-22.1465580108257,
85.1212686975038));
#125316=CARTESIAN_POINT('Ctrl Pts',(-7.98909910267082,-22.1248416438096,
85.1539936246758));
#125317=CARTESIAN_POINT('Ctrl Pts',(-7.98534474887514,-22.1200932799991,
85.1611490508008));
#125318=CARTESIAN_POINT('Ctrl Pts',(-7.98157932470578,-22.1153638238704,
85.1682674700585));
#125319=CARTESIAN_POINT('Ctrl Pts',(-7.9778032608764,-22.1106532030564,
85.175349023635));
#125320=CARTESIAN_POINT('Ctrl Pts',(-7.94852432800735,-22.0741278801764,
85.2302581409442));
#125321=CARTESIAN_POINT('Ctrl Pts',(-7.91860782492171,-22.0387338144514,
85.2829470085377));
#125322=CARTESIAN_POINT('Ctrl Pts',(-7.88822657837118,-22.004449586861,
85.3335014088525));
#125323=CARTESIAN_POINT('Ctrl Pts',(-7.87547986902107,-21.9900653487534,
85.3547119357514));
#125324=CARTESIAN_POINT('Ctrl Pts',(-7.86265104172624,-21.9758766378046,
85.3755472904137));
#125325=CARTESIAN_POINT('Ctrl Pts',(-7.84975157984563,-21.9618824200467,
85.3960160906175));
#125326=CARTESIAN_POINT('Ctrl Pts',(-7.84380464228576,-21.9554307757863,
85.4054526607522));
#125327=CARTESIAN_POINT('Ctrl Pts',(-7.83784275699324,-21.949020523473,
85.4148111914716));
#125328=CARTESIAN_POINT('Ctrl Pts',(-7.83186694184561,-21.9426512253961,
85.4240923487898));
#125329=CARTESIAN_POINT('Ctrl Pts',(-7.79856222503536,-21.9071535295188,
85.4758185666391));
#125330=CARTESIAN_POINT('Ctrl Pts',(-7.76482751222371,-21.8729277948954,
85.5251380270165));
#125331=CARTESIAN_POINT('Ctrl Pts',(-7.73082285967433,-21.8399335685685,
85.5721737374828));
#125332=CARTESIAN_POINT('Ctrl Pts',(-7.72208232225891,-21.8314527505603,
85.5842637709449));
#125333=CARTESIAN_POINT('Ctrl Pts',(-7.71332377777891,-21.8230533025536,
85.596203127984));
#125334=CARTESIAN_POINT('Ctrl Pts',(-7.70454958924842,-21.8147345355726,
85.6079943060831));
#125335=CARTESIAN_POINT('Ctrl Pts',(-7.69638193440349,-21.8069908203333,
85.6189703949367));
#125336=CARTESIAN_POINT('Ctrl Pts',(-7.68820087496758,-21.7993171648251,
85.6298178953534));
#125337=CARTESIAN_POINT('Ctrl Pts',(-7.68000800769289,-21.791712453889,
85.6405386121853));
#125338=CARTESIAN_POINT('Ctrl Pts',(-7.64389923360224,-21.7581958863665,
85.6877884856661));
#125339=CARTESIAN_POINT('Ctrl Pts',(-7.60756450920095,-21.7260191702926,
85.7325732292101));
#125340=CARTESIAN_POINT('Ctrl Pts',(-7.57112643839262,-21.6951172731443,
85.7750551354326));
#125341=CARTESIAN_POINT('Ctrl Pts',(-7.56619751991202,-21.6909372238562,
85.7808015936843));
#125342=CARTESIAN_POINT('Ctrl Pts',(-7.56126664530471,-21.6867804895583,
85.7865059566646));
#125343=CARTESIAN_POINT('Ctrl Pts',(-7.55633405710516,-21.6826468987909,
85.7921686615137));
#125344=CARTESIAN_POINT('Ctrl Pts',(-7.54599295193706,-21.6739808810496,
85.8040404464694));
#125345=CARTESIAN_POINT('Ctrl Pts',(-7.53564465326263,-21.665416940057,
85.8157289319937));
#125346=CARTESIAN_POINT('Ctrl Pts',(-7.52529102525006,-21.6569528433106,
85.8272375230484));
#125347=CARTESIAN_POINT('Ctrl Pts',(-7.48591297578626,-21.6247612656395,
85.8710082541641));
#125348=CARTESIAN_POINT('Ctrl Pts',(-7.44646243495958,-21.5940151597803,
85.9121755393748));
#125349=CARTESIAN_POINT('Ctrl Pts',(-7.40703126209498,-21.5646271272466,
85.9509322071749));
#125350=CARTESIAN_POINT('Ctrl Pts',(-7.39459833707732,-21.5553608747269,
85.9631524560209));
#125351=CARTESIAN_POINT('Ctrl Pts',(-7.38216737807832,-21.5462301568784,
85.9751332185511));
#125352=CARTESIAN_POINT('Ctrl Pts',(-7.36974224252354,-21.5372329843712,
85.9868776265169));
#125353=CARTESIAN_POINT('Ctrl Pts',(-7.33239980939396,-21.5101929322747,
86.0221742047455));
#125354=CARTESIAN_POINT('Ctrl Pts',(-7.29511245957576,-21.4843604653004,
86.0553350106453));
#125355=CARTESIAN_POINT('Ctrl Pts',(-7.25799097947772,-21.4597047804485,
86.0864591384738));
#125356=CARTESIAN_POINT('Ctrl Pts',(-7.24357553249829,-21.4501301967631,
86.0985456235306));
#125357=CARTESIAN_POINT('Ctrl Pts',(-7.22918530724825,-21.4407334617653,
86.1103252009181));
#125358=CARTESIAN_POINT('Ctrl Pts',(-7.21482430868666,-21.4315109200846,
86.1218036380714));
#125359=CARTESIAN_POINT('Ctrl Pts',(-7.17989907466988,-21.4090821575549,
86.1497186261558));
#125360=CARTESIAN_POINT('Ctrl Pts',(-7.1451486333736,-21.3876844720568,
86.1758528094717));
#125361=CARTESIAN_POINT('Ctrl Pts',(-7.11063583301104,-21.3672816186261,
86.2003008191494));
#125362=CARTESIAN_POINT('Ctrl Pts',(-7.09441751541707,-21.357693872825,
86.2117894720934));
#125363=CARTESIAN_POINT('Ctrl Pts',(-7.07825187942197,-21.3483262000986,
86.2229060358246));
#125364=CARTESIAN_POINT('Ctrl Pts',(-7.06214060964175,-21.3391720258857,
86.2336599246193));
#125365=CARTESIAN_POINT('Ctrl Pts',(-7.0298691387285,-21.3208358754224,
86.2552003627211));
#125366=CARTESIAN_POINT('Ctrl Pts',(-6.99781709896481,-21.3033565079906,
86.27528664282));
#125367=CARTESIAN_POINT('Ctrl Pts',(-6.96600003195233,-21.2866931565165,
86.2940024449842));
#125368=CARTESIAN_POINT('Ctrl Pts',(-6.94815056474316,-21.2773449678347,
86.3045020644775));
#125369=CARTESIAN_POINT('Ctrl Pts',(-6.93037501697478,-21.2682542386513,
86.3145713105324));
#125370=CARTESIAN_POINT('Ctrl Pts',(-6.9126858637405,-21.2594190155966,
86.3242147374989));
#125371=CARTESIAN_POINT('Ctrl Pts',(-6.88310196576389,-21.2446427098013,
86.340342709016));
#125372=CARTESIAN_POINT('Ctrl Pts',(-6.85375997369321,-21.230581377448,
86.3552799987662));
#125373=CARTESIAN_POINT('Ctrl Pts',(-6.8247237715537,-21.2172277935325,
86.3690639227611));
#125374=CARTESIAN_POINT('Ctrl Pts',(-6.80541826317748,-21.2083493002333,
86.3782285393615));
#125375=CARTESIAN_POINT('Ctrl Pts',(-6.78624741907278,-21.1997836333197,
86.3868840470772));
#125376=CARTESIAN_POINT('Ctrl Pts',(-6.76723753695952,-21.1915311822395,
86.3950378247371));
#125377=CARTESIAN_POINT('Ctrl Pts',(-6.74056004148214,-21.1799501148213,
86.4064804189285));
#125378=CARTESIAN_POINT('Ctrl Pts',(-6.71419947662327,-21.1689861593937,
86.4169351580929));
#125379=CARTESIAN_POINT('Ctrl Pts',(-6.68823034809353,-21.158635001424,
86.4264373456855));
#125380=CARTESIAN_POINT('Ctrl Pts',(-6.66785902462152,-21.150515099092,
86.4338912784163));
#125381=CARTESIAN_POINT('Ctrl Pts',(-6.64772783612135,-21.1427714979923,
86.4407584809481));
#125382=CARTESIAN_POINT('Ctrl Pts',(-6.62785299516616,-21.1353933240402,
86.4470647112304));
#125383=CARTESIAN_POINT('Ctrl Pts',(-6.6043375045663,-21.1266636249897,
86.454526109249));
#125384=CARTESIAN_POINT('Ctrl Pts',(-6.58118076088298,-21.1184454494094,
86.461202477795));
#125385=CARTESIAN_POINT('Ctrl Pts',(-6.55840481740494,-21.1107171824041,
86.4671409404535));
#125386=CARTESIAN_POINT('Ctrl Pts',(-6.53741878493808,-21.1035962628056,
86.4726127124693));
#125387=CARTESIAN_POINT('Ctrl Pts',(-6.51675554276146,-21.0968907643728,
86.4774570680671));
#125388=CARTESIAN_POINT('Ctrl Pts',(-6.49641502090829,-21.0905794474349,
86.4817141253824));
#125389=CARTESIAN_POINT('Ctrl Pts',(-6.47602248136917,-21.0842519902964,
86.4859820694523));
#125390=CARTESIAN_POINT('Ctrl Pts',(-6.45595416530781,-21.078320662806,
86.4896597311807));
#125391=CARTESIAN_POINT('Ctrl Pts',(-6.43620364679814,-21.0727627584111,
86.4927862263515));
#125392=CARTESIAN_POINT('Ctrl Pts',(-6.41485383265773,-21.0667548034412,
86.4961658890564));
#125393=CARTESIAN_POINT('Ctrl Pts',(-6.39387591799712,-21.0611827407742,
86.4989005495489));
#125394=CARTESIAN_POINT('Ctrl Pts',(-6.37322590319923,-21.0560128857335,
86.5010337758867));
#125395=CARTESIAN_POINT('Ctrl Pts',(-6.35571836562928,-21.051629768712,
86.5028423721815));
#125396=CARTESIAN_POINT('Ctrl Pts',(-6.33844642442226,-21.0475358633691,
86.5042184324612));
#125397=CARTESIAN_POINT('Ctrl Pts',(-6.32137803192766,-21.0437131274736,
86.5051841797176));
#125398=CARTESIAN_POINT('Ctrl Pts',(-6.29975624133946,-21.0388705862072,
86.5064075629357));
#125399=CARTESIAN_POINT('Ctrl Pts',(-6.27846158278878,-21.0344644269352,
86.5069734461553));
#125400=CARTESIAN_POINT('Ctrl Pts',(-6.25754083755047,-21.0304847535283,
86.5069156039064));
#125401=CARTESIAN_POINT('Ctrl Pts',(-6.24246729728511,-21.0276173715752,
86.5068739281699));
#125402=CARTESIAN_POINT('Ctrl Pts',(-6.22758792701389,-21.0249712982746,
86.5065084226784));
#125403=CARTESIAN_POINT('Ctrl Pts',(-6.2129177451068,-21.0225402179311,
86.5058302683033));
#125404=CARTESIAN_POINT('Origin',(-8.75366715310791,111.0724296188,85.97453149762));
#125405=CARTESIAN_POINT('',(-6.54682286637191,-10.,85.58540530765));
#125406=CARTESIAN_POINT('Origin',(-6.80729512863291,-10.,84.10819367738));
#125407=CARTESIAN_POINT('Origin',(-6.80729512863291,-10.,84.10819367738));
#125408=CARTESIAN_POINT('Origin',(-6.80729512863291,-10.,84.10819367738));
#125409=CARTESIAN_POINT('Origin',(-9.10739291134991,-8.5,88.57546942229));
#125410=CARTESIAN_POINT('',(-5.70733149011427,-8.50000000000053,58.9263899029757));
#125411=CARTESIAN_POINT('Origin',(27.4324635166691,-8.5,72.98888938658));
#125412=CARTESIAN_POINT('',(-2.22484390946918,-8.50000000000039,56.4938787766194));
#125413=CARTESIAN_POINT('Origin',(-2.02513312664091,-8.50000000000099,60.48888938658));
#125414=CARTESIAN_POINT('Origin',(1.07038457110909,-8.5,122.41156512159));
#125415=CARTESIAN_POINT('Origin',(1.07038457110909,-10.,122.41156512159));
#125416=CARTESIAN_POINT('',(-2.29973550275294,-10.,54.9957487971695));
#125417=CARTESIAN_POINT('Origin',(-2.22484394585091,-10.,56.49387804884));
#125418=CARTESIAN_POINT('Origin',(1.07038457110909,-10.,122.41156512159));
#125419=CARTESIAN_POINT('Origin',(18.4825952511691,-2.36409272922499,58.74984256216));
#125420=CARTESIAN_POINT('',(18.8781175927891,-10.0002140775,57.30292794298));
#125421=CARTESIAN_POINT('Ctrl Pts',(-3.58430183424491,-12.77734752092,56.71623037308));
#125422=CARTESIAN_POINT('Ctrl Pts',(-2.82654579637091,-13.56823877579,56.66356760301));
#125423=CARTESIAN_POINT('Ctrl Pts',(-1.22510960093091,-14.96301005098,56.57763219321));
#125424=CARTESIAN_POINT('Ctrl Pts',(1.36103340034909,-16.52464473566,56.54069563469));
#125425=CARTESIAN_POINT('Ctrl Pts',(3.87584585923909,-17.55452762874,56.60358098145));
#125426=CARTESIAN_POINT('Ctrl Pts',(6.19710063835909,-18.15797232338,56.74716429009));
#125427=CARTESIAN_POINT('Ctrl Pts',(8.31505282592909,-18.45204200109,56.94959224141));
#125428=CARTESIAN_POINT('Ctrl Pts',(10.3190076082391,-18.5227178858,57.20308600798));
#125429=CARTESIAN_POINT('Ctrl Pts',(12.2966611152891,-18.39728886114,57.51358361024));
#125430=CARTESIAN_POINT('Ctrl Pts',(14.2762842352891,-18.07077538528,57.88694259276));
#125431=CARTESIAN_POINT('Ctrl Pts',(16.1913087147191,-17.5550687573,58.30881641828));
#125432=CARTESIAN_POINT('Ctrl Pts',(18.0106355730791,-16.87094604643,58.76532096745));
#125433=CARTESIAN_POINT('Ctrl Pts',(19.7936798013391,-16.00018983021,59.26535024511));
#125434=CARTESIAN_POINT('Ctrl Pts',(21.6152587953191,-14.87219739396,59.8316118168));
#125435=CARTESIAN_POINT('Ctrl Pts',(23.5037332083091,-13.38226243744,60.48072054854));
#125436=CARTESIAN_POINT('Ctrl Pts',(25.4089773760291,-11.42609024385,61.20195839564));
#125437=CARTESIAN_POINT('Ctrl Pts',(27.1843832993891,-8.93696435445999,
61.93748494782));
#125438=CARTESIAN_POINT('Ctrl Pts',(28.5837262234791,-5.98779183204199,
62.56306222481));
#125439=CARTESIAN_POINT('Ctrl Pts',(29.4131721215591,-2.80038937228799,
62.95281639517));
#125440=CARTESIAN_POINT('Ctrl Pts',(29.5612752799991,-0.620166171525686,
63.023935917286));
#125441=CARTESIAN_POINT('Ctrl Pts',(29.5343220504091,0.444915684091514,
63.011087634094));
#125442=CARTESIAN_POINT('Ctrl Pts',(29.5338703742191,0.461774656562614,
63.0108722771));
#125443=CARTESIAN_POINT('Ctrl Pts',(-3.72288960953291,-12.85329830414,55.62299833527));
#125444=CARTESIAN_POINT('Ctrl Pts',(-2.94901860386991,-13.64890746123,55.56862071173));
#125445=CARTESIAN_POINT('Ctrl Pts',(-1.31349980804092,-15.05199668853,55.47970165767));
#125446=CARTESIAN_POINT('Ctrl Pts',(1.32767713553909,-16.6228801163,55.44051598947));
#125447=CARTESIAN_POINT('Ctrl Pts',(3.89588111527909,-17.65877088157,55.5036943663299));
#125448=CARTESIAN_POINT('Ctrl Pts',(6.26621663463909,-18.26566107639,55.64967374489));
#125449=CARTESIAN_POINT('Ctrl Pts',(8.42872386496909,-18.56136755362,55.8560400985301));
#125450=CARTESIAN_POINT('Ctrl Pts',(10.4746065168291,-18.63242271852,56.11476044379));
#125451=CARTESIAN_POINT('Ctrl Pts',(12.4933994745791,-18.50631935278,56.431858726));
#125452=CARTESIAN_POINT('Ctrl Pts',(14.5139561217791,-18.17810478474,56.81330363737));
#125453=CARTESIAN_POINT('Ctrl Pts',(16.4683569012591,-17.65977495691,57.24442226139));
#125454=CARTESIAN_POINT('Ctrl Pts',(18.3249224039791,-16.97222998037,57.71101147142));
#125455=CARTESIAN_POINT('Ctrl Pts',(20.1443477633591,-16.09715278017,58.22215868751));
#125456=CARTESIAN_POINT('Ctrl Pts',(22.0030374225591,-14.96355146807,58.80109378072));
#125457=CARTESIAN_POINT('Ctrl Pts',(23.9300250610891,-13.46607983077,59.4648497644901));
#125458=CARTESIAN_POINT('Ctrl Pts',(25.8743271231091,-11.49961504094,60.20254853862));
#125459=CARTESIAN_POINT('Ctrl Pts',(27.6865453689491,-8.99647741870398,
60.9551385269801));
#125460=CARTESIAN_POINT('Ctrl Pts',(29.1154374711391,-6.02908615362698,
61.59554524518));
#125461=CARTESIAN_POINT('Ctrl Pts',(29.9627342908991,-2.82017517727099,
61.99473019848));
#125462=CARTESIAN_POINT('Ctrl Pts',(30.1140601046791,-0.624535642130786,
62.06759020103));
#125463=CARTESIAN_POINT('Ctrl Pts',(30.0865221951591,0.448052485067714,
62.05442854821));
#125464=CARTESIAN_POINT('Ctrl Pts',(30.0860607192791,0.465030265795814,
62.05420793871));
#125465=CARTESIAN_POINT('Ctrl Pts',(-3.17320105054691,-12.28484166745,54.85174559045));
#125466=CARTESIAN_POINT('Ctrl Pts',(-2.42508695642091,-13.04513949903,54.80503919576));
#125467=CARTESIAN_POINT('Ctrl Pts',(-0.844253174050915,-14.3859726853,54.73047035947));
#125468=CARTESIAN_POINT('Ctrl Pts',(1.70866986857909,-15.8876335301,54.70700946437));
#125469=CARTESIAN_POINT('Ctrl Pts',(4.19228482572909,-16.87855813869,54.77837472681));
#125470=CARTESIAN_POINT('Ctrl Pts',(6.48653288913908,-17.45966035134,54.92597342556));
#125471=CARTESIAN_POINT('Ctrl Pts',(8.58186134395909,-17.74311613794,55.12908301981));
#125472=CARTESIAN_POINT('Ctrl Pts',(10.5664452653491,-17.81133256526,55.38081209437));
#125473=CARTESIAN_POINT('Ctrl Pts',(12.5270981927391,-17.69027633198,55.68738173201));
#125474=CARTESIAN_POINT('Ctrl Pts',(14.4918977503591,-17.37479365556,56.05469422228));
#125475=CARTESIAN_POINT('Ctrl Pts',(16.3945506037791,-16.87609727056,56.4687746378201));
#125476=CARTESIAN_POINT('Ctrl Pts',(18.2036342066391,-16.21416637664,56.91612646381));
#125477=CARTESIAN_POINT('Ctrl Pts',(19.9776601847591,-15.37142975168,57.40549259896));
#125478=CARTESIAN_POINT('Ctrl Pts',(21.7905301121891,-14.27980829232,57.95894164));
#125479=CARTESIAN_POINT('Ctrl Pts',(23.6696227303091,-12.83874523999,58.59230118133));
#125480=CARTESIAN_POINT('Ctrl Pts',(25.5636008457491,-10.94931579331,59.29438635056));
#125481=CARTESIAN_POINT('Ctrl Pts',(27.3248106085391,-8.55104953890899,
60.00792469414));
#125482=CARTESIAN_POINT('Ctrl Pts',(28.7082158942091,-5.72001717281198,
60.61198629947));
#125483=CARTESIAN_POINT('Ctrl Pts',(29.5252295808991,-2.67208753843899,
60.98663314509));
#125484=CARTESIAN_POINT('Ctrl Pts',(29.6707996220691,-0.591832166815786,
61.0548216514));
#125485=CARTESIAN_POINT('Ctrl Pts',(29.6442913120391,0.424574974273814,
61.04249344665));
#125486=CARTESIAN_POINT('Ctrl Pts',(29.6438471072391,0.440663529910414,
61.04228680651));
#125487=CARTESIAN_POINT('Ctrl Pts',(-2.38244347352091,-11.53445397631,55.02993629904));
#125488=CARTESIAN_POINT('Ctrl Pts',(-1.68100325115091,-12.24813930956,54.99404617299));
#125489=CARTESIAN_POINT('Ctrl Pts',(-0.199132288740913,-13.50679179131,
54.93948658306));
#125490=CARTESIAN_POINT('Ctrl Pts',(2.19404928560909,-14.91707579071,54.93693122039));
#125491=CARTESIAN_POINT('Ctrl Pts',(4.52391333623909,-15.8486431004,55.0177166612));
#125492=CARTESIAN_POINT('Ctrl Pts',(6.67880783080909,-16.3957040456,55.16484050833));
#125493=CARTESIAN_POINT('Ctrl Pts',(8.6498779854791,-16.6629883833,55.36014776661));
#125494=CARTESIAN_POINT('Ctrl Pts',(10.5198070717491,-16.72745755252,55.5983555735));
#125495=CARTESIAN_POINT('Ctrl Pts',(12.3703411755791,-16.61306375545,55.88583297768));
#125496=CARTESIAN_POINT('Ctrl Pts',(14.2280550377091,-16.31438773435,56.22829233863));
#125497=CARTESIAN_POINT('Ctrl Pts',(16.0299360351191,-15.84160835493,56.61291322706));
#125498=CARTESIAN_POINT('Ctrl Pts',(17.7454468009191,-15.21348917344,57.02735648449));
#125499=CARTESIAN_POINT('Ctrl Pts',(19.4292282283691,-14.41344352614,57.47976284219));
#125500=CARTESIAN_POINT('Ctrl Pts',(21.1506253523991,-13.37723731351,57.99030081481));
#125501=CARTESIAN_POINT('Ctrl Pts',(22.9343804115591,-12.01063606723,58.57294969782));
#125502=CARTESIAN_POINT('Ctrl Pts',(24.7295945359991,-10.22289665205,59.2163207090301));
#125503=CARTESIAN_POINT('Ctrl Pts',(26.3934737214891,-7.96306520251299,
59.86646337428));
#125504=CARTESIAN_POINT('Ctrl Pts',(27.6933626732391,-5.31203256334299,
60.41257442068));
#125505=CARTESIAN_POINT('Ctrl Pts',(28.4565964661691,-2.47660536052199,
60.74867761106));
#125506=CARTESIAN_POINT('Ctrl Pts',(28.5921150013391,-0.548662145128386,
60.80958320983));
#125507=CARTESIAN_POINT('Ctrl Pts',(28.5674129242191,0.393583630375914,
60.79855720673));
#125508=CARTESIAN_POINT('Ctrl Pts',(28.5669990101191,0.408498369893214,
60.79837239285));
#125509=CARTESIAN_POINT('',(-2.29980340878172,-12.0404106862218,54.9957613512899));
#125510=CARTESIAN_POINT('Ctrl Pts',(-2.29980340878172,-12.0404106862218,
54.9957613512899));
#125511=CARTESIAN_POINT('Ctrl Pts',(-2.11823697781814,-12.2161790760666,
54.9866899612617));
#125512=CARTESIAN_POINT('Ctrl Pts',(-1.93310846652742,-12.3876152127252,
54.9781755580477));
#125513=CARTESIAN_POINT('Ctrl Pts',(-1.74444833532541,-12.5547517442881,
54.9703033857551));
#125514=CARTESIAN_POINT('Ctrl Pts',(-1.55486486079395,-12.7227062780466,
54.9623926853552));
#125515=CARTESIAN_POINT('Ctrl Pts',(-1.36171473698319,-12.8863192680378,
54.9551303640825));
#125516=CARTESIAN_POINT('Ctrl Pts',(-1.16499499631772,-13.0455840037535,
54.9486081660288));
#125517=CARTESIAN_POINT('Ctrl Pts',(-1.03792296467273,-13.1484618007063,
54.944395121854));
#125518=CARTESIAN_POINT('Ctrl Pts',(-0.909360813004725,-13.2495244394935,
54.9404910116767));
#125519=CARTESIAN_POINT('Ctrl Pts',(-0.779301391391256,-13.3487605877945,
54.9369221775477));
#125520=CARTESIAN_POINT('Ctrl Pts',(-0.611246867493417,-13.476987235655,
54.9323107567604));
#125521=CARTESIAN_POINT('Ctrl Pts',(-0.440702356432936,-13.6021849644138,
54.9282592889589));
#125522=CARTESIAN_POINT('Ctrl Pts',(-0.267676715340883,-13.7243431957544,
54.924828715228));
#125523=CARTESIAN_POINT('Ctrl Pts',(-0.166953501828351,-13.7954550236891,
54.9228316793657));
#125524=CARTESIAN_POINT('Ctrl Pts',(-0.0653892044135112,-13.8655365188882,
54.921045112895));
#125525=CARTESIAN_POINT('Ctrl Pts',(0.0370171584764496,-13.9345929491547,
54.9194792680636));
#125526=CARTESIAN_POINT('Ctrl Pts',(0.176178845081396,-14.0284348651803,
54.917351415833));
#125527=CARTESIAN_POINT('Ctrl Pts',(0.316893525903645,-14.1203783761309,
54.9156311299842));
#125528=CARTESIAN_POINT('Ctrl Pts',(0.459158674092703,-14.2104234819286,
54.9143456426954));
#125529=CARTESIAN_POINT('Ctrl Pts',(0.530291248187232,-14.2554460348274,
54.913702899051));
#125530=CARTESIAN_POINT('Ctrl Pts',(0.601811440288151,-14.2999939864225,
54.9131688810108));
#125531=CARTESIAN_POINT('Ctrl Pts',(0.673718918977216,-14.3440673366463,
54.9127471525551));
#125532=CARTESIAN_POINT('Ctrl Pts',(0.709672658321749,-14.3661040117582,
54.9125362883272));
#125533=CARTESIAN_POINT('Ctrl Pts',(0.745723219351884,-14.388022036527,
54.9123534981929));
#125534=CARTESIAN_POINT('Ctrl Pts',(0.781870558597959,-14.4098214109445,
54.912199237989));
#125535=CARTESIAN_POINT('Ctrl Pts',(0.808981063032514,-14.4261709417575,
54.9120835428361));
#125536=CARTESIAN_POINT('Ctrl Pts',(0.836146005216066,-14.4424537317479,
54.9119838959101));
#125537=CARTESIAN_POINT('Ctrl Pts',(0.86336536634066,-14.4586697809128,
54.9119004921109));
#125538=CARTESIAN_POINT('Ctrl Pts',(0.872438486715524,-14.4640751306344,
54.9118726908444));
#125539=CARTESIAN_POINT('Ctrl Pts',(0.882845358372333,-14.4702608301792,
54.9118431601062));
#125540=CARTESIAN_POINT('Ctrl Pts',(0.890602866371274,-14.4748635831357,
54.9118225100166));
#125541=CARTESIAN_POINT('Ctrl Pts',(1.12238678087696,-14.6123876563195,
54.9112055130879));
#125542=CARTESIAN_POINT('Ctrl Pts',(1.35703325424795,-14.7444222465215,
54.9117700146229));
#125543=CARTESIAN_POINT('Ctrl Pts',(1.59451843150642,-14.8709914875867,
54.9136088011056));
#125544=CARTESIAN_POINT('Ctrl Pts',(1.78986036435338,-14.9751002175464,
54.9151212833151));
#125545=CARTESIAN_POINT('Ctrl Pts',(1.98712346942663,-15.0755104066668,
54.9174960503598));
#125546=CARTESIAN_POINT('Ctrl Pts',(2.18630472440888,-15.1722117185856,
54.9207900375331));
#125547=CARTESIAN_POINT('Ctrl Pts',(2.26366130372528,-15.2097678766996,
54.9220693325153));
#125548=CARTESIAN_POINT('Ctrl Pts',(2.34130728992583,-15.2467643796092,
54.9234873317818));
#125549=CARTESIAN_POINT('Ctrl Pts',(2.4192417879567,-15.2832011533707,54.925046539226));
#125550=CARTESIAN_POINT('Ctrl Pts',(2.66203537948802,-15.3967146215894,
54.9299040232015));
#125551=CARTESIAN_POINT('Ctrl Pts',(2.90762907197283,-15.504802566863,54.9361310672224));
#125552=CARTESIAN_POINT('Ctrl Pts',(3.15600542837689,-15.6074668205158,
54.9438115552215));
#125553=CARTESIAN_POINT('Ctrl Pts',(3.17491982026466,-15.6152849234729,
54.9443964408443));
#125554=CARTESIAN_POINT('Ctrl Pts',(3.1938503567678,-15.6230715505705,54.9449897614188));
#125555=CARTESIAN_POINT('Ctrl Pts',(3.21279703372886,-15.6308266911595,
54.9455915571066));
#125556=CARTESIAN_POINT('Ctrl Pts',(3.34667052785487,-15.6856229897515,
54.949843727112));
#125557=CARTESIAN_POINT('Ctrl Pts',(3.48134941726851,-15.7388486429223,
54.9545189197661));
#125558=CARTESIAN_POINT('Ctrl Pts',(3.61683074223619,-15.7905036503555,
54.9596318684309));
#125559=CARTESIAN_POINT('Ctrl Pts',(3.68457140472003,-15.816331154072,54.9621883427633));
#125560=CARTESIAN_POINT('Ctrl Pts',(3.75251267553316,-15.8417659963483,
54.9648542730921));
#125561=CARTESIAN_POINT('Ctrl Pts',(3.82065417045425,-15.8668081771434,
54.9676316045845));
#125562=CARTESIAN_POINT('Ctrl Pts',(3.85472491791479,-15.879329267541,54.9690202703307));
#125563=CARTESIAN_POINT('Ctrl Pts',(3.88884572134119,-15.8917521925685,
54.9704367874654));
#125564=CARTESIAN_POINT('Ctrl Pts',(3.92301653121896,-15.9040769522236,
54.9718814057418));
#125565=CARTESIAN_POINT('Ctrl Pts',(3.94864463862729,-15.9133205219649,
54.9729648694492));
#125566=CARTESIAN_POINT('Ctrl Pts',(3.97430087465893,-15.9225088736842,
54.9740641401396));
#125567=CARTESIAN_POINT('Ctrl Pts',(3.99998521807188,-15.9316420073814,
54.9751793248278));
#125568=CARTESIAN_POINT('Ctrl Pts',(4.0085466658762,-15.9346863852804,54.9755510530572));
#125569=CARTESIAN_POINT('Ctrl Pts',(4.01841638730849,-15.9381865207366,
54.9759817156855));
#125570=CARTESIAN_POINT('Ctrl Pts',(4.02567892979854,-15.9407567350712,
54.9762998182153));
#125571=CARTESIAN_POINT('Ctrl Pts',(4.19513949895062,-16.0007288432664,
54.9837222650809));
#125572=CARTESIAN_POINT('Ctrl Pts',(4.36540762168142,-16.0581700333998,
54.9918196982076));
#125573=CARTESIAN_POINT('Ctrl Pts',(4.53647535322449,-16.1130769852884,
55.0006148639831));
#125574=CARTESIAN_POINT('Ctrl Pts',(4.79577701300262,-16.1963040417861,
55.0139464319126));
#125575=CARTESIAN_POINT('Ctrl Pts',(5.05691578284093,-16.2737107959004,
55.0288804604544));
#125576=CARTESIAN_POINT('Ctrl Pts',(5.31987357742345,-16.3453019227047,
55.0454711014457));
#125577=CARTESIAN_POINT('Ctrl Pts',(5.35926275247959,-16.3560257555184,
55.0479562594283));
#125578=CARTESIAN_POINT('Ctrl Pts',(5.39869274909326,-16.3666190063023,
55.0504786131046));
#125579=CARTESIAN_POINT('Ctrl Pts',(5.43816351149184,-16.3770815939634,
55.053038370818));
#125580=CARTESIAN_POINT('Ctrl Pts',(5.67656967670919,-16.4402763551221,
55.0684994864194));
#125581=CARTESIAN_POINT('Ctrl Pts',(5.91646148577811,-16.4987080922576,
55.0853243446279));
#125582=CARTESIAN_POINT('Ctrl Pts',(6.15782167811788,-16.5523768050417,
55.1035638143412));
#125583=CARTESIAN_POINT('Ctrl Pts',(6.27850177428777,-16.5792111614337,
55.1126835491979));
#125584=CARTESIAN_POINT('Ctrl Pts',(6.3995489559653,-16.6048547617057,55.1221570798402));
#125585=CARTESIAN_POINT('Ctrl Pts',(6.52096086026782,-16.6293076058599,
55.1319916333416));
#125586=CARTESIAN_POINT('Ctrl Pts',(6.58166681241908,-16.641534027937,55.1369089100924));
#125587=CARTESIAN_POINT('Ctrl Pts',(6.64246394417776,-16.6534627609877,
55.141916451863));
#125588=CARTESIAN_POINT('Ctrl Pts',(6.70335194954774,-16.6650938050292,
55.1470152184466));
#125589=CARTESIAN_POINT('Ctrl Pts',(6.70722592634993,-16.6658338259007,
55.147339625583));
#125590=CARTESIAN_POINT('Ctrl Pts',(6.71110027104119,-16.6665726417745,
55.1476644020211));
#125591=CARTESIAN_POINT('Ctrl Pts',(6.71497498351283,-16.6673102525422,
55.1479895480109));
#125592=CARTESIAN_POINT('Ctrl Pts',(6.76438739306036,-16.6767166602704,
55.1521359838887));
#125593=CARTESIAN_POINT('Ctrl Pts',(6.81385961344467,-16.6859270892099,
55.1563425176269));
#125594=CARTESIAN_POINT('Ctrl Pts',(6.86339149624892,-16.6949415412016,
55.1606094699931));
#125595=CARTESIAN_POINT('Ctrl Pts',(6.87102234822951,-16.6963303022367,
55.1612668341002));
#125596=CARTESIAN_POINT('Ctrl Pts',(6.87987773679538,-16.6979354380448,
55.1620314192965));
#125597=CARTESIAN_POINT('Ctrl Pts',(6.88628829968681,-16.6990938701348,
55.162585865581));
#125598=CARTESIAN_POINT('Ctrl Pts',(7.09142631221265,-16.736163697014,55.1803281466857));
#125599=CARTESIAN_POINT('Ctrl Pts',(7.29906866836621,-16.7699660342097,
55.1992345884685));
#125600=CARTESIAN_POINT('Ctrl Pts',(7.50920025566267,-16.8005008816512,
55.2193722461986));
#125601=CARTESIAN_POINT('Ctrl Pts',(7.6142660493109,-16.8157683053719,55.2294410750636));
#125602=CARTESIAN_POINT('Ctrl Pts',(7.71995414520202,-16.8302188565267,
55.2398177960984));
#125603=CARTESIAN_POINT('Ctrl Pts',(7.82626245270495,-16.8438525347216,
55.2505113355578));
#125604=CARTESIAN_POINT('Ctrl Pts',(7.88848917012429,-16.8518328991949,
55.256770713341));
#125605=CARTESIAN_POINT('Ctrl Pts',(7.9516382434093,-16.8596206660257,55.2632112213451));
#125606=CARTESIAN_POINT('Ctrl Pts',(8.01446306451706,-16.8670588826418,
55.2697083472482));
#125607=CARTESIAN_POINT('Ctrl Pts',(8.05896835301694,-16.8723281372229,
55.2743109303935));
#125608=CARTESIAN_POINT('Ctrl Pts',(8.10331079659642,-16.8774230378983,
55.2789416187177));
#125609=CARTESIAN_POINT('Ctrl Pts',(8.14704586474734,-16.8823029504198,
55.2835517443369));
#125610=CARTESIAN_POINT('Ctrl Pts',(8.3264698772246,-16.9023228914453,55.3024648790727));
#125611=CARTESIAN_POINT('Ctrl Pts',(8.50485641498181,-16.9197600629979,
55.3219956359713));
#125612=CARTESIAN_POINT('Ctrl Pts',(8.68198013956874,-16.9345906189262,
55.3420966134434));
#125613=CARTESIAN_POINT('Ctrl Pts',(8.92133811413511,-16.954632043851,55.3692602769545));
#125614=CARTESIAN_POINT('Ctrl Pts',(9.15839074252427,-16.9699118174646,
55.3974658526435));
#125615=CARTESIAN_POINT('Ctrl Pts',(9.39257368191784,-16.9804287123046,
55.426561672554));
#125616=CARTESIAN_POINT('Ctrl Pts',(9.5963122636134,-16.9895783849669,55.4518749643642));
#125617=CARTESIAN_POINT('Ctrl Pts',(9.79845889006155,-16.9955813380872,
55.4779328650654));
#125618=CARTESIAN_POINT('Ctrl Pts',(9.99901038774821,-16.9984375726291,
55.5046948396689));
#125619=CARTESIAN_POINT('Ctrl Pts',(10.0992861365915,-16.9998656899,55.5180758269706));
#125620=CARTESIAN_POINT('Ctrl Pts',(10.1991630943723,-17.0005071275631,
55.5316328999386));
#125621=CARTESIAN_POINT('Ctrl Pts',(10.2986408939489,-17.0003618855091,
55.5453613709104));
#125622=CARTESIAN_POINT('Ctrl Pts',(10.3622868047177,-17.0002689596217,
55.5541448486529));
#125623=CARTESIAN_POINT('Ctrl Pts',(10.4251100046831,-16.9998594984302,
55.5629062774401));
#125624=CARTESIAN_POINT('Ctrl Pts',(10.4883760042335,-16.9991254956933,
55.5718207460435));
#125625=CARTESIAN_POINT('Ctrl Pts',(10.4931746518341,-16.9990698224961,
55.572496897431));
#125626=CARTESIAN_POINT('Ctrl Pts',(10.4979758457689,-16.9990122583866,
55.5731739361208));
#125627=CARTESIAN_POINT('Ctrl Pts',(10.5027801376696,-16.9989527881453,
55.5738519418908));
#125628=CARTESIAN_POINT('Ctrl Pts',(10.5336357439578,-16.9985708400058,
55.5782064398132));
#125629=CARTESIAN_POINT('Ctrl Pts',(10.5646191521784,-16.9981104984623,
55.5826007620461));
#125630=CARTESIAN_POINT('Ctrl Pts',(10.5958764208502,-16.9975661198121,
55.5870564767843));
#125631=CARTESIAN_POINT('Ctrl Pts',(10.7964545168402,-16.994072838479,55.6156488271859));
#125632=CARTESIAN_POINT('Ctrl Pts',(10.9986788730587,-16.9872735133215,
55.6453989040006));
#125633=CARTESIAN_POINT('Ctrl Pts',(11.2025344927777,-16.9771681456159,
55.6763506604447));
#125634=CARTESIAN_POINT('Ctrl Pts',(11.3110439159274,-16.9717892032941,
55.6928258365612));
#125635=CARTESIAN_POINT('Ctrl Pts',(11.4195641712537,-16.96549941776,55.7095718230664));
#125636=CARTESIAN_POINT('Ctrl Pts',(11.5288140096561,-16.9582626105621,
55.7267056358984));
#125637=CARTESIAN_POINT('Ctrl Pts',(11.6248108020557,-16.9519036970079,
55.7417609540344));
#125638=CARTESIAN_POINT('Ctrl Pts',(11.7213709309547,-16.9448129094927,
55.7571159141607));
#125639=CARTESIAN_POINT('Ctrl Pts',(11.8189787193469,-16.9369339119195,
55.7728589214683));
#125640=CARTESIAN_POINT('Ctrl Pts',(12.0087112421133,-16.9216185143365,
55.8034605828888));
#125641=CARTESIAN_POINT('Ctrl Pts',(12.1981250333715,-16.903544034879,55.8348412411284));
#125642=CARTESIAN_POINT('Ctrl Pts',(12.3872110443822,-16.8827131212053,
55.8669978109124));
#125643=CARTESIAN_POINT('Ctrl Pts',(12.6140848726673,-16.8577192620268,
55.9055806973587));
#125644=CARTESIAN_POINT('Ctrl Pts',(12.8404870703923,-16.8287575946014,
55.945280530211));
#125645=CARTESIAN_POINT('Ctrl Pts',(13.0664108967834,-16.7958240268103,
55.9860824040969));
#125646=CARTESIAN_POINT('Ctrl Pts',(13.273519930093,-16.7656331456729,56.023486323784));
#125647=CARTESIAN_POINT('Ctrl Pts',(13.480225796256,-16.7321059811549,56.0618162294752));
#125648=CARTESIAN_POINT('Ctrl Pts',(13.6865207180361,-16.695242533248,56.1010641528426));
#125649=CARTESIAN_POINT('Ctrl Pts',(13.7896681789261,-16.6768108092946,
56.1206881145263));
#125650=CARTESIAN_POINT('Ctrl Pts',(13.8927128932393,-16.657545014482,56.1405416383219));
#125651=CARTESIAN_POINT('Ctrl Pts',(13.9956538238716,-16.6374451487844,
56.160624077633));
#125652=CARTESIAN_POINT('Ctrl Pts',(14.0471242891877,-16.6273952159356,
56.1706652972885));
#125653=CARTESIAN_POINT('Ctrl Pts',(14.0985688077801,-16.6171367653659,
56.180763749469));
#125654=CARTESIAN_POINT('Ctrl Pts',(14.1499872456801,-16.6066697970753,
56.1909193754892));
#125655=CARTESIAN_POINT('Ctrl Pts',(14.188520764919,-16.5988257407315,56.1985301086545));
#125656=CARTESIAN_POINT('Ctrl Pts',(14.2279621434588,-16.5906724585696,
56.2063564186179));
#125657=CARTESIAN_POINT('Ctrl Pts',(14.2662370443747,-16.5826408526218,
56.2139860715531));
#125658=CARTESIAN_POINT('Ctrl Pts',(14.2750639199052,-16.5807886208899,
56.2157456057436));
#125659=CARTESIAN_POINT('Ctrl Pts',(14.2838288110896,-16.5789430676027,
56.2174946280228));
#125660=CARTESIAN_POINT('Ctrl Pts',(14.2925063727919,-16.5771098442795,
56.2192279890994));
#125661=CARTESIAN_POINT('Ctrl Pts',(14.2964107562995,-16.5762850034827,
56.2200078978609));
#125662=CARTESIAN_POINT('Ctrl Pts',(14.3002974607726,-16.5754626606167,
56.2207846356224));
#125663=CARTESIAN_POINT('Ctrl Pts',(14.3041641799629,-16.5746433390449,
56.2215577311178));
#125664=CARTESIAN_POINT('Ctrl Pts',(14.5915131589416,-16.5137567823796,
56.2790090717243));
#125665=CARTESIAN_POINT('Ctrl Pts',(14.8766803030032,-16.4466339001003,
56.3379743812551));
#125666=CARTESIAN_POINT('Ctrl Pts',(15.1596819051769,-16.3733807048929,
56.398376378207));
#125667=CARTESIAN_POINT('Ctrl Pts',(15.4451387650363,-16.2994919815855,
56.4593024091789));
#125668=CARTESIAN_POINT('Ctrl Pts',(15.7283927043861,-16.2193660075623,
56.5216903084838));
#125669=CARTESIAN_POINT('Ctrl Pts',(16.0094473939293,-16.1330620148757,
56.585473450932));
#125670=CARTESIAN_POINT('Ctrl Pts',(16.051085209621,-16.1202762124157,56.594922824411));
#125671=CARTESIAN_POINT('Ctrl Pts',(16.0926747273626,-16.1073547287579,
56.6044028408523));
#125672=CARTESIAN_POINT('Ctrl Pts',(16.1342159274268,-16.0942976671956,
56.6139133040204));
#125673=CARTESIAN_POINT('Ctrl Pts',(16.425505046536,-16.0027408524006,56.6806011809788));
#125674=CARTESIAN_POINT('Ctrl Pts',(16.7144204396943,-15.9045221819093,
56.7487852650238));
#125675=CARTESIAN_POINT('Ctrl Pts',(17.0009678150187,-15.7996448168294,
56.8183790298192));
#125676=CARTESIAN_POINT('Ctrl Pts',(17.2875151903431,-15.6947674517495,
56.8879727946147));
#125677=CARTESIAN_POINT('Ctrl Pts',(17.5716949479418,-15.5832312167085,
56.9589764659462));
#125678=CARTESIAN_POINT('Ctrl Pts',(17.853484767978,-15.4649874495282,57.0313116212954));
#125679=CARTESIAN_POINT('Ctrl Pts',(18.1244197179,-15.3512985691583,57.1008603427135));
#125680=CARTESIAN_POINT('Ctrl Pts',(18.3931454302537,-15.2314085628236,
57.171640227598));
#125681=CARTESIAN_POINT('Ctrl Pts',(18.6596279924013,-15.105223090577,57.2435655992374));
#125682=CARTESIAN_POINT('Ctrl Pts',(18.7326997853566,-15.0706219571007,
57.2632881500201));
#125683=CARTESIAN_POINT('Ctrl Pts',(18.8056027326372,-15.0355472259604,
57.2830968401248));
#125684=CARTESIAN_POINT('Ctrl Pts',(18.8783357065489,-14.9999964140997,
57.3029899158076));
#125685=CARTESIAN_POINT('',(4.86118769045346,-16.9627432173458,55.1997076232029));
#125686=CARTESIAN_POINT('Ctrl Pts',(-2.29980340878007,-12.0404106862236,
54.9957613512899));
#125687=CARTESIAN_POINT('Ctrl Pts',(-2.06567740026702,-12.2943912214082,
54.9840649350874));
#125688=CARTESIAN_POINT('Ctrl Pts',(-1.82554507595862,-12.5407219961361,
54.9736741258264));
#125689=CARTESIAN_POINT('Ctrl Pts',(-1.58014432233485,-12.7792889509596,
54.9649000176596));
#125690=CARTESIAN_POINT('Ctrl Pts',(-1.34235247712726,-13.0104588864848,
54.9563979599428));
#125691=CARTESIAN_POINT('Ctrl Pts',(-1.09961332086077,-13.2343393853548,
54.9494138090859));
#125692=CARTESIAN_POINT('Ctrl Pts',(-0.852552136993808,-13.4508341796129,
54.944230727073));
#125693=CARTESIAN_POINT('Ctrl Pts',(-0.692492947152338,-13.5910908594825,
54.9408728547643));
#125694=CARTESIAN_POINT('Ctrl Pts',(-0.530618838552155,-13.7282478118966,
54.9382709254756));
#125695=CARTESIAN_POINT('Ctrl Pts',(-0.367090522438706,-13.8622794667611,
54.9365021757409));
#125696=CARTESIAN_POINT('Ctrl Pts',(-0.274164418016843,-13.9384438880172,
54.9354970713868));
#125697=CARTESIAN_POINT('Ctrl Pts',(-0.180704010652601,-14.0135991241281,
54.934761014906));
#125698=CARTESIAN_POINT('Ctrl Pts',(-0.0867375050534825,-14.0877495088467,
54.9343060611869));
#125699=CARTESIAN_POINT('Ctrl Pts',(0.0429253377670358,-14.1900684108592,
54.9336782779977));
#125700=CARTESIAN_POINT('Ctrl Pts',(0.173551750225582,-14.2904740468692,
54.9335857285551));
#125701=CARTESIAN_POINT('Ctrl Pts',(0.305069580466433,-14.3889768459098,
54.9340602809736));
#125702=CARTESIAN_POINT('Ctrl Pts',(0.370828495586858,-14.4382282454301,
54.9342975571829));
#125703=CARTESIAN_POINT('Ctrl Pts',(0.436810266016493,-14.4870039344858,
54.9346766178456));
#125704=CARTESIAN_POINT('Ctrl Pts',(0.503006110322588,-14.535305081866,
54.9352014595083));
#125705=CARTESIAN_POINT('Ctrl Pts',(0.536104032475637,-14.5594556555561,
54.9354638803397));
#125706=CARTESIAN_POINT('Ctrl Pts',(0.569255473146564,-14.5834875937639,
54.9357627469423));
#125707=CARTESIAN_POINT('Ctrl Pts',(0.602459340381778,-14.6074010376774,
54.9360985608908));
#125708=CARTESIAN_POINT('Ctrl Pts',(0.619061273999385,-14.6193577596341,
54.9362664678651));
#125709=CARTESIAN_POINT('Ctrl Pts',(0.635676314261408,-14.6312848580121,
54.9364436117096));
#125710=CARTESIAN_POINT('Ctrl Pts',(0.652304325438487,-14.6431823499626,
54.9366300551795));
#125711=CARTESIAN_POINT('Ctrl Pts',(0.664775333821296,-14.6521054689255,
54.9367698877819));
#125712=CARTESIAN_POINT('Ctrl Pts',(0.677253638344097,-14.6610119342725,
54.9369149514262));
#125713=CARTESIAN_POINT('Ctrl Pts',(0.689739181907747,-14.6699017531266,
54.9370652726049));
#125714=CARTESIAN_POINT('Ctrl Pts',(0.693901029762297,-14.6728650260779,
54.9371153796645));
#125715=CARTESIAN_POINT('Ctrl Pts',(0.696714681788608,-14.6748675183456,
54.9371494568424));
#125716=CARTESIAN_POINT('Ctrl Pts',(0.702227136384261,-14.6787860234036,
54.9372173472754));
#125717=CARTESIAN_POINT('Ctrl Pts',(0.935316961053932,-14.8444769404133,
54.9400880410572));
#125718=CARTESIAN_POINT('Ctrl Pts',(1.16882069079971,-15.0029006935076,
54.9447710833822));
#125719=CARTESIAN_POINT('Ctrl Pts',(1.40215622931578,-15.1543843049336,
54.9513409451183));
#125720=CARTESIAN_POINT('Ctrl Pts',(1.60396128131111,-15.2853980299524,
54.9570230255149));
#125721=CARTESIAN_POINT('Ctrl Pts',(1.80564149725469,-15.4112205074094,
54.9641162477073));
#125722=CARTESIAN_POINT('Ctrl Pts',(2.00685028315897,-15.5320598165629,
54.9726602222318));
#125723=CARTESIAN_POINT('Ctrl Pts',(2.24133468443142,-15.6728833543111,
54.982617186794));
#125724=CARTESIAN_POINT('Ctrl Pts',(2.47517761250087,-15.8069400864488,
54.9945443759754));
#125725=CARTESIAN_POINT('Ctrl Pts',(2.70784486479394,-15.9345930464969,
55.0084597313433));
#125726=CARTESIAN_POINT('Ctrl Pts',(2.94360679681554,-16.0639439035367,
55.0225601732145));
#125727=CARTESIAN_POINT('Ctrl Pts',(3.17816178474359,-16.186719595967,55.0387021617065));
#125728=CARTESIAN_POINT('Ctrl Pts',(3.41100385579573,-16.3032809225961,
55.056892462709));
#125729=CARTESIAN_POINT('Ctrl Pts',(3.64796053047498,-16.4219020301537,
55.0754042085353));
#125730=CARTESIAN_POINT('Ctrl Pts',(3.88314339365675,-16.5340872788256,
55.0960374899752));
#125731=CARTESIAN_POINT('Ctrl Pts',(4.11606747139699,-16.6401981973185,
55.1187846528849));
#125732=CARTESIAN_POINT('Ctrl Pts',(4.18606844953421,-16.6720878506236,
55.1256208875455));
#125733=CARTESIAN_POINT('Ctrl Pts',(4.2558657319487,-16.7034287456591,55.1326479351931));
#125734=CARTESIAN_POINT('Ctrl Pts',(4.32544694935167,-16.7342303598792,
55.1398652916536));
#125735=CARTESIAN_POINT('Ctrl Pts',(4.50554310797927,-16.8139537767382,
55.1585458813659));
#125736=CARTESIAN_POINT('Ctrl Pts',(4.68419074392955,-16.8900651847476,
55.1785017228101));
#125737=CARTESIAN_POINT('Ctrl Pts',(4.86118763155564,-16.9627435466136,
55.1997069862893));
#125738=CARTESIAN_POINT('Ctrl Pts',(4.86118763155564,-16.9627435466136,
55.1997069862893));
#125739=CARTESIAN_POINT('Ctrl Pts',(5.13408696149748,-17.0747940674125,
55.2323981770183));
#125740=CARTESIAN_POINT('Ctrl Pts',(5.41104329099708,-17.1804252386101,
55.2682238076182));
#125741=CARTESIAN_POINT('Ctrl Pts',(5.69165293468597,-17.2792384440373,
55.3072587814995));
#125742=CARTESIAN_POINT('Ctrl Pts',(5.83195775653042,-17.3286450467509,
55.3267762684401));
#125743=CARTESIAN_POINT('Ctrl Pts',(5.97317512545962,-17.3763471920351,
55.3470957603042));
#125744=CARTESIAN_POINT('Ctrl Pts',(6.11524996609304,-17.4222956096913,
55.3682246325463));
#125745=CARTESIAN_POINT('Ctrl Pts',(6.18628738640975,-17.4452698185194,
55.3787890686673));
#125746=CARTESIAN_POINT('Ctrl Pts',(6.25753917329986,-17.4678056092315,
55.3895558296405));
#125747=CARTESIAN_POINT('Ctrl Pts',(6.32899810955315,-17.4898968769833,
55.4005257120424));
#125748=CARTESIAN_POINT('Ctrl Pts',(6.36472757767979,-17.5009425108593,
55.4060106532433));
#125749=CARTESIAN_POINT('Ctrl Pts',(6.40050883304789,-17.5118770148992,
55.411546373421));
#125750=CARTESIAN_POINT('Ctrl Pts',(6.43634096453578,-17.5226996315496,
55.4171329644763));
#125751=CARTESIAN_POINT('Ctrl Pts',(6.45425703027973,-17.5281109398747,
55.419926260004));
#125752=CARTESIAN_POINT('Ctrl Pts',(6.47218581504866,-17.5334942764124,
55.4227322731676));
#125753=CARTESIAN_POINT('Ctrl Pts',(6.4901272038462,-17.5388495467521,55.4255510149582));
#125754=CARTESIAN_POINT('Ctrl Pts',(6.49909789824497,-17.5415271819219,
55.4269603858535));
#125755=CARTESIAN_POINT('Ctrl Pts',(6.50807174365058,-17.544197800546,55.4283729389003));
#125756=CARTESIAN_POINT('Ctrl Pts',(6.51704872561684,-17.5468613908419,
55.4297886754419));
#125757=CARTESIAN_POINT('Ctrl Pts',(6.51794605115068,-17.5471276392975,
55.4299301903244));
#125758=CARTESIAN_POINT('Ctrl Pts',(6.51886222152525,-17.5473993989782,
55.4300747038184));
#125759=CARTESIAN_POINT('Ctrl Pts',(6.51979159730476,-17.547674988676,55.4302213294836));
#125760=CARTESIAN_POINT('Ctrl Pts',(6.52815983905417,-17.5501564404902,
55.4315415694125));
#125761=CARTESIAN_POINT('Ctrl Pts',(6.53759930005029,-17.5529464639317,
55.4330338954395));
#125762=CARTESIAN_POINT('Ctrl Pts',(6.54398906712212,-17.5548310661202,
55.4340454359284));
#125763=CARTESIAN_POINT('Ctrl Pts',(6.68482944491206,-17.5963706216668,
55.4563413573604));
#125764=CARTESIAN_POINT('Ctrl Pts',(6.83166069154892,-17.6378547174454,
55.4803409554723));
#125765=CARTESIAN_POINT('Ctrl Pts',(6.984546755397,-17.6788176469995,55.5062351627957));
#125766=CARTESIAN_POINT('Ctrl Pts',(7.13416335766372,-17.7189045861522,
55.5315756236631));
#125767=CARTESIAN_POINT('Ctrl Pts',(7.28957895861548,-17.7584923310297,
55.5587307194324));
#125768=CARTESIAN_POINT('Ctrl Pts',(7.45082986615249,-17.797101452478,55.5878880173816));
#125769=CARTESIAN_POINT('Ctrl Pts',(7.52348653070042,-17.814498005641,55.6010257543939));
#125770=CARTESIAN_POINT('Ctrl Pts',(7.59732754358988,-17.8316952951325,
55.6145700863502));
#125771=CARTESIAN_POINT('Ctrl Pts',(7.67235428721205,-17.8486465937323,
55.6285385959872));
#125772=CARTESIAN_POINT('Ctrl Pts',(7.74096883591555,-17.8641491418532,
55.6413132805667));
#125773=CARTESIAN_POINT('Ctrl Pts',(7.81057508931384,-17.8794459293272,
55.6544427411163));
#125774=CARTESIAN_POINT('Ctrl Pts',(7.88117307932695,-17.8944998967529,
55.667940560898));
#125775=CARTESIAN_POINT('Ctrl Pts',(7.91647207433351,-17.9020268804658,
55.6746894707888));
#125776=CARTESIAN_POINT('Ctrl Pts',(7.95201900356004,-17.9094931491135,
55.6815304811982));
#125777=CARTESIAN_POINT('Ctrl Pts',(7.98781375337589,-17.9168939410521,
55.6884652887162));
#125778=CARTESIAN_POINT('Ctrl Pts',(8.00571112828382,-17.9205943370214,
55.6919326924753));
#125779=CARTESIAN_POINT('Ctrl Pts',(8.02367045834657,-17.9242783632166,
55.6954235461614));
#125780=CARTESIAN_POINT('Ctrl Pts',(8.04169172558814,-17.9279454187725,
55.6989380638335));
#125781=CARTESIAN_POINT('Ctrl Pts',(8.05070235920893,-17.9297789465505,
55.7006953226695));
#125782=CARTESIAN_POINT('Ctrl Pts',(8.05972847712441,-17.9316082316297,
55.7024584975425));
#125783=CARTESIAN_POINT('Ctrl Pts',(8.06877007664731,-17.9334331984247,
55.7042276152159));
#125784=CARTESIAN_POINT('Ctrl Pts',(8.07781167617023,-17.9352581652196,
55.7059967328893));
#125785=CARTESIAN_POINT('Ctrl Pts',(8.08877438449428,-17.9374603051664,
55.7081458861864));
#125786=CARTESIAN_POINT('Ctrl Pts',(8.09594131721416,-17.9388950681421,
55.7095528234899));
#125787=CARTESIAN_POINT('Ctrl Pts',(8.24515499940074,-17.9687664615305,
55.7388448935938));
#125788=CARTESIAN_POINT('Ctrl Pts',(8.39258291270406,-17.9962919149135,
55.7686163247889));
#125789=CARTESIAN_POINT('Ctrl Pts',(8.53813373952569,-18.0216103412977,
55.7987959487959));
#125790=CARTESIAN_POINT('Ctrl Pts',(8.76031886400935,-18.0602592300793,
55.8448655154433));
#125791=CARTESIAN_POINT('Ctrl Pts',(8.97812767280675,-18.0937657232564,
55.8918855519334));
#125792=CARTESIAN_POINT('Ctrl Pts',(9.19129301389337,-18.1226368286976,
55.9395949763453));
#125793=CARTESIAN_POINT('Ctrl Pts',(9.40660253590258,-18.1517983419189,
55.987784298836));
#125794=CARTESIAN_POINT('Ctrl Pts',(9.61717482294331,-18.1762309612043,
56.0366767735567));
#125795=CARTESIAN_POINT('Ctrl Pts',(9.82278558814653,-18.1964489204329,
56.0860161043764));
#125796=CARTESIAN_POINT('Ctrl Pts',(9.89514614563819,-18.2035642229789,
56.1033800856876));
#125797=CARTESIAN_POINT('Ctrl Pts',(9.96689264452012,-18.2101574312165,
56.1207995386339));
#125798=CARTESIAN_POINT('Ctrl Pts',(10.0380167407446,-18.2162506428644,
56.1382637195788));
#125799=CARTESIAN_POINT('Ctrl Pts',(10.1387466453931,-18.2248801884174,
56.1629974648876));
#125800=CARTESIAN_POINT('Ctrl Pts',(10.2382280323521,-18.2325068870764,
56.1878208824132));
#125801=CARTESIAN_POINT('Ctrl Pts',(10.3364396630195,-18.2391928519174,
56.2127042782402));
#125802=CARTESIAN_POINT('Ctrl Pts',(10.3662481283228,-18.2412221263488,
56.2202567018798));
#125803=CARTESIAN_POINT('Ctrl Pts',(10.3959396301051,-18.2431647334506,
56.2278146535373));
#125804=CARTESIAN_POINT('Ctrl Pts',(10.4255136353887,-18.2450223953613,
56.2353773236462));
#125805=CARTESIAN_POINT('Ctrl Pts',(10.4446592011181,-18.246225005149,56.2402732312607));
#125806=CARTESIAN_POINT('Ctrl Pts',(10.4637555247294,-18.2473920143967,
56.2451711165242));
#125807=CARTESIAN_POINT('Ctrl Pts',(10.4828024737685,-18.248523895181,56.2500707531901));
#125808=CARTESIAN_POINT('Ctrl Pts',(10.5070367847156,-18.24996403926,56.2563047866958));
#125809=CARTESIAN_POINT('Ctrl Pts',(10.5311911582704,-18.2513473167322,
56.2625416565715));
#125810=CARTESIAN_POINT('Ctrl Pts',(10.5552653290177,-18.2526746938239,
56.268780896882));
#125811=CARTESIAN_POINT('Ctrl Pts',(10.5673024143913,-18.2533383823697,
56.2719005170373));
#125812=CARTESIAN_POINT('Ctrl Pts',(10.5793194490533,-18.2539880957524,
56.2750207298374));
#125813=CARTESIAN_POINT('Ctrl Pts',(10.5913163998402,-18.2546239547716,
56.2781414779492));
#125814=CARTESIAN_POINT('Ctrl Pts',(10.6033133506272,-18.2552598137908,
56.281262226061));
#125815=CARTESIAN_POINT('Ctrl Pts',(10.6136892177232,-18.255800371469,56.2839655080025));
#125816=CARTESIAN_POINT('Ctrl Pts',(10.627246968054,-18.2564900891339,56.2875052709587));
#125817=CARTESIAN_POINT('Ctrl Pts',(10.9015920746051,-18.2704467310282,
56.3591334261967));
#125818=CARTESIAN_POINT('Ctrl Pts',(11.1720029145194,-18.2775353472381,
56.4327922782982));
#125819=CARTESIAN_POINT('Ctrl Pts',(11.4381033505419,-18.2781754605747,
56.5081406300829));
#125820=CARTESIAN_POINT('Ctrl Pts',(11.7013982102515,-18.2788088250053,
56.5826945617075));
#125821=CARTESIAN_POINT('Ctrl Pts',(11.9604729780913,-18.2731289229042,
56.6589021614018));
#125822=CARTESIAN_POINT('Ctrl Pts',(12.2150117560152,-18.261557173146,56.7364262203268));
#125823=CARTESIAN_POINT('Ctrl Pts',(12.2719104662312,-18.2589704645841,
56.7537556779423));
#125824=CARTESIAN_POINT('Ctrl Pts',(12.3285827161712,-18.2560894089725,
56.7711509039483));
#125825=CARTESIAN_POINT('Ctrl Pts',(12.3850253198193,-18.2529188169293,
56.7886081168881));
#125826=CARTESIAN_POINT('Ctrl Pts',(12.6280044057201,-18.2392697733585,
56.8637594630048));
#125827=CARTESIAN_POINT('Ctrl Pts',(12.8667244425015,-18.2202541755889,
56.9400591331704));
#125828=CARTESIAN_POINT('Ctrl Pts',(13.1009783143073,-18.1962710403985,
57.0171918416888));
#125829=CARTESIAN_POINT('Ctrl Pts',(13.3454540417339,-18.1712413818642,
57.0976902978213));
#125830=CARTESIAN_POINT('Ctrl Pts',(13.5850649647323,-18.1408012563723,
57.1790956310876));
#125831=CARTESIAN_POINT('Ctrl Pts',(13.8196238143751,-18.1054157572537,
57.2610588229446));
#125832=CARTESIAN_POINT('Ctrl Pts',(14.0016511419414,-18.0779551525953,
57.3246656354577));
#125833=CARTESIAN_POINT('Ctrl Pts',(14.1806369067664,-18.0475165221978,
57.3886085529791));
#125834=CARTESIAN_POINT('Ctrl Pts',(14.3565139790441,-18.0143210898017,
57.4527306528993));
#125835=CARTESIAN_POINT('Ctrl Pts',(14.5849508451095,-17.9712054042491,
57.5360152525438));
#125836=CARTESIAN_POINT('Ctrl Pts',(14.808142012816,-17.9234390099083,57.6196010152843));
#125837=CARTESIAN_POINT('Ctrl Pts',(15.0260000176933,-17.8715129210895,
57.7031512683577));
#125838=CARTESIAN_POINT('Ctrl Pts',(15.1122043556141,-17.8509662622235,
57.7362113078699));
#125839=CARTESIAN_POINT('Ctrl Pts',(15.197574179134,-17.8297683615518,57.7692660605151));
#125840=CARTESIAN_POINT('Ctrl Pts',(15.2821060147948,-17.8079497558195,
57.8022957994193));
#125841=CARTESIAN_POINT('Ctrl Pts',(4.94558033465909,-16.73691709796,55.07275817496));
#125842=CARTESIAN_POINT('Ctrl Pts',(5.28026245545909,-16.877827078,55.10599062996));
#125843=CARTESIAN_POINT('Ctrl Pts',(6.08156567048909,-17.18655968786,55.19564711277));
#125844=CARTESIAN_POINT('Ctrl Pts',(7.32238711382909,-17.56623194746,55.37236882206));
#125845=CARTESIAN_POINT('Ctrl Pts',(8.60269693009909,-17.85372405277,55.59911231378));
#125846=CARTESIAN_POINT('Ctrl Pts',(9.75286163943908,-18.0317753553,55.8397251211601));
#125847=CARTESIAN_POINT('Ctrl Pts',(10.8188407317891,-18.13130923193,56.09418879665));
#125848=CARTESIAN_POINT('Ctrl Pts',(11.8646555289291,-18.16653886356,56.3744521454));
#125849=CARTESIAN_POINT('Ctrl Pts',(12.9185497408191,-18.13616215699,56.68933508407));
#125850=CARTESIAN_POINT('Ctrl Pts',(13.9431659298891,-18.03863753101,57.02804389316));
#125851=CARTESIAN_POINT('Ctrl Pts',(14.8522303901791,-17.89093940842,57.3563849417));
#125852=CARTESIAN_POINT('Ctrl Pts',(15.4050401168391,-17.76756499744,57.57011599991));
#125853=CARTESIAN_POINT('Ctrl Pts',(15.6447528874391,-17.7074511508,57.66533851275));
#125854=CARTESIAN_POINT('Ctrl Pts',(1.34059656653909,-19.36072534028,56.89732226648));
#125855=CARTESIAN_POINT('Ctrl Pts',(1.74623295480909,-19.53025176889,57.0298489626201));
#125856=CARTESIAN_POINT('Ctrl Pts',(2.69773504947909,-19.86856616523,57.34298332191));
#125857=CARTESIAN_POINT('Ctrl Pts',(4.10404431957909,-20.19175246157,57.82133063031));
#125858=CARTESIAN_POINT('Ctrl Pts',(5.48295515591909,-20.33570170296,58.30871066767));
#125859=CARTESIAN_POINT('Ctrl Pts',(6.66706436789909,-20.33231978859,58.74039296884));
#125860=CARTESIAN_POINT('Ctrl Pts',(7.72117288249909,-20.22891362284,59.13262578937));
#125861=CARTESIAN_POINT('Ctrl Pts',(8.71648603674909,-20.03904678401,59.50701950141));
#125862=CARTESIAN_POINT('Ctrl Pts',(9.68245645954909,-19.76211419568,59.87017792638));
#125863=CARTESIAN_POINT('Ctrl Pts',(10.5890305168591,-19.4126839085,60.20557239847));
#125864=CARTESIAN_POINT('Ctrl Pts',(11.3702963784091,-19.03754467514,60.4854871058399));
#125865=CARTESIAN_POINT('Ctrl Pts',(11.8361982920691,-18.77679247185,60.64563044228));
#125866=CARTESIAN_POINT('Ctrl Pts',(12.0369318547391,-18.657705851,60.71311141309));
#125867=CARTESIAN_POINT('Ctrl Pts',(-1.75622200369091,-22.80586325942,55.57455847696));
#125868=CARTESIAN_POINT('Ctrl Pts',(-1.27988520209091,-23.08527728226,55.82753333339));
#125869=CARTESIAN_POINT('Ctrl Pts',(-0.164033475360911,-23.64821979482,
56.42532032641));
#125870=CARTESIAN_POINT('Ctrl Pts',(1.47552702563909,-24.21351924158,57.33972030603));
#125871=CARTESIAN_POINT('Ctrl Pts',(3.06337678448909,-24.51022608242,58.27488614442));
#125872=CARTESIAN_POINT('Ctrl Pts',(4.40638925420909,-24.57683508764,59.10793062424));
#125873=CARTESIAN_POINT('Ctrl Pts',(5.58071779312909,-24.48672687027,59.87004703943));
#125874=CARTESIAN_POINT('Ctrl Pts',(6.66586605652908,-24.26362966974,60.60326872942));
#125875=CARTESIAN_POINT('Ctrl Pts',(7.6915675903991,-23.90746855691,61.32138257166));
#125876=CARTESIAN_POINT('Ctrl Pts',(8.62353581161909,-23.43716483225,61.9914774074));
#125877=CARTESIAN_POINT('Ctrl Pts',(9.39869767618908,-22.91856774323,62.55627460265));
#125878=CARTESIAN_POINT('Ctrl Pts',(9.84576389899909,-22.55231998127,62.8815147844301));
#125879=CARTESIAN_POINT('Ctrl Pts',(10.0354867964191,-22.3841506822,63.018780147989));
#125880=CARTESIAN_POINT('Ctrl Pts',(-2.89864469832391,-25.46343319653,51.72220450345));
#125881=CARTESIAN_POINT('Ctrl Pts',(-2.38487880508091,-25.88268787062,52.0605315104));
#125882=CARTESIAN_POINT('Ctrl Pts',(-1.16727884272091,-26.76040230889,52.87121160649));
#125883=CARTESIAN_POINT('Ctrl Pts',(0.664366732859086,-27.75334589591,54.152452422));
#125884=CARTESIAN_POINT('Ctrl Pts',(2.47391773298909,-28.42777219138,55.51343497556));
#125885=CARTESIAN_POINT('Ctrl Pts',(4.02658355238909,-28.78311012245,56.77069605527));
#125886=CARTESIAN_POINT('Ctrl Pts',(5.39707932946909,-28.91632763189,57.96207291656));
#125887=CARTESIAN_POINT('Ctrl Pts',(6.67044598217909,-28.86738493337,59.15124563255));
#125888=CARTESIAN_POINT('Ctrl Pts',(7.87563878198909,-28.63632279394,60.3652287628));
#125889=CARTESIAN_POINT('Ctrl Pts',(8.96457825374909,-28.23262639115,61.55173181993));
#125890=CARTESIAN_POINT('Ctrl Pts',(9.85818132202908,-27.72155028017,62.60167870114));
#125891=CARTESIAN_POINT('Ctrl Pts',(10.3632803435291,-27.33095617795,63.233599193963));
#125892=CARTESIAN_POINT('Ctrl Pts',(10.5751031573891,-27.14651616736,63.505585203961));
#125893=CARTESIAN_POINT('',(0.214753670929088,-21.31105119265,55.46569744597));
#125894=CARTESIAN_POINT('Ctrl Pts',(4.86118780824909,-16.96274255881,55.19970889703));
#125895=CARTESIAN_POINT('Ctrl Pts',(3.24795847665787,-18.1787189357449,
55.9775434950793));
#125896=CARTESIAN_POINT('Ctrl Pts',(1.63141885578447,-19.6797052340533,
56.0974256036295));
#125897=CARTESIAN_POINT('Ctrl Pts',(0.214753670929088,-21.31105119265,55.46569744597));
#125898=CARTESIAN_POINT('',(10.422120832449,-26.9525721548983,63.3189206077878));
#125899=CARTESIAN_POINT('Ctrl Pts',(0.214753670929088,-21.31105119265,55.46569744597));
#125900=CARTESIAN_POINT('Ctrl Pts',(0.290187002274114,-21.4155332695987,
55.4996802294028));
#125901=CARTESIAN_POINT('Ctrl Pts',(0.44074324512562,-21.6239539292895,
55.5672851854211));
#125902=CARTESIAN_POINT('Ctrl Pts',(0.673504421678082,-21.9280409589524,
55.6749490529411));
#125903=CARTESIAN_POINT('Ctrl Pts',(0.910137783129716,-22.2247972557687,
55.7869376302151));
#125904=CARTESIAN_POINT('Ctrl Pts',(1.15078407677516,-22.5137264542137,
55.9037690189854));
#125905=CARTESIAN_POINT('Ctrl Pts',(1.39501754485644,-22.7949068800299,
56.0253588111342));
#125906=CARTESIAN_POINT('Ctrl Pts',(1.64265138383823,-23.0681707206839,
56.1517636676972));
#125907=CARTESIAN_POINT('Ctrl Pts',(1.89341726172454,-23.3334286266629,
56.2830032944462));
#125908=CARTESIAN_POINT('Ctrl Pts',(2.14706268673953,-23.5905979055829,
56.4191130640057));
#125909=CARTESIAN_POINT('Ctrl Pts',(2.40331415145427,-23.8396233403112,
56.5601306035357));
#125910=CARTESIAN_POINT('Ctrl Pts',(2.66190654374435,-24.0804379098326,
56.7060819271997));
#125911=CARTESIAN_POINT('Ctrl Pts',(2.92260263037789,-24.312940414964,56.8569721248615));
#125912=CARTESIAN_POINT('Ctrl Pts',(3.18514629285495,-24.537043024692,57.0128078932314));
#125913=CARTESIAN_POINT('Ctrl Pts',(3.44928284702211,-24.7526663920023,
57.1735971708211));
#125914=CARTESIAN_POINT('Ctrl Pts',(3.71474257272434,-24.9597539591783,
57.3393510545193));
#125915=CARTESIAN_POINT('Ctrl Pts',(3.98128843413907,-25.1582070270359,
57.5100682063123));
#125916=CARTESIAN_POINT('Ctrl Pts',(4.248667984514,-25.3479921026865,57.6857082905432));
#125917=CARTESIAN_POINT('Ctrl Pts',(4.51673610366451,-25.5287769949927,
57.8663174785204));
#125918=CARTESIAN_POINT('Ctrl Pts',(4.80979204127848,-25.7174013418108,
58.0688292490302));
#125919=CARTESIAN_POINT('Ctrl Pts',(5.34984032046011,-26.0368282294947,
58.4529844481055));
#125920=CARTESIAN_POINT('Ctrl Pts',(6.00395547931118,-26.3813417007364,
58.9484029796231));
#125921=CARTESIAN_POINT('Ctrl Pts',(6.76922502482267,-26.7008669853632,
59.5749062650414));
#125922=CARTESIAN_POINT('Ctrl Pts',(7.44523296529213,-26.9154311025405,
60.1638164809444));
#125923=CARTESIAN_POINT('Ctrl Pts',(8.05943260808658,-27.0474061126848,
60.7373939732686));
#125924=CARTESIAN_POINT('Ctrl Pts',(8.58328127952353,-27.1133122218592,
61.2563918549296));
#125925=CARTESIAN_POINT('Ctrl Pts',(8.99487194315013,-27.1362136993778,
61.6824057705528));
#125926=CARTESIAN_POINT('Ctrl Pts',(9.38423160485021,-27.1299300466065,
62.1028527403915));
#125927=CARTESIAN_POINT('Ctrl Pts',(9.75118830050383,-27.0960867289846,
62.5160177603512));
#125928=CARTESIAN_POINT('Ctrl Pts',(10.0969192926289,-27.0393423587567,
62.9200265760865));
#125929=CARTESIAN_POINT('Ctrl Pts',(10.3150222716872,-26.9811488497848,
63.1875477293253));
#125930=CARTESIAN_POINT('Ctrl Pts',(10.4221208324491,-26.9525721549,63.318920607788));
#125931=CARTESIAN_POINT('Origin',(17.8170477102388,-26.9525619812102,57.3553028688338));
#125932=CARTESIAN_POINT('Ctrl Pts',(15.3838087950991,-17.76813627932,57.47088283762));
#125933=CARTESIAN_POINT('Ctrl Pts',(15.5136776391891,-17.7399793982,57.61873928627));
#125934=CARTESIAN_POINT('Ctrl Pts',(16.6719036715191,-17.48466648861,58.96026165475));
#125935=CARTESIAN_POINT('Ctrl Pts',(18.6380558813391,-16.98952718735,61.62070291459));
#125936=CARTESIAN_POINT('Ctrl Pts',(20.1925743271491,-16.57554208156,64.475671438406));
#125937=CARTESIAN_POINT('Ctrl Pts',(20.8483496278291,-16.41007917736,65.90602790217));
#125938=CARTESIAN_POINT('Ctrl Pts',(11.8147841629991,-18.75274562585,60.55324082484));
#125939=CARTESIAN_POINT('Ctrl Pts',(11.9272368286891,-18.72450512001,60.68095860922));
#125940=CARTESIAN_POINT('Ctrl Pts',(12.9302993033491,-18.46854961149,61.83994096131));
#125941=CARTESIAN_POINT('Ctrl Pts',(14.6355320841891,-17.97406652798,64.141414936219));
#125942=CARTESIAN_POINT('Ctrl Pts',(15.9859865671191,-17.5628505011,66.6161169938171));
#125943=CARTESIAN_POINT('Ctrl Pts',(16.5558929421091,-17.3987396548,67.85685075686));
#125944=CARTESIAN_POINT('Ctrl Pts',(9.83041017598908,-22.50758332692,62.8274075721));
#125945=CARTESIAN_POINT('Ctrl Pts',(9.93119743901908,-22.47902391565,62.94546639158));
#125946=CARTESIAN_POINT('Ctrl Pts',(10.8283385940591,-22.22061783658,64.014699314213));
#125947=CARTESIAN_POINT('Ctrl Pts',(12.3248185130891,-21.72863725946,66.102727503159));
#125948=CARTESIAN_POINT('Ctrl Pts',(13.4841962641491,-21.32798119921,68.290608316712));
#125949=CARTESIAN_POINT('Ctrl Pts',(13.9709785907491,-21.16902646686,69.377215769556));
#125950=CARTESIAN_POINT('Ctrl Pts',(10.3574012282691,-27.27911795738,63.231333751354));
#125951=CARTESIAN_POINT('Ctrl Pts',(10.4577216764591,-27.25015329071,63.354724099072));
#125952=CARTESIAN_POINT('Ctrl Pts',(11.3476496329491,-26.98863310041,64.468911693823));
#125953=CARTESIAN_POINT('Ctrl Pts',(12.7850320790991,-26.49983263301,66.58869604085));
#125954=CARTESIAN_POINT('Ctrl Pts',(13.8555542937391,-26.11259586023,68.717148050722));
#125955=CARTESIAN_POINT('Ctrl Pts',(14.3007768717191,-25.96019336214,69.757103482774));
#125956=CARTESIAN_POINT('Ctrl Pts',(10.4221208324491,-26.9525721549,63.318920607788));
#125957=CARTESIAN_POINT('Ctrl Pts',(10.4905170530396,-26.9326350193341,
63.4037419898396));
#125958=CARTESIAN_POINT('Ctrl Pts',(11.3467766751192,-26.6801389649098,
64.4784607693732));
#125959=CARTESIAN_POINT('Ctrl Pts',(12.7315159791238,-26.2103421355703,
66.51344276841));
#125960=CARTESIAN_POINT('Ctrl Pts',(13.7906434600985,-25.8290501580449,
68.5975758543698));
#125961=CARTESIAN_POINT('Ctrl Pts',(14.2241252549691,-25.68032884552,69.591853101251));
#125962=CARTESIAN_POINT('Origin',(-10.9843331791359,-89.,80.581991049076));
#125963=CARTESIAN_POINT('',(12.8491777764712,-90.5,70.1914310155131));
#125964=CARTESIAN_POINT('Origin',(12.8491780888091,-89.,70.191430879345));
#125965=CARTESIAN_POINT('',(0.214666886482069,-89.,55.465613970957));
#125966=CARTESIAN_POINT('Origin',(-10.9843331791359,-89.,80.581991049076));
#125967=CARTESIAN_POINT('',(-0.396188736334104,-90.4999999999959,56.8356005834295));
#125968=CARTESIAN_POINT('Origin',(-0.396187662550911,-89.,56.83559817522));
#125969=CARTESIAN_POINT('Origin',(-10.9843331791359,-90.5,80.581991049076));
#125970=CARTESIAN_POINT('Origin',(6.43246351666909,-89.,72.98888938658));
#125971=CARTESIAN_POINT('',(12.8491777757672,-90.5,75.7863477573401));
#125972=CARTESIAN_POINT('Origin',(12.8491780888091,-89.,75.786347893815));
#125973=CARTESIAN_POINT('Origin',(6.43246351666909,-90.5,72.98888938658));
#125974=CARTESIAN_POINT('Origin',(-10.9843331791359,-89.,65.395787724084));
#125975=CARTESIAN_POINT('',(-0.39618873597521,-90.4999999999959,89.1421781905352));
#125976=CARTESIAN_POINT('',(0.214666886482189,-89.,90.5121648022033));
#125977=CARTESIAN_POINT('Origin',(-0.396187662550911,-89.,89.14218059794));
#125978=CARTESIAN_POINT('Origin',(-10.9843331791359,-89.,65.395787724084));
#125979=CARTESIAN_POINT('Origin',(-10.9843331791359,-90.5,65.395787724084));
#125980=CARTESIAN_POINT('Origin',(-10.9843331791359,-92.5,65.395787724084));
#125981=CARTESIAN_POINT('',(0.21473688718606,-24.69203306784,90.5121335898666));
#125982=CARTESIAN_POINT('Ctrl Pts',(8.76687408897909,-16.44294428525,98.6115064056));
#125983=CARTESIAN_POINT('Ctrl Pts',(8.50448839268907,-16.29482593816,98.7748340168099));
#125984=CARTESIAN_POINT('Ctrl Pts',(7.73803846225909,-15.84050813694,99.1889282148399));
#125985=CARTESIAN_POINT('Ctrl Pts',(6.5349477692391,-15.02004513321,99.57986765328));
#125986=CARTESIAN_POINT('Ctrl Pts',(5.27236547025909,-14.00812222941,99.71688058005));
#125987=CARTESIAN_POINT('Ctrl Pts',(4.18367013900909,-13.00986029655,99.6525682338999));
#125988=CARTESIAN_POINT('Ctrl Pts',(3.20714073810909,-11.9973978225,99.4540121251699));
#125989=CARTESIAN_POINT('Ctrl Pts',(2.30415558486909,-10.93738557134,99.14726582813));
#125990=CARTESIAN_POINT('Ctrl Pts',(1.48684448748909,-9.84723726948199,
98.7638938018301));
#125991=CARTESIAN_POINT('Ctrl Pts',(0.762911702719089,-8.74553579959698,
98.3366761029799));
#125992=CARTESIAN_POINT('Ctrl Pts',(0.112673674949087,-7.60752902450998,
97.87904754731));
#125993=CARTESIAN_POINT('Ctrl Pts',(-0.488386309690911,-6.37224922945299,
97.3887134898101));
#125994=CARTESIAN_POINT('Ctrl Pts',(-1.04213634100091,-4.97114208044499,
96.8726660516999));
#125995=CARTESIAN_POINT('Ctrl Pts',(-1.51067364081091,-3.36802983074299,
96.3809404461301));
#125996=CARTESIAN_POINT('Ctrl Pts',(-1.81701727702091,-1.61981132427399,
96.0275490175501));
#125997=CARTESIAN_POINT('Ctrl Pts',(-1.87689058580091,-0.403435681896786,
95.95525979127));
#125998=CARTESIAN_POINT('Ctrl Pts',(-1.86852961382091,0.200651371990514,
95.9651297134299));
#125999=CARTESIAN_POINT('Ctrl Pts',(6.48819653156909,-15.56528785696,92.69131734964));
#126000=CARTESIAN_POINT('Ctrl Pts',(6.38630096531909,-15.47758556196,92.78395944648));
#126001=CARTESIAN_POINT('Ctrl Pts',(6.06771745324909,-15.21581444004,93.0220629079301));
#126002=CARTESIAN_POINT('Ctrl Pts',(5.4599981715091,-14.7540110982,93.25770281466));
#126003=CARTESIAN_POINT('Ctrl Pts',(4.67600680749909,-14.1542490297,93.3348504985));
#126004=CARTESIAN_POINT('Ctrl Pts',(3.89225004337909,-13.51762150969,93.2708681228701));
#126005=CARTESIAN_POINT('Ctrl Pts',(3.10219061563909,-12.82180106148,93.10110938746));
#126006=CARTESIAN_POINT('Ctrl Pts',(2.29351899611909,-12.03547497051,92.8361696333));
#126007=CARTESIAN_POINT('Ctrl Pts',(1.49269764718909,-11.16347023105,92.4954481808701));
#126008=CARTESIAN_POINT('Ctrl Pts',(0.723899763099089,-10.21566958806,92.10308906725));
#126009=CARTESIAN_POINT('Ctrl Pts',(-0.0200535606409112,-9.16446753653399,
91.66798555359));
#126010=CARTESIAN_POINT('Ctrl Pts',(-0.760996247700911,-7.93604781061299,
91.18364248321));
#126011=CARTESIAN_POINT('Ctrl Pts',(-1.50146348324091,-6.42271318686499,
90.65003751555));
#126012=CARTESIAN_POINT('Ctrl Pts',(-2.18733220258091,-4.52156727656799,
90.1121766327));
#126013=CARTESIAN_POINT('Ctrl Pts',(-2.67864361223591,-2.24136809065099,
89.70052285778));
#126014=CARTESIAN_POINT('Ctrl Pts',(-2.78026244461691,-0.556674570830786,
89.61294403093));
#126015=CARTESIAN_POINT('Ctrl Pts',(-2.76634006182491,0.277047208448614,
89.6246271184));
#126016=CARTESIAN_POINT('Ctrl Pts',(2.72889798757909,-19.34707978044,89.1447316619801));
#126017=CARTESIAN_POINT('Ctrl Pts',(2.66091020417909,-19.26097438926,89.20317193542));
#126018=CARTESIAN_POINT('Ctrl Pts',(2.42996072068909,-19.00901506437,89.3612231288901));
#126019=CARTESIAN_POINT('Ctrl Pts',(1.89825599140909,-18.57235792605,89.54995470502));
#126020=CARTESIAN_POINT('Ctrl Pts',(1.10699433400909,-17.98310305551,89.64471299023));
#126021=CARTESIAN_POINT('Ctrl Pts',(0.252027388659088,-17.32630382037,89.6293082806));
#126022=CARTESIAN_POINT('Ctrl Pts',(-0.654644487020914,-16.5759732809,89.5211787480401));
#126023=CARTESIAN_POINT('Ctrl Pts',(-1.61859475251091,-15.69330276297,89.32252842609));
#126024=CARTESIAN_POINT('Ctrl Pts',(-2.60190967346991,-14.67920705201,89.04432012876));
#126025=CARTESIAN_POINT('Ctrl Pts',(-3.56872088692091,-13.5426076308,88.7048190356501));
#126026=CARTESIAN_POINT('Ctrl Pts',(-4.52340351538191,-12.24737090716,88.3108681836801));
#126027=CARTESIAN_POINT('Ctrl Pts',(-5.49218708965691,-10.69472182793,87.8542655723));
#126028=CARTESIAN_POINT('Ctrl Pts',(-6.47884434265791,-8.73212611500698,
87.33045821777));
#126029=CARTESIAN_POINT('Ctrl Pts',(-7.41072188100292,-6.20174180863199,
86.77974038575));
#126030=CARTESIAN_POINT('Ctrl Pts',(-8.09046417872891,-3.09478014856899,
86.34080207947));
#126031=CARTESIAN_POINT('Ctrl Pts',(-8.23255272084991,-0.768163226373987,
86.24527748657));
#126032=CARTESIAN_POINT('Ctrl Pts',(-8.21314998798691,0.382355724809714,
86.2578544693));
#126033=CARTESIAN_POINT('Ctrl Pts',(0.196332399109088,-25.06476693734,90.52591274045));
#126034=CARTESIAN_POINT('Ctrl Pts',(0.011250503809089,-24.92028925106,90.61126618974));
#126035=CARTESIAN_POINT('Ctrl Pts',(-0.555409203350912,-24.48834062706,
90.84285524963));
#126036=CARTESIAN_POINT('Ctrl Pts',(-1.58520004181091,-23.72520655934,91.1268519171499));
#126037=CARTESIAN_POINT('Ctrl Pts',(-2.86435733527191,-22.73723822501,91.3040139279599));
#126038=CARTESIAN_POINT('Ctrl Pts',(-4.11539939684391,-21.69298831769,91.35045014482));
#126039=CARTESIAN_POINT('Ctrl Pts',(-5.35778473735791,-20.55625239098,91.29239781524));
#126040=CARTESIAN_POINT('Ctrl Pts',(-6.61477798365991,-19.27659173514,91.13677980334));
#126041=CARTESIAN_POINT('Ctrl Pts',(-7.84814243484691,-17.86250092626,90.8959268123599));
#126042=CARTESIAN_POINT('Ctrl Pts',(-9.02351089959392,-16.33037133773,90.58921613446));
#126043=CARTESIAN_POINT('Ctrl Pts',(-10.1541748021089,-14.63600828855,90.2254084335399));
#126044=CARTESIAN_POINT('Ctrl Pts',(-11.2746720699649,-12.6615424041,89.79831775978));
#126045=CARTESIAN_POINT('Ctrl Pts',(-12.3896921849461,-10.2361987255,89.30460716211));
#126046=CARTESIAN_POINT('Ctrl Pts',(-13.4190864676907,-7.19853323577899,
88.78356996623));
#126047=CARTESIAN_POINT('Ctrl Pts',(-14.1550194975079,-3.56544121650899,
88.3679745890099));
#126048=CARTESIAN_POINT('Ctrl Pts',(-14.3071566503109,-0.885592743395686,
88.2775704089799));
#126049=CARTESIAN_POINT('Ctrl Pts',(-14.2863014408449,0.440736329119914,
88.28947825565));
#126050=CARTESIAN_POINT('Ctrl Pts',(0.214736886699963,-24.69203306784,90.5121335896161));
#126051=CARTESIAN_POINT('Ctrl Pts',(0.135114761630916,-24.5692710385346,
90.5476371811463));
#126052=CARTESIAN_POINT('Ctrl Pts',(0.052735907442164,-24.4383412814108,
90.5820965139287));
#126053=CARTESIAN_POINT('Ctrl Pts',(-0.0321695795334493,-24.2989037853877,
90.6151059543716));
#126054=CARTESIAN_POINT('Ctrl Pts',(-0.114946239082119,-24.1629623928139,
90.6472877521653));
#126055=CARTESIAN_POINT('Ctrl Pts',(-0.200124190341312,-24.0189345404467,
90.6780910702463));
#126056=CARTESIAN_POINT('Ctrl Pts',(-0.287451667108242,-23.866505156519,
90.7071710142038));
#126057=CARTESIAN_POINT('Ctrl Pts',(-0.373795459489902,-23.7157927854992,
90.7359233924528));
#126058=CARTESIAN_POINT('Ctrl Pts',(-0.462240397255042,-23.5568670919221,
90.7629906234067));
#126059=CARTESIAN_POINT('Ctrl Pts',(-0.552508207420546,-23.3894235317423,
90.7880757248107));
#126060=CARTESIAN_POINT('Ctrl Pts',(-0.641604436653361,-23.2241532123008,
90.8128352480662));
#126061=CARTESIAN_POINT('Ctrl Pts',(-0.732476223101845,-23.0505846972385,
90.8356634669094));
#126062=CARTESIAN_POINT('Ctrl Pts',(-0.824825740468708,-22.8684251472527,
90.8563154157583));
#126063=CARTESIAN_POINT('Ctrl Pts',(-0.885203755326287,-22.749329429927,
90.869817637643));
#126064=CARTESIAN_POINT('Ctrl Pts',(-0.946212818488541,-22.6265614486943,
90.8823904467332));
#126065=CARTESIAN_POINT('Ctrl Pts',(-1.00776358327158,-22.5000393642437,
90.8939758070014));
#126066=CARTESIAN_POINT('Origin',(-2.02513312664091,-22.5,85.48888938658));
#126067=CARTESIAN_POINT('Origin',(-5.70733270705591,-22.5,87.05138938658));
#126068=CARTESIAN_POINT('Origin',(-2.02513312664091,-22.5,85.48888938658));
#126069=CARTESIAN_POINT('Origin',(27.4324635166691,-22.5,72.98888938658));
#126070=CARTESIAN_POINT('Origin',(-6.80729512863291,91.08441266238,84.10819367738));
#126071=CARTESIAN_POINT('Origin',(27.4324635166691,-10.,72.98888938658));
#126072=CARTESIAN_POINT('Origin',(-5.70733270705591,-10.,58.92638938658));
#126073=CARTESIAN_POINT('Origin',(-2.02513312664091,-10.,60.48888938658));
#126074=CARTESIAN_POINT('Origin',(-2.02513312664091,-10.,60.48888938658));
#126075=CARTESIAN_POINT('Origin',(1.07038457110909,25.,122.41156512159));
#126076=CARTESIAN_POINT('',(-2.29980363729091,-12.04041068638,54.99575678068));
#126077=CARTESIAN_POINT('Ctrl Pts',(-2.14405189383092,-11.77841163181,54.98461154933));
#126078=CARTESIAN_POINT('Ctrl Pts',(-2.10733458956091,-11.8187886285,54.98225755956));
#126079=CARTESIAN_POINT('Ctrl Pts',(-1.81762989816091,-12.13455643069,54.96398728809));
#126080=CARTESIAN_POINT('Ctrl Pts',(-1.26179089513091,-12.69950422949,54.933471617));
#126081=CARTESIAN_POINT('Ctrl Pts',(-0.446514994060916,-13.4374136371,54.90142190873));
#126082=CARTESIAN_POINT('Ctrl Pts',(0.421832340659087,-14.13773705744,54.88216946334));
#126083=CARTESIAN_POINT('Ctrl Pts',(1.37110882200909,-14.81739036068,54.87937527486));
#126084=CARTESIAN_POINT('Ctrl Pts',(2.42408380219909,-15.48145775016,54.89986692453));
#126085=CARTESIAN_POINT('Ctrl Pts',(3.59645485546909,-16.12374680622,54.954373838));
#126086=CARTESIAN_POINT('Ctrl Pts',(4.53992671491909,-16.5656803246,55.02943094317));
#126087=CARTESIAN_POINT('Ctrl Pts',(5.09008858763909,-16.7974718924,55.08714039026));
#126088=CARTESIAN_POINT('Ctrl Pts',(5.21318854215909,-16.84808010424,55.10078336932));
#126089=CARTESIAN_POINT('Ctrl Pts',(-4.28237251991691,-12.90485596602,55.1580085027501));
#126090=CARTESIAN_POINT('Ctrl Pts',(-4.24372968062391,-12.94840060018,55.15907732619));
#126091=CARTESIAN_POINT('Ctrl Pts',(-3.93840831922691,-13.28959911889,55.16788641051));
#126092=CARTESIAN_POINT('Ctrl Pts',(-3.34715337824091,-13.90827595377,55.19058747105));
#126093=CARTESIAN_POINT('Ctrl Pts',(-2.48081635714091,-14.71143693515,55.23984234275));
#126094=CARTESIAN_POINT('Ctrl Pts',(-1.55944190911091,-15.46716013561,55.31045650299));
#126095=CARTESIAN_POINT('Ctrl Pts',(-0.557170387470911,-16.1876489274,55.40933310786));
#126096=CARTESIAN_POINT('Ctrl Pts',(0.548874055019088,-16.87559341254,55.54601184312));
#126097=CARTESIAN_POINT('Ctrl Pts',(1.76798737872909,-17.51338121009,55.7316611044));
#126098=CARTESIAN_POINT('Ctrl Pts',(2.73528991332909,-17.92273736427,55.91074213052));
#126099=CARTESIAN_POINT('Ctrl Pts',(3.29175315981909,-18.1226855046,56.02609352246));
#126100=CARTESIAN_POINT('Ctrl Pts',(3.41585682087909,-18.16550598283,56.0524294903401));
#126101=CARTESIAN_POINT('Ctrl Pts',(-6.33980068353391,-13.96283635342,54.43755959959));
#126102=CARTESIAN_POINT('Ctrl Pts',(-6.30013246113791,-14.01063098128,54.44188653861));
#126103=CARTESIAN_POINT('Ctrl Pts',(-5.98625783669891,-14.38591317071,54.47649765105));
#126104=CARTESIAN_POINT('Ctrl Pts',(-5.37248291156191,-15.07664932369,54.5503049645301));
#126105=CARTESIAN_POINT('Ctrl Pts',(-4.47094738816091,-15.97723355204,54.67900680025));
#126106=CARTESIAN_POINT('Ctrl Pts',(-3.50976072054391,-16.82815842919,54.83934263413));
#126107=CARTESIAN_POINT('Ctrl Pts',(-2.46460587503091,-17.63890746411,55.04250813135));
#126108=CARTESIAN_POINT('Ctrl Pts',(-1.31102675741091,-18.41248543844,55.3026771825401));
#126109=CARTESIAN_POINT('Ctrl Pts',(-0.0441936566409133,-19.12227138079,
55.63466619505));
#126110=CARTESIAN_POINT('Ctrl Pts',(0.954446004809087,-19.56714593259,55.93839568086));
#126111=CARTESIAN_POINT('Ctrl Pts',(1.52418405419909,-19.77714734994,56.12781832211));
#126112=CARTESIAN_POINT('Ctrl Pts',(1.65098036279909,-19.82165893627,56.17076531156));
#126113=CARTESIAN_POINT('Ctrl Pts',(-8.03244000396691,-14.8063662618,52.92267673657));
#126114=CARTESIAN_POINT('Ctrl Pts',(-7.99278803894591,-14.85890679976,52.92964751905));
#126115=CARTESIAN_POINT('Ctrl Pts',(-7.67860378938091,-15.27222254309,52.98522301204));
#126116=CARTESIAN_POINT('Ctrl Pts',(-7.05831227750691,-16.04340511569,53.10097414993));
#126117=CARTESIAN_POINT('Ctrl Pts',(-6.14229777174491,-17.06014121543,53.29630276114));
#126118=CARTESIAN_POINT('Ctrl Pts',(-5.16000730910191,-18.03293316272,53.5338349975401));
#126119=CARTESIAN_POINT('Ctrl Pts',(-4.08799815650491,-18.97091254114,53.82951707404));
#126120=CARTESIAN_POINT('Ctrl Pts',(-2.89897827285191,-19.88006417146,54.20343973087));
#126121=CARTESIAN_POINT('Ctrl Pts',(-1.59003255186091,-20.72841292249,54.67677305415));
#126122=CARTESIAN_POINT('Ctrl Pts',(-0.556873398130915,-21.27200059043,
55.10857579009));
#126123=CARTESIAN_POINT('Ctrl Pts',(0.0312811456690863,-21.53256477732,
55.37827818613));
#126124=CARTESIAN_POINT('Ctrl Pts',(0.162087495049087,-21.58801296415,55.43946214072));
#126125=CARTESIAN_POINT('Ctrl Pts',(-2.29980340877935,-12.0404106863416,
54.9957613525836));
#126126=CARTESIAN_POINT('Ctrl Pts',(-2.29979627965971,-12.0404473675576,
54.9957609965661));
#126127=CARTESIAN_POINT('Ctrl Pts',(-2.29978915050876,-12.0404840487877,
54.9957606405607));
#126128=CARTESIAN_POINT('Ctrl Pts',(-2.29978202132649,-12.0405207300321,
54.9957602845673));
#126129=CARTESIAN_POINT('Ctrl Pts',(-2.27572901261885,-12.1642788632817,
54.9945592054126));
#126130=CARTESIAN_POINT('Ctrl Pts',(-2.2513175691152,-12.2882021978735,
54.993495270802));
#126131=CARTESIAN_POINT('Ctrl Pts',(-2.22648966927543,-12.4123811458191,
54.9925841664874));
#126132=CARTESIAN_POINT('Ctrl Pts',(-2.20172610202318,-12.5362383286098,
54.9916754229724));
#126133=CARTESIAN_POINT('Ctrl Pts',(-2.1765480591974,-12.6603501622916,
54.9909187023437));
#126134=CARTESIAN_POINT('Ctrl Pts',(-2.15092231702737,-12.7847590309372,
54.9903311614157));
#126135=CARTESIAN_POINT('Ctrl Pts',(-2.12529657485734,-12.9091678995828,
54.9897436204878));
#126136=CARTESIAN_POINT('Ctrl Pts',(-2.09922294790261,-13.0338741904353,
54.9893252401201));
#126137=CARTESIAN_POINT('Ctrl Pts',(-2.07269530706027,-13.1588672637238,
54.9890950393045));
#126138=CARTESIAN_POINT('Ctrl Pts',(-2.00845697777614,-13.4615457509614,
54.9885375937375));
#126139=CARTESIAN_POINT('Ctrl Pts',(-1.94157305345321,-13.7658810338058,
54.9890823794828));
#126140=CARTESIAN_POINT('Ctrl Pts',(-1.87208962015349,-14.0716870597456,
54.9910178180691));
#126141=CARTESIAN_POINT('Ctrl Pts',(-1.85651589013135,-14.1402291605164,
54.9914516192874));
#126142=CARTESIAN_POINT('Ctrl Pts',(-1.8408114204113,-14.2088450198168,
54.991955403005));
#126143=CARTESIAN_POINT('Ctrl Pts',(-1.82497643282323,-14.2775323299277,
54.9925326544939));
#126144=CARTESIAN_POINT('Ctrl Pts',(-1.78082973392649,-14.4690271435882,
54.9941419862047));
#126145=CARTESIAN_POINT('Ctrl Pts',(-1.735666691271,-14.6610810017041,54.9963214523107));
#126146=CARTESIAN_POINT('Ctrl Pts',(-1.68945916723778,-14.8536488722862,
54.9991469932073));
#126147=CARTESIAN_POINT('Ctrl Pts',(-1.64325164320455,-15.0462167428683,
55.001972534104));
#126148=CARTESIAN_POINT('Ctrl Pts',(-1.59599946347008,-15.2392990217843,
55.0054438945215));
#126149=CARTESIAN_POINT('Ctrl Pts',(-1.54769772308862,-15.4328022255565,
55.0096508046892));
#126150=CARTESIAN_POINT('Ctrl Pts',(-1.53176134994561,-15.4966454584365,
55.0110388062329));
#126151=CARTESIAN_POINT('Ctrl Pts',(-1.51571096741508,-15.5605340258221,
55.0125070139342));
#126152=CARTESIAN_POINT('Ctrl Pts',(-1.49954709930578,-15.6244654940096,
55.0140584675908));
#126153=CARTESIAN_POINT('Ctrl Pts',(-1.47759392156854,-15.7112948887208,
55.0161655955163));
#126154=CARTESIAN_POINT('Ctrl Pts',(-1.45543143911073,-15.798203392864,
55.0184262598809));
#126155=CARTESIAN_POINT('Ctrl Pts',(-1.43306031387933,-15.8851854425692,
55.0208484533193));
#126156=CARTESIAN_POINT('Ctrl Pts',(-1.42187475126362,-15.9286764674218,
55.0220595500385));
#126157=CARTESIAN_POINT('Ctrl Pts',(-1.41063702858815,-15.9721858786649,
55.0233110347678));
#126158=CARTESIAN_POINT('Ctrl Pts',(-1.39934713818154,-16.0157130538162,
55.0246039542798));
#126159=CARTESIAN_POINT('Ctrl Pts',(-1.39370219297824,-16.0374766413918,
55.0252504140358));
#126160=CARTESIAN_POINT('Ctrl Pts',(-1.38804420588604,-16.0592446699445,
55.0259072329045));
#126161=CARTESIAN_POINT('Ctrl Pts',(-1.38237317309397,-16.0810170640224,
55.0265745446507));
#126162=CARTESIAN_POINT('Ctrl Pts',(-1.37953765669793,-16.0919032610614,
55.0269082005238));
#126163=CARTESIAN_POINT('Ctrl Pts',(-1.37669887888011,-16.1027905494816,
55.0272444796433));
#126164=CARTESIAN_POINT('Ctrl Pts',(-1.3738568388251,-16.113678920125,55.027583398937));
#126165=CARTESIAN_POINT('Ctrl Pts',(-1.37101479877008,-16.1245672907683,
55.0279223182307));
#126166=CARTESIAN_POINT('Ctrl Pts',(-1.36865251609714,-16.133610081709,
55.0282055102779));
#126167=CARTESIAN_POINT('Ctrl Pts',(-1.36532093103418,-16.1463472696511,
55.0286080943937));
#126168=CARTESIAN_POINT('Ctrl Pts',(-1.32033570854725,-16.3183330429714,
55.0340440462533));
#126169=CARTESIAN_POINT('Ctrl Pts',(-1.27477572945593,-16.4896151849966,
55.040113685044));
#126170=CARTESIAN_POINT('Ctrl Pts',(-1.22867726285142,-16.6601973448782,
55.0468623692584));
#126171=CARTESIAN_POINT('Ctrl Pts',(-1.16978974220244,-16.8781039522402,
55.0554833345595));
#126172=CARTESIAN_POINT('Ctrl Pts',(-1.11001923437359,-17.0948742436374,
55.0652120839941));
#126173=CARTESIAN_POINT('Ctrl Pts',(-1.04940924672357,-17.3104263127349,
55.0761380260064));
#126174=CARTESIAN_POINT('Ctrl Pts',(-0.988799259073545,-17.5259783818323,
55.0870639680186));
#126175=CARTESIAN_POINT('Ctrl Pts',(-0.927349920031676,-17.7403122086757,
55.0991866017856));
#126176=CARTESIAN_POINT('Ctrl Pts',(-0.865126498396156,-17.9532975613375,
55.1126099267491));
#126177=CARTESIAN_POINT('Ctrl Pts',(-0.861262891894302,-17.9665223498771,
55.1134434142727));
#126178=CARTESIAN_POINT('Ctrl Pts',(-0.857396307508481,-17.9797419240376,
55.1142819226883));
#126179=CARTESIAN_POINT('Ctrl Pts',(-0.853526763430693,-17.9929562465901,
55.1151254794357));
#126180=CARTESIAN_POINT('Ctrl Pts',(-0.828492501792921,-18.0784471471962,
55.1205829234907));
#126181=CARTESIAN_POINT('Ctrl Pts',(-0.803334389201592,-18.163718240567,
55.1262516375727));
#126182=CARTESIAN_POINT('Ctrl Pts',(-0.778057158148713,-18.248764113097,
55.1321368969883));
#126183=CARTESIAN_POINT('Ctrl Pts',(-0.763464992700593,-18.2978598166588,
55.1355343687651));
#126184=CARTESIAN_POINT('Ctrl Pts',(-0.748833131789826,-18.3468804357216,
55.1390040107368));
#126185=CARTESIAN_POINT('Ctrl Pts',(-0.734162426679192,-18.3958249557652,
55.1425469019139));
#126186=CARTESIAN_POINT('Ctrl Pts',(-0.726827074123874,-18.4202972157869,
55.1443183475024));
#126187=CARTESIAN_POINT('Ctrl Pts',(-0.719482010669794,-18.4447504510539,
55.1461081059892));
#126188=CARTESIAN_POINT('Ctrl Pts',(-0.712127340211664,-18.4691845275153,
55.1479163168723));
#126189=CARTESIAN_POINT('Ctrl Pts',(-0.706611337368068,-18.4875100848613,
55.1492724750347));
#126190=CARTESIAN_POINT('Ctrl Pts',(-0.701089930596245,-18.5058248653791,
55.150639012722));
#126191=CARTESIAN_POINT('Ctrl Pts',(-0.695563163090249,-18.5241288135701,
55.1520159900027));
#126192=CARTESIAN_POINT('Ctrl Pts',(-0.693720907254918,-18.5302301296337,
55.1524749824295));
#126193=CARTESIAN_POINT('Ctrl Pts',(-0.692327278617444,-18.5348440206536,
55.1528227186659));
#126194=CARTESIAN_POINT('Ctrl Pts',(-0.690034610190422,-18.5424291489228,
55.1533964494393));
#126195=CARTESIAN_POINT('Ctrl Pts',(-0.614956638884621,-18.7908192064774,
55.1721844006473));
#126196=CARTESIAN_POINT('Ctrl Pts',(-0.539153626642809,-19.0361926767024,
55.1928330519685));
#126197=CARTESIAN_POINT('Ctrl Pts',(-0.462786056000691,-19.2784783689272,
55.2154576486142));
#126198=CARTESIAN_POINT('Ctrl Pts',(-0.44434194325563,-19.336994628988,
55.2209218870054));
#126199=CARTESIAN_POINT('Ctrl Pts',(-0.425864730362313,-19.3953308171107,
55.2265015432689));
#126200=CARTESIAN_POINT('Ctrl Pts',(-0.407356350425952,-19.4534860061815,
55.2321985735646));
#126201=CARTESIAN_POINT('Ctrl Pts',(-0.328708790148578,-19.7006045413324,
55.2564069340542));
#126202=CARTESIAN_POINT('Ctrl Pts',(-0.249496603748653,-19.9444575557464,
55.2827320599704));
#126203=CARTESIAN_POINT('Ctrl Pts',(-0.169859166644958,-20.18488117157,
55.311268127787));
#126204=CARTESIAN_POINT('Ctrl Pts',(-0.09455233110252,-20.4122307995318,
55.3382524337146));
#126205=CARTESIAN_POINT('Ctrl Pts',(-0.0188656993732753,-20.6365133872874,
55.367212997343));
#126206=CARTESIAN_POINT('Ctrl Pts',(0.0570693465599587,-20.8575662264015,
55.3982676679193));
#126207=CARTESIAN_POINT('Ctrl Pts',(0.0757505374372732,-20.9119486295556,
55.4059075951958));
#126208=CARTESIAN_POINT('Ctrl Pts',(0.0944467137683982,-20.9661354554094,
55.4136744827716));
#126209=CARTESIAN_POINT('Ctrl Pts',(0.113155831545745,-21.0201240906044,
55.421570535909));
#126210=CARTESIAN_POINT('Ctrl Pts',(0.146987875206053,-21.1177527380272,
55.4358491148174));
#126211=CARTESIAN_POINT('Ctrl Pts',(0.180862205655314,-21.2147333141768,
55.4505500132441));
#126212=CARTESIAN_POINT('Ctrl Pts',(0.214763979944339,-21.3110511932278,
55.4656743286618));
#126213=CARTESIAN_POINT('Origin',(-10.9843331791359,-92.5,80.581991049076));
#126214=CARTESIAN_POINT('',(0.214770326079967,-21.31105119265,55.4656600933121));
#126215=CARTESIAN_POINT('Origin',(-2.02513312664091,-89.,60.48888938658));
#126216=CARTESIAN_POINT('',(-7.08815755064836,-89.,58.3404518887897));
#126217=CARTESIAN_POINT('Origin',(-2.02513312664091,-89.,60.48888938658));
#126218=CARTESIAN_POINT('',(-5.70733025545361,-90.4999999999959,58.9263904268899));
#126219=CARTESIAN_POINT('Origin',(-5.70733270705591,-89.,58.92638938658));
#126220=CARTESIAN_POINT('Origin',(-2.02513312664091,-90.49999999999,60.48888938658));
#126221=CARTESIAN_POINT('Origin',(-2.27593483123091,-90.5,69.192338555332));
#126222=CARTESIAN_POINT('',(-5.70733025554977,-90.4999999999959,87.0513883463108));
#126223=CARTESIAN_POINT('Origin',(27.4324635166691,-90.5,72.98888938658));
#126224=CARTESIAN_POINT('Origin',(-2.02513312664091,-90.49999999999,85.48888938658));
#126225=CARTESIAN_POINT('Origin',(-2.02513312664091,-89.,85.48888938658));
#126226=CARTESIAN_POINT('',(-7.08815755202979,-89.,87.6373268811148));
#126227=CARTESIAN_POINT('Origin',(-5.70733270705591,-89.,87.05138938658));
#126228=CARTESIAN_POINT('Origin',(-2.02513312664091,-89.,85.48888938658));
#126229=CARTESIAN_POINT('Origin',(-2.02513312664091,-92.5,85.48888938658));
#126230=CARTESIAN_POINT('',(-7.08838180624485,-85.174012662148,87.6374220205403));
#126231=CARTESIAN_POINT('',(-7.08815755434906,25.,87.6373268756495));
#126232=CARTESIAN_POINT('Ctrl Pts',(-7.08838180624485,-85.174012662148,
87.6374220205403));
#126233=CARTESIAN_POINT('Ctrl Pts',(-7.06379631478045,-84.9618158750809,
87.6953760007039));
#126234=CARTESIAN_POINT('Ctrl Pts',(-7.03898074672462,-84.748459068266,
87.7510083865588));
#126235=CARTESIAN_POINT('Ctrl Pts',(-7.01416074376767,-84.5339843926944,
87.8044020256059));
#126236=CARTESIAN_POINT('Ctrl Pts',(-6.98859134290818,-84.3130340179738,
87.8594077950456));
#126237=CARTESIAN_POINT('Ctrl Pts',(-6.96301669278039,-84.0908972668471,
87.9120376933239));
#126238=CARTESIAN_POINT('Ctrl Pts',(-6.93764503641729,-83.8675829154453,
87.9623644050187));
#126239=CARTESIAN_POINT('Ctrl Pts',(-6.91121161522479,-83.6349232016113,
88.0147972122593));
#126240=CARTESIAN_POINT('Ctrl Pts',(-6.88499796602311,-83.400985352606,
88.0647302007003));
#126241=CARTESIAN_POINT('Ctrl Pts',(-6.85920704409652,-83.1657384765946,
88.1122242130556));
#126242=CARTESIAN_POINT('Ctrl Pts',(-6.85103788991991,-83.0912251263091,
88.1272677198562));
#126243=CARTESIAN_POINT('Ctrl Pts',(-6.84291094610431,-83.0165801426965,
88.1420663642715));
#126244=CARTESIAN_POINT('Ctrl Pts',(-6.83483216441449,-82.9418017191346,
88.1566216159116));
#126245=CARTESIAN_POINT('Ctrl Pts',(-6.82950767478839,-82.8925174389302,
88.1662145581817));
#126246=CARTESIAN_POINT('Ctrl Pts',(-6.82420410061484,-82.8431751901153,
88.1757017737205));
#126247=CARTESIAN_POINT('Ctrl Pts',(-6.81892303812862,-82.7937759979044,
88.185084240871));
#126248=CARTESIAN_POINT('Ctrl Pts',(-6.79460184830759,-82.5662749725138,
88.2282938724841));
#126249=CARTESIAN_POINT('Ctrl Pts',(-6.77075938383651,-82.3375651317986,
88.2692827739492));
#126250=CARTESIAN_POINT('Ctrl Pts',(-6.74754396638005,-82.1076627398156,
88.3081343431746));
#126251=CARTESIAN_POINT('Ctrl Pts',(-6.7295030810263,-81.929003764413,88.3383262062985));
#126252=CARTESIAN_POINT('Ctrl Pts',(-6.71184063768807,-81.7496235979736,
88.3672266692105));
#126253=CARTESIAN_POINT('Ctrl Pts',(-6.69462624070162,-81.5695127023199,
88.3948617495597));
#126254=CARTESIAN_POINT('Ctrl Pts',(-6.67494310539971,-81.3635718766673,
88.4264600115273));
#126255=CARTESIAN_POINT('Ctrl Pts',(-6.65584272326395,-81.1566825793778,
88.4564089810734));
#126256=CARTESIAN_POINT('Ctrl Pts',(-6.63741409551801,-80.9488448097589,
88.4847575516344));
#126257=CARTESIAN_POINT('Ctrl Pts',(-6.62819978164503,-80.8449259249494,
88.4989318369149));
#126258=CARTESIAN_POINT('Ctrl Pts',(-6.61915331092193,-80.740769922046,
88.5127059616475));
#126259=CARTESIAN_POINT('Ctrl Pts',(-6.61028508149103,-80.6363768009134,
88.526086081745));
#126260=CARTESIAN_POINT('Ctrl Pts',(-6.60585096677558,-80.5841802403472,
88.5327761417938));
#126261=CARTESIAN_POINT('Ctrl Pts',(-6.6014614077024,-80.5319244002237,
88.5393676980408));
#126262=CARTESIAN_POINT('Ctrl Pts',(-6.59711767521138,-80.479609280531,
88.5458615114224));
#126263=CARTESIAN_POINT('Ctrl Pts',(-6.59494580896587,-80.4534517206847,
88.5491084181132));
#126264=CARTESIAN_POINT('Ctrl Pts',(-6.5927853991295,-80.4272793409462,
88.5523308889536));
#126265=CARTESIAN_POINT('Ctrl Pts',(-6.59063660249566,-80.4010921413147,
88.5555290194189));
#126266=CARTESIAN_POINT('Ctrl Pts',(-6.58848780586183,-80.3749049416833,
88.5587271498841));
#126267=CARTESIAN_POINT('Ctrl Pts',(-6.58644354173115,-80.3498490744125,
88.561763247515));
#126268=CARTESIAN_POINT('Ctrl Pts',(-6.58422520796802,-80.3224860827418,
88.5650504850222));
#126269=CARTESIAN_POINT('Ctrl Pts',(-6.5641013055288,-80.0742591549545,
88.594871086408));
#126270=CARTESIAN_POINT('Ctrl Pts',(-6.54513483205179,-79.8256135763339,
88.622367628329));
#126271=CARTESIAN_POINT('Ctrl Pts',(-6.52746563345973,-79.5765104364289,
88.6476204732732));
#126272=CARTESIAN_POINT('Ctrl Pts',(-6.51570540126308,-79.410712833842,
88.6644282146444));
#126273=CARTESIAN_POINT('Ctrl Pts',(-6.50452000859505,-79.2447115819987,
88.6802414043915));
#126274=CARTESIAN_POINT('Ctrl Pts',(-6.49395442975159,-79.0784852886401,
88.6950766706492));
#126275=CARTESIAN_POINT('Ctrl Pts',(-6.47849511246648,-78.8352667155519,
88.7167832985099));
#126276=CARTESIAN_POINT('Ctrl Pts',(-6.46436081725034,-78.5915678258629,
88.7363976088991));
#126277=CARTESIAN_POINT('Ctrl Pts',(-6.45152907111565,-78.3474341596224,
88.7540024507364));
#126278=CARTESIAN_POINT('Ctrl Pts',(-6.43850088405651,-78.099563056358,
88.7718768047171));
#126279=CARTESIAN_POINT('Ctrl Pts',(-6.42681516618875,-77.8512432568754,
88.787679653157));
#126280=CARTESIAN_POINT('Ctrl Pts',(-6.41648321794231,-77.6024927608509,
88.8014696460193));
#126281=CARTESIAN_POINT('Ctrl Pts',(-6.4060523720161,-77.3513612185502,
88.8153916370552));
#126282=CARTESIAN_POINT('Ctrl Pts',(-6.3970010649043,-77.0997901362597,
88.8272620102371));
#126283=CARTESIAN_POINT('Ctrl Pts',(-6.38938018142158,-76.8477761615928,
88.8371134105489));
#126284=CARTESIAN_POINT('Ctrl Pts',(-6.38178064370192,-76.5964680671039,
88.8469372175172));
#126285=CARTESIAN_POINT('Ctrl Pts',(-6.37560331098471,-76.3447189675036,
88.8547532740801));
#126286=CARTESIAN_POINT('Ctrl Pts',(-6.37094103456924,-76.0925125845702,
88.8605674847034));
#126287=CARTESIAN_POINT('Ctrl Pts',(-6.3663487990775,-75.8440950735223,
88.8662943490076));
#126288=CARTESIAN_POINT('Ctrl Pts',(-6.36322629828271,-75.5952333553235,
88.870078969759));
#126289=CARTESIAN_POINT('Ctrl Pts',(-6.36170597022165,-75.345907828253,
88.8719025711441));
#126290=CARTESIAN_POINT('Ctrl Pts',(-6.36100416191559,-75.2308150859092,
88.8727443753782));
#126291=CARTESIAN_POINT('Ctrl Pts',(-6.36064438933148,-75.1156235047724,
88.8731679708493));
#126292=CARTESIAN_POINT('Ctrl Pts',(-6.36064303502447,-75.0003313582817,
88.8731697877795));
#126293=CARTESIAN_POINT('Ctrl Pts',(-6.36064303474443,-75.0003075183965,
88.8731697881552));
#126294=CARTESIAN_POINT('Ctrl Pts',(-6.36064303447919,-75.0002836785154,
88.8731697885135));
#126295=CARTESIAN_POINT('Ctrl Pts',(-6.36064303422876,-75.0002598386384,
88.8731697888545));
#126296=CARTESIAN_POINT('Ctrl Pts',(-6.36064040478154,-74.749954905453,
88.873173369011));
#126297=CARTESIAN_POINT('Ctrl Pts',(-6.36226546725732,-74.5001035131016,
88.8712654272117));
#126298=CARTESIAN_POINT('Ctrl Pts',(-6.36540095128621,-74.2506871861409,
88.8674288772245));
#126299=CARTESIAN_POINT('Ctrl Pts',(-6.36856865307248,-73.9987080540005,
88.8635529058799));
#126300=CARTESIAN_POINT('Ctrl Pts',(-6.37327831247089,-73.7471724121695,
88.8577085442994));
#126301=CARTESIAN_POINT('Ctrl Pts',(-6.37945535068582,-73.4960730086243,
88.8498538881179));
#126302=CARTESIAN_POINT('Ctrl Pts',(-6.38565345904744,-73.2441170940647,
88.8419724393617));
#126303=CARTESIAN_POINT('Ctrl Pts',(-6.39332933367653,-72.9925998472497,
88.8320670081214));
#126304=CARTESIAN_POINT('Ctrl Pts',(-6.40244871597262,-72.7415341444287,
88.8200701793989));
#126305=CARTESIAN_POINT('Ctrl Pts',(-6.40753807971511,-72.6014188774695,
88.8133749644004));
#126306=CARTESIAN_POINT('Ctrl Pts',(-6.41307773369852,-72.4614446543939,
88.8060279205458));
#126307=CARTESIAN_POINT('Ctrl Pts',(-6.41906664530995,-72.3216174025011,
88.7980138504433));
#126308=CARTESIAN_POINT('Ctrl Pts',(-6.42961412702571,-72.0753580688533,
88.7838997236438));
#126309=CARTESIAN_POINT('Ctrl Pts',(-6.44153217487,-71.8295371924908,88.7677456148225));
#126310=CARTESIAN_POINT('Ctrl Pts',(-6.45477307066889,-71.5841478194717,
88.749542707656));
#126311=CARTESIAN_POINT('Ctrl Pts',(-6.46538522433686,-71.3874761006909,
88.7349536608884));
#126312=CARTESIAN_POINT('Ctrl Pts',(-6.4768478731557,-71.1910816029631,
88.7190480585771));
#126313=CARTESIAN_POINT('Ctrl Pts',(-6.48915450788134,-70.9949691674386,
88.7018075585331));
#126314=CARTESIAN_POINT('Ctrl Pts',(-6.49071134690436,-70.9701601518685,
88.6996265656099));
#126315=CARTESIAN_POINT('Ctrl Pts',(-6.49228157490731,-70.9453555172984,
88.6974243856275));
#126316=CARTESIAN_POINT('Ctrl Pts',(-6.4938652542253,-70.9205553918243,
88.6952008885181));
#126317=CARTESIAN_POINT('Ctrl Pts',(-6.50635089886465,-70.7250325039749,
88.6776709539853));
#126318=CARTESIAN_POINT('Ctrl Pts',(-6.51967225333885,-70.5297886023269,
88.6588166712615));
#126319=CARTESIAN_POINT('Ctrl Pts',(-6.53376669716175,-70.3348221400914,
88.6385974917835));
#126320=CARTESIAN_POINT('Ctrl Pts',(-6.54170778878621,-70.2249741347525,
88.627205601559));
#126321=CARTESIAN_POINT('Ctrl Pts',(-6.54989441621222,-70.1152143819194,
88.6153802361868));
#126322=CARTESIAN_POINT('Ctrl Pts',(-6.55831520320439,-70.0055428830087,
88.6031139835115));
#126323=CARTESIAN_POINT('Ctrl Pts',(-6.56252559670048,-69.9507071335534,
88.5969808571739));
#126324=CARTESIAN_POINT('Ctrl Pts',(-6.56679452679293,-69.8958934475535,
88.5907375074315));
#126325=CARTESIAN_POINT('Ctrl Pts',(-6.57112054094054,-69.8411018250717,
88.5843830071542));
#126326=CARTESIAN_POINT('Ctrl Pts',(-6.57328354801434,-69.8137060138308,
88.5812057570156));
#126327=CARTESIAN_POINT('Ctrl Pts',(-6.57546082583398,-69.7863157184686,
88.5780007191089));
#126328=CARTESIAN_POINT('Ctrl Pts',(-6.57765219046004,-69.7589309389883,
88.574767777654));
#126329=CARTESIAN_POINT('Ctrl Pts',(-6.5798435550861,-69.7315461595081,
88.5715348361991));
#126330=CARTESIAN_POINT('Ctrl Pts',(-6.58214338518519,-69.7030028197464,
88.5681341312207));
#126331=CARTESIAN_POINT('Ctrl Pts',(-6.58426835938578,-69.6767931481951,
88.5649851265532));
#126332=CARTESIAN_POINT('Ctrl Pts',(-6.60448470513764,-69.4274424586774,
88.5350264724128));
#126333=CARTESIAN_POINT('Ctrl Pts',(-6.62580950443919,-69.1794547193134,
88.5028101608645));
#126334=CARTESIAN_POINT('Ctrl Pts',(-6.64806081890539,-68.9327838372194,
88.4683145058022));
#126335=CARTESIAN_POINT('Ctrl Pts',(-6.66995243203797,-68.6901004878794,
88.434376486701));
#126336=CARTESIAN_POINT('Ctrl Pts',(-6.69274146521221,-68.4486914334156,
88.3982322076366));
#126337=CARTESIAN_POINT('Ctrl Pts',(-6.71626520022788,-68.2085505509096,
88.3598306420088));
#126338=CARTESIAN_POINT('Ctrl Pts',(-6.73899437491936,-67.9765208980757,
88.3227261646374));
#126339=CARTESIAN_POINT('Ctrl Pts',(-6.76240999994988,-67.7456750207067,
88.2835142412598));
#126340=CARTESIAN_POINT('Ctrl Pts',(-6.78636679563562,-67.5160464093315,
88.242121012596));
#126341=CARTESIAN_POINT('Ctrl Pts',(-6.80235411105814,-67.3628061726886,
88.2144976771682));
#126342=CARTESIAN_POINT('Ctrl Pts',(-6.81858245485541,-67.2101088308579,
88.1859023530971));
#126343=CARTESIAN_POINT('Ctrl Pts',(-6.8350072566281,-67.0579751615403,
88.1563059844045));
#126344=CARTESIAN_POINT('Ctrl Pts',(-6.85993106443988,-66.8271199957825,
88.1113949884954));
#126345=CARTESIAN_POINT('Ctrl Pts',(-6.8853085719417,-66.5975613278129,
88.0641797110285));
#126346=CARTESIAN_POINT('Ctrl Pts',(-6.91096401058241,-66.3692379839661,
88.0146005159368));
#126347=CARTESIAN_POINT('Ctrl Pts',(-6.9359277552185,-66.1470704455322,
87.9663580211244));
#126348=CARTESIAN_POINT('Ctrl Pts',(-6.96115522877894,-65.9260725236057,
87.9158772269839));
#126349=CARTESIAN_POINT('Ctrl Pts',(-6.98645999388353,-65.7062244363269,
87.8630827857479));
#126350=CARTESIAN_POINT('Ctrl Pts',(-7.01070555469572,-65.4955787279977,
87.8124982088809));
#126351=CARTESIAN_POINT('Ctrl Pts',(-7.03502249709539,-65.2859887012326,
87.7597894706709));
#126352=CARTESIAN_POINT('Ctrl Pts',(-7.05921693797329,-65.077470153448,
87.7048733754824));
#126353=CARTESIAN_POINT('Ctrl Pts',(-7.06896378908785,-64.9934674170285,
87.6827501527844));
#126354=CARTESIAN_POINT('Ctrl Pts',(-7.07869037563948,-64.9096389534572,
87.6602685078946));
#126355=CARTESIAN_POINT('Ctrl Pts',(-7.08838231939817,-64.8259873690431,
87.6374222559034));
#126356=CARTESIAN_POINT('Origin',(-2.02513312664091,25.,60.48888938658));
#126357=CARTESIAN_POINT('',(-6.36087450269922,-74.999999801042,57.1044283173086));
#126358=CARTESIAN_POINT('Ctrl Pts',(-7.08825603872491,-64.825987319,58.34041012264));
#126359=CARTESIAN_POINT('Ctrl Pts',(-6.99794665049256,-65.6045290148126,
58.1278601811754));
#126360=CARTESIAN_POINT('Ctrl Pts',(-6.9052605176683,-66.3985891148802,
57.94616482494));
#126361=CARTESIAN_POINT('Ctrl Pts',(-6.77559174784533,-67.6129568713641,
57.7156393481809));
#126362=CARTESIAN_POINT('Ctrl Pts',(-6.73388211710599,-68.0216257245892,
57.6457863578687));
#126363=CARTESIAN_POINT('Ctrl Pts',(-6.67482143432723,-68.6404484060224,
57.5508991529112));
#126364=CARTESIAN_POINT('Ctrl Pts',(-6.64616303810798,-68.9513145971379,
57.5059287097987));
#126365=CARTESIAN_POINT('Ctrl Pts',(-6.6144832189235,-69.3165378083041,
57.457666220138));
#126366=CARTESIAN_POINT('Ctrl Pts',(-6.60130426161773,-69.4736076105606,
57.4378700643154));
#126367=CARTESIAN_POINT('Ctrl Pts',(-6.59260914456376,-69.5784420495982,
57.4248685010235));
#126368=CARTESIAN_POINT('Ctrl Pts',(-6.58847553231003,-69.6288394451349,
57.4187153470913));
#126369=CARTESIAN_POINT('Ctrl Pts',(-6.44248193445931,-71.4312631171058,
57.202390535774));
#126370=CARTESIAN_POINT('Ctrl Pts',(-6.36088862142065,-73.2034436053334,
57.1049235992306));
#126371=CARTESIAN_POINT('Ctrl Pts',(-6.36082055131842,-74.9999998096187,
57.1044704220667));
#126372=CARTESIAN_POINT('',(-7.08824189517591,-85.17401265925,58.3404161122));
#126373=CARTESIAN_POINT('Ctrl Pts',(-6.36082055131591,-74.99999987577,57.10447042205));
#126374=CARTESIAN_POINT('Ctrl Pts',(-6.36078005345576,-75.8984830421777,
57.104784515926));
#126375=CARTESIAN_POINT('Ctrl Pts',(-6.38054797589447,-76.7906363769049,
57.1296675300475));
